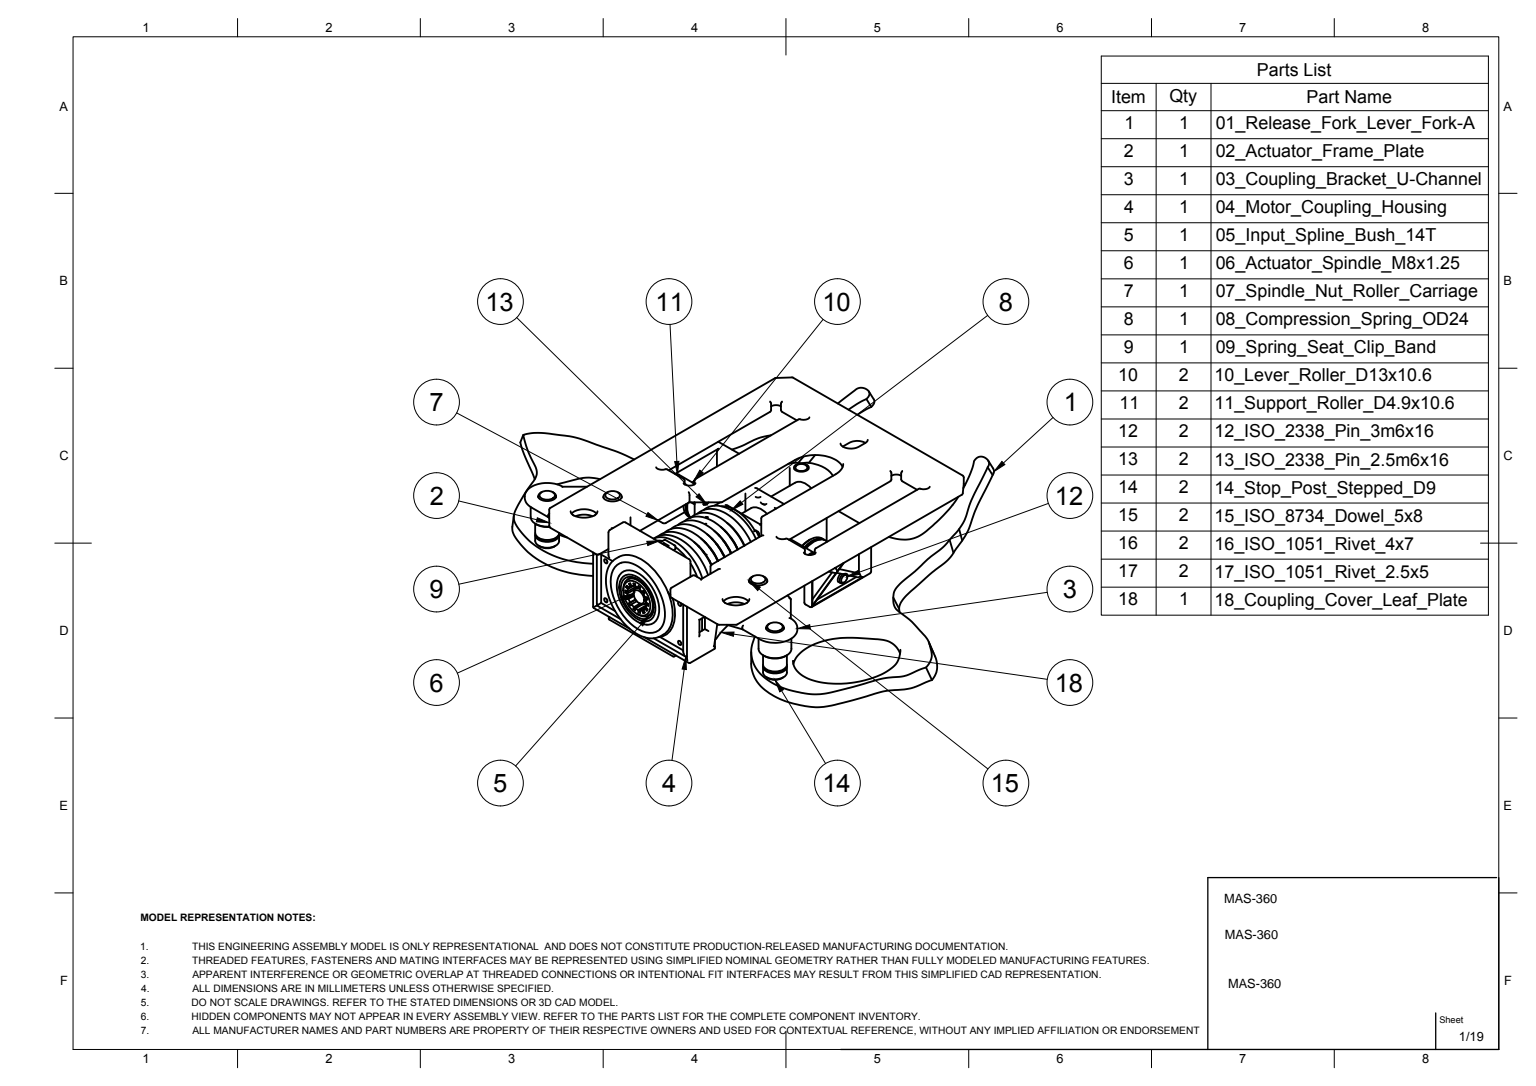
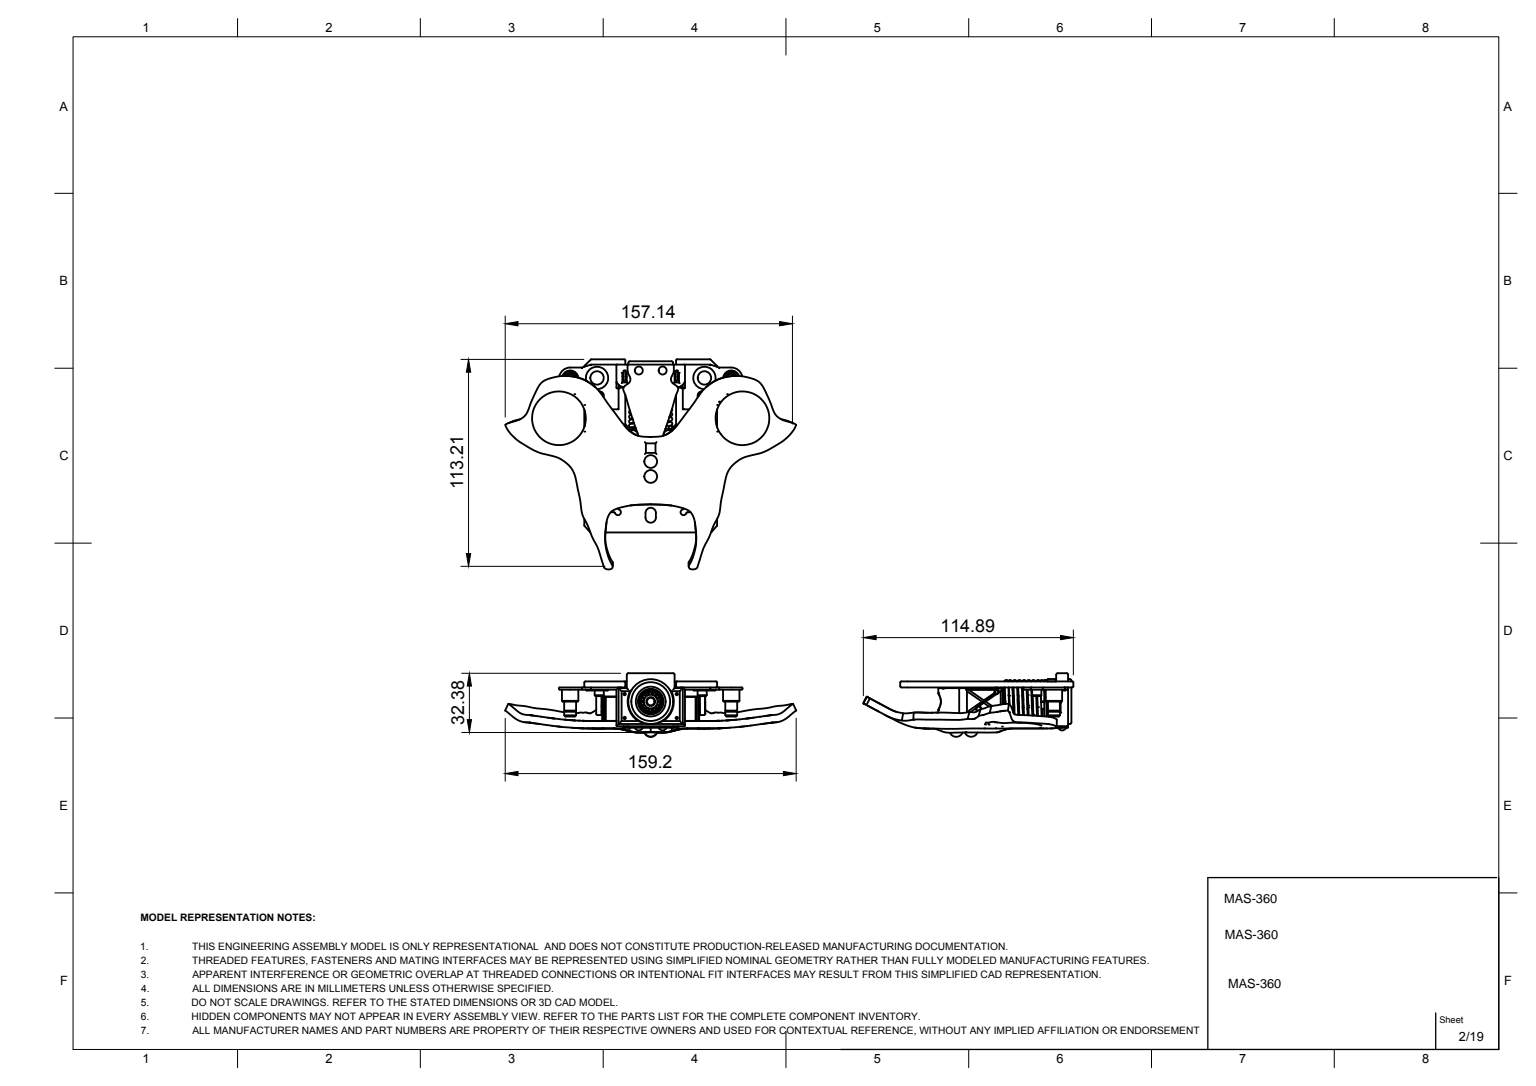
ISO-10303-21;
HEADER;
/* Generated by software containing ST-Developer
 * from STEP Tools, Inc. (www.steptools.com) 
 */

FILE_DESCRIPTION(
/* description */ (''),
/* implementation_level */ '2;1');

FILE_NAME(
/* name */ 'MAS-360',
/* time_stamp */ '2026-11-04T18:53:29-08:00',
/* author */ (''),
/* organization */ (''),
/* preprocessor_version */ 'ST-DEVELOPER v20.2',
/* originating_system */ 'Autodesk Translation Framework v15.17.0.0',
/* authorisation */ '');

FILE_SCHEMA (('AUTOMOTIVE_DESIGN { 1 0 10303 214 3 1 1 }'));
ENDSEC;

DATA;
#10=MECHANICAL_DESIGN_GEOMETRIC_PRESENTATION_REPRESENTATION('',(#1327,#1328,
#1329,#1330,#1331,#1332,#1333,#1334,#1335,#1336,#1337,#1338,#1339,#1340,
#1341,#1342,#1343,#1344),#100031);
#11=ITEM_DEFINED_TRANSFORMATION($,$,#20335,#22499);
#12=ITEM_DEFINED_TRANSFORMATION($,$,#20343,#22500);
#13=ITEM_DEFINED_TRANSFORMATION($,$,#20892,#22501);
#14=ITEM_DEFINED_TRANSFORMATION($,$,#21261,#22502);
#15=ITEM_DEFINED_TRANSFORMATION($,$,#21437,#22503);
#16=ITEM_DEFINED_TRANSFORMATION($,$,#21537,#22504);
#17=ITEM_DEFINED_TRANSFORMATION($,$,#21611,#22505);
#18=ITEM_DEFINED_TRANSFORMATION($,$,#22152,#22506);
#19=ITEM_DEFINED_TRANSFORMATION($,$,#22157,#22507);
#20=ITEM_DEFINED_TRANSFORMATION($,$,#22351,#22508);
#21=ITEM_DEFINED_TRANSFORMATION($,$,#22404,#22509);
#22=ITEM_DEFINED_TRANSFORMATION($,$,#22417,#22510);
#23=ITEM_DEFINED_TRANSFORMATION($,$,#22427,#22511);
#24=ITEM_DEFINED_TRANSFORMATION($,$,#22437,#22512);
#25=ITEM_DEFINED_TRANSFORMATION($,$,#22465,#22513);
#26=ITEM_DEFINED_TRANSFORMATION($,$,#22475,#22514);
#27=ITEM_DEFINED_TRANSFORMATION($,$,#22489,#22515);
#28=ITEM_DEFINED_TRANSFORMATION($,$,#22218,#22516);
#29=ITEM_DEFINED_TRANSFORMATION($,$,#22351,#22517);
#30=ITEM_DEFINED_TRANSFORMATION($,$,#22404,#22518);
#31=ITEM_DEFINED_TRANSFORMATION($,$,#22417,#22519);
#32=ITEM_DEFINED_TRANSFORMATION($,$,#22427,#22520);
#33=ITEM_DEFINED_TRANSFORMATION($,$,#22437,#22521);
#34=ITEM_DEFINED_TRANSFORMATION($,$,#22465,#22522);
#35=ITEM_DEFINED_TRANSFORMATION($,$,#22475,#22523);
#36=ITEM_DEFINED_TRANSFORMATION($,$,#22489,#22524);
#37=(
REPRESENTATION_RELATIONSHIP($,$,#100101,#100100)
REPRESENTATION_RELATIONSHIP_WITH_TRANSFORMATION(#11)
SHAPE_REPRESENTATION_RELATIONSHIP()
);
#38=(
REPRESENTATION_RELATIONSHIP($,$,#100102,#100100)
REPRESENTATION_RELATIONSHIP_WITH_TRANSFORMATION(#12)
SHAPE_REPRESENTATION_RELATIONSHIP()
);
#39=(
REPRESENTATION_RELATIONSHIP($,$,#100103,#100100)
REPRESENTATION_RELATIONSHIP_WITH_TRANSFORMATION(#13)
SHAPE_REPRESENTATION_RELATIONSHIP()
);
#40=(
REPRESENTATION_RELATIONSHIP($,$,#100104,#100100)
REPRESENTATION_RELATIONSHIP_WITH_TRANSFORMATION(#14)
SHAPE_REPRESENTATION_RELATIONSHIP()
);
#41=(
REPRESENTATION_RELATIONSHIP($,$,#100105,#100100)
REPRESENTATION_RELATIONSHIP_WITH_TRANSFORMATION(#15)
SHAPE_REPRESENTATION_RELATIONSHIP()
);
#42=(
REPRESENTATION_RELATIONSHIP($,$,#100106,#100100)
REPRESENTATION_RELATIONSHIP_WITH_TRANSFORMATION(#16)
SHAPE_REPRESENTATION_RELATIONSHIP()
);
#43=(
REPRESENTATION_RELATIONSHIP($,$,#100107,#100100)
REPRESENTATION_RELATIONSHIP_WITH_TRANSFORMATION(#17)
SHAPE_REPRESENTATION_RELATIONSHIP()
);
#44=(
REPRESENTATION_RELATIONSHIP($,$,#100108,#100100)
REPRESENTATION_RELATIONSHIP_WITH_TRANSFORMATION(#18)
SHAPE_REPRESENTATION_RELATIONSHIP()
);
#45=(
REPRESENTATION_RELATIONSHIP($,$,#100109,#100100)
REPRESENTATION_RELATIONSHIP_WITH_TRANSFORMATION(#19)
SHAPE_REPRESENTATION_RELATIONSHIP()
);
#46=(
REPRESENTATION_RELATIONSHIP($,$,#100111,#100100)
REPRESENTATION_RELATIONSHIP_WITH_TRANSFORMATION(#20)
SHAPE_REPRESENTATION_RELATIONSHIP()
);
#47=(
REPRESENTATION_RELATIONSHIP($,$,#100112,#100100)
REPRESENTATION_RELATIONSHIP_WITH_TRANSFORMATION(#21)
SHAPE_REPRESENTATION_RELATIONSHIP()
);
#48=(
REPRESENTATION_RELATIONSHIP($,$,#100113,#100100)
REPRESENTATION_RELATIONSHIP_WITH_TRANSFORMATION(#22)
SHAPE_REPRESENTATION_RELATIONSHIP()
);
#49=(
REPRESENTATION_RELATIONSHIP($,$,#100114,#100100)
REPRESENTATION_RELATIONSHIP_WITH_TRANSFORMATION(#23)
SHAPE_REPRESENTATION_RELATIONSHIP()
);
#50=(
REPRESENTATION_RELATIONSHIP($,$,#100115,#100100)
REPRESENTATION_RELATIONSHIP_WITH_TRANSFORMATION(#24)
SHAPE_REPRESENTATION_RELATIONSHIP()
);
#51=(
REPRESENTATION_RELATIONSHIP($,$,#100116,#100100)
REPRESENTATION_RELATIONSHIP_WITH_TRANSFORMATION(#25)
SHAPE_REPRESENTATION_RELATIONSHIP()
);
#52=(
REPRESENTATION_RELATIONSHIP($,$,#100117,#100100)
REPRESENTATION_RELATIONSHIP_WITH_TRANSFORMATION(#26)
SHAPE_REPRESENTATION_RELATIONSHIP()
);
#53=(
REPRESENTATION_RELATIONSHIP($,$,#100118,#100100)
REPRESENTATION_RELATIONSHIP_WITH_TRANSFORMATION(#27)
SHAPE_REPRESENTATION_RELATIONSHIP()
);
#54=(
REPRESENTATION_RELATIONSHIP($,$,#100110,#100100)
REPRESENTATION_RELATIONSHIP_WITH_TRANSFORMATION(#28)
SHAPE_REPRESENTATION_RELATIONSHIP()
);
#55=(
REPRESENTATION_RELATIONSHIP($,$,#100111,#100100)
REPRESENTATION_RELATIONSHIP_WITH_TRANSFORMATION(#29)
SHAPE_REPRESENTATION_RELATIONSHIP()
);
#56=(
REPRESENTATION_RELATIONSHIP($,$,#100112,#100100)
REPRESENTATION_RELATIONSHIP_WITH_TRANSFORMATION(#30)
SHAPE_REPRESENTATION_RELATIONSHIP()
);
#57=(
REPRESENTATION_RELATIONSHIP($,$,#100113,#100100)
REPRESENTATION_RELATIONSHIP_WITH_TRANSFORMATION(#31)
SHAPE_REPRESENTATION_RELATIONSHIP()
);
#58=(
REPRESENTATION_RELATIONSHIP($,$,#100114,#100100)
REPRESENTATION_RELATIONSHIP_WITH_TRANSFORMATION(#32)
SHAPE_REPRESENTATION_RELATIONSHIP()
);
#59=(
REPRESENTATION_RELATIONSHIP($,$,#100115,#100100)
REPRESENTATION_RELATIONSHIP_WITH_TRANSFORMATION(#33)
SHAPE_REPRESENTATION_RELATIONSHIP()
);
#60=(
REPRESENTATION_RELATIONSHIP($,$,#100116,#100100)
REPRESENTATION_RELATIONSHIP_WITH_TRANSFORMATION(#34)
SHAPE_REPRESENTATION_RELATIONSHIP()
);
#61=(
REPRESENTATION_RELATIONSHIP($,$,#100117,#100100)
REPRESENTATION_RELATIONSHIP_WITH_TRANSFORMATION(#35)
SHAPE_REPRESENTATION_RELATIONSHIP()
);
#62=(
REPRESENTATION_RELATIONSHIP($,$,#100118,#100100)
REPRESENTATION_RELATIONSHIP_WITH_TRANSFORMATION(#36)
SHAPE_REPRESENTATION_RELATIONSHIP()
);
#63=CONTEXT_DEPENDENT_SHAPE_REPRESENTATION(#37,#100074);
#64=CONTEXT_DEPENDENT_SHAPE_REPRESENTATION(#38,#100075);
#65=CONTEXT_DEPENDENT_SHAPE_REPRESENTATION(#39,#100076);
#66=CONTEXT_DEPENDENT_SHAPE_REPRESENTATION(#40,#100077);
#67=CONTEXT_DEPENDENT_SHAPE_REPRESENTATION(#41,#100078);
#68=CONTEXT_DEPENDENT_SHAPE_REPRESENTATION(#42,#100079);
#69=CONTEXT_DEPENDENT_SHAPE_REPRESENTATION(#43,#100080);
#70=CONTEXT_DEPENDENT_SHAPE_REPRESENTATION(#44,#100081);
#71=CONTEXT_DEPENDENT_SHAPE_REPRESENTATION(#45,#100082);
#72=CONTEXT_DEPENDENT_SHAPE_REPRESENTATION(#46,#100083);
#73=CONTEXT_DEPENDENT_SHAPE_REPRESENTATION(#47,#100084);
#74=CONTEXT_DEPENDENT_SHAPE_REPRESENTATION(#48,#100085);
#75=CONTEXT_DEPENDENT_SHAPE_REPRESENTATION(#49,#100086);
#76=CONTEXT_DEPENDENT_SHAPE_REPRESENTATION(#50,#100087);
#77=CONTEXT_DEPENDENT_SHAPE_REPRESENTATION(#51,#100088);
#78=CONTEXT_DEPENDENT_SHAPE_REPRESENTATION(#52,#100089);
#79=CONTEXT_DEPENDENT_SHAPE_REPRESENTATION(#53,#100090);
#80=CONTEXT_DEPENDENT_SHAPE_REPRESENTATION(#54,#100091);
#81=CONTEXT_DEPENDENT_SHAPE_REPRESENTATION(#55,#100092);
#82=CONTEXT_DEPENDENT_SHAPE_REPRESENTATION(#56,#100093);
#83=CONTEXT_DEPENDENT_SHAPE_REPRESENTATION(#57,#100094);
#84=CONTEXT_DEPENDENT_SHAPE_REPRESENTATION(#58,#100095);
#85=CONTEXT_DEPENDENT_SHAPE_REPRESENTATION(#59,#100096);
#86=CONTEXT_DEPENDENT_SHAPE_REPRESENTATION(#60,#100097);
#87=CONTEXT_DEPENDENT_SHAPE_REPRESENTATION(#61,#100098);
#88=CONTEXT_DEPENDENT_SHAPE_REPRESENTATION(#62,#100099);
#89=NEXT_ASSEMBLY_USAGE_OCCURRENCE('01_Release_Fork_Lever_Fork-A:1',
'01_Release_Fork_Lever_Fork-A:1','01_Release_Fork_Lever_Fork-A:1',#100120,
#100121,'01_Release_Fork_Lever_Fork-A:1');
#90=NEXT_ASSEMBLY_USAGE_OCCURRENCE('02_Actuator_Frame_Plate:1',
'02_Actuator_Frame_Plate:1','02_Actuator_Frame_Plate:1',#100120,#100122,
'02_Actuator_Frame_Plate:1');
#91=NEXT_ASSEMBLY_USAGE_OCCURRENCE('03_Coupling_Bracket_U-Channel:1',
'03_Coupling_Bracket_U-Channel:1','03_Coupling_Bracket_U-Channel:1',#100120,
#100123,'03_Coupling_Bracket_U-Channel:1');
#92=NEXT_ASSEMBLY_USAGE_OCCURRENCE('04_Motor_Coupling_Housing:1',
'04_Motor_Coupling_Housing:1','04_Motor_Coupling_Housing:1',#100120,#100124,
'04_Motor_Coupling_Housing:1');
#93=NEXT_ASSEMBLY_USAGE_OCCURRENCE('05_Input_Spline_Bush_14T:1',
'05_Input_Spline_Bush_14T:1','05_Input_Spline_Bush_14T:1',#100120,#100125,
'05_Input_Spline_Bush_14T:1');
#94=NEXT_ASSEMBLY_USAGE_OCCURRENCE('06_Actuator_Spindle_M8x1.25:1',
'06_Actuator_Spindle_M8x1.25:1','06_Actuator_Spindle_M8x1.25:1',#100120,
#100126,'06_Actuator_Spindle_M8x1.25:1');
#95=NEXT_ASSEMBLY_USAGE_OCCURRENCE('07_Spindle_Nut_Roller_Carriage:1',
'07_Spindle_Nut_Roller_Carriage:1','07_Spindle_Nut_Roller_Carriage:1',#100120,
#100127,'07_Spindle_Nut_Roller_Carriage:1');
#96=NEXT_ASSEMBLY_USAGE_OCCURRENCE('08_Compression_Spring_OD24:1',
'08_Compression_Spring_OD24:1','08_Compression_Spring_OD24:1',#100120,#100128,
'08_Compression_Spring_OD24:1');
#97=NEXT_ASSEMBLY_USAGE_OCCURRENCE('09_Spring_Seat_Clip_Band:1',
'09_Spring_Seat_Clip_Band:1','09_Spring_Seat_Clip_Band:1',#100120,#100129,
'09_Spring_Seat_Clip_Band:1');
#98=NEXT_ASSEMBLY_USAGE_OCCURRENCE('10_Lever_Roller_D13x10.6:1',
'10_Lever_Roller_D13x10.6:1','10_Lever_Roller_D13x10.6:1',#100120,#100131,
'10_Lever_Roller_D13x10.6:1');
#99=NEXT_ASSEMBLY_USAGE_OCCURRENCE('11_Support_Roller_D4.9x10.6:1',
'11_Support_Roller_D4.9x10.6:1','11_Support_Roller_D4.9x10.6:1',#100120,
#100132,'11_Support_Roller_D4.9x10.6:1');
#100=NEXT_ASSEMBLY_USAGE_OCCURRENCE('12_ISO_2338_Pin_3m6x16:1',
'12_ISO_2338_Pin_3m6x16:1','12_ISO_2338_Pin_3m6x16:1',#100120,#100133,
'12_ISO_2338_Pin_3m6x16:1');
#101=NEXT_ASSEMBLY_USAGE_OCCURRENCE('13_ISO_2338_Pin_2.5m6x16:1',
'13_ISO_2338_Pin_2.5m6x16:1','13_ISO_2338_Pin_2.5m6x16:1',#100120,#100134,
'13_ISO_2338_Pin_2.5m6x16:1');
#102=NEXT_ASSEMBLY_USAGE_OCCURRENCE('14_Stop_Post_Stepped_D9:1',
'14_Stop_Post_Stepped_D9:1','14_Stop_Post_Stepped_D9:1',#100120,#100135,
'14_Stop_Post_Stepped_D9:1');
#103=NEXT_ASSEMBLY_USAGE_OCCURRENCE('15_ISO_8734_Dowel_5x8:1',
'15_ISO_8734_Dowel_5x8:1','15_ISO_8734_Dowel_5x8:1',#100120,#100136,
'15_ISO_8734_Dowel_5x8:1');
#104=NEXT_ASSEMBLY_USAGE_OCCURRENCE('16_ISO_1051_Rivet_4x7:1',
'16_ISO_1051_Rivet_4x7:1','16_ISO_1051_Rivet_4x7:1',#100120,#100137,
'16_ISO_1051_Rivet_4x7:1');
#105=NEXT_ASSEMBLY_USAGE_OCCURRENCE('17_ISO_1051_Rivet_2.5x5:1',
'17_ISO_1051_Rivet_2.5x5:1','17_ISO_1051_Rivet_2.5x5:1',#100120,#100138,
'17_ISO_1051_Rivet_2.5x5:1');
#106=NEXT_ASSEMBLY_USAGE_OCCURRENCE('18_Coupling_Cover_Leaf_Plate:1',
'18_Coupling_Cover_Leaf_Plate:1','18_Coupling_Cover_Leaf_Plate:1',#100120,
#100130,'18_Coupling_Cover_Leaf_Plate:1');
#107=NEXT_ASSEMBLY_USAGE_OCCURRENCE('10_Lever_Roller_D13x10.6:2',
'10_Lever_Roller_D13x10.6:2','10_Lever_Roller_D13x10.6:2',#100120,#100131,
'10_Lever_Roller_D13x10.6:2');
#108=NEXT_ASSEMBLY_USAGE_OCCURRENCE('11_Support_Roller_D4.9x10.6:2',
'11_Support_Roller_D4.9x10.6:2','11_Support_Roller_D4.9x10.6:2',#100120,
#100132,'11_Support_Roller_D4.9x10.6:2');
#109=NEXT_ASSEMBLY_USAGE_OCCURRENCE('12_ISO_2338_Pin_3m6x16:2',
'12_ISO_2338_Pin_3m6x16:2','12_ISO_2338_Pin_3m6x16:2',#100120,#100133,
'12_ISO_2338_Pin_3m6x16:2');
#110=NEXT_ASSEMBLY_USAGE_OCCURRENCE('13_ISO_2338_Pin_2.5m6x16:2',
'13_ISO_2338_Pin_2.5m6x16:2','13_ISO_2338_Pin_2.5m6x16:2',#100120,#100134,
'13_ISO_2338_Pin_2.5m6x16:2');
#111=NEXT_ASSEMBLY_USAGE_OCCURRENCE('14_Stop_Post_Stepped_D9:2',
'14_Stop_Post_Stepped_D9:2','14_Stop_Post_Stepped_D9:2',#100120,#100135,
'14_Stop_Post_Stepped_D9:2');
#112=NEXT_ASSEMBLY_USAGE_OCCURRENCE('15_ISO_8734_Dowel_5x8:2',
'15_ISO_8734_Dowel_5x8:2','15_ISO_8734_Dowel_5x8:2',#100120,#100136,
'15_ISO_8734_Dowel_5x8:2');
#113=NEXT_ASSEMBLY_USAGE_OCCURRENCE('16_ISO_1051_Rivet_4x7:2',
'16_ISO_1051_Rivet_4x7:2','16_ISO_1051_Rivet_4x7:2',#100120,#100137,
'16_ISO_1051_Rivet_4x7:2');
#114=NEXT_ASSEMBLY_USAGE_OCCURRENCE('17_ISO_1051_Rivet_2.5x5:2',
'17_ISO_1051_Rivet_2.5x5:2','17_ISO_1051_Rivet_2.5x5:2',#100120,#100138,
'17_ISO_1051_Rivet_2.5x5:2');
#115=(
BOUNDED_SURFACE()
B_SPLINE_SURFACE(2,2,((#92994,#92995,#92996),(#92997,#92998,#92999),(#93000,
#93001,#93002)),.UNSPECIFIED.,.F.,.F.,.F.)
B_SPLINE_SURFACE_WITH_KNOTS((3,3),(3,3),(1.57079632679489,3.14159265358979),
(0.249866624394877,1.57079632679493),.UNSPECIFIED.)
GEOMETRIC_REPRESENTATION_ITEM()
RATIONAL_B_SPLINE_SURFACE(((1.,0.789707138049851,1.),(0.707106781186533,
0.558407272466459,0.707106781186533),(1.,0.789707138049851,1.)))
REPRESENTATION_ITEM('')
SURFACE()
);
#116=(
BOUNDED_SURFACE()
B_SPLINE_SURFACE(2,2,((#93105,#93106,#93107),(#93108,#93109,#93110),(#93111,
#93112,#93113)),.UNSPECIFIED.,.F.,.F.,.F.)
B_SPLINE_SURFACE_WITH_KNOTS((3,3),(3,3),(1.57079632679486,3.14159265358979),
(-0.510805552608252,0.510805552608253),.UNSPECIFIED.)
GEOMETRIC_REPRESENTATION_ITEM()
RATIONAL_B_SPLINE_SURFACE(((1.,0.872350972065279,1.),(0.707106781186551,
0.616845287922038,0.707106781186551),(1.,0.872350972065279,1.)))
REPRESENTATION_ITEM('')
SURFACE()
);
#117=SPHERICAL_SURFACE('',#20359,0.6);
#118=SPHERICAL_SURFACE('',#20362,0.6);
#119=SPHERICAL_SURFACE('',#20376,0.6);
#120=SPHERICAL_SURFACE('',#20379,0.6);
#121=SPHERICAL_SURFACE('',#20389,0.6);
#122=SPHERICAL_SURFACE('',#20391,0.6);
#123=SPHERICAL_SURFACE('',#20401,0.6);
#124=SPHERICAL_SURFACE('',#20404,0.6);
#125=SPHERICAL_SURFACE('',#20414,0.6);
#126=SPHERICAL_SURFACE('',#20417,0.6);
#127=SPHERICAL_SURFACE('',#20430,0.6);
#128=SPHERICAL_SURFACE('',#20432,0.6);
#129=SPHERICAL_SURFACE('',#20487,0.6);
#130=SPHERICAL_SURFACE('',#20492,0.6);
#131=SPHERICAL_SURFACE('',#20504,0.6);
#132=SPHERICAL_SURFACE('',#20509,0.600000000000001);
#133=SPHERICAL_SURFACE('',#20513,0.6);
#134=SPHERICAL_SURFACE('',#20518,0.600000000000001);
#135=SPHERICAL_SURFACE('',#20523,0.600000000000001);
#136=SPHERICAL_SURFACE('',#20530,0.6);
#137=SPHERICAL_SURFACE('',#20535,0.6);
#138=SPHERICAL_SURFACE('',#20540,0.6);
#139=SPHERICAL_SURFACE('',#20545,0.6);
#140=SPHERICAL_SURFACE('',#20554,0.6);
#141=SPHERICAL_SURFACE('',#20558,0.6);
#142=SPHERICAL_SURFACE('',#20566,0.6);
#143=SPHERICAL_SURFACE('',#20577,0.6);
#144=SPHERICAL_SURFACE('',#20582,0.6);
#145=SPHERICAL_SURFACE('',#20603,0.600000000000001);
#146=SPHERICAL_SURFACE('',#20608,0.600000000000001);
#147=SPHERICAL_SURFACE('',#20613,0.600000000000001);
#148=SPHERICAL_SURFACE('',#20618,0.600000000000001);
#149=SPHERICAL_SURFACE('',#20627,0.600000000000001);
#150=SPHERICAL_SURFACE('',#20635,0.6);
#151=SPHERICAL_SURFACE('',#20640,0.6);
#152=SPHERICAL_SURFACE('',#20645,0.6);
#153=SPHERICAL_SURFACE('',#20650,0.6);
#154=SPHERICAL_SURFACE('',#20655,0.6);
#155=SPHERICAL_SURFACE('',#20660,0.6);
#156=SPHERICAL_SURFACE('',#20690,0.600000000000001);
#157=SPHERICAL_SURFACE('',#20697,0.6);
#158=SPHERICAL_SURFACE('',#20698,0.6);
#159=SPHERICAL_SURFACE('',#20704,0.6);
#160=SPHERICAL_SURFACE('',#20713,0.600000000000001);
#161=SPHERICAL_SURFACE('',#20716,0.600000000000005);
#162=SPHERICAL_SURFACE('',#20721,0.6);
#163=SPHERICAL_SURFACE('',#20729,0.6);
#164=SPHERICAL_SURFACE('',#20732,0.6);
#165=SPHERICAL_SURFACE('',#20737,0.6);
#166=SPHERICAL_SURFACE('',#20742,0.6);
#167=SPHERICAL_SURFACE('',#20749,0.6);
#168=SPHERICAL_SURFACE('',#20755,0.6);
#169=SPHERICAL_SURFACE('',#20763,0.6);
#170=SPHERICAL_SURFACE('',#20769,0.600000000000001);
#171=SPHERICAL_SURFACE('',#20779,0.600000000000001);
#172=SPHERICAL_SURFACE('',#20788,0.600000000000001);
#173=SPHERICAL_SURFACE('',#20793,0.600000000000001);
#174=SPHERICAL_SURFACE('',#20798,0.600000000000001);
#175=SPHERICAL_SURFACE('',#20810,0.6);
#176=SPHERICAL_SURFACE('',#20815,0.6);
#177=SPHERICAL_SURFACE('',#20820,0.6);
#178=SPHERICAL_SURFACE('',#20825,0.6);
#179=SPHERICAL_SURFACE('',#20830,0.6);
#180=SPHERICAL_SURFACE('',#20832,0.6);
#181=SPHERICAL_SURFACE('',#20936,0.4);
#182=SPHERICAL_SURFACE('',#20950,0.4);
#183=SPHERICAL_SURFACE('',#20969,0.4);
#184=SPHERICAL_SURFACE('',#20993,0.4);
#185=SPHERICAL_SURFACE('',#21262,0.800000000000001);
#186=SPHERICAL_SURFACE('',#21266,0.8);
#187=SPHERICAL_SURFACE('',#21275,0.800000000000001);
#188=SPHERICAL_SURFACE('',#21285,0.800000000000001);
#189=SPHERICAL_SURFACE('',#21292,0.800000000000003);
#190=SPHERICAL_SURFACE('',#21298,0.800000000000001);
#191=SPHERICAL_SURFACE('',#21302,0.800000000000001);
#192=SPHERICAL_SURFACE('',#21308,0.800000000000001);
#193=SPHERICAL_SURFACE('',#21315,0.8);
#194=SPHERICAL_SURFACE('',#21323,0.8);
#195=SPHERICAL_SURFACE('',#21330,0.8);
#196=SPHERICAL_SURFACE('',#21334,0.8);
#197=SPHERICAL_SURFACE('',#21671,0.6);
#198=SPHERICAL_SURFACE('',#21685,0.6);
#199=SPHERICAL_SURFACE('',#21687,0.6);
#200=SPHERICAL_SURFACE('',#21738,0.6);
#201=SPHERICAL_SURFACE('',#21740,0.6);
#202=SPHERICAL_SURFACE('',#21744,0.6);
#203=SPHERICAL_SURFACE('',#21773,0.6);
#204=SPHERICAL_SURFACE('',#21778,0.6);
#205=SPHERICAL_SURFACE('',#21825,0.6);
#206=SPHERICAL_SURFACE('',#21828,0.6);
#207=SPHERICAL_SURFACE('',#21856,0.6);
#208=SPHERICAL_SURFACE('',#21866,0.6);
#209=SPHERICAL_SURFACE('',#21974,0.6);
#210=SPHERICAL_SURFACE('',#21975,0.6);
#211=SPHERICAL_SURFACE('',#21984,0.6);
#212=SPHERICAL_SURFACE('',#21997,0.6);
#213=SPHERICAL_SURFACE('',#21999,0.6);
#214=SPHERICAL_SURFACE('',#22008,0.6);
#215=SPHERICAL_SURFACE('',#22076,0.6);
#216=SPHERICAL_SURFACE('',#22078,0.6);
#217=SPHERICAL_SURFACE('',#22231,0.3);
#218=SPHERICAL_SURFACE('',#22233,0.3);
#219=SPHERICAL_SURFACE('',#22235,0.3);
#220=SPHERICAL_SURFACE('',#22237,0.3);
#221=SPHERICAL_SURFACE('',#22253,0.3);
#222=SPHERICAL_SURFACE('',#22257,0.3);
#223=SPHERICAL_SURFACE('',#22268,0.3);
#224=SPHERICAL_SURFACE('',#22270,0.3);
#225=SPHERICAL_SURFACE('',#22476,3.75208333333333);
#226=SPHERICAL_SURFACE('',#22490,2.36333333333333);
#227=CONICAL_SURFACE('',#20353,4.08,0.785398163397448);
#228=CONICAL_SURFACE('',#20885,4.08,0.785398163397448);
#229=CONICAL_SURFACE('',#21430,4.075,0.785398163397448);
#230=CONICAL_SURFACE('',#21438,5.5488,0.785398163397448);
#231=CONICAL_SURFACE('',#21447,5.4672,0.785398163397448);
#232=CONICAL_SURFACE('',#21595,3.6736,0.785398163397448);
#233=CONICAL_SURFACE('',#21596,3.5,0.78539816339745);
#234=CONICAL_SURFACE('',#21608,2.244,0.785398163397449);
#235=CONICAL_SURFACE('',#22396,6.2832,0.785398163397447);
#236=CONICAL_SURFACE('',#22400,6.2832,0.785398163397447);
#237=CONICAL_SURFACE('',#22405,2.3256,0.785398163397447);
#238=CONICAL_SURFACE('',#22410,2.3256,0.785398163397447);
#239=CONICAL_SURFACE('',#22418,1.3368,0.785398163397446);
#240=CONICAL_SURFACE('',#22423,1.3368,0.785398163397446);
#241=CONICAL_SURFACE('',#22428,1.0868,0.785398163397447);
#242=CONICAL_SURFACE('',#22433,1.0868,0.785398163397447);
#243=CONICAL_SURFACE('',#22440,2.2848,0.785398163397448);
#244=CONICAL_SURFACE('',#22448,4.284,0.785398163397447);
#245=CONICAL_SURFACE('',#22462,2.9376,0.785398163397446);
#246=CONICAL_SURFACE('',#22466,2.2552,0.785398163397448);
#247=CONICAL_SURFACE('',#22471,2.2552,0.785398163397448);
#248=CONICAL_SURFACE('',#22486,3.0368,0.785398163397448);
#249=CONICAL_SURFACE('',#22496,1.1276,0.785398163397447);
#250=CIRCLE('',#20345,3.84773593128807);
#251=CIRCLE('',#20346,0.6);
#252=CIRCLE('',#20347,3.672);
#253=CIRCLE('',#20348,3.672);
#254=CIRCLE('',#20349,3.84773593128807);
#255=CIRCLE('',#20351,3.672);
#256=CIRCLE('',#20352,3.672);
#257=CIRCLE('',#20354,4.31226406871192);
#258=CIRCLE('',#20355,4.31226406871192);
#259=CIRCLE('',#20357,0.600000000000001);
#260=CIRCLE('',#20358,0.599999999999999);
#261=CIRCLE('',#20360,0.6);
#262=CIRCLE('',#20361,0.599999999999999);
#263=CIRCLE('',#20363,0.599999999999999);
#264=CIRCLE('',#20364,0.6);
#265=CIRCLE('',#20366,0.599999999999999);
#266=CIRCLE('',#20368,1.632);
#267=CIRCLE('',#20369,0.599999999999998);
#268=CIRCLE('',#20370,2.232);
#269=CIRCLE('',#20372,1.632);
#270=CIRCLE('',#20374,0.600000000000001);
#271=CIRCLE('',#20375,0.599999999999998);
#272=CIRCLE('',#20377,0.6);
#273=CIRCLE('',#20378,0.599999999999999);
#274=CIRCLE('',#20380,0.6);
#275=CIRCLE('',#20382,2.232);
#276=CIRCLE('',#20383,0.6);
#277=CIRCLE('',#20384,1.632);
#278=CIRCLE('',#20387,0.600000000000001);
#279=CIRCLE('',#20388,0.599999999999998);
#280=CIRCLE('',#20390,0.599999999999999);
#281=CIRCLE('',#20392,0.599999999999999);
#282=CIRCLE('',#20393,0.6);
#283=CIRCLE('',#20395,0.599999999999999);
#284=CIRCLE('',#20397,1.632);
#285=CIRCLE('',#20399,0.600000000000001);
#286=CIRCLE('',#20400,0.600000000000003);
#287=CIRCLE('',#20402,0.6);
#288=CIRCLE('',#20403,0.599999999999999);
#289=CIRCLE('',#20405,0.6);
#290=CIRCLE('',#20407,2.232);
#291=CIRCLE('',#20408,0.600000000000001);
#292=CIRCLE('',#20409,1.632);
#293=CIRCLE('',#20412,0.600000000000001);
#294=CIRCLE('',#20413,0.600000000000003);
#295=CIRCLE('',#20415,0.6);
#296=CIRCLE('',#20416,0.6);
#297=CIRCLE('',#20418,0.6);
#298=CIRCLE('',#20419,0.6);
#299=CIRCLE('',#20421,2.232);
#300=CIRCLE('',#20422,0.6);
#301=CIRCLE('',#20423,1.632);
#302=CIRCLE('',#20425,0.6);
#303=CIRCLE('',#20428,0.599999999999996);
#304=CIRCLE('',#20429,0.599999999999999);
#305=CIRCLE('',#20431,0.599999999999999);
#306=CIRCLE('',#20433,0.599999999999999);
#307=CIRCLE('',#20434,0.6);
#308=CIRCLE('',#20436,0.599999999999999);
#309=CIRCLE('',#20438,1.632);
#310=CIRCLE('',#20440,3.1);
#311=CIRCLE('',#20441,0.6);
#312=CIRCLE('',#20442,2.5);
#313=CIRCLE('',#20443,2.5);
#314=CIRCLE('',#20445,8.1888);
#315=CIRCLE('',#20446,4.272);
#316=CIRCLE('',#20447,3.456);
#317=CIRCLE('',#20448,3.456);
#318=CIRCLE('',#20449,2.232);
#319=CIRCLE('',#20450,2.232);
#320=CIRCLE('',#20451,2.232);
#321=CIRCLE('',#20452,2.232);
#322=CIRCLE('',#20453,3.1);
#323=CIRCLE('',#20454,2.232);
#324=CIRCLE('',#20455,2.232);
#325=CIRCLE('',#20456,2.232);
#326=CIRCLE('',#20457,2.232);
#327=CIRCLE('',#20458,4.272);
#328=CIRCLE('',#20460,2.5);
#329=CIRCLE('',#20461,2.5);
#330=CIRCLE('',#20463,0.6);
#331=CIRCLE('',#20464,3.672);
#332=CIRCLE('',#20465,3.672);
#333=CIRCLE('',#20467,3.672);
#334=CIRCLE('',#20468,3.672);
#335=CIRCLE('',#20470,0.6);
#336=CIRCLE('',#20472,0.600000000000005);
#337=CIRCLE('',#20473,0.6);
#338=CIRCLE('',#20475,0.6);
#339=CIRCLE('',#20476,2.856);
#340=CIRCLE('',#20478,0.6);
#341=CIRCLE('',#20480,2.856);
#342=CIRCLE('',#20482,2.856);
#343=CIRCLE('',#20485,0.600000000000001);
#344=CIRCLE('',#20488,0.600000000000001);
#345=CIRCLE('',#20489,0.6);
#346=CIRCLE('',#20490,0.6);
#347=CIRCLE('',#20493,0.600000000000001);
#348=CIRCLE('',#20494,0.6);
#349=CIRCLE('',#20497,0.599999999999998);
#350=CIRCLE('',#20499,0.600000000000001);
#351=CIRCLE('',#20500,1.632);
#352=CIRCLE('',#20503,0.600000000000001);
#353=CIRCLE('',#20505,0.599999999999999);
#354=CIRCLE('',#20506,0.6);
#355=CIRCLE('',#20508,0.600000000000001);
#356=CIRCLE('',#20510,0.600000000000001);
#357=CIRCLE('',#20511,0.600000000000001);
#358=CIRCLE('',#20512,0.599999999999991);
#359=CIRCLE('',#20514,0.600000000000001);
#360=CIRCLE('',#20515,0.6);
#361=CIRCLE('',#20516,0.600000000000003);
#362=CIRCLE('',#20519,0.600000000000001);
#363=CIRCLE('',#20520,0.600000000000001);
#364=CIRCLE('',#20521,0.599999999999996);
#365=CIRCLE('',#20524,0.599999999999996);
#366=CIRCLE('',#20525,0.600000000000001);
#367=CIRCLE('',#20526,0.600000000000001);
#368=CIRCLE('',#20529,0.600000000000001);
#369=CIRCLE('',#20531,0.600000000000003);
#370=CIRCLE('',#20532,0.6);
#371=CIRCLE('',#20534,0.600000000000001);
#372=CIRCLE('',#20536,0.600000000000003);
#373=CIRCLE('',#20537,0.599999999999999);
#374=CIRCLE('',#20539,0.599999999999996);
#375=CIRCLE('',#20541,0.599999999999999);
#376=CIRCLE('',#20542,0.599999999999998);
#377=CIRCLE('',#20544,0.60000000000001);
#378=CIRCLE('',#20546,0.600000000000003);
#379=CIRCLE('',#20547,0.599999999999999);
#380=CIRCLE('',#20552,0.600000000000003);
#381=CIRCLE('',#20555,0.600000000000001);
#382=CIRCLE('',#20556,0.6);
#383=CIRCLE('',#20557,0.600000000000001);
#384=CIRCLE('',#20559,0.6);
#385=CIRCLE('',#20560,0.599999999999999);
#386=CIRCLE('',#20561,0.6);
#387=CIRCLE('',#20564,0.600000000000003);
#388=CIRCLE('',#20565,1.632);
#389=CIRCLE('',#20567,0.600000000000001);
#390=CIRCLE('',#20568,0.6);
#391=CIRCLE('',#20570,0.600000000000005);
#392=CIRCLE('',#20572,1.632);
#393=CIRCLE('',#20573,0.599999999999998);
#394=CIRCLE('',#20578,0.6);
#395=CIRCLE('',#20579,0.6);
#396=CIRCLE('',#20580,0.6);
#397=CIRCLE('',#20583,0.599999999999998);
#398=CIRCLE('',#20585,2.232);
#399=CIRCLE('',#20586,0.6);
#400=CIRCLE('',#20587,1.632);
#401=CIRCLE('',#20589,0.599999999999999);
#402=CIRCLE('',#20592,0.600000000000004);
#403=CIRCLE('',#20595,0.600000000000001);
#404=CIRCLE('',#20597,0.6);
#405=CIRCLE('',#20598,2.5);
#406=CIRCLE('',#20599,2.5);
#407=CIRCLE('',#20601,2.5);
#408=CIRCLE('',#20602,2.5);
#409=CIRCLE('',#20604,0.600000000000001);
#410=CIRCLE('',#20605,0.600000000000001);
#411=CIRCLE('',#20606,0.599999999999999);
#412=CIRCLE('',#20609,0.599999999999996);
#413=CIRCLE('',#20610,0.600000000000001);
#414=CIRCLE('',#20611,0.599999999999996);
#415=CIRCLE('',#20614,0.599999999999987);
#416=CIRCLE('',#20615,0.600000000000001);
#417=CIRCLE('',#20616,0.600000000000001);
#418=CIRCLE('',#20619,0.600000000000001);
#419=CIRCLE('',#20620,0.600000000000001);
#420=CIRCLE('',#20621,0.600000000000001);
#421=CIRCLE('',#20628,0.600000000000005);
#422=CIRCLE('',#20629,0.600000000000001);
#423=CIRCLE('',#20630,0.600000000000001);
#424=CIRCLE('',#20634,0.600000000000001);
#425=CIRCLE('',#20636,0.599999999999999);
#426=CIRCLE('',#20637,0.599999999999999);
#427=CIRCLE('',#20639,0.600000000000001);
#428=CIRCLE('',#20641,0.600000000000003);
#429=CIRCLE('',#20642,0.599999999999999);
#430=CIRCLE('',#20644,0.600000000000001);
#431=CIRCLE('',#20646,0.599999999999999);
#432=CIRCLE('',#20647,0.599999999999999);
#433=CIRCLE('',#20649,0.599999999999996);
#434=CIRCLE('',#20651,0.599999999999999);
#435=CIRCLE('',#20652,0.600000000000001);
#436=CIRCLE('',#20654,0.599999999999996);
#437=CIRCLE('',#20656,0.600000000000003);
#438=CIRCLE('',#20657,0.599999999999999);
#439=CIRCLE('',#20659,0.600000000000001);
#440=CIRCLE('',#20661,0.599999999999999);
#441=CIRCLE('',#20678,3.1);
#442=CIRCLE('',#20679,0.6);
#443=CIRCLE('',#20681,8.1888);
#444=CIRCLE('',#20682,2.232);
#445=CIRCLE('',#20683,2.232);
#446=CIRCLE('',#20684,2.232);
#447=CIRCLE('',#20685,3.456);
#448=CIRCLE('',#20686,3.456);
#449=CIRCLE('',#20687,4.73652813742386);
#450=CIRCLE('',#20688,4.73652813742386);
#451=CIRCLE('',#20689,3.1);
#452=CIRCLE('',#20691,0.600000000000001);
#453=CIRCLE('',#20693,0.600000000000001);
#454=CIRCLE('',#20696,0.600000000000003);
#455=CIRCLE('',#20705,0.600000000000001);
#456=CIRCLE('',#20706,0.600000000000003);
#457=CIRCLE('',#20707,0.6);
#458=CIRCLE('',#20714,0.599999999999999);
#459=CIRCLE('',#20715,0.600000000000001);
#460=CIRCLE('',#20717,0.600000000000001);
#461=CIRCLE('',#20718,0.600000000000005);
#462=CIRCLE('',#20719,0.599999999999998);
#463=CIRCLE('',#20722,0.599999999999998);
#464=CIRCLE('',#20723,0.599999999999999);
#465=CIRCLE('',#20724,0.599999999999999);
#466=CIRCLE('',#20726,1.632);
#467=CIRCLE('',#20728,0.599999999999998);
#468=CIRCLE('',#20730,0.6);
#469=CIRCLE('',#20731,0.599999999999999);
#470=CIRCLE('',#20733,0.6);
#471=CIRCLE('',#20734,0.599999999999999);
#472=CIRCLE('',#20735,0.6);
#473=CIRCLE('',#20738,0.6);
#474=CIRCLE('',#20740,1.632);
#475=CIRCLE('',#20743,0.599999999999998);
#476=CIRCLE('',#20744,0.6);
#477=CIRCLE('',#20747,1.632);
#478=CIRCLE('',#20748,0.600000000000003);
#479=CIRCLE('',#20750,0.600000000000001);
#480=CIRCLE('',#20751,0.599999999999999);
#481=CIRCLE('',#20753,0.6);
#482=CIRCLE('',#20754,1.632);
#483=CIRCLE('',#20756,0.6);
#484=CIRCLE('',#20757,0.599999999999999);
#485=CIRCLE('',#20758,0.6);
#486=CIRCLE('',#20762,0.600000000000003);
#487=CIRCLE('',#20764,0.599999999999999);
#488=CIRCLE('',#20768,0.599999999999999);
#489=CIRCLE('',#20770,0.600000000000001);
#490=CIRCLE('',#20771,0.600000000000001);
#491=CIRCLE('',#20772,0.599999999999999);
#492=CIRCLE('',#20774,0.600000000000001);
#493=CIRCLE('',#20775,7.5888);
#494=CIRCLE('',#20780,0.600000000000001);
#495=CIRCLE('',#20781,0.600000000000001);
#496=CIRCLE('',#20782,0.600000000000001);
#497=CIRCLE('',#20789,0.600000000000001);
#498=CIRCLE('',#20790,0.600000000000001);
#499=CIRCLE('',#20791,0.600000000000001);
#500=CIRCLE('',#20794,0.600000000000001);
#501=CIRCLE('',#20795,0.600000000000001);
#502=CIRCLE('',#20796,0.599999999999996);
#503=CIRCLE('',#20799,0.599999999999996);
#504=CIRCLE('',#20800,0.600000000000001);
#505=CIRCLE('',#20801,0.599999999999999);
#506=CIRCLE('',#20805,0.599999999999999);
#507=CIRCLE('',#20807,0.600000000000001);
#508=CIRCLE('',#20809,0.599999999999996);
#509=CIRCLE('',#20811,0.599999999999999);
#510=CIRCLE('',#20812,0.599999999999999);
#511=CIRCLE('',#20814,0.600000000000001);
#512=CIRCLE('',#20816,0.599999999999999);
#513=CIRCLE('',#20817,0.600000000000003);
#514=CIRCLE('',#20819,0.600000000000001);
#515=CIRCLE('',#20821,0.599999999999999);
#516=CIRCLE('',#20822,0.599999999999999);
#517=CIRCLE('',#20824,0.599999999999999);
#518=CIRCLE('',#20826,0.599999999999999);
#519=CIRCLE('',#20827,0.6);
#520=CIRCLE('',#20829,0.600000000000001);
#521=CIRCLE('',#20831,0.599999999999999);
#522=CIRCLE('',#20833,0.6);
#523=CIRCLE('',#20835,0.600000000000001);
#524=CIRCLE('',#20855,0.600000000000001);
#525=CIRCLE('',#20857,7.5888);
#526=CIRCLE('',#20863,1.632);
#527=CIRCLE('',#20868,0.6);
#528=CIRCLE('',#20870,0.600000000000001);
#529=CIRCLE('',#20871,0.6);
#530=CIRCLE('',#20873,0.6);
#531=CIRCLE('',#20874,2.856);
#532=CIRCLE('',#20876,0.6);
#533=CIRCLE('',#20880,0.6);
#534=CIRCLE('',#20882,4.31226406871192);
#535=CIRCLE('',#20883,0.6);
#536=CIRCLE('',#20884,4.31226406871192);
#537=CIRCLE('',#20886,3.84773593128807);
#538=CIRCLE('',#20887,3.84773593128807);
#539=CIRCLE('',#20889,0.6);
#540=CIRCLE('',#20937,0.4);
#541=CIRCLE('',#20938,0.4);
#542=CIRCLE('',#20939,0.399999999999999);
#543=CIRCLE('',#20951,0.400000000000003);
#544=CIRCLE('',#20952,0.399999999999999);
#545=CIRCLE('',#20953,0.400000000000001);
#546=CIRCLE('',#20965,0.4);
#547=CIRCLE('',#20970,0.4);
#548=CIRCLE('',#20971,0.400000000000001);
#549=CIRCLE('',#20972,0.399999999999999);
#550=CIRCLE('',#20977,5.72);
#551=CIRCLE('',#20978,6.12);
#552=CIRCLE('',#20984,6.12);
#553=CIRCLE('',#20992,0.4);
#554=CIRCLE('',#20994,0.399999999999999);
#555=CIRCLE('',#20995,0.4);
#556=CIRCLE('',#21012,0.4);
#557=CIRCLE('',#21014,6.12);
#558=CIRCLE('',#21015,5.72);
#559=CIRCLE('',#21025,6.12);
#560=CIRCLE('',#21032,0.400000000000009);
#561=CIRCLE('',#21033,5.72);
#562=CIRCLE('',#21041,4.072);
#563=CIRCLE('',#21042,2.848);
#564=CIRCLE('',#21043,2.9);
#565=CIRCLE('',#21045,5.72);
#566=CIRCLE('',#21046,0.4);
#567=CIRCLE('',#21047,6.12);
#568=CIRCLE('',#21048,6.12);
#569=CIRCLE('',#21050,4.072);
#570=CIRCLE('',#21052,6.12);
#571=CIRCLE('',#21054,0.4);
#572=CIRCLE('',#21065,5.72);
#573=CIRCLE('',#21067,4.072);
#574=CIRCLE('',#21068,2.9);
#575=CIRCLE('',#21069,2.848);
#576=CIRCLE('',#21071,5.72);
#577=CIRCLE('',#21072,0.4);
#578=CIRCLE('',#21073,6.12);
#579=CIRCLE('',#21074,6.12);
#580=CIRCLE('',#21076,4.072);
#581=CIRCLE('',#21078,6.12);
#582=CIRCLE('',#21080,0.4);
#583=CIRCLE('',#21081,3.672);
#584=CIRCLE('',#21082,3.672);
#585=CIRCLE('',#21084,3.672);
#586=CIRCLE('',#21085,3.672);
#587=CIRCLE('',#21087,0.4);
#588=CIRCLE('',#21089,0.4);
#589=CIRCLE('',#21090,3.672);
#590=CIRCLE('',#21091,3.672);
#591=CIRCLE('',#21093,3.672);
#592=CIRCLE('',#21094,3.672);
#593=CIRCLE('',#21096,0.4);
#594=CIRCLE('',#21098,0.4);
#595=CIRCLE('',#21099,2.448);
#596=CIRCLE('',#21100,2.448);
#597=CIRCLE('',#21102,2.448);
#598=CIRCLE('',#21103,2.448);
#599=CIRCLE('',#21105,2.848);
#600=CIRCLE('',#21106,0.4);
#601=CIRCLE('',#21108,2.9);
#602=CIRCLE('',#21110,0.4);
#603=CIRCLE('',#21111,2.5);
#604=CIRCLE('',#21112,2.5);
#605=CIRCLE('',#21114,2.5);
#606=CIRCLE('',#21115,2.5);
#607=CIRCLE('',#21117,2.9);
#608=CIRCLE('',#21118,0.4);
#609=CIRCLE('',#21120,2.848);
#610=CIRCLE('',#21122,0.4);
#611=CIRCLE('',#21123,2.5);
#612=CIRCLE('',#21124,2.5);
#613=CIRCLE('',#21126,2.5);
#614=CIRCLE('',#21127,2.5);
#615=CIRCLE('',#21129,0.4);
#616=CIRCLE('',#21131,0.4);
#617=CIRCLE('',#21132,2.448);
#618=CIRCLE('',#21133,2.448);
#619=CIRCLE('',#21135,2.448);
#620=CIRCLE('',#21136,2.448);
#621=CIRCLE('',#21138,0.4);
#622=CIRCLE('',#21140,1.7);
#623=CIRCLE('',#21141,0.4);
#624=CIRCLE('',#21142,1.3);
#625=CIRCLE('',#21143,1.3);
#626=CIRCLE('',#21145,1.3);
#627=CIRCLE('',#21146,1.3);
#628=CIRCLE('',#21148,1.7);
#629=CIRCLE('',#21160,1.7);
#630=CIRCLE('',#21161,0.4);
#631=CIRCLE('',#21163,1.7);
#632=CIRCLE('',#21172,0.4);
#633=CIRCLE('',#21173,1.3);
#634=CIRCLE('',#21174,1.3);
#635=CIRCLE('',#21176,1.3);
#636=CIRCLE('',#21177,1.3);
#637=CIRCLE('',#21179,0.4);
#638=CIRCLE('',#21191,0.4);
#639=CIRCLE('',#21196,0.4);
#640=CIRCLE('',#21209,0.4);
#641=CIRCLE('',#21214,0.4);
#642=CIRCLE('',#21217,0.4);
#643=CIRCLE('',#21218,0.4);
#644=CIRCLE('',#21219,0.4);
#645=CIRCLE('',#21221,0.4);
#646=CIRCLE('',#21222,0.4);
#647=CIRCLE('',#21224,0.4);
#648=CIRCLE('',#21225,0.4);
#649=CIRCLE('',#21228,0.4);
#650=CIRCLE('',#21229,0.4);
#651=CIRCLE('',#21231,0.4);
#652=CIRCLE('',#21237,0.4);
#653=CIRCLE('',#21238,0.4);
#654=CIRCLE('',#21239,0.4);
#655=CIRCLE('',#21241,0.4);
#656=CIRCLE('',#21242,0.4);
#657=CIRCLE('',#21244,0.4);
#658=CIRCLE('',#21245,0.4);
#659=CIRCLE('',#21248,0.4);
#660=CIRCLE('',#21249,0.4);
#661=CIRCLE('',#21251,0.4);
#662=CIRCLE('',#21263,0.800000000000001);
#663=CIRCLE('',#21264,0.800000000000001);
#664=CIRCLE('',#21265,0.800000000000001);
#665=CIRCLE('',#21267,0.800000000000001);
#666=CIRCLE('',#21268,0.8);
#667=CIRCLE('',#21269,0.800000000000001);
#668=CIRCLE('',#21271,0.800000000000001);
#669=CIRCLE('',#21273,0.8);
#670=CIRCLE('',#21276,0.800000000000001);
#671=CIRCLE('',#21277,0.800000000000001);
#672=CIRCLE('',#21278,0.800000000000001);
#673=CIRCLE('',#21280,0.800000000000001);
#674=CIRCLE('',#21286,0.800000000000001);
#675=CIRCLE('',#21287,0.800000000000001);
#676=CIRCLE('',#21288,0.800000000000001);
#677=CIRCLE('',#21291,0.800000000000001);
#678=CIRCLE('',#21293,0.800000000000001);
#679=CIRCLE('',#21294,0.800000000000003);
#680=CIRCLE('',#21295,0.800000000000001);
#681=CIRCLE('',#21299,0.800000000000001);
#682=CIRCLE('',#21300,0.800000000000001);
#683=CIRCLE('',#21301,0.800000000000001);
#684=CIRCLE('',#21303,0.8);
#685=CIRCLE('',#21304,0.800000000000001);
#686=CIRCLE('',#21305,0.800000000000001);
#687=CIRCLE('',#21307,0.8);
#688=CIRCLE('',#21309,0.800000000000001);
#689=CIRCLE('',#21310,0.800000000000001);
#690=CIRCLE('',#21311,0.800000000000001);
#691=CIRCLE('',#21316,0.799999999999998);
#692=CIRCLE('',#21317,0.799999999999997);
#693=CIRCLE('',#21318,0.799999999999999);
#694=CIRCLE('',#21322,0.800000000000001);
#695=CIRCLE('',#21324,0.799999999999999);
#696=CIRCLE('',#21325,0.800000000000001);
#697=CIRCLE('',#21328,0.800000000000001);
#698=CIRCLE('',#21331,0.799999999999999);
#699=CIRCLE('',#21332,12.24);
#700=CIRCLE('',#21333,12.24);
#701=CIRCLE('',#21335,0.800000000000001);
#702=CIRCLE('',#21338,2.1);
#703=CIRCLE('',#21339,2.1);
#704=CIRCLE('',#21350,5.7528);
#705=CIRCLE('',#21351,0.8);
#706=CIRCLE('',#21352,6.3648);
#707=CIRCLE('',#21354,5.7528);
#708=CIRCLE('',#21356,11.44);
#709=CIRCLE('',#21357,0.8);
#710=CIRCLE('',#21358,12.24);
#711=CIRCLE('',#21360,11.3943409947345);
#712=CIRCLE('',#21362,12.24);
#713=CIRCLE('',#21363,12.24);
#714=CIRCLE('',#21364,12.24);
#715=CIRCLE('',#21365,12.24);
#716=CIRCLE('',#21366,12.24);
#717=CIRCLE('',#21367,12.24);
#718=CIRCLE('',#21369,10.608);
#719=CIRCLE('',#21370,0.8);
#720=CIRCLE('',#21372,0.8);
#721=CIRCLE('',#21373,1.3);
#722=CIRCLE('',#21374,1.3);
#723=CIRCLE('',#21376,1.3);
#724=CIRCLE('',#21378,0.8);
#725=CIRCLE('',#21379,1.3);
#726=CIRCLE('',#21380,1.3);
#727=CIRCLE('',#21382,1.3);
#728=CIRCLE('',#21389,12.648);
#729=CIRCLE('',#21391,12.648);
#730=CIRCLE('',#21399,0.6528);
#731=CIRCLE('',#21400,0.8);
#732=CIRCLE('',#21401,1.13703729720046);
#733=CIRCLE('',#21403,1.13703729720046);
#734=CIRCLE('',#21405,0.6528);
#735=CIRCLE('',#21406,0.8);
#736=CIRCLE('',#21408,0.6528);
#737=CIRCLE('',#21409,0.8);
#738=CIRCLE('',#21410,1.13703729720046);
#739=CIRCLE('',#21412,1.13703729720046);
#740=CIRCLE('',#21414,0.6528);
#741=CIRCLE('',#21415,0.8);
#742=CIRCLE('',#21417,8.16);
#743=CIRCLE('',#21418,0.8);
#744=CIRCLE('',#21419,7.0176);
#745=CIRCLE('',#21429,3.975);
#746=CIRCLE('',#21431,3.975);
#747=CIRCLE('',#21432,4.175);
#748=CIRCLE('',#21439,5.712);
#749=CIRCLE('',#21440,5.3856);
#750=CIRCLE('',#21441,5.712);
#751=CIRCLE('',#21443,5.712);
#752=CIRCLE('',#21444,5.712);
#753=CIRCLE('',#21446,2.448);
#754=CIRCLE('',#21448,5.2224);
#755=CIRCLE('',#21450,4.488);
#756=CIRCLE('',#21451,4.488);
#757=CIRCLE('',#21452,4.488);
#758=CIRCLE('',#21453,4.488);
#759=CIRCLE('',#21454,4.488);
#760=CIRCLE('',#21455,4.488);
#761=CIRCLE('',#21456,4.488);
#762=CIRCLE('',#21457,4.488);
#763=CIRCLE('',#21458,4.488);
#764=CIRCLE('',#21459,4.488);
#765=CIRCLE('',#21460,4.488);
#766=CIRCLE('',#21461,4.488);
#767=CIRCLE('',#21462,4.488);
#768=CIRCLE('',#21463,4.488);
#769=CIRCLE('',#21468,4.488);
#770=CIRCLE('',#21473,4.488);
#771=CIRCLE('',#21478,4.488);
#772=CIRCLE('',#21483,4.488);
#773=CIRCLE('',#21488,4.488);
#774=CIRCLE('',#21493,4.488);
#775=CIRCLE('',#21498,4.488);
#776=CIRCLE('',#21503,4.488);
#777=CIRCLE('',#21508,4.488);
#778=CIRCLE('',#21513,4.488);
#779=CIRCLE('',#21518,4.488);
#780=CIRCLE('',#21523,4.488);
#781=CIRCLE('',#21528,4.488);
#782=CIRCLE('',#21533,4.488);
#783=CIRCLE('',#21534,2.448);
#784=CIRCLE('',#21539,3.22275);
#785=CIRCLE('',#21579,3.933);
#786=CIRCLE('',#21580,3.933);
#787=CIRCLE('',#21582,3.22275);
#788=CIRCLE('',#21584,1.02);
#789=CIRCLE('',#21585,1.02);
#790=CIRCLE('',#21588,3.933);
#791=CIRCLE('',#21589,3.933);
#792=CIRCLE('',#21591,3.933);
#793=CIRCLE('',#21592,3.933);
#794=CIRCLE('',#21594,3.3472);
#795=CIRCLE('',#21597,3.);
#796=CIRCLE('',#21599,3.);
#797=CIRCLE('',#21601,3.95);
#798=CIRCLE('',#21603,3.95);
#799=CIRCLE('',#21605,2.448);
#800=CIRCLE('',#21607,2.448);
#801=CIRCLE('',#21609,2.04);
#802=CIRCLE('',#21613,10.608);
#803=CIRCLE('',#21614,10.008);
#804=CIRCLE('',#21617,10.608);
#805=CIRCLE('',#21618,10.008);
#806=CIRCLE('',#21621,10.008);
#807=CIRCLE('',#21622,10.608);
#808=CIRCLE('',#21625,10.608);
#809=CIRCLE('',#21626,10.008);
#810=CIRCLE('',#21629,10.608);
#811=CIRCLE('',#21630,10.008);
#812=CIRCLE('',#21633,0.6);
#813=CIRCLE('',#21634,0.6);
#814=CIRCLE('',#21638,0.6);
#815=CIRCLE('',#21640,0.6);
#816=CIRCLE('',#21641,0.6);
#817=CIRCLE('',#21642,8.376);
#818=CIRCLE('',#21643,0.6);
#819=CIRCLE('',#21644,0.6);
#820=CIRCLE('',#21646,0.6);
#821=CIRCLE('',#21649,0.6);
#822=CIRCLE('',#21662,1.25);
#823=CIRCLE('',#21664,1.25);
#824=CIRCLE('',#21665,1.25);
#825=CIRCLE('',#21668,0.599999999999999);
#826=CIRCLE('',#21669,0.600000000000001);
#827=CIRCLE('',#21672,0.599999999999999);
#828=CIRCLE('',#21673,0.600000000000001);
#829=CIRCLE('',#21677,0.599999999999999);
#830=CIRCLE('',#21679,0.600000000000001);
#831=CIRCLE('',#21681,0.600000000000001);
#832=CIRCLE('',#21682,0.600000000000001);
#833=CIRCLE('',#21684,0.600000000000001);
#834=CIRCLE('',#21686,0.599999999999999);
#835=CIRCLE('',#21688,0.599999999999999);
#836=CIRCLE('',#21694,0.600000000000001);
#837=CIRCLE('',#21696,0.6);
#838=CIRCLE('',#21698,0.600000000000001);
#839=CIRCLE('',#21699,0.600000000000001);
#840=CIRCLE('',#21700,8.976);
#841=CIRCLE('',#21702,0.6);
#842=CIRCLE('',#21705,0.6);
#843=CIRCLE('',#21707,10.008);
#844=CIRCLE('',#21708,10.608);
#845=CIRCLE('',#21711,10.608);
#846=CIRCLE('',#21712,10.608);
#847=CIRCLE('',#21713,10.608);
#848=CIRCLE('',#21714,10.608);
#849=CIRCLE('',#21716,4.65);
#850=CIRCLE('',#21718,0.6);
#851=CIRCLE('',#21719,4.05);
#852=CIRCLE('',#21720,4.05);
#853=CIRCLE('',#21723,8.976);
#854=CIRCLE('',#21724,8.976);
#855=CIRCLE('',#21726,1.09801213496934);
#856=CIRCLE('',#21727,0.6);
#857=CIRCLE('',#21728,1.632);
#858=CIRCLE('',#21731,0.6);
#859=CIRCLE('',#21733,0.600000000000001);
#860=CIRCLE('',#21734,0.599999999999999);
#861=CIRCLE('',#21736,0.600000000000001);
#862=CIRCLE('',#21737,0.599999999999999);
#863=CIRCLE('',#21739,0.599999999999999);
#864=CIRCLE('',#21741,0.600000000000003);
#865=CIRCLE('',#21743,0.599999999999998);
#866=CIRCLE('',#21745,0.6);
#867=CIRCLE('',#21755,0.600000000000003);
#868=CIRCLE('',#21757,1.25);
#869=CIRCLE('',#21758,1.25);
#870=CIRCLE('',#21759,1.25);
#871=CIRCLE('',#21760,1.25);
#872=CIRCLE('',#21764,1.5);
#873=CIRCLE('',#21765,1.5);
#874=CIRCLE('',#21766,1.5);
#875=CIRCLE('',#21768,0.600000000000001);
#876=CIRCLE('',#21769,0.599999999999998);
#877=CIRCLE('',#21771,0.600000000000001);
#878=CIRCLE('',#21774,0.599999999999999);
#879=CIRCLE('',#21776,0.600000000000001);
#880=CIRCLE('',#21779,0.599999999999999);
#881=CIRCLE('',#21782,0.6);
#882=CIRCLE('',#21783,1.85);
#883=CIRCLE('',#21784,1.85);
#884=CIRCLE('',#21785,2.1);
#885=CIRCLE('',#21787,1.85);
#886=CIRCLE('',#21788,0.6);
#887=CIRCLE('',#21789,1.25);
#888=CIRCLE('',#21790,1.25);
#889=CIRCLE('',#21791,1.85);
#890=CIRCLE('',#21794,0.599999999999999);
#891=CIRCLE('',#21796,1.25);
#892=CIRCLE('',#21798,2.1);
#893=CIRCLE('',#21799,0.6);
#894=CIRCLE('',#21800,1.5);
#895=CIRCLE('',#21801,1.5);
#896=CIRCLE('',#21803,1.5);
#897=CIRCLE('',#21806,0.6);
#898=CIRCLE('',#21808,0.6);
#899=CIRCLE('',#21810,0.599999999999999);
#900=CIRCLE('',#21813,0.6);
#901=CIRCLE('',#21821,0.599999999999999);
#902=CIRCLE('',#21823,0.600000000000001);
#903=CIRCLE('',#21824,0.599999999999999);
#904=CIRCLE('',#21827,0.600000000000001);
#905=CIRCLE('',#21830,2.57398786503066);
#906=CIRCLE('',#21831,2.57398786503066);
#907=CIRCLE('',#21832,0.6);
#908=CIRCLE('',#21833,1.0896);
#909=CIRCLE('',#21834,1.2528);
#910=CIRCLE('',#21835,1.2528);
#911=CIRCLE('',#21840,1.85);
#912=CIRCLE('',#21841,0.6);
#913=CIRCLE('',#21842,1.85);
#914=CIRCLE('',#21857,0.599999999999999);
#915=CIRCLE('',#21862,0.600000000000001);
#916=CIRCLE('',#21864,0.600000000000001);
#917=CIRCLE('',#21865,0.6);
#918=CIRCLE('',#21873,2.1);
#919=CIRCLE('',#21874,0.6);
#920=CIRCLE('',#21875,1.5);
#921=CIRCLE('',#21877,1.5);
#922=CIRCLE('',#21878,1.5);
#923=CIRCLE('',#21880,1.85);
#924=CIRCLE('',#21881,1.85);
#925=CIRCLE('',#21883,0.6);
#926=CIRCLE('',#21884,1.25);
#927=CIRCLE('',#21886,0.600000000000001);
#928=CIRCLE('',#21889,1.25);
#929=CIRCLE('',#21890,1.25);
#930=CIRCLE('',#21892,2.1);
#931=CIRCLE('',#21898,0.6);
#932=CIRCLE('',#21901,0.6);
#933=CIRCLE('',#21908,0.6);
#934=CIRCLE('',#21914,5.712);
#935=CIRCLE('',#21919,5.712);
#936=CIRCLE('',#21924,5.712);
#937=CIRCLE('',#21929,5.712);
#938=CIRCLE('',#21931,0.6);
#939=CIRCLE('',#21932,0.4896);
#940=CIRCLE('',#21933,0.4896);
#941=CIRCLE('',#21943,0.6);
#942=CIRCLE('',#21944,0.6528);
#943=CIRCLE('',#21945,0.6528);
#944=CIRCLE('',#21947,0.6528);
#945=CIRCLE('',#21949,0.6);
#946=CIRCLE('',#21950,0.6528);
#947=CIRCLE('',#21951,0.6528);
#948=CIRCLE('',#21953,0.6528);
#949=CIRCLE('',#21955,0.4896);
#950=CIRCLE('',#21957,2.04);
#951=CIRCLE('',#21958,0.6);
#952=CIRCLE('',#21960,1.85);
#953=CIRCLE('',#21961,0.6);
#954=CIRCLE('',#21962,1.85);
#955=CIRCLE('',#21964,0.599999999999999);
#956=CIRCLE('',#21966,2.1);
#957=CIRCLE('',#21967,0.6);
#958=CIRCLE('',#21970,0.600000000000001);
#959=CIRCLE('',#21971,0.599999999999999);
#960=CIRCLE('',#21973,0.600000000000001);
#961=CIRCLE('',#21976,0.599999999999999);
#962=CIRCLE('',#21978,0.600000000000001);
#963=CIRCLE('',#21980,0.600000000000001);
#964=CIRCLE('',#21983,0.599999999999999);
#965=CIRCLE('',#21985,0.6);
#966=CIRCLE('',#21987,0.6);
#967=CIRCLE('',#21989,0.6);
#968=CIRCLE('',#21991,0.600000000000001);
#969=CIRCLE('',#21993,0.600000000000001);
#970=CIRCLE('',#21994,0.600000000000001);
#971=CIRCLE('',#21996,0.600000000000001);
#972=CIRCLE('',#21998,0.599999999999999);
#973=CIRCLE('',#22000,0.599999999999999);
#974=CIRCLE('',#22003,0.600000000000001);
#975=CIRCLE('',#22006,0.600000000000001);
#976=CIRCLE('',#22010,1.85);
#977=CIRCLE('',#22011,0.6);
#978=CIRCLE('',#22012,1.25);
#979=CIRCLE('',#22013,1.25);
#980=CIRCLE('',#22015,1.25);
#981=CIRCLE('',#22016,1.25);
#982=CIRCLE('',#22017,1.25);
#983=CIRCLE('',#22018,1.25);
#984=CIRCLE('',#22019,1.25);
#985=CIRCLE('',#22021,0.6);
#986=CIRCLE('',#22022,2.1);
#987=CIRCLE('',#22030,0.600000000000001);
#988=CIRCLE('',#22039,0.599999999999999);
#989=CIRCLE('',#22040,0.6);
#990=CIRCLE('',#22048,1.5);
#991=CIRCLE('',#22049,0.6);
#992=CIRCLE('',#22065,0.600000000000005);
#993=CIRCLE('',#22072,0.600000000000001);
#994=CIRCLE('',#22074,0.600000000000001);
#995=CIRCLE('',#22075,0.600000000000001);
#996=CIRCLE('',#22077,0.600000000000003);
#997=CIRCLE('',#22081,0.6);
#998=CIRCLE('',#22086,0.6);
#999=CIRCLE('',#22088,2.1);
#1000=CIRCLE('',#22093,0.600000000000001);
#1001=CIRCLE('',#22105,0.6);
#1002=CIRCLE('',#22106,1.5);
#1003=CIRCLE('',#22107,1.5);
#1004=CIRCLE('',#22109,1.5);
#1005=CIRCLE('',#22110,1.5);
#1006=CIRCLE('',#22113,2.1);
#1007=CIRCLE('',#22159,4.6248);
#1008=CIRCLE('',#22160,0.3);
#1009=CIRCLE('',#22161,4.3248);
#1010=CIRCLE('',#22162,4.3248);
#1011=CIRCLE('',#22164,4.3248);
#1012=CIRCLE('',#22165,4.3248);
#1013=CIRCLE('',#22167,11.532);
#1014=CIRCLE('',#22169,0.3);
#1015=CIRCLE('',#22170,4.6248);
#1016=CIRCLE('',#22172,10.404);
#1017=CIRCLE('',#22174,10.404);
#1018=CIRCLE('',#22175,0.3);
#1019=CIRCLE('',#22176,10.704);
#1020=CIRCLE('',#22177,10.404);
#1021=CIRCLE('',#22179,10.92);
#1022=CIRCLE('',#22182,0.3);
#1023=CIRCLE('',#22183,11.22);
#1024=CIRCLE('',#22184,11.22);
#1025=CIRCLE('',#22186,11.22);
#1026=CIRCLE('',#22187,11.22);
#1027=CIRCLE('',#22188,11.22);
#1028=CIRCLE('',#22190,11.532);
#1029=CIRCLE('',#22191,0.3);
#1030=CIRCLE('',#22192,11.832);
#1031=CIRCLE('',#22193,11.832);
#1032=CIRCLE('',#22195,11.832);
#1033=CIRCLE('',#22196,11.832);
#1034=CIRCLE('',#22199,0.3);
#1035=CIRCLE('',#22220,0.3);
#1036=CIRCLE('',#22221,0.300000000000002);
#1037=CIRCLE('',#22223,0.300000000000011);
#1038=CIRCLE('',#22224,0.3);
#1039=CIRCLE('',#22226,0.3);
#1040=CIRCLE('',#22227,0.300000000000002);
#1041=CIRCLE('',#22229,0.300000000000002);
#1042=CIRCLE('',#22230,0.3);
#1043=CIRCLE('',#22232,0.3);
#1044=CIRCLE('',#22234,0.3);
#1045=CIRCLE('',#22236,0.3);
#1046=CIRCLE('',#22238,0.3);
#1047=CIRCLE('',#22240,0.3);
#1048=CIRCLE('',#22243,0.3);
#1049=CIRCLE('',#22245,1.6);
#1050=CIRCLE('',#22246,1.6);
#1051=CIRCLE('',#22249,0.3);
#1052=CIRCLE('',#22251,0.3);
#1053=CIRCLE('',#22252,0.299999999999996);
#1054=CIRCLE('',#22254,0.299999999999999);
#1055=CIRCLE('',#22256,0.3);
#1056=CIRCLE('',#22258,0.3);
#1057=CIRCLE('',#22259,0.3);
#1058=CIRCLE('',#22260,10.3590843121497);
#1059=CIRCLE('',#22261,0.3);
#1060=CIRCLE('',#22263,1.6);
#1061=CIRCLE('',#22264,1.6);
#1062=CIRCLE('',#22266,0.3);
#1063=CIRCLE('',#22267,0.299999999999998);
#1064=CIRCLE('',#22269,0.3);
#1065=CIRCLE('',#22271,0.3);
#1066=CIRCLE('',#22272,0.3);
#1067=CIRCLE('',#22273,10.3590843136505);
#1068=CIRCLE('',#22274,0.3);
#1069=CIRCLE('',#22275,0.300000000000002);
#1070=CIRCLE('',#22276,0.300000000000001);
#1071=CIRCLE('',#22277,0.3);
#1072=CIRCLE('',#22279,0.3);
#1073=CIRCLE('',#22281,0.3);
#1074=CIRCLE('',#22282,7.0176);
#1075=CIRCLE('',#22283,6.7176);
#1076=CIRCLE('',#22285,0.3);
#1077=CIRCLE('',#22286,0.300000000000001);
#1078=CIRCLE('',#22287,0.299999999999999);
#1079=CIRCLE('',#22289,1.224);
#1080=CIRCLE('',#22292,7.0176);
#1081=CIRCLE('',#22295,1.224);
#1082=CIRCLE('',#22297,0.3);
#1083=CIRCLE('',#22298,0.299999999999999);
#1084=CIRCLE('',#22299,0.3);
#1085=CIRCLE('',#22301,0.299999999999999);
#1086=CIRCLE('',#22302,0.3);
#1087=CIRCLE('',#22303,0.3);
#1088=CIRCLE('',#22306,2.35);
#1089=CIRCLE('',#22307,2.35);
#1090=CIRCLE('',#22309,0.3);
#1091=CIRCLE('',#22310,1.3);
#1092=CIRCLE('',#22311,1.3);
#1093=CIRCLE('',#22313,1.3);
#1094=CIRCLE('',#22314,1.3);
#1095=CIRCLE('',#22316,0.3);
#1096=CIRCLE('',#22318,0.3);
#1097=CIRCLE('',#22319,2.05);
#1098=CIRCLE('',#22320,2.05);
#1099=CIRCLE('',#22322,2.05);
#1100=CIRCLE('',#22323,2.05);
#1101=CIRCLE('',#22325,2.35);
#1102=CIRCLE('',#22326,0.3);
#1103=CIRCLE('',#22328,2.35);
#1104=CIRCLE('',#22330,0.3);
#1105=CIRCLE('',#22331,1.3);
#1106=CIRCLE('',#22332,1.3);
#1107=CIRCLE('',#22334,1.3);
#1108=CIRCLE('',#22335,1.3);
#1109=CIRCLE('',#22337,0.3);
#1110=CIRCLE('',#22339,0.3);
#1111=CIRCLE('',#22340,2.05);
#1112=CIRCLE('',#22341,2.05);
#1113=CIRCLE('',#22343,2.05);
#1114=CIRCLE('',#22344,2.05);
#1115=CIRCLE('',#22346,0.3);
#1116=CIRCLE('',#22353,2.8556);
#1117=CIRCLE('',#22354,1.55);
#1118=CIRCLE('',#22356,2.8556);
#1119=CIRCLE('',#22358,5.3856);
#1120=CIRCLE('',#22359,5.3856);
#1121=CIRCLE('',#22361,3.2636);
#1122=CIRCLE('',#22363,3.2636);
#1123=CIRCLE('',#22366,2.8556);
#1124=CIRCLE('',#22367,2.8556);
#1125=CIRCLE('',#22369,1.55);
#1126=CIRCLE('',#22371,3.2636);
#1127=CIRCLE('',#22372,3.2636);
#1128=CIRCLE('',#22374,5.3856);
#1129=CIRCLE('',#22376,5.3856);
#1130=CIRCLE('',#22378,6.0384);
#1131=CIRCLE('',#22380,6.528);
#1132=CIRCLE('',#22381,6.2424);
#1133=CIRCLE('',#22383,6.2424);
#1134=CIRCLE('',#22385,6.528);
#1135=CIRCLE('',#22387,6.528);
#1136=CIRCLE('',#22389,6.2424);
#1137=CIRCLE('',#22391,6.2424);
#1138=CIRCLE('',#22393,6.528);
#1139=CIRCLE('',#22395,6.528);
#1140=CIRCLE('',#22397,6.0384);
#1141=CIRCLE('',#22399,6.528);
#1142=CIRCLE('',#22406,2.448);
#1143=CIRCLE('',#22407,2.2032);
#1144=CIRCLE('',#22409,2.448);
#1145=CIRCLE('',#22411,2.2032);
#1146=CIRCLE('',#22413,1.3);
#1147=CIRCLE('',#22415,1.3);
#1148=CIRCLE('',#22419,1.5);
#1149=CIRCLE('',#22420,1.1736);
#1150=CIRCLE('',#22422,1.5);
#1151=CIRCLE('',#22424,1.1736);
#1152=CIRCLE('',#22429,1.25);
#1153=CIRCLE('',#22430,0.9236);
#1154=CIRCLE('',#22432,1.25);
#1155=CIRCLE('',#22434,0.9236);
#1156=CIRCLE('',#22439,2.1216);
#1157=CIRCLE('',#22441,2.448);
#1158=CIRCLE('',#22443,2.448);
#1159=CIRCLE('',#22445,4.488);
#1160=CIRCLE('',#22447,4.488);
#1161=CIRCLE('',#22449,4.08);
#1162=CIRCLE('',#22451,3.264);
#1163=CIRCLE('',#22453,3.264);
#1164=CIRCLE('',#22455,2.9376);
#1165=CIRCLE('',#22457,2.9376);
#1166=CIRCLE('',#22459,3.264);
#1167=CIRCLE('',#22461,3.264);
#1168=CIRCLE('',#22463,2.6112);
#1169=CIRCLE('',#22467,2.5);
#1170=CIRCLE('',#22468,2.0104);
#1171=CIRCLE('',#22470,2.5);
#1172=CIRCLE('',#22472,2.0104);
#1173=CIRCLE('',#22477,3.5);
#1174=CIRCLE('',#22479,2.);
#1175=CIRCLE('',#22481,2.);
#1176=CIRCLE('',#22483,3.2);
#1177=CIRCLE('',#22485,3.2);
#1178=CIRCLE('',#22487,2.8736);
#1179=CIRCLE('',#22491,2.2);
#1180=CIRCLE('',#22493,1.25);
#1181=CIRCLE('',#22495,1.25);
#1182=CIRCLE('',#22497,1.0052);
#1183=TOROIDAL_SURFACE('',#20344,4.272,0.6);
#1184=TOROIDAL_SURFACE('',#20367,2.232,0.6);
#1185=TOROIDAL_SURFACE('',#20381,2.232,0.6);
#1186=TOROIDAL_SURFACE('',#20406,2.232,0.6);
#1187=TOROIDAL_SURFACE('',#20420,2.232,0.6);
#1188=TOROIDAL_SURFACE('',#20439,3.1,0.6);
#1189=TOROIDAL_SURFACE('',#20462,4.272,0.6);
#1190=TOROIDAL_SURFACE('',#20469,4.272,0.6);
#1191=TOROIDAL_SURFACE('',#20474,3.456,0.6);
#1192=TOROIDAL_SURFACE('',#20479,3.456,0.6);
#1193=TOROIDAL_SURFACE('',#20486,2.232,0.6);
#1194=TOROIDAL_SURFACE('',#20498,2.232,0.6);
#1195=TOROIDAL_SURFACE('',#20563,2.232,0.6);
#1196=TOROIDAL_SURFACE('',#20571,2.232,0.6);
#1197=TOROIDAL_SURFACE('',#20575,2.232,0.6);
#1198=TOROIDAL_SURFACE('',#20581,2.232,0.6);
#1199=TOROIDAL_SURFACE('',#20584,2.232,0.6);
#1200=TOROIDAL_SURFACE('',#20596,3.1,0.6);
#1201=TOROIDAL_SURFACE('',#20677,3.1,0.6);
#1202=TOROIDAL_SURFACE('',#20725,2.232,0.6);
#1203=TOROIDAL_SURFACE('',#20741,2.232,0.6);
#1204=TOROIDAL_SURFACE('',#20746,2.232,0.6);
#1205=TOROIDAL_SURFACE('',#20752,2.232,0.6);
#1206=TOROIDAL_SURFACE('',#20773,8.1888,0.6);
#1207=TOROIDAL_SURFACE('',#20856,8.1888,0.6);
#1208=TOROIDAL_SURFACE('',#20862,2.232,0.6);
#1209=TOROIDAL_SURFACE('',#20867,3.1,0.6);
#1210=TOROIDAL_SURFACE('',#20872,3.456,0.6);
#1211=TOROIDAL_SURFACE('',#20877,3.456,0.6);
#1212=TOROIDAL_SURFACE('',#20879,4.73652813742386,0.6);
#1213=TOROIDAL_SURFACE('',#20881,4.73652813742386,0.6);
#1214=TOROIDAL_SURFACE('',#20888,4.272,0.6);
#1215=TOROIDAL_SURFACE('',#20976,5.72,0.4);
#1216=TOROIDAL_SURFACE('',#21013,5.72,0.4);
#1217=TOROIDAL_SURFACE('',#21031,5.72,0.4);
#1218=TOROIDAL_SURFACE('',#21044,5.72,0.4);
#1219=TOROIDAL_SURFACE('',#21064,5.72,0.4);
#1220=TOROIDAL_SURFACE('',#21070,5.72,0.4);
#1221=TOROIDAL_SURFACE('',#21079,4.072,0.4);
#1222=TOROIDAL_SURFACE('',#21086,4.072,0.4);
#1223=TOROIDAL_SURFACE('',#21088,4.072,0.4);
#1224=TOROIDAL_SURFACE('',#21095,4.072,0.4);
#1225=TOROIDAL_SURFACE('',#21097,2.848,0.4);
#1226=TOROIDAL_SURFACE('',#21104,2.848,0.4);
#1227=TOROIDAL_SURFACE('',#21109,2.9,0.4);
#1228=TOROIDAL_SURFACE('',#21116,2.9,0.4);
#1229=TOROIDAL_SURFACE('',#21121,2.9,0.4);
#1230=TOROIDAL_SURFACE('',#21128,2.9,0.4);
#1231=TOROIDAL_SURFACE('',#21130,2.848,0.4);
#1232=TOROIDAL_SURFACE('',#21137,2.848,0.4);
#1233=TOROIDAL_SURFACE('',#21139,1.7,0.4);
#1234=TOROIDAL_SURFACE('',#21159,1.7,0.4);
#1235=TOROIDAL_SURFACE('',#21171,1.7,0.4);
#1236=TOROIDAL_SURFACE('',#21178,1.7,0.4);
#1237=TOROIDAL_SURFACE('',#21349,6.5528,0.8);
#1238=TOROIDAL_SURFACE('',#21355,11.44,0.8);
#1239=TOROIDAL_SURFACE('',#21368,11.3943409947345,0.8);
#1240=TOROIDAL_SURFACE('',#21371,2.1,0.8);
#1241=TOROIDAL_SURFACE('',#21377,2.1,0.8);
#1242=TOROIDAL_SURFACE('',#21388,11.8802820935674,0.8);
#1243=TOROIDAL_SURFACE('',#21390,11.8802820935674,0.8);
#1244=TOROIDAL_SURFACE('',#21398,1.13703729720046,0.8);
#1245=TOROIDAL_SURFACE('',#21404,1.13703729720046,0.8);
#1246=TOROIDAL_SURFACE('',#21407,1.13703729720046,0.8);
#1247=TOROIDAL_SURFACE('',#21413,1.13703729720046,0.8);
#1248=TOROIDAL_SURFACE('',#21416,7.4416006562771,0.8);
#1249=TOROIDAL_SURFACE('',#21612,10.008,0.6);
#1250=TOROIDAL_SURFACE('',#21616,10.008,0.6);
#1251=TOROIDAL_SURFACE('',#21620,10.008,0.6);
#1252=TOROIDAL_SURFACE('',#21624,10.008,0.6);
#1253=TOROIDAL_SURFACE('',#21628,10.008,0.6);
#1254=TOROIDAL_SURFACE('',#21697,8.376,0.6);
#1255=TOROIDAL_SURFACE('',#21706,10.008,0.6);
#1256=TOROIDAL_SURFACE('',#21717,4.65,0.6);
#1257=TOROIDAL_SURFACE('',#21725,1.09801213496934,0.6);
#1258=TOROIDAL_SURFACE('',#21786,1.85,0.6);
#1259=TOROIDAL_SURFACE('',#21797,2.1,0.6);
#1260=TOROIDAL_SURFACE('',#21805,2.1,0.6);
#1261=TOROIDAL_SURFACE('',#21807,1.85,0.6);
#1262=TOROIDAL_SURFACE('',#21839,1.85,0.6);
#1263=TOROIDAL_SURFACE('',#21872,2.1,0.6);
#1264=TOROIDAL_SURFACE('',#21882,1.85,0.6);
#1265=TOROIDAL_SURFACE('',#21930,1.0896,0.6);
#1266=TOROIDAL_SURFACE('',#21942,1.2528,0.6);
#1267=TOROIDAL_SURFACE('',#21948,1.2528,0.6);
#1268=TOROIDAL_SURFACE('',#21956,2.57398786503066,0.6);
#1269=TOROIDAL_SURFACE('',#21959,1.85,0.6);
#1270=TOROIDAL_SURFACE('',#21965,2.1,0.6);
#1271=TOROIDAL_SURFACE('',#22009,1.85,0.6);
#1272=TOROIDAL_SURFACE('',#22085,2.1,0.6);
#1273=TOROIDAL_SURFACE('',#22087,2.1,0.6);
#1274=TOROIDAL_SURFACE('',#22104,2.1,0.6);
#1275=TOROIDAL_SURFACE('',#22112,2.1,0.6);
#1276=TOROIDAL_SURFACE('',#22158,4.6248,0.3);
#1277=TOROIDAL_SURFACE('',#22168,4.6248,0.3);
#1278=TOROIDAL_SURFACE('',#22173,10.704,0.3);
#1279=TOROIDAL_SURFACE('',#22181,10.92,0.3);
#1280=TOROIDAL_SURFACE('',#22189,11.532,0.3);
#1281=TOROIDAL_SURFACE('',#22198,11.532,0.3);
#1282=TOROIDAL_SURFACE('',#22280,6.7176,0.3);
#1283=TOROIDAL_SURFACE('',#22308,1.6,0.3);
#1284=TOROIDAL_SURFACE('',#22315,1.6,0.3);
#1285=TOROIDAL_SURFACE('',#22317,2.35,0.3);
#1286=TOROIDAL_SURFACE('',#22324,2.35,0.3);
#1287=TOROIDAL_SURFACE('',#22329,1.6,0.3);
#1288=TOROIDAL_SURFACE('',#22336,1.6,0.3);
#1289=TOROIDAL_SURFACE('',#22338,2.35,0.3);
#1290=TOROIDAL_SURFACE('',#22345,2.35,0.3);
#1291=SHAPE_REPRESENTATION_RELATIONSHIP('SRR','None',#100101,#1309);
#1292=SHAPE_REPRESENTATION_RELATIONSHIP('SRR','None',#100102,#1310);
#1293=SHAPE_REPRESENTATION_RELATIONSHIP('SRR','None',#100103,#1311);
#1294=SHAPE_REPRESENTATION_RELATIONSHIP('SRR','None',#100104,#1312);
#1295=SHAPE_REPRESENTATION_RELATIONSHIP('SRR','None',#100105,#1313);
#1296=SHAPE_REPRESENTATION_RELATIONSHIP('SRR','None',#100106,#1314);
#1297=SHAPE_REPRESENTATION_RELATIONSHIP('SRR','None',#100107,#1315);
#1298=SHAPE_REPRESENTATION_RELATIONSHIP('SRR','None',#100108,#1316);
#1299=SHAPE_REPRESENTATION_RELATIONSHIP('SRR','None',#100109,#1317);
#1300=SHAPE_REPRESENTATION_RELATIONSHIP('SRR','None',#100110,#1318);
#1301=SHAPE_REPRESENTATION_RELATIONSHIP('SRR','None',#100111,#1319);
#1302=SHAPE_REPRESENTATION_RELATIONSHIP('SRR','None',#100112,#1320);
#1303=SHAPE_REPRESENTATION_RELATIONSHIP('SRR','None',#100113,#1321);
#1304=SHAPE_REPRESENTATION_RELATIONSHIP('SRR','None',#100114,#1322);
#1305=SHAPE_REPRESENTATION_RELATIONSHIP('SRR','None',#100115,#1323);
#1306=SHAPE_REPRESENTATION_RELATIONSHIP('SRR','None',#100116,#1324);
#1307=SHAPE_REPRESENTATION_RELATIONSHIP('SRR','None',#100117,#1325);
#1308=SHAPE_REPRESENTATION_RELATIONSHIP('SRR','None',#100118,#1326);
#1309=ADVANCED_BREP_SHAPE_REPRESENTATION('',(#1345),#100013);
#1310=ADVANCED_BREP_SHAPE_REPRESENTATION('',(#1346),#100014);
#1311=ADVANCED_BREP_SHAPE_REPRESENTATION('',(#1347),#100015);
#1312=ADVANCED_BREP_SHAPE_REPRESENTATION('',(#1348),#100016);
#1313=ADVANCED_BREP_SHAPE_REPRESENTATION('',(#1349),#100017);
#1314=ADVANCED_BREP_SHAPE_REPRESENTATION('',(#1350),#100018);
#1315=ADVANCED_BREP_SHAPE_REPRESENTATION('',(#1351),#100019);
#1316=ADVANCED_BREP_SHAPE_REPRESENTATION('',(#1352),#100020);
#1317=ADVANCED_BREP_SHAPE_REPRESENTATION('',(#1353),#100021);
#1318=ADVANCED_BREP_SHAPE_REPRESENTATION('',(#1354),#100022);
#1319=ADVANCED_BREP_SHAPE_REPRESENTATION('',(#1355),#100023);
#1320=ADVANCED_BREP_SHAPE_REPRESENTATION('',(#1356),#100024);
#1321=ADVANCED_BREP_SHAPE_REPRESENTATION('',(#1357),#100025);
#1322=ADVANCED_BREP_SHAPE_REPRESENTATION('',(#1358),#100026);
#1323=ADVANCED_BREP_SHAPE_REPRESENTATION('',(#1359),#100027);
#1324=ADVANCED_BREP_SHAPE_REPRESENTATION('',(#1360),#100028);
#1325=ADVANCED_BREP_SHAPE_REPRESENTATION('',(#1361),#100029);
#1326=ADVANCED_BREP_SHAPE_REPRESENTATION('',(#1362),#100030);
#1327=STYLED_ITEM('',(#100200),#1345);
#1328=STYLED_ITEM('',(#100201),#1346);
#1329=STYLED_ITEM('',(#100201),#1347);
#1330=STYLED_ITEM('',(#100201),#1348);
#1331=STYLED_ITEM('',(#100200),#1349);
#1332=STYLED_ITEM('',(#100200),#1350);
#1333=STYLED_ITEM('',(#100202),#1351);
#1334=STYLED_ITEM('',(#100203),#1352);
#1335=STYLED_ITEM('',(#100203),#1353);
#1336=STYLED_ITEM('',(#100200),#1354);
#1337=STYLED_ITEM('',(#100200),#1355);
#1338=STYLED_ITEM('',(#100200),#1356);
#1339=STYLED_ITEM('',(#100203),#1357);
#1340=STYLED_ITEM('',(#100203),#1358);
#1341=STYLED_ITEM('',(#100200),#1359);
#1342=STYLED_ITEM('',(#100204),#1360);
#1343=STYLED_ITEM('',(#100204),#1361);
#1344=STYLED_ITEM('',(#100204),#1362);
#1345=MANIFOLD_SOLID_BREP('Body1',#20117);
#1346=MANIFOLD_SOLID_BREP('Body1',#20118);
#1347=MANIFOLD_SOLID_BREP('Body1',#20119);
#1348=MANIFOLD_SOLID_BREP('Body1',#20120);
#1349=MANIFOLD_SOLID_BREP('Body1',#20121);
#1350=MANIFOLD_SOLID_BREP('Body1',#20122);
#1351=MANIFOLD_SOLID_BREP('Body1',#20123);
#1352=MANIFOLD_SOLID_BREP('Body1',#20124);
#1353=MANIFOLD_SOLID_BREP('Body1',#20125);
#1354=MANIFOLD_SOLID_BREP('Body1',#20126);
#1355=MANIFOLD_SOLID_BREP('Body1',#20127);
#1356=MANIFOLD_SOLID_BREP('Body1',#20128);
#1357=MANIFOLD_SOLID_BREP('Body1',#20129);
#1358=MANIFOLD_SOLID_BREP('Body1',#20130);
#1359=MANIFOLD_SOLID_BREP('Body1',#20131);
#1360=MANIFOLD_SOLID_BREP('Body1',#20132);
#1361=MANIFOLD_SOLID_BREP('Body1',#20133);
#1362=MANIFOLD_SOLID_BREP('Body1',#20134);
#1363=PLANE('',#20342);
#1364=PLANE('',#20385);
#1365=PLANE('',#20410);
#1366=PLANE('',#20426);
#1367=PLANE('',#20444);
#1368=PLANE('',#20483);
#1369=PLANE('',#20495);
#1370=PLANE('',#20548);
#1371=PLANE('',#20549);
#1372=PLANE('',#20553);
#1373=PLANE('',#20590);
#1374=PLANE('',#20662);
#1375=PLANE('',#20665);
#1376=PLANE('',#20669);
#1377=PLANE('',#20670);
#1378=PLANE('',#20671);
#1379=PLANE('',#20676);
#1380=PLANE('',#20680);
#1381=PLANE('',#20700);
#1382=PLANE('',#20709);
#1383=PLANE('',#20710);
#1384=PLANE('',#20711);
#1385=PLANE('',#20765);
#1386=PLANE('',#20838);
#1387=PLANE('',#20839);
#1388=PLANE('',#20843);
#1389=PLANE('',#20844);
#1390=PLANE('',#20845);
#1391=PLANE('',#20848);
#1392=PLANE('',#20850);
#1393=PLANE('',#20852);
#1394=PLANE('',#20858);
#1395=PLANE('',#20860);
#1396=PLANE('',#20866);
#1397=PLANE('',#20890);
#1398=PLANE('',#20891);
#1399=PLANE('',#20901);
#1400=PLANE('',#20902);
#1401=PLANE('',#20903);
#1402=PLANE('',#20915);
#1403=PLANE('',#20916);
#1404=PLANE('',#20922);
#1405=PLANE('',#20932);
#1406=PLANE('',#20933);
#1407=PLANE('',#20934);
#1408=PLANE('',#20942);
#1409=PLANE('',#20957);
#1410=PLANE('',#20980);
#1411=PLANE('',#20981);
#1412=PLANE('',#20982);
#1413=PLANE('',#20985);
#1414=PLANE('',#20986);
#1415=PLANE('',#21009);
#1416=PLANE('',#21010);
#1417=PLANE('',#21023);
#1418=PLANE('',#21026);
#1419=PLANE('',#21027);
#1420=PLANE('',#21028);
#1421=PLANE('',#21040);
#1422=PLANE('',#21049);
#1423=PLANE('',#21066);
#1424=PLANE('',#21075);
#1425=PLANE('',#21107);
#1426=PLANE('',#21119);
#1427=PLANE('',#21147);
#1428=PLANE('',#21155);
#1429=PLANE('',#21156);
#1430=PLANE('',#21157);
#1431=PLANE('',#21162);
#1432=PLANE('',#21188);
#1433=PLANE('',#21189);
#1434=PLANE('',#21197);
#1435=PLANE('',#21206);
#1436=PLANE('',#21207);
#1437=PLANE('',#21215);
#1438=PLANE('',#21223);
#1439=PLANE('',#21226);
#1440=PLANE('',#21227);
#1441=PLANE('',#21232);
#1442=PLANE('',#21233);
#1443=PLANE('',#21234);
#1444=PLANE('',#21243);
#1445=PLANE('',#21246);
#1446=PLANE('',#21247);
#1447=PLANE('',#21252);
#1448=PLANE('',#21253);
#1449=PLANE('',#21254);
#1450=PLANE('',#21256);
#1451=PLANE('',#21257);
#1452=PLANE('',#21258);
#1453=PLANE('',#21259);
#1454=PLANE('',#21260);
#1455=PLANE('',#21336);
#1456=PLANE('',#21337);
#1457=PLANE('',#21340);
#1458=PLANE('',#21342);
#1459=PLANE('',#21343);
#1460=PLANE('',#21348);
#1461=PLANE('',#21359);
#1462=PLANE('',#21392);
#1463=PLANE('',#21402);
#1464=PLANE('',#21411);
#1465=PLANE('',#21420);
#1466=PLANE('',#21421);
#1467=PLANE('',#21422);
#1468=PLANE('',#21423);
#1469=PLANE('',#21424);
#1470=PLANE('',#21425);
#1471=PLANE('',#21426);
#1472=PLANE('',#21427);
#1473=PLANE('',#21428);
#1474=PLANE('',#21434);
#1475=PLANE('',#21435);
#1476=PLANE('',#21436);
#1477=PLANE('',#21445);
#1478=PLANE('',#21449);
#1479=PLANE('',#21464);
#1480=PLANE('',#21465);
#1481=PLANE('',#21466);
#1482=PLANE('',#21469);
#1483=PLANE('',#21470);
#1484=PLANE('',#21471);
#1485=PLANE('',#21474);
#1486=PLANE('',#21475);
#1487=PLANE('',#21476);
#1488=PLANE('',#21479);
#1489=PLANE('',#21480);
#1490=PLANE('',#21481);
#1491=PLANE('',#21484);
#1492=PLANE('',#21485);
#1493=PLANE('',#21486);
#1494=PLANE('',#21489);
#1495=PLANE('',#21490);
#1496=PLANE('',#21491);
#1497=PLANE('',#21494);
#1498=PLANE('',#21495);
#1499=PLANE('',#21496);
#1500=PLANE('',#21499);
#1501=PLANE('',#21500);
#1502=PLANE('',#21501);
#1503=PLANE('',#21504);
#1504=PLANE('',#21505);
#1505=PLANE('',#21506);
#1506=PLANE('',#21509);
#1507=PLANE('',#21510);
#1508=PLANE('',#21511);
#1509=PLANE('',#21514);
#1510=PLANE('',#21515);
#1511=PLANE('',#21516);
#1512=PLANE('',#21519);
#1513=PLANE('',#21520);
#1514=PLANE('',#21521);
#1515=PLANE('',#21524);
#1516=PLANE('',#21525);
#1517=PLANE('',#21526);
#1518=PLANE('',#21529);
#1519=PLANE('',#21530);
#1520=PLANE('',#21531);
#1521=PLANE('',#21532);
#1522=PLANE('',#21586);
#1523=PLANE('',#21587);
#1524=PLANE('',#21590);
#1525=PLANE('',#21593);
#1526=PLANE('',#21600);
#1527=PLANE('',#21604);
#1528=PLANE('',#21610);
#1529=PLANE('',#21615);
#1530=PLANE('',#21619);
#1531=PLANE('',#21627);
#1532=PLANE('',#21631);
#1533=PLANE('',#21635);
#1534=PLANE('',#21639);
#1535=PLANE('',#21658);
#1536=PLANE('',#21659);
#1537=PLANE('',#21661);
#1538=PLANE('',#21663);
#1539=PLANE('',#21666);
#1540=PLANE('',#21689);
#1541=PLANE('',#21692);
#1542=PLANE('',#21695);
#1543=PLANE('',#21704);
#1544=PLANE('',#21715);
#1545=PLANE('',#21729);
#1546=PLANE('',#21752);
#1547=PLANE('',#21781);
#1548=PLANE('',#21804);
#1549=PLANE('',#21814);
#1550=PLANE('',#21816);
#1551=PLANE('',#21819);
#1552=PLANE('',#21829);
#1553=PLANE('',#21845);
#1554=PLANE('',#21848);
#1555=PLANE('',#21851);
#1556=PLANE('',#21855);
#1557=PLANE('',#21869);
#1558=PLANE('',#21879);
#1559=PLANE('',#21891);
#1560=PLANE('',#21894);
#1561=PLANE('',#21899);
#1562=PLANE('',#21903);
#1563=PLANE('',#21906);
#1564=PLANE('',#21909);
#1565=PLANE('',#21913);
#1566=PLANE('',#21918);
#1567=PLANE('',#21923);
#1568=PLANE('',#21928);
#1569=PLANE('',#21935);
#1570=PLANE('',#21937);
#1571=PLANE('',#21939);
#1572=PLANE('',#21941);
#1573=PLANE('',#21968);
#1574=PLANE('',#21986);
#1575=PLANE('',#22001);
#1576=PLANE('',#22020);
#1577=PLANE('',#22024);
#1578=PLANE('',#22028);
#1579=PLANE('',#22029);
#1580=PLANE('',#22031);
#1581=PLANE('',#22045);
#1582=PLANE('',#22046);
#1583=PLANE('',#22047);
#1584=PLANE('',#22060);
#1585=PLANE('',#22061);
#1586=PLANE('',#22066);
#1587=PLANE('',#22084);
#1588=PLANE('',#22089);
#1589=PLANE('',#22090);
#1590=PLANE('',#22091);
#1591=PLANE('',#22092);
#1592=PLANE('',#22095);
#1593=PLANE('',#22098);
#1594=PLANE('',#22100);
#1595=PLANE('',#22102);
#1596=PLANE('',#22103);
#1597=PLANE('',#22111);
#1598=PLANE('',#22114);
#1599=PLANE('',#22115);
#1600=PLANE('',#22116);
#1601=PLANE('',#22117);
#1602=PLANE('',#22118);
#1603=PLANE('',#22119);
#1604=PLANE('',#22120);
#1605=PLANE('',#22121);
#1606=PLANE('',#22122);
#1607=PLANE('',#22123);
#1608=PLANE('',#22124);
#1609=PLANE('',#22125);
#1610=PLANE('',#22126);
#1611=PLANE('',#22127);
#1612=PLANE('',#22128);
#1613=PLANE('',#22129);
#1614=PLANE('',#22130);
#1615=PLANE('',#22131);
#1616=PLANE('',#22132);
#1617=PLANE('',#22133);
#1618=PLANE('',#22134);
#1619=PLANE('',#22135);
#1620=PLANE('',#22136);
#1621=PLANE('',#22137);
#1622=PLANE('',#22138);
#1623=PLANE('',#22139);
#1624=PLANE('',#22142);
#1625=PLANE('',#22143);
#1626=PLANE('',#22144);
#1627=PLANE('',#22145);
#1628=PLANE('',#22146);
#1629=PLANE('',#22147);
#1630=PLANE('',#22148);
#1631=PLANE('',#22149);
#1632=PLANE('',#22150);
#1633=PLANE('',#22151);
#1634=PLANE('',#22153);
#1635=PLANE('',#22154);
#1636=PLANE('',#22155);
#1637=PLANE('',#22156);
#1638=PLANE('',#22166);
#1639=PLANE('',#22171);
#1640=PLANE('',#22178);
#1641=PLANE('',#22197);
#1642=PLANE('',#22208);
#1643=PLANE('',#22209);
#1644=PLANE('',#22210);
#1645=PLANE('',#22211);
#1646=PLANE('',#22212);
#1647=PLANE('',#22213);
#1648=PLANE('',#22214);
#1649=PLANE('',#22215);
#1650=PLANE('',#22216);
#1651=PLANE('',#22217);
#1652=PLANE('',#22241);
#1653=PLANE('',#22244);
#1654=PLANE('',#22247);
#1655=PLANE('',#22262);
#1656=PLANE('',#22288);
#1657=PLANE('',#22293);
#1658=PLANE('',#22296);
#1659=PLANE('',#22305);
#1660=PLANE('',#22327);
#1661=PLANE('',#22347);
#1662=PLANE('',#22350);
#1663=PLANE('',#22352);
#1664=PLANE('',#22360);
#1665=PLANE('',#22364);
#1666=PLANE('',#22368);
#1667=PLANE('',#22373);
#1668=PLANE('',#22377);
#1669=PLANE('',#22379);
#1670=PLANE('',#22384);
#1671=PLANE('',#22388);
#1672=PLANE('',#22392);
#1673=PLANE('',#22401);
#1674=PLANE('',#22403);
#1675=PLANE('',#22412);
#1676=PLANE('',#22416);
#1677=PLANE('',#22425);
#1678=PLANE('',#22426);
#1679=PLANE('',#22435);
#1680=PLANE('',#22436);
#1681=PLANE('',#22438);
#1682=PLANE('',#22444);
#1683=PLANE('',#22450);
#1684=PLANE('',#22454);
#1685=PLANE('',#22458);
#1686=PLANE('',#22464);
#1687=PLANE('',#22473);
#1688=PLANE('',#22474);
#1689=PLANE('',#22478);
#1690=PLANE('',#22482);
#1691=PLANE('',#22488);
#1692=PLANE('',#22492);
#1693=PLANE('',#22498);
#1694=FACE_BOUND('',#6186,.T.);
#1695=FACE_BOUND('',#6187,.T.);
#1696=FACE_BOUND('',#6188,.T.);
#1697=FACE_BOUND('',#6189,.T.);
#1698=FACE_BOUND('',#6190,.T.);
#1699=FACE_BOUND('',#6193,.T.);
#1700=FACE_BOUND('',#6194,.T.);
#1701=FACE_BOUND('',#6195,.T.);
#1702=FACE_BOUND('',#6196,.T.);
#1703=FACE_BOUND('',#6316,.T.);
#1704=FACE_BOUND('',#6317,.T.);
#1705=FACE_BOUND('',#6318,.T.);
#1706=FACE_BOUND('',#6319,.T.);
#1707=FACE_BOUND('',#6320,.T.);
#1708=FACE_BOUND('',#6321,.T.);
#1709=FACE_BOUND('',#6322,.T.);
#1710=FACE_BOUND('',#6424,.T.);
#1711=FACE_BOUND('',#6425,.T.);
#1712=FACE_BOUND('',#6426,.T.);
#1713=FACE_BOUND('',#6427,.T.);
#1714=FACE_BOUND('',#6428,.T.);
#1715=FACE_BOUND('',#6429,.T.);
#1716=FACE_BOUND('',#6430,.T.);
#1717=FACE_BOUND('',#6546,.T.);
#1718=FACE_BOUND('',#6554,.T.);
#1719=FACE_BOUND('',#6565,.T.);
#1720=FACE_BOUND('',#6604,.T.);
#1721=FACE_BOUND('',#6623,.T.);
#1722=FACE_BOUND('',#6624,.T.);
#1723=FACE_BOUND('',#6625,.T.);
#1724=FACE_BOUND('',#6628,.T.);
#1725=FACE_BOUND('',#6638,.T.);
#1726=FACE_BOUND('',#6639,.T.);
#1727=FACE_BOUND('',#6640,.T.);
#1728=FACE_BOUND('',#6643,.T.);
#1729=FACE_BOUND('',#6655,.T.);
#1730=FACE_BOUND('',#6656,.T.);
#1731=FACE_BOUND('',#6657,.T.);
#1732=FACE_BOUND('',#6662,.T.);
#1733=FACE_BOUND('',#6663,.T.);
#1734=FACE_BOUND('',#6664,.T.);
#1735=FACE_BOUND('',#6674,.T.);
#1736=FACE_BOUND('',#6675,.T.);
#1737=FACE_BOUND('',#6676,.T.);
#1738=FACE_BOUND('',#6677,.T.);
#1739=FACE_BOUND('',#6687,.T.);
#1740=FACE_BOUND('',#6688,.T.);
#1741=FACE_BOUND('',#6689,.T.);
#1742=FACE_BOUND('',#6690,.T.);
#1743=FACE_BOUND('',#6778,.T.);
#1744=FACE_BOUND('',#6779,.T.);
#1745=FACE_BOUND('',#6792,.T.);
#1746=FACE_BOUND('',#6810,.T.);
#1747=FACE_BOUND('',#6811,.T.);
#1748=FACE_BOUND('',#6815,.T.);
#1749=FACE_BOUND('',#6816,.T.);
#1750=FACE_BOUND('',#6820,.T.);
#1751=FACE_BOUND('',#6828,.T.);
#1752=FACE_BOUND('',#6830,.T.);
#1753=FACE_BOUND('',#6834,.T.);
#1754=FACE_BOUND('',#6840,.T.);
#1755=FACE_BOUND('',#6843,.T.);
#1756=FACE_BOUND('',#6900,.T.);
#1757=FACE_BOUND('',#6951,.T.);
#1758=FACE_BOUND('',#6956,.T.);
#1759=FACE_BOUND('',#6959,.T.);
#1760=FACE_BOUND('',#7006,.T.);
#1761=FACE_BOUND('',#7011,.T.);
#1762=FACE_BOUND('',#7036,.T.);
#1763=FACE_BOUND('',#7043,.T.);
#1764=FACE_BOUND('',#7059,.T.);
#1765=FACE_BOUND('',#7060,.T.);
#1766=FACE_BOUND('',#7061,.T.);
#1767=FACE_BOUND('',#7062,.T.);
#1768=FACE_BOUND('',#7086,.T.);
#1769=FACE_BOUND('',#7091,.T.);
#1770=FACE_BOUND('',#7130,.T.);
#1771=FACE_BOUND('',#7154,.T.);
#1772=FACE_BOUND('',#7155,.T.);
#1773=FACE_BOUND('',#7226,.T.);
#1774=FACE_BOUND('',#7247,.T.);
#1775=FACE_BOUND('',#7248,.T.);
#1776=FACE_BOUND('',#7253,.T.);
#1777=FACE_BOUND('',#7256,.T.);
#1778=FACE_BOUND('',#7259,.T.);
#1779=FACE_BOUND('',#7263,.T.);
#1780=FACE_BOUND('',#7267,.T.);
#1781=FACE_BOUND('',#7276,.T.);
#1782=FACE_BOUND('',#7296,.T.);
#1783=FACE_BOUND('',#7297,.T.);
#1784=FACE_BOUND('',#7308,.T.);
#1785=FACE_BOUND('',#7309,.T.);
#1786=FACE_BOUND('',#7342,.T.);
#1787=FACE_BOUND('',#7343,.T.);
#1788=FACE_BOUND('',#7351,.T.);
#1789=FACE_BOUND('',#7352,.T.);
#1790=FACE_BOUND('',#7364,.T.);
#1791=FACE_BOUND('',#7368,.T.);
#1792=FACE_BOUND('',#7371,.T.);
#1793=FACE_BOUND('',#7374,.T.);
#1794=FACE_BOUND('',#7377,.T.);
#1795=FACE_BOUND('',#7380,.T.);
#1796=FACE_BOUND('',#7382,.T.);
#1797=FACE_BOUND('',#7385,.T.);
#1798=FACE_BOUND('',#7388,.T.);
#1799=FACE_BOUND('',#7391,.T.);
#1800=FACE_BOUND('',#7397,.T.);
#1801=FACE_BOUND('',#7400,.T.);
#1802=FACE_BOUND('',#7405,.T.);
#1803=FACE_BOUND('',#7408,.T.);
#1804=FACE_BOUND('',#7423,.T.);
#1805=FACE_BOUND('',#7427,.T.);
#1806=FACE_BOUND('',#7430,.T.);
#1807=FACE_BOUND('',#7433,.T.);
#1808=FACE_BOUND('',#7444,.T.);
#1809=FACE_BOUND('',#7447,.T.);
#1810=FACE_BOUND('',#7453,.T.);
#1811=ELLIPSE('',#20337,11.3271425811526,8.17324773003453);
#1812=ELLIPSE('',#20338,11.1453149409752,7.84400958474998);
#1813=ELLIPSE('',#20502,0.649435320175436,0.6);
#1814=ELLIPSE('',#20624,0.848528137423857,0.6);
#1815=ELLIPSE('',#20626,0.848528137423857,0.6);
#1816=ELLIPSE('',#20668,0.848528137423857,0.6);
#1817=ELLIPSE('',#20673,0.848528137423857,0.6);
#1818=ELLIPSE('',#20675,0.649435320175435,0.6);
#1819=ELLIPSE('',#20778,0.649435320175437,0.6);
#1820=ELLIPSE('',#20785,0.848528137423857,0.6);
#1821=ELLIPSE('',#20787,0.848528137423857,0.6);
#1822=ELLIPSE('',#20837,0.649435320175436,0.6);
#1823=ELLIPSE('',#20842,0.848528137423857,0.6);
#1824=ELLIPSE('',#20847,0.848528137423857,0.6);
#1825=ELLIPSE('',#20894,0.565685424949238,0.4);
#1826=ELLIPSE('',#20895,0.565685424949238,0.4);
#1827=ELLIPSE('',#20897,0.565685424949238,0.4);
#1828=ELLIPSE('',#20899,0.565685424949238,0.4);
#1829=ELLIPSE('',#20904,0.565685424949239,0.4);
#1830=ELLIPSE('',#20906,0.406004087997522,0.4);
#1831=ELLIPSE('',#20908,0.565685424949238,0.4);
#1832=ELLIPSE('',#20909,0.565685424949238,0.4);
#1833=ELLIPSE('',#20911,0.565685424949238,0.4);
#1834=ELLIPSE('',#20912,0.565685424949238,0.4);
#1835=ELLIPSE('',#20918,0.522676873082012,0.4);
#1836=ELLIPSE('',#20919,0.406004087997522,0.4);
#1837=ELLIPSE('',#20921,0.406004087997522,0.4);
#1838=ELLIPSE('',#20923,0.574176487625014,0.4);
#1839=ELLIPSE('',#20925,0.565685424949238,0.4);
#1840=ELLIPSE('',#20926,0.565685424949238,0.4);
#1841=ELLIPSE('',#20928,0.565685424949238,0.4);
#1842=ELLIPSE('',#20930,0.565685424949238,0.4);
#1843=ELLIPSE('',#20935,0.565685424949239,0.4);
#1844=ELLIPSE('',#20941,0.565685424949238,0.4);
#1845=ELLIPSE('',#20944,0.405232582893276,0.4);
#1846=ELLIPSE('',#20946,0.565685424949238,0.4);
#1847=ELLIPSE('',#20948,0.56568542494924,0.4);
#1848=ELLIPSE('',#20949,0.405232582893277,0.4);
#1849=ELLIPSE('',#20956,0.405232582893276,0.4);
#1850=ELLIPSE('',#20959,0.565685424949238,0.4);
#1851=ELLIPSE('',#20961,0.404631208637699,0.4);
#1852=ELLIPSE('',#20963,0.41193011418047,0.4);
#1853=ELLIPSE('',#20966,0.405232582893276,0.4);
#1854=ELLIPSE('',#20968,0.405232582893276,0.4);
#1855=ELLIPSE('',#20974,0.565685424949237,0.4);
#1856=ELLIPSE('',#20989,0.43295688011696,0.4);
#1857=ELLIPSE('',#20991,0.565685424949238,0.4);
#1858=ELLIPSE('',#20997,0.405232582893276,0.4);
#1859=ELLIPSE('',#20999,0.522676873082012,0.4);
#1860=ELLIPSE('',#21000,0.406004087997522,0.4);
#1861=ELLIPSE('',#21002,0.565685424949238,0.4);
#1862=ELLIPSE('',#21003,0.565685424949238,0.4);
#1863=ELLIPSE('',#21005,0.565685424949238,0.4);
#1864=ELLIPSE('',#21006,0.565685424949238,0.4);
#1865=ELLIPSE('',#21017,0.41193011418047,0.4);
#1866=ELLIPSE('',#21019,0.404631208637698,0.4);
#1867=ELLIPSE('',#21021,0.56568542494924,0.4);
#1868=ELLIPSE('',#21030,0.405232582893276,0.4);
#1869=ELLIPSE('',#21036,0.411930114180469,0.4);
#1870=ELLIPSE('',#21038,0.404631208637699,0.4);
#1871=ELLIPSE('',#21055,0.405232582893276,0.4);
#1872=ELLIPSE('',#21058,0.565685424949238,0.4);
#1873=ELLIPSE('',#21060,0.404631208637698,0.4);
#1874=ELLIPSE('',#21062,0.411930114180471,0.4);
#1875=ELLIPSE('',#21150,0.574176487625014,0.4);
#1876=ELLIPSE('',#21151,0.432956880116957,0.4);
#1877=ELLIPSE('',#21153,0.432956880116958,0.4);
#1878=ELLIPSE('',#21165,0.432956880116959,0.4);
#1879=ELLIPSE('',#21166,0.432956880116958,0.4);
#1880=ELLIPSE('',#21169,0.432956880116958,0.4);
#1881=ELLIPSE('',#21181,0.565685424949238,0.4);
#1882=ELLIPSE('',#21182,0.565685424949238,0.4);
#1883=ELLIPSE('',#21184,0.565685424949238,0.4);
#1884=ELLIPSE('',#21186,0.565685424949238,0.4);
#1885=ELLIPSE('',#21192,0.565685424949238,0.4);
#1886=ELLIPSE('',#21194,0.565685424949238,0.4);
#1887=ELLIPSE('',#21199,0.565685424949238,0.4);
#1888=ELLIPSE('',#21200,0.565685424949238,0.4);
#1889=ELLIPSE('',#21202,0.565685424949238,0.4);
#1890=ELLIPSE('',#21204,0.565685424949238,0.4);
#1891=ELLIPSE('',#21210,0.565685424949238,0.4);
#1892=ELLIPSE('',#21212,0.565685424949238,0.4);
#1893=ELLIPSE('',#21282,1.13137084989848,0.8);
#1894=ELLIPSE('',#21284,1.13137084989848,0.8);
#1895=ELLIPSE('',#21314,1.13137084989848,0.8);
#1896=ELLIPSE('',#21346,1.13137084989848,0.8);
#1897=ELLIPSE('',#21384,1.13137084989848,0.800000000000001);
#1898=ELLIPSE('',#21385,1.13137084989848,0.800000000000001);
#1899=ELLIPSE('',#21394,1.13137084989848,0.8);
#1900=ELLIPSE('',#21396,1.13137084989848,0.799999999999998);
#1901=ELLIPSE('',#21637,0.848528137423856,0.6);
#1902=ELLIPSE('',#21647,0.848528137423857,0.6);
#1903=ELLIPSE('',#21651,1.29110397126991,0.6);
#1904=ELLIPSE('',#21652,2.01675243255473,0.6);
#1905=ELLIPSE('',#21653,1.29110397126991,0.6);
#1906=ELLIPSE('',#21654,2.01675243255473,0.6);
#1907=ELLIPSE('',#21655,1.05620174691084,0.6);
#1908=ELLIPSE('',#21656,1.05620174691084,0.6);
#1909=ELLIPSE('',#21657,0.641695030633084,0.6);
#1910=ELLIPSE('',#21660,0.641695030633085,0.600000000000001);
#1911=ELLIPSE('',#21670,0.628456956755705,0.6);
#1912=ELLIPSE('',#21675,0.677615091396383,0.6);
#1913=ELLIPSE('',#21676,0.677615091396385,0.6);
#1914=ELLIPSE('',#21691,0.848528137423857,0.6);
#1915=ELLIPSE('',#21747,1.29110397126991,0.6);
#1916=ELLIPSE('',#21749,1.2911039712699,0.6);
#1917=ELLIPSE('',#21751,0.641695030633084,0.6);
#1918=ELLIPSE('',#21754,0.848528137423857,0.6);
#1919=ELLIPSE('',#21762,0.72905961291191,0.600000000000001);
#1920=ELLIPSE('',#21772,0.848528137423857,0.6);
#1921=ELLIPSE('',#21777,0.848528137423857,0.6);
#1922=ELLIPSE('',#21793,0.848528137423857,0.6);
#1923=ELLIPSE('',#21811,0.848528137423857,0.6);
#1924=ELLIPSE('',#21818,0.848528137423857,0.6);
#1925=ELLIPSE('',#21837,0.848528137423857,0.6);
#1926=ELLIPSE('',#21844,0.84852813742386,0.6);
#1927=ELLIPSE('',#21847,0.729059612911909,0.6);
#1928=ELLIPSE('',#21850,1.05620174691084,0.6);
#1929=ELLIPSE('',#21853,0.848528137423857,0.6);
#1930=ELLIPSE('',#21854,0.677615091396383,0.6);
#1931=ELLIPSE('',#21859,2.01675243255473,0.6);
#1932=ELLIPSE('',#21868,0.848528137423857,0.6);
#1933=ELLIPSE('',#21871,0.848528137423857,0.6);
#1934=ELLIPSE('',#21887,0.848528137423857,0.6);
#1935=ELLIPSE('',#21896,0.848528137423856,0.6);
#1936=ELLIPSE('',#21902,0.848528137423857,0.6);
#1937=ELLIPSE('',#21905,0.848528137423857,0.6);
#1938=ELLIPSE('',#21911,0.848528137423857,0.6);
#1939=ELLIPSE('',#21912,0.848528137423857,0.6);
#1940=ELLIPSE('',#21916,0.848528137423857,0.6);
#1941=ELLIPSE('',#21917,0.848528137423857,0.6);
#1942=ELLIPSE('',#21921,0.848528137423857,0.6);
#1943=ELLIPSE('',#21922,0.848528137423857,0.6);
#1944=ELLIPSE('',#21926,0.848528137423857,0.6);
#1945=ELLIPSE('',#21927,0.848528137423857,0.6);
#1946=ELLIPSE('',#21981,0.848528137423857,0.6);
#1947=ELLIPSE('',#22007,0.848528137423857,0.6);
#1948=ELLIPSE('',#22026,2.01675243255473,0.6);
#1949=ELLIPSE('',#22027,1.2911039712699,0.6);
#1950=ELLIPSE('',#22033,0.848528137423857,0.6);
#1951=ELLIPSE('',#22034,0.848528137423856,0.6);
#1952=ELLIPSE('',#22035,1.29110397126991,0.6);
#1953=ELLIPSE('',#22036,1.2911039712699,0.6);
#1954=ELLIPSE('',#22038,2.01675243255473,0.6);
#1955=ELLIPSE('',#22041,0.848528137423857,0.6);
#1956=ELLIPSE('',#22042,2.01675243255472,0.6);
#1957=ELLIPSE('',#22043,1.05620174691084,0.6);
#1958=ELLIPSE('',#22044,1.05620174691084,0.6);
#1959=ELLIPSE('',#22051,0.729059612911909,0.6);
#1960=ELLIPSE('',#22052,1.05620174691084,0.6);
#1961=ELLIPSE('',#22053,0.641695030633084,0.6);
#1962=ELLIPSE('',#22055,0.729059612911907,0.6);
#1963=ELLIPSE('',#22056,1.05620174691084,0.6);
#1964=ELLIPSE('',#22057,0.641695030633084,0.6);
#1965=ELLIPSE('',#22059,1.29110397126991,0.6);
#1966=ELLIPSE('',#22062,0.641695030633084,0.6);
#1967=ELLIPSE('',#22063,1.05620174691084,0.6);
#1968=ELLIPSE('',#22067,0.641695030633084,0.6);
#1969=ELLIPSE('',#22068,1.05620174691084,0.6);
#1970=ELLIPSE('',#22069,1.05620174691084,0.6);
#1971=ELLIPSE('',#22080,0.848528137423857,0.6);
#1972=ELLIPSE('',#22082,2.01675243255473,0.6);
#1973=ELLIPSE('',#22096,1.05620174691084,0.6);
#1974=ELLIPSE('',#22201,0.424264068711929,0.3);
#1975=ELLIPSE('',#22202,0.424264068711929,0.3);
#1976=ELLIPSE('',#22204,0.424264068711929,0.3);
#1977=ELLIPSE('',#22206,0.424264068711929,0.3);
#1978=ELLIPSE('',#22290,2.28040158611643,0.428995210802967);
#1979=ELLIPSE('',#22294,2.23144347816224,0.415540935948683);
#1980=LINE('',#28809,#3267);
#1981=LINE('',#55728,#3268);
#1982=LINE('',#56082,#3269);
#1983=LINE('',#56334,#3270);
#1984=LINE('',#56576,#3271);
#1985=LINE('',#56606,#3272);
#1986=LINE('',#56688,#3273);
#1987=LINE('',#56725,#3274);
#1988=LINE('',#56751,#3275);
#1989=LINE('',#56752,#3276);
#1990=LINE('',#56777,#3277);
#1991=LINE('',#56803,#3278);
#1992=LINE('',#56804,#3279);
#1993=LINE('',#56830,#3280);
#1994=LINE('',#56831,#3281);
#1995=LINE('',#56856,#3282);
#1996=LINE('',#56885,#3283);
#1997=LINE('',#56926,#3284);
#1998=LINE('',#56963,#3285);
#1999=LINE('',#56997,#3286);
#2000=LINE('',#56998,#3287);
#2001=LINE('',#57040,#3288);
#2002=LINE('',#57041,#3289);
#2003=LINE('',#57079,#3290);
#2004=LINE('',#57080,#3291);
#2005=LINE('',#57109,#3292);
#2006=LINE('',#57130,#3293);
#2007=LINE('',#57168,#3294);
#2008=LINE('',#57169,#3295);
#2009=LINE('',#57170,#3296);
#2010=LINE('',#57199,#3297);
#2011=LINE('',#57240,#3298);
#2012=LINE('',#57269,#3299);
#2013=LINE('',#57294,#3300);
#2014=LINE('',#57311,#3301);
#2015=LINE('',#57336,#3302);
#2016=LINE('',#57337,#3303);
#2017=LINE('',#57358,#3304);
#2018=LINE('',#57379,#3305);
#2019=LINE('',#57408,#3306);
#2020=LINE('',#57450,#3307);
#2021=LINE('',#57451,#3308);
#2022=LINE('',#57496,#3309);
#2023=LINE('',#57533,#3310);
#2024=LINE('',#57535,#3311);
#2025=LINE('',#57536,#3312);
#2026=LINE('',#57578,#3313);
#2027=LINE('',#57579,#3314);
#2028=LINE('',#57625,#3315);
#2029=LINE('',#57626,#3316);
#2030=LINE('',#57671,#3317);
#2031=LINE('',#57704,#3318);
#2032=LINE('',#57737,#3319);
#2033=LINE('',#57770,#3320);
#2034=LINE('',#57800,#3321);
#2035=LINE('',#57801,#3322);
#2036=LINE('',#57839,#3323);
#2037=LINE('',#57840,#3324);
#2038=LINE('',#57873,#3325);
#2039=LINE('',#57894,#3326);
#2040=LINE('',#57911,#3327);
#2041=LINE('',#57928,#3328);
#2042=LINE('',#57962,#3329);
#2043=LINE('',#57963,#3330);
#2044=LINE('',#57964,#3331);
#2045=LINE('',#58001,#3332);
#2046=LINE('',#58034,#3333);
#2047=LINE('',#58051,#3334);
#2048=LINE('',#58088,#3335);
#2049=LINE('',#58113,#3336);
#2050=LINE('',#58162,#3337);
#2051=LINE('',#58191,#3338);
#2052=LINE('',#58224,#3339);
#2053=LINE('',#58289,#3340);
#2054=LINE('',#58330,#3341);
#2055=LINE('',#58367,#3342);
#2056=LINE('',#58368,#3343);
#2057=LINE('',#58393,#3344);
#2058=LINE('',#58430,#3345);
#2059=LINE('',#58467,#3346);
#2060=LINE('',#58484,#3347);
#2061=LINE('',#58533,#3348);
#2062=LINE('',#58550,#3349);
#2063=LINE('',#58575,#3350);
#2064=LINE('',#58608,#3351);
#2065=LINE('',#58646,#3352);
#2066=LINE('',#58647,#3353);
#2067=LINE('',#58684,#3354);
#2068=LINE('',#58849,#3355);
#2069=LINE('',#59048,#3356);
#2070=LINE('',#59081,#3357);
#2071=LINE('',#59084,#3358);
#2072=LINE('',#59093,#3359);
#2073=LINE('',#59096,#3360);
#2074=LINE('',#59107,#3361);
#2075=LINE('',#59110,#3362);
#2076=LINE('',#59120,#3363);
#2077=LINE('',#59125,#3364);
#2078=LINE('',#59128,#3365);
#2079=LINE('',#59142,#3366);
#2080=LINE('',#59147,#3367);
#2081=LINE('',#59150,#3368);
#2082=LINE('',#59159,#3369);
#2083=LINE('',#59162,#3370);
#2084=LINE('',#59169,#3371);
#2085=LINE('',#59172,#3372);
#2086=LINE('',#59186,#3373);
#2087=LINE('',#59192,#3374);
#2088=LINE('',#59195,#3375);
#2089=LINE('',#59212,#3376);
#2090=LINE('',#59215,#3377);
#2091=LINE('',#59218,#3378);
#2092=LINE('',#59219,#3379);
#2093=LINE('',#59224,#3380);
#2094=LINE('',#59227,#3381);
#2095=LINE('',#59236,#3382);
#2096=LINE('',#59239,#3383);
#2097=LINE('',#59253,#3384);
#2098=LINE('',#59255,#3385);
#2099=LINE('',#59257,#3386);
#2100=LINE('',#59259,#3387);
#2101=LINE('',#59261,#3388);
#2102=LINE('',#59263,#3389);
#2103=LINE('',#59265,#3390);
#2104=LINE('',#59267,#3391);
#2105=LINE('',#59269,#3392);
#2106=LINE('',#59271,#3393);
#2107=LINE('',#59273,#3394);
#2108=LINE('',#59275,#3395);
#2109=LINE('',#59277,#3396);
#2110=LINE('',#59279,#3397);
#2111=LINE('',#59281,#3398);
#2112=LINE('',#59283,#3399);
#2113=LINE('',#59285,#3400);
#2114=LINE('',#59287,#3401);
#2115=LINE('',#59289,#3402);
#2116=LINE('',#59291,#3403);
#2117=LINE('',#59293,#3404);
#2118=LINE('',#59295,#3405);
#2119=LINE('',#59298,#3406);
#2120=LINE('',#59303,#3407);
#2121=LINE('',#59307,#3408);
#2122=LINE('',#59310,#3409);
#2123=LINE('',#59314,#3410);
#2124=LINE('',#59318,#3411);
#2125=LINE('',#59321,#3412);
#2126=LINE('',#59329,#3413);
#2127=LINE('',#59331,#3414);
#2128=LINE('',#59333,#3415);
#2129=LINE('',#59336,#3416);
#2130=LINE('',#59341,#3417);
#2131=LINE('',#59353,#3418);
#2132=LINE('',#59363,#3419);
#2133=LINE('',#59372,#3420);
#2134=LINE('',#59377,#3421);
#2135=LINE('',#59380,#3422);
#2136=LINE('',#59383,#3423);
#2137=LINE('',#59384,#3424);
#2138=LINE('',#59387,#3425);
#2139=LINE('',#59401,#3426);
#2140=LINE('',#59404,#3427);
#2141=LINE('',#59415,#3428);
#2142=LINE('',#59423,#3429);
#2143=LINE('',#59437,#3430);
#2144=LINE('',#59445,#3431);
#2145=LINE('',#59453,#3432);
#2146=LINE('',#59457,#3433);
#2147=LINE('',#59466,#3434);
#2148=LINE('',#59467,#3435);
#2149=LINE('',#59476,#3436);
#2150=LINE('',#59477,#3437);
#2151=LINE('',#59486,#3438);
#2152=LINE('',#59487,#3439);
#2153=LINE('',#59493,#3440);
#2154=LINE('',#59495,#3441);
#2155=LINE('',#59497,#3442);
#2156=LINE('',#59500,#3443);
#2157=LINE('',#59503,#3444);
#2158=LINE('',#59505,#3445);
#2159=LINE('',#59520,#3446);
#2160=LINE('',#59521,#3447);
#2161=LINE('',#59533,#3448);
#2162=LINE('',#59557,#3449);
#2163=LINE('',#59559,#3450);
#2164=LINE('',#59561,#3451);
#2165=LINE('',#59563,#3452);
#2166=LINE('',#59568,#3453);
#2167=LINE('',#59578,#3454);
#2168=LINE('',#59589,#3455);
#2169=LINE('',#59597,#3456);
#2170=LINE('',#59605,#3457);
#2171=LINE('',#59613,#3458);
#2172=LINE('',#59616,#3459);
#2173=LINE('',#59621,#3460);
#2174=LINE('',#59629,#3461);
#2175=LINE('',#59631,#3462);
#2176=LINE('',#59636,#3463);
#2177=LINE('',#59637,#3464);
#2178=LINE('',#59646,#3465);
#2179=LINE('',#59647,#3466);
#2180=LINE('',#59656,#3467);
#2181=LINE('',#59657,#3468);
#2182=LINE('',#59666,#3469);
#2183=LINE('',#59667,#3470);
#2184=LINE('',#59676,#3471);
#2185=LINE('',#59677,#3472);
#2186=LINE('',#59684,#3473);
#2187=LINE('',#59689,#3474);
#2188=LINE('',#59691,#3475);
#2189=LINE('',#59692,#3476);
#2190=LINE('',#59694,#3477);
#2191=LINE('',#59696,#3478);
#2192=LINE('',#59698,#3479);
#2193=LINE('',#59701,#3480);
#2194=LINE('',#59704,#3481);
#2195=LINE('',#59706,#3482);
#2196=LINE('',#59709,#3483);
#2197=LINE('',#59710,#3484);
#2198=LINE('',#59712,#3485);
#2199=LINE('',#59715,#3486);
#2200=LINE('',#59719,#3487);
#2201=LINE('',#59722,#3488);
#2202=LINE('',#59724,#3489);
#2203=LINE('',#59731,#3490);
#2204=LINE('',#59733,#3491);
#2205=LINE('',#59737,#3492);
#2206=LINE('',#59739,#3493);
#2207=LINE('',#59741,#3494);
#2208=LINE('',#59743,#3495);
#2209=LINE('',#59745,#3496);
#2210=LINE('',#59747,#3497);
#2211=LINE('',#59749,#3498);
#2212=LINE('',#59751,#3499);
#2213=LINE('',#59753,#3500);
#2214=LINE('',#59754,#3501);
#2215=LINE('',#59755,#3502);
#2216=LINE('',#59756,#3503);
#2217=LINE('',#59757,#3504);
#2218=LINE('',#59761,#3505);
#2219=LINE('',#59765,#3506);
#2220=LINE('',#59769,#3507);
#2221=LINE('',#59773,#3508);
#2222=LINE('',#59777,#3509);
#2223=LINE('',#59787,#3510);
#2224=LINE('',#59789,#3511);
#2225=LINE('',#59791,#3512);
#2226=LINE('',#59793,#3513);
#2227=LINE('',#59800,#3514);
#2228=LINE('',#59809,#3515);
#2229=LINE('',#59813,#3516);
#2230=LINE('',#59815,#3517);
#2231=LINE('',#59827,#3518);
#2232=LINE('',#59840,#3519);
#2233=LINE('',#59841,#3520);
#2234=LINE('',#59852,#3521);
#2235=LINE('',#59853,#3522);
#2236=LINE('',#59864,#3523);
#2237=LINE('',#59884,#3524);
#2238=LINE('',#59885,#3525);
#2239=LINE('',#59887,#3526);
#2240=LINE('',#59889,#3527);
#2241=LINE('',#59892,#3528);
#2242=LINE('',#59896,#3529);
#2243=LINE('',#59901,#3530);
#2244=LINE('',#59913,#3531);
#2245=LINE('',#59916,#3532);
#2246=LINE('',#59925,#3533);
#2247=LINE('',#59928,#3534);
#2248=LINE('',#59933,#3535);
#2249=LINE('',#59941,#3536);
#2250=LINE('',#59949,#3537);
#2251=LINE('',#59957,#3538);
#2252=LINE('',#59959,#3539);
#2253=LINE('',#59964,#3540);
#2254=LINE('',#59965,#3541);
#2255=LINE('',#59968,#3542);
#2256=LINE('',#59973,#3543);
#2257=LINE('',#59974,#3544);
#2258=LINE('',#59982,#3545);
#2259=LINE('',#59983,#3546);
#2260=LINE('',#59991,#3547);
#2261=LINE('',#59992,#3548);
#2262=LINE('',#60000,#3549);
#2263=LINE('',#60001,#3550);
#2264=LINE('',#60007,#3551);
#2265=LINE('',#60009,#3552);
#2266=LINE('',#60017,#3553);
#2267=LINE('',#60020,#3554);
#2268=LINE('',#60023,#3555);
#2269=LINE('',#60025,#3556);
#2270=LINE('',#60029,#3557);
#2271=LINE('',#60032,#3558);
#2272=LINE('',#60035,#3559);
#2273=LINE('',#60036,#3560);
#2274=LINE('',#60038,#3561);
#2275=LINE('',#60042,#3562);
#2276=LINE('',#60045,#3563);
#2277=LINE('',#60051,#3564);
#2278=LINE('',#60056,#3565);
#2279=LINE('',#60058,#3566);
#2280=LINE('',#60064,#3567);
#2281=LINE('',#60078,#3568);
#2282=LINE('',#60081,#3569);
#2283=LINE('',#60095,#3570);
#2284=LINE('',#60104,#3571);
#2285=LINE('',#60108,#3572);
#2286=LINE('',#60112,#3573);
#2287=LINE('',#60114,#3574);
#2288=LINE('',#60118,#3575);
#2289=LINE('',#60120,#3576);
#2290=LINE('',#60123,#3577);
#2291=LINE('',#60124,#3578);
#2292=LINE('',#60127,#3579);
#2293=LINE('',#60129,#3580);
#2294=LINE('',#60130,#3581);
#2295=LINE('',#60133,#3582);
#2296=LINE('',#60134,#3583);
#2297=LINE('',#60138,#3584);
#2298=LINE('',#60142,#3585);
#2299=LINE('',#60144,#3586);
#2300=LINE('',#60146,#3587);
#2301=LINE('',#60147,#3588);
#2302=LINE('',#60168,#3589);
#2303=LINE('',#60172,#3590);
#2304=LINE('',#60175,#3591);
#2305=LINE('',#60180,#3592);
#2306=LINE('',#60184,#3593);
#2307=LINE('',#60186,#3594);
#2308=LINE('',#60187,#3595);
#2309=LINE('',#60189,#3596);
#2310=LINE('',#60193,#3597);
#2311=LINE('',#60195,#3598);
#2312=LINE('',#60197,#3599);
#2313=LINE('',#60199,#3600);
#2314=LINE('',#60201,#3601);
#2315=LINE('',#60202,#3602);
#2316=LINE('',#60208,#3603);
#2317=LINE('',#60229,#3604);
#2318=LINE('',#60232,#3605);
#2319=LINE('',#60237,#3606);
#2320=LINE('',#60239,#3607);
#2321=LINE('',#60240,#3608);
#2322=LINE('',#60244,#3609);
#2323=LINE('',#60248,#3610);
#2324=LINE('',#60252,#3611);
#2325=LINE('',#60254,#3612);
#2326=LINE('',#60258,#3613);
#2327=LINE('',#60260,#3614);
#2328=LINE('',#60263,#3615);
#2329=LINE('',#60264,#3616);
#2330=LINE('',#60267,#3617);
#2331=LINE('',#60269,#3618);
#2332=LINE('',#60270,#3619);
#2333=LINE('',#60273,#3620);
#2334=LINE('',#60274,#3621);
#2335=LINE('',#60277,#3622);
#2336=LINE('',#60279,#3623);
#2337=LINE('',#60281,#3624);
#2338=LINE('',#60283,#3625);
#2339=LINE('',#60294,#3626);
#2340=LINE('',#60297,#3627);
#2341=LINE('',#60299,#3628);
#2342=LINE('',#60301,#3629);
#2343=LINE('',#60303,#3630);
#2344=LINE('',#60305,#3631);
#2345=LINE('',#60307,#3632);
#2346=LINE('',#60309,#3633);
#2347=LINE('',#60311,#3634);
#2348=LINE('',#60313,#3635);
#2349=LINE('',#60315,#3636);
#2350=LINE('',#60316,#3637);
#2351=LINE('',#60319,#3638);
#2352=LINE('',#60324,#3639);
#2353=LINE('',#60328,#3640);
#2354=LINE('',#60338,#3641);
#2355=LINE('',#60341,#3642);
#2356=LINE('',#60344,#3643);
#2357=LINE('',#60345,#3644);
#2358=LINE('',#60348,#3645);
#2359=LINE('',#60352,#3646);
#2360=LINE('',#60355,#3647);
#2361=LINE('',#60358,#3648);
#2362=LINE('',#60361,#3649);
#2363=LINE('',#60365,#3650);
#2364=LINE('',#60369,#3651);
#2365=LINE('',#60373,#3652);
#2366=LINE('',#60375,#3653);
#2367=LINE('',#60384,#3654);
#2368=LINE('',#60419,#3655);
#2369=LINE('',#60420,#3656);
#2370=LINE('',#60423,#3657);
#2371=LINE('',#60424,#3658);
#2372=LINE('',#60427,#3659);
#2373=LINE('',#60428,#3660);
#2374=LINE('',#60431,#3661);
#2375=LINE('',#60432,#3662);
#2376=LINE('',#60435,#3663);
#2377=LINE('',#60439,#3664);
#2378=LINE('',#60440,#3665);
#2379=LINE('',#60442,#3666);
#2380=LINE('',#60444,#3667);
#2381=LINE('',#60448,#3668);
#2382=LINE('',#60454,#3669);
#2383=LINE('',#60462,#3670);
#2384=LINE('',#60468,#3671);
#2385=LINE('',#60472,#3672);
#2386=LINE('',#60475,#3673);
#2387=LINE('',#60480,#3674);
#2388=LINE('',#60484,#3675);
#2389=LINE('',#60486,#3676);
#2390=LINE('',#60487,#3677);
#2391=LINE('',#60489,#3678);
#2392=LINE('',#60492,#3679);
#2393=LINE('',#60494,#3680);
#2394=LINE('',#60495,#3681);
#2395=LINE('',#60496,#3682);
#2396=LINE('',#60501,#3683);
#2397=LINE('',#60502,#3684);
#2398=LINE('',#60538,#3685);
#2399=LINE('',#60541,#3686);
#2400=LINE('',#60544,#3687);
#2401=LINE('',#60547,#3688);
#2402=LINE('',#60550,#3689);
#2403=LINE('',#60553,#3690);
#2404=LINE('',#60554,#3691);
#2405=LINE('',#60557,#3692);
#2406=LINE('',#60558,#3693);
#2407=LINE('',#60561,#3694);
#2408=LINE('',#60565,#3695);
#2409=LINE('',#60566,#3696);
#2410=LINE('',#60569,#3697);
#2411=LINE('',#60570,#3698);
#2412=LINE('',#60572,#3699);
#2413=LINE('',#60575,#3700);
#2414=LINE('',#60611,#3701);
#2415=LINE('',#60614,#3702);
#2416=LINE('',#60618,#3703);
#2417=LINE('',#60621,#3704);
#2418=LINE('',#60642,#3705);
#2419=LINE('',#60648,#3706);
#2420=LINE('',#60651,#3707);
#2421=LINE('',#60654,#3708);
#2422=LINE('',#60658,#3709);
#2423=LINE('',#60662,#3710);
#2424=LINE('',#60666,#3711);
#2425=LINE('',#60717,#3712);
#2426=LINE('',#60727,#3713);
#2427=LINE('',#60741,#3714);
#2428=LINE('',#60758,#3715);
#2429=LINE('',#60777,#3716);
#2430=LINE('',#60783,#3717);
#2431=LINE('',#60797,#3718);
#2432=LINE('',#60811,#3719);
#2433=LINE('',#60827,#3720);
#2434=LINE('',#60831,#3721);
#2435=LINE('',#60832,#3722);
#2436=LINE('',#60833,#3723);
#2437=LINE('',#60835,#3724);
#2438=LINE('',#60836,#3725);
#2439=LINE('',#60841,#3726);
#2440=LINE('',#60843,#3727);
#2441=LINE('',#60845,#3728);
#2442=LINE('',#60846,#3729);
#2443=LINE('',#60849,#3730);
#2444=LINE('',#60851,#3731);
#2445=LINE('',#60853,#3732);
#2446=LINE('',#60854,#3733);
#2447=LINE('',#60857,#3734);
#2448=LINE('',#60863,#3735);
#2449=LINE('',#60865,#3736);
#2450=LINE('',#60868,#3737);
#2451=LINE('',#60869,#3738);
#2452=LINE('',#60872,#3739);
#2453=LINE('',#60873,#3740);
#2454=LINE('',#60875,#3741);
#2455=LINE('',#60883,#3742);
#2456=LINE('',#60885,#3743);
#2457=LINE('',#60887,#3744);
#2458=LINE('',#60888,#3745);
#2459=LINE('',#60891,#3746);
#2460=LINE('',#60893,#3747);
#2461=LINE('',#60895,#3748);
#2462=LINE('',#60897,#3749);
#2463=LINE('',#60899,#3750);
#2464=LINE('',#60901,#3751);
#2465=LINE('',#60903,#3752);
#2466=LINE('',#60904,#3753);
#2467=LINE('',#60907,#3754);
#2468=LINE('',#60909,#3755);
#2469=LINE('',#60911,#3756);
#2470=LINE('',#60913,#3757);
#2471=LINE('',#60915,#3758);
#2472=LINE('',#60917,#3759);
#2473=LINE('',#60919,#3760);
#2474=LINE('',#60920,#3761);
#2475=LINE('',#60938,#3762);
#2476=LINE('',#60948,#3763);
#2477=LINE('',#60952,#3764);
#2478=LINE('',#60956,#3765);
#2479=LINE('',#60959,#3766);
#2480=LINE('',#60962,#3767);
#2481=LINE('',#60964,#3768);
#2482=LINE('',#60965,#3769);
#2483=LINE('',#60968,#3770);
#2484=LINE('',#60969,#3771);
#2485=LINE('',#60978,#3772);
#2486=LINE('',#60980,#3773);
#2487=LINE('',#60985,#3774);
#2488=LINE('',#60989,#3775);
#2489=LINE('',#60993,#3776);
#2490=LINE('',#60996,#3777);
#2491=LINE('',#60999,#3778);
#2492=LINE('',#61001,#3779);
#2493=LINE('',#61002,#3780);
#2494=LINE('',#61005,#3781);
#2495=LINE('',#61006,#3782);
#2496=LINE('',#61015,#3783);
#2497=LINE('',#61017,#3784);
#2498=LINE('',#61023,#3785);
#2499=LINE('',#61027,#3786);
#2500=LINE('',#61030,#3787);
#2501=LINE('',#61035,#3788);
#2502=LINE('',#61039,#3789);
#2503=LINE('',#61044,#3790);
#2504=LINE('',#61045,#3791);
#2505=LINE('',#61047,#3792);
#2506=LINE('',#61050,#3793);
#2507=LINE('',#61055,#3794);
#2508=LINE('',#61060,#3795);
#2509=LINE('',#61061,#3796);
#2510=LINE('',#61062,#3797);
#2511=LINE('',#61064,#3798);
#2512=LINE('',#61066,#3799);
#2513=LINE('',#61069,#3800);
#2514=LINE('',#61075,#3801);
#2515=LINE('',#61079,#3802);
#2516=LINE('',#61082,#3803);
#2517=LINE('',#61087,#3804);
#2518=LINE('',#61091,#3805);
#2519=LINE('',#61096,#3806);
#2520=LINE('',#61097,#3807);
#2521=LINE('',#61099,#3808);
#2522=LINE('',#61102,#3809);
#2523=LINE('',#61107,#3810);
#2524=LINE('',#61112,#3811);
#2525=LINE('',#61113,#3812);
#2526=LINE('',#61114,#3813);
#2527=LINE('',#61116,#3814);
#2528=LINE('',#61118,#3815);
#2529=LINE('',#61121,#3816);
#2530=LINE('',#61146,#3817);
#2531=LINE('',#61147,#3818);
#2532=LINE('',#61152,#3819);
#2533=LINE('',#61153,#3820);
#2534=LINE('',#61155,#3821);
#2535=LINE('',#61156,#3822);
#2536=LINE('',#61167,#3823);
#2537=LINE('',#61168,#3824);
#2538=LINE('',#61171,#3825);
#2539=LINE('',#61173,#3826);
#2540=LINE('',#61177,#3827);
#2541=LINE('',#61179,#3828);
#2542=LINE('',#61189,#3829);
#2543=LINE('',#61190,#3830);
#2544=LINE('',#61195,#3831);
#2545=LINE('',#61196,#3832);
#2546=LINE('',#61205,#3833);
#2547=LINE('',#61206,#3834);
#2548=LINE('',#61208,#3835);
#2549=LINE('',#61209,#3836);
#2550=LINE('',#61228,#3837);
#2551=LINE('',#61229,#3838);
#2552=LINE('',#61238,#3839);
#2553=LINE('',#61239,#3840);
#2554=LINE('',#61242,#3841);
#2555=LINE('',#61244,#3842);
#2556=LINE('',#61254,#3843);
#2557=LINE('',#61255,#3844);
#2558=LINE('',#61257,#3845);
#2559=LINE('',#61258,#3846);
#2560=LINE('',#61263,#3847);
#2561=LINE('',#61264,#3848);
#2562=LINE('',#61270,#3849);
#2563=LINE('',#61271,#3850);
#2564=LINE('',#61275,#3851);
#2565=LINE('',#61276,#3852);
#2566=LINE('',#61278,#3853);
#2567=LINE('',#61279,#3854);
#2568=LINE('',#61389,#3855);
#2569=LINE('',#61391,#3856);
#2570=LINE('',#61397,#3857);
#2571=LINE('',#61399,#3858);
#2572=LINE('',#61403,#3859);
#2573=LINE('',#61406,#3860);
#2574=LINE('',#61409,#3861);
#2575=LINE('',#61411,#3862);
#2576=LINE('',#61412,#3863);
#2577=LINE('',#61414,#3864);
#2578=LINE('',#61424,#3865);
#2579=LINE('',#61436,#3866);
#2580=LINE('',#61459,#3867);
#2581=LINE('',#61469,#3868);
#2582=LINE('',#61474,#3869);
#2583=LINE('',#61478,#3870);
#2584=LINE('',#61496,#3871);
#2585=LINE('',#61497,#3872);
#2586=LINE('',#61516,#3873);
#2587=LINE('',#61517,#3874);
#2588=LINE('',#61558,#3875);
#2589=LINE('',#61560,#3876);
#2590=LINE('',#61561,#3877);
#2591=LINE('',#61565,#3878);
#2592=LINE('',#61568,#3879);
#2593=LINE('',#61571,#3880);
#2594=LINE('',#61619,#3881);
#2595=LINE('',#61622,#3882);
#2596=LINE('',#61632,#3883);
#2597=LINE('',#61640,#3884);
#2598=LINE('',#61646,#3885);
#2599=LINE('',#61653,#3886);
#2600=LINE('',#61655,#3887);
#2601=LINE('',#61657,#3888);
#2602=LINE('',#61661,#3889);
#2603=LINE('',#61663,#3890);
#2604=LINE('',#61665,#3891);
#2605=LINE('',#61669,#3892);
#2606=LINE('',#61671,#3893);
#2607=LINE('',#61673,#3894);
#2608=LINE('',#61677,#3895);
#2609=LINE('',#61679,#3896);
#2610=LINE('',#61681,#3897);
#2611=LINE('',#61685,#3898);
#2612=LINE('',#61687,#3899);
#2613=LINE('',#61689,#3900);
#2614=LINE('',#61693,#3901);
#2615=LINE('',#61695,#3902);
#2616=LINE('',#61697,#3903);
#2617=LINE('',#61701,#3904);
#2618=LINE('',#61703,#3905);
#2619=LINE('',#61705,#3906);
#2620=LINE('',#61709,#3907);
#2621=LINE('',#61711,#3908);
#2622=LINE('',#61713,#3909);
#2623=LINE('',#61717,#3910);
#2624=LINE('',#61719,#3911);
#2625=LINE('',#61721,#3912);
#2626=LINE('',#61725,#3913);
#2627=LINE('',#61727,#3914);
#2628=LINE('',#61729,#3915);
#2629=LINE('',#61733,#3916);
#2630=LINE('',#61735,#3917);
#2631=LINE('',#61737,#3918);
#2632=LINE('',#61741,#3919);
#2633=LINE('',#61743,#3920);
#2634=LINE('',#61745,#3921);
#2635=LINE('',#61749,#3922);
#2636=LINE('',#61751,#3923);
#2637=LINE('',#61753,#3924);
#2638=LINE('',#61757,#3925);
#2639=LINE('',#61759,#3926);
#2640=LINE('',#61760,#3927);
#2641=LINE('',#61763,#3928);
#2642=LINE('',#61765,#3929);
#2643=LINE('',#61766,#3930);
#2644=LINE('',#61769,#3931);
#2645=LINE('',#61771,#3932);
#2646=LINE('',#61772,#3933);
#2647=LINE('',#61774,#3934);
#2648=LINE('',#61778,#3935);
#2649=LINE('',#61781,#3936);
#2650=LINE('',#61782,#3937);
#2651=LINE('',#61785,#3938);
#2652=LINE('',#61787,#3939);
#2653=LINE('',#61788,#3940);
#2654=LINE('',#61790,#3941);
#2655=LINE('',#61794,#3942);
#2656=LINE('',#61797,#3943);
#2657=LINE('',#61798,#3944);
#2658=LINE('',#61801,#3945);
#2659=LINE('',#61803,#3946);
#2660=LINE('',#61804,#3947);
#2661=LINE('',#61806,#3948);
#2662=LINE('',#61810,#3949);
#2663=LINE('',#61813,#3950);
#2664=LINE('',#61814,#3951);
#2665=LINE('',#61817,#3952);
#2666=LINE('',#61819,#3953);
#2667=LINE('',#61820,#3954);
#2668=LINE('',#61822,#3955);
#2669=LINE('',#61826,#3956);
#2670=LINE('',#61829,#3957);
#2671=LINE('',#61830,#3958);
#2672=LINE('',#61833,#3959);
#2673=LINE('',#61835,#3960);
#2674=LINE('',#61836,#3961);
#2675=LINE('',#61838,#3962);
#2676=LINE('',#61842,#3963);
#2677=LINE('',#61845,#3964);
#2678=LINE('',#61846,#3965);
#2679=LINE('',#61849,#3966);
#2680=LINE('',#61851,#3967);
#2681=LINE('',#61852,#3968);
#2682=LINE('',#61854,#3969);
#2683=LINE('',#61858,#3970);
#2684=LINE('',#61861,#3971);
#2685=LINE('',#61862,#3972);
#2686=LINE('',#61865,#3973);
#2687=LINE('',#61867,#3974);
#2688=LINE('',#61868,#3975);
#2689=LINE('',#61870,#3976);
#2690=LINE('',#61874,#3977);
#2691=LINE('',#61877,#3978);
#2692=LINE('',#61878,#3979);
#2693=LINE('',#61881,#3980);
#2694=LINE('',#61883,#3981);
#2695=LINE('',#61884,#3982);
#2696=LINE('',#61886,#3983);
#2697=LINE('',#61890,#3984);
#2698=LINE('',#61893,#3985);
#2699=LINE('',#61894,#3986);
#2700=LINE('',#61897,#3987);
#2701=LINE('',#61899,#3988);
#2702=LINE('',#61900,#3989);
#2703=LINE('',#61902,#3990);
#2704=LINE('',#61906,#3991);
#2705=LINE('',#61909,#3992);
#2706=LINE('',#61910,#3993);
#2707=LINE('',#61913,#3994);
#2708=LINE('',#61915,#3995);
#2709=LINE('',#61916,#3996);
#2710=LINE('',#61918,#3997);
#2711=LINE('',#61922,#3998);
#2712=LINE('',#61925,#3999);
#2713=LINE('',#61926,#4000);
#2714=LINE('',#61929,#4001);
#2715=LINE('',#61931,#4002);
#2716=LINE('',#61932,#4003);
#2717=LINE('',#61934,#4004);
#2718=LINE('',#61938,#4005);
#2719=LINE('',#61941,#4006);
#2720=LINE('',#61942,#4007);
#2721=LINE('',#61945,#4008);
#2722=LINE('',#61947,#4009);
#2723=LINE('',#61948,#4010);
#2724=LINE('',#61950,#4011);
#2725=LINE('',#61954,#4012);
#2726=LINE('',#61957,#4013);
#2727=LINE('',#61958,#4014);
#2728=LINE('',#61961,#4015);
#2729=LINE('',#61963,#4016);
#2730=LINE('',#61964,#4017);
#2731=LINE('',#61966,#4018);
#2732=LINE('',#61970,#4019);
#2733=LINE('',#61973,#4020);
#2734=LINE('',#61975,#4021);
#2735=LINE('',#61976,#4022);
#2736=LINE('',#61979,#4023);
#2737=LINE('',#61980,#4024);
#2738=LINE('',#61982,#4025);
#2739=LINE('',#61989,#4026);
#2740=LINE('',#61994,#4027);
#2741=LINE('',#62177,#4028);
#2742=LINE('',#62607,#4029);
#2743=LINE('',#63034,#4030);
#2744=LINE('',#63490,#4031);
#2745=LINE('',#63954,#4032);
#2746=LINE('',#64297,#4033);
#2747=LINE('',#64695,#4034);
#2748=LINE('',#65028,#4035);
#2749=LINE('',#65420,#4036);
#2750=LINE('',#65803,#4037);
#2751=LINE('',#66202,#4038);
#2752=LINE('',#66758,#4039);
#2753=LINE('',#67219,#4040);
#2754=LINE('',#67749,#4041);
#2755=LINE('',#68202,#4042);
#2756=LINE('',#68741,#4043);
#2757=LINE('',#69203,#4044);
#2758=LINE('',#69714,#4045);
#2759=LINE('',#70197,#4046);
#2760=LINE('',#70661,#4047);
#2761=LINE('',#71128,#4048);
#2762=LINE('',#71592,#4049);
#2763=LINE('',#72044,#4050);
#2764=LINE('',#72530,#4051);
#2765=LINE('',#72983,#4052);
#2766=LINE('',#73456,#4053);
#2767=LINE('',#73924,#4054);
#2768=LINE('',#74396,#4055);
#2769=LINE('',#74858,#4056);
#2770=LINE('',#75318,#4057);
#2771=LINE('',#75804,#4058);
#2772=LINE('',#76261,#4059);
#2773=LINE('',#76732,#4060);
#2774=LINE('',#77194,#4061);
#2775=LINE('',#77655,#4062);
#2776=LINE('',#78092,#4063);
#2777=LINE('',#78388,#4064);
#2778=LINE('',#78748,#4065);
#2779=LINE('',#88562,#4066);
#2780=LINE('',#90954,#4067);
#2781=LINE('',#90957,#4068);
#2782=LINE('',#90962,#4069);
#2783=LINE('',#90969,#4070);
#2784=LINE('',#90976,#4071);
#2785=LINE('',#90979,#4072);
#2786=LINE('',#91011,#4073);
#2787=LINE('',#91050,#4074);
#2788=LINE('',#91051,#4075);
#2789=LINE('',#91106,#4076);
#2790=LINE('',#91108,#4077);
#2791=LINE('',#91160,#4078);
#2792=LINE('',#91199,#4079);
#2793=LINE('',#91200,#4080);
#2794=LINE('',#91206,#4081);
#2795=LINE('',#91209,#4082);
#2796=LINE('',#91212,#4083);
#2797=LINE('',#91214,#4084);
#2798=LINE('',#91215,#4085);
#2799=LINE('',#91220,#4086);
#2800=LINE('',#91224,#4087);
#2801=LINE('',#91228,#4088);
#2802=LINE('',#91232,#4089);
#2803=LINE('',#91236,#4090);
#2804=LINE('',#91240,#4091);
#2805=LINE('',#91244,#4092);
#2806=LINE('',#91246,#4093);
#2807=LINE('',#91248,#4094);
#2808=LINE('',#91249,#4095);
#2809=LINE('',#91251,#4096);
#2810=LINE('',#91252,#4097);
#2811=LINE('',#91268,#4098);
#2812=LINE('',#91272,#4099);
#2813=LINE('',#91277,#4100);
#2814=LINE('',#91290,#4101);
#2815=LINE('',#91312,#4102);
#2816=LINE('',#91318,#4103);
#2817=LINE('',#91322,#4104);
#2818=LINE('',#91326,#4105);
#2819=LINE('',#91330,#4106);
#2820=LINE('',#91332,#4107);
#2821=LINE('',#91333,#4108);
#2822=LINE('',#91338,#4109);
#2823=LINE('',#91339,#4110);
#2824=LINE('',#91342,#4111);
#2825=LINE('',#91345,#4112);
#2826=LINE('',#91348,#4113);
#2827=LINE('',#91350,#4114);
#2828=LINE('',#91352,#4115);
#2829=LINE('',#91356,#4116);
#2830=LINE('',#91358,#4117);
#2831=LINE('',#91361,#4118);
#2832=LINE('',#91365,#4119);
#2833=LINE('',#91367,#4120);
#2834=LINE('',#91369,#4121);
#2835=LINE('',#91371,#4122);
#2836=LINE('',#91372,#4123);
#2837=LINE('',#91376,#4124);
#2838=LINE('',#91380,#4125);
#2839=LINE('',#91397,#4126);
#2840=LINE('',#91401,#4127);
#2841=LINE('',#91406,#4128);
#2842=LINE('',#91407,#4129);
#2843=LINE('',#91412,#4130);
#2844=LINE('',#91415,#4131);
#2845=LINE('',#91429,#4132);
#2846=LINE('',#91431,#4133);
#2847=LINE('',#91438,#4134);
#2848=LINE('',#91440,#4135);
#2849=LINE('',#91442,#4136);
#2850=LINE('',#91443,#4137);
#2851=LINE('',#91446,#4138);
#2852=LINE('',#91449,#4139);
#2853=LINE('',#91451,#4140);
#2854=LINE('',#91453,#4141);
#2855=LINE('',#91455,#4142);
#2856=LINE('',#91457,#4143);
#2857=LINE('',#91459,#4144);
#2858=LINE('',#91460,#4145);
#2859=LINE('',#91463,#4146);
#2860=LINE('',#91469,#4147);
#2861=LINE('',#91471,#4148);
#2862=LINE('',#91472,#4149);
#2863=LINE('',#91483,#4150);
#2864=LINE('',#91495,#4151);
#2865=LINE('',#91498,#4152);
#2866=LINE('',#91502,#4153);
#2867=LINE('',#91503,#4154);
#2868=LINE('',#91568,#4155);
#2869=LINE('',#91569,#4156);
#2870=LINE('',#91572,#4157);
#2871=LINE('',#91575,#4158);
#2872=LINE('',#91595,#4159);
#2873=LINE('',#91596,#4160);
#2874=LINE('',#91617,#4161);
#2875=LINE('',#91620,#4162);
#2876=LINE('',#91655,#4163);
#2877=LINE('',#91813,#4164);
#2878=LINE('',#91834,#4165);
#2879=LINE('',#91841,#4166);
#2880=LINE('',#91844,#4167);
#2881=LINE('',#91848,#4168);
#2882=LINE('',#91851,#4169);
#2883=LINE('',#91857,#4170);
#2884=LINE('',#91865,#4171);
#2885=LINE('',#91886,#4172);
#2886=LINE('',#91890,#4173);
#2887=LINE('',#91896,#4174);
#2888=LINE('',#91900,#4175);
#2889=LINE('',#91902,#4176);
#2890=LINE('',#91905,#4177);
#2891=LINE('',#91918,#4178);
#2892=LINE('',#91921,#4179);
#2893=LINE('',#91923,#4180);
#2894=LINE('',#91926,#4181);
#2895=LINE('',#91931,#4182);
#2896=LINE('',#91933,#4183);
#2897=LINE('',#91954,#4184);
#2898=LINE('',#91982,#4185);
#2899=LINE('',#91985,#4186);
#2900=LINE('',#91987,#4187);
#2901=LINE('',#91993,#4188);
#2902=LINE('',#92000,#4189);
#2903=LINE('',#92007,#4190);
#2904=LINE('',#92009,#4191);
#2905=LINE('',#92013,#4192);
#2906=LINE('',#92016,#4193);
#2907=LINE('',#92020,#4194);
#2908=LINE('',#92022,#4195);
#2909=LINE('',#92024,#4196);
#2910=LINE('',#92029,#4197);
#2911=LINE('',#92059,#4198);
#2912=LINE('',#92063,#4199);
#2913=LINE('',#92066,#4200);
#2914=LINE('',#92070,#4201);
#2915=LINE('',#92082,#4202);
#2916=LINE('',#92084,#4203);
#2917=LINE('',#92085,#4204);
#2918=LINE('',#92108,#4205);
#2919=LINE('',#92112,#4206);
#2920=LINE('',#92115,#4207);
#2921=LINE('',#92117,#4208);
#2922=LINE('',#92119,#4209);
#2923=LINE('',#92122,#4210);
#2924=LINE('',#92124,#4211);
#2925=LINE('',#92126,#4212);
#2926=LINE('',#92127,#4213);
#2927=LINE('',#92130,#4214);
#2928=LINE('',#92132,#4215);
#2929=LINE('',#92138,#4216);
#2930=LINE('',#92145,#4217);
#2931=LINE('',#92146,#4218);
#2932=LINE('',#92151,#4219);
#2933=LINE('',#92153,#4220);
#2934=LINE('',#92155,#4221);
#2935=LINE('',#92159,#4222);
#2936=LINE('',#92161,#4223);
#2937=LINE('',#92163,#4224);
#2938=LINE('',#92165,#4225);
#2939=LINE('',#92167,#4226);
#2940=LINE('',#92169,#4227);
#2941=LINE('',#92171,#4228);
#2942=LINE('',#92172,#4229);
#2943=LINE('',#92174,#4230);
#2944=LINE('',#92176,#4231);
#2945=LINE('',#92177,#4232);
#2946=LINE('',#92179,#4233);
#2947=LINE('',#92180,#4234);
#2948=LINE('',#92183,#4235);
#2949=LINE('',#92185,#4236);
#2950=LINE('',#92187,#4237);
#2951=LINE('',#92188,#4238);
#2952=LINE('',#92191,#4239);
#2953=LINE('',#92193,#4240);
#2954=LINE('',#92197,#4241);
#2955=LINE('',#92199,#4242);
#2956=LINE('',#92200,#4243);
#2957=LINE('',#92208,#4244);
#2958=LINE('',#92210,#4245);
#2959=LINE('',#92235,#4246);
#2960=LINE('',#92236,#4247);
#2961=LINE('',#92239,#4248);
#2962=LINE('',#92241,#4249);
#2963=LINE('',#92242,#4250);
#2964=LINE('',#92246,#4251);
#2965=LINE('',#92249,#4252);
#2966=LINE('',#92250,#4253);
#2967=LINE('',#92254,#4254);
#2968=LINE('',#92257,#4255);
#2969=LINE('',#92258,#4256);
#2970=LINE('',#92260,#4257);
#2971=LINE('',#92265,#4258);
#2972=LINE('',#92270,#4259);
#2973=LINE('',#92280,#4260);
#2974=LINE('',#92284,#4261);
#2975=LINE('',#92286,#4262);
#2976=LINE('',#92288,#4263);
#2977=LINE('',#92290,#4264);
#2978=LINE('',#92292,#4265);
#2979=LINE('',#92293,#4266);
#2980=LINE('',#92297,#4267);
#2981=LINE('',#92309,#4268);
#2982=LINE('',#92315,#4269);
#2983=LINE('',#92317,#4270);
#2984=LINE('',#92319,#4271);
#2985=LINE('',#92321,#4272);
#2986=LINE('',#92323,#4273);
#2987=LINE('',#92351,#4274);
#2988=LINE('',#92353,#4275);
#2989=LINE('',#92357,#4276);
#2990=LINE('',#92364,#4277);
#2991=LINE('',#92366,#4278);
#2992=LINE('',#92372,#4279);
#2993=LINE('',#92374,#4280);
#2994=LINE('',#92375,#4281);
#2995=LINE('',#92376,#4282);
#2996=LINE('',#92380,#4283);
#2997=LINE('',#92383,#4284);
#2998=LINE('',#92385,#4285);
#2999=LINE('',#92386,#4286);
#3000=LINE('',#92390,#4287);
#3001=LINE('',#92393,#4288);
#3002=LINE('',#92394,#4289);
#3003=LINE('',#92399,#4290);
#3004=LINE('',#92403,#4291);
#3005=LINE('',#92405,#4292);
#3006=LINE('',#92409,#4293);
#3007=LINE('',#92410,#4294);
#3008=LINE('',#92415,#4295);
#3009=LINE('',#92419,#4296);
#3010=LINE('',#92421,#4297);
#3011=LINE('',#92425,#4298);
#3012=LINE('',#92426,#4299);
#3013=LINE('',#92431,#4300);
#3014=LINE('',#92435,#4301);
#3015=LINE('',#92437,#4302);
#3016=LINE('',#92441,#4303);
#3017=LINE('',#92442,#4304);
#3018=LINE('',#92464,#4305);
#3019=LINE('',#92468,#4306);
#3020=LINE('',#92470,#4307);
#3021=LINE('',#92474,#4308);
#3022=LINE('',#92475,#4309);
#3023=LINE('',#92483,#4310);
#3024=LINE('',#92485,#4311);
#3025=LINE('',#92487,#4312);
#3026=LINE('',#92489,#4313);
#3027=LINE('',#92491,#4314);
#3028=LINE('',#92493,#4315);
#3029=LINE('',#92495,#4316);
#3030=LINE('',#92497,#4317);
#3031=LINE('',#92506,#4318);
#3032=LINE('',#92516,#4319);
#3033=LINE('',#92520,#4320);
#3034=LINE('',#92548,#4321);
#3035=LINE('',#92551,#4322);
#3036=LINE('',#92557,#4323);
#3037=LINE('',#92558,#4324);
#3038=LINE('',#92560,#4325);
#3039=LINE('',#92561,#4326);
#3040=LINE('',#92576,#4327);
#3041=LINE('',#92584,#4328);
#3042=LINE('',#92586,#4329);
#3043=LINE('',#92588,#4330);
#3044=LINE('',#92590,#4331);
#3045=LINE('',#92592,#4332);
#3046=LINE('',#92596,#4333);
#3047=LINE('',#92598,#4334);
#3048=LINE('',#92600,#4335);
#3049=LINE('',#92601,#4336);
#3050=LINE('',#92608,#4337);
#3051=LINE('',#92609,#4338);
#3052=LINE('',#92613,#4339);
#3053=LINE('',#92617,#4340);
#3054=LINE('',#92624,#4341);
#3055=LINE('',#92626,#4342);
#3056=LINE('',#92627,#4343);
#3057=LINE('',#92645,#4344);
#3058=LINE('',#92656,#4345);
#3059=LINE('',#92660,#4346);
#3060=LINE('',#92714,#4347);
#3061=LINE('',#92718,#4348);
#3062=LINE('',#92744,#4349);
#3063=LINE('',#92748,#4350);
#3064=LINE('',#92760,#4351);
#3065=LINE('',#92770,#4352);
#3066=LINE('',#92772,#4353);
#3067=LINE('',#92776,#4354);
#3068=LINE('',#92777,#4355);
#3069=LINE('',#92780,#4356);
#3070=LINE('',#92783,#4357);
#3071=LINE('',#92784,#4358);
#3072=LINE('',#92788,#4359);
#3073=LINE('',#92790,#4360);
#3074=LINE('',#92792,#4361);
#3075=LINE('',#92793,#4362);
#3076=LINE('',#92799,#4363);
#3077=LINE('',#92805,#4364);
#3078=LINE('',#92811,#4365);
#3079=LINE('',#92819,#4366);
#3080=LINE('',#92823,#4367);
#3081=LINE('',#92826,#4368);
#3082=LINE('',#92829,#4369);
#3083=LINE('',#92830,#4370);
#3084=LINE('',#92834,#4371);
#3085=LINE('',#92836,#4372);
#3086=LINE('',#92838,#4373);
#3087=LINE('',#92839,#4374);
#3088=LINE('',#92842,#4375);
#3089=LINE('',#92844,#4376);
#3090=LINE('',#92854,#4377);
#3091=LINE('',#92873,#4378);
#3092=LINE('',#92876,#4379);
#3093=LINE('',#92881,#4380);
#3094=LINE('',#92883,#4381);
#3095=LINE('',#92886,#4382);
#3096=LINE('',#92889,#4383);
#3097=LINE('',#92891,#4384);
#3098=LINE('',#92896,#4385);
#3099=LINE('',#92898,#4386);
#3100=LINE('',#92900,#4387);
#3101=LINE('',#92905,#4388);
#3102=LINE('',#92910,#4389);
#3103=LINE('',#92912,#4390);
#3104=LINE('',#92914,#4391);
#3105=LINE('',#92919,#4392);
#3106=LINE('',#92933,#4393);
#3107=LINE('',#92957,#4394);
#3108=LINE('',#92986,#4395);
#3109=LINE('',#92988,#4396);
#3110=LINE('',#92989,#4397);
#3111=LINE('',#92991,#4398);
#3112=LINE('',#93005,#4399);
#3113=LINE('',#93010,#4400);
#3114=LINE('',#93012,#4401);
#3115=LINE('',#93024,#4402);
#3116=LINE('',#93026,#4403);
#3117=LINE('',#93029,#4404);
#3118=LINE('',#93031,#4405);
#3119=LINE('',#93032,#4406);
#3120=LINE('',#93034,#4407);
#3121=LINE('',#93036,#4408);
#3122=LINE('',#93038,#4409);
#3123=LINE('',#93041,#4410);
#3124=LINE('',#93043,#4411);
#3125=LINE('',#93044,#4412);
#3126=LINE('',#93046,#4413);
#3127=LINE('',#93055,#4414);
#3128=LINE('',#93058,#4415);
#3129=LINE('',#93104,#4416);
#3130=LINE('',#93128,#4417);
#3131=LINE('',#93131,#4418);
#3132=LINE('',#93135,#4419);
#3133=LINE('',#93136,#4420);
#3134=LINE('',#93138,#4421);
#3135=LINE('',#93141,#4422);
#3136=LINE('',#93145,#4423);
#3137=LINE('',#93146,#4424);
#3138=LINE('',#93148,#4425);
#3139=LINE('',#93151,#4426);
#3140=LINE('',#93155,#4427);
#3141=LINE('',#93156,#4428);
#3142=LINE('',#93158,#4429);
#3143=LINE('',#93162,#4430);
#3144=LINE('',#93163,#4431);
#3145=LINE('',#93165,#4432);
#3146=LINE('',#93167,#4433);
#3147=LINE('',#93175,#4434);
#3148=LINE('',#93176,#4435);
#3149=LINE('',#93178,#4436);
#3150=LINE('',#93179,#4437);
#3151=LINE('',#93226,#4438);
#3152=LINE('',#93320,#4439);
#3153=LINE('',#97681,#4440);
#3154=LINE('',#97707,#4441);
#3155=LINE('',#97716,#4442);
#3156=LINE('',#97722,#4443);
#3157=LINE('',#97725,#4444);
#3158=LINE('',#97736,#4445);
#3159=LINE('',#97746,#4446);
#3160=LINE('',#97750,#4447);
#3161=LINE('',#97754,#4448);
#3162=LINE('',#97756,#4449);
#3163=LINE('',#97760,#4450);
#3164=LINE('',#97762,#4451);
#3165=LINE('',#97765,#4452);
#3166=LINE('',#97766,#4453);
#3167=LINE('',#97768,#4454);
#3168=LINE('',#97769,#4455);
#3169=LINE('',#97771,#4456);
#3170=LINE('',#97775,#4457);
#3171=LINE('',#97777,#4458);
#3172=LINE('',#97779,#4459);
#3173=LINE('',#97780,#4460);
#3174=LINE('',#97783,#4461);
#3175=LINE('',#97785,#4462);
#3176=LINE('',#97786,#4463);
#3177=LINE('',#97789,#4464);
#3178=LINE('',#97790,#4465);
#3179=LINE('',#97793,#4466);
#3180=LINE('',#97794,#4467);
#3181=LINE('',#97796,#4468);
#3182=LINE('',#97799,#4469);
#3183=LINE('',#97807,#4470);
#3184=LINE('',#97810,#4471);
#3185=LINE('',#97816,#4472);
#3186=LINE('',#97818,#4473);
#3187=LINE('',#97823,#4474);
#3188=LINE('',#97826,#4475);
#3189=LINE('',#97831,#4476);
#3190=LINE('',#97833,#4477);
#3191=LINE('',#97844,#4478);
#3192=LINE('',#97847,#4479);
#3193=LINE('',#97850,#4480);
#3194=LINE('',#97851,#4481);
#3195=LINE('',#97854,#4482);
#3196=LINE('',#97858,#4483);
#3197=LINE('',#97889,#4484);
#3198=LINE('',#97923,#4485);
#3199=LINE('',#97929,#4486);
#3200=LINE('',#97932,#4487);
#3201=LINE('',#97937,#4488);
#3202=LINE('',#97939,#4489);
#3203=LINE('',#98313,#4490);
#3204=LINE('',#98546,#4491);
#3205=LINE('',#98555,#4492);
#3206=LINE('',#98952,#4493);
#3207=LINE('',#99248,#4494);
#3208=LINE('',#99251,#4495);
#3209=LINE('',#99259,#4496);
#3210=LINE('',#99261,#4497);
#3211=LINE('',#99394,#4498);
#3212=LINE('',#99396,#4499);
#3213=LINE('',#99400,#4500);
#3214=LINE('',#99426,#4501);
#3215=LINE('',#99452,#4502);
#3216=LINE('',#99455,#4503);
#3217=LINE('',#99551,#4504);
#3218=LINE('',#99636,#4505);
#3219=LINE('',#99637,#4506);
#3220=LINE('',#99651,#4507);
#3221=LINE('',#99665,#4508);
#3222=LINE('',#99674,#4509);
#3223=LINE('',#99685,#4510);
#3224=LINE('',#99699,#4511);
#3225=LINE('',#99707,#4512);
#3226=LINE('',#99709,#4513);
#3227=LINE('',#99720,#4514);
#3228=LINE('',#99725,#4515);
#3229=LINE('',#99732,#4516);
#3230=LINE('',#99739,#4517);
#3231=LINE('',#99748,#4518);
#3232=LINE('',#99755,#4519);
#3233=LINE('',#99767,#4520);
#3234=LINE('',#99774,#4521);
#3235=LINE('',#99781,#4522);
#3236=LINE('',#99788,#4523);
#3237=LINE('',#99792,#4524);
#3238=LINE('',#99797,#4525);
#3239=LINE('',#99799,#4526);
#3240=LINE('',#99802,#4527);
#3241=LINE('',#99809,#4528);
#3242=LINE('',#99814,#4529);
#3243=LINE('',#99817,#4530);
#3244=LINE('',#99825,#4531);
#3245=LINE('',#99832,#4532);
#3246=LINE('',#99837,#4533);
#3247=LINE('',#99840,#4534);
#3248=LINE('',#99849,#4535);
#3249=LINE('',#99854,#4536);
#3250=LINE('',#99857,#4537);
#3251=LINE('',#99868,#4538);
#3252=LINE('',#99872,#4539);
#3253=LINE('',#99879,#4540);
#3254=LINE('',#99882,#4541);
#3255=LINE('',#99890,#4542);
#3256=LINE('',#99897,#4543);
#3257=LINE('',#99904,#4544);
#3258=LINE('',#99907,#4545);
#3259=LINE('',#99915,#4546);
#3260=LINE('',#99920,#4547);
#3261=LINE('',#99923,#4548);
#3262=LINE('',#99937,#4549);
#3263=LINE('',#99944,#4550);
#3264=LINE('',#99947,#4551);
#3265=LINE('',#99960,#4552);
#3266=LINE('',#99963,#4553);
#3267=VECTOR('',#22531,14.688);
#3268=VECTOR('',#22538,14.688);
#3269=VECTOR('',#22541,2.05);
#3270=VECTOR('',#22544,2.05);
#3271=VECTOR('',#22545,10.);
#3272=VECTOR('',#22546,10.);
#3273=VECTOR('',#22547,10.);
#3274=VECTOR('',#22548,10.);
#3275=VECTOR('',#22551,10.);
#3276=VECTOR('',#22552,10.);
#3277=VECTOR('',#22553,10.);
#3278=VECTOR('',#22554,10.);
#3279=VECTOR('',#22555,10.);
#3280=VECTOR('',#22556,10.);
#3281=VECTOR('',#22557,10.);
#3282=VECTOR('',#22558,10.);
#3283=VECTOR('',#22559,10.);
#3284=VECTOR('',#22560,10.);
#3285=VECTOR('',#22561,10.);
#3286=VECTOR('',#22562,10.);
#3287=VECTOR('',#22563,10.);
#3288=VECTOR('',#22564,10.);
#3289=VECTOR('',#22565,10.);
#3290=VECTOR('',#22566,10.);
#3291=VECTOR('',#22567,10.);
#3292=VECTOR('',#22568,10.);
#3293=VECTOR('',#22569,9.99999999999999);
#3294=VECTOR('',#22570,10.);
#3295=VECTOR('',#22571,10.);
#3296=VECTOR('',#22572,10.);
#3297=VECTOR('',#22573,10.);
#3298=VECTOR('',#22574,9.99999999999999);
#3299=VECTOR('',#22575,10.);
#3300=VECTOR('',#22576,10.);
#3301=VECTOR('',#22577,10.);
#3302=VECTOR('',#22578,9.99999999999999);
#3303=VECTOR('',#22579,10.);
#3304=VECTOR('',#22580,10.);
#3305=VECTOR('',#22581,10.);
#3306=VECTOR('',#22582,10.);
#3307=VECTOR('',#22583,10.);
#3308=VECTOR('',#22584,10.);
#3309=VECTOR('',#22585,10.);
#3310=VECTOR('',#22586,10.);
#3311=VECTOR('',#22587,10.);
#3312=VECTOR('',#22588,10.);
#3313=VECTOR('',#22589,10.);
#3314=VECTOR('',#22590,10.);
#3315=VECTOR('',#22591,10.);
#3316=VECTOR('',#22592,10.);
#3317=VECTOR('',#22593,10.);
#3318=VECTOR('',#22594,10.);
#3319=VECTOR('',#22595,10.);
#3320=VECTOR('',#22596,10.);
#3321=VECTOR('',#22597,10.);
#3322=VECTOR('',#22598,10.);
#3323=VECTOR('',#22599,10.);
#3324=VECTOR('',#22600,10.);
#3325=VECTOR('',#22601,10.);
#3326=VECTOR('',#22602,10.);
#3327=VECTOR('',#22603,10.);
#3328=VECTOR('',#22604,10.);
#3329=VECTOR('',#22605,10.);
#3330=VECTOR('',#22606,10.);
#3331=VECTOR('',#22607,10.);
#3332=VECTOR('',#22608,10.);
#3333=VECTOR('',#22609,10.);
#3334=VECTOR('',#22610,10.);
#3335=VECTOR('',#22611,10.);
#3336=VECTOR('',#22612,10.);
#3337=VECTOR('',#22613,10.);
#3338=VECTOR('',#22614,10.);
#3339=VECTOR('',#22615,10.);
#3340=VECTOR('',#22616,10.);
#3341=VECTOR('',#22617,10.);
#3342=VECTOR('',#22618,10.);
#3343=VECTOR('',#22619,10.);
#3344=VECTOR('',#22620,10.);
#3345=VECTOR('',#22621,10.);
#3346=VECTOR('',#22622,10.);
#3347=VECTOR('',#22623,10.);
#3348=VECTOR('',#22624,10.);
#3349=VECTOR('',#22625,10.);
#3350=VECTOR('',#22626,10.);
#3351=VECTOR('',#22627,10.);
#3352=VECTOR('',#22628,10.);
#3353=VECTOR('',#22629,10.);
#3354=VECTOR('',#22630,10.);
#3355=VECTOR('',#22631,10.);
#3356=VECTOR('',#22632,9.99999999999999);
#3357=VECTOR('',#22653,3.672);
#3358=VECTOR('',#22656,4.08);
#3359=VECTOR('',#22665,10.);
#3360=VECTOR('',#22668,10.);
#3361=VECTOR('',#22683,10.);
#3362=VECTOR('',#22686,10.);
#3363=VECTOR('',#22699,10.);
#3364=VECTOR('',#22704,10.);
#3365=VECTOR('',#22707,10.);
#3366=VECTOR('',#22728,10.);
#3367=VECTOR('',#22733,10.);
#3368=VECTOR('',#22736,10.);
#3369=VECTOR('',#22749,10.);
#3370=VECTOR('',#22752,10.);
#3371=VECTOR('',#22761,10.);
#3372=VECTOR('',#22764,10.);
#3373=VECTOR('',#22785,10.);
#3374=VECTOR('',#22790,10.);
#3375=VECTOR('',#22793,10.);
#3376=VECTOR('',#22816,10.);
#3377=VECTOR('',#22819,10.);
#3378=VECTOR('',#22822,10.);
#3379=VECTOR('',#22823,10.);
#3380=VECTOR('',#22828,10.);
#3381=VECTOR('',#22831,10.);
#3382=VECTOR('',#22844,10.);
#3383=VECTOR('',#22847,10.);
#3384=VECTOR('',#22864,10.);
#3385=VECTOR('',#22865,10.);
#3386=VECTOR('',#22866,10.);
#3387=VECTOR('',#22867,10.);
#3388=VECTOR('',#22868,10.);
#3389=VECTOR('',#22869,10.);
#3390=VECTOR('',#22870,10.);
#3391=VECTOR('',#22871,10.);
#3392=VECTOR('',#22872,10.);
#3393=VECTOR('',#22873,10.);
#3394=VECTOR('',#22874,10.);
#3395=VECTOR('',#22875,10.);
#3396=VECTOR('',#22876,10.);
#3397=VECTOR('',#22877,10.);
#3398=VECTOR('',#22878,10.);
#3399=VECTOR('',#22879,10.);
#3400=VECTOR('',#22880,10.);
#3401=VECTOR('',#22881,10.);
#3402=VECTOR('',#22882,10.);
#3403=VECTOR('',#22883,10.);
#3404=VECTOR('',#22884,10.);
#3405=VECTOR('',#22885,10.);
#3406=VECTOR('',#22888,10.);
#3407=VECTOR('',#22891,10.);
#3408=VECTOR('',#22894,10.);
#3409=VECTOR('',#22897,10.);
#3410=VECTOR('',#22900,10.);
#3411=VECTOR('',#22903,10.);
#3412=VECTOR('',#22906,10.);
#3413=VECTOR('',#22913,10.);
#3414=VECTOR('',#22916,10.);
#3415=VECTOR('',#22919,10.);
#3416=VECTOR('',#22922,10.);
#3417=VECTOR('',#22927,2.5);
#3418=VECTOR('',#22942,3.672);
#3419=VECTOR('',#22955,10.);
#3420=VECTOR('',#22968,10.);
#3421=VECTOR('',#22975,10.);
#3422=VECTOR('',#22978,10.);
#3423=VECTOR('',#22981,10.);
#3424=VECTOR('',#22982,10.);
#3425=VECTOR('',#22985,10.);
#3426=VECTOR('',#23008,10.);
#3427=VECTOR('',#23011,10.);
#3428=VECTOR('',#23026,10.);
#3429=VECTOR('',#23037,10.);
#3430=VECTOR('',#23056,10.);
#3431=VECTOR('',#23067,10.);
#3432=VECTOR('',#23078,10.);
#3433=VECTOR('',#23083,10.);
#3434=VECTOR('',#23094,10.);
#3435=VECTOR('',#23095,10.);
#3436=VECTOR('',#23106,10.);
#3437=VECTOR('',#23107,10.);
#3438=VECTOR('',#23118,10.);
#3439=VECTOR('',#23119,10.);
#3440=VECTOR('',#23128,10.);
#3441=VECTOR('',#23131,10.);
#3442=VECTOR('',#23134,10.);
#3443=VECTOR('',#23137,10.);
#3444=VECTOR('',#23140,10.);
#3445=VECTOR('',#23143,10.);
#3446=VECTOR('',#23162,10.);
#3447=VECTOR('',#23163,10.);
#3448=VECTOR('',#23180,10.);
#3449=VECTOR('',#23217,10.);
#3450=VECTOR('',#23220,10.);
#3451=VECTOR('',#23223,10.);
#3452=VECTOR('',#23226,10.);
#3453=VECTOR('',#23233,10.);
#3454=VECTOR('',#23246,2.5);
#3455=VECTOR('',#23261,10.);
#3456=VECTOR('',#23272,10.);
#3457=VECTOR('',#23283,10.);
#3458=VECTOR('',#23294,10.);
#3459=VECTOR('',#23297,10.);
#3460=VECTOR('',#23304,10.);
#3461=VECTOR('',#23315,10.);
#3462=VECTOR('',#23318,10.);
#3463=VECTOR('',#23323,10.);
#3464=VECTOR('',#23324,10.);
#3465=VECTOR('',#23335,10.);
#3466=VECTOR('',#23336,10.);
#3467=VECTOR('',#23347,10.);
#3468=VECTOR('',#23348,10.);
#3469=VECTOR('',#23359,10.);
#3470=VECTOR('',#23360,10.);
#3471=VECTOR('',#23371,10.);
#3472=VECTOR('',#23372,10.);
#3473=VECTOR('',#23381,10.);
#3474=VECTOR('',#23390,10.);
#3475=VECTOR('',#23393,10.);
#3476=VECTOR('',#23394,10.);
#3477=VECTOR('',#23397,10.);
#3478=VECTOR('',#23400,10.);
#3479=VECTOR('',#23403,10.);
#3480=VECTOR('',#23406,10.);
#3481=VECTOR('',#23409,10.);
#3482=VECTOR('',#23412,10.);
#3483=VECTOR('',#23415,10.);
#3484=VECTOR('',#23416,10.);
#3485=VECTOR('',#23419,10.);
#3486=VECTOR('',#23422,10.);
#3487=VECTOR('',#23427,10.);
#3488=VECTOR('',#23430,10.);
#3489=VECTOR('',#23433,10.);
#3490=VECTOR('',#23442,10.);
#3491=VECTOR('',#23443,10.);
#3492=VECTOR('',#23446,10.);
#3493=VECTOR('',#23447,10.);
#3494=VECTOR('',#23448,10.);
#3495=VECTOR('',#23449,10.);
#3496=VECTOR('',#23450,10.);
#3497=VECTOR('',#23451,10.);
#3498=VECTOR('',#23452,10.);
#3499=VECTOR('',#23453,10.);
#3500=VECTOR('',#23454,10.);
#3501=VECTOR('',#23455,10.);
#3502=VECTOR('',#23456,10.);
#3503=VECTOR('',#23457,10.);
#3504=VECTOR('',#23458,10.);
#3505=VECTOR('',#23461,10.);
#3506=VECTOR('',#23464,10.);
#3507=VECTOR('',#23467,10.);
#3508=VECTOR('',#23470,10.);
#3509=VECTOR('',#23475,10.);
#3510=VECTOR('',#23488,10.);
#3511=VECTOR('',#23491,10.);
#3512=VECTOR('',#23494,10.);
#3513=VECTOR('',#23497,10.);
#3514=VECTOR('',#23510,10.);
#3515=VECTOR('',#23523,10.);
#3516=VECTOR('',#23530,10.);
#3517=VECTOR('',#23533,10.);
#3518=VECTOR('',#23550,10.);
#3519=VECTOR('',#23567,10.);
#3520=VECTOR('',#23568,10.);
#3521=VECTOR('',#23585,10.);
#3522=VECTOR('',#23586,10.);
#3523=VECTOR('',#23605,10.);
#3524=VECTOR('',#23634,10.);
#3525=VECTOR('',#23635,10.);
#3526=VECTOR('',#23638,10.);
#3527=VECTOR('',#23641,10.);
#3528=VECTOR('',#23644,10.);
#3529=VECTOR('',#23651,10.);
#3530=VECTOR('',#23658,10.);
#3531=VECTOR('',#23675,10.);
#3532=VECTOR('',#23678,10.);
#3533=VECTOR('',#23691,10.);
#3534=VECTOR('',#23694,10.);
#3535=VECTOR('',#23701,10.);
#3536=VECTOR('',#23712,10.);
#3537=VECTOR('',#23723,10.);
#3538=VECTOR('',#23734,10.);
#3539=VECTOR('',#23737,10.);
#3540=VECTOR('',#23742,10.);
#3541=VECTOR('',#23743,10.);
#3542=VECTOR('',#23748,10.);
#3543=VECTOR('',#23753,10.);
#3544=VECTOR('',#23754,10.);
#3545=VECTOR('',#23765,10.);
#3546=VECTOR('',#23766,10.);
#3547=VECTOR('',#23777,10.);
#3548=VECTOR('',#23778,10.);
#3549=VECTOR('',#23789,10.);
#3550=VECTOR('',#23790,10.);
#3551=VECTOR('',#23799,10.);
#3552=VECTOR('',#23802,10.);
#3553=VECTOR('',#23815,10.);
#3554=VECTOR('',#23818,10.);
#3555=VECTOR('',#23823,10.);
#3556=VECTOR('',#23826,10.);
#3557=VECTOR('',#23831,10.);
#3558=VECTOR('',#23836,10.);
#3559=VECTOR('',#23839,10.);
#3560=VECTOR('',#23840,10.);
#3561=VECTOR('',#23843,10.);
#3562=VECTOR('',#23850,10.);
#3563=VECTOR('',#23855,10.);
#3564=VECTOR('',#23864,10.);
#3565=VECTOR('',#23873,10.);
#3566=VECTOR('',#23876,10.);
#3567=VECTOR('',#23887,10.);
#3568=VECTOR('',#23912,10.);
#3569=VECTOR('',#23917,10.);
#3570=VECTOR('',#23936,4.08);
#3571=VECTOR('',#23949,10.);
#3572=VECTOR('',#23952,10.);
#3573=VECTOR('',#23957,10.);
#3574=VECTOR('',#23958,10.);
#3575=VECTOR('',#23963,10.);
#3576=VECTOR('',#23964,10.);
#3577=VECTOR('',#23969,10.);
#3578=VECTOR('',#23970,10.);
#3579=VECTOR('',#23973,10.);
#3580=VECTOR('',#23974,10.);
#3581=VECTOR('',#23975,10.);
#3582=VECTOR('',#23978,10.);
#3583=VECTOR('',#23979,10.);
#3584=VECTOR('',#23982,10.);
#3585=VECTOR('',#23985,10.);
#3586=VECTOR('',#23986,10.);
#3587=VECTOR('',#23987,10.);
#3588=VECTOR('',#23988,10.);
#3589=VECTOR('',#23993,10.);
#3590=VECTOR('',#23996,10.);
#3591=VECTOR('',#23999,10.);
#3592=VECTOR('',#24004,10.);
#3593=VECTOR('',#24011,10.);
#3594=VECTOR('',#24014,10.);
#3595=VECTOR('',#24015,10.);
#3596=VECTOR('',#24018,10.);
#3597=VECTOR('',#24021,10.);
#3598=VECTOR('',#24022,10.);
#3599=VECTOR('',#24023,10.);
#3600=VECTOR('',#24024,10.);
#3601=VECTOR('',#24025,10.);
#3602=VECTOR('',#24026,10.);
#3603=VECTOR('',#24033,10.);
#3604=VECTOR('',#24036,10.);
#3605=VECTOR('',#24039,10.);
#3606=VECTOR('',#24044,10.);
#3607=VECTOR('',#24045,10.);
#3608=VECTOR('',#24046,10.);
#3609=VECTOR('',#24049,10.);
#3610=VECTOR('',#24052,10.);
#3611=VECTOR('',#24057,10.);
#3612=VECTOR('',#24058,10.);
#3613=VECTOR('',#24063,10.);
#3614=VECTOR('',#24064,10.);
#3615=VECTOR('',#24069,10.);
#3616=VECTOR('',#24070,10.);
#3617=VECTOR('',#24073,10.);
#3618=VECTOR('',#24074,10.);
#3619=VECTOR('',#24075,10.);
#3620=VECTOR('',#24078,10.);
#3621=VECTOR('',#24079,10.);
#3622=VECTOR('',#24082,10.);
#3623=VECTOR('',#24083,10.);
#3624=VECTOR('',#24084,10.);
#3625=VECTOR('',#24085,10.);
#3626=VECTOR('',#24100,10.);
#3627=VECTOR('',#24103,10.);
#3628=VECTOR('',#24104,10.);
#3629=VECTOR('',#24105,10.);
#3630=VECTOR('',#24106,10.);
#3631=VECTOR('',#24107,10.);
#3632=VECTOR('',#24108,10.);
#3633=VECTOR('',#24109,10.);
#3634=VECTOR('',#24110,10.);
#3635=VECTOR('',#24111,10.);
#3636=VECTOR('',#24112,10.);
#3637=VECTOR('',#24113,10.);
#3638=VECTOR('',#24116,10.);
#3639=VECTOR('',#24123,10.);
#3640=VECTOR('',#24128,10.);
#3641=VECTOR('',#24143,10.);
#3642=VECTOR('',#24146,10.);
#3643=VECTOR('',#24149,10.);
#3644=VECTOR('',#24150,10.);
#3645=VECTOR('',#24153,10.);
#3646=VECTOR('',#24158,10.);
#3647=VECTOR('',#24161,10.);
#3648=VECTOR('',#24164,10.);
#3649=VECTOR('',#24167,10.);
#3650=VECTOR('',#24170,10.);
#3651=VECTOR('',#24173,10.);
#3652=VECTOR('',#24178,10.);
#3653=VECTOR('',#24181,10.);
#3654=VECTOR('',#24196,10.);
#3655=VECTOR('',#24205,10.);
#3656=VECTOR('',#24206,10.);
#3657=VECTOR('',#24209,10.);
#3658=VECTOR('',#24210,10.);
#3659=VECTOR('',#24213,10.);
#3660=VECTOR('',#24214,10.);
#3661=VECTOR('',#24217,10.);
#3662=VECTOR('',#24218,10.);
#3663=VECTOR('',#24221,10.);
#3664=VECTOR('',#24226,10.);
#3665=VECTOR('',#24227,10.);
#3666=VECTOR('',#24230,10.);
#3667=VECTOR('',#24233,10.);
#3668=VECTOR('',#24238,10.);
#3669=VECTOR('',#24245,10.);
#3670=VECTOR('',#24256,10.);
#3671=VECTOR('',#24263,10.);
#3672=VECTOR('',#24266,10.);
#3673=VECTOR('',#24269,10.);
#3674=VECTOR('',#24274,10.);
#3675=VECTOR('',#24281,10.);
#3676=VECTOR('',#24284,10.);
#3677=VECTOR('',#24285,10.);
#3678=VECTOR('',#24288,10.);
#3679=VECTOR('',#24291,10.);
#3680=VECTOR('',#24292,10.);
#3681=VECTOR('',#24293,10.);
#3682=VECTOR('',#24294,10.);
#3683=VECTOR('',#24299,10.);
#3684=VECTOR('',#24300,10.);
#3685=VECTOR('',#24309,10.);
#3686=VECTOR('',#24312,10.);
#3687=VECTOR('',#24315,10.);
#3688=VECTOR('',#24318,10.);
#3689=VECTOR('',#24321,10.);
#3690=VECTOR('',#24326,10.);
#3691=VECTOR('',#24327,10.);
#3692=VECTOR('',#24330,10.);
#3693=VECTOR('',#24331,10.);
#3694=VECTOR('',#24334,10.);
#3695=VECTOR('',#24339,10.);
#3696=VECTOR('',#24340,10.);
#3697=VECTOR('',#24343,10.);
#3698=VECTOR('',#24344,10.);
#3699=VECTOR('',#24347,10.);
#3700=VECTOR('',#24350,10.);
#3701=VECTOR('',#24361,10.);
#3702=VECTOR('',#24364,10.);
#3703=VECTOR('',#24369,10.);
#3704=VECTOR('',#24374,10.);
#3705=VECTOR('',#24399,6.12);
#3706=VECTOR('',#24406,10.);
#3707=VECTOR('',#24411,10.);
#3708=VECTOR('',#24414,10.);
#3709=VECTOR('',#24419,10.);
#3710=VECTOR('',#24424,10.);
#3711=VECTOR('',#24429,10.);
#3712=VECTOR('',#24458,6.12);
#3713=VECTOR('',#24471,3.672);
#3714=VECTOR('',#24490,3.672);
#3715=VECTOR('',#24513,2.448);
#3716=VECTOR('',#24538,2.5);
#3717=VECTOR('',#24547,10.);
#3718=VECTOR('',#24564,2.5);
#3719=VECTOR('',#24583,2.448);
#3720=VECTOR('',#24604,1.3);
#3721=VECTOR('',#24607,10.);
#3722=VECTOR('',#24608,10.);
#3723=VECTOR('',#24609,10.);
#3724=VECTOR('',#24610,10.);
#3725=VECTOR('',#24611,10.);
#3726=VECTOR('',#24614,10.);
#3727=VECTOR('',#24615,10.);
#3728=VECTOR('',#24616,10.);
#3729=VECTOR('',#24617,10.);
#3730=VECTOR('',#24618,10.);
#3731=VECTOR('',#24619,10.);
#3732=VECTOR('',#24620,10.);
#3733=VECTOR('',#24621,10.);
#3734=VECTOR('',#24624,10.);
#3735=VECTOR('',#24633,10.);
#3736=VECTOR('',#24636,10.);
#3737=VECTOR('',#24639,10.);
#3738=VECTOR('',#24640,10.);
#3739=VECTOR('',#24643,10.);
#3740=VECTOR('',#24644,10.);
#3741=VECTOR('',#24647,10.);
#3742=VECTOR('',#24658,10.);
#3743=VECTOR('',#24659,10.);
#3744=VECTOR('',#24660,10.);
#3745=VECTOR('',#24661,10.);
#3746=VECTOR('',#24662,10.);
#3747=VECTOR('',#24663,10.);
#3748=VECTOR('',#24664,10.);
#3749=VECTOR('',#24665,10.);
#3750=VECTOR('',#24666,10.);
#3751=VECTOR('',#24667,10.);
#3752=VECTOR('',#24668,10.);
#3753=VECTOR('',#24669,10.);
#3754=VECTOR('',#24670,10.);
#3755=VECTOR('',#24671,10.);
#3756=VECTOR('',#24672,10.);
#3757=VECTOR('',#24673,10.);
#3758=VECTOR('',#24674,10.);
#3759=VECTOR('',#24675,10.);
#3760=VECTOR('',#24676,10.);
#3761=VECTOR('',#24677,10.);
#3762=VECTOR('',#24704,1.3);
#3763=VECTOR('',#24717,10.);
#3764=VECTOR('',#24722,10.);
#3765=VECTOR('',#24727,10.);
#3766=VECTOR('',#24732,10.);
#3767=VECTOR('',#24735,10.);
#3768=VECTOR('',#24736,10.);
#3769=VECTOR('',#24737,10.);
#3770=VECTOR('',#24740,10.);
#3771=VECTOR('',#24741,10.);
#3772=VECTOR('',#24756,10.);
#3773=VECTOR('',#24759,10.);
#3774=VECTOR('',#24764,10.);
#3775=VECTOR('',#24769,10.);
#3776=VECTOR('',#24774,10.);
#3777=VECTOR('',#24779,10.);
#3778=VECTOR('',#24782,10.);
#3779=VECTOR('',#24783,10.);
#3780=VECTOR('',#24784,10.);
#3781=VECTOR('',#24787,10.);
#3782=VECTOR('',#24788,10.);
#3783=VECTOR('',#24803,10.);
#3784=VECTOR('',#24806,10.);
#3785=VECTOR('',#24811,10.);
#3786=VECTOR('',#24814,10.);
#3787=VECTOR('',#24817,10.);
#3788=VECTOR('',#24822,10.);
#3789=VECTOR('',#24827,10.);
#3790=VECTOR('',#24832,10.);
#3791=VECTOR('',#24833,10.);
#3792=VECTOR('',#24836,10.);
#3793=VECTOR('',#24839,10.);
#3794=VECTOR('',#24844,10.);
#3795=VECTOR('',#24849,10.);
#3796=VECTOR('',#24850,10.);
#3797=VECTOR('',#24851,10.);
#3798=VECTOR('',#24854,10.);
#3799=VECTOR('',#24857,10.);
#3800=VECTOR('',#24862,10.);
#3801=VECTOR('',#24867,10.);
#3802=VECTOR('',#24870,10.);
#3803=VECTOR('',#24873,10.);
#3804=VECTOR('',#24878,10.);
#3805=VECTOR('',#24883,10.);
#3806=VECTOR('',#24888,10.);
#3807=VECTOR('',#24889,10.);
#3808=VECTOR('',#24892,10.);
#3809=VECTOR('',#24895,10.);
#3810=VECTOR('',#24900,10.);
#3811=VECTOR('',#24905,10.);
#3812=VECTOR('',#24906,10.);
#3813=VECTOR('',#24907,10.);
#3814=VECTOR('',#24910,10.);
#3815=VECTOR('',#24913,10.);
#3816=VECTOR('',#24918,10.);
#3817=VECTOR('',#24951,10.);
#3818=VECTOR('',#24952,10.);
#3819=VECTOR('',#24957,10.);
#3820=VECTOR('',#24958,10.);
#3821=VECTOR('',#24961,10.);
#3822=VECTOR('',#24962,10.);
#3823=VECTOR('',#24975,10.);
#3824=VECTOR('',#24976,10.);
#3825=VECTOR('',#24979,10.);
#3826=VECTOR('',#24980,10.);
#3827=VECTOR('',#24985,10.);
#3828=VECTOR('',#24986,10.);
#3829=VECTOR('',#24999,10.);
#3830=VECTOR('',#25000,10.);
#3831=VECTOR('',#25005,10.);
#3832=VECTOR('',#25006,10.);
#3833=VECTOR('',#25017,10.);
#3834=VECTOR('',#25018,10.);
#3835=VECTOR('',#25021,10.);
#3836=VECTOR('',#25022,10.);
#3837=VECTOR('',#25043,10.);
#3838=VECTOR('',#25044,10.);
#3839=VECTOR('',#25055,10.);
#3840=VECTOR('',#25056,10.);
#3841=VECTOR('',#25059,10.);
#3842=VECTOR('',#25060,10.);
#3843=VECTOR('',#25073,10.);
#3844=VECTOR('',#25074,10.);
#3845=VECTOR('',#25077,10.);
#3846=VECTOR('',#25078,10.);
#3847=VECTOR('',#25083,10.);
#3848=VECTOR('',#25084,10.);
#3849=VECTOR('',#25093,10.);
#3850=VECTOR('',#25094,10.);
#3851=VECTOR('',#25099,10.);
#3852=VECTOR('',#25100,10.);
#3853=VECTOR('',#25103,10.);
#3854=VECTOR('',#25104,10.);
#3855=VECTOR('',#25119,10.);
#3856=VECTOR('',#25122,10.);
#3857=VECTOR('',#25129,10.);
#3858=VECTOR('',#25132,10.);
#3859=VECTOR('',#25139,10.);
#3860=VECTOR('',#25142,10.);
#3861=VECTOR('',#25145,10.);
#3862=VECTOR('',#25148,10.);
#3863=VECTOR('',#25149,10.);
#3864=VECTOR('',#25152,10.);
#3865=VECTOR('',#25165,5.7528);
#3866=VECTOR('',#25180,12.24);
#3867=VECTOR('',#25209,1.3);
#3868=VECTOR('',#25222,1.3);
#3869=VECTOR('',#25227,0.8);
#3870=VECTOR('',#25230,10.);
#3871=VECTOR('',#25235,10.);
#3872=VECTOR('',#25236,0.8);
#3873=VECTOR('',#25239,0.8);
#3874=VECTOR('',#25240,10.);
#3875=VECTOR('',#25251,10.);
#3876=VECTOR('',#25252,0.8);
#3877=VECTOR('',#25253,10.);
#3878=VECTOR('',#25258,10.);
#3879=VECTOR('',#25261,10.);
#3880=VECTOR('',#25266,10.);
#3881=VECTOR('',#25335,4.075);
#3882=VECTOR('',#25340,3.975);
#3883=VECTOR('',#25353,5.5488);
#3884=VECTOR('',#25364,5.712);
#3885=VECTOR('',#25371,5.4672);
#3886=VECTOR('',#25378,10.);
#3887=VECTOR('',#25379,10.);
#3888=VECTOR('',#25380,10.);
#3889=VECTOR('',#25383,10.);
#3890=VECTOR('',#25384,10.);
#3891=VECTOR('',#25385,10.);
#3892=VECTOR('',#25388,10.);
#3893=VECTOR('',#25389,10.);
#3894=VECTOR('',#25390,10.);
#3895=VECTOR('',#25393,10.);
#3896=VECTOR('',#25394,10.);
#3897=VECTOR('',#25395,10.);
#3898=VECTOR('',#25398,10.);
#3899=VECTOR('',#25399,10.);
#3900=VECTOR('',#25400,10.);
#3901=VECTOR('',#25403,10.);
#3902=VECTOR('',#25404,10.);
#3903=VECTOR('',#25405,10.);
#3904=VECTOR('',#25408,10.);
#3905=VECTOR('',#25409,10.);
#3906=VECTOR('',#25410,10.);
#3907=VECTOR('',#25413,10.);
#3908=VECTOR('',#25414,10.);
#3909=VECTOR('',#25415,10.);
#3910=VECTOR('',#25418,10.);
#3911=VECTOR('',#25419,10.);
#3912=VECTOR('',#25420,10.);
#3913=VECTOR('',#25423,10.);
#3914=VECTOR('',#25424,10.);
#3915=VECTOR('',#25425,10.);
#3916=VECTOR('',#25428,10.);
#3917=VECTOR('',#25429,10.);
#3918=VECTOR('',#25430,10.);
#3919=VECTOR('',#25433,10.);
#3920=VECTOR('',#25434,10.);
#3921=VECTOR('',#25435,10.);
#3922=VECTOR('',#25438,10.);
#3923=VECTOR('',#25439,10.);
#3924=VECTOR('',#25440,10.);
#3925=VECTOR('',#25443,10.);
#3926=VECTOR('',#25444,10.);
#3927=VECTOR('',#25445,10.);
#3928=VECTOR('',#25448,10.);
#3929=VECTOR('',#25449,10.);
#3930=VECTOR('',#25450,10.);
#3931=VECTOR('',#25453,10.);
#3932=VECTOR('',#25454,10.);
#3933=VECTOR('',#25455,10.);
#3934=VECTOR('',#25458,10.);
#3935=VECTOR('',#25463,10.);
#3936=VECTOR('',#25466,10.);
#3937=VECTOR('',#25467,10.);
#3938=VECTOR('',#25470,10.);
#3939=VECTOR('',#25471,10.);
#3940=VECTOR('',#25472,10.);
#3941=VECTOR('',#25475,10.);
#3942=VECTOR('',#25480,10.);
#3943=VECTOR('',#25483,10.);
#3944=VECTOR('',#25484,10.);
#3945=VECTOR('',#25487,10.);
#3946=VECTOR('',#25488,10.);
#3947=VECTOR('',#25489,10.);
#3948=VECTOR('',#25492,10.);
#3949=VECTOR('',#25497,10.);
#3950=VECTOR('',#25500,10.);
#3951=VECTOR('',#25501,10.);
#3952=VECTOR('',#25504,10.);
#3953=VECTOR('',#25505,10.);
#3954=VECTOR('',#25506,10.);
#3955=VECTOR('',#25509,10.);
#3956=VECTOR('',#25514,10.);
#3957=VECTOR('',#25517,10.);
#3958=VECTOR('',#25518,10.);
#3959=VECTOR('',#25521,10.);
#3960=VECTOR('',#25522,10.);
#3961=VECTOR('',#25523,10.);
#3962=VECTOR('',#25526,10.);
#3963=VECTOR('',#25531,10.);
#3964=VECTOR('',#25534,10.);
#3965=VECTOR('',#25535,10.);
#3966=VECTOR('',#25538,10.);
#3967=VECTOR('',#25539,10.);
#3968=VECTOR('',#25540,10.);
#3969=VECTOR('',#25543,10.);
#3970=VECTOR('',#25548,10.);
#3971=VECTOR('',#25551,10.);
#3972=VECTOR('',#25552,10.);
#3973=VECTOR('',#25555,10.);
#3974=VECTOR('',#25556,10.);
#3975=VECTOR('',#25557,10.);
#3976=VECTOR('',#25560,10.);
#3977=VECTOR('',#25565,10.);
#3978=VECTOR('',#25568,10.);
#3979=VECTOR('',#25569,10.);
#3980=VECTOR('',#25572,10.);
#3981=VECTOR('',#25573,10.);
#3982=VECTOR('',#25574,10.);
#3983=VECTOR('',#25577,10.);
#3984=VECTOR('',#25582,10.);
#3985=VECTOR('',#25585,10.);
#3986=VECTOR('',#25586,10.);
#3987=VECTOR('',#25589,10.);
#3988=VECTOR('',#25590,10.);
#3989=VECTOR('',#25591,10.);
#3990=VECTOR('',#25594,10.);
#3991=VECTOR('',#25599,10.);
#3992=VECTOR('',#25602,10.);
#3993=VECTOR('',#25603,10.);
#3994=VECTOR('',#25606,10.);
#3995=VECTOR('',#25607,10.);
#3996=VECTOR('',#25608,10.);
#3997=VECTOR('',#25611,10.);
#3998=VECTOR('',#25616,10.);
#3999=VECTOR('',#25619,10.);
#4000=VECTOR('',#25620,10.);
#4001=VECTOR('',#25623,10.);
#4002=VECTOR('',#25624,10.);
#4003=VECTOR('',#25625,10.);
#4004=VECTOR('',#25628,10.);
#4005=VECTOR('',#25633,10.);
#4006=VECTOR('',#25636,10.);
#4007=VECTOR('',#25637,10.);
#4008=VECTOR('',#25640,10.);
#4009=VECTOR('',#25641,10.);
#4010=VECTOR('',#25642,10.);
#4011=VECTOR('',#25645,10.);
#4012=VECTOR('',#25650,10.);
#4013=VECTOR('',#25653,10.);
#4014=VECTOR('',#25654,10.);
#4015=VECTOR('',#25657,10.);
#4016=VECTOR('',#25658,10.);
#4017=VECTOR('',#25659,10.);
#4018=VECTOR('',#25662,10.);
#4019=VECTOR('',#25667,10.);
#4020=VECTOR('',#25670,10.);
#4021=VECTOR('',#25671,10.);
#4022=VECTOR('',#25672,10.);
#4023=VECTOR('',#25675,10.);
#4024=VECTOR('',#25676,10.);
#4025=VECTOR('',#25679,10.);
#4026=VECTOR('',#25690,2.448);
#4027=VECTOR('',#25695,3.22275);
#4028=VECTOR('',#25700,3.22275);
#4029=VECTOR('',#25703,3.22275);
#4030=VECTOR('',#25706,3.22275);
#4031=VECTOR('',#25709,3.22275);
#4032=VECTOR('',#25712,3.22275);
#4033=VECTOR('',#25715,3.22275);
#4034=VECTOR('',#25718,3.22275);
#4035=VECTOR('',#25721,3.22275);
#4036=VECTOR('',#25724,3.22275);
#4037=VECTOR('',#25727,3.22275);
#4038=VECTOR('',#25730,3.22275);
#4039=VECTOR('',#25733,3.22275);
#4040=VECTOR('',#25736,3.22275);
#4041=VECTOR('',#25739,3.22275);
#4042=VECTOR('',#25742,3.22275);
#4043=VECTOR('',#25745,3.22275);
#4044=VECTOR('',#25748,3.22275);
#4045=VECTOR('',#25751,3.22275);
#4046=VECTOR('',#25754,3.22275);
#4047=VECTOR('',#25757,3.22275);
#4048=VECTOR('',#25760,3.22275);
#4049=VECTOR('',#25763,3.22275);
#4050=VECTOR('',#25766,3.22275);
#4051=VECTOR('',#25769,3.22275);
#4052=VECTOR('',#25772,3.22275);
#4053=VECTOR('',#25775,3.22275);
#4054=VECTOR('',#25778,3.22275);
#4055=VECTOR('',#25781,3.22275);
#4056=VECTOR('',#25784,3.22275);
#4057=VECTOR('',#25787,3.22275);
#4058=VECTOR('',#25790,3.22275);
#4059=VECTOR('',#25793,3.22275);
#4060=VECTOR('',#25796,3.22275);
#4061=VECTOR('',#25799,3.22275);
#4062=VECTOR('',#25802,3.22275);
#4063=VECTOR('',#25805,3.22275);
#4064=VECTOR('',#25808,3.22275);
#4065=VECTOR('',#25811,3.22275);
#4066=VECTOR('',#25826,1.02);
#4067=VECTOR('',#25849,3.6736);
#4068=VECTOR('',#25852,3.5);
#4069=VECTOR('',#25859,3.);
#4070=VECTOR('',#25868,3.95);
#4071=VECTOR('',#25877,2.448);
#4072=VECTOR('',#25880,2.244);
#4073=VECTOR('',#25895,10.);
#4074=VECTOR('',#25904,10.);
#4075=VECTOR('',#25905,10.);
#4076=VECTOR('',#25914,10.);
#4077=VECTOR('',#25915,10.);
#4078=VECTOR('',#25924,10.);
#4079=VECTOR('',#25933,10.);
#4080=VECTOR('',#25934,10.);
#4081=VECTOR('',#25939,10.);
#4082=VECTOR('',#25942,10.);
#4083=VECTOR('',#25945,10.);
#4084=VECTOR('',#25946,10.);
#4085=VECTOR('',#25947,10.);
#4086=VECTOR('',#25952,10.);
#4087=VECTOR('',#25957,10.);
#4088=VECTOR('',#25960,10.);
#4089=VECTOR('',#25963,10.);
#4090=VECTOR('',#25966,10.);
#4091=VECTOR('',#25969,10.);
#4092=VECTOR('',#25972,10.);
#4093=VECTOR('',#25973,10.);
#4094=VECTOR('',#25974,10.);
#4095=VECTOR('',#25975,10.);
#4096=VECTOR('',#25976,10.);
#4097=VECTOR('',#25977,10.);
#4098=VECTOR('',#25982,10.);
#4099=VECTOR('',#25987,10.);
#4100=VECTOR('',#25992,10.);
#4101=VECTOR('',#25997,10.);
#4102=VECTOR('',#25998,10.);
#4103=VECTOR('',#26003,10.);
#4104=VECTOR('',#26006,10.);
#4105=VECTOR('',#26009,10.);
#4106=VECTOR('',#26014,10.);
#4107=VECTOR('',#26015,10.);
#4108=VECTOR('',#26016,10.);
#4109=VECTOR('',#26021,10.);
#4110=VECTOR('',#26022,10.);
#4111=VECTOR('',#26025,10.);
#4112=VECTOR('',#26028,10.);
#4113=VECTOR('',#26031,10.);
#4114=VECTOR('',#26032,10.);
#4115=VECTOR('',#26033,10.);
#4116=VECTOR('',#26036,10.);
#4117=VECTOR('',#26037,10.);
#4118=VECTOR('',#26040,10.);
#4119=VECTOR('',#26043,10.);
#4120=VECTOR('',#26044,10.);
#4121=VECTOR('',#26045,10.);
#4122=VECTOR('',#26046,10.);
#4123=VECTOR('',#26047,10.);
#4124=VECTOR('',#26050,10.);
#4125=VECTOR('',#26053,10.);
#4126=VECTOR('',#26068,10.);
#4127=VECTOR('',#26073,10.);
#4128=VECTOR('',#26078,10.);
#4129=VECTOR('',#26079,10.);
#4130=VECTOR('',#26084,10.);
#4131=VECTOR('',#26087,10.);
#4132=VECTOR('',#26090,10.);
#4133=VECTOR('',#26093,10.);
#4134=VECTOR('',#26104,10.);
#4135=VECTOR('',#26105,10.);
#4136=VECTOR('',#26106,10.);
#4137=VECTOR('',#26107,10.);
#4138=VECTOR('',#26110,10.);
#4139=VECTOR('',#26115,10.);
#4140=VECTOR('',#26116,10.);
#4141=VECTOR('',#26117,10.);
#4142=VECTOR('',#26118,10.);
#4143=VECTOR('',#26119,10.);
#4144=VECTOR('',#26120,10.);
#4145=VECTOR('',#26121,10.);
#4146=VECTOR('',#26124,10.);
#4147=VECTOR('',#26131,10.);
#4148=VECTOR('',#26132,10.);
#4149=VECTOR('',#26133,10.);
#4150=VECTOR('',#26146,10.);
#4151=VECTOR('',#26149,10.);
#4152=VECTOR('',#26152,10.);
#4153=VECTOR('',#26155,10.);
#4154=VECTOR('',#26156,10.);
#4155=VECTOR('',#26165,10.);
#4156=VECTOR('',#26166,10.);
#4157=VECTOR('',#26169,10.);
#4158=VECTOR('',#26172,10.);
#4159=VECTOR('',#26175,10.);
#4160=VECTOR('',#26176,10.);
#4161=VECTOR('',#26179,10.);
#4162=VECTOR('',#26182,10.);
#4163=VECTOR('',#26197,4.05);
#4164=VECTOR('',#26204,10.);
#4165=VECTOR('',#26217,10.);
#4166=VECTOR('',#26224,10.);
#4167=VECTOR('',#26227,10.);
#4168=VECTOR('',#26232,10.);
#4169=VECTOR('',#26235,10.);
#4170=VECTOR('',#26246,10.);
#4171=VECTOR('',#26257,10.);
#4172=VECTOR('',#26262,10.);
#4173=VECTOR('',#26267,10.);
#4174=VECTOR('',#26276,10.);
#4175=VECTOR('',#26281,1.25);
#4176=VECTOR('',#26282,10.);
#4177=VECTOR('',#26285,10.);
#4178=VECTOR('',#26286,10.);
#4179=VECTOR('',#26289,10.);
#4180=VECTOR('',#26290,10.);
#4181=VECTOR('',#26293,10.);
#4182=VECTOR('',#26298,10.);
#4183=VECTOR('',#26299,10.);
#4184=VECTOR('',#26300,10.);
#4185=VECTOR('',#26305,1.5);
#4186=VECTOR('',#26308,10.);
#4187=VECTOR('',#26309,10.);
#4188=VECTOR('',#26316,10.);
#4189=VECTOR('',#26325,10.);
#4190=VECTOR('',#26334,10.);
#4191=VECTOR('',#26337,10.);
#4192=VECTOR('',#26344,10.);
#4193=VECTOR('',#26347,10.);
#4194=VECTOR('',#26350,10.);
#4195=VECTOR('',#26351,10.);
#4196=VECTOR('',#26352,10.);
#4197=VECTOR('',#26357,10.);
#4198=VECTOR('',#26374,10.);
#4199=VECTOR('',#26377,10.);
#4200=VECTOR('',#26380,10.);
#4201=VECTOR('',#26385,1.25);
#4202=VECTOR('',#26400,1.5);
#4203=VECTOR('',#26403,10.);
#4204=VECTOR('',#26404,10.);
#4205=VECTOR('',#26417,10.);
#4206=VECTOR('',#26422,10.);
#4207=VECTOR('',#26425,10.);
#4208=VECTOR('',#26428,10.);
#4209=VECTOR('',#26431,10.);
#4210=VECTOR('',#26434,10.);
#4211=VECTOR('',#26435,10.);
#4212=VECTOR('',#26436,10.);
#4213=VECTOR('',#26437,10.);
#4214=VECTOR('',#26442,10.);
#4215=VECTOR('',#26445,10.);
#4216=VECTOR('',#26456,10.);
#4217=VECTOR('',#26467,10.);
#4218=VECTOR('',#26468,10.);
#4219=VECTOR('',#26473,10.);
#4220=VECTOR('',#26474,10.);
#4221=VECTOR('',#26475,10.);
#4222=VECTOR('',#26478,10.);
#4223=VECTOR('',#26479,10.);
#4224=VECTOR('',#26480,10.);
#4225=VECTOR('',#26481,10.);
#4226=VECTOR('',#26482,10.);
#4227=VECTOR('',#26483,10.);
#4228=VECTOR('',#26484,10.);
#4229=VECTOR('',#26485,10.);
#4230=VECTOR('',#26486,10.);
#4231=VECTOR('',#26487,10.);
#4232=VECTOR('',#26488,10.);
#4233=VECTOR('',#26489,10.);
#4234=VECTOR('',#26490,10.);
#4235=VECTOR('',#26491,10.);
#4236=VECTOR('',#26492,10.);
#4237=VECTOR('',#26493,10.);
#4238=VECTOR('',#26494,10.);
#4239=VECTOR('',#26495,10.);
#4240=VECTOR('',#26496,10.);
#4241=VECTOR('',#26499,10.);
#4242=VECTOR('',#26500,10.);
#4243=VECTOR('',#26501,10.);
#4244=VECTOR('',#26510,10.);
#4245=VECTOR('',#26513,10.);
#4246=VECTOR('',#26526,10.);
#4247=VECTOR('',#26527,10.);
#4248=VECTOR('',#26530,10.);
#4249=VECTOR('',#26531,10.);
#4250=VECTOR('',#26532,10.);
#4251=VECTOR('',#26537,10.);
#4252=VECTOR('',#26540,10.);
#4253=VECTOR('',#26541,10.);
#4254=VECTOR('',#26546,10.);
#4255=VECTOR('',#26549,10.);
#4256=VECTOR('',#26550,10.);
#4257=VECTOR('',#26553,10.);
#4258=VECTOR('',#26560,10.);
#4259=VECTOR('',#26569,10.);
#4260=VECTOR('',#26586,10.);
#4261=VECTOR('',#26591,10.);
#4262=VECTOR('',#26592,10.);
#4263=VECTOR('',#26593,10.);
#4264=VECTOR('',#26594,10.);
#4265=VECTOR('',#26595,10.);
#4266=VECTOR('',#26596,10.);
#4267=VECTOR('',#26601,10.);
#4268=VECTOR('',#26616,1.5);
#4269=VECTOR('',#26621,10.);
#4270=VECTOR('',#26622,10.);
#4271=VECTOR('',#26623,10.);
#4272=VECTOR('',#26624,10.);
#4273=VECTOR('',#26625,10.);
#4274=VECTOR('',#26646,1.25);
#4275=VECTOR('',#26649,10.);
#4276=VECTOR('',#26654,10.);
#4277=VECTOR('',#26665,10.);
#4278=VECTOR('',#26668,10.);
#4279=VECTOR('',#26675,10.);
#4280=VECTOR('',#26678,10.);
#4281=VECTOR('',#26679,10.);
#4282=VECTOR('',#26680,10.);
#4283=VECTOR('',#26685,10.);
#4284=VECTOR('',#26688,10.);
#4285=VECTOR('',#26689,10.);
#4286=VECTOR('',#26690,10.);
#4287=VECTOR('',#26695,10.);
#4288=VECTOR('',#26698,10.);
#4289=VECTOR('',#26699,10.);
#4290=VECTOR('',#26704,10.);
#4291=VECTOR('',#26709,10.);
#4292=VECTOR('',#26710,10.);
#4293=VECTOR('',#26713,10.);
#4294=VECTOR('',#26714,10.);
#4295=VECTOR('',#26719,10.);
#4296=VECTOR('',#26724,10.);
#4297=VECTOR('',#26725,10.);
#4298=VECTOR('',#26728,10.);
#4299=VECTOR('',#26729,10.);
#4300=VECTOR('',#26734,10.);
#4301=VECTOR('',#26739,10.);
#4302=VECTOR('',#26740,10.);
#4303=VECTOR('',#26743,10.);
#4304=VECTOR('',#26744,10.);
#4305=VECTOR('',#26749,10.);
#4306=VECTOR('',#26754,10.);
#4307=VECTOR('',#26755,10.);
#4308=VECTOR('',#26758,10.);
#4309=VECTOR('',#26759,10.);
#4310=VECTOR('',#26770,10.);
#4311=VECTOR('',#26773,10.);
#4312=VECTOR('',#26776,10.);
#4313=VECTOR('',#26779,10.);
#4314=VECTOR('',#26782,10.);
#4315=VECTOR('',#26785,10.);
#4316=VECTOR('',#26788,10.);
#4317=VECTOR('',#26791,10.);
#4318=VECTOR('',#26802,0.6528);
#4319=VECTOR('',#26815,0.6528);
#4320=VECTOR('',#26820,0.4896);
#4321=VECTOR('',#26839,10.);
#4322=VECTOR('',#26842,10.);
#4323=VECTOR('',#26851,10.);
#4324=VECTOR('',#26852,10.);
#4325=VECTOR('',#26853,10.);
#4326=VECTOR('',#26854,10.);
#4327=VECTOR('',#26879,10.);
#4328=VECTOR('',#26892,10.);
#4329=VECTOR('',#26893,10.);
#4330=VECTOR('',#26894,10.);
#4331=VECTOR('',#26895,10.);
#4332=VECTOR('',#26896,10.);
#4333=VECTOR('',#26899,10.);
#4334=VECTOR('',#26900,10.);
#4335=VECTOR('',#26901,10.);
#4336=VECTOR('',#26902,10.);
#4337=VECTOR('',#26911,10.);
#4338=VECTOR('',#26912,10.);
#4339=VECTOR('',#26917,10.);
#4340=VECTOR('',#26924,10.);
#4341=VECTOR('',#26935,10.);
#4342=VECTOR('',#26936,10.);
#4343=VECTOR('',#26937,10.);
#4344=VECTOR('',#26964,1.25);
#4345=VECTOR('',#26967,10.);
#4346=VECTOR('',#26970,10.);
#4347=VECTOR('',#26973,10.);
#4348=VECTOR('',#26976,10.);
#4349=VECTOR('',#26977,10.);
#4350=VECTOR('',#26980,10.);
#4351=VECTOR('',#26983,10.);
#4352=VECTOR('',#26996,10.);
#4353=VECTOR('',#26997,10.);
#4354=VECTOR('',#27002,10.);
#4355=VECTOR('',#27003,10.);
#4356=VECTOR('',#27006,10.);
#4357=VECTOR('',#27009,10.);
#4358=VECTOR('',#27010,10.);
#4359=VECTOR('',#27013,10.);
#4360=VECTOR('',#27014,10.);
#4361=VECTOR('',#27015,10.);
#4362=VECTOR('',#27016,10.);
#4363=VECTOR('',#27021,10.);
#4364=VECTOR('',#27026,10.);
#4365=VECTOR('',#27033,10.);
#4366=VECTOR('',#27042,10.);
#4367=VECTOR('',#27045,10.);
#4368=VECTOR('',#27048,10.);
#4369=VECTOR('',#27051,10.);
#4370=VECTOR('',#27052,10.);
#4371=VECTOR('',#27055,10.);
#4372=VECTOR('',#27056,10.);
#4373=VECTOR('',#27057,10.);
#4374=VECTOR('',#27058,10.);
#4375=VECTOR('',#27061,10.);
#4376=VECTOR('',#27062,10.);
#4377=VECTOR('',#27073,10.);
#4378=VECTOR('',#27074,10.);
#4379=VECTOR('',#27077,10.);
#4380=VECTOR('',#27084,10.);
#4381=VECTOR('',#27085,10.);
#4382=VECTOR('',#27090,10.);
#4383=VECTOR('',#27093,10.);
#4384=VECTOR('',#27096,10.);
#4385=VECTOR('',#27101,10.);
#4386=VECTOR('',#27102,10.);
#4387=VECTOR('',#27103,10.);
#4388=VECTOR('',#27110,10.);
#4389=VECTOR('',#27115,10.);
#4390=VECTOR('',#27116,10.);
#4391=VECTOR('',#27117,10.);
#4392=VECTOR('',#27124,10.);
#4393=VECTOR('',#27149,10.);
#4394=VECTOR('',#27152,10.);
#4395=VECTOR('',#27165,10.);
#4396=VECTOR('',#27166,10.);
#4397=VECTOR('',#27167,10.);
#4398=VECTOR('',#27170,10.);
#4399=VECTOR('',#27179,10.);
#4400=VECTOR('',#27184,10.);
#4401=VECTOR('',#27185,10.);
#4402=VECTOR('',#27186,10.);
#4403=VECTOR('',#27189,10.);
#4404=VECTOR('',#27192,10.);
#4405=VECTOR('',#27193,10.);
#4406=VECTOR('',#27194,10.);
#4407=VECTOR('',#27197,10.);
#4408=VECTOR('',#27200,10.);
#4409=VECTOR('',#27203,10.);
#4410=VECTOR('',#27206,10.);
#4411=VECTOR('',#27207,10.);
#4412=VECTOR('',#27208,10.);
#4413=VECTOR('',#27211,10.);
#4414=VECTOR('',#27222,1.5);
#4415=VECTOR('',#27225,10.);
#4416=VECTOR('',#27230,10.);
#4417=VECTOR('',#27237,10.);
#4418=VECTOR('',#27242,10.);
#4419=VECTOR('',#27247,10.);
#4420=VECTOR('',#27248,10.);
#4421=VECTOR('',#27251,10.);
#4422=VECTOR('',#27256,10.);
#4423=VECTOR('',#27261,10.);
#4424=VECTOR('',#27262,10.);
#4425=VECTOR('',#27265,10.);
#4426=VECTOR('',#27270,10.);
#4427=VECTOR('',#27275,10.);
#4428=VECTOR('',#27276,10.);
#4429=VECTOR('',#27279,10.);
#4430=VECTOR('',#27284,10.);
#4431=VECTOR('',#27285,10.);
#4432=VECTOR('',#27288,10.);
#4433=VECTOR('',#27291,10.);
#4434=VECTOR('',#27306,10.);
#4435=VECTOR('',#27307,10.);
#4436=VECTOR('',#27310,10.);
#4437=VECTOR('',#27311,10.);
#4438=VECTOR('',#27336,10.);
#4439=VECTOR('',#27341,10.);
#4440=VECTOR('',#27358,4.3248);
#4441=VECTOR('',#27393,10.404);
#4442=VECTOR('',#27404,11.22);
#4443=VECTOR('',#27409,10.);
#4444=VECTOR('',#27412,10.);
#4445=VECTOR('',#27425,11.832);
#4446=VECTOR('',#27438,10.);
#4447=VECTOR('',#27441,10.);
#4448=VECTOR('',#27446,10.);
#4449=VECTOR('',#27447,10.);
#4450=VECTOR('',#27452,10.);
#4451=VECTOR('',#27453,10.);
#4452=VECTOR('',#27458,10.);
#4453=VECTOR('',#27459,10.);
#4454=VECTOR('',#27462,10.);
#4455=VECTOR('',#27463,10.);
#4456=VECTOR('',#27466,10.);
#4457=VECTOR('',#27469,10.);
#4458=VECTOR('',#27470,10.);
#4459=VECTOR('',#27471,10.);
#4460=VECTOR('',#27472,10.);
#4461=VECTOR('',#27475,10.);
#4462=VECTOR('',#27476,10.);
#4463=VECTOR('',#27477,10.);
#4464=VECTOR('',#27480,10.);
#4465=VECTOR('',#27481,10.);
#4466=VECTOR('',#27484,10.);
#4467=VECTOR('',#27485,10.);
#4468=VECTOR('',#27488,10.);
#4469=VECTOR('',#27493,10.);
#4470=VECTOR('',#27502,10.);
#4471=VECTOR('',#27505,10.);
#4472=VECTOR('',#27510,10.);
#4473=VECTOR('',#27513,10.);
#4474=VECTOR('',#27518,10.);
#4475=VECTOR('',#27521,10.);
#4476=VECTOR('',#27526,10.);
#4477=VECTOR('',#27529,10.);
#4478=VECTOR('',#27548,10.);
#4479=VECTOR('',#27551,10.);
#4480=VECTOR('',#27554,10.);
#4481=VECTOR('',#27555,10.);
#4482=VECTOR('',#27558,10.);
#4483=VECTOR('',#27563,10.);
#4484=VECTOR('',#27564,10.);
#4485=VECTOR('',#27573,10.);
#4486=VECTOR('',#27580,10.);
#4487=VECTOR('',#27583,10.);
#4488=VECTOR('',#27590,10.);
#4489=VECTOR('',#27593,10.);
#4490=VECTOR('',#27602,10.);
#4491=VECTOR('',#27607,10.);
#4492=VECTOR('',#27616,10.);
#4493=VECTOR('',#27629,10.);
#4494=VECTOR('',#27642,10.);
#4495=VECTOR('',#27645,10.);
#4496=VECTOR('',#27656,10.);
#4497=VECTOR('',#27657,10.);
#4498=VECTOR('',#27666,10.);
#4499=VECTOR('',#27667,10.);
#4500=VECTOR('',#27670,10.);
#4501=VECTOR('',#27675,10.);
#4502=VECTOR('',#27682,10.);
#4503=VECTOR('',#27685,10.);
#4504=VECTOR('',#27696,10.);
#4505=VECTOR('',#27705,10.);
#4506=VECTOR('',#27706,10.);
#4507=VECTOR('',#27723,1.3);
#4508=VECTOR('',#27742,2.05);
#4509=VECTOR('',#27755,10.);
#4510=VECTOR('',#27768,1.3);
#4511=VECTOR('',#27787,2.05);
#4512=VECTOR('',#27800,10.);
#4513=VECTOR('',#27803,10.);
#4514=VECTOR('',#27818,2.8556);
#4515=VECTOR('',#27823,5.3856);
#4516=VECTOR('',#27832,3.2636);
#4517=VECTOR('',#27841,2.8556);
#4518=VECTOR('',#27852,3.2636);
#4519=VECTOR('',#27861,5.3856);
#4520=VECTOR('',#27876,6.2424);
#4521=VECTOR('',#27885,6.528);
#4522=VECTOR('',#27894,6.2424);
#4523=VECTOR('',#27903,6.528);
#4524=VECTOR('',#27908,6.2832);
#4525=VECTOR('',#27915,6.528);
#4526=VECTOR('',#27918,6.2832);
#4527=VECTOR('',#27923,1.55);
#4528=VECTOR('',#27932,2.3256);
#4529=VECTOR('',#27939,2.448);
#4530=VECTOR('',#27942,2.3256);
#4531=VECTOR('',#27953,1.3);
#4532=VECTOR('',#27962,1.3368);
#4533=VECTOR('',#27969,1.5);
#4534=VECTOR('',#27972,1.3368);
#4535=VECTOR('',#27985,1.0868);
#4536=VECTOR('',#27992,1.25);
#4537=VECTOR('',#27995,1.0868);
#4538=VECTOR('',#28012,2.2848);
#4539=VECTOR('',#28017,2.448);
#4540=VECTOR('',#28026,4.488);
#4541=VECTOR('',#28029,4.284);
#4542=VECTOR('',#28040,3.264);
#4543=VECTOR('',#28049,2.9376);
#4544=VECTOR('',#28058,3.264);
#4545=VECTOR('',#28061,2.9376);
#4546=VECTOR('',#28072,2.2552);
#4547=VECTOR('',#28079,2.5);
#4548=VECTOR('',#28082,2.2552);
#4549=VECTOR('',#28103,2.);
#4550=VECTOR('',#28112,3.2);
#4551=VECTOR('',#28115,3.0368);
#4552=VECTOR('',#28134,1.25);
#4553=VECTOR('',#28137,1.1276);
#4554=CYLINDRICAL_SURFACE('',#20336,14.688);
#4555=CYLINDRICAL_SURFACE('',#20339,14.688);
#4556=CYLINDRICAL_SURFACE('',#20340,2.05);
#4557=CYLINDRICAL_SURFACE('',#20341,2.05);
#4558=CYLINDRICAL_SURFACE('',#20350,3.672);
#4559=CYLINDRICAL_SURFACE('',#20356,0.6);
#4560=CYLINDRICAL_SURFACE('',#20365,0.6);
#4561=CYLINDRICAL_SURFACE('',#20371,1.632);
#4562=CYLINDRICAL_SURFACE('',#20373,0.6);
#4563=CYLINDRICAL_SURFACE('',#20386,0.6);
#4564=CYLINDRICAL_SURFACE('',#20394,0.6);
#4565=CYLINDRICAL_SURFACE('',#20396,1.632);
#4566=CYLINDRICAL_SURFACE('',#20398,0.6);
#4567=CYLINDRICAL_SURFACE('',#20411,0.6);
#4568=CYLINDRICAL_SURFACE('',#20424,0.6);
#4569=CYLINDRICAL_SURFACE('',#20427,0.6);
#4570=CYLINDRICAL_SURFACE('',#20435,0.6);
#4571=CYLINDRICAL_SURFACE('',#20437,1.632);
#4572=CYLINDRICAL_SURFACE('',#20459,2.5);
#4573=CYLINDRICAL_SURFACE('',#20466,3.672);
#4574=CYLINDRICAL_SURFACE('',#20471,0.6);
#4575=CYLINDRICAL_SURFACE('',#20477,0.6);
#4576=CYLINDRICAL_SURFACE('',#20481,2.856);
#4577=CYLINDRICAL_SURFACE('',#20484,0.6);
#4578=CYLINDRICAL_SURFACE('',#20491,0.6);
#4579=CYLINDRICAL_SURFACE('',#20496,0.6);
#4580=CYLINDRICAL_SURFACE('',#20501,0.6);
#4581=CYLINDRICAL_SURFACE('',#20507,0.6);
#4582=CYLINDRICAL_SURFACE('',#20517,0.6);
#4583=CYLINDRICAL_SURFACE('',#20522,0.6);
#4584=CYLINDRICAL_SURFACE('',#20527,0.6);
#4585=CYLINDRICAL_SURFACE('',#20528,0.6);
#4586=CYLINDRICAL_SURFACE('',#20533,0.6);
#4587=CYLINDRICAL_SURFACE('',#20538,0.6);
#4588=CYLINDRICAL_SURFACE('',#20543,0.6);
#4589=CYLINDRICAL_SURFACE('',#20550,0.6);
#4590=CYLINDRICAL_SURFACE('',#20551,0.6);
#4591=CYLINDRICAL_SURFACE('',#20562,0.6);
#4592=CYLINDRICAL_SURFACE('',#20569,0.6);
#4593=CYLINDRICAL_SURFACE('',#20574,0.6);
#4594=CYLINDRICAL_SURFACE('',#20576,0.6);
#4595=CYLINDRICAL_SURFACE('',#20588,0.6);
#4596=CYLINDRICAL_SURFACE('',#20591,0.6);
#4597=CYLINDRICAL_SURFACE('',#20593,1.632);
#4598=CYLINDRICAL_SURFACE('',#20594,0.6);
#4599=CYLINDRICAL_SURFACE('',#20600,2.5);
#4600=CYLINDRICAL_SURFACE('',#20607,0.6);
#4601=CYLINDRICAL_SURFACE('',#20612,0.6);
#4602=CYLINDRICAL_SURFACE('',#20617,0.6);
#4603=CYLINDRICAL_SURFACE('',#20622,0.6);
#4604=CYLINDRICAL_SURFACE('',#20623,0.6);
#4605=CYLINDRICAL_SURFACE('',#20625,0.6);
#4606=CYLINDRICAL_SURFACE('',#20631,0.6);
#4607=CYLINDRICAL_SURFACE('',#20632,0.6);
#4608=CYLINDRICAL_SURFACE('',#20633,0.6);
#4609=CYLINDRICAL_SURFACE('',#20638,0.6);
#4610=CYLINDRICAL_SURFACE('',#20643,0.6);
#4611=CYLINDRICAL_SURFACE('',#20648,0.6);
#4612=CYLINDRICAL_SURFACE('',#20653,0.6);
#4613=CYLINDRICAL_SURFACE('',#20658,0.6);
#4614=CYLINDRICAL_SURFACE('',#20663,0.6);
#4615=CYLINDRICAL_SURFACE('',#20664,0.6);
#4616=CYLINDRICAL_SURFACE('',#20666,0.6);
#4617=CYLINDRICAL_SURFACE('',#20667,0.6);
#4618=CYLINDRICAL_SURFACE('',#20672,0.6);
#4619=CYLINDRICAL_SURFACE('',#20674,0.6);
#4620=CYLINDRICAL_SURFACE('',#20692,0.6);
#4621=CYLINDRICAL_SURFACE('',#20694,0.6);
#4622=CYLINDRICAL_SURFACE('',#20695,0.6);
#4623=CYLINDRICAL_SURFACE('',#20699,1.632);
#4624=CYLINDRICAL_SURFACE('',#20701,0.6);
#4625=CYLINDRICAL_SURFACE('',#20702,0.6);
#4626=CYLINDRICAL_SURFACE('',#20703,0.6);
#4627=CYLINDRICAL_SURFACE('',#20708,0.6);
#4628=CYLINDRICAL_SURFACE('',#20712,0.6);
#4629=CYLINDRICAL_SURFACE('',#20720,0.6);
#4630=CYLINDRICAL_SURFACE('',#20727,0.6);
#4631=CYLINDRICAL_SURFACE('',#20736,0.6);
#4632=CYLINDRICAL_SURFACE('',#20739,1.632);
#4633=CYLINDRICAL_SURFACE('',#20745,0.6);
#4634=CYLINDRICAL_SURFACE('',#20759,0.6);
#4635=CYLINDRICAL_SURFACE('',#20760,0.6);
#4636=CYLINDRICAL_SURFACE('',#20761,0.6);
#4637=CYLINDRICAL_SURFACE('',#20766,1.632);
#4638=CYLINDRICAL_SURFACE('',#20767,0.6);
#4639=CYLINDRICAL_SURFACE('',#20776,0.6);
#4640=CYLINDRICAL_SURFACE('',#20777,0.6);
#4641=CYLINDRICAL_SURFACE('',#20783,0.6);
#4642=CYLINDRICAL_SURFACE('',#20784,0.6);
#4643=CYLINDRICAL_SURFACE('',#20786,0.6);
#4644=CYLINDRICAL_SURFACE('',#20792,0.6);
#4645=CYLINDRICAL_SURFACE('',#20797,0.6);
#4646=CYLINDRICAL_SURFACE('',#20802,0.6);
#4647=CYLINDRICAL_SURFACE('',#20803,0.6);
#4648=CYLINDRICAL_SURFACE('',#20804,0.6);
#4649=CYLINDRICAL_SURFACE('',#20806,0.6);
#4650=CYLINDRICAL_SURFACE('',#20808,0.6);
#4651=CYLINDRICAL_SURFACE('',#20813,0.6);
#4652=CYLINDRICAL_SURFACE('',#20818,0.6);
#4653=CYLINDRICAL_SURFACE('',#20823,0.6);
#4654=CYLINDRICAL_SURFACE('',#20828,0.6);
#4655=CYLINDRICAL_SURFACE('',#20834,0.6);
#4656=CYLINDRICAL_SURFACE('',#20836,0.6);
#4657=CYLINDRICAL_SURFACE('',#20840,0.6);
#4658=CYLINDRICAL_SURFACE('',#20841,0.6);
#4659=CYLINDRICAL_SURFACE('',#20846,0.6);
#4660=CYLINDRICAL_SURFACE('',#20849,0.6);
#4661=CYLINDRICAL_SURFACE('',#20851,0.6);
#4662=CYLINDRICAL_SURFACE('',#20853,0.6);
#4663=CYLINDRICAL_SURFACE('',#20854,0.6);
#4664=CYLINDRICAL_SURFACE('',#20859,7.5888);
#4665=CYLINDRICAL_SURFACE('',#20861,0.6);
#4666=CYLINDRICAL_SURFACE('',#20864,0.6);
#4667=CYLINDRICAL_SURFACE('',#20865,1.632);
#4668=CYLINDRICAL_SURFACE('',#20869,0.6);
#4669=CYLINDRICAL_SURFACE('',#20875,0.6);
#4670=CYLINDRICAL_SURFACE('',#20878,2.856);
#4671=CYLINDRICAL_SURFACE('',#20893,0.4);
#4672=CYLINDRICAL_SURFACE('',#20896,0.4);
#4673=CYLINDRICAL_SURFACE('',#20898,0.4);
#4674=CYLINDRICAL_SURFACE('',#20900,0.4);
#4675=CYLINDRICAL_SURFACE('',#20905,0.4);
#4676=CYLINDRICAL_SURFACE('',#20907,0.4);
#4677=CYLINDRICAL_SURFACE('',#20910,0.4);
#4678=CYLINDRICAL_SURFACE('',#20913,0.4);
#4679=CYLINDRICAL_SURFACE('',#20914,0.4);
#4680=CYLINDRICAL_SURFACE('',#20917,0.4);
#4681=CYLINDRICAL_SURFACE('',#20920,0.4);
#4682=CYLINDRICAL_SURFACE('',#20924,0.4);
#4683=CYLINDRICAL_SURFACE('',#20927,0.4);
#4684=CYLINDRICAL_SURFACE('',#20929,0.4);
#4685=CYLINDRICAL_SURFACE('',#20931,0.4);
#4686=CYLINDRICAL_SURFACE('',#20940,0.4);
#4687=CYLINDRICAL_SURFACE('',#20943,0.4);
#4688=CYLINDRICAL_SURFACE('',#20945,0.4);
#4689=CYLINDRICAL_SURFACE('',#20947,0.4);
#4690=CYLINDRICAL_SURFACE('',#20954,0.4);
#4691=CYLINDRICAL_SURFACE('',#20955,0.4);
#4692=CYLINDRICAL_SURFACE('',#20958,0.4);
#4693=CYLINDRICAL_SURFACE('',#20960,0.4);
#4694=CYLINDRICAL_SURFACE('',#20962,0.4);
#4695=CYLINDRICAL_SURFACE('',#20964,0.4);
#4696=CYLINDRICAL_SURFACE('',#20967,0.4);
#4697=CYLINDRICAL_SURFACE('',#20973,0.4);
#4698=CYLINDRICAL_SURFACE('',#20975,0.4);
#4699=CYLINDRICAL_SURFACE('',#20979,0.4);
#4700=CYLINDRICAL_SURFACE('',#20983,6.12);
#4701=CYLINDRICAL_SURFACE('',#20987,0.4);
#4702=CYLINDRICAL_SURFACE('',#20988,0.4);
#4703=CYLINDRICAL_SURFACE('',#20990,0.4);
#4704=CYLINDRICAL_SURFACE('',#20996,0.4);
#4705=CYLINDRICAL_SURFACE('',#20998,0.4);
#4706=CYLINDRICAL_SURFACE('',#21001,0.4);
#4707=CYLINDRICAL_SURFACE('',#21004,0.4);
#4708=CYLINDRICAL_SURFACE('',#21007,0.4);
#4709=CYLINDRICAL_SURFACE('',#21008,0.4);
#4710=CYLINDRICAL_SURFACE('',#21011,0.4);
#4711=CYLINDRICAL_SURFACE('',#21016,0.4);
#4712=CYLINDRICAL_SURFACE('',#21018,0.4);
#4713=CYLINDRICAL_SURFACE('',#21020,0.4);
#4714=CYLINDRICAL_SURFACE('',#21022,0.4);
#4715=CYLINDRICAL_SURFACE('',#21024,6.12);
#4716=CYLINDRICAL_SURFACE('',#21029,0.4);
#4717=CYLINDRICAL_SURFACE('',#21034,0.4);
#4718=CYLINDRICAL_SURFACE('',#21035,0.4);
#4719=CYLINDRICAL_SURFACE('',#21037,0.4);
#4720=CYLINDRICAL_SURFACE('',#21039,0.4);
#4721=CYLINDRICAL_SURFACE('',#21051,6.12);
#4722=CYLINDRICAL_SURFACE('',#21053,0.4);
#4723=CYLINDRICAL_SURFACE('',#21056,0.4);
#4724=CYLINDRICAL_SURFACE('',#21057,0.4);
#4725=CYLINDRICAL_SURFACE('',#21059,0.4);
#4726=CYLINDRICAL_SURFACE('',#21061,0.4);
#4727=CYLINDRICAL_SURFACE('',#21063,0.4);
#4728=CYLINDRICAL_SURFACE('',#21077,6.12);
#4729=CYLINDRICAL_SURFACE('',#21083,3.672);
#4730=CYLINDRICAL_SURFACE('',#21092,3.672);
#4731=CYLINDRICAL_SURFACE('',#21101,2.448);
#4732=CYLINDRICAL_SURFACE('',#21113,2.5);
#4733=CYLINDRICAL_SURFACE('',#21125,2.5);
#4734=CYLINDRICAL_SURFACE('',#21134,2.448);
#4735=CYLINDRICAL_SURFACE('',#21144,1.3);
#4736=CYLINDRICAL_SURFACE('',#21149,0.4);
#4737=CYLINDRICAL_SURFACE('',#21152,0.4);
#4738=CYLINDRICAL_SURFACE('',#21154,0.4);
#4739=CYLINDRICAL_SURFACE('',#21158,0.4);
#4740=CYLINDRICAL_SURFACE('',#21164,0.4);
#4741=CYLINDRICAL_SURFACE('',#21167,0.4);
#4742=CYLINDRICAL_SURFACE('',#21168,0.4);
#4743=CYLINDRICAL_SURFACE('',#21170,0.4);
#4744=CYLINDRICAL_SURFACE('',#21175,1.3);
#4745=CYLINDRICAL_SURFACE('',#21180,0.4);
#4746=CYLINDRICAL_SURFACE('',#21183,0.4);
#4747=CYLINDRICAL_SURFACE('',#21185,0.4);
#4748=CYLINDRICAL_SURFACE('',#21187,0.4);
#4749=CYLINDRICAL_SURFACE('',#21190,0.4);
#4750=CYLINDRICAL_SURFACE('',#21193,0.4);
#4751=CYLINDRICAL_SURFACE('',#21195,0.4);
#4752=CYLINDRICAL_SURFACE('',#21198,0.4);
#4753=CYLINDRICAL_SURFACE('',#21201,0.4);
#4754=CYLINDRICAL_SURFACE('',#21203,0.4);
#4755=CYLINDRICAL_SURFACE('',#21205,0.4);
#4756=CYLINDRICAL_SURFACE('',#21208,0.4);
#4757=CYLINDRICAL_SURFACE('',#21211,0.4);
#4758=CYLINDRICAL_SURFACE('',#21213,0.4);
#4759=CYLINDRICAL_SURFACE('',#21216,0.4);
#4760=CYLINDRICAL_SURFACE('',#21220,0.4);
#4761=CYLINDRICAL_SURFACE('',#21230,0.4);
#4762=CYLINDRICAL_SURFACE('',#21235,0.4);
#4763=CYLINDRICAL_SURFACE('',#21236,0.4);
#4764=CYLINDRICAL_SURFACE('',#21240,0.4);
#4765=CYLINDRICAL_SURFACE('',#21250,0.4);
#4766=CYLINDRICAL_SURFACE('',#21255,0.4);
#4767=CYLINDRICAL_SURFACE('',#21270,0.8);
#4768=CYLINDRICAL_SURFACE('',#21272,0.8);
#4769=CYLINDRICAL_SURFACE('',#21274,0.8);
#4770=CYLINDRICAL_SURFACE('',#21279,0.8);
#4771=CYLINDRICAL_SURFACE('',#21281,0.8);
#4772=CYLINDRICAL_SURFACE('',#21283,0.8);
#4773=CYLINDRICAL_SURFACE('',#21289,0.8);
#4774=CYLINDRICAL_SURFACE('',#21290,0.8);
#4775=CYLINDRICAL_SURFACE('',#21296,0.8);
#4776=CYLINDRICAL_SURFACE('',#21297,0.8);
#4777=CYLINDRICAL_SURFACE('',#21306,0.8);
#4778=CYLINDRICAL_SURFACE('',#21312,0.8);
#4779=CYLINDRICAL_SURFACE('',#21313,0.8);
#4780=CYLINDRICAL_SURFACE('',#21319,0.8);
#4781=CYLINDRICAL_SURFACE('',#21320,0.8);
#4782=CYLINDRICAL_SURFACE('',#21321,0.8);
#4783=CYLINDRICAL_SURFACE('',#21326,0.8);
#4784=CYLINDRICAL_SURFACE('',#21327,0.8);
#4785=CYLINDRICAL_SURFACE('',#21329,0.8);
#4786=CYLINDRICAL_SURFACE('',#21341,0.8);
#4787=CYLINDRICAL_SURFACE('',#21344,0.8);
#4788=CYLINDRICAL_SURFACE('',#21345,0.8);
#4789=CYLINDRICAL_SURFACE('',#21347,0.8);
#4790=CYLINDRICAL_SURFACE('',#21353,5.7528);
#4791=CYLINDRICAL_SURFACE('',#21361,12.24);
#4792=CYLINDRICAL_SURFACE('',#21375,1.3);
#4793=CYLINDRICAL_SURFACE('',#21381,1.3);
#4794=CYLINDRICAL_SURFACE('',#21383,0.8);
#4795=CYLINDRICAL_SURFACE('',#21386,0.8);
#4796=CYLINDRICAL_SURFACE('',#21387,0.799999999999998);
#4797=CYLINDRICAL_SURFACE('',#21393,0.8);
#4798=CYLINDRICAL_SURFACE('',#21395,0.799999999999998);
#4799=CYLINDRICAL_SURFACE('',#21397,0.8);
#4800=CYLINDRICAL_SURFACE('',#21433,3.975);
#4801=CYLINDRICAL_SURFACE('',#21442,5.712);
#4802=CYLINDRICAL_SURFACE('',#21467,4.488);
#4803=CYLINDRICAL_SURFACE('',#21472,4.488);
#4804=CYLINDRICAL_SURFACE('',#21477,4.488);
#4805=CYLINDRICAL_SURFACE('',#21482,4.488);
#4806=CYLINDRICAL_SURFACE('',#21487,4.488);
#4807=CYLINDRICAL_SURFACE('',#21492,4.488);
#4808=CYLINDRICAL_SURFACE('',#21497,4.488);
#4809=CYLINDRICAL_SURFACE('',#21502,4.488);
#4810=CYLINDRICAL_SURFACE('',#21507,4.488);
#4811=CYLINDRICAL_SURFACE('',#21512,4.488);
#4812=CYLINDRICAL_SURFACE('',#21517,4.488);
#4813=CYLINDRICAL_SURFACE('',#21522,4.488);
#4814=CYLINDRICAL_SURFACE('',#21527,4.488);
#4815=CYLINDRICAL_SURFACE('',#21535,4.488);
#4816=CYLINDRICAL_SURFACE('',#21536,2.448);
#4817=CYLINDRICAL_SURFACE('',#21538,3.22275);
#4818=CYLINDRICAL_SURFACE('',#21540,3.22275);
#4819=CYLINDRICAL_SURFACE('',#21541,3.22275);
#4820=CYLINDRICAL_SURFACE('',#21542,3.22275);
#4821=CYLINDRICAL_SURFACE('',#21543,3.22275);
#4822=CYLINDRICAL_SURFACE('',#21544,3.22275);
#4823=CYLINDRICAL_SURFACE('',#21545,3.22275);
#4824=CYLINDRICAL_SURFACE('',#21546,3.22275);
#4825=CYLINDRICAL_SURFACE('',#21547,3.22275);
#4826=CYLINDRICAL_SURFACE('',#21548,3.22275);
#4827=CYLINDRICAL_SURFACE('',#21549,3.22275);
#4828=CYLINDRICAL_SURFACE('',#21550,3.22275);
#4829=CYLINDRICAL_SURFACE('',#21551,3.22275);
#4830=CYLINDRICAL_SURFACE('',#21552,3.22275);
#4831=CYLINDRICAL_SURFACE('',#21553,3.22275);
#4832=CYLINDRICAL_SURFACE('',#21554,3.22275);
#4833=CYLINDRICAL_SURFACE('',#21555,3.22275);
#4834=CYLINDRICAL_SURFACE('',#21556,3.22275);
#4835=CYLINDRICAL_SURFACE('',#21557,3.22275);
#4836=CYLINDRICAL_SURFACE('',#21558,3.22275);
#4837=CYLINDRICAL_SURFACE('',#21559,3.22275);
#4838=CYLINDRICAL_SURFACE('',#21560,3.22275);
#4839=CYLINDRICAL_SURFACE('',#21561,3.22275);
#4840=CYLINDRICAL_SURFACE('',#21562,3.22275);
#4841=CYLINDRICAL_SURFACE('',#21563,3.22275);
#4842=CYLINDRICAL_SURFACE('',#21564,3.22275);
#4843=CYLINDRICAL_SURFACE('',#21565,3.22275);
#4844=CYLINDRICAL_SURFACE('',#21566,3.22275);
#4845=CYLINDRICAL_SURFACE('',#21567,3.22275);
#4846=CYLINDRICAL_SURFACE('',#21568,3.22275);
#4847=CYLINDRICAL_SURFACE('',#21569,3.22275);
#4848=CYLINDRICAL_SURFACE('',#21570,3.22275);
#4849=CYLINDRICAL_SURFACE('',#21571,3.22275);
#4850=CYLINDRICAL_SURFACE('',#21572,3.22275);
#4851=CYLINDRICAL_SURFACE('',#21573,3.22275);
#4852=CYLINDRICAL_SURFACE('',#21574,3.22275);
#4853=CYLINDRICAL_SURFACE('',#21575,3.22275);
#4854=CYLINDRICAL_SURFACE('',#21576,3.22275);
#4855=CYLINDRICAL_SURFACE('',#21577,3.22275);
#4856=CYLINDRICAL_SURFACE('',#21578,3.933);
#4857=CYLINDRICAL_SURFACE('',#21581,3.22275);
#4858=CYLINDRICAL_SURFACE('',#21583,1.02);
#4859=CYLINDRICAL_SURFACE('',#21598,3.);
#4860=CYLINDRICAL_SURFACE('',#21602,3.95);
#4861=CYLINDRICAL_SURFACE('',#21606,2.448);
#4862=CYLINDRICAL_SURFACE('',#21623,0.6);
#4863=CYLINDRICAL_SURFACE('',#21632,0.6);
#4864=CYLINDRICAL_SURFACE('',#21636,0.6);
#4865=CYLINDRICAL_SURFACE('',#21645,0.6);
#4866=CYLINDRICAL_SURFACE('',#21648,0.6);
#4867=CYLINDRICAL_SURFACE('',#21650,0.6);
#4868=CYLINDRICAL_SURFACE('',#21667,0.6);
#4869=CYLINDRICAL_SURFACE('',#21674,0.6);
#4870=CYLINDRICAL_SURFACE('',#21678,0.6);
#4871=CYLINDRICAL_SURFACE('',#21680,0.6);
#4872=CYLINDRICAL_SURFACE('',#21683,0.6);
#4873=CYLINDRICAL_SURFACE('',#21690,0.6);
#4874=CYLINDRICAL_SURFACE('',#21693,0.6);
#4875=CYLINDRICAL_SURFACE('',#21701,0.6);
#4876=CYLINDRICAL_SURFACE('',#21703,0.6);
#4877=CYLINDRICAL_SURFACE('',#21709,0.6);
#4878=CYLINDRICAL_SURFACE('',#21710,10.608);
#4879=CYLINDRICAL_SURFACE('',#21721,4.05);
#4880=CYLINDRICAL_SURFACE('',#21722,8.976);
#4881=CYLINDRICAL_SURFACE('',#21730,0.6);
#4882=CYLINDRICAL_SURFACE('',#21732,0.6);
#4883=CYLINDRICAL_SURFACE('',#21735,0.6);
#4884=CYLINDRICAL_SURFACE('',#21742,0.6);
#4885=CYLINDRICAL_SURFACE('',#21746,0.6);
#4886=CYLINDRICAL_SURFACE('',#21748,0.6);
#4887=CYLINDRICAL_SURFACE('',#21750,0.6);
#4888=CYLINDRICAL_SURFACE('',#21753,0.6);
#4889=CYLINDRICAL_SURFACE('',#21756,1.25);
#4890=CYLINDRICAL_SURFACE('',#21761,0.600000000000001);
#4891=CYLINDRICAL_SURFACE('',#21763,1.5);
#4892=CYLINDRICAL_SURFACE('',#21767,0.6);
#4893=CYLINDRICAL_SURFACE('',#21770,0.6);
#4894=CYLINDRICAL_SURFACE('',#21775,0.6);
#4895=CYLINDRICAL_SURFACE('',#21780,0.6);
#4896=CYLINDRICAL_SURFACE('',#21792,0.6);
#4897=CYLINDRICAL_SURFACE('',#21795,1.25);
#4898=CYLINDRICAL_SURFACE('',#21802,1.5);
#4899=CYLINDRICAL_SURFACE('',#21809,0.6);
#4900=CYLINDRICAL_SURFACE('',#21812,0.6);
#4901=CYLINDRICAL_SURFACE('',#21815,0.6);
#4902=CYLINDRICAL_SURFACE('',#21817,0.6);
#4903=CYLINDRICAL_SURFACE('',#21820,0.6);
#4904=CYLINDRICAL_SURFACE('',#21822,0.6);
#4905=CYLINDRICAL_SURFACE('',#21826,0.6);
#4906=CYLINDRICAL_SURFACE('',#21836,0.6);
#4907=CYLINDRICAL_SURFACE('',#21838,0.6);
#4908=CYLINDRICAL_SURFACE('',#21843,0.6);
#4909=CYLINDRICAL_SURFACE('',#21846,0.6);
#4910=CYLINDRICAL_SURFACE('',#21849,0.6);
#4911=CYLINDRICAL_SURFACE('',#21852,0.6);
#4912=CYLINDRICAL_SURFACE('',#21858,0.6);
#4913=CYLINDRICAL_SURFACE('',#21860,0.6);
#4914=CYLINDRICAL_SURFACE('',#21861,0.6);
#4915=CYLINDRICAL_SURFACE('',#21863,0.6);
#4916=CYLINDRICAL_SURFACE('',#21867,0.6);
#4917=CYLINDRICAL_SURFACE('',#21870,0.6);
#4918=CYLINDRICAL_SURFACE('',#21876,1.5);
#4919=CYLINDRICAL_SURFACE('',#21885,0.6);
#4920=CYLINDRICAL_SURFACE('',#21888,1.25);
#4921=CYLINDRICAL_SURFACE('',#21893,0.6);
#4922=CYLINDRICAL_SURFACE('',#21895,0.6);
#4923=CYLINDRICAL_SURFACE('',#21897,0.6);
#4924=CYLINDRICAL_SURFACE('',#21900,0.6);
#4925=CYLINDRICAL_SURFACE('',#21904,0.6);
#4926=CYLINDRICAL_SURFACE('',#21907,0.6);
#4927=CYLINDRICAL_SURFACE('',#21910,0.6);
#4928=CYLINDRICAL_SURFACE('',#21915,0.6);
#4929=CYLINDRICAL_SURFACE('',#21920,0.6);
#4930=CYLINDRICAL_SURFACE('',#21925,0.6);
#4931=CYLINDRICAL_SURFACE('',#21934,0.6);
#4932=CYLINDRICAL_SURFACE('',#21936,0.6);
#4933=CYLINDRICAL_SURFACE('',#21938,0.6);
#4934=CYLINDRICAL_SURFACE('',#21940,0.6);
#4935=CYLINDRICAL_SURFACE('',#21946,0.6528);
#4936=CYLINDRICAL_SURFACE('',#21952,0.6528);
#4937=CYLINDRICAL_SURFACE('',#21954,0.4896);
#4938=CYLINDRICAL_SURFACE('',#21963,0.6);
#4939=CYLINDRICAL_SURFACE('',#21969,0.6);
#4940=CYLINDRICAL_SURFACE('',#21972,0.6);
#4941=CYLINDRICAL_SURFACE('',#21977,0.6);
#4942=CYLINDRICAL_SURFACE('',#21979,0.6);
#4943=CYLINDRICAL_SURFACE('',#21982,0.6);
#4944=CYLINDRICAL_SURFACE('',#21988,0.6);
#4945=CYLINDRICAL_SURFACE('',#21990,0.6);
#4946=CYLINDRICAL_SURFACE('',#21992,0.6);
#4947=CYLINDRICAL_SURFACE('',#21995,0.6);
#4948=CYLINDRICAL_SURFACE('',#22002,0.6);
#4949=CYLINDRICAL_SURFACE('',#22004,0.6);
#4950=CYLINDRICAL_SURFACE('',#22005,0.6);
#4951=CYLINDRICAL_SURFACE('',#22014,1.25);
#4952=CYLINDRICAL_SURFACE('',#22023,0.6);
#4953=CYLINDRICAL_SURFACE('',#22025,0.6);
#4954=CYLINDRICAL_SURFACE('',#22032,0.6);
#4955=CYLINDRICAL_SURFACE('',#22037,0.6);
#4956=CYLINDRICAL_SURFACE('',#22050,0.6);
#4957=CYLINDRICAL_SURFACE('',#22054,0.6);
#4958=CYLINDRICAL_SURFACE('',#22058,0.6);
#4959=CYLINDRICAL_SURFACE('',#22064,0.6);
#4960=CYLINDRICAL_SURFACE('',#22070,0.6);
#4961=CYLINDRICAL_SURFACE('',#22071,0.6);
#4962=CYLINDRICAL_SURFACE('',#22073,0.6);
#4963=CYLINDRICAL_SURFACE('',#22079,0.6);
#4964=CYLINDRICAL_SURFACE('',#22083,0.6);
#4965=CYLINDRICAL_SURFACE('',#22094,0.6);
#4966=CYLINDRICAL_SURFACE('',#22097,0.6);
#4967=CYLINDRICAL_SURFACE('',#22099,0.6);
#4968=CYLINDRICAL_SURFACE('',#22101,0.6);
#4969=CYLINDRICAL_SURFACE('',#22108,1.5);
#4970=CYLINDRICAL_SURFACE('',#22140,5.712);
#4971=CYLINDRICAL_SURFACE('',#22141,5.712);
#4972=CYLINDRICAL_SURFACE('',#22163,4.3248);
#4973=CYLINDRICAL_SURFACE('',#22180,10.404);
#4974=CYLINDRICAL_SURFACE('',#22185,11.22);
#4975=CYLINDRICAL_SURFACE('',#22194,11.832);
#4976=CYLINDRICAL_SURFACE('',#22200,0.3);
#4977=CYLINDRICAL_SURFACE('',#22203,0.3);
#4978=CYLINDRICAL_SURFACE('',#22205,0.3);
#4979=CYLINDRICAL_SURFACE('',#22207,0.3);
#4980=CYLINDRICAL_SURFACE('',#22219,0.3);
#4981=CYLINDRICAL_SURFACE('',#22222,0.3);
#4982=CYLINDRICAL_SURFACE('',#22225,0.3);
#4983=CYLINDRICAL_SURFACE('',#22228,0.3);
#4984=CYLINDRICAL_SURFACE('',#22239,0.3);
#4985=CYLINDRICAL_SURFACE('',#22242,0.3);
#4986=CYLINDRICAL_SURFACE('',#22248,0.3);
#4987=CYLINDRICAL_SURFACE('',#22250,0.300092189998616);
#4988=CYLINDRICAL_SURFACE('',#22255,0.3);
#4989=CYLINDRICAL_SURFACE('',#22265,0.300092189989763);
#4990=CYLINDRICAL_SURFACE('',#22278,0.3);
#4991=CYLINDRICAL_SURFACE('',#22284,0.3);
#4992=CYLINDRICAL_SURFACE('',#22291,7.0176);
#4993=CYLINDRICAL_SURFACE('',#22300,1.224);
#4994=CYLINDRICAL_SURFACE('',#22304,1.224);
#4995=CYLINDRICAL_SURFACE('',#22312,1.3);
#4996=CYLINDRICAL_SURFACE('',#22321,2.05);
#4997=CYLINDRICAL_SURFACE('',#22333,1.3);
#4998=CYLINDRICAL_SURFACE('',#22342,2.05);
#4999=CYLINDRICAL_SURFACE('',#22348,1.224);
#5000=CYLINDRICAL_SURFACE('',#22349,1.224);
#5001=CYLINDRICAL_SURFACE('',#22355,2.8556);
#5002=CYLINDRICAL_SURFACE('',#22357,5.3856);
#5003=CYLINDRICAL_SURFACE('',#22362,3.2636);
#5004=CYLINDRICAL_SURFACE('',#22365,2.8556);
#5005=CYLINDRICAL_SURFACE('',#22370,3.2636);
#5006=CYLINDRICAL_SURFACE('',#22375,5.3856);
#5007=CYLINDRICAL_SURFACE('',#22382,6.2424);
#5008=CYLINDRICAL_SURFACE('',#22386,6.528);
#5009=CYLINDRICAL_SURFACE('',#22390,6.2424);
#5010=CYLINDRICAL_SURFACE('',#22394,6.528);
#5011=CYLINDRICAL_SURFACE('',#22398,6.528);
#5012=CYLINDRICAL_SURFACE('',#22402,1.55);
#5013=CYLINDRICAL_SURFACE('',#22408,2.448);
#5014=CYLINDRICAL_SURFACE('',#22414,1.3);
#5015=CYLINDRICAL_SURFACE('',#22421,1.5);
#5016=CYLINDRICAL_SURFACE('',#22431,1.25);
#5017=CYLINDRICAL_SURFACE('',#22442,2.448);
#5018=CYLINDRICAL_SURFACE('',#22446,4.488);
#5019=CYLINDRICAL_SURFACE('',#22452,3.264);
#5020=CYLINDRICAL_SURFACE('',#22456,2.9376);
#5021=CYLINDRICAL_SURFACE('',#22460,3.264);
#5022=CYLINDRICAL_SURFACE('',#22469,2.5);
#5023=CYLINDRICAL_SURFACE('',#22480,2.);
#5024=CYLINDRICAL_SURFACE('',#22484,3.2);
#5025=CYLINDRICAL_SURFACE('',#22494,1.25);
#5026=FACE_OUTER_BOUND('',#6183,.T.);
#5027=FACE_OUTER_BOUND('',#6184,.T.);
#5028=FACE_OUTER_BOUND('',#6185,.T.);
#5029=FACE_OUTER_BOUND('',#6191,.T.);
#5030=FACE_OUTER_BOUND('',#6192,.T.);
#5031=FACE_OUTER_BOUND('',#6197,.T.);
#5032=FACE_OUTER_BOUND('',#6198,.T.);
#5033=FACE_OUTER_BOUND('',#6199,.T.);
#5034=FACE_OUTER_BOUND('',#6200,.T.);
#5035=FACE_OUTER_BOUND('',#6201,.T.);
#5036=FACE_OUTER_BOUND('',#6202,.T.);
#5037=FACE_OUTER_BOUND('',#6203,.T.);
#5038=FACE_OUTER_BOUND('',#6204,.T.);
#5039=FACE_OUTER_BOUND('',#6205,.T.);
#5040=FACE_OUTER_BOUND('',#6206,.T.);
#5041=FACE_OUTER_BOUND('',#6207,.T.);
#5042=FACE_OUTER_BOUND('',#6208,.T.);
#5043=FACE_OUTER_BOUND('',#6209,.T.);
#5044=FACE_OUTER_BOUND('',#6210,.T.);
#5045=FACE_OUTER_BOUND('',#6211,.T.);
#5046=FACE_OUTER_BOUND('',#6212,.T.);
#5047=FACE_OUTER_BOUND('',#6213,.T.);
#5048=FACE_OUTER_BOUND('',#6214,.T.);
#5049=FACE_OUTER_BOUND('',#6215,.T.);
#5050=FACE_OUTER_BOUND('',#6216,.T.);
#5051=FACE_OUTER_BOUND('',#6217,.T.);
#5052=FACE_OUTER_BOUND('',#6218,.T.);
#5053=FACE_OUTER_BOUND('',#6219,.T.);
#5054=FACE_OUTER_BOUND('',#6220,.T.);
#5055=FACE_OUTER_BOUND('',#6221,.T.);
#5056=FACE_OUTER_BOUND('',#6222,.T.);
#5057=FACE_OUTER_BOUND('',#6223,.T.);
#5058=FACE_OUTER_BOUND('',#6224,.T.);
#5059=FACE_OUTER_BOUND('',#6225,.T.);
#5060=FACE_OUTER_BOUND('',#6226,.T.);
#5061=FACE_OUTER_BOUND('',#6227,.T.);
#5062=FACE_OUTER_BOUND('',#6228,.T.);
#5063=FACE_OUTER_BOUND('',#6229,.T.);
#5064=FACE_OUTER_BOUND('',#6230,.T.);
#5065=FACE_OUTER_BOUND('',#6231,.T.);
#5066=FACE_OUTER_BOUND('',#6232,.T.);
#5067=FACE_OUTER_BOUND('',#6233,.T.);
#5068=FACE_OUTER_BOUND('',#6234,.T.);
#5069=FACE_OUTER_BOUND('',#6235,.T.);
#5070=FACE_OUTER_BOUND('',#6236,.T.);
#5071=FACE_OUTER_BOUND('',#6237,.T.);
#5072=FACE_OUTER_BOUND('',#6238,.T.);
#5073=FACE_OUTER_BOUND('',#6239,.T.);
#5074=FACE_OUTER_BOUND('',#6240,.T.);
#5075=FACE_OUTER_BOUND('',#6241,.T.);
#5076=FACE_OUTER_BOUND('',#6242,.T.);
#5077=FACE_OUTER_BOUND('',#6243,.T.);
#5078=FACE_OUTER_BOUND('',#6244,.T.);
#5079=FACE_OUTER_BOUND('',#6245,.T.);
#5080=FACE_OUTER_BOUND('',#6246,.T.);
#5081=FACE_OUTER_BOUND('',#6247,.T.);
#5082=FACE_OUTER_BOUND('',#6248,.T.);
#5083=FACE_OUTER_BOUND('',#6249,.T.);
#5084=FACE_OUTER_BOUND('',#6250,.T.);
#5085=FACE_OUTER_BOUND('',#6251,.T.);
#5086=FACE_OUTER_BOUND('',#6252,.T.);
#5087=FACE_OUTER_BOUND('',#6253,.T.);
#5088=FACE_OUTER_BOUND('',#6254,.T.);
#5089=FACE_OUTER_BOUND('',#6255,.T.);
#5090=FACE_OUTER_BOUND('',#6256,.T.);
#5091=FACE_OUTER_BOUND('',#6257,.T.);
#5092=FACE_OUTER_BOUND('',#6258,.T.);
#5093=FACE_OUTER_BOUND('',#6259,.T.);
#5094=FACE_OUTER_BOUND('',#6260,.T.);
#5095=FACE_OUTER_BOUND('',#6261,.T.);
#5096=FACE_OUTER_BOUND('',#6262,.T.);
#5097=FACE_OUTER_BOUND('',#6263,.T.);
#5098=FACE_OUTER_BOUND('',#6264,.T.);
#5099=FACE_OUTER_BOUND('',#6265,.T.);
#5100=FACE_OUTER_BOUND('',#6266,.T.);
#5101=FACE_OUTER_BOUND('',#6267,.T.);
#5102=FACE_OUTER_BOUND('',#6268,.T.);
#5103=FACE_OUTER_BOUND('',#6269,.T.);
#5104=FACE_OUTER_BOUND('',#6270,.T.);
#5105=FACE_OUTER_BOUND('',#6271,.T.);
#5106=FACE_OUTER_BOUND('',#6272,.T.);
#5107=FACE_OUTER_BOUND('',#6273,.T.);
#5108=FACE_OUTER_BOUND('',#6274,.T.);
#5109=FACE_OUTER_BOUND('',#6275,.T.);
#5110=FACE_OUTER_BOUND('',#6276,.T.);
#5111=FACE_OUTER_BOUND('',#6277,.T.);
#5112=FACE_OUTER_BOUND('',#6278,.T.);
#5113=FACE_OUTER_BOUND('',#6279,.T.);
#5114=FACE_OUTER_BOUND('',#6280,.T.);
#5115=FACE_OUTER_BOUND('',#6281,.T.);
#5116=FACE_OUTER_BOUND('',#6282,.T.);
#5117=FACE_OUTER_BOUND('',#6283,.T.);
#5118=FACE_OUTER_BOUND('',#6284,.T.);
#5119=FACE_OUTER_BOUND('',#6285,.T.);
#5120=FACE_OUTER_BOUND('',#6286,.T.);
#5121=FACE_OUTER_BOUND('',#6287,.T.);
#5122=FACE_OUTER_BOUND('',#6288,.T.);
#5123=FACE_OUTER_BOUND('',#6289,.T.);
#5124=FACE_OUTER_BOUND('',#6290,.T.);
#5125=FACE_OUTER_BOUND('',#6291,.T.);
#5126=FACE_OUTER_BOUND('',#6292,.T.);
#5127=FACE_OUTER_BOUND('',#6293,.T.);
#5128=FACE_OUTER_BOUND('',#6294,.T.);
#5129=FACE_OUTER_BOUND('',#6295,.T.);
#5130=FACE_OUTER_BOUND('',#6296,.T.);
#5131=FACE_OUTER_BOUND('',#6297,.T.);
#5132=FACE_OUTER_BOUND('',#6298,.T.);
#5133=FACE_OUTER_BOUND('',#6299,.T.);
#5134=FACE_OUTER_BOUND('',#6300,.T.);
#5135=FACE_OUTER_BOUND('',#6301,.T.);
#5136=FACE_OUTER_BOUND('',#6302,.T.);
#5137=FACE_OUTER_BOUND('',#6303,.T.);
#5138=FACE_OUTER_BOUND('',#6304,.T.);
#5139=FACE_OUTER_BOUND('',#6305,.T.);
#5140=FACE_OUTER_BOUND('',#6306,.T.);
#5141=FACE_OUTER_BOUND('',#6307,.T.);
#5142=FACE_OUTER_BOUND('',#6308,.T.);
#5143=FACE_OUTER_BOUND('',#6309,.T.);
#5144=FACE_OUTER_BOUND('',#6310,.T.);
#5145=FACE_OUTER_BOUND('',#6311,.T.);
#5146=FACE_OUTER_BOUND('',#6312,.T.);
#5147=FACE_OUTER_BOUND('',#6313,.T.);
#5148=FACE_OUTER_BOUND('',#6314,.T.);
#5149=FACE_OUTER_BOUND('',#6315,.T.);
#5150=FACE_OUTER_BOUND('',#6323,.T.);
#5151=FACE_OUTER_BOUND('',#6324,.T.);
#5152=FACE_OUTER_BOUND('',#6325,.T.);
#5153=FACE_OUTER_BOUND('',#6326,.T.);
#5154=FACE_OUTER_BOUND('',#6327,.T.);
#5155=FACE_OUTER_BOUND('',#6328,.T.);
#5156=FACE_OUTER_BOUND('',#6329,.T.);
#5157=FACE_OUTER_BOUND('',#6330,.T.);
#5158=FACE_OUTER_BOUND('',#6331,.T.);
#5159=FACE_OUTER_BOUND('',#6332,.T.);
#5160=FACE_OUTER_BOUND('',#6333,.T.);
#5161=FACE_OUTER_BOUND('',#6334,.T.);
#5162=FACE_OUTER_BOUND('',#6335,.T.);
#5163=FACE_OUTER_BOUND('',#6336,.T.);
#5164=FACE_OUTER_BOUND('',#6337,.T.);
#5165=FACE_OUTER_BOUND('',#6338,.T.);
#5166=FACE_OUTER_BOUND('',#6339,.T.);
#5167=FACE_OUTER_BOUND('',#6340,.T.);
#5168=FACE_OUTER_BOUND('',#6341,.T.);
#5169=FACE_OUTER_BOUND('',#6342,.T.);
#5170=FACE_OUTER_BOUND('',#6343,.T.);
#5171=FACE_OUTER_BOUND('',#6344,.T.);
#5172=FACE_OUTER_BOUND('',#6345,.T.);
#5173=FACE_OUTER_BOUND('',#6346,.T.);
#5174=FACE_OUTER_BOUND('',#6347,.T.);
#5175=FACE_OUTER_BOUND('',#6348,.T.);
#5176=FACE_OUTER_BOUND('',#6349,.T.);
#5177=FACE_OUTER_BOUND('',#6350,.T.);
#5178=FACE_OUTER_BOUND('',#6351,.T.);
#5179=FACE_OUTER_BOUND('',#6352,.T.);
#5180=FACE_OUTER_BOUND('',#6353,.T.);
#5181=FACE_OUTER_BOUND('',#6354,.T.);
#5182=FACE_OUTER_BOUND('',#6355,.T.);
#5183=FACE_OUTER_BOUND('',#6356,.T.);
#5184=FACE_OUTER_BOUND('',#6357,.T.);
#5185=FACE_OUTER_BOUND('',#6358,.T.);
#5186=FACE_OUTER_BOUND('',#6359,.T.);
#5187=FACE_OUTER_BOUND('',#6360,.T.);
#5188=FACE_OUTER_BOUND('',#6361,.T.);
#5189=FACE_OUTER_BOUND('',#6362,.T.);
#5190=FACE_OUTER_BOUND('',#6363,.T.);
#5191=FACE_OUTER_BOUND('',#6364,.T.);
#5192=FACE_OUTER_BOUND('',#6365,.T.);
#5193=FACE_OUTER_BOUND('',#6366,.T.);
#5194=FACE_OUTER_BOUND('',#6367,.T.);
#5195=FACE_OUTER_BOUND('',#6368,.T.);
#5196=FACE_OUTER_BOUND('',#6369,.T.);
#5197=FACE_OUTER_BOUND('',#6370,.T.);
#5198=FACE_OUTER_BOUND('',#6371,.T.);
#5199=FACE_OUTER_BOUND('',#6372,.T.);
#5200=FACE_OUTER_BOUND('',#6373,.T.);
#5201=FACE_OUTER_BOUND('',#6374,.T.);
#5202=FACE_OUTER_BOUND('',#6375,.T.);
#5203=FACE_OUTER_BOUND('',#6376,.T.);
#5204=FACE_OUTER_BOUND('',#6377,.T.);
#5205=FACE_OUTER_BOUND('',#6378,.T.);
#5206=FACE_OUTER_BOUND('',#6379,.T.);
#5207=FACE_OUTER_BOUND('',#6380,.T.);
#5208=FACE_OUTER_BOUND('',#6381,.T.);
#5209=FACE_OUTER_BOUND('',#6382,.T.);
#5210=FACE_OUTER_BOUND('',#6383,.T.);
#5211=FACE_OUTER_BOUND('',#6384,.T.);
#5212=FACE_OUTER_BOUND('',#6385,.T.);
#5213=FACE_OUTER_BOUND('',#6386,.T.);
#5214=FACE_OUTER_BOUND('',#6387,.T.);
#5215=FACE_OUTER_BOUND('',#6388,.T.);
#5216=FACE_OUTER_BOUND('',#6389,.T.);
#5217=FACE_OUTER_BOUND('',#6390,.T.);
#5218=FACE_OUTER_BOUND('',#6391,.T.);
#5219=FACE_OUTER_BOUND('',#6392,.T.);
#5220=FACE_OUTER_BOUND('',#6393,.T.);
#5221=FACE_OUTER_BOUND('',#6394,.T.);
#5222=FACE_OUTER_BOUND('',#6395,.T.);
#5223=FACE_OUTER_BOUND('',#6396,.T.);
#5224=FACE_OUTER_BOUND('',#6397,.T.);
#5225=FACE_OUTER_BOUND('',#6398,.T.);
#5226=FACE_OUTER_BOUND('',#6399,.T.);
#5227=FACE_OUTER_BOUND('',#6400,.T.);
#5228=FACE_OUTER_BOUND('',#6401,.T.);
#5229=FACE_OUTER_BOUND('',#6402,.T.);
#5230=FACE_OUTER_BOUND('',#6403,.T.);
#5231=FACE_OUTER_BOUND('',#6404,.T.);
#5232=FACE_OUTER_BOUND('',#6405,.T.);
#5233=FACE_OUTER_BOUND('',#6406,.T.);
#5234=FACE_OUTER_BOUND('',#6407,.T.);
#5235=FACE_OUTER_BOUND('',#6408,.T.);
#5236=FACE_OUTER_BOUND('',#6409,.T.);
#5237=FACE_OUTER_BOUND('',#6410,.T.);
#5238=FACE_OUTER_BOUND('',#6411,.T.);
#5239=FACE_OUTER_BOUND('',#6412,.T.);
#5240=FACE_OUTER_BOUND('',#6413,.T.);
#5241=FACE_OUTER_BOUND('',#6414,.T.);
#5242=FACE_OUTER_BOUND('',#6415,.T.);
#5243=FACE_OUTER_BOUND('',#6416,.T.);
#5244=FACE_OUTER_BOUND('',#6417,.T.);
#5245=FACE_OUTER_BOUND('',#6418,.T.);
#5246=FACE_OUTER_BOUND('',#6419,.T.);
#5247=FACE_OUTER_BOUND('',#6420,.T.);
#5248=FACE_OUTER_BOUND('',#6421,.T.);
#5249=FACE_OUTER_BOUND('',#6422,.T.);
#5250=FACE_OUTER_BOUND('',#6423,.T.);
#5251=FACE_OUTER_BOUND('',#6431,.T.);
#5252=FACE_OUTER_BOUND('',#6432,.T.);
#5253=FACE_OUTER_BOUND('',#6433,.T.);
#5254=FACE_OUTER_BOUND('',#6434,.T.);
#5255=FACE_OUTER_BOUND('',#6435,.T.);
#5256=FACE_OUTER_BOUND('',#6436,.T.);
#5257=FACE_OUTER_BOUND('',#6437,.T.);
#5258=FACE_OUTER_BOUND('',#6438,.T.);
#5259=FACE_OUTER_BOUND('',#6439,.T.);
#5260=FACE_OUTER_BOUND('',#6440,.T.);
#5261=FACE_OUTER_BOUND('',#6441,.T.);
#5262=FACE_OUTER_BOUND('',#6442,.T.);
#5263=FACE_OUTER_BOUND('',#6443,.T.);
#5264=FACE_OUTER_BOUND('',#6444,.T.);
#5265=FACE_OUTER_BOUND('',#6445,.T.);
#5266=FACE_OUTER_BOUND('',#6446,.T.);
#5267=FACE_OUTER_BOUND('',#6447,.T.);
#5268=FACE_OUTER_BOUND('',#6448,.T.);
#5269=FACE_OUTER_BOUND('',#6449,.T.);
#5270=FACE_OUTER_BOUND('',#6450,.T.);
#5271=FACE_OUTER_BOUND('',#6451,.T.);
#5272=FACE_OUTER_BOUND('',#6452,.T.);
#5273=FACE_OUTER_BOUND('',#6453,.T.);
#5274=FACE_OUTER_BOUND('',#6454,.T.);
#5275=FACE_OUTER_BOUND('',#6455,.T.);
#5276=FACE_OUTER_BOUND('',#6456,.T.);
#5277=FACE_OUTER_BOUND('',#6457,.T.);
#5278=FACE_OUTER_BOUND('',#6458,.T.);
#5279=FACE_OUTER_BOUND('',#6459,.T.);
#5280=FACE_OUTER_BOUND('',#6460,.T.);
#5281=FACE_OUTER_BOUND('',#6461,.T.);
#5282=FACE_OUTER_BOUND('',#6462,.T.);
#5283=FACE_OUTER_BOUND('',#6463,.T.);
#5284=FACE_OUTER_BOUND('',#6464,.T.);
#5285=FACE_OUTER_BOUND('',#6465,.T.);
#5286=FACE_OUTER_BOUND('',#6466,.T.);
#5287=FACE_OUTER_BOUND('',#6467,.T.);
#5288=FACE_OUTER_BOUND('',#6468,.T.);
#5289=FACE_OUTER_BOUND('',#6469,.T.);
#5290=FACE_OUTER_BOUND('',#6470,.T.);
#5291=FACE_OUTER_BOUND('',#6471,.T.);
#5292=FACE_OUTER_BOUND('',#6472,.T.);
#5293=FACE_OUTER_BOUND('',#6473,.T.);
#5294=FACE_OUTER_BOUND('',#6474,.T.);
#5295=FACE_OUTER_BOUND('',#6475,.T.);
#5296=FACE_OUTER_BOUND('',#6476,.T.);
#5297=FACE_OUTER_BOUND('',#6477,.T.);
#5298=FACE_OUTER_BOUND('',#6478,.T.);
#5299=FACE_OUTER_BOUND('',#6479,.T.);
#5300=FACE_OUTER_BOUND('',#6480,.T.);
#5301=FACE_OUTER_BOUND('',#6481,.T.);
#5302=FACE_OUTER_BOUND('',#6482,.T.);
#5303=FACE_OUTER_BOUND('',#6483,.T.);
#5304=FACE_OUTER_BOUND('',#6484,.T.);
#5305=FACE_OUTER_BOUND('',#6485,.T.);
#5306=FACE_OUTER_BOUND('',#6486,.T.);
#5307=FACE_OUTER_BOUND('',#6487,.T.);
#5308=FACE_OUTER_BOUND('',#6488,.T.);
#5309=FACE_OUTER_BOUND('',#6489,.T.);
#5310=FACE_OUTER_BOUND('',#6490,.T.);
#5311=FACE_OUTER_BOUND('',#6491,.T.);
#5312=FACE_OUTER_BOUND('',#6492,.T.);
#5313=FACE_OUTER_BOUND('',#6493,.T.);
#5314=FACE_OUTER_BOUND('',#6494,.T.);
#5315=FACE_OUTER_BOUND('',#6495,.T.);
#5316=FACE_OUTER_BOUND('',#6496,.T.);
#5317=FACE_OUTER_BOUND('',#6497,.T.);
#5318=FACE_OUTER_BOUND('',#6498,.T.);
#5319=FACE_OUTER_BOUND('',#6499,.T.);
#5320=FACE_OUTER_BOUND('',#6500,.T.);
#5321=FACE_OUTER_BOUND('',#6501,.T.);
#5322=FACE_OUTER_BOUND('',#6502,.T.);
#5323=FACE_OUTER_BOUND('',#6503,.T.);
#5324=FACE_OUTER_BOUND('',#6504,.T.);
#5325=FACE_OUTER_BOUND('',#6505,.T.);
#5326=FACE_OUTER_BOUND('',#6506,.T.);
#5327=FACE_OUTER_BOUND('',#6507,.T.);
#5328=FACE_OUTER_BOUND('',#6508,.T.);
#5329=FACE_OUTER_BOUND('',#6509,.T.);
#5330=FACE_OUTER_BOUND('',#6510,.T.);
#5331=FACE_OUTER_BOUND('',#6511,.T.);
#5332=FACE_OUTER_BOUND('',#6512,.T.);
#5333=FACE_OUTER_BOUND('',#6513,.T.);
#5334=FACE_OUTER_BOUND('',#6514,.T.);
#5335=FACE_OUTER_BOUND('',#6515,.T.);
#5336=FACE_OUTER_BOUND('',#6516,.T.);
#5337=FACE_OUTER_BOUND('',#6517,.T.);
#5338=FACE_OUTER_BOUND('',#6518,.T.);
#5339=FACE_OUTER_BOUND('',#6519,.T.);
#5340=FACE_OUTER_BOUND('',#6520,.T.);
#5341=FACE_OUTER_BOUND('',#6521,.T.);
#5342=FACE_OUTER_BOUND('',#6522,.T.);
#5343=FACE_OUTER_BOUND('',#6523,.T.);
#5344=FACE_OUTER_BOUND('',#6524,.T.);
#5345=FACE_OUTER_BOUND('',#6525,.T.);
#5346=FACE_OUTER_BOUND('',#6526,.T.);
#5347=FACE_OUTER_BOUND('',#6527,.T.);
#5348=FACE_OUTER_BOUND('',#6528,.T.);
#5349=FACE_OUTER_BOUND('',#6529,.T.);
#5350=FACE_OUTER_BOUND('',#6530,.T.);
#5351=FACE_OUTER_BOUND('',#6531,.T.);
#5352=FACE_OUTER_BOUND('',#6532,.T.);
#5353=FACE_OUTER_BOUND('',#6533,.T.);
#5354=FACE_OUTER_BOUND('',#6534,.T.);
#5355=FACE_OUTER_BOUND('',#6535,.T.);
#5356=FACE_OUTER_BOUND('',#6536,.T.);
#5357=FACE_OUTER_BOUND('',#6537,.T.);
#5358=FACE_OUTER_BOUND('',#6538,.T.);
#5359=FACE_OUTER_BOUND('',#6539,.T.);
#5360=FACE_OUTER_BOUND('',#6540,.T.);
#5361=FACE_OUTER_BOUND('',#6541,.T.);
#5362=FACE_OUTER_BOUND('',#6542,.T.);
#5363=FACE_OUTER_BOUND('',#6543,.T.);
#5364=FACE_OUTER_BOUND('',#6544,.T.);
#5365=FACE_OUTER_BOUND('',#6545,.T.);
#5366=FACE_OUTER_BOUND('',#6547,.T.);
#5367=FACE_OUTER_BOUND('',#6548,.T.);
#5368=FACE_OUTER_BOUND('',#6549,.T.);
#5369=FACE_OUTER_BOUND('',#6550,.T.);
#5370=FACE_OUTER_BOUND('',#6551,.T.);
#5371=FACE_OUTER_BOUND('',#6552,.T.);
#5372=FACE_OUTER_BOUND('',#6553,.T.);
#5373=FACE_OUTER_BOUND('',#6555,.T.);
#5374=FACE_OUTER_BOUND('',#6556,.T.);
#5375=FACE_OUTER_BOUND('',#6557,.T.);
#5376=FACE_OUTER_BOUND('',#6558,.T.);
#5377=FACE_OUTER_BOUND('',#6559,.T.);
#5378=FACE_OUTER_BOUND('',#6560,.T.);
#5379=FACE_OUTER_BOUND('',#6561,.T.);
#5380=FACE_OUTER_BOUND('',#6562,.T.);
#5381=FACE_OUTER_BOUND('',#6563,.T.);
#5382=FACE_OUTER_BOUND('',#6564,.T.);
#5383=FACE_OUTER_BOUND('',#6566,.T.);
#5384=FACE_OUTER_BOUND('',#6567,.T.);
#5385=FACE_OUTER_BOUND('',#6568,.T.);
#5386=FACE_OUTER_BOUND('',#6569,.T.);
#5387=FACE_OUTER_BOUND('',#6570,.T.);
#5388=FACE_OUTER_BOUND('',#6571,.T.);
#5389=FACE_OUTER_BOUND('',#6572,.T.);
#5390=FACE_OUTER_BOUND('',#6573,.T.);
#5391=FACE_OUTER_BOUND('',#6574,.T.);
#5392=FACE_OUTER_BOUND('',#6575,.T.);
#5393=FACE_OUTER_BOUND('',#6576,.T.);
#5394=FACE_OUTER_BOUND('',#6577,.T.);
#5395=FACE_OUTER_BOUND('',#6578,.T.);
#5396=FACE_OUTER_BOUND('',#6579,.T.);
#5397=FACE_OUTER_BOUND('',#6580,.T.);
#5398=FACE_OUTER_BOUND('',#6581,.T.);
#5399=FACE_OUTER_BOUND('',#6582,.T.);
#5400=FACE_OUTER_BOUND('',#6583,.T.);
#5401=FACE_OUTER_BOUND('',#6584,.T.);
#5402=FACE_OUTER_BOUND('',#6585,.T.);
#5403=FACE_OUTER_BOUND('',#6586,.T.);
#5404=FACE_OUTER_BOUND('',#6587,.T.);
#5405=FACE_OUTER_BOUND('',#6588,.T.);
#5406=FACE_OUTER_BOUND('',#6589,.T.);
#5407=FACE_OUTER_BOUND('',#6590,.T.);
#5408=FACE_OUTER_BOUND('',#6591,.T.);
#5409=FACE_OUTER_BOUND('',#6592,.T.);
#5410=FACE_OUTER_BOUND('',#6593,.T.);
#5411=FACE_OUTER_BOUND('',#6594,.T.);
#5412=FACE_OUTER_BOUND('',#6595,.T.);
#5413=FACE_OUTER_BOUND('',#6596,.T.);
#5414=FACE_OUTER_BOUND('',#6597,.T.);
#5415=FACE_OUTER_BOUND('',#6598,.T.);
#5416=FACE_OUTER_BOUND('',#6599,.T.);
#5417=FACE_OUTER_BOUND('',#6600,.T.);
#5418=FACE_OUTER_BOUND('',#6601,.T.);
#5419=FACE_OUTER_BOUND('',#6602,.T.);
#5420=FACE_OUTER_BOUND('',#6603,.T.);
#5421=FACE_OUTER_BOUND('',#6605,.T.);
#5422=FACE_OUTER_BOUND('',#6606,.T.);
#5423=FACE_OUTER_BOUND('',#6607,.T.);
#5424=FACE_OUTER_BOUND('',#6608,.T.);
#5425=FACE_OUTER_BOUND('',#6609,.T.);
#5426=FACE_OUTER_BOUND('',#6610,.T.);
#5427=FACE_OUTER_BOUND('',#6611,.T.);
#5428=FACE_OUTER_BOUND('',#6612,.T.);
#5429=FACE_OUTER_BOUND('',#6613,.T.);
#5430=FACE_OUTER_BOUND('',#6614,.T.);
#5431=FACE_OUTER_BOUND('',#6615,.T.);
#5432=FACE_OUTER_BOUND('',#6616,.T.);
#5433=FACE_OUTER_BOUND('',#6617,.T.);
#5434=FACE_OUTER_BOUND('',#6618,.T.);
#5435=FACE_OUTER_BOUND('',#6619,.T.);
#5436=FACE_OUTER_BOUND('',#6620,.T.);
#5437=FACE_OUTER_BOUND('',#6621,.T.);
#5438=FACE_OUTER_BOUND('',#6622,.T.);
#5439=FACE_OUTER_BOUND('',#6626,.T.);
#5440=FACE_OUTER_BOUND('',#6627,.T.);
#5441=FACE_OUTER_BOUND('',#6629,.T.);
#5442=FACE_OUTER_BOUND('',#6630,.T.);
#5443=FACE_OUTER_BOUND('',#6631,.T.);
#5444=FACE_OUTER_BOUND('',#6632,.T.);
#5445=FACE_OUTER_BOUND('',#6633,.T.);
#5446=FACE_OUTER_BOUND('',#6634,.T.);
#5447=FACE_OUTER_BOUND('',#6635,.T.);
#5448=FACE_OUTER_BOUND('',#6636,.T.);
#5449=FACE_OUTER_BOUND('',#6637,.T.);
#5450=FACE_OUTER_BOUND('',#6641,.T.);
#5451=FACE_OUTER_BOUND('',#6642,.T.);
#5452=FACE_OUTER_BOUND('',#6644,.T.);
#5453=FACE_OUTER_BOUND('',#6645,.T.);
#5454=FACE_OUTER_BOUND('',#6646,.T.);
#5455=FACE_OUTER_BOUND('',#6647,.T.);
#5456=FACE_OUTER_BOUND('',#6648,.T.);
#5457=FACE_OUTER_BOUND('',#6649,.T.);
#5458=FACE_OUTER_BOUND('',#6650,.T.);
#5459=FACE_OUTER_BOUND('',#6651,.T.);
#5460=FACE_OUTER_BOUND('',#6652,.T.);
#5461=FACE_OUTER_BOUND('',#6653,.T.);
#5462=FACE_OUTER_BOUND('',#6654,.T.);
#5463=FACE_OUTER_BOUND('',#6658,.T.);
#5464=FACE_OUTER_BOUND('',#6659,.T.);
#5465=FACE_OUTER_BOUND('',#6660,.T.);
#5466=FACE_OUTER_BOUND('',#6661,.T.);
#5467=FACE_OUTER_BOUND('',#6665,.T.);
#5468=FACE_OUTER_BOUND('',#6666,.T.);
#5469=FACE_OUTER_BOUND('',#6667,.T.);
#5470=FACE_OUTER_BOUND('',#6668,.T.);
#5471=FACE_OUTER_BOUND('',#6669,.T.);
#5472=FACE_OUTER_BOUND('',#6670,.T.);
#5473=FACE_OUTER_BOUND('',#6671,.T.);
#5474=FACE_OUTER_BOUND('',#6672,.T.);
#5475=FACE_OUTER_BOUND('',#6673,.T.);
#5476=FACE_OUTER_BOUND('',#6678,.T.);
#5477=FACE_OUTER_BOUND('',#6679,.T.);
#5478=FACE_OUTER_BOUND('',#6680,.T.);
#5479=FACE_OUTER_BOUND('',#6681,.T.);
#5480=FACE_OUTER_BOUND('',#6682,.T.);
#5481=FACE_OUTER_BOUND('',#6683,.T.);
#5482=FACE_OUTER_BOUND('',#6684,.T.);
#5483=FACE_OUTER_BOUND('',#6685,.T.);
#5484=FACE_OUTER_BOUND('',#6686,.T.);
#5485=FACE_OUTER_BOUND('',#6691,.T.);
#5486=FACE_OUTER_BOUND('',#6692,.T.);
#5487=FACE_OUTER_BOUND('',#6693,.T.);
#5488=FACE_OUTER_BOUND('',#6694,.T.);
#5489=FACE_OUTER_BOUND('',#6695,.T.);
#5490=FACE_OUTER_BOUND('',#6696,.T.);
#5491=FACE_OUTER_BOUND('',#6697,.T.);
#5492=FACE_OUTER_BOUND('',#6698,.T.);
#5493=FACE_OUTER_BOUND('',#6699,.T.);
#5494=FACE_OUTER_BOUND('',#6700,.T.);
#5495=FACE_OUTER_BOUND('',#6701,.T.);
#5496=FACE_OUTER_BOUND('',#6702,.T.);
#5497=FACE_OUTER_BOUND('',#6703,.T.);
#5498=FACE_OUTER_BOUND('',#6704,.T.);
#5499=FACE_OUTER_BOUND('',#6705,.T.);
#5500=FACE_OUTER_BOUND('',#6706,.T.);
#5501=FACE_OUTER_BOUND('',#6707,.T.);
#5502=FACE_OUTER_BOUND('',#6708,.T.);
#5503=FACE_OUTER_BOUND('',#6709,.T.);
#5504=FACE_OUTER_BOUND('',#6710,.T.);
#5505=FACE_OUTER_BOUND('',#6711,.T.);
#5506=FACE_OUTER_BOUND('',#6712,.T.);
#5507=FACE_OUTER_BOUND('',#6713,.T.);
#5508=FACE_OUTER_BOUND('',#6714,.T.);
#5509=FACE_OUTER_BOUND('',#6715,.T.);
#5510=FACE_OUTER_BOUND('',#6716,.T.);
#5511=FACE_OUTER_BOUND('',#6717,.T.);
#5512=FACE_OUTER_BOUND('',#6718,.T.);
#5513=FACE_OUTER_BOUND('',#6719,.T.);
#5514=FACE_OUTER_BOUND('',#6720,.T.);
#5515=FACE_OUTER_BOUND('',#6721,.T.);
#5516=FACE_OUTER_BOUND('',#6722,.T.);
#5517=FACE_OUTER_BOUND('',#6723,.T.);
#5518=FACE_OUTER_BOUND('',#6724,.T.);
#5519=FACE_OUTER_BOUND('',#6725,.T.);
#5520=FACE_OUTER_BOUND('',#6726,.T.);
#5521=FACE_OUTER_BOUND('',#6727,.T.);
#5522=FACE_OUTER_BOUND('',#6728,.T.);
#5523=FACE_OUTER_BOUND('',#6729,.T.);
#5524=FACE_OUTER_BOUND('',#6730,.T.);
#5525=FACE_OUTER_BOUND('',#6731,.T.);
#5526=FACE_OUTER_BOUND('',#6732,.T.);
#5527=FACE_OUTER_BOUND('',#6733,.T.);
#5528=FACE_OUTER_BOUND('',#6734,.T.);
#5529=FACE_OUTER_BOUND('',#6735,.T.);
#5530=FACE_OUTER_BOUND('',#6736,.T.);
#5531=FACE_OUTER_BOUND('',#6737,.T.);
#5532=FACE_OUTER_BOUND('',#6738,.T.);
#5533=FACE_OUTER_BOUND('',#6739,.T.);
#5534=FACE_OUTER_BOUND('',#6740,.T.);
#5535=FACE_OUTER_BOUND('',#6741,.T.);
#5536=FACE_OUTER_BOUND('',#6742,.T.);
#5537=FACE_OUTER_BOUND('',#6743,.T.);
#5538=FACE_OUTER_BOUND('',#6744,.T.);
#5539=FACE_OUTER_BOUND('',#6745,.T.);
#5540=FACE_OUTER_BOUND('',#6746,.T.);
#5541=FACE_OUTER_BOUND('',#6747,.T.);
#5542=FACE_OUTER_BOUND('',#6748,.T.);
#5543=FACE_OUTER_BOUND('',#6749,.T.);
#5544=FACE_OUTER_BOUND('',#6750,.T.);
#5545=FACE_OUTER_BOUND('',#6751,.T.);
#5546=FACE_OUTER_BOUND('',#6752,.T.);
#5547=FACE_OUTER_BOUND('',#6753,.T.);
#5548=FACE_OUTER_BOUND('',#6754,.T.);
#5549=FACE_OUTER_BOUND('',#6755,.T.);
#5550=FACE_OUTER_BOUND('',#6756,.T.);
#5551=FACE_OUTER_BOUND('',#6757,.T.);
#5552=FACE_OUTER_BOUND('',#6758,.T.);
#5553=FACE_OUTER_BOUND('',#6759,.T.);
#5554=FACE_OUTER_BOUND('',#6760,.T.);
#5555=FACE_OUTER_BOUND('',#6761,.T.);
#5556=FACE_OUTER_BOUND('',#6762,.T.);
#5557=FACE_OUTER_BOUND('',#6763,.T.);
#5558=FACE_OUTER_BOUND('',#6764,.T.);
#5559=FACE_OUTER_BOUND('',#6765,.T.);
#5560=FACE_OUTER_BOUND('',#6766,.T.);
#5561=FACE_OUTER_BOUND('',#6767,.T.);
#5562=FACE_OUTER_BOUND('',#6768,.T.);
#5563=FACE_OUTER_BOUND('',#6769,.T.);
#5564=FACE_OUTER_BOUND('',#6770,.T.);
#5565=FACE_OUTER_BOUND('',#6771,.T.);
#5566=FACE_OUTER_BOUND('',#6772,.T.);
#5567=FACE_OUTER_BOUND('',#6773,.T.);
#5568=FACE_OUTER_BOUND('',#6774,.T.);
#5569=FACE_OUTER_BOUND('',#6775,.T.);
#5570=FACE_OUTER_BOUND('',#6776,.T.);
#5571=FACE_OUTER_BOUND('',#6777,.T.);
#5572=FACE_OUTER_BOUND('',#6780,.T.);
#5573=FACE_OUTER_BOUND('',#6781,.T.);
#5574=FACE_OUTER_BOUND('',#6782,.T.);
#5575=FACE_OUTER_BOUND('',#6783,.T.);
#5576=FACE_OUTER_BOUND('',#6784,.T.);
#5577=FACE_OUTER_BOUND('',#6785,.T.);
#5578=FACE_OUTER_BOUND('',#6786,.T.);
#5579=FACE_OUTER_BOUND('',#6787,.T.);
#5580=FACE_OUTER_BOUND('',#6788,.T.);
#5581=FACE_OUTER_BOUND('',#6789,.T.);
#5582=FACE_OUTER_BOUND('',#6790,.T.);
#5583=FACE_OUTER_BOUND('',#6791,.T.);
#5584=FACE_OUTER_BOUND('',#6793,.T.);
#5585=FACE_OUTER_BOUND('',#6794,.T.);
#5586=FACE_OUTER_BOUND('',#6795,.T.);
#5587=FACE_OUTER_BOUND('',#6796,.T.);
#5588=FACE_OUTER_BOUND('',#6797,.T.);
#5589=FACE_OUTER_BOUND('',#6798,.T.);
#5590=FACE_OUTER_BOUND('',#6799,.T.);
#5591=FACE_OUTER_BOUND('',#6800,.T.);
#5592=FACE_OUTER_BOUND('',#6801,.T.);
#5593=FACE_OUTER_BOUND('',#6802,.T.);
#5594=FACE_OUTER_BOUND('',#6803,.T.);
#5595=FACE_OUTER_BOUND('',#6804,.T.);
#5596=FACE_OUTER_BOUND('',#6805,.T.);
#5597=FACE_OUTER_BOUND('',#6806,.T.);
#5598=FACE_OUTER_BOUND('',#6807,.T.);
#5599=FACE_OUTER_BOUND('',#6808,.T.);
#5600=FACE_OUTER_BOUND('',#6809,.T.);
#5601=FACE_OUTER_BOUND('',#6812,.T.);
#5602=FACE_OUTER_BOUND('',#6813,.T.);
#5603=FACE_OUTER_BOUND('',#6814,.T.);
#5604=FACE_OUTER_BOUND('',#6817,.T.);
#5605=FACE_OUTER_BOUND('',#6818,.T.);
#5606=FACE_OUTER_BOUND('',#6819,.T.);
#5607=FACE_OUTER_BOUND('',#6821,.T.);
#5608=FACE_OUTER_BOUND('',#6822,.T.);
#5609=FACE_OUTER_BOUND('',#6823,.T.);
#5610=FACE_OUTER_BOUND('',#6824,.T.);
#5611=FACE_OUTER_BOUND('',#6825,.T.);
#5612=FACE_OUTER_BOUND('',#6826,.T.);
#5613=FACE_OUTER_BOUND('',#6827,.T.);
#5614=FACE_OUTER_BOUND('',#6829,.T.);
#5615=FACE_OUTER_BOUND('',#6831,.T.);
#5616=FACE_OUTER_BOUND('',#6832,.T.);
#5617=FACE_OUTER_BOUND('',#6833,.T.);
#5618=FACE_OUTER_BOUND('',#6835,.T.);
#5619=FACE_OUTER_BOUND('',#6836,.T.);
#5620=FACE_OUTER_BOUND('',#6837,.T.);
#5621=FACE_OUTER_BOUND('',#6838,.T.);
#5622=FACE_OUTER_BOUND('',#6839,.T.);
#5623=FACE_OUTER_BOUND('',#6841,.T.);
#5624=FACE_OUTER_BOUND('',#6842,.T.);
#5625=FACE_OUTER_BOUND('',#6844,.T.);
#5626=FACE_OUTER_BOUND('',#6845,.T.);
#5627=FACE_OUTER_BOUND('',#6846,.T.);
#5628=FACE_OUTER_BOUND('',#6847,.T.);
#5629=FACE_OUTER_BOUND('',#6848,.T.);
#5630=FACE_OUTER_BOUND('',#6849,.T.);
#5631=FACE_OUTER_BOUND('',#6850,.T.);
#5632=FACE_OUTER_BOUND('',#6851,.T.);
#5633=FACE_OUTER_BOUND('',#6852,.T.);
#5634=FACE_OUTER_BOUND('',#6853,.T.);
#5635=FACE_OUTER_BOUND('',#6854,.T.);
#5636=FACE_OUTER_BOUND('',#6855,.T.);
#5637=FACE_OUTER_BOUND('',#6856,.T.);
#5638=FACE_OUTER_BOUND('',#6857,.T.);
#5639=FACE_OUTER_BOUND('',#6858,.T.);
#5640=FACE_OUTER_BOUND('',#6859,.T.);
#5641=FACE_OUTER_BOUND('',#6860,.T.);
#5642=FACE_OUTER_BOUND('',#6861,.T.);
#5643=FACE_OUTER_BOUND('',#6862,.T.);
#5644=FACE_OUTER_BOUND('',#6863,.T.);
#5645=FACE_OUTER_BOUND('',#6864,.T.);
#5646=FACE_OUTER_BOUND('',#6865,.T.);
#5647=FACE_OUTER_BOUND('',#6866,.T.);
#5648=FACE_OUTER_BOUND('',#6867,.T.);
#5649=FACE_OUTER_BOUND('',#6868,.T.);
#5650=FACE_OUTER_BOUND('',#6869,.T.);
#5651=FACE_OUTER_BOUND('',#6870,.T.);
#5652=FACE_OUTER_BOUND('',#6871,.T.);
#5653=FACE_OUTER_BOUND('',#6872,.T.);
#5654=FACE_OUTER_BOUND('',#6873,.T.);
#5655=FACE_OUTER_BOUND('',#6874,.T.);
#5656=FACE_OUTER_BOUND('',#6875,.T.);
#5657=FACE_OUTER_BOUND('',#6876,.T.);
#5658=FACE_OUTER_BOUND('',#6877,.T.);
#5659=FACE_OUTER_BOUND('',#6878,.T.);
#5660=FACE_OUTER_BOUND('',#6879,.T.);
#5661=FACE_OUTER_BOUND('',#6880,.T.);
#5662=FACE_OUTER_BOUND('',#6881,.T.);
#5663=FACE_OUTER_BOUND('',#6882,.T.);
#5664=FACE_OUTER_BOUND('',#6883,.T.);
#5665=FACE_OUTER_BOUND('',#6884,.T.);
#5666=FACE_OUTER_BOUND('',#6885,.T.);
#5667=FACE_OUTER_BOUND('',#6886,.T.);
#5668=FACE_OUTER_BOUND('',#6887,.T.);
#5669=FACE_OUTER_BOUND('',#6888,.T.);
#5670=FACE_OUTER_BOUND('',#6889,.T.);
#5671=FACE_OUTER_BOUND('',#6890,.T.);
#5672=FACE_OUTER_BOUND('',#6891,.T.);
#5673=FACE_OUTER_BOUND('',#6892,.T.);
#5674=FACE_OUTER_BOUND('',#6893,.T.);
#5675=FACE_OUTER_BOUND('',#6894,.T.);
#5676=FACE_OUTER_BOUND('',#6895,.T.);
#5677=FACE_OUTER_BOUND('',#6896,.T.);
#5678=FACE_OUTER_BOUND('',#6897,.T.);
#5679=FACE_OUTER_BOUND('',#6898,.T.);
#5680=FACE_OUTER_BOUND('',#6899,.T.);
#5681=FACE_OUTER_BOUND('',#6901,.T.);
#5682=FACE_OUTER_BOUND('',#6902,.T.);
#5683=FACE_OUTER_BOUND('',#6903,.T.);
#5684=FACE_OUTER_BOUND('',#6904,.T.);
#5685=FACE_OUTER_BOUND('',#6905,.T.);
#5686=FACE_OUTER_BOUND('',#6906,.T.);
#5687=FACE_OUTER_BOUND('',#6907,.T.);
#5688=FACE_OUTER_BOUND('',#6908,.T.);
#5689=FACE_OUTER_BOUND('',#6909,.T.);
#5690=FACE_OUTER_BOUND('',#6910,.T.);
#5691=FACE_OUTER_BOUND('',#6911,.T.);
#5692=FACE_OUTER_BOUND('',#6912,.T.);
#5693=FACE_OUTER_BOUND('',#6913,.T.);
#5694=FACE_OUTER_BOUND('',#6914,.T.);
#5695=FACE_OUTER_BOUND('',#6915,.T.);
#5696=FACE_OUTER_BOUND('',#6916,.T.);
#5697=FACE_OUTER_BOUND('',#6917,.T.);
#5698=FACE_OUTER_BOUND('',#6918,.T.);
#5699=FACE_OUTER_BOUND('',#6919,.T.);
#5700=FACE_OUTER_BOUND('',#6920,.T.);
#5701=FACE_OUTER_BOUND('',#6921,.T.);
#5702=FACE_OUTER_BOUND('',#6922,.T.);
#5703=FACE_OUTER_BOUND('',#6923,.T.);
#5704=FACE_OUTER_BOUND('',#6924,.T.);
#5705=FACE_OUTER_BOUND('',#6925,.T.);
#5706=FACE_OUTER_BOUND('',#6926,.T.);
#5707=FACE_OUTER_BOUND('',#6927,.T.);
#5708=FACE_OUTER_BOUND('',#6928,.T.);
#5709=FACE_OUTER_BOUND('',#6929,.T.);
#5710=FACE_OUTER_BOUND('',#6930,.T.);
#5711=FACE_OUTER_BOUND('',#6931,.T.);
#5712=FACE_OUTER_BOUND('',#6932,.T.);
#5713=FACE_OUTER_BOUND('',#6933,.T.);
#5714=FACE_OUTER_BOUND('',#6934,.T.);
#5715=FACE_OUTER_BOUND('',#6935,.T.);
#5716=FACE_OUTER_BOUND('',#6936,.T.);
#5717=FACE_OUTER_BOUND('',#6937,.T.);
#5718=FACE_OUTER_BOUND('',#6938,.T.);
#5719=FACE_OUTER_BOUND('',#6939,.T.);
#5720=FACE_OUTER_BOUND('',#6940,.T.);
#5721=FACE_OUTER_BOUND('',#6941,.T.);
#5722=FACE_OUTER_BOUND('',#6942,.T.);
#5723=FACE_OUTER_BOUND('',#6943,.T.);
#5724=FACE_OUTER_BOUND('',#6944,.T.);
#5725=FACE_OUTER_BOUND('',#6945,.T.);
#5726=FACE_OUTER_BOUND('',#6946,.T.);
#5727=FACE_OUTER_BOUND('',#6947,.T.);
#5728=FACE_OUTER_BOUND('',#6948,.T.);
#5729=FACE_OUTER_BOUND('',#6949,.T.);
#5730=FACE_OUTER_BOUND('',#6950,.T.);
#5731=FACE_OUTER_BOUND('',#6952,.T.);
#5732=FACE_OUTER_BOUND('',#6953,.T.);
#5733=FACE_OUTER_BOUND('',#6954,.T.);
#5734=FACE_OUTER_BOUND('',#6955,.T.);
#5735=FACE_OUTER_BOUND('',#6957,.T.);
#5736=FACE_OUTER_BOUND('',#6958,.T.);
#5737=FACE_OUTER_BOUND('',#6960,.T.);
#5738=FACE_OUTER_BOUND('',#6961,.T.);
#5739=FACE_OUTER_BOUND('',#6962,.T.);
#5740=FACE_OUTER_BOUND('',#6963,.T.);
#5741=FACE_OUTER_BOUND('',#6964,.T.);
#5742=FACE_OUTER_BOUND('',#6965,.T.);
#5743=FACE_OUTER_BOUND('',#6966,.T.);
#5744=FACE_OUTER_BOUND('',#6967,.T.);
#5745=FACE_OUTER_BOUND('',#6968,.T.);
#5746=FACE_OUTER_BOUND('',#6969,.T.);
#5747=FACE_OUTER_BOUND('',#6970,.T.);
#5748=FACE_OUTER_BOUND('',#6971,.T.);
#5749=FACE_OUTER_BOUND('',#6972,.T.);
#5750=FACE_OUTER_BOUND('',#6973,.T.);
#5751=FACE_OUTER_BOUND('',#6974,.T.);
#5752=FACE_OUTER_BOUND('',#6975,.T.);
#5753=FACE_OUTER_BOUND('',#6976,.T.);
#5754=FACE_OUTER_BOUND('',#6977,.T.);
#5755=FACE_OUTER_BOUND('',#6978,.T.);
#5756=FACE_OUTER_BOUND('',#6979,.T.);
#5757=FACE_OUTER_BOUND('',#6980,.T.);
#5758=FACE_OUTER_BOUND('',#6981,.T.);
#5759=FACE_OUTER_BOUND('',#6982,.T.);
#5760=FACE_OUTER_BOUND('',#6983,.T.);
#5761=FACE_OUTER_BOUND('',#6984,.T.);
#5762=FACE_OUTER_BOUND('',#6985,.T.);
#5763=FACE_OUTER_BOUND('',#6986,.T.);
#5764=FACE_OUTER_BOUND('',#6987,.T.);
#5765=FACE_OUTER_BOUND('',#6988,.T.);
#5766=FACE_OUTER_BOUND('',#6989,.T.);
#5767=FACE_OUTER_BOUND('',#6990,.T.);
#5768=FACE_OUTER_BOUND('',#6991,.T.);
#5769=FACE_OUTER_BOUND('',#6992,.T.);
#5770=FACE_OUTER_BOUND('',#6993,.T.);
#5771=FACE_OUTER_BOUND('',#6994,.T.);
#5772=FACE_OUTER_BOUND('',#6995,.T.);
#5773=FACE_OUTER_BOUND('',#6996,.T.);
#5774=FACE_OUTER_BOUND('',#6997,.T.);
#5775=FACE_OUTER_BOUND('',#6998,.T.);
#5776=FACE_OUTER_BOUND('',#6999,.T.);
#5777=FACE_OUTER_BOUND('',#7000,.T.);
#5778=FACE_OUTER_BOUND('',#7001,.T.);
#5779=FACE_OUTER_BOUND('',#7002,.T.);
#5780=FACE_OUTER_BOUND('',#7003,.T.);
#5781=FACE_OUTER_BOUND('',#7004,.T.);
#5782=FACE_OUTER_BOUND('',#7005,.T.);
#5783=FACE_OUTER_BOUND('',#7007,.T.);
#5784=FACE_OUTER_BOUND('',#7008,.T.);
#5785=FACE_OUTER_BOUND('',#7009,.T.);
#5786=FACE_OUTER_BOUND('',#7010,.T.);
#5787=FACE_OUTER_BOUND('',#7012,.T.);
#5788=FACE_OUTER_BOUND('',#7013,.T.);
#5789=FACE_OUTER_BOUND('',#7014,.T.);
#5790=FACE_OUTER_BOUND('',#7015,.T.);
#5791=FACE_OUTER_BOUND('',#7016,.T.);
#5792=FACE_OUTER_BOUND('',#7017,.T.);
#5793=FACE_OUTER_BOUND('',#7018,.T.);
#5794=FACE_OUTER_BOUND('',#7019,.T.);
#5795=FACE_OUTER_BOUND('',#7020,.T.);
#5796=FACE_OUTER_BOUND('',#7021,.T.);
#5797=FACE_OUTER_BOUND('',#7022,.T.);
#5798=FACE_OUTER_BOUND('',#7023,.T.);
#5799=FACE_OUTER_BOUND('',#7024,.T.);
#5800=FACE_OUTER_BOUND('',#7025,.T.);
#5801=FACE_OUTER_BOUND('',#7026,.T.);
#5802=FACE_OUTER_BOUND('',#7027,.T.);
#5803=FACE_OUTER_BOUND('',#7028,.T.);
#5804=FACE_OUTER_BOUND('',#7029,.T.);
#5805=FACE_OUTER_BOUND('',#7030,.T.);
#5806=FACE_OUTER_BOUND('',#7031,.T.);
#5807=FACE_OUTER_BOUND('',#7032,.T.);
#5808=FACE_OUTER_BOUND('',#7033,.T.);
#5809=FACE_OUTER_BOUND('',#7034,.T.);
#5810=FACE_OUTER_BOUND('',#7035,.T.);
#5811=FACE_OUTER_BOUND('',#7037,.T.);
#5812=FACE_OUTER_BOUND('',#7038,.T.);
#5813=FACE_OUTER_BOUND('',#7039,.T.);
#5814=FACE_OUTER_BOUND('',#7040,.T.);
#5815=FACE_OUTER_BOUND('',#7041,.T.);
#5816=FACE_OUTER_BOUND('',#7042,.T.);
#5817=FACE_OUTER_BOUND('',#7044,.T.);
#5818=FACE_OUTER_BOUND('',#7045,.T.);
#5819=FACE_OUTER_BOUND('',#7046,.T.);
#5820=FACE_OUTER_BOUND('',#7047,.T.);
#5821=FACE_OUTER_BOUND('',#7048,.T.);
#5822=FACE_OUTER_BOUND('',#7049,.T.);
#5823=FACE_OUTER_BOUND('',#7050,.T.);
#5824=FACE_OUTER_BOUND('',#7051,.T.);
#5825=FACE_OUTER_BOUND('',#7052,.T.);
#5826=FACE_OUTER_BOUND('',#7053,.T.);
#5827=FACE_OUTER_BOUND('',#7054,.T.);
#5828=FACE_OUTER_BOUND('',#7055,.T.);
#5829=FACE_OUTER_BOUND('',#7056,.T.);
#5830=FACE_OUTER_BOUND('',#7057,.T.);
#5831=FACE_OUTER_BOUND('',#7058,.T.);
#5832=FACE_OUTER_BOUND('',#7063,.T.);
#5833=FACE_OUTER_BOUND('',#7064,.T.);
#5834=FACE_OUTER_BOUND('',#7065,.T.);
#5835=FACE_OUTER_BOUND('',#7066,.T.);
#5836=FACE_OUTER_BOUND('',#7067,.T.);
#5837=FACE_OUTER_BOUND('',#7068,.T.);
#5838=FACE_OUTER_BOUND('',#7069,.T.);
#5839=FACE_OUTER_BOUND('',#7070,.T.);
#5840=FACE_OUTER_BOUND('',#7071,.T.);
#5841=FACE_OUTER_BOUND('',#7072,.T.);
#5842=FACE_OUTER_BOUND('',#7073,.T.);
#5843=FACE_OUTER_BOUND('',#7074,.T.);
#5844=FACE_OUTER_BOUND('',#7075,.T.);
#5845=FACE_OUTER_BOUND('',#7076,.T.);
#5846=FACE_OUTER_BOUND('',#7077,.T.);
#5847=FACE_OUTER_BOUND('',#7078,.T.);
#5848=FACE_OUTER_BOUND('',#7079,.T.);
#5849=FACE_OUTER_BOUND('',#7080,.T.);
#5850=FACE_OUTER_BOUND('',#7081,.T.);
#5851=FACE_OUTER_BOUND('',#7082,.T.);
#5852=FACE_OUTER_BOUND('',#7083,.T.);
#5853=FACE_OUTER_BOUND('',#7084,.T.);
#5854=FACE_OUTER_BOUND('',#7085,.T.);
#5855=FACE_OUTER_BOUND('',#7087,.T.);
#5856=FACE_OUTER_BOUND('',#7088,.T.);
#5857=FACE_OUTER_BOUND('',#7089,.T.);
#5858=FACE_OUTER_BOUND('',#7090,.T.);
#5859=FACE_OUTER_BOUND('',#7092,.T.);
#5860=FACE_OUTER_BOUND('',#7093,.T.);
#5861=FACE_OUTER_BOUND('',#7094,.T.);
#5862=FACE_OUTER_BOUND('',#7095,.T.);
#5863=FACE_OUTER_BOUND('',#7096,.T.);
#5864=FACE_OUTER_BOUND('',#7097,.T.);
#5865=FACE_OUTER_BOUND('',#7098,.T.);
#5866=FACE_OUTER_BOUND('',#7099,.T.);
#5867=FACE_OUTER_BOUND('',#7100,.T.);
#5868=FACE_OUTER_BOUND('',#7101,.T.);
#5869=FACE_OUTER_BOUND('',#7102,.T.);
#5870=FACE_OUTER_BOUND('',#7103,.T.);
#5871=FACE_OUTER_BOUND('',#7104,.T.);
#5872=FACE_OUTER_BOUND('',#7105,.T.);
#5873=FACE_OUTER_BOUND('',#7106,.T.);
#5874=FACE_OUTER_BOUND('',#7107,.T.);
#5875=FACE_OUTER_BOUND('',#7108,.T.);
#5876=FACE_OUTER_BOUND('',#7109,.T.);
#5877=FACE_OUTER_BOUND('',#7110,.T.);
#5878=FACE_OUTER_BOUND('',#7111,.T.);
#5879=FACE_OUTER_BOUND('',#7112,.T.);
#5880=FACE_OUTER_BOUND('',#7113,.T.);
#5881=FACE_OUTER_BOUND('',#7114,.T.);
#5882=FACE_OUTER_BOUND('',#7115,.T.);
#5883=FACE_OUTER_BOUND('',#7116,.T.);
#5884=FACE_OUTER_BOUND('',#7117,.T.);
#5885=FACE_OUTER_BOUND('',#7118,.T.);
#5886=FACE_OUTER_BOUND('',#7119,.T.);
#5887=FACE_OUTER_BOUND('',#7120,.T.);
#5888=FACE_OUTER_BOUND('',#7121,.T.);
#5889=FACE_OUTER_BOUND('',#7122,.T.);
#5890=FACE_OUTER_BOUND('',#7123,.T.);
#5891=FACE_OUTER_BOUND('',#7124,.T.);
#5892=FACE_OUTER_BOUND('',#7125,.T.);
#5893=FACE_OUTER_BOUND('',#7126,.T.);
#5894=FACE_OUTER_BOUND('',#7127,.T.);
#5895=FACE_OUTER_BOUND('',#7128,.T.);
#5896=FACE_OUTER_BOUND('',#7129,.T.);
#5897=FACE_OUTER_BOUND('',#7131,.T.);
#5898=FACE_OUTER_BOUND('',#7132,.T.);
#5899=FACE_OUTER_BOUND('',#7133,.T.);
#5900=FACE_OUTER_BOUND('',#7134,.T.);
#5901=FACE_OUTER_BOUND('',#7135,.T.);
#5902=FACE_OUTER_BOUND('',#7136,.T.);
#5903=FACE_OUTER_BOUND('',#7137,.T.);
#5904=FACE_OUTER_BOUND('',#7138,.T.);
#5905=FACE_OUTER_BOUND('',#7139,.T.);
#5906=FACE_OUTER_BOUND('',#7140,.T.);
#5907=FACE_OUTER_BOUND('',#7141,.T.);
#5908=FACE_OUTER_BOUND('',#7142,.T.);
#5909=FACE_OUTER_BOUND('',#7143,.T.);
#5910=FACE_OUTER_BOUND('',#7144,.T.);
#5911=FACE_OUTER_BOUND('',#7145,.T.);
#5912=FACE_OUTER_BOUND('',#7146,.T.);
#5913=FACE_OUTER_BOUND('',#7147,.T.);
#5914=FACE_OUTER_BOUND('',#7148,.T.);
#5915=FACE_OUTER_BOUND('',#7149,.T.);
#5916=FACE_OUTER_BOUND('',#7150,.T.);
#5917=FACE_OUTER_BOUND('',#7151,.T.);
#5918=FACE_OUTER_BOUND('',#7152,.T.);
#5919=FACE_OUTER_BOUND('',#7153,.T.);
#5920=FACE_OUTER_BOUND('',#7156,.T.);
#5921=FACE_OUTER_BOUND('',#7157,.T.);
#5922=FACE_OUTER_BOUND('',#7158,.T.);
#5923=FACE_OUTER_BOUND('',#7159,.T.);
#5924=FACE_OUTER_BOUND('',#7160,.T.);
#5925=FACE_OUTER_BOUND('',#7161,.T.);
#5926=FACE_OUTER_BOUND('',#7162,.T.);
#5927=FACE_OUTER_BOUND('',#7163,.T.);
#5928=FACE_OUTER_BOUND('',#7164,.T.);
#5929=FACE_OUTER_BOUND('',#7165,.T.);
#5930=FACE_OUTER_BOUND('',#7166,.T.);
#5931=FACE_OUTER_BOUND('',#7167,.T.);
#5932=FACE_OUTER_BOUND('',#7168,.T.);
#5933=FACE_OUTER_BOUND('',#7169,.T.);
#5934=FACE_OUTER_BOUND('',#7170,.T.);
#5935=FACE_OUTER_BOUND('',#7171,.T.);
#5936=FACE_OUTER_BOUND('',#7172,.T.);
#5937=FACE_OUTER_BOUND('',#7173,.T.);
#5938=FACE_OUTER_BOUND('',#7174,.T.);
#5939=FACE_OUTER_BOUND('',#7175,.T.);
#5940=FACE_OUTER_BOUND('',#7176,.T.);
#5941=FACE_OUTER_BOUND('',#7177,.T.);
#5942=FACE_OUTER_BOUND('',#7178,.T.);
#5943=FACE_OUTER_BOUND('',#7179,.T.);
#5944=FACE_OUTER_BOUND('',#7180,.T.);
#5945=FACE_OUTER_BOUND('',#7181,.T.);
#5946=FACE_OUTER_BOUND('',#7182,.T.);
#5947=FACE_OUTER_BOUND('',#7183,.T.);
#5948=FACE_OUTER_BOUND('',#7184,.T.);
#5949=FACE_OUTER_BOUND('',#7185,.T.);
#5950=FACE_OUTER_BOUND('',#7186,.T.);
#5951=FACE_OUTER_BOUND('',#7187,.T.);
#5952=FACE_OUTER_BOUND('',#7188,.T.);
#5953=FACE_OUTER_BOUND('',#7189,.T.);
#5954=FACE_OUTER_BOUND('',#7190,.T.);
#5955=FACE_OUTER_BOUND('',#7191,.T.);
#5956=FACE_OUTER_BOUND('',#7192,.T.);
#5957=FACE_OUTER_BOUND('',#7193,.T.);
#5958=FACE_OUTER_BOUND('',#7194,.T.);
#5959=FACE_OUTER_BOUND('',#7195,.T.);
#5960=FACE_OUTER_BOUND('',#7196,.T.);
#5961=FACE_OUTER_BOUND('',#7197,.T.);
#5962=FACE_OUTER_BOUND('',#7198,.T.);
#5963=FACE_OUTER_BOUND('',#7199,.T.);
#5964=FACE_OUTER_BOUND('',#7200,.T.);
#5965=FACE_OUTER_BOUND('',#7201,.T.);
#5966=FACE_OUTER_BOUND('',#7202,.T.);
#5967=FACE_OUTER_BOUND('',#7203,.T.);
#5968=FACE_OUTER_BOUND('',#7204,.T.);
#5969=FACE_OUTER_BOUND('',#7205,.T.);
#5970=FACE_OUTER_BOUND('',#7206,.T.);
#5971=FACE_OUTER_BOUND('',#7207,.T.);
#5972=FACE_OUTER_BOUND('',#7208,.T.);
#5973=FACE_OUTER_BOUND('',#7209,.T.);
#5974=FACE_OUTER_BOUND('',#7210,.T.);
#5975=FACE_OUTER_BOUND('',#7211,.T.);
#5976=FACE_OUTER_BOUND('',#7212,.T.);
#5977=FACE_OUTER_BOUND('',#7213,.T.);
#5978=FACE_OUTER_BOUND('',#7214,.T.);
#5979=FACE_OUTER_BOUND('',#7215,.T.);
#5980=FACE_OUTER_BOUND('',#7216,.T.);
#5981=FACE_OUTER_BOUND('',#7217,.T.);
#5982=FACE_OUTER_BOUND('',#7218,.T.);
#5983=FACE_OUTER_BOUND('',#7219,.T.);
#5984=FACE_OUTER_BOUND('',#7220,.T.);
#5985=FACE_OUTER_BOUND('',#7221,.T.);
#5986=FACE_OUTER_BOUND('',#7222,.T.);
#5987=FACE_OUTER_BOUND('',#7223,.T.);
#5988=FACE_OUTER_BOUND('',#7224,.T.);
#5989=FACE_OUTER_BOUND('',#7225,.T.);
#5990=FACE_OUTER_BOUND('',#7227,.T.);
#5991=FACE_OUTER_BOUND('',#7228,.T.);
#5992=FACE_OUTER_BOUND('',#7229,.T.);
#5993=FACE_OUTER_BOUND('',#7230,.T.);
#5994=FACE_OUTER_BOUND('',#7231,.T.);
#5995=FACE_OUTER_BOUND('',#7232,.T.);
#5996=FACE_OUTER_BOUND('',#7233,.T.);
#5997=FACE_OUTER_BOUND('',#7234,.T.);
#5998=FACE_OUTER_BOUND('',#7235,.T.);
#5999=FACE_OUTER_BOUND('',#7236,.T.);
#6000=FACE_OUTER_BOUND('',#7237,.T.);
#6001=FACE_OUTER_BOUND('',#7238,.T.);
#6002=FACE_OUTER_BOUND('',#7239,.T.);
#6003=FACE_OUTER_BOUND('',#7240,.T.);
#6004=FACE_OUTER_BOUND('',#7241,.T.);
#6005=FACE_OUTER_BOUND('',#7242,.T.);
#6006=FACE_OUTER_BOUND('',#7243,.T.);
#6007=FACE_OUTER_BOUND('',#7244,.T.);
#6008=FACE_OUTER_BOUND('',#7245,.T.);
#6009=FACE_OUTER_BOUND('',#7246,.T.);
#6010=FACE_OUTER_BOUND('',#7249,.T.);
#6011=FACE_OUTER_BOUND('',#7250,.T.);
#6012=FACE_OUTER_BOUND('',#7251,.T.);
#6013=FACE_OUTER_BOUND('',#7252,.T.);
#6014=FACE_OUTER_BOUND('',#7254,.T.);
#6015=FACE_OUTER_BOUND('',#7255,.T.);
#6016=FACE_OUTER_BOUND('',#7257,.T.);
#6017=FACE_OUTER_BOUND('',#7258,.T.);
#6018=FACE_OUTER_BOUND('',#7260,.T.);
#6019=FACE_OUTER_BOUND('',#7261,.T.);
#6020=FACE_OUTER_BOUND('',#7262,.T.);
#6021=FACE_OUTER_BOUND('',#7264,.T.);
#6022=FACE_OUTER_BOUND('',#7265,.T.);
#6023=FACE_OUTER_BOUND('',#7266,.T.);
#6024=FACE_OUTER_BOUND('',#7268,.T.);
#6025=FACE_OUTER_BOUND('',#7269,.T.);
#6026=FACE_OUTER_BOUND('',#7270,.T.);
#6027=FACE_OUTER_BOUND('',#7271,.T.);
#6028=FACE_OUTER_BOUND('',#7272,.T.);
#6029=FACE_OUTER_BOUND('',#7273,.T.);
#6030=FACE_OUTER_BOUND('',#7274,.T.);
#6031=FACE_OUTER_BOUND('',#7275,.T.);
#6032=FACE_OUTER_BOUND('',#7277,.T.);
#6033=FACE_OUTER_BOUND('',#7278,.T.);
#6034=FACE_OUTER_BOUND('',#7279,.T.);
#6035=FACE_OUTER_BOUND('',#7280,.T.);
#6036=FACE_OUTER_BOUND('',#7281,.T.);
#6037=FACE_OUTER_BOUND('',#7282,.T.);
#6038=FACE_OUTER_BOUND('',#7283,.T.);
#6039=FACE_OUTER_BOUND('',#7284,.T.);
#6040=FACE_OUTER_BOUND('',#7285,.T.);
#6041=FACE_OUTER_BOUND('',#7286,.T.);
#6042=FACE_OUTER_BOUND('',#7287,.T.);
#6043=FACE_OUTER_BOUND('',#7288,.T.);
#6044=FACE_OUTER_BOUND('',#7289,.T.);
#6045=FACE_OUTER_BOUND('',#7290,.T.);
#6046=FACE_OUTER_BOUND('',#7291,.T.);
#6047=FACE_OUTER_BOUND('',#7292,.T.);
#6048=FACE_OUTER_BOUND('',#7293,.T.);
#6049=FACE_OUTER_BOUND('',#7294,.T.);
#6050=FACE_OUTER_BOUND('',#7295,.T.);
#6051=FACE_OUTER_BOUND('',#7298,.T.);
#6052=FACE_OUTER_BOUND('',#7299,.T.);
#6053=FACE_OUTER_BOUND('',#7300,.T.);
#6054=FACE_OUTER_BOUND('',#7301,.T.);
#6055=FACE_OUTER_BOUND('',#7302,.T.);
#6056=FACE_OUTER_BOUND('',#7303,.T.);
#6057=FACE_OUTER_BOUND('',#7304,.T.);
#6058=FACE_OUTER_BOUND('',#7305,.T.);
#6059=FACE_OUTER_BOUND('',#7306,.T.);
#6060=FACE_OUTER_BOUND('',#7307,.T.);
#6061=FACE_OUTER_BOUND('',#7310,.T.);
#6062=FACE_OUTER_BOUND('',#7311,.T.);
#6063=FACE_OUTER_BOUND('',#7312,.T.);
#6064=FACE_OUTER_BOUND('',#7313,.T.);
#6065=FACE_OUTER_BOUND('',#7314,.T.);
#6066=FACE_OUTER_BOUND('',#7315,.T.);
#6067=FACE_OUTER_BOUND('',#7316,.T.);
#6068=FACE_OUTER_BOUND('',#7317,.T.);
#6069=FACE_OUTER_BOUND('',#7318,.T.);
#6070=FACE_OUTER_BOUND('',#7319,.T.);
#6071=FACE_OUTER_BOUND('',#7320,.T.);
#6072=FACE_OUTER_BOUND('',#7321,.T.);
#6073=FACE_OUTER_BOUND('',#7322,.T.);
#6074=FACE_OUTER_BOUND('',#7323,.T.);
#6075=FACE_OUTER_BOUND('',#7324,.T.);
#6076=FACE_OUTER_BOUND('',#7325,.T.);
#6077=FACE_OUTER_BOUND('',#7326,.T.);
#6078=FACE_OUTER_BOUND('',#7327,.T.);
#6079=FACE_OUTER_BOUND('',#7328,.T.);
#6080=FACE_OUTER_BOUND('',#7329,.T.);
#6081=FACE_OUTER_BOUND('',#7330,.T.);
#6082=FACE_OUTER_BOUND('',#7331,.T.);
#6083=FACE_OUTER_BOUND('',#7332,.T.);
#6084=FACE_OUTER_BOUND('',#7333,.T.);
#6085=FACE_OUTER_BOUND('',#7334,.T.);
#6086=FACE_OUTER_BOUND('',#7335,.T.);
#6087=FACE_OUTER_BOUND('',#7336,.T.);
#6088=FACE_OUTER_BOUND('',#7337,.T.);
#6089=FACE_OUTER_BOUND('',#7338,.T.);
#6090=FACE_OUTER_BOUND('',#7339,.T.);
#6091=FACE_OUTER_BOUND('',#7340,.T.);
#6092=FACE_OUTER_BOUND('',#7341,.T.);
#6093=FACE_OUTER_BOUND('',#7344,.T.);
#6094=FACE_OUTER_BOUND('',#7345,.T.);
#6095=FACE_OUTER_BOUND('',#7346,.T.);
#6096=FACE_OUTER_BOUND('',#7347,.T.);
#6097=FACE_OUTER_BOUND('',#7348,.T.);
#6098=FACE_OUTER_BOUND('',#7349,.T.);
#6099=FACE_OUTER_BOUND('',#7350,.T.);
#6100=FACE_OUTER_BOUND('',#7353,.T.);
#6101=FACE_OUTER_BOUND('',#7354,.T.);
#6102=FACE_OUTER_BOUND('',#7355,.T.);
#6103=FACE_OUTER_BOUND('',#7356,.T.);
#6104=FACE_OUTER_BOUND('',#7357,.T.);
#6105=FACE_OUTER_BOUND('',#7358,.T.);
#6106=FACE_OUTER_BOUND('',#7359,.T.);
#6107=FACE_OUTER_BOUND('',#7360,.T.);
#6108=FACE_OUTER_BOUND('',#7361,.T.);
#6109=FACE_OUTER_BOUND('',#7362,.T.);
#6110=FACE_OUTER_BOUND('',#7363,.T.);
#6111=FACE_OUTER_BOUND('',#7365,.T.);
#6112=FACE_OUTER_BOUND('',#7366,.T.);
#6113=FACE_OUTER_BOUND('',#7367,.T.);
#6114=FACE_OUTER_BOUND('',#7369,.T.);
#6115=FACE_OUTER_BOUND('',#7370,.T.);
#6116=FACE_OUTER_BOUND('',#7372,.T.);
#6117=FACE_OUTER_BOUND('',#7373,.T.);
#6118=FACE_OUTER_BOUND('',#7375,.T.);
#6119=FACE_OUTER_BOUND('',#7376,.T.);
#6120=FACE_OUTER_BOUND('',#7378,.T.);
#6121=FACE_OUTER_BOUND('',#7379,.T.);
#6122=FACE_OUTER_BOUND('',#7381,.T.);
#6123=FACE_OUTER_BOUND('',#7383,.T.);
#6124=FACE_OUTER_BOUND('',#7384,.T.);
#6125=FACE_OUTER_BOUND('',#7386,.T.);
#6126=FACE_OUTER_BOUND('',#7387,.T.);
#6127=FACE_OUTER_BOUND('',#7389,.T.);
#6128=FACE_OUTER_BOUND('',#7390,.T.);
#6129=FACE_OUTER_BOUND('',#7392,.T.);
#6130=FACE_OUTER_BOUND('',#7393,.T.);
#6131=FACE_OUTER_BOUND('',#7394,.T.);
#6132=FACE_OUTER_BOUND('',#7395,.T.);
#6133=FACE_OUTER_BOUND('',#7396,.T.);
#6134=FACE_OUTER_BOUND('',#7398,.T.);
#6135=FACE_OUTER_BOUND('',#7399,.T.);
#6136=FACE_OUTER_BOUND('',#7401,.T.);
#6137=FACE_OUTER_BOUND('',#7402,.T.);
#6138=FACE_OUTER_BOUND('',#7403,.T.);
#6139=FACE_OUTER_BOUND('',#7404,.T.);
#6140=FACE_OUTER_BOUND('',#7406,.T.);
#6141=FACE_OUTER_BOUND('',#7407,.T.);
#6142=FACE_OUTER_BOUND('',#7409,.T.);
#6143=FACE_OUTER_BOUND('',#7410,.T.);
#6144=FACE_OUTER_BOUND('',#7411,.T.);
#6145=FACE_OUTER_BOUND('',#7412,.T.);
#6146=FACE_OUTER_BOUND('',#7413,.T.);
#6147=FACE_OUTER_BOUND('',#7414,.T.);
#6148=FACE_OUTER_BOUND('',#7415,.T.);
#6149=FACE_OUTER_BOUND('',#7416,.T.);
#6150=FACE_OUTER_BOUND('',#7417,.T.);
#6151=FACE_OUTER_BOUND('',#7418,.T.);
#6152=FACE_OUTER_BOUND('',#7419,.T.);
#6153=FACE_OUTER_BOUND('',#7420,.T.);
#6154=FACE_OUTER_BOUND('',#7421,.T.);
#6155=FACE_OUTER_BOUND('',#7422,.T.);
#6156=FACE_OUTER_BOUND('',#7424,.T.);
#6157=FACE_OUTER_BOUND('',#7425,.T.);
#6158=FACE_OUTER_BOUND('',#7426,.T.);
#6159=FACE_OUTER_BOUND('',#7428,.T.);
#6160=FACE_OUTER_BOUND('',#7429,.T.);
#6161=FACE_OUTER_BOUND('',#7431,.T.);
#6162=FACE_OUTER_BOUND('',#7432,.T.);
#6163=FACE_OUTER_BOUND('',#7434,.T.);
#6164=FACE_OUTER_BOUND('',#7435,.T.);
#6165=FACE_OUTER_BOUND('',#7436,.T.);
#6166=FACE_OUTER_BOUND('',#7437,.T.);
#6167=FACE_OUTER_BOUND('',#7438,.T.);
#6168=FACE_OUTER_BOUND('',#7439,.T.);
#6169=FACE_OUTER_BOUND('',#7440,.T.);
#6170=FACE_OUTER_BOUND('',#7441,.T.);
#6171=FACE_OUTER_BOUND('',#7442,.T.);
#6172=FACE_OUTER_BOUND('',#7443,.T.);
#6173=FACE_OUTER_BOUND('',#7445,.T.);
#6174=FACE_OUTER_BOUND('',#7446,.T.);
#6175=FACE_OUTER_BOUND('',#7448,.T.);
#6176=FACE_OUTER_BOUND('',#7449,.T.);
#6177=FACE_OUTER_BOUND('',#7450,.T.);
#6178=FACE_OUTER_BOUND('',#7451,.T.);
#6179=FACE_OUTER_BOUND('',#7452,.T.);
#6180=FACE_OUTER_BOUND('',#7454,.T.);
#6181=FACE_OUTER_BOUND('',#7455,.T.);
#6182=FACE_OUTER_BOUND('',#7456,.T.);
#6183=EDGE_LOOP('',(#12899,#12900,#12901,#12902,#12903,#12904,#12905,#12906,
#12907,#12908,#12909,#12910,#12911,#12912,#12913));
#6184=EDGE_LOOP('',(#12914,#12915,#12916,#12917,#12918,#12919));
#6185=EDGE_LOOP('',(#12920,#12921,#12922,#12923,#12924,#12925,#12926,#12927,
#12928,#12929,#12930,#12931,#12932,#12933,#12934,#12935,#12936,#12937,#12938,
#12939,#12940,#12941,#12942,#12943,#12944,#12945,#12946,#12947,#12948,#12949,
#12950,#12951,#12952,#12953,#12954,#12955,#12956,#12957,#12958,#12959,#12960,
#12961,#12962,#12963,#12964,#12965,#12966,#12967,#12968,#12969,#12970,#12971,
#12972,#12973,#12974,#12975,#12976,#12977,#12978,#12979,#12980,#12981,#12982,
#12983,#12984,#12985,#12986,#12987));
#6186=EDGE_LOOP('',(#12988,#12989,#12990,#12991,#12992,#12993,#12994,#12995,
#12996,#12997,#12998));
#6187=EDGE_LOOP('',(#12999,#13000,#13001));
#6188=EDGE_LOOP('',(#13002,#13003,#13004,#13005,#13006,#13007,#13008,#13009,
#13010,#13011));
#6189=EDGE_LOOP('',(#13012,#13013,#13014));
#6190=EDGE_LOOP('',(#13015,#13016,#13017,#13018,#13019,#13020,#13021,#13022,
#13023,#13024,#13025));
#6191=EDGE_LOOP('',(#13026,#13027,#13028,#13029,#13030,#13031,#13032,#13033,
#13034,#13035,#13036,#13037,#13038,#13039,#13040));
#6192=EDGE_LOOP('',(#13041,#13042,#13043,#13044,#13045,#13046,#13047,#13048,
#13049,#13050,#13051,#13052,#13053,#13054,#13055,#13056,#13057,#13058,#13059,
#13060,#13061,#13062,#13063,#13064,#13065,#13066,#13067,#13068,#13069,#13070,
#13071,#13072,#13073,#13074,#13075,#13076,#13077,#13078,#13079,#13080,#13081,
#13082,#13083,#13084,#13085,#13086,#13087,#13088,#13089,#13090,#13091,#13092,
#13093,#13094,#13095,#13096,#13097,#13098,#13099,#13100,#13101,#13102,#13103,
#13104,#13105,#13106,#13107,#13108));
#6193=EDGE_LOOP('',(#13109,#13110,#13111,#13112,#13113,#13114,#13115,#13116,
#13117,#13118,#13119));
#6194=EDGE_LOOP('',(#13120,#13121,#13122));
#6195=EDGE_LOOP('',(#13123,#13124,#13125));
#6196=EDGE_LOOP('',(#13126,#13127,#13128,#13129,#13130,#13131,#13132,#13133,
#13134,#13135,#13136));
#6197=EDGE_LOOP('',(#13137,#13138,#13139,#13140,#13141,#13142,#13143,#13144,
#13145,#13146,#13147,#13148,#13149,#13150,#13151));
#6198=EDGE_LOOP('',(#13152,#13153,#13154,#13155,#13156,#13157));
#6199=EDGE_LOOP('',(#13158,#13159,#13160,#13161,#13162,#13163,#13164,#13165,
#13166,#13167,#13168,#13169,#13170,#13171,#13172));
#6200=EDGE_LOOP('',(#13173,#13174,#13175,#13176,#13177,#13178,#13179));
#6201=EDGE_LOOP('',(#13180,#13181,#13182,#13183,#13184,#13185));
#6202=EDGE_LOOP('',(#13186,#13187,#13188,#13189,#13190,#13191,#13192));
#6203=EDGE_LOOP('',(#13193,#13194,#13195,#13196,#13197,#13198,#13199));
#6204=EDGE_LOOP('',(#13200,#13201,#13202,#13203,#13204,#13205));
#6205=EDGE_LOOP('',(#13206,#13207,#13208,#13209,#13210,#13211,#13212));
#6206=EDGE_LOOP('',(#13213,#13214,#13215,#13216));
#6207=EDGE_LOOP('',(#13217,#13218,#13219,#13220,#13221));
#6208=EDGE_LOOP('',(#13222,#13223,#13224,#13225,#13226));
#6209=EDGE_LOOP('',(#13227,#13228,#13229,#13230,#13231,#13232,#13233,#13234));
#6210=EDGE_LOOP('',(#13235,#13236,#13237,#13238));
#6211=EDGE_LOOP('',(#13239,#13240,#13241,#13242));
#6212=EDGE_LOOP('',(#13243,#13244,#13245,#13246));
#6213=EDGE_LOOP('',(#13247,#13248,#13249,#13250,#13251));
#6214=EDGE_LOOP('',(#13252,#13253,#13254,#13255,#13256,#13257));
#6215=EDGE_LOOP('',(#13258,#13259,#13260,#13261,#13262));
#6216=EDGE_LOOP('',(#13263,#13264,#13265,#13266));
#6217=EDGE_LOOP('',(#13267,#13268,#13269,#13270));
#6218=EDGE_LOOP('',(#13271,#13272,#13273,#13274));
#6219=EDGE_LOOP('',(#13275,#13276,#13277,#13278,#13279));
#6220=EDGE_LOOP('',(#13280,#13281,#13282,#13283,#13284,#13285));
#6221=EDGE_LOOP('',(#13286,#13287,#13288,#13289,#13290,#13291));
#6222=EDGE_LOOP('',(#13292,#13293,#13294,#13295,#13296));
#6223=EDGE_LOOP('',(#13297,#13298,#13299,#13300));
#6224=EDGE_LOOP('',(#13301,#13302,#13303,#13304,#13305));
#6225=EDGE_LOOP('',(#13306,#13307,#13308,#13309));
#6226=EDGE_LOOP('',(#13310,#13311,#13312,#13313));
#6227=EDGE_LOOP('',(#13314,#13315,#13316,#13317));
#6228=EDGE_LOOP('',(#13318,#13319,#13320,#13321));
#6229=EDGE_LOOP('',(#13322,#13323,#13324,#13325));
#6230=EDGE_LOOP('',(#13326,#13327,#13328,#13329));
#6231=EDGE_LOOP('',(#13330,#13331,#13332,#13333));
#6232=EDGE_LOOP('',(#13334,#13335,#13336,#13337));
#6233=EDGE_LOOP('',(#13338,#13339,#13340,#13341));
#6234=EDGE_LOOP('',(#13342,#13343,#13344,#13345,#13346));
#6235=EDGE_LOOP('',(#13347,#13348,#13349,#13350,#13351));
#6236=EDGE_LOOP('',(#13352,#13353,#13354,#13355,#13356));
#6237=EDGE_LOOP('',(#13357,#13358,#13359,#13360,#13361,#13362));
#6238=EDGE_LOOP('',(#13363,#13364,#13365,#13366,#13367,#13368));
#6239=EDGE_LOOP('',(#13369,#13370,#13371,#13372,#13373));
#6240=EDGE_LOOP('',(#13374,#13375,#13376,#13377));
#6241=EDGE_LOOP('',(#13378,#13379,#13380,#13381));
#6242=EDGE_LOOP('',(#13382,#13383,#13384,#13385));
#6243=EDGE_LOOP('',(#13386,#13387,#13388,#13389,#13390));
#6244=EDGE_LOOP('',(#13391,#13392,#13393,#13394,#13395,#13396));
#6245=EDGE_LOOP('',(#13397,#13398,#13399,#13400,#13401));
#6246=EDGE_LOOP('',(#13402,#13403,#13404,#13405));
#6247=EDGE_LOOP('',(#13406,#13407,#13408,#13409));
#6248=EDGE_LOOP('',(#13410,#13411,#13412,#13413));
#6249=EDGE_LOOP('',(#13414,#13415,#13416,#13417,#13418));
#6250=EDGE_LOOP('',(#13419,#13420,#13421,#13422));
#6251=EDGE_LOOP('',(#13423,#13424,#13425,#13426));
#6252=EDGE_LOOP('',(#13427,#13428,#13429,#13430));
#6253=EDGE_LOOP('',(#13431,#13432,#13433,#13434));
#6254=EDGE_LOOP('',(#13435,#13436,#13437,#13438));
#6255=EDGE_LOOP('',(#13439,#13440,#13441,#13442));
#6256=EDGE_LOOP('',(#13443,#13444,#13445,#13446));
#6257=EDGE_LOOP('',(#13447,#13448,#13449,#13450));
#6258=EDGE_LOOP('',(#13451,#13452,#13453,#13454));
#6259=EDGE_LOOP('',(#13455,#13456,#13457,#13458));
#6260=EDGE_LOOP('',(#13459,#13460,#13461,#13462));
#6261=EDGE_LOOP('',(#13463,#13464,#13465,#13466));
#6262=EDGE_LOOP('',(#13467,#13468,#13469,#13470));
#6263=EDGE_LOOP('',(#13471,#13472,#13473,#13474));
#6264=EDGE_LOOP('',(#13475,#13476,#13477,#13478));
#6265=EDGE_LOOP('',(#13479,#13480,#13481,#13482));
#6266=EDGE_LOOP('',(#13483,#13484,#13485,#13486));
#6267=EDGE_LOOP('',(#13487,#13488,#13489,#13490));
#6268=EDGE_LOOP('',(#13491,#13492,#13493,#13494));
#6269=EDGE_LOOP('',(#13495,#13496,#13497,#13498,#13499));
#6270=EDGE_LOOP('',(#13500,#13501,#13502,#13503,#13504));
#6271=EDGE_LOOP('',(#13505,#13506,#13507,#13508));
#6272=EDGE_LOOP('',(#13509,#13510,#13511,#13512,#13513));
#6273=EDGE_LOOP('',(#13514,#13515,#13516,#13517));
#6274=EDGE_LOOP('',(#13518,#13519,#13520,#13521));
#6275=EDGE_LOOP('',(#13522,#13523,#13524,#13525));
#6276=EDGE_LOOP('',(#13526,#13527,#13528,#13529,#13530));
#6277=EDGE_LOOP('',(#13531,#13532,#13533,#13534));
#6278=EDGE_LOOP('',(#13535,#13536,#13537,#13538));
#6279=EDGE_LOOP('',(#13539,#13540,#13541,#13542,#13543,#13544));
#6280=EDGE_LOOP('',(#13545,#13546,#13547,#13548,#13549,#13550));
#6281=EDGE_LOOP('',(#13551,#13552,#13553,#13554,#13555,#13556));
#6282=EDGE_LOOP('',(#13557,#13558,#13559,#13560));
#6283=EDGE_LOOP('',(#13561,#13562,#13563));
#6284=EDGE_LOOP('',(#13564,#13565,#13566));
#6285=EDGE_LOOP('',(#13567,#13568,#13569,#13570));
#6286=EDGE_LOOP('',(#13571,#13572,#13573,#13574));
#6287=EDGE_LOOP('',(#13575,#13576,#13577,#13578));
#6288=EDGE_LOOP('',(#13579,#13580,#13581,#13582));
#6289=EDGE_LOOP('',(#13583,#13584,#13585));
#6290=EDGE_LOOP('',(#13586,#13587,#13588));
#6291=EDGE_LOOP('',(#13589,#13590,#13591,#13592));
#6292=EDGE_LOOP('',(#13593,#13594,#13595,#13596));
#6293=EDGE_LOOP('',(#13597,#13598,#13599,#13600));
#6294=EDGE_LOOP('',(#13601,#13602,#13603));
#6295=EDGE_LOOP('',(#13604,#13605,#13606));
#6296=EDGE_LOOP('',(#13607,#13608,#13609,#13610));
#6297=EDGE_LOOP('',(#13611,#13612,#13613,#13614));
#6298=EDGE_LOOP('',(#13615,#13616,#13617,#13618));
#6299=EDGE_LOOP('',(#13619,#13620,#13621));
#6300=EDGE_LOOP('',(#13622,#13623,#13624));
#6301=EDGE_LOOP('',(#13625,#13626,#13627,#13628));
#6302=EDGE_LOOP('',(#13629,#13630,#13631,#13632));
#6303=EDGE_LOOP('',(#13633,#13634,#13635,#13636));
#6304=EDGE_LOOP('',(#13637,#13638,#13639));
#6305=EDGE_LOOP('',(#13640,#13641,#13642));
#6306=EDGE_LOOP('',(#13643,#13644,#13645,#13646));
#6307=EDGE_LOOP('',(#13647,#13648,#13649,#13650));
#6308=EDGE_LOOP('',(#13651,#13652,#13653,#13654));
#6309=EDGE_LOOP('',(#13655,#13656,#13657,#13658));
#6310=EDGE_LOOP('',(#13659,#13660,#13661));
#6311=EDGE_LOOP('',(#13662,#13663,#13664));
#6312=EDGE_LOOP('',(#13665,#13666,#13667,#13668));
#6313=EDGE_LOOP('',(#13669,#13670,#13671,#13672));
#6314=EDGE_LOOP('',(#13673,#13674,#13675,#13676,#13677));
#6315=EDGE_LOOP('',(#13678,#13679,#13680,#13681,#13682,#13683,#13684,#13685,
#13686,#13687,#13688,#13689,#13690,#13691,#13692,#13693,#13694,#13695,#13696,
#13697,#13698,#13699,#13700,#13701));
#6316=EDGE_LOOP('',(#13702));
#6317=EDGE_LOOP('',(#13703,#13704,#13705,#13706));
#6318=EDGE_LOOP('',(#13707,#13708,#13709,#13710,#13711,#13712,#13713,#13714));
#6319=EDGE_LOOP('',(#13715));
#6320=EDGE_LOOP('',(#13716,#13717,#13718,#13719,#13720,#13721,#13722,#13723));
#6321=EDGE_LOOP('',(#13724));
#6322=EDGE_LOOP('',(#13725));
#6323=EDGE_LOOP('',(#13726,#13727,#13728,#13729,#13730,#13731));
#6324=EDGE_LOOP('',(#13732,#13733,#13734,#13735,#13736));
#6325=EDGE_LOOP('',(#13737,#13738,#13739,#13740,#13741,#13742));
#6326=EDGE_LOOP('',(#13743,#13744,#13745,#13746,#13747));
#6327=EDGE_LOOP('',(#13748,#13749,#13750,#13751));
#6328=EDGE_LOOP('',(#13752,#13753,#13754,#13755));
#6329=EDGE_LOOP('',(#13756,#13757,#13758,#13759));
#6330=EDGE_LOOP('',(#13760,#13761,#13762,#13763));
#6331=EDGE_LOOP('',(#13764,#13765,#13766,#13767));
#6332=EDGE_LOOP('',(#13768,#13769,#13770,#13771));
#6333=EDGE_LOOP('',(#13772,#13773,#13774,#13775));
#6334=EDGE_LOOP('',(#13776,#13777,#13778,#13779));
#6335=EDGE_LOOP('',(#13780,#13781,#13782));
#6336=EDGE_LOOP('',(#13783,#13784,#13785,#13786));
#6337=EDGE_LOOP('',(#13787,#13788,#13789));
#6338=EDGE_LOOP('',(#13790,#13791,#13792,#13793));
#6339=EDGE_LOOP('',(#13794,#13795,#13796,#13797));
#6340=EDGE_LOOP('',(#13798,#13799,#13800,#13801));
#6341=EDGE_LOOP('',(#13802,#13803,#13804,#13805));
#6342=EDGE_LOOP('',(#13806,#13807,#13808));
#6343=EDGE_LOOP('',(#13809,#13810,#13811,#13812));
#6344=EDGE_LOOP('',(#13813,#13814,#13815));
#6345=EDGE_LOOP('',(#13816,#13817,#13818));
#6346=EDGE_LOOP('',(#13819,#13820,#13821,#13822));
#6347=EDGE_LOOP('',(#13823,#13824,#13825));
#6348=EDGE_LOOP('',(#13826,#13827,#13828,#13829));
#6349=EDGE_LOOP('',(#13830,#13831,#13832));
#6350=EDGE_LOOP('',(#13833,#13834,#13835,#13836));
#6351=EDGE_LOOP('',(#13837,#13838,#13839,#13840));
#6352=EDGE_LOOP('',(#13841,#13842,#13843));
#6353=EDGE_LOOP('',(#13844,#13845,#13846,#13847));
#6354=EDGE_LOOP('',(#13848,#13849,#13850));
#6355=EDGE_LOOP('',(#13851,#13852,#13853,#13854));
#6356=EDGE_LOOP('',(#13855,#13856,#13857));
#6357=EDGE_LOOP('',(#13858,#13859,#13860,#13861));
#6358=EDGE_LOOP('',(#13862,#13863,#13864));
#6359=EDGE_LOOP('',(#13865,#13866,#13867,#13868));
#6360=EDGE_LOOP('',(#13869,#13870,#13871,#13872));
#6361=EDGE_LOOP('',(#13873,#13874,#13875,#13876));
#6362=EDGE_LOOP('',(#13877,#13878,#13879,#13880));
#6363=EDGE_LOOP('',(#13881,#13882,#13883,#13884));
#6364=EDGE_LOOP('',(#13885,#13886,#13887));
#6365=EDGE_LOOP('',(#13888,#13889,#13890));
#6366=EDGE_LOOP('',(#13891,#13892,#13893,#13894));
#6367=EDGE_LOOP('',(#13895,#13896,#13897,#13898));
#6368=EDGE_LOOP('',(#13899,#13900,#13901));
#6369=EDGE_LOOP('',(#13902,#13903,#13904,#13905));
#6370=EDGE_LOOP('',(#13906,#13907,#13908,#13909));
#6371=EDGE_LOOP('',(#13910,#13911,#13912,#13913));
#6372=EDGE_LOOP('',(#13914,#13915,#13916,#13917));
#6373=EDGE_LOOP('',(#13918,#13919,#13920,#13921));
#6374=EDGE_LOOP('',(#13922,#13923,#13924));
#6375=EDGE_LOOP('',(#13925,#13926,#13927,#13928));
#6376=EDGE_LOOP('',(#13929,#13930,#13931));
#6377=EDGE_LOOP('',(#13932,#13933,#13934,#13935));
#6378=EDGE_LOOP('',(#13936,#13937,#13938,#13939));
#6379=EDGE_LOOP('',(#13940,#13941,#13942,#13943));
#6380=EDGE_LOOP('',(#13944,#13945,#13946,#13947));
#6381=EDGE_LOOP('',(#13948,#13949,#13950,#13951));
#6382=EDGE_LOOP('',(#13952,#13953,#13954,#13955));
#6383=EDGE_LOOP('',(#13956,#13957,#13958,#13959,#13960));
#6384=EDGE_LOOP('',(#13961,#13962,#13963,#13964,#13965,#13966));
#6385=EDGE_LOOP('',(#13967,#13968,#13969));
#6386=EDGE_LOOP('',(#13970,#13971,#13972,#13973));
#6387=EDGE_LOOP('',(#13974,#13975,#13976));
#6388=EDGE_LOOP('',(#13977,#13978,#13979,#13980));
#6389=EDGE_LOOP('',(#13981,#13982,#13983));
#6390=EDGE_LOOP('',(#13984,#13985,#13986,#13987));
#6391=EDGE_LOOP('',(#13988,#13989,#13990));
#6392=EDGE_LOOP('',(#13991,#13992,#13993,#13994));
#6393=EDGE_LOOP('',(#13995,#13996,#13997,#13998));
#6394=EDGE_LOOP('',(#13999,#14000,#14001,#14002));
#6395=EDGE_LOOP('',(#14003,#14004,#14005));
#6396=EDGE_LOOP('',(#14006,#14007,#14008,#14009));
#6397=EDGE_LOOP('',(#14010,#14011,#14012,#14013));
#6398=EDGE_LOOP('',(#14014,#14015,#14016,#14017));
#6399=EDGE_LOOP('',(#14018,#14019,#14020));
#6400=EDGE_LOOP('',(#14021,#14022,#14023,#14024));
#6401=EDGE_LOOP('',(#14025,#14026,#14027));
#6402=EDGE_LOOP('',(#14028,#14029,#14030,#14031));
#6403=EDGE_LOOP('',(#14032,#14033,#14034));
#6404=EDGE_LOOP('',(#14035,#14036,#14037,#14038));
#6405=EDGE_LOOP('',(#14039,#14040,#14041));
#6406=EDGE_LOOP('',(#14042,#14043,#14044,#14045));
#6407=EDGE_LOOP('',(#14046,#14047,#14048));
#6408=EDGE_LOOP('',(#14049,#14050,#14051,#14052));
#6409=EDGE_LOOP('',(#14053,#14054,#14055));
#6410=EDGE_LOOP('',(#14056,#14057,#14058,#14059));
#6411=EDGE_LOOP('',(#14060,#14061,#14062,#14063));
#6412=EDGE_LOOP('',(#14064,#14065,#14066,#14067));
#6413=EDGE_LOOP('',(#14068,#14069,#14070,#14071));
#6414=EDGE_LOOP('',(#14072,#14073,#14074,#14075));
#6415=EDGE_LOOP('',(#14076,#14077,#14078,#14079));
#6416=EDGE_LOOP('',(#14080,#14081,#14082,#14083));
#6417=EDGE_LOOP('',(#14084,#14085,#14086,#14087));
#6418=EDGE_LOOP('',(#14088,#14089,#14090,#14091));
#6419=EDGE_LOOP('',(#14092,#14093,#14094,#14095));
#6420=EDGE_LOOP('',(#14096,#14097,#14098,#14099));
#6421=EDGE_LOOP('',(#14100,#14101,#14102,#14103));
#6422=EDGE_LOOP('',(#14104,#14105,#14106,#14107,#14108));
#6423=EDGE_LOOP('',(#14109,#14110,#14111,#14112,#14113,#14114,#14115,#14116,
#14117,#14118,#14119,#14120,#14121,#14122,#14123,#14124,#14125,#14126,#14127,
#14128,#14129,#14130,#14131,#14132));
#6424=EDGE_LOOP('',(#14133,#14134,#14135,#14136,#14137,#14138,#14139,#14140));
#6425=EDGE_LOOP('',(#14141,#14142,#14143,#14144));
#6426=EDGE_LOOP('',(#14145));
#6427=EDGE_LOOP('',(#14146,#14147,#14148,#14149,#14150,#14151,#14152,#14153));
#6428=EDGE_LOOP('',(#14154));
#6429=EDGE_LOOP('',(#14155));
#6430=EDGE_LOOP('',(#14156));
#6431=EDGE_LOOP('',(#14157,#14158,#14159));
#6432=EDGE_LOOP('',(#14160,#14161,#14162,#14163));
#6433=EDGE_LOOP('',(#14164,#14165,#14166,#14167));
#6434=EDGE_LOOP('',(#14168,#14169,#14170,#14171));
#6435=EDGE_LOOP('',(#14172,#14173,#14174));
#6436=EDGE_LOOP('',(#14175,#14176,#14177));
#6437=EDGE_LOOP('',(#14178,#14179,#14180,#14181));
#6438=EDGE_LOOP('',(#14182,#14183,#14184,#14185));
#6439=EDGE_LOOP('',(#14186,#14187,#14188,#14189));
#6440=EDGE_LOOP('',(#14190,#14191,#14192,#14193));
#6441=EDGE_LOOP('',(#14194,#14195,#14196,#14197));
#6442=EDGE_LOOP('',(#14198,#14199,#14200));
#6443=EDGE_LOOP('',(#14201,#14202,#14203,#14204));
#6444=EDGE_LOOP('',(#14205,#14206,#14207,#14208));
#6445=EDGE_LOOP('',(#14209,#14210,#14211,#14212));
#6446=EDGE_LOOP('',(#14213,#14214,#14215,#14216));
#6447=EDGE_LOOP('',(#14217,#14218,#14219,#14220));
#6448=EDGE_LOOP('',(#14221,#14222,#14223));
#6449=EDGE_LOOP('',(#14224,#14225,#14226));
#6450=EDGE_LOOP('',(#14227,#14228,#14229,#14230));
#6451=EDGE_LOOP('',(#14231,#14232,#14233));
#6452=EDGE_LOOP('',(#14234,#14235,#14236,#14237));
#6453=EDGE_LOOP('',(#14238,#14239,#14240,#14241));
#6454=EDGE_LOOP('',(#14242,#14243,#14244));
#6455=EDGE_LOOP('',(#14245,#14246,#14247));
#6456=EDGE_LOOP('',(#14248,#14249,#14250,#14251));
#6457=EDGE_LOOP('',(#14252,#14253,#14254));
#6458=EDGE_LOOP('',(#14255,#14256,#14257,#14258));
#6459=EDGE_LOOP('',(#14259,#14260,#14261,#14262));
#6460=EDGE_LOOP('',(#14263,#14264,#14265));
#6461=EDGE_LOOP('',(#14266,#14267,#14268,#14269));
#6462=EDGE_LOOP('',(#14270,#14271,#14272,#14273));
#6463=EDGE_LOOP('',(#14274,#14275,#14276));
#6464=EDGE_LOOP('',(#14277,#14278,#14279,#14280));
#6465=EDGE_LOOP('',(#14281,#14282,#14283));
#6466=EDGE_LOOP('',(#14284,#14285,#14286,#14287));
#6467=EDGE_LOOP('',(#14288,#14289,#14290,#14291));
#6468=EDGE_LOOP('',(#14292,#14293,#14294,#14295));
#6469=EDGE_LOOP('',(#14296,#14297,#14298));
#6470=EDGE_LOOP('',(#14299,#14300,#14301,#14302));
#6471=EDGE_LOOP('',(#14303,#14304,#14305,#14306));
#6472=EDGE_LOOP('',(#14307,#14308,#14309,#14310));
#6473=EDGE_LOOP('',(#14311,#14312,#14313));
#6474=EDGE_LOOP('',(#14314,#14315,#14316,#14317));
#6475=EDGE_LOOP('',(#14318,#14319,#14320,#14321));
#6476=EDGE_LOOP('',(#14322,#14323,#14324,#14325));
#6477=EDGE_LOOP('',(#14326,#14327,#14328));
#6478=EDGE_LOOP('',(#14329,#14330,#14331,#14332));
#6479=EDGE_LOOP('',(#14333,#14334,#14335,#14336));
#6480=EDGE_LOOP('',(#14337,#14338,#14339,#14340));
#6481=EDGE_LOOP('',(#14341,#14342,#14343));
#6482=EDGE_LOOP('',(#14344,#14345,#14346,#14347));
#6483=EDGE_LOOP('',(#14348,#14349,#14350));
#6484=EDGE_LOOP('',(#14351,#14352,#14353,#14354));
#6485=EDGE_LOOP('',(#14355,#14356,#14357));
#6486=EDGE_LOOP('',(#14358,#14359,#14360,#14361));
#6487=EDGE_LOOP('',(#14362,#14363,#14364,#14365));
#6488=EDGE_LOOP('',(#14366,#14367,#14368,#14369));
#6489=EDGE_LOOP('',(#14370,#14371,#14372,#14373));
#6490=EDGE_LOOP('',(#14374,#14375,#14376,#14377));
#6491=EDGE_LOOP('',(#14378,#14379,#14380));
#6492=EDGE_LOOP('',(#14381,#14382,#14383,#14384));
#6493=EDGE_LOOP('',(#14385,#14386,#14387));
#6494=EDGE_LOOP('',(#14388,#14389,#14390,#14391));
#6495=EDGE_LOOP('',(#14392,#14393,#14394));
#6496=EDGE_LOOP('',(#14395,#14396,#14397,#14398));
#6497=EDGE_LOOP('',(#14399,#14400,#14401));
#6498=EDGE_LOOP('',(#14402,#14403,#14404,#14405));
#6499=EDGE_LOOP('',(#14406,#14407,#14408));
#6500=EDGE_LOOP('',(#14409,#14410,#14411));
#6501=EDGE_LOOP('',(#14412,#14413,#14414,#14415));
#6502=EDGE_LOOP('',(#14416,#14417,#14418,#14419));
#6503=EDGE_LOOP('',(#14420,#14421,#14422,#14423));
#6504=EDGE_LOOP('',(#14424,#14425,#14426,#14427));
#6505=EDGE_LOOP('',(#14428,#14429,#14430,#14431));
#6506=EDGE_LOOP('',(#14432,#14433,#14434,#14435));
#6507=EDGE_LOOP('',(#14436,#14437,#14438,#14439));
#6508=EDGE_LOOP('',(#14440,#14441,#14442,#14443));
#6509=EDGE_LOOP('',(#14444,#14445,#14446,#14447));
#6510=EDGE_LOOP('',(#14448,#14449,#14450,#14451));
#6511=EDGE_LOOP('',(#14452,#14453,#14454,#14455));
#6512=EDGE_LOOP('',(#14456,#14457,#14458,#14459));
#6513=EDGE_LOOP('',(#14460,#14461,#14462,#14463));
#6514=EDGE_LOOP('',(#14464,#14465,#14466,#14467));
#6515=EDGE_LOOP('',(#14468,#14469,#14470,#14471));
#6516=EDGE_LOOP('',(#14472,#14473,#14474,#14475));
#6517=EDGE_LOOP('',(#14476,#14477,#14478,#14479));
#6518=EDGE_LOOP('',(#14480,#14481,#14482,#14483));
#6519=EDGE_LOOP('',(#14484,#14485,#14486,#14487));
#6520=EDGE_LOOP('',(#14488,#14489,#14490,#14491));
#6521=EDGE_LOOP('',(#14492,#14493,#14494,#14495));
#6522=EDGE_LOOP('',(#14496,#14497,#14498,#14499));
#6523=EDGE_LOOP('',(#14500,#14501,#14502,#14503));
#6524=EDGE_LOOP('',(#14504,#14505,#14506,#14507));
#6525=EDGE_LOOP('',(#14508,#14509,#14510,#14511));
#6526=EDGE_LOOP('',(#14512,#14513,#14514,#14515));
#6527=EDGE_LOOP('',(#14516,#14517,#14518,#14519,#14520));
#6528=EDGE_LOOP('',(#14521,#14522,#14523,#14524));
#6529=EDGE_LOOP('',(#14525,#14526,#14527,#14528));
#6530=EDGE_LOOP('',(#14529,#14530,#14531,#14532));
#6531=EDGE_LOOP('',(#14533,#14534,#14535,#14536));
#6532=EDGE_LOOP('',(#14537,#14538,#14539,#14540));
#6533=EDGE_LOOP('',(#14541,#14542,#14543,#14544,#14545));
#6534=EDGE_LOOP('',(#14546,#14547,#14548,#14549,#14550));
#6535=EDGE_LOOP('',(#14551,#14552,#14553,#14554,#14555,#14556));
#6536=EDGE_LOOP('',(#14557,#14558,#14559,#14560,#14561,#14562));
#6537=EDGE_LOOP('',(#14563,#14564,#14565,#14566));
#6538=EDGE_LOOP('',(#14567,#14568,#14569,#14570));
#6539=EDGE_LOOP('',(#14571,#14572,#14573,#14574));
#6540=EDGE_LOOP('',(#14575,#14576,#14577,#14578));
#6541=EDGE_LOOP('',(#14579,#14580,#14581,#14582));
#6542=EDGE_LOOP('',(#14583,#14584,#14585,#14586));
#6543=EDGE_LOOP('',(#14587,#14588,#14589,#14590));
#6544=EDGE_LOOP('',(#14591,#14592,#14593,#14594));
#6545=EDGE_LOOP('',(#14595,#14596,#14597,#14598,#14599,#14600));
#6546=EDGE_LOOP('',(#14601,#14602,#14603,#14604));
#6547=EDGE_LOOP('',(#14605,#14606,#14607,#14608));
#6548=EDGE_LOOP('',(#14609,#14610,#14611,#14612));
#6549=EDGE_LOOP('',(#14613,#14614,#14615,#14616));
#6550=EDGE_LOOP('',(#14617,#14618,#14619,#14620));
#6551=EDGE_LOOP('',(#14621,#14622,#14623,#14624));
#6552=EDGE_LOOP('',(#14625,#14626,#14627,#14628));
#6553=EDGE_LOOP('',(#14629,#14630,#14631,#14632,#14633,#14634));
#6554=EDGE_LOOP('',(#14635,#14636,#14637,#14638));
#6555=EDGE_LOOP('',(#14639,#14640,#14641,#14642));
#6556=EDGE_LOOP('',(#14643,#14644,#14645,#14646));
#6557=EDGE_LOOP('',(#14647,#14648,#14649,#14650,#14651));
#6558=EDGE_LOOP('',(#14652,#14653,#14654,#14655));
#6559=EDGE_LOOP('',(#14656,#14657,#14658,#14659));
#6560=EDGE_LOOP('',(#14660,#14661,#14662,#14663));
#6561=EDGE_LOOP('',(#14664,#14665,#14666,#14667));
#6562=EDGE_LOOP('',(#14668,#14669,#14670,#14671));
#6563=EDGE_LOOP('',(#14672,#14673,#14674,#14675));
#6564=EDGE_LOOP('',(#14676,#14677,#14678,#14679,#14680,#14681));
#6565=EDGE_LOOP('',(#14682,#14683,#14684,#14685));
#6566=EDGE_LOOP('',(#14686,#14687,#14688));
#6567=EDGE_LOOP('',(#14689,#14690,#14691,#14692));
#6568=EDGE_LOOP('',(#14693,#14694,#14695,#14696,#14697,#14698,#14699,#14700,
#14701,#14702,#14703,#14704));
#6569=EDGE_LOOP('',(#14705,#14706,#14707,#14708));
#6570=EDGE_LOOP('',(#14709,#14710,#14711,#14712));
#6571=EDGE_LOOP('',(#14713,#14714,#14715,#14716));
#6572=EDGE_LOOP('',(#14717,#14718,#14719));
#6573=EDGE_LOOP('',(#14720,#14721,#14722,#14723));
#6574=EDGE_LOOP('',(#14724,#14725,#14726,#14727));
#6575=EDGE_LOOP('',(#14728,#14729,#14730,#14731));
#6576=EDGE_LOOP('',(#14732,#14733,#14734,#14735));
#6577=EDGE_LOOP('',(#14736,#14737,#14738,#14739));
#6578=EDGE_LOOP('',(#14740,#14741,#14742,#14743));
#6579=EDGE_LOOP('',(#14744,#14745,#14746,#14747));
#6580=EDGE_LOOP('',(#14748,#14749,#14750,#14751));
#6581=EDGE_LOOP('',(#14752,#14753,#14754));
#6582=EDGE_LOOP('',(#14755,#14756,#14757,#14758));
#6583=EDGE_LOOP('',(#14759,#14760,#14761,#14762));
#6584=EDGE_LOOP('',(#14763,#14764,#14765,#14766));
#6585=EDGE_LOOP('',(#14767,#14768,#14769,#14770));
#6586=EDGE_LOOP('',(#14771,#14772,#14773,#14774));
#6587=EDGE_LOOP('',(#14775,#14776,#14777,#14778));
#6588=EDGE_LOOP('',(#14779,#14780,#14781,#14782));
#6589=EDGE_LOOP('',(#14783,#14784,#14785,#14786));
#6590=EDGE_LOOP('',(#14787,#14788,#14789,#14790));
#6591=EDGE_LOOP('',(#14791,#14792,#14793,#14794));
#6592=EDGE_LOOP('',(#14795,#14796,#14797,#14798));
#6593=EDGE_LOOP('',(#14799,#14800,#14801,#14802));
#6594=EDGE_LOOP('',(#14803,#14804,#14805,#14806));
#6595=EDGE_LOOP('',(#14807,#14808,#14809));
#6596=EDGE_LOOP('',(#14810,#14811,#14812,#14813));
#6597=EDGE_LOOP('',(#14814,#14815,#14816,#14817));
#6598=EDGE_LOOP('',(#14818,#14819,#14820,#14821));
#6599=EDGE_LOOP('',(#14822,#14823,#14824,#14825));
#6600=EDGE_LOOP('',(#14826,#14827,#14828,#14829));
#6601=EDGE_LOOP('',(#14830,#14831,#14832,#14833));
#6602=EDGE_LOOP('',(#14834,#14835,#14836,#14837));
#6603=EDGE_LOOP('',(#14838,#14839,#14840,#14841,#14842,#14843));
#6604=EDGE_LOOP('',(#14844,#14845,#14846,#14847));
#6605=EDGE_LOOP('',(#14848,#14849,#14850,#14851));
#6606=EDGE_LOOP('',(#14852,#14853,#14854,#14855));
#6607=EDGE_LOOP('',(#14856,#14857,#14858,#14859));
#6608=EDGE_LOOP('',(#14860,#14861,#14862,#14863));
#6609=EDGE_LOOP('',(#14864,#14865,#14866,#14867));
#6610=EDGE_LOOP('',(#14868,#14869,#14870,#14871));
#6611=EDGE_LOOP('',(#14872,#14873,#14874,#14875));
#6612=EDGE_LOOP('',(#14876,#14877,#14878,#14879));
#6613=EDGE_LOOP('',(#14880,#14881,#14882,#14883));
#6614=EDGE_LOOP('',(#14884,#14885,#14886,#14887));
#6615=EDGE_LOOP('',(#14888,#14889,#14890,#14891));
#6616=EDGE_LOOP('',(#14892,#14893,#14894,#14895));
#6617=EDGE_LOOP('',(#14896,#14897,#14898,#14899));
#6618=EDGE_LOOP('',(#14900,#14901,#14902,#14903));
#6619=EDGE_LOOP('',(#14904,#14905,#14906,#14907));
#6620=EDGE_LOOP('',(#14908,#14909,#14910,#14911));
#6621=EDGE_LOOP('',(#14912,#14913,#14914,#14915));
#6622=EDGE_LOOP('',(#14916,#14917,#14918,#14919,#14920,#14921,#14922,#14923));
#6623=EDGE_LOOP('',(#14924));
#6624=EDGE_LOOP('',(#14925));
#6625=EDGE_LOOP('',(#14926));
#6626=EDGE_LOOP('',(#14927,#14928,#14929,#14930,#14931));
#6627=EDGE_LOOP('',(#14932));
#6628=EDGE_LOOP('',(#14933));
#6629=EDGE_LOOP('',(#14934,#14935,#14936,#14937,#14938));
#6630=EDGE_LOOP('',(#14939,#14940,#14941,#14942));
#6631=EDGE_LOOP('',(#14943,#14944,#14945,#14946));
#6632=EDGE_LOOP('',(#14947,#14948,#14949,#14950));
#6633=EDGE_LOOP('',(#14951,#14952,#14953,#14954));
#6634=EDGE_LOOP('',(#14955,#14956,#14957,#14958));
#6635=EDGE_LOOP('',(#14959,#14960,#14961,#14962));
#6636=EDGE_LOOP('',(#14963,#14964,#14965,#14966));
#6637=EDGE_LOOP('',(#14967,#14968,#14969,#14970,#14971,#14972,#14973,#14974));
#6638=EDGE_LOOP('',(#14975));
#6639=EDGE_LOOP('',(#14976));
#6640=EDGE_LOOP('',(#14977));
#6641=EDGE_LOOP('',(#14978,#14979,#14980,#14981,#14982));
#6642=EDGE_LOOP('',(#14983));
#6643=EDGE_LOOP('',(#14984));
#6644=EDGE_LOOP('',(#14985,#14986,#14987,#14988,#14989));
#6645=EDGE_LOOP('',(#14990,#14991,#14992,#14993,#14994));
#6646=EDGE_LOOP('',(#14995,#14996,#14997,#14998,#14999,#15000));
#6647=EDGE_LOOP('',(#15001,#15002,#15003,#15004,#15005));
#6648=EDGE_LOOP('',(#15006,#15007,#15008,#15009,#15010));
#6649=EDGE_LOOP('',(#15011,#15012,#15013,#15014,#15015,#15016));
#6650=EDGE_LOOP('',(#15017,#15018,#15019,#15020,#15021));
#6651=EDGE_LOOP('',(#15022,#15023,#15024,#15025,#15026));
#6652=EDGE_LOOP('',(#15027,#15028,#15029,#15030,#15031,#15032));
#6653=EDGE_LOOP('',(#15033,#15034,#15035,#15036,#15037));
#6654=EDGE_LOOP('',(#15038,#15039,#15040,#15041,#15042,#15043,#15044,#15045,
#15046,#15047,#15048));
#6655=EDGE_LOOP('',(#15049));
#6656=EDGE_LOOP('',(#15050));
#6657=EDGE_LOOP('',(#15051));
#6658=EDGE_LOOP('',(#15052,#15053,#15054,#15055,#15056));
#6659=EDGE_LOOP('',(#15057,#15058,#15059,#15060,#15061,#15062));
#6660=EDGE_LOOP('',(#15063,#15064,#15065,#15066,#15067));
#6661=EDGE_LOOP('',(#15068,#15069,#15070,#15071,#15072,#15073,#15074,#15075,
#15076,#15077,#15078));
#6662=EDGE_LOOP('',(#15079));
#6663=EDGE_LOOP('',(#15080));
#6664=EDGE_LOOP('',(#15081));
#6665=EDGE_LOOP('',(#15082,#15083,#15084,#15085,#15086));
#6666=EDGE_LOOP('',(#15087,#15088,#15089,#15090,#15091,#15092));
#6667=EDGE_LOOP('',(#15093,#15094,#15095,#15096,#15097));
#6668=EDGE_LOOP('',(#15098,#15099,#15100,#15101,#15102));
#6669=EDGE_LOOP('',(#15103,#15104,#15105,#15106,#15107,#15108));
#6670=EDGE_LOOP('',(#15109,#15110,#15111,#15112,#15113));
#6671=EDGE_LOOP('',(#15114,#15115,#15116,#15117,#15118));
#6672=EDGE_LOOP('',(#15119,#15120,#15121,#15122,#15123,#15124));
#6673=EDGE_LOOP('',(#15125,#15126,#15127,#15128,#15129,#15130,#15131,#15132,
#15133,#15134));
#6674=EDGE_LOOP('',(#15135));
#6675=EDGE_LOOP('',(#15136,#15137,#15138,#15139));
#6676=EDGE_LOOP('',(#15140,#15141,#15142,#15143));
#6677=EDGE_LOOP('',(#15144));
#6678=EDGE_LOOP('',(#15145,#15146,#15147,#15148,#15149,#15150));
#6679=EDGE_LOOP('',(#15151,#15152,#15153,#15154));
#6680=EDGE_LOOP('',(#15155,#15156,#15157,#15158,#15159,#15160));
#6681=EDGE_LOOP('',(#15161,#15162,#15163,#15164));
#6682=EDGE_LOOP('',(#15165,#15166,#15167,#15168));
#6683=EDGE_LOOP('',(#15169,#15170,#15171,#15172));
#6684=EDGE_LOOP('',(#15173,#15174,#15175,#15176));
#6685=EDGE_LOOP('',(#15177,#15178,#15179,#15180,#15181));
#6686=EDGE_LOOP('',(#15182,#15183,#15184,#15185,#15186,#15187));
#6687=EDGE_LOOP('',(#15188,#15189,#15190,#15191,#15192,#15193,#15194,#15195));
#6688=EDGE_LOOP('',(#15196,#15197,#15198,#15199,#15200,#15201,#15202,#15203));
#6689=EDGE_LOOP('',(#15204));
#6690=EDGE_LOOP('',(#15205));
#6691=EDGE_LOOP('',(#15206,#15207,#15208,#15209));
#6692=EDGE_LOOP('',(#15210,#15211,#15212,#15213));
#6693=EDGE_LOOP('',(#15214,#15215,#15216,#15217));
#6694=EDGE_LOOP('',(#15218,#15219,#15220,#15221));
#6695=EDGE_LOOP('',(#15222,#15223,#15224,#15225,#15226));
#6696=EDGE_LOOP('',(#15227,#15228,#15229,#15230,#15231,#15232));
#6697=EDGE_LOOP('',(#15233,#15234,#15235,#15236,#15237));
#6698=EDGE_LOOP('',(#15238,#15239,#15240,#15241));
#6699=EDGE_LOOP('',(#15242,#15243,#15244,#15245));
#6700=EDGE_LOOP('',(#15246,#15247,#15248,#15249));
#6701=EDGE_LOOP('',(#15250,#15251,#15252,#15253));
#6702=EDGE_LOOP('',(#15254,#15255,#15256,#15257));
#6703=EDGE_LOOP('',(#15258,#15259,#15260,#15261));
#6704=EDGE_LOOP('',(#15262,#15263,#15264,#15265));
#6705=EDGE_LOOP('',(#15266,#15267,#15268,#15269));
#6706=EDGE_LOOP('',(#15270,#15271,#15272,#15273));
#6707=EDGE_LOOP('',(#15274,#15275,#15276,#15277));
#6708=EDGE_LOOP('',(#15278,#15279,#15280,#15281));
#6709=EDGE_LOOP('',(#15282,#15283,#15284,#15285));
#6710=EDGE_LOOP('',(#15286,#15287,#15288,#15289));
#6711=EDGE_LOOP('',(#15290,#15291,#15292,#15293));
#6712=EDGE_LOOP('',(#15294,#15295,#15296,#15297));
#6713=EDGE_LOOP('',(#15298,#15299,#15300,#15301));
#6714=EDGE_LOOP('',(#15302,#15303,#15304,#15305));
#6715=EDGE_LOOP('',(#15306,#15307,#15308,#15309));
#6716=EDGE_LOOP('',(#15310,#15311,#15312,#15313));
#6717=EDGE_LOOP('',(#15314,#15315,#15316,#15317));
#6718=EDGE_LOOP('',(#15318,#15319,#15320,#15321,#15322,#15323));
#6719=EDGE_LOOP('',(#15324,#15325,#15326,#15327));
#6720=EDGE_LOOP('',(#15328,#15329,#15330,#15331,#15332,#15333,#15334,#15335,
#15336,#15337,#15338,#15339,#15340,#15341));
#6721=EDGE_LOOP('',(#15342,#15343,#15344,#15345));
#6722=EDGE_LOOP('',(#15346,#15347,#15348,#15349,#15350,#15351));
#6723=EDGE_LOOP('',(#15352,#15353,#15354,#15355,#15356,#15357));
#6724=EDGE_LOOP('',(#15358,#15359,#15360,#15361));
#6725=EDGE_LOOP('',(#15362,#15363,#15364,#15365,#15366,#15367));
#6726=EDGE_LOOP('',(#15368,#15369,#15370,#15371));
#6727=EDGE_LOOP('',(#15372,#15373,#15374,#15375));
#6728=EDGE_LOOP('',(#15376,#15377,#15378,#15379,#15380,#15381));
#6729=EDGE_LOOP('',(#15382,#15383,#15384,#15385));
#6730=EDGE_LOOP('',(#15386,#15387,#15388,#15389,#15390,#15391,#15392,#15393,
#15394,#15395,#15396,#15397,#15398,#15399));
#6731=EDGE_LOOP('',(#15400,#15401,#15402,#15403));
#6732=EDGE_LOOP('',(#15404,#15405,#15406,#15407,#15408,#15409));
#6733=EDGE_LOOP('',(#15410,#15411,#15412,#15413,#15414,#15415));
#6734=EDGE_LOOP('',(#15416,#15417,#15418,#15419));
#6735=EDGE_LOOP('',(#15420,#15421,#15422,#15423,#15424,#15425));
#6736=EDGE_LOOP('',(#15426,#15427,#15428,#15429));
#6737=EDGE_LOOP('',(#15430,#15431,#15432,#15433));
#6738=EDGE_LOOP('',(#15434,#15435,#15436,#15437));
#6739=EDGE_LOOP('',(#15438,#15439,#15440,#15441));
#6740=EDGE_LOOP('',(#15442,#15443,#15444,#15445));
#6741=EDGE_LOOP('',(#15446,#15447,#15448,#15449,#15450));
#6742=EDGE_LOOP('',(#15451,#15452,#15453,#15454));
#6743=EDGE_LOOP('',(#15455,#15456,#15457));
#6744=EDGE_LOOP('',(#15458,#15459,#15460));
#6745=EDGE_LOOP('',(#15461,#15462,#15463,#15464));
#6746=EDGE_LOOP('',(#15465,#15466,#15467,#15468));
#6747=EDGE_LOOP('',(#15469,#15470,#15471,#15472));
#6748=EDGE_LOOP('',(#15473,#15474,#15475));
#6749=EDGE_LOOP('',(#15476,#15477,#15478,#15479));
#6750=EDGE_LOOP('',(#15480,#15481,#15482,#15483));
#6751=EDGE_LOOP('',(#15484,#15485,#15486,#15487));
#6752=EDGE_LOOP('',(#15488,#15489,#15490));
#6753=EDGE_LOOP('',(#15491,#15492,#15493,#15494));
#6754=EDGE_LOOP('',(#15495,#15496,#15497,#15498));
#6755=EDGE_LOOP('',(#15499,#15500,#15501));
#6756=EDGE_LOOP('',(#15502,#15503,#15504,#15505));
#6757=EDGE_LOOP('',(#15506,#15507,#15508,#15509));
#6758=EDGE_LOOP('',(#15510,#15511,#15512));
#6759=EDGE_LOOP('',(#15513,#15514,#15515));
#6760=EDGE_LOOP('',(#15516,#15517,#15518,#15519));
#6761=EDGE_LOOP('',(#15520,#15521,#15522));
#6762=EDGE_LOOP('',(#15523,#15524,#15525,#15526));
#6763=EDGE_LOOP('',(#15527,#15528,#15529,#15530));
#6764=EDGE_LOOP('',(#15531,#15532,#15533));
#6765=EDGE_LOOP('',(#15534,#15535,#15536,#15537));
#6766=EDGE_LOOP('',(#15538,#15539,#15540,#15541));
#6767=EDGE_LOOP('',(#15542,#15543,#15544,#15545));
#6768=EDGE_LOOP('',(#15546,#15547,#15548));
#6769=EDGE_LOOP('',(#15549,#15550,#15551,#15552));
#6770=EDGE_LOOP('',(#15553,#15554,#15555,#15556));
#6771=EDGE_LOOP('',(#15557,#15558,#15559,#15560));
#6772=EDGE_LOOP('',(#15561,#15562,#15563,#15564));
#6773=EDGE_LOOP('',(#15565,#15566,#15567));
#6774=EDGE_LOOP('',(#15568,#15569,#15570,#15571));
#6775=EDGE_LOOP('',(#15572,#15573,#15574));
#6776=EDGE_LOOP('',(#15575,#15576,#15577,#15578));
#6777=EDGE_LOOP('',(#15579,#15580,#15581,#15582,#15583,#15584,#15585));
#6778=EDGE_LOOP('',(#15586));
#6779=EDGE_LOOP('',(#15587));
#6780=EDGE_LOOP('',(#15588,#15589,#15590,#15591));
#6781=EDGE_LOOP('',(#15592,#15593,#15594,#15595));
#6782=EDGE_LOOP('',(#15596,#15597,#15598,#15599));
#6783=EDGE_LOOP('',(#15600,#15601,#15602,#15603));
#6784=EDGE_LOOP('',(#15604,#15605,#15606,#15607));
#6785=EDGE_LOOP('',(#15608,#15609,#15610,#15611));
#6786=EDGE_LOOP('',(#15612,#15613,#15614,#15615));
#6787=EDGE_LOOP('',(#15616,#15617,#15618,#15619));
#6788=EDGE_LOOP('',(#15620,#15621,#15622,#15623));
#6789=EDGE_LOOP('',(#15624,#15625,#15626,#15627));
#6790=EDGE_LOOP('',(#15628,#15629,#15630,#15631));
#6791=EDGE_LOOP('',(#15632));
#6792=EDGE_LOOP('',(#15633));
#6793=EDGE_LOOP('',(#15634,#15635,#15636,#15637,#15638,#15639,#15640,#15641,
#15642,#15643,#15644,#15645,#15646));
#6794=EDGE_LOOP('',(#15647,#15648,#15649,#15650));
#6795=EDGE_LOOP('',(#15651,#15652,#15653,#15654,#15655));
#6796=EDGE_LOOP('',(#15656,#15657,#15658,#15659,#15660));
#6797=EDGE_LOOP('',(#15661,#15662,#15663,#15664,#15665));
#6798=EDGE_LOOP('',(#15666,#15667,#15668,#15669,#15670));
#6799=EDGE_LOOP('',(#15671,#15672,#15673,#15674));
#6800=EDGE_LOOP('',(#15675,#15676,#15677,#15678));
#6801=EDGE_LOOP('',(#15679,#15680,#15681,#15682));
#6802=EDGE_LOOP('',(#15683,#15684,#15685,#15686,#15687));
#6803=EDGE_LOOP('',(#15688,#15689,#15690,#15691));
#6804=EDGE_LOOP('',(#15692,#15693,#15694,#15695,#15696,#15697,#15698,#15699,
#15700,#15701,#15702,#15703,#15704,#15705,#15706,#15707,#15708,#15709));
#6805=EDGE_LOOP('',(#15710,#15711,#15712,#15713));
#6806=EDGE_LOOP('',(#15714,#15715,#15716,#15717));
#6807=EDGE_LOOP('',(#15718,#15719,#15720,#15721));
#6808=EDGE_LOOP('',(#15722,#15723,#15724,#15725));
#6809=EDGE_LOOP('',(#15726,#15727,#15728,#15729));
#6810=EDGE_LOOP('',(#15730));
#6811=EDGE_LOOP('',(#15731));
#6812=EDGE_LOOP('',(#15732,#15733,#15734,#15735));
#6813=EDGE_LOOP('',(#15736,#15737,#15738,#15739));
#6814=EDGE_LOOP('',(#15740,#15741,#15742,#15743));
#6815=EDGE_LOOP('',(#15744));
#6816=EDGE_LOOP('',(#15745));
#6817=EDGE_LOOP('',(#15746,#15747,#15748,#15749));
#6818=EDGE_LOOP('',(#15750,#15751,#15752,#15753));
#6819=EDGE_LOOP('',(#15754));
#6820=EDGE_LOOP('',(#15755));
#6821=EDGE_LOOP('',(#15756));
#6822=EDGE_LOOP('',(#15757));
#6823=EDGE_LOOP('',(#15758));
#6824=EDGE_LOOP('',(#15759));
#6825=EDGE_LOOP('',(#15760));
#6826=EDGE_LOOP('',(#15761));
#6827=EDGE_LOOP('',(#15762));
#6828=EDGE_LOOP('',(#15763));
#6829=EDGE_LOOP('',(#15764));
#6830=EDGE_LOOP('',(#15765));
#6831=EDGE_LOOP('',(#15766,#15767,#15768,#15769));
#6832=EDGE_LOOP('',(#15770,#15771,#15772,#15773));
#6833=EDGE_LOOP('',(#15774,#15775,#15776,#15777,#15778,#15779,#15780,#15781));
#6834=EDGE_LOOP('',(#15782));
#6835=EDGE_LOOP('',(#15783,#15784,#15785,#15786));
#6836=EDGE_LOOP('',(#15787,#15788,#15789,#15790));
#6837=EDGE_LOOP('',(#15791,#15792,#15793,#15794,#15795));
#6838=EDGE_LOOP('',(#15796,#15797,#15798,#15799,#15800,#15801));
#6839=EDGE_LOOP('',(#15802));
#6840=EDGE_LOOP('',(#15803));
#6841=EDGE_LOOP('',(#15804,#15805,#15806,#15807,#15808));
#6842=EDGE_LOOP('',(#15809));
#6843=EDGE_LOOP('',(#15810,#15811,#15812,#15813,#15814,#15815,#15816,#15817,
#15818,#15819,#15820,#15821,#15822,#15823,#15824,#15825,#15826,#15827,#15828,
#15829,#15830,#15831,#15832,#15833,#15834,#15835,#15836,#15837,#15838,#15839,
#15840,#15841,#15842,#15843,#15844,#15845,#15846,#15847,#15848,#15849,#15850,
#15851,#15852,#15853,#15854,#15855,#15856,#15857,#15858,#15859,#15860,#15861,
#15862,#15863,#15864,#15865));
#6844=EDGE_LOOP('',(#15866,#15867,#15868,#15869));
#6845=EDGE_LOOP('',(#15870,#15871,#15872,#15873));
#6846=EDGE_LOOP('',(#15874,#15875,#15876,#15877));
#6847=EDGE_LOOP('',(#15878,#15879,#15880,#15881));
#6848=EDGE_LOOP('',(#15882,#15883,#15884,#15885));
#6849=EDGE_LOOP('',(#15886,#15887,#15888,#15889));
#6850=EDGE_LOOP('',(#15890,#15891,#15892,#15893));
#6851=EDGE_LOOP('',(#15894,#15895,#15896,#15897));
#6852=EDGE_LOOP('',(#15898,#15899,#15900,#15901));
#6853=EDGE_LOOP('',(#15902,#15903,#15904,#15905));
#6854=EDGE_LOOP('',(#15906,#15907,#15908,#15909));
#6855=EDGE_LOOP('',(#15910,#15911,#15912,#15913));
#6856=EDGE_LOOP('',(#15914,#15915,#15916,#15917));
#6857=EDGE_LOOP('',(#15918,#15919,#15920,#15921));
#6858=EDGE_LOOP('',(#15922,#15923,#15924,#15925));
#6859=EDGE_LOOP('',(#15926,#15927,#15928,#15929));
#6860=EDGE_LOOP('',(#15930,#15931,#15932,#15933));
#6861=EDGE_LOOP('',(#15934,#15935,#15936,#15937));
#6862=EDGE_LOOP('',(#15938,#15939,#15940,#15941));
#6863=EDGE_LOOP('',(#15942,#15943,#15944,#15945));
#6864=EDGE_LOOP('',(#15946,#15947,#15948,#15949));
#6865=EDGE_LOOP('',(#15950,#15951,#15952,#15953));
#6866=EDGE_LOOP('',(#15954,#15955,#15956,#15957));
#6867=EDGE_LOOP('',(#15958,#15959,#15960,#15961));
#6868=EDGE_LOOP('',(#15962,#15963,#15964,#15965));
#6869=EDGE_LOOP('',(#15966,#15967,#15968,#15969));
#6870=EDGE_LOOP('',(#15970,#15971,#15972,#15973));
#6871=EDGE_LOOP('',(#15974,#15975,#15976,#15977));
#6872=EDGE_LOOP('',(#15978,#15979,#15980,#15981));
#6873=EDGE_LOOP('',(#15982,#15983,#15984,#15985));
#6874=EDGE_LOOP('',(#15986,#15987,#15988,#15989));
#6875=EDGE_LOOP('',(#15990,#15991,#15992,#15993));
#6876=EDGE_LOOP('',(#15994,#15995,#15996,#15997));
#6877=EDGE_LOOP('',(#15998,#15999,#16000,#16001));
#6878=EDGE_LOOP('',(#16002,#16003,#16004,#16005));
#6879=EDGE_LOOP('',(#16006,#16007,#16008,#16009));
#6880=EDGE_LOOP('',(#16010,#16011,#16012,#16013));
#6881=EDGE_LOOP('',(#16014,#16015,#16016,#16017));
#6882=EDGE_LOOP('',(#16018,#16019,#16020,#16021));
#6883=EDGE_LOOP('',(#16022,#16023,#16024,#16025));
#6884=EDGE_LOOP('',(#16026,#16027,#16028,#16029));
#6885=EDGE_LOOP('',(#16030,#16031,#16032,#16033));
#6886=EDGE_LOOP('',(#16034,#16035,#16036,#16037));
#6887=EDGE_LOOP('',(#16038,#16039,#16040,#16041));
#6888=EDGE_LOOP('',(#16042,#16043,#16044,#16045));
#6889=EDGE_LOOP('',(#16046,#16047,#16048,#16049));
#6890=EDGE_LOOP('',(#16050,#16051,#16052,#16053));
#6891=EDGE_LOOP('',(#16054,#16055,#16056,#16057));
#6892=EDGE_LOOP('',(#16058,#16059,#16060,#16061));
#6893=EDGE_LOOP('',(#16062,#16063,#16064,#16065));
#6894=EDGE_LOOP('',(#16066,#16067,#16068,#16069));
#6895=EDGE_LOOP('',(#16070,#16071,#16072,#16073));
#6896=EDGE_LOOP('',(#16074,#16075,#16076,#16077));
#6897=EDGE_LOOP('',(#16078,#16079,#16080,#16081));
#6898=EDGE_LOOP('',(#16082,#16083,#16084,#16085));
#6899=EDGE_LOOP('',(#16086,#16087,#16088,#16089,#16090,#16091,#16092,#16093,
#16094,#16095,#16096,#16097,#16098,#16099,#16100,#16101,#16102,#16103,#16104,
#16105,#16106,#16107,#16108,#16109,#16110,#16111,#16112,#16113,#16114,#16115,
#16116,#16117,#16118,#16119,#16120,#16121,#16122,#16123,#16124,#16125,#16126,
#16127,#16128,#16129,#16130,#16131,#16132,#16133,#16134,#16135,#16136,#16137,
#16138,#16139,#16140,#16141));
#6900=EDGE_LOOP('',(#16142));
#6901=EDGE_LOOP('',(#16143,#16144,#16145,#16146));
#6902=EDGE_LOOP('',(#16147,#16148,#16149,#16150));
#6903=EDGE_LOOP('',(#16151,#16152,#16153,#16154));
#6904=EDGE_LOOP('',(#16155,#16156,#16157,#16158,#16159,#16160));
#6905=EDGE_LOOP('',(#16161,#16162,#16163,#16164,#16165,#16166));
#6906=EDGE_LOOP('',(#16167,#16168,#16169,#16170,#16171,#16172));
#6907=EDGE_LOOP('',(#16173,#16174,#16175,#16176,#16177));
#6908=EDGE_LOOP('',(#16178,#16179,#16180,#16181,#16182,#16183));
#6909=EDGE_LOOP('',(#16184,#16185,#16186,#16187,#16188));
#6910=EDGE_LOOP('',(#16189,#16190,#16191,#16192,#16193,#16194));
#6911=EDGE_LOOP('',(#16195,#16196,#16197,#16198,#16199));
#6912=EDGE_LOOP('',(#16200,#16201,#16202,#16203,#16204,#16205));
#6913=EDGE_LOOP('',(#16206,#16207,#16208,#16209,#16210));
#6914=EDGE_LOOP('',(#16211,#16212,#16213,#16214,#16215,#16216));
#6915=EDGE_LOOP('',(#16217,#16218,#16219,#16220,#16221));
#6916=EDGE_LOOP('',(#16222,#16223,#16224,#16225,#16226,#16227));
#6917=EDGE_LOOP('',(#16228,#16229,#16230,#16231,#16232));
#6918=EDGE_LOOP('',(#16233,#16234,#16235,#16236,#16237,#16238));
#6919=EDGE_LOOP('',(#16239,#16240,#16241,#16242,#16243));
#6920=EDGE_LOOP('',(#16244,#16245,#16246,#16247,#16248,#16249));
#6921=EDGE_LOOP('',(#16250,#16251,#16252,#16253,#16254));
#6922=EDGE_LOOP('',(#16255,#16256,#16257,#16258,#16259,#16260));
#6923=EDGE_LOOP('',(#16261,#16262,#16263,#16264,#16265));
#6924=EDGE_LOOP('',(#16266,#16267,#16268,#16269,#16270,#16271));
#6925=EDGE_LOOP('',(#16272,#16273,#16274,#16275,#16276));
#6926=EDGE_LOOP('',(#16277,#16278,#16279,#16280,#16281,#16282));
#6927=EDGE_LOOP('',(#16283,#16284,#16285,#16286,#16287,#16288));
#6928=EDGE_LOOP('',(#16289,#16290,#16291,#16292,#16293));
#6929=EDGE_LOOP('',(#16294,#16295,#16296,#16297,#16298,#16299));
#6930=EDGE_LOOP('',(#16300,#16301,#16302,#16303,#16304));
#6931=EDGE_LOOP('',(#16305,#16306,#16307,#16308,#16309,#16310));
#6932=EDGE_LOOP('',(#16311,#16312,#16313,#16314,#16315));
#6933=EDGE_LOOP('',(#16316,#16317,#16318,#16319,#16320,#16321));
#6934=EDGE_LOOP('',(#16322,#16323,#16324,#16325,#16326,#16327));
#6935=EDGE_LOOP('',(#16328,#16329,#16330,#16331,#16332));
#6936=EDGE_LOOP('',(#16333,#16334,#16335,#16336,#16337,#16338));
#6937=EDGE_LOOP('',(#16339,#16340,#16341,#16342,#16343));
#6938=EDGE_LOOP('',(#16344,#16345,#16346,#16347,#16348,#16349));
#6939=EDGE_LOOP('',(#16350,#16351,#16352,#16353,#16354,#16355));
#6940=EDGE_LOOP('',(#16356,#16357,#16358,#16359,#16360,#16361));
#6941=EDGE_LOOP('',(#16362,#16363,#16364,#16365,#16366,#16367));
#6942=EDGE_LOOP('',(#16368,#16369,#16370,#16371,#16372,#16373,#16374,#16375,
#16376,#16377,#16378,#16379,#16380,#16381,#16382,#16383,#16384,#16385,#16386,
#16387,#16388,#16389,#16390,#16391,#16392,#16393,#16394,#16395,#16396,#16397,
#16398,#16399,#16400,#16401,#16402,#16403,#16404,#16405,#16406,#16407,#16408,
#16409,#16410,#16411,#16412,#16413,#16414,#16415,#16416,#16417,#16418,#16419,
#16420,#16421,#16422,#16423,#16424,#16425,#16426,#16427,#16428,#16429,#16430,
#16431,#16432,#16433,#16434,#16435,#16436,#16437,#16438,#16439,#16440,#16441,
#16442,#16443,#16444,#16445,#16446,#16447,#16448,#16449));
#6943=EDGE_LOOP('',(#16450,#16451,#16452,#16453,#16454,#16455));
#6944=EDGE_LOOP('',(#16456,#16457,#16458,#16459));
#6945=EDGE_LOOP('',(#16460));
#6946=EDGE_LOOP('',(#16461,#16462,#16463,#16464,#16465));
#6947=EDGE_LOOP('',(#16466,#16467,#16468,#16469,#16470,#16471,#16472,#16473,
#16474,#16475,#16476,#16477,#16478,#16479,#16480,#16481,#16482,#16483,#16484,
#16485,#16486,#16487,#16488,#16489,#16490,#16491,#16492,#16493,#16494,#16495,
#16496,#16497,#16498,#16499,#16500,#16501,#16502,#16503,#16504,#16505,#16506,
#16507,#16508,#16509,#16510,#16511,#16512,#16513,#16514,#16515,#16516,#16517,
#16518,#16519,#16520,#16521,#16522,#16523,#16524,#16525,#16526,#16527,#16528,
#16529,#16530,#16531,#16532,#16533,#16534,#16535,#16536,#16537,#16538,#16539,
#16540,#16541,#16542,#16543,#16544,#16545,#16546,#16547,#16548,#16549,#16550,
#16551,#16552,#16553,#16554,#16555,#16556,#16557,#16558,#16559,#16560,#16561,
#16562,#16563,#16564,#16565,#16566,#16567,#16568,#16569,#16570,#16571,#16572,
#16573,#16574,#16575,#16576,#16577,#16578,#16579,#16580,#16581,#16582,#16583,
#16584,#16585,#16586,#16587));
#6948=EDGE_LOOP('',(#16588,#16589,#16590,#16591,#16592));
#6949=EDGE_LOOP('',(#16593,#16594,#16595,#16596,#16597,#16598,#16599,#16600,
#16601,#16602,#16603,#16604,#16605,#16606,#16607,#16608,#16609,#16610,#16611,
#16612,#16613,#16614,#16615,#16616,#16617,#16618,#16619,#16620,#16621,#16622,
#16623,#16624,#16625,#16626,#16627,#16628,#16629,#16630,#16631,#16632,#16633,
#16634,#16635,#16636,#16637,#16638,#16639,#16640,#16641,#16642,#16643,#16644,
#16645,#16646,#16647,#16648,#16649,#16650,#16651,#16652,#16653,#16654,#16655,
#16656,#16657,#16658,#16659,#16660,#16661,#16662,#16663,#16664,#16665,#16666,
#16667,#16668,#16669,#16670,#16671,#16672,#16673,#16674,#16675,#16676,#16677,
#16678,#16679,#16680,#16681,#16682,#16683,#16684,#16685,#16686,#16687,#16688,
#16689,#16690,#16691,#16692,#16693,#16694,#16695,#16696,#16697,#16698,#16699));
#6950=EDGE_LOOP('',(#16700));
#6951=EDGE_LOOP('',(#16701));
#6952=EDGE_LOOP('',(#16702,#16703,#16704,#16705,#16706,#16707,#16708));
#6953=EDGE_LOOP('',(#16709,#16710,#16711,#16712,#16713,#16714,#16715));
#6954=EDGE_LOOP('',(#16716,#16717,#16718,#16719));
#6955=EDGE_LOOP('',(#16720));
#6956=EDGE_LOOP('',(#16721));
#6957=EDGE_LOOP('',(#16722,#16723,#16724,#16725));
#6958=EDGE_LOOP('',(#16726));
#6959=EDGE_LOOP('',(#16727));
#6960=EDGE_LOOP('',(#16728,#16729,#16730,#16731));
#6961=EDGE_LOOP('',(#16732,#16733,#16734,#16735));
#6962=EDGE_LOOP('',(#16736));
#6963=EDGE_LOOP('',(#16737,#16738,#16739,#16740));
#6964=EDGE_LOOP('',(#16741,#16742));
#6965=EDGE_LOOP('',(#16743,#16744,#16745,#16746,#16747));
#6966=EDGE_LOOP('',(#16748,#16749,#16750));
#6967=EDGE_LOOP('',(#16751,#16752,#16753,#16754,#16755));
#6968=EDGE_LOOP('',(#16756,#16757,#16758,#16759));
#6969=EDGE_LOOP('',(#16760,#16761,#16762,#16763,#16764));
#6970=EDGE_LOOP('',(#16765,#16766,#16767,#16768));
#6971=EDGE_LOOP('',(#16769,#16770,#16771,#16772,#16773));
#6972=EDGE_LOOP('',(#16774,#16775,#16776));
#6973=EDGE_LOOP('',(#16777,#16778,#16779,#16780));
#6974=EDGE_LOOP('',(#16781,#16782,#16783,#16784));
#6975=EDGE_LOOP('',(#16785,#16786,#16787,#16788));
#6976=EDGE_LOOP('',(#16789,#16790,#16791,#16792,#16793,#16794,#16795,#16796,
#16797,#16798,#16799,#16800,#16801,#16802,#16803,#16804,#16805,#16806,#16807,
#16808));
#6977=EDGE_LOOP('',(#16809,#16810,#16811,#16812,#16813));
#6978=EDGE_LOOP('',(#16814,#16815,#16816,#16817));
#6979=EDGE_LOOP('',(#16818,#16819,#16820,#16821,#16822,#16823,#16824,#16825,
#16826,#16827,#16828,#16829,#16830,#16831,#16832));
#6980=EDGE_LOOP('',(#16833,#16834,#16835,#16836));
#6981=EDGE_LOOP('',(#16837,#16838,#16839,#16840));
#6982=EDGE_LOOP('',(#16841,#16842,#16843,#16844));
#6983=EDGE_LOOP('',(#16845,#16846,#16847,#16848,#16849,#16850,#16851,#16852,
#16853));
#6984=EDGE_LOOP('',(#16854,#16855,#16856,#16857,#16858));
#6985=EDGE_LOOP('',(#16859,#16860,#16861,#16862,#16863,#16864));
#6986=EDGE_LOOP('',(#16865,#16866,#16867,#16868,#16869));
#6987=EDGE_LOOP('',(#16870,#16871,#16872,#16873,#16874,#16875,#16876,#16877));
#6988=EDGE_LOOP('',(#16878,#16879,#16880,#16881,#16882));
#6989=EDGE_LOOP('',(#16883,#16884,#16885,#16886));
#6990=EDGE_LOOP('',(#16887,#16888,#16889,#16890,#16891));
#6991=EDGE_LOOP('',(#16892,#16893,#16894));
#6992=EDGE_LOOP('',(#16895,#16896,#16897));
#6993=EDGE_LOOP('',(#16898,#16899,#16900,#16901,#16902,#16903));
#6994=EDGE_LOOP('',(#16904,#16905,#16906,#16907));
#6995=EDGE_LOOP('',(#16908,#16909,#16910,#16911,#16912,#16913,#16914,#16915,
#16916,#16917));
#6996=EDGE_LOOP('',(#16918,#16919,#16920,#16921));
#6997=EDGE_LOOP('',(#16922,#16923,#16924,#16925,#16926,#16927));
#6998=EDGE_LOOP('',(#16928,#16929,#16930,#16931));
#6999=EDGE_LOOP('',(#16932,#16933,#16934,#16935,#16936));
#7000=EDGE_LOOP('',(#16937,#16938,#16939,#16940,#16941));
#7001=EDGE_LOOP('',(#16942,#16943,#16944,#16945,#16946));
#7002=EDGE_LOOP('',(#16947,#16948,#16949,#16950));
#7003=EDGE_LOOP('',(#16951,#16952,#16953,#16954));
#7004=EDGE_LOOP('',(#16955,#16956,#16957,#16958,#16959,#16960,#16961,#16962,
#16963,#16964,#16965,#16966,#16967,#16968,#16969,#16970,#16971,#16972,#16973,
#16974));
#7005=EDGE_LOOP('',(#16975,#16976));
#7006=EDGE_LOOP('',(#16977));
#7007=EDGE_LOOP('',(#16978,#16979,#16980,#16981,#16982));
#7008=EDGE_LOOP('',(#16983,#16984,#16985,#16986,#16987,#16988));
#7009=EDGE_LOOP('',(#16989,#16990,#16991,#16992,#16993));
#7010=EDGE_LOOP('',(#16994,#16995,#16996,#16997,#16998,#16999));
#7011=EDGE_LOOP('',(#17000));
#7012=EDGE_LOOP('',(#17001,#17002,#17003,#17004));
#7013=EDGE_LOOP('',(#17005));
#7014=EDGE_LOOP('',(#17006,#17007,#17008,#17009,#17010));
#7015=EDGE_LOOP('',(#17011,#17012,#17013,#17014));
#7016=EDGE_LOOP('',(#17015,#17016,#17017,#17018));
#7017=EDGE_LOOP('',(#17019,#17020,#17021));
#7018=EDGE_LOOP('',(#17022,#17023,#17024));
#7019=EDGE_LOOP('',(#17025,#17026,#17027,#17028));
#7020=EDGE_LOOP('',(#17029,#17030,#17031));
#7021=EDGE_LOOP('',(#17032,#17033,#17034,#17035,#17036,#17037));
#7022=EDGE_LOOP('',(#17038,#17039,#17040,#17041));
#7023=EDGE_LOOP('',(#17042,#17043,#17044,#17045,#17046));
#7024=EDGE_LOOP('',(#17047,#17048,#17049,#17050));
#7025=EDGE_LOOP('',(#17051,#17052,#17053,#17054,#17055,#17056,#17057));
#7026=EDGE_LOOP('',(#17058,#17059,#17060,#17061,#17062,#17063,#17064,#17065,
#17066,#17067,#17068,#17069,#17070,#17071,#17072,#17073,#17074,#17075));
#7027=EDGE_LOOP('',(#17076,#17077,#17078,#17079,#17080,#17081,#17082,#17083,
#17084));
#7028=EDGE_LOOP('',(#17085,#17086,#17087,#17088,#17089,#17090,#17091,#17092));
#7029=EDGE_LOOP('',(#17093,#17094,#17095,#17096));
#7030=EDGE_LOOP('',(#17097,#17098,#17099,#17100));
#7031=EDGE_LOOP('',(#17101,#17102,#17103));
#7032=EDGE_LOOP('',(#17104,#17105,#17106,#17107));
#7033=EDGE_LOOP('',(#17108,#17109,#17110));
#7034=EDGE_LOOP('',(#17111,#17112,#17113,#17114));
#7035=EDGE_LOOP('',(#17115,#17116,#17117,#17118,#17119,#17120,#17121,#17122,
#17123,#17124,#17125,#17126,#17127));
#7036=EDGE_LOOP('',(#17128));
#7037=EDGE_LOOP('',(#17129,#17130,#17131,#17132,#17133,#17134,#17135));
#7038=EDGE_LOOP('',(#17136,#17137,#17138,#17139,#17140,#17141));
#7039=EDGE_LOOP('',(#17142,#17143,#17144,#17145,#17146));
#7040=EDGE_LOOP('',(#17147,#17148,#17149,#17150,#17151));
#7041=EDGE_LOOP('',(#17152,#17153,#17154,#17155,#17156));
#7042=EDGE_LOOP('',(#17157,#17158,#17159,#17160,#17161,#17162,#17163));
#7043=EDGE_LOOP('',(#17164));
#7044=EDGE_LOOP('',(#17165,#17166,#17167,#17168));
#7045=EDGE_LOOP('',(#17169,#17170,#17171,#17172,#17173,#17174));
#7046=EDGE_LOOP('',(#17175,#17176,#17177,#17178,#17179,#17180));
#7047=EDGE_LOOP('',(#17181,#17182,#17183,#17184));
#7048=EDGE_LOOP('',(#17185,#17186,#17187,#17188));
#7049=EDGE_LOOP('',(#17189,#17190,#17191,#17192,#17193));
#7050=EDGE_LOOP('',(#17194,#17195,#17196,#17197,#17198,#17199,#17200,#17201));
#7051=EDGE_LOOP('',(#17202,#17203,#17204,#17205,#17206));
#7052=EDGE_LOOP('',(#17207,#17208,#17209,#17210,#17211,#17212));
#7053=EDGE_LOOP('',(#17213,#17214,#17215,#17216));
#7054=EDGE_LOOP('',(#17217,#17218,#17219,#17220));
#7055=EDGE_LOOP('',(#17221,#17222,#17223));
#7056=EDGE_LOOP('',(#17224,#17225,#17226,#17227));
#7057=EDGE_LOOP('',(#17228,#17229,#17230));
#7058=EDGE_LOOP('',(#17231,#17232,#17233,#17234,#17235,#17236,#17237,#17238,
#17239,#17240,#17241,#17242,#17243,#17244,#17245,#17246,#17247,#17248,#17249,
#17250,#17251,#17252,#17253,#17254,#17255,#17256,#17257,#17258,#17259,#17260,
#17261,#17262,#17263,#17264));
#7059=EDGE_LOOP('',(#17265,#17266,#17267,#17268));
#7060=EDGE_LOOP('',(#17269,#17270,#17271,#17272,#17273,#17274));
#7061=EDGE_LOOP('',(#17275));
#7062=EDGE_LOOP('',(#17276));
#7063=EDGE_LOOP('',(#17277,#17278,#17279,#17280));
#7064=EDGE_LOOP('',(#17281,#17282,#17283,#17284));
#7065=EDGE_LOOP('',(#17285,#17286,#17287,#17288,#17289,#17290));
#7066=EDGE_LOOP('',(#17291,#17292,#17293,#17294,#17295,#17296));
#7067=EDGE_LOOP('',(#17297,#17298,#17299,#17300));
#7068=EDGE_LOOP('',(#17301,#17302,#17303,#17304,#17305));
#7069=EDGE_LOOP('',(#17306,#17307,#17308,#17309));
#7070=EDGE_LOOP('',(#17310,#17311,#17312,#17313));
#7071=EDGE_LOOP('',(#17314,#17315,#17316,#17317));
#7072=EDGE_LOOP('',(#17318,#17319,#17320,#17321,#17322,#17323,#17324));
#7073=EDGE_LOOP('',(#17325,#17326,#17327,#17328));
#7074=EDGE_LOOP('',(#17329,#17330,#17331));
#7075=EDGE_LOOP('',(#17332,#17333,#17334,#17335,#17336,#17337,#17338));
#7076=EDGE_LOOP('',(#17339,#17340,#17341,#17342));
#7077=EDGE_LOOP('',(#17343,#17344,#17345,#17346));
#7078=EDGE_LOOP('',(#17347,#17348,#17349,#17350));
#7079=EDGE_LOOP('',(#17351,#17352,#17353));
#7080=EDGE_LOOP('',(#17354,#17355,#17356,#17357,#17358));
#7081=EDGE_LOOP('',(#17359,#17360,#17361,#17362,#17363,#17364,#17365,#17366));
#7082=EDGE_LOOP('',(#17367,#17368,#17369,#17370,#17371));
#7083=EDGE_LOOP('',(#17372,#17373,#17374,#17375));
#7084=EDGE_LOOP('',(#17376,#17377,#17378,#17379,#17380));
#7085=EDGE_LOOP('',(#17381,#17382,#17383,#17384,#17385,#17386,#17387));
#7086=EDGE_LOOP('',(#17388));
#7087=EDGE_LOOP('',(#17389,#17390,#17391,#17392,#17393,#17394));
#7088=EDGE_LOOP('',(#17395,#17396,#17397,#17398,#17399,#17400));
#7089=EDGE_LOOP('',(#17401,#17402,#17403,#17404,#17405));
#7090=EDGE_LOOP('',(#17406,#17407,#17408,#17409,#17410,#17411,#17412));
#7091=EDGE_LOOP('',(#17413));
#7092=EDGE_LOOP('',(#17414,#17415,#17416,#17417));
#7093=EDGE_LOOP('',(#17418,#17419,#17420,#17421));
#7094=EDGE_LOOP('',(#17422,#17423,#17424,#17425));
#7095=EDGE_LOOP('',(#17426,#17427,#17428,#17429));
#7096=EDGE_LOOP('',(#17430,#17431,#17432,#17433));
#7097=EDGE_LOOP('',(#17434,#17435,#17436,#17437));
#7098=EDGE_LOOP('',(#17438,#17439,#17440,#17441,#17442,#17443,#17444,#17445,
#17446,#17447));
#7099=EDGE_LOOP('',(#17448,#17449,#17450,#17451));
#7100=EDGE_LOOP('',(#17452,#17453,#17454,#17455,#17456,#17457));
#7101=EDGE_LOOP('',(#17458,#17459,#17460,#17461));
#7102=EDGE_LOOP('',(#17462,#17463,#17464,#17465));
#7103=EDGE_LOOP('',(#17466,#17467,#17468,#17469));
#7104=EDGE_LOOP('',(#17470,#17471,#17472,#17473,#17474,#17475));
#7105=EDGE_LOOP('',(#17476,#17477,#17478,#17479));
#7106=EDGE_LOOP('',(#17480,#17481,#17482,#17483,#17484,#17485));
#7107=EDGE_LOOP('',(#17486,#17487,#17488,#17489));
#7108=EDGE_LOOP('',(#17490,#17491,#17492,#17493,#17494,#17495));
#7109=EDGE_LOOP('',(#17496,#17497,#17498,#17499,#17500,#17501,#17502));
#7110=EDGE_LOOP('',(#17503,#17504,#17505,#17506,#17507,#17508));
#7111=EDGE_LOOP('',(#17509,#17510,#17511,#17512,#17513,#17514,#17515));
#7112=EDGE_LOOP('',(#17516,#17517,#17518,#17519));
#7113=EDGE_LOOP('',(#17520,#17521,#17522,#17523));
#7114=EDGE_LOOP('',(#17524,#17525,#17526,#17527));
#7115=EDGE_LOOP('',(#17528,#17529,#17530,#17531));
#7116=EDGE_LOOP('',(#17532,#17533,#17534,#17535));
#7117=EDGE_LOOP('',(#17536,#17537,#17538,#17539));
#7118=EDGE_LOOP('',(#17540,#17541,#17542,#17543));
#7119=EDGE_LOOP('',(#17544,#17545,#17546,#17547));
#7120=EDGE_LOOP('',(#17548,#17549,#17550,#17551,#17552));
#7121=EDGE_LOOP('',(#17553,#17554,#17555,#17556,#17557));
#7122=EDGE_LOOP('',(#17558,#17559,#17560,#17561,#17562));
#7123=EDGE_LOOP('',(#17563,#17564,#17565,#17566,#17567));
#7124=EDGE_LOOP('',(#17568,#17569,#17570,#17571,#17572));
#7125=EDGE_LOOP('',(#17573,#17574,#17575,#17576,#17577,#17578));
#7126=EDGE_LOOP('',(#17579,#17580,#17581,#17582,#17583,#17584,#17585));
#7127=EDGE_LOOP('',(#17586,#17587,#17588,#17589,#17590,#17591));
#7128=EDGE_LOOP('',(#17592,#17593,#17594,#17595,#17596));
#7129=EDGE_LOOP('',(#17597,#17598,#17599,#17600,#17601,#17602,#17603,#17604,
#17605,#17606,#17607,#17608,#17609));
#7130=EDGE_LOOP('',(#17610));
#7131=EDGE_LOOP('',(#17611,#17612,#17613,#17614));
#7132=EDGE_LOOP('',(#17615,#17616,#17617,#17618));
#7133=EDGE_LOOP('',(#17619,#17620,#17621));
#7134=EDGE_LOOP('',(#17622,#17623,#17624));
#7135=EDGE_LOOP('',(#17625,#17626,#17627,#17628));
#7136=EDGE_LOOP('',(#17629,#17630,#17631,#17632));
#7137=EDGE_LOOP('',(#17633,#17634,#17635,#17636));
#7138=EDGE_LOOP('',(#17637,#17638,#17639));
#7139=EDGE_LOOP('',(#17640,#17641,#17642,#17643,#17644,#17645,#17646,#17647,
#17648,#17649,#17650));
#7140=EDGE_LOOP('',(#17651,#17652,#17653,#17654));
#7141=EDGE_LOOP('',(#17655,#17656,#17657,#17658,#17659));
#7142=EDGE_LOOP('',(#17660,#17661,#17662,#17663));
#7143=EDGE_LOOP('',(#17664,#17665,#17666,#17667,#17668));
#7144=EDGE_LOOP('',(#17669,#17670,#17671));
#7145=EDGE_LOOP('',(#17672,#17673,#17674));
#7146=EDGE_LOOP('',(#17675,#17676,#17677,#17678,#17679,#17680));
#7147=EDGE_LOOP('',(#17681,#17682,#17683,#17684));
#7148=EDGE_LOOP('',(#17685,#17686,#17687,#17688));
#7149=EDGE_LOOP('',(#17689,#17690,#17691,#17692));
#7150=EDGE_LOOP('',(#17693,#17694,#17695));
#7151=EDGE_LOOP('',(#17696,#17697,#17698,#17699,#17700));
#7152=EDGE_LOOP('',(#17701,#17702,#17703,#17704,#17705,#17706,#17707,#17708,
#17709,#17710,#17711,#17712,#17713,#17714,#17715,#17716,#17717,#17718,#17719,
#17720));
#7153=EDGE_LOOP('',(#17721,#17722,#17723,#17724,#17725,#17726));
#7154=EDGE_LOOP('',(#17727));
#7155=EDGE_LOOP('',(#17728));
#7156=EDGE_LOOP('',(#17729,#17730,#17731,#17732));
#7157=EDGE_LOOP('',(#17733,#17734,#17735,#17736));
#7158=EDGE_LOOP('',(#17737,#17738,#17739,#17740,#17741,#17742));
#7159=EDGE_LOOP('',(#17743,#17744,#17745,#17746));
#7160=EDGE_LOOP('',(#17747,#17748,#17749,#17750,#17751,#17752,#17753));
#7161=EDGE_LOOP('',(#17754,#17755,#17756,#17757));
#7162=EDGE_LOOP('',(#17758,#17759,#17760,#17761,#17762,#17763));
#7163=EDGE_LOOP('',(#17764,#17765,#17766,#17767,#17768,#17769,#17770,#17771,
#17772,#17773,#17774,#17775,#17776,#17777));
#7164=EDGE_LOOP('',(#17778,#17779,#17780,#17781));
#7165=EDGE_LOOP('',(#17782,#17783,#17784,#17785));
#7166=EDGE_LOOP('',(#17786,#17787,#17788,#17789,#17790));
#7167=EDGE_LOOP('',(#17791,#17792,#17793,#17794,#17795,#17796,#17797,#17798,
#17799,#17800));
#7168=EDGE_LOOP('',(#17801,#17802,#17803,#17804,#17805,#17806,#17807));
#7169=EDGE_LOOP('',(#17808,#17809,#17810,#17811,#17812,#17813));
#7170=EDGE_LOOP('',(#17814,#17815,#17816,#17817));
#7171=EDGE_LOOP('',(#17818,#17819,#17820,#17821,#17822,#17823,#17824,#17825));
#7172=EDGE_LOOP('',(#17826,#17827,#17828,#17829));
#7173=EDGE_LOOP('',(#17830,#17831,#17832,#17833,#17834,#17835,#17836,#17837));
#7174=EDGE_LOOP('',(#17838,#17839,#17840,#17841));
#7175=EDGE_LOOP('',(#17842,#17843,#17844,#17845));
#7176=EDGE_LOOP('',(#17846,#17847,#17848,#17849));
#7177=EDGE_LOOP('',(#17850,#17851,#17852));
#7178=EDGE_LOOP('',(#17853,#17854,#17855));
#7179=EDGE_LOOP('',(#17856,#17857,#17858,#17859,#17860,#17861,#17862,#17863,
#17864,#17865,#17866,#17867,#17868,#17869));
#7180=EDGE_LOOP('',(#17870,#17871,#17872,#17873));
#7181=EDGE_LOOP('',(#17874,#17875,#17876,#17877,#17878,#17879));
#7182=EDGE_LOOP('',(#17880,#17881,#17882,#17883));
#7183=EDGE_LOOP('',(#17884,#17885,#17886,#17887,#17888));
#7184=EDGE_LOOP('',(#17889,#17890,#17891,#17892,#17893));
#7185=EDGE_LOOP('',(#17894,#17895,#17896,#17897));
#7186=EDGE_LOOP('',(#17898,#17899,#17900,#17901,#17902));
#7187=EDGE_LOOP('',(#17903,#17904,#17905,#17906,#17907));
#7188=EDGE_LOOP('',(#17908,#17909,#17910,#17911));
#7189=EDGE_LOOP('',(#17912,#17913,#17914,#17915));
#7190=EDGE_LOOP('',(#17916,#17917,#17918,#17919,#17920,#17921,#17922));
#7191=EDGE_LOOP('',(#17923,#17924,#17925,#17926));
#7192=EDGE_LOOP('',(#17927,#17928,#17929,#17930));
#7193=EDGE_LOOP('',(#17931,#17932,#17933,#17934,#17935,#17936));
#7194=EDGE_LOOP('',(#17937,#17938,#17939,#17940));
#7195=EDGE_LOOP('',(#17941,#17942,#17943,#17944,#17945,#17946));
#7196=EDGE_LOOP('',(#17947,#17948,#17949,#17950));
#7197=EDGE_LOOP('',(#17951,#17952,#17953,#17954));
#7198=EDGE_LOOP('',(#17955,#17956,#17957,#17958,#17959));
#7199=EDGE_LOOP('',(#17960,#17961,#17962,#17963,#17964,#17965,#17966,#17967,
#17968,#17969));
#7200=EDGE_LOOP('',(#17970,#17971,#17972,#17973));
#7201=EDGE_LOOP('',(#17974,#17975,#17976,#17977));
#7202=EDGE_LOOP('',(#17978,#17979,#17980,#17981,#17982));
#7203=EDGE_LOOP('',(#17983,#17984,#17985,#17986,#17987));
#7204=EDGE_LOOP('',(#17988,#17989,#17990,#17991,#17992));
#7205=EDGE_LOOP('',(#17993,#17994,#17995,#17996));
#7206=EDGE_LOOP('',(#17997,#17998,#17999,#18000));
#7207=EDGE_LOOP('',(#18001,#18002,#18003,#18004));
#7208=EDGE_LOOP('',(#18005,#18006,#18007,#18008));
#7209=EDGE_LOOP('',(#18009,#18010,#18011));
#7210=EDGE_LOOP('',(#18012,#18013,#18014,#18015));
#7211=EDGE_LOOP('',(#18016,#18017,#18018,#18019,#18020));
#7212=EDGE_LOOP('',(#18021,#18022,#18023,#18024));
#7213=EDGE_LOOP('',(#18025,#18026,#18027,#18028));
#7214=EDGE_LOOP('',(#18029,#18030,#18031));
#7215=EDGE_LOOP('',(#18032,#18033,#18034,#18035));
#7216=EDGE_LOOP('',(#18036,#18037,#18038,#18039,#18040,#18041));
#7217=EDGE_LOOP('',(#18042,#18043,#18044,#18045));
#7218=EDGE_LOOP('',(#18046,#18047,#18048,#18049));
#7219=EDGE_LOOP('',(#18050,#18051,#18052));
#7220=EDGE_LOOP('',(#18053,#18054,#18055,#18056));
#7221=EDGE_LOOP('',(#18057,#18058,#18059,#18060));
#7222=EDGE_LOOP('',(#18061,#18062,#18063,#18064,#18065,#18066));
#7223=EDGE_LOOP('',(#18067,#18068,#18069,#18070,#18071));
#7224=EDGE_LOOP('',(#18072,#18073,#18074));
#7225=EDGE_LOOP('',(#18075));
#7226=EDGE_LOOP('',(#18076));
#7227=EDGE_LOOP('',(#18077));
#7228=EDGE_LOOP('',(#18078));
#7229=EDGE_LOOP('',(#18079));
#7230=EDGE_LOOP('',(#18080,#18081,#18082,#18083));
#7231=EDGE_LOOP('',(#18084,#18085,#18086,#18087));
#7232=EDGE_LOOP('',(#18088,#18089,#18090,#18091));
#7233=EDGE_LOOP('',(#18092,#18093,#18094,#18095));
#7234=EDGE_LOOP('',(#18096,#18097,#18098,#18099));
#7235=EDGE_LOOP('',(#18100,#18101,#18102,#18103));
#7236=EDGE_LOOP('',(#18104,#18105,#18106,#18107,#18108,#18109));
#7237=EDGE_LOOP('',(#18110,#18111,#18112,#18113));
#7238=EDGE_LOOP('',(#18114,#18115,#18116,#18117,#18118,#18119,#18120,#18121,
#18122,#18123));
#7239=EDGE_LOOP('',(#18124,#18125,#18126,#18127));
#7240=EDGE_LOOP('',(#18128,#18129,#18130,#18131));
#7241=EDGE_LOOP('',(#18132,#18133,#18134,#18135,#18136));
#7242=EDGE_LOOP('',(#18137,#18138));
#7243=EDGE_LOOP('',(#18139,#18140,#18141,#18142,#18143,#18144,#18145));
#7244=EDGE_LOOP('',(#18146,#18147));
#7245=EDGE_LOOP('',(#18148,#18149,#18150,#18151,#18152,#18153,#18154));
#7246=EDGE_LOOP('',(#18155,#18156,#18157,#18158,#18159,#18160,#18161,#18162));
#7247=EDGE_LOOP('',(#18163,#18164));
#7248=EDGE_LOOP('',(#18165,#18166));
#7249=EDGE_LOOP('',(#18167,#18168,#18169,#18170,#18171,#18172,#18173,#18174,
#18175,#18176));
#7250=EDGE_LOOP('',(#18177,#18178,#18179,#18180,#18181));
#7251=EDGE_LOOP('',(#18182,#18183,#18184,#18185,#18186,#18187));
#7252=EDGE_LOOP('',(#18188));
#7253=EDGE_LOOP('',(#18189));
#7254=EDGE_LOOP('',(#18190,#18191,#18192,#18193,#18194));
#7255=EDGE_LOOP('',(#18195));
#7256=EDGE_LOOP('',(#18196));
#7257=EDGE_LOOP('',(#18197,#18198,#18199,#18200,#18201));
#7258=EDGE_LOOP('',(#18202));
#7259=EDGE_LOOP('',(#18203));
#7260=EDGE_LOOP('',(#18204,#18205,#18206,#18207,#18208));
#7261=EDGE_LOOP('',(#18209,#18210,#18211,#18212,#18213));
#7262=EDGE_LOOP('',(#18214,#18215,#18216,#18217,#18218));
#7263=EDGE_LOOP('',(#18219,#18220,#18221,#18222));
#7264=EDGE_LOOP('',(#18223,#18224,#18225,#18226,#18227));
#7265=EDGE_LOOP('',(#18228,#18229,#18230,#18231,#18232,#18233));
#7266=EDGE_LOOP('',(#18234));
#7267=EDGE_LOOP('',(#18235));
#7268=EDGE_LOOP('',(#18236,#18237,#18238,#18239,#18240));
#7269=EDGE_LOOP('',(#18241,#18242,#18243,#18244));
#7270=EDGE_LOOP('',(#18245,#18246,#18247,#18248));
#7271=EDGE_LOOP('',(#18249,#18250,#18251,#18252));
#7272=EDGE_LOOP('',(#18253,#18254,#18255,#18256));
#7273=EDGE_LOOP('',(#18257,#18258,#18259,#18260));
#7274=EDGE_LOOP('',(#18261,#18262,#18263,#18264));
#7275=EDGE_LOOP('',(#18265,#18266,#18267,#18268));
#7276=EDGE_LOOP('',(#18269,#18270,#18271,#18272));
#7277=EDGE_LOOP('',(#18273,#18274,#18275,#18276));
#7278=EDGE_LOOP('',(#18277,#18278,#18279,#18280));
#7279=EDGE_LOOP('',(#18281,#18282,#18283,#18284));
#7280=EDGE_LOOP('',(#18285,#18286,#18287,#18288));
#7281=EDGE_LOOP('',(#18289,#18290,#18291,#18292));
#7282=EDGE_LOOP('',(#18293,#18294,#18295,#18296));
#7283=EDGE_LOOP('',(#18297,#18298,#18299,#18300));
#7284=EDGE_LOOP('',(#18301,#18302,#18303,#18304));
#7285=EDGE_LOOP('',(#18305,#18306,#18307,#18308));
#7286=EDGE_LOOP('',(#18309,#18310,#18311,#18312));
#7287=EDGE_LOOP('',(#18313,#18314,#18315,#18316));
#7288=EDGE_LOOP('',(#18317,#18318,#18319));
#7289=EDGE_LOOP('',(#18320,#18321,#18322));
#7290=EDGE_LOOP('',(#18323,#18324,#18325));
#7291=EDGE_LOOP('',(#18326,#18327,#18328));
#7292=EDGE_LOOP('',(#18329,#18330,#18331,#18332));
#7293=EDGE_LOOP('',(#18333,#18334,#18335,#18336));
#7294=EDGE_LOOP('',(#18337,#18338,#18339,#18340));
#7295=EDGE_LOOP('',(#18341,#18342,#18343,#18344,#18345,#18346));
#7296=EDGE_LOOP('',(#18347));
#7297=EDGE_LOOP('',(#18348));
#7298=EDGE_LOOP('',(#18349,#18350,#18351,#18352));
#7299=EDGE_LOOP('',(#18353,#18354,#18355,#18356));
#7300=EDGE_LOOP('',(#18357,#18358,#18359,#18360));
#7301=EDGE_LOOP('',(#18361,#18362,#18363));
#7302=EDGE_LOOP('',(#18364,#18365,#18366,#18367));
#7303=EDGE_LOOP('',(#18368,#18369,#18370));
#7304=EDGE_LOOP('',(#18371,#18372,#18373,#18374));
#7305=EDGE_LOOP('',(#18375,#18376,#18377,#18378,#18379,#18380,#18381,#18382,
#18383,#18384,#18385,#18386));
#7306=EDGE_LOOP('',(#18387,#18388,#18389,#18390));
#7307=EDGE_LOOP('',(#18391,#18392,#18393,#18394,#18395,#18396));
#7308=EDGE_LOOP('',(#18397));
#7309=EDGE_LOOP('',(#18398));
#7310=EDGE_LOOP('',(#18399,#18400,#18401,#18402));
#7311=EDGE_LOOP('',(#18403,#18404,#18405));
#7312=EDGE_LOOP('',(#18406,#18407,#18408));
#7313=EDGE_LOOP('',(#18409,#18410,#18411,#18412));
#7314=EDGE_LOOP('',(#18413,#18414,#18415,#18416,#18417,#18418,#18419,#18420,
#18421,#18422,#18423,#18424));
#7315=EDGE_LOOP('',(#18425,#18426,#18427,#18428));
#7316=EDGE_LOOP('',(#18429,#18430,#18431,#18432));
#7317=EDGE_LOOP('',(#18433,#18434,#18435,#18436));
#7318=EDGE_LOOP('',(#18437,#18438,#18439,#18440));
#7319=EDGE_LOOP('',(#18441,#18442,#18443,#18444));
#7320=EDGE_LOOP('',(#18445,#18446,#18447,#18448));
#7321=EDGE_LOOP('',(#18449,#18450,#18451,#18452));
#7322=EDGE_LOOP('',(#18453,#18454,#18455,#18456));
#7323=EDGE_LOOP('',(#18457,#18458,#18459,#18460));
#7324=EDGE_LOOP('',(#18461,#18462,#18463,#18464));
#7325=EDGE_LOOP('',(#18465,#18466,#18467,#18468));
#7326=EDGE_LOOP('',(#18469,#18470,#18471,#18472));
#7327=EDGE_LOOP('',(#18473,#18474,#18475,#18476,#18477,#18478,#18479,#18480,
#18481));
#7328=EDGE_LOOP('',(#18482,#18483,#18484,#18485));
#7329=EDGE_LOOP('',(#18486,#18487,#18488,#18489,#18490,#18491,#18492,#18493,
#18494));
#7330=EDGE_LOOP('',(#18495,#18496,#18497,#18498));
#7331=EDGE_LOOP('',(#18499,#18500,#18501,#18502,#18503));
#7332=EDGE_LOOP('',(#18504,#18505,#18506,#18507));
#7333=EDGE_LOOP('',(#18508,#18509,#18510));
#7334=EDGE_LOOP('',(#18511,#18512,#18513,#18514));
#7335=EDGE_LOOP('',(#18515,#18516,#18517,#18518));
#7336=EDGE_LOOP('',(#18519,#18520,#18521,#18522,#18523));
#7337=EDGE_LOOP('',(#18524,#18525,#18526,#18527));
#7338=EDGE_LOOP('',(#18528,#18529,#18530,#18531));
#7339=EDGE_LOOP('',(#18532,#18533,#18534));
#7340=EDGE_LOOP('',(#18535,#18536,#18537,#18538));
#7341=EDGE_LOOP('',(#18539,#18540,#18541,#18542));
#7342=EDGE_LOOP('',(#18543));
#7343=EDGE_LOOP('',(#18544));
#7344=EDGE_LOOP('',(#18545,#18546,#18547,#18548,#18549));
#7345=EDGE_LOOP('',(#18550,#18551,#18552,#18553,#18554,#18555));
#7346=EDGE_LOOP('',(#18556,#18557,#18558,#18559,#18560));
#7347=EDGE_LOOP('',(#18561,#18562,#18563,#18564,#18565));
#7348=EDGE_LOOP('',(#18566,#18567,#18568,#18569,#18570,#18571));
#7349=EDGE_LOOP('',(#18572,#18573,#18574,#18575,#18576));
#7350=EDGE_LOOP('',(#18577,#18578,#18579,#18580,#18581,#18582));
#7351=EDGE_LOOP('',(#18583));
#7352=EDGE_LOOP('',(#18584));
#7353=EDGE_LOOP('',(#18585,#18586,#18587,#18588,#18589));
#7354=EDGE_LOOP('',(#18590,#18591,#18592,#18593,#18594,#18595));
#7355=EDGE_LOOP('',(#18596,#18597,#18598,#18599,#18600));
#7356=EDGE_LOOP('',(#18601,#18602,#18603,#18604,#18605));
#7357=EDGE_LOOP('',(#18606,#18607,#18608,#18609,#18610,#18611));
#7358=EDGE_LOOP('',(#18612,#18613,#18614,#18615,#18616));
#7359=EDGE_LOOP('',(#18617,#18618,#18619,#18620,#18621,#18622));
#7360=EDGE_LOOP('',(#18623,#18624,#18625,#18626));
#7361=EDGE_LOOP('',(#18627,#18628,#18629,#18630));
#7362=EDGE_LOOP('',(#18631,#18632,#18633,#18634));
#7363=EDGE_LOOP('',(#18635));
#7364=EDGE_LOOP('',(#18636));
#7365=EDGE_LOOP('',(#18637,#18638,#18639,#18640));
#7366=EDGE_LOOP('',(#18641,#18642,#18643,#18644));
#7367=EDGE_LOOP('',(#18645));
#7368=EDGE_LOOP('',(#18646));
#7369=EDGE_LOOP('',(#18647,#18648,#18649,#18650));
#7370=EDGE_LOOP('',(#18651));
#7371=EDGE_LOOP('',(#18652));
#7372=EDGE_LOOP('',(#18653,#18654,#18655,#18656));
#7373=EDGE_LOOP('',(#18657));
#7374=EDGE_LOOP('',(#18658));
#7375=EDGE_LOOP('',(#18659,#18660,#18661,#18662));
#7376=EDGE_LOOP('',(#18663));
#7377=EDGE_LOOP('',(#18664));
#7378=EDGE_LOOP('',(#18665,#18666,#18667,#18668));
#7379=EDGE_LOOP('',(#18669));
#7380=EDGE_LOOP('',(#18670));
#7381=EDGE_LOOP('',(#18671));
#7382=EDGE_LOOP('',(#18672));
#7383=EDGE_LOOP('',(#18673,#18674,#18675,#18676));
#7384=EDGE_LOOP('',(#18677));
#7385=EDGE_LOOP('',(#18678));
#7386=EDGE_LOOP('',(#18679,#18680,#18681,#18682));
#7387=EDGE_LOOP('',(#18683));
#7388=EDGE_LOOP('',(#18684));
#7389=EDGE_LOOP('',(#18685,#18686,#18687,#18688));
#7390=EDGE_LOOP('',(#18689));
#7391=EDGE_LOOP('',(#18690));
#7392=EDGE_LOOP('',(#18691,#18692,#18693,#18694));
#7393=EDGE_LOOP('',(#18695,#18696,#18697,#18698));
#7394=EDGE_LOOP('',(#18699,#18700,#18701,#18702));
#7395=EDGE_LOOP('',(#18703,#18704,#18705,#18706));
#7396=EDGE_LOOP('',(#18707));
#7397=EDGE_LOOP('',(#18708));
#7398=EDGE_LOOP('',(#18709,#18710,#18711,#18712));
#7399=EDGE_LOOP('',(#18713));
#7400=EDGE_LOOP('',(#18714));
#7401=EDGE_LOOP('',(#18715,#18716,#18717,#18718));
#7402=EDGE_LOOP('',(#18719,#18720,#18721,#18722));
#7403=EDGE_LOOP('',(#18723,#18724,#18725,#18726));
#7404=EDGE_LOOP('',(#18727));
#7405=EDGE_LOOP('',(#18728));
#7406=EDGE_LOOP('',(#18729,#18730,#18731,#18732));
#7407=EDGE_LOOP('',(#18733));
#7408=EDGE_LOOP('',(#18734));
#7409=EDGE_LOOP('',(#18735,#18736,#18737,#18738));
#7410=EDGE_LOOP('',(#18739,#18740,#18741,#18742));
#7411=EDGE_LOOP('',(#18743,#18744,#18745,#18746));
#7412=EDGE_LOOP('',(#18747));
#7413=EDGE_LOOP('',(#18748));
#7414=EDGE_LOOP('',(#18749,#18750,#18751,#18752));
#7415=EDGE_LOOP('',(#18753,#18754,#18755,#18756));
#7416=EDGE_LOOP('',(#18757,#18758,#18759,#18760));
#7417=EDGE_LOOP('',(#18761));
#7418=EDGE_LOOP('',(#18762));
#7419=EDGE_LOOP('',(#18763));
#7420=EDGE_LOOP('',(#18764,#18765,#18766,#18767));
#7421=EDGE_LOOP('',(#18768,#18769,#18770,#18771));
#7422=EDGE_LOOP('',(#18772));
#7423=EDGE_LOOP('',(#18773));
#7424=EDGE_LOOP('',(#18774,#18775,#18776,#18777));
#7425=EDGE_LOOP('',(#18778,#18779,#18780,#18781));
#7426=EDGE_LOOP('',(#18782));
#7427=EDGE_LOOP('',(#18783));
#7428=EDGE_LOOP('',(#18784,#18785,#18786,#18787));
#7429=EDGE_LOOP('',(#18788));
#7430=EDGE_LOOP('',(#18789));
#7431=EDGE_LOOP('',(#18790,#18791,#18792,#18793));
#7432=EDGE_LOOP('',(#18794));
#7433=EDGE_LOOP('',(#18795));
#7434=EDGE_LOOP('',(#18796,#18797,#18798,#18799));
#7435=EDGE_LOOP('',(#18800,#18801,#18802,#18803));
#7436=EDGE_LOOP('',(#18804));
#7437=EDGE_LOOP('',(#18805,#18806,#18807,#18808));
#7438=EDGE_LOOP('',(#18809,#18810,#18811,#18812));
#7439=EDGE_LOOP('',(#18813,#18814,#18815,#18816));
#7440=EDGE_LOOP('',(#18817));
#7441=EDGE_LOOP('',(#18818));
#7442=EDGE_LOOP('',(#18819));
#7443=EDGE_LOOP('',(#18820));
#7444=EDGE_LOOP('',(#18821));
#7445=EDGE_LOOP('',(#18822,#18823,#18824,#18825));
#7446=EDGE_LOOP('',(#18826));
#7447=EDGE_LOOP('',(#18827));
#7448=EDGE_LOOP('',(#18828,#18829,#18830,#18831));
#7449=EDGE_LOOP('',(#18832,#18833,#18834,#18835));
#7450=EDGE_LOOP('',(#18836));
#7451=EDGE_LOOP('',(#18837));
#7452=EDGE_LOOP('',(#18838));
#7453=EDGE_LOOP('',(#18839));
#7454=EDGE_LOOP('',(#18840,#18841,#18842,#18843));
#7455=EDGE_LOOP('',(#18844,#18845,#18846,#18847));
#7456=EDGE_LOOP('',(#18848));
#7457=B_SPLINE_CURVE_WITH_KNOTS('',3,(#28468,#28469,#28470,#28471,#28472,
#28473),.UNSPECIFIED.,.F.,.F.,(4,1,1,4),(-0.999999999999995,-0.571428571428571,
-0.285714285714286,0.),.UNSPECIFIED.);
#7458=B_SPLINE_CURVE_WITH_KNOTS('',3,(#28475,#28476,#28477,#28478,#28479,
#28480,#28481,#28482),.UNSPECIFIED.,.F.,.F.,(4,2,2,4),(-13.0076216717983,
-12.6762562420903,-11.8531689108674,-11.7197155434785),.UNSPECIFIED.);
#7459=B_SPLINE_CURVE_WITH_KNOTS('',3,(#28483,#28484,#28485,#28486,#28487,
#28488,#28489,#28490,#28491,#28492,#28493,#28494,#28495,#28496,#28497,#28498,
#28499,#28500,#28501,#28502,#28503,#28504,#28505,#28506,#28507,#28508,#28509,
#28510,#28511,#28512,#28513,#28514,#28515,#28516,#28517,#28518,#28519,#28520,
#28521,#28522,#28523),.UNSPECIFIED.,.F.,.F.,(4,2,2,1,1,2,2,1,2,1,1,1,2,
1,1,1,2,1,1,1,1,1,1,1,1,1,1,2,1,1,4),(-11.7197155434785,-11.05258106389,
-10.1188927640438,-8.47830334468407,-7.04278760274435,-6.83771392532439,
-5.90055842268743,-5.54885349043522,-5.09666143468238,-4.98988621289018,
-4.88311099109797,-4.50939771482526,-4.24245966034475,-3.88978669781647,
-3.67818292029951,-3.43131184652972,-3.11390618025428,-3.0769781504351,
-2.96619406097756,-2.81848194170084,-2.7076978522433,-2.5230577031474,-1.93220922604053,
-1.78449710676381,-1.74756907694463,-1.34136074893366,-1.04593651038022,
-0.750512271826782,-0.60979122085926,-0.469070169891739,0.),
 .UNSPECIFIED.);
#7460=B_SPLINE_CURVE_WITH_KNOTS('',3,(#28525,#28526,#28527,#28528,#28529,
#28530),.UNSPECIFIED.,.F.,.F.,(4,1,1,4),(0.,0.469070169891739,0.60979122085926,
0.750512271826782),.UNSPECIFIED.);
#7461=B_SPLINE_CURVE_WITH_KNOTS('',3,(#28532,#28533,#28534,#28535,#28536,
#28537,#28538,#28539,#28540,#28541,#28542,#28543,#28544,#28545,#28546,#28547,
#28548,#28549,#28550,#28551,#28552,#28553,#28554,#28555,#28556,#28557,#28558,
#28559,#28560,#28561,#28562,#28563,#28564,#28565,#28566,#28567,#28568,#28569,
#28570,#28571,#28572,#28573,#28574,#28575,#28576,#28577,#28578,#28579,#28580,
#28581,#28582,#28583,#28584,#28585,#28586,#28587,#28588,#28589,#28590,#28591,
#28592,#28593,#28594,#28595,#28596,#28597,#28598,#28599,#28600,#28601,#28602,
#28603,#28604,#28605,#28606,#28607,#28608,#28609,#28610,#28611,#28612,#28613,
#28614,#28615,#28616,#28617,#28618,#28619,#28620,#28621,#28622,#28623,#28624,
#28625,#28626,#28627,#28628,#28629,#28630,#28631,#28632,#28633,#28634,#28635,
#28636,#28637,#28638,#28639,#28640,#28641,#28642,#28643,#28644,#28645,#28646,
#28647,#28648,#28649,#28650,#28651,#28652,#28653,#28654,#28655,#28656,#28657,
#28658,#28659,#28660,#28661,#28662,#28663,#28664,#28665,#28666,#28667,#28668,
#28669,#28670,#28671,#28672,#28673,#28674,#28675,#28676,#28677,#28678,#28679,
#28680,#28681,#28682,#28683,#28684,#28685,#28686,#28687,#28688,#28689,#28690,
#28691,#28692,#28693,#28694,#28695,#28696,#28697,#28698,#28699,#28700,#28701,
#28702,#28703,#28704,#28705,#28706),.UNSPECIFIED.,.F.,.F.,(4,3,3,3,3,3,
3,3,3,3,3,3,3,3,3,3,3,3,3,3,3,3,3,3,3,3,3,3,3,3,3,3,3,3,3,3,3,3,3,3,3,3,
3,3,3,3,3,3,3,3,3,3,3,3,3,3,3,3,4),(0.750707263401336,0.751073491522809,
0.770788600839354,0.797141727621928,0.801285493755856,0.847209334720936,
0.851576628686437,0.892702424300306,0.909155014790277,0.945842604423156,
0.959283328964777,0.973653029900114,1.02857295555953,1.04593651038022,1.10213659378528,
1.15946870078418,1.21910603297729,1.25714745759372,1.32249197142089,1.33169604227939,
1.34136074893366,1.40008364166717,1.46200856506941,1.53008670118818,1.60161378753395,
1.67565478609667,1.72643723062008,1.74756907694463,1.78449710676381,1.85969939535229,
1.93220922604053,2.0009848480779,2.06808195029472,2.1044635537539,2.17677612815408,
2.25426089464543,2.33537778995665,2.42383992559276,2.48665348358685,2.5230577031474,
2.55048767867042,2.63206152994388,2.7076978522433,2.81035120800203,2.81848194170084,
2.86928839618313,2.89438186295904,2.94470693815227,2.96619406097756,2.99737852476675,
3.02773642991363,3.05710875945002,3.07552489670663,3.0769781504351,3.08925644295071,
3.10116317170119,3.11177854192958,3.11306990045168,3.11390618025428),
 .UNSPECIFIED.);
#7462=B_SPLINE_CURVE_WITH_KNOTS('',3,(#28708,#28709,#28710,#28711,#28712,
#28713,#28714),.UNSPECIFIED.,.F.,.F.,(4,1,1,1,4),(3.1140516289664,3.43131184652972,
3.67818292029951,3.88978669781647,4.24245966034475),.UNSPECIFIED.);
#7463=B_SPLINE_CURVE_WITH_KNOTS('',3,(#28716,#28717,#28718,#28719,#28720,
#28721,#28722),.UNSPECIFIED.,.F.,.F.,(4,1,1,1,4),(4.24281193045545,4.50939771482526,
4.88311099109797,4.98988621289018,5.09562751764158),.UNSPECIFIED.);
#7464=B_SPLINE_CURVE_WITH_KNOTS('',3,(#28724,#28725,#28726,#28727,#28728,
#28729,#28730,#28731,#28732,#28733,#28734,#28735,#28736,#28737,#28738,#28739,
#28740,#28741,#28742,#28743,#28744,#28745,#28746,#28747,#28748,#28749,#28750,
#28751,#28752,#28753,#28754,#28755,#28756,#28757,#28758,#28759,#28760,#28761,
#28762,#28763,#28764,#28765,#28766,#28767,#28768,#28769,#28770,#28771,#28772,
#28773,#28774,#28775),.UNSPECIFIED.,.F.,.F.,(4,3,3,3,3,3,3,3,3,3,3,3,3,
3,3,3,3,4),(5.09666143468238,5.15433284711348,5.21357578985293,5.27511503720701,
5.34195092279717,5.41296344455248,5.48882370921057,5.4948675217662,5.54885349043522,
5.62257616633349,5.69588741785513,5.71679169498887,5.78286561201951,5.79781169784479,
5.83813276584378,5.84909385748713,5.87479360889014,5.90049336029315),
 .UNSPECIFIED.);
#7465=B_SPLINE_CURVE_WITH_KNOTS('',3,(#28777,#28778,#28779,#28780),
 .UNSPECIFIED.,.F.,.F.,(4,4),(5.90055842268743,6.83750114647945),
 .UNSPECIFIED.);
#7466=B_SPLINE_CURVE_WITH_KNOTS('',3,(#28782,#28783,#28784,#28785,#28786,
#28787),.UNSPECIFIED.,.F.,.F.,(4,1,1,4),(6.83771392532439,7.04278760274435,
8.47830334468407,10.1186669136909),.UNSPECIFIED.);
#7467=B_SPLINE_CURVE_WITH_KNOTS('',3,(#28789,#28790,#28791,#28792),
 .UNSPECIFIED.,.F.,.F.,(4,4),(10.1188927640438,11.05258106389),
 .UNSPECIFIED.);
#7468=B_SPLINE_CURVE_WITH_KNOTS('',3,(#28794,#28795,#28796,#28797),
 .UNSPECIFIED.,.F.,.F.,(4,4),(11.0525853415176,11.8531689108674),
 .UNSPECIFIED.);
#7469=B_SPLINE_CURVE_WITH_KNOTS('',3,(#28799,#28800,#28801,#28802),
 .UNSPECIFIED.,.F.,.F.,(4,4),(11.8532319611187,12.6762562420903),
 .UNSPECIFIED.);
#7470=B_SPLINE_CURVE_WITH_KNOTS('',3,(#28803,#28804,#28805,#28806),
 .UNSPECIFIED.,.F.,.F.,(4,4),(12.6763300349415,13.0076216717983),
 .UNSPECIFIED.);
#7471=B_SPLINE_CURVE_WITH_KNOTS('',3,(#28811,#28812,#28813,#28814,#28815,
#28816,#28817,#28818,#28819,#28820,#28821,#28822,#28823,#28824,#28825,#28826,
#28827,#28828,#28829,#28830,#28831,#28832,#28833,#28834,#28835,#28836,#28837,
#28838,#28839,#28840,#28841,#28842),.UNSPECIFIED.,.F.,.F.,(4,1,1,1,2,1,
1,1,1,2,1,1,1,2,1,1,1,2,2,1,2,2,4),(-9.55960092302324,-9.1896794456085,
-8.81975796819377,-8.44983649077903,-8.0799150133643,-8.03266253512535,
-7.98541005688641,-7.89090510040853,-7.70189518745276,-7.32387536154123,
-7.17881214312514,-7.03374892470906,-6.88868570629297,-6.74362248787689,
-6.67050437063,-6.59738625338311,-6.45115001888933,-6.15867754990177,-5.47160541199434,
-4.26766323501505,-3.06372105803577,-2.37819810334092,-1.88848372186453),
 .UNSPECIFIED.);
#7472=B_SPLINE_CURVE_WITH_KNOTS('',3,(#28843,#28844,#28845,#28846,#28847,
#28848,#28849,#28850,#28851,#28852,#28853,#28854,#28855),.UNSPECIFIED.,
 .F.,.F.,(4,2,2,1,2,1,1,4),(-1.88848372186453,-1.79056374069951,-1.18667868852568,
-0.800342864550781,-0.414007040575882,-0.310505280431912,-0.207003520287941,
0.),.UNSPECIFIED.);
#7473=B_SPLINE_CURVE_WITH_KNOTS('',3,(#38650,#38651,#38652,#38653,#38654,
#38655,#38656,#38657,#38658),.UNSPECIFIED.,.F.,.F.,(4,1,1,1,1,1,4),(0.,
0.208981284264062,0.626943852792187,0.835925137056249,1.04490642132031,
1.25388770558437,1.46286898984844),.UNSPECIFIED.);
#7474=B_SPLINE_CURVE_WITH_KNOTS('',3,(#38660,#38661,#38662,#38663,#38664,
#38665,#38666,#38667,#38668),.UNSPECIFIED.,.F.,.F.,(4,1,1,1,1,1,4),(1.46286898984844,
1.57811142102339,1.80859628337331,1.92383871454827,2.03908114572322,2.15432357689818,
2.26956600807314),.UNSPECIFIED.);
#7475=B_SPLINE_CURVE_WITH_KNOTS('',3,(#38670,#38671,#38672,#38673,#38674,
#38675,#38676,#38677,#38678,#38679,#38680,#38681,#38682,#38683,#38684,#38685,
#38686,#38687,#38688,#38689,#38690,#38691,#38692,#38693,#38694,#38695,#38696,
#38697,#38698,#38699,#38700,#38701,#38702,#38703,#38704,#38705,#38706,#38707,
#38708,#38709,#38710,#38711,#38712,#38713,#38714,#38715,#38716,#38717,#38718,
#38719,#38720,#38721,#38722,#38723,#38724,#38725,#38726,#38727,#38728,#38729,
#38730,#38731,#38732,#38733,#38734,#38735,#38736,#38737,#38738,#38739,#38740,
#38741,#38742,#38743,#38744,#38745,#38746,#38747,#38748,#38749,#38750,#38751,
#38752,#38753,#38754,#38755,#38756,#38757,#38758,#38759,#38760,#38761,#38762,
#38763),.UNSPECIFIED.,.F.,.F.,(4,3,3,3,3,3,3,3,3,3,3,3,3,3,3,3,3,3,3,3,
3,3,3,3,3,3,3,3,3,3,3,4),(2.26956600807314,2.31868576460897,2.36442460789209,
2.40351503906262,2.42718620051329,2.44122087175842,2.44260547023316,2.45341326627912,
2.46020489685124,2.46598765674336,2.4975277476721,2.51361070216978,2.52906783860085,
2.54765629078654,2.56502674195218,2.57656452038008,2.61240308621125,2.61582222590599,
2.62445098833827,2.62880283765034,2.63139315501457,2.63314063742138,2.65910316373393,
2.6848523253642,2.7024591242981,2.70904066964155,2.74512184182599,2.77027473318896,
2.78990851485099,2.83207741398362,2.86861528379491,2.87518401914012),
 .UNSPECIFIED.);
#7476=B_SPLINE_CURVE_WITH_KNOTS('',3,(#38765,#38766,#38767,#38768,#38769,
#38770,#38771,#38772,#38773,#38774),.UNSPECIFIED.,.F.,.F.,(4,2,2,2,4),(7.35574899264912E-13,
0.182950620511092,0.366672640482893,0.532787709398147,0.700945883028127),
 .UNSPECIFIED.);
#7477=B_SPLINE_CURVE_WITH_KNOTS('',3,(#38776,#38777,#38778,#38779,#38780,
#38781),.UNSPECIFIED.,.F.,.F.,(4,2,4),(0.,0.425557203103372,0.889753425869099),
 .UNSPECIFIED.);
#7478=B_SPLINE_CURVE_WITH_KNOTS('',3,(#38783,#38784,#38785,#38786,#38787,
#38788,#38789,#38790,#38791,#38792,#38793,#38794),.UNSPECIFIED.,.F.,.F.,
(4,1,1,1,1,1,1,1,1,4),(4.48918216137468,4.66429138725693,4.75184600019805,
4.83940061313917,5.53983751666817,5.89005596843266,6.06516519431491,6.24027442019716,
6.59049287196166,6.94071132372615),.UNSPECIFIED.);
#7479=B_SPLINE_CURVE_WITH_KNOTS('',3,(#38796,#38797,#38798,#38799),
 .UNSPECIFIED.,.F.,.F.,(4,4),(6.94071132372615,7.92790045161141),
 .UNSPECIFIED.);
#7480=B_SPLINE_CURVE_WITH_KNOTS('',3,(#38801,#38802,#38803,#38804,#38805,
#38806,#38807,#38808,#38809),.UNSPECIFIED.,.F.,.F.,(4,1,1,1,1,1,4),(7.92790045161141,
8.77117777664964,9.19281643916875,9.61445510168786,10.036093764207,10.4577324267261,
10.8793710892452),.UNSPECIFIED.);
#7481=B_SPLINE_CURVE_WITH_KNOTS('',3,(#38811,#38812,#38813,#38814,#38815,
#38816,#38817,#38818),.UNSPECIFIED.,.F.,.F.,(4,2,2,4),(3.5904242252203E-11,
0.260393756917535,0.343613662591379,0.431907573073398),.UNSPECIFIED.);
#7482=B_SPLINE_CURVE_WITH_KNOTS('',3,(#38820,#38821,#38822,#38823,#38824,
#38825),.UNSPECIFIED.,.F.,.F.,(4,1,1,4),(12.3501209228208,13.0134488895805,
13.455667534087,13.897886155505),.UNSPECIFIED.);
#7483=B_SPLINE_CURVE_WITH_KNOTS('',3,(#38827,#38828,#38829,#38830,#38831,
#38832,#38833,#38834,#38835,#38836,#38837,#38838,#38839,#38840,#38841,#38842,
#38843,#38844,#38845,#38846,#38847,#38848,#38849,#38850,#38851,#38852,#38853,
#38854,#38855,#38856,#38857,#38858,#38859,#38860,#38861,#38862,#38863,#38864,
#38865,#38866,#38867,#38868,#38869,#38870,#38871,#38872,#38873,#38874,#38875,
#38876,#38877,#38878,#38879,#38880,#38881,#38882,#38883,#38884,#38885,#38886,
#38887,#38888,#38889,#38890,#38891,#38892,#38893,#38894,#38895,#38896,#38897,
#38898,#38899,#38900,#38901,#38902,#38903,#38904,#38905,#38906,#38907,#38908,
#38909,#38910,#38911,#38912,#38913,#38914,#38915,#38916,#38917,#38918,#38919,
#38920,#38921,#38922,#38923,#38924,#38925,#38926,#38927,#38928,#38929,#38930,
#38931,#38932,#38933,#38934,#38935),.UNSPECIFIED.,.F.,.F.,(4,3,3,3,3,3,
3,3,3,3,3,3,3,3,3,3,3,3,3,3,3,3,3,3,3,3,3,3,3,3,3,3,3,3,3,3,4),(13.8978861785935,
13.9380361760921,13.9783662868224,14.0186963975526,14.0811238320635,14.1320902001938,
14.2193450517567,14.309644201861,14.3469219867698,14.4395096610908,14.5292417963811,
14.6174410389455,14.7034058274742,14.7629556872226,14.8165856516271,14.862262798083,
14.9374055100664,15.0109004941316,15.0838111850265,15.1563912070055,15.1837216712462,
15.255912890478,15.3277216735112,15.398965330592,15.4693404586375,15.5051805444094,
15.5645429684139,15.6227879721599,15.6376791692706,15.6977923210042,15.7622158692884,
15.8266394175726,15.8921244883675,15.960846906809,16.0317141617619,16.1063877532203,
16.1480982806684),.UNSPECIFIED.);
#7484=B_SPLINE_CURVE_WITH_KNOTS('',3,(#38937,#38938,#38939,#38940,#38941,
#38942,#38943,#38944),.UNSPECIFIED.,.F.,.F.,(4,1,1,1,1,4),(16.1480989104869,
17.1122318399124,17.4336096896379,17.7549875393634,17.9156764642262,18.3977432388145),
 .UNSPECIFIED.);
#7485=B_SPLINE_CURVE_WITH_KNOTS('',3,(#38946,#38947,#38948,#38949,#38950),
 .UNSPECIFIED.,.F.,.F.,(4,1,4),(-27.614177239717,-26.6900911654903,-25.4579763998548),
 .UNSPECIFIED.);
#7486=B_SPLINE_CURVE_WITH_KNOTS('',3,(#38952,#38953,#38954,#38955,#38956,
#38957,#38958,#38959,#38960,#38961,#38962,#38963,#38964,#38965,#38966,#38967,
#38968,#38969,#38970,#38971,#38972,#38973,#38974,#38975,#38976,#38977,#38978,
#38979,#38980,#38981,#38982,#38983,#38984,#38985,#38986,#38987,#38988,#38989,
#38990,#38991,#38992,#38993,#38994,#38995,#38996,#38997,#38998,#38999,#39000,
#39001,#39002,#39003,#39004,#39005,#39006,#39007,#39008,#39009,#39010,#39011,
#39012,#39013,#39014,#39015,#39016,#39017,#39018,#39019,#39020,#39021,#39022,
#39023,#39024,#39025,#39026,#39027,#39028,#39029,#39030,#39031,#39032,#39033,
#39034,#39035,#39036,#39037,#39038,#39039,#39040,#39041,#39042,#39043,#39044,
#39045,#39046,#39047,#39048,#39049,#39050,#39051),.UNSPECIFIED.,.F.,.F.,
(4,3,3,3,3,3,3,3,3,3,3,3,3,3,3,3,3,3,3,3,3,3,3,3,3,3,3,3,3,3,3,3,3,4),(-25.4579763998548,
-25.3889893896019,-25.3213768105525,-25.2555098807919,-25.2220083007855,
-25.1146742426374,-25.010880056723,-24.9872519938033,-24.8083237297656,
-24.6450684781262,-24.5215312467475,-24.3975168143727,-24.1846371236323,
-23.9923963326571,-23.8672870216316,-23.7144002286166,-23.6130418747886,
-23.4679899517189,-23.3238431903892,-23.1802452769976,-23.1590824865092,
-23.0157070639962,-22.8650467350538,-22.8068274361495,-22.7212423399242,
-22.5325850737667,-22.3597054148946,-22.2394602855688,-22.0850152108554,
-21.9930212690266,-21.8160728505053,-21.7959801689209,-21.7477190509971,
-21.7463678515301),.UNSPECIFIED.);
#7487=B_SPLINE_CURVE_WITH_KNOTS('',3,(#39053,#39054,#39055,#39056,#39057,
#39058,#39059,#39060,#39061),.UNSPECIFIED.,.F.,.F.,(4,1,1,1,1,1,4),(-21.7463678506673,
-21.0251854504292,-19.5828206499531,-18.861638249715,-18.140455849477,-17.4192734492389,
-16.6980910490008),.UNSPECIFIED.);
#7488=B_SPLINE_CURVE_WITH_KNOTS('',3,(#39063,#39064,#39065,#39066,#39067,
#39068,#39069,#39070,#39071,#39072),.UNSPECIFIED.,.F.,.F.,(4,1,1,1,1,1,
1,4),(-16.6980910490008,-16.0242682824596,-14.6766227493771,-14.0027999828359,
-13.3289772162947,-12.6551544497534,-12.3182430664828,-11.9813316832122),
 .UNSPECIFIED.);
#7489=B_SPLINE_CURVE_WITH_KNOTS('',3,(#39074,#39075,#39076,#39077,#39078,
#39079,#39080,#39081),.UNSPECIFIED.,.F.,.F.,(4,1,1,1,1,4),(-11.9813316832122,
-11.8608434310554,-11.7403551788986,-11.2584021702716,-10.7764491616445,
-10.2944961530174),.UNSPECIFIED.);
#7490=B_SPLINE_CURVE_WITH_KNOTS('',3,(#39083,#39084,#39085,#39086,#39087,
#39088,#39089,#39090,#39091),.UNSPECIFIED.,.F.,.F.,(4,1,1,1,1,1,4),(-10.2944961530174,
-9.9233650238383,-9.5522338946592,-9.18110276548009,-8.43884050712189,-8.06770937794279,
-7.69657824876369),.UNSPECIFIED.);
#7491=B_SPLINE_CURVE_WITH_KNOTS('',3,(#39093,#39094,#39095,#39096,#39097,
#39098,#39099,#39100,#39101,#39102),.UNSPECIFIED.,.F.,.F.,(4,1,1,1,1,1,
1,4),(-7.69657824876369,-7.30181972429585,-7.10444046206193,-6.90706119982801,
-6.80837156871105,-6.70968193759409,-6.51230267536017,-6.31492341312625),
 .UNSPECIFIED.);
#7492=B_SPLINE_CURVE_WITH_KNOTS('',3,(#39104,#39105,#39106,#39107,#39108,
#39109,#39110,#39111,#39112,#39113),.UNSPECIFIED.,.F.,.F.,(4,2,2,2,4),(6.84506442931943E-11,
0.102096969345333,0.201193147379825,0.268916988037693,0.641886390881406),
 .UNSPECIFIED.);
#7493=B_SPLINE_CURVE_WITH_KNOTS('',3,(#39115,#39116,#39117,#39118,#39119,
#39120),.UNSPECIFIED.,.F.,.F.,(4,1,1,4),(-5.24963521037055,-5.08288401419063,
-4.74938156648641,-4.08237667107798),.UNSPECIFIED.);
#7494=B_SPLINE_CURVE_WITH_KNOTS('',3,(#39122,#39123,#39124,#39125,#39126,
#39127),.UNSPECIFIED.,.F.,.F.,(4,1,1,4),(-4.08237667107798,-3.69276867472374,
-3.43303001048758,-3.17329134625142),.UNSPECIFIED.);
#7495=B_SPLINE_CURVE_WITH_KNOTS('',3,(#39129,#39130,#39131,#39132,#39133,
#39134),.UNSPECIFIED.,.F.,.F.,(4,1,1,4),(-3.17329134625142,-3.0004111005852,
-2.65465060925274,-1.96312962658784),.UNSPECIFIED.);
#7496=B_SPLINE_CURVE_WITH_KNOTS('',3,(#39136,#39137,#39138,#39139,#39140,
#39141),.UNSPECIFIED.,.F.,.F.,(4,1,1,4),(-1.96312962658784,-1.63061718285122,
-1.46436096098291,-0.799336073509661),.UNSPECIFIED.);
#7497=B_SPLINE_CURVE_WITH_KNOTS('',3,(#39143,#39144,#39145,#39146,#39147,
#39148,#39149,#39150,#39151,#39152,#39153,#39154,#39155,#39156,#39157,#39158),
 .UNSPECIFIED.,.F.,.F.,(4,2,2,2,2,2,2,4),(0.,0.0152664079390442,0.027653014192354,
0.0523618805947198,0.101540119432788,0.198808909364561,0.307282372348676,
0.415444261708341),.UNSPECIFIED.);
#7498=B_SPLINE_CURVE_WITH_KNOTS('',3,(#39160,#39161,#39162,#39163),
 .UNSPECIFIED.,.F.,.F.,(4,4),(-0.083360384276397,0.),.UNSPECIFIED.);
#7499=B_SPLINE_CURVE_WITH_KNOTS('',3,(#39165,#39166,#39167,#39168,#39169,
#39170,#39171,#39172,#39173,#39174,#39175,#39176,#39177,#39178,#39179,#39180,
#39181,#39182,#39183,#39184),.UNSPECIFIED.,.F.,.F.,(4,2,2,2,2,2,2,2,2,4),
(-0.858618632215441,-0.796721982029608,-0.711742820019591,-0.588477642133705,
-0.447897244908574,-0.350522204727673,-0.263299666311678,-0.166095103471627,
-0.0806423683440006,0.),.UNSPECIFIED.);
#7500=B_SPLINE_CURVE_WITH_KNOTS('',3,(#39186,#39187,#39188,#39189),
 .UNSPECIFIED.,.F.,.F.,(4,4),(0.,0.0412699530886637),.UNSPECIFIED.);
#7501=B_SPLINE_CURVE_WITH_KNOTS('',3,(#39191,#39192,#39193,#39194,#39195,
#39196,#39197,#39198,#39199,#39200,#39201,#39202,#39203,#39204,#39205,#39206,
#39207,#39208,#39209,#39210,#39211,#39212,#39213,#39214,#39215,#39216,#39217,
#39218,#39219,#39220,#39221,#39222,#39223,#39224,#39225,#39226,#39227,#39228,
#39229,#39230,#39231,#39232,#39233,#39234,#39235,#39236,#39237,#39238,#39239,
#39240,#39241,#39242,#39243,#39244,#39245,#39246,#39247,#39248,#39249,#39250,
#39251,#39252,#39253,#39254,#39255,#39256,#39257,#39258,#39259,#39260,#39261,
#39262,#39263),.UNSPECIFIED.,.F.,.F.,(4,3,3,3,3,3,3,3,3,3,3,3,3,3,3,3,3,
3,3,3,3,3,3,3,4),(0.0412699530886637,0.0818316212945925,0.127280583877176,
0.167222965675975,0.208677982151513,0.222888544302312,0.27017141431169,
0.306401513271525,0.345336818831997,0.360014116656582,0.363335263361059,
0.366168598848722,0.380743899105821,0.389827752889108,0.404046010130338,
0.437987441830756,0.459544829305343,0.475688276182035,0.525660573069947,
0.570392796077007,0.596688962991176,0.616464757561649,0.631242934104657,
0.642319205961073,0.675577463733683),.UNSPECIFIED.);
#7502=B_SPLINE_CURVE_WITH_KNOTS('',3,(#39265,#39266,#39267,#39268,#39269,
#39270,#39271),.UNSPECIFIED.,.F.,.F.,(4,1,1,1,4),(0.675577463735769,0.762573445120124,
0.936565407888833,1.11055737065754,1.28454933342625),.UNSPECIFIED.);
#7503=B_SPLINE_CURVE_WITH_KNOTS('',3,(#39273,#39274,#39275,#39276,#39277,
#39278,#39279,#39280,#39281,#39282),.UNSPECIFIED.,.F.,.F.,(4,1,1,1,1,1,
1,4),(1.28454933342625,1.68637707337851,1.88729094335464,1.93751941084867,
1.9877478783427,2.08820481333076,2.28911868330689,2.69094642325915),
 .UNSPECIFIED.);
#7504=B_SPLINE_CURVE_WITH_KNOTS('',3,(#39284,#39285,#39286,#39287,#39288,
#39289,#39290),.UNSPECIFIED.,.F.,.F.,(4,1,1,1,4),(2.69094642325915,3.62889794602885,
4.25419896120866,4.56684946879856,4.87949997638846),.UNSPECIFIED.);
#7505=B_SPLINE_CURVE_WITH_KNOTS('',3,(#39292,#39293,#39294,#39295,#39296,
#39297,#39298,#39299,#39300,#39301,#39302,#39303,#39304,#39305,#39306,#39307,
#39308,#39309,#39310,#39311,#39312,#39313,#39314,#39315,#39316,#39317,#39318,
#39319,#39320,#39321,#39322,#39323,#39324,#39325,#39326,#39327,#39328,#39329,
#39330,#39331,#39332,#39333,#39334,#39335,#39336,#39337,#39338,#39339,#39340,
#39341,#39342,#39343,#39344,#39345,#39346,#39347,#39348,#39349,#39350,#39351,
#39352,#39353,#39354,#39355,#39356,#39357,#39358,#39359,#39360,#39361,#39362,
#39363,#39364,#39365,#39366,#39367,#39368,#39369,#39370),.UNSPECIFIED.,
 .F.,.F.,(4,3,3,3,3,3,3,3,3,3,3,3,3,3,3,3,3,3,3,3,3,3,3,3,3,3,4),(4.87949998907266,
4.95846601833617,5.03754218990488,5.11201692992118,5.20633440915355,5.23893182822998,
5.33304562294149,5.42574668845617,5.51308570121414,5.56887242574961,5.57705083698662,
5.58713238475521,5.66474271049979,5.74432138797377,5.80956779051934,5.8835277857574,
5.96178045115228,5.96678376268769,6.04208474405206,6.13407813110945,6.21754073459664,
6.27460169758478,6.34310415203667,6.36106023233793,6.39702927495987,6.45672816597949,
6.5071186511175),.UNSPECIFIED.);
#7506=B_SPLINE_CURVE_WITH_KNOTS('',3,(#39372,#39373,#39374,#39375,#39376,
#39377,#39378,#39379,#39380,#39381,#39382,#39383,#39384,#39385,#39386,#39387,
#39388,#39389,#39390,#39391,#39392,#39393,#39394,#39395,#39396,#39397,#39398,
#39399,#39400,#39401,#39402,#39403,#39404,#39405,#39406,#39407,#39408,#39409,
#39410,#39411,#39412,#39413,#39414,#39415,#39416,#39417,#39418,#39419,#39420,
#39421,#39422,#39423,#39424,#39425,#39426,#39427,#39428,#39429,#39430,#39431,
#39432,#39433,#39434,#39435,#39436,#39437,#39438,#39439,#39440,#39441,#39442,
#39443,#39444,#39445,#39446,#39447,#39448,#39449,#39450,#39451,#39452,#39453,
#39454,#39455,#39456,#39457,#39458,#39459,#39460,#39461,#39462,#39463,#39464,
#39465,#39466,#39467,#39468,#39469,#39470,#39471,#39472,#39473,#39474),
 .UNSPECIFIED.,.F.,.F.,(4,3,3,3,3,3,3,3,3,3,3,3,3,3,3,3,3,3,3,3,3,3,3,3,
3,3,3,3,3,3,3,3,3,3,4),(6.50711865139611,6.50759747783067,6.55849518506602,
6.6055514827624,6.62030760880029,6.68061776690407,6.712779658626,6.76357285335593,
6.7827251429892,6.78667493342774,6.84072368001367,6.89838802619721,6.91844066613449,
6.9313826792552,6.93513738770287,6.96985591801162,7.02127116988874,7.08319431987471,
7.12333562472304,7.21448912595546,7.22693217739724,7.31027538715254,7.32976268115149,
7.39278093652575,7.48282966703091,7.48400843678286,7.53542368865998,7.54291222503036,
7.6182601558594,7.67703169440616,7.74108469616848,7.80585932729412,7.89114585771929,
7.94672668976107,7.94674570367697),.UNSPECIFIED.);
#7507=B_SPLINE_CURVE_WITH_KNOTS('',3,(#39476,#39477,#39478,#39479,#39480,
#39481,#39482,#39483,#39484,#39485,#39486),.UNSPECIFIED.,.F.,.F.,(4,1,1,
1,1,1,1,1,4),(0.,0.561198674779733,0.701498343474666,0.841798012169599,
0.982097680864532,1.12239734955947,1.40299668694933,1.6835960243392,1.96419536172906),
 .UNSPECIFIED.);
#7508=B_SPLINE_CURVE_WITH_KNOTS('',3,(#39488,#39489,#39490,#39491,#39492,
#39493,#39494,#39495,#39496,#39497,#39498,#39499,#39500,#39501,#39502,#39503,
#39504,#39505,#39506,#39507,#39508,#39509,#39510,#39511,#39512,#39513,#39514,
#39515,#39516,#39517,#39518,#39519,#39520,#39521,#39522,#39523,#39524,#39525,
#39526,#39527,#39528,#39529,#39530,#39531,#39532,#39533,#39534,#39535,#39536,
#39537,#39538,#39539,#39540,#39541,#39542,#39543,#39544,#39545,#39546,#39547,
#39548,#39549,#39550,#39551,#39552,#39553,#39554,#39555,#39556,#39557,#39558,
#39559,#39560,#39561,#39562,#39563,#39564,#39565,#39566,#39567,#39568,#39569,
#39570,#39571,#39572,#39573,#39574,#39575,#39576,#39577,#39578,#39579,#39580,
#39581),.UNSPECIFIED.,.F.,.F.,(4,3,3,3,3,3,3,3,3,3,3,3,3,3,3,3,3,3,3,3,
3,3,3,3,3,3,3,3,3,3,3,4),(1.96419536172906,2.02278079718735,2.08132684226757,
2.14059323164455,2.1643872272574,2.1995405412518,2.29893902795959,2.31381748093507,
2.34843033506652,2.43488572077454,2.55267608477937,2.66314540186569,2.67023090029728,
2.67711184811797,2.7608378847451,2.83320698228256,2.89993723462245,2.90557607982002,
2.97452259973018,3.04107121308078,3.10415755340534,3.12000863076421,3.14092125934276,
3.20590661407528,3.26963227096302,3.33186628772024,3.3762664388655,3.37817772008658,
3.45298028284022,3.52444999935711,3.59189483482569,3.61161161838824),
 .UNSPECIFIED.);
#7509=B_SPLINE_CURVE_WITH_KNOTS('',3,(#39583,#39584,#39585,#39586,#39587,
#39588,#39589),.UNSPECIFIED.,.F.,.F.,(4,1,1,1,4),(3.61161161838824,4.07783568596737,
4.23324370849375,4.54405975354651,4.69946777607289),.UNSPECIFIED.);
#7510=B_SPLINE_CURVE_WITH_KNOTS('',3,(#39591,#39592,#39593,#39594,#39595,
#39596,#39597,#39598,#39599,#39600,#39601,#39602,#39603,#39604,#39605,#39606,
#39607,#39608,#39609,#39610,#39611,#39612,#39613,#39614,#39615,#39616,#39617,
#39618,#39619,#39620,#39621,#39622,#39623,#39624,#39625,#39626,#39627,#39628,
#39629,#39630,#39631,#39632,#39633,#39634,#39635,#39636,#39637,#39638,#39639,
#39640,#39641,#39642,#39643,#39644,#39645,#39646,#39647,#39648,#39649,#39650,
#39651,#39652,#39653,#39654,#39655,#39656,#39657,#39658,#39659,#39660,#39661,
#39662,#39663,#39664,#39665,#39666,#39667,#39668,#39669),.UNSPECIFIED.,
 .F.,.F.,(4,3,3,3,3,3,3,3,3,3,3,3,3,3,3,3,3,3,3,3,3,3,3,3,3,3,4),(4.69946777607289,
4.70008212677047,4.72337034362506,4.74665856047964,4.78464222436074,4.79437105296614,
4.86335173767338,4.89331619143087,4.99100694367976,5.09449896259877,5.10579756798661,
5.21863815454279,5.34210882161955,5.47819569571612,5.58490842306537,5.73454801258545,
5.80455488046634,5.84054271537192,6.04704511696064,6.10124092996291,6.16726926099793,
6.23355124993576,6.36668501266555,6.43343772256572,6.46683837248413,6.50024667222643,
6.63337020876143),.UNSPECIFIED.);
#7511=B_SPLINE_CURVE_WITH_KNOTS('',3,(#39671,#39672,#39673,#39674,#39675,
#39676,#39677,#39678,#39679,#39680,#39681,#39682,#39683,#39684,#39685,#39686,
#39687,#39688,#39689,#39690,#39691,#39692,#39693,#39694,#39695,#39696,#39697,
#39698,#39699,#39700,#39701,#39702,#39703,#39704,#39705,#39706,#39707,#39708,
#39709,#39710,#39711,#39712,#39713,#39714,#39715,#39716,#39717,#39718,#39719,
#39720,#39721,#39722),.UNSPECIFIED.,.F.,.F.,(4,3,3,3,3,3,3,3,3,3,3,3,3,
3,3,3,3,4),(6.63337020876143,6.71835164595222,6.76468949711311,6.7848176488122,
6.86918510077649,6.91824398486027,7.12465942928312,7.21977330459364,7.45975726452654,
7.55231050612421,7.69215232698206,7.72134807390837,7.73908189390303,7.95493068281924,
8.18846010117661,8.41215537152321,8.61841637768341,8.77692550510397),
 .UNSPECIFIED.);
#7512=B_SPLINE_CURVE_WITH_KNOTS('',3,(#39724,#39725,#39726,#39727,#39728,
#39729),.UNSPECIFIED.,.F.,.F.,(4,1,1,4),(8.77692550510397,9.17723620667681,
9.97785760982251,11.5791004161139),.UNSPECIFIED.);
#7513=B_SPLINE_CURVE_WITH_KNOTS('',3,(#39731,#39732,#39733,#39734),
 .UNSPECIFIED.,.F.,.F.,(4,4),(11.5791004161139,11.7855397152994),
 .UNSPECIFIED.);
#7514=B_SPLINE_CURVE_WITH_KNOTS('',3,(#39736,#39737,#39738,#39739,#39740,
#39741,#39742,#39743,#39744,#39745,#39746,#39747,#39748,#39749,#39750,#39751,
#39752,#39753,#39754,#39755,#39756,#39757,#39758,#39759,#39760,#39761,#39762,
#39763,#39764,#39765,#39766,#39767,#39768,#39769,#39770,#39771,#39772,#39773,
#39774,#39775,#39776,#39777,#39778,#39779,#39780,#39781,#39782,#39783,#39784,
#39785,#39786,#39787),.UNSPECIFIED.,.F.,.F.,(4,3,3,3,3,3,3,3,3,3,3,3,3,
3,3,3,3,4),(0.,0.0536833715747986,0.107366743149597,0.161050114724396,0.214733486299194,
0.228154329192894,0.241575172086594,0.268416857873993,0.322100229448792,
0.34058124806175,0.37578360102359,0.429466972598389,0.509992029960587,0.590517087322785,
0.644200458897583,0.648567865518541,0.697883830472382,0.75156720204718),
 .UNSPECIFIED.);
#7515=B_SPLINE_CURVE_WITH_KNOTS('',3,(#39789,#39790,#39791,#39792),
 .UNSPECIFIED.,.F.,.F.,(4,4),(-76.3862538744791,-75.2949305236969),
 .UNSPECIFIED.);
#7516=B_SPLINE_CURVE_WITH_KNOTS('',3,(#39794,#39795,#39796,#39797,#39798,
#39799,#39800,#39801,#39802,#39803,#39804,#39805,#39806,#39807,#39808,#39809),
 .UNSPECIFIED.,.F.,.F.,(4,2,2,2,2,2,2,4),(0.,0.183117048783268,0.366537301552345,
0.538130301316899,0.626221380614023,0.670497094381026,0.692705457368327,
0.719797781043186),.UNSPECIFIED.);
#7517=B_SPLINE_CURVE_WITH_KNOTS('',3,(#39811,#39812,#39813,#39814,#39815),
 .UNSPECIFIED.,.F.,.F.,(4,1,4),(-66.1031756239825,-60.0916422517874,-52.076264422194),
 .UNSPECIFIED.);
#7518=B_SPLINE_CURVE_WITH_KNOTS('',3,(#39817,#39818,#39819,#39820,#39821,
#39822,#39823,#39824),.UNSPECIFIED.,.F.,.F.,(4,1,1,1,1,4),(-52.076264422194,
-47.0953817384218,-43.7747932825737,-42.1144990546496,-41.2843519406876,
-40.4542048267256),.UNSPECIFIED.);
#7519=B_SPLINE_CURVE_WITH_KNOTS('',3,(#39826,#39827,#39828,#39829,#39830,
#39831,#39832,#39833,#39834,#39835,#39836,#39837,#39838,#39839,#39840,#39841,
#39842,#39843,#39844,#39845,#39846,#39847,#39848,#39849,#39850,#39851,#39852,
#39853,#39854,#39855,#39856,#39857,#39858,#39859,#39860,#39861,#39862,#39863,
#39864,#39865,#39866,#39867,#39868,#39869,#39870,#39871,#39872,#39873,#39874,
#39875,#39876,#39877,#39878,#39879,#39880,#39881,#39882,#39883,#39884,#39885,
#39886,#39887,#39888,#39889,#39890,#39891,#39892,#39893,#39894,#39895,#39896,
#39897,#39898,#39899,#39900,#39901,#39902,#39903,#39904,#39905,#39906,#39907,
#39908,#39909,#39910,#39911,#39912,#39913,#39914,#39915,#39916,#39917,#39918,
#39919,#39920,#39921,#39922,#39923,#39924,#39925,#39926,#39927,#39928,#39929,
#39930,#39931,#39932,#39933,#39934,#39935,#39936,#39937,#39938,#39939,#39940,
#39941,#39942,#39943,#39944,#39945,#39946,#39947,#39948,#39949,#39950,#39951,
#39952,#39953,#39954,#39955,#39956,#39957,#39958,#39959,#39960,#39961),
 .UNSPECIFIED.,.F.,.F.,(4,3,3,3,3,3,3,3,3,3,3,3,3,3,3,3,3,3,3,3,3,3,3,3,
3,3,3,3,3,3,3,3,3,3,3,3,3,3,3,3,3,3,3,3,3,4),(-40.4542048267256,-40.1022888941731,
-39.7562065398827,-39.4194632193958,-39.1058191008429,-38.933143939164,
-38.6244983462993,-38.3981006364017,-38.3280947633795,-38.2582169507945,
-38.1717029265041,-38.1044071679005,-38.0424313761866,-37.8847341943161,
-37.8522360082441,-37.8370823843021,-37.6848449686041,-37.5482438086545,
-37.5103390037277,-37.4116426487049,-37.3168209132788,-37.26909277659,-37.2226826845227,
-37.0094865067236,-36.83127763601,-36.7421017606314,-36.702172602122,-36.6530687652964,
-36.5482684339635,-36.4793361229095,-36.3083732393702,-36.2040398925353,
-36.1567733945135,-36.1373900755466,-36.119432910608,-35.9439828384436,
-35.8910398520304,-35.7861271288821,-35.6763044151121,-35.5398153198633,
-35.475355900409,-35.431857525938,-35.3193842642253,-35.2761527725057,-35.1765274058965,
-35.1303480341168),.UNSPECIFIED.);
#7520=B_SPLINE_CURVE_WITH_KNOTS('',3,(#39963,#39964,#39965,#39966,#39967,
#39968,#39969,#39970,#39971,#39972,#39973,#39974,#39975,#39976,#39977,#39978,
#39979,#39980,#39981,#39982,#39983,#39984,#39985,#39986,#39987,#39988,#39989,
#39990,#39991,#39992,#39993,#39994,#39995,#39996,#39997,#39998,#39999,#40000,
#40001,#40002,#40003,#40004,#40005,#40006,#40007,#40008,#40009,#40010,#40011,
#40012,#40013,#40014,#40015,#40016,#40017,#40018,#40019,#40020,#40021,#40022,
#40023,#40024,#40025,#40026,#40027,#40028,#40029,#40030,#40031,#40032,#40033,
#40034,#40035),.UNSPECIFIED.,.F.,.F.,(4,3,3,3,3,3,3,3,3,3,3,3,3,3,3,3,3,
3,3,3,3,3,3,3,4),(-35.1303480022468,-35.1258447959463,-34.8587472887927,
-34.5695675087557,-34.2705671521664,-33.9510365315198,-33.7020281686448,
-33.4584584867811,-33.1570167675092,-32.7424918126182,-32.3093224434396,
-32.2207562081337,-31.7865689394453,-31.4628125680942,-31.1408963345733,
-30.9506241657775,-30.8303818716246,-30.4481649386763,-30.0912580436924,
-29.8395659206186,-29.6953645849095,-29.5361530629831,-29.3729500851293,
-29.2794465468541,-29.2787346184417),.UNSPECIFIED.);
#7521=B_SPLINE_CURVE_WITH_KNOTS('',3,(#40037,#40038,#40039,#40040,#40041,
#40042,#40043,#40044,#40045,#40046),.UNSPECIFIED.,.F.,.F.,(4,2,2,2,4),(0.,
0.081213735526853,0.152682973202012,0.298883812384628,0.584812965668925),
 .UNSPECIFIED.);
#7522=B_SPLINE_CURVE_WITH_KNOTS('',3,(#40048,#40049,#40050,#40051,#40052,
#40053,#40054,#40055),.UNSPECIFIED.,.F.,.F.,(4,1,1,1,1,4),(-20.9230961620266,
-17.7936201740765,-15.7073028487765,-14.6641441861265,-14.1425648548015,
-13.6209855234765),.UNSPECIFIED.);
#7523=B_SPLINE_CURVE_WITH_KNOTS('',3,(#40057,#40058,#40059,#40060,#40061,
#40062,#40063,#40064),.UNSPECIFIED.,.F.,.F.,(4,1,1,1,1,4),(-13.6209855234765,
-10.9458199140635,-10.0540980442592,-9.16237617445491,-8.2706543046506,
-7.37893243484629),.UNSPECIFIED.);
#7524=B_SPLINE_CURVE_WITH_KNOTS('',3,(#40066,#40067,#40068,#40069,#40070,
#40071,#40072,#40073,#40074,#40075,#40076),.UNSPECIFIED.,.F.,.F.,(4,1,1,
1,1,1,1,1,4),(-7.37893243484629,-6.86694230253758,-5.84296203792017,-4.81898177330275,
-4.56298670714839,-4.46698855734051,-4.30699164099404,-4.05099657483969,
-3.79500150868533),.UNSPECIFIED.);
#7525=B_SPLINE_CURVE_WITH_KNOTS('',3,(#40078,#40079,#40080,#40081,#40082,
#40083,#40084,#40085,#40086,#40087,#40088),.UNSPECIFIED.,.F.,.F.,(4,1,1,
1,1,1,1,1,4),(-3.79500150868533,-3.54558322444133,-3.04674665595333,-2.92203751383133,
-2.79732837170933,-2.67261922958733,-2.54791008746534,-2.29849180322134,
-2.04907351897734),.UNSPECIFIED.);
#7526=B_SPLINE_CURVE_WITH_KNOTS('',3,(#40090,#40091,#40092,#40093,#40094,
#40095,#40096,#40097,#40098,#40099),.UNSPECIFIED.,.F.,.F.,(4,1,1,1,1,1,
1,4),(-2.04907351897734,-1.91473526774895,-1.64605876529219,-1.5117205140638,
-1.37738226283542,-1.24304401160704,-1.17587488599285,-1.10870576037865),
 .UNSPECIFIED.);
#7527=B_SPLINE_CURVE_WITH_KNOTS('',3,(#40101,#40102,#40103,#40104,#40105,
#40106,#40107,#40108,#40109),.UNSPECIFIED.,.F.,.F.,(4,1,1,1,1,1,4),(-1.10870576037865,
-1.01091721837057,-0.913128676362484,-0.815340134354398,-0.766445863350356,
-0.619763050338228,-0.424185966322057),.UNSPECIFIED.);
#7528=B_SPLINE_CURVE_WITH_KNOTS('',3,(#40111,#40112,#40113,#40114),
 .UNSPECIFIED.,.F.,.F.,(4,4),(-0.424185966322057,0.),.UNSPECIFIED.);
#7529=B_SPLINE_CURVE_WITH_KNOTS('',3,(#40116,#40117,#40118,#40119,#40120,
#40121,#40122,#40123,#40124,#40125),.UNSPECIFIED.,.F.,.F.,(4,1,1,1,1,1,
1,4),(0.,0.21623669638068,0.324355044571019,0.432473392761359,0.540591740951699,
0.648710089142039,0.702769263237209,0.756828282974645),.UNSPECIFIED.);
#7530=B_SPLINE_CURVE_WITH_KNOTS('',3,(#40127,#40128,#40129,#40130,#40131,
#40132,#40133,#40134,#40135,#40136,#40137,#40138,#40139,#40140,#40141,#40142,
#40143,#40144,#40145,#40146,#40147,#40148,#40149,#40150,#40151,#40152,#40153,
#40154,#40155,#40156,#40157,#40158,#40159,#40160,#40161,#40162,#40163,#40164,
#40165,#40166,#40167,#40168,#40169,#40170,#40171,#40172,#40173,#40174,#40175,
#40176,#40177,#40178,#40179,#40180,#40181,#40182,#40183,#40184,#40185,#40186,
#40187,#40188,#40189,#40190,#40191,#40192,#40193,#40194,#40195,#40196,#40197,
#40198,#40199,#40200,#40201,#40202,#40203,#40204,#40205,#40206,#40207,#40208,
#40209,#40210,#40211,#40212,#40213,#40214,#40215,#40216,#40217,#40218,#40219,
#40220,#40221,#40222,#40223,#40224,#40225,#40226,#40227,#40228,#40229,#40230,
#40231,#40232,#40233,#40234,#40235,#40236,#40237,#40238,#40239,#40240,#40241,
#40242,#40243,#40244,#40245,#40246,#40247,#40248,#40249,#40250),
 .UNSPECIFIED.,.F.,.F.,(4,3,3,3,3,3,3,3,3,3,3,3,3,3,3,3,3,3,3,3,3,3,3,3,
3,3,3,3,3,3,3,3,3,3,3,3,3,3,3,3,3,4),(0.75682843983895,0.777855768006281,
0.798415570084359,0.818399869123068,0.828970599685942,0.84657569246793,
0.863552669234487,0.879734247088197,0.887389032088879,0.901112762039505,
0.912418616344217,0.919148302627896,0.933698235587157,0.937183843216286,
0.958433684197906,0.973254924393068,0.994408075484192,1.00932600556985,
1.02736154615824,1.03637931645244,1.04539708674663,1.06102318516838,1.07723388409314,
1.09375127908744,1.11068703369019,1.11753924910019,1.12521404406605,1.13678529162007,
1.15070887827124,1.16479420266661,1.17931025663697,1.18968141145376,1.20343576632493,
1.20608689093743,1.22052173269292,1.22575249263054,1.23445659171005,1.24399746592949,
1.2482472022461,1.254096563094,1.25979095927171,1.26182357380732),
 .UNSPECIFIED.);
#7531=B_SPLINE_CURVE_WITH_KNOTS('',3,(#40252,#40253,#40254,#40255,#40256,
#40257,#40258,#40259,#40260,#40261,#40262,#40263,#40264,#40265,#40266,#40267,
#40268,#40269,#40270,#40271,#40272,#40273,#40274,#40275,#40276,#40277,#40278,
#40279,#40280,#40281,#40282,#40283,#40284,#40285,#40286,#40287,#40288,#40289,
#40290,#40291,#40292,#40293,#40294,#40295,#40296,#40297,#40298,#40299,#40300,
#40301,#40302,#40303,#40304,#40305,#40306,#40307,#40308,#40309,#40310,#40311,
#40312,#40313,#40314,#40315,#40316,#40317,#40318),.UNSPECIFIED.,.F.,.F.,
(4,3,3,3,3,3,3,3,3,3,3,3,3,3,3,3,3,3,3,3,3,3,4),(1.26182357380732,1.26310836126709,
1.26448943174598,1.28057362669222,1.28823756969933,1.30269384661357,1.30996639391098,
1.32430281701794,1.32960413527727,1.33493261849779,1.34310096601661,1.3469432325596,
1.34924187664357,1.35187874054377,1.3592939367365,1.36865825613663,1.38371245588514,
1.38814353058811,1.39144562654905,1.39590278038911,1.4118599289142,1.42978166972109,
1.43249195629979),.UNSPECIFIED.);
#7532=B_SPLINE_CURVE_WITH_KNOTS('',3,(#40320,#40321,#40322,#40323,#40324,
#40325,#40326,#40327,#40328,#40329,#40330,#40331,#40332,#40333),
 .UNSPECIFIED.,.F.,.F.,(4,2,2,2,2,2,4),(0.,0.0578367417336795,0.106933208379369,
0.202213644056447,0.263225317305196,0.417445308347203,0.566894598811129),
 .UNSPECIFIED.);
#7533=B_SPLINE_CURVE_WITH_KNOTS('',3,(#40335,#40336,#40337,#40338,#40339,
#40340,#40341,#40342,#40343,#40344,#40345,#40346,#40347,#40348,#40349,#40350,
#40351,#40352,#40353,#40354,#40355,#40356,#40357,#40358,#40359,#40360,#40361,
#40362,#40363,#40364,#40365,#40366,#40367,#40368,#40369,#40370,#40371,#40372,
#40373,#40374,#40375,#40376,#40377,#40378,#40379,#40380,#40381,#40382,#40383,
#40384,#40385,#40386,#40387,#40388,#40389,#40390,#40391,#40392,#40393,#40394,
#40395,#40396,#40397,#40398,#40399,#40400,#40401,#40402,#40403,#40404,#40405,
#40406,#40407,#40408,#40409,#40410,#40411,#40412,#40413,#40414,#40415,#40416,
#40417,#40418,#40419,#40420,#40421,#40422,#40423,#40424,#40425),
 .UNSPECIFIED.,.F.,.F.,(4,3,3,3,3,3,3,3,3,3,3,3,3,3,3,3,3,3,3,3,3,3,3,3,
3,3,3,3,3,3,4),(1.56845677767309,1.56846172637483,1.57845303864828,1.58918112661639,
1.60105011224252,1.60181606521468,1.62530741495631,1.65075769300814,1.65649085724454,
1.66853464029784,1.67051106563605,1.69204727198684,1.70189392783942,1.71900500530774,
1.735253215381,1.73723529695383,1.7435930372664,1.74892582684199,1.75193285915179,
1.75254514822567,1.75874043000982,1.76460430548112,1.76861250292259,1.77474630213318,
1.78135331945415,1.78529214669338,1.79226862981698,1.79301029063736,1.79918428811343,
1.80197176948314,1.80197179046417),.UNSPECIFIED.);
#7534=B_SPLINE_CURVE_WITH_KNOTS('',3,(#40427,#40428,#40429,#40430,#40431,
#40432),.UNSPECIFIED.,.F.,.F.,(4,1,1,4),(1.80197179046417,1.80928949299685,
1.8129483442632,1.82758374932857),.UNSPECIFIED.);
#7535=B_SPLINE_CURVE_WITH_KNOTS('',3,(#40434,#40435,#40436,#40437,#40438,
#40439,#40440,#40441,#40442),.UNSPECIFIED.,.F.,.F.,(4,1,1,1,1,1,4),(1.82758374932857,
1.83805116497033,1.84328487279121,1.85898599625385,1.87992082753738,1.89038824317914,
1.9008556588209),.UNSPECIFIED.);
#7536=B_SPLINE_CURVE_WITH_KNOTS('',3,(#40444,#40445,#40446,#40447,#40448,
#40449,#40450,#40451,#40452,#40453,#40454,#40455),.UNSPECIFIED.,.F.,.F.,
(4,2,2,2,2,4),(0.,0.399925490199206,0.590873146475409,0.6853407600757,0.732736191576422,
0.780059088229237),.UNSPECIFIED.);
#7537=B_SPLINE_CURVE_WITH_KNOTS('',3,(#40457,#40458,#40459,#40460,#40461,
#40462,#40463,#40464),.UNSPECIFIED.,.F.,.F.,(4,1,1,1,1,4),(1.96650114296421,
1.97401285460172,1.97651675848088,1.98653237399755,2.00656360503089,2.03661045158091),
 .UNSPECIFIED.);
#7538=B_SPLINE_CURVE_WITH_KNOTS('',3,(#40466,#40467,#40468,#40469,#40470,
#40471,#40472,#40473,#40474,#40475,#40476,#40477,#40478,#40479,#40480,#40481,
#40482,#40483,#40484,#40485,#40486,#40487,#40488,#40489,#40490,#40491,#40492,
#40493,#40494,#40495,#40496,#40497,#40498,#40499,#40500,#40501,#40502,#40503,
#40504,#40505,#40506,#40507,#40508,#40509,#40510,#40511,#40512,#40513,#40514,
#40515,#40516,#40517,#40518,#40519,#40520,#40521,#40522,#40523,#40524,#40525,
#40526,#40527,#40528,#40529,#40530,#40531,#40532,#40533,#40534,#40535,#40536,
#40537,#40538,#40539,#40540,#40541),.UNSPECIFIED.,.F.,.F.,(4,3,3,3,3,3,
3,3,3,3,3,3,3,3,3,3,3,3,3,3,3,3,3,3,3,4),(2.03661045158091,2.04094396755524,
2.04146916453237,2.04613737339918,2.05247626445997,2.05498033734634,2.05614902505797,
2.05989481366869,2.06138177904424,2.06402869927639,2.06416861681123,2.06575962872735,
2.06835564146826,2.06972997740258,2.07334626528165,2.07526740689269,2.07848486059925,
2.08105152526794,2.08251647649159,2.0869107221265,2.09126152036397,2.09170330290054,
2.09261961436811,2.09495872614039,2.09994461036642,2.10087562037983),
 .UNSPECIFIED.);
#7539=B_SPLINE_CURVE_WITH_KNOTS('',3,(#40543,#40544,#40545,#40546,#40547,
#40548,#40549,#40550),.UNSPECIFIED.,.F.,.F.,(4,1,1,1,1,4),(2.10087562037983,
2.11383027239681,2.12678492441379,2.13973957643076,2.15269422844774,2.19155818449868),
 .UNSPECIFIED.);
#7540=B_SPLINE_CURVE_WITH_KNOTS('',3,(#40551,#40552,#40553,#40554,#40555,
#40556,#40557,#40558,#40559,#40560,#40561),.UNSPECIFIED.,.F.,.F.,(4,1,1,
1,1,1,1,1,4),(2.19155818449868,2.25090656855756,2.280580760587,2.31025495261644,
2.32509204863116,2.33992914464588,2.36960333667532,2.48830010479308,2.60699687291084),
 .UNSPECIFIED.);
#7541=B_SPLINE_CURVE_WITH_KNOTS('',3,(#40564,#40565,#40566,#40567),
 .UNSPECIFIED.,.F.,.F.,(4,4),(8.92039936009897,9.19419977830157),
 .UNSPECIFIED.);
#7542=B_SPLINE_CURVE_WITH_KNOTS('',3,(#40569,#40570,#40571,#40572,#40573),
 .UNSPECIFIED.,.F.,.F.,(4,1,4),(8.15775006426363,8.53897544224619,8.92020082022876),
 .UNSPECIFIED.);
#7543=B_SPLINE_CURVE_WITH_KNOTS('',3,(#40575,#40576,#40577,#40578,#40579,
#40580,#40581,#40582,#40583,#40584),.UNSPECIFIED.,.F.,.F.,(4,1,1,1,1,1,
1,4),(6.48647098475663,6.695380869695,6.79983581216419,7.11320063957175,
7.32211052451013,7.73993029438688,7.94884017932526,8.15741223597716),
 .UNSPECIFIED.);
#7544=B_SPLINE_CURVE_WITH_KNOTS('',3,(#40586,#40587,#40588,#40589,#40590,
#40591,#40592,#40593),.UNSPECIFIED.,.F.,.F.,(4,1,1,1,1,4),(5.69008244730366,
5.73985673089448,6.08827671603015,6.28737385039339,6.38692241757501,6.48619760405534),
 .UNSPECIFIED.);
#7545=B_SPLINE_CURVE_WITH_KNOTS('',3,(#40595,#40596,#40597,#40598,#40599,
#40600),.UNSPECIFIED.,.F.,.F.,(4,1,1,4),(5.0872072523488,5.23775148821748,
5.46391696776057,5.68999089118309),.UNSPECIFIED.);
#7546=B_SPLINE_CURVE_WITH_KNOTS('',3,(#40602,#40603,#40604,#40605,#40606,
#40607,#40608,#40609,#40610,#40611,#40612,#40613,#40614,#40615,#40616,#40617,
#40618,#40619,#40620,#40621,#40622,#40623,#40624,#40625,#40626,#40627,#40628,
#40629,#40630,#40631,#40632,#40633,#40634,#40635,#40636,#40637,#40638,#40639,
#40640,#40641,#40642,#40643,#40644,#40645,#40646,#40647,#40648,#40649,#40650,
#40651,#40652,#40653,#40654,#40655,#40656,#40657,#40658,#40659,#40660,#40661,
#40662,#40663,#40664,#40665,#40666,#40667,#40668,#40669,#40670,#40671,#40672,
#40673,#40674,#40675,#40676,#40677,#40678,#40679,#40680,#40681,#40682,#40683,
#40684,#40685,#40686,#40687,#40688,#40689),.UNSPECIFIED.,.F.,.F.,(4,3,3,
3,3,3,3,3,3,3,3,3,3,3,3,3,3,3,3,3,3,3,3,3,3,3,3,3,3,4),(4.51907254078117,
4.53712760209195,4.55524502799627,4.58345241158194,4.59126693036747,4.63722241805352,
4.67952721516863,4.7331373450095,4.76807910083128,4.77947322679447,4.78810538931333,
4.79482326640033,4.80302085665306,4.85270069873456,4.89887935926951,4.92360162081649,
4.94505801980446,4.95913352209898,4.9876580014522,4.99800173990669,5.00635849847016,
5.01618248080543,5.0429821330202,5.04445279252107,5.04585552133343,5.06059676426369,
5.06978178523498,5.07641636177966,5.08212660863856,5.08697450185542),
 .UNSPECIFIED.);
#7547=B_SPLINE_CURVE_WITH_KNOTS('',3,(#40691,#40692,#40693,#40694,#40695,
#40696,#40697,#40698,#40699,#40700,#40701,#40702,#40703,#40704,#40705,#40706,
#40707,#40708,#40709,#40710,#40711,#40712,#40713,#40714,#40715,#40716,#40717,
#40718,#40719,#40720,#40721,#40722,#40723,#40724,#40725,#40726,#40727),
 .UNSPECIFIED.,.F.,.F.,(4,3,3,3,3,3,3,3,3,3,3,3,4),(3.85684119100481,3.91047824257307,
3.95181977233274,4.01079062239622,4.04211759527654,4.1085062410119,4.17423090387904,
4.21136616955803,4.27069680674408,4.33497634591462,4.3997079256963,4.46637693241926,
4.51901017618764),.UNSPECIFIED.);
#7548=B_SPLINE_CURVE_WITH_KNOTS('',3,(#40729,#40730,#40731,#40732,#40733,
#40734,#40735,#40736,#40737,#40738,#40739,#40740,#40741,#40742,#40743,#40744,
#40745,#40746,#40747,#40748,#40749,#40750,#40751,#40752,#40753,#40754,#40755,
#40756,#40757,#40758,#40759,#40760,#40761,#40762,#40763,#40764,#40765,#40766,
#40767,#40768,#40769,#40770,#40771,#40772,#40773,#40774,#40775,#40776,#40777,
#40778,#40779,#40780,#40781,#40782,#40783,#40784,#40785,#40786,#40787,#40788,
#40789,#40790,#40791,#40792,#40793,#40794,#40795,#40796,#40797,#40798,#40799,
#40800,#40801,#40802,#40803,#40804,#40805,#40806,#40807,#40808,#40809,#40810,
#40811,#40812,#40813,#40814,#40815,#40816,#40817,#40818,#40819,#40820,#40821,
#40822,#40823,#40824,#40825,#40826,#40827,#40828),.UNSPECIFIED.,.F.,.F.,
(4,3,3,3,3,3,3,3,3,3,3,3,3,3,3,3,3,3,3,3,3,3,3,3,3,3,3,3,3,3,3,3,3,4),(1.53737298748225,
1.537475501564,1.62471277683277,1.68224296751281,1.77970297709453,1.78982695102308,
1.89509654051106,1.94309417534619,2.01390543033174,2.13717094946317,2.22810612528141,
2.34701828393927,2.47132786358456,2.4844090542388,2.49779593851528,2.611265334802,
2.69705547180907,2.7627193750795,2.88707829944944,2.90505995762026,3.03180902855002,
3.05948850905774,3.17551646821549,3.28049105931471,3.31567602520587,3.3763625860723,
3.46415464024906,3.54686387816802,3.61857318381905,3.62957311608698,3.69899296203923,
3.76450131194205,3.82520333218962,3.8565699837029),.UNSPECIFIED.);
#7549=B_SPLINE_CURVE_WITH_KNOTS('',3,(#40830,#40831,#40832,#40833,#40834),
 .UNSPECIFIED.,.F.,.F.,(4,1,4),(0.876829184656479,1.28960453962952,1.53726975261334),
 .UNSPECIFIED.);
#7550=B_SPLINE_CURVE_WITH_KNOTS('',3,(#40836,#40837,#40838,#40839),
 .UNSPECIFIED.,.F.,.F.,(4,4),(0.308773622131097,0.87661110736348),
 .UNSPECIFIED.);
#7551=B_SPLINE_CURVE_WITH_KNOTS('',3,(#40843,#40844,#40845,#40846,#40847,
#40848,#40849,#40850),.UNSPECIFIED.,.F.,.F.,(4,1,1,1,1,4),(0.775828301632668,
0.878761919402114,0.982054302260506,1.0853466851189,1.18863906797729,1.29193144447076),
 .UNSPECIFIED.);
#7552=B_SPLINE_CURVE_WITH_KNOTS('',3,(#40852,#40853,#40854,#40855,#40856,
#40857,#40858,#40859,#40860,#40861,#40862,#40863,#40864,#40865,#40866,#40867,
#40868,#40869,#40870,#40871,#40872,#40873,#40874,#40875,#40876,#40877,#40878,
#40879,#40880,#40881,#40882,#40883,#40884,#40885,#40886,#40887,#40888,#40889,
#40890,#40891,#40892,#40893,#40894,#40895,#40896,#40897,#40898,#40899,#40900,
#40901,#40902,#40903,#40904,#40905,#40906,#40907,#40908,#40909,#40910,#40911,
#40912,#40913,#40914,#40915,#40916,#40917,#40918,#40919,#40920,#40921),
 .UNSPECIFIED.,.F.,.F.,(4,3,3,3,3,3,3,3,3,3,3,3,3,3,3,3,3,3,3,3,3,3,3,4),
(0.226711159264386,0.240430118696369,0.254149078128352,0.281586996992319,
0.309024915856286,0.336462834720253,0.345475183164287,0.367386959070664,
0.395956346646867,0.424538765869713,0.44621451017612,0.473767544818013,
0.501191131249028,0.528641986740118,0.555966185631988,0.582919689839201,
0.609300375584998,0.634902866651908,0.6564639477599,0.665717861087855,0.694693069811103,
0.720593698815789,0.751264274684911,0.775469536543723),.UNSPECIFIED.);
#7553=B_SPLINE_CURVE_WITH_KNOTS('',3,(#40922,#40923,#40924,#40925,#40926,
#40927,#40928,#40929,#40930,#40931,#40932,#40933,#40934,#40935,#40936,#40937,
#40938,#40939,#40940,#40941,#40942,#40943,#40944,#40945,#40946,#40947,#40948,
#40949,#40950,#40951,#40952,#40953,#40954,#40955,#40956,#40957,#40958,#40959,
#40960,#40961,#40962,#40963,#40964,#40965,#40966,#40967,#40968,#40969,#40970,
#40971,#40972,#40973,#40974,#40975,#40976),.UNSPECIFIED.,.F.,.F.,(4,3,3,
3,3,3,3,3,3,3,3,3,3,3,3,3,3,3,4),(0.,0.00642281904770877,0.0274552042125774,
0.0483280032850625,0.0693493298709818,0.0906129623706381,0.112532404043595,
0.127771446025698,0.136026695558631,0.157567456770955,0.177849900137661,
0.181368927411508,0.193072040312714,0.201907114453229,0.209483636975919,
0.213952085004803,0.218360348732736,0.222453779943677,0.226477259692083),
 .UNSPECIFIED.);
#7554=B_SPLINE_CURVE_WITH_KNOTS('',3,(#40979,#40980,#40981,#40982),
 .UNSPECIFIED.,.F.,.F.,(4,4),(-0.314285883924713,-0.267175740076542),
 .UNSPECIFIED.);
#7555=B_SPLINE_CURVE_WITH_KNOTS('',3,(#40984,#40985,#40986,#40987,#40988,
#40989,#40990,#40991,#40992,#40993,#40994,#40995,#40996,#40997,#40998,#40999,
#41000,#41001,#41002,#41003,#41004,#41005,#41006,#41007,#41008,#41009,#41010,
#41011,#41012,#41013,#41014),.UNSPECIFIED.,.F.,.F.,(4,3,3,3,3,3,3,3,3,3,
4),(-0.267175770913084,-0.202641536318522,-0.184830688168289,-0.122723770586227,
-0.0570251245949306,7.73147172802893E-5,0.0628601143819659,0.123897646499237,
0.184935178616508,0.242766080933253,0.26717572254583),.UNSPECIFIED.);
#7556=B_SPLINE_CURVE_WITH_KNOTS('',3,(#41016,#41017,#41018,#41019),
 .UNSPECIFIED.,.F.,.F.,(4,4),(0.267175770913084,0.314279348079497),
 .UNSPECIFIED.);
#7557=B_SPLINE_CURVE_WITH_KNOTS('',3,(#41021,#41022,#41023,#41024),
 .UNSPECIFIED.,.F.,.F.,(4,4),(0.314279364233837,0.330164730316111),
 .UNSPECIFIED.);
#7558=B_SPLINE_CURVE_WITH_KNOTS('',3,(#41026,#41027,#41028,#41029,#41030,
#41031,#41032,#41033,#41034,#41035,#41036,#41037,#41038,#41039,#41040),
 .UNSPECIFIED.,.F.,.F.,(4,1,1,1,1,1,1,1,1,1,2,4),(-0.292787369885449,-0.24676514268468,
-0.186369611422536,-0.125974080160392,-0.0655785488982472,-0.00518301763610282,
0.0552125136260416,0.115608044888186,0.17600357615033,0.236399107412475,
0.296794638674619,0.297794018458462),.UNSPECIFIED.);
#7559=B_SPLINE_CURVE_WITH_KNOTS('',3,(#41042,#41043,#41044,#41045,#41046,
#41047),.UNSPECIFIED.,.F.,.F.,(4,2,4),(0.292787369885449,0.307160673946825,
0.361386326815235),.UNSPECIFIED.);
#7560=B_SPLINE_CURVE_WITH_KNOTS('',3,(#41049,#41050,#41051,#41052,#41053),
 .UNSPECIFIED.,.F.,.F.,(4,1,4),(-0.297985235446007,0.0164065923085981,0.299498223131783),
 .UNSPECIFIED.);
#7561=B_SPLINE_CURVE_WITH_KNOTS('',3,(#41055,#41056,#41057,#41058),
 .UNSPECIFIED.,.F.,.F.,(4,4),(0.297985235446007,0.361048915455649),
 .UNSPECIFIED.);
#7562=B_SPLINE_CURVE_WITH_KNOTS('',3,(#41060,#41061,#41062,#41063,#41064,
#41065,#41066,#41067),.UNSPECIFIED.,.F.,.F.,(4,2,2,4),(-0.329193263838381,
-0.328202711224253,0.275040863381023,0.32931292451793),.UNSPECIFIED.);
#7563=B_SPLINE_CURVE_WITH_KNOTS('',3,(#41068,#41069,#41070,#41071),
 .UNSPECIFIED.,.F.,.F.,(4,4),(-0.330172300337303,-0.314285888542252),
 .UNSPECIFIED.);
#7564=B_SPLINE_CURVE_WITH_KNOTS('',3,(#41074,#41075,#41076,#41077,#41078,
#41079,#41080,#41081,#41082,#41083,#41084,#41085,#41086,#41087,#41088,#41089,
#41090,#41091,#41092,#41093,#41094,#41095,#41096,#41097,#41098,#41099,#41100,
#41101,#41102,#41103,#41104,#41105,#41106,#41107,#41108,#41109,#41110,#41111,
#41112,#41113,#41114,#41115,#41116,#41117,#41118,#41119,#41120,#41121,#41122,
#41123,#41124,#41125,#41126,#41127,#41128,#41129,#41130,#41131),
 .UNSPECIFIED.,.F.,.F.,(4,3,3,3,3,3,3,3,3,3,3,3,3,3,3,3,3,3,3,4),(0.922264651271228,
0.95196229570932,0.980227193678782,0.985427844641358,1.01109405489662,1.03772298675017,
1.06426603988274,1.07002883462318,1.08636335889452,1.11299901067983,1.14013007212248,
1.14501308601341,1.17206434693218,1.19916477205921,1.2038740932211,1.21783674573549,
1.2452436598711,1.27296352011674,1.27880009503193,1.29174070129165),
 .UNSPECIFIED.);
#7565=B_SPLINE_CURVE_WITH_KNOTS('',3,(#41133,#41134,#41135,#41136,#41137,
#41138,#41139,#41140,#41141,#41142,#41143),.UNSPECIFIED.,.F.,.F.,(4,1,1,
1,1,1,1,1,4),(0.076362086282034,0.245533853727799,0.330119737450682,0.414705621173564,
0.583877388619329,0.668463272342212,0.753049156065094,0.795342097926536,
0.922220923510859),.UNSPECIFIED.);
#7566=B_SPLINE_CURVE_WITH_KNOTS('',3,(#41144,#41145,#41146,#41147,#41148,
#41149,#41150,#41151,#41152,#41153,#41154,#41155,#41156),.UNSPECIFIED.,
 .F.,.F.,(4,3,3,3,4),(0.,0.0131413461079839,0.0403155240278326,0.046632901256244,
0.076362086282034),.UNSPECIFIED.);
#7567=B_SPLINE_CURVE_WITH_KNOTS('',3,(#41363,#41364,#41365,#41366,#41367),
 .UNSPECIFIED.,.F.,.F.,(4,1,4),(-1.,-0.571428571428571,0.),
 .UNSPECIFIED.);
#7568=B_SPLINE_CURVE_WITH_KNOTS('',3,(#41369,#41370,#41371,#41372,#41373,
#41374),.UNSPECIFIED.,.F.,.F.,(4,1,1,4),(0.,0.207003520287941,0.310505280431912,
0.414007040575882),.UNSPECIFIED.);
#7569=B_SPLINE_CURVE_WITH_KNOTS('',3,(#41376,#41377,#41378,#41379,#41380),
 .UNSPECIFIED.,.F.,.F.,(4,1,4),(0.41430190159583,0.800342864550781,1.18640341854514),
 .UNSPECIFIED.);
#7570=B_SPLINE_CURVE_WITH_KNOTS('',3,(#41382,#41383,#41384,#41385),
 .UNSPECIFIED.,.F.,.F.,(4,4),(1.18667868852568,1.79026296795331),
 .UNSPECIFIED.);
#7571=B_SPLINE_CURVE_WITH_KNOTS('',3,(#41387,#41388,#41389,#41390),
 .UNSPECIFIED.,.F.,.F.,(4,4),(1.79056374069951,2.37790470859936),
 .UNSPECIFIED.);
#7572=B_SPLINE_CURVE_WITH_KNOTS('',3,(#41392,#41393,#41394,#41395),
 .UNSPECIFIED.,.F.,.F.,(4,4),(2.37819810334092,3.06372105803577),
 .UNSPECIFIED.);
#7573=B_SPLINE_CURVE_WITH_KNOTS('',3,(#41397,#41398,#41399,#41400,#41401),
 .UNSPECIFIED.,.F.,.F.,(4,1,4),(3.06374723112025,4.26766323501505,5.47160541199434),
 .UNSPECIFIED.);
#7574=B_SPLINE_CURVE_WITH_KNOTS('',3,(#41403,#41404,#41405,#41406,#41407,
#41408,#41409,#41410,#41411,#41412,#41413,#41414,#41415,#41416,#41417,#41418,
#41419,#41420,#41421,#41422,#41423,#41424,#41425,#41426,#41427,#41428,#41429,
#41430,#41431,#41432,#41433,#41434,#41435,#41436,#41437,#41438,#41439,#41440,
#41441,#41442,#41443,#41444,#41445,#41446,#41447,#41448,#41449,#41450,#41451,
#41452,#41453,#41454),.UNSPECIFIED.,.F.,.F.,(4,3,3,3,3,3,3,3,3,3,3,3,3,
3,3,3,3,4),(5.47162410746305,5.47176153560927,5.52922135523733,5.57009016359045,
5.58683833384667,5.64822065753784,5.66347324806546,5.72523068157049,5.78644857689101,
5.83662615005217,5.83886338715682,5.90578533070501,5.97118984657676,5.99390868625701,
6.00292892981675,6.0644494923277,6.1289173026227,6.15867754990177),
 .UNSPECIFIED.);
#7575=B_SPLINE_CURVE_WITH_KNOTS('',3,(#41456,#41457,#41458,#41459,#41460,
#41461,#41462,#41463,#41464,#41465,#41466,#41467,#41468,#41469,#41470,#41471,
#41472,#41473,#41474,#41475,#41476,#41477,#41478,#41479,#41480,#41481,#41482,
#41483,#41484,#41485,#41486,#41487,#41488,#41489,#41490,#41491,#41492,#41493,
#41494,#41495,#41496,#41497,#41498,#41499,#41500,#41501,#41502,#41503,#41504,
#41505,#41506,#41507,#41508,#41509,#41510,#41511,#41512,#41513,#41514,#41515,
#41516),.UNSPECIFIED.,.F.,.F.,(4,3,3,3,3,3,3,3,3,3,3,3,3,3,3,3,3,3,3,3,
4),(6.15871642666174,6.15875530745073,6.17769523512538,6.19663516280003,
6.19981654499319,6.22890881990579,6.23445739445574,6.28406964878603,6.30977254860284,
6.36393898412319,6.4210906697559,6.45115001888933,6.4580679089126,6.52098880059716,
6.5825270089927,6.59738625338311,6.63690964823477,6.67050437063,6.70043365602453,
6.7287738754379,6.74301820316605),.UNSPECIFIED.);
#7576=B_SPLINE_CURVE_WITH_KNOTS('',3,(#41518,#41519,#41520,#41521,#41522,
#41523,#41524),.UNSPECIFIED.,.F.,.F.,(4,1,1,1,4),(6.74362248787689,6.88868570629297,
7.03374892470906,7.17881214312514,7.32387536154123),.UNSPECIFIED.);
#7577=B_SPLINE_CURVE_WITH_KNOTS('',3,(#41526,#41527,#41528,#41529,#41530,
#41531,#41532,#41533),.UNSPECIFIED.,.F.,.F.,(4,1,1,1,1,4),(7.32434227776303,
7.70189518745276,7.89090510040853,7.98541005688641,8.03266253512535,8.0799150133643),
 .UNSPECIFIED.);
#7578=B_SPLINE_CURVE_WITH_KNOTS('',3,(#41534,#41535,#41536,#41537,#41538,
#41539,#41540),.UNSPECIFIED.,.F.,.F.,(4,1,1,1,4),(8.08029222326494,8.44983649077903,
8.81975796819377,9.1896794456085,9.55960092302324),.UNSPECIFIED.);
#7579=B_SPLINE_CURVE_WITH_KNOTS('',3,(#52343,#52344,#52345,#52346,#52347,
#52348,#52349,#52350,#52351),.UNSPECIFIED.,.F.,.F.,(4,1,1,1,1,1,4),(0.,
0.208981284264062,0.626943852792187,0.835925137056249,1.04490642132031,
1.25388770558437,1.46286897295086),.UNSPECIFIED.);
#7580=B_SPLINE_CURVE_WITH_KNOTS('',3,(#52353,#52354,#52355,#52356,#52357,
#52358,#52359,#52360,#52361,#52362,#52363),.UNSPECIFIED.,.F.,.F.,(4,1,1,
1,1,1,1,1,4),(2.19155818661609,2.25090656855756,2.280580760587,2.31025495261644,
2.32509204863116,2.33992914464588,2.36960333667532,2.48830010479308,2.60699687291084),
 .UNSPECIFIED.);
#7581=B_SPLINE_CURVE_WITH_KNOTS('',3,(#52365,#52366,#52367,#52368,#52369,
#52370,#52371,#52372,#52373,#52374,#52375,#52376,#52377,#52378,#52379,#52380,
#52381,#52382,#52383,#52384,#52385,#52386,#52387,#52388,#52389,#52390,#52391,
#52392,#52393,#52394,#52395,#52396,#52397,#52398,#52399,#52400,#52401,#52402,
#52403,#52404,#52405,#52406,#52407,#52408,#52409,#52410,#52411,#52412,#52413,
#52414,#52415,#52416,#52417,#52418,#52419,#52420,#52421,#52422,#52423,#52424,
#52425,#52426,#52427,#52428,#52429,#52430,#52431,#52432,#52433,#52434,#52435,
#52436,#52437,#52438,#52439,#52440,#52441,#52442,#52443,#52444,#52445,#52446,
#52447,#52448,#52449),.UNSPECIFIED.,.F.,.F.,(4,3,3,3,3,3,3,3,3,3,3,3,3,
3,3,3,3,3,3,3,3,3,3,3,3,3,3,3,4),(2.10087562040851,2.10088372270372,2.10247346027013,
2.10307601393069,2.10530413110765,2.10956542752656,2.1098519820788,2.11383027239681,
2.1191966968775,2.12453719979532,2.12678492441379,2.12874159509156,2.13208059695754,
2.13544318756292,2.13854861386098,2.13973957643076,2.14058122681814,2.14566146932938,
2.1509697282011,2.15269422844774,2.15809938906919,2.16160847183393,2.16688124293776,
2.17213694886275,2.17745117941117,2.18283434334936,2.18837389162331,2.19070800154593,
2.1915581843749),.UNSPECIFIED.);
#7582=B_SPLINE_CURVE_WITH_KNOTS('',3,(#52451,#52452,#52453,#52454,#52455,
#52456,#52457,#52458,#52459,#52460,#52461,#52462,#52463,#52464,#52465,#52466,
#52467,#52468,#52469,#52470,#52471,#52472,#52473,#52474,#52475,#52476,#52477,
#52478,#52479,#52480,#52481,#52482,#52483,#52484,#52485,#52486,#52487,#52488,
#52489,#52490,#52491,#52492,#52493,#52494,#52495,#52496,#52497,#52498,#52499,
#52500,#52501,#52502,#52503,#52504,#52505,#52506,#52507,#52508,#52509,#52510,
#52511,#52512,#52513,#52514,#52515,#52516,#52517,#52518,#52519,#52520,#52521,
#52522,#52523,#52524,#52525,#52526,#52527,#52528,#52529),.UNSPECIFIED.,
 .F.,.F.,(4,3,3,3,3,3,3,3,3,3,3,3,3,3,3,3,3,3,3,3,3,3,3,3,3,3,4),(2.03661045158091,
2.04096442896004,2.04146916453237,2.04613737339918,2.05268993684172,2.05312613965519,
2.05483225415638,2.05497936272896,2.05614902505797,2.05989669434489,2.06181300865997,
2.06416787026005,2.06638674823242,2.06835564146826,2.06972997740258,2.07334448964751,
2.07503624001787,2.07828886994786,2.08055225390468,2.08251295441833,2.08611159999046,
2.09083174338144,2.09155081643771,2.09169749444627,2.09495872614039,2.10019830691549,
2.10087562037779),.UNSPECIFIED.);
#7583=B_SPLINE_CURVE_WITH_KNOTS('',3,(#52531,#52532,#52533,#52534,#52535,
#52536,#52537,#52538),.UNSPECIFIED.,.F.,.F.,(4,1,1,1,1,4),(1.96650114296421,
1.97401285460172,1.97651675848088,1.98653237399755,2.00656360503089,2.03661045158091),
 .UNSPECIFIED.);
#7584=B_SPLINE_CURVE_WITH_KNOTS('',3,(#52540,#52541,#52542,#52543),
 .UNSPECIFIED.,.F.,.F.,(4,4),(1.9008556588209,1.96650114296421),
 .UNSPECIFIED.);
#7585=B_SPLINE_CURVE_WITH_KNOTS('',3,(#52545,#52546,#52547,#52548,#52549,
#52550,#52551,#52552,#52553,#52554,#52555,#52556,#52557,#52558,#52559,#52560,
#52561,#52562,#52563,#52564,#52565,#52566,#52567,#52568,#52569,#52570,#52571,
#52572,#52573,#52574,#52575,#52576,#52577,#52578,#52579,#52580,#52581,#52582,
#52583,#52584,#52585,#52586,#52587,#52588,#52589,#52590,#52591,#52592,#52593,
#52594,#52595,#52596,#52597,#52598,#52599,#52600,#52601,#52602,#52603,#52604,
#52605,#52606,#52607,#52608),.UNSPECIFIED.,.F.,.F.,(4,3,3,3,3,3,3,3,3,3,
3,3,3,3,3,3,3,3,3,3,3,4),(1.82758374932864,1.83223656565234,1.83571939203226,
1.83805116497033,1.84328487279121,1.84723441497955,1.84752017146434,1.85145117989987,
1.85343502410761,1.85550702434553,1.85898599625385,1.85962279895688,1.86512727908069,
1.8703298765575,1.87389394219687,1.878955199903,1.87992082753738,1.8853048835742,
1.89038824317914,1.89383938180255,1.89888316294158,1.90085565882082),
 .UNSPECIFIED.);
#7586=B_SPLINE_CURVE_WITH_KNOTS('',3,(#52610,#52611,#52612,#52613,#52614,
#52615,#52616,#52617),.UNSPECIFIED.,.F.,.F.,(4,2,2,4),(0.,0.115811547018689,
0.233145512161403,0.495737219621106),.UNSPECIFIED.);
#7587=B_SPLINE_CURVE_WITH_KNOTS('',3,(#52619,#52620,#52621,#52622,#52623,
#52624,#52625,#52626,#52627,#52628,#52629,#52630,#52631,#52632,#52633,#52634,
#52635,#52636,#52637,#52638,#52639,#52640,#52641,#52642,#52643,#52644,#52645,
#52646,#52647,#52648,#52649,#52650,#52651,#52652,#52653,#52654,#52655,#52656,
#52657,#52658,#52659,#52660,#52661,#52662,#52663,#52664,#52665,#52666,#52667,
#52668,#52669,#52670,#52671,#52672,#52673,#52674,#52675,#52676,#52677,#52678,
#52679,#52680,#52681,#52682,#52683,#52684,#52685,#52686,#52687,#52688,#52689,
#52690,#52691,#52692,#52693,#52694,#52695,#52696,#52697,#52698,#52699,#52700,
#52701,#52702,#52703),.UNSPECIFIED.,.F.,.F.,(4,3,3,3,3,3,3,3,3,3,3,3,3,
3,3,3,3,3,3,3,3,3,3,3,3,3,3,3,4),(1.56845677768168,1.57875898200853,1.5902875236116,
1.60181606521468,1.6232153440662,1.64400711162625,1.65649115942018,1.66853464029784,
1.67051171542687,1.69446829604668,1.70189392783942,1.71857357161021,1.73390383611253,
1.735253215381,1.7372376198041,1.7435930372664,1.74883573095845,1.75193285915179,
1.7525462632204,1.75878493231427,1.76473025775148,1.76861250292259,1.774746297528,
1.78151033410548,1.78529214669338,1.79301009099815,1.79922230536369,1.8019717371715,
1.80197179046417),.UNSPECIFIED.);
#7588=B_SPLINE_CURVE_WITH_KNOTS('',3,(#52705,#52706,#52707,#52708,#52709,
#52710,#52711),.UNSPECIFIED.,.F.,.F.,(4,1,1,1,4),(1.43249195629979,1.45191550221026,
1.4616272751655,1.4907625940312,1.56845677767309),.UNSPECIFIED.);
#7589=B_SPLINE_CURVE_WITH_KNOTS('',3,(#52713,#52714,#52715,#52716,#52717,
#52718,#52719,#52720,#52721,#52722,#52723,#52724,#52725,#52726,#52727,#52728,
#52729,#52730,#52731,#52732,#52733,#52734,#52735,#52736,#52737,#52738,#52739,
#52740,#52741,#52742,#52743,#52744,#52745,#52746,#52747,#52748,#52749,#52750,
#52751,#52752,#52753,#52754,#52755,#52756,#52757,#52758,#52759,#52760,#52761,
#52762,#52763,#52764,#52765,#52766,#52767,#52768,#52769,#52770,#52771,#52772,
#52773,#52774,#52775,#52776,#52777,#52778,#52779,#52780,#52781,#52782),
 .UNSPECIFIED.,.F.,.F.,(4,3,3,3,3,3,3,3,3,3,3,3,3,3,3,3,3,3,3,3,3,3,3,4),
(1.26182357380732,1.26321146371325,1.27965145505579,1.28695964770261,1.30171395524456,
1.30640755132645,1.31070783169197,1.32482659735197,1.32772758608418,1.33496166264828,
1.34362369478369,1.34924187664357,1.35187874054377,1.35931072547827,1.36767009102177,
1.36865825613663,1.38372247757944,1.38551167246194,1.39144562654905,1.39591154434102,
1.40850579340837,1.41185992891419,1.41833945977598,1.43249195629979),
 .UNSPECIFIED.);
#7590=B_SPLINE_CURVE_WITH_KNOTS('',3,(#52784,#52785,#52786,#52787,#52788,
#52789,#52790,#52791,#52792,#52793,#52794,#52795,#52796,#52797,#52798,#52799,
#52800,#52801,#52802,#52803,#52804,#52805,#52806,#52807,#52808,#52809,#52810,
#52811,#52812,#52813,#52814,#52815,#52816,#52817,#52818,#52819,#52820,#52821,
#52822,#52823,#52824,#52825,#52826,#52827,#52828,#52829,#52830,#52831,#52832,
#52833,#52834,#52835,#52836,#52837,#52838,#52839,#52840,#52841,#52842,#52843,
#52844,#52845,#52846,#52847,#52848,#52849,#52850,#52851,#52852,#52853,#52854,
#52855,#52856,#52857,#52858,#52859,#52860,#52861,#52862,#52863,#52864,#52865,
#52866,#52867,#52868,#52869,#52870,#52871,#52872,#52873,#52874,#52875,#52876,
#52877,#52878,#52879,#52880,#52881,#52882,#52883,#52884,#52885,#52886,#52887,
#52888,#52889,#52890,#52891,#52892,#52893,#52894,#52895,#52896,#52897,#52898,
#52899,#52900,#52901,#52902,#52903,#52904,#52905,#52906,#52907),
 .UNSPECIFIED.,.F.,.F.,(4,3,3,3,3,3,3,3,3,3,3,3,3,3,3,3,3,3,3,3,3,3,3,3,
3,3,3,3,3,3,3,3,3,3,3,3,3,3,3,3,3,4),(0.756828437332379,0.758034303676285,
0.783022641448518,0.80599662056723,0.828970599685942,0.847245434940196,
0.865650791288596,0.884491811769908,0.887471652364765,0.901112762039505,
0.914245954975312,0.919148302627896,0.935599586414352,0.937183843216286,
0.958717360320901,0.973254924393068,0.995700399707761,1.00932600556985,
1.02736154615824,1.03637931645244,1.04539708674663,1.06072425960333,1.07628417862955,
1.09205523917646,1.10854629296799,1.11753924910019,1.12498697740592,1.13697906116791,
1.15138005679454,1.16628135084883,1.18230149406609,1.18968141145376,1.20308754755323,
1.20616298993056,1.2203814875239,1.22575249263054,1.23458163997862,1.24312622221273,
1.24848732199679,1.25626046603962,1.26177001350472,1.26182357380732),
 .UNSPECIFIED.);
#7591=B_SPLINE_CURVE_WITH_KNOTS('',3,(#52909,#52910,#52911,#52912,#52913,
#52914,#52915,#52916,#52917,#52918,#52919,#52920,#52921,#52922,#52923,#52924,
#52925,#52926,#52927,#52928,#52929,#52930,#52931,#52932,#52933,#52934,#52935,
#52936,#52937,#52938,#52939,#52940,#52941,#52942,#52943,#52944,#52945,#52946,
#52947,#52948,#52949,#52950,#52951,#52952,#52953,#52954,#52955,#52956,#52957,
#52958,#52959,#52960,#52961,#52962,#52963,#52964,#52965,#52966,#52967,#52968,
#52969,#52970,#52971,#52972,#52973,#52974,#52975,#52976,#52977,#52978,#52979,
#52980,#52981,#52982,#52983,#52984,#52985,#52986,#52987,#52988,#52989,#52990),
 .UNSPECIFIED.,.F.,.F.,(4,3,3,3,3,3,3,3,3,3,3,3,3,3,3,3,3,3,3,3,3,3,3,3,
3,3,3,4),(0.,0.039559842189632,0.0812965112238326,0.126691965812033,0.168113098584215,
0.21623669638068,0.255008832123529,0.297122618085817,0.324355044571019,
0.340152984197433,0.385149402756223,0.417620481855091,0.432473392761359,
0.483357467834262,0.537497172053552,0.540591740951699,0.571362633267615,
0.597869133211754,0.626131984061165,0.648710089142039,0.661547104722673,
0.678554902855057,0.689471163857318,0.702769263237209,0.720830101771721,
0.738829266170943,0.75573965977665,0.756828430570164),.UNSPECIFIED.);
#7592=B_SPLINE_CURVE_WITH_KNOTS('',3,(#52992,#52993,#52994,#52995,#52996,
#52997),.UNSPECIFIED.,.F.,.F.,(4,2,4),(1.03501879872334E-10,0.211555879027688,
0.425996794857508),.UNSPECIFIED.);
#7593=B_SPLINE_CURVE_WITH_KNOTS('',3,(#52999,#53000,#53001,#53002,#53003,
#53004,#53005,#53006,#53007),.UNSPECIFIED.,.F.,.F.,(4,1,1,1,1,1,4),(-1.10870576037865,
-1.01091721837057,-0.913128676362484,-0.815340134354398,-0.766445863350356,
-0.619763050338228,-0.424185972875504),.UNSPECIFIED.);
#7594=B_SPLINE_CURVE_WITH_KNOTS('',3,(#53009,#53010,#53011,#53012,#53013,
#53014,#53015,#53016,#53017,#53018),.UNSPECIFIED.,.F.,.F.,(4,1,1,1,1,1,
1,4),(-2.04907351897734,-1.91473526774895,-1.64605876529219,-1.5117205140638,
-1.37738226283542,-1.24304401160704,-1.17587488599285,-1.10870576037865),
 .UNSPECIFIED.);
#7595=B_SPLINE_CURVE_WITH_KNOTS('',3,(#53020,#53021,#53022,#53023,#53024,
#53025,#53026,#53027,#53028,#53029,#53030),.UNSPECIFIED.,.F.,.F.,(4,1,1,
1,1,1,1,1,4),(-3.79500099688023,-3.54558322444133,-3.04674665595333,-2.92203751383133,
-2.79732837170933,-2.67261922958733,-2.54791008746534,-2.29849180322134,
-2.04907351897734),.UNSPECIFIED.);
#7596=B_SPLINE_CURVE_WITH_KNOTS('',3,(#53032,#53033,#53034,#53035,#53036,
#53037,#53038,#53039,#53040,#53041,#53042,#53043,#53044,#53045,#53046,#53047,
#53048,#53049,#53050,#53051,#53052,#53053,#53054,#53055,#53056,#53057,#53058,
#53059,#53060,#53061,#53062,#53063,#53064,#53065,#53066,#53067,#53068,#53069,
#53070,#53071,#53072,#53073,#53074,#53075,#53076,#53077,#53078,#53079,#53080,
#53081,#53082,#53083,#53084,#53085,#53086,#53087,#53088,#53089,#53090,#53091,
#53092,#53093,#53094,#53095,#53096,#53097,#53098,#53099,#53100,#53101,#53102,
#53103,#53104,#53105,#53106,#53107,#53108,#53109,#53110,#53111,#53112,#53113,
#53114,#53115,#53116,#53117,#53118,#53119,#53120,#53121,#53122,#53123,#53124,
#53125),.UNSPECIFIED.,.F.,.F.,(4,3,3,3,3,3,3,3,3,3,3,3,3,3,3,3,3,3,3,3,
3,3,3,3,3,3,3,3,3,3,3,4),(-7.37893243484629,-7.09721253804601,-6.86694230253758,
-6.54165526017816,-6.25323500527255,-6.10927151562258,-5.88100661174727,
-5.84296203792017,-5.64313657722973,-5.45391307940915,-5.27371499028469,
-5.10400017747741,-5.04555890996164,-4.89298656830114,-4.81898177330275,
-4.64872543377383,-4.56298670714839,-4.50669086603314,-4.46698855734051,
-4.38699009916728,-4.30699164099404,-4.2439746894317,-4.17377747724209,
-4.1052835011459,-4.05099657483969,-4.00647424691738,-3.94815423137164,
-3.9004735048502,-3.87188483858507,-3.84491918341313,-3.81938938067703,
-3.79500153778596),.UNSPECIFIED.);
#7597=B_SPLINE_CURVE_WITH_KNOTS('',3,(#53127,#53128,#53129,#53130,#53131,
#53132,#53133,#53134,#53135,#53136,#53137,#53138,#53139,#53140,#53141,#53142,
#53143,#53144,#53145,#53146,#53147,#53148,#53149,#53150,#53151,#53152,#53153,
#53154,#53155,#53156,#53157,#53158,#53159,#53160,#53161,#53162,#53163,#53164,
#53165,#53166,#53167,#53168,#53169,#53170,#53171,#53172,#53173,#53174,#53175,
#53176,#53177,#53178,#53179,#53180,#53181,#53182,#53183,#53184,#53185,#53186,
#53187,#53188,#53189,#53190),.UNSPECIFIED.,.F.,.F.,(4,3,3,3,3,3,3,3,3,3,
3,3,3,3,3,3,3,3,3,3,3,4),(-13.6209854494249,-12.8511378970195,-12.0643898935444,
-11.3085768590722,-10.9458199140635,-10.4479935674583,-10.0540980442592,
-9.67335324653639,-9.31475312865825,-9.16237617445491,-8.77668431314733,
-8.42708589080824,-8.2706543046506,-8.04416328397843,-7.81656010161982,
-7.70334373657069,-7.58867356571361,-7.5400351581434,-7.47104988566852,
-7.40480342889605,-7.38202025346192,-7.37893251061186),.UNSPECIFIED.);
#7598=B_SPLINE_CURVE_WITH_KNOTS('',3,(#53192,#53193,#53194,#53195,#53196,
#53197,#53198,#53199),.UNSPECIFIED.,.F.,.F.,(4,1,1,1,1,4),(-20.9230961620266,
-17.7936201740765,-15.7073028487765,-14.6641441861265,-14.1425648548015,
-13.6209855234765),.UNSPECIFIED.);
#7599=B_SPLINE_CURVE_WITH_KNOTS('',3,(#53201,#53202,#53203,#53204,#53205,
#53206,#53207,#53208,#53209,#53210,#53211,#53212,#53213,#53214,#53215,#53216,
#53217,#53218,#53219,#53220,#53221,#53222,#53223,#53224,#53225,#53226,#53227,
#53228,#53229,#53230,#53231,#53232,#53233,#53234,#53235,#53236,#53237,#53238,
#53239,#53240,#53241,#53242,#53243,#53244,#53245,#53246,#53247,#53248,#53249,
#53250,#53251,#53252,#53253,#53254,#53255,#53256,#53257,#53258,#53259,#53260,
#53261,#53262,#53263,#53264,#53265,#53266,#53267,#53268,#53269,#53270,#53271,
#53272,#53273,#53274,#53275,#53276,#53277,#53278,#53279,#53280,#53281,#53282,
#53283,#53284,#53285,#53286,#53287,#53288,#53289,#53290,#53291,#53292,#53293,
#53294,#53295,#53296,#53297),.UNSPECIFIED.,.F.,.F.,(4,3,3,3,3,3,3,3,3,3,
3,3,3,3,3,3,3,3,3,3,3,3,3,3,3,3,3,3,3,3,3,3,4),(-29.2787346184417,-29.1096960603127,
-28.9240346326721,-28.7261490220601,-28.6427305271377,-28.6263089729943,
-28.4309678069006,-28.3150441010112,-28.2510346319925,-28.0852673066811,
-27.7865835801735,-27.7048845006206,-27.1030463193419,-26.3994219069812,
-26.2152821750297,-26.0888102114573,-25.6957974946206,-25.5456719507069,
-25.467698483279,-25.227004099114,-25.196215795191,-25.1722521850178,-24.8236888062035,
-24.5049209466192,-23.9082511095742,-23.4566708142076,-23.3115812725292,
-22.884956861632,-22.600429531231,-22.1810961889299,-22.0014436072201,-21.4779708271961,
-20.9230961620266),.UNSPECIFIED.);
#7600=B_SPLINE_CURVE_WITH_KNOTS('',3,(#53299,#53300,#53301,#53302,#53303,
#53304,#53305),.UNSPECIFIED.,.F.,.F.,(4,1,1,1,4),(-35.1303480341168,-33.4584584867811,
-31.7865689394453,-30.9506241657775,-29.2787346184417),.UNSPECIFIED.);
#7601=B_SPLINE_CURVE_WITH_KNOTS('',3,(#53307,#53308,#53309,#53310,#53311,
#53312,#53313,#53314,#53315,#53316,#53317,#53318,#53319,#53320,#53321,#53322,
#53323,#53324,#53325,#53326,#53327,#53328,#53329,#53330,#53331,#53332,#53333,
#53334,#53335,#53336,#53337,#53338,#53339,#53340,#53341,#53342,#53343,#53344,
#53345,#53346,#53347,#53348,#53349,#53350,#53351,#53352,#53353,#53354,#53355,
#53356,#53357,#53358,#53359,#53360,#53361,#53362,#53363,#53364,#53365,#53366,
#53367,#53368,#53369,#53370,#53371,#53372,#53373,#53374,#53375,#53376,#53377,
#53378,#53379,#53380,#53381,#53382,#53383,#53384,#53385,#53386,#53387,#53388,
#53389,#53390,#53391,#53392,#53393,#53394,#53395,#53396,#53397,#53398,#53399,
#53400,#53401,#53402,#53403,#53404,#53405,#53406,#53407,#53408,#53409,#53410,
#53411,#53412,#53413,#53414,#53415,#53416,#53417,#53418,#53419,#53420,#53421,
#53422,#53423,#53424,#53425,#53426,#53427,#53428,#53429,#53430,#53431,#53432,
#53433,#53434,#53435,#53436,#53437,#53438,#53439),.UNSPECIFIED.,.F.,.F.,
(4,3,3,3,3,3,3,3,3,3,3,3,3,3,3,3,3,3,3,3,3,3,3,3,3,3,3,3,3,3,3,3,3,3,3,
3,3,3,3,3,3,3,3,3,4),(-40.4542025593683,-40.2883379357545,-40.1291560510175,
-40.0863253858464,-39.7317546341407,-39.3799231675408,-39.1055719541562,
-38.9809430220555,-38.932487814856,-38.7733967870736,-38.6017505770459,
-38.38709626168,-38.3278541581916,-38.2684208184249,-38.172441946314,-38.0773070542021,
-38.015978412303,-37.8649593582531,-37.8489781650965,-37.8363222855412,
-37.6893279450614,-37.5506150705823,-37.5098081397409,-37.4119021961033,
-37.308503196221,-37.2599229565623,-37.0129942138183,-36.9983061965739,
-36.8094454257336,-36.7412333947959,-36.6544112504103,-36.5012970422284,
-36.3546539033726,-36.1589984452356,-36.1281858125416,-35.929935933668,
-35.8935455269148,-35.8445105517863,-35.7695403285612,-35.5371810458801,
-35.4574426980158,-35.314925666407,-35.27725046187,-35.1434968058668,-35.1303480341168),
 .UNSPECIFIED.);
#7602=B_SPLINE_CURVE_WITH_KNOTS('',3,(#53441,#53442,#53443,#53444,#53445,
#53446,#53447,#53448,#53449,#53450,#53451,#53452,#53453,#53454,#53455,#53456,
#53457,#53458,#53459,#53460,#53461,#53462,#53463,#53464,#53465,#53466,#53467,
#53468,#53469,#53470,#53471,#53472,#53473,#53474,#53475,#53476,#53477,#53478,
#53479,#53480,#53481,#53482,#53483,#53484,#53485,#53486,#53487,#53488,#53489,
#53490,#53491,#53492,#53493,#53494,#53495,#53496,#53497,#53498,#53499,#53500,
#53501,#53502,#53503,#53504,#53505,#53506,#53507,#53508,#53509,#53510,#53511,
#53512,#53513,#53514,#53515,#53516,#53517,#53518,#53519,#53520,#53521,#53522,
#53523,#53524,#53525,#53526,#53527,#53528,#53529,#53530,#53531,#53532,#53533,
#53534,#53535,#53536,#53537),.UNSPECIFIED.,.F.,.F.,(4,3,3,3,3,3,3,3,3,3,
3,3,3,3,3,3,3,3,3,3,3,3,3,3,3,3,3,3,3,3,3,3,4),(-52.076264422194,-52.0737402609872,
-51.1412180731238,-50.9105567633614,-50.6813407101697,-50.2280521562142,
-49.3467857029178,-49.298229902108,-48.9208946312172,-48.5057751083927,
-47.6156904523358,-47.0953817384218,-46.9581990673406,-46.257134327466,
-45.5668109774429,-44.8893364381591,-44.1815864308004,-43.7747932825737,
-42.9979057491396,-42.1621977116501,-42.1144990546496,-41.7255776485795,
-41.2843519406876,-41.0649893227899,-40.9009393220907,-40.7763014969501,
-40.7368893213915,-40.6649750650259,-40.5977989171732,-40.5344428881694,
-40.4755069476578,-40.4591070372058,-40.4542057498323),.UNSPECIFIED.);
#7603=B_SPLINE_CURVE_WITH_KNOTS('',3,(#53539,#53540,#53541,#53542,#53543),
 .UNSPECIFIED.,.F.,.F.,(4,1,4),(-66.1031756239825,-60.0916422517874,-52.076264422194),
 .UNSPECIFIED.);
#7604=B_SPLINE_CURVE_WITH_KNOTS('',3,(#53545,#53546,#53547,#53548),
 .UNSPECIFIED.,.F.,.F.,(4,4),(-75.2949305236969,-66.1031756239825),
 .UNSPECIFIED.);
#7605=B_SPLINE_CURVE_WITH_KNOTS('',3,(#53550,#53551,#53552,#53553,#53554,
#53555),.UNSPECIFIED.,.F.,.F.,(4,2,4),(0.,0.0420132838931537,0.0846653479954924),
 .UNSPECIFIED.);
#7606=B_SPLINE_CURVE_WITH_KNOTS('',3,(#53557,#53558,#53559,#53560,#53561,
#53562,#53563,#53564,#53565,#53566,#53567,#53568,#53569,#53570,#53571,#53572,
#53573,#53574),.UNSPECIFIED.,.F.,.F.,(4,1,1,1,1,1,1,1,1,1,1,1,1,1,1,4),
(0.,0.0536833715747986,0.107366743149597,0.161050114724396,0.214733486299194,
0.228154329192894,0.241575172086594,0.268416857873993,0.322100229448792,
0.37578360102359,0.429466972598389,0.509992029960587,0.590517087322785,
0.644200458897583,0.697883830472382,0.75156720204718),.UNSPECIFIED.);
#7607=B_SPLINE_CURVE_WITH_KNOTS('',3,(#53576,#53577,#53578,#53579,#53580,
#53581),.UNSPECIFIED.,.F.,.F.,(4,2,4),(0.,0.021085550105349,0.0417920803786918),
 .UNSPECIFIED.);
#7608=B_SPLINE_CURVE_WITH_KNOTS('',3,(#53583,#53584,#53585,#53586,#53587,
#53588,#53589,#53590,#53591,#53592,#53593,#53594),.UNSPECIFIED.,.F.,.F.,
(4,2,2,2,2,4),(0.,0.050505315546523,0.100790126577494,0.199632092084437,
0.400786097856356,0.745503643800359),.UNSPECIFIED.);
#7609=B_SPLINE_CURVE_WITH_KNOTS('',3,(#53596,#53597,#53598,#53599,#53600,
#53601,#53602,#53603,#53604,#53605,#53606,#53607,#53608,#53609,#53610,#53611,
#53612,#53613,#53614,#53615,#53616,#53617,#53618,#53619,#53620,#53621,#53622,
#53623,#53624,#53625,#53626,#53627,#53628,#53629,#53630,#53631,#53632,#53633,
#53634,#53635,#53636,#53637,#53638,#53639,#53640,#53641,#53642,#53643,#53644),
 .UNSPECIFIED.,.F.,.F.,(4,3,3,3,3,3,3,3,3,3,3,3,3,3,3,3,4),(6.63337020876143,
6.7190850448111,6.73676856887547,6.77580516745678,6.89645053985051,6.91763430915923,
7.16564608140866,7.19816645514471,7.4501548123097,7.55120883330657,7.59415354968106,
7.72134807390837,7.95982866477617,8.31850358376712,8.58822017944783,8.63541402258988,
8.77692550510397),.UNSPECIFIED.);
#7610=B_SPLINE_CURVE_WITH_KNOTS('',3,(#53646,#53647,#53648,#53649,#53650),
 .UNSPECIFIED.,.F.,.F.,(4,1,4),(4.69946777607289,5.80455488046634,6.63337020876143),
 .UNSPECIFIED.);
#7611=B_SPLINE_CURVE_WITH_KNOTS('',3,(#53652,#53653,#53654,#53655,#53656,
#53657,#53658,#53659,#53660,#53661,#53662,#53663,#53664,#53665,#53666,#53667,
#53668,#53669),.UNSPECIFIED.,.F.,.F.,(4,2,2,2,2,2,2,2,4),(5.5366310029957E-11,
0.170051968698641,0.346390851185846,0.408566423903585,0.45559735651897,
0.526633190057164,0.562379031383655,0.580309052858196,0.602548551079055),
 .UNSPECIFIED.);
#7612=B_SPLINE_CURVE_WITH_KNOTS('',3,(#53671,#53672,#53673,#53674,#53675,
#53676,#53677,#53678,#53679,#53680,#53681,#53682,#53683,#53684,#53685,#53686,
#53687,#53688,#53689,#53690,#53691,#53692,#53693,#53694,#53695,#53696,#53697,
#53698,#53699,#53700,#53701,#53702,#53703,#53704,#53705,#53706,#53707,#53708,
#53709,#53710,#53711,#53712,#53713,#53714,#53715,#53716,#53717,#53718,#53719,
#53720,#53721,#53722,#53723,#53724,#53725,#53726,#53727,#53728,#53729,#53730,
#53731,#53732,#53733,#53734,#53735,#53736,#53737,#53738,#53739,#53740,#53741,
#53742,#53743,#53744,#53745,#53746,#53747,#53748,#53749,#53750,#53751,#53752,
#53753,#53754,#53755,#53756,#53757,#53758,#53759,#53760,#53761,#53762,#53763,
#53764,#53765,#53766,#53767),.UNSPECIFIED.,.F.,.F.,(4,3,3,3,3,3,3,3,3,3,
3,3,3,3,3,3,3,3,3,3,3,3,3,3,3,3,3,3,3,3,3,3,4),(1.96419536172906,1.96505190012007,
2.00759893446084,2.05907348647213,2.14856512578498,2.16116833461418,2.1995405412518,
2.29009841588943,2.31368035746746,2.34538948007777,2.43488572077454,2.56742771999767,
2.67023090029728,2.67502081956359,2.75992963007049,2.83275285494525,2.90048454253916,
2.90557607982002,2.9770366712957,3.04749917809138,3.10307095323777,3.12007497461443,
3.14092125934276,3.20896093626124,3.27403989704861,3.33678902877863,3.3762664388655,
3.37737317695638,3.45628612936796,3.53381374195537,3.60353111799624,3.61134135454277,
3.61161161790059),.UNSPECIFIED.);
#7613=B_SPLINE_CURVE_WITH_KNOTS('',3,(#53769,#53770,#53771,#53772,#53773,
#53774,#53775,#53776,#53777,#53778,#53779,#53780,#53781,#53782,#53783,#53784,
#53785,#53786,#53787,#53788,#53789,#53790,#53791,#53792,#53793,#53794,#53795,
#53796,#53797,#53798,#53799,#53800,#53801,#53802,#53803,#53804,#53805,#53806,
#53807,#53808,#53809,#53810,#53811,#53812,#53813,#53814,#53815,#53816,#53817,
#53818,#53819,#53820,#53821,#53822,#53823,#53824,#53825,#53826,#53827,#53828,
#53829,#53830,#53831,#53832,#53833,#53834,#53835,#53836,#53837,#53838,#53839,
#53840,#53841,#53842,#53843,#53844,#53845,#53846,#53847,#53848,#53849,#53850,
#53851,#53852,#53853,#53854,#53855,#53856,#53857,#53858,#53859,#53860,#53861,
#53862,#53863,#53864,#53865),.UNSPECIFIED.,.F.,.F.,(4,3,3,3,3,3,3,3,3,3,
3,3,3,3,3,3,3,3,3,3,3,3,3,3,3,3,3,3,3,3,3,3,4),(0.,1.8138297394372E-5,0.121063268185862,
0.17473067075732,0.307769204317186,0.337354379440942,0.449276527110338,
0.552000632372627,0.561198674779733,0.602830722877044,0.699305190558911,
0.701498343474666,0.823662523240613,0.841798012169599,0.955815263928068,
0.982097680864532,1.06417937027259,1.11100143720994,1.12239734955947,1.22569592643638,
1.32149205669811,1.32899450331328,1.40299668694933,1.42878061011154,1.50546259251116,
1.55154822774982,1.62807430325076,1.6835960243392,1.77144305862835,1.79740964584924,
1.87394598522444,1.9554396253416,1.96419535735387),.UNSPECIFIED.);
#7614=B_SPLINE_CURVE_WITH_KNOTS('',3,(#53867,#53868,#53869,#53870,#53871,
#53872,#53873,#53874,#53875,#53876,#53877,#53878,#53879),.UNSPECIFIED.,
 .F.,.F.,(4,1,1,1,1,1,1,1,1,1,4),(6.5071186511175,6.712779658626,6.91844066613449,
6.96985591801162,7.02127116988874,7.22693217739724,7.32976268115149,7.48400843678286,
7.53542368865998,7.74108469616848,7.94674570367697),.UNSPECIFIED.);
#7615=B_SPLINE_CURVE_WITH_KNOTS('',3,(#53881,#53882,#53883,#53884,#53885,
#53886,#53887,#53888,#53889),.UNSPECIFIED.,.F.,.F.,(4,1,1,1,1,1,4),(4.87949997638846,
5.11201692992118,5.57705083698662,5.80956779051934,6.04208474405206,6.27460169758478,
6.5071186511175),.UNSPECIFIED.);
#7616=B_SPLINE_CURVE_WITH_KNOTS('',3,(#53891,#53892,#53893,#53894,#53895,
#53896,#53897),.UNSPECIFIED.,.F.,.F.,(4,1,1,1,4),(2.69094642325915,3.62889794602885,
4.25419896120866,4.56684946879856,4.87949997638846),.UNSPECIFIED.);
#7617=B_SPLINE_CURVE_WITH_KNOTS('',3,(#53899,#53900,#53901,#53902,#53903,
#53904,#53905,#53906,#53907,#53908,#53909,#53910,#53911,#53912,#53913,#53914,
#53915,#53916,#53917,#53918,#53919,#53920,#53921,#53922,#53923,#53924,#53925,
#53926,#53927,#53928,#53929,#53930,#53931,#53932,#53933,#53934,#53935,#53936,
#53937,#53938,#53939,#53940,#53941,#53942,#53943,#53944,#53945,#53946,#53947,
#53948,#53949,#53950,#53951,#53952,#53953,#53954,#53955,#53956,#53957,#53958,
#53959,#53960,#53961,#53962,#53963,#53964,#53965,#53966,#53967,#53968,#53969,
#53970,#53971,#53972,#53973,#53974,#53975,#53976,#53977,#53978,#53979,#53980,
#53981,#53982,#53983,#53984,#53985,#53986,#53987,#53988,#53989,#53990,#53991,
#53992,#53993,#53994,#53995,#53996,#53997,#53998),.UNSPECIFIED.,.F.,.F.,
(4,3,3,3,3,3,3,3,3,3,3,3,3,3,3,3,3,3,3,3,3,3,3,3,3,3,3,3,3,3,3,3,3,4),(1.28454933342625,
1.284663099846,1.32335780443299,1.33323468515429,1.34320009665895,1.36341289207583,
1.40509748435979,1.42665711008932,1.44876554198746,1.4998586819635,1.54419214844141,
1.59590059132183,1.64959023195339,1.65716554088604,1.68637707337851,1.75981977009417,
1.84800901712936,1.88729094335464,1.92692609574672,1.93751941084867,1.9877478783427,
2.07341022478126,2.08212877066919,2.08820481333076,2.24310543462275,2.28911868330689,
2.38245055444688,2.50274947638037,2.53443926298747,2.59672405888692,2.61222200346954,
2.65158421336434,2.68765429596537,2.69094642325915),.UNSPECIFIED.);
#7618=B_SPLINE_CURVE_WITH_KNOTS('',3,(#54000,#54001,#54002,#54003,#54004,
#54005,#54006),.UNSPECIFIED.,.F.,.F.,(4,1,1,1,4),(0.675577463735769,0.762573445120124,
0.936565407888833,1.11055737065754,1.28454933342625),.UNSPECIFIED.);
#7619=B_SPLINE_CURVE_WITH_KNOTS('',3,(#54008,#54009,#54010,#54011,#54012,
#54013,#54014,#54015,#54016,#54017,#54018,#54019,#54020,#54021,#54022,#54023,
#54024,#54025,#54026,#54027,#54028,#54029,#54030,#54031,#54032,#54033,#54034,
#54035,#54036,#54037,#54038,#54039,#54040,#54041,#54042,#54043,#54044,#54045,
#54046,#54047,#54048,#54049,#54050,#54051,#54052,#54053,#54054,#54055,#54056,
#54057,#54058,#54059,#54060,#54061,#54062),.UNSPECIFIED.,.F.,.F.,(4,3,3,
3,3,3,3,3,3,3,3,3,3,3,3,3,3,3,4),(0.0412699530928034,0.0821005929720136,
0.127945523936301,0.168857136488049,0.20941548589726,0.22294409466857,0.269878070913077,
0.316812047157585,0.355434901557536,0.364399147418465,0.383769517079644,
0.404141522876379,0.451848303292714,0.459901618097689,0.522642871293701,
0.532913366941116,0.604380509650793,0.639978986693281,0.675577463735768),
 .UNSPECIFIED.);
#7620=B_SPLINE_CURVE_WITH_KNOTS('',3,(#54064,#54065,#54066,#54067),
 .UNSPECIFIED.,.F.,.F.,(4,4),(0.,0.0412699530886637),.UNSPECIFIED.);
#7621=B_SPLINE_CURVE_WITH_KNOTS('',3,(#54069,#54070,#54071,#54072,#54073,
#54074,#54075,#54076,#54077,#54078,#54079,#54080,#54081,#54082,#54083,#54084,
#54085,#54086,#54087,#54088,#54089,#54090,#54091,#54092,#54093,#54094),
 .UNSPECIFIED.,.F.,.F.,(4,1,1,1,1,1,1,1,1,1,1,1,1,1,1,1,1,1,1,1,1,1,1,4),
(0.,0.0539979975781232,0.107995995156246,0.215991990312493,0.269989987890616,
0.323987985468739,0.377985983046862,0.431983980624985,0.458982979414047,
0.472482478808578,0.485981978203109,0.49948147759764,0.51298097699217,0.519730726689436,
0.521418164113752,0.526480476386701,0.529855351235334,0.533230226083967,
0.536605100932599,0.538292538356915,0.539979975781232,0.593977973359355,
0.647975970937478,0.755971966093725),.UNSPECIFIED.);
#7622=B_SPLINE_CURVE_WITH_KNOTS('',3,(#54096,#54097,#54098,#54099),
 .UNSPECIFIED.,.F.,.F.,(4,4),(-0.0833603842763953,0.),.UNSPECIFIED.);
#7623=B_SPLINE_CURVE_WITH_KNOTS('',3,(#54101,#54102,#54103,#54104,#54105,
#54106),.UNSPECIFIED.,.F.,.F.,(4,1,1,4),(-0.799336073509661,-0.594771590871585,
-0.39020710823351,-0.0833603842763964),.UNSPECIFIED.);
#7624=B_SPLINE_CURVE_WITH_KNOTS('',3,(#54108,#54109,#54110,#54111,#54112,
#54113,#54114,#54115,#54116,#54117,#54118,#54119,#54120,#54121,#54122,#54123),
 .UNSPECIFIED.,.F.,.F.,(4,2,2,2,2,2,2,4),(0.0118379321062938,0.107024163210369,
0.335817375141192,0.559775143232002,0.672782851896336,0.729545183131027,
0.757993915544536,0.787301420911162),.UNSPECIFIED.);
#7625=B_SPLINE_CURVE_WITH_KNOTS('',3,(#54125,#54126,#54127,#54128,#54129,
#54130),.UNSPECIFIED.,.F.,.F.,(4,1,1,4),(-3.17329134625142,-3.0004111005852,
-2.65465060925274,-1.96312962658784),.UNSPECIFIED.);
#7626=B_SPLINE_CURVE_WITH_KNOTS('',3,(#54132,#54133,#54134,#54135,#54136,
#54137),.UNSPECIFIED.,.F.,.F.,(4,1,1,4),(-4.08237667107798,-3.69276867472374,
-3.43303001048758,-3.17329134625142),.UNSPECIFIED.);
#7627=B_SPLINE_CURVE_WITH_KNOTS('',3,(#54139,#54140,#54141,#54142,#54143,
#54144,#54145,#54146,#54147,#54148,#54149,#54150,#54151,#54152,#54153,#54154,
#54155,#54156,#54157,#54158,#54159,#54160,#54161,#54162,#54163,#54164,#54165,
#54166,#54167,#54168,#54169,#54170,#54171,#54172,#54173,#54174,#54175,#54176,
#54177,#54178,#54179,#54180,#54181,#54182,#54183,#54184,#54185,#54186,#54187,
#54188,#54189,#54190,#54191,#54192,#54193,#54194,#54195,#54196,#54197,#54198,
#54199,#54200,#54201,#54202,#54203,#54204,#54205,#54206,#54207,#54208,#54209,
#54210,#54211),.UNSPECIFIED.,.F.,.F.,(4,3,3,3,3,3,3,3,3,3,3,3,3,3,3,3,3,
3,3,3,3,3,3,3,4),(-5.24963523804274,-5.22555794291826,-5.19586107911791,
-5.18687812799744,-5.14098553954611,-5.12430645426268,-5.08288401419063,
-5.01504766740605,-4.99102394383036,-4.91855573999006,-4.84257002484868,
-4.76122999602307,-4.74938156648641,-4.68977118521554,-4.60201605684906,
-4.51864743190061,-4.48764588312174,-4.41261409008418,-4.37103514543172,
-4.30477017347109,-4.24196226368263,-4.18335539931493,-4.16463763971098,
-4.11019379776344,-4.08237667199167),.UNSPECIFIED.);
#7628=B_SPLINE_CURVE_WITH_KNOTS('',3,(#54213,#54214,#54215,#54216,#54217,
#54218,#54219),.UNSPECIFIED.,.F.,.F.,(4,1,1,1,4),(-6.31492339087005,-6.01055536310239,
-5.85837133809046,-5.5540032880666,-5.24963523804274),.UNSPECIFIED.);
#7629=B_SPLINE_CURVE_WITH_KNOTS('',3,(#54221,#54222,#54223,#54224,#54225,
#54226,#54227,#54228,#54229,#54230,#54231,#54232,#54233,#54234,#54235,#54236,
#54237,#54238,#54239,#54240,#54241,#54242,#54243,#54244,#54245,#54246,#54247,
#54248,#54249,#54250,#54251,#54252,#54253,#54254,#54255,#54256,#54257,#54258,
#54259,#54260,#54261,#54262,#54263,#54264,#54265,#54266,#54267,#54268,#54269,
#54270,#54271,#54272,#54273,#54274,#54275,#54276,#54277,#54278,#54279,#54280,
#54281,#54282,#54283,#54284),.UNSPECIFIED.,.F.,.F.,(4,3,3,3,3,3,3,3,3,3,
3,3,3,3,3,3,3,3,3,3,3,4),(-7.69657824876369,-7.69585220010023,-7.63949305537026,
-7.5897176515031,-7.56210720609799,-7.48884902843925,-7.43938651036202,
-7.32366994771237,-7.30181972429585,-7.22643881215268,-7.10444046206193,
-7.091900638509,-6.97438837483062,-6.90706119982801,-6.89058485139341,-6.80837156871105,
-6.74329402873901,-6.70968193759409,-6.54917179381872,-6.51230267536017,
-6.37970879985935,-6.31492341362349),.UNSPECIFIED.);
#7630=B_SPLINE_CURVE_WITH_KNOTS('',3,(#54286,#54287,#54288,#54289,#54290,
#54291,#54292,#54293,#54294),.UNSPECIFIED.,.F.,.F.,(4,1,1,1,1,1,4),(-10.2944961530174,
-9.9233650238383,-9.5522338946592,-9.18110276548009,-8.43884050712189,-8.06770937794279,
-7.69657825451453),.UNSPECIFIED.);
#7631=B_SPLINE_CURVE_WITH_KNOTS('',3,(#54296,#54297,#54298,#54299,#54300,
#54301,#54302,#54303),.UNSPECIFIED.,.F.,.F.,(4,1,1,1,1,4),(-11.9813316832122,
-11.8608434310554,-11.7403551788986,-11.2584021702716,-10.7764491616445,
-10.2944961530174),.UNSPECIFIED.);
#7632=B_SPLINE_CURVE_WITH_KNOTS('',3,(#54305,#54306,#54307,#54308,#54309,
#54310,#54311,#54312,#54313,#54314),.UNSPECIFIED.,.F.,.F.,(4,1,1,1,1,1,
1,4),(-16.6980910490008,-16.0242682824596,-14.6766227493771,-14.0027999828359,
-13.3289772162947,-12.6551544497534,-12.3182430664828,-11.9813316832122),
 .UNSPECIFIED.);
#7633=B_SPLINE_CURVE_WITH_KNOTS('',3,(#54316,#54317,#54318,#54319,#54320,
#54321,#54322,#54323,#54324),.UNSPECIFIED.,.F.,.F.,(4,1,1,1,1,1,4),(-21.7463678506673,
-21.0251854504292,-19.5828206499531,-18.861638249715,-18.140455849477,-17.4192734492389,
-16.6980910490008),.UNSPECIFIED.);
#7634=B_SPLINE_CURVE_WITH_KNOTS('',3,(#54326,#54327,#54328,#54329,#54330,
#54331,#54332),.UNSPECIFIED.,.F.,.F.,(4,1,1,1,4),(-25.457976371469,-24.3975168143727,
-23.8672870216316,-22.8068274361495,-21.7463678506673),.UNSPECIFIED.);
#7635=B_SPLINE_CURVE_WITH_KNOTS('',3,(#54334,#54335,#54336,#54337,#54338,
#54339,#54340,#54341),.UNSPECIFIED.,.F.,.F.,(4,2,2,4),(0.,0.213844974168118,
0.318336498142317,0.426627456126852),.UNSPECIFIED.);
#7636=B_SPLINE_CURVE_WITH_KNOTS('',3,(#54343,#54344,#54345,#54346,#54347,
#54348,#54349,#54350,#54351,#54352,#54353,#54354,#54355,#54356,#54357,#54358,
#54359,#54360,#54361,#54362,#54363,#54364,#54365,#54366,#54367,#54368,#54369,
#54370,#54371,#54372,#54373,#54374,#54375,#54376,#54377,#54378,#54379,#54380,
#54381,#54382,#54383,#54384,#54385,#54386,#54387,#54388,#54389,#54390,#54391,
#54392,#54393,#54394,#54395,#54396,#54397,#54398,#54399,#54400,#54401,#54402,
#54403,#54404,#54405,#54406,#54407,#54408,#54409,#54410,#54411,#54412,#54413,
#54414,#54415,#54416,#54417,#54418,#54419,#54420,#54421,#54422,#54423,#54424,
#54425,#54426,#54427),.UNSPECIFIED.,.F.,.F.,(4,3,3,3,3,3,3,3,3,3,3,3,3,
3,3,3,3,3,3,3,3,3,3,3,3,3,3,3,4),(16.1480982907358,16.2248435932826,16.3131664751049,
16.4010510064408,16.4871457020177,16.6179036047363,16.6781446318289,16.8189376696365,
16.955144254623,17.0336892409042,17.0716499935151,17.0956876497882,17.1122342271853,
17.1875859385791,17.2753698848045,17.3642719148437,17.402362983002,17.4328164230854,
17.5413519673841,17.6932989709641,17.7543954310227,17.8465699788546,17.9023081464328,
17.9153013030841,18.0357572506602,18.1619936402749,18.2808910196376,18.3561955540817,
18.3977432388145),.UNSPECIFIED.);
#7637=B_SPLINE_CURVE_WITH_KNOTS('',3,(#54429,#54430,#54431,#54432,#54433,
#54434,#54435,#54436,#54437,#54438,#54439,#54440,#54441,#54442,#54443,#54444,
#54445,#54446,#54447,#54448,#54449,#54450,#54451,#54452,#54453,#54454,#54455,
#54456,#54457,#54458,#54459,#54460,#54461,#54462,#54463,#54464,#54465,#54466,
#54467,#54468,#54469,#54470,#54471,#54472,#54473,#54474,#54475,#54476,#54477,
#54478,#54479,#54480,#54481,#54482,#54483,#54484,#54485,#54486,#54487,#54488,
#54489,#54490,#54491,#54492,#54493,#54494,#54495,#54496,#54497,#54498,#54499,
#54500,#54501,#54502,#54503,#54504,#54505,#54506,#54507,#54508,#54509,#54510,
#54511,#54512,#54513,#54514,#54515,#54516,#54517,#54518,#54519,#54520,#54521,
#54522,#54523,#54524,#54525,#54526,#54527,#54528,#54529,#54530,#54531,#54532,
#54533,#54534),.UNSPECIFIED.,.F.,.F.,(4,3,3,3,3,3,3,3,3,3,3,3,3,3,3,3,3,
3,3,3,3,3,3,3,3,3,3,3,3,3,3,3,3,3,3,4),(13.8978862047801,13.8984130587941,
13.9451297113282,13.9886893494331,14.0168480477334,14.0848270634095,14.131175493238,
14.2193450517567,14.3102533857122,14.3465462347775,14.4385871510249,14.5269329935135,
14.6138701631047,14.6996609714898,14.7622448570774,14.8183725724115,14.862262798083,
14.9426275163738,15.0148788949253,15.0849903110361,15.1538012013756,15.1837216712462,
15.2582774812726,15.3362859342931,15.420896880999,15.5051805444094,15.5789709859087,
15.6375672112739,15.7048255919162,15.7713399419104,15.8266394175726,15.9080154600573,
15.9937473972911,16.0847574555634,16.1427982324843,16.1480982907358),
 .UNSPECIFIED.);
#7638=B_SPLINE_CURVE_WITH_KNOTS('',3,(#54536,#54537,#54538,#54539,#54540,
#54541,#54542,#54543,#54544,#54545,#54546,#54547,#54548,#54549,#54550,#54551,
#54552,#54553,#54554,#54555,#54556,#54557,#54558,#54559,#54560,#54561,#54562,
#54563,#54564,#54565,#54566,#54567,#54568,#54569,#54570,#54571,#54572,#54573,
#54574,#54575,#54576,#54577,#54578,#54579,#54580,#54581,#54582,#54583,#54584),
 .UNSPECIFIED.,.F.,.F.,(4,3,3,3,3,3,3,3,3,3,3,3,3,3,3,3,4),(12.3501209228208,
12.3501377830757,12.4774048190594,12.5359956487871,12.6983861874045,12.7208084228289,
12.8726544490315,12.9290663407961,13.0134488895805,13.0860855995525,13.231115647179,
13.3679133715857,13.455667534087,13.4592103546039,13.6071368603549,13.7603835918095,
13.8978861785935),.UNSPECIFIED.);
#7639=B_SPLINE_CURVE_WITH_KNOTS('',3,(#54586,#54587,#54588,#54589,#54590,
#54591,#54592,#54593,#54594),.UNSPECIFIED.,.F.,.F.,(4,1,1,1,1,1,4),(10.8793710892452,
11.0894782083274,11.2995853274097,11.5096924464919,11.7197995655741,11.9299066846563,
12.3501209228208),.UNSPECIFIED.);
#7640=B_SPLINE_CURVE_WITH_KNOTS('',3,(#54596,#54597,#54598,#54599,#54600,
#54601,#54602,#54603,#54604,#54605,#54606,#54607,#54608,#54609,#54610,#54611,
#54612,#54613,#54614,#54615,#54616,#54617,#54618,#54619,#54620,#54621,#54622,
#54623,#54624,#54625,#54626,#54627,#54628,#54629,#54630,#54631,#54632,#54633,
#54634,#54635,#54636,#54637,#54638,#54639,#54640,#54641,#54642,#54643,#54644,
#54645,#54646,#54647,#54648,#54649,#54650,#54651,#54652,#54653,#54654,#54655,
#54656,#54657,#54658,#54659,#54660,#54661,#54662,#54663,#54664,#54665,#54666,
#54667,#54668),.UNSPECIFIED.,.F.,.F.,(4,3,3,3,3,3,3,3,3,3,3,3,3,3,3,3,3,
3,3,3,3,3,3,3,4),(7.92790045161141,7.92790443383917,8.08238192001809,8.21014604617211,
8.3584935347356,8.50965281881294,8.66649295639789,8.68369720698906,8.77117777664964,
8.93535063493343,9.07053253199945,9.19281643916875,9.2095400889765,9.34694768700197,
9.5026441951939,9.61445510168786,9.81054146163073,9.89179677630612,10.0351653028737,
10.036093764207,10.2469130954665,10.4577324267261,10.6253794515734,10.7842352433031,
10.8793710891041),.UNSPECIFIED.);
#7641=B_SPLINE_CURVE_WITH_KNOTS('',3,(#54670,#54671,#54672,#54673,#54674,
#54675),.UNSPECIFIED.,.F.,.F.,(4,2,4),(0.,0.241870352729709,0.496358334674456),
 .UNSPECIFIED.);
#7642=B_SPLINE_CURVE_WITH_KNOTS('',3,(#54677,#54678,#54679,#54680,#54681,
#54682,#54683,#54684,#54685,#54686,#54687,#54688,#54689,#54690,#54691,#54692,
#54693,#54694,#54695,#54696,#54697,#54698,#54699,#54700,#54701,#54702,#54703,
#54704,#54705,#54706,#54707,#54708,#54709,#54710,#54711,#54712,#54713,#54714,
#54715,#54716,#54717,#54718,#54719,#54720,#54721,#54722,#54723,#54724,#54725,
#54726,#54727,#54728,#54729,#54730,#54731,#54732,#54733,#54734,#54735,#54736,
#54737,#54738,#54739,#54740,#54741,#54742,#54743,#54744,#54745,#54746,#54747,
#54748,#54749,#54750,#54751,#54752,#54753,#54754,#54755),.UNSPECIFIED.,
 .F.,.F.,(4,3,3,3,3,3,3,3,3,3,3,3,3,3,3,3,3,3,3,3,3,3,3,3,3,3,4),(4.48918216137468,
4.57836268956684,4.66429138725693,4.70204447593824,4.75184600019805,4.83940061313917,
4.92497557084337,5.00655520602809,5.10614528180705,5.20279005119437,5.30456419127571,
5.44718714106359,5.5287983194506,5.53983751666817,5.74220502779296,5.79984794218939,
5.89005596843266,5.98727783913441,6.06516519431491,6.21635416528659,6.24027442019716,
6.44087192221132,6.52618822266893,6.59049287196166,6.84221467108407,6.94070913857473,
6.94071132372615),.UNSPECIFIED.);
#7643=B_SPLINE_CURVE_WITH_KNOTS('',3,(#54757,#54758,#54759,#54760),
 .UNSPECIFIED.,.F.,.F.,(4,4),(3.57654770812807,4.48918216137468),
 .UNSPECIFIED.);
#7644=B_SPLINE_CURVE_WITH_KNOTS('',3,(#54762,#54763,#54764,#54765,#54766,
#54767,#54768,#54769,#54770,#54771,#54772,#54773,#54774,#54775,#54776,#54777,
#54778,#54779,#54780,#54781,#54782,#54783,#54784,#54785,#54786,#54787,#54788,
#54789,#54790,#54791,#54792,#54793,#54794,#54795,#54796,#54797,#54798,#54799,
#54800,#54801),.UNSPECIFIED.,.F.,.F.,(4,3,3,3,3,3,3,3,3,3,3,3,3,4),(2.87518401914012,
3.02563515937007,3.11017562117646,3.17608629960003,3.18735576179043,3.2379900880792,
3.30733349478453,3.35480663273688,3.37667690148986,3.39282841371691,3.43385902271625,
3.47939932986374,3.53071044652234,3.57654770812807),.UNSPECIFIED.);
#7645=B_SPLINE_CURVE_WITH_KNOTS('',3,(#54803,#54804,#54805,#54806,#54807,
#54808,#54809,#54810,#54811,#54812,#54813,#54814,#54815,#54816,#54817,#54818,
#54819,#54820,#54821,#54822,#54823,#54824,#54825,#54826,#54827,#54828,#54829,
#54830,#54831,#54832,#54833,#54834,#54835,#54836,#54837,#54838,#54839,#54840,
#54841,#54842,#54843,#54844,#54845,#54846,#54847,#54848,#54849,#54850,#54851,
#54852,#54853,#54854,#54855,#54856,#54857,#54858,#54859,#54860,#54861,#54862,
#54863,#54864,#54865,#54866,#54867,#54868,#54869,#54870,#54871,#54872,#54873,
#54874,#54875,#54876,#54877,#54878,#54879,#54880,#54881),.UNSPECIFIED.,
 .F.,.F.,(4,3,3,3,3,3,3,3,3,3,3,3,3,3,3,3,3,3,3,3,3,3,3,3,3,3,4),(2.26956600808026,
2.30568082207415,2.31814480426122,2.35518314641223,2.39329029907104,2.43342479089149,
2.44265392439187,2.46304008322477,2.5008316930767,2.50395325324957,2.52910268948728,
2.55062012891362,2.55910730470815,2.57081062046563,2.60742859742941,2.61583165898047,
2.62631661195726,2.63142841550033,2.65685256816584,2.68832611522751,2.70246454006634,
2.70904066964155,2.74494826348243,2.77791213560758,2.82654807737385,2.85614989666385,
2.87518401914012),.UNSPECIFIED.);
#7646=B_SPLINE_CURVE_WITH_KNOTS('',3,(#54882,#54883,#54884,#54885,#54886,
#54887,#54888,#54889,#54890,#54891,#54892,#54893,#54894,#54895,#54896,#54897,
#54898,#54899,#54900,#54901,#54902,#54903,#54904,#54905,#54906,#54907,#54908,
#54909,#54910,#54911,#54912,#54913,#54914,#54915,#54916,#54917,#54918,#54919,
#54920,#54921,#54922,#54923,#54924,#54925,#54926,#54927,#54928,#54929,#54930,
#54931,#54932,#54933,#54934,#54935,#54936,#54937,#54938,#54939,#54940,#54941,
#54942,#54943,#54944,#54945,#54946,#54947,#54948,#54949,#54950,#54951,#54952,
#54953,#54954,#54955,#54956,#54957,#54958,#54959,#54960,#54961,#54962,#54963,
#54964,#54965,#54966,#54967,#54968,#54969,#54970,#54971,#54972,#54973,#54974,
#54975,#54976,#54977,#54978),.UNSPECIFIED.,.F.,.F.,(4,3,3,3,3,3,3,3,3,3,
3,3,3,3,3,3,3,3,3,3,3,3,3,3,3,3,3,3,3,3,3,3,4),(1.46286899092626,1.46985285769437,
1.5137075307432,1.55730858759994,1.57811142102339,1.61237368561188,1.64995874630276,
1.68914538920166,1.72860789735176,1.74425867666418,1.78111773623103,1.79707974781328,
1.80859628337331,1.84907728093944,1.889870666217,1.92383871454827,1.96141591955071,
1.96555135546924,2.00234636696739,2.03908114572322,2.05196363571095,2.07839684177744,
2.10581001941975,2.12770951388927,2.15432357689818,2.18891560494525,2.1991989789344,
2.22850627287637,2.23444430767235,2.25199383424393,2.26342001656095,2.26950924404891,
2.26956600807314),.UNSPECIFIED.);
#7647=B_SPLINE_CURVE_WITH_KNOTS('',3,(#54983,#54984,#54985,#54986),
 .UNSPECIFIED.,.F.,.F.,(4,4),(8.29205753853133,8.85500373849296),
 .UNSPECIFIED.);
#7648=B_SPLINE_CURVE_WITH_KNOTS('',3,(#54988,#54989,#54990,#54991),
 .UNSPECIFIED.,.F.,.F.,(4,4),(7.63533633256183,8.29189845043642),
 .UNSPECIFIED.);
#7649=B_SPLINE_CURVE_WITH_KNOTS('',3,(#54993,#54994,#54995,#54996,#54997),
 .UNSPECIFIED.,.F.,.F.,(4,1,4),(5.32811515172559,6.48172574214371,7.63514290575142),
 .UNSPECIFIED.);
#7650=B_SPLINE_CURVE_WITH_KNOTS('',3,(#54999,#55000,#55001,#55002,#55003,
#55004,#55005,#55006,#55007,#55008,#55009,#55010,#55011,#55012,#55013,#55014,
#55015,#55016,#55017,#55018,#55019,#55020,#55021,#55022,#55023,#55024,#55025,
#55026,#55027,#55028,#55029,#55030,#55031,#55032,#55033,#55034,#55035,#55036,
#55037,#55038,#55039,#55040,#55041,#55042,#55043,#55044,#55045,#55046,#55047,
#55048,#55049,#55050),.UNSPECIFIED.,.F.,.F.,(4,3,3,3,3,3,3,3,3,3,3,3,3,
3,3,3,3,4),(4.66932841177279,4.73492083097529,4.79747132048363,4.8190732798771,
4.8275011041002,4.8860357191341,4.94431270889177,4.97628795542774,4.97834918285331,
5.03679836578301,5.09530709015466,5.14398063744379,5.2028087815468,5.21750136742543,
5.23326287582971,5.28067425968518,5.32743480017277,5.32765283089508),
 .UNSPECIFIED.);
#7651=B_SPLINE_CURVE_WITH_KNOTS('',3,(#55052,#55053,#55054,#55055),
 .UNSPECIFIED.,.F.,.F.,(4,4),(4.10897615004708,4.66916207727921),
 .UNSPECIFIED.);
#7652=B_SPLINE_CURVE_WITH_KNOTS('',3,(#55057,#55058,#55059,#55060,#55061,
#55062,#55063,#55064,#55065,#55066,#55067,#55068,#55069,#55070,#55071,#55072,
#55073,#55074,#55075,#55076,#55077,#55078,#55079,#55080,#55081,#55082,#55083,
#55084,#55085,#55086,#55087,#55088,#55089,#55090,#55091,#55092,#55093,#55094,
#55095,#55096,#55097,#55098,#55099,#55100,#55101,#55102,#55103,#55104,#55105,
#55106,#55107,#55108,#55109,#55110,#55111,#55112,#55113,#55114,#55115,#55116,
#55117,#55118,#55119,#55120,#55121,#55122,#55123,#55124,#55125,#55126,#55127,
#55128,#55129,#55130,#55131,#55132,#55133,#55134,#55135,#55136,#55137,#55138),
 .UNSPECIFIED.,.F.,.F.,(4,3,3,3,3,3,3,3,3,3,3,3,3,3,3,3,3,3,3,3,3,3,3,3,
3,3,3,4),(3.55050287755944,3.58233413005538,3.61346023613394,3.64477916715078,
3.67699342493071,3.685706834098,3.71988312339799,3.7380145269766,3.77519268224312,
3.81488249921756,3.82215303959738,3.8294256312647,3.86853740020997,3.89174467951658,
3.93186243524685,3.96260357314154,3.96888700811733,4.00385538849654,4.03492331319416,
4.03861769654365,4.05423052961338,4.07222654910159,4.08279331553507,4.09092247278122,
4.09689520868099,4.10262179682547,4.10783906800098,4.10834838496996),
 .UNSPECIFIED.);
#7653=B_SPLINE_CURVE_WITH_KNOTS('',3,(#55140,#55141,#55142,#55143,#55144),
 .UNSPECIFIED.,.F.,.F.,(4,1,4),(2.82488904953941,3.18769596354942,3.5497180136926),
 .UNSPECIFIED.);
#7654=B_SPLINE_CURVE_WITH_KNOTS('',3,(#55146,#55147,#55148,#55149,#55150,
#55151,#55152,#55153,#55154,#55155,#55156),.UNSPECIFIED.,.F.,.F.,(4,1,1,
1,1,1,1,1,4),(1.00983872354131,1.23672001429108,1.46360130504084,1.91736388654036,
2.37112646803988,2.59800775878964,2.71144840416452,2.76816872685197,2.82467737519672),
 .UNSPECIFIED.);
#7655=B_SPLINE_CURVE_WITH_KNOTS('',3,(#55158,#55159,#55160,#55161,#55162,
#55163),.UNSPECIFIED.,.F.,.F.,(4,1,1,4),(0.268956516008204,0.639397619774759,
0.824618171658037,1.00958216337679),.UNSPECIFIED.);
#7656=B_SPLINE_CURVE_WITH_KNOTS('',3,(#55164,#55165,#55166,#55167),
 .UNSPECIFIED.,.F.,.F.,(4,4),(0.,0.268918781548623),.UNSPECIFIED.);
#7657=B_SPLINE_CURVE_WITH_KNOTS('',3,(#55170,#55171,#55172,#55173,#55174),
 .UNSPECIFIED.,.F.,.F.,(4,1,4),(1.03844659662145,1.19032888736264,1.29158374785677),
 .UNSPECIFIED.);
#7658=B_SPLINE_CURVE_WITH_KNOTS('',3,(#55176,#55177,#55178,#55179,#55180,
#55181,#55182,#55183,#55184),.UNSPECIFIED.,.F.,.F.,(4,1,1,1,1,1,4),(0.489962919054084,
0.599485472462595,0.709225753502309,0.818966034542023,0.928706315581737,
0.983576456101594,1.03817397537901),.UNSPECIFIED.);
#7659=B_SPLINE_CURVE_WITH_KNOTS('',3,(#55185,#55186,#55187,#55188,#55189,
#55190,#55191,#55192,#55193),.UNSPECIFIED.,.F.,.F.,(4,1,1,1,1,1,4),(0.,
0.0979490382845762,0.195898076569152,0.293847114853729,0.391796153138305,
0.440770672280593,0.489745191422881),.UNSPECIFIED.);
#7660=B_SPLINE_CURVE_WITH_KNOTS('',3,(#55196,#55197,#55198,#55199),
 .UNSPECIFIED.,.F.,.F.,(4,4),(1.18065640410841,1.2915881661436),
 .UNSPECIFIED.);
#7661=B_SPLINE_CURVE_WITH_KNOTS('',3,(#55201,#55202,#55203,#55204,#55205,
#55206,#55207,#55208,#55209),.UNSPECIFIED.,.F.,.F.,(4,1,1,1,1,1,4),(0.334860544053774,
0.50397957342097,0.673148781092829,0.757733384928759,0.842317988764689,
1.01148719643655,1.18065599249865),.UNSPECIFIED.);
#7662=B_SPLINE_CURVE_WITH_KNOTS('',3,(#55210,#55211,#55212,#55213,#55214,
#55215),.UNSPECIFIED.,.F.,.F.,(4,1,1,4),(0.,0.133924146299644,0.234367256024377,
0.334810365749111),.UNSPECIFIED.);
#7663=B_SPLINE_CURVE_WITH_KNOTS('',3,(#55493,#55494,#55495,#55496,#55497,
#55498),.UNSPECIFIED.,.F.,.F.,(4,1,1,4),(-1.,-0.571428571428571,-0.285714285714286,
0.),.UNSPECIFIED.);
#7664=B_SPLINE_CURVE_WITH_KNOTS('',3,(#55500,#55501,#55502,#55503,#55504,
#55505,#55506,#55507,#55508,#55509,#55510,#55511,#55512,#55513,#55514,#55515,
#55516,#55517,#55518,#55519,#55520,#55521,#55522,#55523,#55524,#55525,#55526,
#55527,#55528,#55529,#55530,#55531,#55532,#55533,#55534,#55535,#55536,#55537,
#55538,#55539,#55540,#55541,#55542,#55543,#55544,#55545,#55546,#55547,#55548,
#55549,#55550,#55551,#55552,#55553,#55554,#55555,#55556,#55557,#55558,#55559,
#55560,#55561,#55562,#55563,#55564,#55565,#55566,#55567,#55568,#55569,#55570,
#55571,#55572,#55573,#55574,#55575,#55576,#55577,#55578,#55579,#55580,#55581,
#55582,#55583,#55584,#55585,#55586,#55587,#55588,#55589,#55590,#55591,#55592,
#55593,#55594,#55595,#55596,#55597,#55598,#55599,#55600,#55601,#55602,#55603,
#55604,#55605,#55606,#55607,#55608,#55609,#55610,#55611,#55612,#55613,#55614,
#55615,#55616,#55617,#55618,#55619,#55620,#55621,#55622,#55623,#55624,#55625,
#55626,#55627,#55628,#55629,#55630,#55631,#55632,#55633,#55634,#55635,#55636,
#55637,#55638,#55639,#55640,#55641,#55642,#55643,#55644,#55645,#55646,#55647,
#55648,#55649,#55650,#55651,#55652,#55653,#55654,#55655,#55656,#55657,#55658,
#55659,#55660,#55661,#55662,#55663,#55664,#55665,#55666,#55667,#55668,#55669,
#55670,#55671,#55672,#55673,#55674,#55675,#55676,#55677,#55678,#55679,#55680,
#55681,#55682,#55683,#55684,#55685,#55686,#55687,#55688,#55689,#55690,#55691,
#55692,#55693,#55694,#55695,#55696,#55697,#55698,#55699,#55700,#55701,#55702,
#55703,#55704),.UNSPECIFIED.,.F.,.F.,(4,3,3,3,3,3,3,3,3,3,3,3,3,3,3,3,3,
3,3,3,3,3,3,3,3,3,3,3,3,3,3,3,3,3,3,3,3,3,3,3,3,3,3,3,3,3,3,3,3,3,3,3,3,
3,3,3,3,3,3,3,3,3,3,3,3,3,3,3,4),(-9.19419977830157,-9.10967608036533,-9.02523282363516,
-8.94087429868734,-8.92020082022876,-8.83188380164302,-8.74236525285732,
-8.65258172389636,-8.56298604858251,-8.53897544224619,-8.46560848396481,
-8.38864387903952,-8.31528837316212,-8.2419149911821,-8.16847927352024,
-8.15775006426363,-8.07380735585024,-7.98974952828677,-7.94884017932526,
-7.87139630781852,-7.79379299394296,-7.73993029438688,-7.66519283888366,
-7.59001323218429,-7.5145357766191,-7.43911146275571,-7.36405403236351,
-7.32211052451013,-7.21765558204094,-7.12139380485458,-7.11320063957175,
-7.04908916983143,-6.9851270843274,-6.92121820544923,-6.85730830828777,
-6.79983581216419,-6.73688596392217,-6.695380869695,-6.62424896314964,-6.55311746674484,
-6.48647098475663,-6.43485622044857,-6.38692241757501,-6.33535788303195,
-6.28737385039339,-6.22503102968951,-6.16273885291714,-6.1004508403693,
-6.08827671603015,-5.99093468403265,-5.89334485331293,-5.79536092392622,
-5.73985673089448,-5.70857737642468,-5.69008244730366,-5.63354107741789,
-5.5779611592562,-5.52093906350838,-5.46391696776057,-5.39948019473393,
-5.33491566029492,-5.27038189381646,-5.23775148821748,-5.16837194734185,
-5.09905627112296,-5.08697450185542,-5.0692256166783,-5.01597896114694,
-4.99026184062722),.UNSPECIFIED.);
#7665=B_SPLINE_CURVE_WITH_KNOTS('',3,(#55705,#55706,#55707,#55708,#55709,
#55710,#55711,#55712,#55713,#55714,#55715,#55716,#55717,#55718,#55719,#55720,
#55721,#55722,#55723,#55724,#55725),.UNSPECIFIED.,.F.,.F.,(4,1,1,2,1,2,
1,1,1,2,1,2,2,4),(-4.99026184062445,-4.94498342043847,-4.80299233902153,
-4.51901017618764,-4.27069680674408,-3.85684119100481,-3.05948850905774,
-2.69705547180907,-1.68224296751281,-1.53726975261334,-1.28960453962952,
-0.876829184656479,-0.308773384377632,0.),.UNSPECIFIED.);
#7666=B_SPLINE_CURVE_WITH_KNOTS('',3,(#55730,#55731,#55732,#55733,#55734,
#55735,#55736,#55737,#55738,#55739,#55740,#55741,#55742,#55743,#55744),
 .UNSPECIFIED.,.F.,.F.,(4,2,2,2,1,2,2,4),(-9.1649736818217,-8.85500373849296,
-8.29205753853133,-7.63533633256183,-6.48172574214371,-5.32811515172559,
-4.66932841177279,-4.19968198790815),.UNSPECIFIED.);
#7667=B_SPLINE_CURVE_WITH_KNOTS('',3,(#55745,#55746,#55747,#55748,#55749,
#55750,#55751,#55752,#55753,#55754,#55755,#55756,#55757,#55758,#55759,#55760,
#55761,#55762,#55763,#55764,#55765,#55766,#55767,#55768,#55769,#55770,#55771),
 .UNSPECIFIED.,.F.,.F.,(4,2,1,1,1,2,1,2,1,1,1,1,1,1,1,2,1,1,2,4),(-4.19968198790815,
-4.10834838496996,-4.03861769654365,-3.96888700811733,-3.8294256312647,
-3.55050287755944,-3.18769596354942,-2.82488904953941,-2.76816872685197,
-2.71144840416452,-2.59800775878964,-2.37112646803988,-1.91736388654036,
-1.46360130504084,-1.23672001429108,-1.00983872354131,-0.824618171658037,
-0.639397619774759,-0.268956516008204,0.),.UNSPECIFIED.);
#7668=B_SPLINE_CURVE_WITH_KNOTS('',3,(#55962,#55963,#55964,#55965,#55966),
 .UNSPECIFIED.,.F.,.F.,(4,1,4),(-1.,-0.571428571428571,0.),
 .UNSPECIFIED.);
#7669=B_SPLINE_CURVE_WITH_KNOTS('',3,(#56053,#56054,#56055,#56056,#56057),
 .UNSPECIFIED.,.F.,.F.,(4,1,4),(-0.999999907726918,-0.571428571428571,0.),
 .UNSPECIFIED.);
#7670=B_SPLINE_CURVE_WITH_KNOTS('',3,(#56059,#56060,#56061,#56062,#56063,
#56064,#56065,#56066),.UNSPECIFIED.,.F.,.F.,(4,1,1,2,4),(-1.29174070129165,
-1.21783674573549,-1.07002883462318,-0.922220923510859,-0.822192426456486),
 .UNSPECIFIED.);
#7671=B_SPLINE_CURVE_WITH_KNOTS('',3,(#56067,#56068,#56069,#56070,#56071,
#56072,#56073,#56074,#56075,#56076,#56077,#56078,#56079),.UNSPECIFIED.,
 .F.,.F.,(4,1,1,1,1,1,1,1,2,4),(-0.822192426456486,-0.795342097926536,-0.753049156065094,
-0.668463272342212,-0.583877388619329,-0.414705621173564,-0.330119737450682,
-0.245533853727799,-0.076362086282034,0.),.UNSPECIFIED.);
#7672=B_SPLINE_CURVE_WITH_KNOTS('',3,(#56084,#56085,#56086,#56087,#56088,
#56089,#56090,#56091,#56092,#56093,#56094),.UNSPECIFIED.,.F.,.F.,(4,2,1,
1,1,1,1,4),(-1.2915881661436,-1.18065640410841,-1.01148719643655,-0.842317988764689,
-0.757733384928759,-0.673148781092829,-0.50397957342097,-0.434852353670097),
 .UNSPECIFIED.);
#7673=B_SPLINE_CURVE_WITH_KNOTS('',3,(#56095,#56096,#56097,#56098,#56099,
#56100,#56101,#56102),.UNSPECIFIED.,.F.,.F.,(4,2,1,1,4),(-0.434852353670097,
-0.334810365749111,-0.234367256024377,-0.133924146299644,0.),
 .UNSPECIFIED.);
#7674=B_SPLINE_CURVE_WITH_KNOTS('',3,(#56178,#56179,#56180,#56181,#56182),
 .UNSPECIFIED.,.F.,.F.,(4,1,4),(-1.,-0.571428571428571,0.),
 .UNSPECIFIED.);
#7675=B_SPLINE_CURVE_WITH_KNOTS('',3,(#56299,#56300,#56301,#56302,#56303),
 .UNSPECIFIED.,.F.,.F.,(4,1,4),(-0.999999920592112,-0.571428571428571,0.),
 .UNSPECIFIED.);
#7676=B_SPLINE_CURVE_WITH_KNOTS('',3,(#56305,#56306,#56307,#56308,#56309,
#56310,#56311,#56312),.UNSPECIFIED.,.F.,.F.,(4,1,1,1,1,4),(-1.29193145083568,
-1.18863906797729,-1.0853466851189,-0.982054302260506,-0.878761919402114,
-0.824095347984701),.UNSPECIFIED.);
#7677=B_SPLINE_CURVE_WITH_KNOTS('',3,(#56313,#56314,#56315,#56316,#56317,
#56318,#56319,#56320,#56321,#56322,#56323,#56324,#56325,#56326,#56327,#56328,
#56329,#56330,#56331),.UNSPECIFIED.,.F.,.F.,(4,2,1,1,1,1,1,1,1,1,1,2,1,
1,4),(-0.824095347984701,-0.775469536543723,-0.720593698815789,-0.665717861087855,
-0.555966185631988,-0.44621451017612,-0.336462834720253,-0.309024915856286,
-0.281586996992319,-0.254149078128352,-0.240430118696369,-0.226711159264386,
-0.181368927411508,-0.136026695558631,0.),.UNSPECIFIED.);
#7678=B_SPLINE_CURVE_WITH_KNOTS('',3,(#56336,#56337,#56338,#56339,#56340,
#56341,#56342,#56343,#56344,#56345,#56346,#56347,#56348,#56349),
 .UNSPECIFIED.,.F.,.F.,(4,1,2,1,1,1,1,1,2,4),(-1.29158374785677,-1.19032888736264,
-1.03844659662145,-0.983576456101594,-0.928706315581737,-0.818966034542023,
-0.709225753502309,-0.599485472462595,-0.489745191422881,-0.441202445761129),
 .UNSPECIFIED.);
#7679=B_SPLINE_CURVE_WITH_KNOTS('',3,(#56350,#56351,#56352,#56353,#56354,
#56355,#56356,#56357,#56358,#56359,#56360,#56361,#56362,#56363,#56364,#56365,
#56366,#56367,#56368,#56369,#56370,#56371,#56372,#56373,#56374,#56375,#56376,
#56377,#56378,#56379,#56380,#56381,#56382,#56383,#56384,#56385,#56386,#56387,
#56388,#56389,#56390,#56391,#56392,#56393,#56394,#56395,#56396,#56397,#56398,
#56399,#56400,#56401,#56402,#56403,#56404,#56405,#56406,#56407,#56408,#56409,
#56410,#56411,#56412,#56413,#56414,#56415,#56416,#56417,#56418,#56419),
 .UNSPECIFIED.,.F.,.F.,(4,3,3,3,3,3,3,3,3,3,3,3,3,3,3,3,3,3,3,3,3,3,3,4),
(-0.441202445748346,-0.440770672280593,-0.405187169748375,-0.391796153138305,
-0.370654147970551,-0.34952071493269,-0.328392763829246,-0.307253153744854,
-0.293847114853729,-0.270911242372769,-0.247950260814622,-0.224979378588364,
-0.201991894436606,-0.195898076569152,-0.171410816998008,-0.148142630717063,
-0.124879289690075,-0.101624933779237,-0.0979490382845762,-0.0768368069651967,
-0.055721769904546,-0.0346058366391704,-0.013467980506352,0.),
 .UNSPECIFIED.);
#7680=B_SPLINE_CURVE_WITH_KNOTS('',3,(#56515,#56516,#56517,#56518,#56519),
 .UNSPECIFIED.,.F.,.F.,(4,1,4),(-1.,-0.571428571428571,0.),
 .UNSPECIFIED.);
#7681=B_SPLINE_CURVE_WITH_KNOTS('',3,(#56553,#56554,#56555,#56556,#56557,
#56558,#56559,#56560,#56561,#56562,#56563,#56564,#56565,#56566),
 .UNSPECIFIED.,.F.,.F.,(4,2,2,2,2,2,4),(-0.0984980483372994,-0.0979809036544454,
-0.0915892250220569,-0.0852756446727988,-0.0728984092156269,-0.0491501163779407,
0.),.UNSPECIFIED.);
#7682=B_SPLINE_CURVE_WITH_KNOTS('',3,(#56568,#56569,#56570,#56571,#56572,
#56573,#56574,#56575),.UNSPECIFIED.,.F.,.F.,(4,2,2,4),(-0.0967838852773191,
-0.0481707148393364,0.,0.000510029835108177),.UNSPECIFIED.);
#7683=B_SPLINE_CURVE_WITH_KNOTS('',3,(#56598,#56599,#56600,#56601,#56602,
#56603,#56604,#56605),.UNSPECIFIED.,.F.,.F.,(4,2,2,4),(0.,0.0483258768809437,
0.0962566348254112,0.096764418539181),.UNSPECIFIED.);
#7684=B_SPLINE_CURVE_WITH_KNOTS('',3,(#56676,#56677,#56678,#56679,#56680,
#56681,#56682,#56683,#56684,#56685,#56686,#56687),.UNSPECIFIED.,.F.,.F.,
(4,2,2,2,2,4),(-0.0983831478381398,-0.0490393370760392,-0.0251933545123771,
-0.012733468587,0.,0.000519901458665688),.UNSPECIFIED.);
#7685=B_SPLINE_CURVE_WITH_KNOTS('',3,(#60150,#60151,#60152,#60153,#60154,
#60155,#60156,#60157,#60158,#60159,#60160,#60161,#60162,#60163,#60164,#60165),
 .UNSPECIFIED.,.F.,.F.,(4,2,2,2,2,2,2,4),(0.272063574481699,0.273032221187168,
0.283104685038129,0.293177148889091,0.303249612740052,0.323878507973205,
0.334192955589781,0.334675296855046),.UNSPECIFIED.);
#7686=B_SPLINE_CURVE_WITH_KNOTS('',3,(#60212,#60213,#60214,#60215,#60216,
#60217,#60218,#60219,#60220,#60221,#60222,#60223,#60224,#60225,#60226,#60227),
 .UNSPECIFIED.,.F.,.F.,(4,2,2,2,2,2,2,4),(0.0707623923472314,0.0712447336124956,
0.0815591812290722,0.102188076462226,0.112260540313187,0.122333004164148,
0.13240546801511,0.13337411472058),.UNSPECIFIED.);
#7687=B_SPLINE_CURVE_WITH_KNOTS('',3,(#60390,#60391,#60392,#60393,#60394,
#60395,#60396,#60397,#60398,#60399,#60400,#60401,#60402,#60403,#60404,#60405,
#60406,#60407,#60408,#60409,#60410,#60411,#60412,#60413,#60414,#60415,#60416,
#60417),.UNSPECIFIED.,.F.,.F.,(4,3,3,3,3,3,3,3,3,4),(-0.0655070673051713,
-0.055900414383695,-0.0509627360763416,-0.0429749138091241,-0.0358530951083412,
-0.0278292322065516,-0.0195094227834791,-0.00979725211699082,0.,0.000308517528353623),
 .UNSPECIFIED.);
#7688=B_SPLINE_CURVE_WITH_KNOTS('',3,(#60508,#60509,#60510,#60511,#60512,
#60513,#60514,#60515,#60516,#60517,#60518,#60519,#60520,#60521,#60522,#60523,
#60524,#60525,#60526,#60527,#60528,#60529,#60530,#60531,#60532,#60533,#60534,
#60535),.UNSPECIFIED.,.F.,.F.,(4,3,3,3,3,3,3,3,3,4),(-0.131322652134434,
-0.131014134605989,-0.121216882489304,-0.111504711823152,-0.10288152233867,
-0.0951610394988666,-0.0866179312032352,-0.0800513985314073,-0.0695209906596313,
-0.0655070673030884),.UNSPECIFIED.);
#7689=B_SPLINE_CURVE_WITH_KNOTS('',3,(#60582,#60583,#60584,#60585,#60586,
#60587,#60588,#60589,#60590,#60591,#60592,#60593,#60594,#60595,#60596,#60597,
#60598,#60599,#60600,#60601,#60602,#60603,#60604,#60605,#60606,#60607,#60608,
#60609),.UNSPECIFIED.,.F.,.F.,(4,3,3,3,3,3,3,3,3,4),(-0.131322652140315,
-0.13101413461217,-0.121216882493846,-0.111504711827276,-0.102881522342513,
-0.0951610395023411,-0.0866179312064961,-0.0800513985342769,-0.0695209906621001,
-0.0655070673053875),.UNSPECIFIED.);
#7690=B_SPLINE_CURVE_WITH_KNOTS('',3,(#60667,#60668,#60669,#60670,#60671,
#60672,#60673,#60674,#60675,#60676,#60677,#60678,#60679,#60680,#60681,#60682,
#60683,#60684,#60685,#60686,#60687,#60688,#60689,#60690,#60691,#60692,#60693,
#60694),.UNSPECIFIED.,.F.,.F.,(4,3,3,3,3,3,3,3,3,4),(-0.000308517528449134,
0.,0.00979725211682612,0.0195094227831066,0.0281326122676244,0.0358530951076058,
0.0443962034033454,0.050962736075265,0.0614931439471759,0.0655070673037764),
 .UNSPECIFIED.);
#7691=B_SPLINE_CURVE_WITH_KNOTS('',3,(#61321,#61322,#61323,#61324,#61325,
#61326,#61327,#61328),.UNSPECIFIED.,.F.,.F.,(4,1,1,2,4),(0.886448358529016,
0.974711394590892,1.06297443065277,1.3277635388384,1.32899011332275),
 .UNSPECIFIED.);
#7692=B_SPLINE_CURVE_WITH_KNOTS('',3,(#61330,#61331,#61332,#61333),
 .UNSPECIFIED.,.F.,.F.,(4,4),(-0.111726598224603,-0.107341152681297),
 .UNSPECIFIED.);
#7693=B_SPLINE_CURVE_WITH_KNOTS('',3,(#61334,#61335,#61336,#61337,#61338,
#61339,#61340,#61341,#61342,#61343,#61344),.UNSPECIFIED.,.F.,.F.,(4,1,2,
2,2,4),(-0.107341152681297,-0.0558632991123017,0.,0.110861644323643,0.224510220235513,
0.333435958612223),.UNSPECIFIED.);
#7694=B_SPLINE_CURVE_WITH_KNOTS('',3,(#61380,#61381,#61382,#61383,#61384,
#61385),.UNSPECIFIED.,.F.,.F.,(4,2,4),(-0.00122657448435937,0.,0.44131518030938),
 .UNSPECIFIED.);
#7695=B_SPLINE_CURVE_WITH_KNOTS('',3,(#61482,#61483,#61484,#61485,#61486,
#61487,#61488,#61489,#61490,#61491,#61492,#61493,#61494,#61495),
 .UNSPECIFIED.,.F.,.F.,(4,2,2,2,2,2,4),(-4.00267101076923,-3.97980879370467,
-3.86999664917252,-3.77335331431691,-3.71746622872759,-3.69720180919271,
-3.6853266531919),.UNSPECIFIED.);
#7696=B_SPLINE_CURVE_WITH_KNOTS('',3,(#61500,#61501,#61502,#61503,#61504,
#61505,#61506,#61507,#61508,#61509,#61510,#61511,#61512,#61513,#61514,#61515),
 .UNSPECIFIED.,.F.,.F.,(4,2,2,2,2,2,2,4),(-0.827425542979679,-0.826220339571657,
-0.824592036045519,-0.820443574755297,-0.781909027879826,-0.745118942396318,
-0.725073379095867,-0.724859868833872),.UNSPECIFIED.);
#7697=B_SPLINE_CURVE_WITH_KNOTS('',3,(#61522,#61523,#61524,#61525,#61526,
#61527,#61528,#61529,#61530,#61531,#61532,#61533,#61534,#61535),
 .UNSPECIFIED.,.F.,.F.,(4,2,2,2,2,2,4),(0.0275854854772956,0.0545477001455191,
0.147140622467183,0.269392757315554,0.297346368764049,0.310172163976987,
0.314080909465034),.UNSPECIFIED.);
#7698=B_SPLINE_CURVE_WITH_KNOTS('',3,(#61538,#61539,#61540,#61541,#61542,
#61543,#61544,#61545,#61546,#61547,#61548,#61549,#61550,#61551,#61552,#61553,
#61554,#61555),.UNSPECIFIED.,.F.,.F.,(4,2,2,2,2,2,2,2,4),(0.121304483487225,
0.121522867409781,0.122956741161004,0.125266692582563,0.133381651141487,
0.155840009541048,0.198528123526881,0.228063475003939,0.232050075067381),
 .UNSPECIFIED.);
#7699=B_SPLINE_CURVE_WITH_KNOTS('',3,(#61996,#61997,#61998,#61999,#62000,
#62001,#62002,#62003,#62004,#62005,#62006,#62007,#62008,#62009,#62010,#62011,
#62012,#62013,#62014,#62015,#62016,#62017,#62018,#62019,#62020,#62021,#62022,
#62023,#62024,#62025,#62026,#62027,#62028,#62029,#62030,#62031,#62032,#62033,
#62034,#62035,#62036,#62037,#62038,#62039,#62040,#62041,#62042,#62043,#62044,
#62045,#62046,#62047,#62048,#62049,#62050,#62051,#62052,#62053,#62054,#62055,
#62056,#62057,#62058,#62059,#62060,#62061,#62062,#62063,#62064,#62065,#62066,
#62067,#62068,#62069,#62070,#62071,#62072,#62073,#62074,#62075,#62076,#62077,
#62078,#62079,#62080,#62081,#62082,#62083,#62084,#62085,#62086,#62087,#62088,
#62089,#62090,#62091,#62092,#62093,#62094,#62095,#62096,#62097,#62098,#62099,
#62100,#62101,#62102,#62103,#62104),.UNSPECIFIED.,.F.,.F.,(4,3,3,3,3,3,
3,3,3,3,3,3,3,3,3,3,3,3,3,3,3,3,3,3,3,3,3,3,3,3,3,3,3,3,3,3,4),(10.3762744482256,
10.4685616448508,10.5607276261043,10.6547964435211,10.7468093354631,10.8387943991844,
10.9307772613786,11.0264024873936,11.1185108557443,11.2106815902354,11.3029864495802,
11.3132781654386,11.4065164375908,11.4996317690644,11.5926515496584,11.6856071336555,
11.7785297343733,11.8714439672823,11.9643744342891,12.0574057190744,12.15049000187,
12.2437296619365,12.3127933039653,12.4057444841292,12.4985679912201,12.5912916301099,
12.6839457888757,12.7765638151076,12.8691706791047,12.9617913353808,13.0545109207409,
13.1472819693773,13.2402091284387,13.3123084424921,13.4054129193392,13.4983783998293,
13.5490822577306),.UNSPECIFIED.);
#7700=B_SPLINE_CURVE_WITH_KNOTS('',3,(#62107,#62108,#62109,#62110,#62111,
#62112,#62113,#62114,#62115,#62116,#62117,#62118,#62119,#62120,#62121,#62122,
#62123,#62124,#62125,#62126,#62127,#62128,#62129,#62130,#62131,#62132,#62133,
#62134,#62135,#62136,#62137,#62138,#62139,#62140,#62141,#62142,#62143,#62144,
#62145,#62146,#62147,#62148,#62149,#62150,#62151,#62152,#62153,#62154,#62155,
#62156,#62157,#62158,#62159,#62160,#62161,#62162,#62163,#62164,#62165,#62166,
#62167,#62168,#62169,#62170,#62171,#62172,#62173),.UNSPECIFIED.,.F.,.F.,
(4,3,3,3,3,3,3,3,3,3,3,3,3,3,3,3,3,3,3,3,3,3,4),(11.6152142277551,11.7104709514056,
11.805672798299,11.9008419087062,11.9960272735159,12.0912269901345,12.186461164303,
12.2817499296462,12.3771800378493,12.472688391674,12.5683655133993,12.6147293662818,
12.7068652367845,12.7988611340536,12.8925181866135,12.9843156369482,13.0760684890777,
13.1678025610073,13.2628813093886,13.3547002092736,13.4465675973497,13.5385499644351,
13.5481175545326),.UNSPECIFIED.);
#7701=B_SPLINE_CURVE_WITH_KNOTS('',3,(#62179,#62180,#62181,#62182,#62183,
#62184,#62185,#62186,#62187,#62188,#62189,#62190,#62191,#62192,#62193,#62194,
#62195,#62196,#62197,#62198,#62199,#62200,#62201,#62202,#62203,#62204,#62205,
#62206,#62207,#62208,#62209,#62210,#62211,#62212,#62213,#62214,#62215,#62216,
#62217,#62218,#62219,#62220,#62221,#62222,#62223,#62224,#62225,#62226,#62227,
#62228,#62229,#62230,#62231,#62232,#62233,#62234,#62235,#62236,#62237,#62238,
#62239,#62240,#62241,#62242,#62243,#62244,#62245,#62246,#62247,#62248,#62249,
#62250,#62251,#62252,#62253,#62254,#62255,#62256,#62257,#62258,#62259,#62260,
#62261,#62262,#62263,#62264,#62265,#62266,#62267,#62268,#62269,#62270,#62271,
#62272,#62273,#62274,#62275,#62276,#62277,#62278,#62279,#62280,#62281,#62282,
#62283,#62284,#62285,#62286,#62287,#62288,#62289,#62290,#62291,#62292,#62293,
#62294,#62295,#62296,#62297,#62298,#62299,#62300,#62301,#62302,#62303,#62304,
#62305,#62306,#62307,#62308,#62309,#62310,#62311,#62312,#62313,#62314,#62315,
#62316,#62317),.UNSPECIFIED.,.F.,.F.,(4,3,3,3,3,3,3,3,3,3,3,3,3,3,3,3,3,
3,3,3,3,3,3,3,3,3,3,3,3,3,3,3,3,3,3,3,3,3,3,3,3,3,3,3,3,3,4),(15.7079632679493,
15.801862704237,15.8957881015399,15.9897621227233,16.0838725098807,16.1780606852298,
16.2724168889073,16.3108538580724,16.403934049719,16.4968882171655,16.5897439863011,
16.6825319537682,16.775284780659,16.8680272835037,16.9607842637073,17.053640404213,
17.1465483531614,17.2396115558221,17.3103689965991,17.403446464583,17.4963979243741,
17.5892510054323,17.6820363258165,17.7747865316696,17.8675264427482,17.9602808637086,
18.0531345118179,18.1460400015679,18.2391008256502,18.3098841351259,18.4029568890223,
18.495903548684,18.5887517503804,18.6815320919292,18.7742772593972,18.8670120783317,
18.9597613591359,19.0526098238704,19.1455100981482,19.2385657080346,19.3093992736527,
19.4024726918571,19.4954250802269,19.5882679505022,19.681046896648,19.7737939705685,
19.8316169097465),.UNSPECIFIED.);
#7702=B_SPLINE_CURVE_WITH_KNOTS('',3,(#62318,#62319,#62320,#62321,#62322,
#62323,#62324,#62325,#62326,#62327,#62328,#62329,#62330,#62331,#62332,#62333,
#62334,#62335,#62336,#62337,#62338,#62339,#62340,#62341,#62342,#62343,#62344,
#62345,#62346,#62347,#62348,#62349,#62350,#62351,#62352,#62353,#62354,#62355,
#62356,#62357,#62358,#62359,#62360,#62361,#62362,#62363,#62364,#62365,#62366,
#62367,#62368,#62369,#62370,#62371,#62372,#62373,#62374,#62375,#62376,#62377,
#62378,#62379,#62380,#62381,#62382,#62383,#62384,#62385,#62386,#62387,#62388,
#62389,#62390),.UNSPECIFIED.,.F.,.F.,(4,3,3,3,3,3,3,3,3,3,3,3,3,3,3,3,3,
3,3,3,3,3,3,3,4),(13.5490822577306,13.6444249231416,13.7372107374818,13.8299755857438,
13.9227442480459,14.0200140812891,14.1129202918713,14.20589203575,14.2990021749612,
14.3118235810189,14.4049182756249,14.4978873068571,14.5907582790323,14.6835618991959,
14.7763306500945,14.8690893301786,14.9618627229779,15.054735542364,15.1476603440171,
15.2407405112384,15.3113387195456,15.4149720236937,15.5182945666206,15.6210595353514,
15.7079632677657),.UNSPECIFIED.);
#7703=B_SPLINE_CURVE_WITH_KNOTS('',3,(#62392,#62393,#62394,#62395,#62396,
#62397,#62398,#62399,#62400,#62401,#62402,#62403,#62404,#62405,#62406,#62407,
#62408,#62409,#62410,#62411,#62412,#62413,#62414,#62415,#62416,#62417,#62418,
#62419,#62420,#62421,#62422,#62423,#62424,#62425,#62426,#62427,#62428,#62429,
#62430,#62431,#62432,#62433,#62434,#62435,#62436,#62437,#62438,#62439,#62440,
#62441,#62442,#62443,#62444,#62445,#62446,#62447,#62448,#62449,#62450,#62451,
#62452,#62453,#62454,#62455,#62456,#62457,#62458,#62459,#62460,#62461,#62462,
#62463,#62464),.UNSPECIFIED.,.F.,.F.,(4,3,3,3,3,3,3,3,3,3,3,3,3,3,3,3,3,
3,3,3,3,3,3,3,4),(13.5481175545326,13.6142445048086,13.7074539898319,13.8005374759601,
13.8935224081086,13.9864387418312,14.079319398333,14.1721890329815,14.2650722854203,
14.358052555288,14.4510836331598,14.5442670228022,14.6137596433353,14.7069979410332,
14.8001132987202,14.8931331061577,14.9860887178402,15.0790113467516,15.1719256083309,
15.264856104453,15.357887418871,15.4509717316316,15.5442114219034,15.6132747818621,
15.7079632679492),.UNSPECIFIED.);
#7704=B_SPLINE_CURVE_WITH_KNOTS('',3,(#62465,#62466,#62467,#62468,#62469,
#62470,#62471,#62472,#62473,#62474,#62475,#62476,#62477,#62478,#62479,#62480,
#62481,#62482,#62483,#62484,#62485,#62486,#62487,#62488,#62489,#62490,#62491,
#62492,#62493,#62494,#62495,#62496,#62497,#62498,#62499,#62500,#62501,#62502,
#62503,#62504,#62505,#62506,#62507,#62508,#62509,#62510,#62511,#62512,#62513,
#62514,#62515,#62516,#62517,#62518,#62519,#62520,#62521,#62522,#62523,#62524,
#62525,#62526,#62527,#62528,#62529,#62530,#62531,#62532,#62533,#62534,#62535,
#62536,#62537,#62538,#62539,#62540,#62541,#62542,#62543,#62544,#62545,#62546,
#62547,#62548,#62549,#62550,#62551,#62552,#62553,#62554,#62555,#62556,#62557,
#62558,#62559,#62560,#62561,#62562,#62563,#62564,#62565,#62566,#62567,#62568,
#62569,#62570,#62571,#62572,#62573,#62574,#62575,#62576,#62577,#62578,#62579,
#62580,#62581,#62582,#62583,#62584,#62585,#62586,#62587,#62588,#62589,#62590,
#62591,#62592,#62593,#62594,#62595,#62596,#62597,#62598,#62599,#62600,#62601,
#62602,#62603),.UNSPECIFIED.,.F.,.F.,(4,3,3,3,3,3,3,3,3,3,3,3,3,3,3,3,3,
3,3,3,3,3,3,3,3,3,3,3,3,3,3,3,3,3,3,3,3,3,3,3,3,3,3,3,3,3,4),(15.7079632682196,
15.7997431632769,15.8914080252224,15.9829843740528,16.0745131018752,16.1660202549873,
16.2575318536328,16.3491336017902,16.4407804137139,16.5325825781659,16.6127899203889,
16.7058910985793,16.7988663175293,16.8917431744402,16.984552195471,17.0773260480196,
17.1700895232903,17.2628673973129,17.3557441784495,17.4486726596649,17.5417560010965,
17.6123050589156,17.7053997604146,17.7983687987123,17.8912397781156,17.9840434057244,
18.076812164199,18.1695708519817,18.262344252594,18.3552170799245,18.448141889607,
18.5412220649159,18.6118201974424,18.7048774940281,18.7978084850565,18.890640828656,
18.9834050917185,19.0761340503132,19.1688525487697,19.2615854161865,19.354417423974,
19.4473011913083,19.5403403836925,19.6113353359692,19.7044230626322,19.7973722083033,
19.8322838807155),.UNSPECIFIED.);
#7705=B_SPLINE_CURVE_WITH_KNOTS('',3,(#62609,#62610,#62611,#62612,#62613,
#62614,#62615,#62616,#62617,#62618,#62619,#62620,#62621,#62622,#62623,#62624,
#62625,#62626,#62627,#62628,#62629,#62630,#62631,#62632,#62633,#62634,#62635,
#62636,#62637,#62638,#62639,#62640,#62641,#62642,#62643,#62644,#62645,#62646,
#62647,#62648,#62649,#62650,#62651,#62652,#62653,#62654,#62655,#62656,#62657,
#62658,#62659,#62660,#62661,#62662,#62663,#62664,#62665,#62666,#62667,#62668,
#62669,#62670,#62671,#62672,#62673,#62674,#62675,#62676,#62677,#62678,#62679,
#62680,#62681,#62682,#62683,#62684,#62685,#62686,#62687,#62688,#62689,#62690,
#62691,#62692,#62693,#62694,#62695,#62696,#62697,#62698,#62699,#62700,#62701,
#62702,#62703,#62704,#62705,#62706,#62707,#62708,#62709,#62710,#62711,#62712,
#62713,#62714,#62715,#62716,#62717,#62718,#62719,#62720,#62721,#62722,#62723,
#62724,#62725,#62726,#62727,#62728,#62729,#62730,#62731,#62732,#62733,#62734,
#62735,#62736,#62737,#62738,#62739,#62740,#62741,#62742,#62743,#62744),
 .UNSPECIFIED.,.F.,.F.,(4,3,3,3,3,3,3,3,3,3,3,3,3,3,3,3,3,3,3,3,3,3,3,3,
3,3,3,3,3,3,3,3,3,3,3,3,3,3,3,3,3,3,3,3,3,4),(21.9911485752977,22.1009390578722,
22.2120192264695,22.307944689233,22.4010201395792,22.4939695339534,22.5868205047926,
22.67960365598,22.7723516570805,22.8650893303511,22.9578414829215,23.0506928288605,
23.1435959940919,23.2366544809095,23.3074598277597,23.4005351530306,23.4934844215758,
23.5863352660045,23.679118290433,23.7718661646011,23.8646037109164,23.9573557366592,
24.0502069567598,24.1431099965046,24.2361683597274,24.3069749662865,24.4000502264934,
24.4929994285521,24.585850205167,24.6786331600566,24.7713809636478,24.8641184384285,
24.9568703917587,25.049721538522,25.1426245043015,25.2356827932911,25.3064901048132,
25.3995782757944,25.4925102707237,25.5853528984435,25.6781310827416,25.7708696868248,
25.8636232533134,25.9563823167374,26.0492200497298,26.1142762800646),
 .UNSPECIFIED.);
#7706=B_SPLINE_CURVE_WITH_KNOTS('',3,(#62745,#62746,#62747,#62748,#62749,
#62750,#62751,#62752,#62753,#62754,#62755,#62756,#62757,#62758,#62759,#62760,
#62761,#62762,#62763,#62764,#62765,#62766,#62767,#62768,#62769,#62770,#62771,
#62772,#62773,#62774,#62775,#62776,#62777,#62778,#62779,#62780,#62781,#62782,
#62783,#62784,#62785,#62786,#62787,#62788,#62789,#62790,#62791,#62792,#62793,
#62794,#62795,#62796,#62797,#62798,#62799,#62800,#62801,#62802,#62803,#62804,
#62805,#62806,#62807,#62808,#62809,#62810,#62811,#62812,#62813,#62814,#62815,
#62816,#62817),.UNSPECIFIED.,.F.,.F.,(4,3,3,3,3,3,3,3,3,3,3,3,3,3,3,3,3,
3,3,3,3,3,3,3,4),(19.8316169097465,19.9243614290183,20.0204996748086,20.1133834001034,
20.2111489061414,20.3089144121794,20.4019899358734,20.4949394080688,20.5877904610795,
20.6805737006823,20.7733217940077,20.8660595632167,20.9588118153459,21.0516632658938,
21.1445665387003,21.2376251368815,21.3084295507062,21.4011773356687,21.4938045011336,
21.5863363897949,21.67879825315,21.7712257642586,21.8636335735842,21.9560698252548,
21.9911485751289),.UNSPECIFIED.);
#7707=B_SPLINE_CURVE_WITH_KNOTS('',3,(#62819,#62820,#62821,#62822,#62823,
#62824,#62825,#62826,#62827,#62828,#62829,#62830,#62831,#62832,#62833,#62834,
#62835,#62836,#62837,#62838,#62839,#62840,#62841,#62842,#62843,#62844,#62845,
#62846,#62847,#62848,#62849,#62850,#62851,#62852,#62853,#62854,#62855,#62856,
#62857,#62858,#62859,#62860,#62861,#62862,#62863,#62864,#62865,#62866,#62867,
#62868,#62869,#62870,#62871,#62872,#62873,#62874,#62875,#62876,#62877,#62878,
#62879,#62880,#62881,#62882,#62883,#62884,#62885,#62886,#62887,#62888,#62889,
#62890,#62891),.UNSPECIFIED.,.F.,.F.,(4,3,3,3,3,3,3,3,3,3,3,3,3,3,3,3,3,
3,3,3,3,3,3,3,4),(19.8322838807155,19.9296047049381,20.0223747342139,20.1151201566221,
20.2078657798381,20.3006364048605,20.3935117970783,20.4864484588977,20.5795288783454,
20.6108504744959,20.7039279435914,20.796879404527,20.8897324867605,20.9825178083623,
21.0752680154586,21.1680079278048,21.2607623500554,21.353615999483,21.446521490569,
21.5395823160024,21.6103656130227,21.7152591306476,21.8197981287288,21.9237013079083,
21.9911485749378),.UNSPECIFIED.);
#7708=B_SPLINE_CURVE_WITH_KNOTS('',3,(#62892,#62893,#62894,#62895,#62896,
#62897,#62898,#62899,#62900,#62901,#62902,#62903,#62904,#62905,#62906,#62907,
#62908,#62909,#62910,#62911,#62912,#62913,#62914,#62915,#62916,#62917,#62918,
#62919,#62920,#62921,#62922,#62923,#62924,#62925,#62926,#62927,#62928,#62929,
#62930,#62931,#62932,#62933,#62934,#62935,#62936,#62937,#62938,#62939,#62940,
#62941,#62942,#62943,#62944,#62945,#62946,#62947,#62948,#62949,#62950,#62951,
#62952,#62953,#62954,#62955,#62956,#62957,#62958,#62959,#62960,#62961,#62962,
#62963,#62964,#62965,#62966,#62967,#62968,#62969,#62970,#62971,#62972,#62973,
#62974,#62975,#62976,#62977,#62978,#62979,#62980,#62981,#62982,#62983,#62984,
#62985,#62986,#62987,#62988,#62989,#62990,#62991,#62992,#62993,#62994,#62995,
#62996,#62997,#62998,#62999,#63000,#63001,#63002,#63003,#63004,#63005,#63006,
#63007,#63008,#63009,#63010,#63011,#63012,#63013,#63014,#63015,#63016,#63017,
#63018,#63019,#63020,#63021,#63022,#63023,#63024,#63025,#63026,#63027,#63028,
#63029,#63030),.UNSPECIFIED.,.F.,.F.,(4,3,3,3,3,3,3,3,3,3,3,3,3,3,3,3,3,
3,3,3,3,3,3,3,3,3,3,3,3,3,3,3,3,3,3,3,3,3,3,3,3,3,3,3,3,3,4),(21.9911485751288,
22.0847067914567,22.1782793405872,22.2718895786102,22.3656265377757,22.4594329192013,
22.5534084578545,22.6098807515494,22.7029569153201,22.7959070291147,22.8887587243788,
22.9815426045203,23.0742913371258,23.1670297435889,23.2597826301769,23.3526347068616,
23.4455386021667,23.5385978103277,23.6093958900762,23.702471413893,23.7954208862163,
23.8882719393601,23.9810551791027,24.0738032725722,24.1665410419292,24.2592932942106,
24.3521447449158,24.4450480178827,24.5381066162279,24.608911028603,24.7019859816036,
24.79493487186,24.8877853325149,24.9805679664762,25.0733154461881,25.166052594514,
25.2588042191871,25.3516550358887,25.4445576703103,25.5376156292532,25.6084261671297,
25.7015007924706,25.7944540138807,25.8872964718783,25.9800748558386,26.0728176554707,
26.1148515779882),.UNSPECIFIED.);
#7709=B_SPLINE_CURVE_WITH_KNOTS('',3,(#63036,#63037,#63038,#63039,#63040,
#63041,#63042,#63043,#63044,#63045,#63046,#63047,#63048,#63049,#63050,#63051,
#63052,#63053,#63054,#63055,#63056,#63057,#63058,#63059,#63060,#63061,#63062,
#63063,#63064,#63065,#63066,#63067,#63068,#63069,#63070,#63071,#63072,#63073,
#63074,#63075,#63076,#63077,#63078,#63079,#63080,#63081,#63082,#63083,#63084,
#63085,#63086,#63087,#63088,#63089,#63090,#63091,#63092,#63093,#63094,#63095,
#63096,#63097,#63098,#63099,#63100,#63101,#63102,#63103,#63104,#63105,#63106,
#63107,#63108,#63109,#63110,#63111,#63112,#63113,#63114,#63115,#63116,#63117,
#63118,#63119,#63120,#63121,#63122,#63123,#63124,#63125,#63126,#63127,#63128,
#63129,#63130,#63131,#63132,#63133,#63134,#63135,#63136,#63137,#63138,#63139,
#63140,#63141,#63142,#63143,#63144,#63145,#63146,#63147,#63148,#63149,#63150,
#63151,#63152,#63153,#63154,#63155,#63156,#63157,#63158,#63159,#63160,#63161,
#63162,#63163,#63164,#63165,#63166,#63167,#63168,#63169,#63170,#63171,#63172,
#63173,#63174),.UNSPECIFIED.,.F.,.F.,(4,3,3,3,3,3,3,3,3,3,3,3,3,3,3,3,3,
3,3,3,3,3,3,3,3,3,3,3,3,3,3,3,3,3,3,3,3,3,3,3,3,3,3,3,3,3,4),(28.2743338823085,
28.3050355203935,28.3981108323836,28.4910600870279,28.583910916957,28.6766939260394,
28.7694417843463,28.8621793143023,28.9549313232044,29.0477825258147,29.1406855476817,
29.2337438925711,29.3045506589203,29.3976259671484,29.4905752179945,29.5834260440944,
29.6762090493171,29.7689569037467,29.8616944298121,29.9544464348151,30.0472976335374,
30.1402006515163,30.2332589925582,30.3040657974471,30.3971411050901,30.4900903553313,
30.5829411808073,30.6757241853799,30.7684720391435,30.861209564528,30.9539615688355,
31.0468127668442,31.1397157840982,31.2327741244043,31.3035809359738,31.3966562449754,
31.4896054965963,31.5824563234711,31.6752393294658,31.7679871846652,31.8607247114976,
31.9534767172635,32.0463279167379,32.1392309354639,32.2322892772372,32.3030960745006,
32.398493560417),.UNSPECIFIED.);
#7710=B_SPLINE_CURVE_WITH_KNOTS('',3,(#63175,#63176,#63177,#63178,#63179,
#63180,#63181,#63182,#63183,#63184,#63185,#63186,#63187,#63188,#63189,#63190,
#63191,#63192,#63193,#63194,#63195,#63196,#63197,#63198,#63199,#63200,#63201,
#63202,#63203,#63204,#63205,#63206,#63207,#63208,#63209,#63210,#63211,#63212,
#63213,#63214,#63215,#63216,#63217,#63218,#63219,#63220,#63221,#63222,#63223,
#63224,#63225,#63226,#63227,#63228,#63229,#63230,#63231,#63232,#63233,#63234,
#63235,#63236,#63237,#63238,#63239,#63240,#63241,#63242,#63243,#63244,#63245,
#63246,#63247),.UNSPECIFIED.,.F.,.F.,(4,3,3,3,3,3,3,3,3,3,3,3,3,3,3,3,3,
3,3,3,3,3,3,3,4),(26.1142762800646,26.2101407617023,26.30600524334,26.3990805521692,
26.4920298036781,26.5848806305009,26.6776636365352,26.7704114918303,26.8631490188147,
26.9559010247892,27.048752224559,27.1416552436292,27.2347135858238,27.3055203818668,
27.398127088502,27.4906081096177,27.5829916645036,27.6753091644605,27.7675934136574,
27.8598697536049,27.9521635127291,28.0445556641859,28.137003309307,28.2295960455401,
28.2743338820371),.UNSPECIFIED.);
#7711=B_SPLINE_CURVE_WITH_KNOTS('',3,(#63249,#63250,#63251,#63252,#63253,
#63254,#63255,#63256,#63257,#63258,#63259,#63260,#63261,#63262,#63263,#63264,
#63265,#63266,#63267,#63268,#63269,#63270,#63271,#63272,#63273,#63274,#63275,
#63276,#63277,#63278,#63279,#63280,#63281,#63282,#63283,#63284,#63285,#63286,
#63287,#63288,#63289,#63290,#63291,#63292,#63293,#63294,#63295,#63296,#63297,
#63298,#63299,#63300,#63301,#63302,#63303,#63304,#63305,#63306,#63307,#63308,
#63309,#63310,#63311,#63312,#63313,#63314,#63315,#63316,#63317,#63318,#63319,
#63320,#63321,#63322,#63323,#63324),.UNSPECIFIED.,.F.,.F.,(4,3,3,3,3,3,
3,3,3,3,3,3,3,3,3,3,3,3,3,3,3,3,3,3,3,4),(26.1148515779882,26.2075927385225,
26.3003596186431,26.3932316639966,26.48616563344,26.5792426776218,26.6079413056565,
26.7010166309318,26.793965899482,26.8868167439165,26.9795997683517,27.0723476425272,
27.1650851888503,27.257837214602,27.3506884347121,27.4435914744667,27.5366498377001,
27.6074564441833,27.7004615096694,27.7933436061491,27.8861277750852,27.983179301891,
28.0758475566346,28.1684942988224,28.2611592745444,28.2743338823084),
 .UNSPECIFIED.);
#7712=B_SPLINE_CURVE_WITH_KNOTS('',3,(#63325,#63326,#63327,#63328,#63329,
#63330,#63331,#63332,#63333,#63334,#63335,#63336,#63337,#63338,#63339,#63340,
#63341,#63342,#63343,#63344,#63345,#63346,#63347,#63348,#63349,#63350,#63351,
#63352,#63353,#63354,#63355,#63356,#63357,#63358,#63359,#63360,#63361,#63362,
#63363,#63364,#63365,#63366,#63367,#63368,#63369,#63370,#63371,#63372,#63373,
#63374,#63375,#63376,#63377,#63378,#63379,#63380,#63381,#63382,#63383,#63384,
#63385,#63386,#63387,#63388,#63389,#63390,#63391,#63392,#63393,#63394,#63395,
#63396,#63397,#63398,#63399,#63400,#63401,#63402,#63403,#63404,#63405,#63406,
#63407,#63408,#63409,#63410,#63411,#63412,#63413,#63414,#63415,#63416,#63417,
#63418,#63419,#63420,#63421,#63422,#63423,#63424,#63425,#63426,#63427,#63428,
#63429,#63430,#63431,#63432,#63433,#63434,#63435,#63436,#63437,#63438,#63439,
#63440,#63441,#63442,#63443,#63444,#63445,#63446,#63447,#63448,#63449,#63450,
#63451,#63452,#63453,#63454,#63455,#63456,#63457,#63458,#63459,#63460,#63461,
#63462,#63463,#63464,#63465,#63466,#63467,#63468,#63469,#63470,#63471,#63472,
#63473,#63474,#63475,#63476,#63477,#63478,#63479,#63480,#63481,#63482,#63483,
#63484,#63485,#63486),.UNSPECIFIED.,.F.,.F.,(4,2,2,2,2,2,2,2,2,2,2,2,2,
2,2,2,2,2,2,2,2,2,2,2,2,2,2,2,2,2,2,2,2,2,2,2,2,2,2,2,2,2,2,2,2,2,2,2,2,
2,2,2,2,2,2,2,2,2,2,2,2,2,2,2,2,2,2,2,2,2,2,2,2,2,2,2,2,2,2,2,4),(-4.06009964275302,
-3.97992804425977,-3.96517398667009,-3.95678377382771,-3.95452870825207,
-3.9531780547404,-3.95196135775498,-3.95038794534511,-3.94698733061644,
-3.91886649491486,-3.91045137537565,-3.85776107645835,-3.82255752159171,
-3.80754592901665,-3.79758773386062,-3.79413282759724,-3.79210932390034,
-3.78993640432826,-3.78714302821738,-3.78266268571291,-3.75832162644589,
-3.70528286411963,-3.66421138389992,-3.64457413495014,-3.63430714257539,
-3.63189422565866,-3.63050841326076,-3.62929859484687,-3.62775822086802,
-3.62471682384807,-3.60590243236951,-3.5725571285863,-3.48761628522174,
-3.47943881250414,-3.47327952724946,-3.47042080337634,-3.46836213818299,
-3.46632966626124,-3.46357617879369,-3.45819033677073,-3.39359557716868,
-3.31963054963236,-3.31109910549482,-3.30883090241771,-3.30747727247695,
-3.30626125705462,-3.30469314677703,-3.30132078000891,-3.2742951446889,
-3.18912983371585,-3.16632631665581,-3.15261180098397,-3.14870379115348,
-3.1463089258773,-3.14413616406669,-3.14134342034613,-3.13686495810699,
-3.11255043628448,-3.10990108166594,-3.09652553009939,-3.09486150594946,
-3.09394210084471,-3.01861394134868,-2.9988052292843,-2.9884762911639,-2.98605865522537,
-2.98467177976948,-2.98346207776363,-2.9819232178282,-2.97878652000038,
-2.95864089803314,-2.86592438364308,-2.84329961633336,-2.82966428311039,
-2.82576435743104,-2.82337134818679,-2.82119823648568,-2.81840219482107,
-2.81260245303326,-2.73661235803911,-2.72814588356085),.UNSPECIFIED.);
#7713=B_SPLINE_CURVE_WITH_KNOTS('',3,(#63492,#63493,#63494,#63495,#63496,
#63497,#63498,#63499,#63500,#63501,#63502,#63503,#63504,#63505,#63506,#63507,
#63508,#63509,#63510,#63511,#63512,#63513,#63514,#63515,#63516,#63517,#63518,
#63519,#63520,#63521,#63522,#63523,#63524,#63525,#63526,#63527,#63528,#63529,
#63530,#63531,#63532,#63533,#63534,#63535,#63536,#63537,#63538,#63539,#63540,
#63541,#63542,#63543,#63544,#63545,#63546,#63547,#63548,#63549,#63550,#63551,
#63552,#63553,#63554,#63555,#63556,#63557,#63558,#63559,#63560,#63561,#63562,
#63563,#63564,#63565,#63566,#63567,#63568,#63569,#63570,#63571,#63572,#63573,
#63574,#63575,#63576,#63577,#63578,#63579,#63580,#63581,#63582,#63583,#63584,
#63585,#63586,#63587,#63588,#63589,#63590,#63591,#63592,#63593,#63594,#63595,
#63596,#63597,#63598,#63599,#63600,#63601,#63602,#63603,#63604,#63605,#63606,
#63607,#63608,#63609,#63610,#63611,#63612,#63613,#63614,#63615,#63616,#63617,
#63618,#63619,#63620,#63621,#63622,#63623,#63624,#63625,#63626,#63627),
 .UNSPECIFIED.,.F.,.F.,(4,3,3,3,3,3,3,3,3,3,3,3,3,3,3,3,3,3,3,3,3,3,3,3,
3,3,3,3,3,3,3,3,3,3,3,3,3,3,3,3,3,3,3,3,3,4),(34.557519189488,34.6505344770621,
34.7422837385077,34.8340075184537,34.9257316641358,35.0197091206221,35.1115640588596,
35.2066027744702,35.3016414900809,35.3947167985334,35.4876660495984,35.5805168759114,
35.6732998813377,35.7660477359647,35.8587852622214,35.951537267409,36.0443884663047,
36.1372914844509,36.2303498256485,36.3011566286076,36.3942319370643,36.4871811881334,
36.5800320144501,36.6728150198798,36.7655628745103,36.8583004007699,36.951052405961,
37.0439036048593,37.136806623008,37.2298649642077,37.3006717671344,37.3937470756148,
37.486696326708,37.5795471530493,37.672330158504,37.7650780131595,37.8578155394447,
37.9505675446612,38.0434187435853,38.1363217617599,38.2293801029855,38.3001869056612,
38.3955381070791,38.4884751037719,38.5850334075524,38.6815917113328),
 .UNSPECIFIED.);
#7714=B_SPLINE_CURVE_WITH_KNOTS('',3,(#63628,#63629,#63630,#63631,#63632,
#63633,#63634,#63635,#63636,#63637,#63638,#63639,#63640,#63641,#63642,#63643,
#63644,#63645,#63646,#63647,#63648,#63649,#63650,#63651,#63652,#63653,#63654,
#63655,#63656,#63657,#63658,#63659,#63660,#63661,#63662,#63663,#63664,#63665,
#63666,#63667,#63668,#63669,#63670,#63671,#63672,#63673,#63674,#63675,#63676,
#63677,#63678,#63679,#63680,#63681,#63682,#63683,#63684,#63685,#63686,#63687,
#63688,#63689,#63690,#63691,#63692,#63693,#63694,#63695,#63696,#63697,#63698,
#63699,#63700),.UNSPECIFIED.,.F.,.F.,(4,3,3,3,3,3,3,3,3,3,3,3,3,3,3,3,3,
3,3,3,3,3,3,3,4),(32.398493560417,32.4914400181045,32.584288739484,32.6770705647979,
32.7698178594356,32.862555445206,32.9553081292875,33.0481603497384,33.1410649461116,
33.234124163174,33.3026112130273,33.3956865213933,33.48863577237,33.5814865985929,
33.6742696039268,33.7670174584601,33.859754984622,33.9525069897136,34.0453581885121,
34.1382612065603,34.2313195476595,34.3021263515541,34.4230279815628,34.5413368973612,
34.5575191892658),.UNSPECIFIED.);
#7715=B_SPLINE_CURVE_WITH_KNOTS('',3,(#63701,#63702,#63703,#63704,#63705,
#63706,#63707,#63708,#63709,#63710,#63711,#63712,#63713,#63714,#63715,#63716,
#63717,#63718,#63719,#63720,#63721,#63722,#63723,#63724,#63725,#63726,#63727,
#63728,#63729,#63730,#63731,#63732,#63733,#63734,#63735,#63736,#63737,#63738,
#63739,#63740,#63741,#63742,#63743,#63744,#63745,#63746,#63747,#63748,#63749,
#63750,#63751,#63752,#63753,#63754,#63755,#63756,#63757,#63758,#63759,#63760,
#63761,#63762,#63763,#63764,#63765,#63766,#63767,#63768,#63769,#63770,#63771,
#63772,#63773,#63774,#63775,#63776,#63777,#63778,#63779,#63780,#63781,#63782,
#63783,#63784,#63785,#63786,#63787,#63788,#63789,#63790,#63791,#63792,#63793,
#63794,#63795,#63796,#63797,#63798,#63799,#63800,#63801,#63802,#63803,#63804,
#63805,#63806,#63807,#63808,#63809,#63810,#63811,#63812,#63813,#63814,#63815,
#63816,#63817,#63818,#63819,#63820,#63821,#63822,#63823,#63824,#63825,#63826,
#63827,#63828,#63829,#63830,#63831,#63832,#63833,#63834,#63835,#63836,#63837,
#63838,#63839,#63840,#63841,#63842,#63843,#63844,#63845,#63846,#63847,#63848,
#63849,#63850,#63851,#63852,#63853,#63854,#63855,#63856,#63857,#63858,#63859,
#63860,#63861,#63862,#63863,#63864,#63865,#63866,#63867,#63868,#63869,#63870,
#63871,#63872,#63873,#63874,#63875,#63876,#63877,#63878,#63879,#63880,#63881,
#63882,#63883,#63884,#63885,#63886,#63887,#63888,#63889,#63890,#63891,#63892,
#63893,#63894,#63895,#63896,#63897,#63898,#63899,#63900,#63901,#63902,#63903,
#63904,#63905,#63906,#63907,#63908,#63909,#63910,#63911,#63912,#63913,#63914,
#63915,#63916,#63917,#63918,#63919,#63920,#63921,#63922,#63923,#63924,#63925,
#63926,#63927,#63928,#63929,#63930,#63931,#63932,#63933,#63934,#63935,#63936,
#63937,#63938,#63939,#63940,#63941,#63942,#63943,#63944,#63945,#63946,#63947,
#63948,#63949,#63950),.UNSPECIFIED.,.F.,.F.,(4,2,2,2,2,2,2,2,2,2,2,2,2,
2,2,2,2,2,2,2,2,2,2,2,2,2,2,2,2,2,2,2,2,2,2,2,2,2,2,2,2,2,2,2,2,2,2,2,2,
2,2,2,2,2,2,2,2,2,2,2,2,2,2,2,2,2,2,2,2,2,2,2,2,2,2,2,2,2,2,2,2,2,2,2,2,
2,2,2,2,2,2,2,2,2,2,2,2,2,2,2,2,2,2,2,2,2,2,2,2,2,2,2,2,2,2,2,2,2,2,2,2,
2,2,2,4),(-2.72814588356085,-2.69177019645693,-2.67469536912849,-2.6653842791166,
-2.66304772262018,-2.66167889882582,-2.66046631150317,-2.65889895582188,
-2.65561775181486,-2.63158790163194,-2.62226201497484,-2.58316380457146,
-2.53923007112731,-2.50878040828248,-2.50381151041301,-2.50118462972761,
-2.49923549235549,-2.49680525591804,-2.49273872662273,-2.48427542112654,
-2.39726184509183,-2.37454583812146,-2.35350537375744,-2.3427389936437,
-2.34028905285507,-2.33889500416378,-2.33768617044934,-2.33615765294834,
-2.3331718265721,-2.31558103914529,-2.3114885611968,-2.21984808954366,-2.19740622093779,
-2.18385187173493,-2.17996005560742,-2.17756878509788,-2.17539512226456,
-2.17259538194739,-2.16677713791361,-2.12156670703388,-2.05122762924548,
-2.03046261082839,-2.02873442653731,-2.01974902820571,-2.01735889172253,
-2.01596410454751,-2.01475542108896,-2.01322811613195,-2.01014890330072,
-1.98368475041267,-1.93598780387023,-1.86441515715643,-1.8585190716148,
-1.85573432728855,-1.85355637139788,-1.8511808486918,-1.84735993970525,
-1.83448580519281,-1.81355154928986,-1.73889503830003,-1.7219793371213,
-1.69829405485457,-1.69502441251635,-1.69345924589282,-1.69224683121482,
-1.69087653377583,-1.68853364736509,-1.67914819348075,-1.66188264541755,
-1.61609963980977,-1.5414427893468,-1.53560596690257,-1.53280254004759,
-1.53062834547738,-1.52823883758531,-1.52435515703171,-1.51088134676842,
-1.48861763988004,-1.39802364593873,-1.39223862795602,-1.3749313452562,
-1.37196007320653,-1.37043463216816,-1.36922597841465,-1.36782958747718,
-1.36536929923475,-1.35445976583099,-1.33301233667467,-1.281722969468,-1.21874264275385,
-1.21334850096477,-1.21059263099112,-1.20855930969112,-1.20635326583741,
-1.20334556885714,-1.19640858621183,-1.12672517474231,-1.08757374952794,
-1.07608608943866,-1.05245554303779,-1.04918756186492,-1.04762263744003,
-1.04641015718119,-1.0450395089811,-1.04269538767841,-1.03329678168576,
-1.01599754217349,-0.97008734354019,-0.895598191242403,-0.889757955984397,
-0.886953712970418,-0.884779250325259,-0.882389815124442,-0.878507075747928,
-0.86504464698163,-0.842807184137572,-0.752802436087622,-0.729463685135623,
-0.726205556361693,-0.724642475779657,-0.723430104813524,-0.722058136793483,
-0.719755606108128,-0.710772727979108,-0.698275120787947),.UNSPECIFIED.);
#7716=B_SPLINE_CURVE_WITH_KNOTS('',3,(#63956,#63957,#63958,#63959,#63960,
#63961,#63962,#63963),.UNSPECIFIED.,.F.,.F.,(4,1,1,1,1,4),(40.8407078890674,
41.2987323212414,42.2982474597682,43.297762598295,44.2972777368217,44.9636567851415),
 .UNSPECIFIED.);
#7717=B_SPLINE_CURVE_WITH_KNOTS('',3,(#63964,#63965,#63966,#63967,#63968,
#63969,#63970,#63971,#63972,#63973,#63974,#63975,#63976,#63977,#63978,#63979,
#63980,#63981,#63982,#63983,#63984,#63985,#63986,#63987,#63988,#63989,#63990,
#63991,#63992,#63993,#63994,#63995,#63996,#63997,#63998,#63999,#64000,#64001,
#64002,#64003,#64004,#64005,#64006,#64007,#64008,#64009,#64010,#64011,#64012,
#64013,#64014,#64015,#64016,#64017,#64018,#64019,#64020,#64021,#64022,#64023,
#64024,#64025,#64026,#64027,#64028,#64029,#64030,#64031,#64032,#64033,#64034,
#64035,#64036),.UNSPECIFIED.,.F.,.F.,(4,3,3,3,3,3,3,3,3,3,3,3,3,3,3,3,3,
3,3,3,3,3,3,3,4),(38.6815917113328,38.7743373141285,38.8670751954702,38.9598301622261,
39.0526857539774,39.1455955076823,39.2386576504075,39.2997020441879,39.3927773526555,
39.4857266037357,39.578577430063,39.6713604355043,39.7641082901464,39.8568458164183,
39.9495978216212,40.0424490205317,40.1353520386925,40.2284103799043,40.2992171827147,
40.3954403882719,40.4915029124347,40.5873785224333,40.6831438364891,40.7787909004466,
40.8407044966676),.UNSPECIFIED.);
#7718=B_SPLINE_CURVE_WITH_KNOTS('',3,(#64038,#64039,#64040,#64041,#64042,
#64043,#64044,#64045,#64046,#64047,#64048,#64049,#64050,#64051,#64052,#64053,
#64054,#64055,#64056,#64057,#64058,#64059,#64060,#64061,#64062,#64063,#64064,
#64065,#64066,#64067,#64068,#64069,#64070,#64071,#64072,#64073,#64074,#64075,
#64076,#64077,#64078,#64079,#64080,#64081,#64082,#64083,#64084,#64085,#64086,
#64087,#64088,#64089,#64090,#64091,#64092,#64093,#64094,#64095,#64096,#64097,
#64098,#64099,#64100,#64101,#64102,#64103,#64104,#64105,#64106,#64107,#64108,
#64109,#64110,#64111,#64112,#64113,#64114,#64115,#64116,#64117,#64118,#64119,
#64120,#64121,#64122,#64123),.UNSPECIFIED.,.F.,.F.,(4,2,2,2,2,2,2,2,2,2,
2,2,2,2,2,2,2,2,2,2,2,2,2,2,2,2,2,2,2,2,2,2,2,2,2,2,2,2,2,2,2,2,4),(-0.698275120787947,
-0.694481754168329,-0.65359834429961,-0.578887684233614,-0.576569126139477,
-0.568139734998153,-0.564785870407424,-0.562739283312044,-0.560542299228753,
-0.55758817756562,-0.551187301956559,-0.518818663659694,-0.456087107595393,
-0.407076956377958,-0.40346512407881,-0.401852332517518,-0.40062951497057,
-0.399297883999417,-0.397128777122514,-0.39078755961723,-0.380253630449211,
-0.342088828524308,-0.30547068583101,-0.249936696390069,-0.244560221483311,
-0.241808730477856,-0.239776381400394,-0.237569209632325,-0.234556060611483,
-0.23122828167922,-0.209077898377296,-0.177515406120868,-0.150746248996183,
-0.112175633548954,-0.083931029342986,-0.0805266912655971,-0.0789523815532209,
-0.0777353548320273,-0.0763847196102382,-0.0749803046708111,-0.0728817699842837,
-0.0690783852891989,-0.000960649026662135),.UNSPECIFIED.);
#7719=B_SPLINE_CURVE_WITH_KNOTS('',3,(#64124,#64125,#64126,#64127,#64128,
#64129,#64130,#64131,#64132,#64133,#64134,#64135,#64136,#64137,#64138,#64139,
#64140,#64141,#64142,#64143,#64144,#64145,#64146,#64147,#64148,#64149,#64150,
#64151,#64152,#64153,#64154,#64155,#64156,#64157,#64158,#64159,#64160,#64161,
#64162,#64163,#64164,#64165,#64166,#64167,#64168,#64169,#64170,#64171,#64172,
#64173,#64174,#64175,#64176,#64177,#64178,#64179,#64180,#64181,#64182,#64183,
#64184,#64185,#64186,#64187,#64188,#64189,#64190,#64191,#64192,#64193,#64194,
#64195,#64196,#64197,#64198,#64199,#64200,#64201,#64202,#64203,#64204,#64205,
#64206,#64207,#64208,#64209,#64210,#64211,#64212,#64213,#64214,#64215,#64216,
#64217,#64218,#64219,#64220,#64221,#64222,#64223,#64224,#64225,#64226,#64227,
#64228,#64229,#64230,#64231,#64232,#64233,#64234,#64235,#64236,#64237,#64238,
#64239,#64240,#64241,#64242,#64243,#64244,#64245,#64246,#64247,#64248,#64249,
#64250,#64251,#64252,#64253,#64254,#64255,#64256,#64257,#64258,#64259,#64260,
#64261,#64262,#64263,#64264,#64265,#64266,#64267,#64268,#64269,#64270,#64271,
#64272,#64273,#64274,#64275,#64276,#64277,#64278,#64279,#64280,#64281,#64282,
#64283,#64284,#64285,#64286,#64287,#64288,#64289,#64290,#64291,#64292,#64293),
 .UNSPECIFIED.,.F.,.F.,(4,2,2,2,2,2,2,2,2,2,2,2,2,2,2,2,2,2,2,2,2,2,2,2,
2,2,2,2,2,2,2,2,2,2,2,2,2,2,2,2,2,2,2,2,2,2,2,2,2,2,2,2,2,2,2,2,2,2,2,2,
2,2,2,2,2,2,2,2,2,2,2,2,2,2,2,2,2,2,2,2,2,2,2,2,4),(-4.0612507056947,-3.99202977575391,
-3.98577881057836,-3.98222911984111,-3.97979640459323,-3.97742408197083,
-3.97524503370926,-3.97245334071522,-3.96652141533724,-3.89685826979705,
-3.86584932583547,-3.8236133732283,-3.81861094457848,-3.81717794025091,
-3.8158073704685,-3.81459495984103,-3.81303013495953,-3.8097623808746,-3.7861333078054,
-3.77473796988285,-3.7542447443314,-3.71336236918133,-3.6797773212617,-3.66791235714937,
-3.65962581215465,-3.65713960343181,-3.65473005278243,-3.6525601792093,
-3.64979354641334,-3.6454015300522,-3.62249741686864,-3.61044938039733,
-3.5968227551182,-3.54055228905148,-3.5022385741652,-3.49630373938915,-3.4942794784051,
-3.49293703422616,-3.49171784914348,-3.49012803862183,-3.48745817868347,
-3.47097173587069,-3.46779248679077,-3.43521151009245,-3.35011627573823,
-3.33783876516051,-3.33409499609949,-3.3317195680478,-3.32954142462936,
-3.32675606230569,-3.32085724289751,-3.27111715895282,-3.2322756078014,
-3.19641892663022,-3.18194008908594,-3.17366279865676,-3.17141824798157,
-3.17006989349282,-3.16885249613876,-3.16727450776883,-3.16464470905579,
-3.14895241260511,-3.05240067973554,-3.0291282786678,-3.01520770265688,
-3.0112791872356,-3.0088798054648,-3.00670819738217,-3.00392425108982,-2.99947457783985,
-2.97561243519846,-2.97408799060702,-2.97263934896084,-2.95434332048045,
-2.88206334934274,-2.86162985528179,-2.85107770609007,-2.84864352035311,
-2.84725302616619,-2.84604387431351,-2.84451053707853,-2.84150191877917,
-2.82340927730233,-2.72895044739071,-2.72876388076409),.UNSPECIFIED.);
#7720=B_SPLINE_CURVE_WITH_KNOTS('',3,(#64299,#64300,#64301,#64302,#64303,
#64304,#64305,#64306,#64307,#64308,#64309,#64310,#64311,#64312,#64313,#64314,
#64315,#64316,#64317,#64318,#64319,#64320,#64321,#64322,#64323,#64324,#64325,
#64326,#64327,#64328,#64329,#64330,#64331,#64332,#64333,#64334,#64335,#64336,
#64337,#64338,#64339,#64340,#64341,#64342,#64343,#64344,#64345,#64346,#64347,
#64348,#64349,#64350,#64351,#64352,#64353,#64354,#64355,#64356,#64357,#64358,
#64359,#64360,#64361,#64362,#64363,#64364,#64365,#64366,#64367,#64368,#64369,
#64370,#64371,#64372,#64373,#64374,#64375,#64376,#64377,#64378,#64379,#64380,
#64381,#64382,#64383,#64384,#64385,#64386,#64387,#64388,#64389,#64390,#64391,
#64392,#64393,#64394,#64395,#64396,#64397,#64398,#64399,#64400,#64401,#64402,
#64403,#64404,#64405,#64406,#64407,#64408,#64409,#64410,#64411,#64412,#64413,
#64414,#64415,#64416,#64417,#64418,#64419,#64420,#64421,#64422,#64423,#64424,
#64425,#64426,#64427,#64428,#64429,#64430,#64431,#64432,#64433,#64434,#64435,
#64436,#64437),.UNSPECIFIED.,.F.,.F.,(4,3,3,3,3,3,3,3,3,3,3,3,3,3,3,3,3,
3,3,3,3,3,3,3,3,3,3,3,3,3,3,3,3,3,3,3,3,3,3,3,3,3,3,3,3,3,4),(47.1238898038472,
47.2690103312467,47.295823152402,47.3888984608709,47.4818477119524,47.5746985382818,
47.6674815437246,47.7602293983682,47.8529669246414,47.9457189298455,48.0385701287575,
48.1314731469199,48.2245314881333,48.2953382909288,48.3884135993978,48.4813628504793,
48.5742136768088,48.6669966822516,48.7597445368951,48.8524820631684,48.9452340683726,
49.0380852672846,49.1309882854469,49.2240466266604,49.2948534294556,49.3879287379245,
49.4808779890061,49.5737288153355,49.6665118207783,49.7592596754218,49.8519972016951,
49.9447492068992,50.0376004058112,50.1305034239736,50.2235617651871,50.2943685679823,
50.3874468243774,50.480398265598,50.5762688023673,50.6690483864422,50.7617925555681,
50.8545261311983,50.9472739191532,51.0401081233949,51.1329944299035,51.2260053885434,
51.2473625597526),.UNSPECIFIED.);
#7721=B_SPLINE_CURVE_WITH_KNOTS('',3,(#64438,#64439,#64440,#64441,#64442,
#64443),.UNSPECIFIED.,.F.,.F.,(4,1,1,4),(44.9636567851415,45.2967928753485,
46.2963080138753,47.1238839646002),.UNSPECIFIED.);
#7722=B_SPLINE_CURVE_WITH_KNOTS('',3,(#64444,#64445,#64446,#64447,#64448,
#64449,#64450,#64451,#64452,#64453,#64454,#64455,#64456,#64457,#64458,#64459,
#64460,#64461,#64462,#64463,#64464,#64465,#64466,#64467,#64468,#64469,#64470,
#64471,#64472,#64473,#64474,#64475,#64476,#64477,#64478,#64479,#64480,#64481,
#64482,#64483,#64484,#64485,#64486,#64487,#64488,#64489,#64490,#64491,#64492,
#64493,#64494,#64495,#64496,#64497,#64498,#64499,#64500,#64501,#64502,#64503,
#64504,#64505,#64506,#64507,#64508,#64509,#64510,#64511,#64512,#64513,#64514,
#64515,#64516,#64517,#64518,#64519,#64520,#64521,#64522,#64523,#64524,#64525,
#64526,#64527,#64528,#64529,#64530,#64531,#64532,#64533,#64534,#64535,#64536,
#64537,#64538,#64539,#64540,#64541,#64542,#64543,#64544,#64545,#64546,#64547,
#64548,#64549,#64550,#64551,#64552,#64553,#64554,#64555,#64556,#64557,#64558,
#64559,#64560,#64561,#64562,#64563,#64564,#64565,#64566,#64567,#64568,#64569,
#64570,#64571,#64572,#64573,#64574,#64575,#64576,#64577,#64578,#64579,#64580,
#64581,#64582,#64583,#64584,#64585,#64586,#64587,#64588,#64589,#64590,#64591,
#64592,#64593,#64594,#64595,#64596,#64597,#64598,#64599,#64600,#64601,#64602,
#64603,#64604,#64605,#64606,#64607,#64608,#64609,#64610,#64611,#64612,#64613,
#64614,#64615,#64616,#64617,#64618,#64619,#64620,#64621,#64622,#64623,#64624,
#64625,#64626,#64627,#64628,#64629,#64630,#64631,#64632,#64633,#64634,#64635,
#64636,#64637,#64638,#64639,#64640,#64641,#64642,#64643,#64644,#64645,#64646,
#64647,#64648,#64649,#64650,#64651,#64652,#64653,#64654,#64655,#64656,#64657,
#64658,#64659,#64660,#64661,#64662,#64663,#64664,#64665,#64666,#64667,#64668,
#64669,#64670,#64671,#64672,#64673,#64674,#64675,#64676,#64677,#64678,#64679,
#64680,#64681,#64682,#64683,#64684,#64685,#64686,#64687,#64688,#64689,#64690,
#64691),.UNSPECIFIED.,.F.,.F.,(4,2,2,2,2,2,2,2,2,2,2,2,2,2,2,2,2,2,2,2,
2,2,2,2,2,2,2,2,2,2,2,2,2,2,2,2,2,2,2,2,2,2,2,2,2,2,2,2,2,2,2,2,2,2,2,2,
2,2,2,2,2,2,2,2,2,2,2,2,2,2,2,2,2,2,2,2,2,2,2,2,2,2,2,2,2,2,2,2,2,2,2,2,
2,2,2,2,2,2,2,2,2,2,2,2,2,2,2,2,2,2,2,2,2,2,2,2,2,2,2,2,2,2,2,4),(-2.72876388076409,
-2.70602756235829,-2.69226073086636,-2.68834769640442,-2.68595185125752,
-2.68377957454858,-2.68098937381791,-2.67521891085425,-2.5980940570774,
-2.53558913764033,-2.52768699829943,-2.52547884152408,-2.52413869965223,
-2.52291909162726,-2.52132535198181,-2.51864161040144,-2.50186592293099,
-2.49699869828275,-2.48767090755633,-2.4445283258113,-2.37305419959333,
-2.36697078421131,-2.36411985033116,-2.36193931598696,-2.3598631099989,
-2.35694252463151,-2.34915560857357,-2.34605591497491,-2.26875091452462,
-2.21225011000985,-2.20472664652994,-2.20255672876644,-2.20122508894515,
-2.20000261584029,-2.19839076081773,-2.19478300369353,-2.15157901288759,
-2.13963522134518,-2.08940052766873,-2.06236063068565,-2.04684165996687,
-2.04276264129758,-2.04032955827826,-2.03816420018406,-2.03543801766571,
-2.03117758609425,-2.00596574729667,-1.9496717496429,-1.88867971437931,
-1.8819080804077,-1.8797373446587,-1.87853822289915,-1.87744802182779,-1.87595362009319,
-1.87303552811591,-1.85260943450499,-1.81963255525067,-1.73231608544955,
-1.72708474619877,-1.72172197231819,-1.71897428525977,-1.7169431841603,
-1.71473585613343,-1.71171977789322,-1.70473385443277,-1.64117642788127,
-1.59865860289724,-1.5782920231787,-1.56051261179462,-1.55751723321027,
-1.55598671581549,-1.55477778106601,-1.55338527508967,-1.55094209177177,
-1.54026747308313,-1.51949089623647,-1.44927318145286,-1.40402799963735,
-1.39820944487283,-1.39540963885789,-1.39323596155489,-1.3908447119159,
-1.38695301317143,-1.37339996795555,-1.35095797420423,-1.25928426084271,
-1.2553040496369,-1.23757931627163,-1.23458650537719,-1.2330564434065,-1.23184742982321,
-1.23045433970987,-1.22800893195824,-1.21730619280207,-1.19645074136639,
-1.12648050037713,-1.08108697270815,-1.07526514695507,-1.07246451857569,
-1.07029053698862,-1.06789928970158,-1.06400835211364,-1.05046548273603,
-1.02804727024587,-0.936520137852073,-0.932813543499302,-0.914648270766425,
-0.911635716583265,-0.910101318196676,-0.9088918114962,-0.907501443260302,
-0.905068778167366,-0.89454260015925,-0.874187499231618,-0.783057456156521,
-0.756866100645749,-0.75228490523195,-0.749491188763659,-0.7473117221757,
-0.744940117456575,-0.741137677410085,-0.72868292852517,-0.708565803663826,
-0.698900011106378),.UNSPECIFIED.);
#7723=B_SPLINE_CURVE_WITH_KNOTS('',3,(#64697,#64698,#64699,#64700,#64701,
#64702,#64703,#64704),.UNSPECIFIED.,.F.,.F.,(4,1,1,1,1,4),(53.4070839884957,
54.2924291220894,55.2919442606161,56.2914593991429,57.2909745376696,57.5317208912133),
 .UNSPECIFIED.);
#7724=B_SPLINE_CURVE_WITH_KNOTS('',3,(#64705,#64706,#64707,#64708,#64709,
#64710,#64711,#64712,#64713,#64714,#64715,#64716,#64717,#64718,#64719,#64720,
#64721,#64722,#64723,#64724,#64725,#64726,#64727,#64728,#64729,#64730,#64731,
#64732,#64733,#64734,#64735,#64736,#64737,#64738,#64739,#64740,#64741,#64742,
#64743,#64744,#64745,#64746,#64747,#64748,#64749,#64750,#64751,#64752,#64753,
#64754,#64755,#64756,#64757,#64758,#64759,#64760,#64761,#64762,#64763,#64764,
#64765,#64766,#64767,#64768,#64769,#64770,#64771,#64772,#64773,#64774,#64775,
#64776,#64777),.UNSPECIFIED.,.F.,.F.,(4,3,3,3,3,3,3,3,3,3,3,3,3,3,3,3,3,
3,3,3,3,3,3,3,4),(51.2473625597526,51.2938837065091,51.386959014978,51.4799082660596,
51.5727590923892,51.6655420978319,51.7582899524755,51.8510274787487,51.9437794839529,
52.0366306828649,52.1295337010273,52.2225920422408,52.2933988450358,52.3864741535047,
52.4794234045863,52.5722742309156,52.6650572363584,52.7578050910019,52.8505426172751,
52.9432946224792,53.0361458213912,53.1290488395536,53.222107180767,53.2929139835626,
53.4070751110268),.UNSPECIFIED.);
#7725=B_SPLINE_CURVE_WITH_KNOTS('',3,(#64779,#64780,#64781,#64782,#64783,
#64784,#64785,#64786,#64787,#64788,#64789,#64790,#64791,#64792,#64793,#64794,
#64795,#64796,#64797,#64798,#64799,#64800,#64801,#64802,#64803,#64804,#64805,
#64806,#64807,#64808,#64809,#64810,#64811,#64812,#64813,#64814,#64815,#64816,
#64817,#64818,#64819,#64820,#64821,#64822,#64823,#64824,#64825,#64826,#64827,
#64828,#64829,#64830,#64831,#64832,#64833,#64834,#64835,#64836,#64837,#64838,
#64839,#64840,#64841,#64842,#64843,#64844,#64845,#64846,#64847,#64848,#64849,
#64850,#64851,#64852,#64853,#64854,#64855,#64856,#64857,#64858,#64859,#64860,
#64861,#64862),.UNSPECIFIED.,.F.,.F.,(4,2,2,2,2,2,2,2,2,2,2,2,2,2,2,2,2,
2,2,2,2,2,2,2,2,2,2,2,2,2,2,2,2,2,2,2,2,2,2,2,2,4),(-0.698900011106378,
-0.664621630843526,-0.616528634413205,-0.592100740903726,-0.588805704293141,
-0.587252280301598,-0.586038107846558,-0.584675991467339,-0.582416399969052,
-0.573965824956321,-0.50096915406343,-0.473014118631769,-0.459328988812959,
-0.456875210752135,-0.433699831937314,-0.429291313732653,-0.426519650652467,
-0.424349205785662,-0.42194248599253,-0.417982213918182,-0.404016206776864,
-0.380538053041719,-0.313060341648312,-0.269698333722163,-0.266089288043848,
-0.264477082834381,-0.26325443855795,-0.261922709538034,-0.260545508384321,
-0.256155984822727,-0.221941283444193,-0.195052399865455,-0.118521449148602,
-0.116433301572504,-0.107893624668228,-0.104521269988041,-0.102471308191436,
-0.100276752428945,-0.097336400912601,-0.0907751578210967,-0.0820187210215503,
-0.00096106920673559),.UNSPECIFIED.);
#7726=B_SPLINE_CURVE_WITH_KNOTS('',3,(#64863,#64864,#64865,#64866,#64867,
#64868,#64869,#64870,#64871,#64872,#64873,#64874,#64875,#64876,#64877,#64878,
#64879,#64880,#64881,#64882,#64883,#64884,#64885,#64886,#64887,#64888,#64889,
#64890,#64891,#64892,#64893,#64894,#64895,#64896,#64897,#64898,#64899,#64900,
#64901,#64902,#64903,#64904,#64905,#64906,#64907,#64908,#64909,#64910,#64911,
#64912,#64913,#64914,#64915,#64916,#64917,#64918,#64919,#64920,#64921,#64922,
#64923,#64924,#64925,#64926,#64927,#64928,#64929,#64930,#64931,#64932,#64933,
#64934,#64935,#64936,#64937,#64938,#64939,#64940,#64941,#64942,#64943,#64944,
#64945,#64946,#64947,#64948,#64949,#64950,#64951,#64952,#64953,#64954,#64955,
#64956,#64957,#64958,#64959,#64960,#64961,#64962,#64963,#64964,#64965,#64966,
#64967,#64968,#64969,#64970,#64971,#64972,#64973,#64974,#64975,#64976,#64977,
#64978,#64979,#64980,#64981,#64982,#64983,#64984,#64985,#64986,#64987,#64988,
#64989,#64990,#64991,#64992,#64993,#64994,#64995,#64996,#64997,#64998,#64999,
#65000,#65001,#65002,#65003,#65004,#65005,#65006,#65007,#65008,#65009,#65010,
#65011,#65012,#65013,#65014,#65015,#65016,#65017,#65018,#65019,#65020,#65021,
#65022,#65023,#65024),.UNSPECIFIED.,.F.,.F.,(4,2,2,2,2,2,2,2,2,2,2,2,2,
2,2,2,2,2,2,2,2,2,2,2,2,2,2,2,2,2,2,2,2,2,2,2,2,2,2,2,2,2,2,2,2,2,2,2,2,
2,2,2,2,2,2,2,2,2,2,2,2,2,2,2,2,2,2,2,2,2,2,2,2,2,2,2,2,2,2,2,4),(-4.06068215332971,
-4.01016739059331,-4.00563546502231,-4.0034750215586,-4.00204496752844,
-4.00067647320423,-3.99946368735555,-3.99789541860962,-3.99460996949297,
-3.97046173073304,-3.94341465850605,-3.92453635391737,-3.90748724446368,
-3.85923553553613,-3.84585301283487,-3.84194707613627,-3.83955247588097,
-3.83737929525466,-3.83458509090088,-3.82879611066212,-3.75232872134662,
-3.70466219579208,-3.68981300428414,-3.68141227696476,-3.67915992946697,
-3.67779944745224,-3.67658487540966,-3.67502853482328,-3.67171841939994,
-3.64683347272879,-3.5986079407557,-3.5277772219995,-3.52091448859619,-3.51791991256651,
-3.51571617170279,-3.51367980834526,-3.5103799048344,-3.50227006628849,
-3.49960685706945,-3.4225178097056,-3.36580317974603,-3.35829040904099,
-3.35612722825411,-3.3547870362861,-3.35356705766937,-3.35197239791703,
-3.34928616392161,-3.33246838087751,-3.23688512807977,-3.21377106282806,
-3.19991935773195,-3.19599730288214,-3.19359912742348,-3.19142682324009,
-3.188639494635,-3.18417941815438,-3.16015656097722,-3.15886779619432,-3.15733800062712,
-3.13904129165035,-3.1137563079839,-3.0656739991336,-3.04605268995558,-3.03579126197613,
-3.03337866513771,-3.03199287042536,-3.03078296031161,-3.02924233038554,
-3.02609695918307,-3.00574312816377,-2.91319853156648,-2.89060292282442,
-2.87698036037882,-2.87308162481383,-2.87068881823995,-2.86851554397552,
-2.86571880733699,-2.85991586749835,-2.81554783012779,-2.74408992563194,
-2.72867715037577),.UNSPECIFIED.);
#7727=B_SPLINE_CURVE_WITH_KNOTS('',3,(#65030,#65031,#65032,#65033,#65034,
#65035,#65036,#65037,#65038,#65039,#65040,#65041,#65042,#65043,#65044,#65045,
#65046,#65047,#65048,#65049,#65050,#65051,#65052,#65053,#65054,#65055,#65056,
#65057,#65058,#65059,#65060,#65061,#65062,#65063,#65064,#65065,#65066,#65067,
#65068,#65069,#65070,#65071,#65072,#65073,#65074,#65075,#65076,#65077,#65078,
#65079,#65080,#65081,#65082,#65083,#65084,#65085,#65086,#65087,#65088,#65089,
#65090,#65091,#65092,#65093,#65094,#65095,#65096,#65097,#65098,#65099,#65100,
#65101,#65102,#65103,#65104,#65105,#65106,#65107,#65108,#65109,#65110,#65111,
#65112,#65113,#65114,#65115,#65116,#65117,#65118,#65119,#65120,#65121,#65122,
#65123,#65124,#65125,#65126,#65127,#65128,#65129,#65130,#65131,#65132,#65133,
#65134,#65135,#65136,#65137,#65138,#65139,#65140,#65141,#65142,#65143,#65144,
#65145,#65146,#65147,#65148,#65149,#65150,#65151,#65152,#65153,#65154,#65155,
#65156,#65157,#65158,#65159,#65160,#65161,#65162,#65163,#65164,#65165,#65166,
#65167,#65168),.UNSPECIFIED.,.F.,.F.,(4,3,3,3,3,3,3,3,3,3,3,3,3,3,3,3,3,
3,3,3,3,3,3,3,3,3,3,3,3,3,3,3,3,3,3,3,3,3,3,3,3,3,3,3,3,3,4),(59.6902604182064,
59.7842625762968,59.8782936636862,59.9723761264494,60.0665973185503,60.1608983242092,
60.2553670544362,60.2895199532499,60.3825952617188,60.4755445128005,60.5683953391299,
60.6611783445727,60.7539261992163,60.8466637254895,60.9394157306936,61.0322669296056,
61.125169947768,61.2182282889814,61.2890350917767,61.3821104002456,61.4750596513273,
61.5679104776568,61.6606934830996,61.7534413377431,61.8461788640163,61.9389308692204,
62.0317820681324,62.1246850862947,62.2177434275082,62.2885502303035,62.3816255387724,
62.474574789854,62.5674256161836,62.6602086216264,62.75295647627,62.8456940025433,
62.9384460077475,63.0312972066595,63.1242002248218,63.2172585660352,63.2880653688302,
63.3811374997221,63.4740886781739,63.5669306360504,63.659708699058,63.7524558212429,
63.8139030978781),.UNSPECIFIED.);
#7728=B_SPLINE_CURVE_WITH_KNOTS('',3,(#65169,#65170,#65171,#65172,#65173,
#65174),.UNSPECIFIED.,.F.,.F.,(4,1,1,4),(57.5317208912133,58.2904896761964,
59.2900048147232,59.6902534604737),.UNSPECIFIED.);
#7729=B_SPLINE_CURVE_WITH_KNOTS('',3,(#65175,#65176,#65177,#65178,#65179,
#65180,#65181,#65182,#65183,#65184,#65185,#65186,#65187,#65188,#65189,#65190,
#65191,#65192,#65193,#65194,#65195,#65196,#65197,#65198,#65199,#65200,#65201,
#65202,#65203,#65204,#65205,#65206,#65207,#65208,#65209,#65210,#65211,#65212,
#65213,#65214,#65215,#65216,#65217,#65218,#65219,#65220,#65221,#65222,#65223,
#65224,#65225,#65226,#65227,#65228,#65229,#65230,#65231,#65232,#65233,#65234,
#65235,#65236,#65237,#65238,#65239,#65240,#65241,#65242,#65243,#65244,#65245,
#65246,#65247,#65248,#65249,#65250,#65251,#65252,#65253,#65254,#65255,#65256,
#65257,#65258,#65259,#65260,#65261,#65262,#65263,#65264,#65265,#65266,#65267,
#65268,#65269,#65270,#65271,#65272,#65273,#65274,#65275,#65276,#65277,#65278,
#65279,#65280,#65281,#65282,#65283,#65284,#65285,#65286,#65287,#65288,#65289,
#65290,#65291,#65292,#65293,#65294,#65295,#65296,#65297,#65298,#65299,#65300,
#65301,#65302,#65303,#65304,#65305,#65306,#65307,#65308,#65309,#65310,#65311,
#65312,#65313,#65314,#65315,#65316,#65317,#65318,#65319,#65320,#65321,#65322,
#65323,#65324,#65325,#65326,#65327,#65328,#65329,#65330,#65331,#65332,#65333,
#65334,#65335,#65336,#65337,#65338,#65339,#65340,#65341,#65342,#65343,#65344,
#65345,#65346,#65347,#65348,#65349,#65350,#65351,#65352,#65353,#65354,#65355,
#65356,#65357,#65358,#65359,#65360,#65361,#65362,#65363,#65364,#65365,#65366,
#65367,#65368,#65369,#65370,#65371,#65372,#65373,#65374,#65375,#65376,#65377,
#65378,#65379,#65380,#65381,#65382,#65383,#65384,#65385,#65386,#65387,#65388,
#65389,#65390,#65391,#65392,#65393,#65394,#65395,#65396,#65397,#65398,#65399,
#65400,#65401,#65402,#65403,#65404,#65405,#65406,#65407,#65408,#65409,#65410,
#65411,#65412,#65413,#65414,#65415,#65416),.UNSPECIFIED.,.F.,.F.,(4,2,2,
2,2,2,2,2,2,2,2,2,2,2,2,2,2,2,2,2,2,2,2,2,2,2,2,2,2,2,2,2,2,2,2,2,2,2,2,
2,2,2,2,2,2,2,2,2,2,2,2,2,2,2,2,2,2,2,2,2,2,2,2,2,2,2,2,2,2,2,2,2,2,2,2,
2,2,2,2,2,2,2,2,2,2,2,2,2,2,2,2,2,2,2,2,2,2,2,2,2,2,2,2,2,2,2,2,2,2,2,2,
2,2,2,2,2,2,2,2,2,4),(-2.72867715037577,-2.72350407496648,-2.71289780256903,
-2.71045956996983,-2.7090681448379,-2.70785905156677,-2.70632691622698,
-2.7033240763568,-2.6853563718748,-2.68156789265345,-2.59001279875908,-2.56758563996592,
-2.55403799014216,-2.55014696977012,-2.54775594541731,-2.54558234649511,
-2.54278246399505,-2.53696310998938,-2.49167948101183,-2.42159372062447,
-2.40070650571641,-2.38999416984859,-2.38754828733318,-2.38615521232169,
-2.38494638716493,-2.38341679765986,-2.38042561307028,-2.36272687962605,
-2.30347046810249,-2.23548875402994,-2.22901404479245,-2.22608979732971,
-2.22389810728979,-2.22184417016827,-2.21844985692808,-2.20977639605324,
-2.20785070940592,-2.13190923664674,-2.07019963873847,-2.06572801028936,
-2.06395013605944,-2.06270319861711,-2.06157159851997,-2.06003674240042,
-2.05703041579629,-2.03124821076372,-1.98393231425603,-1.96311396042574,
-1.91178647330223,-1.90586452634126,-1.90307477011337,-1.90089603121276,
-1.89852283013627,-1.89471261053369,-1.88193890002056,-1.86122446382206,
-1.80297127806423,-1.7460374583062,-1.74250172915425,-1.74090302913681,
-1.73968256174143,-1.73834460923278,-1.73614666178869,-1.72834864008394,
-1.66756532909262,-1.59504583184413,-1.59273614794498,-1.58429649915555,
-1.58094122807485,-1.57889461635511,-1.57669824672687,-1.57374606860842,
-1.56711899847704,-1.55825199323859,-1.53608757523221,-1.44611393163774,
-1.42265032937607,-1.41938806983371,-1.41782425288784,-1.41661188217892,
-1.41524053939206,-1.41289334816374,-1.40345803212728,-1.38606288984755,
-1.33982106713559,-1.26581435253348,-1.25996542384353,-1.25715945918686,
-1.25498474766144,-1.25259613138786,-1.2487171680703,-1.23529188428178,
-1.21313777151261,-1.12323423133126,-1.09967625403648,-1.09641051067266,
-1.09484592602631,-1.09363337371947,-1.09226227760491,-1.08991654809614,
-1.08050059269318,-1.06315678286072,-1.01708785574675,-0.942809611863748,
-0.936966950096965,-0.934162055932783,-0.931987316175677,-0.929597805724423,
-0.925715457600736,-0.912259444858125,-0.890037214079459,-0.799709511656546,
-0.776638477923404,-0.773389424747365,-0.771828023925658,-0.770615724651503,
-0.769242488722856,-0.766887502364802,-0.757361245570541,-0.739728680357567,
-0.698670975029854),.UNSPECIFIED.);
#7730=B_SPLINE_CURVE_WITH_KNOTS('',3,(#65422,#65423,#65424,#65425,#65426,
#65427,#65428,#65429),.UNSPECIFIED.,.F.,.F.,(4,1,1,1,1,4),(65.9734521657886,
66.2866107844105,67.2861259229373,68.285641061464,69.2851561999908,70.0962929016582),
 .UNSPECIFIED.);
#7731=B_SPLINE_CURVE_WITH_KNOTS('',3,(#65430,#65431,#65432,#65433,#65434,
#65435,#65436,#65437,#65438,#65439,#65440,#65441,#65442,#65443,#65444,#65445,
#65446,#65447,#65448,#65449,#65450,#65451,#65452,#65453,#65454,#65455,#65456,
#65457,#65458,#65459,#65460,#65461,#65462,#65463,#65464,#65465,#65466,#65467,
#65468,#65469,#65470,#65471,#65472,#65473,#65474,#65475,#65476,#65477,#65478,
#65479,#65480,#65481,#65482,#65483,#65484,#65485,#65486,#65487,#65488,#65489,
#65490,#65491,#65492,#65493,#65494,#65495,#65496,#65497,#65498,#65499,#65500,
#65501,#65502),.UNSPECIFIED.,.F.,.F.,(4,3,3,3,3,3,3,3,3,3,3,3,3,3,3,3,3,
3,3,3,3,3,3,3,4),(63.8139030978781,63.9066474418343,64.001880708215,64.0947651897081,
64.1911728485326,64.287580507357,64.380655815826,64.4736050669074,64.5664558932367,
64.6592388986794,64.751986753323,64.8447242795962,64.9374762848006,65.0303274837126,
65.123230501875,65.2162888430884,65.2870956458838,65.37978898859,65.4723622086882,
65.564840709142,65.6572498016576,65.7496260993385,65.8419832821929,65.9343713417692,
65.973445725386),.UNSPECIFIED.);
#7732=B_SPLINE_CURVE_WITH_KNOTS('',3,(#65504,#65505,#65506,#65507,#65508,
#65509,#65510,#65511,#65512,#65513,#65514,#65515,#65516,#65517,#65518,#65519,
#65520,#65521,#65522,#65523,#65524,#65525,#65526,#65527,#65528,#65529,#65530,
#65531,#65532,#65533,#65534,#65535,#65536,#65537,#65538,#65539,#65540,#65541,
#65542,#65543,#65544,#65545,#65546,#65547,#65548,#65549,#65550,#65551,#65552,
#65553,#65554,#65555,#65556,#65557,#65558,#65559,#65560,#65561,#65562,#65563,
#65564,#65565,#65566,#65567,#65568,#65569,#65570,#65571,#65572,#65573,#65574,
#65575,#65576,#65577,#65578,#65579,#65580,#65581,#65582,#65583,#65584,#65585,
#65586,#65587,#65588,#65589),.UNSPECIFIED.,.F.,.F.,(4,2,2,2,2,2,2,2,2,2,
2,2,2,2,2,2,2,2,2,2,2,2,2,2,2,2,2,2,2,2,2,2,2,2,2,2,2,2,2,2,2,2,4),(-0.698670975029854,
-0.692823758210332,-0.619834095291595,-0.613960179767915,-0.61117919205671,
-0.609001231608271,-0.60670600431764,-0.603057183924118,-0.598757398167659,
-0.590584728168661,-0.505518213053075,-0.472576763803538,-0.471041835003278,
-0.453279465037479,-0.450284201222689,-0.448753387532379,-0.447544037092701,
-0.446150848025735,-0.4437059697061,-0.433016337434033,-0.412200570169519,
-0.366623274314038,-0.296924322599318,-0.291577216408451,-0.28883307806977,
-0.286802414879055,-0.284744543073832,-0.281876158665878,-0.275661204429219,
-0.267397018166896,-0.247307535613368,-0.203469221567176,-0.163588703485155,
-0.155263457366295,-0.130778221950257,-0.127480746525178,-0.125926659863407,
-0.124712189090788,-0.123349980676063,-0.12104447028807,-0.1121016596629,
-0.0959764796556443,-0.000961420122294117),.UNSPECIFIED.);
#7733=B_SPLINE_CURVE_WITH_KNOTS('',3,(#65590,#65591,#65592,#65593,#65594,
#65595,#65596,#65597,#65598,#65599,#65600,#65601,#65602,#65603,#65604,#65605,
#65606,#65607,#65608,#65609,#65610,#65611,#65612,#65613,#65614,#65615,#65616,
#65617,#65618,#65619,#65620,#65621,#65622,#65623,#65624,#65625,#65626,#65627,
#65628,#65629,#65630,#65631,#65632,#65633,#65634,#65635,#65636,#65637,#65638,
#65639,#65640,#65641,#65642,#65643,#65644,#65645,#65646,#65647,#65648,#65649,
#65650,#65651,#65652,#65653,#65654,#65655,#65656,#65657,#65658,#65659,#65660,
#65661,#65662,#65663,#65664,#65665,#65666,#65667,#65668,#65669,#65670,#65671,
#65672,#65673,#65674,#65675,#65676,#65677,#65678,#65679,#65680,#65681,#65682,
#65683,#65684,#65685,#65686,#65687,#65688,#65689,#65690,#65691,#65692,#65693,
#65694,#65695,#65696,#65697,#65698,#65699,#65700,#65701,#65702,#65703,#65704,
#65705,#65706,#65707,#65708,#65709,#65710,#65711,#65712,#65713,#65714,#65715,
#65716,#65717,#65718,#65719,#65720,#65721,#65722,#65723,#65724,#65725,#65726,
#65727,#65728,#65729,#65730,#65731,#65732,#65733,#65734,#65735,#65736,#65737,
#65738,#65739,#65740,#65741,#65742,#65743,#65744,#65745,#65746,#65747,#65748,
#65749,#65750,#65751,#65752,#65753,#65754,#65755,#65756,#65757,#65758,#65759,
#65760,#65761,#65762,#65763,#65764,#65765,#65766,#65767,#65768,#65769,#65770,
#65771,#65772,#65773,#65774,#65775,#65776,#65777,#65778,#65779,#65780,#65781,
#65782,#65783,#65784,#65785,#65786,#65787,#65788,#65789,#65790,#65791,#65792,
#65793,#65794,#65795,#65796,#65797,#65798,#65799),.UNSPECIFIED.,.F.,.F.,
(4,2,2,2,2,2,2,2,2,2,2,2,2,2,2,2,2,2,2,2,2,2,2,2,2,2,2,2,2,2,2,2,2,2,2,
2,2,2,2,2,2,2,2,2,2,2,2,2,2,2,2,2,2,2,2,2,2,2,2,2,2,2,2,2,2,2,2,2,2,2,2,
2,2,2,2,2,2,2,2,2,2,2,2,2,2,2,2,2,2,2,2,2,2,2,2,2,2,2,2,2,2,2,2,2,4),(-4.03619647859404,
-4.00809560787024,-4.00448225059761,-4.00202961525425,-4.00000131875697,
-3.99805863747667,-3.99555167918774,-3.99121004393426,-3.97419108135287,
-3.97153499754223,-3.95858297357044,-3.91144482001015,-3.85027590673282,
-3.84248202592952,-3.84029403739073,-3.83896400863578,-3.83775209233207,
-3.83616637406576,-3.83266647616008,-3.77540646349739,-3.7262991672328,
-3.70047909168305,-3.69061502854576,-3.68569640163624,-3.68162020687213,
-3.67921365188643,-3.67920325006476,-3.67919269124366,-3.67918197277497,
-3.67917109195598,-3.67916004607431,-3.67914883235244,-3.6791374479344,
-3.67912588994352,-3.67911415545363,-3.67910224146535,-3.67909014493247,
-3.6790778627553,-3.67906539177035,-3.6790527287561,-3.6790398704526,-3.67902681353936,
-3.67901355459893,-3.67900009018701,-3.6789864166821,-3.67897268481082,
-3.67895802553466,-3.6789423755487,-3.67892566713863,-3.67890782795825,
-3.67674380707064,-3.67397297347634,-3.6680914963686,-3.61764329708662,
-3.5629577084575,-3.52519736541063,-3.52088099693056,-3.51913529924332,
-3.51790067272656,-3.51677258600318,-3.51523195235049,-3.51218254848548,
-3.48396307303133,-3.39891886334032,-3.3774930570738,-3.36885471474969,
-3.36438786215256,-3.36061713192714,-3.35828193829274,-3.35612484208294,
-3.35335910345943,-3.34765699647645,-3.27008450488472,-3.20884616877966,
-3.20104817914338,-3.19885982728458,-3.1975297444059,-3.19631789735988,
-3.19473242895523,-3.19205856183358,-3.17523020180477,-3.08041523800341,
-3.05747873455699,-3.04373049714645,-3.03983625825116,-3.03745477821521,
-3.03529739268434,-3.0325289217795,-3.02681273198776,-2.94973204157224,
-2.88806015314576,-2.88023589715105,-2.87804497313629,-2.87671433692944,
-2.87550270319164,-2.87391847662165,-2.87042634739002,-2.8128213530936,
-2.76383108936271,-2.73816152981094,-2.72324021783761,-2.71923333894717,
-2.71682661077525,-2.71467416823324,-2.71282346300387),.UNSPECIFIED.);
#7734=B_SPLINE_CURVE_WITH_KNOTS('',3,(#65805,#65806,#65807,#65808,#65809,
#65810,#65811,#65812,#65813,#65814,#65815,#65816,#65817,#65818,#65819,#65820,
#65821,#65822,#65823,#65824,#65825,#65826,#65827,#65828,#65829,#65830,#65831,
#65832,#65833,#65834,#65835,#65836,#65837,#65838,#65839,#65840,#65841,#65842,
#65843,#65844,#65845,#65846,#65847,#65848,#65849,#65850,#65851,#65852,#65853,
#65854,#65855,#65856,#65857,#65858,#65859,#65860,#65861,#65862,#65863,#65864,
#65865,#65866,#65867,#65868,#65869,#65870,#65871,#65872,#65873,#65874,#65875,
#65876,#65877,#65878,#65879,#65880,#65881,#65882,#65883,#65884,#65885,#65886,
#65887,#65888,#65889,#65890,#65891,#65892,#65893,#65894,#65895,#65896,#65897,
#65898,#65899,#65900,#65901,#65902,#65903,#65904,#65905,#65906,#65907,#65908,
#65909,#65910,#65911,#65912,#65913,#65914,#65915,#65916,#65917,#65918,#65919,
#65920,#65921,#65922,#65923,#65924,#65925,#65926,#65927,#65928,#65929,#65930,
#65931,#65932,#65933,#65934,#65935,#65936,#65937,#65938,#65939,#65940,#65941,
#65942,#65943,#65944,#65945,#65946),.UNSPECIFIED.,.F.,.F.,(4,3,3,3,3,3,
3,3,3,3,3,3,3,3,3,3,3,3,3,3,3,3,3,3,3,3,3,3,3,3,3,3,3,3,3,3,3,3,3,3,3,3,
3,3,3,3,3,4),(72.2566310325656,72.2837016155711,72.37677692404,72.4697261751215,
72.5625770014511,72.6553600068939,72.7481078615374,72.8408453878106,72.9335973930147,
73.0264485919267,73.1193516100891,73.2124099513025,73.2832167540979,73.3762920625668,
73.4692413136484,73.5620921399779,73.6548751454206,73.7476230000642,73.8403605263374,
73.9331125315415,74.0259637304535,74.1188667486159,74.2119250898294,74.2827318926246,
74.3758072010935,74.468756452175,74.5616072785045,74.6543902839473,74.7471381385908,
74.839875664864,74.9326276700682,75.0254788689801,75.1183818871425,75.211440228356,
75.2822470311514,75.3753223396203,75.4682715907019,75.5611224170314,75.6539054224742,
75.7466532771177,75.8393908033909,75.9321428085951,76.0249940075071,76.1178970256695,
76.210955366883,76.2817621696781,76.374851433623,76.380801467099),
 .UNSPECIFIED.);
#7735=B_SPLINE_CURVE_WITH_KNOTS('',3,(#65947,#65948,#65949,#65950,#65951,
#65952),.UNSPECIFIED.,.F.,.F.,(4,1,1,4),(70.0962929016582,70.2846713385176,
71.2841864770443,72.2566272414748),.UNSPECIFIED.);
#7736=B_SPLINE_CURVE_WITH_KNOTS('',3,(#65953,#65954,#65955,#65956,#65957,
#65958,#65959,#65960,#65961,#65962,#65963,#65964,#65965,#65966,#65967,#65968,
#65969,#65970,#65971,#65972,#65973,#65974,#65975,#65976,#65977,#65978,#65979,
#65980,#65981,#65982,#65983,#65984,#65985,#65986,#65987,#65988,#65989,#65990,
#65991,#65992,#65993,#65994,#65995,#65996,#65997,#65998,#65999,#66000,#66001,
#66002,#66003,#66004,#66005,#66006,#66007,#66008,#66009,#66010,#66011,#66012,
#66013,#66014,#66015,#66016,#66017,#66018,#66019,#66020,#66021,#66022,#66023,
#66024,#66025,#66026,#66027,#66028,#66029,#66030,#66031,#66032,#66033,#66034,
#66035,#66036,#66037,#66038,#66039,#66040,#66041,#66042,#66043,#66044,#66045,
#66046,#66047,#66048,#66049,#66050,#66051,#66052,#66053,#66054,#66055,#66056,
#66057,#66058,#66059,#66060,#66061,#66062,#66063,#66064,#66065,#66066,#66067,
#66068,#66069,#66070,#66071,#66072,#66073,#66074,#66075,#66076,#66077,#66078,
#66079,#66080,#66081,#66082,#66083,#66084,#66085,#66086,#66087,#66088,#66089,
#66090,#66091,#66092,#66093,#66094,#66095,#66096,#66097,#66098,#66099,#66100,
#66101,#66102,#66103,#66104,#66105,#66106,#66107,#66108,#66109,#66110,#66111,
#66112,#66113,#66114,#66115,#66116,#66117,#66118,#66119,#66120,#66121,#66122,
#66123,#66124,#66125,#66126,#66127,#66128,#66129,#66130,#66131,#66132,#66133,
#66134,#66135,#66136,#66137,#66138,#66139,#66140,#66141,#66142,#66143,#66144,
#66145,#66146,#66147,#66148,#66149,#66150,#66151,#66152,#66153,#66154,#66155,
#66156,#66157,#66158,#66159,#66160,#66161,#66162,#66163,#66164,#66165,#66166,
#66167,#66168,#66169,#66170,#66171,#66172,#66173,#66174,#66175,#66176,#66177,
#66178,#66179,#66180,#66181,#66182,#66183,#66184,#66185,#66186,#66187,#66188,
#66189,#66190,#66191,#66192,#66193,#66194,#66195,#66196,#66197,#66198),
 .UNSPECIFIED.,.F.,.F.,(4,2,2,2,2,2,2,2,2,2,2,2,2,2,2,2,2,2,2,2,2,2,2,2,
2,2,2,2,2,2,2,2,2,2,2,2,2,2,2,2,2,2,2,2,2,2,2,2,2,2,2,2,2,2,2,2,2,2,2,2,
2,2,2,2,2,2,2,2,2,2,2,2,2,2,2,2,2,2,2,2,2,2,2,2,2,2,2,2,2,2,2,2,2,2,2,2,
2,2,2,2,2,2,2,2,2,2,2,2,2,2,2,2,2,2,2,2,2,2,2,2,2,2,4),(-2.71282346300387,
-2.71195001267204,-2.70766508087925,-2.68614652012974,-2.59027107316476,
-2.57026216330264,-2.5598826085674,-2.55747199598722,-2.55609227919899,
-2.55489080165277,-2.55336498530999,-2.55036438706897,-2.53213835472559,
-2.53155062342198,-2.49852763948949,-2.41412170693746,-2.40185705050541,
-2.39811859083517,-2.39577148623095,-2.393604037411,-2.3908111081901,-2.38619997321621,
-2.35901042891315,-2.34699181388133,-2.3450678046571,-2.34442344452801,
-2.27062411729961,-2.24980866519993,-2.23914361759669,-2.2367120766484,
-2.23532774382593,-2.23412686365069,-2.23260779242953,-2.22963857897059,
-2.21210268904967,-2.20809273471183,-2.11706870009749,-2.09477709593845,
-2.08131325677669,-2.07744730149775,-2.07507189348216,-2.07291263164853,
-2.07013141496413,-2.06435157391243,-2.01943223056741,-1.94998010095846,
-1.9404679404936,-1.91955881753204,-1.91640663883009,-1.91487075813651,
-1.91366840032819,-1.91229549358337,-1.90991540464985,-1.89993594979191,
-1.88103433376462,-1.77069743540713,-1.767724277275,-1.75931203894651,-1.75597457548543,
-1.7539409924426,-1.75176026778187,-1.74883201311585,-1.74227081926397,
-1.73349895408688,-1.71160660346678,-1.6230273179456,-1.59881209953064,
-1.59554106945206,-1.59399853115264,-1.59279267210641,-1.59143966663562,
-1.58914870702585,-1.58024989926437,-1.56419027039911,-1.54003092374437,
-1.48200758979014,-1.46790802729868,-1.44185251571303,-1.43730028268749,
-1.43452493998363,-1.43236023742578,-1.43000513236345,-1.42623009320188,
-1.41363054025839,-1.39324757705729,-1.37106249507141,-1.29548306605084,
-1.27775242624812,-1.27477340730196,-1.27325229440039,-1.27205132246873,
-1.2706685888863,-1.26824400916414,-1.25767293758014,-1.23712697205462,
-1.16679448607912,-1.12228766638433,-1.11651573685802,-1.11373608906869,
-1.11157704807818,-1.10920087608156,-1.10533141352298,-1.09183287044736,
-1.06945994169842,-0.977920863755642,-0.957170174292333,-0.954024060577004,
-0.95248930389804,-0.951286960949317,-0.949913110514963,-0.947529108902472,
-0.937500993239768,-0.918467300685122,-0.85724353276297,-0.801741171713293,
-0.796398138609899,-0.793664512253074,-0.791645723315301,-0.789453630618654,
-0.786461699382029,-0.779546580694334,-0.723083846394838,-0.696237685186134),
 .UNSPECIFIED.);
#7737=B_SPLINE_CURVE_WITH_KNOTS('',3,(#66204,#66205,#66206,#66207,#66208,
#66209,#66210,#66211,#66212,#66213,#66214,#66215,#66216,#66217,#66218,#66219,
#66220,#66221,#66222,#66223,#66224,#66225,#66226,#66227,#66228,#66229,#66230,
#66231,#66232,#66233,#66234,#66235,#66236,#66237,#66238,#66239,#66240,#66241,
#66242,#66243,#66244,#66245,#66246,#66247,#66248,#66249,#66250,#66251,#66252,
#66253,#66254,#66255,#66256,#66257,#66258,#66259,#66260,#66261,#66262,#66263,
#66264,#66265,#66266,#66267,#66268,#66269,#66270,#66271,#66272,#66273,#66274,
#66275,#66276,#66277,#66278,#66279,#66280,#66281,#66282,#66283,#66284,#66285,
#66286,#66287,#66288,#66289,#66290,#66291,#66292,#66293,#66294,#66295,#66296,
#66297,#66298,#66299,#66300,#66301,#66302,#66303,#66304,#66305,#66306,#66307,
#66308,#66309,#66310,#66311,#66312,#66313,#66314,#66315,#66316,#66317,#66318,
#66319,#66320,#66321,#66322,#66323,#66324,#66325,#66326,#66327,#66328,#66329,
#66330,#66331,#66332,#66333,#66334,#66335,#66336,#66337,#66338,#66339,#66340,
#66341,#66342),.UNSPECIFIED.,.F.,.F.,(4,3,3,3,3,3,3,3,3,3,3,3,3,3,3,3,3,
3,3,3,3,3,3,3,3,3,3,3,3,3,3,3,3,3,3,3,3,3,3,3,3,3,3,3,3,3,4),(78.5398163397452,
78.6323777454344,78.7241557666759,78.8159095945813,78.9076650481199,79.0008256824045,
79.0927135108167,79.1865105480376,79.2803075852584,79.3733828937274,79.4663321448089,
79.5591829711384,79.6519659765812,79.7447138312248,79.837451357498,79.9302033627021,
80.023054561614,80.1159575797763,80.2090159209898,80.2798227237852,80.3728980322541,
80.4658472833355,80.5586981096652,80.6514811151079,80.7442289697515,80.8369664960247,
80.929718501229,81.022569700141,81.1154727183036,81.2085310595171,81.2793378623119,
81.3724131707809,81.4653624218621,81.5582132481916,81.6509962536344,81.7437441082779,
81.8364816345511,81.9292336397553,82.0220848386673,82.1149878568298,82.2080461980432,
82.2788530008387,82.375109601286,82.4680451601066,82.5608939237312,82.6536708061284,
82.663879402628),.UNSPECIFIED.);
#7738=B_SPLINE_CURVE_WITH_KNOTS('',3,(#66343,#66344,#66345,#66346,#66347,
#66348,#66349,#66350,#66351,#66352,#66353,#66354,#66355,#66356,#66357,#66358,
#66359,#66360,#66361,#66362,#66363,#66364,#66365,#66366,#66367,#66368,#66369,
#66370,#66371,#66372,#66373,#66374,#66375,#66376,#66377,#66378,#66379,#66380,
#66381,#66382,#66383,#66384,#66385,#66386,#66387,#66388,#66389,#66390,#66391,
#66392,#66393,#66394,#66395,#66396,#66397,#66398,#66399,#66400,#66401,#66402,
#66403,#66404,#66405,#66406,#66407,#66408,#66409,#66410,#66411,#66412,#66413,
#66414,#66415),.UNSPECIFIED.,.F.,.F.,(4,3,3,3,3,3,3,3,3,3,3,3,3,3,3,3,3,
3,3,3,3,3,3,3,4),(76.380801467099,76.4737435786687,76.5665890335125,76.6593690393854,
76.7521154870988,76.8448531975143,76.9376069776423,77.0304608283556,77.1233679280772,
77.2164285534006,77.2812773082049,77.3743526166739,77.4673018677554,77.5601526940849,
77.6529356995276,77.7456835541712,77.8384210804444,77.9311730856486,78.0240242845606,
78.116927302723,78.2099856439365,78.2807924467317,78.4009736434012,78.5186931112108,
78.5398163394889),.UNSPECIFIED.);
#7739=B_SPLINE_CURVE_WITH_KNOTS('',3,(#66417,#66418,#66419,#66420,#66421,
#66422,#66423,#66424,#66425,#66426,#66427,#66428,#66429,#66430,#66431,#66432,
#66433,#66434,#66435,#66436,#66437,#66438,#66439,#66440,#66441,#66442,#66443,
#66444,#66445,#66446,#66447,#66448,#66449,#66450,#66451,#66452,#66453,#66454,
#66455,#66456,#66457,#66458,#66459,#66460,#66461,#66462,#66463,#66464,#66465,
#66466,#66467,#66468,#66469,#66470,#66471,#66472,#66473,#66474,#66475,#66476,
#66477,#66478,#66479,#66480,#66481,#66482,#66483,#66484,#66485,#66486,#66487,
#66488,#66489,#66490,#66491,#66492,#66493,#66494,#66495,#66496,#66497,#66498,
#66499,#66500,#66501,#66502,#66503,#66504,#66505,#66506,#66507,#66508,#66509,
#66510,#66511,#66512,#66513,#66514,#66515,#66516,#66517,#66518,#66519,#66520,
#66521,#66522,#66523,#66524,#66525,#66526,#66527,#66528,#66529,#66530,#66531,
#66532,#66533,#66534,#66535,#66536,#66537,#66538,#66539,#66540,#66541,#66542,
#66543,#66544,#66545,#66546,#66547,#66548,#66549,#66550,#66551,#66552,#66553,
#66554,#66555,#66556,#66557,#66558,#66559,#66560,#66561,#66562,#66563,#66564,
#66565,#66566,#66567,#66568,#66569,#66570,#66571,#66572,#66573,#66574,#66575,
#66576,#66577,#66578),.UNSPECIFIED.,.F.,.F.,(4,2,2,2,2,2,2,2,2,2,2,2,2,
2,2,2,2,2,2,2,2,2,2,2,2,2,2,2,2,2,2,2,2,2,2,2,2,2,2,2,2,2,2,2,2,2,2,2,2,
2,2,2,2,2,2,2,2,2,2,2,2,2,2,2,2,2,2,2,2,2,2,2,2,2,2,2,2,2,2,2,4),(-0.696237685186134,
-0.675519558018449,-0.63707121428382,-0.633868815383757,-0.632289699751432,
-0.631151450179954,-0.62994933489026,-0.628297395338522,-0.626437311549927,
-0.623224737378464,-0.59937290706623,-0.551993457336766,-0.480880591906853,
-0.475023217996447,-0.472256733081436,-0.470093047332004,-0.467733078494461,
-0.463937163530348,-0.451147023877335,-0.430349155678461,-0.37587278332947,
-0.348494934235186,-0.316229019233684,-0.312760130818892,-0.311180063771606,
-0.3100031458416,-0.309999456281614,-0.309995806463445,-0.309992189866261,
-0.309988606157959,-0.309985054915406,-0.309981535819848,-0.309978048491879,
-0.309974592527943,-0.309971167610816,-0.309967773405964,-0.309964409568612,
-0.309961075745882,-0.309957771642774,-0.309954496902071,-0.30995125121917,
-0.309948034197928,-0.309944845575585,-0.30994168509736,-0.309938552419312,
-0.309935447209036,-0.309932369207409,-0.309929318090706,-0.309926293635987,
-0.30992329550613,-0.309920323410833,-0.309917377125776,-0.309915182175273,
-0.309912971521832,-0.309910765262554,-0.309908563412812,-0.309906365965786,
-0.309904172890775,-0.309901984153585,-0.309899799744197,-0.309897619594419,
-0.309895443784985,-0.309893272298244,-0.30989110505302,-0.308550667851128,
-0.307131486242876,-0.304997177291619,-0.301101797104602,-0.292132144811765,
-0.262433051302041,-0.164279929548461,-0.162678479377572,-0.154449448137997,
-0.151129851316645,-0.149090120683716,-0.146889582561246,-0.143911480787282,
-0.137139189781584,-0.128027141416022,-0.104998842794788,-0.000961222373964137),
 .UNSPECIFIED.);
#7740=B_SPLINE_CURVE_WITH_KNOTS('',3,(#66579,#66580,#66581,#66582,#66583,
#66584,#66585,#66586,#66587,#66588,#66589,#66590,#66591,#66592,#66593,#66594,
#66595,#66596,#66597,#66598,#66599,#66600,#66601,#66602,#66603,#66604,#66605,
#66606,#66607,#66608,#66609,#66610,#66611,#66612,#66613,#66614,#66615,#66616,
#66617,#66618,#66619,#66620,#66621,#66622,#66623,#66624,#66625,#66626,#66627,
#66628,#66629,#66630,#66631,#66632,#66633,#66634,#66635,#66636,#66637,#66638,
#66639,#66640,#66641,#66642,#66643,#66644,#66645,#66646,#66647,#66648,#66649,
#66650,#66651,#66652,#66653,#66654,#66655,#66656,#66657,#66658,#66659,#66660,
#66661,#66662,#66663,#66664,#66665,#66666,#66667,#66668,#66669,#66670,#66671,
#66672,#66673,#66674,#66675,#66676,#66677,#66678,#66679,#66680,#66681,#66682,
#66683,#66684,#66685,#66686,#66687,#66688,#66689,#66690,#66691,#66692,#66693,
#66694,#66695,#66696,#66697,#66698,#66699,#66700,#66701,#66702,#66703,#66704,
#66705,#66706,#66707,#66708,#66709,#66710,#66711,#66712,#66713,#66714,#66715,
#66716,#66717,#66718,#66719,#66720,#66721,#66722,#66723,#66724,#66725,#66726,
#66727,#66728,#66729,#66730,#66731,#66732,#66733,#66734,#66735,#66736,#66737,
#66738,#66739,#66740,#66741,#66742,#66743,#66744,#66745,#66746,#66747,#66748,
#66749,#66750,#66751,#66752,#66753,#66754),.UNSPECIFIED.,.F.,.F.,(4,2,2,
2,2,2,2,2,2,2,2,2,2,2,2,2,2,2,2,2,2,2,2,2,2,2,2,2,2,2,2,2,2,2,2,2,2,2,2,
2,2,2,2,2,2,2,2,2,2,2,2,2,2,2,2,2,2,2,2,2,2,2,2,2,2,2,2,2,2,2,2,2,2,2,2,
2,2,2,2,2,2,2,2,2,2,2,2,4),(-4.05943779606569,-4.05345026639121,-4.04937125481813,
-4.04778731189876,-4.04658704028464,-4.04542945739733,-4.04427265622474,
-4.04231135777569,-4.03703563664029,-4.02875353085773,-3.95031088242969,
-3.92314694508256,-3.89313164899935,-3.88818239634357,-3.88556062224259,
-3.88340436345589,-3.88089933367909,-3.8766058757658,-3.86029037889877,
-3.85691847335429,-3.84967007276564,-3.83128400784498,-3.7578363111733,
-3.73768340141623,-3.73077027769674,-3.72754503646094,-3.7256764746319,
-3.72401795386332,-3.72280903317128,-3.7216637241096,-3.72007428244317,
-3.71684927119908,-3.67775103490949,-3.63533718282447,-3.57269258993827,
-3.56634300135146,-3.56344278369877,-3.56125578350722,-3.55919647411765,
-3.55577034916008,-3.54689076585914,-3.4449722742975,-3.40946946957931,
-3.4055134280881,-3.40335586861807,-3.40192725752373,-3.40058160606482,
-3.39940508476045,-3.39786762443795,-3.39473597666216,-3.37468828546699,
-3.28193568244436,-3.25930760931743,-3.24567235800386,-3.24177351831663,
-3.23938140286203,-3.23720925216673,-3.23441465623715,-3.22861866947255,
-3.15261089554197,-3.08915493135136,-3.08119750761457,-3.07898443646193,
-3.07764351047602,-3.07642474020449,-3.07483418114361,-3.07146685277802,
-3.04290505166636,-3.00097468545075,-2.92786175903349,-2.92093316603533,
-2.91792795207206,-2.91572328851612,-2.91369092657029,-2.91093587962425,
-2.90554190084967,-2.84431123868312,-2.79134437728056,-2.76985703612609,
-2.75893672734631,-2.75647660291086,-2.75508072570095,-2.75387277482531,
-2.75234856053968,-2.7493806904627,-2.73211639887814,-2.73136055880086,
-2.72791817214398),.UNSPECIFIED.);
#7741=B_SPLINE_CURVE_WITH_KNOTS('',3,(#66760,#66761,#66762,#66763,#66764,
#66765,#66766,#66767,#66768,#66769,#66770,#66771,#66772,#66773,#66774,#66775,
#66776,#66777,#66778,#66779,#66780,#66781,#66782,#66783,#66784,#66785,#66786,
#66787,#66788,#66789,#66790,#66791,#66792,#66793,#66794,#66795,#66796,#66797,
#66798,#66799,#66800,#66801,#66802,#66803,#66804,#66805,#66806,#66807,#66808,
#66809,#66810,#66811,#66812,#66813,#66814,#66815,#66816,#66817,#66818,#66819,
#66820,#66821,#66822,#66823,#66824,#66825,#66826,#66827,#66828,#66829,#66830,
#66831,#66832,#66833,#66834,#66835,#66836,#66837,#66838,#66839,#66840,#66841,
#66842,#66843,#66844,#66845,#66846,#66847,#66848,#66849,#66850,#66851,#66852,
#66853,#66854,#66855,#66856,#66857,#66858,#66859,#66860,#66861,#66862,#66863,
#66864,#66865,#66866,#66867,#66868,#66869,#66870,#66871,#66872,#66873,#66874,
#66875,#66876,#66877,#66878,#66879,#66880,#66881,#66882,#66883,#66884,#66885,
#66886,#66887,#66888,#66889,#66890,#66891,#66892,#66893,#66894,#66895,#66896,
#66897,#66898),.UNSPECIFIED.,.F.,.F.,(4,3,3,3,3,3,3,3,3,3,3,3,3,3,3,3,3,
3,3,3,3,3,3,3,3,3,3,3,3,3,3,3,3,3,3,3,3,3,3,3,3,3,3,3,3,3,4),(84.8230016471138,
84.9221960598312,85.0217585077651,85.1215123023174,85.2215704894812,85.277398416419,
85.3704737248879,85.4634229759694,85.5562738022989,85.6490568077416,85.7418046623852,
85.8345421886584,85.9272941938625,86.0201453927745,86.1130484109369,86.2061067521504,
86.2769135549458,86.3699888634147,86.4629381144963,86.5557889408258,86.6485719462685,
86.7413198009121,86.8340573271853,86.9268093323895,87.0196605313014,87.1125635494638,
87.2056218906773,87.2764286934725,87.3695040019414,87.4624532530229,87.5553040793525,
87.6480870847952,87.7408349394388,87.833572465712,87.9263244709162,88.0191756698281,
88.1120786879905,88.205137029204,88.2759438319993,88.3690008063904,88.461940195998,
88.5547870208806,88.6475662149387,88.740312112707,88.8330399906779,88.925793178824,
88.9462551936448),.UNSPECIFIED.);
#7742=B_SPLINE_CURVE_WITH_KNOTS('',3,(#66899,#66900,#66901,#66902,#66903,
#66904,#66905,#66906,#66907,#66908,#66909,#66910,#66911,#66912,#66913,#66914,
#66915,#66916,#66917,#66918,#66919,#66920,#66921,#66922,#66923,#66924,#66925,
#66926,#66927,#66928,#66929,#66930,#66931,#66932,#66933,#66934,#66935,#66936,
#66937,#66938,#66939,#66940,#66941,#66942,#66943,#66944,#66945,#66946,#66947,
#66948,#66949,#66950,#66951,#66952,#66953,#66954,#66955,#66956,#66957,#66958,
#66959,#66960,#66961,#66962,#66963,#66964,#66965,#66966,#66967,#66968,#66969,
#66970,#66971),.UNSPECIFIED.,.F.,.F.,(4,3,3,3,3,3,3,3,3,3,3,3,3,3,3,3,3,
3,3,3,3,3,3,3,4),(82.663879402628,82.756624238485,82.8493623215592,82.9421184586138,
83.034975745376,83.1278880647113,83.2209516972694,83.2783681393655,83.3714434478346,
83.4643926989164,83.5572435252462,83.6500265306889,83.7427743853325,83.8355119116059,
83.9282639168099,84.0211151157219,84.1140181338843,84.2070764750979,84.2778832778922,
84.3739789574075,84.4699157807353,84.5656692160942,84.6613146280951,84.7568461508212,
84.8230016469248),.UNSPECIFIED.);
#7743=B_SPLINE_CURVE_WITH_KNOTS('',3,(#66972,#66973,#66974,#66975,#66976,
#66977,#66978,#66979,#66980,#66981,#66982,#66983,#66984,#66985,#66986,#66987,
#66988,#66989,#66990,#66991,#66992,#66993,#66994,#66995,#66996,#66997,#66998,
#66999,#67000,#67001,#67002,#67003,#67004,#67005,#67006,#67007,#67008,#67009,
#67010,#67011,#67012,#67013,#67014,#67015,#67016,#67017,#67018,#67019,#67020,
#67021,#67022,#67023,#67024,#67025,#67026,#67027,#67028,#67029,#67030,#67031,
#67032,#67033,#67034,#67035,#67036,#67037,#67038,#67039,#67040,#67041,#67042,
#67043,#67044,#67045,#67046,#67047,#67048,#67049,#67050,#67051,#67052,#67053,
#67054,#67055,#67056,#67057,#67058,#67059,#67060,#67061,#67062,#67063,#67064,
#67065,#67066,#67067,#67068,#67069,#67070,#67071,#67072,#67073,#67074,#67075,
#67076,#67077,#67078,#67079,#67080,#67081,#67082,#67083,#67084,#67085,#67086,
#67087,#67088,#67089,#67090,#67091,#67092,#67093,#67094,#67095,#67096,#67097,
#67098,#67099,#67100,#67101,#67102,#67103,#67104,#67105,#67106,#67107,#67108,
#67109,#67110,#67111,#67112,#67113,#67114,#67115,#67116,#67117,#67118,#67119,
#67120,#67121,#67122,#67123,#67124,#67125,#67126,#67127,#67128,#67129,#67130,
#67131,#67132,#67133,#67134,#67135,#67136,#67137,#67138,#67139,#67140,#67141,
#67142,#67143,#67144,#67145,#67146,#67147,#67148,#67149,#67150,#67151,#67152,
#67153,#67154,#67155,#67156,#67157,#67158,#67159,#67160,#67161,#67162,#67163,
#67164,#67165,#67166,#67167,#67168,#67169,#67170,#67171,#67172,#67173,#67174,
#67175,#67176,#67177,#67178,#67179,#67180,#67181,#67182,#67183,#67184,#67185,
#67186,#67187,#67188,#67189,#67190,#67191,#67192,#67193,#67194,#67195,#67196,
#67197,#67198,#67199,#67200,#67201,#67202,#67203,#67204,#67205,#67206,#67207,
#67208,#67209,#67210,#67211,#67212,#67213,#67214,#67215),.UNSPECIFIED.,
 .F.,.F.,(4,2,2,2,2,2,2,2,2,2,2,2,2,2,2,2,2,2,2,2,2,2,2,2,2,2,2,2,2,2,2,
2,2,2,2,2,2,2,2,2,2,2,2,2,2,2,2,2,2,2,2,2,2,2,2,2,2,2,2,2,2,2,2,2,2,2,2,
2,2,2,2,2,2,2,2,2,2,2,2,2,2,2,2,2,2,2,2,2,2,2,2,2,2,2,2,2,2,2,2,2,2,2,2,
2,2,2,2,2,2,2,2,2,2,2,2,2,2,2,2,2,2,4),(-2.72791817214398,-2.72757626591806,
-2.63606423622718,-2.61364743619176,-2.60010597703889,-2.59621670021499,
-2.59382673984744,-2.59165410327153,-2.58885545353705,-2.58303863684278,
-2.53777278075375,-2.46757445614939,-2.4468006529931,-2.43612968947032,
-2.43368754860676,-2.4322956772014,-2.4310873152038,-2.42955755808693,-2.42656376975906,
-2.40879609562139,-2.40362799523738,-2.36164703988015,-2.31387673393604,
-2.29115522479557,-2.27747843013807,-2.27357525369854,-2.27118208793889,
-2.26901004012297,-2.26621705573284,-2.26042974982179,-2.18406065452215,
-2.13955489082282,-2.12253517903094,-2.11324633531875,-2.11091222739375,
-2.10954426436202,-2.10833205980341,-2.10676469062215,-2.10348165207084,
-2.0793708307666,-2.07038120131137,-2.03098267213065,-2.00150754288925,
-1.98320508308051,-1.9569259361281,-1.95234162313692,-1.94954767734819,
-1.94736904150918,-1.94499935936886,-1.94120222235277,-1.9285404958871,
-1.90806703907829,-1.86348636951593,-1.85221772371789,-1.79250429774525,
-1.78936577225568,-1.78779773404084,-1.78665788573919,-1.78541928043255,
-1.78368315126966,-1.77946496675649,-1.77353820369554,-1.75739282920614,
-1.73312304476404,-1.67426543170373,-1.66107005697728,-1.65678086589297,
-1.63388940415156,-1.62949949223706,-1.62673412195209,-1.62456520901261,
-1.62215669461167,-1.618185424533,-1.60382042053993,-1.57951830025907,-1.47524112956354,
-1.46763106527624,-1.46535938045523,-1.46400507216974,-1.46291118894332,
-1.46138455471068,-1.45830817447062,-1.43196075869977,-1.38442482316929,
-1.31258924828251,-1.30669155012857,-1.30390667812202,-1.30172889928891,
-1.29935385059284,-1.2955343206081,-1.28267057289477,-1.26175827083863,
-1.18787387231184,-1.14697220243633,-1.14373246823237,-1.14213897733664,
-1.14099222527729,-1.13975828868846,-1.1380491629104,-1.13399267647375,
-1.12835480743113,-1.05489408021853,-0.989838763503215,-0.984451155629457,
-0.98169725921509,-0.979664731717884,-0.977458909751686,-0.974450370147237,
-0.967506352156097,-0.958102665041172,-0.934031818129519,-0.831849242160278,
-0.822171057473247,-0.819712181452299,-0.818301385567433,-0.817094137215332,
-0.815588126430419,-0.812613955076298,-0.790352774030541,-0.752809828950054,
-0.72170275952839,-0.698709454689423),.UNSPECIFIED.);
#7744=B_SPLINE_CURVE_WITH_KNOTS('',3,(#67221,#67222,#67223,#67224,#67225,
#67226,#67227,#67228,#67229,#67230,#67231,#67232,#67233,#67234,#67235,#67236,
#67237,#67238,#67239,#67240,#67241,#67242,#67243,#67244,#67245,#67246,#67247,
#67248,#67249,#67250,#67251,#67252,#67253,#67254,#67255,#67256,#67257,#67258,
#67259,#67260,#67261,#67262,#67263,#67264,#67265,#67266,#67267,#67268,#67269,
#67270,#67271,#67272,#67273,#67274,#67275,#67276,#67277,#67278,#67279,#67280,
#67281,#67282,#67283,#67284,#67285,#67286,#67287,#67288,#67289,#67290,#67291,
#67292,#67293,#67294,#67295,#67296,#67297,#67298,#67299,#67300,#67301,#67302,
#67303,#67304,#67305,#67306,#67307,#67308,#67309,#67310,#67311,#67312,#67313,
#67314,#67315,#67316,#67317,#67318,#67319,#67320,#67321,#67322,#67323,#67324,
#67325,#67326,#67327,#67328,#67329,#67330,#67331,#67332,#67333,#67334,#67335,
#67336,#67337,#67338,#67339,#67340,#67341,#67342,#67343,#67344,#67345,#67346,
#67347,#67348,#67349,#67350,#67351,#67352,#67353,#67354,#67355,#67356,#67357,
#67358,#67359),.UNSPECIFIED.,.F.,.F.,(4,3,3,3,3,3,3,3,3,3,3,3,3,3,3,3,3,
3,3,3,3,3,3,3,3,3,3,3,3,3,3,3,3,3,3,3,3,3,3,3,3,3,3,3,3,3,4),(91.1061869541044,
91.2531720643649,91.2744892475796,91.3675645560485,91.46051380713,91.5533646334596,
91.6461476389023,91.7388954935459,91.8316330198191,91.9243850250232,92.0172362239352,
92.1101392420976,92.2031975833111,92.2740043861063,92.3670796945753,92.4600289456567,
92.5528797719863,92.6456627774291,92.7384106320726,92.8311481583459,92.9239001635501,
93.0167513624621,93.1096543806244,93.2027127218379,93.2735195246331,93.366594833102,
93.4595440841836,93.5523949105131,93.6451779159559,93.7379257705994,93.8306632968727,
93.9234153020768,94.0162665009888,94.1091695191512,94.2022278603647,94.2730346631599,
94.3661126845117,94.4590639501153,94.5553905369303,94.6481700190462,94.7409142923435,
94.8336481781563,94.9263964823739,95.0192322633309,95.11212029076,95.2051350095969,
95.2296766446352),.UNSPECIFIED.);
#7745=B_SPLINE_CURVE_WITH_KNOTS('',3,(#67360,#67361,#67362,#67363,#67364,
#67365,#67366,#67367,#67368,#67369,#67370,#67371,#67372,#67373,#67374,#67375,
#67376,#67377,#67378,#67379,#67380,#67381,#67382,#67383,#67384,#67385,#67386,
#67387,#67388,#67389,#67390,#67391,#67392,#67393,#67394,#67395,#67396,#67397,
#67398,#67399,#67400,#67401,#67402,#67403,#67404,#67405,#67406,#67407,#67408,
#67409,#67410,#67411,#67412,#67413,#67414,#67415,#67416,#67417,#67418,#67419,
#67420,#67421,#67422,#67423,#67424,#67425,#67426,#67427,#67428,#67429,#67430,
#67431,#67432),.UNSPECIFIED.,.F.,.F.,(4,3,3,3,3,3,3,3,3,3,3,3,3,3,3,3,3,
3,3,3,3,3,3,3,4),(88.9462551936448,89.0391158747113,89.1320332819789,89.2250999323282,
89.2754589705261,89.368534278995,89.4614835300766,89.5543343564061,89.6471173618489,
89.7398652164924,89.8326027427657,89.9253547479699,90.0182059468818,90.1111089650442,
90.2041673062577,90.2749741090528,90.3666596755061,90.4591005853075,90.5505540119022,
90.6419502073382,90.7333153498863,90.8265332508942,90.9179528502677,91.0120699020928,
91.1061869539178),.UNSPECIFIED.);
#7746=B_SPLINE_CURVE_WITH_KNOTS('',3,(#67434,#67435,#67436,#67437,#67438,
#67439,#67440,#67441,#67442,#67443,#67444,#67445,#67446,#67447,#67448,#67449,
#67450,#67451,#67452,#67453,#67454,#67455,#67456,#67457,#67458,#67459,#67460,
#67461,#67462,#67463,#67464,#67465,#67466,#67467,#67468,#67469,#67470,#67471,
#67472,#67473,#67474,#67475,#67476,#67477,#67478,#67479,#67480,#67481,#67482,
#67483,#67484,#67485,#67486,#67487,#67488,#67489,#67490,#67491,#67492,#67493,
#67494,#67495,#67496,#67497,#67498,#67499,#67500,#67501,#67502,#67503,#67504,
#67505,#67506,#67507,#67508,#67509,#67510,#67511,#67512,#67513,#67514,#67515,
#67516,#67517,#67518,#67519,#67520,#67521,#67522,#67523,#67524,#67525,#67526,
#67527,#67528,#67529),.UNSPECIFIED.,.F.,.F.,(4,2,2,2,2,2,2,2,2,2,2,2,2,
2,2,2,2,2,2,2,2,2,2,2,2,2,2,2,2,2,2,2,2,2,2,2,2,2,2,2,2,2,2,2,2,2,2,4),
(-0.698709454689423,-0.666843047260533,-0.661476341095949,-0.65872745721161,
-0.656695869584792,-0.654533359844537,-0.651607160765785,-0.648348827884347,
-0.642816925899491,-0.60419136741942,-0.522692176465372,-0.518714738765864,
-0.500239647899331,-0.49721286352588,-0.495675406849351,-0.494465613389275,
-0.493077291147427,-0.490653923314244,-0.480253064841465,-0.460248997720133,
-0.432060003842914,-0.393483763796674,-0.343849805060601,-0.337942919617727,
-0.335155682029959,-0.333024184723614,-0.330711578533513,-0.328309636399378,
-0.324834993657877,-0.318771010917819,-0.272728776753478,-0.221750380227524,
-0.178215503478459,-0.174605378645141,-0.172992857261096,-0.17177004161356,
-0.170438198229673,-0.16826830305091,-0.160748296120402,-0.104322696345831,
-0.0266090166975272,-0.0167918801592759,-0.0132205824828429,-0.0111319304901992,
-0.00903511934187455,-0.00692965682314765,-0.00390544029746683,-0.000960255622328456),
 .UNSPECIFIED.);
#7747=B_SPLINE_CURVE_WITH_KNOTS('',3,(#67530,#67531,#67532,#67533,#67534,
#67535,#67536,#67537,#67538,#67539,#67540,#67541,#67542,#67543,#67544,#67545,
#67546,#67547,#67548,#67549,#67550,#67551,#67552,#67553,#67554,#67555,#67556,
#67557,#67558,#67559,#67560,#67561,#67562,#67563,#67564,#67565,#67566,#67567,
#67568,#67569,#67570,#67571,#67572,#67573,#67574,#67575,#67576,#67577,#67578,
#67579,#67580,#67581,#67582,#67583,#67584,#67585,#67586,#67587,#67588,#67589,
#67590,#67591,#67592,#67593,#67594,#67595,#67596,#67597,#67598,#67599,#67600,
#67601,#67602,#67603,#67604,#67605,#67606,#67607,#67608,#67609,#67610,#67611,
#67612,#67613,#67614,#67615,#67616,#67617,#67618,#67619,#67620,#67621,#67622,
#67623,#67624,#67625,#67626,#67627,#67628,#67629,#67630,#67631,#67632,#67633,
#67634,#67635,#67636,#67637,#67638,#67639,#67640,#67641,#67642,#67643,#67644,
#67645,#67646,#67647,#67648,#67649,#67650,#67651,#67652,#67653,#67654,#67655,
#67656,#67657,#67658,#67659,#67660,#67661,#67662,#67663,#67664,#67665,#67666,
#67667,#67668,#67669,#67670,#67671,#67672,#67673,#67674,#67675,#67676,#67677,
#67678,#67679,#67680,#67681,#67682,#67683,#67684,#67685,#67686,#67687,#67688,
#67689,#67690,#67691,#67692,#67693,#67694,#67695,#67696,#67697,#67698,#67699,
#67700,#67701,#67702,#67703,#67704,#67705,#67706,#67707,#67708,#67709,#67710,
#67711,#67712,#67713,#67714,#67715,#67716,#67717,#67718,#67719,#67720,#67721,
#67722,#67723,#67724,#67725,#67726,#67727,#67728,#67729,#67730,#67731,#67732,
#67733,#67734,#67735,#67736,#67737,#67738,#67739,#67740,#67741,#67742,#67743,
#67744,#67745),.UNSPECIFIED.,.F.,.F.,(4,2,2,2,2,2,2,2,2,2,2,2,2,2,2,2,2,
2,2,2,2,2,2,2,2,2,2,2,2,2,2,2,2,2,2,2,2,2,2,2,2,2,2,2,2,2,2,2,2,2,2,2,2,
2,2,2,2,2,2,2,2,2,2,2,2,2,2,2,2,2,2,2,2,2,2,2,2,2,2,2,2,2,2,2,2,2,2,2,2,
2,2,2,2,2,2,2,2,2,2,2,2,2,2,2,2,2,2,4),(-4.07343079861933,-4.05868086012299,
-4.00070276921845,-3.94757887152325,-3.93322662474479,-3.92499404069726,
-3.92274888238868,-3.92139757638515,-3.92017571218205,-3.91858954295225,
-3.91513791088693,-3.88524540260387,-3.84114529928722,-3.76918518529934,
-3.76518640952024,-3.76256311752847,-3.76009117896046,-3.76007768496206,
-3.76006641279559,-3.76005478721725,-3.76004279342015,-3.76003041574761,
-3.76001763766328,-3.76000444167587,-3.75999080921395,-3.75997672065096,
-3.7599621551369,-3.75994709050131,-3.75993150320342,-3.75991536818062,
-3.75989865870716,-3.75988134626247,-3.75986340042684,-3.75984478867069,
-3.75982547613537,-3.75980542545279,-3.75978459651623,-3.7597629461998,
-3.75974042808431,-3.75971699210076,-3.75969258416886,-3.75966714577552,
-3.75964061362145,-3.75961407793517,-3.75747458745472,-3.75467131028805,
-3.74903269843729,-3.67049183693619,-3.62629931062385,-3.61011557126601,
-3.60417269546198,-3.59994234018484,-3.5982003266796,-3.59695721127157,
-3.59581297562757,-3.59423857414969,-3.5910863099696,-3.53129239165828,
-3.48233396966627,-3.44807027094141,-3.44286467798937,-3.43973730486539,
-3.43690281053057,-3.43475000691286,-3.43268445406497,-3.42925470231979,
-3.42040355244149,-3.41907416512816,-3.33567645248822,-3.29983126820865,
-3.28534028525411,-3.27705013432687,-3.27479938695166,-3.27344676232086,
-3.27222512888126,-3.27064114535644,-3.26800028572343,-3.25221357285803,
-3.18228815148936,-3.12209639384945,-3.11578947928084,-3.11289038014352,
-3.11069660767051,-3.10862529989861,-3.10573986943086,-3.09821343094713,
-3.09470483027559,-3.01714854722788,-2.96042814404654,-2.95287698461928,
-2.95069935961224,-2.9493630513823,-2.94813633708804,-2.94651895044135,
-2.94289906091532,-2.89964953477856,-2.88756018818637,-2.82321089587945,
-2.79577825945987,-2.79092530355689,-2.78831755263476,-2.78617382284054,
-2.78364519987737,-2.77927657401761,-2.76227589742534,-2.75942583678824,
-2.7523504486624,-2.73686895463578),.UNSPECIFIED.);
#7748=B_SPLINE_CURVE_WITH_KNOTS('',3,(#67751,#67752,#67753,#67754,#67755,
#67756,#67757,#67758,#67759,#67760,#67761,#67762,#67763,#67764,#67765,#67766,
#67767,#67768,#67769,#67770,#67771,#67772,#67773,#67774,#67775,#67776,#67777,
#67778,#67779,#67780,#67781,#67782,#67783,#67784,#67785,#67786,#67787,#67788,
#67789,#67790,#67791,#67792,#67793,#67794,#67795,#67796,#67797,#67798,#67799,
#67800,#67801,#67802,#67803,#67804,#67805,#67806,#67807,#67808,#67809,#67810,
#67811,#67812,#67813,#67814,#67815,#67816,#67817,#67818,#67819,#67820,#67821,
#67822,#67823,#67824,#67825,#67826,#67827,#67828,#67829,#67830,#67831,#67832,
#67833,#67834,#67835,#67836,#67837,#67838,#67839,#67840,#67841,#67842,#67843,
#67844,#67845,#67846,#67847,#67848,#67849,#67850,#67851,#67852,#67853,#67854,
#67855,#67856,#67857,#67858,#67859,#67860,#67861,#67862,#67863,#67864,#67865,
#67866,#67867,#67868,#67869,#67870,#67871,#67872,#67873,#67874,#67875,#67876,
#67877,#67878,#67879,#67880,#67881,#67882,#67883,#67884,#67885,#67886,#67887,
#67888,#67889),.UNSPECIFIED.,.F.,.F.,(4,3,3,3,3,3,3,3,3,3,3,3,3,3,3,3,3,
3,3,3,3,3,3,3,3,3,3,3,3,3,3,3,3,3,3,3,3,3,3,3,3,3,3,3,3,3,4),(97.389372261552,
97.4811078775329,97.5727347819261,97.6642817274812,97.7557867563104,97.8472759289302,
97.9387752853951,98.0303675879002,98.1220101752803,98.2138004326156,98.2710952172669,
98.3641705257358,98.4571197768173,98.5499706031467,98.6427536085893,98.7355014632329,
98.828238989506,98.9209909947099,99.0138421936218,99.1067452117843,99.1998035529977,
99.2706103557937,99.3636856642626,99.4566349153438,99.5494857416735,99.6422687471163,
99.7350166017598,99.8277541280328,99.9205061332367,100.013357332149,100.106260350311,
100.199318691524,100.27012549432,100.363200802789,100.45615005387,100.5490008802,
100.641783885643,100.734531740286,100.827269266559,100.920021271764,101.012872470675,
101.105775488838,101.198833830051,101.269640632847,101.362717406679,101.455655050019,
101.513685257635),.UNSPECIFIED.);
#7749=B_SPLINE_CURVE_WITH_KNOTS('',3,(#67890,#67891,#67892,#67893,#67894,
#67895,#67896,#67897,#67898,#67899,#67900,#67901,#67902,#67903,#67904,#67905,
#67906,#67907,#67908,#67909,#67910,#67911,#67912,#67913,#67914,#67915,#67916,
#67917,#67918,#67919,#67920,#67921,#67922,#67923,#67924,#67925,#67926,#67927,
#67928,#67929,#67930,#67931,#67932,#67933,#67934,#67935,#67936,#67937,#67938,
#67939,#67940,#67941,#67942,#67943,#67944,#67945,#67946,#67947,#67948,#67949,
#67950,#67951,#67952,#67953,#67954,#67955,#67956,#67957,#67958,#67959,#67960,
#67961,#67962),.UNSPECIFIED.,.F.,.F.,(4,3,3,3,3,3,3,3,3,3,3,3,3,3,3,3,3,
3,3,3,3,3,3,3,4),(95.2296766446352,95.2725498016866,95.3656251101555,95.4585743612371,
95.5514251875666,95.6442081930094,95.736956047653,95.8296935739262,95.9224455791303,
96.0152967780422,96.1081997962046,96.2012581374181,96.2720649402134,96.3651402486823,
96.458089499764,96.5509403260934,96.6437233315362,96.7364711861798,96.829208712453,
96.9219607176573,97.0148119165692,97.1077149347317,97.2007732759451,97.2715800787402,
97.389372261284),.UNSPECIFIED.);
#7750=B_SPLINE_CURVE_WITH_KNOTS('',3,(#67963,#67964,#67965,#67966,#67967,
#67968,#67969,#67970,#67971,#67972,#67973,#67974,#67975,#67976,#67977,#67978,
#67979,#67980,#67981,#67982,#67983,#67984,#67985,#67986,#67987,#67988,#67989,
#67990,#67991,#67992,#67993,#67994,#67995,#67996,#67997,#67998,#67999,#68000,
#68001,#68002,#68003,#68004,#68005,#68006,#68007,#68008,#68009,#68010,#68011,
#68012,#68013,#68014,#68015,#68016,#68017,#68018,#68019,#68020,#68021,#68022,
#68023,#68024,#68025,#68026,#68027,#68028,#68029,#68030,#68031,#68032,#68033,
#68034,#68035,#68036,#68037,#68038,#68039,#68040,#68041,#68042,#68043,#68044,
#68045,#68046,#68047,#68048,#68049,#68050,#68051,#68052,#68053,#68054,#68055,
#68056,#68057,#68058,#68059,#68060,#68061,#68062,#68063,#68064,#68065,#68066,
#68067,#68068,#68069,#68070,#68071,#68072,#68073,#68074,#68075,#68076,#68077,
#68078,#68079,#68080,#68081,#68082,#68083,#68084,#68085,#68086,#68087,#68088,
#68089,#68090,#68091,#68092,#68093,#68094,#68095,#68096,#68097,#68098,#68099,
#68100,#68101,#68102,#68103,#68104,#68105,#68106,#68107,#68108,#68109,#68110,
#68111,#68112,#68113,#68114,#68115,#68116,#68117,#68118,#68119,#68120,#68121,
#68122,#68123,#68124,#68125,#68126,#68127,#68128,#68129,#68130,#68131,#68132,
#68133,#68134,#68135,#68136,#68137,#68138,#68139,#68140,#68141,#68142,#68143,
#68144,#68145,#68146,#68147,#68148,#68149,#68150,#68151,#68152,#68153,#68154,
#68155,#68156,#68157,#68158,#68159,#68160,#68161,#68162,#68163,#68164,#68165,
#68166,#68167,#68168,#68169,#68170,#68171,#68172,#68173,#68174,#68175,#68176,
#68177,#68178,#68179,#68180,#68181,#68182,#68183,#68184,#68185,#68186,#68187,
#68188,#68189,#68190,#68191,#68192,#68193,#68194,#68195,#68196,#68197,#68198),
 .UNSPECIFIED.,.F.,.F.,(4,2,2,2,2,2,2,2,2,2,2,2,2,2,2,2,2,2,2,2,2,2,2,2,
2,2,2,2,2,2,2,2,2,2,2,2,2,2,2,2,2,2,2,2,2,2,2,2,2,2,2,2,2,2,2,2,2,2,2,2,
2,2,2,2,2,2,2,2,2,2,2,2,2,2,2,2,2,2,2,2,2,2,2,2,2,2,2,2,2,2,2,2,2,2,2,2,
2,2,2,2,2,2,2,2,2,2,2,2,2,2,2,2,2,2,2,2,2,4),(-2.73686895463578,-2.73388730285763,
-2.66011865704339,-2.63988763936745,-2.6293958949297,-2.62696028404078,
-2.62556643453363,-2.62435276064524,-2.62281159969532,-2.61967941241045,
-2.59983448907064,-2.58191759228708,-2.53965441226648,-2.47516168097801,
-2.46814886853108,-2.46512174206217,-2.46290653940541,-2.46086833666914,
-2.4581112612923,-2.45273078577678,-2.39846961740717,-2.36789471114992,
-2.30864033319991,-2.30411095537683,-2.30232010844391,-2.30106744101009,
-2.29993312179565,-2.29839794978084,-2.29540098596644,-2.27026090131758,
-2.25842758730487,-2.21615921911973,-2.14971664683455,-2.14368826812459,
-2.14084178207042,-2.13865544145626,-2.13656674090385,-2.13301890294904,
-2.12340974795611,-2.03651462736593,-1.99755993244561,-1.98218304391205,
-1.97956310119471,-1.97798514365945,-1.97676418151719,-1.97540796471224,
-1.97314182278633,-1.96469028643018,-1.89264997288797,-1.82552428878395,
-1.82014081083182,-1.81738292016307,-1.81534447340827,-1.81312935298962,
-1.8101029698597,-1.80309471206197,-1.73997465401417,-1.69748958517456,
-1.67433022377027,-1.65820723893921,-1.65554908162721,-1.65395992169028,
-1.65273743118205,-1.65138723380575,-1.64914780072375,-1.6409780263386,
-1.62677989769963,-1.59201912493646,-1.50700320710355,-1.5040027496952,
-1.49645892661612,-1.49357055413664,-1.49149835632751,-1.48930476274978,
-1.48640779825481,-1.48011304796233,-1.42040269999896,-1.35099130777964,
-1.33420361338767,-1.33151255295096,-1.32991376317028,-1.32868986548002,
-1.32734455212532,-1.32512690971973,-1.31718074812204,-1.25420022609978,
-1.17713917059732,-1.17134014377745,-1.1685383275136,-1.16635798993175,
-1.16395425009545,-1.16003057412773,-1.14624918161625,-1.12332016493283,
-1.02892694259301,-1.01022124786251,-1.00717659223332,-1.00563227182597,
-1.00441819657332,-1.00302621045053,-1.00059944440604,-0.990228090045812,
-0.970336686344806,-0.894802018007452,-0.893861286757274,-0.892185982919815,
-0.878754979068072,-0.876472456611157,-0.851775628695121,-0.847261070117154,
-0.844452129634196,-0.842270673831992,-0.839870173828236,-0.835961861536232,
-0.822335439318625,-0.799757619653653,-0.707428796331635,-0.699700907542827),
 .UNSPECIFIED.);
#7751=B_SPLINE_CURVE_WITH_KNOTS('',3,(#68204,#68205,#68206,#68207,#68208,
#68209,#68210,#68211,#68212,#68213,#68214,#68215,#68216,#68217,#68218,#68219,
#68220,#68221,#68222,#68223,#68224,#68225,#68226,#68227,#68228,#68229,#68230,
#68231,#68232,#68233,#68234,#68235,#68236,#68237,#68238,#68239,#68240,#68241,
#68242,#68243,#68244,#68245,#68246,#68247,#68248,#68249,#68250,#68251,#68252,
#68253,#68254,#68255,#68256,#68257,#68258,#68259,#68260,#68261,#68262,#68263,
#68264,#68265,#68266,#68267,#68268,#68269,#68270,#68271,#68272,#68273,#68274,
#68275,#68276,#68277,#68278,#68279,#68280,#68281,#68282,#68283,#68284,#68285,
#68286,#68287,#68288,#68289,#68290,#68291,#68292,#68293,#68294,#68295,#68296,
#68297,#68298,#68299,#68300,#68301,#68302,#68303,#68304,#68305,#68306,#68307,
#68308,#68309,#68310,#68311,#68312,#68313,#68314,#68315,#68316,#68317,#68318,
#68319,#68320,#68321,#68322,#68323,#68324,#68325,#68326,#68327,#68328,#68329,
#68330,#68331,#68332,#68333,#68334,#68335,#68336,#68337,#68338,#68339,#68340,
#68341,#68342),.UNSPECIFIED.,.F.,.F.,(4,3,3,3,3,3,3,3,3,3,3,3,3,3,3,3,3,
3,3,3,3,3,3,3,3,3,3,3,3,3,3,3,3,3,3,3,3,3,3,3,3,3,3,3,3,3,4),(103.672557568464,
103.766647671507,103.860769614952,103.954945648423,104.049262783787,104.143661761202,
104.238228269711,104.268186048427,104.361261356896,104.454210607977,104.547061434307,
104.63984443975,104.732592294393,104.825329820666,104.91808182587,105.010933024782,
105.103836042945,105.196894384158,105.267701186954,105.360776495423,105.453725746505,
105.546576572834,105.639359578277,105.73210743292,105.824844959194,105.917596964398,
106.01044816331,106.103351181473,106.196409522686,106.267216325481,106.36029163395,
106.453240885032,106.546091711361,106.638874716804,106.731622571448,106.824360097721,
106.917112102925,107.009963301837,107.10286632,107.195924661213,107.266731464008,
107.359803164529,107.452753997043,107.545595921847,107.638373985326,107.731122073524,
107.796189056121),.UNSPECIFIED.);
#7752=B_SPLINE_CURVE_WITH_KNOTS('',3,(#68343,#68344,#68345,#68346,#68347,
#68348,#68349,#68350,#68351,#68352,#68353,#68354,#68355,#68356,#68357,#68358,
#68359,#68360,#68361,#68362,#68363,#68364,#68365,#68366,#68367,#68368,#68369,
#68370,#68371,#68372,#68373,#68374,#68375,#68376,#68377,#68378,#68379,#68380,
#68381,#68382,#68383,#68384,#68385,#68386,#68387,#68388,#68389,#68390,#68391,
#68392,#68393,#68394,#68395,#68396,#68397,#68398,#68399,#68400,#68401,#68402,
#68403,#68404,#68405,#68406,#68407,#68408,#68409,#68410,#68411,#68412),
 .UNSPECIFIED.,.F.,.F.,(4,3,3,3,3,3,3,3,3,3,3,3,3,3,3,3,3,3,3,3,3,3,3,4),
(101.513685257635,101.608119071853,101.700876645965,101.793615016353,101.886358993441,
101.982058187924,102.074941828636,102.172048800005,102.269155771374,102.362231079843,
102.455180330925,102.548031157254,102.640814162697,102.733562017341,102.826299543614,
102.919051548818,103.01190274773,103.104805765893,103.197864107106,103.268670909901,
103.371807499052,103.474650856928,103.576968184871,103.672557568288),
 .UNSPECIFIED.);
#7753=B_SPLINE_CURVE_WITH_KNOTS('',3,(#68414,#68415,#68416,#68417,#68418,
#68419,#68420,#68421,#68422,#68423,#68424,#68425,#68426,#68427,#68428,#68429,
#68430,#68431,#68432,#68433,#68434,#68435,#68436,#68437,#68438,#68439,#68440,
#68441,#68442,#68443,#68444,#68445,#68446,#68447,#68448,#68449,#68450,#68451,
#68452,#68453,#68454,#68455,#68456,#68457,#68458,#68459,#68460,#68461,#68462,
#68463,#68464,#68465,#68466,#68467,#68468,#68469,#68470,#68471,#68472,#68473,
#68474,#68475,#68476,#68477,#68478,#68479,#68480,#68481,#68482,#68483,#68484,
#68485,#68486,#68487,#68488,#68489,#68490,#68491,#68492,#68493,#68494,#68495,
#68496,#68497,#68498,#68499,#68500,#68501,#68502,#68503,#68504,#68505,#68506,
#68507,#68508,#68509,#68510,#68511,#68512,#68513,#68514,#68515,#68516,#68517,
#68518,#68519,#68520,#68521,#68522,#68523,#68524,#68525,#68526,#68527,#68528,
#68529,#68530,#68531,#68532,#68533,#68534,#68535,#68536,#68537,#68538,#68539,
#68540,#68541,#68542,#68543,#68544,#68545,#68546,#68547,#68548,#68549,#68550,
#68551,#68552,#68553,#68554,#68555,#68556,#68557,#68558,#68559,#68560,#68561,
#68562,#68563,#68564,#68565,#68566,#68567,#68568,#68569,#68570,#68571,#68572,
#68573),.UNSPECIFIED.,.F.,.F.,(4,2,2,2,2,2,2,2,2,2,2,2,2,2,2,2,2,2,2,2,
2,2,2,2,2,2,2,2,2,2,2,2,2,2,2,2,2,2,2,2,2,2,2,2,2,2,2,2,2,2,2,2,2,2,2,2,
2,2,2,2,2,2,2,2,2,2,2,2,2,2,2,2,2,2,2,2,2,2,2,4),(-0.699700907542827,-0.686276977291691,
-0.683090925269945,-0.681538817046756,-0.680323886225827,-0.67896463697359,
-0.676645519823317,-0.673816968646951,-0.668059250540234,-0.587081823132608,
-0.529188097564907,-0.52377856154388,-0.521013837396152,-0.518973503301894,
-0.51675938760021,-0.51373985575832,-0.506771888317632,-0.433021140757069,
-0.396756974035746,-0.362681609868573,-0.359151545261417,-0.357550439722318,
-0.356326037876926,-0.356323848908466,-0.356321668848628,-0.35631949503184,
-0.356317327499221,-0.356315166128531,-0.35631301087063,-0.356310861764773,
-0.356308718876209,-0.356306582117758,-0.356304451406605,-0.356302326795541,
-0.356300208305847,-0.356298095798876,-0.356295989256645,-0.356293888744311,
-0.356291794264536,-0.356289705718492,-0.356287623082072,-0.356285546382978,
-0.356283475636906,-0.356281410790512,-0.356279351818326,-0.356277298610011,
-0.356275251223554,-0.356273209631598,-0.356271173873063,-0.356269143935612,
-0.356267119756429,-0.356265101212907,-0.356263088398756,-0.356261081377777,
-0.354927488733254,-0.352714821937657,-0.350038332508006,-0.344697150099441,
-0.330767951082596,-0.295818739667679,-0.211059178126563,-0.207945712296062,
-0.200515320845831,-0.19765094718273,-0.195589496447442,-0.193401317782504,
-0.190501403999757,-0.184159968387535,-0.121984694899469,-0.0691891517033401,
-0.0603199487069786,-0.0391893757664143,-0.0360126303896894,-0.0344656778862046,
-0.0332550758510056,-0.0321181940600108,-0.0307556468514484,-0.0287583570317623,
-0.021127039844488,-0.000959563674068928),.UNSPECIFIED.);
#7754=B_SPLINE_CURVE_WITH_KNOTS('',3,(#68574,#68575,#68576,#68577,#68578,
#68579,#68580,#68581,#68582,#68583,#68584,#68585,#68586,#68587,#68588,#68589,
#68590,#68591,#68592,#68593,#68594,#68595,#68596,#68597,#68598,#68599,#68600,
#68601,#68602,#68603,#68604,#68605,#68606,#68607,#68608,#68609,#68610,#68611,
#68612,#68613,#68614,#68615,#68616,#68617,#68618,#68619,#68620,#68621,#68622,
#68623,#68624,#68625,#68626,#68627,#68628,#68629,#68630,#68631,#68632,#68633,
#68634,#68635,#68636,#68637,#68638,#68639,#68640,#68641,#68642,#68643,#68644,
#68645,#68646,#68647,#68648,#68649,#68650,#68651,#68652,#68653,#68654,#68655,
#68656,#68657,#68658,#68659,#68660,#68661,#68662,#68663,#68664,#68665,#68666,
#68667,#68668,#68669,#68670,#68671,#68672,#68673,#68674,#68675,#68676,#68677,
#68678,#68679,#68680,#68681,#68682,#68683,#68684,#68685,#68686,#68687,#68688,
#68689,#68690,#68691,#68692,#68693,#68694,#68695,#68696,#68697,#68698,#68699,
#68700,#68701,#68702,#68703,#68704,#68705,#68706,#68707,#68708,#68709,#68710,
#68711,#68712,#68713,#68714,#68715,#68716,#68717,#68718,#68719,#68720,#68721,
#68722,#68723,#68724,#68725,#68726,#68727,#68728,#68729,#68730,#68731,#68732,
#68733,#68734,#68735,#68736,#68737),.UNSPECIFIED.,.F.,.F.,(4,2,2,2,2,2,
2,2,2,2,2,2,2,2,2,2,2,2,2,2,2,2,2,2,2,2,2,2,2,2,2,2,2,2,2,2,2,2,2,2,2,2,
2,2,2,2,2,2,2,2,2,2,2,2,2,2,2,2,2,2,2,2,2,2,2,2,2,2,2,2,2,2,2,2,2,2,2,2,
2,2,2,4),(-4.06129944956447,-3.97151586264303,-3.95158912669357,-3.93917790955167,
-3.93540729509048,-3.93304290918269,-3.93086148363844,-3.92805330769949,
-3.92342290913847,-3.89628110083149,-3.88370298359696,-3.82449984179205,
-3.79387526844183,-3.78197789163054,-3.77720478610657,-3.77368640709198,
-3.7720720349562,-3.77091915711506,-3.76976961872058,-3.76816585116467,
-3.76399544257687,-3.75809392296904,-3.68917863719632,-3.62163510889708,
-3.61463414732928,-3.6116154975118,-3.6094077678175,-3.60737732831911,-3.60463210061525,
-3.59927873050048,-3.53116209791604,-3.47478810332283,-3.46036544553658,
-3.4548915060975,-3.45216734064375,-3.44993412374128,-3.44859050843053,
-3.44737828965449,-3.44581465811106,-3.44255273325622,-3.41908873370272,
-3.32918274164586,-3.30702628181322,-3.29816119141286,-3.29153503242736,
-3.28858317450383,-3.2863870081591,-3.28434055739519,-3.2809854956126,-3.27254604705071,
-3.27023564293484,-3.19767550216652,-3.16159285770879,-3.14041018890563,
-3.12959450428564,-3.12714121018804,-3.12574651895218,-3.12453791794615,
-3.1230107162738,-3.12003053070776,-3.10254433619555,-3.00756772688076,
-2.98455719726473,-2.97075187851068,-2.96683505873477,-2.96443841173925,
-2.96226639903812,-2.95947792022273,-2.95501294001386,-2.93090117019321,
-2.9122987851847,-2.91164859934651,-2.83687096950397,-2.81698081522216,
-2.80662296006521,-2.80420334496349,-2.80281613370736,-2.8016066461644,
-2.80006872129379,-2.79693615006555,-2.77688322487906,-2.72883210508927),
 .UNSPECIFIED.);
#7755=B_SPLINE_CURVE_WITH_KNOTS('',3,(#68743,#68744,#68745,#68746,#68747,
#68748,#68749,#68750,#68751,#68752,#68753,#68754,#68755,#68756,#68757,#68758,
#68759,#68760,#68761,#68762,#68763,#68764,#68765,#68766,#68767,#68768,#68769,
#68770,#68771,#68772,#68773,#68774,#68775,#68776,#68777,#68778,#68779,#68780,
#68781,#68782,#68783,#68784,#68785,#68786,#68787,#68788,#68789,#68790,#68791,
#68792,#68793,#68794,#68795,#68796,#68797,#68798,#68799,#68800,#68801,#68802,
#68803,#68804,#68805,#68806,#68807,#68808,#68809,#68810,#68811,#68812,#68813,
#68814,#68815,#68816,#68817,#68818,#68819,#68820,#68821,#68822,#68823,#68824,
#68825,#68826,#68827,#68828,#68829,#68830,#68831,#68832,#68833,#68834,#68835,
#68836,#68837,#68838,#68839,#68840,#68841,#68842,#68843,#68844,#68845,#68846,
#68847,#68848,#68849,#68850,#68851,#68852,#68853,#68854,#68855,#68856,#68857,
#68858,#68859,#68860,#68861,#68862,#68863,#68864,#68865,#68866,#68867,#68868,
#68869,#68870,#68871,#68872,#68873,#68874,#68875,#68876,#68877,#68878),
 .UNSPECIFIED.,.F.,.F.,(4,3,3,3,3,3,3,3,3,3,3,3,3,3,3,3,3,3,3,3,3,3,3,3,
3,3,3,3,3,3,3,3,3,3,3,3,3,3,3,3,3,3,3,3,3,4),(109.955742875803,110.066352379532,
110.178347846238,110.265276879588,110.358352188057,110.451301439139,110.544152265468,
110.636935270911,110.729683125555,110.822420651828,110.915172657032,111.008023855944,
111.100926874107,111.19398521532,111.264792018115,111.357867326584,111.450816577665,
111.543667403995,111.636450409438,111.729198264081,111.821935790354,111.914687795559,
112.007538994471,112.100442012633,112.193500353846,112.264307156642,112.357382465111,
112.450331716192,112.543182542522,112.635965547965,112.728713402608,112.821450928881,
112.914202934085,113.007054132997,113.09995715116,113.193015492373,113.263822295168,
113.356909923667,113.449841610519,113.542684098276,113.635462310275,113.728201109468,
113.820956427048,113.913717308636,114.00656069971,114.078874363373),
 .UNSPECIFIED.);
#7756=B_SPLINE_CURVE_WITH_KNOTS('',3,(#68879,#68880,#68881,#68882,#68883,
#68884,#68885,#68886,#68887,#68888,#68889,#68890,#68891,#68892,#68893,#68894,
#68895,#68896,#68897,#68898,#68899,#68900,#68901,#68902,#68903,#68904,#68905,
#68906,#68907,#68908,#68909,#68910,#68911,#68912,#68913,#68914,#68915,#68916,
#68917,#68918,#68919,#68920,#68921,#68922,#68923,#68924,#68925,#68926,#68927,
#68928,#68929,#68930,#68931,#68932,#68933,#68934,#68935,#68936,#68937,#68938,
#68939,#68940,#68941,#68942,#68943,#68944,#68945,#68946,#68947,#68948,#68949,
#68950,#68951),.UNSPECIFIED.,.F.,.F.,(4,3,3,3,3,3,3,3,3,3,3,3,3,3,3,3,3,
3,3,3,3,3,3,3,4),(107.796189056121,107.888934141404,107.983262256686,108.076148385988,
108.171197494262,108.266246602535,108.359321911004,108.452271162085,108.545121988415,
108.637904993858,108.730652848501,108.823390374774,108.916142379978,109.00899357889,
109.101896597053,109.194954938266,109.265761741061,109.358401812315,109.450922236623,
109.543348474802,109.635705896307,109.728032055204,109.820339659303,109.912680590917,
109.955742875643),.UNSPECIFIED.);
#7757=B_SPLINE_CURVE_WITH_KNOTS('',3,(#68952,#68953,#68954,#68955,#68956,
#68957,#68958,#68959,#68960,#68961,#68962,#68963,#68964,#68965,#68966,#68967,
#68968,#68969,#68970,#68971,#68972,#68973,#68974,#68975,#68976,#68977,#68978,
#68979,#68980,#68981,#68982,#68983,#68984,#68985,#68986,#68987,#68988,#68989,
#68990,#68991,#68992,#68993,#68994,#68995,#68996,#68997,#68998,#68999,#69000,
#69001,#69002,#69003,#69004,#69005,#69006,#69007,#69008,#69009,#69010,#69011,
#69012,#69013,#69014,#69015,#69016,#69017,#69018,#69019,#69020,#69021,#69022,
#69023,#69024,#69025,#69026,#69027,#69028,#69029,#69030,#69031,#69032,#69033,
#69034,#69035,#69036,#69037,#69038,#69039,#69040,#69041,#69042,#69043,#69044,
#69045,#69046,#69047,#69048,#69049,#69050,#69051,#69052,#69053,#69054,#69055,
#69056,#69057,#69058,#69059,#69060,#69061,#69062,#69063,#69064,#69065,#69066,
#69067,#69068,#69069,#69070,#69071,#69072,#69073,#69074,#69075,#69076,#69077,
#69078,#69079,#69080,#69081,#69082,#69083,#69084,#69085,#69086,#69087,#69088,
#69089,#69090,#69091,#69092,#69093,#69094,#69095,#69096,#69097,#69098,#69099,
#69100,#69101,#69102,#69103,#69104,#69105,#69106,#69107,#69108,#69109,#69110,
#69111,#69112,#69113,#69114,#69115,#69116,#69117,#69118,#69119,#69120,#69121,
#69122,#69123,#69124,#69125,#69126,#69127,#69128,#69129,#69130,#69131,#69132,
#69133,#69134,#69135,#69136,#69137,#69138,#69139,#69140,#69141,#69142,#69143,
#69144,#69145,#69146,#69147,#69148,#69149,#69150,#69151,#69152,#69153,#69154,
#69155,#69156,#69157,#69158,#69159,#69160,#69161,#69162,#69163,#69164,#69165,
#69166,#69167,#69168,#69169,#69170,#69171,#69172,#69173,#69174,#69175,#69176,
#69177,#69178,#69179,#69180,#69181,#69182,#69183,#69184,#69185,#69186,#69187,
#69188,#69189,#69190,#69191,#69192,#69193,#69194,#69195,#69196,#69197,#69198,
#69199),.UNSPECIFIED.,.F.,.F.,(4,2,2,2,2,2,2,2,2,2,2,2,2,2,2,2,2,2,2,2,
2,2,2,2,2,2,2,2,2,2,2,2,2,2,2,2,2,2,2,2,2,2,2,2,2,2,2,2,2,2,2,2,2,2,2,2,
2,2,2,2,2,2,2,2,2,2,2,2,2,2,2,2,2,2,2,2,2,2,2,2,2,2,2,2,2,2,2,2,2,2,2,2,
2,2,2,2,2,2,2,2,2,2,2,2,2,2,2,2,2,2,2,2,2,2,2,2,2,2,2,2,2,2,2,4),(-2.72883210508927,
-2.6841013492052,-2.66146619148852,-2.64782669258225,-2.64392664933061,
-2.64153379778537,-2.6393609802297,-2.63656552850915,-2.63076777465074,
-2.55473613567879,-2.50993870810493,-2.49287229865924,-2.48356477933245,
-2.48122871033572,-2.47986009745189,-2.47864764736345,-2.4770804028602,
-2.47379919688275,-2.44976056957312,-2.44050155878647,-2.39639801574435,
-2.32997950921624,-2.32304639898441,-2.32003989149577,-2.31783453259101,
-2.31580170768498,-2.31304630455377,-2.30765243667475,-2.24501528304617,
-2.19337101920306,-2.1719123281163,-2.16100097949913,-2.15854102102134,
-2.15714494235822,-2.15593663334916,-2.15441172994718,-2.15144180856355,
-2.13414924667854,-2.09658843617803,-2.03156058092475,-2.03115640637577,
-2.02774431840743,-2.00409062487207,-1.99965389048755,-1.9968739845647,
-1.99470301124488,-1.99230176301732,-1.98836434117902,-1.97435177457992,
-1.95086494018577,-1.85290350080089,-1.8387391983045,-1.83619038522102,
-1.83463637041616,-1.83342220206355,-1.83206060483199,-1.82975673906367,
-1.82082769340627,-1.80473550240286,-1.79142580027802,-1.69024688906587,
-1.68833882962245,-1.67850324606158,-1.67492935530327,-1.67284063072717,
-1.67066521932038,-1.66785080218272,-1.66195654730544,-1.61618253528898,
-1.52504637561318,-1.51514132746889,-1.51266220554993,-1.51124681249597,
-1.51004002260378,-1.50854012896904,-1.5055953042289,-1.48431844973386,
-1.44908562752498,-1.36528407491663,-1.36323806846359,-1.35498641881049,
-1.35166285507353,-1.34962226533088,-1.34742202800553,-1.34444649872162,
-1.33768940068295,-1.32860323088797,-1.30566737323272,-1.21109256500193,
-1.19305057683538,-1.19004395938819,-1.18851090748547,-1.18730160743296,
-1.18591051780852,-1.18347427146321,-1.17289763340506,-1.15239965219208,
-1.08045093077643,-1.03648697106238,-1.03069121398188,-1.0278956565347,
-1.02572227912818,-1.02332832774368,-1.01942540299238,-1.00576496657007,
-0.983081827162041,-0.889992956048792,-0.870192546954515,-0.867069731336651,
-0.865533440972608,-0.864323729552294,-0.862934566324437,-0.860507480771691,
-0.850057292791093,-0.829915631721224,-0.756292265417527,-0.737894637092599,
-0.732583435711295,-0.711756182889704,-0.707496295141879,-0.704770004335944,
-0.702604276151083,-0.700219330519851,-0.698829799056907),.UNSPECIFIED.);
#7758=B_SPLINE_CURVE_WITH_KNOTS('',3,(#69205,#69206,#69207,#69208,#69209,
#69210,#69211,#69212,#69213,#69214,#69215,#69216,#69217,#69218,#69219,#69220,
#69221,#69222,#69223,#69224,#69225,#69226,#69227,#69228,#69229,#69230,#69231,
#69232,#69233,#69234,#69235,#69236,#69237,#69238,#69239,#69240,#69241,#69242,
#69243,#69244,#69245,#69246,#69247,#69248,#69249,#69250,#69251,#69252,#69253,
#69254,#69255,#69256,#69257,#69258,#69259,#69260,#69261,#69262,#69263,#69264,
#69265,#69266,#69267,#69268,#69269,#69270,#69271,#69272,#69273,#69274,#69275,
#69276,#69277,#69278,#69279,#69280,#69281,#69282,#69283,#69284,#69285,#69286,
#69287,#69288,#69289,#69290,#69291,#69292,#69293,#69294,#69295,#69296,#69297,
#69298,#69299,#69300,#69301,#69302,#69303,#69304,#69305,#69306,#69307,#69308,
#69309,#69310,#69311,#69312,#69313,#69314,#69315,#69316,#69317,#69318,#69319,
#69320,#69321,#69322,#69323,#69324,#69325,#69326,#69327,#69328,#69329,#69330,
#69331,#69332,#69333,#69334,#69335,#69336,#69337,#69338,#69339,#69340,#69341,
#69342,#69343,#69344,#69345,#69346),.UNSPECIFIED.,.F.,.F.,(4,3,3,3,3,3,
3,3,3,3,3,3,3,3,3,3,3,3,3,3,3,3,3,3,3,3,3,3,3,3,3,3,3,3,3,3,3,3,3,3,3,3,
3,3,3,3,3,4),(116.238928182823,116.262367710749,116.355443019218,116.448392270299,
116.541243096629,116.634026102072,116.726773956715,116.819511482989,116.912263488193,
117.005114687105,117.098017705267,117.191076046481,117.261882849275,117.354958157744,
117.447907408825,117.540758235155,117.633541240597,117.726289095241,117.819026621514,
117.911778626718,118.00462982563,118.097532843793,118.190591185006,118.261397987802,
118.354473296271,118.447422547353,118.540273373682,118.633056379125,118.725804233769,
118.818541760042,118.911293765246,119.004144964158,119.097047982321,119.190106323534,
119.260913126329,119.353988434798,119.446937685879,119.539788512209,119.632571517652,
119.725319372295,119.818056898568,119.910808903772,120.003660102684,120.096563120847,
120.18962146206,120.260428264856,120.353515438102,120.36310897423),
 .UNSPECIFIED.);
#7759=B_SPLINE_CURVE_WITH_KNOTS('',3,(#69347,#69348,#69349,#69350,#69351,
#69352,#69353,#69354,#69355,#69356,#69357,#69358,#69359,#69360,#69361,#69362,
#69363,#69364,#69365,#69366,#69367,#69368,#69369,#69370,#69371,#69372,#69373,
#69374,#69375,#69376,#69377,#69378,#69379,#69380,#69381,#69382,#69383,#69384,
#69385,#69386,#69387,#69388,#69389,#69390,#69391,#69392,#69393,#69394,#69395,
#69396,#69397,#69398,#69399,#69400,#69401,#69402,#69403,#69404,#69405,#69406,
#69407,#69408,#69409,#69410,#69411,#69412,#69413,#69414,#69415,#69416,#69417,
#69418,#69419),.UNSPECIFIED.,.F.,.F.,(4,3,3,3,3,3,3,3,3,3,3,3,3,3,3,3,3,
3,3,3,3,3,3,3,4),(114.078874363373,114.171925674316,114.263337433695,114.356412742164,
114.449361993246,114.542212819575,114.634995825018,114.727743679662,114.820481205935,
114.913233211139,115.006084410051,115.098987428214,115.192045769427,115.262852572222,
115.355560923056,115.44814349422,115.540628385212,115.633046882578,115.725431735228,
115.817808179262,115.910201437255,116.002693497524,116.095240289185,116.187934829135,
116.238928182608),.UNSPECIFIED.);
#7760=B_SPLINE_CURVE_WITH_KNOTS('',3,(#69421,#69422,#69423,#69424,#69425,
#69426,#69427,#69428,#69429,#69430,#69431,#69432,#69433,#69434,#69435,#69436,
#69437,#69438,#69439,#69440,#69441,#69442,#69443,#69444,#69445,#69446,#69447,
#69448,#69449,#69450,#69451,#69452,#69453,#69454,#69455,#69456,#69457,#69458,
#69459,#69460,#69461,#69462,#69463,#69464,#69465,#69466,#69467,#69468,#69469,
#69470,#69471,#69472,#69473,#69474,#69475,#69476,#69477,#69478,#69479,#69480,
#69481,#69482,#69483,#69484,#69485,#69486,#69487,#69488,#69489,#69490,#69491,
#69492,#69493,#69494,#69495,#69496,#69497,#69498,#69499,#69500,#69501,#69502,
#69503,#69504,#69505,#69506,#69507,#69508,#69509,#69510,#69511,#69512,#69513,
#69514,#69515,#69516,#69517,#69518),.UNSPECIFIED.,.F.,.F.,(4,2,2,2,2,2,
2,2,2,2,2,2,2,2,2,2,2,2,2,2,2,2,2,2,2,2,2,2,2,2,2,2,2,2,2,2,2,2,2,2,2,2,
2,2,2,2,2,2,4),(-0.698829799056907,-0.696283571084546,-0.691577884397476,
-0.682320401807412,-0.658777460441537,-0.594435323804517,-0.548031763846652,
-0.544415798399543,-0.54280221646017,-0.541579234139466,-0.540247882620269,
-0.538080176332597,-0.53058121904335,-0.474473115536343,-0.407688301766228,
-0.403537468993245,-0.395057480192895,-0.386288396708483,-0.382878033263585,
-0.380820634461199,-0.378629963688585,-0.375773329976131,-0.36961868589772,
-0.361453985045792,-0.341698772604676,-0.301511021545795,-0.256424265931702,
-0.250739562221718,-0.246149332569339,-0.242452966807125,-0.224275436340046,
-0.221262349514428,-0.219727851903959,-0.218518354530284,-0.217128095134346,
-0.21469585739779,-0.204175085882081,-0.183835028169646,-0.117555057193131,
-0.104050809409281,-0.0673725117839966,-0.0618635266257452,-0.0590867455823338,
-0.0569155169559284,-0.0548907916827107,-0.0525321504819316,-0.0491630845345916,
-0.0363424731010816,-0.000959780702671639),.UNSPECIFIED.);
#7761=B_SPLINE_CURVE_WITH_KNOTS('',3,(#69519,#69520,#69521,#69522,#69523,
#69524,#69525,#69526,#69527,#69528,#69529,#69530,#69531,#69532,#69533,#69534,
#69535,#69536,#69537,#69538,#69539,#69540,#69541,#69542,#69543,#69544,#69545,
#69546,#69547,#69548,#69549,#69550,#69551,#69552,#69553,#69554,#69555,#69556,
#69557,#69558,#69559,#69560,#69561,#69562,#69563,#69564,#69565,#69566,#69567,
#69568,#69569,#69570,#69571,#69572,#69573,#69574,#69575,#69576,#69577,#69578,
#69579,#69580,#69581,#69582,#69583,#69584,#69585,#69586,#69587,#69588,#69589,
#69590,#69591,#69592,#69593,#69594,#69595,#69596,#69597,#69598,#69599,#69600,
#69601,#69602,#69603,#69604,#69605,#69606,#69607,#69608,#69609,#69610,#69611,
#69612,#69613,#69614,#69615,#69616,#69617,#69618,#69619,#69620,#69621,#69622,
#69623,#69624,#69625,#69626,#69627,#69628,#69629,#69630,#69631,#69632,#69633,
#69634,#69635,#69636,#69637,#69638,#69639,#69640,#69641,#69642,#69643,#69644,
#69645,#69646,#69647,#69648,#69649,#69650,#69651,#69652,#69653,#69654,#69655,
#69656,#69657,#69658,#69659,#69660,#69661,#69662,#69663,#69664,#69665,#69666,
#69667,#69668,#69669,#69670,#69671,#69672,#69673,#69674,#69675,#69676,#69677,
#69678,#69679,#69680,#69681,#69682,#69683,#69684,#69685,#69686,#69687,#69688,
#69689,#69690,#69691,#69692,#69693,#69694,#69695,#69696,#69697,#69698,#69699,
#69700,#69701,#69702,#69703,#69704,#69705,#69706,#69707,#69708,#69709,#69710),
 .UNSPECIFIED.,.F.,.F.,(4,2,2,2,2,2,2,2,2,2,2,2,2,2,2,2,2,2,2,2,2,2,2,2,
2,2,2,2,2,2,2,2,2,2,2,2,2,2,2,2,2,2,2,2,2,2,2,2,2,2,2,2,2,2,2,2,2,2,2,2,
2,2,2,2,2,2,2,2,2,2,2,2,2,2,2,2,2,2,2,2,2,2,2,2,2,2,2,2,2,2,2,2,2,2,2,4),
(-4.05953948686282,-4.02804717577849,-3.96639928240388,-3.95854999347298,
-3.95634738771327,-3.9550086713052,-3.9537889795346,-3.95219327647582,-3.94950221092906,
-3.93256736994538,-3.9111114248824,-3.8606273404071,-3.82470830543548,-3.80955149306956,
-3.79952132351166,-3.79607170407889,-3.79404796095421,-3.79187750704361,
-3.78910054767651,-3.7846730447942,-3.76116755294912,-3.75483229669635,
-3.69956780167767,-3.63946713098213,-3.6349485083312,-3.63316339283032,
-3.63191523201871,-3.63078535967416,-3.62925670285534,-3.62627392473511,
-3.60133038383909,-3.59959761812075,-3.56742826705854,-3.51147451009267,
-3.49038028512578,-3.48182197790361,-3.47737701085475,-3.47363453691837,
-3.47128784834473,-3.47128420386158,-3.47128054925519,-3.4712768844594,
-3.47127320949574,-3.47126952428425,-3.47126582877831,-3.47126212291703,
-3.47125840666092,-3.47125467999486,-3.47125094285677,-3.47124719524596,
-3.471243437102,-3.47123966835957,-3.47123588900434,-3.46905960782723,-3.46628384948736,
-3.46043259606198,-3.38656982718402,-3.3402154807693,-3.32279031209362,
-3.31334540447379,-3.31099794060826,-3.30962682601396,-3.30841490733978,
-3.30685201653149,-3.30359288322983,-3.28019472580136,-3.19516950811749,
-3.16978371419665,-3.15495502179838,-3.15093967076339,-3.14852122248431,
-3.14635408162173,-3.14360559448257,-3.13927118409039,-3.11727380187453,
-3.1133801939102,-3.09496196018341,-3.02118365504073,-3.00109466504002,
-2.99066586918709,-2.98824112673003,-2.98685287582207,-2.98564368408787,
-2.98410770285012,-2.98098433340946,-2.96114515167558,-2.86819425500871,
-2.84553086029295,-2.83187926459257,-2.82797827943683,-2.82558538826315,
-2.82341288808368,-2.82061833962584,-2.81482424680385,-2.7708603527225,
-2.72806160371598),.UNSPECIFIED.);
#7762=B_SPLINE_CURVE_WITH_KNOTS('',3,(#69716,#69717,#69718,#69719,#69720,
#69721,#69722,#69723,#69724,#69725,#69726,#69727,#69728,#69729,#69730,#69731,
#69732,#69733,#69734,#69735,#69736,#69737,#69738,#69739,#69740,#69741,#69742,
#69743,#69744,#69745,#69746,#69747,#69748,#69749,#69750,#69751,#69752,#69753,
#69754,#69755,#69756,#69757,#69758,#69759,#69760,#69761,#69762,#69763,#69764,
#69765,#69766,#69767,#69768,#69769,#69770,#69771,#69772,#69773,#69774,#69775,
#69776,#69777,#69778,#69779,#69780,#69781,#69782,#69783,#69784,#69785,#69786,
#69787,#69788,#69789,#69790,#69791,#69792,#69793,#69794,#69795,#69796,#69797,
#69798,#69799,#69800,#69801,#69802,#69803,#69804,#69805,#69806,#69807,#69808,
#69809,#69810,#69811,#69812,#69813,#69814,#69815,#69816,#69817,#69818,#69819,
#69820,#69821,#69822,#69823,#69824,#69825,#69826,#69827,#69828,#69829,#69830,
#69831,#69832,#69833,#69834,#69835,#69836,#69837,#69838,#69839,#69840,#69841,
#69842,#69843,#69844,#69845,#69846,#69847,#69848,#69849,#69850,#69851,#69852,
#69853,#69854),.UNSPECIFIED.,.F.,.F.,(4,3,3,3,3,3,3,3,3,3,3,3,3,3,3,3,3,
3,3,3,3,3,3,3,3,3,3,3,3,3,3,3,3,3,3,3,3,3,3,3,3,3,3,3,3,3,4),(122.522113490002,
122.614221013806,122.706029130239,122.797814360325,122.889602493242,122.98194529004,
123.073867389215,123.166420534826,123.258973680436,123.352048988905,123.444998239987,
123.537849066316,123.630632071759,123.723379926402,123.816117452676,123.90886945788,
124.001720656792,124.094623674954,124.187682016168,124.258488818963,124.351564127432,
124.444513378513,124.537364204843,124.630147210286,124.722895064929,124.815632591202,
124.908384596407,125.001235795318,125.094138813481,125.187197154694,125.25800395749,
125.351079265959,125.44402851704,125.53687934337,125.629662348812,125.722410203456,
125.815147729729,125.907899734933,126.000750933845,126.093653952008,126.186712293221,
126.257519096016,126.354681067361,126.447615201551,126.540462792668,126.633238985787,
126.646166981397),.UNSPECIFIED.);
#7763=B_SPLINE_CURVE_WITH_KNOTS('',3,(#69855,#69856,#69857,#69858,#69859,
#69860,#69861,#69862,#69863,#69864,#69865,#69866,#69867,#69868,#69869,#69870,
#69871,#69872,#69873,#69874,#69875,#69876,#69877,#69878,#69879,#69880,#69881,
#69882,#69883,#69884,#69885,#69886,#69887,#69888,#69889,#69890,#69891,#69892,
#69893,#69894,#69895,#69896,#69897,#69898,#69899,#69900,#69901,#69902,#69903,
#69904,#69905,#69906,#69907,#69908,#69909,#69910,#69911,#69912,#69913,#69914,
#69915,#69916,#69917,#69918,#69919,#69920,#69921,#69922,#69923,#69924,#69925,
#69926,#69927),.UNSPECIFIED.,.F.,.F.,(4,3,3,3,3,3,3,3,3,3,3,3,3,3,3,3,3,
3,3,3,3,3,3,3,4),(120.36310897423,120.456046782208,120.54888901282,120.641667237396,
120.734412876219,120.827150749232,120.91990566331,121.012761178263,121.105670815306,
121.198732890817,121.259943403382,121.353018711851,121.445967962932,121.538818789262,
121.631601794705,121.724349649348,121.817087175621,121.909839180825,122.002690379737,
122.095593397899,122.188651739113,122.259458541909,122.378943455942,122.496088061442,
122.522113489712),.UNSPECIFIED.);
#7764=B_SPLINE_CURVE_WITH_KNOTS('',3,(#69928,#69929,#69930,#69931,#69932,
#69933,#69934,#69935,#69936,#69937,#69938,#69939,#69940,#69941,#69942,#69943,
#69944,#69945,#69946,#69947,#69948,#69949,#69950,#69951,#69952,#69953,#69954,
#69955,#69956,#69957,#69958,#69959,#69960,#69961,#69962,#69963,#69964,#69965,
#69966,#69967,#69968,#69969,#69970,#69971,#69972,#69973,#69974,#69975,#69976,
#69977,#69978,#69979,#69980,#69981,#69982,#69983,#69984,#69985,#69986,#69987,
#69988,#69989,#69990,#69991,#69992,#69993,#69994,#69995,#69996,#69997,#69998,
#69999,#70000,#70001,#70002,#70003,#70004,#70005,#70006,#70007,#70008,#70009,
#70010,#70011,#70012,#70013,#70014,#70015,#70016,#70017,#70018,#70019,#70020,
#70021,#70022,#70023,#70024,#70025,#70026,#70027,#70028,#70029,#70030,#70031,
#70032,#70033,#70034,#70035,#70036,#70037,#70038,#70039,#70040,#70041,#70042,
#70043,#70044,#70045,#70046,#70047,#70048,#70049,#70050,#70051,#70052,#70053,
#70054,#70055,#70056,#70057,#70058,#70059,#70060,#70061,#70062,#70063,#70064,
#70065,#70066,#70067,#70068,#70069,#70070,#70071,#70072,#70073,#70074,#70075,
#70076,#70077,#70078,#70079,#70080,#70081,#70082,#70083,#70084,#70085,#70086,
#70087,#70088,#70089,#70090,#70091,#70092,#70093,#70094,#70095,#70096,#70097,
#70098,#70099,#70100,#70101,#70102,#70103,#70104,#70105,#70106,#70107,#70108,
#70109,#70110,#70111,#70112,#70113,#70114,#70115,#70116,#70117,#70118,#70119,
#70120,#70121,#70122,#70123,#70124,#70125,#70126,#70127,#70128,#70129,#70130,
#70131,#70132,#70133,#70134,#70135,#70136,#70137,#70138,#70139,#70140,#70141,
#70142,#70143,#70144,#70145,#70146,#70147,#70148,#70149,#70150,#70151,#70152,
#70153,#70154,#70155,#70156,#70157,#70158,#70159,#70160,#70161,#70162,#70163,
#70164,#70165,#70166,#70167,#70168,#70169,#70170,#70171,#70172,#70173,#70174,
#70175,#70176,#70177,#70178,#70179,#70180,#70181,#70182,#70183,#70184,#70185,
#70186,#70187,#70188,#70189,#70190,#70191,#70192,#70193),.UNSPECIFIED.,
 .F.,.F.,(4,2,2,2,2,2,2,2,2,2,2,2,2,2,2,2,2,2,2,2,2,2,2,2,2,2,2,2,2,2,2,
2,2,2,2,2,2,2,2,2,2,2,2,2,2,2,2,2,2,2,2,2,2,2,2,2,2,2,2,2,2,2,2,2,2,2,2,
2,2,2,2,2,2,2,2,2,2,2,2,2,2,2,2,2,2,2,2,2,2,2,2,2,2,2,2,2,2,2,2,2,2,2,2,
2,2,2,2,2,2,2,2,2,2,2,2,2,2,2,2,2,2,2,2,2,2,2,2,2,2,2,2,2,4),(-2.72806160371598,
-2.69888338142189,-2.67839882741157,-2.66782932224088,-2.66539423811918,
-2.66400374012005,-2.66279490550071,-2.66126238715696,-2.65825664047353,
-2.64026252180287,-2.63538895716395,-2.6270834926754,-2.54340626855923,
-2.52203106568523,-2.508956214092,-2.50511476799622,-2.50273514854462,-2.5005592320277,
-2.49778502694809,-2.49194113288248,-2.41780109569306,-2.37163929988056,
-2.35427337529901,-2.34485131700401,-2.34250587520145,-2.34113528022046,
-2.33992338574495,-2.33835994563103,-2.33509761985756,-2.31160129531681,
-2.30823998944257,-2.26456356245751,-2.19125805651105,-2.18431857555433,
-2.18131119871924,-2.17910592268382,-2.17707367981462,-2.1743198360413,
-2.16893131379304,-2.11123761132658,-2.0305335632662,-2.02205832394373,
-2.01969181789282,-2.01831646417313,-2.01722657586411,-2.01573275322975,
-2.01281629785216,-1.99242185431692,-1.95952371040605,-1.87212020111034,
-1.86792491119328,-1.86137627378458,-1.85868818720353,-1.85667220563599,
-1.85445271214574,-1.85136742998131,-1.84397572512746,-1.81167326964969,
-1.71214799531086,-1.69970928484751,-1.69726635150294,-1.69572776854459,
-1.6945181913891,-1.69313134864069,-1.69071351622612,-1.68037985450563,
-1.66056012468515,-1.58531909736759,-1.58436809280869,-1.58271914516889,
-1.56929482908524,-1.56722009427172,-1.54245182500913,-1.53794814689526,
-1.53514783971042,-1.53297423732035,-1.53058353811107,-1.52669378654129,
-1.51315796654392,-1.49075411318256,-1.39930497583082,-1.39597207984956,
-1.37739183906319,-1.37436075142821,-1.37282255047578,-1.3716129005424,
-1.37022555762943,-1.36780585411014,-1.35744952599924,-1.33756770196131,
-1.26270629800734,-1.26188754619618,-1.2614466864697,-1.2598540866088,-1.24630564923713,
-1.24467196781882,-1.2435717746257,-1.21946138662273,-1.21499601683425,
-1.2122071870316,-1.21003484446982,-1.20763777607806,-1.2037201382674,-1.18991068920238,
-1.16688886543605,-1.07180623019604,-1.05435244406824,-1.05137349378257,
-1.04984637142369,-1.04863754927178,-1.04724227673317,-1.04478717249939,
-1.03395102234872,-1.01271493268722,-0.971951618413559,-0.89790973947994,
-0.892058985882461,-0.88928272211937,-0.887105716227925,-0.884725442045078,
-0.880884125927783,-0.867821042142076,-0.846472329926201,-0.763267470149372,
-0.755653994097213,-0.731814253632982,-0.728538875876849,-0.726972421183132,
-0.725759674828243,-0.724389729536665,-0.722049112380113,-0.712877250629526,
-0.698254248219955),.UNSPECIFIED.);
#7765=B_SPLINE_CURVE_WITH_KNOTS('',3,(#70199,#70200,#70201,#70202,#70203,
#70204,#70205,#70206,#70207,#70208,#70209,#70210,#70211,#70212,#70213,#70214,
#70215,#70216,#70217,#70218,#70219,#70220,#70221,#70222,#70223,#70224,#70225,
#70226,#70227,#70228,#70229,#70230,#70231,#70232,#70233,#70234,#70235,#70236,
#70237,#70238,#70239,#70240,#70241,#70242,#70243,#70244,#70245,#70246,#70247,
#70248,#70249,#70250,#70251,#70252,#70253,#70254,#70255,#70256,#70257,#70258,
#70259,#70260,#70261,#70262,#70263,#70264,#70265,#70266,#70267,#70268,#70269,
#70270,#70271,#70272,#70273,#70274,#70275,#70276,#70277,#70278,#70279,#70280,
#70281,#70282,#70283,#70284,#70285,#70286,#70287,#70288,#70289,#70290,#70291,
#70292,#70293,#70294,#70295,#70296,#70297,#70298,#70299,#70300,#70301,#70302,
#70303,#70304,#70305,#70306,#70307,#70308,#70309,#70310,#70311,#70312,#70313,
#70314,#70315,#70316,#70317,#70318,#70319,#70320,#70321,#70322,#70323,#70324,
#70325,#70326,#70327,#70328,#70329,#70330,#70331,#70332,#70333,#70334,#70335,
#70336,#70337),.UNSPECIFIED.,.F.,.F.,(4,3,3,3,3,3,3,3,3,3,3,3,3,3,3,3,3,
3,3,3,3,3,3,3,3,3,3,3,3,3,3,3,3,3,3,3,3,3,3,3,3,3,3,3,3,3,4),(128.805298797385,
128.904677691686,129.004435593514,129.104391172187,129.204654417159,129.256064511597,
129.349139820066,129.442089071147,129.534939897477,129.62772290292,129.720470757563,
129.813208283837,129.905960289041,129.998811487953,130.091714506115,130.184772847329,
130.255579650123,130.348654958592,130.441604209673,130.534455036003,130.627238041446,
130.719985896089,130.812723422362,130.905475427566,130.998326626478,131.091229644641,
131.184287985854,131.25509478865,131.348170097119,131.441119348201,131.53397017453,
131.626753179973,131.719501034617,131.81223856089,131.904990566094,131.997841765006,
132.090744783169,132.183803124382,132.254609927177,132.347666574696,132.440605721842,
132.533452388277,132.626231507612,132.718977855737,132.811706217422,132.904461102758,
132.928545070227),.UNSPECIFIED.);
#7766=B_SPLINE_CURVE_WITH_KNOTS('',3,(#70338,#70339,#70340,#70341,#70342,
#70343,#70344,#70345,#70346,#70347,#70348,#70349,#70350,#70351,#70352,#70353,
#70354,#70355,#70356,#70357,#70358,#70359,#70360,#70361,#70362,#70363,#70364,
#70365,#70366,#70367,#70368,#70369,#70370,#70371,#70372,#70373,#70374,#70375,
#70376,#70377,#70378,#70379,#70380,#70381,#70382,#70383,#70384,#70385,#70386,
#70387,#70388,#70389,#70390,#70391,#70392,#70393,#70394,#70395,#70396,#70397,
#70398,#70399,#70400,#70401,#70402,#70403,#70404,#70405,#70406,#70407,#70408,
#70409,#70410),.UNSPECIFIED.,.F.,.F.,(4,3,3,3,3,3,3,3,3,3,3,3,3,3,3,3,3,
3,3,3,3,3,3,3,4),(126.646166981397,126.738911088157,126.83164941077,126.924406755924,
127.017265771619,127.110180690541,127.203245854743,127.257034234543,127.350109543012,
127.443058794094,127.535909620423,127.628692625866,127.721440480509,127.814178006783,
127.906930011986,127.999781210898,128.092684229061,128.185742570274,128.25654937307,
128.352519890112,128.448333313375,128.543966784371,128.639494412394,128.734912471125,
128.805298797182),.UNSPECIFIED.);
#7767=B_SPLINE_CURVE_WITH_KNOTS('',3,(#70412,#70413,#70414,#70415,#70416,
#70417,#70418,#70419,#70420,#70421,#70422,#70423,#70424,#70425,#70426,#70427,
#70428,#70429,#70430,#70431,#70432,#70433,#70434,#70435,#70436,#70437,#70438,
#70439,#70440,#70441,#70442,#70443,#70444,#70445,#70446,#70447,#70448,#70449,
#70450,#70451,#70452,#70453,#70454,#70455,#70456,#70457,#70458,#70459,#70460,
#70461,#70462,#70463,#70464,#70465,#70466,#70467,#70468,#70469,#70470,#70471,
#70472,#70473,#70474,#70475,#70476,#70477,#70478,#70479,#70480,#70481,#70482,
#70483,#70484,#70485,#70486,#70487,#70488,#70489,#70490,#70491,#70492,#70493,
#70494,#70495,#70496,#70497),.UNSPECIFIED.,.F.,.F.,(4,2,2,2,2,2,2,2,2,2,
2,2,2,2,2,2,2,2,2,2,2,2,2,2,2,2,2,2,2,2,2,2,2,2,2,2,2,2,2,2,2,2,4),(-0.698254248219955,
-0.696102458516538,-0.635703733506079,-0.57518441543688,-0.569787984618583,
-0.567031427577486,-0.56499783329478,-0.56279171896029,-0.56061624404223,
-0.555477492209153,-0.522551661170759,-0.460002500985555,-0.435548709256675,
-0.409042994892415,-0.405726524438106,-0.404145618701489,-0.402927650588259,
-0.401580471982622,-0.399341792948716,-0.391326356640898,-0.37740592219274,
-0.343734221167373,-0.305915556585983,-0.252260526407009,-0.246902563946533,
-0.24415582419305,-0.242124683685358,-0.239916596334023,-0.237737657931382,
-0.234827254215558,-0.220808933442814,-0.183594512867419,-0.155274513005722,
-0.135713331536938,-0.0865880444975021,-0.082976479782648,-0.0813637553983931,
-0.0801409672278459,-0.0788093454703919,-0.0766402066409501,-0.0740683031706375,
-0.069014208624824,-0.000960727163108736),.UNSPECIFIED.);
#7768=B_SPLINE_CURVE_WITH_KNOTS('',3,(#70498,#70499,#70500,#70501,#70502,
#70503,#70504,#70505,#70506,#70507,#70508,#70509,#70510,#70511,#70512,#70513,
#70514,#70515,#70516,#70517,#70518,#70519,#70520,#70521,#70522,#70523,#70524,
#70525,#70526,#70527,#70528,#70529,#70530,#70531,#70532,#70533,#70534,#70535,
#70536,#70537,#70538,#70539,#70540,#70541,#70542,#70543,#70544,#70545,#70546,
#70547,#70548,#70549,#70550,#70551,#70552,#70553,#70554,#70555,#70556,#70557,
#70558,#70559,#70560,#70561,#70562,#70563,#70564,#70565,#70566,#70567,#70568,
#70569,#70570,#70571,#70572,#70573,#70574,#70575,#70576,#70577,#70578,#70579,
#70580,#70581,#70582,#70583,#70584,#70585,#70586,#70587,#70588,#70589,#70590,
#70591,#70592,#70593,#70594,#70595,#70596,#70597,#70598,#70599,#70600,#70601,
#70602,#70603,#70604,#70605,#70606,#70607,#70608,#70609,#70610,#70611,#70612,
#70613,#70614,#70615,#70616,#70617,#70618,#70619,#70620,#70621,#70622,#70623,
#70624,#70625,#70626,#70627,#70628,#70629,#70630,#70631,#70632,#70633,#70634,
#70635,#70636,#70637,#70638,#70639,#70640,#70641,#70642,#70643,#70644,#70645,
#70646,#70647,#70648,#70649,#70650,#70651,#70652,#70653,#70654,#70655,#70656,
#70657),.UNSPECIFIED.,.F.,.F.,(4,2,2,2,2,2,2,2,2,2,2,2,2,2,2,2,2,2,2,2,
2,2,2,2,2,2,2,2,2,2,2,2,2,2,2,2,2,2,2,2,2,2,2,2,2,2,2,2,2,2,2,2,2,2,2,2,
2,2,2,2,2,2,2,2,2,2,2,2,2,2,2,2,2,2,2,2,2,2,2,4),(-4.06075106093832,-3.99275036976407,
-3.9870394039298,-3.98370816777374,-3.98069268381622,-3.97848566267548,
-3.97645475111405,-3.97370717918828,-3.96834418522565,-3.90077993838917,
-3.86942222463597,-3.82865236952972,-3.82115784686525,-3.81895120518124,
-3.81761144710722,-3.81639180828979,-3.81479751869627,-3.81128481555614,
-3.75311507797128,-3.70942281512221,-3.67988888438663,-3.6690300230973,
-3.66130573155778,-3.65887183688258,-3.65649879022691,-3.65432033547206,
-3.65153113825552,-3.64696413637091,-3.62102581528763,-3.60265705529881,
-3.54800463754439,-3.50467275325379,-3.49836723347806,-3.49617304162426,
-3.49483604299982,-3.49361549207006,-3.49201540129283,-3.48847143678877,
-3.45269017344621,-3.37752958586565,-3.35410805051516,-3.34488481108031,
-3.33809530996548,-3.33508634047439,-3.33288044749564,-3.33084802253915,
-3.32809452057118,-3.32270841780889,-3.26569571332101,-3.22603231864836,
-3.20121539918965,-3.18483342318615,-3.17884583715928,-3.17459385746229,
-3.17285187725894,-3.17161196867734,-3.17047308885195,-3.16890941538682,
-3.16578898478335,-3.10338486944329,-3.02806989536521,-3.01671510848104,
-3.01306663349531,-3.01072957300689,-3.00853879031984,-3.00566914982275,
-3.00082878499004,-2.96898495607456,-2.87514949668317,-2.86088624025076,
-2.85269824021717,-2.85046225338921,-2.84911585911558,-2.84789801161689,
-2.84631649294655,-2.84367454400887,-2.82774200210274,-2.82025644963418,
-2.72989675923859,-2.72842990354347),.UNSPECIFIED.);
#7769=B_SPLINE_CURVE_WITH_KNOTS('',3,(#70663,#70664,#70665,#70666,#70667,
#70668,#70669,#70670,#70671,#70672,#70673,#70674,#70675,#70676,#70677,#70678,
#70679,#70680,#70681,#70682,#70683,#70684,#70685,#70686,#70687,#70688,#70689,
#70690,#70691,#70692,#70693,#70694,#70695,#70696,#70697,#70698,#70699,#70700,
#70701,#70702,#70703,#70704,#70705,#70706,#70707,#70708,#70709,#70710,#70711,
#70712,#70713,#70714,#70715,#70716,#70717,#70718,#70719,#70720,#70721,#70722,
#70723,#70724,#70725,#70726,#70727,#70728,#70729,#70730,#70731,#70732,#70733,
#70734,#70735,#70736,#70737,#70738,#70739,#70740,#70741,#70742,#70743,#70744,
#70745,#70746,#70747,#70748,#70749,#70750,#70751,#70752,#70753,#70754,#70755,
#70756,#70757,#70758,#70759,#70760,#70761,#70762,#70763,#70764,#70765,#70766,
#70767,#70768,#70769,#70770,#70771,#70772,#70773,#70774,#70775,#70776,#70777,
#70778,#70779,#70780,#70781,#70782,#70783,#70784,#70785,#70786,#70787,#70788,
#70789,#70790,#70791,#70792,#70793,#70794,#70795,#70796,#70797,#70798,#70799,
#70800,#70801),.UNSPECIFIED.,.F.,.F.,(4,3,3,3,3,3,3,3,3,3,3,3,3,3,3,3,3,
3,3,3,3,3,3,3,3,3,3,3,3,3,3,3,3,3,3,3,3,3,3,3,3,3,3,3,3,3,4),(135.088484104361,
135.237436223158,135.253155342757,135.346230651226,135.439179902308,135.532030728637,
135.62481373408,135.717561588724,135.810299114997,135.903051120201,135.995902319113,
136.088805337276,136.181863678489,136.252670481284,136.345745789753,136.438695040834,
136.531545867164,136.624328872607,136.71707672725,136.809814253523,136.902566258727,
136.995417457639,137.088320475802,137.181378817015,137.252185619811,137.34526092828,
137.438210179361,137.531061005691,137.623844011134,137.716591865777,137.80932939205,
137.902081397254,137.994932596166,138.087835614329,138.180893955542,138.251700758337,
138.344778545276,138.4377296359,138.534512329863,138.627291714081,138.720036095634,
138.81277029574,138.905519120361,138.998356489675,139.091246249693,139.184264767409,
139.211991187604),.UNSPECIFIED.);
#7770=B_SPLINE_CURVE_WITH_KNOTS('',3,(#70802,#70803,#70804,#70805,#70806,
#70807,#70808,#70809,#70810,#70811,#70812,#70813,#70814,#70815,#70816,#70817,
#70818,#70819,#70820,#70821,#70822,#70823,#70824,#70825,#70826,#70827,#70828,
#70829,#70830,#70831,#70832,#70833,#70834,#70835,#70836,#70837,#70838,#70839,
#70840,#70841,#70842,#70843,#70844,#70845,#70846,#70847,#70848,#70849,#70850,
#70851,#70852,#70853,#70854,#70855,#70856,#70857,#70858,#70859,#70860,#70861,
#70862,#70863,#70864,#70865,#70866,#70867,#70868,#70869,#70870,#70871,#70872,
#70873,#70874),.UNSPECIFIED.,.F.,.F.,(4,3,3,3,3,3,3,3,3,3,3,3,3,3,3,3,3,
3,3,3,3,3,3,3,4),(132.928545070227,133.021407547004,133.114327621085,133.207395885124,
133.254125065704,133.347200374173,133.440149625254,133.533000451584,133.625783457027,
133.71853131167,133.811268837943,133.904020843148,133.99687204206,134.089775060222,
134.182833401435,134.25364020423,134.345326368138,134.438221085142,134.529675013034,
134.621071924508,134.712437996792,134.806449523636,134.897871489002,134.993177796584,
135.088484104166),.UNSPECIFIED.);
#7771=B_SPLINE_CURVE_WITH_KNOTS('',3,(#70875,#70876,#70877,#70878,#70879,
#70880,#70881,#70882,#70883,#70884,#70885,#70886,#70887,#70888,#70889,#70890,
#70891,#70892,#70893,#70894,#70895,#70896,#70897,#70898,#70899,#70900,#70901,
#70902,#70903,#70904,#70905,#70906,#70907,#70908,#70909,#70910,#70911,#70912,
#70913,#70914,#70915,#70916,#70917,#70918,#70919,#70920,#70921,#70922,#70923,
#70924,#70925,#70926,#70927,#70928,#70929,#70930,#70931,#70932,#70933,#70934,
#70935,#70936,#70937,#70938,#70939,#70940,#70941,#70942,#70943,#70944,#70945,
#70946,#70947,#70948,#70949,#70950,#70951,#70952,#70953,#70954,#70955,#70956,
#70957,#70958,#70959,#70960,#70961,#70962,#70963,#70964,#70965,#70966,#70967,
#70968,#70969,#70970,#70971,#70972,#70973,#70974,#70975,#70976,#70977,#70978,
#70979,#70980,#70981,#70982,#70983,#70984,#70985,#70986,#70987,#70988,#70989,
#70990,#70991,#70992,#70993,#70994,#70995,#70996,#70997,#70998,#70999,#71000,
#71001,#71002,#71003,#71004,#71005,#71006,#71007,#71008,#71009,#71010,#71011,
#71012,#71013,#71014,#71015,#71016,#71017,#71018,#71019,#71020,#71021,#71022,
#71023,#71024,#71025,#71026,#71027,#71028,#71029,#71030,#71031,#71032,#71033,
#71034,#71035,#71036,#71037,#71038,#71039,#71040,#71041,#71042,#71043,#71044,
#71045,#71046,#71047,#71048,#71049,#71050,#71051,#71052,#71053,#71054,#71055,
#71056,#71057,#71058,#71059,#71060,#71061,#71062,#71063,#71064,#71065,#71066,
#71067,#71068,#71069,#71070,#71071,#71072,#71073,#71074,#71075,#71076,#71077,
#71078,#71079,#71080,#71081,#71082,#71083,#71084,#71085,#71086,#71087,#71088,
#71089,#71090,#71091,#71092,#71093,#71094,#71095,#71096,#71097,#71098,#71099,
#71100,#71101,#71102,#71103,#71104,#71105,#71106,#71107,#71108,#71109,#71110,
#71111,#71112,#71113,#71114,#71115,#71116,#71117,#71118,#71119,#71120,#71121,
#71122,#71123,#71124),.UNSPECIFIED.,.F.,.F.,(4,2,2,2,2,2,2,2,2,2,2,2,2,
2,2,2,2,2,2,2,2,2,2,2,2,2,2,2,2,2,2,2,2,2,2,2,2,2,2,2,2,2,2,2,2,2,2,2,2,
2,2,2,2,2,2,2,2,2,2,2,2,2,2,2,2,2,2,2,2,2,2,2,2,2,2,2,2,2,2,2,2,2,2,2,2,
2,2,2,2,2,2,2,2,2,2,2,2,2,2,2,2,2,2,2,2,2,2,2,2,2,2,2,2,2,2,2,2,2,2,2,2,
2,2,2,4),(-2.72842990354347,-2.70766769512995,-2.6942083450261,-2.69032641412718,
-2.68793745525578,-2.68576341178936,-2.68295968932953,-2.67712046877146,
-2.63063934267072,-2.5880968797651,-2.55250460569061,-2.53809976652567,
-2.52985337158713,-2.52761196869737,-2.52626444661439,-2.52504706458398,
-2.52346812029311,-2.52003765440959,-2.49066090251216,-2.44506140859784,
-2.37653288206304,-2.36952857624585,-2.36650951654422,-2.36430187674465,
-2.36227179210575,-2.35952745695151,-2.3541770481256,-2.28584341494831,
-2.23778788037546,-2.21777201815287,-2.20736906762255,-2.20494608305251,
-2.20355813185942,-2.20234875391929,-2.20081195290185,-2.1977868448031,
-2.17933208759673,-2.1753358924617,-2.08437847485296,-2.06205206729347,
-2.05313873604425,-2.04648403466199,-2.0435272227084,-2.04133043614501,
-2.0392856062088,-2.03648311220173,-2.030903432398,-1.97413015221405,-1.92470006520282,
-1.9015739586996,-1.88541533275022,-1.88276232408945,-1.88117770976386,
-1.87995959945233,-1.8786151925395,-1.87638740526087,-1.8682819902373,-1.85421801922655,
-1.81989185582541,-1.73472430248931,-1.7293547575476,-1.72342226494308,
-1.72058897177721,-1.71840420938142,-1.71605222655256,-1.71233554621172,
-1.70039715851024,-1.61408834712132,-1.59029772359292,-1.56321271142551,
-1.55983930037145,-1.55827120114759,-1.55705541744229,-1.55570227929214,
-1.55343542648626,-1.54491496137658,-1.47115370504828,-1.44011485971511,
-1.43564879486142,-1.42803458413242,-1.40474841923989,-1.4003341190964,
-1.39756113872085,-1.39539111341917,-1.39298634665299,-1.38903270132803,
-1.37485292224637,-1.35098092468692,-1.25034652258437,-1.23908396608546,
-1.23672112735015,-1.23520707213294,-1.23399943703651,-1.23259510849258,
-1.23009818647201,-1.21865563785451,-1.14229811453678,-1.08350902914624,
-1.07811614283608,-1.07536084387891,-1.07332790972965,-1.07112225295888,
-1.0681150247259,-1.06117886109398,-0.990354423422638,-0.952969625905835,
-0.940083104741701,-0.933118628276231,-0.916759211860557,-0.914095936035225,
-0.912508195943698,-0.911289487506822,-0.90994636280351,-0.907724848615461,
-0.899686326135728,-0.834882493174149,-0.760393619317092,-0.754552239014083,
-0.751748112899278,-0.749574036381803,-0.747185322837953,-0.743304422160899,
-0.72985492972577,-0.707644843877127,-0.69888673766205),.UNSPECIFIED.);
#7772=B_SPLINE_CURVE_WITH_KNOTS('',3,(#71130,#71131,#71132,#71133,#71134,
#71135,#71136,#71137,#71138,#71139,#71140,#71141,#71142,#71143,#71144,#71145,
#71146,#71147,#71148,#71149,#71150,#71151,#71152,#71153,#71154,#71155,#71156,
#71157,#71158,#71159,#71160,#71161,#71162,#71163,#71164,#71165,#71166,#71167,
#71168,#71169,#71170,#71171,#71172,#71173,#71174,#71175,#71176,#71177,#71178,
#71179,#71180,#71181,#71182,#71183,#71184,#71185,#71186,#71187,#71188,#71189,
#71190,#71191,#71192,#71193,#71194,#71195,#71196,#71197,#71198,#71199,#71200,
#71201,#71202,#71203,#71204,#71205,#71206,#71207,#71208,#71209,#71210,#71211,
#71212,#71213,#71214,#71215,#71216,#71217,#71218,#71219,#71220,#71221,#71222,
#71223,#71224,#71225,#71226,#71227,#71228,#71229,#71230,#71231,#71232,#71233,
#71234,#71235,#71236,#71237,#71238,#71239,#71240,#71241,#71242,#71243,#71244,
#71245,#71246,#71247,#71248,#71249,#71250,#71251,#71252,#71253,#71254,#71255,
#71256,#71257,#71258,#71259,#71260,#71261,#71262,#71263,#71264,#71265,#71266,
#71267,#71268),.UNSPECIFIED.,.F.,.F.,(4,3,3,3,3,3,3,3,3,3,3,3,3,3,3,3,3,
3,3,3,3,3,3,3,3,3,3,3,3,3,3,3,3,3,3,3,3,3,3,3,3,3,3,3,3,3,4),(141.371669411806,
141.463384214536,141.554991223589,141.646519531568,141.738006772963,141.829479020253,
141.920962326293,142.012539031028,142.104166831879,142.195941236867,142.249761312444,
142.342836620913,142.435785871994,142.528636698324,142.621419703766,142.71416755841,
142.806905084683,142.899657089887,142.992508288799,143.085411306962,143.178469648175,
143.249276450971,143.34235175944,143.435301010522,143.528151836851,143.620934842294,
143.713682696937,143.806420223211,143.899172228415,143.992023427327,144.084926445489,
144.177984786703,144.248791589498,144.341866897967,144.434816149048,144.527666975378,
144.620449980821,144.713197835464,144.805935361737,144.898687366942,144.991538565854,
145.084441584016,145.17749992523,145.248306728025,145.341382587312,145.434319351534,
145.495979852349),.UNSPECIFIED.);
#7773=B_SPLINE_CURVE_WITH_KNOTS('',3,(#71269,#71270,#71271,#71272,#71273,
#71274,#71275,#71276,#71277,#71278,#71279,#71280,#71281,#71282,#71283,#71284,
#71285,#71286,#71287,#71288,#71289,#71290,#71291,#71292,#71293,#71294,#71295,
#71296,#71297,#71298,#71299,#71300,#71301,#71302,#71303,#71304,#71305,#71306,
#71307,#71308,#71309,#71310,#71311,#71312,#71313,#71314,#71315,#71316,#71317,
#71318,#71319,#71320,#71321,#71322,#71323,#71324,#71325,#71326,#71327,#71328,
#71329,#71330,#71331,#71332,#71333,#71334,#71335,#71336,#71337,#71338,#71339,
#71340,#71341),.UNSPECIFIED.,.F.,.F.,(4,3,3,3,3,3,3,3,3,3,3,3,3,3,3,3,3,
3,3,3,3,3,3,3,4),(139.211991187604,139.251215896864,139.344291205333,139.437240456415,
139.530091282744,139.622874288187,139.715622142831,139.808359669104,139.901111674308,
139.99396287322,140.086865891383,140.179924232596,140.250731035391,140.34380634386,
140.436755594941,140.529606421271,140.622389426714,140.715137281357,140.807874807631,
140.900626812835,140.993478011747,141.086381029909,141.179439371123,141.250246173918,
141.371669411541),.UNSPECIFIED.);
#7774=B_SPLINE_CURVE_WITH_KNOTS('',3,(#71343,#71344,#71345,#71346,#71347,
#71348,#71349,#71350,#71351,#71352,#71353,#71354,#71355,#71356,#71357,#71358,
#71359,#71360,#71361,#71362,#71363,#71364,#71365,#71366,#71367,#71368,#71369,
#71370,#71371,#71372,#71373,#71374,#71375,#71376,#71377,#71378,#71379,#71380,
#71381,#71382,#71383,#71384,#71385,#71386,#71387,#71388,#71389,#71390,#71391,
#71392,#71393,#71394,#71395,#71396,#71397,#71398,#71399,#71400,#71401,#71402,
#71403,#71404,#71405,#71406,#71407,#71408,#71409,#71410,#71411,#71412,#71413,
#71414,#71415,#71416,#71417,#71418,#71419,#71420),.UNSPECIFIED.,.F.,.F.,
(4,2,2,2,2,2,2,2,2,2,2,2,2,2,2,2,2,2,2,2,2,2,2,2,2,2,2,2,2,2,2,2,2,2,2,
2,2,2,4),(-0.69888673766205,-0.61737787321185,-0.594275608976044,-0.591026220873479,
-0.589465041978538,-0.588253091333074,-0.587117868684638,-0.585062158207513,
-0.578589646343834,-0.535932535679405,-0.486495518521697,-0.437574746740716,
-0.431689648993861,-0.428906969588854,-0.426729261503032,-0.424352620734406,
-0.420526861896465,-0.407607888619948,-0.386575505212662,-0.314006926819699,
-0.271968688127983,-0.268365761394296,-0.266754730065773,-0.265532332063873,
-0.264200190209017,-0.262822357527625,-0.258425659352045,-0.225457271361734,
-0.198905423977322,-0.168653175776428,-0.114842416928233,-0.109483429210097,
-0.106736599750281,-0.104705605295463,-0.102497882458647,-0.0994803463246609,
-0.0924869291109943,-0.0829993670765108,-0.000961141795237354),
 .UNSPECIFIED.);
#7775=B_SPLINE_CURVE_WITH_KNOTS('',3,(#71421,#71422,#71423,#71424,#71425,
#71426,#71427,#71428,#71429,#71430,#71431,#71432,#71433,#71434,#71435,#71436,
#71437,#71438,#71439,#71440,#71441,#71442,#71443,#71444,#71445,#71446,#71447,
#71448,#71449,#71450,#71451,#71452,#71453,#71454,#71455,#71456,#71457,#71458,
#71459,#71460,#71461,#71462,#71463,#71464,#71465,#71466,#71467,#71468,#71469,
#71470,#71471,#71472,#71473,#71474,#71475,#71476,#71477,#71478,#71479,#71480,
#71481,#71482,#71483,#71484,#71485,#71486,#71487,#71488,#71489,#71490,#71491,
#71492,#71493,#71494,#71495,#71496,#71497,#71498,#71499,#71500,#71501,#71502,
#71503,#71504,#71505,#71506,#71507,#71508,#71509,#71510,#71511,#71512,#71513,
#71514,#71515,#71516,#71517,#71518,#71519,#71520,#71521,#71522,#71523,#71524,
#71525,#71526,#71527,#71528,#71529,#71530,#71531,#71532,#71533,#71534,#71535,
#71536,#71537,#71538,#71539,#71540,#71541,#71542,#71543,#71544,#71545,#71546,
#71547,#71548,#71549,#71550,#71551,#71552,#71553,#71554,#71555,#71556,#71557,
#71558,#71559,#71560,#71561,#71562,#71563,#71564,#71565,#71566,#71567,#71568,
#71569,#71570,#71571,#71572,#71573,#71574,#71575,#71576,#71577,#71578,#71579,
#71580,#71581,#71582,#71583,#71584,#71585,#71586,#71587,#71588),
 .UNSPECIFIED.,.F.,.F.,(4,2,2,2,2,2,2,2,2,2,2,2,2,2,2,2,2,2,2,2,2,2,2,2,
2,2,2,2,2,2,2,2,2,2,2,2,2,2,2,2,2,2,2,2,2,2,2,2,2,2,2,2,2,2,2,2,2,2,2,2,
2,2,2,2,2,2,2,2,2,2,2,2,2,2,2,2,2,2,2,2,2,2,2,4),(-4.06093435138946,-4.01153152329989,
-4.00789799007013,-4.00586629122596,-4.00448963764063,-4.0031583524371,
-4.00193575656261,-4.00032313025772,-3.99671113649732,-3.94836980179485,
-3.93081203940535,-3.91540010078564,-3.8783489475813,-3.85346745779512,
-3.84649300711091,-3.84347886169196,-3.841271802689,-3.83924014409437,-3.83649047935593,
-3.83112019156007,-3.77619062026438,-3.74501588752085,-3.70204042269368,
-3.69068050460192,-3.68378080101615,-3.68168021627958,-3.68054226929608,
-3.67933272562805,-3.67779581283627,-3.67477078687394,-3.65632486505783,
-3.65227377042139,-3.60355190709301,-3.53018787326717,-3.52350438671813,
-3.52054201660475,-3.51834394656903,-3.51629995882664,-3.51295859473903,
-3.50460146736822,-3.50270997680874,-3.41873810735623,-3.3835693899566,
-3.369279173774,-3.36110458940688,-3.35887608705832,-3.35752108400561,-3.35630532340663,
-3.35473949451488,-3.35215100395849,-3.3372448520238,-3.23999313708196,
-3.2166081869537,-3.20263822828317,-3.19870472567385,-3.19630417514178,
-3.19413273119173,-3.19135069325714,-3.18562245873916,-3.10696899088985,
-3.04581173522982,-3.03799123386341,-3.0357910532956,-3.03445261470516,
-3.03323232429893,-3.03163469322602,-3.02810467681065,-2.97096909782754,
-2.92135992783375,-2.8951429948549,-2.87996436177344,-2.87591591822703,
-2.87348960525738,-2.87132304597746,-2.86858561631221,-2.86428873470835,
-2.84289084550076,-2.83880702740414,-2.83710395355222,-2.82351885727087,
-2.82195046521615,-2.82092381306869,-2.74570799838588,-2.72901630049176),
 .UNSPECIFIED.);
#7776=B_SPLINE_CURVE_WITH_KNOTS('',3,(#71594,#71595,#71596,#71597,#71598,
#71599,#71600,#71601,#71602,#71603,#71604,#71605,#71606,#71607,#71608,#71609,
#71610,#71611,#71612,#71613,#71614,#71615,#71616,#71617,#71618,#71619,#71620,
#71621,#71622,#71623,#71624,#71625,#71626,#71627,#71628,#71629,#71630,#71631,
#71632,#71633,#71634,#71635,#71636,#71637,#71638,#71639,#71640,#71641,#71642,
#71643,#71644,#71645,#71646,#71647,#71648,#71649,#71650,#71651,#71652,#71653,
#71654,#71655,#71656,#71657,#71658,#71659,#71660,#71661,#71662,#71663,#71664,
#71665,#71666,#71667,#71668,#71669,#71670,#71671,#71672,#71673,#71674,#71675,
#71676,#71677,#71678,#71679,#71680,#71681,#71682,#71683,#71684,#71685,#71686,
#71687,#71688,#71689,#71690,#71691,#71692,#71693,#71694,#71695,#71696,#71697,
#71698,#71699,#71700,#71701,#71702,#71703,#71704,#71705,#71706,#71707,#71708,
#71709,#71710,#71711,#71712,#71713,#71714,#71715,#71716,#71717,#71718,#71719,
#71720,#71721,#71722,#71723,#71724,#71725,#71726,#71727,#71728,#71729,#71730,
#71731,#71732),.UNSPECIFIED.,.F.,.F.,(4,3,3,3,3,3,3,3,3,3,3,3,3,3,3,3,3,
3,3,3,3,3,3,3,3,3,3,3,3,3,3,3,3,3,3,3,3,3,3,3,3,3,3,3,3,3,4),(147.654854718721,
147.749034590717,147.843249280477,147.937520831394,148.031935902181,148.126434874257,
148.221101205661,148.246852143605,148.339927452074,148.432876703156,148.525727529485,
148.618510534928,148.711258389572,148.803995915845,148.896747921049,148.989599119961,
149.082502138124,149.175560479337,149.246367282132,149.339442590601,149.432391841682,
149.525242668012,149.618025673454,149.710773528098,149.803511054371,149.896263059575,
149.989114258487,150.08201727665,150.175075617863,150.245882420659,150.338957729128,
150.431906980209,150.524757806539,150.617540811982,150.710288666625,150.803026192899,
150.895778198103,150.988629397015,151.081532415177,151.174590756391,151.245397559185,
151.338468831933,151.431419321105,151.524261223258,151.617039297619,151.709788393534,
151.778475043453),.UNSPECIFIED.);
#7777=B_SPLINE_CURVE_WITH_KNOTS('',3,(#71733,#71734,#71735,#71736,#71737,
#71738,#71739,#71740,#71741,#71742,#71743,#71744,#71745,#71746,#71747,#71748,
#71749,#71750,#71751,#71752,#71753,#71754,#71755,#71756,#71757,#71758,#71759,
#71760,#71761,#71762,#71763,#71764,#71765,#71766,#71767,#71768,#71769,#71770,
#71771,#71772,#71773,#71774,#71775,#71776,#71777,#71778,#71779,#71780,#71781,
#71782,#71783,#71784,#71785,#71786,#71787,#71788,#71789,#71790,#71791,#71792,
#71793,#71794,#71795,#71796,#71797,#71798,#71799,#71800,#71801,#71802),
 .UNSPECIFIED.,.F.,.F.,(4,3,3,3,3,3,3,3,3,3,3,3,3,3,3,3,3,3,3,3,3,3,3,4),
(145.495979852349,145.589960104124,145.682716610858,145.775454763184,145.868199371119,
145.963104994977,146.055990070736,146.151905968644,146.247821866552,146.340897175021,
146.433846426103,146.526697252432,146.619480257875,146.712228112519,146.804965638792,
146.897717643997,146.990568842909,147.083471861071,147.176530202285,147.247337005078,
147.350216986418,147.452811717714,147.554895483707,147.654854718549),
 .UNSPECIFIED.);
#7778=B_SPLINE_CURVE_WITH_KNOTS('',3,(#71803,#71804,#71805,#71806,#71807,
#71808,#71809,#71810,#71811,#71812,#71813,#71814,#71815,#71816,#71817,#71818,
#71819,#71820,#71821,#71822,#71823,#71824,#71825,#71826,#71827,#71828,#71829,
#71830,#71831,#71832,#71833,#71834,#71835,#71836,#71837,#71838,#71839,#71840,
#71841,#71842,#71843,#71844,#71845,#71846,#71847,#71848,#71849,#71850,#71851,
#71852,#71853,#71854,#71855,#71856,#71857,#71858,#71859,#71860,#71861,#71862,
#71863,#71864,#71865,#71866,#71867,#71868,#71869,#71870,#71871,#71872,#71873,
#71874,#71875,#71876,#71877,#71878,#71879,#71880,#71881,#71882,#71883,#71884,
#71885,#71886,#71887,#71888,#71889,#71890,#71891,#71892,#71893,#71894,#71895,
#71896,#71897,#71898,#71899,#71900,#71901,#71902,#71903,#71904,#71905,#71906,
#71907,#71908,#71909,#71910,#71911,#71912,#71913,#71914,#71915,#71916,#71917,
#71918,#71919,#71920,#71921,#71922,#71923,#71924,#71925,#71926,#71927,#71928,
#71929,#71930,#71931,#71932,#71933,#71934,#71935,#71936,#71937,#71938,#71939,
#71940,#71941,#71942,#71943,#71944,#71945,#71946,#71947,#71948,#71949,#71950,
#71951,#71952,#71953,#71954,#71955,#71956,#71957,#71958,#71959,#71960,#71961,
#71962,#71963,#71964,#71965,#71966,#71967,#71968,#71969,#71970,#71971,#71972,
#71973,#71974,#71975,#71976,#71977,#71978,#71979,#71980,#71981,#71982,#71983,
#71984,#71985,#71986,#71987,#71988,#71989,#71990,#71991,#71992,#71993,#71994,
#71995,#71996,#71997,#71998,#71999,#72000,#72001,#72002,#72003,#72004,#72005,
#72006,#72007,#72008,#72009,#72010,#72011,#72012,#72013,#72014,#72015,#72016,
#72017,#72018,#72019,#72020,#72021,#72022,#72023,#72024,#72025,#72026,#72027,
#72028,#72029,#72030,#72031,#72032,#72033,#72034,#72035,#72036,#72037,#72038,
#72039,#72040),.UNSPECIFIED.,.F.,.F.,(4,2,2,2,2,2,2,2,2,2,2,2,2,2,2,2,2,
2,2,2,2,2,2,2,2,2,2,2,2,2,2,2,2,2,2,2,2,2,2,2,2,2,2,2,2,2,2,2,2,2,2,2,2,
2,2,2,2,2,2,2,2,2,2,2,2,2,2,2,2,2,2,2,2,2,2,2,2,2,2,2,2,2,2,2,2,2,2,2,2,
2,2,2,2,2,2,2,2,2,2,2,2,2,2,2,2,2,2,2,2,2,2,2,2,2,2,2,2,2,4),(-2.72901630049176,
-2.72588029484488,-2.71554420431033,-2.71312586823548,-2.71173875403762,
-2.71052894744365,-2.70899008968555,-2.70595629961924,-2.6873194778769,
-2.59330998046564,-2.57046281203296,-2.55672882229577,-2.55281870986864,
-2.55042328960037,-2.54825050475498,-2.54545840305993,-2.53967951871034,
-2.46283569056572,-2.4000599990981,-2.39214097159969,-2.38993093493505,
-2.38859024706071,-2.38737056367352,-2.38577729038927,-2.38309555495988,
-2.36636665265747,-2.36348263533094,-2.3080487493928,-2.23712415971649,
-2.23126258824115,-2.22845421704563,-2.22627925759363,-2.22418772303356,
-2.22060091265583,-2.21068025805306,-2.12938578572331,-2.09248124940335,
-2.07769558917056,-2.06929209686111,-2.0670355730592,-2.06568446694449,
-2.06446765524131,-2.06289447889109,-2.05949583878602,-2.03146916409239,
-1.98357305133032,-1.91431881122955,-1.9089700478127,-1.90622580222741,
-1.90419542231494,-1.9019871110333,-1.89896650844108,-1.89195582167329,
-1.82240058939648,-1.77796017705985,-1.74836136439719,-1.74492514771631,
-1.74334489704457,-1.74212709261085,-1.74077972603305,-1.73853993891986,
-1.73031419686828,-1.71596244845137,-1.680570361235,-1.59700231945177,-1.59465226744745,
-1.58660505333646,-1.58331582383525,-1.58128151727221,-1.57907643227049,
-1.57607366703063,-1.56916411469123,-1.55981954888957,-1.53596303824289,
-1.43546509614923,-1.42402577210174,-1.42164993718324,-1.42013165984848,
-1.41892341312118,-1.41752150841245,-1.41503670331932,-1.40377937417503,
-1.32822615235987,-1.2683871392199,-1.26299112223109,-1.26023463817137,
-1.25820103060483,-1.25599483710384,-1.25298722417104,-1.24605171485911,
-1.1821508514095,-1.13971819026412,-1.12039022732583,-1.1017834573835,-1.09875077771291,
-1.09721207318116,-1.0960021810802,-1.09461473225072,-1.0921952559819,-1.08184595260976,
-1.06198529371962,-0.98695710065982,-0.945058158606808,-0.939326159771434,
-0.936543030143212,-0.93437106551414,-0.931970277146261,-0.928037154741231,
-0.914076572114394,-0.890711584586582,-0.793545756854862,-0.77844788971629,
-0.775848604212841,-0.774279368708628,-0.773062877220329,-0.771709140413467,
-0.769441699493578,-0.760923745953994,-0.698659185575319),.UNSPECIFIED.);
#7779=B_SPLINE_CURVE_WITH_KNOTS('',3,(#72046,#72047,#72048,#72049,#72050,
#72051,#72052,#72053,#72054,#72055,#72056,#72057,#72058,#72059,#72060,#72061,
#72062,#72063,#72064,#72065,#72066,#72067,#72068,#72069,#72070,#72071,#72072,
#72073,#72074,#72075,#72076,#72077,#72078,#72079,#72080,#72081,#72082,#72083,
#72084,#72085,#72086,#72087,#72088,#72089,#72090,#72091,#72092,#72093,#72094,
#72095,#72096,#72097,#72098,#72099,#72100,#72101,#72102,#72103,#72104,#72105,
#72106,#72107,#72108,#72109,#72110,#72111,#72112,#72113,#72114,#72115,#72116,
#72117,#72118,#72119,#72120,#72121,#72122,#72123,#72124,#72125,#72126,#72127,
#72128,#72129,#72130,#72131,#72132,#72133,#72134,#72135,#72136,#72137,#72138,
#72139,#72140,#72141,#72142,#72143,#72144,#72145,#72146,#72147,#72148,#72149,
#72150,#72151,#72152,#72153,#72154,#72155,#72156,#72157,#72158,#72159,#72160,
#72161,#72162,#72163,#72164,#72165,#72166,#72167,#72168,#72169,#72170,#72171,
#72172,#72173,#72174,#72175,#72176,#72177,#72178,#72179,#72180,#72181),
 .UNSPECIFIED.,.F.,.F.,(4,3,3,3,3,3,3,3,3,3,3,3,3,3,3,3,3,3,3,3,3,3,3,3,
3,3,3,3,3,3,3,3,3,3,3,3,3,3,3,3,3,3,3,3,3,4),(153.938040026209,154.04907363987,
154.161545321533,154.243942974766,154.337018283235,154.429967534316,154.522818360646,
154.615601366089,154.708349220732,154.801086747005,154.893838752209,154.986689951121,
155.079592969284,155.172651310497,155.243458113292,155.336533421761,155.429482672842,
155.522333499172,155.615116504615,155.707864359258,155.800601885531,155.893353890736,
155.986205089648,156.07910810781,156.172166449023,156.242973251819,156.336048560288,
156.42899781137,156.521848637699,156.614631643142,156.707379497786,156.800117024059,
156.892869029263,156.985720228175,157.078623246338,157.171681587551,157.242488390346,
157.335575759881,157.428507308114,157.521349741414,157.614127982882,157.706866895333,
157.799623116126,157.892384934503,157.985231229661,158.0611738712),
 .UNSPECIFIED.);
#7780=B_SPLINE_CURVE_WITH_KNOTS('',3,(#72182,#72183,#72184,#72185,#72186,
#72187,#72188,#72189,#72190,#72191,#72192,#72193,#72194,#72195,#72196,#72197,
#72198,#72199,#72200,#72201,#72202,#72203,#72204,#72205,#72206,#72207,#72208,
#72209,#72210,#72211,#72212,#72213,#72214,#72215,#72216,#72217,#72218,#72219,
#72220,#72221,#72222,#72223,#72224,#72225,#72226,#72227,#72228,#72229,#72230,
#72231,#72232,#72233,#72234,#72235,#72236,#72237,#72238,#72239,#72240,#72241,
#72242,#72243,#72244,#72245,#72246,#72247,#72248,#72249,#72250,#72251,#72252,
#72253,#72254),.UNSPECIFIED.,.F.,.F.,(4,3,3,3,3,3,3,3,3,3,3,3,3,3,3,3,3,
3,3,3,3,3,3,3,4),(151.778475043453,151.871220907862,151.964643855325,152.057531651525,
152.151222174619,152.244912697712,152.337988006181,152.430937257262,152.523788083591,
152.616571089034,152.709318943678,152.802056469951,152.894808475155,152.987659674067,
153.08056269223,153.173621033443,153.244427836239,153.337016135053,153.429485246562,
153.521860686742,153.614167880084,153.706445323099,153.798704748058,153.890999970072,
153.9380400259),.UNSPECIFIED.);
#7781=B_SPLINE_CURVE_WITH_KNOTS('',3,(#72256,#72257,#72258,#72259,#72260,
#72261,#72262,#72263,#72264,#72265,#72266,#72267,#72268,#72269,#72270,#72271,
#72272,#72273,#72274,#72275,#72276,#72277,#72278,#72279,#72280,#72281,#72282,
#72283,#72284,#72285,#72286,#72287,#72288,#72289,#72290,#72291,#72292,#72293,
#72294,#72295,#72296,#72297,#72298,#72299,#72300,#72301,#72302,#72303,#72304,
#72305,#72306,#72307,#72308,#72309,#72310,#72311,#72312,#72313,#72314,#72315,
#72316,#72317,#72318,#72319,#72320,#72321,#72322,#72323,#72324,#72325,#72326,
#72327,#72328,#72329,#72330,#72331,#72332,#72333,#72334,#72335,#72336,#72337,
#72338,#72339,#72340,#72341,#72342,#72343,#72344,#72345,#72346,#72347,#72348,
#72349,#72350,#72351,#72352,#72353,#72354,#72355,#72356,#72357,#72358,#72359,
#72360,#72361,#72362,#72363,#72364,#72365,#72366,#72367,#72368,#72369,#72370,
#72371,#72372,#72373,#72374,#72375,#72376,#72377,#72378,#72379,#72380,#72381,
#72382,#72383,#72384,#72385,#72386,#72387),.UNSPECIFIED.,.F.,.F.,(4,2,2,
2,2,2,2,2,2,2,2,2,2,2,2,2,2,2,2,2,2,2,2,2,2,2,2,2,2,2,2,2,2,2,2,2,2,2,2,
2,2,2,2,2,2,2,2,2,2,2,2,2,2,2,2,2,2,2,2,2,2,2,2,2,2,4),(-0.698659185575319,
-0.687266515453911,-0.622356187764353,-0.616969918375531,-0.614215814685308,
-0.612182701337184,-0.610019936900468,-0.607121258634964,-0.603881266552389,
-0.598394520947855,-0.560376419496656,-0.490122354470279,-0.48025461911514,
-0.456084254210486,-0.452797334160289,-0.451245263777175,-0.450031031409607,
-0.448667611165948,-0.446356722551842,-0.437352533337298,-0.421071586591021,
-0.371014250546084,-0.299259701627354,-0.29336012398568,-0.290574201590711,
-0.288395530193951,-0.288370833317646,-0.288347238818523,-0.288324689518502,
-0.288303131734123,-0.288282515070775,-0.288262792170785,-0.288243918504708,
-0.288225852161942,-0.288208553689533,-0.288191985917783,-0.288176113790564,
-0.288160904224996,-0.288146325992296,-0.288132349575939,-0.288118947105193,
-0.288106092203015,-0.288093759882848,-0.288081926500809,-0.288068418482872,
-0.288055037864439,-0.288041781084367,-0.288028646155354,-0.288015631104619,
-0.288002734006105,-0.285546058246958,-0.281311570021109,-0.276154174713262,
-0.265653300801223,-0.237507845314393,-0.170139024840153,-0.157172011659093,
-0.13312383978533,-0.129841074410973,-0.128289806795767,-0.127075677672748,
-0.125711792394532,-0.12339880635479,-0.114370410182652,-0.0980277981269592,
-0.000961400426472246),.UNSPECIFIED.);
#7782=B_SPLINE_CURVE_WITH_KNOTS('',3,(#72388,#72389,#72390,#72391,#72392,
#72393,#72394,#72395,#72396,#72397,#72398,#72399,#72400,#72401,#72402,#72403,
#72404,#72405,#72406,#72407,#72408,#72409,#72410,#72411,#72412,#72413,#72414,
#72415,#72416,#72417,#72418,#72419,#72420,#72421,#72422,#72423,#72424,#72425,
#72426,#72427,#72428,#72429,#72430,#72431,#72432,#72433,#72434,#72435,#72436,
#72437,#72438,#72439,#72440,#72441,#72442,#72443,#72444,#72445,#72446,#72447,
#72448,#72449,#72450,#72451,#72452,#72453,#72454,#72455,#72456,#72457,#72458,
#72459,#72460,#72461,#72462,#72463,#72464,#72465,#72466,#72467,#72468,#72469,
#72470,#72471,#72472,#72473,#72474,#72475,#72476,#72477,#72478,#72479,#72480,
#72481,#72482,#72483,#72484,#72485,#72486,#72487,#72488,#72489,#72490,#72491,
#72492,#72493,#72494,#72495,#72496,#72497,#72498,#72499,#72500,#72501,#72502,
#72503,#72504,#72505,#72506,#72507,#72508,#72509,#72510,#72511,#72512,#72513,
#72514,#72515,#72516,#72517,#72518,#72519,#72520,#72521,#72522,#72523,#72524,
#72525,#72526),.UNSPECIFIED.,.F.,.F.,(4,3,3,3,3,3,3,3,3,3,3,3,3,3,3,3,3,
3,3,3,3,3,3,3,3,3,3,3,3,3,3,3,3,3,3,3,3,3,3,3,3,3,3,3,3,3,4),(153.9380400259,
154.031841518464,154.125665311938,154.219534280467,154.313536546128,154.407613950455,
154.50185962512,154.545879037082,154.638954345551,154.731903596633,154.824754422962,
154.917537428405,155.010285283049,155.103022809322,155.195774814526,155.288626013438,
155.381529031601,155.474587372814,155.545394175609,155.638469484078,155.731418735159,
155.824269561489,155.917052566932,156.009800421575,156.102537947848,156.195289953053,
156.288141151965,156.381044170127,156.47410251134,156.544909314136,156.637984622605,
156.730933873686,156.823784700016,156.916567705459,157.009315560102,157.102053086375,
157.194805091579,157.287656290491,157.380559308654,157.473617649867,157.544424452662,
157.637497610758,157.730449616904,157.823291694321,157.916069797578,158.008814802925,
158.061709245204),.UNSPECIFIED.);
#7783=B_SPLINE_CURVE_WITH_KNOTS('',3,(#72532,#72533,#72534,#72535,#72536,
#72537,#72538,#72539,#72540,#72541,#72542,#72543,#72544,#72545,#72546,#72547,
#72548,#72549,#72550,#72551,#72552,#72553,#72554,#72555,#72556,#72557,#72558,
#72559,#72560,#72561,#72562,#72563,#72564,#72565,#72566,#72567,#72568,#72569,
#72570,#72571,#72572,#72573,#72574,#72575,#72576,#72577,#72578,#72579,#72580,
#72581,#72582,#72583,#72584,#72585,#72586,#72587,#72588,#72589,#72590,#72591,
#72592,#72593,#72594,#72595,#72596,#72597,#72598,#72599,#72600,#72601,#72602,
#72603,#72604,#72605,#72606,#72607,#72608,#72609,#72610,#72611,#72612,#72613,
#72614,#72615,#72616,#72617,#72618,#72619,#72620,#72621,#72622,#72623,#72624,
#72625,#72626,#72627,#72628,#72629,#72630,#72631,#72632,#72633,#72634,#72635,
#72636,#72637,#72638,#72639,#72640,#72641,#72642,#72643,#72644,#72645,#72646,
#72647,#72648,#72649,#72650,#72651,#72652,#72653,#72654,#72655,#72656,#72657,
#72658,#72659,#72660,#72661,#72662,#72663,#72664,#72665,#72666,#72667,#72668,
#72669,#72670,#72671,#72672,#72673),.UNSPECIFIED.,.F.,.F.,(4,3,3,3,3,3,
3,3,3,3,3,3,3,3,3,3,3,3,3,3,3,3,3,3,3,3,3,3,3,3,3,3,3,3,3,3,3,3,3,3,3,3,
3,3,3,3,3,4),(160.22122533308,160.241033805926,160.334109114395,160.427058365477,
160.519909191806,160.612692197249,160.705440051892,160.798177578166,160.89092958337,
160.983780782282,161.076683800445,161.169742141658,161.240548944453,161.333624252922,
161.426573504003,161.519424330333,161.612207335776,161.704955190419,161.797692716692,
161.890444721897,161.983295920809,162.076198938971,162.169257280184,162.24006408298,
162.333139391449,162.42608864253,162.51893946886,162.611722474303,162.704470328946,
162.797207855219,162.889959860423,162.982811059335,163.075714077498,163.168772418711,
163.239579221506,163.332654529975,163.425603781056,163.518454607386,163.611237612829,
163.703985467472,163.796722993745,163.88947499895,163.982326197861,164.075229216024,
164.168287557237,164.239094360033,164.332179484883,164.345416085528),
 .UNSPECIFIED.);
#7784=B_SPLINE_CURVE_WITH_KNOTS('',3,(#72674,#72675,#72676,#72677,#72678,
#72679,#72680,#72681,#72682,#72683,#72684,#72685,#72686,#72687,#72688,#72689,
#72690,#72691,#72692,#72693,#72694,#72695,#72696,#72697,#72698,#72699,#72700,
#72701,#72702,#72703,#72704,#72705,#72706,#72707,#72708,#72709,#72710,#72711,
#72712,#72713,#72714,#72715,#72716,#72717,#72718,#72719,#72720,#72721,#72722,
#72723,#72724,#72725,#72726,#72727,#72728,#72729,#72730,#72731,#72732,#72733,
#72734,#72735,#72736,#72737,#72738,#72739,#72740,#72741,#72742,#72743,#72744,
#72745,#72746),.UNSPECIFIED.,.F.,.F.,(4,3,3,3,3,3,3,3,3,3,3,3,3,3,3,3,3,
3,3,3,3,3,3,3,4),(158.0611738712,158.154226324278,158.242003528873,158.335078837342,
158.428028088423,158.520878914753,158.613661920196,158.706409774839,158.799147301112,
158.891899306317,158.984750505229,159.077653523391,159.170711864604,159.241518667399,
159.334279950863,159.426915408281,159.519453075191,159.611924161267,159.704361393212,
159.796789950703,159.889234999661,159.98177900834,160.074377343998,160.167124708233,
160.221225332896),.UNSPECIFIED.);
#7785=B_SPLINE_CURVE_WITH_KNOTS('',3,(#72748,#72749,#72750,#72751,#72752,
#72753,#72754,#72755,#72756,#72757,#72758,#72759,#72760,#72761,#72762,#72763,
#72764,#72765,#72766,#72767,#72768,#72769,#72770,#72771,#72772,#72773,#72774,
#72775,#72776,#72777,#72778,#72779,#72780,#72781,#72782,#72783,#72784,#72785,
#72786,#72787,#72788,#72789,#72790,#72791,#72792,#72793,#72794,#72795,#72796,
#72797,#72798,#72799,#72800,#72801,#72802,#72803,#72804,#72805,#72806,#72807,
#72808,#72809,#72810,#72811,#72812,#72813,#72814,#72815,#72816,#72817,#72818,
#72819,#72820,#72821,#72822,#72823),.UNSPECIFIED.,.F.,.F.,(4,3,3,3,3,3,
3,3,3,3,3,3,3,3,3,3,3,3,3,3,3,3,3,3,3,4),(158.061709245204,158.154451987715,
158.251823888583,158.344704552456,158.43765085974,158.530736002963,158.543939591189,
158.637014899658,158.729964150739,158.822814977069,158.915597982512,159.008345837155,
159.101083363429,159.193835368633,159.286686567545,159.379589585707,159.472647926921,
159.543454729716,159.636279965892,159.72898388903,159.821591754,159.914128724522,
160.006629196486,160.099109132765,160.191614229513,160.22122533308),
 .UNSPECIFIED.);
#7786=B_SPLINE_CURVE_WITH_KNOTS('',3,(#72824,#72825,#72826,#72827,#72828,
#72829,#72830,#72831,#72832,#72833,#72834,#72835,#72836,#72837,#72838,#72839,
#72840,#72841,#72842,#72843,#72844,#72845,#72846,#72847,#72848,#72849,#72850,
#72851,#72852,#72853,#72854,#72855,#72856,#72857,#72858,#72859,#72860,#72861,
#72862,#72863,#72864,#72865,#72866,#72867,#72868,#72869,#72870,#72871,#72872,
#72873,#72874,#72875,#72876,#72877,#72878,#72879,#72880,#72881,#72882,#72883,
#72884,#72885,#72886,#72887,#72888,#72889,#72890,#72891,#72892,#72893,#72894,
#72895,#72896,#72897,#72898,#72899,#72900,#72901,#72902,#72903,#72904,#72905,
#72906,#72907,#72908,#72909,#72910,#72911,#72912,#72913,#72914,#72915,#72916,
#72917,#72918,#72919,#72920,#72921,#72922,#72923,#72924,#72925,#72926,#72927,
#72928,#72929,#72930,#72931,#72932,#72933,#72934,#72935,#72936,#72937,#72938,
#72939,#72940,#72941,#72942,#72943,#72944,#72945,#72946,#72947,#72948,#72949,
#72950,#72951,#72952,#72953,#72954,#72955,#72956,#72957,#72958,#72959,#72960,
#72961,#72962,#72963,#72964,#72965,#72966,#72967,#72968,#72969,#72970,#72971,
#72972,#72973,#72974,#72975,#72976,#72977,#72978,#72979),.UNSPECIFIED.,
 .F.,.F.,(4,2,2,2,2,2,2,2,2,2,2,2,2,2,2,2,2,2,2,2,2,2,2,2,2,2,2,2,2,2,2,
2,2,2,2,2,2,2,2,2,2,2,2,2,2,2,2,2,2,2,2,2,2,2,2,2,2,2,2,2,2,2,2,2,2,2,2,
2,2,2,2,2,2,2,2,2,2,4),(-4.05945128562048,-4.041155615787,-3.96822305735629,
-3.95974543906513,-3.95748283761133,-3.95613082929757,-3.95491508830725,
-3.95334577591954,-3.9499649216044,-3.9225742929906,-3.91027746944697,-3.86234400841248,
-3.82583015536063,-3.81066255166307,-3.80062850272235,-3.79718115304648,
-3.79515755425338,-3.79298773552869,-3.79021391736335,-3.78579606338421,
-3.76244312156547,-3.7563929350647,-3.70573924716846,-3.64476492051424,
-3.6369572793063,-3.63475894152135,-3.63342124781676,-3.63220136847798,
-3.63060391511297,-3.62707284668614,-3.56994341699948,-3.51539368170489,
-3.49248589976508,-3.48340788196599,-3.47670951636516,-3.47375105999008,
-3.47154383658876,-3.46951425843179,-3.46677079532305,-3.46142264065606,
-3.39273544649311,-3.34509188086973,-3.32505480631329,-3.31464494853154,
-3.31222180014704,-3.31083399522521,-3.30962489668847,-3.30808864885882,
-3.30496345058287,-3.28507478640793,-3.26523581763717,-3.22340431140956,
-3.16086200942504,-3.15398071286598,-3.15098361266331,-3.14878015255424,
-3.14674555589994,-3.14345187975107,-3.13537402198371,-3.13267340178628,
-3.05582409796174,-2.99894158311332,-2.99139393853123,-2.98922186692513,
-2.98788995657361,-2.98666799641334,-2.98505785126534,-2.98145816821869,
-2.93978845584888,-2.88546371535253,-2.83676602464008,-2.83075906639412,
-2.8279230611756,-2.82574492911033,-2.82366419049867,-2.82013017169038,
-2.8105608213515,-2.72811779794129),.UNSPECIFIED.);
#7787=B_SPLINE_CURVE_WITH_KNOTS('',3,(#72985,#72986,#72987,#72988,#72989,
#72990,#72991,#72992,#72993,#72994,#72995,#72996,#72997,#72998,#72999,#73000,
#73001,#73002,#73003,#73004,#73005,#73006,#73007,#73008,#73009,#73010,#73011,
#73012,#73013,#73014,#73015,#73016,#73017,#73018,#73019,#73020,#73021,#73022,
#73023,#73024,#73025,#73026,#73027,#73028,#73029,#73030,#73031,#73032,#73033,
#73034,#73035,#73036,#73037,#73038,#73039,#73040,#73041,#73042,#73043,#73044,
#73045,#73046,#73047,#73048,#73049,#73050,#73051,#73052,#73053,#73054,#73055,
#73056,#73057,#73058,#73059,#73060,#73061,#73062,#73063,#73064,#73065,#73066,
#73067,#73068,#73069,#73070,#73071,#73072,#73073,#73074,#73075,#73076,#73077,
#73078,#73079,#73080,#73081,#73082,#73083,#73084,#73085,#73086,#73087,#73088,
#73089,#73090,#73091,#73092,#73093,#73094,#73095,#73096,#73097,#73098,#73099,
#73100,#73101,#73102,#73103,#73104,#73105,#73106,#73107,#73108,#73109,#73110,
#73111,#73112,#73113,#73114,#73115,#73116,#73117,#73118,#73119,#73120,#73121,
#73122,#73123),.UNSPECIFIED.,.F.,.F.,(4,3,3,3,3,3,3,3,3,3,3,3,3,3,3,3,3,
3,3,3,3,3,3,3,3,3,3,3,3,3,3,3,3,3,3,3,3,3,3,3,3,3,3,3,3,3,4),(166.504410640259,
166.596297384287,166.688136850633,166.779954822237,166.871777056864,166.963690802419,
167.055648939086,167.147767225871,167.237639775614,167.330715084083,167.423664335165,
167.516515161494,167.609298166937,167.702046021581,167.794783547854,167.887535553058,
167.98038675197,168.073289770132,168.166348111346,168.23715491414,168.330230222609,
168.42317947369,168.51603030002,168.608813305462,168.701561160106,168.794298686379,
168.887050691583,168.979901890495,169.072804908657,169.165863249871,169.236670052667,
169.329745361136,169.422694612218,169.515545438547,169.60832844399,169.701076298634,
169.793813824907,169.886565830111,169.979417029023,170.072320047186,170.165378388399,
170.236185191194,170.329275020313,170.422212993343,170.515063477816,170.607841724268,
170.6284544512),.UNSPECIFIED.);
#7788=B_SPLINE_CURVE_WITH_KNOTS('',3,(#73124,#73125,#73126,#73127,#73128,
#73129,#73130,#73131,#73132,#73133,#73134,#73135,#73136,#73137,#73138,#73139,
#73140,#73141,#73142,#73143,#73144,#73145,#73146,#73147,#73148,#73149,#73150,
#73151,#73152,#73153,#73154,#73155,#73156,#73157,#73158,#73159,#73160,#73161,
#73162,#73163,#73164,#73165,#73166,#73167,#73168,#73169,#73170,#73171,#73172,
#73173,#73174,#73175,#73176,#73177,#73178,#73179,#73180,#73181,#73182,#73183,
#73184,#73185,#73186,#73187,#73188,#73189,#73190,#73191,#73192,#73193,#73194,
#73195,#73196),.UNSPECIFIED.,.F.,.F.,(4,3,3,3,3,3,3,3,3,3,3,3,3,3,3,3,3,
3,3,3,3,3,3,3,4),(164.345416085528,164.438349632499,164.531188681243,164.623965162733,
164.716710030763,164.809448104393,164.90220419039,164.995061403628,165.087973612034,
165.181037179722,165.23860949856,165.331684807029,165.42463405811,165.51748488444,
165.610267889883,165.703015744526,165.795753270799,165.888505276004,165.981356474916,
166.074259493078,166.167317834292,166.238124637087,166.356936113553,166.47352002816,
166.504410640098),.UNSPECIFIED.);
#7789=B_SPLINE_CURVE_WITH_KNOTS('',3,(#73197,#73198,#73199,#73200,#73201,
#73202,#73203,#73204,#73205,#73206,#73207,#73208,#73209,#73210,#73211,#73212,
#73213,#73214,#73215,#73216,#73217,#73218,#73219,#73220,#73221,#73222,#73223,
#73224,#73225,#73226,#73227,#73228,#73229,#73230,#73231,#73232,#73233,#73234,
#73235,#73236,#73237,#73238,#73239,#73240,#73241,#73242,#73243,#73244,#73245,
#73246,#73247,#73248,#73249,#73250,#73251,#73252,#73253,#73254,#73255,#73256,
#73257,#73258,#73259,#73260,#73261,#73262,#73263,#73264,#73265,#73266,#73267,
#73268,#73269,#73270,#73271,#73272,#73273,#73274,#73275,#73276,#73277,#73278,
#73279,#73280,#73281,#73282,#73283,#73284,#73285,#73286,#73287,#73288,#73289,
#73290,#73291,#73292,#73293,#73294,#73295,#73296,#73297,#73298,#73299,#73300,
#73301,#73302,#73303,#73304,#73305,#73306,#73307,#73308,#73309,#73310,#73311,
#73312,#73313,#73314,#73315,#73316,#73317,#73318,#73319,#73320,#73321,#73322,
#73323,#73324,#73325,#73326,#73327,#73328,#73329,#73330,#73331,#73332,#73333,
#73334,#73335,#73336,#73337,#73338,#73339,#73340,#73341,#73342,#73343,#73344,
#73345,#73346,#73347,#73348,#73349,#73350,#73351,#73352,#73353,#73354,#73355,
#73356,#73357,#73358,#73359,#73360,#73361,#73362,#73363,#73364,#73365,#73366,
#73367,#73368,#73369,#73370,#73371,#73372,#73373,#73374,#73375,#73376,#73377,
#73378,#73379,#73380,#73381,#73382,#73383,#73384,#73385,#73386,#73387,#73388,
#73389,#73390,#73391,#73392,#73393,#73394,#73395,#73396,#73397,#73398,#73399,
#73400,#73401,#73402,#73403,#73404,#73405,#73406,#73407,#73408,#73409,#73410,
#73411,#73412,#73413,#73414,#73415,#73416,#73417,#73418,#73419,#73420,#73421,
#73422,#73423,#73424,#73425,#73426,#73427,#73428,#73429,#73430,#73431,#73432,
#73433,#73434,#73435,#73436,#73437,#73438,#73439,#73440,#73441,#73442,#73443,
#73444,#73445,#73446,#73447,#73448,#73449,#73450,#73451,#73452),
 .UNSPECIFIED.,.F.,.F.,(4,2,2,2,2,2,2,2,2,2,2,2,2,2,2,2,2,2,2,2,2,2,2,2,
2,2,2,2,2,2,2,2,2,2,2,2,2,2,2,2,2,2,2,2,2,2,2,2,2,2,2,2,2,2,2,2,2,2,2,2,
2,2,2,2,2,2,2,2,2,2,2,2,2,2,2,2,2,2,2,2,2,2,2,2,2,2,2,2,2,2,2,2,2,2,2,2,
2,2,2,2,2,2,2,2,2,2,2,2,2,2,2,2,2,2,2,2,2,2,2,2,2,2,2,2,2,2,2,4),(-2.72811779794129,
-2.72395110668382,-2.67214372911574,-2.66770327696862,-2.66593056720559,
-2.66468478331899,-2.66355240133755,-2.66201398564284,-2.65899323474141,
-2.63265304698429,-2.62727950601053,-2.58612276171778,-2.54256551362552,
-2.522557501376,-2.51010895070006,-2.50633454472439,-2.50396952913755,-2.50178871273713,
-2.49898297806673,-2.49436014269696,-2.46735794526941,-2.45451366521268,
-2.45257996453047,-2.42732072097454,-2.35444894230556,-2.34597271640488,
-2.34370972377173,-2.34235733079876,-2.34114114016076,-2.3395711107769,
-2.33618819295914,-2.30875441231986,-2.22227930203469,-2.2006097493273,
-2.19188462749187,-2.18534205429394,-2.18240550078208,-2.18021194879892,
-2.17816159727414,-2.17478554877441,-2.16622125912555,-2.16412020904491,
-2.08915274747851,-2.03056794345043,-2.02305692286148,-2.02079664516133,
-2.01944485868361,-2.01835037092282,-2.0168193746106,-2.0137214999958,-1.9863704763543,
-1.98179260014154,-1.91866485598044,-1.86807240373345,-1.86216145073006,
-1.85937396663502,-1.85719573536469,-1.85482180445761,-1.85100760403844,
-1.8381945786011,-1.8173935604341,-1.74966121054221,-1.70246644744588,-1.69885221381119,
-1.69723921972435,-1.69601660680437,-1.69468557699312,-1.69251822885215,
-1.6850189049682,-1.62888906401457,-1.55123210913802,-1.5471206336117,-1.54005485758152,
-1.53725177005974,-1.53520665040658,-1.53300968839347,-1.5300528838765,
-1.52339923649665,-1.51448732470994,-1.49216475184124,-1.40120640086452,
-1.39713375453935,-1.37866987777084,-1.37564401409106,-1.37410692220622,
-1.37289736368568,-1.37150925279333,-1.36908611389428,-1.35868416845536,
-1.33867537156219,-1.26448736477213,-1.24604259680287,-1.24474684748415,
-1.22073604873522,-1.21627691660736,-1.21348996404287,-1.21131783025235,
-1.20891971810611,-1.20499748437284,-1.1911423305844,-1.16801659902872,
-1.07231322063664,-1.05557206801261,-1.0528895752296,-1.05129602192942,
-1.05007622009373,-1.04873550241299,-1.04652563350474,-1.03860937833421,
-0.975893656646214,-0.89903356947111,-0.893254984098914,-0.890462776620163,
-0.888289796714404,-0.885894047037265,-0.881983139126685,-0.868243816872639,
-0.845382206504173,-0.755778912812782,-0.749368840161065,-0.732556805166441,
-0.729870738587598,-0.728276089402476,-0.727056060560214,-0.725715748591423,
-0.723507933882403,-0.715781123137751,-0.698279883412001),.UNSPECIFIED.);
#7790=B_SPLINE_CURVE_WITH_KNOTS('',3,(#73458,#73459,#73460,#73461,#73462,
#73463,#73464,#73465,#73466,#73467,#73468,#73469,#73470,#73471,#73472,#73473,
#73474,#73475,#73476,#73477,#73478,#73479,#73480,#73481,#73482,#73483,#73484,
#73485,#73486,#73487,#73488,#73489,#73490,#73491,#73492,#73493,#73494,#73495,
#73496,#73497,#73498,#73499,#73500,#73501,#73502,#73503,#73504,#73505,#73506,
#73507,#73508,#73509,#73510,#73511,#73512,#73513,#73514,#73515,#73516,#73517,
#73518,#73519,#73520,#73521,#73522,#73523,#73524,#73525,#73526,#73527,#73528,
#73529,#73530,#73531,#73532,#73533,#73534,#73535,#73536,#73537,#73538,#73539,
#73540,#73541,#73542,#73543,#73544,#73545,#73546,#73547,#73548,#73549,#73550,
#73551,#73552,#73553,#73554,#73555,#73556,#73557,#73558,#73559,#73560,#73561,
#73562,#73563,#73564,#73565,#73566,#73567,#73568,#73569,#73570,#73571,#73572,
#73573,#73574,#73575,#73576,#73577,#73578,#73579,#73580,#73581,#73582,#73583,
#73584,#73585,#73586,#73587,#73588,#73589,#73590,#73591,#73592,#73593,#73594,
#73595,#73596),.UNSPECIFIED.,.F.,.F.,(4,3,3,3,3,3,3,3,3,3,3,3,3,3,3,3,3,
3,3,3,3,3,3,3,3,3,3,3,3,3,3,3,3,3,3,3,3,3,3,3,3,3,3,3,3,3,4),(172.787595947656,
172.8871626731,172.987119762976,173.087281060253,173.187753394168,173.234730606774,
173.327805915243,173.420755166325,173.513605992654,173.606388998097,173.699136852741,
173.791874379014,173.884626384218,173.97747758313,174.070380601293,174.163438942506,
174.234245745301,174.32732105377,174.420270304851,174.513121131181,174.605904136624,
174.698651991267,174.79138951754,174.884141522745,174.976992721657,175.069895739819,
175.162954081032,175.233760883828,175.326836192297,175.419785443378,175.512636269708,
175.605419275151,175.698167129794,175.790904656067,175.883656661271,175.976507860183,
176.069410878346,176.162469219559,176.233276022354,176.326332345594,176.419271252874,
176.512117763458,176.604896810671,176.697643619617,176.79037247548,176.883129099829,
176.910835117971),.UNSPECIFIED.);
#7791=B_SPLINE_CURVE_WITH_KNOTS('',3,(#73597,#73598,#73599,#73600,#73601,
#73602,#73603,#73604,#73605,#73606,#73607,#73608,#73609,#73610,#73611,#73612,
#73613,#73614,#73615,#73616,#73617,#73618,#73619,#73620,#73621,#73622,#73623,
#73624,#73625,#73626,#73627,#73628,#73629,#73630,#73631,#73632,#73633,#73634,
#73635,#73636,#73637,#73638,#73639,#73640,#73641,#73642,#73643,#73644,#73645,
#73646,#73647,#73648,#73649,#73650,#73651,#73652,#73653,#73654,#73655,#73656,
#73657,#73658,#73659,#73660,#73661,#73662,#73663,#73664,#73665,#73666,#73667,
#73668,#73669),.UNSPECIFIED.,.F.,.F.,(4,3,3,3,3,3,3,3,3,3,3,3,3,3,3,3,3,
3,3,3,3,3,3,3,4),(170.6284544512,170.721197866704,170.813936466662,170.906695057718,
170.999555836272,171.092473388744,171.185540126405,171.235700329721,171.32877563819,
171.421724889271,171.514575715601,171.607358721043,171.700106575687,171.79284410196,
171.885596107164,171.978447306076,172.071350324239,172.164408665452,172.235215468247,
172.331063150332,172.426755440666,172.522271127769,172.617683064162,172.712989713064,
172.787595947439),.UNSPECIFIED.);
#7792=B_SPLINE_CURVE_WITH_KNOTS('',3,(#73671,#73672,#73673,#73674,#73675,
#73676,#73677,#73678,#73679,#73680,#73681,#73682,#73683,#73684,#73685,#73686,
#73687,#73688,#73689,#73690,#73691,#73692,#73693,#73694,#73695,#73696,#73697,
#73698,#73699,#73700,#73701,#73702,#73703,#73704,#73705,#73706,#73707,#73708,
#73709,#73710,#73711,#73712,#73713,#73714,#73715,#73716,#73717,#73718,#73719,
#73720,#73721,#73722,#73723,#73724,#73725,#73726,#73727,#73728,#73729,#73730,
#73731,#73732,#73733,#73734,#73735,#73736,#73737,#73738,#73739,#73740,#73741,
#73742,#73743,#73744,#73745,#73746,#73747,#73748,#73749,#73750,#73751,#73752,
#73753,#73754,#73755,#73756,#73757,#73758),.UNSPECIFIED.,.F.,.F.,(4,2,2,
2,2,2,2,2,2,2,2,2,2,2,2,2,2,2,2,2,2,2,2,2,2,2,2,2,2,2,2,2,2,2,2,2,2,2,2,
2,2,2,2,4),(-0.698279883412001,-0.655716239155022,-0.582384763997299,-0.580089716678059,
-0.571647991594463,-0.568292023643063,-0.566245027112785,-0.564048275461205,
-0.561889775826729,-0.556910973500573,-0.52418670685209,-0.461881483768417,
-0.429319886945314,-0.425595040338129,-0.409551507910414,-0.406903546297833,
-0.405320093762229,-0.404101759828532,-0.402755900656432,-0.400523120639394,
-0.392568704408371,-0.378793281726092,-0.345569525091147,-0.306496731668398,
-0.253420285334502,-0.248068499169068,-0.245323342899425,-0.243292601448471,
-0.241084199689339,-0.238904706007487,-0.235992792150057,-0.22194899313286,
-0.185427869244203,-0.157367425044713,-0.110411449899891,-0.0872156099288681,
-0.0839625211221422,-0.0824004538400775,-0.0811882228664128,-0.0798157059024843,
-0.0774634337029379,-0.0746186557645858,-0.0688073377720556,-0.000960765454798418),
 .UNSPECIFIED.);
#7793=B_SPLINE_CURVE_WITH_KNOTS('',3,(#73759,#73760,#73761,#73762,#73763,
#73764,#73765,#73766,#73767,#73768,#73769,#73770,#73771,#73772,#73773,#73774,
#73775,#73776,#73777,#73778,#73779,#73780,#73781,#73782,#73783,#73784,#73785,
#73786,#73787,#73788,#73789,#73790,#73791,#73792,#73793,#73794,#73795,#73796,
#73797,#73798,#73799,#73800,#73801,#73802,#73803,#73804,#73805,#73806,#73807,
#73808,#73809,#73810,#73811,#73812,#73813,#73814,#73815,#73816,#73817,#73818,
#73819,#73820,#73821,#73822,#73823,#73824,#73825,#73826,#73827,#73828,#73829,
#73830,#73831,#73832,#73833,#73834,#73835,#73836,#73837,#73838,#73839,#73840,
#73841,#73842,#73843,#73844,#73845,#73846,#73847,#73848,#73849,#73850,#73851,
#73852,#73853,#73854,#73855,#73856,#73857,#73858,#73859,#73860,#73861,#73862,
#73863,#73864,#73865,#73866,#73867,#73868,#73869,#73870,#73871,#73872,#73873,
#73874,#73875,#73876,#73877,#73878,#73879,#73880,#73881,#73882,#73883,#73884,
#73885,#73886,#73887,#73888,#73889,#73890,#73891,#73892,#73893,#73894,#73895,
#73896,#73897,#73898,#73899,#73900,#73901,#73902,#73903,#73904,#73905,#73906,
#73907,#73908,#73909,#73910,#73911,#73912,#73913,#73914,#73915,#73916,#73917,
#73918,#73919,#73920),.UNSPECIFIED.,.F.,.F.,(4,2,2,2,2,2,2,2,2,2,2,2,2,
2,2,2,2,2,2,2,2,2,2,2,2,2,2,2,2,2,2,2,2,2,2,2,2,2,2,2,2,2,2,2,2,2,2,2,2,
2,2,2,2,2,2,2,2,2,2,2,2,2,2,2,2,2,2,2,2,2,2,2,2,2,2,2,2,2,2,2,4),(-4.0614106989193,
-3.99228506372147,-3.9876033094368,-3.98469694766783,-3.98251988180079,
-3.98031316472839,-3.97828193046893,-3.97553300655311,-3.97016465951742,
-3.90361299184908,-3.87182005557505,-3.83040509925833,-3.82297583915289,
-3.82077735713258,-3.81943943627122,-3.81821925041248,-3.81662126200902,
-3.8130884750255,-3.75601465138605,-3.71827807558768,-3.683855053423,-3.67179005332648,
-3.66339375805551,-3.6608980041791,-3.65848190585864,-3.65631387026672,
-3.65356015755285,-3.64797400788947,-3.61102704137617,-3.58185610201154,
-3.5087902943652,-3.50054759970581,-3.49817514379088,-3.49678754776283,
-3.49557802092071,-3.49404043260096,-3.49101194429058,-3.47248585425543,
-3.45310768893786,-3.37788492837381,-3.35541179000501,-3.34645631485711,
-3.33982506483717,-3.33684465478391,-3.3346436528514,-3.33260437061923,
-3.32982411963792,-3.32289272752485,-3.31858543406109,-3.24097232964601,
-3.18473761487104,-3.17723174205773,-3.17506364343871,-3.17373240724197,
-3.17250978747459,-3.17089703598277,-3.16728437570639,-3.11928508348387,
-3.05839292779267,-3.03369225449793,-3.01915348230543,-3.01516469340242,
-3.01275174097405,-3.01058280133526,-3.00782284075543,-3.0022062971183,
-2.96431096727881,-2.96194062159995,-2.96100161645296,-2.96004101568985,
-2.88505864429494,-2.86519668185836,-2.85484839930311,-2.85242921512255,
-2.85104194936685,-2.84983222304432,-2.8482937448214,-2.84515920897857,
-2.82506877194222,-2.73229937467288,-2.72904212225825),.UNSPECIFIED.);
#7794=B_SPLINE_CURVE_WITH_KNOTS('',3,(#73926,#73927,#73928,#73929,#73930,
#73931,#73932,#73933,#73934,#73935,#73936,#73937,#73938,#73939,#73940,#73941,
#73942,#73943,#73944,#73945,#73946,#73947,#73948,#73949,#73950,#73951,#73952,
#73953,#73954,#73955,#73956,#73957,#73958,#73959,#73960,#73961,#73962,#73963,
#73964,#73965,#73966,#73967,#73968,#73969,#73970,#73971,#73972,#73973,#73974,
#73975,#73976,#73977,#73978,#73979,#73980,#73981,#73982,#73983,#73984,#73985,
#73986,#73987,#73988,#73989,#73990,#73991,#73992,#73993,#73994,#73995,#73996,
#73997,#73998,#73999,#74000,#74001,#74002,#74003,#74004,#74005,#74006,#74007,
#74008,#74009,#74010,#74011,#74012,#74013,#74014,#74015,#74016,#74017,#74018,
#74019,#74020,#74021,#74022,#74023,#74024,#74025,#74026,#74027,#74028,#74029,
#74030,#74031,#74032,#74033,#74034,#74035,#74036,#74037,#74038,#74039,#74040,
#74041,#74042,#74043,#74044,#74045,#74046,#74047,#74048,#74049,#74050,#74051,
#74052,#74053,#74054,#74055,#74056,#74057,#74058,#74059,#74060,#74061,#74062,
#74063,#74064),.UNSPECIFIED.,.F.,.F.,(4,3,3,3,3,3,3,3,3,3,3,3,3,3,3,3,3,
3,3,3,3,3,3,3,3,3,3,3,3,3,3,3,3,3,3,3,3,3,3,3,3,3,3,3,3,3,4),(179.070781254618,
179.221807303043,179.231821437935,179.324896746404,179.417845997485,179.510696823815,
179.603479829258,179.696227683901,179.788965210175,179.881717215379,179.974568414291,
180.067471432453,180.160529773666,180.231336576461,180.32441188493,180.417361136011,
180.510211962341,180.602994967784,180.695742822427,180.7884803487,180.881232353904,
180.974083552816,181.066986570979,181.160044912192,181.230851714988,181.323927023457,
181.416876274539,181.509727100868,181.602510106311,181.695257960955,181.787995487228,
181.880747492432,181.973598691344,182.066501709507,182.15956005072,182.230366853515,
182.323444406673,182.416395322955,182.513634181647,182.606413472028,182.699157965924,
182.791892484436,182.884641833602,182.97748080292,183.070372307203,183.163394662495,
183.194306192493),.UNSPECIFIED.);
#7795=B_SPLINE_CURVE_WITH_KNOTS('',3,(#74065,#74066,#74067,#74068,#74069,
#74070,#74071,#74072,#74073,#74074,#74075,#74076,#74077,#74078,#74079,#74080,
#74081,#74082,#74083,#74084,#74085,#74086,#74087,#74088,#74089,#74090,#74091,
#74092,#74093,#74094,#74095,#74096,#74097,#74098,#74099,#74100,#74101,#74102,
#74103,#74104,#74105,#74106,#74107,#74108,#74109,#74110,#74111,#74112,#74113,
#74114,#74115,#74116,#74117,#74118,#74119,#74120,#74121,#74122,#74123,#74124,
#74125,#74126,#74127,#74128,#74129,#74130,#74131,#74132,#74133,#74134,#74135,
#74136,#74137,#74138,#74139,#74140),.UNSPECIFIED.,.F.,.F.,(4,3,3,3,3,3,
3,3,3,3,3,3,3,3,3,3,3,3,3,3,3,3,3,3,3,4),(176.910835117971,177.003699424499,
177.09662219951,177.189692119164,177.232791160881,177.32586646935,177.418815720431,
177.511666546761,177.604449552204,177.697197406847,177.789934933121,177.882686938325,
177.975538137237,178.068441155399,178.161499496613,178.232306299408,178.323994332173,
178.417342697453,178.508798385829,178.600197264804,178.69156550965,178.786369445841,
178.877795002929,178.969259727769,179.060827527326,179.070781254415),
 .UNSPECIFIED.);
#7796=B_SPLINE_CURVE_WITH_KNOTS('',3,(#74141,#74142,#74143,#74144,#74145,
#74146,#74147,#74148,#74149,#74150,#74151,#74152,#74153,#74154,#74155,#74156,
#74157,#74158,#74159,#74160,#74161,#74162,#74163,#74164,#74165,#74166,#74167,
#74168,#74169,#74170,#74171,#74172,#74173,#74174,#74175,#74176,#74177,#74178,
#74179,#74180,#74181,#74182,#74183,#74184,#74185,#74186,#74187,#74188,#74189,
#74190,#74191,#74192,#74193,#74194,#74195,#74196,#74197,#74198,#74199,#74200,
#74201,#74202,#74203,#74204,#74205,#74206,#74207,#74208,#74209,#74210,#74211,
#74212,#74213,#74214,#74215,#74216,#74217,#74218,#74219,#74220,#74221,#74222,
#74223,#74224,#74225,#74226,#74227,#74228,#74229,#74230,#74231,#74232,#74233,
#74234,#74235,#74236,#74237,#74238,#74239,#74240,#74241,#74242,#74243,#74244,
#74245,#74246,#74247,#74248,#74249,#74250,#74251,#74252,#74253,#74254,#74255,
#74256,#74257,#74258,#74259,#74260,#74261,#74262,#74263,#74264,#74265,#74266,
#74267,#74268,#74269,#74270,#74271,#74272,#74273,#74274,#74275,#74276,#74277,
#74278,#74279,#74280,#74281,#74282,#74283,#74284,#74285,#74286,#74287,#74288,
#74289,#74290,#74291,#74292,#74293,#74294,#74295,#74296,#74297,#74298,#74299,
#74300,#74301,#74302,#74303,#74304,#74305,#74306,#74307,#74308,#74309,#74310,
#74311,#74312,#74313,#74314,#74315,#74316,#74317,#74318,#74319,#74320,#74321,
#74322,#74323,#74324,#74325,#74326,#74327,#74328,#74329,#74330,#74331,#74332,
#74333,#74334,#74335,#74336,#74337,#74338,#74339,#74340,#74341,#74342,#74343,
#74344,#74345,#74346,#74347,#74348,#74349,#74350,#74351,#74352,#74353,#74354,
#74355,#74356,#74357,#74358,#74359,#74360,#74361,#74362,#74363,#74364,#74365,
#74366,#74367,#74368,#74369,#74370,#74371,#74372,#74373,#74374,#74375,#74376,
#74377,#74378,#74379,#74380,#74381,#74382,#74383,#74384,#74385,#74386,#74387,
#74388,#74389,#74390,#74391,#74392),.UNSPECIFIED.,.F.,.F.,(4,2,2,2,2,2,
2,2,2,2,2,2,2,2,2,2,2,2,2,2,2,2,2,2,2,2,2,2,2,2,2,2,2,2,2,2,2,2,2,2,2,2,
2,2,2,2,2,2,2,2,2,2,2,2,2,2,2,2,2,2,2,2,2,2,2,2,2,2,2,2,2,2,2,2,2,2,2,2,
2,2,2,2,2,2,2,2,2,2,2,2,2,2,2,2,2,2,2,2,2,2,2,2,2,2,2,2,2,2,2,2,2,2,2,2,
2,2,2,2,2,2,2,2,2,2,2,4),(-2.72904212225825,-2.7096651709315,-2.69602545808056,
-2.69212494961878,-2.68973172616695,-2.68755851411208,-2.68476247527617,
-2.67896321621483,-2.60289747541373,-2.55810956252402,-2.54104292983353,
-2.531734842726,-2.52939845241835,-2.52802961859972,-2.52681695116883,-2.52524939679029,
-2.52196743925711,-2.49791946724824,-2.48831897280193,-2.44442462656818,
-2.37821246114565,-2.37121657832867,-2.36819874187792,-2.36599108684224,
-2.36396035244451,-2.36121417440949,-2.35585731864392,-2.28806768611129,
-2.24097684756257,-2.21987855483446,-2.20909205322214,-2.20664071608534,
-2.20524638594833,-2.20403762870615,-2.2025096226319,-2.19952604277416,
-2.18197753713693,-2.1057616669061,-2.05512938201318,-2.04826665240209,
-2.04527229631557,-2.0430688012067,-2.04103272414874,-2.03826530770182,
-2.03140910827594,-1.96482105341071,-1.92029027564777,-1.91226534281901,
-1.88762034289611,-1.88431836815378,-1.88276371444013,-1.88154949997741,
-1.88018835115652,-1.87788636516013,-1.86897814098527,-1.85293841799216,
-1.82864051509322,-1.76889916123524,-1.75624620062414,-1.75442947408398,
-1.72945902116641,-1.72494443156872,-1.72214066848004,-1.71996643204178,
-1.71757709850527,-1.71369419516701,-1.70022795258352,-1.67798121549115,
-1.58749193959003,-1.58071857266496,-1.56420097464093,-1.56152953528697,
-1.55993925426578,-1.55871998778577,-1.55737774395299,-1.5551608703745,
-1.54717265089241,-1.48324292026851,-1.40774467666465,-1.40193223307344,
-1.3991334599275,-1.39695973527136,-1.39456757618578,-1.39067246937472,
-1.37708835451865,-1.35457718661359,-1.26249713958991,-1.24151098694972,
-1.23833977044067,-1.23679385334928,-1.23558327972654,-1.2342005934865,
-1.23180260751651,-1.22173477837889,-1.2026493164265,-1.09681243331176,
-1.09099732815778,-1.08874740821701,-1.08022367300834,-1.07685411898269,
-1.07480477302285,-1.07261004571721,-1.06966802390856,-1.06309704576979,
-1.05432417256677,-1.03248820457026,-0.944742200725109,-0.941821990447943,
-0.918543457617666,-0.91528760267979,-0.913725036381304,-0.912512799338056,
-0.911140692820344,-0.908790086456956,-0.8993135626672,-0.881810415545471,
-0.796462788900646,-0.792002954519274,-0.760893371064953,-0.756081833748309,
-0.753220249612018,-0.751030370257043,-0.748689176677537,-0.74502366105497,
-0.733530766169098,-0.69895630341018),.UNSPECIFIED.);
#7797=B_SPLINE_CURVE_WITH_KNOTS('',3,(#74398,#74399,#74400,#74401,#74402,
#74403,#74404,#74405,#74406,#74407,#74408,#74409,#74410,#74411,#74412,#74413,
#74414,#74415,#74416,#74417,#74418,#74419,#74420,#74421,#74422,#74423,#74424,
#74425,#74426,#74427,#74428,#74429,#74430,#74431,#74432,#74433,#74434,#74435,
#74436,#74437,#74438,#74439,#74440,#74441,#74442,#74443,#74444,#74445,#74446,
#74447,#74448,#74449,#74450,#74451,#74452,#74453,#74454,#74455,#74456,#74457,
#74458,#74459,#74460,#74461,#74462,#74463,#74464,#74465,#74466,#74467,#74468,
#74469,#74470,#74471,#74472,#74473,#74474,#74475,#74476,#74477,#74478,#74479,
#74480,#74481,#74482,#74483,#74484,#74485,#74486,#74487,#74488,#74489,#74490,
#74491,#74492,#74493,#74494,#74495,#74496,#74497,#74498,#74499,#74500,#74501,
#74502,#74503,#74504,#74505,#74506,#74507,#74508,#74509,#74510,#74511,#74512,
#74513,#74514,#74515,#74516,#74517,#74518,#74519,#74520,#74521,#74522,#74523,
#74524,#74525,#74526,#74527,#74528,#74529,#74530,#74531,#74532,#74533,#74534,
#74535,#74536),.UNSPECIFIED.,.F.,.F.,(4,3,3,3,3,3,3,3,3,3,3,3,3,3,3,3,3,
3,3,3,3,3,3,3,3,3,3,3,3,3,3,3,3,3,3,3,3,3,3,3,3,3,3,3,3,3,4),(185.35396656206,
185.445661763843,185.537250107984,185.62876102844,185.720231746724,185.81168834625,
185.903156891666,185.994719296751,186.086333618337,186.178093488036,186.228427407622,
186.321502716091,186.414451967172,186.507302793502,186.600085798945,186.692833653589,
186.785571179862,186.878323185066,186.971174383978,187.064077402141,187.157135743354,
187.227942546149,187.321017854618,187.413967105699,187.506817932029,187.599600937472,
187.692348792115,187.785086318389,187.877838323593,187.970689522505,188.063592540667,
188.156650881881,188.227457684676,188.320532993145,188.413482244226,188.506333070556,
188.599116075998,188.691863930642,188.784601456915,188.877353462119,188.970204661031,
189.063107679194,189.156166020407,189.226972823202,189.320047778457,189.412983705485,
189.478274198416),.UNSPECIFIED.);
#7798=B_SPLINE_CURVE_WITH_KNOTS('',3,(#74537,#74538,#74539,#74540,#74541,
#74542,#74543,#74544,#74545,#74546,#74547,#74548,#74549,#74550,#74551,#74552,
#74553,#74554,#74555,#74556,#74557,#74558,#74559,#74560,#74561,#74562,#74563,
#74564,#74565,#74566,#74567,#74568,#74569,#74570,#74571,#74572,#74573,#74574,
#74575,#74576,#74577,#74578,#74579,#74580,#74581,#74582,#74583,#74584,#74585,
#74586,#74587,#74588,#74589,#74590,#74591,#74592,#74593,#74594,#74595,#74596,
#74597,#74598,#74599,#74600,#74601,#74602,#74603,#74604,#74605,#74606,#74607,
#74608,#74609),.UNSPECIFIED.,.F.,.F.,(4,3,3,3,3,3,3,3,3,3,3,3,3,3,3,3,3,
3,3,3,3,3,3,3,4),(183.194306192493,183.229881992042,183.322957300511,183.415906551592,
183.508757377922,183.601540383365,183.694288238008,183.787025764281,183.879777769486,
183.972628968398,184.06553198656,184.158590327773,184.229397130569,184.322472439038,
184.41542169012,184.508272516449,184.601055521892,184.693803376535,184.786540902809,
184.879292908013,184.972144106925,185.065047125087,185.158105466301,185.228912269095,
185.353966561798),.UNSPECIFIED.);
#7799=B_SPLINE_CURVE_WITH_KNOTS('',3,(#74611,#74612,#74613,#74614,#74615,
#74616,#74617,#74618,#74619,#74620,#74621,#74622,#74623,#74624,#74625,#74626,
#74627,#74628,#74629,#74630,#74631,#74632,#74633,#74634,#74635,#74636,#74637,
#74638,#74639,#74640,#74641,#74642,#74643,#74644,#74645,#74646,#74647,#74648,
#74649,#74650,#74651,#74652,#74653,#74654,#74655,#74656,#74657,#74658,#74659,
#74660,#74661,#74662,#74663,#74664,#74665,#74666,#74667,#74668,#74669,#74670,
#74671,#74672,#74673,#74674,#74675,#74676,#74677,#74678,#74679,#74680,#74681,
#74682,#74683,#74684,#74685,#74686,#74687,#74688),.UNSPECIFIED.,.F.,.F.,
(4,2,2,2,2,2,2,2,2,2,2,2,2,2,2,2,2,2,2,2,2,2,2,2,2,2,2,2,2,2,2,2,2,2,2,
2,2,2,4),(-0.69895630341018,-0.653222363512318,-0.595973469885204,-0.592443956624196,
-0.590846319211679,-0.589625926629394,-0.588495068878159,-0.586538692516284,
-0.580868418552731,-0.547466923850817,-0.495683828749448,-0.438965088257273,
-0.433579876649729,-0.430826256283266,-0.428793471788008,-0.426586925954228,
-0.423576601641367,-0.416624914529298,-0.4072087442495,-0.383095294269286,
-0.313154443422782,-0.273184331142939,-0.269947121986367,-0.268354061644838,
-0.267207245452141,-0.26597284971414,-0.264745458556692,-0.261806726216356,
-0.238946538780567,-0.203054838158422,-0.121755971280362,-0.111837607330222,
-0.108250977057591,-0.106159380370009,-0.103984232393372,-0.101175423469589,
-0.095312231075147,-0.0242159529617381,-0.000961145727620849),
 .UNSPECIFIED.);
#7800=B_SPLINE_CURVE_WITH_KNOTS('',3,(#74689,#74690,#74691,#74692,#74693,
#74694,#74695,#74696,#74697,#74698,#74699,#74700,#74701,#74702,#74703,#74704,
#74705,#74706,#74707,#74708,#74709,#74710,#74711,#74712,#74713,#74714,#74715,
#74716,#74717,#74718,#74719,#74720,#74721,#74722,#74723,#74724,#74725,#74726,
#74727,#74728,#74729,#74730,#74731,#74732,#74733,#74734,#74735,#74736,#74737,
#74738,#74739,#74740,#74741,#74742,#74743,#74744,#74745,#74746,#74747,#74748,
#74749,#74750,#74751,#74752,#74753,#74754,#74755,#74756,#74757,#74758,#74759,
#74760,#74761,#74762,#74763,#74764,#74765,#74766,#74767,#74768,#74769,#74770,
#74771,#74772,#74773,#74774,#74775,#74776,#74777,#74778,#74779,#74780,#74781,
#74782,#74783,#74784,#74785,#74786,#74787,#74788,#74789,#74790,#74791,#74792,
#74793,#74794,#74795,#74796,#74797,#74798,#74799,#74800,#74801,#74802,#74803,
#74804,#74805,#74806,#74807,#74808,#74809,#74810,#74811,#74812,#74813,#74814,
#74815,#74816,#74817,#74818,#74819,#74820,#74821,#74822,#74823,#74824,#74825,
#74826,#74827,#74828,#74829,#74830,#74831,#74832,#74833,#74834,#74835,#74836,
#74837,#74838,#74839,#74840,#74841,#74842,#74843,#74844,#74845,#74846,#74847,
#74848,#74849,#74850,#74851,#74852,#74853,#74854),.UNSPECIFIED.,.F.,.F.,
(4,2,2,2,2,2,2,2,2,2,2,2,2,2,2,2,2,2,2,2,2,2,2,2,2,2,2,2,2,2,2,2,2,2,2,
2,2,2,2,2,2,2,2,2,2,2,2,2,2,2,2,2,2,2,2,2,2,2,2,2,2,2,2,2,2,2,2,2,2,2,2,
2,2,2,2,2,2,2,2,2,2,2,4),(-4.06105614040862,-4.01281509053043,-4.00918237775696,
-4.00715091961412,-4.00577429085302,-4.00444297002081,-4.00322015272408,
-4.00160697777479,-3.99799269723706,-3.95063061388278,-3.93289700077417,
-3.91725583559134,-3.87962863295169,-3.85473739475367,-3.84775867645504,
-3.84474353435691,-3.8425360666918,-3.84050425667464,-3.83775472853369,
-3.83238572033902,-3.77765707346459,-3.74665168036196,-3.70336625740058,
-3.69195226863712,-3.68502734002993,-3.68292407769409,-3.68178582067001,
-3.6805762200488,-3.67904032207358,-3.67602061250708,-3.65769797190969,
-3.65326931918034,-3.63978204584763,-3.56391094538317,-3.52917299141871,
-3.52394190915962,-3.52126000404874,-3.5191181986428,-3.51666235107179,
-3.5124817117955,-3.50379872002775,-3.42153333535804,-3.38535990467376,
-3.37068115605294,-3.36513834285786,-3.36238930390365,-3.36012995751842,
-3.35878476540911,-3.35757256118003,-3.3560108768971,-3.35275979510313,
-3.32962131565407,-3.32150112954287,-3.23813619279374,-3.21678114772272,
-3.20371386731093,-3.19987208624882,-3.19749169098694,-3.19531468560247,
-3.19253857351094,-3.18668871495556,-3.11265819380833,-3.06637870434854,
-3.04897584105275,-3.03953839183453,-3.03719095473982,-3.03581952563101,
-3.03460711186989,-3.03304329301138,-3.02978120372506,-3.00632433996406,
-2.99841654155468,-2.95776715607303,-2.88427405163893,-2.87840260427826,
-2.87559216264935,-2.87341677426765,-2.87132572876852,-2.8677420163138,
-2.85784365320879,-2.77609765754925,-2.73947398900245,-2.72901306494186),
 .UNSPECIFIED.);
#7801=B_SPLINE_CURVE_WITH_KNOTS('',3,(#74860,#74861,#74862,#74863,#74864,
#74865,#74866,#74867,#74868,#74869,#74870,#74871,#74872,#74873,#74874,#74875,
#74876,#74877,#74878,#74879,#74880,#74881,#74882,#74883,#74884,#74885,#74886,
#74887,#74888,#74889,#74890,#74891,#74892,#74893,#74894,#74895,#74896,#74897,
#74898,#74899,#74900,#74901,#74902,#74903,#74904,#74905,#74906,#74907,#74908,
#74909,#74910,#74911,#74912,#74913,#74914,#74915,#74916,#74917,#74918,#74919,
#74920,#74921,#74922,#74923,#74924,#74925,#74926,#74927,#74928,#74929,#74930,
#74931,#74932,#74933,#74934,#74935,#74936,#74937,#74938,#74939,#74940,#74941,
#74942,#74943,#74944,#74945,#74946,#74947,#74948,#74949,#74950,#74951,#74952,
#74953,#74954,#74955,#74956,#74957,#74958,#74959,#74960,#74961,#74962,#74963,
#74964,#74965,#74966,#74967,#74968,#74969,#74970,#74971,#74972,#74973,#74974,
#74975,#74976,#74977,#74978,#74979,#74980,#74981,#74982,#74983,#74984,#74985,
#74986,#74987,#74988,#74989,#74990,#74991,#74992,#74993,#74994,#74995,#74996,
#74997,#74998),.UNSPECIFIED.,.F.,.F.,(4,3,3,3,3,3,3,3,3,3,3,3,3,3,3,3,3,
3,3,3,3,3,3,3,3,3,3,3,3,3,3,3,3,3,3,3,3,3,3,3,3,3,3,3,3,3,4),(191.637151868978,
191.731423354596,191.825732704026,191.920101744143,192.014616768741,192.109217785349,
192.203986010753,192.225518238783,192.318593547252,192.411542798333,192.504393624663,
192.597176630106,192.689924484749,192.782662011022,192.875414016227,192.968265215139,
193.061168233301,193.154226574514,193.225033377309,193.318108685778,193.41105793686,
193.503908763189,193.596691768632,193.689439623275,193.782177149549,193.874929154753,
193.967780353665,194.060683371827,194.15374171304,194.224548515836,194.317623824305,
194.410573075386,194.503423901716,194.596206907159,194.688954761803,194.781692288076,
194.87444429328,194.967295492192,195.060198510355,195.153256851568,195.224063654363,
195.317134501935,195.410084650361,195.502926540283,195.595704635939,195.688454781277,
195.760761063421),.UNSPECIFIED.);
#7802=B_SPLINE_CURVE_WITH_KNOTS('',3,(#74999,#75000,#75001,#75002,#75003,
#75004,#75005,#75006,#75007,#75008,#75009,#75010,#75011,#75012,#75013,#75014,
#75015,#75016,#75017,#75018,#75019,#75020,#75021,#75022,#75023,#75024,#75025,
#75026,#75027,#75028,#75029,#75030,#75031,#75032,#75033,#75034,#75035,#75036,
#75037,#75038,#75039,#75040,#75041,#75042,#75043,#75044,#75045,#75046,#75047,
#75048,#75049,#75050,#75051,#75052,#75053,#75054,#75055,#75056,#75057,#75058,
#75059,#75060,#75061,#75062,#75063,#75064,#75065,#75066,#75067,#75068),
 .UNSPECIFIED.,.F.,.F.,(4,3,3,3,3,3,3,3,3,3,3,3,3,3,3,3,3,3,3,3,3,3,3,4),
(189.478274198416,189.57180091883,189.664556387319,189.757294350647,189.850039618445,
189.944151704266,190.037038229662,190.131763095696,190.226487961729,190.319563270198,
190.41251252128,190.505363347609,190.598146353052,190.690894207695,190.783631733968,
190.876383739173,190.969234938085,191.062137956247,191.155196297461,191.226003100256,
191.328790292394,191.431140646895,191.534146257852,191.63715186881),
 .UNSPECIFIED.);
#7803=B_SPLINE_CURVE_WITH_KNOTS('',3,(#75069,#75070,#75071,#75072,#75073,
#75074,#75075,#75076,#75077,#75078,#75079,#75080,#75081,#75082,#75083,#75084,
#75085,#75086,#75087,#75088,#75089,#75090,#75091,#75092,#75093,#75094,#75095,
#75096,#75097,#75098,#75099,#75100,#75101,#75102,#75103,#75104,#75105,#75106,
#75107,#75108,#75109,#75110,#75111,#75112,#75113,#75114,#75115,#75116,#75117,
#75118,#75119,#75120,#75121,#75122,#75123,#75124,#75125,#75126,#75127,#75128,
#75129,#75130,#75131,#75132,#75133,#75134,#75135,#75136,#75137,#75138,#75139,
#75140,#75141,#75142,#75143,#75144,#75145,#75146,#75147,#75148,#75149,#75150,
#75151,#75152,#75153,#75154,#75155,#75156,#75157,#75158,#75159,#75160,#75161,
#75162,#75163,#75164,#75165,#75166,#75167,#75168,#75169,#75170,#75171,#75172,
#75173,#75174,#75175,#75176,#75177,#75178,#75179,#75180,#75181,#75182,#75183,
#75184,#75185,#75186,#75187,#75188,#75189,#75190,#75191,#75192,#75193,#75194,
#75195,#75196,#75197,#75198,#75199,#75200,#75201,#75202,#75203,#75204,#75205,
#75206,#75207,#75208,#75209,#75210,#75211,#75212,#75213,#75214,#75215,#75216,
#75217,#75218,#75219,#75220,#75221,#75222,#75223,#75224,#75225,#75226,#75227,
#75228,#75229,#75230,#75231,#75232,#75233,#75234,#75235,#75236,#75237,#75238,
#75239,#75240,#75241,#75242,#75243,#75244,#75245,#75246,#75247,#75248,#75249,
#75250,#75251,#75252,#75253,#75254,#75255,#75256,#75257,#75258,#75259,#75260,
#75261,#75262,#75263,#75264,#75265,#75266,#75267,#75268,#75269,#75270,#75271,
#75272,#75273,#75274,#75275,#75276,#75277,#75278,#75279,#75280,#75281,#75282,
#75283,#75284,#75285,#75286,#75287,#75288,#75289,#75290,#75291,#75292,#75293,
#75294,#75295,#75296,#75297,#75298,#75299,#75300,#75301,#75302,#75303,#75304,
#75305,#75306,#75307,#75308,#75309,#75310,#75311,#75312,#75313,#75314),
 .UNSPECIFIED.,.F.,.F.,(4,2,2,2,2,2,2,2,2,2,2,2,2,2,2,2,2,2,2,2,2,2,2,2,
2,2,2,2,2,2,2,2,2,2,2,2,2,2,2,2,2,2,2,2,2,2,2,2,2,2,2,2,2,2,2,2,2,2,2,2,
2,2,2,2,2,2,2,2,2,2,2,2,2,2,2,2,2,2,2,2,2,2,2,2,2,2,2,2,2,2,2,2,2,2,2,2,
2,2,2,2,2,2,2,2,2,2,2,2,2,2,2,2,2,2,2,2,2,2,2,2,2,2,4),(-2.72901306494186,
-2.72477364011638,-2.71640486488902,-2.71415145026102,-2.71280096346963,
-2.71158385092473,-2.71000915187469,-2.70739100514283,-2.69193033226944,
-2.68750566272187,-2.63576830998419,-2.56158533791962,-2.55552669117122,
-2.55268006862981,-2.55049970367852,-2.54842130129309,-2.54490219628208,
-2.53544222733974,-2.44749595013701,-2.41838914949135,-2.40238529547798,
-2.39349142334825,-2.39119028661007,-2.38982910201483,-2.38861448840587,
-2.38705885655547,-2.38375306194745,-2.35901108167993,-2.28438538781544,
-2.23833748639376,-2.23243698840548,-2.22962077866105,-2.22744450301178,
-2.22535534409205,-2.2217817092066,-2.21195290468737,-2.12895815915762,
-2.0931354471405,-2.07866495134814,-2.07039051731158,-2.06814586635709,
-2.06679727495931,-2.06557954094937,-2.06400095361309,-2.06057440453013,
-2.03141688303343,-1.95842185949297,-1.94007620069372,-1.91404559796006,
-1.90947252280475,-1.90668100432502,-1.90450158603502,-1.90212834963577,
-1.8983196141261,-1.8855650713607,-1.86489414908399,-1.81657315048713,-1.78022925891761,
-1.77208955338483,-1.76500916385351,-1.74873667024826,-1.74607715321061,
-1.74449027015011,-1.74327138853623,-1.74192717813143,-1.73970195716114,
-1.73162975110238,-1.66626549521913,-1.59234549952807,-1.58649397242468,
-1.58368735969116,-1.58151241079025,-1.57912380012112,-1.5752454417142,
-1.56182810048295,-1.53969243827198,-1.44991094673835,-1.42619877569986,
-1.42292752427725,-1.4213617844141,-1.42014901582044,-1.41877841679308,
-1.41643524069789,-1.40705154140513,-1.38979259026638,-1.34404220538955,
-1.26929918769843,-1.263462838317,-1.26068910544669,-1.25851218652711,-1.25613006982783,
-1.2522814915,-1.23915287902074,-1.21766047132007,-1.13287256271414,-1.10343549751271,
-1.10000222809799,-1.09842229768116,-1.09720429179256,-1.09585621698809,
-1.09361420501081,-1.08536886914662,-1.07097113259015,-1.03541541954631,
-0.952066357763789,-0.949787545788717,-0.941671350205491,-0.938369985271233,
-0.93633306752268,-0.934128994280459,-0.931134448914878,-0.92427390750016,
-0.876439924359826,-0.821000778995854,-0.780688685812408,-0.777451952840973,
-0.775858898687265,-0.774711981768323,-0.773477367847489,-0.771766465900398,
-0.767701893927945,-0.762050299029744,-0.69862383258841),.UNSPECIFIED.);
#7804=B_SPLINE_CURVE_WITH_KNOTS('',3,(#75320,#75321,#75322,#75323,#75324,
#75325,#75326,#75327,#75328,#75329,#75330,#75331,#75332,#75333,#75334,#75335,
#75336,#75337,#75338,#75339,#75340,#75341,#75342,#75343,#75344,#75345,#75346,
#75347,#75348,#75349,#75350,#75351,#75352,#75353,#75354,#75355,#75356,#75357,
#75358,#75359,#75360,#75361,#75362,#75363,#75364,#75365,#75366,#75367,#75368,
#75369,#75370,#75371,#75372,#75373,#75374,#75375,#75376,#75377,#75378,#75379,
#75380,#75381,#75382,#75383,#75384,#75385,#75386,#75387,#75388,#75389,#75390,
#75391,#75392,#75393,#75394,#75395,#75396,#75397,#75398,#75399,#75400,#75401,
#75402,#75403,#75404,#75405,#75406,#75407,#75408,#75409,#75410,#75411,#75412,
#75413,#75414,#75415,#75416,#75417,#75418,#75419,#75420,#75421,#75422,#75423,
#75424,#75425,#75426,#75427,#75428,#75429,#75430,#75431,#75432,#75433,#75434,
#75435,#75436,#75437,#75438,#75439,#75440,#75441,#75442,#75443,#75444,#75445,
#75446,#75447,#75448,#75449,#75450,#75451,#75452,#75453,#75454,#75455),
 .UNSPECIFIED.,.F.,.F.,(4,3,3,3,3,3,3,3,3,3,3,3,3,3,3,3,3,3,3,3,3,3,3,3,
3,3,3,3,3,3,3,3,3,3,3,3,3,3,3,3,3,3,3,3,3,4),(197.920337176455,198.031805350229,
198.144766608287,198.222609069943,198.315684378412,198.408633629494,198.501484455823,
198.594267461266,198.687015315909,198.779752842183,198.872504847387,198.965356046299,
199.058259064462,199.151317405675,199.22212420847,199.315199516939,199.40814876802,
199.50099959435,199.593782599793,199.686530454436,199.779267980709,199.872019985914,
199.964871184826,200.057774202988,200.150832544201,200.221639346997,200.314714655466,
200.407663906547,200.500514732877,200.59329773832,200.686045592963,200.778783119236,
200.87153512444,200.964386323352,201.057289341515,201.150347682728,201.221154485523,
201.314241596727,201.407173008952,201.500015390413,201.592793663975,201.685532692314,
201.7782898269,201.871052592644,201.963901834055,202.043473694958),
 .UNSPECIFIED.);
#7805=B_SPLINE_CURVE_WITH_KNOTS('',3,(#75456,#75457,#75458,#75459,#75460,
#75461,#75462,#75463,#75464,#75465,#75466,#75467,#75468,#75469,#75470,#75471,
#75472,#75473,#75474,#75475,#75476,#75477,#75478,#75479,#75480,#75481,#75482,
#75483,#75484,#75485,#75486,#75487,#75488,#75489,#75490,#75491,#75492,#75493,
#75494,#75495,#75496,#75497,#75498,#75499,#75500,#75501,#75502,#75503,#75504,
#75505,#75506,#75507,#75508,#75509,#75510,#75511,#75512,#75513,#75514,#75515,
#75516,#75517,#75518,#75519,#75520,#75521,#75522,#75523,#75524,#75525,#75526,
#75527,#75528),.UNSPECIFIED.,.F.,.F.,(4,3,3,3,3,3,3,3,3,3,3,3,3,3,3,3,3,
3,3,3,3,3,3,3,4),(195.760761063421,195.85350774476,195.946350525372,196.039240210634,
196.132291560014,196.22357879289,196.316654101359,196.40960335244,196.502454178769,
196.595237184212,196.687985038856,196.780722565129,196.873474570333,196.966325769245,
197.059228787407,197.15228712862,197.223093931416,197.315631945497,197.408051216362,
197.500377312576,197.592635711061,197.684865852227,197.777078489631,197.86932941234,
197.920337176157),.UNSPECIFIED.);
#7806=B_SPLINE_CURVE_WITH_KNOTS('',3,(#75530,#75531,#75532,#75533,#75534,
#75535,#75536,#75537,#75538,#75539,#75540,#75541,#75542,#75543,#75544,#75545,
#75546,#75547,#75548,#75549,#75550,#75551,#75552,#75553,#75554,#75555,#75556,
#75557,#75558,#75559,#75560,#75561,#75562,#75563,#75564,#75565,#75566,#75567,
#75568,#75569,#75570,#75571,#75572,#75573,#75574,#75575,#75576,#75577,#75578,
#75579,#75580,#75581,#75582,#75583,#75584,#75585,#75586,#75587,#75588,#75589,
#75590,#75591,#75592,#75593,#75594,#75595,#75596,#75597,#75598,#75599,#75600,
#75601,#75602,#75603,#75604,#75605,#75606,#75607,#75608,#75609,#75610,#75611,
#75612,#75613,#75614,#75615,#75616,#75617,#75618,#75619,#75620,#75621,#75622,
#75623,#75624,#75625,#75626,#75627,#75628,#75629,#75630,#75631,#75632,#75633,
#75634,#75635,#75636,#75637,#75638,#75639,#75640,#75641,#75642,#75643,#75644,
#75645,#75646,#75647,#75648,#75649,#75650,#75651,#75652,#75653,#75654,#75655,
#75656,#75657,#75658,#75659,#75660,#75661),.UNSPECIFIED.,.F.,.F.,(4,2,2,
2,2,2,2,2,2,2,2,2,2,2,2,2,2,2,2,2,2,2,2,2,2,2,2,2,2,2,2,2,2,2,2,2,2,2,2,
2,2,2,2,2,2,2,2,2,2,2,2,2,2,2,2,2,2,2,2,2,2,2,2,2,2,4),(-0.69862383258841,
-0.688206000384788,-0.623497102447362,-0.618109859171754,-0.61535552328661,
-0.613322367576281,-0.611159681285807,-0.608261189507177,-0.605021558347607,
-0.599535663912179,-0.561528443492525,-0.491622262480999,-0.481349664126729,
-0.457224093883082,-0.453938725562586,-0.452370224694936,-0.45115713940628,
-0.449788168472257,-0.447452320511715,-0.438156169058778,-0.421125009291424,
-0.371411706140605,-0.300422273982887,-0.294512655811967,-0.291724827940602,
-0.289545903590539,-0.2895211130373,-0.289497431938669,-0.289474802519147,
-0.28945317053688,-0.289432485096465,-0.289412698379625,-0.289393765449707,
-0.289375644026989,-0.289358294325546,-0.28934167885546,-0.289325762273646,
-0.289310511248986,-0.289295894329481,-0.289281881787081,-0.289268445533295,
-0.289255559022813,-0.289243197126645,-0.289231336030225,-0.289217823197679,
-0.289204437977887,-0.289191176814999,-0.289178037708408,-0.289165018682222,
-0.289152117811758,-0.286696323519249,-0.282464003546999,-0.277310946950807,
-0.266822157181432,-0.238722877026035,-0.173853007258257,-0.154236015493879,
-0.134054366045775,-0.130915486417587,-0.129375926588919,-0.128165853573525,
-0.126778746031436,-0.124361179437544,-0.114039305183661,-0.0942556630349844,
-0.000961385530181774),.UNSPECIFIED.);
#7807=B_SPLINE_CURVE_WITH_KNOTS('',3,(#75662,#75663,#75664,#75665,#75666,
#75667,#75668,#75669,#75670,#75671,#75672,#75673,#75674,#75675,#75676,#75677,
#75678,#75679,#75680,#75681,#75682,#75683,#75684,#75685,#75686,#75687,#75688,
#75689,#75690,#75691,#75692,#75693,#75694,#75695,#75696,#75697,#75698,#75699,
#75700,#75701,#75702,#75703,#75704,#75705,#75706,#75707,#75708,#75709,#75710,
#75711,#75712,#75713,#75714,#75715,#75716,#75717,#75718,#75719,#75720,#75721,
#75722,#75723,#75724,#75725,#75726,#75727,#75728,#75729,#75730,#75731,#75732,
#75733,#75734,#75735,#75736,#75737,#75738,#75739,#75740,#75741,#75742,#75743,
#75744,#75745,#75746,#75747,#75748,#75749,#75750,#75751,#75752,#75753,#75754,
#75755,#75756,#75757,#75758,#75759,#75760,#75761,#75762,#75763,#75764,#75765,
#75766,#75767,#75768,#75769,#75770,#75771,#75772,#75773,#75774,#75775,#75776,
#75777,#75778,#75779,#75780,#75781,#75782,#75783,#75784,#75785,#75786,#75787,
#75788,#75789,#75790,#75791,#75792,#75793,#75794,#75795,#75796,#75797,#75798,
#75799,#75800),.UNSPECIFIED.,.F.,.F.,(4,3,3,3,3,3,3,3,3,3,3,3,3,3,3,3,3,
3,3,3,3,3,3,3,3,3,3,3,3,3,3,3,3,3,3,3,3,3,3,3,3,3,3,3,3,3,4),(197.920337176157,
198.014222382866,198.108132654103,198.202090688791,198.296184290483,198.390354989505,
198.484693712474,198.52454513226,198.617620440729,198.710569691811,198.80342051814,
198.896203523583,198.988951378226,199.0816889045,199.174440909704,199.267292108616,
199.360195126778,199.453253467992,199.524060270786,199.617135579255,199.710084830336,
199.802935656666,199.895718662109,199.988466516752,200.081204043025,200.173956048229,
200.266807247141,200.359710265304,200.452768606517,200.523575409313,200.616650717782,
200.709599968864,200.802450795193,200.895233800636,200.98798165528,201.080719181553,
201.173471186757,201.266322385669,201.359225403832,201.452283745045,201.52309054784,
201.616163269426,201.709114923502,201.801956943226,201.894735022355,201.987480895189,
202.043995148801),.UNSPECIFIED.);
#7808=B_SPLINE_CURVE_WITH_KNOTS('',3,(#75806,#75807,#75808,#75809,#75810,
#75811,#75812,#75813,#75814,#75815,#75816,#75817,#75818,#75819,#75820,#75821,
#75822,#75823,#75824,#75825,#75826,#75827,#75828,#75829,#75830,#75831,#75832,
#75833,#75834,#75835,#75836,#75837,#75838,#75839,#75840,#75841,#75842,#75843,
#75844,#75845,#75846,#75847,#75848,#75849,#75850,#75851,#75852,#75853,#75854,
#75855,#75856,#75857,#75858,#75859,#75860,#75861,#75862,#75863,#75864,#75865,
#75866,#75867,#75868,#75869,#75870,#75871,#75872,#75873,#75874,#75875,#75876,
#75877,#75878,#75879,#75880,#75881,#75882,#75883,#75884,#75885,#75886,#75887,
#75888,#75889,#75890,#75891,#75892,#75893,#75894,#75895,#75896,#75897,#75898,
#75899,#75900,#75901,#75902,#75903,#75904,#75905,#75906,#75907,#75908,#75909,
#75910,#75911,#75912,#75913,#75914,#75915,#75916,#75917,#75918,#75919,#75920,
#75921,#75922,#75923,#75924,#75925,#75926,#75927,#75928,#75929,#75930,#75931,
#75932,#75933,#75934,#75935,#75936,#75937,#75938,#75939,#75940,#75941,#75942,
#75943,#75944,#75945,#75946,#75947),.UNSPECIFIED.,.F.,.F.,(4,3,3,3,3,3,
3,3,3,3,3,3,3,3,3,3,3,3,3,3,3,3,3,3,3,3,3,3,3,3,3,3,3,3,3,3,3,3,3,3,3,3,
3,3,3,3,3,4),(204.203522483337,204.219699901104,204.312775209573,204.405724460654,
204.498575286984,204.591358292427,204.68410614707,204.776843673343,204.869595678547,
204.962446877459,205.055349895621,205.148408236835,205.219215039631,205.3122903481,
205.405239599181,205.498090425511,205.590873430954,205.683621285597,205.77635881187,
205.869110817074,205.961962015986,206.054865034149,206.147923375362,206.218730178157,
206.311805486626,206.404754737707,206.497605564037,206.59038856948,206.683136424123,
206.775873950396,206.8686259556,206.961477154512,207.054380172675,207.147438513888,
207.218245316684,207.311320625153,207.404269876235,207.497120702564,207.589903708007,
207.682651562651,207.775389088924,207.868141094128,207.96099229304,208.053895311203,
208.146953652416,208.217760455211,208.310843573954,208.327722804751),
 .UNSPECIFIED.);
#7809=B_SPLINE_CURVE_WITH_KNOTS('',3,(#75948,#75949,#75950,#75951,#75952,
#75953,#75954,#75955,#75956,#75957,#75958,#75959,#75960,#75961,#75962,#75963,
#75964,#75965,#75966,#75967,#75968,#75969,#75970,#75971,#75972,#75973,#75974,
#75975,#75976,#75977,#75978,#75979,#75980,#75981,#75982,#75983,#75984,#75985,
#75986,#75987,#75988,#75989,#75990,#75991,#75992,#75993,#75994,#75995,#75996,
#75997,#75998,#75999,#76000,#76001,#76002,#76003,#76004,#76005,#76006,#76007,
#76008,#76009,#76010,#76011,#76012,#76013,#76014,#76015,#76016,#76017,#76018,
#76019,#76020),.UNSPECIFIED.,.F.,.F.,(4,3,3,3,3,3,3,3,3,3,3,3,3,3,3,3,3,
3,3,3,3,3,3,3,4),(202.043473694958,202.136527332252,202.22066962405,202.313744932519,
202.406694183601,202.49954500993,202.592328015373,202.685075870017,202.77781339629,
202.870565401494,202.963416600406,203.056319618569,203.149377959782,203.220184762577,
203.313000399415,203.405690164659,203.498282027013,203.590807109206,203.683298119373,
203.775780178135,203.868278392127,203.960875689901,204.053526894021,204.146328371649,
204.203522483032),.UNSPECIFIED.);
#7810=B_SPLINE_CURVE_WITH_KNOTS('',3,(#76022,#76023,#76024,#76025,#76026,
#76027,#76028,#76029,#76030,#76031,#76032,#76033,#76034,#76035,#76036,#76037,
#76038,#76039,#76040,#76041,#76042,#76043,#76044,#76045,#76046,#76047,#76048,
#76049,#76050,#76051,#76052,#76053,#76054,#76055,#76056,#76057,#76058,#76059,
#76060,#76061,#76062,#76063,#76064,#76065,#76066,#76067,#76068,#76069,#76070,
#76071,#76072,#76073,#76074,#76075,#76076,#76077,#76078,#76079,#76080,#76081,
#76082,#76083,#76084,#76085,#76086,#76087,#76088,#76089,#76090,#76091,#76092,
#76093,#76094,#76095,#76096,#76097),.UNSPECIFIED.,.F.,.F.,(4,3,3,3,3,3,
3,3,3,3,3,3,3,3,3,3,3,3,3,3,3,3,3,3,3,4),(202.043995148801,202.136738543329,
202.233205329089,202.326087595671,202.419036158692,202.512122828016,202.522605686367,
202.615680994836,202.708630245918,202.801481072247,202.89426407769,202.987011932334,
203.079749458607,203.172501463811,203.265352662723,203.358255680885,203.451314022099,
203.522120824893,203.614889200762,203.707536779099,203.800088879478,203.892570730299,
203.985017664774,204.077444682146,204.169899266479,204.203522483337),
 .UNSPECIFIED.);
#7811=B_SPLINE_CURVE_WITH_KNOTS('',3,(#76098,#76099,#76100,#76101,#76102,
#76103,#76104,#76105,#76106,#76107,#76108,#76109,#76110,#76111,#76112,#76113,
#76114,#76115,#76116,#76117,#76118,#76119,#76120,#76121,#76122,#76123,#76124,
#76125,#76126,#76127,#76128,#76129,#76130,#76131,#76132,#76133,#76134,#76135,
#76136,#76137,#76138,#76139,#76140,#76141,#76142,#76143,#76144,#76145,#76146,
#76147,#76148,#76149,#76150,#76151,#76152,#76153,#76154,#76155,#76156,#76157,
#76158,#76159,#76160,#76161,#76162,#76163,#76164,#76165,#76166,#76167,#76168,
#76169,#76170,#76171,#76172,#76173,#76174,#76175,#76176,#76177,#76178,#76179,
#76180,#76181,#76182,#76183,#76184,#76185,#76186,#76187,#76188,#76189,#76190,
#76191,#76192,#76193,#76194,#76195,#76196,#76197,#76198,#76199,#76200,#76201,
#76202,#76203,#76204,#76205,#76206,#76207,#76208,#76209,#76210,#76211,#76212,
#76213,#76214,#76215,#76216,#76217,#76218,#76219,#76220,#76221,#76222,#76223,
#76224,#76225,#76226,#76227,#76228,#76229,#76230,#76231,#76232,#76233,#76234,
#76235,#76236,#76237,#76238,#76239,#76240,#76241,#76242,#76243,#76244,#76245,
#76246,#76247,#76248,#76249,#76250,#76251,#76252,#76253,#76254,#76255,#76256,
#76257),.UNSPECIFIED.,.F.,.F.,(4,2,2,2,2,2,2,2,2,2,2,2,2,2,2,2,2,2,2,2,
2,2,2,2,2,2,2,2,2,2,2,2,2,2,2,2,2,2,2,2,2,2,2,2,2,2,2,2,2,2,2,2,2,2,2,2,
2,2,2,2,2,2,2,2,2,2,2,2,2,2,2,2,2,2,2,2,2,2,2,4),(-4.05986099759803,-4.02576223123953,
-3.96872201555675,-3.96116384617764,-3.95899062086544,-3.95765841144894,
-3.95643647240339,-3.954826756049,-3.95122967675135,-3.9100451979651,-3.86444290545402,
-3.8271367881249,-3.81211578674789,-3.80215777048877,-3.79870928481081,
-3.79668581398197,-3.79451411551451,-3.79172809227603,-3.78727116476695,
-3.76328723965276,-3.75678359119935,-3.7074043137533,-3.64629138354934,
-3.63847432402484,-3.63627473711878,-3.63493658034862,-3.63371649037272,
-3.63211904573086,-3.62858913687769,-3.57131498764554,-3.51638324418888,
-3.49379665177095,-3.48480907633369,-3.47816462200802,-3.47521520166415,
-3.47300924714719,-3.4709770026663,-3.46822410630542,-3.46284026184193,
-3.39804152928679,-3.32427463907567,-3.31575333375218,-3.31348614838437,
-3.31213279533161,-3.31091680218605,-3.3093484227072,-3.30597434864698,
-3.27887885092024,-3.19369867665139,-3.17095811182818,-3.16192678464934,
-3.15520190713397,-3.15223228821098,-3.15003318425868,-3.14799133516145,
-3.14520089482977,-3.13820949621613,-3.13398935005969,-3.05641953614232,
-3.00015056469761,-2.99264255687667,-2.99047428636812,-2.98914304204955,
-2.98792048552601,-2.98630791357827,-2.98269605167618,-2.93823928713803,
-2.87377305793219,-2.84909369421916,-2.83456419641673,-2.83057639883793,
-2.82816373125916,-2.82599484577514,-2.82323467753118,-2.8188632027548,
-2.79628602049327,-2.78766796436437,-2.78318617050587,-2.75237580113267,
-2.72824210628548),.UNSPECIFIED.);
#7812=B_SPLINE_CURVE_WITH_KNOTS('',3,(#76263,#76264,#76265,#76266,#76267,
#76268,#76269,#76270,#76271,#76272,#76273,#76274,#76275,#76276,#76277,#76278,
#76279,#76280,#76281,#76282,#76283,#76284,#76285,#76286,#76287,#76288,#76289,
#76290,#76291,#76292,#76293,#76294,#76295,#76296,#76297,#76298,#76299,#76300,
#76301,#76302,#76303,#76304,#76305,#76306,#76307,#76308,#76309,#76310,#76311,
#76312,#76313,#76314,#76315,#76316,#76317,#76318,#76319,#76320,#76321,#76322,
#76323,#76324,#76325,#76326,#76327,#76328,#76329,#76330,#76331,#76332,#76333,
#76334,#76335,#76336,#76337,#76338,#76339,#76340,#76341,#76342,#76343,#76344,
#76345,#76346,#76347,#76348,#76349,#76350,#76351,#76352,#76353,#76354,#76355,
#76356,#76357,#76358,#76359,#76360,#76361,#76362,#76363,#76364,#76365,#76366,
#76367,#76368,#76369,#76370,#76371,#76372,#76373,#76374,#76375,#76376,#76377,
#76378,#76379,#76380,#76381,#76382,#76383,#76384,#76385,#76386,#76387,#76388,
#76389,#76390,#76391,#76392,#76393,#76394,#76395,#76396,#76397,#76398,#76399,
#76400,#76401),.UNSPECIFIED.,.F.,.F.,(4,3,3,3,3,3,3,3,3,3,3,3,3,3,3,3,3,
3,3,3,3,3,3,3,3,3,3,3,3,3,3,3,3,3,3,3,3,3,3,3,3,3,3,3,3,3,4),(210.486707790516,
210.578625634296,210.670497716477,210.762349785492,210.85420756602,210.94615796819,
211.038153997138,211.13030926565,211.216305870791,211.30938117926,211.402330430342,
211.495181256671,211.587964262114,211.680712116758,211.773449643031,211.866201648235,
211.959052847147,212.05195586531,212.145014206523,212.215821009318,212.308896317787,
212.401845568869,212.494696395198,212.587479400641,212.680227255284,212.772964781557,
212.865716786762,212.958567985674,213.051471003836,213.144529345049,213.215336147845,
213.308411456314,213.401360707395,213.494211533725,213.586994539168,213.679742393811,
213.772479920084,213.865231925288,213.9580831242,214.050986142363,214.144044483576,
214.214851286371,214.307940588984,214.400878110334,214.493728177278,214.586506318758,
214.610741815597),.UNSPECIFIED.);
#7813=B_SPLINE_CURVE_WITH_KNOTS('',3,(#76402,#76403,#76404,#76405,#76406,
#76407,#76408,#76409,#76410,#76411,#76412,#76413,#76414,#76415,#76416,#76417,
#76418,#76419,#76420,#76421,#76422,#76423,#76424,#76425,#76426,#76427,#76428,
#76429,#76430,#76431,#76432,#76433,#76434,#76435,#76436,#76437,#76438,#76439,
#76440,#76441,#76442,#76443,#76444,#76445,#76446,#76447,#76448,#76449,#76450,
#76451,#76452,#76453,#76454,#76455,#76456,#76457,#76458,#76459,#76460,#76461,
#76462,#76463,#76464,#76465,#76466,#76467,#76468,#76469,#76470,#76471,#76472,
#76473,#76474),.UNSPECIFIED.,.F.,.F.,(4,3,3,3,3,3,3,3,3,3,3,3,3,3,3,3,3,
3,3,3,3,3,3,3,4),(208.327722804751,208.420652133282,208.513488042509,208.606262819109,
208.699006954437,208.791745266695,208.884502562575,208.977361508141,209.070276321948,
209.163341423797,209.217275593738,209.310350902207,209.403300153288,209.496150979618,
209.588933985061,209.681681839704,209.774419365978,209.867171371182,209.960022570094,
210.052925588256,210.145983929469,210.216790732264,210.334950410375,210.450987392898,
210.486707790339),.UNSPECIFIED.);
#7814=B_SPLINE_CURVE_WITH_KNOTS('',3,(#76475,#76476,#76477,#76478,#76479,
#76480,#76481,#76482,#76483,#76484,#76485,#76486,#76487,#76488,#76489,#76490,
#76491,#76492,#76493,#76494,#76495,#76496,#76497,#76498,#76499,#76500,#76501,
#76502,#76503,#76504,#76505,#76506,#76507,#76508,#76509,#76510,#76511,#76512,
#76513,#76514,#76515,#76516,#76517,#76518,#76519,#76520,#76521,#76522,#76523,
#76524,#76525,#76526,#76527,#76528,#76529,#76530,#76531,#76532,#76533,#76534,
#76535,#76536,#76537,#76538,#76539,#76540,#76541,#76542,#76543,#76544,#76545,
#76546,#76547,#76548,#76549,#76550,#76551,#76552,#76553,#76554,#76555,#76556,
#76557,#76558,#76559,#76560,#76561,#76562,#76563,#76564,#76565,#76566,#76567,
#76568,#76569,#76570,#76571,#76572,#76573,#76574,#76575,#76576,#76577,#76578,
#76579,#76580,#76581,#76582,#76583,#76584,#76585,#76586,#76587,#76588,#76589,
#76590,#76591,#76592,#76593,#76594,#76595,#76596,#76597,#76598,#76599,#76600,
#76601,#76602,#76603,#76604,#76605,#76606,#76607,#76608,#76609,#76610,#76611,
#76612,#76613,#76614,#76615,#76616,#76617,#76618,#76619,#76620,#76621,#76622,
#76623,#76624,#76625,#76626,#76627,#76628,#76629,#76630,#76631,#76632,#76633,
#76634,#76635,#76636,#76637,#76638,#76639,#76640,#76641,#76642,#76643,#76644,
#76645,#76646,#76647,#76648,#76649,#76650,#76651,#76652,#76653,#76654,#76655,
#76656,#76657,#76658,#76659,#76660,#76661,#76662,#76663,#76664,#76665,#76666,
#76667,#76668,#76669,#76670,#76671,#76672,#76673,#76674,#76675,#76676,#76677,
#76678,#76679,#76680,#76681,#76682,#76683,#76684,#76685,#76686,#76687,#76688,
#76689,#76690,#76691,#76692,#76693,#76694,#76695,#76696,#76697,#76698,#76699,
#76700,#76701,#76702,#76703,#76704,#76705,#76706,#76707,#76708,#76709,#76710,
#76711,#76712,#76713,#76714,#76715,#76716,#76717,#76718,#76719,#76720,#76721,
#76722,#76723,#76724,#76725,#76726,#76727,#76728),.UNSPECIFIED.,.F.,.F.,
(4,2,2,2,2,2,2,2,2,2,2,2,2,2,2,2,2,2,2,2,2,2,2,2,2,2,2,2,2,2,2,2,2,2,2,
2,2,2,2,2,2,2,2,2,2,2,2,2,2,2,2,2,2,2,2,2,2,2,2,2,2,2,2,2,2,2,2,2,2,2,2,
2,2,2,2,2,2,2,2,2,2,2,2,2,2,2,2,2,2,2,2,2,2,2,2,2,2,2,2,2,2,2,2,2,2,2,2,
2,2,2,2,2,2,2,2,2,2,2,2,2,2,2,2,2,2,2,4),(-2.72824210628548,-2.67852407763522,
-2.67287321466086,-2.6688095324003,-2.66709909064221,-2.66586484198403,
-2.66471828953474,-2.66312578185406,-2.65902535892125,-2.64055267506025,
-2.54774833062229,-2.52510852554374,-2.5114665411853,-2.50756594854955,
-2.50517279445116,-2.50299972483053,-2.50020398057078,-2.49440573473097,
-2.41835748719278,-2.37356069082141,-2.35649321346231,-2.34718495941917,
-2.3448486449642,-2.34347987711388,-2.34226728236056,-2.34069984098145,
-2.33741818772582,-2.31337497309463,-2.30378412772626,-2.30091872085506,
-2.25866528852906,-2.22182349637285,-2.20120518060028,-2.18847445192995,
-2.18466896546489,-2.18229687319757,-2.18011791145235,-2.17732615666466,
-2.17275093318077,-2.1466641883321,-2.13214669930338,-2.10263952289169,
-2.07570264161224,-2.03065325308063,-2.0294374316876,-2.02382022735442,
-2.02180480281561,-2.02063687971356,-2.01941507978655,-2.01777911045846,
-2.01413552917229,-1.96425809066924,-1.89487396085978,-1.88902732452201,
-1.86747550260778,-1.86316897048048,-1.86042871358817,-1.85826204701629,
-1.85583784366866,-1.85179817552488,-1.83671275203561,-1.81071424854568,
-1.76123192226472,-1.70357778772267,-1.70005372611599,-1.69845726120448,
-1.69723721782919,-1.69589835975162,-1.69369604001752,-1.68585301898887,
-1.62433239010156,-1.5461605463489,-1.54041984804851,-1.53763543573816,
-1.53546379460622,-1.53306471272793,-1.52913745393183,-1.51522927559619,
-1.4919817953294,-1.39553371564686,-1.37965592789621,-1.37701655758102,
-1.37543572110865,-1.37421787633615,-1.37287090985163,-1.37063274642979,
-1.3624233887018,-1.34811096154892,-1.3128625450552,-1.2290793513748,-1.22700430765647,
-1.21877196034975,-1.21545156787524,-1.21341151436176,-1.21121075714733,
-1.20823258703191,-1.20146112658946,-1.1923507701389,-1.16932960721208,
-1.07425177338058,-1.05678977944133,-1.05381036013184,-1.05228311815893,
-1.0510742634838,-1.0496790235126,-1.04722414799254,-1.03639168413504,-1.01516637589849,
-0.975616759790904,-0.900292475584009,-0.894472192478007,-0.891671752273947,
-0.889497670426158,-0.887106064350868,-0.883213984609284,-0.869661591757753,
-0.847222502185259,-0.758360745244659,-0.734227241895671,-0.730941726183378,
-0.729373242301046,-0.728160209938668,-0.726791342088824,-0.724455769088684,
-0.715345680138289,-0.698729442027986,-0.698305350374428),.UNSPECIFIED.);
#7815=B_SPLINE_CURVE_WITH_KNOTS('',3,(#76734,#76735,#76736,#76737,#76738,
#76739,#76740,#76741,#76742,#76743,#76744,#76745,#76746,#76747,#76748,#76749,
#76750,#76751,#76752,#76753,#76754,#76755,#76756,#76757,#76758,#76759,#76760,
#76761,#76762,#76763,#76764,#76765,#76766,#76767,#76768,#76769,#76770,#76771,
#76772,#76773,#76774,#76775,#76776,#76777,#76778,#76779,#76780,#76781,#76782,
#76783,#76784,#76785,#76786,#76787,#76788,#76789,#76790,#76791,#76792,#76793,
#76794,#76795,#76796,#76797,#76798,#76799,#76800,#76801,#76802,#76803,#76804,
#76805,#76806,#76807,#76808,#76809,#76810,#76811,#76812,#76813,#76814,#76815,
#76816,#76817,#76818,#76819,#76820,#76821,#76822,#76823,#76824,#76825,#76826,
#76827,#76828,#76829,#76830,#76831,#76832,#76833,#76834,#76835,#76836,#76837,
#76838,#76839,#76840,#76841,#76842,#76843,#76844,#76845,#76846,#76847,#76848,
#76849,#76850,#76851,#76852,#76853,#76854,#76855,#76856,#76857,#76858,#76859,
#76860,#76861,#76862,#76863,#76864,#76865,#76866,#76867,#76868,#76869,#76870,
#76871,#76872),.UNSPECIFIED.,.F.,.F.,(4,3,3,3,3,3,3,3,3,3,3,3,3,3,3,3,3,
3,3,3,3,3,3,3,3,3,3,3,3,3,3,3,3,3,3,3,3,3,3,3,3,3,3,3,3,3,4),(216.769893097926,
216.869651071983,216.969811169133,217.070182213147,217.17086776107,217.213396701952,
217.306472010421,217.399421261502,217.492272087832,217.585055093275,217.677802947918,
217.770540474191,217.863292479395,217.956143678307,218.04904669647,218.142105037683,
218.212911840478,218.305987148947,218.398936400028,218.491787226358,218.5845702318,
218.677318086444,218.770055612717,218.862807617921,218.955658816833,219.048561834995,
219.141620176209,219.212426979005,219.305502287474,219.398451538556,219.491302364886,
219.584085370329,219.676833224973,219.769570751246,219.862322756451,219.955173955363,
220.048076973526,220.14113531474,220.211942117532,220.304998119087,220.397936789095,
220.490783146426,220.583562124117,220.676309404351,220.769038764856,220.861797170051,
220.893125340463),.UNSPECIFIED.);
#7816=B_SPLINE_CURVE_WITH_KNOTS('',3,(#76873,#76874,#76875,#76876,#76877,
#76878,#76879,#76880,#76881,#76882,#76883,#76884,#76885,#76886,#76887,#76888,
#76889,#76890,#76891,#76892,#76893,#76894,#76895,#76896,#76897,#76898,#76899,
#76900,#76901,#76902,#76903,#76904,#76905,#76906,#76907,#76908,#76909,#76910,
#76911,#76912,#76913,#76914,#76915,#76916,#76917,#76918,#76919,#76920,#76921,
#76922,#76923,#76924,#76925,#76926,#76927,#76928,#76929,#76930,#76931,#76932,
#76933,#76934,#76935,#76936,#76937,#76938,#76939,#76940,#76941,#76942,#76943,
#76944,#76945),.UNSPECIFIED.,.F.,.F.,(4,3,3,3,3,3,3,3,3,3,3,3,3,3,3,3,3,
3,3,3,3,3,3,3,4),(214.610741815597,214.703484577683,214.796223492791,214.888983367554,
214.981845942894,215.074766162879,215.167834515814,215.214366424898,215.307441733367,
215.400390984448,215.493241810778,215.58602481622,215.678772670864,215.771510197137,
215.864262202342,215.957113401254,216.050016419416,216.14307476063,216.213881563425,
216.309608703086,216.405182094946,216.50058214959,216.595880461535,216.691077732157,
216.769893097696),.UNSPECIFIED.);
#7817=B_SPLINE_CURVE_WITH_KNOTS('',3,(#76947,#76948,#76949,#76950,#76951,
#76952,#76953,#76954,#76955,#76956,#76957,#76958,#76959,#76960,#76961,#76962,
#76963,#76964,#76965,#76966,#76967,#76968,#76969,#76970,#76971,#76972,#76973,
#76974,#76975,#76976,#76977,#76978,#76979,#76980,#76981,#76982,#76983,#76984,
#76985,#76986,#76987,#76988,#76989,#76990,#76991,#76992,#76993,#76994,#76995,
#76996,#76997,#76998,#76999,#77000,#77001,#77002,#77003,#77004,#77005,#77006,
#77007,#77008,#77009,#77010,#77011,#77012,#77013,#77014,#77015,#77016,#77017,
#77018,#77019,#77020,#77021,#77022,#77023,#77024,#77025,#77026,#77027,#77028,
#77029,#77030,#77031,#77032),.UNSPECIFIED.,.F.,.F.,(4,2,2,2,2,2,2,2,2,2,
2,2,2,2,2,2,2,2,2,2,2,2,2,2,2,2,2,2,2,2,2,2,2,2,2,2,2,2,2,2,2,2,4),(-0.698305350374428,
-0.656602296723661,-0.5836007993435,-0.581296347343703,-0.572859560935384,
-0.569504337187169,-0.567457413271066,-0.565260446374895,-0.562365998599244,
-0.556090346092476,-0.525063542871785,-0.463552101857718,-0.428094800229727,
-0.41086283905656,-0.407895258124277,-0.406370511292322,-0.405161787517078,
-0.403764614847878,-0.401301228903959,-0.390569851377794,-0.369562917374765,
-0.311750669171721,-0.254652755354803,-0.249264796733979,-0.246510347511368,
-0.244477230676223,-0.242270594034031,-0.240094263862954,-0.237191031589334,
-0.223294328449439,-0.187307110233393,-0.159451886526668,-0.12645111570544,
-0.104840459848454,-0.0879709537271096,-0.0852821735269327,-0.0836867663510794,
-0.0824666652261892,-0.0811268171269208,-0.0789209138754966,-0.076294655508303,
-0.0710918457574639,-0.000960804717552517),.UNSPECIFIED.);
#7818=B_SPLINE_CURVE_WITH_KNOTS('',3,(#77033,#77034,#77035,#77036,#77037,
#77038,#77039,#77040,#77041,#77042,#77043,#77044,#77045,#77046,#77047,#77048,
#77049,#77050,#77051,#77052,#77053,#77054,#77055,#77056,#77057,#77058,#77059,
#77060,#77061,#77062,#77063,#77064,#77065,#77066,#77067,#77068,#77069,#77070,
#77071,#77072,#77073,#77074,#77075,#77076,#77077,#77078,#77079,#77080,#77081,
#77082,#77083,#77084,#77085,#77086,#77087,#77088,#77089,#77090,#77091,#77092,
#77093,#77094,#77095,#77096,#77097,#77098,#77099,#77100,#77101,#77102,#77103,
#77104,#77105,#77106,#77107,#77108,#77109,#77110,#77111,#77112,#77113,#77114,
#77115,#77116,#77117,#77118,#77119,#77120,#77121,#77122,#77123,#77124,#77125,
#77126,#77127,#77128,#77129,#77130,#77131,#77132,#77133,#77134,#77135,#77136,
#77137,#77138,#77139,#77140,#77141,#77142,#77143,#77144,#77145,#77146,#77147,
#77148,#77149,#77150,#77151,#77152,#77153,#77154,#77155,#77156,#77157,#77158,
#77159,#77160,#77161,#77162,#77163,#77164,#77165,#77166,#77167,#77168,#77169,
#77170,#77171,#77172,#77173,#77174,#77175,#77176,#77177,#77178,#77179,#77180,
#77181,#77182,#77183,#77184,#77185,#77186,#77187,#77188,#77189,#77190),
 .UNSPECIFIED.,.F.,.F.,(4,2,2,2,2,2,2,2,2,2,2,2,2,2,2,2,2,2,2,2,2,2,2,2,
2,2,2,2,2,2,2,2,2,2,2,2,2,2,2,2,2,2,2,2,2,2,2,2,2,2,2,2,2,2,2,2,2,2,2,2,
2,2,2,2,2,2,2,2,2,2,2,2,2,2,2,2,2,2,4),(-4.06074652321885,-4.00420181140675,
-3.99046747971543,-3.98674482363625,-3.98424035421656,-3.98181813822638,
-3.97965121865307,-3.97690789302334,-3.97155361209754,-3.93882987105843,
-3.93475254135369,-3.90520762882977,-3.8730234492749,-3.83125007689878,
-3.82362382756395,-3.82138927291519,-3.82004326991225,-3.81882544732652,
-3.81724352392913,-3.81379724292883,-3.75215627857054,-3.70260485625695,
-3.67926851237964,-3.66536382420609,-3.66144859956524,-3.65903440907588,
-3.65686599649988,-3.65410895013348,-3.64850613561617,-3.61103029927893,
-3.55822868792299,-3.50356807558886,-3.4996998197946,-3.497990063621,-3.49675603121309,
-3.49560946577059,-3.49401663354439,-3.49077951948604,-3.45026773922722,
-3.37510109841307,-3.35479905282181,-3.34647261850833,-3.34021854013855,
-3.33734456972756,-3.33515162047842,-3.33310015854671,-3.3297184103972,
-3.32112023375118,-3.31910826908826,-3.24301297294014,-3.18148255110523,
-3.17698672771155,-3.17520505285234,-3.17395741806212,-3.17282663671404,
-3.17129486673413,-3.16830044296302,-3.14295811528901,-3.13611906064314,
-3.05370880117024,-3.03243234602709,-3.01940152557661,-3.01556419497734,
-3.01318516247597,-3.01100847128319,-3.00823148459069,-3.0023749898022,
-2.9287361382604,-2.88222220729951,-2.86474412707506,-2.8552786728533,-2.85292930212111,
-2.85155765059864,-2.85034563626801,-2.84878312725429,-2.84552656855973,
-2.82221202367707,-2.73218752784015,-2.72845886412415),.UNSPECIFIED.);
#7819=B_SPLINE_CURVE_WITH_KNOTS('',3,(#77196,#77197,#77198,#77199,#77200,
#77201,#77202,#77203,#77204,#77205,#77206,#77207,#77208,#77209,#77210,#77211,
#77212,#77213,#77214,#77215,#77216,#77217,#77218,#77219,#77220,#77221,#77222,
#77223,#77224,#77225,#77226,#77227,#77228,#77229,#77230,#77231,#77232,#77233,
#77234,#77235,#77236,#77237,#77238,#77239,#77240,#77241,#77242,#77243,#77244,
#77245,#77246,#77247,#77248,#77249,#77250,#77251,#77252,#77253,#77254,#77255,
#77256,#77257,#77258,#77259,#77260,#77261,#77262,#77263,#77264,#77265,#77266,
#77267,#77268,#77269,#77270,#77271,#77272,#77273,#77274,#77275,#77276,#77277,
#77278,#77279,#77280,#77281,#77282,#77283,#77284,#77285,#77286,#77287,#77288,
#77289,#77290,#77291,#77292,#77293,#77294,#77295,#77296,#77297,#77298,#77299,
#77300,#77301,#77302,#77303,#77304,#77305,#77306,#77307,#77308,#77309,#77310,
#77311,#77312,#77313,#77314,#77315,#77316,#77317,#77318,#77319,#77320,#77321,
#77322,#77323,#77324,#77325,#77326,#77327,#77328,#77329,#77330,#77331),
 .UNSPECIFIED.,.F.,.F.,(4,3,3,3,3,3,3,3,3,3,3,3,3,3,3,3,3,3,3,3,3,3,3,3,
3,3,3,3,3,3,3,3,3,3,3,3,3,3,3,3,3,3,3,3,3,4),(223.053078404875,223.210487533112,
223.303562841579,223.396512092659,223.489362918987,223.582145924429,223.674893779071,
223.767631305342,223.860383310545,223.953234509456,224.046137527617,224.139195868829,
224.210002671639,224.303077980105,224.396027231183,224.48887805751,224.581661062949,
224.67440891759,224.76714644386,224.859898449061,224.95274964797,225.045652666129,
225.13871100734,225.209517810166,225.302593118647,225.395542369741,225.488393196082,
225.581176201537,225.673924056193,225.766661582478,225.859413587694,225.952264786618,
226.045167804792,226.138226146017,226.209032948693,226.302110268686,226.395061011251,
226.492756092736,226.58553529333,226.678279903642,226.771014744662,226.863764622504,
226.956605203468,227.049498463682,227.142524695251,227.176621663132),
 .UNSPECIFIED.);
#7820=B_SPLINE_CURVE_WITH_KNOTS('',3,(#77332,#77333,#77334,#77335,#77336,
#77337,#77338,#77339,#77340,#77341,#77342,#77343,#77344,#77345,#77346,#77347,
#77348,#77349,#77350,#77351,#77352,#77353,#77354,#77355,#77356,#77357,#77358,
#77359,#77360,#77361,#77362,#77363,#77364,#77365,#77366,#77367,#77368,#77369,
#77370,#77371,#77372,#77373,#77374,#77375,#77376,#77377,#77378,#77379,#77380,
#77381,#77382,#77383,#77384,#77385,#77386,#77387,#77388,#77389,#77390,#77391,
#77392,#77393,#77394,#77395,#77396,#77397,#77398,#77399,#77400,#77401,#77402,
#77403,#77404,#77405,#77406,#77407),.UNSPECIFIED.,.F.,.F.,(4,3,3,3,3,3,
3,3,3,3,3,3,3,3,3,3,3,3,3,3,3,3,3,3,3,4),(220.893125340463,220.985991510786,
221.078917020852,221.171988638053,221.211457256059,221.304532564527,221.397481815608,
221.490332641937,221.583115647379,221.675863502022,221.768601028295,221.861353033499,
221.95420423241,222.047107250572,222.140165591785,222.210972394585,222.302663566803,
222.396465421535,222.487924128935,222.579326226343,222.670697886161,222.766293015787,
222.857723389603,222.949193261442,223.040767905907,223.053078404664),
 .UNSPECIFIED.);
#7821=B_SPLINE_CURVE_WITH_KNOTS('',3,(#77408,#77409,#77410,#77411,#77412,
#77413,#77414,#77415,#77416,#77417,#77418,#77419,#77420,#77421,#77422,#77423,
#77424,#77425,#77426,#77427,#77428,#77429,#77430,#77431,#77432,#77433,#77434,
#77435,#77436,#77437,#77438,#77439,#77440,#77441,#77442,#77443,#77444,#77445,
#77446,#77447,#77448,#77449,#77450,#77451,#77452,#77453,#77454,#77455,#77456,
#77457,#77458,#77459,#77460,#77461,#77462,#77463,#77464,#77465,#77466,#77467,
#77468,#77469,#77470,#77471,#77472,#77473,#77474,#77475,#77476,#77477,#77478,
#77479,#77480,#77481,#77482,#77483,#77484,#77485,#77486,#77487,#77488,#77489,
#77490,#77491,#77492,#77493,#77494,#77495,#77496,#77497,#77498,#77499,#77500,
#77501,#77502,#77503,#77504,#77505,#77506,#77507,#77508,#77509,#77510,#77511,
#77512,#77513,#77514,#77515,#77516,#77517,#77518,#77519,#77520,#77521,#77522,
#77523,#77524,#77525,#77526,#77527,#77528,#77529,#77530,#77531,#77532,#77533,
#77534,#77535,#77536,#77537,#77538,#77539,#77540,#77541,#77542,#77543,#77544,
#77545,#77546,#77547,#77548,#77549,#77550,#77551,#77552,#77553,#77554,#77555,
#77556,#77557,#77558,#77559,#77560,#77561,#77562,#77563,#77564,#77565,#77566,
#77567,#77568,#77569,#77570,#77571,#77572,#77573,#77574,#77575,#77576,#77577,
#77578,#77579,#77580,#77581,#77582,#77583,#77584,#77585,#77586,#77587,#77588,
#77589,#77590,#77591,#77592,#77593,#77594,#77595,#77596,#77597,#77598,#77599,
#77600,#77601,#77602,#77603,#77604,#77605,#77606,#77607,#77608,#77609,#77610,
#77611,#77612,#77613,#77614,#77615,#77616,#77617,#77618,#77619,#77620,#77621,
#77622,#77623,#77624,#77625,#77626,#77627,#77628,#77629,#77630,#77631,#77632,
#77633,#77634,#77635,#77636,#77637,#77638,#77639,#77640,#77641,#77642,#77643,
#77644,#77645,#77646,#77647,#77648,#77649,#77650,#77651),.UNSPECIFIED.,
 .F.,.F.,(4,2,2,2,2,2,2,2,2,2,2,2,2,2,2,2,2,2,2,2,2,2,2,2,2,2,2,2,2,2,2,
2,2,2,2,2,2,2,2,2,2,2,2,2,2,2,2,2,2,2,2,2,2,2,2,2,2,2,2,2,2,2,2,2,2,2,2,
2,2,2,2,2,2,2,2,2,2,2,2,2,2,2,2,2,2,2,2,2,2,2,2,2,2,2,2,2,2,2,2,2,2,2,2,
2,2,2,2,2,2,2,2,2,2,2,2,2,2,2,2,2,2,4),(-2.72845886412415,-2.71001279977591,
-2.69657787429951,-2.69269857406263,-2.69031027732171,-2.68813620453566,
-2.68533155419949,-2.67948715661297,-2.60527466696577,-2.55914728337796,
-2.54179073794797,-2.53237180970001,-2.53002637276707,-2.52865564050188,
-2.52744353242815,-2.52587969369927,-2.5226161019591,-2.49909467156313,
-2.43991905172684,-2.37881321260368,-2.37183825355244,-2.36882434268467,
-2.36661762755231,-2.36458640597858,-2.36183751579458,-2.35646928375539,
-2.30151500041319,-2.27032292316156,-2.21287082737795,-2.20839393884449,
-2.20661536930995,-2.20536841789368,-2.20423715498222,-2.20270323302731,
-2.19970015270593,-2.17402919617101,-2.16293092294055,-2.11020944659234,
-2.05482308593342,-2.04866328370565,-2.04579791762929,-2.04361539114066,
-2.04154405610076,-2.03864134239,-2.03096905040347,-1.99518099585338,-1.94535750253001,
-1.88874768203199,-1.88520913094023,-1.88361006582725,-1.88238970260562,
-1.88105227281296,-1.87885604177945,-1.87107282816111,-1.81051782954846,
-1.7377736667202,-1.73545842664585,-1.72702575517347,-1.72367198292562,
-1.72162588679548,-1.71942976397209,-1.71647738319536,-1.70984760486484,
-1.70097567802221,-1.67879259321744,-1.58869294089384,-1.56539872153345,
-1.56214273229629,-1.56058029499789,-1.55936824693066,-1.55799645161876,
-1.55564660270053,-1.54617606268826,-1.5286873839148,-1.48216183136456,
-1.46323556128996,-1.40881717619814,-1.40345244271557,-1.40070427770551,
-1.39867307942983,-1.39646589373025,-1.39345045557174,-1.38646801001133,
-1.32377633119451,-1.28161764831226,-1.25869018225871,-1.24214087145075,
-1.23946814558484,-1.23787760757627,-1.23665844839001,-1.23531664944845,
-1.23310120508212,-1.22512541286547,-1.16139587585269,-1.08569561489839,
-1.07988968784281,-1.07709243740587,-1.07491917577603,-1.07252679925682,
-1.06862970216058,-1.05502230906744,-1.03245745711464,-0.940054888513039,
-0.91946872661804,-0.916313859413043,-0.914771331100262,-0.913561239757791,
-0.912176688746589,-0.909769726874033,-0.899582201415185,-0.880167558926365,
-0.790388161454498,-0.784314923696493,-0.761221371325372,-0.75681819724679,
-0.754048339794272,-0.75187833410778,-0.749471100226588,-0.745507681248915,
-0.73123229426808,-0.707140932609663,-0.698901174862512),.UNSPECIFIED.);
#7822=B_SPLINE_CURVE_WITH_KNOTS('',3,(#77657,#77658,#77659,#77660,#77661,
#77662,#77663,#77664,#77665,#77666,#77667,#77668,#77669,#77670,#77671,#77672,
#77673,#77674,#77675,#77676,#77677,#77678,#77679,#77680,#77681,#77682,#77683,
#77684,#77685,#77686,#77687,#77688,#77689,#77690,#77691,#77692,#77693,#77694,
#77695,#77696,#77697,#77698,#77699,#77700,#77701,#77702,#77703,#77704,#77705,
#77706,#77707,#77708,#77709,#77710,#77711,#77712,#77713,#77714,#77715,#77716,
#77717,#77718,#77719,#77720,#77721,#77722,#77723,#77724,#77725,#77726,#77727,
#77728,#77729,#77730,#77731,#77732,#77733,#77734,#77735,#77736,#77737,#77738,
#77739,#77740,#77741,#77742,#77743,#77744,#77745,#77746,#77747,#77748,#77749,
#77750,#77751,#77752,#77753,#77754,#77755,#77756,#77757,#77758,#77759,#77760,
#77761,#77762,#77763,#77764,#77765,#77766,#77767,#77768,#77769,#77770,#77771,
#77772,#77773,#77774,#77775,#77776,#77777,#77778,#77779,#77780,#77781,#77782,
#77783,#77784,#77785,#77786,#77787,#77788,#77789,#77790,#77791,#77792,#77793,
#77794,#77795),.UNSPECIFIED.,.F.,.F.,(4,3,3,3,3,3,3,3,3,3,3,3,3,3,3,3,3,
3,3,3,3,3,3,3,3,3,3,3,3,3,3,3,3,3,3,3,3,3,3,3,3,3,3,3,3,3,4),(229.336263712314,
229.42794052537,229.51951143474,229.611006217099,229.702461675838,229.793903904296,
229.885358977926,229.976908380405,230.068510528856,230.160257179368,230.2070935028,
230.300168811201,230.393118062213,230.485968888472,230.578751893843,230.671499748413,
230.764237274613,230.856989279742,230.949840478579,231.042743496666,231.135801837804,
231.206608641326,231.299683950353,231.392633201994,231.485484028883,231.578267034885,
231.671014890088,231.763752416918,231.856504422678,231.949355622139,232.042258640847,
232.135316982596,232.206123779853,232.299199087417,232.392148337595,232.484999163024,
232.577782167573,232.670530021328,232.763267546718,232.856019551046,232.948870749098,
233.041773766408,233.134832106789,233.20563891838,233.298712979945,233.391648111515,
233.460568299342),.UNSPECIFIED.);
#7823=B_SPLINE_CURVE_WITH_KNOTS('',3,(#77796,#77797,#77798,#77799,#77800,
#77801,#77802,#77803,#77804,#77805,#77806,#77807,#77808,#77809,#77810,#77811,
#77812,#77813,#77814,#77815,#77816,#77817,#77818,#77819,#77820,#77821,#77822,
#77823,#77824,#77825,#77826,#77827,#77828,#77829,#77830,#77831,#77832,#77833,
#77834,#77835,#77836,#77837,#77838,#77839,#77840,#77841,#77842,#77843,#77844,
#77845,#77846,#77847,#77848,#77849,#77850,#77851,#77852,#77853,#77854,#77855,
#77856,#77857,#77858,#77859,#77860,#77861,#77862,#77863,#77864,#77865,#77866,
#77867,#77868),.UNSPECIFIED.,.F.,.F.,(4,3,3,3,3,3,3,3,3,3,3,3,3,3,3,3,3,
3,3,3,3,3,3,3,4),(227.176621663132,227.208548087219,227.301623395672,227.394572646738,
227.487423473051,227.580206478477,227.672954333105,227.765691859361,227.858443864549,
227.951295063444,228.04419808159,228.137256422787,228.208063225746,228.301138534298,
228.394087785463,228.486938611876,228.579721617402,228.672469472128,228.765206998484,
228.857959003771,228.950810202764,229.043713221007,229.1367715623,229.207578364273,
229.336263712055),.UNSPECIFIED.);
#7824=B_SPLINE_CURVE_WITH_KNOTS('',3,(#77870,#77871,#77872,#77873,#77874,
#77875,#77876,#77877,#77878,#77879,#77880,#77881,#77882,#77883,#77884,#77885,
#77886,#77887,#77888,#77889,#77890,#77891,#77892,#77893,#77894,#77895,#77896,
#77897,#77898,#77899,#77900,#77901,#77902,#77903,#77904,#77905,#77906,#77907,
#77908,#77909,#77910,#77911,#77912,#77913,#77914,#77915,#77916,#77917,#77918,
#77919,#77920,#77921,#77922,#77923,#77924,#77925,#77926,#77927,#77928,#77929,
#77930,#77931,#77932,#77933,#77934,#77935,#77936,#77937,#77938,#77939,#77940,
#77941,#77942,#77943,#77944,#77945,#77946,#77947,#77948,#77949),
 .UNSPECIFIED.,.F.,.F.,(4,2,2,2,2,2,2,2,2,2,2,2,2,2,2,2,2,2,2,2,2,2,2,2,
2,2,2,2,2,2,2,2,2,2,2,2,2,2,2,4),(-0.698901174862512,-0.611495796291315,
-0.596051005993559,-0.593433809350015,-0.591859456069309,-0.590642471395465,
-0.589510302508336,-0.587519147633891,-0.581576145476372,-0.545177789928452,
-0.494622345725019,-0.439993713122243,-0.434626150818557,-0.431877052633319,
-0.429845415760875,-0.427637996498952,-0.424622675931284,-0.417642456949691,
-0.35579623815866,-0.308932067628198,-0.297335225995657,-0.273758642113154,
-0.270492487481298,-0.268927908972513,-0.267715454508635,-0.266580401025271,
-0.265228370368795,-0.261099824300877,-0.229049521682879,-0.202712653639273,
-0.171785000905427,-0.117145974473519,-0.111778219304424,-0.109029046073699,
-0.106997365292933,-0.104789909502786,-0.101774559122264,-0.0947943609913781,
-0.0329865007214043,-0.000961184047303124),.UNSPECIFIED.);
#7825=B_SPLINE_CURVE_WITH_KNOTS('',3,(#77950,#77951,#77952,#77953,#77954,
#77955,#77956,#77957,#77958,#77959,#77960,#77961,#77962,#77963,#77964,#77965,
#77966,#77967,#77968,#77969,#77970,#77971,#77972,#77973,#77974,#77975,#77976,
#77977,#77978,#77979,#77980,#77981,#77982,#77983,#77984,#77985,#77986,#77987,
#77988,#77989,#77990,#77991,#77992,#77993,#77994,#77995,#77996,#77997,#77998,
#77999,#78000,#78001,#78002,#78003,#78004,#78005,#78006,#78007,#78008,#78009,
#78010,#78011,#78012,#78013,#78014,#78015,#78016,#78017,#78018,#78019,#78020,
#78021,#78022,#78023,#78024,#78025,#78026,#78027,#78028,#78029,#78030,#78031,
#78032,#78033,#78034,#78035,#78036,#78037,#78038,#78039,#78040,#78041,#78042,
#78043,#78044,#78045,#78046,#78047,#78048,#78049,#78050,#78051,#78052,#78053,
#78054,#78055,#78056,#78057,#78058,#78059,#78060,#78061,#78062,#78063,#78064,
#78065,#78066,#78067,#78068,#78069,#78070,#78071,#78072,#78073,#78074,#78075,
#78076,#78077,#78078,#78079,#78080,#78081,#78082,#78083,#78084,#78085,#78086,
#78087,#78088),.UNSPECIFIED.,.F.,.F.,(4,3,3,3,3,3,3,3,3,3,3,3,3,3,3,3,3,
3,3,3,3,3,3,3,3,3,3,3,3,3,3,3,3,3,3,3,3,3,3,3,3,3,3,3,3,3,4),(229.336263712055,
229.480732042408,229.509514426589,229.602589735044,229.695538986112,229.788389812428,
229.881172817857,229.973920672487,230.066658198747,230.159410203938,230.252261402838,
230.345164420987,230.438222762188,230.509029565116,230.602104873569,230.695054124635,
230.787904950948,230.880687956375,230.973435811002,231.066173337259,231.158925342446,
231.251776541342,231.344679559487,231.437737900684,231.508544703643,231.601620012195,
231.69456926336,231.787420089773,231.880203095299,231.972950950026,232.065688476382,
232.158440481668,232.251291680662,232.344194698905,232.437253040198,232.50805984217,
232.601138183882,232.694089688861,232.789794782308,232.882574404265,232.975318536495,
233.068052000494,233.160799602059,233.253633237029,233.346518921955,233.439528525831,
233.459730436439),.UNSPECIFIED.);
#7826=B_SPLINE_CURVE_WITH_KNOTS('',3,(#78094,#78095,#78096,#78097,#78098,
#78099,#78100,#78101,#78102,#78103,#78104,#78105,#78106,#78107,#78108,#78109,
#78110,#78111,#78112,#78113,#78114,#78115,#78116,#78117,#78118,#78119,#78120,
#78121,#78122,#78123,#78124,#78125,#78126,#78127,#78128,#78129,#78130,#78131,
#78132,#78133,#78134,#78135,#78136,#78137,#78138,#78139,#78140,#78141,#78142,
#78143,#78144,#78145,#78146,#78147,#78148,#78149,#78150,#78151,#78152,#78153,
#78154,#78155,#78156,#78157,#78158,#78159,#78160,#78161,#78162,#78163,#78164,
#78165,#78166,#78167,#78168,#78169,#78170,#78171,#78172,#78173,#78174,#78175,
#78176,#78177,#78178,#78179,#78180,#78181,#78182,#78183,#78184,#78185,#78186,
#78187,#78188,#78189,#78190,#78191,#78192,#78193,#78194,#78195,#78196,#78197,
#78198,#78199,#78200,#78201,#78202,#78203,#78204,#78205,#78206,#78207,#78208,
#78209,#78210,#78211,#78212,#78213,#78214,#78215,#78216,#78217,#78218,#78219,
#78220,#78221,#78222,#78223,#78224,#78225,#78226,#78227,#78228,#78229,#78230,
#78231,#78232),.UNSPECIFIED.,.F.,.F.,(4,3,3,3,3,3,3,3,3,3,3,3,3,3,3,3,3,
3,3,3,3,3,3,3,3,3,3,3,3,3,3,3,3,3,3,3,3,3,3,3,3,3,3,3,3,3,4),(235.619449019234,
235.713813979303,235.80821992053,235.907211023888,236.001831808201,236.096541649386,
236.191416982274,236.20418433396,236.297259643421,236.390208895436,236.483059722638,
236.575842728861,236.668590584227,236.761328111166,236.854080116978,236.946931316405,
237.039834335032,237.132892676623,237.203699472487,237.29677480437,237.389724078969,
237.482574928889,237.575357957936,237.668105836185,237.760843386037,237.853595414767,
237.946446636975,238.039349678344,238.132408042374,238.203214611014,238.296289867411,
238.389239066424,238.482089840753,238.574872794507,238.667620597668,238.760358072723,
238.853110027033,238.945961175863,239.038864144314,239.131922436942,239.20272974954,
239.295800196545,239.388750028471,239.481591937618,239.574370085677,239.667121342208,
239.743047127969),.UNSPECIFIED.);
#7827=B_SPLINE_CURVE_WITH_KNOTS('',3,(#78233,#78234,#78235,#78236,#78237,
#78238,#78239,#78240,#78241,#78242,#78243,#78244,#78245,#78246,#78247,#78248,
#78249,#78250,#78251,#78252,#78253,#78254,#78255,#78256,#78257,#78258,#78259,
#78260,#78261,#78262,#78263,#78264,#78265,#78266,#78267,#78268,#78269,#78270,
#78271,#78272,#78273,#78274,#78275,#78276,#78277,#78278,#78279,#78280,#78281,
#78282,#78283,#78284,#78285,#78286,#78287,#78288,#78289,#78290,#78291,#78292,
#78293,#78294,#78295,#78296,#78297,#78298,#78299,#78300,#78301,#78302),
 .UNSPECIFIED.,.F.,.F.,(4,3,3,3,3,3,3,3,3,3,3,3,3,3,3,3,3,3,3,3,3,3,3,4),
(233.460568299342,233.553641519038,233.646395978204,233.739133781382,233.831879737838,
233.925198317605,234.018086306996,234.111620181952,234.205154056907,234.298229369038,
234.391178623795,234.484029453808,234.576812462933,234.669560321256,234.762297851202,
234.855049860068,234.947901062601,235.040804084369,235.133862429124,235.204669195433,
235.308364151342,235.410472004582,235.514960511826,235.61944901907),
 .UNSPECIFIED.);
#7828=B_SPLINE_CURVE_WITH_KNOTS('',3,(#78304,#78305,#78306,#78307,#78308,
#78309,#78310,#78311,#78312,#78313,#78314,#78315,#78316,#78317,#78318,#78319,
#78320,#78321,#78322,#78323,#78324,#78325,#78326,#78327,#78328,#78329,#78330,
#78331,#78332,#78333,#78334,#78335,#78336,#78337,#78338,#78339,#78340,#78341,
#78342,#78343,#78344,#78345,#78346,#78347,#78348,#78349,#78350,#78351,#78352,
#78353,#78354,#78355,#78356,#78357,#78358,#78359,#78360,#78361,#78362,#78363,
#78364,#78365,#78366,#78367,#78368,#78369,#78370,#78371,#78372,#78373,#78374,
#78375,#78376),.UNSPECIFIED.,.F.,.F.,(4,3,3,3,3,3,3,3,3,3,3,3,3,3,3,3,3,
3,3,3,3,3,3,3,4),(233.459730436439,233.507574980696,233.600650289097,233.693599540109,
233.786450366367,233.879233371738,233.971981226308,234.064718752508,234.157470757637,
234.250321956474,234.34322497456,234.436283315698,234.507090119223,234.600165428251,
234.693114679893,234.785965506785,234.878748512788,234.971496367992,235.064233894824,
235.156985900585,235.249837100047,235.342740118756,235.435798460507,235.50660525775,
235.619449019234),.UNSPECIFIED.);
#7829=B_SPLINE_CURVE_WITH_KNOTS('',3,(#78377,#78378,#78379,#78380,#78381,
#78382,#78383,#78384),.UNSPECIFIED.,.F.,.F.,(4,1,1,1,1,4),(235.619457915363,
236.506120396277,237.505635534803,238.50515067333,239.504665811857,239.744094875057),
 .UNSPECIFIED.);
#7830=B_SPLINE_CURVE_WITH_KNOTS('',3,(#78390,#78391,#78392,#78393,#78394,
#78395,#78396,#78397,#78398,#78399,#78400,#78401,#78402,#78403,#78404,#78405,
#78406,#78407,#78408,#78409,#78410,#78411,#78412,#78413,#78414,#78415,#78416,
#78417,#78418,#78419,#78420,#78421,#78422,#78423,#78424,#78425,#78426,#78427,
#78428,#78429,#78430,#78431,#78432,#78433,#78434,#78435,#78436,#78437,#78438,
#78439,#78440,#78441,#78442,#78443,#78444,#78445,#78446,#78447,#78448,#78449,
#78450,#78451,#78452,#78453,#78454,#78455,#78456,#78457,#78458,#78459,#78460,
#78461,#78462,#78463,#78464,#78465,#78466,#78467,#78468,#78469,#78470,#78471,
#78472,#78473,#78474,#78475,#78476,#78477,#78478,#78479,#78480,#78481,#78482,
#78483,#78484,#78485,#78486,#78487,#78488,#78489,#78490,#78491,#78492,#78493,
#78494,#78495,#78496,#78497,#78498,#78499,#78500,#78501,#78502,#78503,#78504,
#78505,#78506,#78507,#78508,#78509,#78510,#78511,#78512,#78513,#78514,#78515,
#78516,#78517,#78518,#78519,#78520,#78521,#78522,#78523,#78524,#78525),
 .UNSPECIFIED.,.F.,.F.,(4,3,3,3,3,3,3,3,3,3,3,3,3,3,3,3,3,3,3,3,3,3,3,3,
3,3,3,3,3,3,3,3,3,3,3,3,3,3,3,3,3,3,3,3,3,4),(241.902634326701,242.014547276602,
242.128011485217,242.201275165121,242.294350730384,242.387300235814,242.480151313763,
242.572934565756,242.665682663774,242.758420429985,242.851172671426,242.944024099428,
243.036927343076,243.12998590156,243.200790303647,243.293866473918,243.386816592658,
243.479668291321,243.572452172529,243.665200904769,243.757939309439,243.850692192807,
243.943544264079,244.036448152747,244.129507352332,244.200305442174,244.293378028059,
244.386324553392,244.479172654295,244.571952945761,244.664698094259,244.757432925305,
244.850182249303,244.943030805156,245.035931197279,245.128986967606,245.199820580701,
245.292909915226,245.385843649138,245.478688419339,245.571469145869,245.664210688667,
245.756971097239,245.849737147195,245.942591646576,246.025775112553),
 .UNSPECIFIED.);
#7831=B_SPLINE_CURVE_WITH_KNOTS('',3,(#78526,#78527,#78528,#78529,#78530,
#78531,#78532,#78533,#78534,#78535,#78536,#78537,#78538,#78539,#78540,#78541,
#78542,#78543,#78544,#78545,#78546,#78547,#78548,#78549,#78550,#78551,#78552,
#78553,#78554,#78555,#78556,#78557,#78558,#78559,#78560,#78561,#78562,#78563,
#78564,#78565,#78566,#78567,#78568,#78569,#78570,#78571,#78572,#78573,#78574,
#78575,#78576,#78577,#78578,#78579,#78580,#78581,#78582,#78583,#78584,#78585,
#78586,#78587,#78588,#78589,#78590,#78591,#78592,#78593,#78594,#78595,#78596,
#78597,#78598),.UNSPECIFIED.,.F.,.F.,(4,3,3,3,3,3,3,3,3,3,3,3,3,3,3,3,3,
3,3,3,3,3,3,3,4),(239.743047127969,239.835794683293,239.928638893887,240.02153087869,
240.114583385812,240.202244888067,240.295320341527,240.38826973839,240.481120711097,
240.573903863212,240.666651864664,240.75938953771,240.85214168948,240.944993033731,
241.037896196778,241.130954680623,241.201760026594,241.29424884327,241.386619345769,
241.478897153144,241.571107792623,241.663291651751,241.755458500974,241.847666146414,
241.902634326414),.UNSPECIFIED.);
#7832=B_SPLINE_CURVE_WITH_KNOTS('',3,(#78600,#78601,#78602,#78603,#78604,
#78605),.UNSPECIFIED.,.F.,.F.,(4,1,1,4),(239.744094875057,240.504180950384,
241.50369608891,241.902627319837),.UNSPECIFIED.);
#7833=B_SPLINE_CURVE_WITH_KNOTS('',3,(#78606,#78607,#78608,#78609,#78610,
#78611,#78612,#78613,#78614,#78615,#78616,#78617,#78618,#78619,#78620,#78621,
#78622,#78623,#78624,#78625,#78626,#78627,#78628,#78629,#78630,#78631,#78632,
#78633,#78634,#78635,#78636,#78637,#78638,#78639,#78640,#78641,#78642,#78643,
#78644,#78645,#78646,#78647,#78648,#78649,#78650,#78651,#78652,#78653,#78654,
#78655,#78656,#78657,#78658,#78659,#78660,#78661,#78662,#78663,#78664,#78665,
#78666,#78667,#78668,#78669,#78670,#78671,#78672,#78673,#78674,#78675,#78676,
#78677,#78678,#78679,#78680,#78681,#78682,#78683,#78684,#78685,#78686,#78687,
#78688,#78689,#78690,#78691,#78692,#78693,#78694,#78695,#78696,#78697,#78698,
#78699,#78700,#78701,#78702,#78703,#78704,#78705,#78706,#78707,#78708,#78709,
#78710,#78711,#78712,#78713,#78714,#78715,#78716,#78717,#78718,#78719,#78720,
#78721,#78722,#78723,#78724,#78725,#78726,#78727,#78728,#78729,#78730,#78731,
#78732,#78733,#78734,#78735,#78736,#78737,#78738,#78739,#78740,#78741,#78742,
#78743,#78744),.UNSPECIFIED.,.F.,.F.,(4,3,3,3,3,3,3,3,3,3,3,3,3,3,3,3,3,
3,3,3,3,3,3,3,3,3,3,3,3,3,3,3,3,3,3,3,3,3,3,3,3,3,3,3,3,3,4),(241.902634326414,
241.996604979565,242.090603522195,242.184652469409,242.278839297194,242.373105210619,
242.467538925424,242.503211227437,242.596286557953,242.689235830694,242.782086678273,
242.87486970427,242.967617579037,243.060355124983,243.153107149387,243.245958366654,
243.338861402733,243.431919760961,243.502726365964,243.59580181966,243.68875121676,
243.781602189705,243.874385342059,243.96713334375,244.059871017034,244.152623169041,
244.245474513527,244.33837767681,244.431436160885,244.502241504491,244.59531643186,
244.688265301624,244.781115746902,244.873898373223,244.966645850041,245.059383000215,
245.152134631479,245.244985462082,245.337888114483,245.430946097903,245.501756643018,
245.594829187545,245.687780746752,245.780622969611,245.873401283084,245.966148308563,
246.026281163792),.UNSPECIFIED.);
#7834=B_SPLINE_CURVE_WITH_KNOTS('',3,(#78750,#78751,#78752,#78753,#78754,
#78755,#78756,#78757,#78758,#78759,#78760,#78761,#78762,#78763,#78764,#78765,
#78766,#78767,#78768,#78769,#78770,#78771,#78772,#78773,#78774,#78775,#78776,
#78777,#78778,#78779,#78780,#78781,#78782,#78783,#78784,#78785,#78786,#78787,
#78788,#78789,#78790,#78791,#78792,#78793,#78794,#78795,#78796,#78797,#78798,
#78799,#78800,#78801,#78802,#78803,#78804,#78805,#78806,#78807,#78808,#78809,
#78810,#78811,#78812,#78813,#78814,#78815,#78816,#78817,#78818,#78819,#78820,
#78821,#78822,#78823,#78824,#78825,#78826,#78827,#78828,#78829,#78830,#78831,
#78832,#78833,#78834,#78835,#78836,#78837,#78838,#78839,#78840,#78841,#78842,
#78843,#78844,#78845,#78846,#78847,#78848,#78849,#78850,#78851,#78852,#78853,
#78854,#78855,#78856,#78857,#78858,#78859,#78860,#78861,#78862,#78863,#78864,
#78865,#78866,#78867,#78868,#78869,#78870,#78871,#78872,#78873,#78874,#78875,
#78876,#78877,#78878,#78879,#78880,#78881,#78882,#78883,#78884,#78885,#78886,
#78887,#78888,#78889,#78890,#78891),.UNSPECIFIED.,.F.,.F.,(4,3,3,3,3,3,
3,3,3,3,3,3,3,3,3,3,3,3,3,3,3,3,3,3,3,3,3,3,3,3,3,3,3,3,3,3,3,3,3,3,3,3,
3,3,3,3,3,4),(248.185819633594,248.198365996281,248.291463087134,248.384434034099,
248.477306443604,248.570110777739,248.662879798763,248.755638305531,248.848411081612,
248.941282600742,249.034205720857,249.127283599223,249.197881134808,249.290981271026,
249.383955651114,249.47683187142,249.569640561775,249.662414271377,249.755177791293,
249.84795589757,249.940833200336,250.033762364561,250.126846646318,250.197396273335,
250.290340851261,250.38315907809,250.475878752769,250.56853093863,250.661148212794,
250.753755544434,250.846377887958,250.939101043765,251.031876711656,251.12481016674,
251.196911411862,251.290167611414,251.38329726983,251.476327792447,251.569288701951,
251.662213301877,251.755126210699,251.848052030612,251.94107355418,252.034145218454,
252.127367725925,252.196426550388,252.289631618365,252.310073042627),
 .UNSPECIFIED.);
#7835=B_SPLINE_CURVE_WITH_KNOTS('',3,(#78892,#78893,#78894,#78895,#78896,
#78897,#78898,#78899,#78900,#78901,#78902,#78903,#78904,#78905,#78906,#78907,
#78908,#78909,#78910,#78911,#78912,#78913,#78914,#78915,#78916,#78917,#78918,
#78919,#78920,#78921,#78922,#78923,#78924,#78925,#78926,#78927,#78928,#78929,
#78930,#78931,#78932,#78933,#78934,#78935,#78936,#78937,#78938,#78939,#78940,
#78941,#78942,#78943,#78944,#78945,#78946,#78947,#78948,#78949,#78950,#78951,
#78952,#78953,#78954,#78955,#78956,#78957,#78958,#78959,#78960,#78961,#78962,
#78963,#78964),.UNSPECIFIED.,.F.,.F.,(4,3,3,3,3,3,3,3,3,3,3,3,3,3,3,3,3,
3,3,3,3,3,3,3,4),(246.025775112553,246.118832148656,246.199335719228,246.292415864885,
246.385369995563,246.478225737109,246.57101369087,246.66376651257,246.756509018734,
246.849266010765,246.942122176217,247.035030157428,247.128093404009,247.198850857755,
247.291703398481,247.384429991938,247.477058559664,247.569620194277,247.662147570796,
247.75466576799,247.847199850451,247.939833337813,248.032520394819,248.125359274108,
248.185819633352),.UNSPECIFIED.);
#7836=B_SPLINE_CURVE_WITH_KNOTS('',3,(#78966,#78967,#78968,#78969,#78970,
#78971,#78972,#78973,#78974,#78975,#78976,#78977,#78978,#78979,#78980,#78981,
#78982,#78983,#78984,#78985,#78986,#78987,#78988,#78989,#78990,#78991,#78992,
#78993,#78994,#78995,#78996,#78997,#78998,#78999,#79000,#79001,#79002,#79003,
#79004,#79005,#79006,#79007,#79008,#79009,#79010,#79011,#79012,#79013,#79014,
#79015,#79016,#79017,#79018,#79019,#79020,#79021,#79022,#79023,#79024,#79025,
#79026,#79027,#79028,#79029,#79030,#79031,#79032,#79033,#79034,#79035,#79036,
#79037,#79038),.UNSPECIFIED.,.F.,.F.,(4,3,3,3,3,3,3,3,3,3,3,3,3,3,3,3,3,
3,3,3,3,3,3,3,4),(246.026281163792,246.119025485589,246.214587059578,246.307471173777,
246.40437147766,246.501271781544,246.594347953035,246.687298073003,246.780149772899,
246.872933655342,246.965682388819,247.058420794725,247.151173679327,247.244025751824,
247.336929641714,247.429988842502,247.500786920071,247.593497367521,247.686087513679,
247.778582742491,247.871008346648,247.963400609079,248.055773554489,248.148176514885,
248.185819633594),.UNSPECIFIED.);
#7837=B_SPLINE_CURVE_WITH_KNOTS('',3,(#79039,#79040,#79041,#79042,#79043,
#79044,#79045,#79046),.UNSPECIFIED.,.F.,.F.,(4,1,1,1,1,4),(248.18582614159,
248.500302058598,249.499817197125,250.499332335651,251.498847474178,252.308677356644),
 .UNSPECIFIED.);
#7838=B_SPLINE_CURVE_WITH_KNOTS('',3,(#79050,#79051,#79052,#79053,#79054,
#79055,#79056,#79057,#79058,#79059,#79060,#79061,#79062,#79063,#79064,#79065,
#79066,#79067,#79068,#79069,#79070,#79071,#79072,#79073,#79074,#79075,#79076,
#79077,#79078,#79079,#79080,#79081,#79082,#79083,#79084,#79085,#79086,#79087,
#79088,#79089,#79090,#79091,#79092,#79093,#79094,#79095,#79096,#79097,#79098,
#79099,#79100,#79101,#79102,#79103,#79104,#79105,#79106,#79107,#79108,#79109,
#79110,#79111,#79112,#79113,#79114,#79115,#79116,#79117,#79118,#79119,#79120,
#79121,#79122),.UNSPECIFIED.,.F.,.F.,(4,3,3,3,3,3,3,3,3,3,3,3,3,3,3,3,3,
3,3,3,3,3,3,3,4),(-4.09274904019422,-3.99806055410705,-3.90933401922389,
-3.82072263115133,-3.73220278454794,-3.64049561342698,-3.55208063682188,
-3.46368033464884,-3.37527351717314,-3.286838995271,-3.19830733410243,-3.10971782729645,
-3.02100177211767,-2.99854541558029,-2.91073114418483,-2.82302915589964,
-2.73541486759979,-2.64786150605922,-2.56033956926054,-2.472826981501,-2.38530167908133,
-2.29768996361524,-2.21003219394396,-2.12224023889375,-2.0613590937516),
 .UNSPECIFIED.);
#7839=B_SPLINE_CURVE_WITH_KNOTS('',3,(#79126,#79127,#79128,#79129,#79130),
 .UNSPECIFIED.,.F.,.F.,(4,1,4),(0.,0.999515138526753,1.11004521091174),
 .UNSPECIFIED.);
#7840=B_SPLINE_CURVE_WITH_KNOTS('',3,(#79132,#79133,#79134,#79135,#79136,
#79137,#79138,#79139,#79140,#79141,#79142,#79143,#79144,#79145,#79146,#79147,
#79148,#79149,#79150,#79151,#79152,#79153,#79154,#79155,#79156,#79157,#79158,
#79159,#79160,#79161,#79162,#79163,#79164,#79165,#79166,#79167,#79168,#79169,
#79170,#79171,#79172,#79173,#79174,#79175,#79176,#79177,#79178,#79179,#79180,
#79181,#79182,#79183,#79184,#79185,#79186,#79187,#79188,#79189,#79190,#79191,
#79192,#79193,#79194,#79195,#79196,#79197,#79198,#79199,#79200,#79201,#79202,
#79203,#79204,#79205,#79206,#79207,#79208,#79209,#79210,#79211,#79212,#79213,
#79214,#79215,#79216,#79217,#79218,#79219,#79220,#79221,#79222,#79223,#79224,
#79225,#79226,#79227,#79228,#79229,#79230,#79231,#79232,#79233,#79234,#79235,
#79236,#79237,#79238,#79239,#79240,#79241,#79242,#79243,#79244,#79245,#79246,
#79247,#79248,#79249,#79250,#79251,#79252,#79253,#79254,#79255,#79256,#79257,
#79258,#79259,#79260,#79261,#79262,#79263,#79264,#79265,#79266,#79267,#79268,
#79269,#79270,#79271,#79272,#79273,#79274,#79275,#79276,#79277,#79278,#79279,
#79280,#79281,#79282,#79283,#79284,#79285,#79286,#79287,#79288,#79289,#79290,
#79291,#79292,#79293,#79294,#79295,#79296,#79297,#79298,#79299,#79300,#79301,
#79302,#79303,#79304,#79305,#79306,#79307,#79308,#79309,#79310,#79311,#79312,
#79313,#79314,#79315,#79316,#79317,#79318,#79319,#79320,#79321,#79322,#79323,
#79324,#79325,#79326,#79327,#79328,#79329,#79330,#79331,#79332,#79333,#79334,
#79335,#79336,#79337,#79338,#79339,#79340,#79341,#79342,#79343,#79344,#79345,
#79346,#79347,#79348,#79349,#79350,#79351,#79352,#79353,#79354,#79355,#79356,
#79357),.UNSPECIFIED.,.F.,.F.,(4,3,3,3,3,3,3,3,3,3,3,3,3,3,3,3,3,3,3,3,
3,3,3,3,3,3,3,3,3,3,3,3,3,3,3,3,3,3,3,3,3,3,3,3,3,3,3,3,3,3,3,3,3,3,3,3,
3,3,3,3,3,3,3,3,3,3,3,3,3,3,3,3,3,3,3,4),(1.11004521091174,1.19654441799083,
1.28293646607715,1.3724481924492,1.45870649482798,1.54494140864206,1.63117580777507,
1.71743256483515,1.80378323591016,1.89018992682975,1.97672445273537,1.99903027705352,
2.08771220340936,2.17627947182013,2.26475572191515,2.35647943362329,2.44485231996562,
2.53321114595239,2.62157713365239,2.70997150502374,2.79846419126683,2.88701535992536,
2.97569427651059,2.99854541558028,3.08725486513629,3.17585242746601,3.26436169446516,
3.3560740519204,3.44448659204278,3.53288746941176,3.62129787310793,3.70973899383516,
3.79828167792104,3.88688480079563,3.97561815529859,3.99806055410704,4.08649685647091,
4.17481697886979,4.26304487091473,4.35486122362961,4.44298432440019,4.53109327174227,
4.61920955868426,4.70735467852735,4.79560005164762,4.8839047331063,4.9723402938607,
4.9975756926338,5.08615468069272,5.17461904443609,5.26299255454003,5.3547548391176,
5.44302609570133,5.53128388824983,5.61954955605335,5.70784443890993,5.79623939193333,
5.88469373435058,5.97327791518406,5.99709083116056,6.0856636771011,6.17412216660342,
6.26249007643259,6.35425456308943,6.4425209458385,6.53077414267478,6.61903549927753,
6.70732636205143,6.79571775052301,6.88416878954928,6.97275007846284,6.99660596968732,
7.09576204967982,7.19407935025374,7.29365481995553,7.39323028965731),
 .UNSPECIFIED.);
#7841=B_SPLINE_CURVE_WITH_KNOTS('',3,(#79359,#79360,#79361,#79362,#79363,
#79364,#79365,#79366,#79367,#79368),.UNSPECIFIED.,.F.,.F.,(4,1,1,1,1,1,
1,4),(7.39323051809133,7.99612110821409,8.99563624674086,9.99515138526763,
10.9946665237944,11.9941816623212,12.9936968008479,13.6764158252709),
 .UNSPECIFIED.);
#7842=B_SPLINE_CURVE_WITH_KNOTS('',3,(#79370,#79371,#79372,#79373,#79374,
#79375,#79376,#79377,#79378,#79379,#79380,#79381,#79382,#79383,#79384,#79385,
#79386,#79387,#79388,#79389,#79390,#79391,#79392,#79393,#79394,#79395,#79396,
#79397,#79398,#79399,#79400,#79401,#79402,#79403,#79404,#79405,#79406,#79407,
#79408,#79409,#79410,#79411,#79412,#79413,#79414,#79415,#79416,#79417,#79418,
#79419,#79420,#79421,#79422,#79423,#79424,#79425,#79426,#79427,#79428,#79429,
#79430,#79431,#79432,#79433,#79434,#79435,#79436,#79437,#79438,#79439,#79440,
#79441,#79442,#79443,#79444,#79445,#79446,#79447,#79448,#79449,#79450,#79451,
#79452,#79453,#79454,#79455,#79456,#79457,#79458,#79459,#79460,#79461,#79462,
#79463,#79464,#79465,#79466,#79467,#79468,#79469,#79470,#79471,#79472,#79473,
#79474,#79475,#79476,#79477,#79478,#79479,#79480,#79481,#79482,#79483,#79484,
#79485,#79486,#79487,#79488,#79489,#79490,#79491,#79492,#79493,#79494,#79495,
#79496,#79497,#79498,#79499,#79500,#79501,#79502,#79503,#79504,#79505,#79506,
#79507,#79508,#79509,#79510,#79511,#79512,#79513,#79514,#79515,#79516,#79517,
#79518,#79519,#79520,#79521,#79522,#79523,#79524,#79525,#79526,#79527,#79528,
#79529,#79530,#79531,#79532,#79533,#79534,#79535,#79536,#79537,#79538,#79539,
#79540,#79541,#79542,#79543,#79544,#79545,#79546,#79547,#79548,#79549,#79550,
#79551,#79552,#79553,#79554,#79555,#79556,#79557,#79558,#79559,#79560,#79561,
#79562,#79563,#79564,#79565,#79566,#79567,#79568,#79569,#79570,#79571,#79572,
#79573,#79574,#79575,#79576,#79577,#79578,#79579,#79580,#79581,#79582,#79583,
#79584,#79585,#79586,#79587,#79588,#79589,#79590,#79591,#79592),
 .UNSPECIFIED.,.F.,.F.,(4,3,3,3,3,3,3,3,3,3,3,3,3,3,3,3,3,3,3,3,3,3,3,3,
3,3,3,3,3,3,3,3,3,3,3,3,3,3,3,3,3,3,3,3,3,3,3,3,3,3,3,3,3,3,3,3,3,3,3,3,
3,3,3,3,3,3,3,3,3,3,3,3,3,3,4),(13.6764160373865,13.7808737156826,13.8870428275287,
13.9932119393747,14.0817664757986,14.1702062997995,14.2585552123784,14.3503266955688,
14.4385733694417,14.5268066274285,14.6150478355601,14.7033183604559,14.7916892311257,
14.880119622141,14.9686802307502,14.9927270779015,15.0812814953253,15.16972119964,
15.2580699919952,15.3498415200493,15.4380880731251,15.5263212103106,15.6145622977665,
15.7028327022423,15.7912034534845,15.8796337255028,15.9681942166741,15.9922422164282,
16.0807965719483,16.1692362130696,16.2575849410238,16.3493564927652,16.4376029788168,
16.5258360481204,16.6140770669054,16.7023474019894,16.7907180831137,16.8791482845041,
16.9677087048413,16.991757354955,17.0803117779812,17.1687514875251,17.2571002847314,
17.3488718108252,17.4371183677683,17.5253515084495,17.6135925990237,17.7018630062345,
17.790233759625,17.8786640334521,17.9672245259167,17.9912724934817,18.0798268952625,
18.1682665833952,18.2566153590514,18.348386893171,18.4366334283541,18.5248665472347,
18.6131076159914,18.7013780013908,18.7897487330894,18.8781789852675,18.9667394563144,
18.9907876320085,19.0788961928086,19.1668903635541,19.2547944509364,19.3428952860973,
19.4307012445493,19.5184950937299,19.6062986484043,19.6946242693592,19.7825588282261,
19.871079980225,19.9596011322238),.UNSPECIFIED.);
#7843=B_SPLINE_CURVE_WITH_KNOTS('',3,(#79594,#79595,#79596,#79597,#79598,
#79599,#79600,#79601,#79602,#79603,#79604,#79605,#79606,#79607,#79608,#79609,
#79610,#79611,#79612,#79613,#79614,#79615,#79616,#79617,#79618,#79619,#79620,
#79621,#79622,#79623,#79624,#79625,#79626,#79627,#79628,#79629,#79630,#79631,
#79632,#79633,#79634,#79635,#79636,#79637,#79638,#79639,#79640,#79641,#79642,
#79643,#79644,#79645,#79646,#79647,#79648,#79649,#79650,#79651,#79652,#79653,
#79654,#79655,#79656,#79657,#79658,#79659,#79660,#79661,#79662,#79663,#79664,
#79665,#79666,#79667,#79668,#79669,#79670,#79671,#79672,#79673,#79674,#79675,
#79676,#79677,#79678,#79679,#79680,#79681,#79682,#79683,#79684,#79685,#79686,
#79687,#79688,#79689,#79690,#79691,#79692,#79693,#79694,#79695,#79696,#79697,
#79698,#79699,#79700,#79701,#79702,#79703,#79704,#79705,#79706,#79707,#79708,
#79709,#79710,#79711,#79712,#79713,#79714,#79715,#79716,#79717,#79718,#79719,
#79720,#79721,#79722,#79723,#79724,#79725,#79726,#79727,#79728,#79729,#79730,
#79731,#79732,#79733,#79734,#79735,#79736,#79737,#79738,#79739,#79740,#79741,
#79742,#79743,#79744,#79745,#79746,#79747,#79748,#79749,#79750,#79751,#79752,
#79753,#79754,#79755,#79756,#79757,#79758,#79759,#79760,#79761,#79762,#79763,
#79764,#79765,#79766,#79767,#79768,#79769,#79770,#79771,#79772,#79773,#79774,
#79775,#79776,#79777,#79778,#79779,#79780,#79781,#79782,#79783,#79784,#79785,
#79786,#79787,#79788,#79789,#79790,#79791,#79792,#79793,#79794,#79795,#79796,
#79797,#79798,#79799,#79800,#79801,#79802,#79803,#79804,#79805,#79806,#79807,
#79808,#79809,#79810,#79811,#79812,#79813,#79814,#79815,#79816,#79817,#79818,
#79819,#79820,#79821,#79822),.UNSPECIFIED.,.F.,.F.,(4,3,3,3,3,3,3,3,3,3,
3,3,3,3,3,3,3,3,3,3,3,3,3,3,3,3,3,3,3,3,3,3,3,3,3,3,3,3,3,3,3,3,3,3,3,3,
3,3,3,3,3,3,3,3,3,3,3,3,3,3,3,3,3,3,3,3,3,3,3,3,3,3,3,3,3,3,4),(19.9596011324505,
19.9903027705352,20.0788571753237,20.1672968664412,20.2556456450556,20.3474171780564,
20.4356637161121,20.5238968378287,20.6121379093813,20.7004082975332,20.7887790319058,
20.8772092867154,20.9657697603104,20.989817909062,21.0783723102708,21.1668119977757,
21.2551607727494,21.3469323071043,21.4351788414715,21.5234119594882,21.6116530273334,
21.6999234117745,21.7882941424499,21.8767243935656,21.9652848635004,21.9893330475888,
22.0778874482409,22.1663271351713,22.2546759095531,22.3464474441234,22.434693977859,
22.5229270952307,22.6111681624178,22.6994385461886,22.7878092761785,22.8762395265992,
22.96479999583,22.9888481861155,23.0774025880603,23.1658422763025,23.2541910520137,
23.3459625860922,23.4342091211927,23.5224422399398,23.6106833085118,23.6989536936755,
23.787324425063,23.8757546768859,23.9643151475147,23.9883633246423,24.0769177260085,
24.1653574136662,24.2537061887876,24.3454777230853,24.4337242575869,24.5219573757327,
24.6101984437018,24.6984688282613,24.7868395590461,24.8752698102663,24.9638302802972,
24.9878784631691,25.0764328645092,25.1648725521388,25.2532213272304,25.3449928615386,
25.4332393960058,25.5214725141157,25.6097135820472,25.6979839665675,25.7863546973111,
25.8747849484889,25.9633454184758,25.9873936016958,26.1024227289662,26.2150525142496,
26.2427863701391),.UNSPECIFIED.);
#7844=B_SPLINE_CURVE_WITH_KNOTS('',3,(#79824,#79825,#79826,#79827,#79828,
#79829,#79830,#79831,#79832,#79833),.UNSPECIFIED.,.F.,.F.,(4,1,1,1,1,1,
1,4),(26.2427864396301,26.9869087402226,27.9864238787494,28.9859390172761,
29.9854541558029,30.9849692943297,31.9844844328564,32.5259717468097),
 .UNSPECIFIED.);
#7845=B_SPLINE_CURVE_WITH_KNOTS('',3,(#79835,#79836,#79837,#79838,#79839,
#79840,#79841,#79842,#79843,#79844,#79845,#79846,#79847,#79848,#79849,#79850,
#79851,#79852,#79853,#79854,#79855,#79856,#79857,#79858,#79859,#79860,#79861,
#79862,#79863,#79864,#79865,#79866,#79867,#79868,#79869,#79870,#79871,#79872,
#79873,#79874,#79875,#79876,#79877,#79878,#79879,#79880,#79881,#79882,#79883,
#79884,#79885,#79886,#79887,#79888,#79889,#79890,#79891,#79892,#79893,#79894,
#79895,#79896,#79897,#79898,#79899,#79900,#79901,#79902,#79903,#79904,#79905,
#79906,#79907,#79908,#79909,#79910,#79911,#79912,#79913,#79914,#79915,#79916,
#79917,#79918,#79919,#79920,#79921,#79922,#79923,#79924,#79925,#79926,#79927,
#79928,#79929,#79930,#79931,#79932,#79933,#79934,#79935,#79936,#79937,#79938,
#79939,#79940,#79941,#79942,#79943,#79944,#79945,#79946,#79947,#79948,#79949,
#79950,#79951,#79952,#79953,#79954,#79955,#79956,#79957,#79958,#79959,#79960,
#79961,#79962,#79963,#79964,#79965,#79966,#79967,#79968,#79969,#79970,#79971,
#79972,#79973,#79974,#79975,#79976,#79977,#79978,#79979,#79980,#79981,#79982,
#79983,#79984,#79985,#79986,#79987,#79988,#79989,#79990,#79991,#79992,#79993,
#79994,#79995,#79996,#79997,#79998,#79999,#80000,#80001,#80002,#80003,#80004,
#80005,#80006,#80007,#80008,#80009,#80010,#80011,#80012,#80013,#80014,#80015,
#80016,#80017,#80018,#80019,#80020,#80021,#80022,#80023,#80024,#80025,#80026,
#80027,#80028,#80029,#80030,#80031,#80032,#80033,#80034,#80035,#80036,#80037,
#80038,#80039,#80040,#80041,#80042,#80043,#80044,#80045,#80046,#80047,#80048,
#80049,#80050,#80051,#80052,#80053,#80054,#80055,#80056,#80057,#80058,#80059,
#80060),.UNSPECIFIED.,.F.,.F.,(4,3,3,3,3,3,3,3,3,3,3,3,3,3,3,3,3,3,3,3,
3,3,3,3,3,3,3,3,3,3,3,3,3,3,3,3,3,3,3,3,3,3,3,3,3,3,3,3,3,3,3,3,3,3,3,3,
3,3,3,3,3,3,3,3,3,3,3,3,3,3,3,3,3,3,3,4),(32.525971971786,32.6201758608884,
32.7147113282288,32.8094143342101,32.9044060802361,32.9839995713832,33.0725539728206,
33.1609936605494,33.2493424357416,33.3411139700126,33.4293605045839,33.517593622799,
33.6058346908367,33.6941050754642,33.7824758063156,33.8709060576017,33.959466527697,
33.9835147099099,34.0720691113478,34.160508799077,34.2488575742697,34.3406291085406,
34.4288756431123,34.5171087613279,34.605349829366,34.6936202139939,34.7819909448457,
34.8704211961323,34.958981666228,34.9830298484367,35.0715842498749,35.1600239376044,
35.2483727127975,35.3401442470682,35.4283907816403,35.5166238998561,35.6048649678946,
35.6931353525228,35.781506083375,35.8699363346619,35.958496804758,35.9825449869634,
36.0710993884013,36.1595390761305,36.2478878513232,36.3396593855941,36.4279059201658,
36.5161390383814,36.6043801064195,36.6926504910474,36.7810212218993,36.8694514731859,
36.9580119432816,36.9820601254902,37.0706145269282,37.1590542146575,37.2474029898504,
37.3391745241212,37.4274210586931,37.5156541769087,37.603895244947,37.6921656295751,
37.7805363604271,37.8689666117138,37.9575270818097,37.981575264017,38.0688080689725,
38.1559267275216,38.2429457173611,38.3299097067977,38.4168412476983,38.5037628572331,
38.5907342193606,38.6777330343992,38.7648291874566,38.8091570539893),
 .UNSPECIFIED.);
#7846=B_SPLINE_CURVE_WITH_KNOTS('',3,(#80062,#80063,#80064,#80065,#80066,
#80067,#80068,#80069,#80070,#80071,#80072),.UNSPECIFIED.,.F.,.F.,(4,1,1,
1,1,1,1,1,4),(38.8091570539893,38.9810904025437,39.9806055410705,40.9801206795973,
41.979635818124,42.9791509566508,43.9786660951776,44.9781812337044,45.0923423611689),
 .UNSPECIFIED.);
#7847=B_SPLINE_CURVE_WITH_KNOTS('',3,(#80074,#80075,#80076,#80077,#80078,
#80079,#80080,#80081,#80082,#80083,#80084,#80085,#80086,#80087,#80088,#80089,
#80090,#80091,#80092,#80093,#80094,#80095,#80096,#80097,#80098,#80099,#80100,
#80101,#80102,#80103,#80104,#80105,#80106,#80107,#80108,#80109,#80110,#80111,
#80112,#80113,#80114,#80115,#80116,#80117,#80118,#80119,#80120,#80121,#80122,
#80123,#80124,#80125,#80126,#80127,#80128,#80129,#80130,#80131,#80132,#80133,
#80134,#80135,#80136,#80137,#80138,#80139,#80140,#80141,#80142,#80143,#80144,
#80145,#80146,#80147,#80148,#80149,#80150,#80151,#80152,#80153,#80154,#80155,
#80156,#80157,#80158,#80159,#80160,#80161,#80162,#80163,#80164,#80165,#80166,
#80167,#80168,#80169,#80170,#80171,#80172,#80173,#80174,#80175,#80176,#80177,
#80178,#80179,#80180,#80181,#80182,#80183,#80184,#80185,#80186,#80187,#80188,
#80189,#80190,#80191,#80192,#80193,#80194,#80195,#80196,#80197,#80198,#80199,
#80200,#80201,#80202,#80203,#80204,#80205,#80206,#80207,#80208,#80209,#80210,
#80211,#80212,#80213,#80214,#80215,#80216,#80217,#80218,#80219,#80220,#80221,
#80222,#80223,#80224,#80225,#80226,#80227,#80228,#80229,#80230,#80231,#80232,
#80233,#80234,#80235,#80236,#80237,#80238,#80239,#80240,#80241,#80242,#80243,
#80244,#80245,#80246,#80247,#80248,#80249,#80250,#80251,#80252,#80253,#80254,
#80255,#80256,#80257,#80258,#80259,#80260,#80261,#80262,#80263,#80264,#80265,
#80266,#80267,#80268,#80269,#80270,#80271,#80272,#80273,#80274,#80275,#80276,
#80277,#80278,#80279,#80280,#80281,#80282,#80283,#80284,#80285,#80286,#80287,
#80288,#80289,#80290,#80291,#80292,#80293,#80294,#80295,#80296),
 .UNSPECIFIED.,.F.,.F.,(4,3,3,3,3,3,3,3,3,3,3,3,3,3,3,3,3,3,3,3,3,3,3,3,
3,3,3,3,3,3,3,3,3,3,3,3,3,3,3,3,3,3,3,3,3,3,3,3,3,3,3,3,3,3,3,3,3,3,3,3,
3,3,3,3,3,3,3,3,3,3,3,3,3,3,4),(45.0923423611689,45.1796430982707,45.2668439792167,
45.3557005283435,45.442782837144,45.5298464622534,45.6169138198322,45.7071094579319,
45.7943002142326,45.8859982932319,45.9776963722311,46.0662507736692,46.1546904613985,
46.2430392365914,46.3348107708622,46.4230573054341,46.5112904236498,46.599531491688,
46.6878018763162,46.7761726071682,46.8646028584548,46.9531633285507,46.9772115107579,
47.065765912196,47.1542055999253,47.242554375118,47.3343259093888,47.4225724439607,
47.5108055621764,47.5990466302145,47.6873170148423,47.7756877456943,47.8641179969809,
47.9526784670765,47.9767266492846,48.0652810507226,48.1537207384518,48.2420695136444,
48.3338410479152,48.4220875824871,48.5103207007027,48.598561768741,48.6868321533692,
48.7752028842212,48.8636331355078,48.9521936056038,48.9762417878114,49.0647961892494,
49.1532358769787,49.2415846521716,49.3333561864424,49.4216027210143,49.50983583923,
49.5980769072683,49.686347291896,49.7747180227479,49.863148274035,49.9517087441309,
49.9757569263381,50.064311327776,50.1527510155053,50.2410997906977,50.3328713249686,
50.4211178595405,50.5093509777562,50.5975920457948,50.6858624304227,50.7742331612748,
50.8626634125615,50.9512238826574,50.9752720648649,51.0753359098083,51.1734347141415,
51.27448107939,51.3755274446384),.UNSPECIFIED.);
#7848=B_SPLINE_CURVE_WITH_KNOTS('',3,(#80298,#80299,#80300,#80301,#80302,
#80303,#80304,#80305,#80306,#80307),.UNSPECIFIED.,.F.,.F.,(4,1,1,1,1,1,
1,4),(51.3755276683485,51.9747872033916,52.9743023419184,53.9738174804452,
54.973332618972,55.9728477574987,56.9723628960255,57.6587129755281),
 .UNSPECIFIED.);
#7849=B_SPLINE_CURVE_WITH_KNOTS('',3,(#80309,#80310,#80311,#80312,#80313,
#80314,#80315,#80316,#80317,#80318,#80319,#80320,#80321,#80322,#80323,#80324,
#80325,#80326,#80327,#80328,#80329,#80330,#80331,#80332,#80333,#80334,#80335,
#80336,#80337,#80338,#80339,#80340,#80341,#80342,#80343,#80344,#80345,#80346,
#80347,#80348,#80349,#80350,#80351,#80352,#80353,#80354,#80355,#80356,#80357,
#80358,#80359,#80360,#80361,#80362,#80363,#80364,#80365,#80366,#80367,#80368,
#80369,#80370,#80371,#80372,#80373,#80374,#80375,#80376,#80377,#80378,#80379,
#80380,#80381,#80382,#80383,#80384,#80385,#80386,#80387,#80388,#80389,#80390,
#80391,#80392,#80393,#80394,#80395,#80396,#80397,#80398,#80399,#80400,#80401,
#80402,#80403,#80404,#80405,#80406,#80407,#80408,#80409,#80410,#80411,#80412,
#80413,#80414,#80415,#80416,#80417,#80418,#80419,#80420,#80421,#80422,#80423,
#80424,#80425,#80426,#80427,#80428,#80429,#80430,#80431,#80432,#80433,#80434,
#80435,#80436,#80437,#80438,#80439,#80440,#80441,#80442,#80443,#80444,#80445,
#80446,#80447,#80448,#80449,#80450,#80451,#80452,#80453,#80454,#80455,#80456,
#80457,#80458,#80459,#80460,#80461,#80462,#80463,#80464,#80465,#80466,#80467,
#80468,#80469,#80470,#80471,#80472,#80473,#80474,#80475,#80476,#80477,#80478,
#80479,#80480,#80481,#80482,#80483,#80484,#80485,#80486,#80487,#80488,#80489,
#80490,#80491,#80492,#80493,#80494,#80495,#80496,#80497,#80498,#80499,#80500,
#80501,#80502,#80503,#80504,#80505,#80506,#80507,#80508,#80509,#80510,#80511,
#80512,#80513,#80514,#80515,#80516,#80517,#80518,#80519,#80520,#80521,#80522,
#80523,#80524,#80525,#80526,#80527,#80528,#80529,#80530,#80531),
 .UNSPECIFIED.,.F.,.F.,(4,3,3,3,3,3,3,3,3,3,3,3,3,3,3,3,3,3,3,3,3,3,3,3,
3,3,3,3,3,3,3,3,3,3,3,3,3,3,3,3,3,3,3,3,3,3,3,3,3,3,3,3,3,3,3,3,3,3,3,3,
3,3,3,3,3,3,3,3,3,3,3,3,3,3,4),(57.6587131819983,57.7635561766369,57.8696480169293,
57.9718780345523,58.0604324359903,58.1488721237196,58.2372208989125,58.3289924331833,
58.4172389677552,58.5054720859708,58.5937131540089,58.681983538637,58.7703542694889,
58.8587845207756,58.9473449908714,58.971393173079,59.059947574517,59.1483872622463,
59.2367360374391,59.3285075717099,59.4167541062818,59.5049872244974,59.5932282925357,
59.6814986771637,59.7698694080157,59.8582996593024,59.9468601293982,59.9709083116058,
60.0594627130438,60.1479024007732,60.236251175966,60.3280227102368,60.4162692448087,
60.5045023630244,60.5927434310627,60.6810138156907,60.7693845465427,60.8578147978294,
60.9463752679252,60.9704234501326,61.0589778515706,61.1474175392999,61.2357663144927,
61.3275378487635,61.4157843833353,61.5040175015509,61.5922585695892,61.6805289542171,
61.7688996850691,61.8573299363557,61.9458904064515,61.9699385886593,62.0584929900973,
62.1469326778267,62.2352814530195,62.3270529872903,62.4152995218621,62.5035326400778,
62.5917737081161,62.6800440927442,62.7684148235962,62.8568450748829,62.9454055449787,
62.9694537271861,63.0576099768535,63.1456517950404,63.2336034379488,63.3221402935183,
63.409993392867,63.4978342680855,63.5856846894268,63.6747380876961,63.7627199693434,
63.8523091259238,63.9418982825042),.UNSPECIFIED.);
#7850=B_SPLINE_CURVE_WITH_KNOTS('',3,(#80533,#80534,#80535,#80536,#80537,
#80538,#80539,#80540,#80541,#80542,#80543,#80544,#80545,#80546,#80547,#80548,
#80549,#80550,#80551,#80552,#80553,#80554,#80555,#80556,#80557,#80558,#80559,
#80560,#80561,#80562,#80563,#80564,#80565,#80566,#80567,#80568,#80569,#80570,
#80571,#80572,#80573,#80574,#80575,#80576,#80577,#80578,#80579,#80580,#80581,
#80582,#80583,#80584,#80585,#80586,#80587,#80588,#80589,#80590,#80591,#80592,
#80593,#80594,#80595,#80596,#80597,#80598,#80599,#80600,#80601,#80602,#80603,
#80604,#80605,#80606,#80607,#80608,#80609,#80610,#80611,#80612,#80613,#80614,
#80615,#80616,#80617,#80618,#80619,#80620,#80621,#80622,#80623,#80624,#80625,
#80626,#80627,#80628,#80629,#80630,#80631,#80632,#80633,#80634,#80635,#80636,
#80637,#80638,#80639,#80640,#80641,#80642,#80643,#80644,#80645,#80646,#80647,
#80648,#80649,#80650,#80651,#80652,#80653,#80654,#80655,#80656,#80657,#80658,
#80659,#80660,#80661,#80662,#80663,#80664,#80665,#80666,#80667,#80668,#80669,
#80670,#80671,#80672,#80673,#80674,#80675,#80676,#80677,#80678,#80679,#80680,
#80681,#80682,#80683,#80684,#80685,#80686,#80687,#80688,#80689,#80690,#80691,
#80692,#80693,#80694,#80695,#80696,#80697,#80698,#80699,#80700,#80701,#80702,
#80703,#80704,#80705,#80706,#80707,#80708,#80709,#80710,#80711,#80712,#80713,
#80714,#80715,#80716,#80717,#80718,#80719,#80720,#80721,#80722,#80723,#80724,
#80725,#80726,#80727,#80728,#80729,#80730,#80731,#80732,#80733,#80734,#80735,
#80736,#80737,#80738,#80739,#80740,#80741,#80742,#80743,#80744,#80745,#80746,
#80747,#80748,#80749,#80750,#80751,#80752,#80753,#80754,#80755,#80756,#80757,
#80758,#80759,#80760,#80761),.UNSPECIFIED.,.F.,.F.,(4,3,3,3,3,3,3,3,3,3,
3,3,3,3,3,3,3,3,3,3,3,3,3,3,3,3,3,3,3,3,3,3,3,3,3,3,3,3,3,3,3,3,3,3,3,3,
3,3,3,3,3,3,3,3,3,3,3,3,3,3,3,3,3,3,3,3,3,3,3,3,3,3,3,3,3,3,4),(63.9418982827076,
63.9689688657128,64.0575232671507,64.1459629548799,64.2343117300728,64.3260832643437,
64.4143297989155,64.5025629171311,64.5908039851692,64.6790743697972,64.7674451006491,
64.8558753519356,64.9444358220313,64.9684840042396,65.0570384056776,65.1454780934069,
65.2338268685997,65.3255984028705,65.4138449374424,65.502078055658,65.5903191236962,
65.6785895083243,65.7669602391763,65.8553904904629,65.9439509605588,65.9679991427663,
66.0565535442043,66.1449932319336,66.2333420071265,66.3251135413973,66.4133600759691,
66.5015931941848,66.5898342622231,66.6781046468511,66.766475377703,66.8549056289897,
66.9434660990856,66.9675142812931,67.0560686827311,67.1445083704604,67.2328571456533,
67.3246286799241,67.412875214496,67.5011083327116,67.5893494007499,67.6776197853779,
67.7659905162299,67.8544207675166,67.9429812376125,67.9670294198199,68.0555838212579,
68.1440235089871,68.2323722841799,68.3241438184508,68.4123903530226,68.5006234712382,
68.5888645392764,68.6771349239043,68.7655056547563,68.8539359060429,68.9424963761388,
68.9665445583466,69.0550989597846,69.143538647514,69.2318874227069,69.3236589569777,
69.4119054915496,69.5001386097652,69.5883796778035,69.6766500624318,69.7650207932838,
69.8534510445703,69.9420115146663,69.9660596968734,70.0804033841329,70.1924681488945,
70.2250835097423),.UNSPECIFIED.);
#7851=B_SPLINE_CURVE_WITH_KNOTS('',3,(#80763,#80764,#80765,#80766,#80767,
#80768,#80769,#80770,#80771,#80772),.UNSPECIFIED.,.F.,.F.,(4,1,1,1,1,1,
1,4),(70.2250835898872,70.9655748354001,71.9650899739269,72.9646051124537,
73.9641202509804,74.9636353895072,75.9631505280339,76.5082688970668),
 .UNSPECIFIED.);
#7852=B_SPLINE_CURVE_WITH_KNOTS('',3,(#80774,#80775,#80776,#80777,#80778,
#80779,#80780,#80781,#80782,#80783,#80784,#80785,#80786,#80787,#80788,#80789,
#80790,#80791,#80792,#80793,#80794,#80795,#80796,#80797,#80798,#80799,#80800,
#80801,#80802,#80803,#80804,#80805,#80806,#80807,#80808,#80809,#80810,#80811,
#80812,#80813,#80814,#80815,#80816,#80817,#80818,#80819,#80820,#80821,#80822,
#80823,#80824,#80825,#80826,#80827,#80828,#80829,#80830,#80831,#80832,#80833,
#80834,#80835,#80836,#80837,#80838,#80839,#80840,#80841,#80842,#80843,#80844,
#80845,#80846,#80847,#80848,#80849,#80850,#80851,#80852,#80853,#80854,#80855,
#80856,#80857,#80858,#80859,#80860,#80861,#80862,#80863,#80864,#80865,#80866,
#80867,#80868,#80869,#80870,#80871,#80872,#80873,#80874,#80875,#80876,#80877,
#80878,#80879,#80880,#80881,#80882,#80883,#80884,#80885,#80886,#80887,#80888,
#80889,#80890,#80891,#80892,#80893,#80894,#80895,#80896,#80897,#80898,#80899,
#80900,#80901,#80902,#80903,#80904,#80905,#80906,#80907,#80908,#80909,#80910,
#80911,#80912,#80913,#80914,#80915,#80916,#80917,#80918,#80919,#80920,#80921,
#80922,#80923,#80924,#80925,#80926,#80927,#80928,#80929,#80930,#80931,#80932,
#80933,#80934,#80935,#80936,#80937,#80938,#80939,#80940,#80941,#80942,#80943,
#80944,#80945,#80946,#80947,#80948,#80949,#80950,#80951,#80952,#80953,#80954,
#80955,#80956,#80957,#80958,#80959,#80960,#80961,#80962,#80963,#80964,#80965,
#80966,#80967,#80968,#80969,#80970,#80971,#80972,#80973,#80974,#80975,#80976,
#80977,#80978,#80979,#80980,#80981,#80982,#80983,#80984,#80985,#80986,#80987,
#80988,#80989,#80990,#80991,#80992,#80993,#80994,#80995,#80996,#80997,#80998,
#80999),.UNSPECIFIED.,.F.,.F.,(4,3,3,3,3,3,3,3,3,3,3,3,3,3,3,3,3,3,3,3,
3,3,3,3,3,3,3,3,3,3,3,3,3,3,3,3,3,3,3,3,3,3,3,3,3,3,3,3,3,3,3,3,3,3,3,3,
3,3,3,3,3,3,3,3,3,3,3,3,3,3,3,3,3,3,3,4),(76.5082691399735,76.6026454255836,
76.697363068653,76.7922538820692,76.8874364963458,76.9626656665607,77.0512200679987,
77.1396597557281,77.2280085309208,77.3197800651916,77.4080265997635,77.4962597179792,
77.5845007860174,77.6727711706453,77.7611419014973,77.8495721527841,77.9381326228799,
77.9621808050875,78.0507352065255,78.1391748942548,78.2275236694476,78.3192952037184,
78.4075417382902,78.4957748565058,78.584015924544,78.672286309172,78.760657040024,
78.8490872913106,78.9376477614065,78.9616959436142,79.0502503450522,79.1386900327815,
79.2270388079743,79.3188103422452,79.407056876817,79.4952899950327,79.5835310630709,
79.6718014476989,79.7601721785509,79.8486024298375,79.9371628999333,79.961211082141,
80.049765483579,80.1382051713083,80.2265539465012,80.318325480772,80.4065720153439,
80.4948051335595,80.5830462015978,80.6713165862258,80.7596873170778,80.8481175683645,
80.9366780384603,80.9607262206678,81.0492806221058,81.1377203098352,81.2260690850281,
81.3178406192989,81.4060871538708,81.4943202720864,81.5825613401247,81.6708317247528,
81.7592024556047,81.8476327068913,81.9361931769871,81.9602413591946,82.0474735219598,
82.1345915975361,82.2216101893339,82.3085738643474,82.3955051745341,82.482426637279,
82.5693987263293,82.6563983044652,82.7434972344772,82.7914542042464),
 .UNSPECIFIED.);
#7853=B_SPLINE_CURVE_WITH_KNOTS('',3,(#81001,#81002,#81003,#81004,#81005,
#81006,#81007,#81008,#81009,#81010,#81011),.UNSPECIFIED.,.F.,.F.,(4,1,1,
1,1,1,1,1,4),(82.7914542042464,82.9597564977213,83.9592716362481,84.9587867747749,
85.9583019133016,86.9578170518284,87.9573321903551,88.9568473288819,89.074639511426),
 .UNSPECIFIED.);
#7854=B_SPLINE_CURVE_WITH_KNOTS('',3,(#81013,#81014,#81015,#81016,#81017,
#81018,#81019,#81020,#81021,#81022,#81023,#81024,#81025,#81026,#81027,#81028,
#81029,#81030,#81031,#81032,#81033,#81034,#81035,#81036,#81037,#81038,#81039,
#81040,#81041,#81042,#81043,#81044,#81045,#81046,#81047,#81048,#81049,#81050,
#81051,#81052,#81053,#81054,#81055,#81056,#81057,#81058,#81059,#81060,#81061,
#81062,#81063,#81064,#81065,#81066,#81067,#81068,#81069,#81070,#81071,#81072,
#81073,#81074,#81075,#81076,#81077,#81078,#81079,#81080,#81081,#81082,#81083,
#81084,#81085,#81086,#81087,#81088,#81089,#81090,#81091,#81092,#81093,#81094,
#81095,#81096,#81097,#81098,#81099,#81100,#81101,#81102,#81103,#81104,#81105,
#81106,#81107,#81108,#81109,#81110,#81111,#81112,#81113,#81114,#81115,#81116,
#81117,#81118,#81119,#81120,#81121,#81122,#81123,#81124,#81125,#81126,#81127,
#81128,#81129,#81130,#81131,#81132,#81133,#81134,#81135,#81136,#81137,#81138,
#81139,#81140,#81141,#81142,#81143,#81144,#81145,#81146,#81147,#81148,#81149,
#81150,#81151,#81152,#81153,#81154,#81155,#81156,#81157,#81158,#81159,#81160,
#81161,#81162,#81163,#81164,#81165,#81166,#81167,#81168,#81169,#81170,#81171,
#81172,#81173,#81174,#81175,#81176,#81177,#81178,#81179,#81180,#81181,#81182,
#81183,#81184,#81185,#81186,#81187,#81188,#81189,#81190,#81191,#81192,#81193,
#81194,#81195,#81196,#81197,#81198,#81199,#81200,#81201,#81202,#81203,#81204,
#81205,#81206,#81207,#81208,#81209,#81210,#81211,#81212,#81213,#81214,#81215,
#81216,#81217,#81218,#81219,#81220,#81221,#81222,#81223,#81224,#81225,#81226,
#81227,#81228,#81229,#81230,#81231,#81232,#81233,#81234,#81235,#81236,#81237,
#81238),.UNSPECIFIED.,.F.,.F.,(4,3,3,3,3,3,3,3,3,3,3,3,3,3,3,3,3,3,3,3,
3,3,3,3,3,3,3,3,3,3,3,3,3,3,3,3,3,3,3,3,3,3,3,3,3,3,3,3,3,3,3,3,3,3,3,3,
3,3,3,3,3,3,3,3,3,3,3,3,3,3,3,3,3,3,3,4),(89.074639511426,89.1619192926847,
89.2491000317712,89.3375078362259,89.4245720601888,89.5116182563224,89.5986688526275,
89.6880922563228,89.7752668003224,89.8658146338655,89.9563624674086,90.0449168688466,
90.133356556576,90.2217053317688,90.3134768660396,90.4017234006115,90.4899565188271,
90.5781975868654,90.6664679714935,90.7548387023455,90.8432689536321,90.9318294237279,
90.9558776059354,91.0444320073733,91.1328716951027,91.2212204702956,91.3129920045664,
91.4012385391384,91.489471657354,91.5777127253922,91.6659831100203,91.7543538408723,
91.842784092159,91.9313445622549,91.9553927444622,92.0439471459002,92.1323868336295,
92.2207356088222,92.312507143093,92.4007536776648,92.4889867958805,92.5772278639185,
92.6654982485467,92.7538689793986,92.8422992306851,92.9308597007809,92.9549078829889,
93.0434622844269,93.1319019721563,93.2202507473492,93.31202228162,93.4002688161919,
93.4885019344076,93.5767430024456,93.6650133870734,93.7533841179253,93.8418143692118,
93.9303748393076,93.9544230215157,94.0429774229538,94.1314171106833,94.2197658858762,
94.311537420147,94.3997839547188,94.4880170729345,94.5762581409729,94.6645285256012,
94.7528992564532,94.8413295077404,94.9298899778364,94.9539381600425,95.0549097698975,
95.1527638742767,95.2552942368696,95.3524272501556,95.3578245994625),
 .UNSPECIFIED.);
#7855=B_SPLINE_CURVE_WITH_KNOTS('',3,(#81240,#81241,#81242,#81243,#81244,
#81245,#81246,#81247,#81248,#81249),.UNSPECIFIED.,.F.,.F.,(4,1,1,1,1,1,
1,4),(95.3578248186056,95.9534532985692,96.952968437096,97.9524835756227,
98.9519987141495,99.9515138526763,100.951028991203,101.641010125785),
 .UNSPECIFIED.);
#7856=B_SPLINE_CURVE_WITH_KNOTS('',3,(#81251,#81252,#81253,#81254,#81255,
#81256,#81257,#81258,#81259,#81260,#81261,#81262,#81263,#81264,#81265,#81266,
#81267,#81268,#81269,#81270,#81271,#81272,#81273,#81274,#81275,#81276,#81277,
#81278,#81279,#81280,#81281,#81282,#81283,#81284,#81285,#81286,#81287,#81288,
#81289,#81290,#81291,#81292,#81293,#81294,#81295,#81296,#81297,#81298,#81299,
#81300,#81301,#81302,#81303,#81304,#81305,#81306,#81307,#81308,#81309,#81310,
#81311,#81312,#81313,#81314,#81315,#81316,#81317,#81318,#81319,#81320,#81321,
#81322,#81323,#81324,#81325,#81326,#81327,#81328,#81329,#81330,#81331,#81332,
#81333,#81334,#81335,#81336,#81337,#81338,#81339,#81340,#81341,#81342,#81343,
#81344,#81345,#81346,#81347,#81348,#81349,#81350,#81351,#81352,#81353,#81354,
#81355,#81356,#81357,#81358,#81359,#81360,#81361,#81362,#81363,#81364,#81365,
#81366,#81367,#81368,#81369,#81370,#81371,#81372,#81373,#81374,#81375,#81376,
#81377,#81378,#81379,#81380,#81381,#81382,#81383,#81384,#81385,#81386,#81387,
#81388,#81389,#81390,#81391,#81392,#81393,#81394,#81395,#81396,#81397,#81398,
#81399,#81400,#81401,#81402,#81403,#81404,#81405,#81406,#81407,#81408,#81409,
#81410,#81411,#81412,#81413,#81414,#81415,#81416,#81417,#81418,#81419,#81420,
#81421,#81422,#81423,#81424,#81425,#81426,#81427,#81428,#81429,#81430,#81431,
#81432,#81433,#81434,#81435,#81436,#81437,#81438,#81439,#81440,#81441,#81442,
#81443,#81444,#81445,#81446,#81447,#81448,#81449,#81450,#81451,#81452,#81453,
#81454,#81455,#81456,#81457,#81458,#81459,#81460,#81461,#81462,#81463,#81464,
#81465,#81466,#81467,#81468,#81469,#81470,#81471,#81472,#81473),
 .UNSPECIFIED.,.F.,.F.,(4,3,3,3,3,3,3,3,3,3,3,3,3,3,3,3,3,3,3,3,3,3,3,3,
3,3,3,3,3,3,3,3,3,3,3,3,3,3,3,3,3,3,3,3,3,3,3,3,3,3,3,3,3,3,3,3,3,3,3,3,
3,3,3,3,3,3,3,3,3,3,3,3,3,3,4),(101.641010326215,101.746247243759,101.852779011131,
101.95054412973,102.039098531168,102.127538218897,102.21588699409,102.307658528361,
102.395905062932,102.484138181148,102.572379249186,102.660649633814,102.749020364665,
102.837450615952,102.926011086048,102.950059268257,103.038613669695,103.127053357424,
103.215402132616,103.307173666887,103.395420201459,103.483653319674,103.571894387712,
103.66016477234,103.748535503192,103.836965754478,103.925526224574,103.949574406783,
104.038128808221,104.12656849595,104.214917271143,104.306688805414,104.394935339986,
104.483168458202,104.57140952624,104.659679910868,104.74805064172,104.836480893007,
104.925041363102,104.94908954531,105.037643946748,105.126083634478,105.21443240967,
105.306203943941,105.394450478513,105.482683596729,105.570924664767,105.659195049395,
105.747565780248,105.835996031534,105.92455650163,105.948604683837,106.037159085275,
106.125598773004,106.213947548197,106.305719082468,106.39396561704,106.482198735256,
106.570439803294,106.658710187922,106.747080918774,106.83551117006,106.924071640156,
106.948119822364,107.036325090243,107.124415885493,107.212416411561,107.301388789214,
107.389290338596,107.477179538862,107.565078113673,107.654857443451,107.742887885958,
107.833541659372,107.924195432786),.UNSPECIFIED.);
#7857=B_SPLINE_CURVE_WITH_KNOTS('',3,(#81475,#81476,#81477,#81478,#81479,
#81480,#81481,#81482,#81483,#81484,#81485,#81486,#81487,#81488,#81489,#81490,
#81491,#81492,#81493,#81494,#81495,#81496,#81497,#81498,#81499,#81500,#81501,
#81502,#81503,#81504,#81505,#81506,#81507,#81508,#81509,#81510,#81511,#81512,
#81513,#81514,#81515,#81516,#81517,#81518,#81519,#81520,#81521,#81522,#81523,
#81524,#81525,#81526,#81527,#81528,#81529,#81530,#81531,#81532,#81533,#81534,
#81535,#81536,#81537,#81538,#81539,#81540,#81541,#81542,#81543,#81544,#81545,
#81546,#81547,#81548,#81549,#81550,#81551,#81552,#81553,#81554,#81555,#81556,
#81557,#81558,#81559,#81560,#81561,#81562,#81563,#81564,#81565,#81566,#81567,
#81568,#81569,#81570,#81571,#81572,#81573,#81574,#81575,#81576,#81577,#81578,
#81579,#81580,#81581,#81582,#81583,#81584,#81585,#81586,#81587,#81588,#81589,
#81590,#81591,#81592,#81593,#81594,#81595,#81596,#81597,#81598,#81599,#81600,
#81601,#81602,#81603,#81604,#81605,#81606,#81607,#81608,#81609,#81610,#81611,
#81612,#81613,#81614,#81615,#81616,#81617,#81618,#81619,#81620,#81621,#81622,
#81623,#81624,#81625,#81626,#81627,#81628,#81629,#81630,#81631,#81632,#81633,
#81634,#81635,#81636,#81637,#81638,#81639,#81640,#81641,#81642,#81643,#81644,
#81645,#81646,#81647,#81648,#81649,#81650,#81651,#81652,#81653,#81654,#81655,
#81656,#81657,#81658,#81659,#81660,#81661,#81662,#81663,#81664,#81665,#81666,
#81667,#81668,#81669,#81670,#81671,#81672,#81673,#81674,#81675,#81676,#81677,
#81678,#81679,#81680,#81681,#81682,#81683,#81684,#81685,#81686,#81687,#81688,
#81689,#81690,#81691,#81692,#81693,#81694,#81695,#81696,#81697,#81698,#81699,
#81700,#81701,#81702,#81703),.UNSPECIFIED.,.F.,.F.,(4,3,3,3,3,3,3,3,3,3,
3,3,3,3,3,3,3,3,3,3,3,3,3,3,3,3,3,3,3,3,3,3,3,3,3,3,3,3,3,3,3,3,3,3,3,3,
3,3,3,3,3,3,3,3,3,3,3,3,3,3,3,3,3,3,3,3,3,3,3,3,3,3,3,3,3,3,4),(107.924195432965,
107.94763496089,108.036189362328,108.124629050057,108.21297782525,108.304749359521,
108.392995894093,108.481229012309,108.569470080347,108.657740464975,108.746111195827,
108.834541447114,108.92310191721,108.947150099417,109.035704500855,109.124144188584,
109.212492963777,109.304264498048,109.39251103262,109.480744150836,109.568985218874,
109.657255603502,109.745626334354,109.834056585641,109.922617055736,109.946665237944,
110.035219639382,110.123659327112,110.212008102304,110.303779636575,110.392026171147,
110.480259289363,110.568500357401,110.65677074203,110.745141472882,110.833571724168,
110.922132194264,110.946180376471,111.034734777909,111.123174465638,111.21152324083,
111.303294775101,111.391541309673,111.479774427888,111.568015495926,111.656285880554,
111.744656611406,111.833086862692,111.921647332788,111.945695514997,112.034249916435,
112.122689604164,112.211038379357,112.302809913628,112.3910564482,112.479289566415,
112.567530634454,112.655801019082,112.744171749934,112.83260200122,112.921162471316,
112.945210653524,113.033765054962,113.122204742692,113.210553517885,113.302325052156,
113.390571586728,113.478804704944,113.567045772982,113.65531615761,113.743686888462,
113.832117139749,113.920677609846,113.944725792051,114.058407016934,114.16992096901,
114.207380649555),.UNSPECIFIED.);
#7858=B_SPLINE_CURVE_WITH_KNOTS('',3,(#81705,#81706,#81707,#81708,#81709,
#81710,#81711,#81712,#81713,#81714),.UNSPECIFIED.,.F.,.F.,(4,1,1,1,1,1,
1,4),(114.207380740144,114.944240930578,115.943756069104,116.943271207631,
117.942786346158,118.942301484685,119.941816623212,120.490566047324),
 .UNSPECIFIED.);
#7859=B_SPLINE_CURVE_WITH_KNOTS('',3,(#81716,#81717,#81718,#81719,#81720,
#81721,#81722,#81723,#81724,#81725,#81726,#81727,#81728,#81729,#81730,#81731,
#81732,#81733,#81734,#81735,#81736,#81737,#81738,#81739,#81740,#81741,#81742,
#81743,#81744,#81745,#81746,#81747,#81748,#81749,#81750,#81751,#81752,#81753,
#81754,#81755,#81756,#81757,#81758,#81759,#81760,#81761,#81762,#81763,#81764,
#81765,#81766,#81767,#81768,#81769,#81770,#81771,#81772,#81773,#81774,#81775,
#81776,#81777,#81778,#81779,#81780,#81781,#81782,#81783,#81784,#81785,#81786,
#81787,#81788,#81789,#81790,#81791,#81792,#81793,#81794,#81795,#81796,#81797,
#81798,#81799,#81800,#81801,#81802,#81803,#81804,#81805,#81806,#81807,#81808,
#81809,#81810,#81811,#81812,#81813,#81814,#81815,#81816,#81817,#81818,#81819,
#81820,#81821,#81822,#81823,#81824,#81825,#81826,#81827,#81828,#81829,#81830,
#81831,#81832,#81833,#81834,#81835,#81836,#81837,#81838,#81839,#81840,#81841,
#81842,#81843,#81844,#81845,#81846,#81847,#81848,#81849,#81850,#81851,#81852,
#81853,#81854,#81855,#81856,#81857,#81858,#81859,#81860,#81861,#81862,#81863,
#81864,#81865,#81866,#81867,#81868,#81869,#81870,#81871,#81872,#81873,#81874,
#81875,#81876,#81877,#81878,#81879,#81880,#81881,#81882,#81883,#81884,#81885,
#81886,#81887,#81888,#81889,#81890,#81891,#81892,#81893,#81894,#81895,#81896,
#81897,#81898,#81899,#81900,#81901,#81902,#81903,#81904,#81905,#81906,#81907,
#81908,#81909,#81910,#81911,#81912,#81913,#81914,#81915,#81916,#81917,#81918,
#81919,#81920,#81921,#81922,#81923,#81924,#81925,#81926,#81927,#81928,#81929,
#81930,#81931,#81932,#81933,#81934,#81935,#81936,#81937,#81938,#81939,#81940,
#81941),.UNSPECIFIED.,.F.,.F.,(4,3,3,3,3,3,3,3,3,3,3,3,3,3,3,3,3,3,3,3,
3,3,3,3,3,3,3,3,3,3,3,3,3,3,3,3,3,3,3,3,3,3,3,3,3,3,3,3,3,3,3,3,3,3,3,3,
3,3,3,3,3,3,3,3,3,3,3,3,3,3,3,3,3,3,3,4),(120.490566307756,120.585118114269,
120.680021397524,120.775103661094,120.870480885623,120.941331761738,121.029886163176,
121.118325850906,121.206674626099,121.29844616037,121.386692694942,121.474925813157,
121.563166881196,121.651437265824,121.739807996676,121.828238247963,121.916798718059,
121.940846900265,122.029401301703,122.117840989432,122.206189764625,122.297961298896,
122.386207833468,122.474440951684,122.562682019722,122.65095240435,122.739323135202,
122.827753386489,122.916313856585,122.940362038792,123.02891644023,123.117356127959,
123.205704903152,123.297476437423,123.385722971995,123.473956090211,123.562197158249,
123.650467542877,123.738838273729,123.827268525016,123.915828995112,123.939877177319,
124.028431578757,124.116871266486,124.205220041679,124.296991575949,124.385238110521,
124.473471228737,124.561712296775,124.649982681402,124.738353412254,124.826783663541,
124.915344133636,124.939392315845,125.027946717283,125.116386405012,125.204735180205,
125.296506714476,125.384753249047,125.472986367263,125.561227435301,125.649497819929,
125.737868550781,125.826298802068,125.914859272163,125.938907454372,126.026140185572,
126.11325888379,126.20027827459,126.287242825609,126.374175088105,126.461097578889,
126.548071560608,126.63507305944,126.722175935449,126.773751354504),
 .UNSPECIFIED.);
#7860=B_SPLINE_CURVE_WITH_KNOTS('',3,(#81943,#81944,#81945,#81946,#81947,
#81948,#81949,#81950,#81951,#81952,#81953),.UNSPECIFIED.,.F.,.F.,(4,1,1,
1,1,1,1,1,4),(126.773751354504,126.938422592899,127.937937731426,128.937452869952,
129.936968008479,130.936483147006,131.935998285533,132.935513424059,133.056936661683),
 .UNSPECIFIED.);
#7861=B_SPLINE_CURVE_WITH_KNOTS('',3,(#81955,#81956,#81957,#81958,#81959,
#81960,#81961,#81962,#81963,#81964,#81965,#81966,#81967,#81968,#81969,#81970,
#81971,#81972,#81973,#81974,#81975,#81976,#81977,#81978,#81979,#81980,#81981,
#81982,#81983,#81984,#81985,#81986,#81987,#81988,#81989,#81990,#81991,#81992,
#81993,#81994,#81995,#81996,#81997,#81998,#81999,#82000,#82001,#82002,#82003,
#82004,#82005,#82006,#82007,#82008,#82009,#82010,#82011,#82012,#82013,#82014,
#82015,#82016,#82017,#82018,#82019,#82020,#82021,#82022,#82023,#82024,#82025,
#82026,#82027,#82028,#82029,#82030,#82031,#82032,#82033,#82034,#82035,#82036,
#82037,#82038,#82039,#82040,#82041,#82042,#82043,#82044,#82045,#82046,#82047,
#82048,#82049,#82050,#82051,#82052,#82053,#82054,#82055,#82056,#82057,#82058,
#82059,#82060,#82061,#82062,#82063,#82064,#82065,#82066,#82067,#82068,#82069,
#82070,#82071,#82072,#82073,#82074,#82075,#82076,#82077,#82078,#82079,#82080,
#82081,#82082,#82083,#82084,#82085,#82086,#82087,#82088,#82089,#82090,#82091,
#82092,#82093,#82094,#82095,#82096,#82097,#82098,#82099,#82100,#82101,#82102,
#82103,#82104,#82105,#82106,#82107,#82108,#82109,#82110,#82111,#82112,#82113,
#82114,#82115,#82116,#82117,#82118,#82119,#82120,#82121,#82122,#82123,#82124,
#82125,#82126,#82127,#82128,#82129,#82130,#82131,#82132,#82133,#82134,#82135,
#82136,#82137,#82138,#82139,#82140,#82141,#82142,#82143,#82144,#82145,#82146,
#82147,#82148,#82149,#82150,#82151,#82152,#82153,#82154,#82155,#82156,#82157,
#82158,#82159,#82160,#82161,#82162,#82163,#82164,#82165,#82166,#82167,#82168,
#82169,#82170,#82171,#82172,#82173,#82174,#82175,#82176,#82177,#82178,#82179,
#82180),.UNSPECIFIED.,.F.,.F.,(4,3,3,3,3,3,3,3,3,3,3,3,3,3,3,3,3,3,3,3,
3,3,3,3,3,3,3,3,3,3,3,3,3,3,3,3,3,3,3,3,3,3,3,3,3,3,3,3,3,3,3,3,3,3,3,3,
3,3,3,3,3,3,3,3,3,3,3,3,3,3,3,3,3,3,3,4),(133.056936661683,133.144196640644,
133.231358408055,133.319317177371,133.406364512018,133.493394486404,133.580429539472,
133.66907929525,133.75623885054,133.845633706563,133.935028562586,134.023582964024,
134.112022651753,134.200371426946,134.292142961217,134.380389495789,134.468622614005,
134.556863682043,134.645134066671,134.733504797523,134.821935048809,134.910495518905,
134.934543701113,135.023098102551,135.111537790281,135.199886565474,135.291658099744,
135.379904634316,135.468137752532,135.556378820571,135.644649205199,135.733019936051,
135.821450187337,135.910010657433,135.93405883964,136.022613241078,136.111052928807,
136.199401703999,136.29117323827,136.379419772842,136.467652891057,136.555893959095,
136.644164343723,136.732535074575,136.820965325861,136.909525795957,136.933573978166,
137.022128379604,137.110568067333,137.198916842526,137.290688376797,137.378934911368,
137.467168029584,137.555409097622,137.64367948225,137.732050213102,137.820480464389,
137.909040934484,137.933089116693,138.021643518131,138.110083205861,138.198431981054,
138.290203515325,138.378450049897,138.466683168112,138.554924236151,138.643194620779,
138.731565351631,138.819995602918,138.908556073014,138.93260425522,139.034483630081,
139.132097818871,139.229434282969,139.326360752829,139.340121754662),
 .UNSPECIFIED.);
#7862=B_SPLINE_CURVE_WITH_KNOTS('',3,(#82182,#82183,#82184,#82185,#82186,
#82187,#82188,#82189,#82190,#82191),.UNSPECIFIED.,.F.,.F.,(4,1,1,1,1,1,
1,4),(139.340121968863,139.932119393747,140.931634532274,141.9311496708,
142.930664809327,143.930179947854,144.929695086381,145.623307276042),
 .UNSPECIFIED.);
#7863=B_SPLINE_CURVE_WITH_KNOTS('',3,(#82193,#82194,#82195,#82196,#82197,
#82198,#82199,#82200,#82201,#82202,#82203,#82204,#82205,#82206,#82207,#82208,
#82209,#82210,#82211,#82212,#82213,#82214,#82215,#82216,#82217,#82218,#82219,
#82220,#82221,#82222,#82223,#82224,#82225,#82226,#82227,#82228,#82229,#82230,
#82231,#82232,#82233,#82234,#82235,#82236,#82237,#82238,#82239,#82240,#82241,
#82242,#82243,#82244,#82245,#82246,#82247,#82248,#82249,#82250,#82251,#82252,
#82253,#82254,#82255,#82256,#82257,#82258,#82259,#82260,#82261,#82262,#82263,
#82264,#82265,#82266,#82267,#82268,#82269,#82270,#82271,#82272,#82273,#82274,
#82275,#82276,#82277,#82278,#82279,#82280,#82281,#82282,#82283,#82284,#82285,
#82286,#82287,#82288,#82289,#82290,#82291,#82292,#82293,#82294,#82295,#82296,
#82297,#82298,#82299,#82300,#82301,#82302,#82303,#82304,#82305,#82306,#82307,
#82308,#82309,#82310,#82311,#82312,#82313,#82314,#82315,#82316,#82317,#82318,
#82319,#82320,#82321,#82322,#82323,#82324,#82325,#82326,#82327,#82328,#82329,
#82330,#82331,#82332,#82333,#82334,#82335,#82336,#82337,#82338,#82339,#82340,
#82341,#82342,#82343,#82344,#82345,#82346,#82347,#82348,#82349,#82350,#82351,
#82352,#82353,#82354,#82355,#82356,#82357,#82358,#82359,#82360,#82361,#82362,
#82363,#82364,#82365,#82366,#82367,#82368,#82369,#82370,#82371,#82372,#82373,
#82374,#82375,#82376,#82377,#82378,#82379,#82380,#82381,#82382,#82383,#82384,
#82385,#82386,#82387,#82388,#82389,#82390,#82391,#82392,#82393,#82394,#82395,
#82396,#82397,#82398,#82399,#82400,#82401,#82402,#82403,#82404,#82405,#82406,
#82407,#82408,#82409,#82410,#82411,#82412,#82413,#82414,#82415),
 .UNSPECIFIED.,.F.,.F.,(4,3,3,3,3,3,3,3,3,3,3,3,3,3,3,3,3,3,3,3,3,3,3,3,
3,3,3,3,3,3,3,3,3,3,3,3,3,3,3,3,3,3,3,3,3,3,3,3,3,3,3,3,3,3,3,3,3,3,3,3,
3,3,3,3,3,3,3,3,3,3,3,3,3,3,4),(145.623307470037,145.728947897427,145.835931712352,
145.929210224907,146.017764626345,146.106204314075,146.194553089268,146.286324623538,
146.37457115811,146.462804276326,146.551045344364,146.639315728992,146.727686459845,
146.816116711131,146.904677181227,146.928725363434,147.017279764872,147.105719452601,
147.194068227794,147.285839762065,147.374086296637,147.462319414853,147.550560482891,
147.638830867519,147.727201598371,147.815631849658,147.904192319754,147.928240501961,
148.016794903399,148.105234591128,148.193583366321,148.285354900592,148.373601435164,
148.46183455338,148.550075621418,148.638346006046,148.726716736898,148.815146988185,
148.903707458281,148.927755640488,149.016310041926,149.104749729655,149.193098504848,
149.284870039118,149.37311657369,149.461349691906,149.549590759944,149.637861144571,
149.726231875423,149.81466212671,149.903222596805,149.927270779014,150.015825180452,
150.104264868181,150.192613643374,150.284385177645,150.372631712217,150.460864830432,
150.549105898471,150.637376283099,150.72574701395,150.814177265237,150.902737735333,
150.926785917541,151.015041546976,151.103182663218,151.191233414591,151.28064081067,
151.368592133533,151.456530971977,151.5444790009,151.63498239648,151.723062649854,
151.814777616538,151.906492583222),.UNSPECIFIED.);
#7864=B_SPLINE_CURVE_WITH_KNOTS('',3,(#82417,#82418,#82419,#82420,#82421,
#82422,#82423,#82424,#82425,#82426,#82427,#82428),.UNSPECIFIED.,.F.,.F.,
(4,2,1,1,1,1,1,1,4),(151.906492583222,151.926301056068,152.925816194595,
153.925331333121,154.924846471648,155.924361610175,156.923876748702,157.923391887229,
158.189674734771),.UNSPECIFIED.);
#7865=B_SPLINE_CURVE_WITH_KNOTS('',3,(#82430,#82431,#82432,#82433,#82434,
#82435,#82436,#82437,#82438,#82439,#82440,#82441,#82442,#82443,#82444,#82445,
#82446,#82447,#82448,#82449,#82450,#82451,#82452,#82453,#82454,#82455,#82456,
#82457,#82458,#82459,#82460,#82461,#82462,#82463,#82464,#82465,#82466,#82467,
#82468,#82469,#82470,#82471,#82472,#82473,#82474,#82475,#82476,#82477,#82478,
#82479,#82480,#82481,#82482,#82483,#82484,#82485,#82486,#82487,#82488,#82489,
#82490,#82491,#82492,#82493,#82494,#82495,#82496,#82497,#82498,#82499,#82500,
#82501,#82502,#82503,#82504,#82505,#82506,#82507,#82508,#82509,#82510,#82511,
#82512,#82513,#82514,#82515,#82516,#82517,#82518,#82519,#82520,#82521,#82522,
#82523,#82524,#82525,#82526,#82527,#82528,#82529,#82530,#82531,#82532,#82533,
#82534,#82535,#82536,#82537,#82538,#82539,#82540,#82541,#82542,#82543,#82544,
#82545,#82546,#82547,#82548,#82549,#82550,#82551,#82552,#82553,#82554,#82555,
#82556,#82557,#82558,#82559,#82560,#82561,#82562,#82563,#82564,#82565,#82566,
#82567,#82568,#82569,#82570,#82571,#82572,#82573,#82574,#82575,#82576,#82577,
#82578,#82579,#82580,#82581,#82582,#82583,#82584,#82585,#82586,#82587,#82588,
#82589,#82590,#82591,#82592,#82593,#82594,#82595,#82596,#82597,#82598,#82599,
#82600,#82601,#82602,#82603,#82604,#82605,#82606,#82607,#82608,#82609,#82610,
#82611,#82612,#82613,#82614,#82615,#82616,#82617,#82618,#82619,#82620,#82621,
#82622,#82623,#82624,#82625,#82626,#82627,#82628,#82629,#82630,#82631,#82632,
#82633,#82634,#82635,#82636,#82637,#82638,#82639,#82640,#82641,#82642,#82643,
#82644,#82645,#82646,#82647,#82648,#82649,#82650,#82651,#82652,#82653,#82654,
#82655),.UNSPECIFIED.,.F.,.F.,(4,3,3,3,3,3,3,3,3,3,3,3,3,3,3,3,3,3,3,3,
3,3,3,3,3,3,3,3,3,3,3,3,3,3,3,3,3,3,3,3,3,3,3,3,3,3,3,3,3,3,3,3,3,3,3,3,
3,3,3,3,3,3,3,3,3,3,3,3,3,3,3,3,3,3,3,4),(158.189677890401,158.28133153232,
158.368710202749,158.456068790346,158.543429479056,158.630814450445,158.718295863631,
158.8058337789,158.893502610368,158.922907025755,159.011461427193,159.099901114922,
159.188249890115,159.280021424386,159.368267958958,159.456501077174,159.544742145212,
159.63301252984,159.721383260692,159.809813511979,159.898373982075,159.922422164282,
160.01097656572,160.09941625345,160.187765028642,160.279536562913,160.367783097485,
160.456016215701,160.544257283739,160.632527668367,160.720898399219,160.809328650506,
160.897889120601,160.921937302809,161.010491704247,161.098931391976,161.187280167169,
161.27905170144,161.367298236012,161.455531354228,161.543772422266,161.632042806894,
161.720413537746,161.808843789033,161.897404259129,161.921452441336,162.010006842774,
162.098446530503,162.186795305695,162.278566839966,162.366813374538,162.455046492753,
162.543287560791,162.631557945419,162.719928676271,162.808358927557,162.896919397653,
162.920967579862,163.0095219813,163.097961669029,163.186310444222,163.278081978493,
163.366328513065,163.45456163128,163.542802699318,163.631073083946,163.719443814798,
163.807874066084,163.89643453618,163.920482718389,164.01167483213,164.102725861115,
164.195260195231,164.286049488575,164.379456343078,164.472863197581),
 .UNSPECIFIED.);
#7866=B_SPLINE_CURVE_WITH_KNOTS('',3,(#82657,#82658,#82659,#82660,#82661,
#82662,#82663,#82664,#82665,#82666),.UNSPECIFIED.,.F.,.F.,(4,1,1,1,1,1,
1,4),(164.472867375453,164.919997856916,165.919512995443,166.919028133969,
167.918543272496,168.918058411023,169.91757354955,170.756048504761),
 .UNSPECIFIED.);
#7867=B_SPLINE_CURVE_WITH_KNOTS('',3,(#82668,#82669,#82670,#82671,#82672,
#82673,#82674,#82675,#82676,#82677,#82678),.UNSPECIFIED.,.F.,.F.,(4,1,1,
1,1,1,1,1,4),(170.756048504761,170.917088688076,171.916603826603,172.91611896513,
173.915634103657,174.915149242183,175.91466438071,176.914179519237,177.03923381194),
 .UNSPECIFIED.);
#7868=B_SPLINE_CURVE_WITH_KNOTS('',3,(#82680,#82681,#82682,#82683,#82684,
#82685,#82686,#82687,#82688,#82689,#82690,#82691,#82692,#82693,#82694,#82695,
#82696,#82697,#82698,#82699,#82700,#82701,#82702,#82703,#82704,#82705,#82706,
#82707,#82708,#82709,#82710,#82711,#82712,#82713,#82714,#82715,#82716,#82717,
#82718,#82719,#82720,#82721,#82722,#82723,#82724,#82725,#82726,#82727,#82728,
#82729,#82730,#82731,#82732,#82733,#82734,#82735,#82736,#82737,#82738,#82739,
#82740,#82741,#82742,#82743,#82744,#82745,#82746,#82747,#82748,#82749,#82750,
#82751,#82752,#82753,#82754,#82755,#82756,#82757,#82758,#82759,#82760,#82761,
#82762,#82763,#82764,#82765,#82766,#82767,#82768,#82769,#82770,#82771,#82772,
#82773,#82774,#82775,#82776,#82777,#82778,#82779,#82780,#82781,#82782,#82783,
#82784,#82785,#82786,#82787,#82788,#82789,#82790,#82791,#82792,#82793,#82794,
#82795,#82796,#82797,#82798,#82799,#82800,#82801,#82802,#82803,#82804,#82805,
#82806,#82807,#82808,#82809,#82810,#82811,#82812,#82813,#82814,#82815,#82816,
#82817,#82818,#82819,#82820,#82821,#82822,#82823,#82824,#82825,#82826,#82827,
#82828,#82829,#82830,#82831,#82832,#82833,#82834,#82835,#82836,#82837,#82838,
#82839,#82840,#82841,#82842,#82843,#82844,#82845,#82846,#82847,#82848,#82849,
#82850,#82851,#82852,#82853,#82854,#82855,#82856,#82857,#82858,#82859,#82860,
#82861,#82862,#82863,#82864,#82865,#82866,#82867,#82868,#82869,#82870,#82871,
#82872,#82873,#82874,#82875,#82876,#82877,#82878,#82879,#82880,#82881,#82882,
#82883,#82884,#82885,#82886,#82887,#82888,#82889,#82890,#82891,#82892,#82893,
#82894,#82895,#82896,#82897,#82898,#82899,#82900,#82901,#82902,#82903,#82904,
#82905),.UNSPECIFIED.,.F.,.F.,(4,3,3,3,3,3,3,3,3,3,3,3,3,3,3,3,3,3,3,3,
3,3,3,3,3,3,3,3,3,3,3,3,3,3,3,3,3,3,3,3,3,3,3,3,3,3,3,3,3,3,3,3,3,3,3,3,
3,3,3,3,3,3,3,3,3,3,3,3,3,3,3,3,3,3,3,4),(177.03923381194,177.126475142022,
177.213619107611,177.30112855138,177.388160191197,177.475175149924,177.562195876577,
177.650070571874,177.737216360473,177.825455509119,177.913694657764,178.002249059202,
178.090688746931,178.179037522124,178.270809056395,178.359055590967,178.447288709183,
178.535529777221,178.623800161849,178.712170892701,178.800601143988,178.889161614084,
178.913209796291,179.001764197729,179.090203885458,179.17855266065,179.270324194921,
179.358570729493,179.446803847708,179.535044915746,179.623315300374,179.711686031225,
179.800116282512,179.888676752608,179.912724934817,180.001279336255,180.089719023984,
180.178067799177,180.269839333448,180.35808586802,180.446318986235,180.534560054274,
180.622830438902,180.711201169754,180.799631421041,180.888191891136,180.912240073344,
181.000794474782,181.089234162512,181.177582937705,181.269354471975,181.357601006547,
181.445834124763,181.534075192802,181.62234557743,181.710716308282,181.799146559569,
181.887707029665,181.911755211871,182.000309613309,182.088749301038,182.177098076231,
182.268869610502,182.357116145074,182.44534926329,182.533590331328,182.621860715958,
182.71023144681,182.798661698097,182.887222168193,182.911270350398,183.014057490355,
183.111436425305,183.208546480735,183.305258922378,183.322418910228),
 .UNSPECIFIED.);
#7869=B_SPLINE_CURVE_WITH_KNOTS('',3,(#82907,#82908,#82909,#82910,#82911,
#82912,#82913,#82914,#82915,#82916),.UNSPECIFIED.,.F.,.F.,(4,1,1,1,1,1,
1,4),(183.32241911912,183.910785488924,184.910300627451,185.909815765978,
186.909330904505,187.908846043031,188.908361181558,189.605604426299),
 .UNSPECIFIED.);
#7870=B_SPLINE_CURVE_WITH_KNOTS('',3,(#82918,#82919,#82920,#82921,#82922,
#82923,#82924,#82925,#82926,#82927,#82928,#82929,#82930,#82931,#82932,#82933,
#82934,#82935,#82936,#82937,#82938,#82939,#82940,#82941,#82942,#82943,#82944,
#82945,#82946,#82947,#82948,#82949,#82950,#82951,#82952,#82953,#82954,#82955,
#82956,#82957,#82958,#82959,#82960,#82961,#82962,#82963,#82964,#82965,#82966,
#82967,#82968,#82969,#82970,#82971,#82972,#82973,#82974,#82975,#82976,#82977,
#82978,#82979,#82980,#82981,#82982,#82983,#82984,#82985,#82986,#82987,#82988,
#82989,#82990,#82991,#82992,#82993,#82994,#82995,#82996,#82997,#82998,#82999,
#83000,#83001,#83002,#83003,#83004,#83005,#83006,#83007,#83008,#83009,#83010,
#83011,#83012,#83013,#83014,#83015,#83016,#83017,#83018,#83019,#83020,#83021,
#83022,#83023,#83024,#83025,#83026,#83027,#83028,#83029,#83030,#83031,#83032,
#83033,#83034,#83035,#83036,#83037,#83038,#83039,#83040,#83041,#83042,#83043,
#83044,#83045,#83046,#83047,#83048,#83049,#83050,#83051,#83052,#83053,#83054,
#83055,#83056,#83057,#83058,#83059,#83060,#83061,#83062,#83063,#83064,#83065,
#83066,#83067,#83068,#83069,#83070,#83071,#83072,#83073,#83074,#83075,#83076,
#83077,#83078,#83079,#83080,#83081,#83082,#83083,#83084,#83085,#83086,#83087,
#83088,#83089,#83090,#83091,#83092,#83093,#83094,#83095,#83096,#83097,#83098,
#83099,#83100,#83101,#83102,#83103,#83104,#83105,#83106,#83107,#83108,#83109,
#83110,#83111,#83112,#83113,#83114,#83115,#83116,#83117,#83118,#83119,#83120,
#83121,#83122,#83123,#83124,#83125,#83126,#83127,#83128,#83129,#83130,#83131,
#83132,#83133,#83134,#83135,#83136,#83137,#83138,#83139,#83140),
 .UNSPECIFIED.,.F.,.F.,(4,3,3,3,3,3,3,3,3,3,3,3,3,3,3,3,3,3,3,3,3,3,3,3,
3,3,3,3,3,3,3,3,3,3,3,3,3,3,3,3,3,3,3,3,3,3,3,3,3,3,3,3,3,3,3,3,3,3,3,3,
3,3,3,3,3,3,3,3,3,3,3,3,3,3,4),(189.605604613475,189.711658493287,189.819107013171,
189.907876320085,189.996430721523,190.084870409252,190.173219184445,190.264990718716,
190.353237253288,190.441470371503,190.529711439541,190.617981824169,190.706352555021,
190.794782806308,190.883343276404,190.907391458612,190.99594586005,191.084385547779,
191.172734322972,191.264505857242,191.352752391814,191.440985510029,191.529226578067,
191.617496962695,191.705867693547,191.794297944834,191.882858414929,191.906906597138,
191.995460998576,192.083900686305,192.172249461498,192.264020995769,192.352267530341,
192.440500648556,192.528741716595,192.617012101223,192.705382832075,192.793813083361,
192.882373553457,192.906421735665,192.994976137103,193.083415824833,193.171764600026,
193.263536134296,193.351782668868,193.440015787084,193.528256855123,193.616527239751,
193.704897970603,193.79332822189,193.881888691986,193.905936874192,193.99449127563,
194.082930963359,194.171279738552,194.263051272823,194.351297807395,194.439530925611,
194.527771993649,194.616042378277,194.704413109129,194.792843360415,194.881403830511,
194.905452012719,194.993759355444,195.081952145223,195.170054472789,195.259896380375,
195.347898808515,195.435888606357,195.523887397765,195.615112981694,195.703244301595,
195.796017017537,195.888789733479),.UNSPECIFIED.);
#7871=B_SPLINE_CURVE_WITH_KNOTS('',3,(#83142,#83143,#83144,#83145,#83146,
#83147,#83148,#83149,#83150,#83151,#83152,#83153),.UNSPECIFIED.,.F.,.F.,
(4,2,1,1,1,1,1,1,4),(195.888789733479,195.904967151245,196.904482289772,
197.903997428299,198.903512566826,199.903027705353,200.902542843879,201.902057982406,
202.171971572916),.UNSPECIFIED.);
#7872=B_SPLINE_CURVE_WITH_KNOTS('',3,(#83155,#83156,#83157,#83158,#83159,
#83160,#83161,#83162,#83163,#83164,#83165,#83166,#83167,#83168,#83169,#83170,
#83171,#83172,#83173,#83174,#83175,#83176,#83177,#83178,#83179,#83180,#83181,
#83182,#83183,#83184,#83185,#83186,#83187,#83188,#83189,#83190,#83191,#83192,
#83193,#83194,#83195,#83196,#83197,#83198,#83199,#83200,#83201,#83202,#83203,
#83204,#83205,#83206,#83207,#83208,#83209,#83210,#83211,#83212,#83213,#83214,
#83215,#83216,#83217,#83218,#83219,#83220,#83221,#83222,#83223,#83224,#83225,
#83226,#83227,#83228,#83229,#83230,#83231,#83232,#83233,#83234,#83235,#83236,
#83237,#83238,#83239,#83240,#83241,#83242,#83243,#83244,#83245,#83246,#83247,
#83248,#83249,#83250,#83251,#83252,#83253,#83254,#83255,#83256,#83257,#83258,
#83259,#83260,#83261,#83262,#83263,#83264,#83265,#83266,#83267,#83268,#83269,
#83270,#83271,#83272,#83273,#83274,#83275,#83276,#83277,#83278,#83279,#83280,
#83281,#83282,#83283,#83284,#83285,#83286,#83287,#83288,#83289,#83290,#83291,
#83292,#83293,#83294,#83295,#83296,#83297,#83298,#83299,#83300,#83301,#83302,
#83303,#83304,#83305,#83306,#83307,#83308,#83309,#83310,#83311,#83312,#83313,
#83314,#83315,#83316,#83317,#83318,#83319,#83320,#83321,#83322,#83323,#83324,
#83325,#83326,#83327,#83328,#83329,#83330,#83331,#83332,#83333,#83334,#83335,
#83336,#83337,#83338,#83339,#83340,#83341,#83342,#83343,#83344,#83345,#83346,
#83347,#83348,#83349,#83350,#83351,#83352,#83353,#83354,#83355,#83356,#83357,
#83358,#83359,#83360,#83361,#83362,#83363,#83364,#83365,#83366,#83367,#83368,
#83369,#83370,#83371,#83372,#83373,#83374,#83375,#83376,#83377,#83378,#83379,
#83380),.UNSPECIFIED.,.F.,.F.,(4,3,3,3,3,3,3,3,3,3,3,3,3,3,3,3,3,3,3,3,
3,3,3,3,3,3,3,3,3,3,3,3,3,3,3,3,3,3,3,3,3,3,3,3,3,3,3,3,3,3,3,3,3,3,3,3,
3,3,3,3,3,3,3,3,3,3,3,3,3,3,3,3,3,3,3,4),(202.171975040658,202.263174800692,
202.350584664857,202.437975665214,202.525369957242,202.612789694942,202.700306666439,
202.78788112853,202.875585818985,202.901573120933,202.990127522371,203.078567210101,
203.166915985293,203.258687519564,203.346934054136,203.435167172352,203.52340824039,
203.611678625018,203.70004935587,203.788479607157,203.877040077253,203.90108825946,
203.989642660898,204.078082348627,204.166431123819,204.25820265809,204.346449192662,
204.434682310877,204.522923378915,204.611193763543,204.699564494395,204.787994745681,
204.876555215777,204.900603397986,204.989157799424,205.077597487154,205.165946262346,
205.257717796617,205.345964331189,205.434197449405,205.522438517443,205.61070890207,
205.699079632922,205.787509884209,205.876070354305,205.900118536513,205.988672937951,
206.077112625681,206.165461400874,206.257232935144,206.345479469716,206.433712587932,
206.521953655971,206.6102240406,206.698594771452,206.787025022738,206.875585492834,
206.89963367504,206.988188076478,207.076627764207,207.164976539401,207.256748073671,
207.344994608243,207.433227726459,207.521468794497,207.609739179125,207.698109909977,
207.786540161264,207.87510063136,207.899148813567,207.990226239938,208.081164061968,
208.174663133436,208.265343039278,208.360251693558,208.455160347838),
 .UNSPECIFIED.);
#7873=B_SPLINE_CURVE_WITH_KNOTS('',3,(#83382,#83383,#83384,#83385,#83386,
#83387,#83388,#83389,#83390,#83391),.UNSPECIFIED.,.F.,.F.,(4,1,1,1,1,1,
1,4),(208.455164776037,208.898663952093,209.89817909062,210.897694229147,
211.897209367674,212.8967245062,213.896239644727,214.738345655017),
 .UNSPECIFIED.);
#7874=B_SPLINE_CURVE_WITH_KNOTS('',3,(#83393,#83394,#83395,#83396,#83397,
#83398,#83399,#83400,#83401,#83402,#83403),.UNSPECIFIED.,.F.,.F.,(4,1,1,
1,1,1,1,1,4),(214.738345655017,214.895754783254,215.895269921781,216.894785060307,
217.894300198834,218.893815337361,219.893330475888,220.892845614415,221.021530962197),
 .UNSPECIFIED.);
#7875=B_SPLINE_CURVE_WITH_KNOTS('',3,(#83405,#83406,#83407,#83408,#83409,
#83410,#83411,#83412,#83413,#83414,#83415,#83416,#83417,#83418,#83419,#83420,
#83421,#83422,#83423,#83424,#83425,#83426,#83427,#83428,#83429,#83430,#83431,
#83432,#83433,#83434,#83435,#83436,#83437,#83438,#83439,#83440,#83441,#83442,
#83443,#83444,#83445,#83446,#83447,#83448,#83449,#83450,#83451,#83452,#83453,
#83454,#83455,#83456,#83457,#83458,#83459,#83460,#83461,#83462,#83463,#83464,
#83465,#83466,#83467,#83468,#83469,#83470,#83471,#83472,#83473,#83474,#83475,
#83476,#83477,#83478,#83479,#83480,#83481,#83482,#83483,#83484,#83485,#83486,
#83487,#83488,#83489,#83490,#83491,#83492,#83493,#83494,#83495,#83496,#83497,
#83498,#83499,#83500,#83501,#83502,#83503,#83504,#83505,#83506,#83507,#83508,
#83509,#83510,#83511,#83512,#83513,#83514,#83515,#83516,#83517,#83518,#83519,
#83520,#83521,#83522,#83523,#83524,#83525,#83526,#83527,#83528,#83529,#83530,
#83531,#83532,#83533,#83534,#83535,#83536,#83537,#83538,#83539,#83540,#83541,
#83542,#83543,#83544,#83545,#83546,#83547,#83548,#83549,#83550,#83551,#83552,
#83553,#83554,#83555,#83556,#83557,#83558,#83559,#83560,#83561,#83562,#83563,
#83564,#83565,#83566,#83567,#83568,#83569,#83570,#83571,#83572,#83573,#83574,
#83575,#83576,#83577,#83578,#83579,#83580,#83581,#83582,#83583,#83584,#83585,
#83586,#83587,#83588,#83589,#83590,#83591,#83592,#83593,#83594,#83595,#83596,
#83597,#83598,#83599,#83600,#83601,#83602,#83603,#83604,#83605,#83606,#83607,
#83608,#83609,#83610,#83611,#83612,#83613,#83614,#83615,#83616,#83617,#83618,
#83619,#83620,#83621,#83622,#83623,#83624,#83625,#83626,#83627,#83628,#83629,
#83630),.UNSPECIFIED.,.F.,.F.,(4,3,3,3,3,3,3,3,3,3,3,3,3,3,3,3,3,3,3,3,
3,3,3,3,3,3,3,3,3,3,3,3,3,3,3,3,3,3,3,3,3,3,3,3,3,3,3,3,3,3,3,3,3,3,3,3,
3,3,3,3,3,3,3,3,3,3,3,3,3,3,3,3,3,3,3,4),(221.021530962197,221.108754796741,
221.195882130097,221.282941957953,221.369959096486,221.456960244626,221.543967860593,
221.63106608368,221.718199326175,221.805477327452,221.892360752941,221.980915154314,
222.069354841978,222.157703617104,222.2494751514,222.337721685902,222.425954804048,
222.514195872016,222.602466256572,222.690836987352,222.779267238567,222.867827708591,
222.891875891468,222.980430293437,223.068869981698,223.157218757425,223.248990291496,
223.3372368266,223.425469945346,223.513711013913,223.601981399067,223.690352130439,
223.778782382243,223.867342852848,223.891391029995,223.979945430572,224.068385117442,
224.156733891777,224.24850542637,224.336751960095,224.424985077469,224.513226144672,
224.601496528473,224.689867258511,224.778297508992,224.866857978299,224.890906168522,
224.979460569799,225.067900257359,225.156249032376,225.24802056671,225.336267101086,
225.4245002191,225.512741286931,225.601011671346,225.689382401977,225.777812653038,
225.866373122903,225.890421307048,225.97897571197,226.067415403196,226.155764181893,
226.247535714853,226.335782252927,226.424015374639,226.512256446163,226.600526834263,
226.688897568548,226.77732782325,226.865888296708,226.889936445575,226.987493993785,
227.084658138073,227.181562779715,227.278077411535,227.304716066149),
 .UNSPECIFIED.);
#7876=B_SPLINE_CURVE_WITH_KNOTS('',3,(#83632,#83633,#83634,#83635,#83636,
#83637,#83638,#83639,#83640,#83641),.UNSPECIFIED.,.F.,.F.,(4,1,1,1,1,1,
1,4),(227.304716269377,227.889451584102,228.888966722629,229.888481861155,
230.887996999682,231.887512138209,232.887027276736,233.587901576556),
 .UNSPECIFIED.);
#7877=B_SPLINE_CURVE_WITH_KNOTS('',3,(#83643,#83644,#83645,#83646,#83647,
#83648,#83649,#83650,#83651,#83652,#83653,#83654,#83655,#83656,#83657,#83658,
#83659,#83660,#83661,#83662,#83663,#83664,#83665,#83666,#83667,#83668,#83669,
#83670,#83671,#83672,#83673,#83674,#83675,#83676,#83677,#83678,#83679,#83680,
#83681,#83682,#83683,#83684,#83685,#83686,#83687,#83688,#83689,#83690,#83691,
#83692,#83693,#83694,#83695,#83696,#83697,#83698,#83699,#83700,#83701,#83702,
#83703,#83704,#83705,#83706,#83707,#83708,#83709,#83710,#83711,#83712,#83713,
#83714,#83715,#83716,#83717,#83718,#83719,#83720,#83721,#83722,#83723,#83724,
#83725,#83726,#83727,#83728,#83729,#83730,#83731,#83732,#83733,#83734,#83735,
#83736,#83737,#83738,#83739,#83740,#83741,#83742,#83743,#83744,#83745,#83746,
#83747,#83748,#83749,#83750,#83751,#83752,#83753,#83754,#83755,#83756,#83757,
#83758,#83759,#83760,#83761,#83762,#83763,#83764,#83765,#83766,#83767,#83768,
#83769,#83770,#83771,#83772,#83773,#83774,#83775,#83776,#83777,#83778,#83779,
#83780,#83781,#83782,#83783,#83784,#83785,#83786,#83787,#83788,#83789,#83790,
#83791,#83792,#83793,#83794,#83795,#83796,#83797,#83798,#83799,#83800,#83801,
#83802,#83803,#83804,#83805,#83806,#83807,#83808,#83809,#83810,#83811,#83812,
#83813,#83814,#83815,#83816,#83817,#83818,#83819,#83820,#83821,#83822,#83823,
#83824,#83825,#83826,#83827,#83828,#83829,#83830,#83831,#83832,#83833,#83834,
#83835,#83836,#83837,#83838,#83839,#83840,#83841,#83842,#83843,#83844,#83845,
#83846,#83847,#83848,#83849,#83850,#83851,#83852,#83853,#83854,#83855,#83856,
#83857,#83858,#83859,#83860,#83861,#83862,#83863,#83864,#83865,#83866,#83867,
#83868),.UNSPECIFIED.,.F.,.F.,(4,3,3,3,3,3,3,3,3,3,3,3,3,3,3,3,3,3,3,3,
3,3,3,3,3,3,3,3,3,3,3,3,3,3,3,3,3,3,3,3,3,3,3,3,3,3,3,3,3,3,3,3,3,3,3,3,
3,3,3,3,3,3,3,3,3,3,3,3,3,3,3,3,3,3,3,4),(233.587901756539,233.694378808573,
233.802304697791,233.886542415262,233.975097061021,234.063536990865,234.151886005719,
234.243657449228,234.331904215935,234.420137563137,234.508378856785,234.596649463416,
234.685020409845,234.773450873236,234.862011548726,234.886057553789,234.974612775169,
235.063053288167,235.151402892939,235.243174117861,235.331421487515,235.419655441421,
235.50789734487,235.596168563739,235.68454012287,235.77297119999,235.861532485909,
235.885572692316,235.974124503413,236.06256159786,236.150907779833,236.242680286209,
236.330924243718,236.419154795135,236.507393309305,236.595661155676,236.684029384112,
236.77245715074,236.861015181431,236.885087830843,236.973644590983,237.062086624006,
237.150437728593,237.24220838369,237.330457194067,237.41869256461,237.50693585923,
237.595208442402,237.68358131942,237.772013689061,237.860576220479,237.88460296937,
237.973161973041,238.061606301539,238.149959750189,238.241729544902,238.329980804653,
238.418218659028,238.506464469126,238.594739596636,238.683115047461,238.771550011202,
238.860115146021,238.884118107896,238.972460561993,239.060688395686,239.148825659066,
239.239108312124,239.327145265534,239.415169489258,239.503202570966,239.595173649107,
239.68333984933,239.771567865194,239.859922378897,239.871086883532),
 .UNSPECIFIED.);
#7878=B_SPLINE_CURVE_WITH_KNOTS('',3,(#83870,#83871,#83872,#83873,#83874,
#83875,#83876,#83877,#83878,#83879,#83880,#83881,#83882,#83883,#83884,#83885,
#83886,#83887,#83888,#83889,#83890,#83891,#83892,#83893,#83894,#83895,#83896,
#83897,#83898,#83899,#83900,#83901,#83902,#83903,#83904,#83905,#83906,#83907,
#83908,#83909,#83910,#83911,#83912,#83913,#83914,#83915,#83916,#83917,#83918,
#83919,#83920,#83921,#83922,#83923,#83924,#83925,#83926,#83927,#83928,#83929,
#83930,#83931,#83932,#83933,#83934,#83935,#83936,#83937,#83938,#83939,#83940,
#83941,#83942,#83943,#83944,#83945,#83946,#83947,#83948,#83949,#83950,#83951,
#83952,#83953,#83954,#83955,#83956,#83957,#83958,#83959,#83960,#83961,#83962,
#83963,#83964,#83965,#83966,#83967,#83968,#83969,#83970,#83971,#83972,#83973,
#83974,#83975,#83976,#83977,#83978,#83979,#83980,#83981,#83982,#83983,#83984,
#83985,#83986,#83987,#83988,#83989,#83990,#83991,#83992,#83993,#83994,#83995,
#83996,#83997,#83998,#83999,#84000,#84001,#84002,#84003,#84004,#84005,#84006,
#84007,#84008,#84009,#84010,#84011,#84012,#84013,#84014,#84015,#84016,#84017,
#84018,#84019,#84020,#84021,#84022,#84023,#84024,#84025,#84026,#84027,#84028,
#84029,#84030,#84031,#84032,#84033,#84034,#84035,#84036,#84037,#84038,#84039,
#84040,#84041,#84042,#84043,#84044,#84045,#84046,#84047,#84048,#84049,#84050),
 .UNSPECIFIED.,.F.,.F.,(4,3,3,3,3,3,3,3,3,3,3,3,3,3,3,3,3,3,3,3,3,3,3,3,
3,3,3,3,3,3,3,3,3,3,3,3,3,3,3,3,3,3,3,3,3,3,3,3,3,3,3,3,3,3,3,3,3,3,3,3,
4),(239.871086883736,239.883633246423,239.972208372219,240.060668706586,
240.149038028121,240.240801822725,240.329068529199,240.417321647942,240.505582524723,
240.593872505738,240.682262421262,240.770711641347,240.859290618007,240.88314838495,
240.97172640819,241.060189991207,241.148562903905,241.240325481352,241.32859660096,
241.416854426589,241.505120297491,241.593415553553,241.681811129969,241.770266242208,
241.858851401616,241.882663523477,241.97109354429,242.059408581874,242.147632580698,
242.239450840861,242.327573045086,242.415682201121,242.503799801744,242.591947340844,
242.680196761928,242.768506443136,242.856948365817,242.882178662003,242.970905168179,
243.059516527781,243.14803634618,243.239743527974,243.328158477201,243.416558752347,
243.504965543172,243.593400038828,243.681931674474,243.770521156149,243.859237186955,
243.88169380053,243.96950795302,244.057209821738,244.14482398992,244.232377230877,
244.319899046808,244.407411513512,244.49493669478,244.582548289539,244.670205938562,
244.757997774109,244.81888007831),.UNSPECIFIED.);
#7879=B_SPLINE_CURVE_WITH_KNOTS('',3,(#84054,#84055,#84056,#84057,#84058,
#84059,#84060,#84061),.UNSPECIFIED.,.F.,.F.,(4,1,1,1,1,4),(-246.88023921611,
-245.880724077584,-244.881208939057,-243.88169380053,-242.882178662003,
-242.853790713018),.UNSPECIFIED.);
#7880=B_SPLINE_CURVE_WITH_KNOTS('',3,(#84063,#84064,#84065,#84066,#84067,
#84068,#84069,#84070,#84071,#84072,#84073,#84074,#84075,#84076,#84077,#84078,
#84079,#84080,#84081,#84082,#84083,#84084,#84085,#84086,#84087,#84088,#84089,
#84090,#84091,#84092,#84093,#84094,#84095,#84096,#84097,#84098,#84099,#84100,
#84101,#84102,#84103,#84104,#84105,#84106,#84107,#84108,#84109,#84110,#84111,
#84112,#84113,#84114,#84115,#84116,#84117,#84118,#84119,#84120,#84121,#84122,
#84123,#84124,#84125,#84126,#84127,#84128,#84129,#84130,#84131,#84132,#84133,
#84134,#84135,#84136,#84137,#84138,#84139,#84140,#84141,#84142,#84143,#84144,
#84145,#84146,#84147,#84148,#84149,#84150,#84151,#84152,#84153,#84154,#84155,
#84156,#84157,#84158,#84159,#84160,#84161,#84162,#84163,#84164,#84165,#84166,
#84167,#84168,#84169,#84170,#84171,#84172,#84173,#84174,#84175,#84176,#84177,
#84178,#84179,#84180,#84181,#84182,#84183,#84184,#84185,#84186,#84187,#84188,
#84189,#84190,#84191,#84192,#84193,#84194,#84195,#84196,#84197,#84198,#84199,
#84200,#84201,#84202,#84203,#84204,#84205,#84206,#84207,#84208,#84209,#84210,
#84211,#84212,#84213,#84214,#84215,#84216,#84217,#84218,#84219,#84220,#84221,
#84222,#84223,#84224,#84225,#84226,#84227,#84228,#84229,#84230,#84231,#84232,
#84233,#84234,#84235,#84236,#84237,#84238,#84239,#84240,#84241,#84242,#84243,
#84244,#84245,#84246,#84247,#84248,#84249,#84250,#84251,#84252,#84253,#84254,
#84255,#84256,#84257,#84258,#84259,#84260,#84261,#84262,#84263,#84264,#84265,
#84266,#84267,#84268,#84269,#84270,#84271,#84272,#84273,#84274,#84275,#84276,
#84277,#84278,#84279,#84280,#84281,#84282,#84283,#84284,#84285),
 .UNSPECIFIED.,.F.,.F.,(4,3,3,3,3,3,3,3,3,3,3,3,3,3,3,3,3,3,3,3,3,3,3,3,
3,3,3,3,3,3,3,3,3,3,3,3,3,3,3,3,3,3,3,3,3,3,3,3,3,3,3,3,3,3,3,3,3,3,3,3,
3,3,3,3,3,3,3,3,3,3,3,3,3,3,4),(-242.853790713018,-242.765773024893,-242.677869948349,
-242.590057088657,-242.501632893009,-242.413917985828,-242.326214927956,
-242.238501828221,-242.149542252035,-242.061695811257,-241.972179667367,
-241.882663523477,-241.794084508876,-241.705620118365,-241.6172465813,-241.525484306756,
-241.437213022899,-241.348955203009,-241.260689507824,-241.172394597576,
-241.083999617283,-240.995545247635,-240.906961039838,-240.88314838495,
-240.794575532451,-240.706117036234,-240.617749119541,-240.525984635402,
-240.437718245461,-240.349465041323,-240.261203677315,-240.172912807041,
-240.084521410963,-239.996070364259,-239.907489067623,-239.883633246423,
-239.795095981985,-239.706673656451,-239.618342446681,-239.526564404333,
-239.438335833301,-239.350120795425,-239.261897905745,-239.173645778763,
-239.085293331673,-238.996881402064,-238.908339167613,-238.884118107896,
-238.795559054846,-238.707114685267,-238.618761203808,-238.526991424503,
-238.438740152753,-238.350502294075,-238.262256487372,-238.173981370968,
-238.085605942618,-237.997171008,-237.908605911828,-237.88460296937,-237.796046512253,
-237.707604724215,-237.619253806823,-237.527483059826,-237.439234291475,
-237.350998909353,-237.262755549564,-237.174482847605,-237.086109772928,
-236.997677159474,-236.909114318416,-236.885087830843,-236.778947052171,
-236.673986362008,-236.570605614479),.UNSPECIFIED.);
#7881=B_SPLINE_CURVE_WITH_KNOTS('',3,(#84287,#84288,#84289,#84290,#84291,
#84292,#84293,#84294,#84295,#84296),.UNSPECIFIED.,.F.,.F.,(4,1,1,1,1,1,
1,4),(-236.570605405839,-235.885572692316,-234.886057553789,-233.886542415262,
-232.887027276736,-231.887512138209,-230.887996999682,-230.287420098659),
 .UNSPECIFIED.);
#7882=B_SPLINE_CURVE_WITH_KNOTS('',3,(#84298,#84299,#84300,#84301,#84302,
#84303,#84304,#84305,#84306,#84307,#84308,#84309,#84310,#84311,#84312,#84313,
#84314,#84315,#84316,#84317,#84318,#84319,#84320,#84321,#84322,#84323,#84324,
#84325,#84326,#84327,#84328,#84329,#84330,#84331,#84332,#84333,#84334,#84335,
#84336,#84337,#84338,#84339,#84340,#84341,#84342,#84343,#84344,#84345,#84346,
#84347,#84348,#84349,#84350,#84351,#84352,#84353,#84354,#84355,#84356,#84357,
#84358,#84359,#84360,#84361,#84362,#84363,#84364,#84365,#84366,#84367,#84368,
#84369,#84370,#84371,#84372,#84373,#84374,#84375,#84376,#84377,#84378,#84379,
#84380,#84381,#84382,#84383,#84384,#84385,#84386,#84387,#84388,#84389,#84390,
#84391,#84392,#84393,#84394,#84395,#84396,#84397,#84398,#84399,#84400,#84401,
#84402,#84403,#84404,#84405,#84406,#84407,#84408,#84409,#84410,#84411,#84412,
#84413,#84414,#84415,#84416,#84417,#84418,#84419,#84420,#84421,#84422,#84423,
#84424,#84425,#84426,#84427,#84428,#84429,#84430,#84431,#84432,#84433,#84434,
#84435,#84436,#84437,#84438,#84439,#84440,#84441,#84442,#84443,#84444,#84445,
#84446,#84447,#84448,#84449,#84450,#84451,#84452,#84453,#84454,#84455,#84456,
#84457,#84458,#84459,#84460,#84461,#84462,#84463,#84464,#84465,#84466,#84467,
#84468,#84469,#84470,#84471,#84472,#84473,#84474,#84475,#84476,#84477,#84478,
#84479,#84480,#84481,#84482,#84483,#84484,#84485,#84486,#84487,#84488,#84489,
#84490,#84491,#84492,#84493,#84494,#84495,#84496,#84497,#84498,#84499,#84500,
#84501,#84502,#84503,#84504,#84505,#84506,#84507,#84508,#84509,#84510,#84511,
#84512,#84513,#84514,#84515,#84516,#84517,#84518,#84519,#84520,#84521,#84522,
#84523),.UNSPECIFIED.,.F.,.F.,(4,3,3,3,3,3,3,3,3,3,3,3,3,3,3,3,3,3,3,3,
3,3,3,3,3,3,3,3,3,3,3,3,3,3,3,3,3,3,3,3,3,3,3,3,3,3,3,3,3,3,3,3,3,3,3,3,
3,3,3,3,3,3,3,3,3,3,3,3,3,3,3,3,3,3,3,4),(-230.287419873382,-230.187685370325,
-230.089695435759,-229.989088648457,-229.888481861155,-229.799927438089,
-229.711487728505,-229.623138931259,-229.53136740518,-229.443120848196,
-229.354887707474,-229.266646616858,-229.178376209606,-229.090005456174,
-229.001575182305,-228.9130146898,-228.888966722629,-228.80041232085,-228.71197263272,
-228.623623857066,-228.531852322945,-228.443605787764,-228.355372668885,
-228.267131600131,-228.178861214733,-228.090490483036,-228.002060230859,
-227.913499759814,-227.889451584102,-227.800897188767,-227.712457507237,
-227.624108738331,-227.532337201737,-227.444090673634,-227.355857561944,
-227.267616500481,-227.17934612247,-227.090975398267,-227.002545153654,
-226.913984690219,-226.889936445575,-226.80138204078,-226.712942349655,
-226.624593571034,-226.532822038036,-226.444575499973,-226.35634237825,
-226.26810130669,-226.179830918531,-226.091460184152,-226.003029929335,
-225.914469455733,-225.890421307048,-225.80186690584,-225.713427218336,
-225.625078443363,-225.533306909008,-225.445060374642,-225.356827256626,
-225.268586188782,-225.180315804342,-225.091945073667,-225.003514822552,
-224.914954352618,-224.890906168522,-224.803533528896,-224.716274617417,
-224.627269639174,-224.540163709119,-224.453089248357,-224.366023837001,
-224.275576575621,-224.188419159953,-224.101213336875,-224.013898682601,
-224.00423479148),.UNSPECIFIED.);
#7883=B_SPLINE_CURVE_WITH_KNOTS('',3,(#84525,#84526,#84527,#84528,#84529,
#84530,#84531,#84532,#84533,#84534,#84535),.UNSPECIFIED.,.F.,.F.,(4,1,1,
1,1,1,1,1,4),(-224.00423479148,-223.891391029995,-222.891875891468,-221.892360752941,
-220.892845614415,-219.893330475888,-218.893815337361,-217.894300198834,
-217.7210494843),.UNSPECIFIED.);
#7884=B_SPLINE_CURVE_WITH_KNOTS('',3,(#84537,#84538,#84539,#84540,#84541,
#84542,#84543,#84544,#84545,#84546,#84547,#84548,#84549,#84550,#84551,#84552,
#84553,#84554,#84555,#84556,#84557,#84558,#84559,#84560,#84561,#84562,#84563,
#84564,#84565,#84566,#84567,#84568,#84569,#84570,#84571,#84572,#84573,#84574,
#84575,#84576,#84577,#84578,#84579,#84580,#84581,#84582,#84583,#84584,#84585,
#84586,#84587,#84588,#84589,#84590,#84591,#84592,#84593,#84594,#84595,#84596,
#84597,#84598,#84599,#84600,#84601,#84602,#84603,#84604,#84605,#84606,#84607,
#84608,#84609,#84610,#84611,#84612,#84613,#84614,#84615,#84616,#84617,#84618,
#84619,#84620,#84621,#84622,#84623,#84624,#84625,#84626,#84627,#84628,#84629,
#84630,#84631,#84632,#84633,#84634,#84635,#84636,#84637,#84638,#84639,#84640,
#84641,#84642,#84643,#84644,#84645,#84646,#84647,#84648,#84649,#84650,#84651,
#84652,#84653,#84654,#84655,#84656,#84657,#84658,#84659,#84660,#84661,#84662,
#84663,#84664,#84665,#84666,#84667,#84668,#84669,#84670,#84671,#84672,#84673,
#84674,#84675,#84676,#84677,#84678,#84679,#84680,#84681,#84682,#84683,#84684,
#84685,#84686,#84687,#84688,#84689,#84690,#84691,#84692,#84693,#84694,#84695,
#84696,#84697,#84698,#84699,#84700,#84701,#84702,#84703,#84704,#84705,#84706,
#84707,#84708,#84709,#84710,#84711,#84712,#84713,#84714,#84715,#84716,#84717,
#84718,#84719,#84720,#84721,#84722,#84723,#84724,#84725,#84726,#84727,#84728,
#84729,#84730,#84731,#84732,#84733,#84734,#84735,#84736,#84737,#84738,#84739,
#84740,#84741,#84742,#84743,#84744,#84745,#84746,#84747,#84748,#84749,#84750,
#84751,#84752,#84753,#84754,#84755,#84756,#84757,#84758,#84759,#84760,#84761,
#84762),.UNSPECIFIED.,.F.,.F.,(4,3,3,3,3,3,3,3,3,3,3,3,3,3,3,3,3,3,3,3,
3,3,3,3,3,3,3,3,3,3,3,3,3,3,3,3,3,3,3,3,3,3,3,3,3,3,3,3,3,3,3,3,3,3,3,3,
3,3,3,3,3,3,3,3,3,3,3,3,3,3,3,3,3,3,3,4),(-217.7210494843,-217.633946217353,
-217.546927581786,-217.45996462197,-217.373029360669,-217.286099284211,
-217.199151886862,-217.112114065454,-217.02502534541,-216.937804740184,
-216.894785060307,-216.806230658872,-216.717790971146,-216.629442195957,
-216.537670661685,-216.449424127116,-216.361191008904,-216.272949940869,
-216.184679556244,-216.096308825396,-216.007878574112,-215.91931810402,
-215.895269921781,-215.806715520344,-215.718275832616,-215.629927057425,
-215.538155523154,-215.449908988583,-215.361675870369,-215.273434802332,
-215.185164417706,-215.096793686855,-215.00836343557,-214.919802965476,
-214.895754783254,-214.807200381814,-214.718760694083,-214.630411918888,
-214.538640384618,-214.450393850045,-214.362160731827,-214.273919663787,
-214.185649279157,-214.097278548303,-214.008848297015,-213.920287826917,
-213.896239644727,-213.807685243289,-213.719245555561,-213.630896780368,
-213.539125246097,-213.450878711526,-213.362645593311,-213.274404525273,
-213.186134140645,-213.097763409794,-213.009333158508,-212.920772688412,
-212.8967245062,-212.808170104762,-212.719730417033,-212.63138164184,-212.53961010757,
-212.451363572998,-212.363130454783,-212.274889386745,-212.186619002118,
-212.098248271266,-212.00981801998,-211.921257549884,-211.897209367674,
-211.802221668775,-211.707535983373,-211.613032966347,-211.51880605863,
-211.437864395501),.UNSPECIFIED.);
#7885=B_SPLINE_CURVE_WITH_KNOTS('',3,(#84764,#84765,#84766,#84767,#84768,
#84769,#84770,#84771,#84772,#84773),.UNSPECIFIED.,.F.,.F.,(4,1,1,1,1,1,
1,4),(-211.43786417712,-210.897694229147,-209.89817909062,-208.898663952093,
-207.899148813567,-206.89963367504,-205.900118536513,-205.154678869941),
 .UNSPECIFIED.);
#7886=B_SPLINE_CURVE_WITH_KNOTS('',3,(#84775,#84776,#84777,#84778,#84779,
#84780,#84781,#84782,#84783,#84784,#84785,#84786,#84787,#84788,#84789,#84790,
#84791,#84792,#84793,#84794,#84795,#84796,#84797,#84798,#84799,#84800,#84801,
#84802,#84803,#84804,#84805,#84806,#84807,#84808,#84809,#84810,#84811,#84812,
#84813,#84814,#84815,#84816,#84817,#84818,#84819,#84820,#84821,#84822,#84823,
#84824,#84825,#84826,#84827,#84828,#84829,#84830,#84831,#84832,#84833,#84834,
#84835,#84836,#84837,#84838,#84839,#84840,#84841,#84842,#84843,#84844,#84845,
#84846,#84847,#84848,#84849,#84850,#84851,#84852,#84853,#84854,#84855,#84856,
#84857,#84858,#84859,#84860,#84861,#84862,#84863,#84864,#84865,#84866,#84867,
#84868,#84869,#84870,#84871,#84872,#84873,#84874,#84875,#84876,#84877,#84878,
#84879,#84880,#84881,#84882,#84883,#84884,#84885,#84886,#84887,#84888,#84889,
#84890,#84891,#84892,#84893,#84894,#84895,#84896,#84897,#84898,#84899,#84900,
#84901,#84902,#84903,#84904,#84905,#84906,#84907,#84908,#84909,#84910,#84911,
#84912,#84913,#84914,#84915,#84916,#84917,#84918,#84919,#84920,#84921,#84922,
#84923,#84924,#84925,#84926,#84927,#84928,#84929,#84930,#84931,#84932,#84933,
#84934,#84935,#84936,#84937,#84938,#84939,#84940,#84941,#84942,#84943,#84944,
#84945,#84946,#84947,#84948,#84949,#84950,#84951,#84952,#84953,#84954,#84955,
#84956,#84957,#84958,#84959,#84960,#84961,#84962,#84963,#84964,#84965,#84966,
#84967,#84968,#84969,#84970,#84971,#84972,#84973,#84974,#84975,#84976,#84977,
#84978,#84979,#84980,#84981,#84982,#84983,#84984,#84985,#84986,#84987,#84988,
#84989,#84990,#84991,#84992,#84993,#84994,#84995,#84996,#84997,#84998,#84999,
#85000,#85001,#85002,#85003),.UNSPECIFIED.,.F.,.F.,(4,3,3,3,3,3,3,3,3,3,
3,3,3,3,3,3,3,3,3,3,3,3,3,3,3,3,3,3,3,3,3,3,3,3,3,3,3,3,3,3,3,3,3,3,3,3,
3,3,3,3,3,3,3,3,3,3,3,3,3,3,3,3,3,3,3,3,3,3,3,3,3,3,3,3,3,3,4),(-205.154678738782,
-205.041978910697,-204.926813848051,-204.900603397986,-204.812048996549,
-204.723609308821,-204.635260533629,-204.543488999358,-204.455242464787,
-204.367009346572,-204.278768278535,-204.190497893908,-204.102127163057,
-204.013696911771,-203.925136441676,-203.90108825946,-203.812533858022,
-203.724094170292,-203.635745395099,-203.543973860829,-203.455727326257,
-203.367494208041,-203.279253140003,-203.190982755375,-203.102612024522,
-203.014181773236,-202.92562130314,-202.901573120933,-202.813018719495,
-202.724579031765,-202.636230256572,-202.544458722301,-202.456212187729,
-202.367979069513,-202.279738001475,-202.191467616847,-202.103096885994,
-202.014666634708,-201.926106164611,-201.902057982406,-201.813503580968,
-201.725063893239,-201.636715118046,-201.544943583775,-201.456697049203,
-201.368463930988,-201.280222862949,-201.191952478321,-201.103581747469,
-201.015151496183,-200.926591026087,-200.902542843879,-200.813988442441,
-200.725548754712,-200.63719997952,-200.545428445249,-200.457181910677,
-200.368948792462,-200.280707724424,-200.192437339796,-200.104066608944,
-200.015636357657,-199.927075887562,-199.903027705353,-199.814473303915,
-199.726033616186,-199.637684840994,-199.545913306723,-199.457666772151,
-199.369433653935,-199.281192585897,-199.19292220127,-199.104551470418,
-199.016121219131,-198.927560749036,-198.903512566826,-198.871493562761),
 .UNSPECIFIED.);
#7887=B_SPLINE_CURVE_WITH_KNOTS('',3,(#85005,#85006,#85007,#85008,#85009,
#85010,#85011,#85012,#85013,#85014,#85015,#85016,#85017,#85018,#85019,#85020,
#85021,#85022,#85023,#85024,#85025,#85026,#85027,#85028,#85029,#85030,#85031,
#85032,#85033,#85034,#85035,#85036,#85037,#85038,#85039,#85040,#85041,#85042,
#85043,#85044,#85045,#85046,#85047,#85048,#85049,#85050,#85051,#85052,#85053,
#85054,#85055,#85056,#85057,#85058,#85059,#85060,#85061,#85062,#85063,#85064,
#85065,#85066,#85067,#85068,#85069,#85070,#85071,#85072,#85073,#85074,#85075,
#85076,#85077,#85078,#85079,#85080,#85081,#85082,#85083,#85084,#85085,#85086,
#85087,#85088,#85089,#85090,#85091,#85092,#85093,#85094,#85095,#85096,#85097,
#85098,#85099,#85100,#85101,#85102,#85103,#85104,#85105,#85106,#85107,#85108,
#85109,#85110,#85111,#85112,#85113,#85114,#85115,#85116,#85117,#85118,#85119,
#85120,#85121,#85122,#85123,#85124,#85125,#85126,#85127,#85128,#85129,#85130,
#85131,#85132,#85133,#85134,#85135,#85136,#85137,#85138,#85139,#85140,#85141,
#85142,#85143,#85144,#85145,#85146,#85147,#85148,#85149,#85150,#85151,#85152,
#85153,#85154,#85155,#85156,#85157,#85158,#85159,#85160,#85161,#85162,#85163,
#85164,#85165,#85166,#85167,#85168,#85169,#85170,#85171,#85172,#85173,#85174,
#85175,#85176,#85177,#85178,#85179,#85180,#85181,#85182,#85183,#85184,#85185,
#85186,#85187,#85188,#85189,#85190,#85191,#85192,#85193,#85194,#85195,#85196,
#85197,#85198,#85199,#85200,#85201,#85202,#85203,#85204,#85205,#85206,#85207,
#85208,#85209,#85210,#85211,#85212,#85213,#85214,#85215,#85216,#85217,#85218,
#85219,#85220,#85221,#85222,#85223,#85224,#85225,#85226,#85227),
 .UNSPECIFIED.,.F.,.F.,(4,3,3,3,3,3,3,3,3,3,3,3,3,3,3,3,3,3,3,3,3,3,3,3,
3,3,3,3,3,3,3,3,3,3,3,3,3,3,3,3,3,3,3,3,3,3,3,3,3,3,3,3,3,3,3,3,3,3,3,3,
3,3,3,3,3,3,3,3,3,3,3,3,3,3,4),(-198.871493562533,-198.783408527569,-198.6954365812,
-198.607553404627,-198.519608907586,-198.431820567895,-198.344043110297,
-198.256254704546,-198.168190385484,-198.080268257862,-197.992132843081,
-197.903997428299,-197.815443026861,-197.727003339132,-197.638654563939,
-197.546883029668,-197.458636495096,-197.37040337688,-197.282162308842,
-197.193891924214,-197.105521193362,-197.017090942075,-196.928530471979,
-196.904482289772,-196.815927888334,-196.727488200604,-196.639139425411,
-196.54736789114,-196.459121356568,-196.370888238353,-196.282647170314,
-196.194376785686,-196.106006054834,-196.017575803547,-195.929015333451,
-195.904967151245,-195.816412749807,-195.727973062078,-195.639624286886,
-195.547852752615,-195.459606218043,-195.371373099828,-195.28313203179,
-195.194861647162,-195.106490916311,-195.018060665024,-194.929500194928,
-194.905452012719,-194.816897611281,-194.728457923552,-194.640109148359,
-194.548337614088,-194.460091079516,-194.371857961301,-194.283616893262,
-194.195346508634,-194.106975777782,-194.018545526496,-193.9299850564,-193.905936874192,
-193.817382472754,-193.728942785024,-193.640594009831,-193.54882247556,
-193.460575940988,-193.372342822773,-193.284101754734,-193.195831370106,
-193.107460639254,-193.019030387966,-192.93046991787,-192.906421735665,
-192.800699836041,-192.694504152843,-192.588308469644),.UNSPECIFIED.);
#7888=B_SPLINE_CURVE_WITH_KNOTS('',3,(#85229,#85230,#85231,#85232,#85233,
#85234,#85235,#85236,#85237,#85238),.UNSPECIFIED.,.F.,.F.,(4,1,1,1,1,1,
1,4),(-192.588308255582,-191.906906597138,-190.907391458612,-189.907876320085,
-188.908361181558,-187.908846043031,-186.909330904505,-186.305122948402),
 .UNSPECIFIED.);
#7889=B_SPLINE_CURVE_WITH_KNOTS('',3,(#85240,#85241,#85242,#85243,#85244,
#85245,#85246,#85247,#85248,#85249,#85250,#85251,#85252,#85253,#85254,#85255,
#85256,#85257,#85258,#85259,#85260,#85261,#85262,#85263,#85264,#85265,#85266,
#85267,#85268,#85269,#85270,#85271,#85272,#85273,#85274,#85275,#85276,#85277,
#85278,#85279,#85280,#85281,#85282,#85283,#85284,#85285,#85286,#85287,#85288,
#85289,#85290,#85291,#85292,#85293,#85294,#85295,#85296,#85297,#85298,#85299,
#85300,#85301,#85302,#85303,#85304,#85305,#85306,#85307,#85308,#85309,#85310,
#85311,#85312,#85313,#85314,#85315,#85316,#85317,#85318,#85319,#85320,#85321,
#85322,#85323,#85324,#85325,#85326,#85327,#85328,#85329,#85330,#85331,#85332,
#85333,#85334,#85335,#85336,#85337,#85338,#85339,#85340,#85341,#85342,#85343,
#85344,#85345,#85346,#85347,#85348,#85349,#85350,#85351,#85352,#85353,#85354,
#85355,#85356,#85357,#85358,#85359,#85360,#85361,#85362,#85363,#85364,#85365,
#85366,#85367,#85368,#85369,#85370,#85371,#85372,#85373,#85374,#85375,#85376,
#85377,#85378,#85379,#85380,#85381,#85382,#85383,#85384,#85385,#85386,#85387,
#85388,#85389,#85390,#85391,#85392,#85393,#85394,#85395,#85396,#85397,#85398,
#85399,#85400,#85401,#85402,#85403,#85404,#85405,#85406,#85407,#85408,#85409,
#85410,#85411,#85412,#85413,#85414,#85415,#85416,#85417,#85418,#85419,#85420,
#85421,#85422,#85423,#85424,#85425,#85426,#85427,#85428,#85429,#85430,#85431,
#85432,#85433,#85434,#85435,#85436,#85437,#85438,#85439,#85440,#85441,#85442,
#85443,#85444,#85445,#85446,#85447,#85448,#85449,#85450,#85451,#85452,#85453,
#85454,#85455,#85456,#85457,#85458,#85459,#85460,#85461,#85462,#85463,#85464,
#85465),.UNSPECIFIED.,.F.,.F.,(4,3,3,3,3,3,3,3,3,3,3,3,3,3,3,3,3,3,3,3,
3,3,3,3,3,3,3,3,3,3,3,3,3,3,3,3,3,3,3,3,3,3,3,3,3,3,3,3,3,3,3,3,3,3,3,3,
3,3,3,3,3,3,3,3,3,3,3,3,3,3,3,3,3,3,3,4),(-186.305122719083,-186.206295980807,
-186.108059058831,-186.008937412404,-185.909815765978,-185.82126136454,
-185.73282167681,-185.644472901617,-185.552701367347,-185.464454832775,
-185.376221714559,-185.28798064652,-185.199710261892,-185.11133953104,-185.022909279753,
-184.934348809657,-184.910300627451,-184.821746226013,-184.733306538283,
-184.64495776309,-184.55318622882,-184.464939694248,-184.376706576032,-184.288465507994,
-184.200195123365,-184.111824392513,-184.023394141226,-183.93483367113,
-183.910785488924,-183.822231087486,-183.733791399757,-183.645442624565,
-183.553671090294,-183.465424555722,-183.377191437507,-183.288950369469,
-183.200679984841,-183.112309253989,-183.023879002703,-182.935318532607,
-182.911270350398,-182.82271594896,-182.734276261231,-182.645927486038,
-182.554155951767,-182.465909417195,-182.377676298979,-182.289435230941,
-182.201164846313,-182.112794115461,-182.024363864175,-181.935803394079,
-181.911755211871,-181.823200810433,-181.734761122703,-181.64641234751,
-181.554640813239,-181.466394278667,-181.378161160451,-181.289920092413,
-181.201649707785,-181.113278976933,-181.024848725646,-180.93628825555,
-180.912240073344,-180.824848370936,-180.737570403042,-180.648116307815,
-180.560991488546,-180.473898053107,-180.386813595069,-180.295594606608,
-180.208417027578,-180.121190868464,-180.033854467656,-180.021937641223),
 .UNSPECIFIED.);
#7890=B_SPLINE_CURVE_WITH_KNOTS('',3,(#85467,#85468,#85469,#85470,#85471,
#85472,#85473,#85474,#85475,#85476,#85477),.UNSPECIFIED.,.F.,.F.,(4,1,1,
1,1,1,1,1,4),(-180.021937641223,-179.912724934817,-178.913209796291,-177.913694657764,
-176.914179519237,-175.91466438071,-174.915149242184,-173.915634103657,
-173.738752334043),.UNSPECIFIED.);
#7891=B_SPLINE_CURVE_WITH_KNOTS('',3,(#85479,#85480,#85481,#85482,#85483,
#85484,#85485,#85486,#85487,#85488,#85489,#85490,#85491,#85492,#85493,#85494,
#85495,#85496,#85497,#85498,#85499,#85500,#85501,#85502,#85503,#85504,#85505,
#85506,#85507,#85508,#85509,#85510,#85511,#85512,#85513,#85514,#85515,#85516,
#85517,#85518,#85519,#85520,#85521,#85522,#85523,#85524,#85525,#85526,#85527,
#85528,#85529,#85530,#85531,#85532,#85533,#85534,#85535,#85536,#85537,#85538,
#85539,#85540,#85541,#85542,#85543,#85544,#85545,#85546,#85547,#85548,#85549,
#85550,#85551,#85552,#85553,#85554,#85555,#85556,#85557,#85558,#85559,#85560,
#85561,#85562,#85563,#85564,#85565,#85566,#85567,#85568,#85569,#85570,#85571,
#85572,#85573,#85574,#85575,#85576,#85577,#85578,#85579,#85580,#85581,#85582,
#85583,#85584,#85585,#85586,#85587,#85588,#85589,#85590,#85591,#85592,#85593,
#85594,#85595,#85596,#85597,#85598,#85599,#85600,#85601,#85602,#85603,#85604,
#85605,#85606,#85607,#85608,#85609,#85610,#85611,#85612,#85613,#85614,#85615,
#85616,#85617,#85618,#85619,#85620,#85621,#85622,#85623,#85624,#85625,#85626,
#85627,#85628,#85629,#85630,#85631,#85632,#85633,#85634,#85635,#85636,#85637,
#85638,#85639,#85640,#85641,#85642,#85643,#85644,#85645,#85646,#85647,#85648,
#85649,#85650,#85651,#85652,#85653,#85654,#85655,#85656,#85657,#85658,#85659,
#85660,#85661,#85662,#85663,#85664,#85665,#85666,#85667,#85668,#85669,#85670,
#85671,#85672,#85673,#85674,#85675,#85676,#85677,#85678,#85679,#85680,#85681,
#85682,#85683,#85684,#85685,#85686,#85687,#85688,#85689,#85690,#85691,#85692,
#85693,#85694,#85695,#85696,#85697,#85698,#85699,#85700,#85701,#85702,#85703,
#85704),.UNSPECIFIED.,.F.,.F.,(4,3,3,3,3,3,3,3,3,3,3,3,3,3,3,3,3,3,3,3,
3,3,3,3,3,3,3,3,3,3,3,3,3,3,3,3,3,3,3,3,3,3,3,3,3,3,3,3,3,3,3,3,3,3,3,3,
3,3,3,3,3,3,3,3,3,3,3,3,3,3,3,3,3,3,3,4),(-173.738752334043,-173.651651184399,
-173.564633597389,-173.477670273051,-173.390733687792,-173.303801330066,
-173.216850695373,-173.129809112975,-173.0427157747,-172.955491530016,-172.91611896513,
-172.827564563692,-172.739124875963,-172.65077610077,-172.559004566499,
-172.470758031927,-172.382524913711,-172.294283845673,-172.206013461045,
-172.117642730193,-172.029212478907,-171.940652008811,-171.916603826603,
-171.828049425165,-171.739609737435,-171.651260962242,-171.559489427972,
-171.4712428934,-171.383009775184,-171.294768707145,-171.206498322517,-171.118127591665,
-171.029697340378,-170.941136870282,-170.917088688076,-170.828534286638,
-170.740094598909,-170.651745823717,-170.559974289446,-170.471727754874,
-170.383494636659,-170.295253568621,-170.206983183993,-170.118612453141,
-170.030182201854,-169.941621731759,-169.91757354955,-169.829019148112,
-169.740579460383,-169.65223068519,-169.560459150919,-169.472212616347,
-169.383979498132,-169.295738430094,-169.207468045466,-169.119097314613,
-169.030667063327,-168.942106593231,-168.918058411023,-168.829504009585,
-168.741064321855,-168.652715546662,-168.560944012392,-168.47269747782,
-168.384464359604,-168.296223291566,-168.207952906938,-168.119582176085,
-168.031151924799,-167.942591454702,-167.918543272496,-167.823739794189,
-167.729232464533,-167.634903277923,-167.54084246258,-167.45556722681),
 .UNSPECIFIED.);
#7892=B_SPLINE_CURVE_WITH_KNOTS('',3,(#85706,#85707,#85708,#85709,#85710,
#85711,#85712,#85713,#85714,#85715),.UNSPECIFIED.,.F.,.F.,(4,1,1,1,1,1,
1,4),(-167.455567026863,-166.919028133969,-165.919512995443,-164.919997856916,
-163.920482718389,-162.920967579862,-161.921452441336,-161.172381719684),
 .UNSPECIFIED.);
#7893=B_SPLINE_CURVE_WITH_KNOTS('',3,(#85717,#85718,#85719,#85720,#85721,
#85722,#85723,#85724,#85725,#85726,#85727,#85728,#85729,#85730,#85731,#85732,
#85733,#85734,#85735,#85736,#85737,#85738,#85739,#85740,#85741,#85742,#85743,
#85744,#85745,#85746,#85747,#85748,#85749,#85750,#85751,#85752,#85753,#85754,
#85755,#85756,#85757,#85758,#85759,#85760,#85761,#85762,#85763,#85764,#85765,
#85766,#85767,#85768,#85769,#85770,#85771,#85772,#85773,#85774,#85775,#85776,
#85777,#85778,#85779,#85780,#85781,#85782,#85783,#85784,#85785,#85786,#85787,
#85788,#85789,#85790,#85791,#85792,#85793,#85794,#85795,#85796,#85797,#85798,
#85799,#85800,#85801,#85802,#85803,#85804,#85805,#85806,#85807,#85808,#85809,
#85810,#85811,#85812,#85813,#85814,#85815,#85816,#85817,#85818,#85819,#85820,
#85821,#85822,#85823,#85824,#85825,#85826,#85827,#85828,#85829,#85830,#85831,
#85832,#85833,#85834,#85835,#85836,#85837,#85838,#85839,#85840,#85841,#85842,
#85843,#85844,#85845,#85846,#85847,#85848,#85849,#85850,#85851,#85852,#85853,
#85854,#85855,#85856,#85857,#85858,#85859,#85860,#85861,#85862,#85863,#85864,
#85865,#85866,#85867,#85868,#85869,#85870,#85871,#85872,#85873,#85874,#85875,
#85876,#85877,#85878,#85879,#85880,#85881,#85882,#85883,#85884,#85885,#85886,
#85887,#85888,#85889,#85890,#85891,#85892,#85893,#85894,#85895,#85896,#85897,
#85898,#85899,#85900,#85901,#85902,#85903,#85904,#85905,#85906,#85907,#85908,
#85909,#85910,#85911,#85912,#85913,#85914,#85915,#85916,#85917,#85918,#85919,
#85920,#85921,#85922,#85923,#85924,#85925,#85926,#85927,#85928,#85929,#85930,
#85931,#85932,#85933,#85934,#85935,#85936,#85937,#85938,#85939,#85940,#85941,
#85942,#85943,#85944,#85945),.UNSPECIFIED.,.F.,.F.,(4,3,3,3,3,3,3,3,3,3,
3,3,3,3,3,3,3,3,3,3,3,3,3,3,3,3,3,3,3,3,3,3,3,3,3,3,3,3,3,3,3,3,3,3,3,3,
3,3,3,3,3,3,3,3,3,3,3,3,3,3,3,3,3,3,3,3,3,3,3,3,3,3,3,3,3,3,4),(-161.172381610342,
-161.059073294057,-160.943174354892,-160.921937302809,-160.833382901371,
-160.744943213641,-160.656594438448,-160.564822904177,-160.476576369605,
-160.38834325139,-160.300102183351,-160.211831798723,-160.123461067871,
-160.035030816584,-159.946470346488,-159.922422164282,-159.833867762844,
-159.745428075115,-159.657079299922,-159.565307765651,-159.477061231079,
-159.388828112864,-159.300587044825,-159.212316660197,-159.123945929345,
-159.035515678059,-158.946955207963,-158.922907025755,-158.834352624317,
-158.745912936587,-158.657564161395,-158.565792627124,-158.477546092552,
-158.389312974336,-158.301071906298,-158.21280152167,-158.124430790818,
-158.036000539531,-157.947440069435,-157.923391887228,-157.83483748579,
-157.746397798061,-157.658049022869,-157.566277488598,-157.478030954026,
-157.389797835811,-157.301556767773,-157.213286383145,-157.124915652293,
-157.036485401007,-156.947924930911,-156.923876748702,-156.835322347264,
-156.746882659535,-156.658533884342,-156.566762350071,-156.478515815499,
-156.390282697283,-156.302041629245,-156.213771244617,-156.125400513765,
-156.036970262479,-155.948409792383,-155.924361610175,-155.835807208737,
-155.747367521008,-155.659018745815,-155.567247211544,-155.479000676972,
-155.390767558756,-155.302526490718,-155.21425610609,-155.125885375237,
-155.037455123951,-154.948894653855,-154.924846471648,-154.889196412504),
 .UNSPECIFIED.);
#7894=B_SPLINE_CURVE_WITH_KNOTS('',3,(#85947,#85948,#85949,#85950,#85951,
#85952,#85953,#85954,#85955,#85956,#85957,#85958,#85959,#85960,#85961,#85962,
#85963,#85964,#85965,#85966,#85967,#85968,#85969,#85970,#85971,#85972,#85973,
#85974,#85975,#85976,#85977,#85978,#85979,#85980,#85981,#85982,#85983,#85984,
#85985,#85986,#85987,#85988,#85989,#85990,#85991,#85992,#85993,#85994,#85995,
#85996,#85997,#85998,#85999,#86000,#86001,#86002,#86003,#86004,#86005,#86006,
#86007,#86008,#86009,#86010,#86011,#86012,#86013,#86014,#86015,#86016,#86017,
#86018,#86019,#86020,#86021,#86022,#86023,#86024,#86025,#86026,#86027,#86028,
#86029,#86030,#86031,#86032,#86033,#86034,#86035,#86036,#86037,#86038,#86039,
#86040,#86041,#86042,#86043,#86044,#86045,#86046,#86047,#86048,#86049,#86050,
#86051,#86052,#86053,#86054,#86055,#86056,#86057,#86058,#86059,#86060,#86061,
#86062,#86063,#86064,#86065,#86066,#86067,#86068,#86069,#86070,#86071,#86072,
#86073,#86074,#86075,#86076,#86077,#86078,#86079,#86080,#86081,#86082,#86083,
#86084,#86085,#86086,#86087,#86088,#86089,#86090,#86091,#86092,#86093,#86094,
#86095,#86096,#86097,#86098,#86099,#86100,#86101,#86102,#86103,#86104,#86105,
#86106,#86107,#86108,#86109,#86110,#86111,#86112,#86113,#86114,#86115,#86116,
#86117,#86118,#86119,#86120,#86121,#86122,#86123,#86124,#86125,#86126,#86127,
#86128,#86129,#86130,#86131,#86132,#86133,#86134,#86135,#86136,#86137,#86138,
#86139,#86140,#86141,#86142,#86143,#86144,#86145,#86146,#86147,#86148,#86149,
#86150,#86151,#86152,#86153,#86154,#86155,#86156,#86157,#86158,#86159,#86160,
#86161,#86162,#86163,#86164,#86165,#86166,#86167,#86168,#86169),
 .UNSPECIFIED.,.F.,.F.,(4,3,3,3,3,3,3,3,3,3,3,3,3,3,3,3,3,3,3,3,3,3,3,3,
3,3,3,3,3,3,3,3,3,3,3,3,3,3,3,3,3,3,3,3,3,3,3,3,3,3,3,3,3,3,3,3,3,3,3,3,
3,3,3,3,3,3,3,3,3,3,3,3,3,3,4),(-154.889196412254,-154.801158728298,-154.713233796906,
-154.625397253078,-154.537622184238,-154.449879442421,-154.362147142838,
-154.274403413472,-154.186569833671,-154.098691851588,-154.010667087164,
-153.925331333121,-153.836776931683,-153.748337243954,-153.659988468762,
-153.568216934491,-153.479970399919,-153.391737281704,-153.303496213666,
-153.215225829038,-153.126855098186,-153.038424846899,-152.949864376804,
-152.925816194595,-152.837261793157,-152.748822105428,-152.660473330235,
-152.568701795964,-152.480455261392,-152.392222143177,-152.303981075138,
-152.21571069051,-152.127339959658,-152.038909708372,-151.950349238276,
-151.926301056068,-151.83774665463,-151.7493069669,-151.660958191708,-151.569186657437,
-151.480940122865,-151.392707004649,-151.30446593661,-151.216195551982,
-151.12782482113,-151.039394569843,-150.950834099747,-150.926785917541,
-150.838231516103,-150.749791828374,-150.661443053181,-150.56967151891,
-150.481424984338,-150.393191866122,-150.304950798084,-150.216680413455,
-150.128309682603,-150.039879431317,-149.951318961221,-149.927270779014,
-149.838716377576,-149.750276689847,-149.661927914655,-149.570156380384,
-149.481909845812,-149.393676727597,-149.305435659559,-149.217165274931,
-149.128794544079,-149.040364292792,-148.951803822697,-148.927755640488,
-148.822446806093,-148.714229065279,-148.606011324466),.UNSPECIFIED.);
#7895=B_SPLINE_CURVE_WITH_KNOTS('',3,(#86171,#86172,#86173,#86174,#86175,
#86176,#86177,#86178,#86179,#86180),.UNSPECIFIED.,.F.,.F.,(4,1,1,1,1,1,
1,4),(-148.606011105325,-147.928240501961,-146.928725363434,-145.929210224907,
-144.929695086381,-143.930179947854,-142.930664809327,-142.322825798145),
 .UNSPECIFIED.);
#7896=B_SPLINE_CURVE_WITH_KNOTS('',3,(#86182,#86183,#86184,#86185,#86186,
#86187,#86188,#86189,#86190,#86191),.UNSPECIFIED.,.F.,.F.,(4,1,1,1,1,1,
1,4),(-142.322825798145,-141.9311496708,-140.931634532274,-139.932119393747,
-138.93260425522,-137.933089116693,-136.933573978166,-136.039640490966),
 .UNSPECIFIED.);
#7897=B_SPLINE_CURVE_WITH_KNOTS('',3,(#86193,#86194,#86195,#86196,#86197,
#86198,#86199,#86200,#86201,#86202,#86203),.UNSPECIFIED.,.F.,.F.,(4,1,1,
1,1,1,1,1,4),(-136.039640490966,-135.93405883964,-134.934543701113,-133.935028562586,
-132.935513424059,-131.935998285533,-130.936483147006,-129.936968008479,
-129.756455183786),.UNSPECIFIED.);
#7898=B_SPLINE_CURVE_WITH_KNOTS('',3,(#86205,#86206,#86207,#86208,#86209,
#86210,#86211,#86212,#86213,#86214,#86215,#86216,#86217,#86218,#86219,#86220,
#86221,#86222,#86223,#86224,#86225,#86226,#86227,#86228,#86229,#86230,#86231,
#86232,#86233,#86234,#86235,#86236,#86237,#86238,#86239,#86240,#86241,#86242,
#86243,#86244,#86245,#86246,#86247,#86248,#86249,#86250,#86251,#86252,#86253,
#86254,#86255,#86256,#86257,#86258,#86259,#86260,#86261,#86262,#86263,#86264,
#86265,#86266,#86267,#86268,#86269,#86270,#86271,#86272,#86273,#86274,#86275,
#86276,#86277,#86278,#86279,#86280,#86281,#86282,#86283,#86284,#86285,#86286,
#86287,#86288,#86289,#86290,#86291,#86292,#86293,#86294,#86295,#86296,#86297,
#86298,#86299,#86300,#86301,#86302,#86303,#86304,#86305,#86306,#86307,#86308,
#86309,#86310,#86311,#86312,#86313,#86314,#86315,#86316,#86317,#86318,#86319,
#86320,#86321,#86322,#86323,#86324,#86325,#86326,#86327,#86328,#86329,#86330,
#86331,#86332,#86333,#86334,#86335,#86336,#86337,#86338,#86339,#86340,#86341,
#86342,#86343,#86344,#86345,#86346,#86347,#86348,#86349,#86350,#86351,#86352,
#86353,#86354,#86355,#86356,#86357,#86358,#86359,#86360,#86361,#86362,#86363,
#86364,#86365,#86366,#86367,#86368,#86369,#86370,#86371,#86372,#86373,#86374,
#86375,#86376,#86377,#86378,#86379,#86380,#86381,#86382,#86383,#86384,#86385,
#86386,#86387,#86388,#86389,#86390,#86391,#86392,#86393,#86394,#86395,#86396,
#86397,#86398,#86399,#86400,#86401,#86402,#86403,#86404,#86405,#86406,#86407,
#86408,#86409,#86410,#86411,#86412,#86413,#86414,#86415,#86416,#86417,#86418,
#86419,#86420,#86421,#86422,#86423,#86424,#86425,#86426,#86427,#86428,#86429,
#86430),.UNSPECIFIED.,.F.,.F.,(4,3,3,3,3,3,3,3,3,3,3,3,3,3,3,3,3,3,3,3,
3,3,3,3,3,3,3,3,3,3,3,3,3,3,3,3,3,3,3,3,3,3,3,3,3,3,3,3,3,3,3,3,3,3,3,3,
3,3,3,3,3,3,3,3,3,3,3,3,3,3,3,3,3,3,3,4),(-129.756455183786,-129.66935498244,
-129.577867218379,-129.490904202965,-129.403965797651,-129.317029494613,
-129.230072791103,-129.143023997227,-129.05592154166,-128.968690340322,
-128.937452869952,-128.848898468514,-128.760458780785,-128.672110005592,
-128.580338471322,-128.49209193675,-128.403858818535,-128.315617750497,
-128.227347365869,-128.138976635018,-128.050546383731,-127.961985913635,
-127.937937731426,-127.849383329988,-127.760943642259,-127.672594867066,
-127.580823332796,-127.492576798224,-127.404343680008,-127.31610261197,
-127.227832227342,-127.13946149649,-127.051031245203,-126.962470775107,
-126.938422592899,-126.849868191461,-126.761428503731,-126.673079728539,
-126.581308194268,-126.493061659696,-126.40482854148,-126.316587473442,
-126.228317088813,-126.139946357961,-126.051516106674,-125.962955636579,
-125.938907454372,-125.850353052934,-125.761913365205,-125.673564590012,
-125.581793055741,-125.493546521169,-125.405313402953,-125.317072334915,
-125.228801950287,-125.140431219435,-125.052000968148,-124.963440498052,
-124.939392315845,-124.850837914407,-124.762398226678,-124.674049451486,
-124.582277917215,-124.494031382643,-124.405798264428,-124.31755719639,
-124.229286811762,-124.14091608091,-124.052485829624,-123.963925359529,
-123.939877177319,-123.845254519537,-123.750922331933,-123.656763961693,
-123.562866404263,-123.473270057579),.UNSPECIFIED.);
#7899=B_SPLINE_CURVE_WITH_KNOTS('',3,(#86432,#86433,#86434,#86435,#86436,
#86437,#86438,#86439,#86440,#86441),.UNSPECIFIED.,.F.,.F.,(4,1,1,1,1,1,
1,4),(-123.473269876606,-122.940362038792,-121.940846900265,-120.941331761738,
-119.941816623212,-118.942301484685,-117.942786346158,-117.190084569427),
 .UNSPECIFIED.);
#7900=B_SPLINE_CURVE_WITH_KNOTS('',3,(#86443,#86444,#86445,#86446,#86447,
#86448,#86449,#86450,#86451,#86452,#86453,#86454,#86455,#86456,#86457,#86458,
#86459,#86460,#86461,#86462,#86463,#86464,#86465,#86466,#86467,#86468,#86469,
#86470,#86471,#86472,#86473,#86474,#86475,#86476,#86477,#86478,#86479,#86480,
#86481,#86482,#86483,#86484,#86485,#86486,#86487,#86488,#86489,#86490,#86491,
#86492,#86493,#86494,#86495,#86496,#86497,#86498,#86499,#86500,#86501,#86502,
#86503,#86504,#86505,#86506,#86507,#86508,#86509,#86510,#86511,#86512,#86513,
#86514,#86515,#86516,#86517,#86518,#86519,#86520,#86521,#86522,#86523,#86524,
#86525,#86526,#86527,#86528,#86529,#86530,#86531,#86532,#86533,#86534,#86535,
#86536,#86537,#86538,#86539,#86540,#86541,#86542,#86543,#86544,#86545,#86546,
#86547,#86548,#86549,#86550,#86551,#86552,#86553,#86554,#86555,#86556,#86557,
#86558,#86559,#86560,#86561,#86562,#86563,#86564,#86565,#86566,#86567,#86568,
#86569,#86570,#86571,#86572,#86573,#86574,#86575,#86576,#86577,#86578,#86579,
#86580,#86581,#86582,#86583,#86584,#86585,#86586,#86587,#86588,#86589,#86590,
#86591,#86592,#86593,#86594,#86595,#86596,#86597,#86598,#86599,#86600,#86601,
#86602,#86603,#86604,#86605,#86606,#86607,#86608,#86609,#86610,#86611,#86612,
#86613,#86614,#86615,#86616,#86617,#86618,#86619,#86620,#86621,#86622,#86623,
#86624,#86625,#86626,#86627,#86628,#86629,#86630,#86631,#86632,#86633,#86634,
#86635,#86636,#86637,#86638,#86639,#86640,#86641,#86642,#86643,#86644,#86645,
#86646,#86647,#86648,#86649,#86650,#86651,#86652,#86653,#86654,#86655,#86656,
#86657,#86658,#86659,#86660,#86661,#86662,#86663,#86664,#86665,#86666,#86667,
#86668,#86669,#86670,#86671),.UNSPECIFIED.,.F.,.F.,(4,3,3,3,3,3,3,3,3,3,
3,3,3,3,3,3,3,3,3,3,3,3,3,3,3,3,3,3,3,3,3,3,3,3,3,3,3,3,3,3,3,3,3,3,3,3,
3,3,3,3,3,3,3,3,3,3,3,3,3,3,3,3,3,3,3,3,3,3,3,3,3,3,3,3,3,3,4),(-117.190084482236,
-117.076148942948,-116.959487829622,-116.943271207631,-116.854716806193,
-116.766277118464,-116.677928343272,-116.586156809001,-116.497910274429,
-116.409677156214,-116.321436088176,-116.233165703548,-116.144794972696,
-116.05636472141,-115.967804251314,-115.943756069104,-115.855201667666,
-115.766761979937,-115.678413204744,-115.586641670474,-115.498395135902,
-115.410162017687,-115.321920949649,-115.233650565021,-115.145279834169,
-115.056849582883,-114.968289112787,-114.944240930578,-114.85568652914,
-114.767246841411,-114.678898066218,-114.587126531947,-114.498879997375,
-114.410646879159,-114.322405811121,-114.234135426493,-114.145764695641,
-114.057334444354,-113.968773974258,-113.944725792051,-113.856171390613,
-113.767731702883,-113.679382927691,-113.58761139342,-113.499364858848,
-113.411131740632,-113.322890672594,-113.234620287966,-113.146249557113,
-113.057819305827,-112.969258835731,-112.945210653524,-112.856656252086,
-112.768216564357,-112.679867789164,-112.588096254893,-112.499849720321,
-112.411616602105,-112.323375534067,-112.235105149439,-112.146734418587,
-112.0583041673,-111.969743697204,-111.945695514997,-111.857141113559,-111.76870142583,
-111.680352650638,-111.588581116367,-111.500334581795,-111.41210146358,
-111.323860395542,-111.235590010914,-111.147219280062,-111.058789028776,
-110.97022855868,-110.946180376471,-110.906899262247),.UNSPECIFIED.);
#7901=B_SPLINE_CURVE_WITH_KNOTS('',3,(#86673,#86674,#86675,#86676,#86677,
#86678,#86679,#86680,#86681,#86682),.UNSPECIFIED.,.F.,.F.,(4,1,1,1,1,1,
1,4),(-110.906894042246,-109.946665237944,-108.947150099417,-107.94763496089,
-106.948119822364,-105.948604683837,-104.94908954531,-104.623720933803),
 .UNSPECIFIED.);
#7902=B_SPLINE_CURVE_WITH_KNOTS('',3,(#86684,#86685,#86686,#86687,#86688,
#86689,#86690,#86691,#86692,#86693,#86694,#86695,#86696,#86697,#86698,#86699,
#86700,#86701,#86702,#86703,#86704,#86705,#86706,#86707,#86708,#86709,#86710,
#86711,#86712,#86713,#86714,#86715,#86716,#86717,#86718,#86719,#86720,#86721,
#86722,#86723,#86724,#86725,#86726,#86727,#86728,#86729,#86730,#86731,#86732,
#86733,#86734,#86735,#86736,#86737,#86738,#86739,#86740,#86741,#86742,#86743,
#86744,#86745,#86746,#86747,#86748,#86749,#86750,#86751,#86752,#86753,#86754,
#86755,#86756,#86757,#86758,#86759,#86760,#86761,#86762,#86763,#86764,#86765,
#86766,#86767,#86768,#86769,#86770,#86771,#86772,#86773,#86774,#86775,#86776,
#86777,#86778,#86779,#86780,#86781,#86782,#86783,#86784,#86785,#86786,#86787,
#86788,#86789,#86790,#86791,#86792,#86793,#86794,#86795,#86796,#86797,#86798,
#86799,#86800,#86801,#86802,#86803,#86804,#86805,#86806,#86807,#86808,#86809,
#86810,#86811,#86812,#86813,#86814,#86815,#86816,#86817,#86818,#86819,#86820,
#86821,#86822,#86823,#86824,#86825,#86826,#86827,#86828,#86829,#86830,#86831,
#86832,#86833,#86834,#86835,#86836,#86837,#86838,#86839,#86840,#86841,#86842,
#86843,#86844,#86845,#86846,#86847,#86848,#86849,#86850,#86851,#86852,#86853,
#86854,#86855,#86856,#86857,#86858,#86859,#86860,#86861,#86862,#86863,#86864,
#86865,#86866,#86867,#86868,#86869,#86870,#86871,#86872,#86873,#86874,#86875,
#86876,#86877,#86878,#86879,#86880,#86881,#86882,#86883,#86884,#86885,#86886,
#86887,#86888,#86889,#86890,#86891,#86892,#86893,#86894,#86895,#86896,#86897,
#86898,#86899,#86900,#86901,#86902,#86903,#86904,#86905,#86906,#86907,#86908,
#86909),.UNSPECIFIED.,.F.,.F.,(4,3,3,3,3,3,3,3,3,3,3,3,3,3,3,3,3,3,3,3,
3,3,3,3,3,3,3,3,3,3,3,3,3,3,3,3,3,3,3,3,3,3,3,3,3,3,3,3,3,3,3,3,3,3,3,3,
3,3,3,3,3,3,3,3,3,3,3,3,3,3,3,3,3,3,3,4),(-104.623713955068,-104.535644705966,
-104.447593713946,-104.359539482352,-104.271460517181,-104.183279470856,
-104.095042939218,-104.006661658045,-103.949574406783,-103.861020005345,
-103.772580317616,-103.684231542424,-103.592460008153,-103.504213473581,
-103.415980355366,-103.327739287328,-103.239468902701,-103.151098171849,
-103.062667920562,-102.974107450467,-102.950059268257,-102.861504866819,
-102.77306517909,-102.684716403897,-102.592944869626,-102.504698335054,
-102.416465216839,-102.3282241488,-102.239953764172,-102.15158303332,-102.063152782034,
-101.974592311938,-101.95054412973,-101.861989728292,-101.773550040562,
-101.685201265369,-101.593429731098,-101.505183196526,-101.41695007831,
-101.328709010272,-101.240438625644,-101.152067894791,-101.063637643504,
-100.975077173408,-100.951028991203,-100.862474589765,-100.774034902036,
-100.685686126843,-100.593914592572,-100.505668058,-100.417434939784,-100.329193871746,
-100.240923487118,-100.152552756266,-100.064122504979,-99.9755620348834,
-99.9515138526763,-99.8629594512383,-99.774519763509,-99.686170988316,-99.5943994540452,
-99.5061529194733,-99.4179198012576,-99.3296787332196,-99.241408348592,
-99.15303761774,-99.0646073664534,-98.9760468963575,-98.9519987141495,-98.862422794307,
-98.7729691408607,-98.6836176547323,-98.5943606830314,-98.5051598633551,
-98.4159876281948,-98.3405286478881),.UNSPECIFIED.);
#7903=B_SPLINE_CURVE_WITH_KNOTS('',3,(#86911,#86912,#86913,#86914,#86915,
#86916,#86917,#86918,#86919,#86920),.UNSPECIFIED.,.F.,.F.,(4,1,1,1,1,1,
1,4),(-98.3405213020582,-97.9524835756228,-96.952968437096,-95.9534532985692,
-94.9539381600425,-93.9544230215157,-92.9549078829889,-92.057352313836),
 .UNSPECIFIED.);
#7904=B_SPLINE_CURVE_WITH_KNOTS('',3,(#86922,#86923,#86924,#86925,#86926,
#86927,#86928,#86929,#86930,#86931,#86932,#86933,#86934,#86935,#86936,#86937,
#86938,#86939,#86940,#86941,#86942,#86943,#86944,#86945,#86946,#86947,#86948,
#86949,#86950,#86951,#86952,#86953,#86954,#86955,#86956,#86957,#86958,#86959,
#86960,#86961,#86962,#86963,#86964,#86965,#86966,#86967,#86968,#86969,#86970,
#86971,#86972,#86973,#86974,#86975,#86976,#86977,#86978,#86979,#86980,#86981,
#86982,#86983,#86984,#86985,#86986,#86987,#86988,#86989,#86990,#86991,#86992,
#86993,#86994,#86995,#86996,#86997,#86998,#86999,#87000,#87001,#87002,#87003,
#87004,#87005,#87006,#87007,#87008,#87009,#87010,#87011,#87012,#87013,#87014,
#87015,#87016,#87017,#87018,#87019,#87020,#87021,#87022,#87023,#87024,#87025,
#87026,#87027,#87028,#87029,#87030,#87031,#87032,#87033,#87034,#87035,#87036,
#87037,#87038,#87039,#87040,#87041,#87042,#87043,#87044,#87045,#87046,#87047,
#87048,#87049,#87050,#87051,#87052,#87053,#87054,#87055,#87056,#87057,#87058,
#87059,#87060,#87061,#87062,#87063,#87064,#87065,#87066,#87067,#87068,#87069,
#87070,#87071,#87072,#87073,#87074,#87075,#87076,#87077,#87078,#87079,#87080,
#87081,#87082,#87083,#87084,#87085,#87086,#87087,#87088,#87089,#87090,#87091,
#87092,#87093,#87094,#87095,#87096,#87097,#87098,#87099,#87100,#87101,#87102,
#87103,#87104,#87105,#87106,#87107,#87108,#87109,#87110,#87111,#87112,#87113,
#87114,#87115,#87116,#87117,#87118,#87119,#87120,#87121,#87122,#87123,#87124,
#87125,#87126,#87127,#87128,#87129,#87130,#87131,#87132,#87133,#87134,#87135,
#87136,#87137,#87138,#87139,#87140,#87141,#87142,#87143,#87144,#87145,#87146,
#87147),.UNSPECIFIED.,.F.,.F.,(4,3,3,3,3,3,3,3,3,3,3,3,3,3,3,3,3,3,3,3,
3,3,3,3,3,3,3,3,3,3,3,3,3,3,3,3,3,3,3,3,3,3,3,3,3,3,3,3,3,3,3,3,3,3,3,3,
3,3,3,3,3,3,3,3,3,3,3,3,3,3,3,3,3,3,3,4),(-92.0573433407085,-91.9553927444622,
-91.8668383430241,-91.7783986552946,-91.6900498801017,-91.5982783458309,
-91.5100318112589,-91.421798693043,-91.3335576250045,-91.2452872403763,
-91.1569165095242,-91.0684862582373,-90.9799257881413,-90.9558776059354,
-90.8673232044974,-90.7788835167681,-90.6905347415753,-90.5987632073045,
-90.5105166727327,-90.422283554517,-90.3340424864788,-90.2457721018508,
-90.1574013709988,-90.0689711197121,-89.9804106496163,-89.9563624674086,
-89.8678080659707,-89.7793683782414,-89.6910196030486,-89.5992480687778,
-89.5110015342059,-89.4227684159903,-89.3345273479521,-89.2462569633242,
-89.1578862324723,-89.0694559811856,-88.9808955110898,-88.9568473288819,
-88.8682929274439,-88.7798532397146,-88.6915044645217,-88.5997329302509,
-88.511486395679,-88.4232532774634,-88.3350122094251,-88.2467418247971,
-88.1583710939451,-88.0699408426584,-87.9813803725626,-87.9573321903551,
-87.8687777889171,-87.7803381011878,-87.6919893259951,-87.6002177917242,
-87.5119712571524,-87.4237381389367,-87.3354970708985,-87.2472266862704,
-87.1588559554184,-87.0704257041317,-86.9818652340359,-86.9578170518284,
-86.8692626503904,-86.780822962661,-86.6924741874681,-86.6007026531973,
-86.5124561186254,-86.4242230004098,-86.3359819323716,-86.2477115477435,
-86.1593408168916,-86.0709105656049,-85.9823500955091,-85.9583019133016,
-85.8255508273588,-85.7741580335289),.UNSPECIFIED.);
#7905=B_SPLINE_CURVE_WITH_KNOTS('',3,(#87149,#87150,#87151,#87152,#87153,
#87154,#87155,#87156,#87157,#87158),.UNSPECIFIED.,.F.,.F.,(4,1,1,1,1,1,
1,4),(-85.7741532391098,-84.9587867747748,-83.9592716362481,-82.9597564977213,
-81.9602413591946,-80.9607262206678,-79.961211082141,-79.4909727263493),
 .UNSPECIFIED.);
#7906=B_SPLINE_CURVE_WITH_KNOTS('',3,(#87160,#87161,#87162,#87163,#87164,
#87165,#87166,#87167,#87168,#87169),.UNSPECIFIED.,.F.,.F.,(4,1,1,1,1,1,
1,4),(-79.4909727263493,-78.9616959436142,-77.9621808050875,-76.9626656665607,
-75.963150528034,-74.9636353895072,-73.9641202509805,-73.2077874191697),
 .UNSPECIFIED.);
#7907=B_SPLINE_CURVE_WITH_KNOTS('',3,(#87171,#87172,#87173,#87174,#87175,
#87176,#87177,#87178,#87179,#87180,#87181,#87182,#87183,#87184,#87185,#87186,
#87187,#87188,#87189,#87190,#87191,#87192,#87193,#87194,#87195,#87196,#87197,
#87198,#87199,#87200,#87201,#87202,#87203,#87204,#87205,#87206,#87207,#87208,
#87209,#87210,#87211,#87212,#87213,#87214,#87215,#87216,#87217,#87218,#87219,
#87220,#87221,#87222,#87223,#87224,#87225,#87226,#87227,#87228,#87229,#87230,
#87231,#87232,#87233,#87234,#87235,#87236,#87237,#87238,#87239,#87240,#87241,
#87242,#87243,#87244,#87245,#87246,#87247,#87248,#87249,#87250,#87251,#87252,
#87253,#87254,#87255,#87256,#87257,#87258,#87259,#87260,#87261,#87262,#87263,
#87264,#87265,#87266,#87267,#87268,#87269,#87270,#87271,#87272,#87273,#87274,
#87275,#87276,#87277,#87278,#87279,#87280,#87281,#87282,#87283,#87284,#87285,
#87286,#87287,#87288,#87289,#87290,#87291,#87292,#87293,#87294,#87295,#87296,
#87297,#87298,#87299,#87300,#87301,#87302,#87303,#87304,#87305,#87306,#87307,
#87308,#87309,#87310,#87311,#87312,#87313,#87314,#87315,#87316,#87317,#87318,
#87319,#87320,#87321,#87322,#87323,#87324,#87325,#87326,#87327,#87328,#87329,
#87330,#87331,#87332,#87333,#87334,#87335,#87336,#87337,#87338,#87339,#87340,
#87341,#87342,#87343,#87344,#87345,#87346,#87347,#87348,#87349,#87350,#87351,
#87352,#87353,#87354,#87355,#87356,#87357,#87358,#87359,#87360,#87361,#87362,
#87363,#87364,#87365,#87366,#87367,#87368,#87369,#87370,#87371,#87372,#87373,
#87374,#87375,#87376,#87377,#87378,#87379,#87380,#87381,#87382,#87383,#87384,
#87385,#87386,#87387,#87388,#87389,#87390,#87391,#87392,#87393,#87394,#87395,
#87396,#87397,#87398,#87399),.UNSPECIFIED.,.F.,.F.,(4,3,3,3,3,3,3,3,3,3,
3,3,3,3,3,3,3,3,3,3,3,3,3,3,3,3,3,3,3,3,3,3,3,3,3,3,3,3,3,3,3,3,3,3,3,3,
3,3,3,3,3,3,3,3,3,3,3,3,3,3,3,3,3,3,3,3,3,3,3,3,3,3,3,3,3,3,4),(-73.2077873547606,
-73.0932049597969,-72.9757514791561,-72.9646051124537,-72.8760507110156,
-72.7876110232862,-72.6992622480933,-72.6074907138225,-72.5192441792505,
-72.4310110610349,-72.3427699929966,-72.2544996083684,-72.1661288775164,
-72.0776986262297,-71.9891381561337,-71.9650899739269,-71.8765355724889,
-71.7880958847597,-71.6997471095669,-71.6079755752961,-71.5197290407243,
-71.4314959225087,-71.3432548544705,-71.2549844698426,-71.1666137389907,
-71.0781834877041,-70.9896230176082,-70.9655748354002,-70.8770204339622,
-70.7885807462329,-70.7002319710401,-70.6084604367693,-70.5202139021974,
-70.4319807839818,-70.3437397159435,-70.2554693313156,-70.1670986004636,
-70.0786683491769,-69.9901078790811,-69.9660596968734,-69.8775052954354,
-69.789065607706,-69.7007168325132,-69.6089452982423,-69.5206987636705,
-69.4324656454548,-69.3442245774165,-69.2559541927885,-69.1675834619365,
-69.0791532106498,-68.9905927405539,-68.9665445583466,-68.8779901569086,
-68.7895504691793,-68.7012016939865,-68.6094301597157,-68.5211836251439,
-68.4329505069282,-68.34470943889,-68.256439054262,-68.16806832341,-68.0796380721234,
-67.9910776020276,-67.9670294198199,-67.8784750183819,-67.7900353306526,
-67.7016865554598,-67.609915021189,-67.5216684866171,-67.4334353684015,
-67.3451943003633,-67.2569239157355,-67.1685531848836,-67.080122933597,
-66.9915624635012,-66.9675142812931,-66.9246021119901),.UNSPECIFIED.);
#7908=B_SPLINE_CURVE_WITH_KNOTS('',3,(#87401,#87402,#87403,#87404,#87405,
#87406,#87407,#87408,#87409,#87410),.UNSPECIFIED.,.F.,.F.,(4,1,1,1,1,1,
1,4),(-66.9245965145714,-65.9679991427663,-64.9684840042396,-63.9689688657128,
-62.9694537271861,-61.9699385886593,-60.9704234501325,-60.6414239154789),
 .UNSPECIFIED.);
#7909=B_SPLINE_CURVE_WITH_KNOTS('',3,(#87412,#87413,#87414,#87415,#87416,
#87417,#87418,#87419,#87420,#87421,#87422,#87423,#87424,#87425,#87426,#87427,
#87428,#87429,#87430,#87431,#87432,#87433,#87434,#87435,#87436,#87437,#87438,
#87439,#87440,#87441,#87442,#87443,#87444,#87445,#87446,#87447,#87448,#87449,
#87450,#87451,#87452,#87453,#87454,#87455,#87456,#87457,#87458,#87459,#87460,
#87461,#87462,#87463,#87464,#87465,#87466,#87467,#87468,#87469,#87470,#87471,
#87472,#87473,#87474,#87475,#87476,#87477,#87478,#87479,#87480,#87481,#87482,
#87483,#87484,#87485,#87486,#87487,#87488,#87489,#87490,#87491,#87492,#87493,
#87494,#87495,#87496,#87497,#87498,#87499,#87500,#87501,#87502,#87503,#87504,
#87505,#87506,#87507,#87508,#87509,#87510,#87511,#87512,#87513,#87514,#87515,
#87516,#87517,#87518,#87519,#87520,#87521,#87522,#87523,#87524,#87525,#87526,
#87527,#87528,#87529,#87530,#87531,#87532,#87533,#87534,#87535,#87536,#87537,
#87538,#87539,#87540,#87541,#87542,#87543,#87544,#87545,#87546,#87547,#87548,
#87549,#87550,#87551,#87552,#87553,#87554,#87555,#87556,#87557,#87558,#87559,
#87560,#87561,#87562,#87563,#87564,#87565,#87566,#87567,#87568,#87569,#87570,
#87571,#87572,#87573,#87574,#87575,#87576,#87577,#87578,#87579,#87580,#87581,
#87582,#87583,#87584,#87585,#87586,#87587,#87588,#87589,#87590,#87591,#87592,
#87593,#87594,#87595,#87596,#87597,#87598,#87599,#87600,#87601,#87602,#87603,
#87604,#87605,#87606,#87607,#87608,#87609,#87610,#87611,#87612,#87613,#87614,
#87615,#87616,#87617,#87618,#87619,#87620,#87621,#87622,#87623,#87624,#87625,
#87626,#87627,#87628,#87629,#87630,#87631,#87632,#87633,#87634,#87635,#87636,
#87637),.UNSPECIFIED.,.F.,.F.,(4,3,3,3,3,3,3,3,3,3,3,3,3,3,3,3,3,3,3,3,
3,3,3,3,3,3,3,3,3,3,3,3,3,3,3,3,3,3,3,3,3,3,3,3,3,3,3,3,3,3,3,3,3,3,3,3,
3,3,3,3,3,3,3,3,3,3,3,3,3,3,3,3,3,3,3,4),(-60.6414168048105,-60.553296060957,
-60.4651918097365,-60.3770826180884,-60.2889470544044,-60.2007081252582,
-60.1124123690869,-60.0239725402644,-59.9709083116058,-59.8823539101678,
-59.7939142224383,-59.7055654472453,-59.6137939129745,-59.5255473784026,
-59.4373142601871,-59.3490731921489,-59.2608028075208,-59.1724320766688,
-59.0840018253821,-58.9954413552862,-58.971393173079,-58.882838771641,-58.7943990839117,
-58.7060503087186,-58.6142787744478,-58.526032239876,-58.4377991216604,
-58.3495580536221,-58.2612876689941,-58.1729169381422,-58.0844866868554,
-57.9959262167595,-57.9718780345522,-57.8833236331142,-57.7948839453851,
-57.7065351701922,-57.6147636359213,-57.5265171013496,-57.4382839831339,
-57.3500429150957,-57.2617725304679,-57.173401799616,-57.0849715483293,
-56.9964110782334,-56.9723628960255,-56.8838084945875,-56.795368806858,
-56.707020031665,-56.6152484973942,-56.5270019628223,-56.4387688446066,
-56.3505277765684,-56.2622573919405,-56.1738866610886,-56.0854564098019,
-55.9968959397059,-55.9728477574987,-55.8842933560608,-55.7958536683313,
-55.7075048931387,-55.6157333588678,-55.527486824296,-55.4392537060804,
-55.3510126380422,-55.2627422534145,-55.1743715225625,-55.0859412712757,
-54.99738080118,-54.973332618972,-54.8838398296381,-54.7944684518599,-54.7051982540858,
-54.6160204771488,-54.5268978074483,-54.4378006945073,-54.3582314976309),
 .UNSPECIFIED.);
#7910=B_SPLINE_CURVE_WITH_KNOTS('',3,(#87639,#87640,#87641,#87642,#87643,
#87644,#87645,#87646,#87647,#87648),.UNSPECIFIED.,.F.,.F.,(4,1,1,1,1,1,
1,4),(-54.3582240635315,-53.9738174804452,-52.9743023419184,-51.9747872033917,
-50.9752720648649,-49.9757569263381,-48.9762417878114,-48.075055138789),
 .UNSPECIFIED.);
#7911=B_SPLINE_CURVE_WITH_KNOTS('',3,(#87650,#87651,#87652,#87653,#87654,
#87655,#87656,#87657,#87658,#87659,#87660,#87661,#87662,#87663,#87664,#87665,
#87666,#87667,#87668,#87669,#87670,#87671,#87672,#87673,#87674,#87675,#87676,
#87677,#87678,#87679,#87680,#87681,#87682,#87683,#87684,#87685,#87686,#87687,
#87688,#87689,#87690,#87691,#87692,#87693,#87694,#87695,#87696,#87697,#87698,
#87699,#87700,#87701,#87702,#87703,#87704,#87705,#87706,#87707,#87708,#87709,
#87710,#87711,#87712,#87713,#87714,#87715,#87716,#87717,#87718,#87719,#87720,
#87721,#87722,#87723,#87724,#87725,#87726,#87727,#87728,#87729,#87730,#87731,
#87732,#87733,#87734,#87735,#87736,#87737,#87738,#87739,#87740,#87741,#87742,
#87743,#87744,#87745,#87746,#87747,#87748,#87749,#87750,#87751,#87752,#87753,
#87754,#87755,#87756,#87757,#87758,#87759,#87760,#87761,#87762,#87763,#87764,
#87765,#87766,#87767,#87768,#87769,#87770,#87771,#87772,#87773,#87774,#87775,
#87776,#87777,#87778,#87779,#87780,#87781,#87782,#87783,#87784,#87785,#87786,
#87787,#87788,#87789,#87790,#87791,#87792,#87793,#87794,#87795,#87796,#87797,
#87798,#87799,#87800,#87801,#87802,#87803,#87804,#87805,#87806,#87807,#87808,
#87809,#87810,#87811,#87812,#87813,#87814,#87815,#87816,#87817,#87818,#87819,
#87820,#87821,#87822,#87823,#87824,#87825,#87826,#87827,#87828,#87829,#87830,
#87831,#87832,#87833,#87834,#87835,#87836,#87837,#87838,#87839,#87840,#87841,
#87842,#87843,#87844,#87845,#87846,#87847,#87848,#87849,#87850,#87851,#87852,
#87853,#87854,#87855,#87856,#87857,#87858,#87859,#87860,#87861,#87862,#87863,
#87864,#87865,#87866,#87867,#87868,#87869,#87870,#87871,#87872,#87873,#87874,
#87875),.UNSPECIFIED.,.F.,.F.,(4,3,3,3,3,3,3,3,3,3,3,3,3,3,3,3,3,3,3,3,
3,3,3,3,3,3,3,3,3,3,3,3,3,3,3,3,3,3,3,3,3,3,3,3,3,3,3,3,3,3,3,3,3,3,3,3,
3,3,3,3,3,3,3,3,3,3,3,3,3,3,3,3,3,3,3,4),(-48.0750461904513,-47.9767266492846,
-47.8881722478465,-47.7997325601169,-47.7113837849239,-47.6196122506532,
-47.5313657160812,-47.4431325978654,-47.3548915298271,-47.266621145199,
-47.1782504143468,-47.08982016306,-47.001259692964,-46.9772115107578,-46.8886571093199,
-46.8002174215906,-46.7118686463979,-46.620097112127,-46.5318505775552,
-46.4436174593396,-46.3553763913014,-46.2671060066735,-46.1787352758216,
-46.090305024535,-46.0017445544392,-45.9776963722311,-45.8891419707931,
-45.8007022830638,-45.712353507871,-45.6205819736002,-45.5323354390283,
-45.4441023208127,-45.3558612527744,-45.2675908681464,-45.1792201372944,
-45.0907898860077,-45.0022294159119,-44.9781812337043,-44.8896268322663,
-44.801187144537,-44.7128383693442,-44.6210668350733,-44.5328203005015,
-44.4445871822858,-44.3563461142475,-44.2680757296195,-44.1797049987675,
-44.0912747474808,-44.002714277385,-43.9786660951776,-43.8901116937396,
-43.8016720060103,-43.7133232308176,-43.6215516965467,-43.5333051619749,
-43.4450720437592,-43.3568309757211,-43.2685605910932,-43.1801898602412,
-43.0917596089546,-43.0031991388587,-42.9791509566508,-42.8905965552128,
-42.8021568674835,-42.7138080922906,-42.6220365580198,-42.533790023448,
-42.4455569052323,-42.357315837194,-42.2690454525658,-42.1806747217138,
-42.0922444704272,-42.0036840003312,-41.979635818124,-41.8482965029249,
-41.7918608832718),.UNSPECIFIED.);
#7912=B_SPLINE_CURVE_WITH_KNOTS('',3,(#87877,#87878,#87879,#87880,#87881,
#87882,#87883,#87884,#87885,#87886),.UNSPECIFIED.,.F.,.F.,(4,1,1,1,1,1,
1,4),(-41.7918564217168,-40.9801206795973,-39.9806055410705,-38.9810904025437,
-37.981575264017,-36.9820601254902,-35.9825449869635,-35.5086755760922),
 .UNSPECIFIED.);
#7913=B_SPLINE_CURVE_WITH_KNOTS('',3,(#87888,#87889,#87890,#87891,#87892,
#87893,#87894,#87895,#87896,#87897),.UNSPECIFIED.,.F.,.F.,(4,1,1,1,1,1,
1,4),(-35.5086755760922,-34.9830298484367,-33.9835147099099,-32.9839995713832,
-31.9844844328564,-30.9849692943296,-29.9854541558029,-29.2254902689126),
 .UNSPECIFIED.);
#7914=B_SPLINE_CURVE_WITH_KNOTS('',3,(#87899,#87900,#87901,#87902,#87903,
#87904,#87905,#87906,#87907,#87908,#87909,#87910,#87911,#87912,#87913,#87914,
#87915,#87916,#87917,#87918,#87919,#87920,#87921,#87922,#87923,#87924,#87925,
#87926,#87927,#87928,#87929,#87930,#87931,#87932,#87933,#87934,#87935,#87936,
#87937,#87938,#87939,#87940,#87941,#87942,#87943,#87944,#87945,#87946,#87947,
#87948,#87949,#87950,#87951,#87952,#87953,#87954,#87955,#87956,#87957,#87958,
#87959,#87960,#87961,#87962,#87963,#87964,#87965,#87966,#87967,#87968,#87969,
#87970,#87971,#87972,#87973,#87974,#87975,#87976,#87977,#87978,#87979,#87980,
#87981,#87982,#87983,#87984,#87985,#87986,#87987,#87988,#87989,#87990,#87991,
#87992,#87993,#87994,#87995,#87996,#87997,#87998,#87999,#88000,#88001,#88002,
#88003,#88004,#88005,#88006,#88007,#88008,#88009,#88010,#88011,#88012,#88013,
#88014,#88015,#88016,#88017,#88018,#88019,#88020,#88021,#88022,#88023,#88024,
#88025,#88026,#88027,#88028,#88029,#88030,#88031,#88032,#88033,#88034,#88035,
#88036,#88037,#88038,#88039,#88040,#88041,#88042,#88043,#88044,#88045,#88046,
#88047,#88048,#88049,#88050,#88051,#88052,#88053,#88054,#88055,#88056,#88057,
#88058,#88059,#88060,#88061,#88062,#88063,#88064,#88065,#88066,#88067,#88068,
#88069,#88070,#88071,#88072,#88073,#88074,#88075,#88076,#88077,#88078,#88079,
#88080,#88081,#88082,#88083,#88084,#88085,#88086,#88087,#88088,#88089,#88090,
#88091,#88092,#88093,#88094,#88095,#88096,#88097,#88098,#88099,#88100,#88101,
#88102,#88103,#88104,#88105,#88106,#88107,#88108,#88109,#88110,#88111,#88112,
#88113,#88114,#88115,#88116,#88117,#88118,#88119,#88120,#88121,#88122,#88123,
#88124),.UNSPECIFIED.,.F.,.F.,(4,3,3,3,3,3,3,3,3,3,3,3,3,3,3,3,3,3,3,3,
3,3,3,3,3,3,3,3,3,3,3,3,3,3,3,3,3,3,3,3,3,3,3,3,3,3,3,3,3,3,3,3,3,3,3,3,
3,3,3,3,3,3,3,3,3,3,3,3,3,3,3,3,3,3,3,4),(-29.2254902272523,-29.1057146222642,
-28.9859390172761,-28.8973846158514,-28.8089449281353,-28.7205961529556,
-28.6288246186798,-28.5405780841208,-28.4523449659179,-28.3641038978923,
-28.2758335132768,-28.187462782437,-28.0990325311624,-28.0104720610784,
-27.9864238787494,-27.8978694773265,-27.8094297896124,-27.7210810144349,
-27.6293094801583,-27.5410629456021,-27.4528298274022,-27.3645887593798,
-27.2763183747675,-27.1879476439314,-27.0995173926606,-27.0109569225804,
-26.9869087402226,-26.8983543387054,-26.8099146508967,-26.7215658756244,
-26.6297943413833,-26.5415478067323,-26.4533146884377,-26.3650736203208,
-26.2768032356146,-26.1884325046853,-26.1000022533219,-26.0114417831506,
-25.9873936016958,-25.8988392003665,-25.8103995127456,-25.7220507376609,
-25.6302792033494,-25.542032668884,-25.453799550774,-25.3655584828405,-25.2772880983163,
-25.1889173675661,-25.1004871163802,-25.0119266463829,-24.9878784631691,
-24.899324061796,-24.8108843741328,-24.7225355990072,-24.6307640647116,
-24.5425175302093,-24.4542844120639,-24.3660433440966,-24.2777729595402,
-24.1894022287601,-24.1009719775459,-24.0124115075223,-23.9883633246423,
-23.8998089226723,-23.8113692344095,-23.7230204586822,-23.6312489246113,
-23.5430023895063,-23.4547692707586,-23.3665282021903,-23.2782578170346,
-23.1898870856612,-23.1014568338562,-23.0128963632503,-22.9888481861155,
-22.942304961733),.UNSPECIFIED.);
#7915=B_SPLINE_CURVE_WITH_KNOTS('',3,(#88126,#88127,#88128,#88129,#88130,
#88131,#88132,#88133,#88134,#88135),.UNSPECIFIED.,.F.,.F.,(4,1,1,1,1,1,
1,4),(-22.9422988168085,-21.9893330475888,-20.989817909062,-19.9903027705353,
-18.9907876320085,-17.9912724934817,-16.991757354955,-16.6591268838038),
 .UNSPECIFIED.);
#7916=B_SPLINE_CURVE_WITH_KNOTS('',3,(#88137,#88138,#88139,#88140,#88141,
#88142,#88143,#88144,#88145,#88146,#88147,#88148,#88149,#88150,#88151,#88152,
#88153,#88154,#88155,#88156,#88157,#88158,#88159,#88160,#88161,#88162,#88163,
#88164,#88165,#88166,#88167,#88168,#88169,#88170,#88171,#88172,#88173,#88174,
#88175,#88176,#88177,#88178,#88179,#88180,#88181,#88182,#88183,#88184,#88185,
#88186,#88187,#88188,#88189,#88190,#88191,#88192,#88193,#88194,#88195,#88196,
#88197,#88198,#88199,#88200,#88201,#88202,#88203,#88204,#88205,#88206,#88207,
#88208,#88209,#88210,#88211,#88212,#88213,#88214,#88215,#88216,#88217,#88218,
#88219,#88220,#88221,#88222,#88223,#88224,#88225,#88226,#88227,#88228,#88229,
#88230,#88231,#88232,#88233,#88234,#88235,#88236,#88237,#88238,#88239,#88240,
#88241,#88242,#88243,#88244,#88245,#88246,#88247,#88248,#88249,#88250,#88251,
#88252,#88253,#88254,#88255,#88256,#88257,#88258,#88259,#88260,#88261,#88262,
#88263,#88264,#88265,#88266,#88267,#88268,#88269,#88270,#88271,#88272,#88273,
#88274,#88275,#88276,#88277,#88278,#88279,#88280,#88281,#88282,#88283,#88284,
#88285,#88286,#88287,#88288,#88289,#88290,#88291,#88292,#88293,#88294,#88295,
#88296,#88297,#88298,#88299,#88300,#88301,#88302,#88303,#88304,#88305,#88306,
#88307,#88308,#88309,#88310,#88311,#88312,#88313,#88314,#88315,#88316,#88317,
#88318,#88319,#88320,#88321,#88322,#88323,#88324,#88325,#88326,#88327,#88328,
#88329,#88330,#88331,#88332,#88333,#88334,#88335,#88336,#88337,#88338,#88339,
#88340,#88341,#88342,#88343,#88344,#88345,#88346,#88347,#88348,#88349,#88350,
#88351,#88352,#88353,#88354,#88355,#88356,#88357,#88358,#88359,#88360,#88361,
#88362),.UNSPECIFIED.,.F.,.F.,(4,3,3,3,3,3,3,3,3,3,3,3,3,3,3,3,3,3,3,3,
3,3,3,3,3,3,3,3,3,3,3,3,3,3,3,3,3,3,3,3,3,3,3,3,3,3,3,3,3,3,3,3,3,3,3,3,
3,3,3,3,3,3,3,3,3,3,3,3,3,3,3,3,3,3,3,4),(-16.6591196545534,-16.5709460304396,
-16.4827871038465,-16.3946215082956,-16.3064278775447,-16.2181295773855,
-16.1297730926494,-16.0412731937529,-15.9922422164282,-15.9036877940136,
-15.8152480856589,-15.7268992902101,-15.6351277636715,-15.5468812098802,
-15.4586480728573,-15.3704069864418,-15.2821365838848,-15.1937658358538,
-15.1053355678029,-15.0167750816777,-14.9927270779014,-14.9041725382909,
-14.8157327116674,-14.7273837970277,-14.6356123148211,-14.5473656403005,
-14.4591323821879,-14.3708911744529,-14.2826206504764,-14.1942497814962,
-14.1058193926208,-14.0172587867959,-13.9932119393747,-13.9046579005256,
-13.8162185755933,-13.7278701629882,-13.6360984927206,-13.5478523179822,
-13.4596195579839,-13.3713788461756,-13.2831088154164,-13.1947384331657,
-13.1063085278465,-13.0177483971823,-12.9936968008479,-12.9051421549328,
-12.8167022249362,-12.7283532099315,-12.6365817664802,-12.548334999631,
-12.4601016522911,-12.3718603585081,-12.2835897517449,-12.195218805191,
-12.106788341677,-12.0182276660702,-11.9941816623212,-11.90562643978,-11.8171859256139,
-11.7288363196698,-11.6370650951853,-11.5488177243544,-11.4605837692713,
-11.3723418646475,-11.284070644607,-11.195699084313,-11.107268006035,-11.0187067189732,
-10.9946665237944,-10.9052576557781,-10.815969374525,-10.7267813186863,
-10.6376836161944,-10.5486400098947,-10.4596189026895,-10.3759343473738),
 .UNSPECIFIED.);
#7917=B_SPLINE_CURVE_WITH_KNOTS('',3,(#88363,#88364,#88365,#88366,#88367,
#88368,#88369,#88370,#88371,#88372),.UNSPECIFIED.,.F.,.F.,(4,1,1,1,1,1,
1,4),(-10.375926835712,-9.99515138526762,-8.99563624674086,-7.9961211082141,
-6.99660596968734,-5.99709083116058,-4.99757569263381,-4.09275795343756),
 .UNSPECIFIED.);
#7918=B_SPLINE_CURVE_WITH_KNOTS('',3,(#88375,#88376,#88377,#88378,#88379,
#88380),.UNSPECIFIED.,.F.,.F.,(4,1,1,4),(252.308677356644,252.498362612705,
253.497877751232,254.469000888742),.UNSPECIFIED.);
#7919=B_SPLINE_CURVE_WITH_KNOTS('',3,(#88382,#88383,#88384,#88385,#88386,
#88387,#88388,#88389,#88390,#88391,#88392,#88393,#88394,#88395,#88396,#88397,
#88398,#88399,#88400,#88401,#88402,#88403,#88404,#88405,#88406,#88407,#88408,
#88409,#88410,#88411,#88412,#88413,#88414,#88415,#88416,#88417,#88418,#88419,
#88420,#88421,#88422,#88423,#88424,#88425,#88426,#88427,#88428,#88429,#88430,
#88431,#88432,#88433,#88434,#88435,#88436,#88437,#88438,#88439,#88440,#88441,
#88442,#88443,#88444,#88445,#88446,#88447,#88448,#88449,#88450,#88451),
 .UNSPECIFIED.,.F.,.F.,(4,3,3,3,3,3,3,3,3,3,3,3,3,3,3,3,3,3,3,3,3,3,3,4),
(254.469004940773,254.497392889758,254.590649119483,254.68377880781,254.77680936004,
254.869770298601,254.962694927233,255.055607864379,255.148533712202,255.241555262876,
255.334626953852,255.427849487097,255.496908028285,255.589205413268,255.681379450479,
255.775485081436,255.867500738229,255.959486608717,256.051468320863,256.147157365181,
256.239259819415,256.331422968314,256.423718068013,256.434224498135),
 .UNSPECIFIED.);
#7920=B_SPLINE_CURVE_WITH_KNOTS('',3,(#88455,#88456,#88457,#88458,#88459,
#88460,#88461,#88462,#88463,#88464,#88465,#88466,#88467,#88468,#88469,#88470,
#88471,#88472,#88473,#88474,#88475,#88476,#88477,#88478,#88479,#88480,#88481,
#88482,#88483,#88484),.UNSPECIFIED.,.F.,.F.,(4,2,2,2,2,2,2,2,2,2,2,2,2,
2,4),(8.65291084783846E-5,0.077874969031854,0.0827087440970379,0.0857834642134888,
0.0886858313289599,0.0910799432465732,0.0938706143043208,0.0986813974108899,
0.117540885301815,0.170467162182005,0.225402500043114,0.23121802579301,
0.233440203541218,0.234288768021479,0.235068244192406),.UNSPECIFIED.);
#7921=B_SPLINE_CURVE_WITH_KNOTS('',3,(#88485,#88486,#88487,#88488,#88489,
#88490,#88491,#88492,#88493,#88494,#88495,#88496,#88497,#88498,#88499,#88500,
#88501,#88502,#88503,#88504,#88505,#88506,#88507,#88508,#88509,#88510,#88511,
#88512,#88513,#88514,#88515,#88516,#88517,#88518,#88519,#88520,#88521,#88522,
#88523,#88524,#88525,#88526,#88527,#88528,#88529,#88530,#88531,#88532,#88533,
#88534,#88535,#88536,#88537,#88538,#88539,#88540,#88541,#88542,#88543,#88544,
#88545,#88546,#88547,#88548,#88549,#88550,#88551,#88552,#88553,#88554,#88555,
#88556,#88557),.UNSPECIFIED.,.F.,.F.,(4,3,3,3,3,3,3,3,3,3,3,3,3,3,3,3,3,
3,3,3,3,3,3,3,4),(252.310073042627,252.403124865208,252.496086135635,252.588989817175,
252.681865086057,252.77473659135,252.867628972223,252.960624120039,253.053676529113,
253.146877714681,253.195941688915,253.288011824282,253.379955289568,253.471800843291,
253.563583111008,253.655333096758,253.747076606481,253.838839435191,253.930714929871,
254.022647931948,254.11475605418,254.195456827442,254.323775817272,254.448100230519,
254.468996577584),.UNSPECIFIED.);
#7922=B_SPLINE_CURVE_WITH_KNOTS('',3,(#88569,#88570,#88571,#88572,#88573,
#88574,#88575,#88576,#88577,#88578,#88579,#88580,#88581,#88582,#88583,#88584,
#88585,#88586,#88587,#88588,#88589,#88590,#88591,#88592,#88593,#88594,#88595,
#88596,#88597,#88598,#88599,#88600,#88601,#88602,#88603,#88604,#88605,#88606,
#88607,#88608,#88609,#88610,#88611,#88612,#88613,#88614,#88615,#88616,#88617,
#88618,#88619,#88620,#88621,#88622,#88623,#88624,#88625,#88626,#88627,#88628,
#88629,#88630,#88631,#88632,#88633,#88634,#88635,#88636,#88637,#88638,#88639,
#88640,#88641,#88642,#88643,#88644,#88645,#88646,#88647,#88648,#88649,#88650,
#88651,#88652,#88653,#88654,#88655,#88656,#88657,#88658,#88659,#88660,#88661,
#88662),.UNSPECIFIED.,.F.,.F.,(4,3,3,3,3,3,3,3,3,3,3,3,3,3,3,3,3,3,3,3,
3,3,3,3,3,3,3,3,3,3,3,4),(-0.733254803425731,-0.716860866713633,-0.679748362314261,
-0.642635857914888,-0.636142894777821,-0.600007081989827,-0.56382585245897,
-0.553070625843985,-0.54406265969124,-0.537131974197663,-0.501769106615608,
-0.46673168776426,-0.43271025548486,-0.39921344459524,-0.394763476316668,
-0.361144611505345,-0.341796862292531,-0.307536621934649,-0.28230306870699,
-0.26968629209316,-0.261838674652597,-0.25706951547933,-0.223658877959798,
-0.190162157167782,-0.157167270601885,-0.13748660874309,-0.127812017122585,
-0.123152698597241,-0.090954045835124,-0.059210042099216,-0.0284424625824032,
0.),.UNSPECIFIED.);
#7923=B_SPLINE_CURVE_WITH_KNOTS('',3,(#88663,#88664,#88665,#88666,#88667,
#88668,#88669,#88670,#88671,#88672,#88673,#88674,#88675,#88676,#88677,#88678,
#88679,#88680,#88681,#88682,#88683,#88684,#88685,#88686,#88687,#88688,#88689,
#88690,#88691,#88692,#88693,#88694,#88695,#88696,#88697,#88698,#88699,#88700,
#88701,#88702,#88703,#88704,#88705,#88706,#88707,#88708,#88709,#88710,#88711,
#88712,#88713,#88714,#88715,#88716,#88717,#88718,#88719,#88720,#88721,#88722,
#88723,#88724,#88725,#88726,#88727,#88728,#88729,#88730,#88731,#88732,#88733,
#88734,#88735,#88736,#88737,#88738,#88739,#88740,#88741,#88742,#88743,#88744,
#88745,#88746,#88747,#88748,#88749,#88750,#88751,#88752,#88753,#88754,#88755,
#88756),.UNSPECIFIED.,.F.,.F.,(4,3,3,3,3,3,3,3,3,3,3,3,3,3,3,3,3,3,3,3,
3,3,3,3,3,3,3,3,3,3,3,4),(-0.744397949170787,-0.724090770909356,-0.692915940750181,
-0.673393480001504,-0.66080333861376,-0.655138471145222,-0.623098446486558,
-0.590256033718165,-0.579287000783627,-0.573000422069116,-0.567857258151979,
-0.534328239229759,-0.500402513905905,-0.466554389450806,-0.444853816956689,
-0.43717569305135,-0.432782155152661,-0.397866775303715,-0.379066408601939,
-0.345035254109968,-0.311004099617997,-0.300241994933858,-0.295254487285989,
-0.26002895078779,-0.224649697158664,-0.188790758835381,-0.154352341293194,
-0.14704631389687,-0.110284735422653,-0.0734773653247291,-0.0367386826623646,
0.),.UNSPECIFIED.);
#7924=B_SPLINE_CURVE_WITH_KNOTS('',3,(#89758,#89759,#89760,#89761),
 .UNSPECIFIED.,.F.,.F.,(4,4),(-0.0803409632413212,0.),.UNSPECIFIED.);
#7925=B_SPLINE_CURVE_WITH_KNOTS('',3,(#89762,#89763,#89764,#89765,#89766,
#89767,#89768,#89769,#89770,#89771,#89772,#89773,#89774,#89775,#89776,#89777,
#89778,#89779,#89780,#89781,#89782,#89783,#89784,#89785,#89786,#89787,#89788,
#89789,#89790,#89791,#89792,#89793,#89794,#89795,#89796,#89797,#89798,#89799,
#89800,#89801,#89802,#89803,#89804,#89805,#89806,#89807,#89808,#89809,#89810,
#89811,#89812,#89813,#89814,#89815,#89816,#89817,#89818,#89819,#89820,#89821,
#89822,#89823,#89824,#89825,#89826,#89827,#89828,#89829,#89830,#89831,#89832,
#89833,#89834,#89835,#89836,#89837,#89838,#89839,#89840,#89841,#89842,#89843,
#89844,#89845,#89846,#89847,#89848,#89849,#89850,#89851,#89852,#89853,#89854,
#89855),.UNSPECIFIED.,.F.,.F.,(4,3,3,3,3,3,3,3,3,3,3,3,3,3,3,3,3,3,3,3,
3,3,3,3,3,3,3,3,3,3,3,4),(-0.744397949170576,-0.724090770909119,-0.692447050614166,
-0.660803330319212,-0.655138464383618,-0.623098432155756,-0.590256016159068,
-0.579286988813744,-0.573000381486176,-0.567857225037418,-0.534328202041861,
-0.500402475785612,-0.466554351992817,-0.444853787732292,-0.437346141655956,
-0.432781471426868,-0.397866091919205,-0.37906640860182,-0.345356387811567,
-0.311004091679875,-0.300241984011793,-0.291751811164854,-0.257317537005326,
-0.221788209983448,-0.185939475150322,-0.162697040756532,-0.153848887443103,
-0.146031932641978,-0.109290096749417,-0.0724860010487071,-0.0362430005243535,
0.),.UNSPECIFIED.);
#7926=B_SPLINE_CURVE_WITH_KNOTS('',3,(#89861,#89862,#89863,#89864,#89865,
#89866,#89867,#89868,#89869,#89870,#89871,#89872,#89873,#89874,#89875,#89876,
#89877,#89878,#89879,#89880,#89881,#89882,#89883,#89884,#89885,#89886,#89887,
#89888,#89889,#89890,#89891,#89892,#89893,#89894,#89895,#89896,#89897,#89898,
#89899,#89900,#89901,#89902,#89903,#89904,#89905,#89906,#89907,#89908,#89909,
#89910,#89911,#89912,#89913,#89914,#89915,#89916,#89917,#89918,#89919,#89920,
#89921,#89922,#89923,#89924,#89925,#89926,#89927,#89928,#89929,#89930,#89931,
#89932,#89933,#89934,#89935,#89936,#89937,#89938,#89939,#89940,#89941,#89942,
#89943,#89944,#89945),.UNSPECIFIED.,.F.,.F.,(4,3,3,3,3,3,3,3,3,3,3,3,3,
3,3,3,3,3,3,3,3,3,3,3,3,3,3,3,4),(-0.73325467290433,-0.716860866713702,
-0.679748364117748,-0.642635861521795,-0.636142895543889,-0.599983228880824,
-0.563846742146268,-0.544365777261658,-0.537678149333536,-0.502312771444872,
-0.467268175507533,-0.433239334102402,-0.399213462994925,-0.394763515206197,
-0.361144657010498,-0.341796862292533,-0.307557044899139,-0.273156786925689,
-0.262814068526211,-0.257069517219618,-0.223635413959772,-0.190149431339904,
-0.157260198228449,-0.127811989049523,-0.123152691782714,-0.0909540316151254,
-0.0592100170113393,-0.0284424232172037,-2.14959275585417E-14),
 .UNSPECIFIED.);
#7927=B_SPLINE_CURVE_WITH_KNOTS('',3,(#90946,#90947,#90948,#90949),
 .UNSPECIFIED.,.F.,.F.,(4,4),(0.,0.0803420936465104),.UNSPECIFIED.);
#7928=B_SPLINE_CURVE_WITH_KNOTS('',3,(#90986,#90987,#90988,#90989,#90990,
#90991,#90992,#90993,#90994,#90995),.UNSPECIFIED.,.F.,.F.,(4,2,2,2,4),(0.,
0.0198203077394276,0.0433989762369911,0.0727052081845461,0.108839631579722),
 .UNSPECIFIED.);
#7929=B_SPLINE_CURVE_WITH_KNOTS('',3,(#90999,#91000,#91001,#91002,#91003,
#91004,#91005,#91006,#91007,#91008),.UNSPECIFIED.,.F.,.F.,(4,2,2,2,4),(0.335564963946802,
0.371699387341978,0.401005619289533,0.424584287787096,0.444404595526524),
 .UNSPECIFIED.);
#7930=B_SPLINE_CURVE_WITH_KNOTS('',3,(#91015,#91016,#91017,#91018,#91019,
#91020,#91021,#91022,#91023,#91024,#91025,#91026),.UNSPECIFIED.,.F.,.F.,
(4,2,2,2,2,4),(0.,0.00831861880117899,0.0174994849977743,0.0424016409784866,
0.0803702669813532,0.139810685907233),.UNSPECIFIED.);
#7931=B_SPLINE_CURVE_WITH_KNOTS('',3,(#91030,#91031,#91032,#91033,#91034,
#91035,#91036,#91037),.UNSPECIFIED.,.F.,.F.,(4,2,2,4),(0.567555107088231,
0.577206887836704,0.594334223162494,0.613200757592396),.UNSPECIFIED.);
#7932=B_SPLINE_CURVE_WITH_KNOTS('',3,(#91039,#91040,#91041,#91042,#91043,
#91044,#91045,#91046),.UNSPECIFIED.,.F.,.F.,(4,2,2,4),(0.268421316333155,
0.291025391015721,0.313464123275544,0.318616532882621),.UNSPECIFIED.);
#7933=B_SPLINE_CURVE_WITH_KNOTS('',3,(#91057,#91058,#91059,#91060,#91061,
#91062,#91063,#91064),.UNSPECIFIED.,.F.,.F.,(4,2,2,4),(-0.373632853319188,
-0.370925235245078,-0.34375119436819,-0.312176495568083),.UNSPECIFIED.);
#7934=B_SPLINE_CURVE_WITH_KNOTS('',3,(#91066,#91067,#91068,#91069,#91070,
#91071,#91072,#91073),.UNSPECIFIED.,.F.,.F.,(4,2,2,4),(0.102055810558895,
0.10300662226153,0.123623520705077,0.14314601433674),.UNSPECIFIED.);
#7935=B_SPLINE_CURVE_WITH_KNOTS('',3,(#91076,#91077,#91078,#91079,#91080,
#91081,#91082,#91083,#91084,#91085,#91086,#91087,#91088,#91089,#91090,#91091,
#91092,#91093,#91094,#91095,#91096,#91097,#91098,#91099,#91100,#91101,#91102,
#91103),.UNSPECIFIED.,.F.,.F.,(4,3,3,3,3,3,3,3,3,4),(0.,0.0144825766165643,
0.0225740708747328,0.0346938168103142,0.0456054571019101,0.0576817551653054,
0.0695937263660513,0.0828019048720541,0.0960623063922353,0.0964246649222208),
 .UNSPECIFIED.);
#7936=B_SPLINE_CURVE_WITH_KNOTS('',3,(#91109,#91110,#91111,#91112,#91113,
#91114,#91115,#91116,#91117,#91118,#91119,#91120,#91121,#91122,#91123,#91124,
#91125,#91126,#91127,#91128,#91129,#91130,#91131,#91132,#91133,#91134,#91135,
#91136),.UNSPECIFIED.,.F.,.F.,(4,3,3,3,3,3,3,3,3,4),(-0.0962049341565272,
-0.0817008546465319,-0.0735973466051622,-0.0614596059708162,-0.0505317647059319,
-0.0384375364526582,-0.0265078790450698,-0.013280089798481,0.,0.000362896539003327),
 .UNSPECIFIED.);
#7937=B_SPLINE_CURVE_WITH_KNOTS('',3,(#91141,#91142,#91143,#91144,#91145,
#91146,#91147,#91148),.UNSPECIFIED.,.F.,.F.,(4,2,2,4),(0.620143406782201,
0.624498876460084,0.646574469367965,0.671320484075565),.UNSPECIFIED.);
#7938=B_SPLINE_CURVE_WITH_KNOTS('',3,(#91150,#91151,#91152,#91153,#91154,
#91155,#91156,#91157),.UNSPECIFIED.,.F.,.F.,(4,2,2,4),(-0.102413024431803,
-0.0708383256316961,-0.0436642847548089,-0.0409566666806992),
 .UNSPECIFIED.);
#7939=B_SPLINE_CURVE_WITH_KNOTS('',3,(#91164,#91165,#91166,#91167,#91168,
#91169,#91170,#91171),.UNSPECIFIED.,.F.,.F.,(4,2,2,4),(0.105220546930268,
0.118812208671315,0.137355851603631,0.150522503003572),.UNSPECIFIED.);
#7940=B_SPLINE_CURVE_WITH_KNOTS('',3,(#91175,#91176,#91177,#91178,#91179,
#91180,#91181,#91182,#91183,#91184,#91185,#91186),.UNSPECIFIED.,.F.,.F.,
(4,2,2,2,2,4),(0.481937503575851,0.54137792250173,0.579346548504597,0.604248704485309,
0.613429570681904,0.621748189483083),.UNSPECIFIED.);
#7941=B_SPLINE_CURVE_WITH_KNOTS('',3,(#91189,#91190,#91191,#91192,#91193,
#91194,#91195,#91196),.UNSPECIFIED.,.F.,.F.,(4,2,2,4),(0.0392364555962475,
0.0443888652033245,0.066827597463148,0.0894316721457135),.UNSPECIFIED.);
#7942=B_SPLINE_CURVE_WITH_KNOTS('',3,(#91255,#91256,#91257,#91258,#91259,
#91260,#91261,#91262,#91263,#91264),.UNSPECIFIED.,.F.,.F.,(4,2,2,2,4),(0.198387340813371,
0.203960430205622,0.218045744690312,0.232131059175001,0.241802651428953),
 .UNSPECIFIED.);
#7943=B_SPLINE_CURVE_WITH_KNOTS('',3,(#91281,#91282,#91283,#91284,#91285,
#91286),.UNSPECIFIED.,.F.,.F.,(4,2,4),(0.00719864469771614,0.0137080667973639,
0.0162984458358511),.UNSPECIFIED.);
#7944=B_SPLINE_CURVE_WITH_KNOTS('',3,(#91292,#91293,#91294,#91295,#91296,
#91297,#91298,#91299,#91300,#91301,#91302,#91303,#91304,#91305,#91306,#91307,
#91308,#91309,#91310),.UNSPECIFIED.,.F.,.F.,(4,2,2,2,3,2,2,2,4),(0.582619764185682,
0.587048813927463,0.608772997184351,0.63176112026293,0.65474924334151,0.67542743189983,
0.69610562045815,0.716170507416666,0.720537010002502),.UNSPECIFIED.);
#7945=B_SPLINE_CURVE_WITH_KNOTS('',3,(#91384,#91385,#91386,#91387,#91388,
#91389),.UNSPECIFIED.,.F.,.F.,(4,2,4),(-0.209156427629457,-0.206361653740428,
-0.198150656776162),.UNSPECIFIED.);
#7946=B_SPLINE_CURVE_WITH_KNOTS('',3,(#91418,#91419,#91420,#91421,#91422,
#91423,#91424,#91425,#91426,#91427),.UNSPECIFIED.,.F.,.F.,(4,2,2,2,4),(0.0519371314826972,
0.0616087237366522,0.0756940382213414,0.0897793527060307,0.0953524420982795),
 .UNSPECIFIED.);
#7947=B_SPLINE_CURVE_WITH_KNOTS('',3,(#91484,#91485,#91486,#91487,#91488,
#91489,#91490,#91491,#91492,#91493),.UNSPECIFIED.,.F.,.F.,(4,2,2,2,4),(0.198387340813371,
0.203960430205622,0.218045744690312,0.232131059175001,0.241802651428953),
 .UNSPECIFIED.);
#7948=B_SPLINE_CURVE_WITH_KNOTS('',3,(#91509,#91510,#91511,#91512,#91513,
#91514,#91515,#91516,#91517,#91518,#91519,#91520,#91521,#91522,#91523,#91524,
#91525,#91526,#91527,#91528,#91529,#91530,#91531,#91532,#91533,#91534,#91535,
#91536),.UNSPECIFIED.,.F.,.F.,(4,3,3,3,3,3,3,3,3,4),(-0.000362896539001219,
0.,0.0132800897984686,0.0265078790450441,0.0400863342838971,0.0505317647058842,
0.0641209451936965,0.0735973466050953,0.0904711570682583,0.0962049341564403),
 .UNSPECIFIED.);
#7949=B_SPLINE_CURVE_WITH_KNOTS('',3,(#91539,#91540,#91541,#91542,#91543,
#91544,#91545,#91546,#91547,#91548,#91549,#91550,#91551,#91552,#91553,#91554,
#91555,#91556,#91557,#91558,#91559,#91560,#91561,#91562,#91563,#91564,#91565,
#91566),.UNSPECIFIED.,.F.,.F.,(4,3,3,3,3,3,3,3,3,4),(-0.0964246649222091,
-0.0960623063922242,-0.0828019048720443,-0.0695937263660441,-0.0560354017445019,
-0.0456054571019059,-0.032036423132379,-0.0225740708747317,-0.00572527652771826,
0.),.UNSPECIFIED.);
#7950=B_SPLINE_CURVE_WITH_KNOTS('',3,(#91577,#91578,#91579,#91580,#91581,
#91582,#91583,#91584),.UNSPECIFIED.,.F.,.F.,(4,2,2,4),(-0.322668635476185,
-0.317356379278157,-0.294587204940379,-0.2718180306026),.UNSPECIFIED.);
#7951=B_SPLINE_CURVE_WITH_KNOTS('',3,(#91587,#91588,#91589,#91590,#91591,
#91592,#91593,#91594),.UNSPECIFIED.,.F.,.F.,(4,2,2,4),(-0.101192488668761,
-0.073104459771632,-0.045016430874503,-0.0417266688079848),
 .UNSPECIFIED.);
#7952=B_SPLINE_CURVE_WITH_KNOTS('',3,(#91598,#91599,#91600,#91601,#91602,
#91603,#91604,#91605),.UNSPECIFIED.,.F.,.F.,(4,2,2,4),(-0.35842166827265,
-0.355131906206132,-0.327043877309003,-0.298955848411874),.UNSPECIFIED.);
#7953=B_SPLINE_CURVE_WITH_KNOTS('',3,(#91608,#91609,#91610,#91611,#91612,
#91613,#91614,#91615),.UNSPECIFIED.,.F.,.F.,(4,2,2,4),(-0.0907502340909058,
-0.0679810597531271,-0.0452118854153484,-0.0398996293942076),
 .UNSPECIFIED.);
#7954=B_SPLINE_CURVE_WITH_KNOTS('',3,(#91633,#91634,#91635,#91636,#91637,
#91638,#91639,#91640,#91641,#91642,#91643),.UNSPECIFIED.,.F.,.F.,(4,1,1,
1,1,1,1,1,4),(0.,0.177176435663881,0.354352871327763,0.531529306991644,
0.708705742655525,0.885882178319406,1.06305861398329,1.18117623775921,1.24023145903364),
 .UNSPECIFIED.);
#7955=B_SPLINE_CURVE_WITH_KNOTS('',3,(#91644,#91645,#91646,#91647,#91648,
#91649,#91650,#91651,#91652,#91653,#91654),.UNSPECIFIED.,.F.,.F.,(4,1,1,
1,1,1,1,1,4),(1.24023145903364,1.29929386153513,1.41741148531105,1.65364673286289,
1.77176435663881,1.94894079230269,2.12611722796658,2.30329366363046,2.48047009929434),
 .UNSPECIFIED.);
#7956=B_SPLINE_CURVE_WITH_KNOTS('',3,(#91765,#91766,#91767,#91768,#91769,
#91770),.UNSPECIFIED.,.F.,.F.,(4,1,1,4),(-1.,-0.571428571428571,-0.285714285714286,
0.),.UNSPECIFIED.);
#7957=B_SPLINE_CURVE_WITH_KNOTS('',3,(#91771,#91772,#91773,#91774,#91775,
#91776,#91777,#91778,#91779,#91780,#91781,#91782,#91783,#91784,#91785,#91786,
#91787,#91788),.UNSPECIFIED.,.T.,.F.,(4,1,1,1,1,1,1,1,1,1,1,1,1,1,1,4),
(-2.48047009929434,-2.30329366363046,-2.12611722796658,-1.94894079230269,
-1.77176435663881,-1.65364673286289,-1.41741148531105,-1.29929386153513,
-1.18117623775921,-1.06305861398329,-0.885882178319406,-0.708705742655525,
-0.531529306991644,-0.354352871327763,-0.177176435663881,0.),
 .UNSPECIFIED.);
#7958=B_SPLINE_CURVE_WITH_KNOTS('',3,(#91793,#91794,#91795,#91796,#91797,
#91798,#91799,#91800,#91801,#91802,#91803,#91804,#91805,#91806,#91807,#91808,
#91809,#91810),.UNSPECIFIED.,.F.,.F.,(4,2,2,2,2,2,2,2,4),(1.09281023327069,
1.11399476693488,1.22799035827166,1.26102591181177,1.27988731437487,1.29913397363528,
1.33595457523744,1.42951419043064,1.46012340372434),.UNSPECIFIED.);
#7959=B_SPLINE_CURVE_WITH_KNOTS('',3,(#91823,#91824,#91825,#91826,#91827,
#91828,#91829,#91830,#91831,#91832),.UNSPECIFIED.,.F.,.F.,(4,2,2,2,4),(0.345676914394354,
0.355348506648306,0.369433821132995,0.383519135617684,0.389092225009936),
 .UNSPECIFIED.);
#7960=B_SPLINE_CURVE_WITH_KNOTS('',3,(#91867,#91868,#91869,#91870,#91871,
#91872,#91873,#91874,#91875,#91876),.UNSPECIFIED.,.F.,.F.,(4,2,2,2,4),(-0.190661625341085,
-0.178777035039909,-0.166892444738732,-0.14312326413638,-0.130096727258007),
 .UNSPECIFIED.);
#7961=B_SPLINE_CURVE_WITH_KNOTS('',3,(#91877,#91878,#91879,#91880,#91881,
#91882),.UNSPECIFIED.,.F.,.F.,(4,2,4),(-0.130096727258007,-0.117129563552769,
-0.0911358629691591),.UNSPECIFIED.);
#7962=B_SPLINE_CURVE_WITH_KNOTS('',3,(#91907,#91908,#91909,#91910,#91911,
#91912,#91913,#91914,#91915,#91916),.UNSPECIFIED.,.F.,.F.,(4,2,2,2,4),(0.193462588866382,
0.216085589979445,0.238708591092508,0.26177940398235,0.284850216872191),
 .UNSPECIFIED.);
#7963=B_SPLINE_CURVE_WITH_KNOTS('',3,(#91935,#91936,#91937,#91938,#91939,
#91940,#91941,#91942,#91943,#91944,#91945,#91946,#91947,#91948,#91949,#91950,
#91951,#91952),.UNSPECIFIED.,.F.,.F.,(4,2,2,2,2,2,2,2,4),(-0.415205355258057,
-0.40606214045211,-0.378053329963949,-0.350044519475788,-0.294026898499466,
-0.238009277523144,-0.210000467034983,-0.181991656546822,-0.172848441740874),
 .UNSPECIFIED.);
#7964=B_SPLINE_CURVE_WITH_KNOTS('',3,(#91956,#91957,#91958,#91959,#91960,
#91961,#91962,#91963,#91964,#91965),.UNSPECIFIED.,.F.,.F.,(4,2,2,2,4),(-0.261823472878211,
-0.204378823595008,-0.175621234943912,-0.146863646292815,-0.143979996599966),
 .UNSPECIFIED.);
#7965=B_SPLINE_CURVE_WITH_KNOTS('',3,(#91966,#91967,#91968,#91969,#91970,
#91971,#91972,#91973,#91974,#91975,#91976,#91977),.UNSPECIFIED.,.F.,.F.,
(4,2,2,2,2,4),(-0.252564986900111,-0.250043378084573,-0.229478062042114,
-0.208912745999654,-0.167782113914736,-0.167733445562344),.UNSPECIFIED.);
#7966=B_SPLINE_CURVE_WITH_KNOTS('',3,(#92043,#92044,#92045,#92046,#92047,
#92048,#92049,#92050,#92051,#92052,#92053,#92054,#92055,#92056),
 .UNSPECIFIED.,.F.,.F.,(4,2,2,2,2,2,4),(-0.000843143910697069,0.,0.0635581866099015,
0.111277859499319,0.158997532388736,0.222555718998638,0.223398862910045),
 .UNSPECIFIED.);
#7967=B_SPLINE_CURVE_WITH_KNOTS('',3,(#92090,#92091,#92092,#92093,#92094,
#92095,#92096,#92097,#92098,#92099,#92100,#92101,#92102,#92103),
 .UNSPECIFIED.,.F.,.F.,(4,2,2,2,2,2,4),(-0.000843143910697069,0.,0.0635581866099015,
0.111277859499319,0.158997532388736,0.222555718998638,0.223398862910045),
 .UNSPECIFIED.);
#7968=B_SPLINE_CURVE_WITH_KNOTS('',3,(#92218,#92219,#92220,#92221,#92222,
#92223,#92224,#92225,#92226,#92227,#92228,#92229,#92230,#92231),
 .UNSPECIFIED.,.F.,.F.,(4,2,2,2,2,2,4),(-0.000843143936325221,0.,0.0635581870754678,
0.11127786061665,0.158997534157832,0.222555721233299,0.223398865170335),
 .UNSPECIFIED.);
#7969=B_SPLINE_CURVE_WITH_KNOTS('',3,(#92329,#92330,#92331,#92332,#92333,
#92334,#92335,#92336,#92337,#92338,#92339,#92340,#92341,#92342),
 .UNSPECIFIED.,.F.,.F.,(4,2,2,2,2,2,4),(-0.000843143910697069,0.,0.0635581866099015,
0.111277859499319,0.158997532388736,0.222555718998638,0.223398862910045),
 .UNSPECIFIED.);
#7970=B_SPLINE_CURVE_WITH_KNOTS('',3,(#92445,#92446,#92447,#92448,#92449,
#92450,#92451,#92452),.UNSPECIFIED.,.F.,.F.,(4,2,2,4),(-0.170972401837901,
-0.1704030415541,-0.130663926012498,-0.0852015207771597),.UNSPECIFIED.);
#7971=B_SPLINE_CURVE_WITH_KNOTS('',3,(#92453,#92454,#92455,#92456,#92457,
#92458,#92459,#92460),.UNSPECIFIED.,.F.,.F.,(4,2,2,4),(-0.0852015207771597,
-0.0397391155418221,0.,0.000569360283792102),.UNSPECIFIED.);
#7972=B_SPLINE_CURVE_WITH_KNOTS('',3,(#92533,#92534,#92535,#92536,#92537,
#92538,#92539,#92540,#92541,#92542,#92543,#92544,#92545,#92546),
 .UNSPECIFIED.,.F.,.F.,(4,2,2,2,2,2,4),(-0.000843143910697069,0.,0.0635581866099015,
0.111277859499319,0.158997532388736,0.222555718998638,0.223398862910045),
 .UNSPECIFIED.);
#7973=B_SPLINE_CURVE_WITH_KNOTS('',3,(#92647,#92648,#92649,#92650,#92651,
#92652),.UNSPECIFIED.,.F.,.F.,(4,2,4),(0.091135862969159,0.117129563552768,
0.130096727258013),.UNSPECIFIED.);
#7974=B_SPLINE_CURVE_WITH_KNOTS('',3,(#92664,#92665,#92666,#92667,#92668,
#92669,#92670,#92671,#92672,#92673,#92674,#92675,#92676,#92677,#92678,#92679,
#92680,#92681,#92682,#92683,#92684,#92685,#92686,#92687,#92688,#92689,#92690,
#92691,#92692,#92693,#92694,#92695,#92696,#92697,#92698,#92699,#92700,#92701,
#92702,#92703,#92704,#92705,#92706,#92707,#92708,#92709,#92710,#92711,#92712),
 .UNSPECIFIED.,.F.,.F.,(4,3,3,3,3,3,3,3,3,3,3,3,3,3,3,3,4),(-0.000437248893796375,
-0.000327936670347281,-0.000218624446898187,0.,0.00769621191313966,0.0157118108669416,
0.024299765927154,0.0286905322178578,0.0386811779250504,0.0500503744658259,
0.0512366156247202,0.0620983057078456,0.0708608493966852,0.0729599957909709,
0.081430010034257,0.0896747028777473,0.0949866108739304),.UNSPECIFIED.);
#7975=B_SPLINE_CURVE_WITH_KNOTS('',3,(#92720,#92721,#92722,#92723,#92724,
#92725,#92726,#92727,#92728,#92729),.UNSPECIFIED.,.F.,.F.,(4,2,2,2,4),(0.105097916683049,
0.124999987614685,0.147923775725783,0.170693182296083,0.193462588866383),
 .UNSPECIFIED.);
#7976=B_SPLINE_CURVE_WITH_KNOTS('',3,(#92731,#92732,#92733,#92734,#92735,
#92736,#92737,#92738,#92739,#92740,#92741,#92742),.UNSPECIFIED.,.F.,.F.,
(4,2,2,2,2,4),(0.190661625341083,0.202546215642259,0.214430805943435,0.238199986545788,
0.264193687129397,0.287183234818408),.UNSPECIFIED.);
#7977=B_SPLINE_CURVE_WITH_KNOTS('',3,(#92749,#92750,#92751,#92752,#92753,
#92754,#92755,#92756,#92757,#92758),.UNSPECIFIED.,.F.,.F.,(4,2,2,2,4),(0.130096727258013,
0.143123264136378,0.16689244473873,0.178777035039906,0.190661625341083),
 .UNSPECIFIED.);
#7978=B_SPLINE_CURVE_WITH_KNOTS('',3,(#92856,#92857,#92858,#92859,#92860,
#92861,#92862,#92863,#92864,#92865,#92866,#92867,#92868,#92869,#92870,#92871),
 .UNSPECIFIED.,.F.,.F.,(4,3,3,3,3,4),(-0.0505851231124638,-0.0494104061932021,
-0.0393505169387521,-0.0372626146808706,-0.0276893855942847,-0.0247052030966232),
 .UNSPECIFIED.);
#7979=B_SPLINE_CURVE_WITH_KNOTS('',3,(#92934,#92935,#92936,#92937,#92938,
#92939,#92940,#92941,#92942,#92943,#92944,#92945,#92946,#92947,#92948,#92949,
#92950,#92951,#92952,#92953,#92954,#92955),.UNSPECIFIED.,.F.,.F.,(4,3,3,
3,3,3,3,4),(-0.0474813620491253,-0.0386630667071124,-0.0351633788899156,
-0.0253798710348694,-0.0187891022782665,-0.00732222521866259,0.,0.000730628320777441),
 .UNSPECIFIED.);
#7980=B_SPLINE_CURVE_WITH_KNOTS('',3,(#92963,#92964,#92965,#92966,#92967,
#92968,#92969,#92970,#92971,#92972),.UNSPECIFIED.,.F.,.F.,(4,2,2,2,4),(-0.296437784487761,
-0.268297213606933,-0.240327871275254,-0.215765565720465,-0.195631865775833),
 .UNSPECIFIED.);
#7981=B_SPLINE_CURVE_WITH_KNOTS('',3,(#92975,#92976,#92977,#92978,#92979,
#92980,#92981,#92982,#92983,#92984),.UNSPECIFIED.,.F.,.F.,(4,2,2,2,4),(-0.195631865775833,
-0.175498165831202,-0.150935860276413,-0.122966517944734,-0.0948259470639069),
 .UNSPECIFIED.);
#7982=B_SPLINE_CURVE_WITH_KNOTS('',3,(#93014,#93015,#93016,#93017,#93018,
#93019,#93020,#93021,#93022,#93023),.UNSPECIFIED.,.F.,.F.,(4,2,2,2,4),(0.0948259470639078,
0.122966517944735,0.150935860276413,0.175498165831201,0.195631865775832),
 .UNSPECIFIED.);
#7983=B_SPLINE_CURVE_WITH_KNOTS('',3,(#93059,#93060,#93061,#93062,#93063,
#93064,#93065,#93066,#93067,#93068,#93069,#93070,#93071,#93072,#93073,#93074,
#93075,#93076,#93077,#93078,#93079,#93080,#93081,#93082,#93083,#93084,#93085,
#93086,#93087,#93088,#93089,#93090,#93091,#93092,#93093,#93094,#93095,#93096,
#93097,#93098,#93099,#93100,#93101),.UNSPECIFIED.,.F.,.F.,(4,3,3,3,3,3,
3,3,3,3,3,3,3,3,4),(0.,0.00819151153137603,0.0168429948726552,0.0224161551166588,
0.0314142253231794,0.0424572406680403,0.0446099777430671,0.0563743860269171,
0.066180614352991,0.0674313049384604,0.0761831144290232,0.0844743257223039,
0.0922212797822719,0.0946135652781465,0.0947043969996347),.UNSPECIFIED.);
#7984=B_SPLINE_CURVE_WITH_KNOTS('',3,(#93117,#93118,#93119,#93120,#93121,
#93122,#93123,#93124,#93125,#93126),.UNSPECIFIED.,.F.,.F.,(4,2,2,2,4),(-0.195631865775832,
-0.175498165831201,-0.150935860276413,-0.122966517944735,-0.0948259470639078),
 .UNSPECIFIED.);
#7985=B_SPLINE_CURVE_WITH_KNOTS('',3,(#93194,#93195,#93196,#93197,#93198,
#93199,#93200,#93201,#93202,#93203,#93204,#93205,#93206,#93207,#93208,#93209,
#93210,#93211,#93212,#93213,#93214,#93215,#93216,#93217,#93218,#93219,#93220,
#93221,#93222,#93223,#93224,#93225),.UNSPECIFIED.,.F.,.F.,(4,2,2,2,2,2,
2,2,2,2,2,2,2,2,2,4),(3.54152458065573E-10,0.288711445101139,0.523258332244725,
0.921227317049852,1.09267154481917,1.12602826877806,1.13805490776081,1.14561247672485,
1.15218349843735,1.15992334586198,1.17330081210199,1.20544465265463,1.30433060811633,
1.73541082798229,2.00533365271455,2.34908372554942),.UNSPECIFIED.);
#7986=B_SPLINE_CURVE_WITH_KNOTS('',3,(#93229,#93230,#93231,#93232,#93233,
#93234,#93235,#93236,#93237,#93238),.UNSPECIFIED.,.F.,.F.,(4,2,2,2,4),(-0.235035705616533,
-0.164045621201278,-0.0870897131881243,-0.0381417578315876,0.),
 .UNSPECIFIED.);
#7987=B_SPLINE_CURVE_WITH_KNOTS('',3,(#93240,#93241,#93242,#93243,#93244,
#93245,#93246,#93247,#93248,#93249),.UNSPECIFIED.,.F.,.F.,(4,2,2,2,4),(-0.0803122862957921,
-0.0602646333915054,-0.0402202940526313,-0.0201483463522527,-3.56243524540593E-5),
 .UNSPECIFIED.);
#7988=B_SPLINE_CURVE_WITH_KNOTS('',3,(#93251,#93252,#93253,#93254,#93255,
#93256),.UNSPECIFIED.,.F.,.F.,(4,2,4),(8.43662143615864E-5,0.00327116298064693,
0.00646179051431274),.UNSPECIFIED.);
#7989=B_SPLINE_CURVE_WITH_KNOTS('',3,(#93258,#93259,#93260,#93261,#93262,
#93263,#93264,#93265,#93266,#93267),.UNSPECIFIED.,.F.,.F.,(4,2,2,2,4),(-0.106351401183245,
-0.0798864576605021,-0.0531877160318232,-0.0265812067152108,-7.06104949174502E-6),
 .UNSPECIFIED.);
#7990=B_SPLINE_CURVE_WITH_KNOTS('',3,(#93269,#93270,#93271,#93272,#93273,
#93274,#93275,#93276,#93277,#93278),.UNSPECIFIED.,.F.,.F.,(4,2,2,2,4),(-0.0971883190541716,
-0.0727561460747867,-0.048468056376207,-0.0242270507757942,0.),
 .UNSPECIFIED.);
#7991=B_SPLINE_CURVE_WITH_KNOTS('',3,(#93279,#93280,#93281,#93282,#93283,
#93284),.UNSPECIFIED.,.F.,.F.,(4,2,4),(-0.0301723368590298,-0.0150922159606526,
-2.55953913249195E-6),.UNSPECIFIED.);
#7992=B_SPLINE_CURVE_WITH_KNOTS('',3,(#93288,#93289,#93290,#93291,#93292,
#93293,#93294,#93295,#93296,#93297,#93298,#93299,#93300,#93301,#93302,#93303,
#93304,#93305,#93306,#93307,#93308,#93309,#93310,#93311,#93312,#93313,#93314,
#93315,#93316,#93317,#93318,#93319),.UNSPECIFIED.,.F.,.F.,(4,2,2,2,2,2,
2,2,2,2,2,2,2,2,2,4),(-2.01212438752124,-1.76578196828659,-1.5647664663706,
-1.20118246901991,-1.06053517315717,-1.02977885200715,-1.0193276272259,
-1.01279623524482,-1.00715009449403,-1.00055979488344,-0.989257775261865,
-0.96242213266161,-0.881471927659453,-0.518895860123459,-0.290806811506921,
-8.2501916409683E-10),.UNSPECIFIED.);
#7993=B_SPLINE_CURVE_WITH_KNOTS('',3,(#93323,#93324,#93325,#93326,#93327,
#93328,#93329,#93330,#93331,#93332),.UNSPECIFIED.,.F.,.F.,(4,2,2,2,4),(-0.189468447311924,
-0.155678960910493,-0.111541963335214,-0.0470106922386932,-7.10058815808075E-6),
 .UNSPECIFIED.);
#7994=B_SPLINE_CURVE_WITH_KNOTS('',3,(#93334,#93335,#93336,#93337,#93338,
#93339,#93340,#93341,#93342,#93343),.UNSPECIFIED.,.F.,.F.,(4,2,2,2,4),(-0.0812741980146226,
-0.061010630542918,-0.0406258560977219,-0.0203042042142377,0.),
 .UNSPECIFIED.);
#7995=B_SPLINE_CURVE_WITH_KNOTS('',3,(#93345,#93346,#93347,#93348,#93349,
#93350),.UNSPECIFIED.,.F.,.F.,(4,2,4),(-0.0064959341341575,-0.00329347810601311,
-8.81436577924804E-5),.UNSPECIFIED.);
#7996=B_SPLINE_CURVE_WITH_KNOTS('',3,(#93352,#93353,#93354,#93355,#93356,
#93357),.UNSPECIFIED.,.F.,.F.,(4,2,4),(-0.00936112110047215,-0.00472017132367055,
-6.30707363171211E-5),.UNSPECIFIED.);
#7997=B_SPLINE_CURVE_WITH_KNOTS('',3,(#93359,#93360,#93361,#93362,#93363,
#93364,#93365,#93366,#93367,#93368,#93369,#93370,#93371,#93372,#93373,#93374),
 .UNSPECIFIED.,.F.,.F.,(4,2,2,2,2,2,2,4),(-0.201490383661384,-0.178130230033713,
-0.154775766161226,-0.145700922114215,-0.102563961887103,-0.0587557032775208,
-0.029368346867021,-7.06104927835685E-6),.UNSPECIFIED.);
#7998=B_SPLINE_CURVE_WITH_KNOTS('',3,(#93375,#93376,#93377,#93378,#93379,
#93380),.UNSPECIFIED.,.F.,.F.,(4,2,4),(-0.0308102197342027,-0.0154008404140284,
0.),.UNSPECIFIED.);
#7999=B_SPLINE_CURVE_WITH_KNOTS('',3,(#94481,#94482,#94483,#94484,#94485,
#94486,#94487,#94488,#94489,#94490,#94491,#94492,#94493,#94494,#94495,#94496,
#94497,#94498,#94499,#94500,#94501,#94502,#94503,#94504,#94505,#94506,#94507,
#94508,#94509,#94510,#94511,#94512,#94513,#94514,#94515,#94516,#94517,#94518,
#94519,#94520,#94521,#94522,#94523,#94524,#94525,#94526,#94527,#94528,#94529,
#94530,#94531,#94532,#94533,#94534,#94535,#94536,#94537,#94538,#94539,#94540,
#94541,#94542,#94543,#94544,#94545,#94546,#94547,#94548,#94549,#94550,#94551,
#94552,#94553,#94554,#94555,#94556,#94557,#94558,#94559,#94560,#94561,#94562,
#94563,#94564,#94565,#94566,#94567,#94568,#94569,#94570,#94571,#94572,#94573,
#94574,#94575,#94576,#94577,#94578,#94579,#94580,#94581,#94582,#94583,#94584,
#94585,#94586,#94587,#94588,#94589,#94590,#94591,#94592,#94593,#94594,#94595,
#94596,#94597,#94598,#94599,#94600,#94601,#94602,#94603,#94604,#94605,#94606,
#94607,#94608,#94609,#94610,#94611,#94612,#94613,#94614,#94615,#94616,#94617,
#94618,#94619,#94620,#94621,#94622,#94623,#94624,#94625,#94626,#94627,#94628,
#94629,#94630,#94631,#94632,#94633,#94634,#94635,#94636,#94637,#94638,#94639,
#94640,#94641,#94642,#94643,#94644,#94645,#94646,#94647,#94648,#94649,#94650,
#94651,#94652,#94653,#94654,#94655,#94656,#94657,#94658,#94659,#94660,#94661,
#94662,#94663,#94664,#94665,#94666,#94667,#94668,#94669,#94670,#94671,#94672,
#94673,#94674,#94675,#94676,#94677,#94678,#94679,#94680,#94681,#94682,#94683,
#94684,#94685,#94686,#94687,#94688,#94689,#94690,#94691,#94692,#94693,#94694,
#94695,#94696,#94697,#94698,#94699,#94700,#94701,#94702,#94703,#94704,#94705,
#94706,#94707,#94708,#94709,#94710,#94711,#94712,#94713,#94714,#94715,#94716,
#94717,#94718,#94719,#94720,#94721,#94722,#94723,#94724,#94725,#94726,#94727,
#94728,#94729,#94730,#94731,#94732,#94733,#94734,#94735,#94736,#94737,#94738,
#94739,#94740,#94741,#94742,#94743,#94744,#94745,#94746,#94747,#94748,#94749,
#94750,#94751,#94752,#94753,#94754,#94755,#94756,#94757,#94758,#94759,#94760,
#94761,#94762,#94763,#94764,#94765,#94766,#94767,#94768,#94769,#94770,#94771,
#94772,#94773,#94774,#94775,#94776,#94777,#94778,#94779,#94780,#94781,#94782,
#94783,#94784,#94785,#94786,#94787,#94788,#94789,#94790,#94791,#94792,#94793,
#94794,#94795,#94796,#94797,#94798,#94799,#94800,#94801,#94802,#94803,#94804,
#94805,#94806,#94807,#94808,#94809,#94810,#94811,#94812,#94813,#94814,#94815,
#94816,#94817,#94818,#94819,#94820,#94821,#94822,#94823,#94824,#94825,#94826,
#94827,#94828,#94829,#94830,#94831,#94832,#94833,#94834,#94835,#94836,#94837,
#94838,#94839,#94840,#94841,#94842,#94843,#94844,#94845,#94846,#94847,#94848,
#94849,#94850,#94851,#94852,#94853,#94854,#94855,#94856,#94857,#94858,#94859,
#94860,#94861,#94862,#94863,#94864,#94865,#94866,#94867,#94868,#94869,#94870,
#94871,#94872,#94873,#94874,#94875,#94876,#94877,#94878,#94879,#94880,#94881,
#94882,#94883,#94884,#94885,#94886,#94887,#94888,#94889,#94890,#94891,#94892,
#94893,#94894,#94895,#94896,#94897,#94898,#94899,#94900,#94901,#94902,#94903,
#94904,#94905,#94906,#94907,#94908,#94909,#94910,#94911,#94912,#94913,#94914,
#94915,#94916,#94917,#94918,#94919,#94920,#94921,#94922,#94923,#94924,#94925,
#94926,#94927,#94928,#94929,#94930,#94931,#94932,#94933,#94934,#94935,#94936,
#94937,#94938,#94939,#94940,#94941,#94942,#94943,#94944,#94945,#94946,#94947,
#94948,#94949,#94950,#94951,#94952,#94953,#94954,#94955,#94956,#94957,#94958,
#94959,#94960,#94961,#94962,#94963,#94964,#94965,#94966,#94967,#94968,#94969,
#94970,#94971,#94972,#94973,#94974,#94975,#94976,#94977,#94978,#94979,#94980,
#94981,#94982,#94983,#94984,#94985,#94986,#94987,#94988,#94989,#94990,#94991,
#94992,#94993,#94994,#94995,#94996,#94997,#94998,#94999,#95000,#95001,#95002,
#95003,#95004,#95005,#95006,#95007,#95008,#95009,#95010,#95011,#95012,#95013,
#95014,#95015,#95016,#95017,#95018,#95019,#95020,#95021,#95022,#95023,#95024,
#95025,#95026,#95027,#95028,#95029,#95030,#95031,#95032,#95033,#95034,#95035,
#95036,#95037,#95038,#95039,#95040,#95041,#95042,#95043,#95044,#95045,#95046,
#95047,#95048,#95049,#95050,#95051,#95052,#95053,#95054,#95055,#95056,#95057,
#95058,#95059,#95060,#95061,#95062,#95063,#95064,#95065,#95066,#95067,#95068,
#95069,#95070,#95071,#95072,#95073,#95074,#95075,#95076,#95077,#95078,#95079,
#95080,#95081,#95082,#95083,#95084,#95085,#95086,#95087,#95088,#95089,#95090,
#95091,#95092,#95093,#95094,#95095,#95096,#95097,#95098,#95099,#95100,#95101,
#95102,#95103,#95104,#95105,#95106,#95107,#95108,#95109,#95110,#95111,#95112,
#95113,#95114,#95115,#95116,#95117,#95118,#95119,#95120,#95121,#95122,#95123,
#95124,#95125,#95126,#95127,#95128,#95129,#95130,#95131,#95132,#95133,#95134,
#95135,#95136,#95137,#95138,#95139,#95140,#95141,#95142,#95143,#95144,#95145,
#95146,#95147,#95148,#95149,#95150,#95151,#95152,#95153,#95154,#95155,#95156,
#95157,#95158,#95159,#95160,#95161,#95162,#95163,#95164,#95165,#95166,#95167,
#95168,#95169,#95170,#95171,#95172,#95173,#95174,#95175,#95176,#95177,#95178,
#95179,#95180,#95181,#95182,#95183,#95184,#95185,#95186,#95187,#95188,#95189,
#95190,#95191,#95192,#95193,#95194,#95195,#95196,#95197,#95198,#95199,#95200,
#95201,#95202,#95203,#95204,#95205,#95206,#95207,#95208,#95209,#95210,#95211,
#95212,#95213,#95214,#95215,#95216,#95217,#95218,#95219,#95220,#95221,#95222,
#95223,#95224,#95225,#95226,#95227,#95228,#95229,#95230,#95231,#95232,#95233,
#95234,#95235,#95236,#95237,#95238,#95239,#95240,#95241,#95242,#95243,#95244,
#95245,#95246,#95247,#95248,#95249,#95250,#95251,#95252,#95253,#95254,#95255,
#95256,#95257,#95258,#95259,#95260,#95261,#95262,#95263,#95264,#95265,#95266,
#95267,#95268,#95269,#95270,#95271,#95272,#95273,#95274,#95275,#95276,#95277,
#95278,#95279,#95280,#95281,#95282,#95283,#95284,#95285,#95286,#95287,#95288,
#95289,#95290,#95291,#95292,#95293,#95294,#95295,#95296,#95297,#95298,#95299,
#95300,#95301,#95302,#95303,#95304,#95305,#95306,#95307,#95308,#95309,#95310,
#95311,#95312,#95313,#95314,#95315,#95316,#95317,#95318,#95319,#95320,#95321,
#95322,#95323,#95324,#95325,#95326,#95327,#95328,#95329,#95330,#95331,#95332,
#95333,#95334,#95335,#95336,#95337,#95338,#95339,#95340,#95341,#95342,#95343,
#95344,#95345,#95346,#95347,#95348,#95349,#95350,#95351,#95352,#95353,#95354,
#95355,#95356,#95357,#95358,#95359,#95360,#95361,#95362,#95363,#95364,#95365,
#95366,#95367,#95368,#95369,#95370,#95371,#95372,#95373,#95374,#95375,#95376,
#95377,#95378,#95379,#95380,#95381,#95382,#95383,#95384,#95385,#95386,#95387,
#95388,#95389,#95390,#95391,#95392,#95393,#95394,#95395,#95396,#95397,#95398,
#95399,#95400,#95401,#95402,#95403,#95404,#95405,#95406,#95407,#95408,#95409,
#95410,#95411,#95412,#95413,#95414,#95415,#95416,#95417,#95418,#95419,#95420,
#95421,#95422,#95423,#95424,#95425,#95426,#95427,#95428,#95429,#95430,#95431,
#95432,#95433,#95434,#95435,#95436,#95437,#95438,#95439,#95440,#95441,#95442,
#95443,#95444,#95445,#95446,#95447,#95448,#95449,#95450,#95451,#95452,#95453,
#95454,#95455,#95456,#95457,#95458,#95459,#95460,#95461,#95462,#95463,#95464,
#95465,#95466,#95467,#95468,#95469,#95470,#95471,#95472,#95473,#95474,#95475,
#95476,#95477,#95478,#95479,#95480,#95481,#95482,#95483,#95484,#95485,#95486,
#95487,#95488,#95489,#95490,#95491,#95492,#95493,#95494,#95495,#95496,#95497,
#95498,#95499,#95500,#95501,#95502,#95503,#95504,#95505,#95506,#95507,#95508,
#95509,#95510,#95511,#95512,#95513,#95514,#95515,#95516,#95517,#95518,#95519,
#95520,#95521,#95522,#95523,#95524,#95525,#95526,#95527,#95528,#95529,#95530,
#95531,#95532,#95533,#95534,#95535,#95536,#95537,#95538,#95539,#95540,#95541,
#95542,#95543,#95544,#95545,#95546,#95547,#95548,#95549,#95550,#95551,#95552,
#95553,#95554,#95555,#95556,#95557,#95558,#95559,#95560,#95561,#95562,#95563,
#95564,#95565,#95566,#95567,#95568,#95569,#95570,#95571,#95572,#95573,#95574,
#95575,#95576,#95577,#95578,#95579,#95580,#95581,#95582,#95583,#95584,#95585,
#95586,#95587,#95588,#95589,#95590,#95591,#95592,#95593,#95594,#95595,#95596,
#95597,#95598,#95599,#95600,#95601,#95602,#95603,#95604,#95605,#95606,#95607,
#95608,#95609,#95610,#95611,#95612,#95613,#95614,#95615,#95616,#95617,#95618,
#95619,#95620,#95621,#95622,#95623,#95624,#95625,#95626,#95627,#95628,#95629,
#95630,#95631,#95632,#95633,#95634,#95635,#95636,#95637,#95638,#95639,#95640,
#95641,#95642,#95643,#95644,#95645,#95646,#95647,#95648,#95649,#95650,#95651,
#95652,#95653,#95654,#95655,#95656,#95657,#95658,#95659,#95660,#95661,#95662,
#95663,#95664,#95665,#95666),.UNSPECIFIED.,.F.,.F.,(4,3,3,3,3,3,3,3,3,3,
3,3,3,3,3,3,3,3,3,3,3,3,3,3,3,3,3,3,3,3,3,3,3,3,3,3,3,3,3,3,3,3,3,3,3,3,
3,3,3,3,3,3,3,3,3,3,3,3,3,3,3,3,3,3,3,3,3,3,3,3,3,3,3,3,3,3,3,3,3,3,3,3,
3,3,3,3,3,3,3,3,3,3,3,3,3,3,3,3,3,3,3,3,3,3,3,3,3,3,3,3,3,3,3,3,3,3,3,3,
3,3,3,3,3,3,3,3,3,3,3,3,3,3,3,3,3,3,3,3,3,3,3,3,3,3,3,3,3,3,3,3,3,3,3,3,
3,3,3,3,3,3,3,3,3,3,3,3,3,3,3,3,3,3,3,3,3,3,3,3,3,3,3,3,3,3,3,3,3,3,3,3,
3,3,3,3,3,3,3,3,3,3,3,3,3,3,3,3,3,3,3,3,3,3,3,3,3,3,3,3,3,3,3,3,3,3,3,3,
3,3,3,3,3,3,3,3,3,3,3,3,3,3,3,3,3,3,3,3,3,3,3,3,3,3,3,3,3,3,3,3,3,3,3,3,
3,3,3,3,3,3,3,3,3,3,3,3,3,3,3,3,3,3,3,3,3,3,3,3,3,3,3,3,3,3,3,3,3,3,3,3,
3,3,3,3,3,3,3,3,3,3,3,3,3,3,3,3,3,3,3,3,3,3,3,3,3,3,3,3,3,3,3,3,3,3,3,3,
3,3,3,3,3,3,3,3,3,3,3,3,3,3,3,3,3,3,3,3,3,3,3,3,3,3,3,3,3,3,3,3,3,3,3,3,
3,3,3,3,3,3,3,3,3,3,3,3,3,3,3,3,3,3,3,3,3,3,3,3,3,4),(-1.,-0.991071428571429,
-0.991071389429951,-0.982142857142857,-0.982142822785736,-0.973214285714286,
-0.973214273423607,-0.964285719587971,-0.964285714285714,-0.955357154845019,
-0.955357142857143,-0.946428582987328,-0.946428571428571,-0.937500007454815,
-0.9375,-0.928571435886753,-0.928571428571429,-0.919642857142857,-0.910714285714286,
-0.910714278487105,-0.903444178215078,-0.901785714285714,-0.8962006132777,
-0.892857142857143,-0.89285703296426,-0.888392835478123,-0.883928637991986,
-0.883928571428571,-0.880170831457046,-0.876470542060389,-0.875,-0.874999572863337,
-0.871518316066235,-0.868090467473807,-0.866071717001134,-0.866071428571429,
-0.863200415042696,-0.860343926901775,-0.857531528156535,-0.857143004738549,
-0.857142857142857,-0.854312859661374,-0.852678571428572,-0.850614304741742,
-0.848565036595157,-0.848214285714286,-0.846890953347238,-0.845982142857143,
-0.845238193734111,-0.843631148930307,-0.842633928571428,-0.840878948010448,
-0.839285714285714,-0.836887599372128,-0.834821428571428,-0.833333913300317,
-0.832589285714286,-0.831300035123872,-0.830357142857143,-0.828357848817079,
-0.826356039658343,-0.825892857142857,-0.823988309272079,-0.822088982612407,
-0.821428571428571,-0.821428367725019,-0.819505414596167,-0.8175860310261,
-0.816964285714285,-0.814956467981351,-0.812947024322632,-0.8125,-0.810292489456701,
-0.809523200608117,-0.807330760640928,-0.805140498994953,-0.803571428571428,
-0.801586644036287,-0.798469918994543,-0.795270754281138,-0.794642857142857,
-0.793650917020491,-0.790320032619685,-0.787044258957954,-0.785714306584564,
-0.785714285714286,-0.783413209641271,-0.781107750138836,-0.780867818478783,
-0.778951670344505,-0.777780830372113,-0.777338671144154,-0.775574097476839,
-0.773809523809524,-0.770273481108357,-0.769838188635457,-0.7689930392807,
-0.767153440241231,-0.765448900592731,-0.763199787229666,-0.761904871965663,
-0.761904761904762,-0.760089872236183,-0.758275764324489,-0.757077354179359,
-0.755244041175192,-0.75396837627968,-0.753538677089679,-0.751655164247817,
-0.75,-0.748015716198947,-0.747767857142857,-0.746029646317197,-0.743550537444313,
-0.741071428571428,-0.739773961496372,-0.738839285714285,-0.738095686705119,
-0.736694105353861,-0.735491071428571,-0.733673411592545,-0.732142857142857,
-0.730204502448423,-0.728272184556273,-0.727678571428572,-0.72619055472343,
-0.725446428571429,-0.724300149594122,-0.723214285714286,-0.721270255978889,
-0.719314481159982,-0.71875,-0.717013707960798,-0.715279745045851,-0.714285714285714,
-0.714284646236362,-0.712090385576223,-0.709893252584267,-0.708333333333333,
-0.706097031223049,-0.703882549937917,-0.702381642308063,-0.702380952380952,
-0.699974534521517,-0.697519859321161,-0.695069959055868,-0.692693401084694,
-0.69047619047619,-0.690474133472452,-0.688920512294885,-0.687369792937533,
-0.686507936507937,-0.684145833909582,-0.682539682539683,-0.680167707232127,
-0.678571620568218,-0.67621012605145,-0.674603174603175,-0.67261819681719,
-0.66998184520372,-0.667337275851678,-0.666667233377128,-0.666666666666667,
-0.663645875002391,-0.660576136857663,-0.658730158730159,-0.658729978699635,
-0.655155726859902,-0.651537345370322,-0.650793955011456,-0.650793650793651,
-0.64648921283136,-0.642857384281078,-0.642857142857143,-0.637654450300913,
-0.634921030719177,-0.634920634920635,-0.627923928049837,-0.626984354640624,
-0.626984126984127,-0.622156503929432,-0.619047619047619,-0.619047289450574,
-0.613700647719127,-0.608263744404841,-0.607142857142857,-0.607142848983513,
-0.599710180861582,-0.595238127445014,-0.595238095238095,-0.586752880028379,
-0.583333340923382,-0.583333333333333,-0.573056502544092,-0.571428587791853,
-0.571428571428571,-0.559523813525363,-0.55952380952381,-0.547619052167738,
-0.547619047619048,-0.535714288277056,-0.535714285714286,-0.523809523809524,
-0.515873015873016,-0.507936512898811,-0.507936507936508,-0.5,-0.499999995871733,
-0.492063492063492,-0.492063478197101,-0.484467253634067,-0.481481481481481,
-0.481481440717216,-0.476190476190476,-0.476190396250867,-0.471892865305429,
-0.46825409755741,-0.468253968253968,-0.464547293860793,-0.460878327493757,
-0.46031746031746,-0.460317416879269,-0.457285356553107,-0.45429626344784,
-0.452381592760412,-0.452380952380952,-0.44969797322538,-0.447000164675377,
-0.444320561617439,-0.441723294699108,-0.44047619047619,-0.440476006991694,
-0.438220240631386,-0.43596270509345,-0.43452380952381,-0.432270078724781,
-0.430045371855419,-0.428571428571429,-0.428568980975705,-0.426647084103455,
-0.424633391022285,-0.422619697941116,-0.422619047619048,-0.420858569468115,
-0.419096741455247,-0.417339083079523,-0.416666903236966,-0.416666666666667,
-0.414332050427676,-0.411997434188685,-0.409856872686492,-0.40771882742928,
-0.405591465610837,-0.404761904761905,-0.404761616116348,-0.403144853246966,
-0.401526682096213,-0.400793650793651,-0.398777598024052,-0.396825396825397,
-0.395471659185257,-0.39484126984127,-0.393176998777955,-0.392858194162737,
-0.39186507936508,-0.390357253125332,-0.388888888888889,-0.387207358382915,
-0.386904761904762,-0.385110812996099,-0.383928571428572,-0.382587499125909,
-0.381247225112031,-0.380952457568705,-0.380952380952381,-0.378563261893649,
-0.376224906962247,-0.375661375661376,-0.373920443009037,-0.372193839494745,
-0.37097458200055,-0.369358460438232,-0.3690480190967,-0.368026973539958,
-0.365516896588505,-0.365079365079365,-0.363326640224003,-0.363095238095238,
-0.361512105321307,-0.35992885568622,-0.358346761150496,-0.357145070531906,
-0.357142857142857,-0.355546286153388,-0.35394320567017,-0.353174603174603,
-0.351902018190071,-0.351190476190476,-0.349634484581003,-0.349206349206349,
-0.347221939748124,-0.3452375302899,-0.34325368577987,-0.341269841269841,
-0.339198036849855,-0.337301587301587,-0.33531747481785,-0.333333362334113,
-0.333333333333333,-0.331306663695514,-0.329285252778724,-0.327382478472304,
-0.327380952380952,-0.325604664984563,-0.323826219469051,-0.322049559443716,
-0.321428739717564,-0.321428571428571,-0.318170228212089,-0.314792094541723,
-0.311349092498602,-0.309524714317972,-0.30952380952381,-0.306242345183409,
-0.302855094187904,-0.299476694932263,-0.297619047619048,-0.297618383218759,
-0.293739893156044,-0.28972711509084,-0.285714337025636,-0.285714285714286,
-0.280392556199838,-0.274939048722368,-0.273809527057199,-0.273809523809524,
-0.267759242157021,-0.261904904421664,-0.261904761904762,-0.255743652740556,
-0.250000588693953,-0.25,-0.243006450702321,-0.238095981836014,-0.236300908282312,
-0.23015906433374,-0.23015873015873,-0.226125727537763,-0.222222574129115,
-0.222222222222222,-0.218754557253951,-0.215242389059935,-0.214286338712583,
-0.214285714285714,-0.209074191895231,-0.203699859680209,-0.2023814347069,
-0.202380952380952,-0.195767114280798,-0.190476314984547,-0.19047619047619,
-0.182700873239942,-0.178571466870454,-0.178571428571429,-0.166666671143928,
-0.166666666666667,-0.154761914101637,-0.154761904761905,-0.142857151151493,
-0.142857142857143,-0.133928577582602,-0.133928571428571,-0.125000003845394,
-0.125,-0.116071430990516,-0.116071428571429,-0.107142857142857,-0.0982142857142857,
-0.0892857142857143,-0.0803571428571428,-0.0714285714285714,-0.0714285693344336,
-0.0625,-0.0624999960539666,-0.0535714285714286,-0.0535714237366097,-0.0446428571428571,
-0.0446428521159013,-0.0357142857142857,-0.0267857244811938,-0.0267857142857143,
-0.0178571653672693,-0.0178571428571429,-0.00892859399562328,-0.00892857142857143,
0.),.UNSPECIFIED.);
#8000=B_SPLINE_CURVE_WITH_KNOTS('',3,(#95667,#95668,#95669,#95670,#95671,
#95672,#95673,#95674,#95675,#95676,#95677,#95678,#95679,#95680,#95681,#95682,
#95683,#95684,#95685,#95686,#95687,#95688,#95689,#95690,#95691,#95692,#95693,
#95694,#95695,#95696,#95697,#95698,#95699,#95700,#95701,#95702,#95703,#95704,
#95705,#95706,#95707,#95708,#95709,#95710,#95711,#95712,#95713,#95714,#95715,
#95716,#95717,#95718,#95719,#95720,#95721,#95722,#95723,#95724,#95725,#95726,
#95727,#95728,#95729,#95730,#95731,#95732,#95733,#95734,#95735,#95736,#95737,
#95738,#95739,#95740,#95741,#95742,#95743,#95744,#95745,#95746,#95747,#95748,
#95749,#95750,#95751,#95752,#95753,#95754,#95755,#95756,#95757,#95758,#95759,
#95760,#95761,#95762,#95763,#95764,#95765,#95766,#95767,#95768,#95769,#95770,
#95771,#95772,#95773,#95774,#95775,#95776,#95777,#95778,#95779,#95780,#95781,
#95782,#95783,#95784,#95785,#95786,#95787,#95788,#95789,#95790,#95791,#95792,
#95793,#95794,#95795,#95796,#95797,#95798,#95799,#95800,#95801,#95802,#95803,
#95804,#95805,#95806,#95807,#95808,#95809,#95810,#95811,#95812,#95813,#95814,
#95815,#95816,#95817,#95818,#95819,#95820,#95821,#95822,#95823,#95824,#95825,
#95826,#95827,#95828,#95829,#95830,#95831,#95832,#95833,#95834,#95835,#95836,
#95837,#95838,#95839,#95840,#95841,#95842,#95843,#95844,#95845,#95846,#95847,
#95848,#95849,#95850,#95851,#95852,#95853,#95854,#95855,#95856,#95857,#95858,
#95859,#95860,#95861,#95862,#95863,#95864,#95865,#95866,#95867,#95868,#95869,
#95870,#95871,#95872,#95873,#95874,#95875,#95876,#95877,#95878,#95879,#95880,
#95881,#95882,#95883,#95884,#95885,#95886,#95887,#95888,#95889,#95890,#95891,
#95892,#95893,#95894,#95895,#95896,#95897,#95898,#95899,#95900,#95901,#95902,
#95903,#95904,#95905,#95906,#95907,#95908,#95909,#95910,#95911,#95912,#95913,
#95914,#95915,#95916,#95917,#95918,#95919,#95920,#95921,#95922,#95923,#95924,
#95925,#95926,#95927,#95928,#95929,#95930,#95931,#95932,#95933,#95934,#95935,
#95936,#95937,#95938,#95939,#95940,#95941,#95942,#95943,#95944,#95945,#95946,
#95947,#95948,#95949,#95950,#95951,#95952,#95953,#95954,#95955,#95956,#95957,
#95958,#95959,#95960,#95961,#95962,#95963,#95964,#95965,#95966,#95967,#95968,
#95969,#95970,#95971,#95972,#95973,#95974,#95975,#95976,#95977,#95978,#95979,
#95980,#95981,#95982,#95983,#95984,#95985,#95986,#95987,#95988,#95989,#95990,
#95991,#95992,#95993,#95994,#95995,#95996,#95997,#95998,#95999,#96000,#96001,
#96002,#96003,#96004,#96005,#96006,#96007,#96008,#96009,#96010,#96011,#96012,
#96013,#96014,#96015,#96016,#96017,#96018,#96019,#96020,#96021,#96022,#96023,
#96024,#96025,#96026,#96027,#96028,#96029,#96030,#96031,#96032,#96033,#96034,
#96035,#96036,#96037,#96038,#96039,#96040,#96041,#96042,#96043,#96044,#96045,
#96046,#96047,#96048,#96049,#96050,#96051,#96052,#96053,#96054,#96055,#96056,
#96057,#96058,#96059,#96060,#96061,#96062,#96063,#96064,#96065,#96066,#96067,
#96068,#96069,#96070,#96071,#96072,#96073,#96074,#96075,#96076,#96077,#96078,
#96079,#96080,#96081,#96082,#96083,#96084,#96085,#96086,#96087,#96088,#96089,
#96090,#96091,#96092,#96093,#96094,#96095,#96096,#96097,#96098,#96099,#96100,
#96101,#96102,#96103,#96104,#96105,#96106,#96107,#96108,#96109,#96110,#96111,
#96112,#96113,#96114,#96115,#96116,#96117,#96118,#96119,#96120,#96121,#96122,
#96123,#96124,#96125,#96126,#96127,#96128,#96129,#96130,#96131,#96132,#96133,
#96134,#96135,#96136,#96137,#96138,#96139,#96140,#96141,#96142,#96143,#96144,
#96145,#96146,#96147,#96148,#96149,#96150,#96151,#96152,#96153,#96154,#96155,
#96156,#96157,#96158,#96159,#96160,#96161,#96162,#96163,#96164,#96165,#96166,
#96167,#96168,#96169,#96170,#96171,#96172,#96173,#96174,#96175,#96176,#96177,
#96178,#96179,#96180,#96181,#96182,#96183,#96184,#96185,#96186,#96187,#96188,
#96189,#96190,#96191,#96192,#96193,#96194,#96195,#96196,#96197,#96198,#96199,
#96200,#96201,#96202,#96203,#96204,#96205,#96206,#96207,#96208,#96209,#96210,
#96211,#96212,#96213,#96214,#96215,#96216,#96217,#96218,#96219,#96220,#96221,
#96222,#96223,#96224,#96225,#96226,#96227,#96228,#96229,#96230,#96231,#96232,
#96233,#96234,#96235,#96236,#96237,#96238,#96239,#96240,#96241,#96242,#96243,
#96244,#96245,#96246,#96247,#96248,#96249,#96250,#96251,#96252,#96253,#96254,
#96255,#96256,#96257,#96258,#96259,#96260,#96261,#96262,#96263,#96264,#96265,
#96266,#96267,#96268,#96269,#96270,#96271,#96272,#96273,#96274,#96275,#96276,
#96277,#96278,#96279,#96280,#96281,#96282,#96283,#96284,#96285,#96286,#96287,
#96288,#96289,#96290,#96291,#96292,#96293,#96294,#96295,#96296,#96297,#96298,
#96299,#96300,#96301,#96302,#96303,#96304,#96305,#96306,#96307,#96308,#96309,
#96310,#96311,#96312,#96313,#96314,#96315,#96316,#96317,#96318,#96319,#96320,
#96321,#96322,#96323,#96324,#96325,#96326,#96327,#96328,#96329,#96330,#96331,
#96332,#96333,#96334,#96335,#96336,#96337,#96338,#96339,#96340,#96341,#96342,
#96343,#96344,#96345,#96346,#96347,#96348,#96349,#96350,#96351,#96352,#96353,
#96354,#96355,#96356,#96357,#96358,#96359,#96360,#96361,#96362,#96363,#96364,
#96365,#96366,#96367,#96368,#96369,#96370,#96371,#96372,#96373,#96374,#96375,
#96376,#96377,#96378,#96379,#96380,#96381,#96382,#96383,#96384,#96385,#96386,
#96387,#96388,#96389,#96390,#96391,#96392,#96393,#96394,#96395,#96396,#96397,
#96398,#96399,#96400,#96401,#96402,#96403,#96404,#96405,#96406,#96407,#96408,
#96409,#96410,#96411,#96412,#96413,#96414,#96415,#96416,#96417,#96418,#96419,
#96420,#96421,#96422,#96423,#96424,#96425,#96426,#96427,#96428,#96429,#96430,
#96431,#96432,#96433,#96434,#96435,#96436,#96437,#96438,#96439,#96440,#96441,
#96442,#96443,#96444,#96445,#96446,#96447,#96448,#96449,#96450,#96451,#96452,
#96453,#96454,#96455,#96456,#96457,#96458,#96459,#96460,#96461,#96462,#96463,
#96464,#96465,#96466,#96467,#96468,#96469,#96470,#96471,#96472,#96473,#96474,
#96475,#96476,#96477,#96478,#96479,#96480,#96481,#96482,#96483,#96484,#96485,
#96486,#96487,#96488,#96489,#96490,#96491,#96492,#96493,#96494,#96495,#96496,
#96497,#96498,#96499,#96500,#96501,#96502,#96503,#96504,#96505,#96506,#96507,
#96508,#96509,#96510,#96511,#96512,#96513,#96514,#96515,#96516,#96517,#96518,
#96519,#96520,#96521,#96522,#96523,#96524,#96525,#96526,#96527,#96528,#96529,
#96530,#96531,#96532,#96533,#96534,#96535,#96536,#96537,#96538,#96539,#96540,
#96541,#96542,#96543,#96544,#96545,#96546,#96547,#96548,#96549,#96550,#96551,
#96552,#96553,#96554,#96555,#96556,#96557,#96558,#96559,#96560,#96561,#96562,
#96563,#96564,#96565,#96566,#96567,#96568,#96569,#96570,#96571,#96572,#96573,
#96574,#96575,#96576,#96577,#96578,#96579,#96580,#96581,#96582,#96583,#96584,
#96585,#96586,#96587,#96588,#96589,#96590,#96591,#96592,#96593,#96594,#96595,
#96596,#96597,#96598,#96599,#96600,#96601,#96602,#96603,#96604,#96605,#96606,
#96607,#96608,#96609,#96610,#96611,#96612,#96613,#96614,#96615,#96616,#96617,
#96618,#96619,#96620,#96621,#96622,#96623,#96624,#96625,#96626,#96627,#96628,
#96629,#96630,#96631,#96632,#96633,#96634,#96635,#96636,#96637,#96638,#96639,
#96640,#96641,#96642,#96643,#96644,#96645,#96646,#96647,#96648,#96649,#96650,
#96651,#96652,#96653,#96654,#96655,#96656,#96657,#96658,#96659,#96660,#96661,
#96662,#96663,#96664,#96665,#96666,#96667,#96668,#96669,#96670,#96671,#96672,
#96673,#96674,#96675,#96676,#96677,#96678,#96679,#96680,#96681,#96682,#96683,
#96684,#96685,#96686,#96687,#96688,#96689,#96690,#96691,#96692,#96693,#96694,
#96695,#96696,#96697,#96698,#96699,#96700,#96701,#96702,#96703,#96704,#96705,
#96706,#96707,#96708,#96709,#96710,#96711,#96712,#96713,#96714,#96715,#96716,
#96717,#96718,#96719,#96720,#96721,#96722,#96723,#96724,#96725,#96726,#96727,
#96728,#96729,#96730,#96731,#96732,#96733,#96734,#96735,#96736,#96737,#96738,
#96739,#96740,#96741,#96742,#96743,#96744,#96745,#96746,#96747,#96748,#96749,
#96750,#96751,#96752,#96753,#96754,#96755,#96756,#96757,#96758,#96759,#96760,
#96761,#96762,#96763,#96764,#96765,#96766,#96767,#96768,#96769,#96770,#96771,
#96772,#96773,#96774,#96775,#96776,#96777,#96778,#96779,#96780,#96781,#96782,
#96783,#96784,#96785,#96786,#96787,#96788,#96789,#96790,#96791,#96792,#96793,
#96794,#96795,#96796,#96797,#96798,#96799,#96800,#96801,#96802,#96803,#96804,
#96805,#96806,#96807,#96808,#96809,#96810,#96811,#96812,#96813,#96814,#96815,
#96816,#96817,#96818,#96819,#96820,#96821,#96822,#96823,#96824,#96825,#96826,
#96827,#96828,#96829,#96830,#96831,#96832,#96833,#96834,#96835,#96836,#96837,
#96838,#96839,#96840,#96841,#96842,#96843,#96844,#96845,#96846,#96847,#96848,
#96849,#96850,#96851,#96852,#96853,#96854,#96855),.UNSPECIFIED.,.F.,.F.,
(4,3,3,3,3,3,3,3,3,3,3,3,3,3,3,3,3,3,3,3,3,3,3,3,3,3,3,3,3,3,3,3,3,3,3,
3,3,3,3,3,3,3,3,3,3,3,3,3,3,3,3,3,3,3,3,3,3,3,3,3,3,3,3,3,3,3,3,3,3,3,3,
3,3,3,3,3,3,3,3,3,3,3,3,3,3,3,3,3,3,3,3,3,3,3,3,3,3,3,3,3,3,3,3,3,3,3,3,
3,3,3,3,3,3,3,3,3,3,3,3,3,3,3,3,3,3,3,3,3,3,3,3,3,3,3,3,3,3,3,3,3,3,3,3,
3,3,3,3,3,3,3,3,3,3,3,3,3,3,3,3,3,3,3,3,3,3,3,3,3,3,3,3,3,3,3,3,3,3,3,3,
3,3,3,3,3,3,3,3,3,3,3,3,3,3,3,3,3,3,3,3,3,3,3,3,3,3,3,3,3,3,3,3,3,3,3,3,
3,3,3,3,3,3,3,3,3,3,3,3,3,3,3,3,3,3,3,3,3,3,3,3,3,3,3,3,3,3,3,3,3,3,3,3,
3,3,3,3,3,3,3,3,3,3,3,3,3,3,3,3,3,3,3,3,3,3,3,3,3,3,3,3,3,3,3,3,3,3,3,3,
3,3,3,3,3,3,3,3,3,3,3,3,3,3,3,3,3,3,3,3,3,3,3,3,3,3,3,3,3,3,3,3,3,3,3,3,
3,3,3,3,3,3,3,3,3,3,3,3,3,3,3,3,3,3,3,3,3,3,3,3,3,3,3,3,3,3,3,3,3,3,3,3,
3,3,3,3,3,3,3,3,3,3,3,3,3,3,3,3,3,3,3,3,3,3,3,3,3,3,3,3,3,3,3,3,3,3,3,3,
3,4),(-1.,-0.991071428571429,-0.991071405973057,-0.982142857142857,-0.982142834599964,
-0.973214285714286,-0.973214275566846,-0.964285714285714,-0.955357148041666,
-0.955357142857143,-0.946428577574046,-0.946428571428571,-0.937500003529489,
-0.9375,-0.928571433763255,-0.928571428571429,-0.919642857142857,-0.919642854683641,
-0.910714285714286,-0.910714277856615,-0.90397538929407,-0.901785714285714,
-0.896448418480331,-0.892857142857143,-0.892857035697021,-0.888647751552121,
-0.884506308889022,-0.883928673279972,-0.883928571428571,-0.88041123636024,
-0.876936336614861,-0.875,-0.874999573070411,-0.871773427601126,-0.868596771569603,
-0.866071877050543,-0.866071428571429,-0.863553536977713,-0.861044051593477,
-0.858566757473106,-0.857142933290389,-0.857142857142857,-0.854570729186596,
-0.852678571428572,-0.85068776613329,-0.848709234709232,-0.848214285714286,
-0.846942082102984,-0.845982142857143,-0.845238122918132,-0.844308035714286,
-0.842397782896502,-0.84048082150259,-0.839285714285714,-0.836995449126508,
-0.834821428571428,-0.833333712411568,-0.832589285714286,-0.831404902334418,
-0.830357142857143,-0.828409477636648,-0.826459457474174,-0.825892857142857,
-0.824172305158491,-0.822455192368131,-0.821428571428571,-0.821428483905876,
-0.819673336332699,-0.817918766447867,-0.816964285714285,-0.814732142857143,
-0.812990646808756,-0.8125,-0.81036867528272,-0.809523164919251,-0.807406437369691,
-0.805288805989849,-0.803571428571428,-0.801586675846038,-0.798563483815412,
-0.795467160554859,-0.794642857142857,-0.793650901470626,-0.790649071482189,
-0.787671978429273,-0.785714352289099,-0.785714285714286,-0.783406367608846,
-0.781098449503405,-0.779191458689562,-0.777780811792261,-0.777453986656465,
-0.775780896057209,-0.774094604477016,-0.773809523809524,-0.771455749275321,
-0.76983811830604,-0.769213886916033,-0.767482043422238,-0.765748581194053,
-0.765559324410398,-0.763527082629347,-0.761904879293183,-0.761904761904762,
-0.760211049423132,-0.758515188736367,-0.757289982687192,-0.755564339818027,
-0.753968278094141,-0.753644991343596,-0.751592831764285,-0.75,-0.748096146219864,
-0.747767857142857,-0.74602971015346,-0.743681153771395,-0.741326561883123,
-0.741071428571428,-0.739858902252659,-0.738839285714285,-0.738095637949478,
-0.737165178571428,-0.735178034352797,-0.734654017857143,-0.732935246119744,
-0.732142857142857,-0.730345907498532,-0.728557322034361,-0.727678571428572,
-0.726190464852684,-0.725446428571429,-0.724330357142857,-0.723214285714286,
-0.72132026187379,-0.71941280023548,-0.71875,-0.717118396276431,-0.71548846609358,
-0.714285714285714,-0.714284569279444,-0.712216868730684,-0.710146110364231,
-0.708333333333333,-0.706148636368604,-0.70398158883087,-0.702381597545649,
-0.702380952380952,-0.700040414155766,-0.697649358235872,-0.695270917610902,
-0.692873554043546,-0.690611885254948,-0.69047619047619,-0.690474022748346,
-0.688991753412322,-0.687509575139147,-0.686507936507937,-0.68452380952381,
-0.682539682539683,-0.680209262317156,-0.678571642685386,-0.676249377708499,
-0.674603174603175,-0.672618218450647,-0.670006806663296,-0.667384818573573,
-0.666667242024944,-0.666666666666667,-0.663694851668887,-0.660671770900525,
-0.658730158730159,-0.658729982998985,-0.655241597700335,-0.651709329701969,
-0.650793945959924,-0.650793650793651,-0.646576917414535,-0.642857379584437,
-0.642857142857143,-0.637731109382087,-0.634921028244712,-0.634920634920635,
-0.627838030023722,-0.626984353632836,-0.626984126984127,-0.622201404100147,
-0.619047619047619,-0.619047284573871,-0.613777427854794,-0.608408257537255,
-0.607142857142857,-0.60714284698062,-0.599891750889435,-0.595238125156089,
-0.595238095238095,-0.586965854968285,-0.583333340606969,-0.583333333333333,
-0.573165496153514,-0.571428587757185,-0.571428571428571,-0.559523813319172,
-0.55952380952381,-0.547619052116877,-0.547619047619048,-0.535714288280767,
-0.535714285714286,-0.523809523809524,-0.515873015873016,-0.507936512944415,
-0.507936507936508,-0.5,-0.499999996192246,-0.492063492063492,-0.492063478932126,
-0.484366949200099,-0.481481481481481,-0.481481440867044,-0.476190476190476,
-0.476190397017408,-0.471865439838946,-0.468254089647458,-0.468253968253968,
-0.464527668076928,-0.460836274986932,-0.46031746031746,-0.460317411536264,
-0.457262710573874,-0.454249774708069,-0.452381581581904,-0.452380952380952,
-0.449658807753246,-0.446917421123731,-0.444194891123593,-0.441559195015103,
-0.44047619047619,-0.440475982902852,-0.438215137353949,-0.435950436844339,
-0.43452380952381,-0.432258637549228,-0.430021071347414,-0.428571428571429,
-0.428568978804424,-0.426612283828262,-0.424615914690795,-0.422619545553327,
-0.422619047619048,-0.42082140712734,-0.419022095758401,-0.417226299865472,
-0.416666926024893,-0.416666666666667,-0.414295625247005,-0.411934470395318,
-0.410714285714286,-0.408493656754785,-0.406283905537045,-0.404761904761905,
-0.404761500519256,-0.403096206743634,-0.401430208287845,-0.400793650793651,
-0.398674168851715,-0.396825396825397,-0.394841709488377,-0.392858022151356,
-0.390873455520123,-0.388888888888889,-0.38719943767456,-0.386904761904762,
-0.385050373824101,-0.383928571428572,-0.382549746643403,-0.381171896725573,
-0.380952388360775,-0.380952380952381,-0.378568097677262,-0.376234421773945,
-0.375661375661376,-0.373868318870882,-0.372088527038354,-0.370867219366802,
-0.369169637070213,-0.369047893358194,-0.367973292223084,-0.365573066819849,
-0.365079365079365,-0.363318762554276,-0.363095238095238,-0.361445407401825,
-0.359793003859393,-0.358140218092806,-0.357144903583603,-0.357142857142857,
-0.355473461491447,-0.35379548218963,-0.353174603174603,-0.351784903839666,
-0.351190476190476,-0.34957662682823,-0.349206349206349,-0.34722192436045,
-0.345237499514551,-0.343253670392196,-0.341269841269841,-0.339161731810482,
-0.337301587301587,-0.33531747285813,-0.333333358414672,-0.333333333333333,
-0.33058720143975,-0.32779333713046,-0.32738201480293,-0.324561543223382,
-0.321777713208721,-0.321428782196021,-0.321428571428571,-0.318114135640606,
-0.314667391319921,-0.311149612851616,-0.309524729436134,-0.30952380952381,
-0.306184336181973,-0.302734751919678,-0.299293445712499,-0.297619047619048,
-0.297618380297086,-0.293681890016858,-0.289613420134287,-0.285714341509276,
-0.285714285714286,-0.280358734025149,-0.274868515762482,-0.273809523809524,
-0.27380952123257,-0.267412328789522,-0.261904900810491,-0.261904761904762,
-0.255586576240464,-0.250000586120232,-0.25,-0.242926748541942,-0.238095989407649,
-0.236119277627551,-0.230159085420616,-0.23015873015873,-0.225712370063969,
-0.222222557900205,-0.222222222222222,-0.218457566983552,-0.21463599506096,
-0.214286334007192,-0.214285714285714,-0.208717915545674,-0.202946280865649,
-0.202381436484301,-0.202380952380952,-0.195616125035644,-0.190476317028105,
-0.19047619047619,-0.182509579807485,-0.178571468264927,-0.178571428571429,
-0.166666671858936,-0.166666666666667,-0.154761913973698,-0.154761904761905,
-0.142857150422022,-0.142857142857143,-0.133928577558453,-0.133928571428571,
-0.125000004530461,-0.125,-0.116071431663786,-0.116071428571429,-0.107142857142857,
-0.0982142857142857,-0.0892857142857143,-0.0803571428571428,-0.0714285714285714,
-0.0714285676312334,-0.0625,-0.0624999926286917,-0.0535714285714286,-0.0535714184078512,
-0.0446428571428571,-0.0446428453333455,-0.0357142857142857,-0.0357142806094605,
-0.0267857266263663,-0.0267857142857143,-0.0178571772374333,-0.0178571428571429,
-0.00892861062247156,-0.00892857142857143,0.),.UNSPECIFIED.);
#8001=B_SPLINE_CURVE_WITH_KNOTS('',3,(#96856,#96857,#96858,#96859,#96860,
#96861,#96862,#96863,#96864,#96865,#96866,#96867,#96868,#96869,#96870,#96871,
#96872,#96873,#96874,#96875,#96876,#96877),.UNSPECIFIED.,.F.,.F.,(4,2,2,
2,2,2,2,2,2,2,4),(2.02792568943256E-6,0.0187194797883834,0.0270317198253142,
0.0296490618871348,0.030599511546207,0.0312029606220119,0.0317333938792736,
0.0323700195550393,0.0334848245376639,0.0361983254288313,0.0852348509526712),
 .UNSPECIFIED.);
#8002=B_SPLINE_CURVE_WITH_KNOTS('',3,(#96878,#96879,#96880,#96881,#96882,
#96883,#96884,#96885,#96886,#96887,#96888,#96889,#96890,#96891,#96892,#96893,
#96894,#96895,#96896,#96897,#96898,#96899,#96900,#96901,#96902,#96903,#96904,
#96905,#96906,#96907,#96908,#96909,#96910,#96911,#96912,#96913,#96914,#96915,
#96916,#96917,#96918,#96919,#96920),.UNSPECIFIED.,.F.,.F.,(4,3,3,3,3,3,
3,3,3,3,3,3,3,3,4),(1.19276284565608E-6,0.00921698783890213,0.0187194648875106,
0.0270315500022582,0.0296489825432181,0.0305994303610185,0.031202876530675,
0.0317333058143584,0.0323699244425081,0.0334847132766303,0.0361981632966636,
0.0484645045289161,0.0595378820786154,0.0710363226551942,0.0852410290365269),
 .UNSPECIFIED.);
#8003=B_SPLINE_CURVE_WITH_KNOTS('',3,(#97860,#97861,#97862,#97863,#97864,
#97865,#97866,#97867,#97868,#97869,#97870,#97871,#97872,#97873,#97874,#97875,
#97876,#97877,#97878,#97879,#97880,#97881,#97882,#97883,#97884,#97885,#97886,
#97887),.UNSPECIFIED.,.F.,.F.,(4,1,1,1,1,1,1,1,1,1,1,1,1,1,1,1,1,1,1,1,
1,1,1,1,1,4),(3.41679525229117E-14,0.241483590676928,0.482967181353822,
0.96593436270761,1.2074179533845,1.4489015440614,1.69038513473829,1.81112693007674,
1.87149782774596,1.90168327658057,1.93186872541519,2.05261052075363,2.11298141842286,
2.17335231609208,2.2337232137613,2.29409411143053,2.35446500909975,2.41483590676897,
2.53557770210742,2.65631949744587,2.77706129278432,2.89780308812276,3.01854488346121,
3.13928667879966,3.2600284741381,3.38077026947655),.UNSPECIFIED.);
#8004=B_SPLINE_CURVE_WITH_KNOTS('',3,(#97890,#97891,#97892,#97893,#97894,
#97895,#97896,#97897,#97898,#97899,#97900,#97901,#97902,#97903,#97904,#97905,
#97906,#97907,#97908,#97909,#97910,#97911,#97912,#97913,#97914,#97915),
 .UNSPECIFIED.,.F.,.F.,(4,1,1,1,1,1,1,1,1,1,1,1,1,1,1,1,1,1,1,1,1,1,1,4),
(0.00128110943246098,0.1220229047709,0.242764700109339,0.363506495447778,
0.484248290786216,0.604990086124655,0.725731881463094,0.846473676801533,
0.906844574470752,0.967215472139972,1.02758636980919,1.08795726747841,1.14832816514763,
1.20869906281685,1.26906996048607,1.32944085815529,1.45018265349373,1.6916662441706,
1.93314983484748,2.17463342552436,2.41611701620124,2.89908419755499,3.14056778823187,
3.38205137890875),.UNSPECIFIED.);
#8005=B_SPLINE_CURVE_WITH_KNOTS('',3,(#98083,#98084,#98085,#98086,#98087,
#98088,#98089,#98090,#98091,#98092,#98093,#98094,#98095,#98096,#98097,#98098,
#98099,#98100,#98101,#98102,#98103,#98104,#98105,#98106,#98107,#98108,#98109,
#98110),.UNSPECIFIED.,.F.,.F.,(4,1,1,1,1,1,1,1,1,1,1,1,1,1,1,1,1,1,1,1,
1,1,1,1,1,4),(-3.38077026947655,-3.2600284741381,-3.13928667879966,-3.01854488346121,
-2.89780308812276,-2.77706129278432,-2.65631949744587,-2.53557770210742,
-2.41483590676897,-2.35446500909975,-2.29409411143053,-2.2337232137613,
-2.17335231609208,-2.11298141842286,-2.05261052075363,-1.93186872541519,
-1.90168327658057,-1.87149782774596,-1.81112693007674,-1.69038513473829,
-1.4489015440614,-1.2074179533845,-0.96593436270761,-0.482967181353822,
-0.241483590676928,-3.41679525229117E-14),.UNSPECIFIED.);
#8006=B_SPLINE_CURVE_WITH_KNOTS('',3,(#98253,#98254,#98255,#98256,#98257,
#98258,#98259,#98260,#98261,#98262,#98263,#98264,#98265,#98266,#98267,#98268,
#98269,#98270,#98271,#98272,#98273,#98274,#98275,#98276,#98277,#98278,#98279),
 .UNSPECIFIED.,.F.,.F.,(4,1,1,1,1,1,1,1,1,1,1,1,1,1,1,1,1,1,1,1,1,1,1,1,
4),(-3.41890546063757,-3.17478943294163,-2.93067340524569,-2.4424413498538,
-2.19832532215786,-1.95420929446192,-1.83215128061395,-1.71009326676598,
-1.46597723907004,-1.34391922522207,-1.2218612113741,-1.1913467079121,-1.16083220445011,
-1.09980319752612,-1.03877419060214,-0.977745183678154,-0.855687169830184,
-0.733629155982213,-0.611571142134242,-0.489513128286272,-0.367455114438301,
-0.24539710059033,-0.12333908674236,-0.0623100798183742,-0.00128107289438891),
 .UNSPECIFIED.);
#8007=B_SPLINE_CURVE_WITH_KNOTS('',3,(#98281,#98282,#98283,#98284,#98285,
#98286,#98287,#98288,#98289,#98290),.UNSPECIFIED.,.F.,.F.,(4,3,3,4),(0.,
0.0193508010140011,0.0377654905305143,0.0545713498196275),.UNSPECIFIED.);
#8008=B_SPLINE_CURVE_WITH_KNOTS('',3,(#98292,#98293,#98294,#98295),
 .UNSPECIFIED.,.F.,.F.,(4,4),(-0.324683822128034,0.),.UNSPECIFIED.);
#8009=B_SPLINE_CURVE_WITH_KNOTS('',3,(#98297,#98298,#98299,#98300,#98301,
#98302,#98303,#98304,#98305,#98306,#98307,#98308,#98309),.UNSPECIFIED.,
 .F.,.F.,(4,3,3,3,4),(0.,0.0219603143385993,0.0442891506855458,0.067805646823492,
0.0861862379095711),.UNSPECIFIED.);
#8010=B_SPLINE_CURVE_WITH_KNOTS('',3,(#98315,#98316,#98317,#98318),
 .UNSPECIFIED.,.F.,.F.,(4,4),(-0.0771338280522776,-3.23236617932421E-6),
 .UNSPECIFIED.);
#8011=B_SPLINE_CURVE_WITH_KNOTS('',3,(#98320,#98321,#98322,#98323),
 .UNSPECIFIED.,.F.,.F.,(4,4),(0.,0.0523726503223924),.UNSPECIFIED.);
#8012=B_SPLINE_CURVE_WITH_KNOTS('',3,(#98325,#98326,#98327,#98328,#98329,
#98330,#98331,#98332,#98333,#98334,#98335,#98336,#98337,#98338,#98339,#98340,
#98341,#98342,#98343,#98344,#98345,#98346),.UNSPECIFIED.,.F.,.F.,(4,3,3,
3,3,3,3,4),(-0.324714104720811,-0.275894006039472,-0.219811108021725,-0.164858331016294,
-0.117285452027523,-0.0705633041497707,-0.0225934601586412,-2.03395786214367E-15),
 .UNSPECIFIED.);
#8013=B_SPLINE_CURVE_WITH_KNOTS('',3,(#98347,#98348,#98349,#98350),
 .UNSPECIFIED.,.F.,.F.,(4,4),(0.,0.0900393973869889),.UNSPECIFIED.);
#8014=B_SPLINE_CURVE_WITH_KNOTS('',3,(#98487,#98488,#98489,#98490,#98491,
#98492,#98493,#98494,#98495,#98496,#98497,#98498,#98499,#98500,#98501,#98502,
#98503,#98504,#98505,#98506,#98507,#98508,#98509,#98510,#98511,#98512,#98513),
 .UNSPECIFIED.,.F.,.F.,(4,1,1,1,1,1,1,1,1,1,1,1,1,1,1,1,1,1,1,1,1,1,1,1,
4),(0.00128107289438891,0.0623100798183742,0.12333908674236,0.24539710059033,
0.367455114438301,0.489513128286272,0.611571142134242,0.733629155982213,
0.855687169830184,0.977745183678154,1.03877419060214,1.09980319752612,1.16083220445011,
1.1913467079121,1.2218612113741,1.34391922522207,1.46597723907004,1.71009326676598,
1.83215128061395,1.95420929446192,2.19832532215786,2.4424413498538,2.93067340524569,
3.17478943294163,3.41890546063757),.UNSPECIFIED.);
#8015=B_SPLINE_CURVE_WITH_KNOTS('',3,(#98517,#98518,#98519,#98520,#98521,
#98522,#98523,#98524,#98525,#98526,#98527,#98528,#98529,#98530,#98531,#98532,
#98533,#98534,#98535,#98536,#98537,#98538,#98539,#98540,#98541,#98542,#98543,
#98544,#98545),.UNSPECIFIED.,.F.,.F.,(4,1,1,1,1,1,1,1,1,1,1,1,1,1,1,1,1,
1,1,1,1,1,1,1,1,1,4),(0.,0.244116027696041,0.488232055392083,0.976464110784166,
1.22058013848021,1.46469616617625,1.70881219387229,1.83087020772031,1.89189921464432,
1.95292822156833,2.07498623541635,2.13601524234036,2.19704424926437,2.25807325618838,
2.28858775965039,2.31910226311239,2.3801312700364,2.44116027696041,2.56321829080843,
2.68527630465646,2.80733431850448,2.9293923323525,3.05145034620052,3.17350836004854,
3.29556637389656,3.35659538082057,3.41762438774458),.UNSPECIFIED.);
#8016=B_SPLINE_CURVE_WITH_KNOTS('',3,(#98707,#98708,#98709,#98710,#98711,
#98712,#98713,#98714,#98715,#98716,#98717,#98718,#98719,#98720,#98721,#98722,
#98723,#98724,#98725,#98726,#98727,#98728,#98729,#98730,#98731,#98732,#98733,
#98734,#98735),.UNSPECIFIED.,.F.,.F.,(4,1,1,1,1,1,1,1,1,1,1,1,1,1,1,1,1,
1,1,1,1,1,1,1,1,1,4),(-3.41762438774458,-3.35659538082057,-3.29556637389656,
-3.17350836004854,-3.05145034620052,-2.9293923323525,-2.80733431850448,
-2.68527630465646,-2.56321829080843,-2.44116027696041,-2.3801312700364,
-2.31910226311239,-2.28858775965039,-2.25807325618838,-2.19704424926437,
-2.13601524234036,-2.07498623541635,-1.95292822156833,-1.89189921464432,
-1.83087020772031,-1.70881219387229,-1.46469616617625,-1.22058013848021,
-0.976464110784166,-0.488232055392083,-0.244116027696041,0.),
 .UNSPECIFIED.);
#8017=B_SPLINE_CURVE_WITH_KNOTS('',3,(#98878,#98879,#98880,#98881,#98882,
#98883,#98884,#98885,#98886,#98887,#98888,#98889,#98890,#98891,#98892,#98893,
#98894,#98895,#98896,#98897,#98898,#98899,#98900,#98901,#98902,#98903),
 .UNSPECIFIED.,.F.,.F.,(4,1,1,1,1,1,1,1,1,1,1,1,1,1,1,1,1,1,1,1,1,1,1,4),
(-3.38205137890875,-3.14056778823187,-2.89908419755499,-2.41611701620124,
-2.17463342552436,-1.93314983484748,-1.6916662441706,-1.45018265349373,
-1.32944085815529,-1.26906996048607,-1.20869906281685,-1.14832816514763,
-1.08795726747841,-1.02758636980919,-0.967215472139972,-0.906844574470752,
-0.846473676801533,-0.725731881463094,-0.604990086124655,-0.484248290786216,
-0.363506495447778,-0.242764700109339,-0.1220229047709,-0.00128110943246098),
 .UNSPECIFIED.);
#8018=B_SPLINE_CURVE_WITH_KNOTS('',3,(#98905,#98906,#98907,#98908),
 .UNSPECIFIED.,.F.,.F.,(4,4),(0.,0.0900415523927057),.UNSPECIFIED.);
#8019=B_SPLINE_CURVE_WITH_KNOTS('',3,(#98910,#98911,#98912,#98913,#98914,
#98915,#98916,#98917,#98918,#98919,#98920,#98921,#98922,#98923,#98924,#98925,
#98926,#98927,#98928,#98929,#98930,#98931),.UNSPECIFIED.,.F.,.F.,(4,3,3,
3,3,3,3,4),(-0.324714104720872,-0.276900417543011,-0.230088047477266,-0.182596766871424,
-0.130785402885425,-0.0701896017717822,-0.0219763511414979,-9.48740063601895E-16),
 .UNSPECIFIED.);
#8020=B_SPLINE_CURVE_WITH_KNOTS('',3,(#98933,#98934,#98935,#98936),
 .UNSPECIFIED.,.F.,.F.,(4,4),(0.,0.0523713743724485),.UNSPECIFIED.);
#8021=B_SPLINE_CURVE_WITH_KNOTS('',3,(#98938,#98939,#98940,#98941,#98942,
#98943,#98944,#98945,#98946,#98947,#98948,#98949,#98950),.UNSPECIFIED.,
 .F.,.F.,(4,3,3,3,4),(-0.0771330433688407,-0.0532273517721988,-0.0290520233522164,
-0.00468787888284027,-1.22307313571325E-14),.UNSPECIFIED.);
#8022=B_SPLINE_CURVE_WITH_KNOTS('',3,(#98956,#98957,#98958,#98959,#98960,
#98961,#98962,#98963,#98964,#98965,#98966,#98967,#98968),.UNSPECIFIED.,
 .F.,.F.,(4,3,3,3,4),(1.94736699620138E-16,0.0234829329857791,0.0461120293622291,
0.068043235237682,0.0861862379095512),.UNSPECIFIED.);
#8023=B_SPLINE_CURVE_WITH_KNOTS('',3,(#98970,#98971,#98972,#98973),
 .UNSPECIFIED.,.F.,.F.,(4,4),(-0.324683822128098,0.),.UNSPECIFIED.);
#8024=B_SPLINE_CURVE_WITH_KNOTS('',3,(#98974,#98975,#98976,#98977,#98978,
#98979,#98980,#98981,#98982,#98983),.UNSPECIFIED.,.F.,.F.,(4,3,3,4),(0.,
0.0183070922409377,0.0374313150775962,0.0545713498196216),.UNSPECIFIED.);
#8025=B_SPLINE_CURVE_WITH_KNOTS('',3,(#99136,#99137,#99138,#99139),
 .UNSPECIFIED.,.F.,.F.,(4,4),(-0.0900415523927057,0.),.UNSPECIFIED.);
#8026=B_SPLINE_CURVE_WITH_KNOTS('',3,(#99163,#99164,#99165,#99166),
 .UNSPECIFIED.,.F.,.F.,(4,4),(9.48740063601895E-16,0.324714104720872),
 .UNSPECIFIED.);
#8027=B_SPLINE_CURVE_WITH_KNOTS('',3,(#99188,#99189,#99190,#99191),
 .UNSPECIFIED.,.F.,.F.,(4,4),(-0.0523713743724485,0.),.UNSPECIFIED.);
#8028=B_SPLINE_CURVE_WITH_KNOTS('',3,(#99224,#99225,#99226,#99227,#99228,
#99229),.UNSPECIFIED.,.F.,.F.,(4,2,4),(1.22307313571325E-14,0.0771338280521436,
0.0784358874721452),.UNSPECIFIED.);
#8029=B_SPLINE_CURVE_WITH_KNOTS('',3,(#99230,#99231,#99232,#99233,#99234,
#99235,#99236,#99237,#99238,#99239,#99240,#99241,#99242,#99243,#99244,#99245),
 .UNSPECIFIED.,.F.,.F.,(4,2,2,2,2,2,2,4),(-0.00022668224436296,0.,0.00761586611745941,
0.0150248302469871,0.0236797709907964,0.0310979044849912,0.0368289860988756,
0.0428654183141884),.UNSPECIFIED.);
#8030=B_SPLINE_CURVE_WITH_KNOTS('',3,(#99262,#99263,#99264,#99265,#99266,
#99267,#99268,#99269,#99270,#99271,#99272,#99273,#99274,#99275,#99276,#99277),
 .UNSPECIFIED.,.F.,.F.,(4,2,2,2,2,2,2,4),(-0.0509737628840132,-0.0507050440328071,
-0.0417234339127921,-0.0329872447452147,-0.0226497365660009,-0.0138121252681416,
-0.00708364657956319,0.),.UNSPECIFIED.);
#8031=B_SPLINE_CURVE_WITH_KNOTS('',3,(#99301,#99302,#99303,#99304),
 .UNSPECIFIED.,.F.,.F.,(4,4),(-0.0523726503223924,0.),.UNSPECIFIED.);
#8032=B_SPLINE_CURVE_WITH_KNOTS('',3,(#99336,#99337,#99338,#99339,#99340,
#99341),.UNSPECIFIED.,.F.,.F.,(4,2,4),(-0.00130205941990691,0.,0.0771338280522776),
 .UNSPECIFIED.);
#8033=B_SPLINE_CURVE_WITH_KNOTS('',3,(#99364,#99365,#99366,#99367),
 .UNSPECIFIED.,.F.,.F.,(4,4),(2.03395786214367E-15,0.324714104720811),
 .UNSPECIFIED.);
#8034=B_SPLINE_CURVE_WITH_KNOTS('',3,(#99388,#99389,#99390,#99391),
 .UNSPECIFIED.,.F.,.F.,(4,4),(-0.0900393973869889,0.),.UNSPECIFIED.);
#8035=B_SPLINE_CURVE_WITH_KNOTS('',3,(#99404,#99405,#99406,#99407,#99408,
#99409),.UNSPECIFIED.,.F.,.F.,(4,2,4),(-0.0750162613442511,-0.0337302597397184,
-6.17748433559551E-7),.UNSPECIFIED.);
#8036=B_SPLINE_CURVE_WITH_KNOTS('',3,(#99410,#99411,#99412,#99413,#99414,
#99415,#99416,#99417,#99418,#99419,#99420,#99421,#99422,#99423),
 .UNSPECIFIED.,.F.,.F.,(4,2,2,2,2,2,4),(-0.0264541140821501,-0.017390110288006,
-0.011146376492299,-0.00376454098685937,-0.00160326722853797,-0.00077940018444644,
0.),.UNSPECIFIED.);
#8037=B_SPLINE_CURVE_WITH_KNOTS('',3,(#99430,#99431,#99432,#99433,#99434,
#99435,#99436,#99437,#99438,#99439,#99440,#99441),.UNSPECIFIED.,.F.,.F.,
(4,2,2,2,2,4),(-0.0641362373983827,-0.0612026902636628,-0.0580728061365246,
-0.0499071281293661,-0.0252640899793066,-5.18312203295901E-7),
 .UNSPECIFIED.);
#8038=B_SPLINE_CURVE_WITH_KNOTS('',3,(#99443,#99444,#99445,#99446,#99447,
#99448),.UNSPECIFIED.,.F.,.F.,(4,2,4),(-0.0743753002286862,-0.0371638184856682,
-1.00312867462312E-6),.UNSPECIFIED.);
#8039=B_SPLINE_CURVE_WITH_KNOTS('',3,(#99480,#99481,#99482,#99483),
 .UNSPECIFIED.,.F.,.F.,(4,4),(0.,0.261923043407585),.UNSPECIFIED.);
#8040=B_SPLINE_CURVE_WITH_KNOTS('',3,(#99541,#99542,#99543,#99544),
 .UNSPECIFIED.,.F.,.F.,(4,4),(-0.0545713498196275,0.),.UNSPECIFIED.);
#8041=B_SPLINE_CURVE_WITH_KNOTS('',3,(#99547,#99548,#99549,#99550),
 .UNSPECIFIED.,.F.,.F.,(4,4),(-0.0545713498196216,0.),.UNSPECIFIED.);
#8042=B_SPLINE_CURVE_WITH_KNOTS('',3,(#99572,#99573,#99574,#99575),
 .UNSPECIFIED.,.F.,.F.,(4,4),(0.0627607787207755,0.324683822128098),
 .UNSPECIFIED.);
#8043=VERTEX_POINT('',#28466);
#8044=VERTEX_POINT('',#28467);
#8045=VERTEX_POINT('',#28474);
#8046=VERTEX_POINT('',#28524);
#8047=VERTEX_POINT('',#28531);
#8048=VERTEX_POINT('',#28707);
#8049=VERTEX_POINT('',#28715);
#8050=VERTEX_POINT('',#28723);
#8051=VERTEX_POINT('',#28776);
#8052=VERTEX_POINT('',#28781);
#8053=VERTEX_POINT('',#28788);
#8054=VERTEX_POINT('',#28793);
#8055=VERTEX_POINT('',#28798);
#8056=VERTEX_POINT('',#28808);
#8057=VERTEX_POINT('',#28810);
#8058=VERTEX_POINT('',#38648);
#8059=VERTEX_POINT('',#38649);
#8060=VERTEX_POINT('',#38659);
#8061=VERTEX_POINT('',#38669);
#8062=VERTEX_POINT('',#38764);
#8063=VERTEX_POINT('',#38775);
#8064=VERTEX_POINT('',#38782);
#8065=VERTEX_POINT('',#38795);
#8066=VERTEX_POINT('',#38800);
#8067=VERTEX_POINT('',#38810);
#8068=VERTEX_POINT('',#38819);
#8069=VERTEX_POINT('',#38826);
#8070=VERTEX_POINT('',#38936);
#8071=VERTEX_POINT('',#38945);
#8072=VERTEX_POINT('',#38951);
#8073=VERTEX_POINT('',#39052);
#8074=VERTEX_POINT('',#39062);
#8075=VERTEX_POINT('',#39073);
#8076=VERTEX_POINT('',#39082);
#8077=VERTEX_POINT('',#39092);
#8078=VERTEX_POINT('',#39103);
#8079=VERTEX_POINT('',#39114);
#8080=VERTEX_POINT('',#39121);
#8081=VERTEX_POINT('',#39128);
#8082=VERTEX_POINT('',#39135);
#8083=VERTEX_POINT('',#39142);
#8084=VERTEX_POINT('',#39159);
#8085=VERTEX_POINT('',#39164);
#8086=VERTEX_POINT('',#39185);
#8087=VERTEX_POINT('',#39190);
#8088=VERTEX_POINT('',#39264);
#8089=VERTEX_POINT('',#39272);
#8090=VERTEX_POINT('',#39283);
#8091=VERTEX_POINT('',#39291);
#8092=VERTEX_POINT('',#39371);
#8093=VERTEX_POINT('',#39475);
#8094=VERTEX_POINT('',#39487);
#8095=VERTEX_POINT('',#39582);
#8096=VERTEX_POINT('',#39590);
#8097=VERTEX_POINT('',#39670);
#8098=VERTEX_POINT('',#39723);
#8099=VERTEX_POINT('',#39730);
#8100=VERTEX_POINT('',#39735);
#8101=VERTEX_POINT('',#39788);
#8102=VERTEX_POINT('',#39793);
#8103=VERTEX_POINT('',#39810);
#8104=VERTEX_POINT('',#39816);
#8105=VERTEX_POINT('',#39825);
#8106=VERTEX_POINT('',#39962);
#8107=VERTEX_POINT('',#40036);
#8108=VERTEX_POINT('',#40047);
#8109=VERTEX_POINT('',#40056);
#8110=VERTEX_POINT('',#40065);
#8111=VERTEX_POINT('',#40077);
#8112=VERTEX_POINT('',#40089);
#8113=VERTEX_POINT('',#40100);
#8114=VERTEX_POINT('',#40110);
#8115=VERTEX_POINT('',#40115);
#8116=VERTEX_POINT('',#40126);
#8117=VERTEX_POINT('',#40251);
#8118=VERTEX_POINT('',#40319);
#8119=VERTEX_POINT('',#40334);
#8120=VERTEX_POINT('',#40426);
#8121=VERTEX_POINT('',#40433);
#8122=VERTEX_POINT('',#40443);
#8123=VERTEX_POINT('',#40456);
#8124=VERTEX_POINT('',#40465);
#8125=VERTEX_POINT('',#40542);
#8126=VERTEX_POINT('',#40562);
#8127=VERTEX_POINT('',#40563);
#8128=VERTEX_POINT('',#40568);
#8129=VERTEX_POINT('',#40574);
#8130=VERTEX_POINT('',#40585);
#8131=VERTEX_POINT('',#40594);
#8132=VERTEX_POINT('',#40601);
#8133=VERTEX_POINT('',#40690);
#8134=VERTEX_POINT('',#40728);
#8135=VERTEX_POINT('',#40829);
#8136=VERTEX_POINT('',#40835);
#8137=VERTEX_POINT('',#40841);
#8138=VERTEX_POINT('',#40842);
#8139=VERTEX_POINT('',#40851);
#8140=VERTEX_POINT('',#40977);
#8141=VERTEX_POINT('',#40978);
#8142=VERTEX_POINT('',#40983);
#8143=VERTEX_POINT('',#41015);
#8144=VERTEX_POINT('',#41020);
#8145=VERTEX_POINT('',#41025);
#8146=VERTEX_POINT('',#41041);
#8147=VERTEX_POINT('',#41048);
#8148=VERTEX_POINT('',#41054);
#8149=VERTEX_POINT('',#41059);
#8150=VERTEX_POINT('',#41072);
#8151=VERTEX_POINT('',#41073);
#8152=VERTEX_POINT('',#41132);
#8153=VERTEX_POINT('',#41362);
#8154=VERTEX_POINT('',#41368);
#8155=VERTEX_POINT('',#41375);
#8156=VERTEX_POINT('',#41381);
#8157=VERTEX_POINT('',#41386);
#8158=VERTEX_POINT('',#41391);
#8159=VERTEX_POINT('',#41396);
#8160=VERTEX_POINT('',#41402);
#8161=VERTEX_POINT('',#41455);
#8162=VERTEX_POINT('',#41517);
#8163=VERTEX_POINT('',#41525);
#8164=VERTEX_POINT('',#52341);
#8165=VERTEX_POINT('',#52342);
#8166=VERTEX_POINT('',#52352);
#8167=VERTEX_POINT('',#52364);
#8168=VERTEX_POINT('',#52450);
#8169=VERTEX_POINT('',#52530);
#8170=VERTEX_POINT('',#52539);
#8171=VERTEX_POINT('',#52544);
#8172=VERTEX_POINT('',#52609);
#8173=VERTEX_POINT('',#52618);
#8174=VERTEX_POINT('',#52704);
#8175=VERTEX_POINT('',#52712);
#8176=VERTEX_POINT('',#52783);
#8177=VERTEX_POINT('',#52908);
#8178=VERTEX_POINT('',#52991);
#8179=VERTEX_POINT('',#52998);
#8180=VERTEX_POINT('',#53008);
#8181=VERTEX_POINT('',#53019);
#8182=VERTEX_POINT('',#53031);
#8183=VERTEX_POINT('',#53126);
#8184=VERTEX_POINT('',#53191);
#8185=VERTEX_POINT('',#53200);
#8186=VERTEX_POINT('',#53298);
#8187=VERTEX_POINT('',#53306);
#8188=VERTEX_POINT('',#53440);
#8189=VERTEX_POINT('',#53538);
#8190=VERTEX_POINT('',#53544);
#8191=VERTEX_POINT('',#53549);
#8192=VERTEX_POINT('',#53556);
#8193=VERTEX_POINT('',#53575);
#8194=VERTEX_POINT('',#53582);
#8195=VERTEX_POINT('',#53595);
#8196=VERTEX_POINT('',#53645);
#8197=VERTEX_POINT('',#53651);
#8198=VERTEX_POINT('',#53670);
#8199=VERTEX_POINT('',#53768);
#8200=VERTEX_POINT('',#53866);
#8201=VERTEX_POINT('',#53880);
#8202=VERTEX_POINT('',#53890);
#8203=VERTEX_POINT('',#53898);
#8204=VERTEX_POINT('',#53999);
#8205=VERTEX_POINT('',#54007);
#8206=VERTEX_POINT('',#54063);
#8207=VERTEX_POINT('',#54068);
#8208=VERTEX_POINT('',#54095);
#8209=VERTEX_POINT('',#54100);
#8210=VERTEX_POINT('',#54107);
#8211=VERTEX_POINT('',#54124);
#8212=VERTEX_POINT('',#54131);
#8213=VERTEX_POINT('',#54138);
#8214=VERTEX_POINT('',#54212);
#8215=VERTEX_POINT('',#54220);
#8216=VERTEX_POINT('',#54285);
#8217=VERTEX_POINT('',#54295);
#8218=VERTEX_POINT('',#54304);
#8219=VERTEX_POINT('',#54315);
#8220=VERTEX_POINT('',#54325);
#8221=VERTEX_POINT('',#54333);
#8222=VERTEX_POINT('',#54342);
#8223=VERTEX_POINT('',#54428);
#8224=VERTEX_POINT('',#54535);
#8225=VERTEX_POINT('',#54585);
#8226=VERTEX_POINT('',#54595);
#8227=VERTEX_POINT('',#54669);
#8228=VERTEX_POINT('',#54676);
#8229=VERTEX_POINT('',#54756);
#8230=VERTEX_POINT('',#54761);
#8231=VERTEX_POINT('',#54802);
#8232=VERTEX_POINT('',#54979);
#8233=VERTEX_POINT('',#54980);
#8234=VERTEX_POINT('',#54982);
#8235=VERTEX_POINT('',#54987);
#8236=VERTEX_POINT('',#54992);
#8237=VERTEX_POINT('',#54998);
#8238=VERTEX_POINT('',#55051);
#8239=VERTEX_POINT('',#55056);
#8240=VERTEX_POINT('',#55139);
#8241=VERTEX_POINT('',#55145);
#8242=VERTEX_POINT('',#55157);
#8243=VERTEX_POINT('',#55168);
#8244=VERTEX_POINT('',#55169);
#8245=VERTEX_POINT('',#55175);
#8246=VERTEX_POINT('',#55194);
#8247=VERTEX_POINT('',#55195);
#8248=VERTEX_POINT('',#55200);
#8249=VERTEX_POINT('',#55492);
#8250=VERTEX_POINT('',#55499);
#8251=VERTEX_POINT('',#55727);
#8252=VERTEX_POINT('',#55729);
#8253=VERTEX_POINT('',#56052);
#8254=VERTEX_POINT('',#56058);
#8255=VERTEX_POINT('',#56081);
#8256=VERTEX_POINT('',#56083);
#8257=VERTEX_POINT('',#56298);
#8258=VERTEX_POINT('',#56304);
#8259=VERTEX_POINT('',#56333);
#8260=VERTEX_POINT('',#56335);
#8261=VERTEX_POINT('',#56552);
#8262=VERTEX_POINT('',#56567);
#8263=VERTEX_POINT('',#56597);
#8264=VERTEX_POINT('',#56675);
#8265=VERTEX_POINT('',#56802);
#8266=VERTEX_POINT('',#56829);
#8267=VERTEX_POINT('',#56996);
#8268=VERTEX_POINT('',#57039);
#8269=VERTEX_POINT('',#57078);
#8270=VERTEX_POINT('',#57167);
#8271=VERTEX_POINT('',#57449);
#8272=VERTEX_POINT('',#57534);
#8273=VERTEX_POINT('',#57577);
#8274=VERTEX_POINT('',#57624);
#8275=VERTEX_POINT('',#57799);
#8276=VERTEX_POINT('',#57838);
#8277=VERTEX_POINT('',#57961);
#8278=VERTEX_POINT('',#58645);
#8279=VERTEX_POINT('',#59067);
#8280=VERTEX_POINT('',#59068);
#8281=VERTEX_POINT('',#59070);
#8282=VERTEX_POINT('',#59072);
#8283=VERTEX_POINT('',#59077);
#8284=VERTEX_POINT('',#59078);
#8285=VERTEX_POINT('',#59083);
#8286=VERTEX_POINT('',#59085);
#8287=VERTEX_POINT('',#59089);
#8288=VERTEX_POINT('',#59090);
#8289=VERTEX_POINT('',#59092);
#8290=VERTEX_POINT('',#59094);
#8291=VERTEX_POINT('',#59098);
#8292=VERTEX_POINT('',#59102);
#8293=VERTEX_POINT('',#59106);
#8294=VERTEX_POINT('',#59108);
#8295=VERTEX_POINT('',#59112);
#8296=VERTEX_POINT('',#59114);
#8297=VERTEX_POINT('',#59118);
#8298=VERTEX_POINT('',#59122);
#8299=VERTEX_POINT('',#59124);
#8300=VERTEX_POINT('',#59126);
#8301=VERTEX_POINT('',#59130);
#8302=VERTEX_POINT('',#59136);
#8303=VERTEX_POINT('',#59138);
#8304=VERTEX_POINT('',#59144);
#8305=VERTEX_POINT('',#59145);
#8306=VERTEX_POINT('',#59148);
#8307=VERTEX_POINT('',#59154);
#8308=VERTEX_POINT('',#59158);
#8309=VERTEX_POINT('',#59160);
#8310=VERTEX_POINT('',#59166);
#8311=VERTEX_POINT('',#59168);
#8312=VERTEX_POINT('',#59170);
#8313=VERTEX_POINT('',#59174);
#8314=VERTEX_POINT('',#59180);
#8315=VERTEX_POINT('',#59182);
#8316=VERTEX_POINT('',#59188);
#8317=VERTEX_POINT('',#59189);
#8318=VERTEX_POINT('',#59191);
#8319=VERTEX_POINT('',#59193);
#8320=VERTEX_POINT('',#59197);
#8321=VERTEX_POINT('',#59201);
#8322=VERTEX_POINT('',#59205);
#8323=VERTEX_POINT('',#59207);
#8324=VERTEX_POINT('',#59211);
#8325=VERTEX_POINT('',#59213);
#8326=VERTEX_POINT('',#59217);
#8327=VERTEX_POINT('',#59221);
#8328=VERTEX_POINT('',#59222);
#8329=VERTEX_POINT('',#59225);
#8330=VERTEX_POINT('',#59231);
#8331=VERTEX_POINT('',#59235);
#8332=VERTEX_POINT('',#59237);
#8333=VERTEX_POINT('',#59243);
#8334=VERTEX_POINT('',#59245);
#8335=VERTEX_POINT('',#59247);
#8336=VERTEX_POINT('',#59251);
#8337=VERTEX_POINT('',#59252);
#8338=VERTEX_POINT('',#59254);
#8339=VERTEX_POINT('',#59256);
#8340=VERTEX_POINT('',#59258);
#8341=VERTEX_POINT('',#59260);
#8342=VERTEX_POINT('',#59262);
#8343=VERTEX_POINT('',#59264);
#8344=VERTEX_POINT('',#59266);
#8345=VERTEX_POINT('',#59268);
#8346=VERTEX_POINT('',#59270);
#8347=VERTEX_POINT('',#59272);
#8348=VERTEX_POINT('',#59274);
#8349=VERTEX_POINT('',#59276);
#8350=VERTEX_POINT('',#59278);
#8351=VERTEX_POINT('',#59280);
#8352=VERTEX_POINT('',#59282);
#8353=VERTEX_POINT('',#59284);
#8354=VERTEX_POINT('',#59286);
#8355=VERTEX_POINT('',#59288);
#8356=VERTEX_POINT('',#59290);
#8357=VERTEX_POINT('',#59292);
#8358=VERTEX_POINT('',#59294);
#8359=VERTEX_POINT('',#59296);
#8360=VERTEX_POINT('',#59299);
#8361=VERTEX_POINT('',#59301);
#8362=VERTEX_POINT('',#59302);
#8363=VERTEX_POINT('',#59304);
#8364=VERTEX_POINT('',#59306);
#8365=VERTEX_POINT('',#59309);
#8366=VERTEX_POINT('',#59311);
#8367=VERTEX_POINT('',#59313);
#8368=VERTEX_POINT('',#59315);
#8369=VERTEX_POINT('',#59317);
#8370=VERTEX_POINT('',#59319);
#8371=VERTEX_POINT('',#59323);
#8372=VERTEX_POINT('',#59325);
#8373=VERTEX_POINT('',#59326);
#8374=VERTEX_POINT('',#59328);
#8375=VERTEX_POINT('',#59334);
#8376=VERTEX_POINT('',#59337);
#8377=VERTEX_POINT('',#59340);
#8378=VERTEX_POINT('',#59342);
#8379=VERTEX_POINT('',#59346);
#8380=VERTEX_POINT('',#59348);
#8381=VERTEX_POINT('',#59352);
#8382=VERTEX_POINT('',#59354);
#8383=VERTEX_POINT('',#59360);
#8384=VERTEX_POINT('',#59362);
#8385=VERTEX_POINT('',#59366);
#8386=VERTEX_POINT('',#59370);
#8387=VERTEX_POINT('',#59376);
#8388=VERTEX_POINT('',#59378);
#8389=VERTEX_POINT('',#59382);
#8390=VERTEX_POINT('',#59386);
#8391=VERTEX_POINT('',#59392);
#8392=VERTEX_POINT('',#59397);
#8393=VERTEX_POINT('',#59403);
#8394=VERTEX_POINT('',#59407);
#8395=VERTEX_POINT('',#59411);
#8396=VERTEX_POINT('',#59413);
#8397=VERTEX_POINT('',#59417);
#8398=VERTEX_POINT('',#59421);
#8399=VERTEX_POINT('',#59425);
#8400=VERTEX_POINT('',#59426);
#8401=VERTEX_POINT('',#59431);
#8402=VERTEX_POINT('',#59433);
#8403=VERTEX_POINT('',#59439);
#8404=VERTEX_POINT('',#59440);
#8405=VERTEX_POINT('',#59447);
#8406=VERTEX_POINT('',#59448);
#8407=VERTEX_POINT('',#59455);
#8408=VERTEX_POINT('',#59459);
#8409=VERTEX_POINT('',#59463);
#8410=VERTEX_POINT('',#59464);
#8411=VERTEX_POINT('',#59469);
#8412=VERTEX_POINT('',#59473);
#8413=VERTEX_POINT('',#59474);
#8414=VERTEX_POINT('',#59479);
#8415=VERTEX_POINT('',#59483);
#8416=VERTEX_POINT('',#59484);
#8417=VERTEX_POINT('',#59489);
#8418=VERTEX_POINT('',#59499);
#8419=VERTEX_POINT('',#59501);
#8420=VERTEX_POINT('',#59507);
#8421=VERTEX_POINT('',#59509);
#8422=VERTEX_POINT('',#59513);
#8423=VERTEX_POINT('',#59514);
#8424=VERTEX_POINT('',#59516);
#8425=VERTEX_POINT('',#59523);
#8426=VERTEX_POINT('',#59527);
#8427=VERTEX_POINT('',#59531);
#8428=VERTEX_POINT('',#59535);
#8429=VERTEX_POINT('',#59543);
#8430=VERTEX_POINT('',#59550);
#8431=VERTEX_POINT('',#59552);
#8432=VERTEX_POINT('',#59556);
#8433=VERTEX_POINT('',#59567);
#8434=VERTEX_POINT('',#59571);
#8435=VERTEX_POINT('',#59573);
#8436=VERTEX_POINT('',#59577);
#8437=VERTEX_POINT('',#59579);
#8438=VERTEX_POINT('',#59583);
#8439=VERTEX_POINT('',#59584);
#8440=VERTEX_POINT('',#59591);
#8441=VERTEX_POINT('',#59592);
#8442=VERTEX_POINT('',#59599);
#8443=VERTEX_POINT('',#59600);
#8444=VERTEX_POINT('',#59607);
#8445=VERTEX_POINT('',#59608);
#8446=VERTEX_POINT('',#59615);
#8447=VERTEX_POINT('',#59619);
#8448=VERTEX_POINT('',#59623);
#8449=VERTEX_POINT('',#59624);
#8450=VERTEX_POINT('',#59633);
#8451=VERTEX_POINT('',#59634);
#8452=VERTEX_POINT('',#59639);
#8453=VERTEX_POINT('',#59643);
#8454=VERTEX_POINT('',#59644);
#8455=VERTEX_POINT('',#59649);
#8456=VERTEX_POINT('',#59653);
#8457=VERTEX_POINT('',#59654);
#8458=VERTEX_POINT('',#59659);
#8459=VERTEX_POINT('',#59663);
#8460=VERTEX_POINT('',#59664);
#8461=VERTEX_POINT('',#59669);
#8462=VERTEX_POINT('',#59673);
#8463=VERTEX_POINT('',#59674);
#8464=VERTEX_POINT('',#59679);
#8465=VERTEX_POINT('',#59683);
#8466=VERTEX_POINT('',#59700);
#8467=VERTEX_POINT('',#59702);
#8468=VERTEX_POINT('',#59708);
#8469=VERTEX_POINT('',#59714);
#8470=VERTEX_POINT('',#59718);
#8471=VERTEX_POINT('',#59720);
#8472=VERTEX_POINT('',#59726);
#8473=VERTEX_POINT('',#59730);
#8474=VERTEX_POINT('',#59732);
#8475=VERTEX_POINT('',#59734);
#8476=VERTEX_POINT('',#59736);
#8477=VERTEX_POINT('',#59738);
#8478=VERTEX_POINT('',#59740);
#8479=VERTEX_POINT('',#59742);
#8480=VERTEX_POINT('',#59744);
#8481=VERTEX_POINT('',#59746);
#8482=VERTEX_POINT('',#59748);
#8483=VERTEX_POINT('',#59750);
#8484=VERTEX_POINT('',#59752);
#8485=VERTEX_POINT('',#59758);
#8486=VERTEX_POINT('',#59760);
#8487=VERTEX_POINT('',#59762);
#8488=VERTEX_POINT('',#59764);
#8489=VERTEX_POINT('',#59767);
#8490=VERTEX_POINT('',#59768);
#8491=VERTEX_POINT('',#59770);
#8492=VERTEX_POINT('',#59772);
#8493=VERTEX_POINT('',#59775);
#8494=VERTEX_POINT('',#59778);
#8495=VERTEX_POINT('',#59780);
#8496=VERTEX_POINT('',#59785);
#8497=VERTEX_POINT('',#59803);
#8498=VERTEX_POINT('',#59805);
#8499=VERTEX_POINT('',#59817);
#8500=VERTEX_POINT('',#59821);
#8501=VERTEX_POINT('',#59822);
#8502=VERTEX_POINT('',#59829);
#8503=VERTEX_POINT('',#59831);
#8504=VERTEX_POINT('',#59837);
#8505=VERTEX_POINT('',#59838);
#8506=VERTEX_POINT('',#59846);
#8507=VERTEX_POINT('',#59847);
#8508=VERTEX_POINT('',#59860);
#8509=VERTEX_POINT('',#59866);
#8510=VERTEX_POINT('',#59870);
#8511=VERTEX_POINT('',#59874);
#8512=VERTEX_POINT('',#59878);
#8513=VERTEX_POINT('',#59879);
#8514=VERTEX_POINT('',#59890);
#8515=VERTEX_POINT('',#59899);
#8516=VERTEX_POINT('',#59903);
#8517=VERTEX_POINT('',#59904);
#8518=VERTEX_POINT('',#59909);
#8519=VERTEX_POINT('',#59915);
#8520=VERTEX_POINT('',#59919);
#8521=VERTEX_POINT('',#59920);
#8522=VERTEX_POINT('',#59927);
#8523=VERTEX_POINT('',#59931);
#8524=VERTEX_POINT('',#59935);
#8525=VERTEX_POINT('',#59936);
#8526=VERTEX_POINT('',#59943);
#8527=VERTEX_POINT('',#59944);
#8528=VERTEX_POINT('',#59951);
#8529=VERTEX_POINT('',#59952);
#8530=VERTEX_POINT('',#59961);
#8531=VERTEX_POINT('',#59962);
#8532=VERTEX_POINT('',#59970);
#8533=VERTEX_POINT('',#59971);
#8534=VERTEX_POINT('',#59979);
#8535=VERTEX_POINT('',#59980);
#8536=VERTEX_POINT('',#59988);
#8537=VERTEX_POINT('',#59989);
#8538=VERTEX_POINT('',#59997);
#8539=VERTEX_POINT('',#59998);
#8540=VERTEX_POINT('',#60006);
#8541=VERTEX_POINT('',#60015);
#8542=VERTEX_POINT('',#60019);
#8543=VERTEX_POINT('',#60028);
#8544=VERTEX_POINT('',#60034);
#8545=VERTEX_POINT('',#60050);
#8546=VERTEX_POINT('',#60073);
#8547=VERTEX_POINT('',#60085);
#8548=VERTEX_POINT('',#60086);
#8549=VERTEX_POINT('',#60091);
#8550=VERTEX_POINT('',#60092);
#8551=VERTEX_POINT('',#60102);
#8552=VERTEX_POINT('',#60103);
#8553=VERTEX_POINT('',#60105);
#8554=VERTEX_POINT('',#60107);
#8555=VERTEX_POINT('',#60111);
#8556=VERTEX_POINT('',#60113);
#8557=VERTEX_POINT('',#60117);
#8558=VERTEX_POINT('',#60119);
#8559=VERTEX_POINT('',#60126);
#8560=VERTEX_POINT('',#60128);
#8561=VERTEX_POINT('',#60132);
#8562=VERTEX_POINT('',#60136);
#8563=VERTEX_POINT('',#60137);
#8564=VERTEX_POINT('',#60139);
#8565=VERTEX_POINT('',#60141);
#8566=VERTEX_POINT('',#60143);
#8567=VERTEX_POINT('',#60145);
#8568=VERTEX_POINT('',#60149);
#8569=VERTEX_POINT('',#60166);
#8570=VERTEX_POINT('',#60170);
#8571=VERTEX_POINT('',#60171);
#8572=VERTEX_POINT('',#60173);
#8573=VERTEX_POINT('',#60178);
#8574=VERTEX_POINT('',#60179);
#8575=VERTEX_POINT('',#60191);
#8576=VERTEX_POINT('',#60192);
#8577=VERTEX_POINT('',#60194);
#8578=VERTEX_POINT('',#60196);
#8579=VERTEX_POINT('',#60198);
#8580=VERTEX_POINT('',#60200);
#8581=VERTEX_POINT('',#60204);
#8582=VERTEX_POINT('',#60206);
#8583=VERTEX_POINT('',#60210);
#8584=VERTEX_POINT('',#60211);
#8585=VERTEX_POINT('',#60228);
#8586=VERTEX_POINT('',#60230);
#8587=VERTEX_POINT('',#60234);
#8588=VERTEX_POINT('',#60236);
#8589=VERTEX_POINT('',#60238);
#8590=VERTEX_POINT('',#60242);
#8591=VERTEX_POINT('',#60243);
#8592=VERTEX_POINT('',#60245);
#8593=VERTEX_POINT('',#60247);
#8594=VERTEX_POINT('',#60251);
#8595=VERTEX_POINT('',#60253);
#8596=VERTEX_POINT('',#60257);
#8597=VERTEX_POINT('',#60259);
#8598=VERTEX_POINT('',#60266);
#8599=VERTEX_POINT('',#60268);
#8600=VERTEX_POINT('',#60272);
#8601=VERTEX_POINT('',#60276);
#8602=VERTEX_POINT('',#60278);
#8603=VERTEX_POINT('',#60280);
#8604=VERTEX_POINT('',#60282);
#8605=VERTEX_POINT('',#60286);
#8606=VERTEX_POINT('',#60288);
#8607=VERTEX_POINT('',#60292);
#8608=VERTEX_POINT('',#60296);
#8609=VERTEX_POINT('',#60298);
#8610=VERTEX_POINT('',#60300);
#8611=VERTEX_POINT('',#60302);
#8612=VERTEX_POINT('',#60304);
#8613=VERTEX_POINT('',#60306);
#8614=VERTEX_POINT('',#60308);
#8615=VERTEX_POINT('',#60310);
#8616=VERTEX_POINT('',#60312);
#8617=VERTEX_POINT('',#60314);
#8618=VERTEX_POINT('',#60318);
#8619=VERTEX_POINT('',#60322);
#8620=VERTEX_POINT('',#60327);
#8621=VERTEX_POINT('',#60332);
#8622=VERTEX_POINT('',#60337);
#8623=VERTEX_POINT('',#60339);
#8624=VERTEX_POINT('',#60343);
#8625=VERTEX_POINT('',#60347);
#8626=VERTEX_POINT('',#60351);
#8627=VERTEX_POINT('',#60353);
#8628=VERTEX_POINT('',#60357);
#8629=VERTEX_POINT('',#60359);
#8630=VERTEX_POINT('',#60363);
#8631=VERTEX_POINT('',#60364);
#8632=VERTEX_POINT('',#60366);
#8633=VERTEX_POINT('',#60368);
#8634=VERTEX_POINT('',#60372);
#8635=VERTEX_POINT('',#60378);
#8636=VERTEX_POINT('',#60386);
#8637=VERTEX_POINT('',#60388);
#8638=VERTEX_POINT('',#60422);
#8639=VERTEX_POINT('',#60426);
#8640=VERTEX_POINT('',#60430);
#8641=VERTEX_POINT('',#60434);
#8642=VERTEX_POINT('',#60438);
#8643=VERTEX_POINT('',#60446);
#8644=VERTEX_POINT('',#60450);
#8645=VERTEX_POINT('',#60452);
#8646=VERTEX_POINT('',#60456);
#8647=VERTEX_POINT('',#60460);
#8648=VERTEX_POINT('',#60464);
#8649=VERTEX_POINT('',#60466);
#8650=VERTEX_POINT('',#60470);
#8651=VERTEX_POINT('',#60471);
#8652=VERTEX_POINT('',#60473);
#8653=VERTEX_POINT('',#60478);
#8654=VERTEX_POINT('',#60479);
#8655=VERTEX_POINT('',#60491);
#8656=VERTEX_POINT('',#60493);
#8657=VERTEX_POINT('',#60498);
#8658=VERTEX_POINT('',#60499);
#8659=VERTEX_POINT('',#60504);
#8660=VERTEX_POINT('',#60506);
#8661=VERTEX_POINT('',#60537);
#8662=VERTEX_POINT('',#60539);
#8663=VERTEX_POINT('',#60543);
#8664=VERTEX_POINT('',#60545);
#8665=VERTEX_POINT('',#60549);
#8666=VERTEX_POINT('',#60556);
#8667=VERTEX_POINT('',#60560);
#8668=VERTEX_POINT('',#60564);
#8669=VERTEX_POINT('',#60568);
#8670=VERTEX_POINT('',#60574);
#8671=VERTEX_POINT('',#60578);
#8672=VERTEX_POINT('',#60580);
#8673=VERTEX_POINT('',#60613);
#8674=VERTEX_POINT('',#60617);
#8675=VERTEX_POINT('',#60623);
#8676=VERTEX_POINT('',#60625);
#8677=VERTEX_POINT('',#60627);
#8678=VERTEX_POINT('',#60630);
#8679=VERTEX_POINT('',#60632);
#8680=VERTEX_POINT('',#60634);
#8681=VERTEX_POINT('',#60638);
#8682=VERTEX_POINT('',#60641);
#8683=VERTEX_POINT('',#60645);
#8684=VERTEX_POINT('',#60647);
#8685=VERTEX_POINT('',#60653);
#8686=VERTEX_POINT('',#60657);
#8687=VERTEX_POINT('',#60661);
#8688=VERTEX_POINT('',#60665);
#8689=VERTEX_POINT('',#60698);
#8690=VERTEX_POINT('',#60700);
#8691=VERTEX_POINT('',#60702);
#8692=VERTEX_POINT('',#60705);
#8693=VERTEX_POINT('',#60707);
#8694=VERTEX_POINT('',#60709);
#8695=VERTEX_POINT('',#60713);
#8696=VERTEX_POINT('',#60716);
#8697=VERTEX_POINT('',#60720);
#8698=VERTEX_POINT('',#60722);
#8699=VERTEX_POINT('',#60726);
#8700=VERTEX_POINT('',#60728);
#8701=VERTEX_POINT('',#60734);
#8702=VERTEX_POINT('',#60736);
#8703=VERTEX_POINT('',#60740);
#8704=VERTEX_POINT('',#60742);
#8705=VERTEX_POINT('',#60748);
#8706=VERTEX_POINT('',#60750);
#8707=VERTEX_POINT('',#60754);
#8708=VERTEX_POINT('',#60755);
#8709=VERTEX_POINT('',#60760);
#8710=VERTEX_POINT('',#60764);
#8711=VERTEX_POINT('',#60767);
#8712=VERTEX_POINT('',#60769);
#8713=VERTEX_POINT('',#60773);
#8714=VERTEX_POINT('',#60774);
#8715=VERTEX_POINT('',#60779);
#8716=VERTEX_POINT('',#60784);
#8717=VERTEX_POINT('',#60787);
#8718=VERTEX_POINT('',#60789);
#8719=VERTEX_POINT('',#60793);
#8720=VERTEX_POINT('',#60794);
#8721=VERTEX_POINT('',#60801);
#8722=VERTEX_POINT('',#60803);
#8723=VERTEX_POINT('',#60807);
#8724=VERTEX_POINT('',#60808);
#8725=VERTEX_POINT('',#60815);
#8726=VERTEX_POINT('',#60817);
#8727=VERTEX_POINT('',#60819);
#8728=VERTEX_POINT('',#60823);
#8729=VERTEX_POINT('',#60824);
#8730=VERTEX_POINT('',#60829);
#8731=VERTEX_POINT('',#60830);
#8732=VERTEX_POINT('',#60834);
#8733=VERTEX_POINT('',#60837);
#8734=VERTEX_POINT('',#60839);
#8735=VERTEX_POINT('',#60840);
#8736=VERTEX_POINT('',#60842);
#8737=VERTEX_POINT('',#60844);
#8738=VERTEX_POINT('',#60847);
#8739=VERTEX_POINT('',#60848);
#8740=VERTEX_POINT('',#60850);
#8741=VERTEX_POINT('',#60852);
#8742=VERTEX_POINT('',#60856);
#8743=VERTEX_POINT('',#60861);
#8744=VERTEX_POINT('',#60867);
#8745=VERTEX_POINT('',#60871);
#8746=VERTEX_POINT('',#60878);
#8747=VERTEX_POINT('',#60882);
#8748=VERTEX_POINT('',#60884);
#8749=VERTEX_POINT('',#60886);
#8750=VERTEX_POINT('',#60889);
#8751=VERTEX_POINT('',#60890);
#8752=VERTEX_POINT('',#60892);
#8753=VERTEX_POINT('',#60894);
#8754=VERTEX_POINT('',#60896);
#8755=VERTEX_POINT('',#60898);
#8756=VERTEX_POINT('',#60900);
#8757=VERTEX_POINT('',#60902);
#8758=VERTEX_POINT('',#60905);
#8759=VERTEX_POINT('',#60906);
#8760=VERTEX_POINT('',#60908);
#8761=VERTEX_POINT('',#60910);
#8762=VERTEX_POINT('',#60912);
#8763=VERTEX_POINT('',#60914);
#8764=VERTEX_POINT('',#60916);
#8765=VERTEX_POINT('',#60918);
#8766=VERTEX_POINT('',#60921);
#8767=VERTEX_POINT('',#60931);
#8768=VERTEX_POINT('',#60933);
#8769=VERTEX_POINT('',#60937);
#8770=VERTEX_POINT('',#60939);
#8771=VERTEX_POINT('',#60945);
#8772=VERTEX_POINT('',#60947);
#8773=VERTEX_POINT('',#60951);
#8774=VERTEX_POINT('',#60955);
#8775=VERTEX_POINT('',#60961);
#8776=VERTEX_POINT('',#60963);
#8777=VERTEX_POINT('',#60967);
#8778=VERTEX_POINT('',#60976);
#8779=VERTEX_POINT('',#60982);
#8780=VERTEX_POINT('',#60984);
#8781=VERTEX_POINT('',#60988);
#8782=VERTEX_POINT('',#60992);
#8783=VERTEX_POINT('',#60998);
#8784=VERTEX_POINT('',#61000);
#8785=VERTEX_POINT('',#61004);
#8786=VERTEX_POINT('',#61013);
#8787=VERTEX_POINT('',#61019);
#8788=VERTEX_POINT('',#61020);
#8789=VERTEX_POINT('',#61022);
#8790=VERTEX_POINT('',#61024);
#8791=VERTEX_POINT('',#61026);
#8792=VERTEX_POINT('',#61028);
#8793=VERTEX_POINT('',#61032);
#8794=VERTEX_POINT('',#61034);
#8795=VERTEX_POINT('',#61038);
#8796=VERTEX_POINT('',#61040);
#8797=VERTEX_POINT('',#61042);
#8798=VERTEX_POINT('',#61049);
#8799=VERTEX_POINT('',#61051);
#8800=VERTEX_POINT('',#61053);
#8801=VERTEX_POINT('',#61057);
#8802=VERTEX_POINT('',#61058);
#8803=VERTEX_POINT('',#61071);
#8804=VERTEX_POINT('',#61072);
#8805=VERTEX_POINT('',#61074);
#8806=VERTEX_POINT('',#61076);
#8807=VERTEX_POINT('',#61078);
#8808=VERTEX_POINT('',#61080);
#8809=VERTEX_POINT('',#61084);
#8810=VERTEX_POINT('',#61086);
#8811=VERTEX_POINT('',#61090);
#8812=VERTEX_POINT('',#61092);
#8813=VERTEX_POINT('',#61094);
#8814=VERTEX_POINT('',#61101);
#8815=VERTEX_POINT('',#61103);
#8816=VERTEX_POINT('',#61105);
#8817=VERTEX_POINT('',#61109);
#8818=VERTEX_POINT('',#61110);
#8819=VERTEX_POINT('',#61129);
#8820=VERTEX_POINT('',#61130);
#8821=VERTEX_POINT('',#61132);
#8822=VERTEX_POINT('',#61136);
#8823=VERTEX_POINT('',#61137);
#8824=VERTEX_POINT('',#61139);
#8825=VERTEX_POINT('',#61143);
#8826=VERTEX_POINT('',#61144);
#8827=VERTEX_POINT('',#61149);
#8828=VERTEX_POINT('',#61150);
#8829=VERTEX_POINT('',#61158);
#8830=VERTEX_POINT('',#61159);
#8831=VERTEX_POINT('',#61161);
#8832=VERTEX_POINT('',#61165);
#8833=VERTEX_POINT('',#61170);
#8834=VERTEX_POINT('',#61172);
#8835=VERTEX_POINT('',#61176);
#8836=VERTEX_POINT('',#61178);
#8837=VERTEX_POINT('',#61182);
#8838=VERTEX_POINT('',#61183);
#8839=VERTEX_POINT('',#61185);
#8840=VERTEX_POINT('',#61192);
#8841=VERTEX_POINT('',#61193);
#8842=VERTEX_POINT('',#61198);
#8843=VERTEX_POINT('',#61199);
#8844=VERTEX_POINT('',#61201);
#8845=VERTEX_POINT('',#61211);
#8846=VERTEX_POINT('',#61212);
#8847=VERTEX_POINT('',#61214);
#8848=VERTEX_POINT('',#61218);
#8849=VERTEX_POINT('',#61219);
#8850=VERTEX_POINT('',#61221);
#8851=VERTEX_POINT('',#61225);
#8852=VERTEX_POINT('',#61226);
#8853=VERTEX_POINT('',#61231);
#8854=VERTEX_POINT('',#61232);
#8855=VERTEX_POINT('',#61234);
#8856=VERTEX_POINT('',#61241);
#8857=VERTEX_POINT('',#61243);
#8858=VERTEX_POINT('',#61247);
#8859=VERTEX_POINT('',#61248);
#8860=VERTEX_POINT('',#61250);
#8861=VERTEX_POINT('',#61260);
#8862=VERTEX_POINT('',#61261);
#8863=VERTEX_POINT('',#61266);
#8864=VERTEX_POINT('',#61273);
#8865=VERTEX_POINT('',#61320);
#8866=VERTEX_POINT('',#61329);
#8867=VERTEX_POINT('',#61377);
#8868=VERTEX_POINT('',#61392);
#8869=VERTEX_POINT('',#61394);
#8870=VERTEX_POINT('',#61405);
#8871=VERTEX_POINT('',#61407);
#8872=VERTEX_POINT('',#61416);
#8873=VERTEX_POINT('',#61418);
#8874=VERTEX_POINT('',#61422);
#8875=VERTEX_POINT('',#61426);
#8876=VERTEX_POINT('',#61428);
#8877=VERTEX_POINT('',#61432);
#8878=VERTEX_POINT('',#61435);
#8879=VERTEX_POINT('',#61437);
#8880=VERTEX_POINT('',#61440);
#8881=VERTEX_POINT('',#61442);
#8882=VERTEX_POINT('',#61444);
#8883=VERTEX_POINT('',#61448);
#8884=VERTEX_POINT('',#61452);
#8885=VERTEX_POINT('',#61454);
#8886=VERTEX_POINT('',#61458);
#8887=VERTEX_POINT('',#61462);
#8888=VERTEX_POINT('',#61464);
#8889=VERTEX_POINT('',#61468);
#8890=VERTEX_POINT('',#61472);
#8891=VERTEX_POINT('',#61473);
#8892=VERTEX_POINT('',#61475);
#8893=VERTEX_POINT('',#61477);
#8894=VERTEX_POINT('',#61481);
#8895=VERTEX_POINT('',#61499);
#8896=VERTEX_POINT('',#61521);
#8897=VERTEX_POINT('',#61536);
#8898=VERTEX_POINT('',#61557);
#8899=VERTEX_POINT('',#61559);
#8900=VERTEX_POINT('',#61563);
#8901=VERTEX_POINT('',#61567);
#8902=VERTEX_POINT('',#61573);
#8903=VERTEX_POINT('',#61575);
#8904=VERTEX_POINT('',#61579);
#8905=VERTEX_POINT('',#61582);
#8906=VERTEX_POINT('',#61586);
#8907=VERTEX_POINT('',#61588);
#8908=VERTEX_POINT('',#61592);
#8909=VERTEX_POINT('',#61595);
#8910=VERTEX_POINT('',#61599);
#8911=VERTEX_POINT('',#61601);
#8912=VERTEX_POINT('',#61613);
#8913=VERTEX_POINT('',#61616);
#8914=VERTEX_POINT('',#61618);
#8915=VERTEX_POINT('',#61628);
#8916=VERTEX_POINT('',#61629);
#8917=VERTEX_POINT('',#61631);
#8918=VERTEX_POINT('',#61636);
#8919=VERTEX_POINT('',#61637);
#8920=VERTEX_POINT('',#61642);
#8921=VERTEX_POINT('',#61645);
#8922=VERTEX_POINT('',#61649);
#8923=VERTEX_POINT('',#61650);
#8924=VERTEX_POINT('',#61652);
#8925=VERTEX_POINT('',#61654);
#8926=VERTEX_POINT('',#61656);
#8927=VERTEX_POINT('',#61658);
#8928=VERTEX_POINT('',#61660);
#8929=VERTEX_POINT('',#61662);
#8930=VERTEX_POINT('',#61664);
#8931=VERTEX_POINT('',#61666);
#8932=VERTEX_POINT('',#61668);
#8933=VERTEX_POINT('',#61670);
#8934=VERTEX_POINT('',#61672);
#8935=VERTEX_POINT('',#61674);
#8936=VERTEX_POINT('',#61676);
#8937=VERTEX_POINT('',#61678);
#8938=VERTEX_POINT('',#61680);
#8939=VERTEX_POINT('',#61682);
#8940=VERTEX_POINT('',#61684);
#8941=VERTEX_POINT('',#61686);
#8942=VERTEX_POINT('',#61688);
#8943=VERTEX_POINT('',#61690);
#8944=VERTEX_POINT('',#61692);
#8945=VERTEX_POINT('',#61694);
#8946=VERTEX_POINT('',#61696);
#8947=VERTEX_POINT('',#61698);
#8948=VERTEX_POINT('',#61700);
#8949=VERTEX_POINT('',#61702);
#8950=VERTEX_POINT('',#61704);
#8951=VERTEX_POINT('',#61706);
#8952=VERTEX_POINT('',#61708);
#8953=VERTEX_POINT('',#61710);
#8954=VERTEX_POINT('',#61712);
#8955=VERTEX_POINT('',#61714);
#8956=VERTEX_POINT('',#61716);
#8957=VERTEX_POINT('',#61718);
#8958=VERTEX_POINT('',#61720);
#8959=VERTEX_POINT('',#61722);
#8960=VERTEX_POINT('',#61724);
#8961=VERTEX_POINT('',#61726);
#8962=VERTEX_POINT('',#61728);
#8963=VERTEX_POINT('',#61730);
#8964=VERTEX_POINT('',#61732);
#8965=VERTEX_POINT('',#61734);
#8966=VERTEX_POINT('',#61736);
#8967=VERTEX_POINT('',#61738);
#8968=VERTEX_POINT('',#61740);
#8969=VERTEX_POINT('',#61742);
#8970=VERTEX_POINT('',#61744);
#8971=VERTEX_POINT('',#61746);
#8972=VERTEX_POINT('',#61748);
#8973=VERTEX_POINT('',#61750);
#8974=VERTEX_POINT('',#61752);
#8975=VERTEX_POINT('',#61754);
#8976=VERTEX_POINT('',#61756);
#8977=VERTEX_POINT('',#61758);
#8978=VERTEX_POINT('',#61762);
#8979=VERTEX_POINT('',#61764);
#8980=VERTEX_POINT('',#61768);
#8981=VERTEX_POINT('',#61770);
#8982=VERTEX_POINT('',#61776);
#8983=VERTEX_POINT('',#61780);
#8984=VERTEX_POINT('',#61784);
#8985=VERTEX_POINT('',#61786);
#8986=VERTEX_POINT('',#61792);
#8987=VERTEX_POINT('',#61796);
#8988=VERTEX_POINT('',#61800);
#8989=VERTEX_POINT('',#61802);
#8990=VERTEX_POINT('',#61808);
#8991=VERTEX_POINT('',#61812);
#8992=VERTEX_POINT('',#61816);
#8993=VERTEX_POINT('',#61818);
#8994=VERTEX_POINT('',#61824);
#8995=VERTEX_POINT('',#61828);
#8996=VERTEX_POINT('',#61832);
#8997=VERTEX_POINT('',#61834);
#8998=VERTEX_POINT('',#61840);
#8999=VERTEX_POINT('',#61844);
#9000=VERTEX_POINT('',#61848);
#9001=VERTEX_POINT('',#61850);
#9002=VERTEX_POINT('',#61856);
#9003=VERTEX_POINT('',#61860);
#9004=VERTEX_POINT('',#61864);
#9005=VERTEX_POINT('',#61866);
#9006=VERTEX_POINT('',#61872);
#9007=VERTEX_POINT('',#61876);
#9008=VERTEX_POINT('',#61880);
#9009=VERTEX_POINT('',#61882);
#9010=VERTEX_POINT('',#61888);
#9011=VERTEX_POINT('',#61892);
#9012=VERTEX_POINT('',#61896);
#9013=VERTEX_POINT('',#61898);
#9014=VERTEX_POINT('',#61904);
#9015=VERTEX_POINT('',#61908);
#9016=VERTEX_POINT('',#61912);
#9017=VERTEX_POINT('',#61914);
#9018=VERTEX_POINT('',#61920);
#9019=VERTEX_POINT('',#61924);
#9020=VERTEX_POINT('',#61928);
#9021=VERTEX_POINT('',#61930);
#9022=VERTEX_POINT('',#61936);
#9023=VERTEX_POINT('',#61940);
#9024=VERTEX_POINT('',#61944);
#9025=VERTEX_POINT('',#61946);
#9026=VERTEX_POINT('',#61952);
#9027=VERTEX_POINT('',#61956);
#9028=VERTEX_POINT('',#61960);
#9029=VERTEX_POINT('',#61962);
#9030=VERTEX_POINT('',#61968);
#9031=VERTEX_POINT('',#61972);
#9032=VERTEX_POINT('',#61974);
#9033=VERTEX_POINT('',#61978);
#9034=VERTEX_POINT('',#61985);
#9035=VERTEX_POINT('',#61992);
#9036=VERTEX_POINT('',#61993);
#9037=VERTEX_POINT('',#61995);
#9038=VERTEX_POINT('',#62105);
#9039=VERTEX_POINT('',#62175);
#9040=VERTEX_POINT('',#62176);
#9041=VERTEX_POINT('',#62178);
#9042=VERTEX_POINT('',#62391);
#9043=VERTEX_POINT('',#62605);
#9044=VERTEX_POINT('',#62606);
#9045=VERTEX_POINT('',#62608);
#9046=VERTEX_POINT('',#62818);
#9047=VERTEX_POINT('',#63032);
#9048=VERTEX_POINT('',#63033);
#9049=VERTEX_POINT('',#63035);
#9050=VERTEX_POINT('',#63248);
#9051=VERTEX_POINT('',#63488);
#9052=VERTEX_POINT('',#63489);
#9053=VERTEX_POINT('',#63491);
#9054=VERTEX_POINT('',#63952);
#9055=VERTEX_POINT('',#63953);
#9056=VERTEX_POINT('',#63955);
#9057=VERTEX_POINT('',#64037);
#9058=VERTEX_POINT('',#64295);
#9059=VERTEX_POINT('',#64296);
#9060=VERTEX_POINT('',#64298);
#9061=VERTEX_POINT('',#64693);
#9062=VERTEX_POINT('',#64694);
#9063=VERTEX_POINT('',#64696);
#9064=VERTEX_POINT('',#64778);
#9065=VERTEX_POINT('',#65026);
#9066=VERTEX_POINT('',#65027);
#9067=VERTEX_POINT('',#65029);
#9068=VERTEX_POINT('',#65418);
#9069=VERTEX_POINT('',#65419);
#9070=VERTEX_POINT('',#65421);
#9071=VERTEX_POINT('',#65503);
#9072=VERTEX_POINT('',#65801);
#9073=VERTEX_POINT('',#65802);
#9074=VERTEX_POINT('',#65804);
#9075=VERTEX_POINT('',#66200);
#9076=VERTEX_POINT('',#66201);
#9077=VERTEX_POINT('',#66203);
#9078=VERTEX_POINT('',#66416);
#9079=VERTEX_POINT('',#66756);
#9080=VERTEX_POINT('',#66757);
#9081=VERTEX_POINT('',#66759);
#9082=VERTEX_POINT('',#67217);
#9083=VERTEX_POINT('',#67218);
#9084=VERTEX_POINT('',#67220);
#9085=VERTEX_POINT('',#67433);
#9086=VERTEX_POINT('',#67747);
#9087=VERTEX_POINT('',#67748);
#9088=VERTEX_POINT('',#67750);
#9089=VERTEX_POINT('',#68200);
#9090=VERTEX_POINT('',#68201);
#9091=VERTEX_POINT('',#68203);
#9092=VERTEX_POINT('',#68413);
#9093=VERTEX_POINT('',#68739);
#9094=VERTEX_POINT('',#68740);
#9095=VERTEX_POINT('',#68742);
#9096=VERTEX_POINT('',#69201);
#9097=VERTEX_POINT('',#69202);
#9098=VERTEX_POINT('',#69204);
#9099=VERTEX_POINT('',#69420);
#9100=VERTEX_POINT('',#69712);
#9101=VERTEX_POINT('',#69713);
#9102=VERTEX_POINT('',#69715);
#9103=VERTEX_POINT('',#70195);
#9104=VERTEX_POINT('',#70196);
#9105=VERTEX_POINT('',#70198);
#9106=VERTEX_POINT('',#70411);
#9107=VERTEX_POINT('',#70659);
#9108=VERTEX_POINT('',#70660);
#9109=VERTEX_POINT('',#70662);
#9110=VERTEX_POINT('',#71126);
#9111=VERTEX_POINT('',#71127);
#9112=VERTEX_POINT('',#71129);
#9113=VERTEX_POINT('',#71342);
#9114=VERTEX_POINT('',#71590);
#9115=VERTEX_POINT('',#71591);
#9116=VERTEX_POINT('',#71593);
#9117=VERTEX_POINT('',#72042);
#9118=VERTEX_POINT('',#72043);
#9119=VERTEX_POINT('',#72045);
#9120=VERTEX_POINT('',#72255);
#9121=VERTEX_POINT('',#72528);
#9122=VERTEX_POINT('',#72529);
#9123=VERTEX_POINT('',#72531);
#9124=VERTEX_POINT('',#72747);
#9125=VERTEX_POINT('',#72981);
#9126=VERTEX_POINT('',#72982);
#9127=VERTEX_POINT('',#72984);
#9128=VERTEX_POINT('',#73454);
#9129=VERTEX_POINT('',#73455);
#9130=VERTEX_POINT('',#73457);
#9131=VERTEX_POINT('',#73670);
#9132=VERTEX_POINT('',#73922);
#9133=VERTEX_POINT('',#73923);
#9134=VERTEX_POINT('',#73925);
#9135=VERTEX_POINT('',#74394);
#9136=VERTEX_POINT('',#74395);
#9137=VERTEX_POINT('',#74397);
#9138=VERTEX_POINT('',#74610);
#9139=VERTEX_POINT('',#74856);
#9140=VERTEX_POINT('',#74857);
#9141=VERTEX_POINT('',#74859);
#9142=VERTEX_POINT('',#75316);
#9143=VERTEX_POINT('',#75317);
#9144=VERTEX_POINT('',#75319);
#9145=VERTEX_POINT('',#75529);
#9146=VERTEX_POINT('',#75802);
#9147=VERTEX_POINT('',#75803);
#9148=VERTEX_POINT('',#75805);
#9149=VERTEX_POINT('',#76021);
#9150=VERTEX_POINT('',#76259);
#9151=VERTEX_POINT('',#76260);
#9152=VERTEX_POINT('',#76262);
#9153=VERTEX_POINT('',#76730);
#9154=VERTEX_POINT('',#76731);
#9155=VERTEX_POINT('',#76733);
#9156=VERTEX_POINT('',#76946);
#9157=VERTEX_POINT('',#77192);
#9158=VERTEX_POINT('',#77193);
#9159=VERTEX_POINT('',#77195);
#9160=VERTEX_POINT('',#77653);
#9161=VERTEX_POINT('',#77654);
#9162=VERTEX_POINT('',#77656);
#9163=VERTEX_POINT('',#77869);
#9164=VERTEX_POINT('',#78090);
#9165=VERTEX_POINT('',#78091);
#9166=VERTEX_POINT('',#78093);
#9167=VERTEX_POINT('',#78303);
#9168=VERTEX_POINT('',#78386);
#9169=VERTEX_POINT('',#78387);
#9170=VERTEX_POINT('',#78389);
#9171=VERTEX_POINT('',#78599);
#9172=VERTEX_POINT('',#78746);
#9173=VERTEX_POINT('',#78747);
#9174=VERTEX_POINT('',#78749);
#9175=VERTEX_POINT('',#78965);
#9176=VERTEX_POINT('',#79048);
#9177=VERTEX_POINT('',#79049);
#9178=VERTEX_POINT('',#79123);
#9179=VERTEX_POINT('',#79125);
#9180=VERTEX_POINT('',#79131);
#9181=VERTEX_POINT('',#79358);
#9182=VERTEX_POINT('',#79369);
#9183=VERTEX_POINT('',#79593);
#9184=VERTEX_POINT('',#79823);
#9185=VERTEX_POINT('',#79834);
#9186=VERTEX_POINT('',#80061);
#9187=VERTEX_POINT('',#80073);
#9188=VERTEX_POINT('',#80297);
#9189=VERTEX_POINT('',#80308);
#9190=VERTEX_POINT('',#80532);
#9191=VERTEX_POINT('',#80762);
#9192=VERTEX_POINT('',#80773);
#9193=VERTEX_POINT('',#81000);
#9194=VERTEX_POINT('',#81012);
#9195=VERTEX_POINT('',#81239);
#9196=VERTEX_POINT('',#81250);
#9197=VERTEX_POINT('',#81474);
#9198=VERTEX_POINT('',#81704);
#9199=VERTEX_POINT('',#81715);
#9200=VERTEX_POINT('',#81942);
#9201=VERTEX_POINT('',#81954);
#9202=VERTEX_POINT('',#82181);
#9203=VERTEX_POINT('',#82192);
#9204=VERTEX_POINT('',#82416);
#9205=VERTEX_POINT('',#82429);
#9206=VERTEX_POINT('',#82656);
#9207=VERTEX_POINT('',#82667);
#9208=VERTEX_POINT('',#82679);
#9209=VERTEX_POINT('',#82906);
#9210=VERTEX_POINT('',#82917);
#9211=VERTEX_POINT('',#83141);
#9212=VERTEX_POINT('',#83154);
#9213=VERTEX_POINT('',#83381);
#9214=VERTEX_POINT('',#83392);
#9215=VERTEX_POINT('',#83404);
#9216=VERTEX_POINT('',#83631);
#9217=VERTEX_POINT('',#83642);
#9218=VERTEX_POINT('',#83869);
#9219=VERTEX_POINT('',#84051);
#9220=VERTEX_POINT('',#84053);
#9221=VERTEX_POINT('',#84062);
#9222=VERTEX_POINT('',#84286);
#9223=VERTEX_POINT('',#84297);
#9224=VERTEX_POINT('',#84524);
#9225=VERTEX_POINT('',#84536);
#9226=VERTEX_POINT('',#84763);
#9227=VERTEX_POINT('',#84774);
#9228=VERTEX_POINT('',#85004);
#9229=VERTEX_POINT('',#85228);
#9230=VERTEX_POINT('',#85239);
#9231=VERTEX_POINT('',#85466);
#9232=VERTEX_POINT('',#85478);
#9233=VERTEX_POINT('',#85705);
#9234=VERTEX_POINT('',#85716);
#9235=VERTEX_POINT('',#85946);
#9236=VERTEX_POINT('',#86170);
#9237=VERTEX_POINT('',#86181);
#9238=VERTEX_POINT('',#86192);
#9239=VERTEX_POINT('',#86204);
#9240=VERTEX_POINT('',#86431);
#9241=VERTEX_POINT('',#86442);
#9242=VERTEX_POINT('',#86672);
#9243=VERTEX_POINT('',#86683);
#9244=VERTEX_POINT('',#86910);
#9245=VERTEX_POINT('',#86921);
#9246=VERTEX_POINT('',#87148);
#9247=VERTEX_POINT('',#87159);
#9248=VERTEX_POINT('',#87170);
#9249=VERTEX_POINT('',#87400);
#9250=VERTEX_POINT('',#87411);
#9251=VERTEX_POINT('',#87638);
#9252=VERTEX_POINT('',#87649);
#9253=VERTEX_POINT('',#87876);
#9254=VERTEX_POINT('',#87887);
#9255=VERTEX_POINT('',#87898);
#9256=VERTEX_POINT('',#88125);
#9257=VERTEX_POINT('',#88136);
#9258=VERTEX_POINT('',#88374);
#9259=VERTEX_POINT('',#88381);
#9260=VERTEX_POINT('',#88452);
#9261=VERTEX_POINT('',#88454);
#9262=VERTEX_POINT('',#88559);
#9263=VERTEX_POINT('',#88561);
#9264=VERTEX_POINT('',#88566);
#9265=VERTEX_POINT('',#88567);
#9266=VERTEX_POINT('',#89857);
#9267=VERTEX_POINT('',#89859);
#9268=VERTEX_POINT('',#90951);
#9269=VERTEX_POINT('',#90956);
#9270=VERTEX_POINT('',#90960);
#9271=VERTEX_POINT('',#90964);
#9272=VERTEX_POINT('',#90967);
#9273=VERTEX_POINT('',#90971);
#9274=VERTEX_POINT('',#90974);
#9275=VERTEX_POINT('',#90978);
#9276=VERTEX_POINT('',#90984);
#9277=VERTEX_POINT('',#90985);
#9278=VERTEX_POINT('',#90996);
#9279=VERTEX_POINT('',#90998);
#9280=VERTEX_POINT('',#91013);
#9281=VERTEX_POINT('',#91014);
#9282=VERTEX_POINT('',#91027);
#9283=VERTEX_POINT('',#91029);
#9284=VERTEX_POINT('',#91038);
#9285=VERTEX_POINT('',#91049);
#9286=VERTEX_POINT('',#91053);
#9287=VERTEX_POINT('',#91054);
#9288=VERTEX_POINT('',#91056);
#9289=VERTEX_POINT('',#91065);
#9290=VERTEX_POINT('',#91074);
#9291=VERTEX_POINT('',#91105);
#9292=VERTEX_POINT('',#91107);
#9293=VERTEX_POINT('',#91138);
#9294=VERTEX_POINT('',#91140);
#9295=VERTEX_POINT('',#91149);
#9296=VERTEX_POINT('',#91162);
#9297=VERTEX_POINT('',#91163);
#9298=VERTEX_POINT('',#91172);
#9299=VERTEX_POINT('',#91174);
#9300=VERTEX_POINT('',#91187);
#9301=VERTEX_POINT('',#91198);
#9302=VERTEX_POINT('',#91202);
#9303=VERTEX_POINT('',#91203);
#9304=VERTEX_POINT('',#91205);
#9305=VERTEX_POINT('',#91207);
#9306=VERTEX_POINT('',#91211);
#9307=VERTEX_POINT('',#91213);
#9308=VERTEX_POINT('',#91217);
#9309=VERTEX_POINT('',#91219);
#9310=VERTEX_POINT('',#91223);
#9311=VERTEX_POINT('',#91225);
#9312=VERTEX_POINT('',#91227);
#9313=VERTEX_POINT('',#91229);
#9314=VERTEX_POINT('',#91231);
#9315=VERTEX_POINT('',#91233);
#9316=VERTEX_POINT('',#91235);
#9317=VERTEX_POINT('',#91237);
#9318=VERTEX_POINT('',#91239);
#9319=VERTEX_POINT('',#91241);
#9320=VERTEX_POINT('',#91243);
#9321=VERTEX_POINT('',#91245);
#9322=VERTEX_POINT('',#91247);
#9323=VERTEX_POINT('',#91250);
#9324=VERTEX_POINT('',#91254);
#9325=VERTEX_POINT('',#91265);
#9326=VERTEX_POINT('',#91267);
#9327=VERTEX_POINT('',#91271);
#9328=VERTEX_POINT('',#91275);
#9329=VERTEX_POINT('',#91276);
#9330=VERTEX_POINT('',#91278);
#9331=VERTEX_POINT('',#91280);
#9332=VERTEX_POINT('',#91287);
#9333=VERTEX_POINT('',#91289);
#9334=VERTEX_POINT('',#91291);
#9335=VERTEX_POINT('',#91311);
#9336=VERTEX_POINT('',#91313);
#9337=VERTEX_POINT('',#91315);
#9338=VERTEX_POINT('',#91317);
#9339=VERTEX_POINT('',#91319);
#9340=VERTEX_POINT('',#91321);
#9341=VERTEX_POINT('',#91323);
#9342=VERTEX_POINT('',#91325);
#9343=VERTEX_POINT('',#91329);
#9344=VERTEX_POINT('',#91331);
#9345=VERTEX_POINT('',#91335);
#9346=VERTEX_POINT('',#91337);
#9347=VERTEX_POINT('',#91341);
#9348=VERTEX_POINT('',#91343);
#9349=VERTEX_POINT('',#91347);
#9350=VERTEX_POINT('',#91349);
#9351=VERTEX_POINT('',#91351);
#9352=VERTEX_POINT('',#91353);
#9353=VERTEX_POINT('',#91355);
#9354=VERTEX_POINT('',#91357);
#9355=VERTEX_POINT('',#91359);
#9356=VERTEX_POINT('',#91363);
#9357=VERTEX_POINT('',#91364);
#9358=VERTEX_POINT('',#91366);
#9359=VERTEX_POINT('',#91368);
#9360=VERTEX_POINT('',#91370);
#9361=VERTEX_POINT('',#91374);
#9362=VERTEX_POINT('',#91375);
#9363=VERTEX_POINT('',#91377);
#9364=VERTEX_POINT('',#91379);
#9365=VERTEX_POINT('',#91390);
#9366=VERTEX_POINT('',#91394);
#9367=VERTEX_POINT('',#91396);
#9368=VERTEX_POINT('',#91399);
#9369=VERTEX_POINT('',#91403);
#9370=VERTEX_POINT('',#91404);
#9371=VERTEX_POINT('',#91409);
#9372=VERTEX_POINT('',#91411);
#9373=VERTEX_POINT('',#91413);
#9374=VERTEX_POINT('',#91417);
#9375=VERTEX_POINT('',#91428);
#9376=VERTEX_POINT('',#91437);
#9377=VERTEX_POINT('',#91439);
#9378=VERTEX_POINT('',#91441);
#9379=VERTEX_POINT('',#91445);
#9380=VERTEX_POINT('',#91450);
#9381=VERTEX_POINT('',#91452);
#9382=VERTEX_POINT('',#91454);
#9383=VERTEX_POINT('',#91456);
#9384=VERTEX_POINT('',#91458);
#9385=VERTEX_POINT('',#91462);
#9386=VERTEX_POINT('',#91466);
#9387=VERTEX_POINT('',#91468);
#9388=VERTEX_POINT('',#91470);
#9389=VERTEX_POINT('',#91474);
#9390=VERTEX_POINT('',#91476);
#9391=VERTEX_POINT('',#91480);
#9392=VERTEX_POINT('',#91481);
#9393=VERTEX_POINT('',#91497);
#9394=VERTEX_POINT('',#91499);
#9395=VERTEX_POINT('',#91501);
#9396=VERTEX_POINT('',#91505);
#9397=VERTEX_POINT('',#91506);
#9398=VERTEX_POINT('',#91508);
#9399=VERTEX_POINT('',#91537);
#9400=VERTEX_POINT('',#91571);
#9401=VERTEX_POINT('',#91573);
#9402=VERTEX_POINT('',#91576);
#9403=VERTEX_POINT('',#91585);
#9404=VERTEX_POINT('',#91597);
#9405=VERTEX_POINT('',#91606);
#9406=VERTEX_POINT('',#91616);
#9407=VERTEX_POINT('',#91618);
#9408=VERTEX_POINT('',#91622);
#9409=VERTEX_POINT('',#91625);
#9410=VERTEX_POINT('',#91627);
#9411=VERTEX_POINT('',#91631);
#9412=VERTEX_POINT('',#91632);
#9413=VERTEX_POINT('',#91764);
#9414=VERTEX_POINT('',#91790);
#9415=VERTEX_POINT('',#91792);
#9416=VERTEX_POINT('',#91811);
#9417=VERTEX_POINT('',#91815);
#9418=VERTEX_POINT('',#91817);
#9419=VERTEX_POINT('',#91822);
#9420=VERTEX_POINT('',#91833);
#9421=VERTEX_POINT('',#91837);
#9422=VERTEX_POINT('',#91838);
#9423=VERTEX_POINT('',#91840);
#9424=VERTEX_POINT('',#91842);
#9425=VERTEX_POINT('',#91846);
#9426=VERTEX_POINT('',#91849);
#9427=VERTEX_POINT('',#91862);
#9428=VERTEX_POINT('',#91864);
#9429=VERTEX_POINT('',#91866);
#9430=VERTEX_POINT('',#91884);
#9431=VERTEX_POINT('',#91888);
#9432=VERTEX_POINT('',#91894);
#9433=VERTEX_POINT('',#91898);
#9434=VERTEX_POINT('',#91901);
#9435=VERTEX_POINT('',#91903);
#9436=VERTEX_POINT('',#91906);
#9437=VERTEX_POINT('',#91917);
#9438=VERTEX_POINT('',#91919);
#9439=VERTEX_POINT('',#91922);
#9440=VERTEX_POINT('',#91924);
#9441=VERTEX_POINT('',#91928);
#9442=VERTEX_POINT('',#91929);
#9443=VERTEX_POINT('',#91932);
#9444=VERTEX_POINT('',#91934);
#9445=VERTEX_POINT('',#91953);
#9446=VERTEX_POINT('',#91955);
#9447=VERTEX_POINT('',#91979);
#9448=VERTEX_POINT('',#91981);
#9449=VERTEX_POINT('',#91983);
#9450=VERTEX_POINT('',#91986);
#9451=VERTEX_POINT('',#91990);
#9452=VERTEX_POINT('',#91992);
#9453=VERTEX_POINT('',#91996);
#9454=VERTEX_POINT('',#91998);
#9455=VERTEX_POINT('',#92004);
#9456=VERTEX_POINT('',#92006);
#9457=VERTEX_POINT('',#92015);
#9458=VERTEX_POINT('',#92017);
#9459=VERTEX_POINT('',#92019);
#9460=VERTEX_POINT('',#92021);
#9461=VERTEX_POINT('',#92023);
#9462=VERTEX_POINT('',#92025);
#9463=VERTEX_POINT('',#92027);
#9464=VERTEX_POINT('',#92030);
#9465=VERTEX_POINT('',#92033);
#9466=VERTEX_POINT('',#92034);
#9467=VERTEX_POINT('',#92036);
#9468=VERTEX_POINT('',#92038);
#9469=VERTEX_POINT('',#92041);
#9470=VERTEX_POINT('',#92058);
#9471=VERTEX_POINT('',#92060);
#9472=VERTEX_POINT('',#92062);
#9473=VERTEX_POINT('',#92064);
#9474=VERTEX_POINT('',#92068);
#9475=VERTEX_POINT('',#92072);
#9476=VERTEX_POINT('',#92074);
#9477=VERTEX_POINT('',#92076);
#9478=VERTEX_POINT('',#92080);
#9479=VERTEX_POINT('',#92105);
#9480=VERTEX_POINT('',#92107);
#9481=VERTEX_POINT('',#92111);
#9482=VERTEX_POINT('',#92113);
#9483=VERTEX_POINT('',#92121);
#9484=VERTEX_POINT('',#92123);
#9485=VERTEX_POINT('',#92125);
#9486=VERTEX_POINT('',#92144);
#9487=VERTEX_POINT('',#92147);
#9488=VERTEX_POINT('',#92150);
#9489=VERTEX_POINT('',#92152);
#9490=VERTEX_POINT('',#92154);
#9491=VERTEX_POINT('',#92156);
#9492=VERTEX_POINT('',#92158);
#9493=VERTEX_POINT('',#92160);
#9494=VERTEX_POINT('',#92162);
#9495=VERTEX_POINT('',#92164);
#9496=VERTEX_POINT('',#92166);
#9497=VERTEX_POINT('',#92168);
#9498=VERTEX_POINT('',#92170);
#9499=VERTEX_POINT('',#92173);
#9500=VERTEX_POINT('',#92175);
#9501=VERTEX_POINT('',#92178);
#9502=VERTEX_POINT('',#92181);
#9503=VERTEX_POINT('',#92182);
#9504=VERTEX_POINT('',#92184);
#9505=VERTEX_POINT('',#92186);
#9506=VERTEX_POINT('',#92189);
#9507=VERTEX_POINT('',#92190);
#9508=VERTEX_POINT('',#92192);
#9509=VERTEX_POINT('',#92194);
#9510=VERTEX_POINT('',#92196);
#9511=VERTEX_POINT('',#92198);
#9512=VERTEX_POINT('',#92201);
#9513=VERTEX_POINT('',#92203);
#9514=VERTEX_POINT('',#92206);
#9515=VERTEX_POINT('',#92212);
#9516=VERTEX_POINT('',#92213);
#9517=VERTEX_POINT('',#92216);
#9518=VERTEX_POINT('',#92233);
#9519=VERTEX_POINT('',#92238);
#9520=VERTEX_POINT('',#92240);
#9521=VERTEX_POINT('',#92244);
#9522=VERTEX_POINT('',#92248);
#9523=VERTEX_POINT('',#92252);
#9524=VERTEX_POINT('',#92256);
#9525=VERTEX_POINT('',#92261);
#9526=VERTEX_POINT('',#92279);
#9527=VERTEX_POINT('',#92283);
#9528=VERTEX_POINT('',#92285);
#9529=VERTEX_POINT('',#92287);
#9530=VERTEX_POINT('',#92289);
#9531=VERTEX_POINT('',#92291);
#9532=VERTEX_POINT('',#92295);
#9533=VERTEX_POINT('',#92299);
#9534=VERTEX_POINT('',#92301);
#9535=VERTEX_POINT('',#92305);
#9536=VERTEX_POINT('',#92306);
#9537=VERTEX_POINT('',#92311);
#9538=VERTEX_POINT('',#92312);
#9539=VERTEX_POINT('',#92314);
#9540=VERTEX_POINT('',#92316);
#9541=VERTEX_POINT('',#92318);
#9542=VERTEX_POINT('',#92320);
#9543=VERTEX_POINT('',#92322);
#9544=VERTEX_POINT('',#92326);
#9545=VERTEX_POINT('',#92347);
#9546=VERTEX_POINT('',#92348);
#9547=VERTEX_POINT('',#92354);
#9548=VERTEX_POINT('',#92362);
#9549=VERTEX_POINT('',#92368);
#9550=VERTEX_POINT('',#92370);
#9551=VERTEX_POINT('',#92378);
#9552=VERTEX_POINT('',#92382);
#9553=VERTEX_POINT('',#92384);
#9554=VERTEX_POINT('',#92388);
#9555=VERTEX_POINT('',#92392);
#9556=VERTEX_POINT('',#92396);
#9557=VERTEX_POINT('',#92398);
#9558=VERTEX_POINT('',#92402);
#9559=VERTEX_POINT('',#92404);
#9560=VERTEX_POINT('',#92406);
#9561=VERTEX_POINT('',#92408);
#9562=VERTEX_POINT('',#92412);
#9563=VERTEX_POINT('',#92414);
#9564=VERTEX_POINT('',#92418);
#9565=VERTEX_POINT('',#92420);
#9566=VERTEX_POINT('',#92422);
#9567=VERTEX_POINT('',#92424);
#9568=VERTEX_POINT('',#92428);
#9569=VERTEX_POINT('',#92430);
#9570=VERTEX_POINT('',#92434);
#9571=VERTEX_POINT('',#92436);
#9572=VERTEX_POINT('',#92438);
#9573=VERTEX_POINT('',#92440);
#9574=VERTEX_POINT('',#92444);
#9575=VERTEX_POINT('',#92461);
#9576=VERTEX_POINT('',#92463);
#9577=VERTEX_POINT('',#92467);
#9578=VERTEX_POINT('',#92469);
#9579=VERTEX_POINT('',#92471);
#9580=VERTEX_POINT('',#92473);
#9581=VERTEX_POINT('',#92477);
#9582=VERTEX_POINT('',#92479);
#9583=VERTEX_POINT('',#92499);
#9584=VERTEX_POINT('',#92501);
#9585=VERTEX_POINT('',#92505);
#9586=VERTEX_POINT('',#92509);
#9587=VERTEX_POINT('',#92511);
#9588=VERTEX_POINT('',#92515);
#9589=VERTEX_POINT('',#92519);
#9590=VERTEX_POINT('',#92523);
#9591=VERTEX_POINT('',#92527);
#9592=VERTEX_POINT('',#92528);
#9593=VERTEX_POINT('',#92531);
#9594=VERTEX_POINT('',#92549);
#9595=VERTEX_POINT('',#92553);
#9596=VERTEX_POINT('',#92559);
#9597=VERTEX_POINT('',#92573);
#9598=VERTEX_POINT('',#92575);
#9599=VERTEX_POINT('',#92583);
#9600=VERTEX_POINT('',#92585);
#9601=VERTEX_POINT('',#92587);
#9602=VERTEX_POINT('',#92589);
#9603=VERTEX_POINT('',#92591);
#9604=VERTEX_POINT('',#92593);
#9605=VERTEX_POINT('',#92595);
#9606=VERTEX_POINT('',#92597);
#9607=VERTEX_POINT('',#92599);
#9608=VERTEX_POINT('',#92605);
#9609=VERTEX_POINT('',#92606);
#9610=VERTEX_POINT('',#92612);
#9611=VERTEX_POINT('',#92623);
#9612=VERTEX_POINT('',#92625);
#9613=VERTEX_POINT('',#92636);
#9614=VERTEX_POINT('',#92638);
#9615=VERTEX_POINT('',#92640);
#9616=VERTEX_POINT('',#92644);
#9617=VERTEX_POINT('',#92646);
#9618=VERTEX_POINT('',#92653);
#9619=VERTEX_POINT('',#92655);
#9620=VERTEX_POINT('',#92657);
#9621=VERTEX_POINT('',#92659);
#9622=VERTEX_POINT('',#92661);
#9623=VERTEX_POINT('',#92663);
#9624=VERTEX_POINT('',#92713);
#9625=VERTEX_POINT('',#92715);
#9626=VERTEX_POINT('',#92717);
#9627=VERTEX_POINT('',#92719);
#9628=VERTEX_POINT('',#92730);
#9629=VERTEX_POINT('',#92743);
#9630=VERTEX_POINT('',#92745);
#9631=VERTEX_POINT('',#92747);
#9632=VERTEX_POINT('',#92762);
#9633=VERTEX_POINT('',#92767);
#9634=VERTEX_POINT('',#92768);
#9635=VERTEX_POINT('',#92771);
#9636=VERTEX_POINT('',#92775);
#9637=VERTEX_POINT('',#92779);
#9638=VERTEX_POINT('',#92782);
#9639=VERTEX_POINT('',#92786);
#9640=VERTEX_POINT('',#92787);
#9641=VERTEX_POINT('',#92789);
#9642=VERTEX_POINT('',#92791);
#9643=VERTEX_POINT('',#92795);
#9644=VERTEX_POINT('',#92796);
#9645=VERTEX_POINT('',#92798);
#9646=VERTEX_POINT('',#92800);
#9647=VERTEX_POINT('',#92802);
#9648=VERTEX_POINT('',#92804);
#9649=VERTEX_POINT('',#92808);
#9650=VERTEX_POINT('',#92810);
#9651=VERTEX_POINT('',#92814);
#9652=VERTEX_POINT('',#92816);
#9653=VERTEX_POINT('',#92818);
#9654=VERTEX_POINT('',#92820);
#9655=VERTEX_POINT('',#92822);
#9656=VERTEX_POINT('',#92824);
#9657=VERTEX_POINT('',#92828);
#9658=VERTEX_POINT('',#92832);
#9659=VERTEX_POINT('',#92833);
#9660=VERTEX_POINT('',#92835);
#9661=VERTEX_POINT('',#92837);
#9662=VERTEX_POINT('',#92841);
#9663=VERTEX_POINT('',#92843);
#9664=VERTEX_POINT('',#92845);
#9665=VERTEX_POINT('',#92849);
#9666=VERTEX_POINT('',#92850);
#9667=VERTEX_POINT('',#92852);
#9668=VERTEX_POINT('',#92855);
#9669=VERTEX_POINT('',#92872);
#9670=VERTEX_POINT('',#92874);
#9671=VERTEX_POINT('',#92879);
#9672=VERTEX_POINT('',#92882);
#9673=VERTEX_POINT('',#92887);
#9674=VERTEX_POINT('',#92893);
#9675=VERTEX_POINT('',#92895);
#9676=VERTEX_POINT('',#92897);
#9677=VERTEX_POINT('',#92899);
#9678=VERTEX_POINT('',#92903);
#9679=VERTEX_POINT('',#92907);
#9680=VERTEX_POINT('',#92909);
#9681=VERTEX_POINT('',#92911);
#9682=VERTEX_POINT('',#92913);
#9683=VERTEX_POINT('',#92915);
#9684=VERTEX_POINT('',#92932);
#9685=VERTEX_POINT('',#92962);
#9686=VERTEX_POINT('',#92973);
#9687=VERTEX_POINT('',#92987);
#9688=VERTEX_POINT('',#93007);
#9689=VERTEX_POINT('',#93009);
#9690=VERTEX_POINT('',#93011);
#9691=VERTEX_POINT('',#93013);
#9692=VERTEX_POINT('',#93028);
#9693=VERTEX_POINT('',#93030);
#9694=VERTEX_POINT('',#93040);
#9695=VERTEX_POINT('',#93042);
#9696=VERTEX_POINT('',#93048);
#9697=VERTEX_POINT('',#93050);
#9698=VERTEX_POINT('',#93054);
#9699=VERTEX_POINT('',#93056);
#9700=VERTEX_POINT('',#93115);
#9701=VERTEX_POINT('',#93134);
#9702=VERTEX_POINT('',#93144);
#9703=VERTEX_POINT('',#93154);
#9704=VERTEX_POINT('',#93161);
#9705=VERTEX_POINT('',#93192);
#9706=VERTEX_POINT('',#93193);
#9707=VERTEX_POINT('',#93228);
#9708=VERTEX_POINT('',#93239);
#9709=VERTEX_POINT('',#93250);
#9710=VERTEX_POINT('',#93257);
#9711=VERTEX_POINT('',#93268);
#9712=VERTEX_POINT('',#93286);
#9713=VERTEX_POINT('',#93287);
#9714=VERTEX_POINT('',#93322);
#9715=VERTEX_POINT('',#93333);
#9716=VERTEX_POINT('',#93344);
#9717=VERTEX_POINT('',#93351);
#9718=VERTEX_POINT('',#93358);
#9719=VERTEX_POINT('',#97672);
#9720=VERTEX_POINT('',#97674);
#9721=VERTEX_POINT('',#97676);
#9722=VERTEX_POINT('',#97680);
#9723=VERTEX_POINT('',#97682);
#9724=VERTEX_POINT('',#97686);
#9725=VERTEX_POINT('',#97689);
#9726=VERTEX_POINT('',#97693);
#9727=VERTEX_POINT('',#97696);
#9728=VERTEX_POINT('',#97697);
#9729=VERTEX_POINT('',#97699);
#9730=VERTEX_POINT('',#97704);
#9731=VERTEX_POINT('',#97709);
#9732=VERTEX_POINT('',#97711);
#9733=VERTEX_POINT('',#97715);
#9734=VERTEX_POINT('',#97718);
#9735=VERTEX_POINT('',#97719);
#9736=VERTEX_POINT('',#97721);
#9737=VERTEX_POINT('',#97723);
#9738=VERTEX_POINT('',#97727);
#9739=VERTEX_POINT('',#97729);
#9740=VERTEX_POINT('',#97731);
#9741=VERTEX_POINT('',#97735);
#9742=VERTEX_POINT('',#97737);
#9743=VERTEX_POINT('',#97744);
#9744=VERTEX_POINT('',#97745);
#9745=VERTEX_POINT('',#97747);
#9746=VERTEX_POINT('',#97749);
#9747=VERTEX_POINT('',#97753);
#9748=VERTEX_POINT('',#97755);
#9749=VERTEX_POINT('',#97759);
#9750=VERTEX_POINT('',#97761);
#9751=VERTEX_POINT('',#97773);
#9752=VERTEX_POINT('',#97774);
#9753=VERTEX_POINT('',#97776);
#9754=VERTEX_POINT('',#97778);
#9755=VERTEX_POINT('',#97782);
#9756=VERTEX_POINT('',#97784);
#9757=VERTEX_POINT('',#97788);
#9758=VERTEX_POINT('',#97792);
#9759=VERTEX_POINT('',#97803);
#9760=VERTEX_POINT('',#97804);
#9761=VERTEX_POINT('',#97806);
#9762=VERTEX_POINT('',#97808);
#9763=VERTEX_POINT('',#97812);
#9764=VERTEX_POINT('',#97813);
#9765=VERTEX_POINT('',#97815);
#9766=VERTEX_POINT('',#97820);
#9767=VERTEX_POINT('',#97822);
#9768=VERTEX_POINT('',#97824);
#9769=VERTEX_POINT('',#97828);
#9770=VERTEX_POINT('',#97830);
#9771=VERTEX_POINT('',#97843);
#9772=VERTEX_POINT('',#97845);
#9773=VERTEX_POINT('',#97849);
#9774=VERTEX_POINT('',#97853);
#9775=VERTEX_POINT('',#97857);
#9776=VERTEX_POINT('',#97859);
#9777=VERTEX_POINT('',#97888);
#9778=VERTEX_POINT('',#97916);
#9779=VERTEX_POINT('',#97918);
#9780=VERTEX_POINT('',#97922);
#9781=VERTEX_POINT('',#97926);
#9782=VERTEX_POINT('',#97928);
#9783=VERTEX_POINT('',#97930);
#9784=VERTEX_POINT('',#97936);
#9785=VERTEX_POINT('',#98082);
#9786=VERTEX_POINT('',#98252);
#9787=VERTEX_POINT('',#98280);
#9788=VERTEX_POINT('',#98291);
#9789=VERTEX_POINT('',#98296);
#9790=VERTEX_POINT('',#98310);
#9791=VERTEX_POINT('',#98312);
#9792=VERTEX_POINT('',#98314);
#9793=VERTEX_POINT('',#98319);
#9794=VERTEX_POINT('',#98324);
#9795=VERTEX_POINT('',#98486);
#9796=VERTEX_POINT('',#98516);
#9797=VERTEX_POINT('',#98547);
#9798=VERTEX_POINT('',#98549);
#9799=VERTEX_POINT('',#98552);
#9800=VERTEX_POINT('',#98554);
#9801=VERTEX_POINT('',#98706);
#9802=VERTEX_POINT('',#98877);
#9803=VERTEX_POINT('',#98904);
#9804=VERTEX_POINT('',#98909);
#9805=VERTEX_POINT('',#98932);
#9806=VERTEX_POINT('',#98937);
#9807=VERTEX_POINT('',#98951);
#9808=VERTEX_POINT('',#98953);
#9809=VERTEX_POINT('',#98955);
#9810=VERTEX_POINT('',#98969);
#9811=VERTEX_POINT('',#99135);
#9812=VERTEX_POINT('',#99161);
#9813=VERTEX_POINT('',#99187);
#9814=VERTEX_POINT('',#99223);
#9815=VERTEX_POINT('',#99247);
#9816=VERTEX_POINT('',#99249);
#9817=VERTEX_POINT('',#99253);
#9818=VERTEX_POINT('',#99254);
#9819=VERTEX_POINT('',#99260);
#9820=VERTEX_POINT('',#99298);
#9821=VERTEX_POINT('',#99300);
#9822=VERTEX_POINT('',#99362);
#9823=VERTEX_POINT('',#99393);
#9824=VERTEX_POINT('',#99395);
#9825=VERTEX_POINT('',#99397);
#9826=VERTEX_POINT('',#99399);
#9827=VERTEX_POINT('',#99401);
#9828=VERTEX_POINT('',#99403);
#9829=VERTEX_POINT('',#99425);
#9830=VERTEX_POINT('',#99429);
#9831=VERTEX_POINT('',#99442);
#9832=VERTEX_POINT('',#99449);
#9833=VERTEX_POINT('',#99451);
#9834=VERTEX_POINT('',#99453);
#9835=VERTEX_POINT('',#99478);
#9836=VERTEX_POINT('',#99546);
#9837=VERTEX_POINT('',#99639);
#9838=VERTEX_POINT('',#99641);
#9839=VERTEX_POINT('',#99644);
#9840=VERTEX_POINT('',#99646);
#9841=VERTEX_POINT('',#99650);
#9842=VERTEX_POINT('',#99652);
#9843=VERTEX_POINT('',#99658);
#9844=VERTEX_POINT('',#99660);
#9845=VERTEX_POINT('',#99664);
#9846=VERTEX_POINT('',#99666);
#9847=VERTEX_POINT('',#99670);
#9848=VERTEX_POINT('',#99675);
#9849=VERTEX_POINT('',#99678);
#9850=VERTEX_POINT('',#99680);
#9851=VERTEX_POINT('',#99684);
#9852=VERTEX_POINT('',#99686);
#9853=VERTEX_POINT('',#99692);
#9854=VERTEX_POINT('',#99694);
#9855=VERTEX_POINT('',#99698);
#9856=VERTEX_POINT('',#99700);
#9857=VERTEX_POINT('',#99713);
#9858=VERTEX_POINT('',#99715);
#9859=VERTEX_POINT('',#99718);
#9860=VERTEX_POINT('',#99722);
#9861=VERTEX_POINT('',#99724);
#9862=VERTEX_POINT('',#99728);
#9863=VERTEX_POINT('',#99731);
#9864=VERTEX_POINT('',#99736);
#9865=VERTEX_POINT('',#99738);
#9866=VERTEX_POINT('',#99742);
#9867=VERTEX_POINT('',#99745);
#9868=VERTEX_POINT('',#99747);
#9869=VERTEX_POINT('',#99751);
#9870=VERTEX_POINT('',#99754);
#9871=VERTEX_POINT('',#99758);
#9872=VERTEX_POINT('',#99761);
#9873=VERTEX_POINT('',#99763);
#9874=VERTEX_POINT('',#99766);
#9875=VERTEX_POINT('',#99770);
#9876=VERTEX_POINT('',#99773);
#9877=VERTEX_POINT('',#99777);
#9878=VERTEX_POINT('',#99780);
#9879=VERTEX_POINT('',#99784);
#9880=VERTEX_POINT('',#99787);
#9881=VERTEX_POINT('',#99791);
#9882=VERTEX_POINT('',#99795);
#9883=VERTEX_POINT('',#99806);
#9884=VERTEX_POINT('',#99808);
#9885=VERTEX_POINT('',#99812);
#9886=VERTEX_POINT('',#99816);
#9887=VERTEX_POINT('',#99820);
#9888=VERTEX_POINT('',#99823);
#9889=VERTEX_POINT('',#99829);
#9890=VERTEX_POINT('',#99831);
#9891=VERTEX_POINT('',#99835);
#9892=VERTEX_POINT('',#99839);
#9893=VERTEX_POINT('',#99846);
#9894=VERTEX_POINT('',#99848);
#9895=VERTEX_POINT('',#99852);
#9896=VERTEX_POINT('',#99856);
#9897=VERTEX_POINT('',#99863);
#9898=VERTEX_POINT('',#99866);
#9899=VERTEX_POINT('',#99870);
#9900=VERTEX_POINT('',#99874);
#9901=VERTEX_POINT('',#99877);
#9902=VERTEX_POINT('',#99881);
#9903=VERTEX_POINT('',#99885);
#9904=VERTEX_POINT('',#99888);
#9905=VERTEX_POINT('',#99892);
#9906=VERTEX_POINT('',#99895);
#9907=VERTEX_POINT('',#99899);
#9908=VERTEX_POINT('',#99902);
#9909=VERTEX_POINT('',#99906);
#9910=VERTEX_POINT('',#99912);
#9911=VERTEX_POINT('',#99914);
#9912=VERTEX_POINT('',#99918);
#9913=VERTEX_POINT('',#99922);
#9914=VERTEX_POINT('',#99929);
#9915=VERTEX_POINT('',#99932);
#9916=VERTEX_POINT('',#99935);
#9917=VERTEX_POINT('',#99939);
#9918=VERTEX_POINT('',#99942);
#9919=VERTEX_POINT('',#99946);
#9920=VERTEX_POINT('',#99952);
#9921=VERTEX_POINT('',#99955);
#9922=VERTEX_POINT('',#99958);
#9923=VERTEX_POINT('',#99962);
#9924=EDGE_CURVE('',#8043,#8044,#7457,.T.);
#9925=EDGE_CURVE('',#8044,#8045,#7458,.T.);
#9926=EDGE_CURVE('',#8045,#8044,#7459,.T.);
#9927=EDGE_CURVE('',#8043,#8046,#7460,.T.);
#9928=EDGE_CURVE('',#8046,#8047,#7461,.T.);
#9929=EDGE_CURVE('',#8047,#8048,#7462,.T.);
#9930=EDGE_CURVE('',#8048,#8049,#7463,.T.);
#9931=EDGE_CURVE('',#8049,#8050,#7464,.T.);
#9932=EDGE_CURVE('',#8050,#8051,#7465,.T.);
#9933=EDGE_CURVE('',#8051,#8052,#7466,.T.);
#9934=EDGE_CURVE('',#8052,#8053,#7467,.T.);
#9935=EDGE_CURVE('',#8053,#8054,#7468,.T.);
#9936=EDGE_CURVE('',#8054,#8055,#7469,.T.);
#9937=EDGE_CURVE('',#8055,#8043,#7470,.T.);
#9938=EDGE_CURVE('',#8045,#8056,#1980,.T.);
#9939=EDGE_CURVE('',#8057,#8056,#7471,.T.);
#9940=EDGE_CURVE('',#8056,#8057,#7472,.T.);
#9941=EDGE_CURVE('',#8058,#8059,#7473,.T.);
#9942=EDGE_CURVE('',#8059,#8060,#7474,.T.);
#9943=EDGE_CURVE('',#8060,#8061,#7475,.T.);
#9944=EDGE_CURVE('',#8061,#8062,#7476,.T.);
#9945=EDGE_CURVE('',#8062,#8063,#7477,.T.);
#9946=EDGE_CURVE('',#8063,#8064,#7478,.T.);
#9947=EDGE_CURVE('',#8064,#8065,#7479,.T.);
#9948=EDGE_CURVE('',#8065,#8066,#7480,.T.);
#9949=EDGE_CURVE('',#8066,#8067,#7481,.T.);
#9950=EDGE_CURVE('',#8067,#8068,#7482,.T.);
#9951=EDGE_CURVE('',#8068,#8069,#7483,.T.);
#9952=EDGE_CURVE('',#8069,#8070,#7484,.T.);
#9953=EDGE_CURVE('',#8070,#8071,#7485,.T.);
#9954=EDGE_CURVE('',#8071,#8072,#7486,.T.);
#9955=EDGE_CURVE('',#8072,#8073,#7487,.T.);
#9956=EDGE_CURVE('',#8073,#8074,#7488,.T.);
#9957=EDGE_CURVE('',#8074,#8075,#7489,.T.);
#9958=EDGE_CURVE('',#8075,#8076,#7490,.T.);
#9959=EDGE_CURVE('',#8076,#8077,#7491,.T.);
#9960=EDGE_CURVE('',#8077,#8078,#7492,.T.);
#9961=EDGE_CURVE('',#8078,#8079,#7493,.T.);
#9962=EDGE_CURVE('',#8079,#8080,#7494,.T.);
#9963=EDGE_CURVE('',#8080,#8081,#7495,.T.);
#9964=EDGE_CURVE('',#8081,#8082,#7496,.T.);
#9965=EDGE_CURVE('',#8082,#8083,#7497,.T.);
#9966=EDGE_CURVE('',#8083,#8084,#7498,.T.);
#9967=EDGE_CURVE('',#8084,#8085,#7499,.T.);
#9968=EDGE_CURVE('',#8085,#8086,#7500,.T.);
#9969=EDGE_CURVE('',#8086,#8087,#7501,.T.);
#9970=EDGE_CURVE('',#8087,#8088,#7502,.T.);
#9971=EDGE_CURVE('',#8088,#8089,#7503,.T.);
#9972=EDGE_CURVE('',#8089,#8090,#7504,.T.);
#9973=EDGE_CURVE('',#8090,#8091,#7505,.T.);
#9974=EDGE_CURVE('',#8091,#8092,#7506,.T.);
#9975=EDGE_CURVE('',#8092,#8093,#7507,.T.);
#9976=EDGE_CURVE('',#8093,#8094,#7508,.T.);
#9977=EDGE_CURVE('',#8094,#8095,#7509,.T.);
#9978=EDGE_CURVE('',#8095,#8096,#7510,.T.);
#9979=EDGE_CURVE('',#8096,#8097,#7511,.T.);
#9980=EDGE_CURVE('',#8097,#8098,#7512,.T.);
#9981=EDGE_CURVE('',#8098,#8099,#7513,.T.);
#9982=EDGE_CURVE('',#8099,#8100,#7514,.T.);
#9983=EDGE_CURVE('',#8100,#8101,#7515,.T.);
#9984=EDGE_CURVE('',#8101,#8102,#7516,.T.);
#9985=EDGE_CURVE('',#8102,#8103,#7517,.T.);
#9986=EDGE_CURVE('',#8103,#8104,#7518,.T.);
#9987=EDGE_CURVE('',#8104,#8105,#7519,.T.);
#9988=EDGE_CURVE('',#8105,#8106,#7520,.T.);
#9989=EDGE_CURVE('',#8106,#8107,#7521,.T.);
#9990=EDGE_CURVE('',#8107,#8108,#7522,.T.);
#9991=EDGE_CURVE('',#8108,#8109,#7523,.T.);
#9992=EDGE_CURVE('',#8109,#8110,#7524,.T.);
#9993=EDGE_CURVE('',#8110,#8111,#7525,.T.);
#9994=EDGE_CURVE('',#8111,#8112,#7526,.T.);
#9995=EDGE_CURVE('',#8112,#8113,#7527,.T.);
#9996=EDGE_CURVE('',#8113,#8114,#7528,.T.);
#9997=EDGE_CURVE('',#8114,#8115,#7529,.T.);
#9998=EDGE_CURVE('',#8115,#8116,#7530,.T.);
#9999=EDGE_CURVE('',#8116,#8117,#7531,.T.);
#10000=EDGE_CURVE('',#8117,#8118,#7532,.T.);
#10001=EDGE_CURVE('',#8118,#8119,#7533,.T.);
#10002=EDGE_CURVE('',#8119,#8120,#7534,.T.);
#10003=EDGE_CURVE('',#8120,#8121,#7535,.T.);
#10004=EDGE_CURVE('',#8121,#8122,#7536,.T.);
#10005=EDGE_CURVE('',#8122,#8123,#7537,.T.);
#10006=EDGE_CURVE('',#8123,#8124,#7538,.T.);
#10007=EDGE_CURVE('',#8124,#8125,#7539,.T.);
#10008=EDGE_CURVE('',#8125,#8058,#7540,.T.);
#10009=EDGE_CURVE('',#8126,#8127,#7541,.T.);
#10010=EDGE_CURVE('',#8128,#8126,#7542,.T.);
#10011=EDGE_CURVE('',#8129,#8128,#7543,.T.);
#10012=EDGE_CURVE('',#8130,#8129,#7544,.T.);
#10013=EDGE_CURVE('',#8131,#8130,#7545,.T.);
#10014=EDGE_CURVE('',#8132,#8131,#7546,.T.);
#10015=EDGE_CURVE('',#8133,#8132,#7547,.T.);
#10016=EDGE_CURVE('',#8134,#8133,#7548,.T.);
#10017=EDGE_CURVE('',#8135,#8134,#7549,.T.);
#10018=EDGE_CURVE('',#8136,#8135,#7550,.T.);
#10019=EDGE_CURVE('',#8127,#8136,#1811,.T.);
#10020=EDGE_CURVE('',#8137,#8138,#7551,.T.);
#10021=EDGE_CURVE('',#8139,#8137,#7552,.T.);
#10022=EDGE_CURVE('',#8138,#8139,#7553,.T.);
#10023=EDGE_CURVE('',#8140,#8141,#7554,.T.);
#10024=EDGE_CURVE('',#8142,#8141,#7555,.T.);
#10025=EDGE_CURVE('',#8142,#8143,#7556,.T.);
#10026=EDGE_CURVE('',#8143,#8144,#7557,.T.);
#10027=EDGE_CURVE('',#8145,#8144,#7558,.T.);
#10028=EDGE_CURVE('',#8145,#8146,#7559,.T.);
#10029=EDGE_CURVE('',#8147,#8146,#7560,.T.);
#10030=EDGE_CURVE('',#8147,#8148,#7561,.T.);
#10031=EDGE_CURVE('',#8149,#8148,#7562,.T.);
#10032=EDGE_CURVE('',#8149,#8140,#7563,.T.);
#10033=EDGE_CURVE('',#8150,#8151,#7564,.T.);
#10034=EDGE_CURVE('',#8152,#8150,#7565,.T.);
#10035=EDGE_CURVE('',#8151,#8152,#7566,.T.);
#10036=EDGE_CURVE('',#8153,#8057,#7567,.T.);
#10037=EDGE_CURVE('',#8153,#8154,#7568,.T.);
#10038=EDGE_CURVE('',#8154,#8155,#7569,.T.);
#10039=EDGE_CURVE('',#8155,#8156,#7570,.T.);
#10040=EDGE_CURVE('',#8156,#8157,#7571,.T.);
#10041=EDGE_CURVE('',#8157,#8158,#7572,.T.);
#10042=EDGE_CURVE('',#8158,#8159,#7573,.T.);
#10043=EDGE_CURVE('',#8159,#8160,#7574,.T.);
#10044=EDGE_CURVE('',#8160,#8161,#7575,.T.);
#10045=EDGE_CURVE('',#8161,#8162,#7576,.T.);
#10046=EDGE_CURVE('',#8162,#8163,#7577,.T.);
#10047=EDGE_CURVE('',#8163,#8153,#7578,.T.);
#10048=EDGE_CURVE('',#8164,#8165,#7579,.T.);
#10049=EDGE_CURVE('',#8166,#8164,#7580,.T.);
#10050=EDGE_CURVE('',#8167,#8166,#7581,.T.);
#10051=EDGE_CURVE('',#8168,#8167,#7582,.T.);
#10052=EDGE_CURVE('',#8169,#8168,#7583,.T.);
#10053=EDGE_CURVE('',#8170,#8169,#7584,.T.);
#10054=EDGE_CURVE('',#8171,#8170,#7585,.T.);
#10055=EDGE_CURVE('',#8172,#8171,#7586,.T.);
#10056=EDGE_CURVE('',#8173,#8172,#7587,.T.);
#10057=EDGE_CURVE('',#8174,#8173,#7588,.T.);
#10058=EDGE_CURVE('',#8175,#8174,#7589,.T.);
#10059=EDGE_CURVE('',#8176,#8175,#7590,.T.);
#10060=EDGE_CURVE('',#8177,#8176,#7591,.T.);
#10061=EDGE_CURVE('',#8178,#8177,#7592,.T.);
#10062=EDGE_CURVE('',#8179,#8178,#7593,.T.);
#10063=EDGE_CURVE('',#8180,#8179,#7594,.T.);
#10064=EDGE_CURVE('',#8181,#8180,#7595,.T.);
#10065=EDGE_CURVE('',#8182,#8181,#7596,.T.);
#10066=EDGE_CURVE('',#8183,#8182,#7597,.T.);
#10067=EDGE_CURVE('',#8184,#8183,#7598,.T.);
#10068=EDGE_CURVE('',#8185,#8184,#7599,.T.);
#10069=EDGE_CURVE('',#8186,#8185,#7600,.T.);
#10070=EDGE_CURVE('',#8187,#8186,#7601,.T.);
#10071=EDGE_CURVE('',#8188,#8187,#7602,.T.);
#10072=EDGE_CURVE('',#8189,#8188,#7603,.T.);
#10073=EDGE_CURVE('',#8190,#8189,#7604,.T.);
#10074=EDGE_CURVE('',#8191,#8190,#7605,.T.);
#10075=EDGE_CURVE('',#8192,#8191,#7606,.T.);
#10076=EDGE_CURVE('',#8193,#8192,#7607,.T.);
#10077=EDGE_CURVE('',#8194,#8193,#7608,.T.);
#10078=EDGE_CURVE('',#8195,#8194,#7609,.T.);
#10079=EDGE_CURVE('',#8196,#8195,#7610,.T.);
#10080=EDGE_CURVE('',#8197,#8196,#7611,.T.);
#10081=EDGE_CURVE('',#8198,#8197,#7612,.T.);
#10082=EDGE_CURVE('',#8199,#8198,#7613,.T.);
#10083=EDGE_CURVE('',#8200,#8199,#7614,.T.);
#10084=EDGE_CURVE('',#8201,#8200,#7615,.T.);
#10085=EDGE_CURVE('',#8202,#8201,#7616,.T.);
#10086=EDGE_CURVE('',#8203,#8202,#7617,.T.);
#10087=EDGE_CURVE('',#8204,#8203,#7618,.T.);
#10088=EDGE_CURVE('',#8205,#8204,#7619,.T.);
#10089=EDGE_CURVE('',#8206,#8205,#7620,.T.);
#10090=EDGE_CURVE('',#8207,#8206,#7621,.T.);
#10091=EDGE_CURVE('',#8208,#8207,#7622,.T.);
#10092=EDGE_CURVE('',#8209,#8208,#7623,.T.);
#10093=EDGE_CURVE('',#8210,#8209,#7624,.T.);
#10094=EDGE_CURVE('',#8211,#8210,#7625,.T.);
#10095=EDGE_CURVE('',#8212,#8211,#7626,.T.);
#10096=EDGE_CURVE('',#8213,#8212,#7627,.T.);
#10097=EDGE_CURVE('',#8214,#8213,#7628,.T.);
#10098=EDGE_CURVE('',#8215,#8214,#7629,.T.);
#10099=EDGE_CURVE('',#8216,#8215,#7630,.T.);
#10100=EDGE_CURVE('',#8217,#8216,#7631,.T.);
#10101=EDGE_CURVE('',#8218,#8217,#7632,.T.);
#10102=EDGE_CURVE('',#8219,#8218,#7633,.T.);
#10103=EDGE_CURVE('',#8220,#8219,#7634,.T.);
#10104=EDGE_CURVE('',#8221,#8220,#7635,.T.);
#10105=EDGE_CURVE('',#8222,#8221,#7636,.T.);
#10106=EDGE_CURVE('',#8223,#8222,#7637,.T.);
#10107=EDGE_CURVE('',#8224,#8223,#7638,.T.);
#10108=EDGE_CURVE('',#8225,#8224,#7639,.T.);
#10109=EDGE_CURVE('',#8226,#8225,#7640,.T.);
#10110=EDGE_CURVE('',#8227,#8226,#7641,.T.);
#10111=EDGE_CURVE('',#8228,#8227,#7642,.T.);
#10112=EDGE_CURVE('',#8229,#8228,#7643,.T.);
#10113=EDGE_CURVE('',#8230,#8229,#7644,.T.);
#10114=EDGE_CURVE('',#8231,#8230,#7645,.T.);
#10115=EDGE_CURVE('',#8165,#8231,#7646,.T.);
#10116=EDGE_CURVE('',#8232,#8233,#1812,.T.);
#10117=EDGE_CURVE('',#8234,#8232,#7647,.T.);
#10118=EDGE_CURVE('',#8235,#8234,#7648,.T.);
#10119=EDGE_CURVE('',#8236,#8235,#7649,.T.);
#10120=EDGE_CURVE('',#8237,#8236,#7650,.T.);
#10121=EDGE_CURVE('',#8238,#8237,#7651,.T.);
#10122=EDGE_CURVE('',#8239,#8238,#7652,.T.);
#10123=EDGE_CURVE('',#8240,#8239,#7653,.T.);
#10124=EDGE_CURVE('',#8241,#8240,#7654,.T.);
#10125=EDGE_CURVE('',#8242,#8241,#7655,.T.);
#10126=EDGE_CURVE('',#8233,#8242,#7656,.T.);
#10127=EDGE_CURVE('',#8243,#8244,#7657,.T.);
#10128=EDGE_CURVE('',#8245,#8243,#7658,.T.);
#10129=EDGE_CURVE('',#8244,#8245,#7659,.T.);
#10130=EDGE_CURVE('',#8246,#8247,#7660,.T.);
#10131=EDGE_CURVE('',#8248,#8246,#7661,.T.);
#10132=EDGE_CURVE('',#8247,#8248,#7662,.T.);
#10133=EDGE_CURVE('',#8127,#8249,#7663,.T.);
#10134=EDGE_CURVE('',#8249,#8250,#7664,.T.);
#10135=EDGE_CURVE('',#8250,#8249,#7665,.T.);
#10136=EDGE_CURVE('',#8250,#8251,#1981,.T.);
#10137=EDGE_CURVE('',#8252,#8251,#7666,.T.);
#10138=EDGE_CURVE('',#8251,#8252,#7667,.T.);
#10139=EDGE_CURVE('',#8233,#8252,#7668,.T.);
#10140=EDGE_CURVE('',#8151,#8253,#7669,.T.);
#10141=EDGE_CURVE('',#8253,#8254,#7670,.T.);
#10142=EDGE_CURVE('',#8254,#8253,#7671,.T.);
#10143=EDGE_CURVE('',#8254,#8255,#1982,.T.);
#10144=EDGE_CURVE('',#8256,#8255,#7672,.T.);
#10145=EDGE_CURVE('',#8255,#8256,#7673,.T.);
#10146=EDGE_CURVE('',#8247,#8256,#7674,.T.);
#10147=EDGE_CURVE('',#8138,#8257,#7675,.T.);
#10148=EDGE_CURVE('',#8257,#8258,#7676,.T.);
#10149=EDGE_CURVE('',#8258,#8257,#7677,.T.);
#10150=EDGE_CURVE('',#8258,#8259,#1983,.T.);
#10151=EDGE_CURVE('',#8260,#8259,#7678,.T.);
#10152=EDGE_CURVE('',#8259,#8260,#7679,.T.);
#10153=EDGE_CURVE('',#8244,#8260,#7680,.T.);
#10154=EDGE_CURVE('',#8149,#8261,#7681,.T.);
#10155=EDGE_CURVE('',#8148,#8262,#7682,.F.);
#10156=EDGE_CURVE('',#8262,#8261,#1984,.T.);
#10157=EDGE_CURVE('',#8146,#8263,#7683,.F.);
#10158=EDGE_CURVE('',#8263,#8262,#1985,.T.);
#10159=EDGE_CURVE('',#8144,#8264,#7684,.F.);
#10160=EDGE_CURVE('',#8264,#8263,#1986,.T.);
#10161=EDGE_CURVE('',#8261,#8264,#1987,.T.);
#10162=EDGE_CURVE('',#8083,#8208,#1988,.T.);
#10163=EDGE_CURVE('',#8082,#8209,#1989,.T.);
#10164=EDGE_CURVE('',#8081,#8210,#1990,.T.);
#10165=EDGE_CURVE('',#8080,#8265,#1991,.T.);
#10166=EDGE_CURVE('',#8265,#8211,#1992,.T.);
#10167=EDGE_CURVE('',#8079,#8266,#1993,.T.);
#10168=EDGE_CURVE('',#8266,#8212,#1994,.T.);
#10169=EDGE_CURVE('',#8078,#8213,#1995,.T.);
#10170=EDGE_CURVE('',#8077,#8214,#1996,.T.);
#10171=EDGE_CURVE('',#8076,#8215,#1997,.T.);
#10172=EDGE_CURVE('',#8075,#8216,#1998,.T.);
#10173=EDGE_CURVE('',#8074,#8267,#1999,.T.);
#10174=EDGE_CURVE('',#8267,#8217,#2000,.T.);
#10175=EDGE_CURVE('',#8073,#8268,#2001,.T.);
#10176=EDGE_CURVE('',#8268,#8218,#2002,.T.);
#10177=EDGE_CURVE('',#8072,#8269,#2003,.T.);
#10178=EDGE_CURVE('',#8269,#8219,#2004,.T.);
#10179=EDGE_CURVE('',#8071,#8220,#2005,.T.);
#10180=EDGE_CURVE('',#8070,#8221,#2006,.T.);
#10181=EDGE_CURVE('',#8091,#8270,#2007,.T.);
#10182=EDGE_CURVE('',#8090,#8201,#2008,.T.);
#10183=EDGE_CURVE('',#8270,#8200,#2009,.T.);
#10184=EDGE_CURVE('',#8089,#8202,#2010,.T.);
#10185=EDGE_CURVE('',#8088,#8203,#2011,.T.);
#10186=EDGE_CURVE('',#8087,#8204,#2012,.T.);
#10187=EDGE_CURVE('',#8086,#8205,#2013,.T.);
#10188=EDGE_CURVE('',#8085,#8206,#2014,.T.);
#10189=EDGE_CURVE('',#8098,#8193,#2015,.T.);
#10190=EDGE_CURVE('',#8097,#8194,#2016,.T.);
#10191=EDGE_CURVE('',#8096,#8195,#2017,.T.);
#10192=EDGE_CURVE('',#8095,#8196,#2018,.T.);
#10193=EDGE_CURVE('',#8094,#8197,#2019,.T.);
#10194=EDGE_CURVE('',#8093,#8271,#2020,.T.);
#10195=EDGE_CURVE('',#8271,#8198,#2021,.T.);
#10196=EDGE_CURVE('',#8092,#8199,#2022,.T.);
#10197=EDGE_CURVE('',#8113,#8178,#2023,.T.);
#10198=EDGE_CURVE('',#8112,#8272,#2024,.T.);
#10199=EDGE_CURVE('',#8272,#8179,#2025,.T.);
#10200=EDGE_CURVE('',#8111,#8273,#2026,.T.);
#10201=EDGE_CURVE('',#8273,#8180,#2027,.T.);
#10202=EDGE_CURVE('',#8110,#8274,#2028,.T.);
#10203=EDGE_CURVE('',#8274,#8181,#2029,.T.);
#10204=EDGE_CURVE('',#8109,#8182,#2030,.T.);
#10205=EDGE_CURVE('',#8108,#8183,#2031,.T.);
#10206=EDGE_CURVE('',#8107,#8184,#2032,.T.);
#10207=EDGE_CURVE('',#8106,#8185,#2033,.T.);
#10208=EDGE_CURVE('',#8105,#8275,#2034,.T.);
#10209=EDGE_CURVE('',#8275,#8186,#2035,.T.);
#10210=EDGE_CURVE('',#8104,#8276,#2036,.T.);
#10211=EDGE_CURVE('',#8276,#8187,#2037,.T.);
#10212=EDGE_CURVE('',#8103,#8188,#2038,.T.);
#10213=EDGE_CURVE('',#8102,#8189,#2039,.T.);
#10214=EDGE_CURVE('',#8101,#8190,#2040,.T.);
#10215=EDGE_CURVE('',#8100,#8191,#2041,.T.);
#10216=EDGE_CURVE('',#8125,#8277,#2042,.T.);
#10217=EDGE_CURVE('',#8124,#8167,#2043,.T.);
#10218=EDGE_CURVE('',#8277,#8166,#2044,.T.);
#10219=EDGE_CURVE('',#8123,#8168,#2045,.T.);
#10220=EDGE_CURVE('',#8122,#8169,#2046,.T.);
#10221=EDGE_CURVE('',#8121,#8170,#2047,.T.);
#10222=EDGE_CURVE('',#8120,#8171,#2048,.T.);
#10223=EDGE_CURVE('',#8119,#8172,#2049,.T.);
#10224=EDGE_CURVE('',#8118,#8173,#2050,.T.);
#10225=EDGE_CURVE('',#8117,#8174,#2051,.T.);
#10226=EDGE_CURVE('',#8116,#8175,#2052,.T.);
#10227=EDGE_CURVE('',#8115,#8176,#2053,.T.);
#10228=EDGE_CURVE('',#8114,#8177,#2054,.T.);
#10229=EDGE_CURVE('',#8069,#8222,#2055,.T.);
#10230=EDGE_CURVE('',#8068,#8223,#2056,.T.);
#10231=EDGE_CURVE('',#8067,#8224,#2057,.T.);
#10232=EDGE_CURVE('',#8066,#8225,#2058,.T.);
#10233=EDGE_CURVE('',#8065,#8226,#2059,.T.);
#10234=EDGE_CURVE('',#8064,#8227,#2060,.T.);
#10235=EDGE_CURVE('',#8063,#8228,#2061,.T.);
#10236=EDGE_CURVE('',#8062,#8229,#2062,.T.);
#10237=EDGE_CURVE('',#8061,#8230,#2063,.T.);
#10238=EDGE_CURVE('',#8060,#8231,#2064,.T.);
#10239=EDGE_CURVE('',#8059,#8278,#2065,.T.);
#10240=EDGE_CURVE('',#8278,#8165,#2066,.T.);
#10241=EDGE_CURVE('',#8058,#8164,#2067,.T.);
#10242=EDGE_CURVE('',#8099,#8192,#2068,.T.);
#10243=EDGE_CURVE('',#8084,#8207,#2069,.T.);
#10244=EDGE_CURVE('',#8279,#8280,#250,.T.);
#10245=EDGE_CURVE('',#8280,#8281,#251,.T.);
#10246=EDGE_CURVE('',#8281,#8282,#252,.T.);
#10247=EDGE_CURVE('',#8282,#8281,#253,.T.);
#10248=EDGE_CURVE('',#8280,#8279,#254,.T.);
#10249=EDGE_CURVE('',#8283,#8284,#255,.T.);
#10250=EDGE_CURVE('',#8284,#8283,#256,.T.);
#10251=EDGE_CURVE('',#8284,#8282,#2070,.T.);
#10252=EDGE_CURVE('',#8279,#8285,#2071,.T.);
#10253=EDGE_CURVE('',#8286,#8285,#257,.T.);
#10254=EDGE_CURVE('',#8285,#8286,#258,.T.);
#10255=EDGE_CURVE('',#8287,#8288,#259,.T.);
#10256=EDGE_CURVE('',#8288,#8289,#2072,.T.);
#10257=EDGE_CURVE('',#8289,#8290,#260,.T.);
#10258=EDGE_CURVE('',#8290,#8287,#2073,.T.);
#10259=EDGE_CURVE('',#8289,#8291,#261,.T.);
#10260=EDGE_CURVE('',#8291,#8290,#262,.T.);
#10261=EDGE_CURVE('',#8287,#8292,#263,.T.);
#10262=EDGE_CURVE('',#8292,#8288,#264,.T.);
#10263=EDGE_CURVE('',#8291,#8293,#2074,.T.);
#10264=EDGE_CURVE('',#8294,#8293,#265,.T.);
#10265=EDGE_CURVE('',#8294,#8290,#2075,.T.);
#10266=EDGE_CURVE('',#8289,#8295,#266,.T.);
#10267=EDGE_CURVE('',#8295,#8296,#267,.F.);
#10268=EDGE_CURVE('',#8296,#8291,#268,.T.);
#10269=EDGE_CURVE('',#8297,#8288,#269,.T.);
#10270=EDGE_CURVE('',#8295,#8297,#2076,.T.);
#10271=EDGE_CURVE('',#8294,#8298,#270,.T.);
#10272=EDGE_CURVE('',#8298,#8299,#2077,.T.);
#10273=EDGE_CURVE('',#8299,#8300,#271,.T.);
#10274=EDGE_CURVE('',#8300,#8294,#2078,.T.);
#10275=EDGE_CURVE('',#8299,#8301,#272,.T.);
#10276=EDGE_CURVE('',#8301,#8300,#273,.T.);
#10277=EDGE_CURVE('',#8293,#8298,#274,.T.);
#10278=EDGE_CURVE('',#8293,#8302,#275,.T.);
#10279=EDGE_CURVE('',#8303,#8302,#276,.T.);
#10280=EDGE_CURVE('',#8303,#8298,#277,.T.);
#10281=EDGE_CURVE('',#8287,#8300,#2079,.T.);
#10282=EDGE_CURVE('',#8304,#8305,#278,.T.);
#10283=EDGE_CURVE('',#8305,#8303,#2080,.T.);
#10284=EDGE_CURVE('',#8303,#8306,#279,.T.);
#10285=EDGE_CURVE('',#8306,#8304,#2081,.T.);
#10286=EDGE_CURVE('',#8302,#8306,#280,.T.);
#10287=EDGE_CURVE('',#8304,#8307,#281,.T.);
#10288=EDGE_CURVE('',#8307,#8305,#282,.T.);
#10289=EDGE_CURVE('',#8302,#8308,#2082,.T.);
#10290=EDGE_CURVE('',#8309,#8308,#283,.T.);
#10291=EDGE_CURVE('',#8309,#8306,#2083,.T.);
#10292=EDGE_CURVE('',#8299,#8305,#284,.T.);
#10293=EDGE_CURVE('',#8309,#8310,#285,.T.);
#10294=EDGE_CURVE('',#8310,#8311,#2084,.T.);
#10295=EDGE_CURVE('',#8311,#8312,#286,.T.);
#10296=EDGE_CURVE('',#8312,#8309,#2085,.T.);
#10297=EDGE_CURVE('',#8311,#8313,#287,.T.);
#10298=EDGE_CURVE('',#8313,#8312,#288,.T.);
#10299=EDGE_CURVE('',#8308,#8310,#289,.T.);
#10300=EDGE_CURVE('',#8308,#8314,#290,.T.);
#10301=EDGE_CURVE('',#8314,#8315,#291,.T.);
#10302=EDGE_CURVE('',#8315,#8310,#292,.T.);
#10303=EDGE_CURVE('',#8304,#8312,#2086,.T.);
#10304=EDGE_CURVE('',#8316,#8317,#293,.T.);
#10305=EDGE_CURVE('',#8317,#8318,#2087,.T.);
#10306=EDGE_CURVE('',#8318,#8319,#294,.T.);
#10307=EDGE_CURVE('',#8319,#8316,#2088,.T.);
#10308=EDGE_CURVE('',#8318,#8320,#295,.T.);
#10309=EDGE_CURVE('',#8320,#8319,#296,.T.);
#10310=EDGE_CURVE('',#8316,#8321,#297,.T.);
#10311=EDGE_CURVE('',#8321,#8317,#298,.T.);
#10312=EDGE_CURVE('',#8321,#8322,#299,.T.);
#10313=EDGE_CURVE('',#8323,#8322,#300,.T.);
#10314=EDGE_CURVE('',#8323,#8317,#301,.T.);
#10315=EDGE_CURVE('',#8316,#8324,#2089,.T.);
#10316=EDGE_CURVE('',#8325,#8324,#302,.T.);
#10317=EDGE_CURVE('',#8325,#8321,#2090,.T.);
#10318=EDGE_CURVE('',#8326,#8319,#2091,.T.);
#10319=EDGE_CURVE('',#8324,#8326,#2092,.T.);
#10320=EDGE_CURVE('',#8327,#8328,#303,.T.);
#10321=EDGE_CURVE('',#8328,#8323,#2093,.T.);
#10322=EDGE_CURVE('',#8323,#8329,#304,.T.);
#10323=EDGE_CURVE('',#8329,#8327,#2094,.T.);
#10324=EDGE_CURVE('',#8322,#8329,#305,.T.);
#10325=EDGE_CURVE('',#8327,#8330,#306,.T.);
#10326=EDGE_CURVE('',#8330,#8328,#307,.T.);
#10327=EDGE_CURVE('',#8322,#8331,#2095,.T.);
#10328=EDGE_CURVE('',#8332,#8331,#308,.T.);
#10329=EDGE_CURVE('',#8332,#8329,#2096,.T.);
#10330=EDGE_CURVE('',#8318,#8328,#309,.T.);
#10331=EDGE_CURVE('',#8333,#8333,#310,.T.);
#10332=EDGE_CURVE('',#8333,#8334,#311,.T.);
#10333=EDGE_CURVE('',#8334,#8335,#312,.T.);
#10334=EDGE_CURVE('',#8335,#8334,#313,.T.);
#10335=EDGE_CURVE('',#8336,#8337,#2097,.T.);
#10336=EDGE_CURVE('',#8338,#8336,#2098,.T.);
#10337=EDGE_CURVE('',#8339,#8338,#2099,.T.);
#10338=EDGE_CURVE('',#8340,#8339,#2100,.T.);
#10339=EDGE_CURVE('',#8341,#8340,#2101,.T.);
#10340=EDGE_CURVE('',#8342,#8341,#2102,.T.);
#10341=EDGE_CURVE('',#8343,#8342,#2103,.T.);
#10342=EDGE_CURVE('',#8344,#8343,#2104,.T.);
#10343=EDGE_CURVE('',#8345,#8344,#2105,.T.);
#10344=EDGE_CURVE('',#8346,#8345,#2106,.T.);
#10345=EDGE_CURVE('',#8347,#8346,#2107,.T.);
#10346=EDGE_CURVE('',#8348,#8347,#2108,.T.);
#10347=EDGE_CURVE('',#8349,#8348,#2109,.T.);
#10348=EDGE_CURVE('',#8350,#8349,#2110,.T.);
#10349=EDGE_CURVE('',#8351,#8350,#2111,.T.);
#10350=EDGE_CURVE('',#8352,#8351,#2112,.T.);
#10351=EDGE_CURVE('',#8353,#8352,#2113,.T.);
#10352=EDGE_CURVE('',#8354,#8353,#2114,.T.);
#10353=EDGE_CURVE('',#8355,#8354,#2115,.T.);
#10354=EDGE_CURVE('',#8356,#8355,#2116,.T.);
#10355=EDGE_CURVE('',#8357,#8356,#2117,.T.);
#10356=EDGE_CURVE('',#8358,#8357,#2118,.T.);
#10357=EDGE_CURVE('',#8359,#8358,#314,.T.);
#10358=EDGE_CURVE('',#8337,#8359,#2119,.T.);
#10359=EDGE_CURVE('',#8360,#8360,#315,.T.);
#10360=EDGE_CURVE('',#8361,#8362,#2120,.T.);
#10361=EDGE_CURVE('',#8363,#8361,#316,.T.);
#10362=EDGE_CURVE('',#8364,#8363,#2121,.T.);
#10363=EDGE_CURVE('',#8362,#8364,#317,.T.);
#10364=EDGE_CURVE('',#8365,#8330,#2122,.T.);
#10365=EDGE_CURVE('',#8366,#8365,#318,.T.);
#10366=EDGE_CURVE('',#8367,#8366,#2123,.T.);
#10367=EDGE_CURVE('',#8368,#8367,#319,.T.);
#10368=EDGE_CURVE('',#8369,#8368,#2124,.T.);
#10369=EDGE_CURVE('',#8370,#8369,#320,.T.);
#10370=EDGE_CURVE('',#8320,#8370,#2125,.T.);
#10371=EDGE_CURVE('',#8330,#8320,#321,.T.);
#10372=EDGE_CURVE('',#8371,#8371,#322,.T.);
#10373=EDGE_CURVE('',#8372,#8373,#323,.T.);
#10374=EDGE_CURVE('',#8374,#8372,#2126,.T.);
#10375=EDGE_CURVE('',#8292,#8374,#324,.T.);
#10376=EDGE_CURVE('',#8301,#8292,#2127,.T.);
#10377=EDGE_CURVE('',#8307,#8301,#325,.T.);
#10378=EDGE_CURVE('',#8313,#8307,#2128,.T.);
#10379=EDGE_CURVE('',#8375,#8313,#326,.T.);
#10380=EDGE_CURVE('',#8373,#8375,#2129,.T.);
#10381=EDGE_CURVE('',#8376,#8376,#327,.T.);
#10382=EDGE_CURVE('',#8335,#8377,#2130,.T.);
#10383=EDGE_CURVE('',#8378,#8377,#328,.T.);
#10384=EDGE_CURVE('',#8377,#8378,#329,.T.);
#10385=EDGE_CURVE('',#8360,#8379,#330,.T.);
#10386=EDGE_CURVE('',#8379,#8380,#331,.T.);
#10387=EDGE_CURVE('',#8380,#8379,#332,.T.);
#10388=EDGE_CURVE('',#8380,#8381,#2131,.T.);
#10389=EDGE_CURVE('',#8382,#8381,#333,.T.);
#10390=EDGE_CURVE('',#8381,#8382,#334,.T.);
#10391=EDGE_CURVE('',#8376,#8283,#335,.T.);
#10392=EDGE_CURVE('',#8362,#8383,#336,.T.);
#10393=EDGE_CURVE('',#8383,#8384,#2132,.T.);
#10394=EDGE_CURVE('',#8384,#8361,#337,.T.);
#10395=EDGE_CURVE('',#8385,#8363,#338,.T.);
#10396=EDGE_CURVE('',#8384,#8385,#339,.T.);
#10397=EDGE_CURVE('',#8386,#8364,#340,.T.);
#10398=EDGE_CURVE('',#8385,#8386,#2133,.T.);
#10399=EDGE_CURVE('',#8386,#8383,#341,.T.);
#10400=EDGE_CURVE('',#8384,#8387,#2134,.T.);
#10401=EDGE_CURVE('',#8388,#8387,#342,.T.);
#10402=EDGE_CURVE('',#8385,#8388,#2135,.T.);
#10403=EDGE_CURVE('',#8383,#8389,#2136,.T.);
#10404=EDGE_CURVE('',#8387,#8389,#2137,.T.);
#10405=EDGE_CURVE('',#8327,#8390,#2138,.T.);
#10406=EDGE_CURVE('',#8390,#8365,#343,.T.);
#10407=EDGE_CURVE('',#8326,#8370,#344,.T.);
#10408=EDGE_CURVE('',#8370,#8391,#345,.T.);
#10409=EDGE_CURVE('',#8391,#8326,#346,.T.);
#10410=EDGE_CURVE('',#8390,#8392,#347,.T.);
#10411=EDGE_CURVE('',#8392,#8365,#348,.T.);
#10412=EDGE_CURVE('',#8390,#8332,#2139,.T.);
#10413=EDGE_CURVE('',#8391,#8393,#2140,.T.);
#10414=EDGE_CURVE('',#8393,#8324,#349,.T.);
#10415=EDGE_CURVE('',#8369,#8394,#350,.F.);
#10416=EDGE_CURVE('',#8394,#8391,#351,.T.);
#10417=EDGE_CURVE('',#8395,#8336,#1813,.F.);
#10418=EDGE_CURVE('',#8337,#8396,#352,.T.);
#10419=EDGE_CURVE('',#8396,#8395,#2141,.T.);
#10420=EDGE_CURVE('',#8337,#8397,#353,.T.);
#10421=EDGE_CURVE('',#8397,#8396,#354,.T.);
#10422=EDGE_CURVE('',#8359,#8398,#355,.T.);
#10423=EDGE_CURVE('',#8398,#8397,#2142,.T.);
#10424=EDGE_CURVE('',#8399,#8400,#356,.F.);
#10425=EDGE_CURVE('',#8348,#8399,#357,.F.);
#10426=EDGE_CURVE('',#8400,#8348,#358,.F.);
#10427=EDGE_CURVE('',#8349,#8401,#359,.T.);
#10428=EDGE_CURVE('',#8401,#8402,#360,.T.);
#10429=EDGE_CURVE('',#8402,#8349,#361,.T.);
#10430=EDGE_CURVE('',#8399,#8401,#2143,.T.);
#10431=EDGE_CURVE('',#8403,#8404,#362,.F.);
#10432=EDGE_CURVE('',#8347,#8403,#363,.F.);
#10433=EDGE_CURVE('',#8404,#8347,#364,.F.);
#10434=EDGE_CURVE('',#8403,#8400,#2144,.T.);
#10435=EDGE_CURVE('',#8405,#8406,#365,.F.);
#10436=EDGE_CURVE('',#8346,#8405,#366,.F.);
#10437=EDGE_CURVE('',#8406,#8346,#367,.F.);
#10438=EDGE_CURVE('',#8405,#8404,#2145,.T.);
#10439=EDGE_CURVE('',#8345,#8407,#368,.T.);
#10440=EDGE_CURVE('',#8407,#8406,#2146,.T.);
#10441=EDGE_CURVE('',#8345,#8408,#369,.T.);
#10442=EDGE_CURVE('',#8408,#8407,#370,.T.);
#10443=EDGE_CURVE('',#8409,#8410,#371,.T.);
#10444=EDGE_CURVE('',#8410,#8405,#2147,.T.);
#10445=EDGE_CURVE('',#8406,#8409,#2148,.T.);
#10446=EDGE_CURVE('',#8409,#8411,#372,.T.);
#10447=EDGE_CURVE('',#8411,#8410,#373,.T.);
#10448=EDGE_CURVE('',#8412,#8413,#374,.T.);
#10449=EDGE_CURVE('',#8413,#8403,#2149,.T.);
#10450=EDGE_CURVE('',#8404,#8412,#2150,.T.);
#10451=EDGE_CURVE('',#8412,#8414,#375,.T.);
#10452=EDGE_CURVE('',#8414,#8413,#376,.T.);
#10453=EDGE_CURVE('',#8415,#8416,#377,.T.);
#10454=EDGE_CURVE('',#8416,#8399,#2151,.T.);
#10455=EDGE_CURVE('',#8400,#8415,#2152,.T.);
#10456=EDGE_CURVE('',#8415,#8417,#378,.T.);
#10457=EDGE_CURVE('',#8417,#8416,#379,.T.);
#10458=EDGE_CURVE('',#8415,#8413,#2153,.T.);
#10459=EDGE_CURVE('',#8412,#8410,#2154,.T.);
#10460=EDGE_CURVE('',#8411,#8414,#2155,.T.);
#10461=EDGE_CURVE('',#8409,#8418,#2156,.T.);
#10462=EDGE_CURVE('',#8419,#8418,#380,.T.);
#10463=EDGE_CURVE('',#8419,#8411,#2157,.T.);
#10464=EDGE_CURVE('',#8418,#8407,#2158,.T.);
#10465=EDGE_CURVE('',#8420,#8373,#381,.F.);
#10466=EDGE_CURVE('',#8421,#8420,#382,.F.);
#10467=EDGE_CURVE('',#8373,#8421,#383,.F.);
#10468=EDGE_CURVE('',#8422,#8423,#384,.T.);
#10469=EDGE_CURVE('',#8423,#8424,#385,.T.);
#10470=EDGE_CURVE('',#8424,#8422,#386,.T.);
#10471=EDGE_CURVE('',#8422,#8421,#2159,.T.);
#10472=EDGE_CURVE('',#8420,#8423,#2160,.T.);
#10473=EDGE_CURVE('',#8425,#8372,#387,.T.);
#10474=EDGE_CURVE('',#8421,#8425,#388,.T.);
#10475=EDGE_CURVE('',#8425,#8426,#389,.T.);
#10476=EDGE_CURVE('',#8426,#8372,#390,.T.);
#10477=EDGE_CURVE('',#8375,#8427,#391,.T.);
#10478=EDGE_CURVE('',#8427,#8420,#2161,.T.);
#10479=EDGE_CURVE('',#8311,#8428,#392,.T.);
#10480=EDGE_CURVE('',#8428,#8375,#393,.T.);
#10481=EDGE_CURVE('',#8297,#8374,#394,.T.);
#10482=EDGE_CURVE('',#8374,#8429,#395,.T.);
#10483=EDGE_CURVE('',#8429,#8297,#396,.T.);
#10484=EDGE_CURVE('',#8428,#8427,#397,.T.);
#10485=EDGE_CURVE('',#8424,#8430,#398,.T.);
#10486=EDGE_CURVE('',#8431,#8430,#399,.T.);
#10487=EDGE_CURVE('',#8431,#8422,#400,.T.);
#10488=EDGE_CURVE('',#8423,#8432,#2162,.T.);
#10489=EDGE_CURVE('',#8314,#8432,#401,.T.);
#10490=EDGE_CURVE('',#8314,#8424,#2163,.T.);
#10491=EDGE_CURVE('',#8432,#8427,#2164,.T.);
#10492=EDGE_CURVE('',#8428,#8315,#2165,.T.);
#10493=EDGE_CURVE('',#8315,#8432,#402,.T.);
#10494=EDGE_CURVE('',#8429,#8433,#2166,.T.);
#10495=EDGE_CURVE('',#8433,#8295,#403,.F.);
#10496=EDGE_CURVE('',#8371,#8434,#404,.T.);
#10497=EDGE_CURVE('',#8434,#8435,#405,.T.);
#10498=EDGE_CURVE('',#8435,#8434,#406,.T.);
#10499=EDGE_CURVE('',#8435,#8436,#2167,.T.);
#10500=EDGE_CURVE('',#8437,#8436,#407,.T.);
#10501=EDGE_CURVE('',#8436,#8437,#408,.T.);
#10502=EDGE_CURVE('',#8438,#8439,#409,.F.);
#10503=EDGE_CURVE('',#8344,#8438,#410,.F.);
#10504=EDGE_CURVE('',#8439,#8344,#411,.F.);
#10505=EDGE_CURVE('',#8438,#8408,#2168,.T.);
#10506=EDGE_CURVE('',#8440,#8441,#412,.F.);
#10507=EDGE_CURVE('',#8343,#8440,#413,.F.);
#10508=EDGE_CURVE('',#8441,#8343,#414,.F.);
#10509=EDGE_CURVE('',#8440,#8439,#2169,.T.);
#10510=EDGE_CURVE('',#8442,#8443,#415,.F.);
#10511=EDGE_CURVE('',#8342,#8442,#416,.F.);
#10512=EDGE_CURVE('',#8443,#8342,#417,.F.);
#10513=EDGE_CURVE('',#8442,#8441,#2170,.T.);
#10514=EDGE_CURVE('',#8444,#8445,#418,.F.);
#10515=EDGE_CURVE('',#8341,#8444,#419,.F.);
#10516=EDGE_CURVE('',#8445,#8341,#420,.F.);
#10517=EDGE_CURVE('',#8444,#8443,#2171,.T.);
#10518=EDGE_CURVE('',#8446,#8445,#2172,.T.);
#10519=EDGE_CURVE('',#8340,#8446,#1814,.T.);
#10520=EDGE_CURVE('',#8339,#8447,#1815,.T.);
#10521=EDGE_CURVE('',#8447,#8446,#2173,.T.);
#10522=EDGE_CURVE('',#8448,#8449,#421,.F.);
#10523=EDGE_CURVE('',#8338,#8448,#422,.F.);
#10524=EDGE_CURVE('',#8449,#8338,#423,.F.);
#10525=EDGE_CURVE('',#8448,#8447,#2174,.T.);
#10526=EDGE_CURVE('',#8395,#8449,#2175,.T.);
#10527=EDGE_CURVE('',#8450,#8451,#424,.T.);
#10528=EDGE_CURVE('',#8451,#8448,#2176,.T.);
#10529=EDGE_CURVE('',#8449,#8450,#2177,.T.);
#10530=EDGE_CURVE('',#8450,#8452,#425,.T.);
#10531=EDGE_CURVE('',#8452,#8451,#426,.T.);
#10532=EDGE_CURVE('',#8453,#8454,#427,.T.);
#10533=EDGE_CURVE('',#8454,#8444,#2178,.T.);
#10534=EDGE_CURVE('',#8445,#8453,#2179,.T.);
#10535=EDGE_CURVE('',#8453,#8455,#428,.T.);
#10536=EDGE_CURVE('',#8455,#8454,#429,.T.);
#10537=EDGE_CURVE('',#8456,#8457,#430,.T.);
#10538=EDGE_CURVE('',#8457,#8442,#2180,.T.);
#10539=EDGE_CURVE('',#8443,#8456,#2181,.T.);
#10540=EDGE_CURVE('',#8456,#8458,#431,.T.);
#10541=EDGE_CURVE('',#8458,#8457,#432,.T.);
#10542=EDGE_CURVE('',#8459,#8460,#433,.T.);
#10543=EDGE_CURVE('',#8460,#8440,#2182,.T.);
#10544=EDGE_CURVE('',#8441,#8459,#2183,.T.);
#10545=EDGE_CURVE('',#8459,#8461,#434,.T.);
#10546=EDGE_CURVE('',#8461,#8460,#435,.T.);
#10547=EDGE_CURVE('',#8462,#8463,#436,.T.);
#10548=EDGE_CURVE('',#8463,#8438,#2184,.T.);
#10549=EDGE_CURVE('',#8439,#8462,#2185,.T.);
#10550=EDGE_CURVE('',#8462,#8464,#437,.T.);
#10551=EDGE_CURVE('',#8464,#8463,#438,.T.);
#10552=EDGE_CURVE('',#8408,#8465,#2186,.T.);
#10553=EDGE_CURVE('',#8465,#8418,#439,.T.);
#10554=EDGE_CURVE('',#8465,#8419,#440,.T.);
#10555=EDGE_CURVE('',#8459,#8457,#2187,.T.);
#10556=EDGE_CURVE('',#8461,#8464,#2188,.T.);
#10557=EDGE_CURVE('',#8462,#8460,#2189,.T.);
#10558=EDGE_CURVE('',#8458,#8461,#2190,.T.);
#10559=EDGE_CURVE('',#8456,#8454,#2191,.T.);
#10560=EDGE_CURVE('',#8455,#8458,#2192,.T.);
#10561=EDGE_CURVE('',#8453,#8466,#2193,.T.);
#10562=EDGE_CURVE('',#8467,#8466,#1816,.T.);
#10563=EDGE_CURVE('',#8467,#8455,#2194,.T.);
#10564=EDGE_CURVE('',#8446,#8466,#2195,.T.);
#10565=EDGE_CURVE('',#8447,#8468,#2196,.T.);
#10566=EDGE_CURVE('',#8466,#8468,#2197,.T.);
#10567=EDGE_CURVE('',#8468,#8451,#2198,.T.);
#10568=EDGE_CURVE('',#8452,#8469,#2199,.T.);
#10569=EDGE_CURVE('',#8469,#8468,#1817,.T.);
#10570=EDGE_CURVE('',#8450,#8470,#2200,.T.);
#10571=EDGE_CURVE('',#8470,#8471,#1818,.F.);
#10572=EDGE_CURVE('',#8471,#8452,#2201,.T.);
#10573=EDGE_CURVE('',#8395,#8470,#2202,.T.);
#10574=EDGE_CURVE('',#8472,#8472,#441,.T.);
#10575=EDGE_CURVE('',#8472,#8437,#442,.T.);
#10576=EDGE_CURVE('',#8473,#8471,#2203,.T.);
#10577=EDGE_CURVE('',#8474,#8473,#2204,.T.);
#10578=EDGE_CURVE('',#8475,#8474,#443,.T.);
#10579=EDGE_CURVE('',#8476,#8475,#2205,.T.);
#10580=EDGE_CURVE('',#8477,#8476,#2206,.T.);
#10581=EDGE_CURVE('',#8478,#8477,#2207,.T.);
#10582=EDGE_CURVE('',#8479,#8478,#2208,.T.);
#10583=EDGE_CURVE('',#8480,#8479,#2209,.T.);
#10584=EDGE_CURVE('',#8481,#8480,#2210,.T.);
#10585=EDGE_CURVE('',#8482,#8481,#2211,.T.);
#10586=EDGE_CURVE('',#8483,#8482,#2212,.T.);
#10587=EDGE_CURVE('',#8484,#8483,#2213,.T.);
#10588=EDGE_CURVE('',#8417,#8484,#2214,.T.);
#10589=EDGE_CURVE('',#8414,#8417,#2215,.T.);
#10590=EDGE_CURVE('',#8464,#8419,#2216,.T.);
#10591=EDGE_CURVE('',#8469,#8467,#2217,.T.);
#10592=EDGE_CURVE('',#8485,#8325,#444,.T.);
#10593=EDGE_CURVE('',#8486,#8485,#2218,.T.);
#10594=EDGE_CURVE('',#8487,#8486,#445,.T.);
#10595=EDGE_CURVE('',#8488,#8487,#2219,.T.);
#10596=EDGE_CURVE('',#8331,#8488,#446,.T.);
#10597=EDGE_CURVE('',#8489,#8490,#2220,.T.);
#10598=EDGE_CURVE('',#8491,#8489,#447,.T.);
#10599=EDGE_CURVE('',#8492,#8491,#2221,.T.);
#10600=EDGE_CURVE('',#8490,#8492,#448,.T.);
#10601=EDGE_CURVE('',#8493,#8493,#449,.T.);
#10602=EDGE_CURVE('',#8430,#8296,#2222,.T.);
#10603=EDGE_CURVE('',#8494,#8494,#450,.T.);
#10604=EDGE_CURVE('',#8495,#8495,#451,.T.);
#10605=EDGE_CURVE('',#8296,#8433,#452,.F.);
#10606=EDGE_CURVE('',#8496,#8430,#453,.T.);
#10607=EDGE_CURVE('',#8433,#8496,#2223,.T.);
#10608=EDGE_CURVE('',#8426,#8429,#2224,.T.);
#10609=EDGE_CURVE('',#8425,#8431,#2225,.T.);
#10610=EDGE_CURVE('',#8431,#8496,#454,.T.);
#10611=EDGE_CURVE('',#8496,#8426,#2226,.T.);
#10612=EDGE_CURVE('',#8465,#8463,#2227,.T.);
#10613=EDGE_CURVE('',#8497,#8484,#455,.T.);
#10614=EDGE_CURVE('',#8484,#8498,#456,.T.);
#10615=EDGE_CURVE('',#8498,#8497,#457,.T.);
#10616=EDGE_CURVE('',#8497,#8416,#2228,.T.);
#10617=EDGE_CURVE('',#8401,#8497,#2229,.T.);
#10618=EDGE_CURVE('',#8498,#8402,#2230,.T.);
#10619=EDGE_CURVE('',#8394,#8499,#458,.F.);
#10620=EDGE_CURVE('',#8499,#8369,#459,.F.);
#10621=EDGE_CURVE('',#8500,#8501,#460,.F.);
#10622=EDGE_CURVE('',#8368,#8500,#461,.F.);
#10623=EDGE_CURVE('',#8501,#8368,#462,.F.);
#10624=EDGE_CURVE('',#8500,#8499,#2231,.T.);
#10625=EDGE_CURVE('',#8502,#8367,#463,.T.);
#10626=EDGE_CURVE('',#8367,#8503,#464,.T.);
#10627=EDGE_CURVE('',#8503,#8502,#465,.T.);
#10628=EDGE_CURVE('',#8502,#8501,#466,.T.);
#10629=EDGE_CURVE('',#8504,#8505,#467,.T.);
#10630=EDGE_CURVE('',#8505,#8500,#2232,.T.);
#10631=EDGE_CURVE('',#8501,#8504,#2233,.T.);
#10632=EDGE_CURVE('',#8504,#8486,#468,.T.);
#10633=EDGE_CURVE('',#8486,#8505,#469,.T.);
#10634=EDGE_CURVE('',#8506,#8507,#470,.T.);
#10635=EDGE_CURVE('',#8507,#8485,#471,.T.);
#10636=EDGE_CURVE('',#8485,#8506,#472,.T.);
#10637=EDGE_CURVE('',#8506,#8394,#2234,.T.);
#10638=EDGE_CURVE('',#8499,#8507,#2235,.T.);
#10639=EDGE_CURVE('',#8393,#8325,#473,.T.);
#10640=EDGE_CURVE('',#8393,#8506,#474,.T.);
#10641=EDGE_CURVE('',#8508,#8332,#475,.T.);
#10642=EDGE_CURVE('',#8331,#8508,#476,.T.);
#10643=EDGE_CURVE('',#8508,#8392,#2236,.T.);
#10644=EDGE_CURVE('',#8392,#8509,#477,.T.);
#10645=EDGE_CURVE('',#8509,#8366,#478,.T.);
#10646=EDGE_CURVE('',#8509,#8510,#479,.T.);
#10647=EDGE_CURVE('',#8510,#8366,#480,.T.);
#10648=EDGE_CURVE('',#8511,#8488,#481,.T.);
#10649=EDGE_CURVE('',#8511,#8508,#482,.T.);
#10650=EDGE_CURVE('',#8512,#8513,#483,.T.);
#10651=EDGE_CURVE('',#8513,#8487,#484,.T.);
#10652=EDGE_CURVE('',#8487,#8512,#485,.T.);
#10653=EDGE_CURVE('',#8503,#8513,#2237,.T.);
#10654=EDGE_CURVE('',#8512,#8502,#2238,.T.);
#10655=EDGE_CURVE('',#8510,#8503,#2239,.T.);
#10656=EDGE_CURVE('',#8509,#8511,#2240,.T.);
#10657=EDGE_CURVE('',#8511,#8514,#486,.T.);
#10658=EDGE_CURVE('',#8514,#8510,#2241,.T.);
#10659=EDGE_CURVE('',#8488,#8514,#487,.T.);
#10660=EDGE_CURVE('',#8513,#8514,#2242,.T.);
#10661=EDGE_CURVE('',#8515,#8473,#488,.T.);
#10662=EDGE_CURVE('',#8470,#8515,#2243,.T.);
#10663=EDGE_CURVE('',#8516,#8517,#489,.F.);
#10664=EDGE_CURVE('',#8357,#8516,#490,.F.);
#10665=EDGE_CURVE('',#8517,#8357,#491,.F.);
#10666=EDGE_CURVE('',#8358,#8518,#492,.T.);
#10667=EDGE_CURVE('',#8518,#8398,#493,.T.);
#10668=EDGE_CURVE('',#8516,#8518,#2244,.T.);
#10669=EDGE_CURVE('',#8519,#8517,#2245,.T.);
#10670=EDGE_CURVE('',#8356,#8519,#1819,.T.);
#10671=EDGE_CURVE('',#8520,#8521,#494,.F.);
#10672=EDGE_CURVE('',#8355,#8520,#495,.F.);
#10673=EDGE_CURVE('',#8521,#8355,#496,.F.);
#10674=EDGE_CURVE('',#8520,#8519,#2246,.T.);
#10675=EDGE_CURVE('',#8522,#8521,#2247,.T.);
#10676=EDGE_CURVE('',#8354,#8522,#1820,.T.);
#10677=EDGE_CURVE('',#8353,#8523,#1821,.T.);
#10678=EDGE_CURVE('',#8523,#8522,#2248,.T.);
#10679=EDGE_CURVE('',#8524,#8525,#497,.F.);
#10680=EDGE_CURVE('',#8352,#8524,#498,.F.);
#10681=EDGE_CURVE('',#8525,#8352,#499,.F.);
#10682=EDGE_CURVE('',#8524,#8523,#2249,.T.);
#10683=EDGE_CURVE('',#8526,#8527,#500,.F.);
#10684=EDGE_CURVE('',#8351,#8526,#501,.F.);
#10685=EDGE_CURVE('',#8527,#8351,#502,.F.);
#10686=EDGE_CURVE('',#8526,#8525,#2250,.T.);
#10687=EDGE_CURVE('',#8528,#8529,#503,.F.);
#10688=EDGE_CURVE('',#8350,#8528,#504,.F.);
#10689=EDGE_CURVE('',#8529,#8350,#505,.F.);
#10690=EDGE_CURVE('',#8528,#8527,#2251,.T.);
#10691=EDGE_CURVE('',#8402,#8529,#2252,.T.);
#10692=EDGE_CURVE('',#8530,#8531,#506,.T.);
#10693=EDGE_CURVE('',#8531,#8528,#2253,.T.);
#10694=EDGE_CURVE('',#8529,#8530,#2254,.T.);
#10695=EDGE_CURVE('',#8483,#8530,#507,.T.);
#10696=EDGE_CURVE('',#8530,#8498,#2255,.T.);
#10697=EDGE_CURVE('',#8532,#8533,#508,.T.);
#10698=EDGE_CURVE('',#8533,#8526,#2256,.T.);
#10699=EDGE_CURVE('',#8527,#8532,#2257,.T.);
#10700=EDGE_CURVE('',#8532,#8482,#509,.T.);
#10701=EDGE_CURVE('',#8482,#8533,#510,.T.);
#10702=EDGE_CURVE('',#8534,#8535,#511,.T.);
#10703=EDGE_CURVE('',#8535,#8524,#2258,.T.);
#10704=EDGE_CURVE('',#8525,#8534,#2259,.T.);
#10705=EDGE_CURVE('',#8534,#8481,#512,.T.);
#10706=EDGE_CURVE('',#8481,#8535,#513,.T.);
#10707=EDGE_CURVE('',#8536,#8537,#514,.T.);
#10708=EDGE_CURVE('',#8537,#8520,#2260,.T.);
#10709=EDGE_CURVE('',#8521,#8536,#2261,.T.);
#10710=EDGE_CURVE('',#8536,#8478,#515,.T.);
#10711=EDGE_CURVE('',#8478,#8537,#516,.T.);
#10712=EDGE_CURVE('',#8538,#8539,#517,.T.);
#10713=EDGE_CURVE('',#8539,#8516,#2262,.T.);
#10714=EDGE_CURVE('',#8517,#8538,#2263,.T.);
#10715=EDGE_CURVE('',#8538,#8476,#518,.T.);
#10716=EDGE_CURVE('',#8476,#8539,#519,.T.);
#10717=EDGE_CURVE('',#8397,#8540,#2264,.T.);
#10718=EDGE_CURVE('',#8540,#8515,#520,.T.);
#10719=EDGE_CURVE('',#8515,#8396,#2265,.T.);
#10720=EDGE_CURVE('',#8483,#8531,#521,.T.);
#10721=EDGE_CURVE('',#8540,#8473,#522,.T.);
#10722=EDGE_CURVE('',#8541,#8475,#523,.T.);
#10723=EDGE_CURVE('',#8541,#8539,#2266,.T.);
#10724=EDGE_CURVE('',#8538,#8542,#2267,.T.);
#10725=EDGE_CURVE('',#8477,#8542,#1822,.T.);
#10726=EDGE_CURVE('',#8519,#8542,#2268,.T.);
#10727=EDGE_CURVE('',#8542,#8537,#2269,.T.);
#10728=EDGE_CURVE('',#8536,#8543,#2270,.T.);
#10729=EDGE_CURVE('',#8479,#8543,#1823,.T.);
#10730=EDGE_CURVE('',#8522,#8543,#2271,.T.);
#10731=EDGE_CURVE('',#8523,#8544,#2272,.T.);
#10732=EDGE_CURVE('',#8543,#8544,#2273,.T.);
#10733=EDGE_CURVE('',#8544,#8535,#2274,.T.);
#10734=EDGE_CURVE('',#8480,#8544,#1824,.T.);
#10735=EDGE_CURVE('',#8534,#8533,#2275,.T.);
#10736=EDGE_CURVE('',#8532,#8531,#2276,.T.);
#10737=EDGE_CURVE('',#8540,#8545,#2277,.T.);
#10738=EDGE_CURVE('',#8545,#8474,#524,.T.);
#10739=EDGE_CURVE('',#8545,#8541,#525,.T.);
#10740=EDGE_CURVE('',#8518,#8541,#2278,.T.);
#10741=EDGE_CURVE('',#8398,#8545,#2279,.T.);
#10742=EDGE_CURVE('',#8504,#8512,#526,.T.);
#10743=EDGE_CURVE('',#8507,#8505,#2280,.T.);
#10744=EDGE_CURVE('',#8495,#8378,#527,.T.);
#10745=EDGE_CURVE('',#8490,#8387,#528,.T.);
#10746=EDGE_CURVE('',#8389,#8489,#529,.T.);
#10747=EDGE_CURVE('',#8546,#8491,#530,.T.);
#10748=EDGE_CURVE('',#8389,#8546,#531,.T.);
#10749=EDGE_CURVE('',#8388,#8492,#532,.T.);
#10750=EDGE_CURVE('',#8546,#8388,#2281,.T.);
#10751=EDGE_CURVE('',#8386,#8546,#2282,.T.);
#10752=EDGE_CURVE('',#8286,#8494,#533,.T.);
#10753=EDGE_CURVE('',#8547,#8548,#534,.T.);
#10754=EDGE_CURVE('',#8548,#8493,#535,.T.);
#10755=EDGE_CURVE('',#8548,#8547,#536,.T.);
#10756=EDGE_CURVE('',#8549,#8550,#537,.T.);
#10757=EDGE_CURVE('',#8550,#8549,#538,.T.);
#10758=EDGE_CURVE('',#8550,#8547,#2283,.T.);
#10759=EDGE_CURVE('',#8549,#8382,#539,.T.);
#10760=EDGE_CURVE('',#8551,#8552,#2284,.T.);
#10761=EDGE_CURVE('',#8552,#8553,#1825,.T.);
#10762=EDGE_CURVE('',#8553,#8554,#2285,.T.);
#10763=EDGE_CURVE('',#8554,#8551,#1826,.T.);
#10764=EDGE_CURVE('',#8555,#8553,#2286,.T.);
#10765=EDGE_CURVE('',#8552,#8556,#2287,.T.);
#10766=EDGE_CURVE('',#8555,#8556,#1827,.T.);
#10767=EDGE_CURVE('',#8557,#8551,#2288,.T.);
#10768=EDGE_CURVE('',#8554,#8558,#2289,.T.);
#10769=EDGE_CURVE('',#8558,#8557,#1828,.T.);
#10770=EDGE_CURVE('',#8556,#8557,#2290,.T.);
#10771=EDGE_CURVE('',#8558,#8555,#2291,.T.);
#10772=EDGE_CURVE('',#8559,#8554,#2292,.T.);
#10773=EDGE_CURVE('',#8560,#8559,#2293,.T.);
#10774=EDGE_CURVE('',#8560,#8558,#2294,.T.);
#10775=EDGE_CURVE('',#8561,#8553,#2295,.T.);
#10776=EDGE_CURVE('',#8559,#8561,#2296,.T.);
#10777=EDGE_CURVE('',#8562,#8563,#2297,.T.);
#10778=EDGE_CURVE('',#8564,#8562,#1829,.T.);
#10779=EDGE_CURVE('',#8565,#8564,#2298,.T.);
#10780=EDGE_CURVE('',#8566,#8565,#2299,.T.);
#10781=EDGE_CURVE('',#8567,#8566,#2300,.T.);
#10782=EDGE_CURVE('',#8567,#8563,#2301,.T.);
#10783=EDGE_CURVE('',#8568,#8562,#7685,.F.);
#10784=EDGE_CURVE('',#8563,#8569,#1830,.F.);
#10785=EDGE_CURVE('',#8569,#8568,#2302,.T.);
#10786=EDGE_CURVE('',#8570,#8571,#2303,.T.);
#10787=EDGE_CURVE('',#8571,#8572,#1831,.T.);
#10788=EDGE_CURVE('',#8572,#8560,#2304,.T.);
#10789=EDGE_CURVE('',#8570,#8560,#1832,.T.);
#10790=EDGE_CURVE('',#8573,#8574,#2305,.T.);
#10791=EDGE_CURVE('',#8574,#8559,#1833,.T.);
#10792=EDGE_CURVE('',#8561,#8573,#1834,.T.);
#10793=EDGE_CURVE('',#8574,#8570,#2306,.T.);
#10794=EDGE_CURVE('',#8571,#8573,#2307,.T.);
#10795=EDGE_CURVE('',#8561,#8572,#2308,.T.);
#10796=EDGE_CURVE('',#8572,#8555,#2309,.T.);
#10797=EDGE_CURVE('',#8575,#8576,#2310,.T.);
#10798=EDGE_CURVE('',#8577,#8575,#2311,.T.);
#10799=EDGE_CURVE('',#8577,#8578,#2312,.T.);
#10800=EDGE_CURVE('',#8579,#8578,#2313,.T.);
#10801=EDGE_CURVE('',#8580,#8579,#2314,.T.);
#10802=EDGE_CURVE('',#8576,#8580,#2315,.T.);
#10803=EDGE_CURVE('',#8581,#8575,#1835,.F.);
#10804=EDGE_CURVE('',#8576,#8582,#1836,.F.);
#10805=EDGE_CURVE('',#8582,#8581,#2316,.T.);
#10806=EDGE_CURVE('',#8583,#8584,#7686,.F.);
#10807=EDGE_CURVE('',#8584,#8585,#2317,.T.);
#10808=EDGE_CURVE('',#8585,#8586,#1837,.F.);
#10809=EDGE_CURVE('',#8586,#8583,#2318,.T.);
#10810=EDGE_CURVE('',#8587,#8584,#1838,.F.);
#10811=EDGE_CURVE('',#8588,#8587,#2319,.T.);
#10812=EDGE_CURVE('',#8589,#8588,#2320,.T.);
#10813=EDGE_CURVE('',#8589,#8585,#2321,.T.);
#10814=EDGE_CURVE('',#8590,#8591,#2322,.T.);
#10815=EDGE_CURVE('',#8591,#8592,#1839,.T.);
#10816=EDGE_CURVE('',#8592,#8593,#2323,.T.);
#10817=EDGE_CURVE('',#8593,#8590,#1840,.T.);
#10818=EDGE_CURVE('',#8594,#8592,#2324,.T.);
#10819=EDGE_CURVE('',#8591,#8595,#2325,.T.);
#10820=EDGE_CURVE('',#8594,#8595,#1841,.T.);
#10821=EDGE_CURVE('',#8596,#8590,#2326,.T.);
#10822=EDGE_CURVE('',#8593,#8597,#2327,.T.);
#10823=EDGE_CURVE('',#8597,#8596,#1842,.T.);
#10824=EDGE_CURVE('',#8595,#8596,#2328,.T.);
#10825=EDGE_CURVE('',#8597,#8594,#2329,.T.);
#10826=EDGE_CURVE('',#8598,#8593,#2330,.T.);
#10827=EDGE_CURVE('',#8599,#8598,#2331,.T.);
#10828=EDGE_CURVE('',#8599,#8597,#2332,.T.);
#10829=EDGE_CURVE('',#8600,#8592,#2333,.T.);
#10830=EDGE_CURVE('',#8598,#8600,#2334,.T.);
#10831=EDGE_CURVE('',#8586,#8601,#2335,.T.);
#10832=EDGE_CURVE('',#8602,#8601,#2336,.T.);
#10833=EDGE_CURVE('',#8603,#8602,#2337,.T.);
#10834=EDGE_CURVE('',#8603,#8604,#2338,.T.);
#10835=EDGE_CURVE('',#8583,#8604,#1843,.T.);
#10836=EDGE_CURVE('',#8605,#8579,#540,.T.);
#10837=EDGE_CURVE('',#8579,#8606,#541,.T.);
#10838=EDGE_CURVE('',#8606,#8605,#542,.T.);
#10839=EDGE_CURVE('',#8607,#8580,#1844,.F.);
#10840=EDGE_CURVE('',#8605,#8607,#2339,.T.);
#10841=EDGE_CURVE('',#8607,#8608,#2340,.T.);
#10842=EDGE_CURVE('',#8609,#8605,#2341,.T.);
#10843=EDGE_CURVE('',#8610,#8609,#2342,.T.);
#10844=EDGE_CURVE('',#8611,#8610,#2343,.T.);
#10845=EDGE_CURVE('',#8612,#8611,#2344,.T.);
#10846=EDGE_CURVE('',#8613,#8612,#2345,.T.);
#10847=EDGE_CURVE('',#8614,#8613,#2346,.T.);
#10848=EDGE_CURVE('',#8615,#8614,#2347,.T.);
#10849=EDGE_CURVE('',#8615,#8616,#2348,.T.);
#10850=EDGE_CURVE('',#8617,#8616,#2349,.T.);
#10851=EDGE_CURVE('',#8608,#8617,#2350,.T.);
#10852=EDGE_CURVE('',#8606,#8618,#2351,.T.);
#10853=EDGE_CURVE('',#8618,#8609,#1845,.T.);
#10854=EDGE_CURVE('',#8619,#8578,#1846,.T.);
#10855=EDGE_CURVE('',#8619,#8606,#2352,.T.);
#10856=EDGE_CURVE('',#8614,#8601,#1847,.T.);
#10857=EDGE_CURVE('',#8601,#8620,#2353,.T.);
#10858=EDGE_CURVE('',#8620,#8615,#1848,.T.);
#10859=EDGE_CURVE('',#8602,#8613,#543,.T.);
#10860=EDGE_CURVE('',#8613,#8621,#544,.T.);
#10861=EDGE_CURVE('',#8621,#8602,#545,.T.);
#10862=EDGE_CURVE('',#8620,#8622,#2354,.T.);
#10863=EDGE_CURVE('',#8622,#8623,#1849,.F.);
#10864=EDGE_CURVE('',#8623,#8615,#2355,.T.);
#10865=EDGE_CURVE('',#8623,#8624,#2356,.T.);
#10866=EDGE_CURVE('',#8616,#8624,#2357,.T.);
#10867=EDGE_CURVE('',#8581,#8625,#2358,.T.);
#10868=EDGE_CURVE('',#8625,#8577,#1850,.T.);
#10869=EDGE_CURVE('',#8625,#8626,#2359,.T.);
#10870=EDGE_CURVE('',#8626,#8627,#1851,.T.);
#10871=EDGE_CURVE('',#8627,#8577,#2360,.T.);
#10872=EDGE_CURVE('',#8626,#8628,#2361,.T.);
#10873=EDGE_CURVE('',#8628,#8629,#1852,.T.);
#10874=EDGE_CURVE('',#8629,#8627,#2362,.T.);
#10875=EDGE_CURVE('',#8630,#8631,#2363,.T.);
#10876=EDGE_CURVE('',#8631,#8632,#546,.T.);
#10877=EDGE_CURVE('',#8632,#8633,#2364,.T.);
#10878=EDGE_CURVE('',#8633,#8630,#1853,.T.);
#10879=EDGE_CURVE('',#8633,#8634,#2365,.T.);
#10880=EDGE_CURVE('',#8634,#8610,#1854,.T.);
#10881=EDGE_CURVE('',#8610,#8630,#2366,.T.);
#10882=EDGE_CURVE('',#8612,#8566,#547,.T.);
#10883=EDGE_CURVE('',#8566,#8635,#548,.T.);
#10884=EDGE_CURVE('',#8635,#8612,#549,.T.);
#10885=EDGE_CURVE('',#8611,#8567,#1855,.T.);
#10886=EDGE_CURVE('',#8634,#8567,#2367,.T.);
#10887=EDGE_CURVE('',#8636,#8632,#550,.T.);
#10888=EDGE_CURVE('',#8631,#8637,#551,.T.);
#10889=EDGE_CURVE('',#8637,#8636,#7687,.T.);
#10890=EDGE_CURVE('',#8628,#8636,#2368,.T.);
#10891=EDGE_CURVE('',#8637,#8629,#2369,.T.);
#10892=EDGE_CURVE('',#8627,#8638,#2370,.T.);
#10893=EDGE_CURVE('',#8578,#8638,#2371,.T.);
#10894=EDGE_CURVE('',#8629,#8639,#2372,.T.);
#10895=EDGE_CURVE('',#8638,#8639,#2373,.T.);
#10896=EDGE_CURVE('',#8637,#8640,#2374,.T.);
#10897=EDGE_CURVE('',#8639,#8640,#2375,.T.);
#10898=EDGE_CURVE('',#8631,#8641,#2376,.T.);
#10899=EDGE_CURVE('',#8640,#8641,#552,.T.);
#10900=EDGE_CURVE('',#8630,#8642,#2377,.T.);
#10901=EDGE_CURVE('',#8641,#8642,#2378,.T.);
#10902=EDGE_CURVE('',#8642,#8609,#2379,.T.);
#10903=EDGE_CURVE('',#8635,#8621,#2380,.T.);
#10904=EDGE_CURVE('',#8565,#8643,#1856,.T.);
#10905=EDGE_CURVE('',#8643,#8635,#2381,.T.);
#10906=EDGE_CURVE('',#8644,#8608,#1857,.F.);
#10907=EDGE_CURVE('',#8617,#8645,#553,.T.);
#10908=EDGE_CURVE('',#8645,#8644,#2382,.T.);
#10909=EDGE_CURVE('',#8617,#8646,#554,.T.);
#10910=EDGE_CURVE('',#8646,#8645,#555,.T.);
#10911=EDGE_CURVE('',#8647,#8616,#1858,.T.);
#10912=EDGE_CURVE('',#8647,#8646,#2383,.T.);
#10913=EDGE_CURVE('',#8648,#8589,#1859,.F.);
#10914=EDGE_CURVE('',#8588,#8649,#1860,.F.);
#10915=EDGE_CURVE('',#8649,#8648,#2384,.T.);
#10916=EDGE_CURVE('',#8650,#8651,#2385,.T.);
#10917=EDGE_CURVE('',#8651,#8652,#1861,.T.);
#10918=EDGE_CURVE('',#8652,#8599,#2386,.T.);
#10919=EDGE_CURVE('',#8650,#8599,#1862,.T.);
#10920=EDGE_CURVE('',#8653,#8654,#2387,.T.);
#10921=EDGE_CURVE('',#8654,#8598,#1863,.T.);
#10922=EDGE_CURVE('',#8600,#8653,#1864,.T.);
#10923=EDGE_CURVE('',#8654,#8650,#2388,.T.);
#10924=EDGE_CURVE('',#8651,#8653,#2389,.T.);
#10925=EDGE_CURVE('',#8600,#8652,#2390,.T.);
#10926=EDGE_CURVE('',#8652,#8594,#2391,.T.);
#10927=EDGE_CURVE('',#8655,#8645,#2392,.T.);
#10928=EDGE_CURVE('',#8656,#8655,#2393,.T.);
#10929=EDGE_CURVE('',#8648,#8656,#2394,.T.);
#10930=EDGE_CURVE('',#8644,#8649,#2395,.T.);
#10931=EDGE_CURVE('',#8657,#8658,#556,.T.);
#10932=EDGE_CURVE('',#8658,#8623,#2396,.T.);
#10933=EDGE_CURVE('',#8622,#8657,#2397,.T.);
#10934=EDGE_CURVE('',#8659,#8658,#557,.T.);
#10935=EDGE_CURVE('',#8657,#8660,#558,.T.);
#10936=EDGE_CURVE('',#8660,#8659,#7688,.T.);
#10937=EDGE_CURVE('',#8660,#8661,#2398,.T.);
#10938=EDGE_CURVE('',#8661,#8662,#1865,.T.);
#10939=EDGE_CURVE('',#8662,#8659,#2399,.T.);
#10940=EDGE_CURVE('',#8661,#8663,#2400,.T.);
#10941=EDGE_CURVE('',#8663,#8664,#1866,.T.);
#10942=EDGE_CURVE('',#8664,#8662,#2401,.T.);
#10943=EDGE_CURVE('',#8665,#8589,#2402,.T.);
#10944=EDGE_CURVE('',#8656,#8665,#1867,.T.);
#10945=EDGE_CURVE('',#8663,#8665,#2403,.T.);
#10946=EDGE_CURVE('',#8656,#8664,#2404,.T.);
#10947=EDGE_CURVE('',#8658,#8666,#2405,.T.);
#10948=EDGE_CURVE('',#8624,#8666,#2406,.T.);
#10949=EDGE_CURVE('',#8659,#8667,#2407,.T.);
#10950=EDGE_CURVE('',#8666,#8667,#559,.T.);
#10951=EDGE_CURVE('',#8662,#8668,#2408,.T.);
#10952=EDGE_CURVE('',#8667,#8668,#2409,.T.);
#10953=EDGE_CURVE('',#8664,#8669,#2410,.T.);
#10954=EDGE_CURVE('',#8668,#8669,#2411,.T.);
#10955=EDGE_CURVE('',#8669,#8655,#2412,.T.);
#10956=EDGE_CURVE('',#8618,#8670,#2413,.T.);
#10957=EDGE_CURVE('',#8670,#8642,#1868,.T.);
#10958=EDGE_CURVE('',#8641,#8671,#560,.T.);
#10959=EDGE_CURVE('',#8671,#8672,#561,.T.);
#10960=EDGE_CURVE('',#8672,#8640,#7689,.T.);
#10961=EDGE_CURVE('',#8670,#8671,#2414,.T.);
#10962=EDGE_CURVE('',#8672,#8673,#2415,.T.);
#10963=EDGE_CURVE('',#8673,#8639,#1869,.T.);
#10964=EDGE_CURVE('',#8673,#8674,#2416,.T.);
#10965=EDGE_CURVE('',#8674,#8638,#1870,.T.);
#10966=EDGE_CURVE('',#8674,#8619,#2417,.T.);
#10967=EDGE_CURVE('',#8675,#8675,#562,.T.);
#10968=EDGE_CURVE('',#8676,#8676,#563,.T.);
#10969=EDGE_CURVE('',#8677,#8677,#564,.T.);
#10970=EDGE_CURVE('',#8678,#8678,#565,.T.);
#10971=EDGE_CURVE('',#8678,#8679,#566,.T.);
#10972=EDGE_CURVE('',#8679,#8680,#567,.T.);
#10973=EDGE_CURVE('',#8680,#8679,#568,.T.);
#10974=EDGE_CURVE('',#8681,#8681,#569,.T.);
#10975=EDGE_CURVE('',#8680,#8682,#2418,.T.);
#10976=EDGE_CURVE('',#8682,#8682,#570,.T.);
#10977=EDGE_CURVE('',#8666,#8683,#571,.T.);
#10978=EDGE_CURVE('',#8683,#8684,#2419,.T.);
#10979=EDGE_CURVE('',#8684,#8624,#1871,.T.);
#10980=EDGE_CURVE('',#8684,#8647,#2420,.T.);
#10981=EDGE_CURVE('',#8646,#8685,#2421,.T.);
#10982=EDGE_CURVE('',#8685,#8655,#1872,.T.);
#10983=EDGE_CURVE('',#8685,#8686,#2422,.T.);
#10984=EDGE_CURVE('',#8686,#8669,#1873,.T.);
#10985=EDGE_CURVE('',#8686,#8687,#2423,.T.);
#10986=EDGE_CURVE('',#8687,#8668,#1874,.T.);
#10987=EDGE_CURVE('',#8687,#8688,#2424,.T.);
#10988=EDGE_CURVE('',#8688,#8667,#7690,.T.);
#10989=EDGE_CURVE('',#8688,#8683,#572,.T.);
#10990=EDGE_CURVE('',#8689,#8689,#573,.T.);
#10991=EDGE_CURVE('',#8690,#8690,#574,.T.);
#10992=EDGE_CURVE('',#8691,#8691,#575,.T.);
#10993=EDGE_CURVE('',#8692,#8692,#576,.T.);
#10994=EDGE_CURVE('',#8692,#8693,#577,.T.);
#10995=EDGE_CURVE('',#8693,#8694,#578,.T.);
#10996=EDGE_CURVE('',#8694,#8693,#579,.T.);
#10997=EDGE_CURVE('',#8695,#8695,#580,.T.);
#10998=EDGE_CURVE('',#8694,#8696,#2425,.T.);
#10999=EDGE_CURVE('',#8696,#8696,#581,.T.);
#11000=EDGE_CURVE('',#8695,#8697,#582,.T.);
#11001=EDGE_CURVE('',#8697,#8698,#583,.T.);
#11002=EDGE_CURVE('',#8698,#8697,#584,.T.);
#11003=EDGE_CURVE('',#8698,#8699,#2426,.T.);
#11004=EDGE_CURVE('',#8700,#8699,#585,.T.);
#11005=EDGE_CURVE('',#8699,#8700,#586,.T.);
#11006=EDGE_CURVE('',#8689,#8700,#587,.T.);
#11007=EDGE_CURVE('',#8681,#8701,#588,.T.);
#11008=EDGE_CURVE('',#8701,#8702,#589,.T.);
#11009=EDGE_CURVE('',#8702,#8701,#590,.T.);
#11010=EDGE_CURVE('',#8702,#8703,#2427,.T.);
#11011=EDGE_CURVE('',#8704,#8703,#591,.T.);
#11012=EDGE_CURVE('',#8703,#8704,#592,.T.);
#11013=EDGE_CURVE('',#8675,#8704,#593,.T.);
#11014=EDGE_CURVE('',#8691,#8705,#594,.T.);
#11015=EDGE_CURVE('',#8705,#8706,#595,.T.);
#11016=EDGE_CURVE('',#8706,#8705,#596,.T.);
#11017=EDGE_CURVE('',#8707,#8708,#597,.T.);
#11018=EDGE_CURVE('',#8708,#8707,#598,.T.);
#11019=EDGE_CURVE('',#8708,#8706,#2428,.T.);
#11020=EDGE_CURVE('',#8709,#8709,#599,.T.);
#11021=EDGE_CURVE('',#8709,#8707,#600,.T.);
#11022=EDGE_CURVE('',#8710,#8710,#601,.T.);
#11023=EDGE_CURVE('',#8677,#8711,#602,.T.);
#11024=EDGE_CURVE('',#8711,#8712,#603,.T.);
#11025=EDGE_CURVE('',#8712,#8711,#604,.T.);
#11026=EDGE_CURVE('',#8713,#8714,#605,.T.);
#11027=EDGE_CURVE('',#8714,#8713,#606,.T.);
#11028=EDGE_CURVE('',#8714,#8712,#2429,.T.);
#11029=EDGE_CURVE('',#8715,#8715,#607,.T.);
#11030=EDGE_CURVE('',#8715,#8713,#608,.T.);
#11031=EDGE_CURVE('',#8581,#8569,#2430,.T.);
#11032=EDGE_CURVE('',#8716,#8716,#609,.T.);
#11033=EDGE_CURVE('',#8690,#8717,#610,.T.);
#11034=EDGE_CURVE('',#8717,#8718,#611,.T.);
#11035=EDGE_CURVE('',#8718,#8717,#612,.T.);
#11036=EDGE_CURVE('',#8719,#8720,#613,.T.);
#11037=EDGE_CURVE('',#8720,#8719,#614,.T.);
#11038=EDGE_CURVE('',#8720,#8718,#2431,.T.);
#11039=EDGE_CURVE('',#8710,#8719,#615,.T.);
#11040=EDGE_CURVE('',#8676,#8721,#616,.T.);
#11041=EDGE_CURVE('',#8721,#8722,#617,.T.);
#11042=EDGE_CURVE('',#8722,#8721,#618,.T.);
#11043=EDGE_CURVE('',#8723,#8724,#619,.T.);
#11044=EDGE_CURVE('',#8724,#8723,#620,.T.);
#11045=EDGE_CURVE('',#8724,#8722,#2432,.T.);
#11046=EDGE_CURVE('',#8716,#8723,#621,.T.);
#11047=EDGE_CURVE('',#8725,#8725,#622,.T.);
#11048=EDGE_CURVE('',#8725,#8726,#623,.T.);
#11049=EDGE_CURVE('',#8726,#8727,#624,.T.);
#11050=EDGE_CURVE('',#8727,#8726,#625,.T.);
#11051=EDGE_CURVE('',#8728,#8729,#626,.T.);
#11052=EDGE_CURVE('',#8729,#8728,#627,.T.);
#11053=EDGE_CURVE('',#8729,#8727,#2433,.T.);
#11054=EDGE_CURVE('',#8730,#8731,#2434,.T.);
#11055=EDGE_CURVE('',#8730,#8582,#2435,.T.);
#11056=EDGE_CURVE('',#8644,#8580,#2436,.T.);
#11057=EDGE_CURVE('',#8732,#8587,#2437,.T.);
#11058=EDGE_CURVE('',#8731,#8732,#2438,.T.);
#11059=EDGE_CURVE('',#8733,#8733,#628,.T.);
#11060=EDGE_CURVE('',#8734,#8735,#2439,.T.);
#11061=EDGE_CURVE('',#8736,#8734,#2440,.T.);
#11062=EDGE_CURVE('',#8737,#8736,#2441,.T.);
#11063=EDGE_CURVE('',#8735,#8737,#2442,.T.);
#11064=EDGE_CURVE('',#8738,#8739,#2443,.T.);
#11065=EDGE_CURVE('',#8740,#8738,#2444,.T.);
#11066=EDGE_CURVE('',#8741,#8740,#2445,.T.);
#11067=EDGE_CURVE('',#8739,#8741,#2446,.T.);
#11068=EDGE_CURVE('',#8742,#8564,#2447,.T.);
#11069=EDGE_CURVE('',#8730,#8568,#1875,.T.);
#11070=EDGE_CURVE('',#8731,#8742,#1876,.T.);
#11071=EDGE_CURVE('',#8732,#8743,#1877,.T.);
#11072=EDGE_CURVE('',#8743,#8742,#2448,.T.);
#11073=EDGE_CURVE('',#8604,#8743,#2449,.T.);
#11074=EDGE_CURVE('',#8744,#8742,#2450,.T.);
#11075=EDGE_CURVE('',#8565,#8744,#2451,.T.);
#11076=EDGE_CURVE('',#8745,#8743,#2452,.T.);
#11077=EDGE_CURVE('',#8744,#8745,#2453,.T.);
#11078=EDGE_CURVE('',#8745,#8603,#2454,.T.);
#11079=EDGE_CURVE('',#8746,#8746,#629,.T.);
#11080=EDGE_CURVE('',#8746,#8728,#630,.T.);
#11081=EDGE_CURVE('',#8747,#8643,#2455,.T.);
#11082=EDGE_CURVE('',#8748,#8747,#2456,.T.);
#11083=EDGE_CURVE('',#8749,#8748,#2457,.T.);
#11084=EDGE_CURVE('',#8621,#8749,#2458,.T.);
#11085=EDGE_CURVE('',#8750,#8751,#2459,.T.);
#11086=EDGE_CURVE('',#8751,#8752,#2460,.T.);
#11087=EDGE_CURVE('',#8752,#8753,#2461,.T.);
#11088=EDGE_CURVE('',#8753,#8754,#2462,.T.);
#11089=EDGE_CURVE('',#8754,#8755,#2463,.T.);
#11090=EDGE_CURVE('',#8756,#8755,#2464,.T.);
#11091=EDGE_CURVE('',#8757,#8756,#2465,.T.);
#11092=EDGE_CURVE('',#8750,#8757,#2466,.T.);
#11093=EDGE_CURVE('',#8758,#8759,#2467,.T.);
#11094=EDGE_CURVE('',#8759,#8760,#2468,.T.);
#11095=EDGE_CURVE('',#8760,#8761,#2469,.T.);
#11096=EDGE_CURVE('',#8761,#8762,#2470,.T.);
#11097=EDGE_CURVE('',#8762,#8763,#2471,.T.);
#11098=EDGE_CURVE('',#8764,#8763,#2472,.T.);
#11099=EDGE_CURVE('',#8765,#8764,#2473,.T.);
#11100=EDGE_CURVE('',#8758,#8765,#2474,.T.);
#11101=EDGE_CURVE('',#8766,#8766,#631,.T.);
#11102=EDGE_CURVE('',#8747,#8744,#1878,.T.);
#11103=EDGE_CURVE('',#8748,#8745,#1879,.T.);
#11104=EDGE_CURVE('',#8749,#8603,#1880,.T.);
#11105=EDGE_CURVE('',#8766,#8767,#632,.T.);
#11106=EDGE_CURVE('',#8767,#8768,#633,.T.);
#11107=EDGE_CURVE('',#8768,#8767,#634,.T.);
#11108=EDGE_CURVE('',#8768,#8769,#2475,.T.);
#11109=EDGE_CURVE('',#8770,#8769,#635,.T.);
#11110=EDGE_CURVE('',#8769,#8770,#636,.T.);
#11111=EDGE_CURVE('',#8733,#8770,#637,.T.);
#11112=EDGE_CURVE('',#8739,#8771,#1881,.T.);
#11113=EDGE_CURVE('',#8771,#8772,#2476,.T.);
#11114=EDGE_CURVE('',#8772,#8738,#1882,.T.);
#11115=EDGE_CURVE('',#8773,#8771,#2477,.T.);
#11116=EDGE_CURVE('',#8773,#8741,#1883,.T.);
#11117=EDGE_CURVE('',#8772,#8774,#2478,.T.);
#11118=EDGE_CURVE('',#8774,#8740,#1884,.T.);
#11119=EDGE_CURVE('',#8774,#8773,#2479,.T.);
#11120=EDGE_CURVE('',#8775,#8772,#2480,.T.);
#11121=EDGE_CURVE('',#8776,#8775,#2481,.T.);
#11122=EDGE_CURVE('',#8776,#8774,#2482,.T.);
#11123=EDGE_CURVE('',#8777,#8771,#2483,.T.);
#11124=EDGE_CURVE('',#8775,#8777,#2484,.T.);
#11125=EDGE_CURVE('',#8777,#8758,#638,.F.);
#11126=EDGE_CURVE('',#8765,#8775,#1885,.T.);
#11127=EDGE_CURVE('',#8764,#8776,#1886,.T.);
#11128=EDGE_CURVE('',#8763,#8778,#639,.F.);
#11129=EDGE_CURVE('',#8778,#8776,#2485,.T.);
#11130=EDGE_CURVE('',#8778,#8773,#2486,.T.);
#11131=EDGE_CURVE('',#8735,#8779,#1887,.T.);
#11132=EDGE_CURVE('',#8779,#8780,#2487,.T.);
#11133=EDGE_CURVE('',#8780,#8734,#1888,.T.);
#11134=EDGE_CURVE('',#8781,#8779,#2488,.T.);
#11135=EDGE_CURVE('',#8781,#8737,#1889,.T.);
#11136=EDGE_CURVE('',#8780,#8782,#2489,.T.);
#11137=EDGE_CURVE('',#8782,#8736,#1890,.T.);
#11138=EDGE_CURVE('',#8782,#8781,#2490,.T.);
#11139=EDGE_CURVE('',#8783,#8780,#2491,.T.);
#11140=EDGE_CURVE('',#8784,#8783,#2492,.T.);
#11141=EDGE_CURVE('',#8784,#8782,#2493,.T.);
#11142=EDGE_CURVE('',#8785,#8779,#2494,.T.);
#11143=EDGE_CURVE('',#8783,#8785,#2495,.T.);
#11144=EDGE_CURVE('',#8785,#8750,#640,.F.);
#11145=EDGE_CURVE('',#8757,#8783,#1891,.T.);
#11146=EDGE_CURVE('',#8756,#8784,#1892,.T.);
#11147=EDGE_CURVE('',#8755,#8786,#641,.F.);
#11148=EDGE_CURVE('',#8786,#8784,#2496,.T.);
#11149=EDGE_CURVE('',#8786,#8781,#2497,.T.);
#11150=EDGE_CURVE('',#8787,#8788,#642,.T.);
#11151=EDGE_CURVE('',#8788,#8789,#2498,.T.);
#11152=EDGE_CURVE('',#8789,#8790,#643,.T.);
#11153=EDGE_CURVE('',#8790,#8791,#2499,.T.);
#11154=EDGE_CURVE('',#8791,#8792,#644,.T.);
#11155=EDGE_CURVE('',#8792,#8787,#2500,.T.);
#11156=EDGE_CURVE('',#8792,#8793,#645,.F.);
#11157=EDGE_CURVE('',#8793,#8794,#2501,.T.);
#11158=EDGE_CURVE('',#8794,#8787,#646,.T.);
#11159=EDGE_CURVE('',#8762,#8795,#2502,.T.);
#11160=EDGE_CURVE('',#8796,#8795,#647,.T.);
#11161=EDGE_CURVE('',#8796,#8797,#648,.T.);
#11162=EDGE_CURVE('',#8793,#8797,#2503,.T.);
#11163=EDGE_CURVE('',#8791,#8759,#2504,.T.);
#11164=EDGE_CURVE('',#8760,#8790,#2505,.T.);
#11165=EDGE_CURVE('',#8794,#8798,#2506,.T.);
#11166=EDGE_CURVE('',#8799,#8798,#649,.T.);
#11167=EDGE_CURVE('',#8800,#8799,#650,.T.);
#11168=EDGE_CURVE('',#8788,#8800,#2507,.T.);
#11169=EDGE_CURVE('',#8801,#8802,#651,.T.);
#11170=EDGE_CURVE('',#8802,#8800,#2508,.T.);
#11171=EDGE_CURVE('',#8799,#8796,#2509,.T.);
#11172=EDGE_CURVE('',#8795,#8801,#2510,.T.);
#11173=EDGE_CURVE('',#8802,#8789,#2511,.T.);
#11174=EDGE_CURVE('',#8761,#8801,#2512,.T.);
#11175=EDGE_CURVE('',#8798,#8797,#2513,.T.);
#11176=EDGE_CURVE('',#8803,#8804,#652,.T.);
#11177=EDGE_CURVE('',#8804,#8805,#2514,.T.);
#11178=EDGE_CURVE('',#8805,#8806,#653,.T.);
#11179=EDGE_CURVE('',#8806,#8807,#2515,.T.);
#11180=EDGE_CURVE('',#8807,#8808,#654,.T.);
#11181=EDGE_CURVE('',#8808,#8803,#2516,.T.);
#11182=EDGE_CURVE('',#8808,#8809,#655,.F.);
#11183=EDGE_CURVE('',#8809,#8810,#2517,.T.);
#11184=EDGE_CURVE('',#8810,#8803,#656,.T.);
#11185=EDGE_CURVE('',#8754,#8811,#2518,.T.);
#11186=EDGE_CURVE('',#8812,#8811,#657,.T.);
#11187=EDGE_CURVE('',#8812,#8813,#658,.T.);
#11188=EDGE_CURVE('',#8809,#8813,#2519,.T.);
#11189=EDGE_CURVE('',#8807,#8751,#2520,.T.);
#11190=EDGE_CURVE('',#8752,#8806,#2521,.T.);
#11191=EDGE_CURVE('',#8810,#8814,#2522,.T.);
#11192=EDGE_CURVE('',#8815,#8814,#659,.T.);
#11193=EDGE_CURVE('',#8816,#8815,#660,.T.);
#11194=EDGE_CURVE('',#8804,#8816,#2523,.T.);
#11195=EDGE_CURVE('',#8817,#8818,#661,.T.);
#11196=EDGE_CURVE('',#8818,#8816,#2524,.T.);
#11197=EDGE_CURVE('',#8815,#8812,#2525,.T.);
#11198=EDGE_CURVE('',#8811,#8817,#2526,.T.);
#11199=EDGE_CURVE('',#8818,#8805,#2527,.T.);
#11200=EDGE_CURVE('',#8753,#8817,#2528,.T.);
#11201=EDGE_CURVE('',#8814,#8813,#2529,.T.);
#11202=EDGE_CURVE('',#8819,#8820,#662,.F.);
#11203=EDGE_CURVE('',#8821,#8819,#663,.F.);
#11204=EDGE_CURVE('',#8820,#8821,#664,.F.);
#11205=EDGE_CURVE('',#8822,#8823,#665,.F.);
#11206=EDGE_CURVE('',#8824,#8822,#666,.F.);
#11207=EDGE_CURVE('',#8823,#8824,#667,.F.);
#11208=EDGE_CURVE('',#8825,#8826,#668,.T.);
#11209=EDGE_CURVE('',#8826,#8824,#2530,.T.);
#11210=EDGE_CURVE('',#8822,#8825,#2531,.T.);
#11211=EDGE_CURVE('',#8827,#8828,#669,.T.);
#11212=EDGE_CURVE('',#8828,#8823,#2532,.T.);
#11213=EDGE_CURVE('',#8824,#8827,#2533,.T.);
#11214=EDGE_CURVE('',#8819,#8822,#2534,.T.);
#11215=EDGE_CURVE('',#8823,#8821,#2535,.T.);
#11216=EDGE_CURVE('',#8829,#8830,#670,.F.);
#11217=EDGE_CURVE('',#8831,#8829,#671,.F.);
#11218=EDGE_CURVE('',#8830,#8831,#672,.F.);
#11219=EDGE_CURVE('',#8828,#8832,#673,.T.);
#11220=EDGE_CURVE('',#8832,#8831,#2536,.T.);
#11221=EDGE_CURVE('',#8829,#8828,#2537,.T.);
#11222=EDGE_CURVE('',#8833,#8830,#2538,.T.);
#11223=EDGE_CURVE('',#8831,#8834,#2539,.T.);
#11224=EDGE_CURVE('',#8834,#8833,#1893,.T.);
#11225=EDGE_CURVE('',#8835,#8819,#2540,.T.);
#11226=EDGE_CURVE('',#8820,#8836,#2541,.T.);
#11227=EDGE_CURVE('',#8836,#8835,#1894,.T.);
#11228=EDGE_CURVE('',#8837,#8838,#674,.F.);
#11229=EDGE_CURVE('',#8839,#8837,#675,.F.);
#11230=EDGE_CURVE('',#8838,#8839,#676,.F.);
#11231=EDGE_CURVE('',#8834,#8839,#2542,.T.);
#11232=EDGE_CURVE('',#8837,#8833,#2543,.T.);
#11233=EDGE_CURVE('',#8840,#8841,#677,.T.);
#11234=EDGE_CURVE('',#8841,#8838,#2544,.T.);
#11235=EDGE_CURVE('',#8839,#8840,#2545,.T.);
#11236=EDGE_CURVE('',#8842,#8843,#678,.F.);
#11237=EDGE_CURVE('',#8844,#8842,#679,.F.);
#11238=EDGE_CURVE('',#8843,#8844,#680,.F.);
#11239=EDGE_CURVE('',#8836,#8844,#2546,.T.);
#11240=EDGE_CURVE('',#8842,#8835,#2547,.T.);
#11241=EDGE_CURVE('',#8838,#8843,#2548,.T.);
#11242=EDGE_CURVE('',#8844,#8837,#2549,.T.);
#11243=EDGE_CURVE('',#8845,#8846,#681,.F.);
#11244=EDGE_CURVE('',#8847,#8845,#682,.F.);
#11245=EDGE_CURVE('',#8846,#8847,#683,.F.);
#11246=EDGE_CURVE('',#8848,#8849,#684,.F.);
#11247=EDGE_CURVE('',#8850,#8848,#685,.F.);
#11248=EDGE_CURVE('',#8849,#8850,#686,.F.);
#11249=EDGE_CURVE('',#8851,#8852,#687,.T.);
#11250=EDGE_CURVE('',#8852,#8850,#2550,.T.);
#11251=EDGE_CURVE('',#8848,#8851,#2551,.T.);
#11252=EDGE_CURVE('',#8853,#8854,#688,.F.);
#11253=EDGE_CURVE('',#8855,#8853,#689,.F.);
#11254=EDGE_CURVE('',#8854,#8855,#690,.F.);
#11255=EDGE_CURVE('',#8853,#8849,#2552,.T.);
#11256=EDGE_CURVE('',#8850,#8855,#2553,.T.);
#11257=EDGE_CURVE('',#8856,#8854,#2554,.T.);
#11258=EDGE_CURVE('',#8855,#8857,#2555,.T.);
#11259=EDGE_CURVE('',#8857,#8856,#1895,.T.);
#11260=EDGE_CURVE('',#8858,#8859,#691,.T.);
#11261=EDGE_CURVE('',#8859,#8860,#692,.T.);
#11262=EDGE_CURVE('',#8860,#8858,#693,.T.);
#11263=EDGE_CURVE('',#8858,#8853,#2556,.T.);
#11264=EDGE_CURVE('',#8854,#8859,#2557,.T.);
#11265=EDGE_CURVE('',#8857,#8847,#2558,.T.);
#11266=EDGE_CURVE('',#8845,#8856,#2559,.T.);
#11267=EDGE_CURVE('',#8861,#8862,#694,.T.);
#11268=EDGE_CURVE('',#8862,#8848,#2560,.T.);
#11269=EDGE_CURVE('',#8849,#8861,#2561,.T.);
#11270=EDGE_CURVE('',#8861,#8863,#695,.T.);
#11271=EDGE_CURVE('',#8863,#8862,#696,.T.);
#11272=EDGE_CURVE('',#8843,#8846,#2562,.T.);
#11273=EDGE_CURVE('',#8847,#8842,#2563,.T.);
#11274=EDGE_CURVE('',#8841,#8864,#697,.T.);
#11275=EDGE_CURVE('',#8864,#8845,#2564,.T.);
#11276=EDGE_CURVE('',#8846,#8841,#2565,.T.);
#11277=EDGE_CURVE('',#8830,#8820,#2566,.T.);
#11278=EDGE_CURVE('',#8821,#8829,#2567,.T.);
#11279=EDGE_CURVE('',#8851,#8865,#7691,.T.);
#11280=EDGE_CURVE('',#8865,#8866,#7692,.T.);
#11281=EDGE_CURVE('',#8866,#8852,#7693,.T.);
#11282=EDGE_CURVE('',#8840,#8864,#698,.T.);
#11283=EDGE_CURVE('',#8825,#8867,#699,.T.);
#11284=EDGE_CURVE('',#8867,#8865,#700,.T.);
#11285=EDGE_CURVE('',#8865,#8826,#7694,.T.);
#11286=EDGE_CURVE('',#8827,#8832,#701,.T.);
#11287=EDGE_CURVE('',#8833,#8836,#2568,.T.);
#11288=EDGE_CURVE('',#8827,#8862,#2569,.T.);
#11289=EDGE_CURVE('',#8868,#8868,#702,.T.);
#11290=EDGE_CURVE('',#8869,#8869,#703,.T.);
#11291=EDGE_CURVE('',#8861,#8858,#2570,.T.);
#11292=EDGE_CURVE('',#8860,#8863,#2571,.T.);
#11293=EDGE_CURVE('',#8863,#8832,#2572,.T.);
#11294=EDGE_CURVE('',#8859,#8870,#2573,.T.);
#11295=EDGE_CURVE('',#8870,#8871,#1896,.T.);
#11296=EDGE_CURVE('',#8871,#8860,#2574,.T.);
#11297=EDGE_CURVE('',#8840,#8871,#2575,.T.);
#11298=EDGE_CURVE('',#8870,#8864,#2576,.T.);
#11299=EDGE_CURVE('',#8856,#8870,#2577,.T.);
#11300=EDGE_CURVE('',#8872,#8872,#704,.T.);
#11301=EDGE_CURVE('',#8872,#8873,#705,.T.);
#11302=EDGE_CURVE('',#8873,#8873,#706,.T.);
#11303=EDGE_CURVE('',#8874,#8874,#707,.T.);
#11304=EDGE_CURVE('',#8874,#8872,#2578,.T.);
#11305=EDGE_CURVE('',#8875,#8875,#708,.T.);
#11306=EDGE_CURVE('',#8875,#8876,#709,.T.);
#11307=EDGE_CURVE('',#8876,#8876,#710,.T.);
#11308=EDGE_CURVE('',#8877,#8877,#711,.T.);
#11309=EDGE_CURVE('',#8876,#8878,#2579,.T.);
#11310=EDGE_CURVE('',#8879,#8878,#712,.T.);
#11311=EDGE_CURVE('',#8852,#8879,#713,.T.);
#11312=EDGE_CURVE('',#8880,#8825,#714,.T.);
#11313=EDGE_CURVE('',#8881,#8880,#715,.T.);
#11314=EDGE_CURVE('',#8882,#8881,#716,.T.);
#11315=EDGE_CURVE('',#8878,#8882,#717,.T.);
#11316=EDGE_CURVE('',#8883,#8883,#718,.T.);
#11317=EDGE_CURVE('',#8883,#8877,#719,.T.);
#11318=EDGE_CURVE('',#8869,#8884,#720,.T.);
#11319=EDGE_CURVE('',#8884,#8885,#721,.T.);
#11320=EDGE_CURVE('',#8885,#8884,#722,.T.);
#11321=EDGE_CURVE('',#8885,#8886,#2580,.T.);
#11322=EDGE_CURVE('',#8886,#8886,#723,.T.);
#11323=EDGE_CURVE('',#8868,#8887,#724,.T.);
#11324=EDGE_CURVE('',#8887,#8888,#725,.T.);
#11325=EDGE_CURVE('',#8888,#8887,#726,.T.);
#11326=EDGE_CURVE('',#8888,#8889,#2581,.T.);
#11327=EDGE_CURVE('',#8889,#8889,#727,.T.);
#11328=EDGE_CURVE('',#8890,#8891,#2582,.T.);
#11329=EDGE_CURVE('',#8891,#8892,#1897,.T.);
#11330=EDGE_CURVE('',#8892,#8893,#2583,.T.);
#11331=EDGE_CURVE('',#8893,#8890,#1898,.T.);
#11332=EDGE_CURVE('',#8879,#8894,#7695,.F.);
#11333=EDGE_CURVE('',#8894,#8892,#2584,.T.);
#11334=EDGE_CURVE('',#8891,#8879,#2585,.T.);
#11335=EDGE_CURVE('',#8882,#8895,#7696,.T.);
#11336=EDGE_CURVE('',#8882,#8890,#2586,.T.);
#11337=EDGE_CURVE('',#8893,#8895,#2587,.T.);
#11338=EDGE_CURVE('',#8895,#8894,#728,.T.);
#11339=EDGE_CURVE('',#8880,#8896,#7697,.F.);
#11340=EDGE_CURVE('',#8896,#8897,#729,.T.);
#11341=EDGE_CURVE('',#8881,#8897,#7698,.T.);
#11342=EDGE_CURVE('',#8898,#8881,#2588,.T.);
#11343=EDGE_CURVE('',#8899,#8898,#2589,.T.);
#11344=EDGE_CURVE('',#8880,#8899,#2590,.T.);
#11345=EDGE_CURVE('',#8899,#8900,#1899,.T.);
#11346=EDGE_CURVE('',#8900,#8896,#2591,.T.);
#11347=EDGE_CURVE('',#8897,#8901,#2592,.T.);
#11348=EDGE_CURVE('',#8901,#8898,#1900,.T.);
#11349=EDGE_CURVE('',#8901,#8900,#2593,.T.);
#11350=EDGE_CURVE('',#8902,#8902,#730,.T.);
#11351=EDGE_CURVE('',#8902,#8903,#731,.T.);
#11352=EDGE_CURVE('',#8903,#8903,#732,.T.);
#11353=EDGE_CURVE('',#8904,#8904,#733,.T.);
#11354=EDGE_CURVE('',#8905,#8905,#734,.T.);
#11355=EDGE_CURVE('',#8905,#8904,#735,.T.);
#11356=EDGE_CURVE('',#8906,#8906,#736,.T.);
#11357=EDGE_CURVE('',#8906,#8907,#737,.T.);
#11358=EDGE_CURVE('',#8907,#8907,#738,.T.);
#11359=EDGE_CURVE('',#8908,#8908,#739,.T.);
#11360=EDGE_CURVE('',#8909,#8909,#740,.T.);
#11361=EDGE_CURVE('',#8909,#8908,#741,.T.);
#11362=EDGE_CURVE('',#8910,#8910,#742,.T.);
#11363=EDGE_CURVE('',#8910,#8911,#743,.T.);
#11364=EDGE_CURVE('',#8911,#8911,#744,.T.);
#11365=EDGE_CURVE('',#8912,#8912,#745,.T.);
#11366=EDGE_CURVE('',#8913,#8913,#746,.T.);
#11367=EDGE_CURVE('',#8913,#8914,#2594,.T.);
#11368=EDGE_CURVE('',#8914,#8914,#747,.T.);
#11369=EDGE_CURVE('',#8913,#8912,#2595,.T.);
#11370=EDGE_CURVE('',#8915,#8916,#748,.T.);
#11371=EDGE_CURVE('',#8916,#8917,#2596,.T.);
#11372=EDGE_CURVE('',#8917,#8917,#749,.T.);
#11373=EDGE_CURVE('',#8916,#8915,#750,.T.);
#11374=EDGE_CURVE('',#8918,#8919,#751,.T.);
#11375=EDGE_CURVE('',#8919,#8918,#752,.T.);
#11376=EDGE_CURVE('',#8919,#8915,#2597,.T.);
#11377=EDGE_CURVE('',#8920,#8920,#753,.T.);
#11378=EDGE_CURVE('',#8918,#8921,#2598,.T.);
#11379=EDGE_CURVE('',#8921,#8921,#754,.T.);
#11380=EDGE_CURVE('',#8922,#8923,#755,.T.);
#11381=EDGE_CURVE('',#8923,#8924,#2599,.T.);
#11382=EDGE_CURVE('',#8924,#8925,#2600,.T.);
#11383=EDGE_CURVE('',#8925,#8926,#2601,.T.);
#11384=EDGE_CURVE('',#8926,#8927,#756,.T.);
#11385=EDGE_CURVE('',#8927,#8928,#2602,.T.);
#11386=EDGE_CURVE('',#8928,#8929,#2603,.T.);
#11387=EDGE_CURVE('',#8929,#8930,#2604,.T.);
#11388=EDGE_CURVE('',#8930,#8931,#757,.T.);
#11389=EDGE_CURVE('',#8931,#8932,#2605,.T.);
#11390=EDGE_CURVE('',#8932,#8933,#2606,.T.);
#11391=EDGE_CURVE('',#8933,#8934,#2607,.T.);
#11392=EDGE_CURVE('',#8934,#8935,#758,.T.);
#11393=EDGE_CURVE('',#8935,#8936,#2608,.T.);
#11394=EDGE_CURVE('',#8936,#8937,#2609,.T.);
#11395=EDGE_CURVE('',#8937,#8938,#2610,.T.);
#11396=EDGE_CURVE('',#8938,#8939,#759,.T.);
#11397=EDGE_CURVE('',#8939,#8940,#2611,.T.);
#11398=EDGE_CURVE('',#8940,#8941,#2612,.T.);
#11399=EDGE_CURVE('',#8941,#8942,#2613,.T.);
#11400=EDGE_CURVE('',#8942,#8943,#760,.T.);
#11401=EDGE_CURVE('',#8943,#8944,#2614,.T.);
#11402=EDGE_CURVE('',#8944,#8945,#2615,.T.);
#11403=EDGE_CURVE('',#8945,#8946,#2616,.T.);
#11404=EDGE_CURVE('',#8946,#8947,#761,.T.);
#11405=EDGE_CURVE('',#8947,#8948,#2617,.T.);
#11406=EDGE_CURVE('',#8948,#8949,#2618,.T.);
#11407=EDGE_CURVE('',#8949,#8950,#2619,.T.);
#11408=EDGE_CURVE('',#8950,#8951,#762,.T.);
#11409=EDGE_CURVE('',#8951,#8952,#2620,.T.);
#11410=EDGE_CURVE('',#8952,#8953,#2621,.T.);
#11411=EDGE_CURVE('',#8953,#8954,#2622,.T.);
#11412=EDGE_CURVE('',#8954,#8955,#763,.T.);
#11413=EDGE_CURVE('',#8955,#8956,#2623,.T.);
#11414=EDGE_CURVE('',#8956,#8957,#2624,.T.);
#11415=EDGE_CURVE('',#8957,#8958,#2625,.T.);
#11416=EDGE_CURVE('',#8958,#8959,#764,.T.);
#11417=EDGE_CURVE('',#8959,#8960,#2626,.T.);
#11418=EDGE_CURVE('',#8960,#8961,#2627,.T.);
#11419=EDGE_CURVE('',#8961,#8962,#2628,.T.);
#11420=EDGE_CURVE('',#8962,#8963,#765,.T.);
#11421=EDGE_CURVE('',#8963,#8964,#2629,.T.);
#11422=EDGE_CURVE('',#8964,#8965,#2630,.T.);
#11423=EDGE_CURVE('',#8965,#8966,#2631,.T.);
#11424=EDGE_CURVE('',#8966,#8967,#766,.T.);
#11425=EDGE_CURVE('',#8967,#8968,#2632,.T.);
#11426=EDGE_CURVE('',#8968,#8969,#2633,.T.);
#11427=EDGE_CURVE('',#8969,#8970,#2634,.T.);
#11428=EDGE_CURVE('',#8970,#8971,#767,.T.);
#11429=EDGE_CURVE('',#8971,#8972,#2635,.T.);
#11430=EDGE_CURVE('',#8972,#8973,#2636,.T.);
#11431=EDGE_CURVE('',#8973,#8974,#2637,.T.);
#11432=EDGE_CURVE('',#8974,#8975,#768,.T.);
#11433=EDGE_CURVE('',#8975,#8976,#2638,.T.);
#11434=EDGE_CURVE('',#8976,#8977,#2639,.T.);
#11435=EDGE_CURVE('',#8977,#8922,#2640,.T.);
#11436=EDGE_CURVE('',#8978,#8975,#2641,.T.);
#11437=EDGE_CURVE('',#8979,#8978,#2642,.T.);
#11438=EDGE_CURVE('',#8979,#8976,#2643,.T.);
#11439=EDGE_CURVE('',#8922,#8980,#2644,.T.);
#11440=EDGE_CURVE('',#8981,#8977,#2645,.T.);
#11441=EDGE_CURVE('',#8980,#8981,#2646,.T.);
#11442=EDGE_CURVE('',#8981,#8979,#2647,.T.);
#11443=EDGE_CURVE('',#8982,#8980,#769,.T.);
#11444=EDGE_CURVE('',#8982,#8923,#2648,.T.);
#11445=EDGE_CURVE('',#8983,#8982,#2649,.T.);
#11446=EDGE_CURVE('',#8983,#8924,#2650,.T.);
#11447=EDGE_CURVE('',#8926,#8984,#2651,.T.);
#11448=EDGE_CURVE('',#8985,#8925,#2652,.T.);
#11449=EDGE_CURVE('',#8984,#8985,#2653,.T.);
#11450=EDGE_CURVE('',#8985,#8983,#2654,.T.);
#11451=EDGE_CURVE('',#8986,#8984,#770,.T.);
#11452=EDGE_CURVE('',#8986,#8927,#2655,.T.);
#11453=EDGE_CURVE('',#8987,#8986,#2656,.T.);
#11454=EDGE_CURVE('',#8987,#8928,#2657,.T.);
#11455=EDGE_CURVE('',#8930,#8988,#2658,.T.);
#11456=EDGE_CURVE('',#8989,#8929,#2659,.T.);
#11457=EDGE_CURVE('',#8988,#8989,#2660,.T.);
#11458=EDGE_CURVE('',#8989,#8987,#2661,.T.);
#11459=EDGE_CURVE('',#8990,#8988,#771,.T.);
#11460=EDGE_CURVE('',#8990,#8931,#2662,.T.);
#11461=EDGE_CURVE('',#8991,#8990,#2663,.T.);
#11462=EDGE_CURVE('',#8991,#8932,#2664,.T.);
#11463=EDGE_CURVE('',#8934,#8992,#2665,.T.);
#11464=EDGE_CURVE('',#8993,#8933,#2666,.T.);
#11465=EDGE_CURVE('',#8992,#8993,#2667,.T.);
#11466=EDGE_CURVE('',#8993,#8991,#2668,.T.);
#11467=EDGE_CURVE('',#8994,#8992,#772,.T.);
#11468=EDGE_CURVE('',#8994,#8935,#2669,.T.);
#11469=EDGE_CURVE('',#8995,#8994,#2670,.T.);
#11470=EDGE_CURVE('',#8995,#8936,#2671,.T.);
#11471=EDGE_CURVE('',#8938,#8996,#2672,.T.);
#11472=EDGE_CURVE('',#8997,#8937,#2673,.T.);
#11473=EDGE_CURVE('',#8996,#8997,#2674,.T.);
#11474=EDGE_CURVE('',#8997,#8995,#2675,.T.);
#11475=EDGE_CURVE('',#8998,#8996,#773,.T.);
#11476=EDGE_CURVE('',#8998,#8939,#2676,.T.);
#11477=EDGE_CURVE('',#8999,#8998,#2677,.T.);
#11478=EDGE_CURVE('',#8999,#8940,#2678,.T.);
#11479=EDGE_CURVE('',#8942,#9000,#2679,.T.);
#11480=EDGE_CURVE('',#9001,#8941,#2680,.T.);
#11481=EDGE_CURVE('',#9000,#9001,#2681,.T.);
#11482=EDGE_CURVE('',#9001,#8999,#2682,.T.);
#11483=EDGE_CURVE('',#9002,#9000,#774,.T.);
#11484=EDGE_CURVE('',#9002,#8943,#2683,.T.);
#11485=EDGE_CURVE('',#9003,#9002,#2684,.T.);
#11486=EDGE_CURVE('',#9003,#8944,#2685,.T.);
#11487=EDGE_CURVE('',#8946,#9004,#2686,.T.);
#11488=EDGE_CURVE('',#9005,#8945,#2687,.T.);
#11489=EDGE_CURVE('',#9004,#9005,#2688,.T.);
#11490=EDGE_CURVE('',#9005,#9003,#2689,.T.);
#11491=EDGE_CURVE('',#9006,#9004,#775,.T.);
#11492=EDGE_CURVE('',#9006,#8947,#2690,.T.);
#11493=EDGE_CURVE('',#9007,#9006,#2691,.T.);
#11494=EDGE_CURVE('',#9007,#8948,#2692,.T.);
#11495=EDGE_CURVE('',#8950,#9008,#2693,.T.);
#11496=EDGE_CURVE('',#9009,#8949,#2694,.T.);
#11497=EDGE_CURVE('',#9008,#9009,#2695,.T.);
#11498=EDGE_CURVE('',#9009,#9007,#2696,.T.);
#11499=EDGE_CURVE('',#9010,#9008,#776,.T.);
#11500=EDGE_CURVE('',#9010,#8951,#2697,.T.);
#11501=EDGE_CURVE('',#9011,#9010,#2698,.T.);
#11502=EDGE_CURVE('',#9011,#8952,#2699,.T.);
#11503=EDGE_CURVE('',#8954,#9012,#2700,.T.);
#11504=EDGE_CURVE('',#9013,#8953,#2701,.T.);
#11505=EDGE_CURVE('',#9012,#9013,#2702,.T.);
#11506=EDGE_CURVE('',#9013,#9011,#2703,.T.);
#11507=EDGE_CURVE('',#9014,#9012,#777,.T.);
#11508=EDGE_CURVE('',#9014,#8955,#2704,.T.);
#11509=EDGE_CURVE('',#9015,#9014,#2705,.T.);
#11510=EDGE_CURVE('',#9015,#8956,#2706,.T.);
#11511=EDGE_CURVE('',#8958,#9016,#2707,.T.);
#11512=EDGE_CURVE('',#9017,#8957,#2708,.T.);
#11513=EDGE_CURVE('',#9016,#9017,#2709,.T.);
#11514=EDGE_CURVE('',#9017,#9015,#2710,.T.);
#11515=EDGE_CURVE('',#9018,#9016,#778,.T.);
#11516=EDGE_CURVE('',#9018,#8959,#2711,.T.);
#11517=EDGE_CURVE('',#9019,#9018,#2712,.T.);
#11518=EDGE_CURVE('',#9019,#8960,#2713,.T.);
#11519=EDGE_CURVE('',#8962,#9020,#2714,.T.);
#11520=EDGE_CURVE('',#9021,#8961,#2715,.T.);
#11521=EDGE_CURVE('',#9020,#9021,#2716,.T.);
#11522=EDGE_CURVE('',#9021,#9019,#2717,.T.);
#11523=EDGE_CURVE('',#9022,#9020,#779,.T.);
#11524=EDGE_CURVE('',#9022,#8963,#2718,.T.);
#11525=EDGE_CURVE('',#9023,#9022,#2719,.T.);
#11526=EDGE_CURVE('',#9023,#8964,#2720,.T.);
#11527=EDGE_CURVE('',#8966,#9024,#2721,.T.);
#11528=EDGE_CURVE('',#9025,#8965,#2722,.T.);
#11529=EDGE_CURVE('',#9024,#9025,#2723,.T.);
#11530=EDGE_CURVE('',#9025,#9023,#2724,.T.);
#11531=EDGE_CURVE('',#9026,#9024,#780,.T.);
#11532=EDGE_CURVE('',#9026,#8967,#2725,.T.);
#11533=EDGE_CURVE('',#9027,#9026,#2726,.T.);
#11534=EDGE_CURVE('',#9027,#8968,#2727,.T.);
#11535=EDGE_CURVE('',#8970,#9028,#2728,.T.);
#11536=EDGE_CURVE('',#9029,#8969,#2729,.T.);
#11537=EDGE_CURVE('',#9028,#9029,#2730,.T.);
#11538=EDGE_CURVE('',#9029,#9027,#2731,.T.);
#11539=EDGE_CURVE('',#9030,#9028,#781,.T.);
#11540=EDGE_CURVE('',#9030,#8971,#2732,.T.);
#11541=EDGE_CURVE('',#8974,#9031,#2733,.T.);
#11542=EDGE_CURVE('',#9032,#8973,#2734,.T.);
#11543=EDGE_CURVE('',#9031,#9032,#2735,.T.);
#11544=EDGE_CURVE('',#9033,#9030,#2736,.T.);
#11545=EDGE_CURVE('',#9033,#8972,#2737,.T.);
#11546=EDGE_CURVE('',#9032,#9033,#2738,.T.);
#11547=EDGE_CURVE('',#8978,#9031,#782,.T.);
#11548=EDGE_CURVE('',#9034,#9034,#783,.T.);
#11549=EDGE_CURVE('',#8920,#9034,#2739,.T.);
#11550=EDGE_CURVE('',#9035,#9036,#2740,.T.);
#11551=EDGE_CURVE('',#9037,#9035,#7699,.T.);
#11552=EDGE_CURVE('',#9038,#9037,#784,.T.);
#11553=EDGE_CURVE('',#9038,#9036,#7700,.T.);
#11554=EDGE_CURVE('',#9039,#9040,#2741,.T.);
#11555=EDGE_CURVE('',#9041,#9039,#7701,.T.);
#11556=EDGE_CURVE('',#9035,#9041,#7702,.T.);
#11557=EDGE_CURVE('',#9036,#9042,#7703,.T.);
#11558=EDGE_CURVE('',#9042,#9040,#7704,.T.);
#11559=EDGE_CURVE('',#9043,#9044,#2742,.T.);
#11560=EDGE_CURVE('',#9045,#9043,#7705,.T.);
#11561=EDGE_CURVE('',#9039,#9045,#7706,.T.);
#11562=EDGE_CURVE('',#9040,#9046,#7707,.T.);
#11563=EDGE_CURVE('',#9046,#9044,#7708,.T.);
#11564=EDGE_CURVE('',#9047,#9048,#2743,.T.);
#11565=EDGE_CURVE('',#9049,#9047,#7709,.T.);
#11566=EDGE_CURVE('',#9043,#9049,#7710,.T.);
#11567=EDGE_CURVE('',#9044,#9050,#7711,.T.);
#11568=EDGE_CURVE('',#9050,#9048,#7712,.T.);
#11569=EDGE_CURVE('',#9051,#9052,#2744,.T.);
#11570=EDGE_CURVE('',#9053,#9051,#7713,.T.);
#11571=EDGE_CURVE('',#9047,#9053,#7714,.T.);
#11572=EDGE_CURVE('',#9048,#9052,#7715,.T.);
#11573=EDGE_CURVE('',#9054,#9055,#2745,.T.);
#11574=EDGE_CURVE('',#9056,#9054,#7716,.T.);
#11575=EDGE_CURVE('',#9051,#9056,#7717,.T.);
#11576=EDGE_CURVE('',#9052,#9057,#7718,.T.);
#11577=EDGE_CURVE('',#9057,#9055,#7719,.T.);
#11578=EDGE_CURVE('',#9058,#9059,#2746,.T.);
#11579=EDGE_CURVE('',#9060,#9058,#7720,.T.);
#11580=EDGE_CURVE('',#9054,#9060,#7721,.T.);
#11581=EDGE_CURVE('',#9055,#9059,#7722,.T.);
#11582=EDGE_CURVE('',#9061,#9062,#2747,.T.);
#11583=EDGE_CURVE('',#9063,#9061,#7723,.T.);
#11584=EDGE_CURVE('',#9058,#9063,#7724,.T.);
#11585=EDGE_CURVE('',#9059,#9064,#7725,.T.);
#11586=EDGE_CURVE('',#9064,#9062,#7726,.T.);
#11587=EDGE_CURVE('',#9065,#9066,#2748,.T.);
#11588=EDGE_CURVE('',#9067,#9065,#7727,.T.);
#11589=EDGE_CURVE('',#9061,#9067,#7728,.T.);
#11590=EDGE_CURVE('',#9062,#9066,#7729,.T.);
#11591=EDGE_CURVE('',#9068,#9069,#2749,.T.);
#11592=EDGE_CURVE('',#9070,#9068,#7730,.T.);
#11593=EDGE_CURVE('',#9065,#9070,#7731,.T.);
#11594=EDGE_CURVE('',#9066,#9071,#7732,.T.);
#11595=EDGE_CURVE('',#9071,#9069,#7733,.T.);
#11596=EDGE_CURVE('',#9072,#9073,#2750,.T.);
#11597=EDGE_CURVE('',#9074,#9072,#7734,.T.);
#11598=EDGE_CURVE('',#9068,#9074,#7735,.T.);
#11599=EDGE_CURVE('',#9069,#9073,#7736,.T.);
#11600=EDGE_CURVE('',#9075,#9076,#2751,.T.);
#11601=EDGE_CURVE('',#9077,#9075,#7737,.T.);
#11602=EDGE_CURVE('',#9072,#9077,#7738,.T.);
#11603=EDGE_CURVE('',#9073,#9078,#7739,.T.);
#11604=EDGE_CURVE('',#9078,#9076,#7740,.T.);
#11605=EDGE_CURVE('',#9079,#9080,#2752,.T.);
#11606=EDGE_CURVE('',#9081,#9079,#7741,.T.);
#11607=EDGE_CURVE('',#9075,#9081,#7742,.T.);
#11608=EDGE_CURVE('',#9076,#9080,#7743,.T.);
#11609=EDGE_CURVE('',#9082,#9083,#2753,.T.);
#11610=EDGE_CURVE('',#9084,#9082,#7744,.T.);
#11611=EDGE_CURVE('',#9079,#9084,#7745,.T.);
#11612=EDGE_CURVE('',#9080,#9085,#7746,.T.);
#11613=EDGE_CURVE('',#9085,#9083,#7747,.T.);
#11614=EDGE_CURVE('',#9086,#9087,#2754,.T.);
#11615=EDGE_CURVE('',#9088,#9086,#7748,.T.);
#11616=EDGE_CURVE('',#9082,#9088,#7749,.T.);
#11617=EDGE_CURVE('',#9083,#9087,#7750,.T.);
#11618=EDGE_CURVE('',#9089,#9090,#2755,.T.);
#11619=EDGE_CURVE('',#9091,#9089,#7751,.T.);
#11620=EDGE_CURVE('',#9086,#9091,#7752,.T.);
#11621=EDGE_CURVE('',#9087,#9092,#7753,.T.);
#11622=EDGE_CURVE('',#9092,#9090,#7754,.T.);
#11623=EDGE_CURVE('',#9093,#9094,#2756,.T.);
#11624=EDGE_CURVE('',#9095,#9093,#7755,.T.);
#11625=EDGE_CURVE('',#9089,#9095,#7756,.T.);
#11626=EDGE_CURVE('',#9090,#9094,#7757,.T.);
#11627=EDGE_CURVE('',#9096,#9097,#2757,.T.);
#11628=EDGE_CURVE('',#9098,#9096,#7758,.T.);
#11629=EDGE_CURVE('',#9093,#9098,#7759,.T.);
#11630=EDGE_CURVE('',#9094,#9099,#7760,.T.);
#11631=EDGE_CURVE('',#9099,#9097,#7761,.T.);
#11632=EDGE_CURVE('',#9100,#9101,#2758,.T.);
#11633=EDGE_CURVE('',#9102,#9100,#7762,.T.);
#11634=EDGE_CURVE('',#9096,#9102,#7763,.T.);
#11635=EDGE_CURVE('',#9097,#9101,#7764,.T.);
#11636=EDGE_CURVE('',#9103,#9104,#2759,.T.);
#11637=EDGE_CURVE('',#9105,#9103,#7765,.T.);
#11638=EDGE_CURVE('',#9100,#9105,#7766,.T.);
#11639=EDGE_CURVE('',#9101,#9106,#7767,.T.);
#11640=EDGE_CURVE('',#9106,#9104,#7768,.T.);
#11641=EDGE_CURVE('',#9107,#9108,#2760,.T.);
#11642=EDGE_CURVE('',#9109,#9107,#7769,.T.);
#11643=EDGE_CURVE('',#9103,#9109,#7770,.T.);
#11644=EDGE_CURVE('',#9104,#9108,#7771,.T.);
#11645=EDGE_CURVE('',#9110,#9111,#2761,.T.);
#11646=EDGE_CURVE('',#9112,#9110,#7772,.T.);
#11647=EDGE_CURVE('',#9107,#9112,#7773,.T.);
#11648=EDGE_CURVE('',#9108,#9113,#7774,.T.);
#11649=EDGE_CURVE('',#9113,#9111,#7775,.T.);
#11650=EDGE_CURVE('',#9114,#9115,#2762,.T.);
#11651=EDGE_CURVE('',#9116,#9114,#7776,.T.);
#11652=EDGE_CURVE('',#9110,#9116,#7777,.T.);
#11653=EDGE_CURVE('',#9111,#9115,#7778,.T.);
#11654=EDGE_CURVE('',#9117,#9118,#2763,.T.);
#11655=EDGE_CURVE('',#9119,#9117,#7779,.T.);
#11656=EDGE_CURVE('',#9114,#9119,#7780,.T.);
#11657=EDGE_CURVE('',#9115,#9120,#7781,.T.);
#11658=EDGE_CURVE('',#9120,#9118,#7782,.T.);
#11659=EDGE_CURVE('',#9121,#9122,#2764,.T.);
#11660=EDGE_CURVE('',#9123,#9121,#7783,.T.);
#11661=EDGE_CURVE('',#9117,#9123,#7784,.T.);
#11662=EDGE_CURVE('',#9118,#9124,#7785,.T.);
#11663=EDGE_CURVE('',#9124,#9122,#7786,.T.);
#11664=EDGE_CURVE('',#9125,#9126,#2765,.T.);
#11665=EDGE_CURVE('',#9127,#9125,#7787,.T.);
#11666=EDGE_CURVE('',#9121,#9127,#7788,.T.);
#11667=EDGE_CURVE('',#9122,#9126,#7789,.T.);
#11668=EDGE_CURVE('',#9128,#9129,#2766,.T.);
#11669=EDGE_CURVE('',#9130,#9128,#7790,.T.);
#11670=EDGE_CURVE('',#9125,#9130,#7791,.T.);
#11671=EDGE_CURVE('',#9126,#9131,#7792,.T.);
#11672=EDGE_CURVE('',#9131,#9129,#7793,.T.);
#11673=EDGE_CURVE('',#9132,#9133,#2767,.T.);
#11674=EDGE_CURVE('',#9134,#9132,#7794,.T.);
#11675=EDGE_CURVE('',#9128,#9134,#7795,.T.);
#11676=EDGE_CURVE('',#9129,#9133,#7796,.T.);
#11677=EDGE_CURVE('',#9135,#9136,#2768,.T.);
#11678=EDGE_CURVE('',#9137,#9135,#7797,.T.);
#11679=EDGE_CURVE('',#9132,#9137,#7798,.T.);
#11680=EDGE_CURVE('',#9133,#9138,#7799,.T.);
#11681=EDGE_CURVE('',#9138,#9136,#7800,.T.);
#11682=EDGE_CURVE('',#9139,#9140,#2769,.T.);
#11683=EDGE_CURVE('',#9141,#9139,#7801,.T.);
#11684=EDGE_CURVE('',#9135,#9141,#7802,.T.);
#11685=EDGE_CURVE('',#9136,#9140,#7803,.T.);
#11686=EDGE_CURVE('',#9142,#9143,#2770,.T.);
#11687=EDGE_CURVE('',#9144,#9142,#7804,.T.);
#11688=EDGE_CURVE('',#9139,#9144,#7805,.T.);
#11689=EDGE_CURVE('',#9140,#9145,#7806,.T.);
#11690=EDGE_CURVE('',#9145,#9143,#7807,.T.);
#11691=EDGE_CURVE('',#9146,#9147,#2771,.T.);
#11692=EDGE_CURVE('',#9148,#9146,#7808,.T.);
#11693=EDGE_CURVE('',#9142,#9148,#7809,.T.);
#11694=EDGE_CURVE('',#9143,#9149,#7810,.T.);
#11695=EDGE_CURVE('',#9149,#9147,#7811,.T.);
#11696=EDGE_CURVE('',#9150,#9151,#2772,.T.);
#11697=EDGE_CURVE('',#9152,#9150,#7812,.T.);
#11698=EDGE_CURVE('',#9146,#9152,#7813,.T.);
#11699=EDGE_CURVE('',#9147,#9151,#7814,.T.);
#11700=EDGE_CURVE('',#9153,#9154,#2773,.T.);
#11701=EDGE_CURVE('',#9155,#9153,#7815,.T.);
#11702=EDGE_CURVE('',#9150,#9155,#7816,.T.);
#11703=EDGE_CURVE('',#9151,#9156,#7817,.T.);
#11704=EDGE_CURVE('',#9156,#9154,#7818,.T.);
#11705=EDGE_CURVE('',#9157,#9158,#2774,.T.);
#11706=EDGE_CURVE('',#9159,#9157,#7819,.T.);
#11707=EDGE_CURVE('',#9153,#9159,#7820,.T.);
#11708=EDGE_CURVE('',#9154,#9158,#7821,.T.);
#11709=EDGE_CURVE('',#9160,#9161,#2775,.T.);
#11710=EDGE_CURVE('',#9162,#9160,#7822,.T.);
#11711=EDGE_CURVE('',#9157,#9162,#7823,.T.);
#11712=EDGE_CURVE('',#9158,#9163,#7824,.T.);
#11713=EDGE_CURVE('',#9163,#9161,#7825,.T.);
#11714=EDGE_CURVE('',#9164,#9165,#2776,.T.);
#11715=EDGE_CURVE('',#9166,#9164,#7826,.T.);
#11716=EDGE_CURVE('',#9160,#9166,#7827,.T.);
#11717=EDGE_CURVE('',#9161,#9167,#7828,.T.);
#11718=EDGE_CURVE('',#9167,#9165,#7829,.T.);
#11719=EDGE_CURVE('',#9168,#9169,#2777,.T.);
#11720=EDGE_CURVE('',#9170,#9168,#7830,.T.);
#11721=EDGE_CURVE('',#9164,#9170,#7831,.T.);
#11722=EDGE_CURVE('',#9165,#9171,#7832,.T.);
#11723=EDGE_CURVE('',#9171,#9169,#7833,.T.);
#11724=EDGE_CURVE('',#9172,#9173,#2778,.T.);
#11725=EDGE_CURVE('',#9174,#9172,#7834,.T.);
#11726=EDGE_CURVE('',#9168,#9174,#7835,.T.);
#11727=EDGE_CURVE('',#9169,#9175,#7836,.T.);
#11728=EDGE_CURVE('',#9175,#9173,#7837,.T.);
#11729=EDGE_CURVE('',#9176,#9177,#7838,.T.);
#11730=EDGE_CURVE('',#9177,#9178,#785,.T.);
#11731=EDGE_CURVE('',#9178,#9179,#7839,.T.);
#11732=EDGE_CURVE('',#9179,#9180,#7840,.T.);
#11733=EDGE_CURVE('',#9180,#9181,#7841,.T.);
#11734=EDGE_CURVE('',#9181,#9182,#7842,.T.);
#11735=EDGE_CURVE('',#9182,#9183,#7843,.T.);
#11736=EDGE_CURVE('',#9183,#9184,#7844,.T.);
#11737=EDGE_CURVE('',#9184,#9185,#7845,.T.);
#11738=EDGE_CURVE('',#9185,#9186,#7846,.T.);
#11739=EDGE_CURVE('',#9186,#9187,#7847,.T.);
#11740=EDGE_CURVE('',#9187,#9188,#7848,.T.);
#11741=EDGE_CURVE('',#9188,#9189,#7849,.T.);
#11742=EDGE_CURVE('',#9189,#9190,#7850,.T.);
#11743=EDGE_CURVE('',#9190,#9191,#7851,.T.);
#11744=EDGE_CURVE('',#9191,#9192,#7852,.T.);
#11745=EDGE_CURVE('',#9192,#9193,#7853,.T.);
#11746=EDGE_CURVE('',#9193,#9194,#7854,.T.);
#11747=EDGE_CURVE('',#9194,#9195,#7855,.T.);
#11748=EDGE_CURVE('',#9195,#9196,#7856,.T.);
#11749=EDGE_CURVE('',#9196,#9197,#7857,.T.);
#11750=EDGE_CURVE('',#9197,#9198,#7858,.T.);
#11751=EDGE_CURVE('',#9198,#9199,#7859,.T.);
#11752=EDGE_CURVE('',#9199,#9200,#7860,.T.);
#11753=EDGE_CURVE('',#9200,#9201,#7861,.T.);
#11754=EDGE_CURVE('',#9201,#9202,#7862,.T.);
#11755=EDGE_CURVE('',#9202,#9203,#7863,.T.);
#11756=EDGE_CURVE('',#9203,#9204,#7864,.T.);
#11757=EDGE_CURVE('',#9204,#9205,#7865,.T.);
#11758=EDGE_CURVE('',#9205,#9206,#7866,.T.);
#11759=EDGE_CURVE('',#9206,#9207,#7867,.T.);
#11760=EDGE_CURVE('',#9207,#9208,#7868,.T.);
#11761=EDGE_CURVE('',#9208,#9209,#7869,.T.);
#11762=EDGE_CURVE('',#9209,#9210,#7870,.T.);
#11763=EDGE_CURVE('',#9210,#9211,#7871,.T.);
#11764=EDGE_CURVE('',#9211,#9212,#7872,.T.);
#11765=EDGE_CURVE('',#9212,#9213,#7873,.T.);
#11766=EDGE_CURVE('',#9213,#9214,#7874,.T.);
#11767=EDGE_CURVE('',#9214,#9215,#7875,.T.);
#11768=EDGE_CURVE('',#9215,#9216,#7876,.T.);
#11769=EDGE_CURVE('',#9216,#9217,#7877,.T.);
#11770=EDGE_CURVE('',#9217,#9218,#7878,.T.);
#11771=EDGE_CURVE('',#9219,#9218,#786,.F.);
#11772=EDGE_CURVE('',#9219,#9220,#7879,.T.);
#11773=EDGE_CURVE('',#9220,#9221,#7880,.T.);
#11774=EDGE_CURVE('',#9221,#9222,#7881,.T.);
#11775=EDGE_CURVE('',#9222,#9223,#7882,.T.);
#11776=EDGE_CURVE('',#9223,#9224,#7883,.T.);
#11777=EDGE_CURVE('',#9224,#9225,#7884,.T.);
#11778=EDGE_CURVE('',#9225,#9226,#7885,.T.);
#11779=EDGE_CURVE('',#9226,#9227,#7886,.T.);
#11780=EDGE_CURVE('',#9227,#9228,#7887,.T.);
#11781=EDGE_CURVE('',#9228,#9229,#7888,.T.);
#11782=EDGE_CURVE('',#9229,#9230,#7889,.T.);
#11783=EDGE_CURVE('',#9230,#9231,#7890,.T.);
#11784=EDGE_CURVE('',#9231,#9232,#7891,.T.);
#11785=EDGE_CURVE('',#9232,#9233,#7892,.T.);
#11786=EDGE_CURVE('',#9233,#9234,#7893,.T.);
#11787=EDGE_CURVE('',#9234,#9235,#7894,.T.);
#11788=EDGE_CURVE('',#9235,#9236,#7895,.T.);
#11789=EDGE_CURVE('',#9236,#9237,#7896,.T.);
#11790=EDGE_CURVE('',#9237,#9238,#7897,.T.);
#11791=EDGE_CURVE('',#9238,#9239,#7898,.T.);
#11792=EDGE_CURVE('',#9239,#9240,#7899,.T.);
#11793=EDGE_CURVE('',#9240,#9241,#7900,.T.);
#11794=EDGE_CURVE('',#9241,#9242,#7901,.T.);
#11795=EDGE_CURVE('',#9242,#9243,#7902,.T.);
#11796=EDGE_CURVE('',#9243,#9244,#7903,.T.);
#11797=EDGE_CURVE('',#9244,#9245,#7904,.T.);
#11798=EDGE_CURVE('',#9245,#9246,#7905,.T.);
#11799=EDGE_CURVE('',#9246,#9247,#7906,.T.);
#11800=EDGE_CURVE('',#9247,#9248,#7907,.T.);
#11801=EDGE_CURVE('',#9248,#9249,#7908,.T.);
#11802=EDGE_CURVE('',#9249,#9250,#7909,.T.);
#11803=EDGE_CURVE('',#9250,#9251,#7910,.T.);
#11804=EDGE_CURVE('',#9251,#9252,#7911,.T.);
#11805=EDGE_CURVE('',#9252,#9253,#7912,.T.);
#11806=EDGE_CURVE('',#9253,#9254,#7913,.T.);
#11807=EDGE_CURVE('',#9254,#9255,#7914,.T.);
#11808=EDGE_CURVE('',#9255,#9256,#7915,.T.);
#11809=EDGE_CURVE('',#9256,#9257,#7916,.T.);
#11810=EDGE_CURVE('',#9257,#9176,#7917,.T.);
#11811=EDGE_CURVE('',#9173,#9258,#7918,.T.);
#11812=EDGE_CURVE('',#9258,#9259,#7919,.T.);
#11813=EDGE_CURVE('',#9260,#9259,#787,.T.);
#11814=EDGE_CURVE('',#9261,#9260,#7920,.T.);
#11815=EDGE_CURVE('',#9172,#9261,#7921,.T.);
#11816=EDGE_CURVE('',#9262,#9262,#788,.T.);
#11817=EDGE_CURVE('',#9262,#9263,#2779,.T.);
#11818=EDGE_CURVE('',#9263,#9263,#789,.T.);
#11819=EDGE_CURVE('',#9264,#9265,#790,.F.);
#11820=EDGE_CURVE('',#9264,#9260,#7922,.T.);
#11821=EDGE_CURVE('',#9259,#9219,#7923,.T.);
#11822=EDGE_CURVE('',#9265,#9219,#791,.F.);
#11823=EDGE_CURVE('',#9218,#9264,#7924,.T.);
#11824=EDGE_CURVE('',#9037,#9178,#7925,.T.);
#11825=EDGE_CURVE('',#9178,#9266,#792,.T.);
#11826=EDGE_CURVE('',#9266,#9267,#793,.T.);
#11827=EDGE_CURVE('',#9267,#9038,#7926,.T.);
#11828=EDGE_CURVE('',#9267,#9177,#7927,.T.);
#11829=EDGE_CURVE('',#9268,#9268,#794,.T.);
#11830=EDGE_CURVE('',#9266,#9268,#2780,.T.);
#11831=EDGE_CURVE('',#9265,#9269,#2781,.T.);
#11832=EDGE_CURVE('',#9269,#9269,#795,.T.);
#11833=EDGE_CURVE('',#9270,#9270,#796,.T.);
#11834=EDGE_CURVE('',#9270,#9269,#2782,.T.);
#11835=EDGE_CURVE('',#9271,#9271,#797,.T.);
#11836=EDGE_CURVE('',#9272,#9272,#798,.T.);
#11837=EDGE_CURVE('',#9272,#9271,#2783,.T.);
#11838=EDGE_CURVE('',#9273,#9273,#799,.T.);
#11839=EDGE_CURVE('',#9274,#9274,#800,.T.);
#11840=EDGE_CURVE('',#9274,#9273,#2784,.T.);
#11841=EDGE_CURVE('',#9274,#9275,#2785,.T.);
#11842=EDGE_CURVE('',#9275,#9275,#801,.T.);
#11843=EDGE_CURVE('',#9276,#9277,#7928,.T.);
#11844=EDGE_CURVE('',#9276,#9278,#802,.T.);
#11845=EDGE_CURVE('',#9278,#9279,#7929,.F.);
#11846=EDGE_CURVE('',#9279,#9277,#803,.T.);
#11847=EDGE_CURVE('',#9277,#9279,#2786,.T.);
#11848=EDGE_CURVE('',#9280,#9281,#7930,.T.);
#11849=EDGE_CURVE('',#9280,#9282,#804,.T.);
#11850=EDGE_CURVE('',#9282,#9283,#7931,.F.);
#11851=EDGE_CURVE('',#9283,#9284,#7932,.F.);
#11852=EDGE_CURVE('',#9284,#9281,#805,.T.);
#11853=EDGE_CURVE('',#9284,#9285,#2787,.T.);
#11854=EDGE_CURVE('',#9285,#9281,#2788,.T.);
#11855=EDGE_CURVE('',#9286,#9287,#806,.T.);
#11856=EDGE_CURVE('',#9288,#9287,#7933,.T.);
#11857=EDGE_CURVE('',#9289,#9288,#7934,.T.);
#11858=EDGE_CURVE('',#9289,#9290,#807,.T.);
#11859=EDGE_CURVE('',#9290,#9286,#7935,.T.);
#11860=EDGE_CURVE('',#9291,#9286,#2789,.T.);
#11861=EDGE_CURVE('',#9290,#9292,#2790,.T.);
#11862=EDGE_CURVE('',#9292,#9291,#7936,.T.);
#11863=EDGE_CURVE('',#9292,#9293,#808,.T.);
#11864=EDGE_CURVE('',#9293,#9294,#7937,.F.);
#11865=EDGE_CURVE('',#9294,#9295,#7938,.F.);
#11866=EDGE_CURVE('',#9295,#9291,#809,.T.);
#11867=EDGE_CURVE('',#9295,#9287,#2791,.T.);
#11868=EDGE_CURVE('',#9296,#9297,#7939,.T.);
#11869=EDGE_CURVE('',#9296,#9298,#810,.T.);
#11870=EDGE_CURVE('',#9298,#9299,#7940,.F.);
#11871=EDGE_CURVE('',#9299,#9300,#811,.T.);
#11872=EDGE_CURVE('',#9297,#9300,#7941,.T.);
#11873=EDGE_CURVE('',#9301,#9299,#2792,.T.);
#11874=EDGE_CURVE('',#9301,#9300,#2793,.T.);
#11875=EDGE_CURVE('',#9302,#9303,#812,.F.);
#11876=EDGE_CURVE('',#9303,#9304,#2794,.T.);
#11877=EDGE_CURVE('',#9304,#9305,#813,.F.);
#11878=EDGE_CURVE('',#9305,#9302,#2795,.T.);
#11879=EDGE_CURVE('',#9306,#9303,#2796,.T.);
#11880=EDGE_CURVE('',#9307,#9306,#2797,.T.);
#11881=EDGE_CURVE('',#9304,#9307,#2798,.T.);
#11882=EDGE_CURVE('',#9306,#9308,#1901,.F.);
#11883=EDGE_CURVE('',#9308,#9309,#2799,.T.);
#11884=EDGE_CURVE('',#9309,#9307,#814,.F.);
#11885=EDGE_CURVE('',#9310,#9308,#2800,.T.);
#11886=EDGE_CURVE('',#9311,#9310,#815,.F.);
#11887=EDGE_CURVE('',#9311,#9312,#2801,.T.);
#11888=EDGE_CURVE('',#9313,#9312,#816,.F.);
#11889=EDGE_CURVE('',#9314,#9313,#2802,.T.);
#11890=EDGE_CURVE('',#9315,#9314,#817,.T.);
#11891=EDGE_CURVE('',#9316,#9315,#2803,.T.);
#11892=EDGE_CURVE('',#9316,#9317,#818,.T.);
#11893=EDGE_CURVE('',#9317,#9318,#2804,.T.);
#11894=EDGE_CURVE('',#9319,#9318,#819,.F.);
#11895=EDGE_CURVE('',#9320,#9319,#2805,.T.);
#11896=EDGE_CURVE('',#9321,#9320,#2806,.T.);
#11897=EDGE_CURVE('',#9321,#9322,#2807,.T.);
#11898=EDGE_CURVE('',#9288,#9322,#2808,.T.);
#11899=EDGE_CURVE('',#9323,#9294,#2809,.T.);
#11900=EDGE_CURVE('',#9309,#9323,#2810,.T.);
#11901=EDGE_CURVE('',#9319,#9324,#7942,.F.);
#11902=EDGE_CURVE('',#9324,#9325,#820,.F.);
#11903=EDGE_CURVE('',#9325,#9326,#2811,.T.);
#11904=EDGE_CURVE('',#9326,#9320,#1902,.T.);
#11905=EDGE_CURVE('',#9326,#9327,#2812,.T.);
#11906=EDGE_CURVE('',#9327,#9321,#821,.F.);
#11907=EDGE_CURVE('',#9328,#9329,#2813,.T.);
#11908=EDGE_CURVE('',#9329,#9330,#1903,.T.);
#11909=EDGE_CURVE('',#9330,#9331,#7943,.T.);
#11910=EDGE_CURVE('',#9332,#9331,#1904,.T.);
#11911=EDGE_CURVE('',#9332,#9333,#2814,.T.);
#11912=EDGE_CURVE('',#9334,#9333,#7944,.T.);
#11913=EDGE_CURVE('',#9334,#9335,#2815,.T.);
#11914=EDGE_CURVE('',#9335,#9336,#1905,.F.);
#11915=EDGE_CURVE('',#9336,#9337,#1906,.T.);
#11916=EDGE_CURVE('',#9337,#9338,#2816,.T.);
#11917=EDGE_CURVE('',#9338,#9339,#1907,.T.);
#11918=EDGE_CURVE('',#9339,#9340,#2817,.T.);
#11919=EDGE_CURVE('',#9340,#9341,#1908,.T.);
#11920=EDGE_CURVE('',#9341,#9342,#2818,.T.);
#11921=EDGE_CURVE('',#9342,#9328,#1909,.T.);
#11922=EDGE_CURVE('',#9332,#9343,#2819,.T.);
#11923=EDGE_CURVE('',#9343,#9344,#2820,.T.);
#11924=EDGE_CURVE('',#9333,#9344,#2821,.T.);
#11925=EDGE_CURVE('',#9345,#9334,#1910,.F.);
#11926=EDGE_CURVE('',#9345,#9346,#2822,.T.);
#11927=EDGE_CURVE('',#9335,#9346,#2823,.T.);
#11928=EDGE_CURVE('',#9347,#9341,#2824,.T.);
#11929=EDGE_CURVE('',#9347,#9348,#822,.T.);
#11930=EDGE_CURVE('',#9348,#9342,#2825,.T.);
#11931=EDGE_CURVE('',#9349,#9337,#2826,.T.);
#11932=EDGE_CURVE('',#9350,#9349,#2827,.T.);
#11933=EDGE_CURVE('',#9351,#9350,#2828,.T.);
#11934=EDGE_CURVE('',#9351,#9352,#823,.T.);
#11935=EDGE_CURVE('',#9352,#9353,#2829,.T.);
#11936=EDGE_CURVE('',#9353,#9354,#2830,.T.);
#11937=EDGE_CURVE('',#9354,#9355,#824,.T.);
#11938=EDGE_CURVE('',#9355,#9338,#2831,.T.);
#11939=EDGE_CURVE('',#9356,#9357,#2832,.T.);
#11940=EDGE_CURVE('',#9358,#9357,#2833,.T.);
#11941=EDGE_CURVE('',#9359,#9358,#2834,.T.);
#11942=EDGE_CURVE('',#9360,#9359,#2835,.T.);
#11943=EDGE_CURVE('',#9356,#9360,#2836,.T.);
#11944=EDGE_CURVE('',#9361,#9362,#2837,.T.);
#11945=EDGE_CURVE('',#9363,#9362,#825,.T.);
#11946=EDGE_CURVE('',#9363,#9364,#2838,.T.);
#11947=EDGE_CURVE('',#9364,#9359,#826,.T.);
#11948=EDGE_CURVE('',#9358,#9361,#1911,.T.);
#11949=EDGE_CURVE('',#9331,#9362,#7945,.T.);
#11950=EDGE_CURVE('',#9365,#9330,#827,.T.);
#11951=EDGE_CURVE('',#9363,#9365,#828,.T.);
#11952=EDGE_CURVE('',#9329,#9366,#1912,.T.);
#11953=EDGE_CURVE('',#9366,#9367,#2839,.T.);
#11954=EDGE_CURVE('',#9367,#9350,#1913,.T.);
#11955=EDGE_CURVE('',#9368,#9349,#829,.T.);
#11956=EDGE_CURVE('',#9368,#9365,#2840,.T.);
#11957=EDGE_CURVE('',#9369,#9370,#830,.T.);
#11958=EDGE_CURVE('',#9370,#9324,#2841,.T.);
#11959=EDGE_CURVE('',#9318,#9369,#2842,.T.);
#11960=EDGE_CURVE('',#9371,#9369,#831,.T.);
#11961=EDGE_CURVE('',#9369,#9372,#2843,.T.);
#11962=EDGE_CURVE('',#9372,#9373,#832,.T.);
#11963=EDGE_CURVE('',#9373,#9371,#2844,.T.);
#11964=EDGE_CURVE('',#9374,#9316,#7946,.T.);
#11965=EDGE_CURVE('',#9374,#9375,#2845,.T.);
#11966=EDGE_CURVE('',#9375,#9372,#833,.T.);
#11967=EDGE_CURVE('',#9372,#9317,#2846,.T.);
#11968=EDGE_CURVE('',#9375,#9373,#834,.T.);
#11969=EDGE_CURVE('',#9371,#9370,#835,.T.);
#11970=EDGE_CURVE('',#9376,#9370,#2847,.T.);
#11971=EDGE_CURVE('',#9376,#9377,#2848,.T.);
#11972=EDGE_CURVE('',#9378,#9377,#2849,.T.);
#11973=EDGE_CURVE('',#9325,#9378,#2850,.T.);
#11974=EDGE_CURVE('',#9371,#9379,#2851,.T.);
#11975=EDGE_CURVE('',#9379,#9376,#1914,.F.);
#11976=EDGE_CURVE('',#9364,#9373,#2852,.T.);
#11977=EDGE_CURVE('',#9380,#9363,#2853,.T.);
#11978=EDGE_CURVE('',#9381,#9380,#2854,.T.);
#11979=EDGE_CURVE('',#9382,#9381,#2855,.T.);
#11980=EDGE_CURVE('',#9383,#9382,#2856,.T.);
#11981=EDGE_CURVE('',#9384,#9383,#2857,.T.);
#11982=EDGE_CURVE('',#9379,#9384,#2858,.T.);
#11983=EDGE_CURVE('',#9375,#9385,#2859,.T.);
#11984=EDGE_CURVE('',#9385,#9364,#836,.T.);
#11985=EDGE_CURVE('',#9386,#9374,#837,.F.);
#11986=EDGE_CURVE('',#9387,#9386,#2860,.T.);
#11987=EDGE_CURVE('',#9388,#9387,#2861,.T.);
#11988=EDGE_CURVE('',#9385,#9388,#2862,.T.);
#11989=EDGE_CURVE('',#9389,#9315,#838,.T.);
#11990=EDGE_CURVE('',#9314,#9390,#839,.T.);
#11991=EDGE_CURVE('',#9390,#9389,#840,.T.);
#11992=EDGE_CURVE('',#9391,#9392,#841,.F.);
#11993=EDGE_CURVE('',#9392,#9390,#2863,.T.);
#11994=EDGE_CURVE('',#9313,#9391,#7947,.F.);
#11995=EDGE_CURVE('',#9389,#9386,#2864,.T.);
#11996=EDGE_CURVE('',#9392,#9393,#2865,.T.);
#11997=EDGE_CURVE('',#9394,#9393,#842,.F.);
#11998=EDGE_CURVE('',#9395,#9394,#2866,.T.);
#11999=EDGE_CURVE('',#9390,#9395,#2867,.T.);
#12000=EDGE_CURVE('',#9396,#9397,#843,.T.);
#12001=EDGE_CURVE('',#9397,#9398,#7948,.T.);
#12002=EDGE_CURVE('',#9398,#9399,#844,.T.);
#12003=EDGE_CURVE('',#9396,#9399,#7949,.T.);
#12004=EDGE_CURVE('',#9399,#9398,#2868,.T.);
#12005=EDGE_CURVE('',#9397,#9396,#2869,.T.);
#12006=EDGE_CURVE('',#9400,#9276,#2870,.T.);
#12007=EDGE_CURVE('',#9401,#9400,#845,.T.);
#12008=EDGE_CURVE('',#9298,#9401,#2871,.T.);
#12009=EDGE_CURVE('',#9402,#9296,#7950,.F.);
#12010=EDGE_CURVE('',#9402,#9403,#846,.T.);
#12011=EDGE_CURVE('',#9293,#9403,#7951,.F.);
#12012=EDGE_CURVE('',#9292,#9399,#2872,.T.);
#12013=EDGE_CURVE('',#9398,#9290,#2873,.T.);
#12014=EDGE_CURVE('',#9404,#9289,#7952,.F.);
#12015=EDGE_CURVE('',#9404,#9405,#847,.T.);
#12016=EDGE_CURVE('',#9282,#9405,#7953,.F.);
#12017=EDGE_CURVE('',#9406,#9280,#2874,.T.);
#12018=EDGE_CURVE('',#9407,#9406,#848,.T.);
#12019=EDGE_CURVE('',#9278,#9407,#2875,.T.);
#12020=EDGE_CURVE('',#9408,#9408,#849,.T.);
#12021=EDGE_CURVE('',#9408,#9409,#850,.T.);
#12022=EDGE_CURVE('',#9409,#9410,#851,.T.);
#12023=EDGE_CURVE('',#9410,#9409,#852,.T.);
#12024=EDGE_CURVE('',#9411,#9412,#7954,.T.);
#12025=EDGE_CURVE('',#9412,#9411,#7955,.T.);
#12026=EDGE_CURVE('',#9412,#9410,#2876,.T.);
#12027=EDGE_CURVE('',#9413,#9411,#7956,.T.);
#12028=EDGE_CURVE('',#9413,#9413,#7957,.T.);
#12029=EDGE_CURVE('',#9414,#9395,#853,.T.);
#12030=EDGE_CURVE('',#9415,#9414,#7958,.T.);
#12031=EDGE_CURVE('',#9416,#9415,#854,.T.);
#12032=EDGE_CURVE('',#9389,#9416,#2877,.T.);
#12033=EDGE_CURVE('',#9417,#9417,#855,.T.);
#12034=EDGE_CURVE('',#9417,#9418,#856,.T.);
#12035=EDGE_CURVE('',#9418,#9418,#857,.T.);
#12036=EDGE_CURVE('',#9310,#9419,#7959,.T.);
#12037=EDGE_CURVE('',#9306,#9420,#2878,.T.);
#12038=EDGE_CURVE('',#9419,#9420,#858,.T.);
#12039=EDGE_CURVE('',#9421,#9422,#859,.T.);
#12040=EDGE_CURVE('',#9422,#9423,#2879,.T.);
#12041=EDGE_CURVE('',#9423,#9424,#860,.T.);
#12042=EDGE_CURVE('',#9424,#9421,#2880,.T.);
#12043=EDGE_CURVE('',#9425,#9423,#861,.T.);
#12044=EDGE_CURVE('',#9423,#9368,#2881,.T.);
#12045=EDGE_CURVE('',#9368,#9426,#862,.T.);
#12046=EDGE_CURVE('',#9426,#9425,#2882,.T.);
#12047=EDGE_CURVE('',#9425,#9424,#863,.T.);
#12048=EDGE_CURVE('',#9349,#9426,#864,.T.);
#12049=EDGE_CURVE('',#9365,#9422,#2883,.T.);
#12050=EDGE_CURVE('',#9422,#9380,#865,.T.);
#12051=EDGE_CURVE('',#9421,#9380,#866,.T.);
#12052=EDGE_CURVE('',#9427,#9367,#1915,.T.);
#12053=EDGE_CURVE('',#9427,#9428,#2884,.T.);
#12054=EDGE_CURVE('',#9428,#9429,#7960,.T.);
#12055=EDGE_CURVE('',#9429,#9351,#7961,.T.);
#12056=EDGE_CURVE('',#9430,#9366,#1916,.T.);
#12057=EDGE_CURVE('',#9430,#9427,#2885,.T.);
#12058=EDGE_CURVE('',#9328,#9431,#1917,.F.);
#12059=EDGE_CURVE('',#9431,#9430,#2886,.T.);
#12060=EDGE_CURVE('',#9356,#9336,#1918,.T.);
#12061=EDGE_CURVE('',#9432,#9360,#867,.T.);
#12062=EDGE_CURVE('',#9432,#9426,#2887,.T.);
#12063=EDGE_CURVE('',#9433,#9433,#868,.T.);
#12064=EDGE_CURVE('',#9433,#9429,#2888,.T.);
#12065=EDGE_CURVE('',#9428,#9434,#2889,.T.);
#12066=EDGE_CURVE('',#9434,#9435,#869,.T.);
#12067=EDGE_CURVE('',#9435,#9348,#2890,.T.);
#12068=EDGE_CURVE('',#9436,#9347,#7962,.T.);
#12069=EDGE_CURVE('',#9436,#9437,#2891,.T.);
#12070=EDGE_CURVE('',#9437,#9438,#870,.T.);
#12071=EDGE_CURVE('',#9438,#9355,#2892,.T.);
#12072=EDGE_CURVE('',#9354,#9439,#2893,.T.);
#12073=EDGE_CURVE('',#9439,#9440,#871,.T.);
#12074=EDGE_CURVE('',#9440,#9352,#2894,.T.);
#12075=EDGE_CURVE('',#9441,#9442,#1919,.T.);
#12076=EDGE_CURVE('',#9441,#9345,#2895,.T.);
#12077=EDGE_CURVE('',#9333,#9443,#2896,.T.);
#12078=EDGE_CURVE('',#9443,#9444,#7963,.T.);
#12079=EDGE_CURVE('',#9444,#9445,#2897,.T.);
#12080=EDGE_CURVE('',#9445,#9446,#7964,.F.);
#12081=EDGE_CURVE('',#9446,#9442,#7965,.F.);
#12082=EDGE_CURVE('',#9447,#9447,#872,.T.);
#12083=EDGE_CURVE('',#9447,#9448,#2898,.T.);
#12084=EDGE_CURVE('',#9449,#9448,#873,.T.);
#12085=EDGE_CURVE('',#9449,#9444,#2899,.T.);
#12086=EDGE_CURVE('',#9443,#9450,#2900,.T.);
#12087=EDGE_CURVE('',#9448,#9450,#874,.T.);
#12088=EDGE_CURVE('',#9383,#9451,#875,.T.);
#12089=EDGE_CURVE('',#9451,#9452,#2901,.T.);
#12090=EDGE_CURVE('',#9452,#9384,#876,.T.);
#12091=EDGE_CURVE('',#9453,#9383,#877,.T.);
#12092=EDGE_CURVE('',#9382,#9454,#1920,.F.);
#12093=EDGE_CURVE('',#9454,#9453,#2902,.T.);
#12094=EDGE_CURVE('',#9453,#9451,#878,.T.);
#12095=EDGE_CURVE('',#9455,#9452,#879,.T.);
#12096=EDGE_CURVE('',#9452,#9456,#2903,.T.);
#12097=EDGE_CURVE('',#9456,#9322,#1921,.F.);
#12098=EDGE_CURVE('',#9322,#9455,#2904,.T.);
#12099=EDGE_CURVE('',#9455,#9384,#880,.T.);
#12100=EDGE_CURVE('',#9455,#9376,#2905,.T.);
#12101=EDGE_CURVE('',#9327,#9457,#2906,.T.);
#12102=EDGE_CURVE('',#9458,#9457,#881,.F.);
#12103=EDGE_CURVE('',#9459,#9458,#2907,.T.);
#12104=EDGE_CURVE('',#9460,#9459,#2908,.T.);
#12105=EDGE_CURVE('',#9461,#9460,#2909,.T.);
#12106=EDGE_CURVE('',#9462,#9461,#882,.T.);
#12107=EDGE_CURVE('',#9463,#9462,#883,.T.);
#12108=EDGE_CURVE('',#9377,#9463,#2910,.T.);
#12109=EDGE_CURVE('',#9464,#9464,#884,.T.);
#12110=EDGE_CURVE('',#9465,#9466,#885,.T.);
#12111=EDGE_CURVE('',#9466,#9467,#886,.T.);
#12112=EDGE_CURVE('',#9467,#9468,#887,.T.);
#12113=EDGE_CURVE('',#9468,#9467,#888,.T.);
#12114=EDGE_CURVE('',#9466,#9469,#889,.T.);
#12115=EDGE_CURVE('',#9469,#9465,#7966,.T.);
#12116=EDGE_CURVE('',#9469,#9470,#2911,.T.);
#12117=EDGE_CURVE('',#9471,#9470,#1922,.F.);
#12118=EDGE_CURVE('',#9471,#9472,#2912,.T.);
#12119=EDGE_CURVE('',#9473,#9472,#890,.T.);
#12120=EDGE_CURVE('',#9473,#9465,#2913,.T.);
#12121=EDGE_CURVE('',#9474,#9474,#891,.T.);
#12122=EDGE_CURVE('',#9474,#9468,#2914,.T.);
#12123=EDGE_CURVE('',#9475,#9475,#892,.T.);
#12124=EDGE_CURVE('',#9475,#9476,#893,.T.);
#12125=EDGE_CURVE('',#9476,#9477,#894,.T.);
#12126=EDGE_CURVE('',#9477,#9476,#895,.T.);
#12127=EDGE_CURVE('',#9478,#9478,#896,.T.);
#12128=EDGE_CURVE('',#9478,#9477,#2915,.T.);
#12129=EDGE_CURVE('',#9470,#9454,#2916,.T.);
#12130=EDGE_CURVE('',#9453,#9473,#2917,.T.);
#12131=EDGE_CURVE('',#9464,#9478,#897,.T.);
#12132=EDGE_CURVE('',#9462,#9474,#898,.T.);
#12133=EDGE_CURVE('',#9461,#9463,#7967,.T.);
#12134=EDGE_CURVE('',#9479,#9460,#899,.T.);
#12135=EDGE_CURVE('',#9479,#9480,#2918,.T.);
#12136=EDGE_CURVE('',#9480,#9377,#1923,.F.);
#12137=EDGE_CURVE('',#9457,#9481,#2919,.T.);
#12138=EDGE_CURVE('',#9481,#9482,#900,.F.);
#12139=EDGE_CURVE('',#9482,#9458,#2920,.T.);
#12140=EDGE_CURVE('',#9481,#9326,#2921,.T.);
#12141=EDGE_CURVE('',#9456,#9404,#2922,.T.);
#12142=EDGE_CURVE('',#9483,#9451,#2923,.T.);
#12143=EDGE_CURVE('',#9484,#9483,#2924,.T.);
#12144=EDGE_CURVE('',#9485,#9484,#2925,.T.);
#12145=EDGE_CURVE('',#9405,#9485,#2926,.T.);
#12146=EDGE_CURVE('',#9485,#9459,#1924,.F.);
#12147=EDGE_CURVE('',#9459,#9283,#2927,.T.);
#12148=EDGE_CURVE('',#9285,#9482,#2928,.T.);
#12149=EDGE_CURVE('',#9484,#9460,#901,.T.);
#12150=EDGE_CURVE('',#9479,#9484,#902,.T.);
#12151=EDGE_CURVE('',#9483,#9472,#903,.T.);
#12152=EDGE_CURVE('',#9472,#9479,#2929,.T.);
#12153=EDGE_CURVE('',#9473,#9483,#904,.T.);
#12154=EDGE_CURVE('',#9486,#9432,#2930,.T.);
#12155=EDGE_CURVE('',#9486,#9416,#2931,.T.);
#12156=EDGE_CURVE('',#9487,#9415,#905,.T.);
#12157=EDGE_CURVE('',#9414,#9487,#906,.T.);
#12158=EDGE_CURVE('',#9488,#9394,#2932,.T.);
#12159=EDGE_CURVE('',#9489,#9488,#2933,.T.);
#12160=EDGE_CURVE('',#9489,#9490,#2934,.T.);
#12161=EDGE_CURVE('',#9491,#9490,#907,.T.);
#12162=EDGE_CURVE('',#9491,#9492,#2935,.T.);
#12163=EDGE_CURVE('',#9493,#9492,#2936,.T.);
#12164=EDGE_CURVE('',#9494,#9493,#2937,.T.);
#12165=EDGE_CURVE('',#9495,#9494,#2938,.T.);
#12166=EDGE_CURVE('',#9496,#9495,#2939,.T.);
#12167=EDGE_CURVE('',#9497,#9496,#2940,.T.);
#12168=EDGE_CURVE('',#9498,#9497,#2941,.T.);
#12169=EDGE_CURVE('',#9498,#9400,#2942,.T.);
#12170=EDGE_CURVE('',#9407,#9499,#2943,.T.);
#12171=EDGE_CURVE('',#9500,#9499,#2944,.T.);
#12172=EDGE_CURVE('',#9480,#9500,#2945,.T.);
#12173=EDGE_CURVE('',#9501,#9471,#2946,.T.);
#12174=EDGE_CURVE('',#9425,#9501,#2947,.T.);
#12175=EDGE_CURVE('',#9502,#9503,#2948,.T.);
#12176=EDGE_CURVE('',#9504,#9502,#2949,.T.);
#12177=EDGE_CURVE('',#9505,#9504,#2950,.T.);
#12178=EDGE_CURVE('',#9503,#9505,#2951,.T.);
#12179=EDGE_CURVE('',#9506,#9507,#2952,.T.);
#12180=EDGE_CURVE('',#9508,#9506,#2953,.T.);
#12181=EDGE_CURVE('',#9509,#9508,#908,.T.);
#12182=EDGE_CURVE('',#9510,#9509,#2954,.T.);
#12183=EDGE_CURVE('',#9511,#9510,#2955,.T.);
#12184=EDGE_CURVE('',#9507,#9511,#2956,.T.);
#12185=EDGE_CURVE('',#9512,#9512,#909,.T.);
#12186=EDGE_CURVE('',#9513,#9513,#910,.T.);
#12187=EDGE_CURVE('',#9381,#9514,#1925,.F.);
#12188=EDGE_CURVE('',#9514,#9454,#2957,.T.);
#12189=EDGE_CURVE('',#9421,#9514,#2958,.T.);
#12190=EDGE_CURVE('',#9515,#9516,#911,.T.);
#12191=EDGE_CURVE('',#9516,#9433,#912,.T.);
#12192=EDGE_CURVE('',#9516,#9517,#913,.T.);
#12193=EDGE_CURVE('',#9517,#9515,#7968,.T.);
#12194=EDGE_CURVE('',#9501,#9518,#1926,.F.);
#12195=EDGE_CURVE('',#9518,#9515,#2959,.T.);
#12196=EDGE_CURVE('',#9517,#9424,#2960,.T.);
#12197=EDGE_CURVE('',#9431,#9519,#2961,.T.);
#12198=EDGE_CURVE('',#9519,#9520,#2962,.T.);
#12199=EDGE_CURVE('',#9430,#9520,#2963,.T.);
#12200=EDGE_CURVE('',#9340,#9521,#1927,.F.);
#12201=EDGE_CURVE('',#9521,#9436,#2964,.T.);
#12202=EDGE_CURVE('',#9521,#9522,#2965,.T.);
#12203=EDGE_CURVE('',#9522,#9437,#2966,.T.);
#12204=EDGE_CURVE('',#9339,#9523,#1928,.F.);
#12205=EDGE_CURVE('',#9523,#9521,#2967,.T.);
#12206=EDGE_CURVE('',#9523,#9524,#2968,.T.);
#12207=EDGE_CURVE('',#9524,#9522,#2969,.T.);
#12208=EDGE_CURVE('',#9335,#9442,#2970,.T.);
#12209=EDGE_CURVE('',#9446,#9525,#1929,.F.);
#12210=EDGE_CURVE('',#9525,#9357,#1930,.T.);
#12211=EDGE_CURVE('',#9346,#9441,#2971,.T.);
#12212=EDGE_CURVE('',#9385,#9359,#914,.T.);
#12213=EDGE_CURVE('',#9361,#9525,#1931,.F.);
#12214=EDGE_CURVE('',#9445,#9332,#2972,.T.);
#12215=EDGE_CURVE('',#9388,#9360,#915,.T.);
#12216=EDGE_CURVE('',#9432,#9388,#916,.T.);
#12217=EDGE_CURVE('',#9387,#9486,#917,.F.);
#12218=EDGE_CURVE('',#9403,#9526,#2973,.T.);
#12219=EDGE_CURVE('',#9526,#9323,#1932,.F.);
#12220=EDGE_CURVE('',#9526,#9527,#2974,.T.);
#12221=EDGE_CURVE('',#9528,#9402,#2975,.T.);
#12222=EDGE_CURVE('',#9529,#9528,#2976,.T.);
#12223=EDGE_CURVE('',#9530,#9529,#2977,.T.);
#12224=EDGE_CURVE('',#9531,#9530,#2978,.T.);
#12225=EDGE_CURVE('',#9527,#9531,#2979,.T.);
#12226=EDGE_CURVE('',#9532,#9528,#1933,.F.);
#12227=EDGE_CURVE('',#9297,#9532,#2980,.T.);
#12228=EDGE_CURVE('',#9533,#9533,#918,.T.);
#12229=EDGE_CURVE('',#9533,#9534,#919,.T.);
#12230=EDGE_CURVE('',#9534,#9534,#920,.T.);
#12231=EDGE_CURVE('',#9535,#9536,#921,.T.);
#12232=EDGE_CURVE('',#9536,#9535,#922,.T.);
#12233=EDGE_CURVE('',#9536,#9534,#2981,.T.);
#12234=EDGE_CURVE('',#9537,#9538,#923,.T.);
#12235=EDGE_CURVE('',#9539,#9537,#2982,.T.);
#12236=EDGE_CURVE('',#9540,#9539,#2983,.T.);
#12237=EDGE_CURVE('',#9541,#9540,#2984,.T.);
#12238=EDGE_CURVE('',#9542,#9541,#2985,.T.);
#12239=EDGE_CURVE('',#9543,#9542,#2986,.T.);
#12240=EDGE_CURVE('',#9538,#9543,#924,.T.);
#12241=EDGE_CURVE('',#9538,#9544,#925,.T.);
#12242=EDGE_CURVE('',#9544,#9544,#926,.T.);
#12243=EDGE_CURVE('',#9543,#9537,#7969,.T.);
#12244=EDGE_CURVE('',#9542,#9494,#927,.T.);
#12245=EDGE_CURVE('',#9539,#9493,#1934,.F.);
#12246=EDGE_CURVE('',#9545,#9546,#928,.T.);
#12247=EDGE_CURVE('',#9546,#9545,#929,.T.);
#12248=EDGE_CURVE('',#9546,#9544,#2987,.T.);
#12249=EDGE_CURVE('',#9514,#9518,#2988,.T.);
#12250=EDGE_CURVE('',#9547,#9547,#930,.T.);
#12251=EDGE_CURVE('',#9470,#9518,#2989,.T.);
#12252=EDGE_CURVE('',#9500,#9378,#1935,.F.);
#12253=EDGE_CURVE('',#9499,#9548,#931,.T.);
#12254=EDGE_CURVE('',#9548,#9378,#2990,.T.);
#12255=EDGE_CURVE('',#9406,#9548,#2991,.T.);
#12256=EDGE_CURVE('',#9549,#9498,#932,.T.);
#12257=EDGE_CURVE('',#9497,#9550,#1936,.F.);
#12258=EDGE_CURVE('',#9550,#9549,#2992,.T.);
#12259=EDGE_CURVE('',#9302,#9301,#2993,.T.);
#12260=EDGE_CURVE('',#9401,#9549,#2994,.T.);
#12261=EDGE_CURVE('',#9550,#9420,#2995,.T.);
#12262=EDGE_CURVE('',#9496,#9551,#1937,.F.);
#12263=EDGE_CURVE('',#9551,#9550,#2996,.T.);
#12264=EDGE_CURVE('',#9551,#9552,#2997,.T.);
#12265=EDGE_CURVE('',#9553,#9552,#2998,.T.);
#12266=EDGE_CURVE('',#9419,#9553,#2999,.T.);
#12267=EDGE_CURVE('',#9492,#9554,#933,.F.);
#12268=EDGE_CURVE('',#9554,#9539,#3000,.T.);
#12269=EDGE_CURVE('',#9554,#9555,#3001,.T.);
#12270=EDGE_CURVE('',#9540,#9555,#3002,.T.);
#12271=EDGE_CURVE('',#9505,#9556,#1938,.F.);
#12272=EDGE_CURVE('',#9556,#9557,#3003,.T.);
#12273=EDGE_CURVE('',#9557,#9503,#1939,.F.);
#12274=EDGE_CURVE('',#9556,#9558,#3004,.T.);
#12275=EDGE_CURVE('',#9558,#9559,#3005,.T.);
#12276=EDGE_CURVE('',#9559,#9560,#934,.T.);
#12277=EDGE_CURVE('',#9560,#9561,#3006,.T.);
#12278=EDGE_CURVE('',#9557,#9561,#3007,.T.);
#12279=EDGE_CURVE('',#9502,#9562,#1940,.F.);
#12280=EDGE_CURVE('',#9562,#9563,#3008,.T.);
#12281=EDGE_CURVE('',#9563,#9504,#1941,.F.);
#12282=EDGE_CURVE('',#9562,#9564,#3009,.T.);
#12283=EDGE_CURVE('',#9564,#9565,#3010,.T.);
#12284=EDGE_CURVE('',#9565,#9566,#935,.T.);
#12285=EDGE_CURVE('',#9566,#9567,#3011,.T.);
#12286=EDGE_CURVE('',#9563,#9567,#3012,.T.);
#12287=EDGE_CURVE('',#9511,#9568,#1942,.F.);
#12288=EDGE_CURVE('',#9568,#9569,#3013,.T.);
#12289=EDGE_CURVE('',#9569,#9507,#1943,.F.);
#12290=EDGE_CURVE('',#9568,#9570,#3014,.T.);
#12291=EDGE_CURVE('',#9570,#9571,#3015,.T.);
#12292=EDGE_CURVE('',#9571,#9572,#936,.T.);
#12293=EDGE_CURVE('',#9572,#9573,#3016,.T.);
#12294=EDGE_CURVE('',#9569,#9573,#3017,.T.);
#12295=EDGE_CURVE('',#9509,#9574,#7970,.T.);
#12296=EDGE_CURVE('',#9574,#9508,#7971,.T.);
#12297=EDGE_CURVE('',#9506,#9575,#1944,.F.);
#12298=EDGE_CURVE('',#9575,#9576,#3018,.T.);
#12299=EDGE_CURVE('',#9576,#9510,#1945,.F.);
#12300=EDGE_CURVE('',#9575,#9577,#3019,.T.);
#12301=EDGE_CURVE('',#9577,#9578,#3020,.T.);
#12302=EDGE_CURVE('',#9578,#9579,#937,.T.);
#12303=EDGE_CURVE('',#9579,#9580,#3021,.T.);
#12304=EDGE_CURVE('',#9576,#9580,#3022,.T.);
#12305=EDGE_CURVE('',#9574,#9581,#938,.T.);
#12306=EDGE_CURVE('',#9581,#9582,#939,.T.);
#12307=EDGE_CURVE('',#9582,#9581,#940,.T.);
#12308=EDGE_CURVE('',#9569,#9575,#3023,.T.);
#12309=EDGE_CURVE('',#9573,#9577,#3024,.T.);
#12310=EDGE_CURVE('',#9576,#9568,#3025,.T.);
#12311=EDGE_CURVE('',#9580,#9570,#3026,.T.);
#12312=EDGE_CURVE('',#9557,#9562,#3027,.T.);
#12313=EDGE_CURVE('',#9561,#9564,#3028,.T.);
#12314=EDGE_CURVE('',#9563,#9556,#3029,.T.);
#12315=EDGE_CURVE('',#9567,#9558,#3030,.T.);
#12316=EDGE_CURVE('',#9513,#9583,#941,.T.);
#12317=EDGE_CURVE('',#9583,#9584,#942,.T.);
#12318=EDGE_CURVE('',#9584,#9583,#943,.T.);
#12319=EDGE_CURVE('',#9584,#9585,#3031,.T.);
#12320=EDGE_CURVE('',#9585,#9585,#944,.T.);
#12321=EDGE_CURVE('',#9512,#9586,#945,.T.);
#12322=EDGE_CURVE('',#9586,#9587,#946,.T.);
#12323=EDGE_CURVE('',#9587,#9586,#947,.T.);
#12324=EDGE_CURVE('',#9587,#9588,#3032,.T.);
#12325=EDGE_CURVE('',#9588,#9588,#948,.T.);
#12326=EDGE_CURVE('',#9582,#9589,#3033,.T.);
#12327=EDGE_CURVE('',#9589,#9589,#949,.T.);
#12328=EDGE_CURVE('',#9590,#9590,#950,.T.);
#12329=EDGE_CURVE('',#9590,#9487,#951,.T.);
#12330=EDGE_CURVE('',#9591,#9592,#952,.T.);
#12331=EDGE_CURVE('',#9592,#9545,#953,.T.);
#12332=EDGE_CURVE('',#9592,#9593,#954,.T.);
#12333=EDGE_CURVE('',#9593,#9591,#7972,.T.);
#12334=EDGE_CURVE('',#9593,#9551,#3034,.T.);
#12335=EDGE_CURVE('',#9594,#9495,#955,.T.);
#12336=EDGE_CURVE('',#9594,#9591,#3035,.T.);
#12337=EDGE_CURVE('',#9595,#9595,#956,.T.);
#12338=EDGE_CURVE('',#9595,#9535,#957,.T.);
#12339=EDGE_CURVE('',#9532,#9594,#3036,.T.);
#12340=EDGE_CURVE('',#9532,#9305,#3037,.T.);
#12341=EDGE_CURVE('',#9596,#9323,#3038,.T.);
#12342=EDGE_CURVE('',#9552,#9596,#3039,.T.);
#12343=EDGE_CURVE('',#9494,#9530,#958,.T.);
#12344=EDGE_CURVE('',#9529,#9495,#959,.T.);
#12345=EDGE_CURVE('',#9594,#9529,#960,.T.);
#12346=EDGE_CURVE('',#9542,#9530,#961,.T.);
#12347=EDGE_CURVE('',#9541,#9531,#962,.T.);
#12348=EDGE_CURVE('',#9596,#9597,#963,.T.);
#12349=EDGE_CURVE('',#9597,#9598,#3040,.T.);
#12350=EDGE_CURVE('',#9598,#9552,#1946,.F.);
#12351=EDGE_CURVE('',#9527,#9596,#964,.T.);
#12352=EDGE_CURVE('',#9527,#9597,#965,.T.);
#12353=EDGE_CURVE('',#9598,#9599,#3041,.T.);
#12354=EDGE_CURVE('',#9600,#9597,#3042,.T.);
#12355=EDGE_CURVE('',#9601,#9600,#3043,.T.);
#12356=EDGE_CURVE('',#9602,#9601,#3044,.T.);
#12357=EDGE_CURVE('',#9602,#9603,#3045,.T.);
#12358=EDGE_CURVE('',#9604,#9603,#966,.T.);
#12359=EDGE_CURVE('',#9604,#9605,#3046,.T.);
#12360=EDGE_CURVE('',#9606,#9605,#3047,.T.);
#12361=EDGE_CURVE('',#9607,#9606,#3048,.T.);
#12362=EDGE_CURVE('',#9599,#9607,#3049,.T.);
#12363=EDGE_CURVE('',#9600,#9531,#967,.T.);
#12364=EDGE_CURVE('',#9608,#9609,#968,.T.);
#12365=EDGE_CURVE('',#9609,#9391,#3050,.T.);
#12366=EDGE_CURVE('',#9312,#9608,#3051,.T.);
#12367=EDGE_CURVE('',#9607,#9608,#969,.T.);
#12368=EDGE_CURVE('',#9608,#9610,#3052,.T.);
#12369=EDGE_CURVE('',#9610,#9599,#970,.T.);
#12370=EDGE_CURVE('',#9553,#9610,#971,.T.);
#12371=EDGE_CURVE('',#9610,#9311,#3053,.T.);
#12372=EDGE_CURVE('',#9553,#9599,#972,.T.);
#12373=EDGE_CURVE('',#9607,#9609,#973,.T.);
#12374=EDGE_CURVE('',#9611,#9609,#3054,.T.);
#12375=EDGE_CURVE('',#9612,#9611,#3055,.T.);
#12376=EDGE_CURVE('',#9393,#9612,#3056,.T.);
#12377=EDGE_CURVE('',#9606,#9611,#974,.T.);
#12378=EDGE_CURVE('',#9600,#9541,#975,.T.);
#12379=EDGE_CURVE('',#9540,#9601,#1947,.F.);
#12380=EDGE_CURVE('',#9613,#9613,#976,.T.);
#12381=EDGE_CURVE('',#9613,#9614,#977,.T.);
#12382=EDGE_CURVE('',#9614,#9615,#978,.T.);
#12383=EDGE_CURVE('',#9615,#9614,#979,.T.);
#12384=EDGE_CURVE('',#9615,#9616,#3057,.T.);
#12385=EDGE_CURVE('',#9617,#9616,#7973,.T.);
#12386=EDGE_CURVE('',#9618,#9617,#980,.T.);
#12387=EDGE_CURVE('',#9618,#9619,#3058,.T.);
#12388=EDGE_CURVE('',#9619,#9620,#981,.T.);
#12389=EDGE_CURVE('',#9620,#9621,#3059,.T.);
#12390=EDGE_CURVE('',#9622,#9621,#982,.T.);
#12391=EDGE_CURVE('',#9623,#9622,#7974,.T.);
#12392=EDGE_CURVE('',#9623,#9624,#3060,.T.);
#12393=EDGE_CURVE('',#9624,#9625,#983,.T.);
#12394=EDGE_CURVE('',#9625,#9626,#3061,.T.);
#12395=EDGE_CURVE('',#9627,#9626,#7975,.T.);
#12396=EDGE_CURVE('',#9628,#9627,#7976,.T.);
#12397=EDGE_CURVE('',#9628,#9629,#3062,.T.);
#12398=EDGE_CURVE('',#9629,#9630,#984,.T.);
#12399=EDGE_CURVE('',#9630,#9631,#3063,.T.);
#12400=EDGE_CURVE('',#9616,#9631,#7977,.T.);
#12401=EDGE_CURVE('',#9603,#9491,#3064,.T.);
#12402=EDGE_CURVE('',#9555,#9602,#985,.F.);
#12403=EDGE_CURVE('',#9632,#9632,#986,.T.);
#12404=EDGE_CURVE('',#9633,#9634,#1948,.T.);
#12405=EDGE_CURVE('',#9634,#9617,#3065,.T.);
#12406=EDGE_CURVE('',#9631,#9635,#3066,.T.);
#12407=EDGE_CURVE('',#9635,#9633,#1949,.F.);
#12408=EDGE_CURVE('',#9630,#9636,#3067,.T.);
#12409=EDGE_CURVE('',#9635,#9636,#3068,.T.);
#12410=EDGE_CURVE('',#9637,#9634,#3069,.T.);
#12411=EDGE_CURVE('',#9622,#9637,#987,.T.);
#12412=EDGE_CURVE('',#9621,#9638,#3070,.T.);
#12413=EDGE_CURVE('',#9638,#9618,#3071,.T.);
#12414=EDGE_CURVE('',#9639,#9640,#3072,.T.);
#12415=EDGE_CURVE('',#9641,#9640,#3073,.T.);
#12416=EDGE_CURVE('',#9641,#9642,#3074,.T.);
#12417=EDGE_CURVE('',#9639,#9642,#3075,.T.);
#12418=EDGE_CURVE('',#9643,#9644,#1950,.T.);
#12419=EDGE_CURVE('',#9644,#9645,#3076,.T.);
#12420=EDGE_CURVE('',#9645,#9646,#1951,.T.);
#12421=EDGE_CURVE('',#9647,#9646,#1952,.T.);
#12422=EDGE_CURVE('',#9647,#9648,#3077,.T.);
#12423=EDGE_CURVE('',#9648,#9643,#1953,.F.);
#12424=EDGE_CURVE('',#9646,#9649,#1954,.T.);
#12425=EDGE_CURVE('',#9645,#9650,#3078,.T.);
#12426=EDGE_CURVE('',#9606,#9650,#988,.T.);
#12427=EDGE_CURVE('',#9605,#9641,#989,.T.);
#12428=EDGE_CURVE('',#9640,#9651,#1955,.T.);
#12429=EDGE_CURVE('',#9651,#9652,#1956,.T.);
#12430=EDGE_CURVE('',#9652,#9653,#3079,.T.);
#12431=EDGE_CURVE('',#9653,#9654,#1957,.T.);
#12432=EDGE_CURVE('',#9654,#9655,#3080,.T.);
#12433=EDGE_CURVE('',#9655,#9656,#1958,.T.);
#12434=EDGE_CURVE('',#9656,#9649,#3081,.T.);
#12435=EDGE_CURVE('',#9657,#9644,#3082,.T.);
#12436=EDGE_CURVE('',#9650,#9657,#3083,.T.);
#12437=EDGE_CURVE('',#9658,#9659,#3084,.T.);
#12438=EDGE_CURVE('',#9660,#9659,#3085,.T.);
#12439=EDGE_CURVE('',#9660,#9661,#3086,.T.);
#12440=EDGE_CURVE('',#9658,#9661,#3087,.T.);
#12441=EDGE_CURVE('',#9662,#9649,#3088,.T.);
#12442=EDGE_CURVE('',#9656,#9663,#3089,.T.);
#12443=EDGE_CURVE('',#9663,#9664,#990,.T.);
#12444=EDGE_CURVE('',#9662,#9664,#991,.T.);
#12445=EDGE_CURVE('',#9665,#9666,#1959,.T.);
#12446=EDGE_CURVE('',#9667,#9666,#1960,.T.);
#12447=EDGE_CURVE('',#9667,#9647,#3090,.T.);
#12448=EDGE_CURVE('',#9662,#9668,#7978,.T.);
#12449=EDGE_CURVE('',#9668,#9669,#3091,.T.);
#12450=EDGE_CURVE('',#9669,#9670,#1961,.T.);
#12451=EDGE_CURVE('',#9670,#9665,#3092,.T.);
#12452=EDGE_CURVE('',#9666,#9659,#1962,.T.);
#12453=EDGE_CURVE('',#9666,#9671,#1963,.F.);
#12454=EDGE_CURVE('',#9671,#9628,#3093,.T.);
#12455=EDGE_CURVE('',#9627,#9672,#3094,.T.);
#12456=EDGE_CURVE('',#9672,#9660,#1964,.T.);
#12457=EDGE_CURVE('',#9665,#9652,#3095,.T.);
#12458=EDGE_CURVE('',#9651,#9673,#1965,.F.);
#12459=EDGE_CURVE('',#9673,#9671,#3096,.T.);
#12460=EDGE_CURVE('',#9670,#9653,#3097,.T.);
#12461=EDGE_CURVE('',#9674,#9669,#1966,.F.);
#12462=EDGE_CURVE('',#9674,#9675,#3098,.T.);
#12463=EDGE_CURVE('',#9675,#9676,#3099,.T.);
#12464=EDGE_CURVE('',#9677,#9676,#3100,.T.);
#12465=EDGE_CURVE('',#9654,#9677,#1967,.F.);
#12466=EDGE_CURVE('',#9668,#9678,#992,.T.);
#12467=EDGE_CURVE('',#9678,#9674,#3101,.T.);
#12468=EDGE_CURVE('',#9679,#9672,#1968,.F.);
#12469=EDGE_CURVE('',#9679,#9680,#3102,.T.);
#12470=EDGE_CURVE('',#9680,#9681,#3103,.T.);
#12471=EDGE_CURVE('',#9682,#9681,#3104,.T.);
#12472=EDGE_CURVE('',#9683,#9682,#1969,.F.);
#12473=EDGE_CURVE('',#9661,#9683,#1970,.T.);
#12474=EDGE_CURVE('',#9626,#9679,#3105,.T.);
#12475=EDGE_CURVE('',#9612,#9488,#993,.T.);
#12476=EDGE_CURVE('',#9611,#9650,#994,.T.);
#12477=EDGE_CURVE('',#9657,#9612,#995,.T.);
#12478=EDGE_CURVE('',#9657,#9488,#996,.T.);
#12479=EDGE_CURVE('',#9639,#9633,#1971,.T.);
#12480=EDGE_CURVE('',#9642,#9489,#997,.T.);
#12481=EDGE_CURVE('',#9658,#9643,#1972,.T.);
#12482=EDGE_CURVE('',#9683,#9684,#3106,.T.);
#12483=EDGE_CURVE('',#9684,#9637,#7979,.T.);
#12484=EDGE_CURVE('',#9490,#9604,#3107,.T.);
#12485=EDGE_CURVE('',#9547,#9447,#998,.T.);
#12486=EDGE_CURVE('',#9450,#9685,#7980,.F.);
#12487=EDGE_CURVE('',#9685,#9686,#999,.T.);
#12488=EDGE_CURVE('',#9686,#9449,#7981,.F.);
#12489=EDGE_CURVE('',#9344,#9685,#3108,.T.);
#12490=EDGE_CURVE('',#9687,#9343,#3109,.T.);
#12491=EDGE_CURVE('',#9686,#9687,#3110,.T.);
#12492=EDGE_CURVE('',#9445,#9687,#3111,.T.);
#12493=EDGE_CURVE('',#9623,#9684,#1000,.T.);
#12494=EDGE_CURVE('',#9682,#9623,#3112,.T.);
#12495=EDGE_CURVE('',#9688,#9655,#1973,.F.);
#12496=EDGE_CURVE('',#9688,#9689,#3113,.T.);
#12497=EDGE_CURVE('',#9689,#9690,#3114,.T.);
#12498=EDGE_CURVE('',#9691,#9690,#7982,.F.);
#12499=EDGE_CURVE('',#9663,#9691,#3115,.T.);
#12500=EDGE_CURVE('',#9677,#9688,#3116,.T.);
#12501=EDGE_CURVE('',#9673,#9692,#3117,.T.);
#12502=EDGE_CURVE('',#9692,#9693,#3118,.T.);
#12503=EDGE_CURVE('',#9671,#9693,#3119,.T.);
#12504=EDGE_CURVE('',#9635,#9673,#3120,.T.);
#12505=EDGE_CURVE('',#9636,#9692,#3121,.T.);
#12506=EDGE_CURVE('',#9648,#9667,#3122,.T.);
#12507=EDGE_CURVE('',#9648,#9694,#3123,.T.);
#12508=EDGE_CURVE('',#9694,#9695,#3124,.T.);
#12509=EDGE_CURVE('',#9667,#9695,#3125,.T.);
#12510=EDGE_CURVE('',#9681,#9624,#3126,.T.);
#12511=EDGE_CURVE('',#9632,#9696,#1001,.T.);
#12512=EDGE_CURVE('',#9696,#9697,#1002,.T.);
#12513=EDGE_CURVE('',#9697,#9696,#1003,.T.);
#12514=EDGE_CURVE('',#9697,#9698,#3127,.T.);
#12515=EDGE_CURVE('',#9699,#9698,#1004,.T.);
#12516=EDGE_CURVE('',#9699,#9678,#3128,.T.);
#12517=EDGE_CURVE('',#9664,#9678,#7983,.T.);
#12518=EDGE_CURVE('',#9698,#9691,#1005,.T.);
#12519=EDGE_CURVE('',#9676,#9689,#3129,.T.);
#12520=EDGE_CURVE('',#9690,#9700,#1006,.T.);
#12521=EDGE_CURVE('',#9700,#9699,#7984,.F.);
#12522=EDGE_CURVE('',#9700,#9675,#3130,.T.);
#12523=EDGE_CURVE('',#9625,#9680,#3131,.T.);
#12524=EDGE_CURVE('',#9620,#9701,#3132,.T.);
#12525=EDGE_CURVE('',#9638,#9701,#3133,.T.);
#12526=EDGE_CURVE('',#9701,#9619,#3134,.T.);
#12527=EDGE_CURVE('',#9693,#9629,#3135,.T.);
#12528=EDGE_CURVE('',#9647,#9702,#3136,.T.);
#12529=EDGE_CURVE('',#9702,#9694,#3137,.T.);
#12530=EDGE_CURVE('',#9695,#9702,#3138,.T.);
#12531=EDGE_CURVE('',#9438,#9524,#3139,.T.);
#12532=EDGE_CURVE('',#9440,#9703,#3140,.T.);
#12533=EDGE_CURVE('',#9353,#9703,#3141,.T.);
#12534=EDGE_CURVE('',#9703,#9439,#3142,.T.);
#12535=EDGE_CURVE('',#9427,#9704,#3143,.T.);
#12536=EDGE_CURVE('',#9704,#9434,#3144,.T.);
#12537=EDGE_CURVE('',#9520,#9704,#3145,.T.);
#12538=EDGE_CURVE('',#9435,#9519,#3146,.T.);
#12539=EDGE_CURVE('',#9572,#9578,#3147,.T.);
#12540=EDGE_CURVE('',#9579,#9571,#3148,.T.);
#12541=EDGE_CURVE('',#9560,#9565,#3149,.T.);
#12542=EDGE_CURVE('',#9566,#9559,#3150,.T.);
#12543=EDGE_CURVE('',#9705,#9706,#7985,.T.);
#12544=EDGE_CURVE('',#9706,#9705,#3151,.T.);
#12545=EDGE_CURVE('',#9705,#9707,#7986,.T.);
#12546=EDGE_CURVE('',#9707,#9708,#7987,.T.);
#12547=EDGE_CURVE('',#9708,#9709,#7988,.T.);
#12548=EDGE_CURVE('',#9709,#9710,#7989,.T.);
#12549=EDGE_CURVE('',#9710,#9711,#7990,.T.);
#12550=EDGE_CURVE('',#9711,#9706,#7991,.T.);
#12551=EDGE_CURVE('',#9712,#9713,#7992,.T.);
#12552=EDGE_CURVE('',#9713,#9712,#3152,.T.);
#12553=EDGE_CURVE('',#9714,#9712,#7993,.T.);
#12554=EDGE_CURVE('',#9715,#9714,#7994,.T.);
#12555=EDGE_CURVE('',#9715,#9716,#7995,.T.);
#12556=EDGE_CURVE('',#9717,#9716,#7996,.T.);
#12557=EDGE_CURVE('',#9718,#9717,#7997,.T.);
#12558=EDGE_CURVE('',#9713,#9718,#7998,.T.);
#12559=EDGE_CURVE('',#9711,#9714,#7999,.T.);
#12560=EDGE_CURVE('',#9707,#9718,#8000,.T.);
#12561=EDGE_CURVE('',#9709,#9708,#8001,.T.);
#12562=EDGE_CURVE('',#9716,#9715,#8002,.T.);
#12563=EDGE_CURVE('',#9719,#9719,#1007,.T.);
#12564=EDGE_CURVE('',#9719,#9720,#1008,.T.);
#12565=EDGE_CURVE('',#9720,#9721,#1009,.T.);
#12566=EDGE_CURVE('',#9721,#9720,#1010,.T.);
#12567=EDGE_CURVE('',#9721,#9722,#3153,.T.);
#12568=EDGE_CURVE('',#9723,#9722,#1011,.T.);
#12569=EDGE_CURVE('',#9722,#9723,#1012,.T.);
#12570=EDGE_CURVE('',#9724,#9724,#1013,.T.);
#12571=EDGE_CURVE('',#9723,#9725,#1014,.T.);
#12572=EDGE_CURVE('',#9725,#9725,#1015,.T.);
#12573=EDGE_CURVE('',#9726,#9726,#1016,.T.);
#12574=EDGE_CURVE('',#9727,#9728,#1017,.T.);
#12575=EDGE_CURVE('',#9728,#9729,#1018,.T.);
#12576=EDGE_CURVE('',#9729,#9729,#1019,.T.);
#12577=EDGE_CURVE('',#9728,#9727,#1020,.T.);
#12578=EDGE_CURVE('',#9730,#9730,#1021,.T.);
#12579=EDGE_CURVE('',#9726,#9727,#3154,.T.);
#12580=EDGE_CURVE('',#9730,#9731,#1022,.T.);
#12581=EDGE_CURVE('',#9731,#9732,#1023,.T.);
#12582=EDGE_CURVE('',#9732,#9731,#1024,.T.);
#12583=EDGE_CURVE('',#9732,#9733,#3155,.T.);
#12584=EDGE_CURVE('',#9733,#9733,#1025,.T.);
#12585=EDGE_CURVE('',#9734,#9735,#1026,.T.);
#12586=EDGE_CURVE('',#9735,#9736,#3156,.T.);
#12587=EDGE_CURVE('',#9736,#9737,#1027,.T.);
#12588=EDGE_CURVE('',#9737,#9734,#3157,.T.);
#12589=EDGE_CURVE('',#9738,#9738,#1028,.T.);
#12590=EDGE_CURVE('',#9738,#9739,#1029,.T.);
#12591=EDGE_CURVE('',#9739,#9740,#1030,.T.);
#12592=EDGE_CURVE('',#9740,#9739,#1031,.T.);
#12593=EDGE_CURVE('',#9740,#9741,#3158,.T.);
#12594=EDGE_CURVE('',#9742,#9741,#1032,.T.);
#12595=EDGE_CURVE('',#9741,#9742,#1033,.T.);
#12596=EDGE_CURVE('',#9742,#9724,#1034,.T.);
#12597=EDGE_CURVE('',#9743,#9744,#3159,.T.);
#12598=EDGE_CURVE('',#9744,#9745,#1974,.T.);
#12599=EDGE_CURVE('',#9745,#9746,#3160,.T.);
#12600=EDGE_CURVE('',#9746,#9743,#1975,.T.);
#12601=EDGE_CURVE('',#9747,#9745,#3161,.T.);
#12602=EDGE_CURVE('',#9744,#9748,#3162,.T.);
#12603=EDGE_CURVE('',#9748,#9747,#1976,.T.);
#12604=EDGE_CURVE('',#9749,#9743,#3163,.T.);
#12605=EDGE_CURVE('',#9746,#9750,#3164,.T.);
#12606=EDGE_CURVE('',#9750,#9749,#1977,.T.);
#12607=EDGE_CURVE('',#9748,#9749,#3165,.T.);
#12608=EDGE_CURVE('',#9750,#9747,#3166,.T.);
#12609=EDGE_CURVE('',#9735,#9744,#3167,.T.);
#12610=EDGE_CURVE('',#9748,#9734,#3168,.T.);
#12611=EDGE_CURVE('',#9743,#9736,#3169,.T.);
#12612=EDGE_CURVE('',#9751,#9752,#3170,.T.);
#12613=EDGE_CURVE('',#9752,#9753,#3171,.T.);
#12614=EDGE_CURVE('',#9753,#9754,#3172,.T.);
#12615=EDGE_CURVE('',#9754,#9751,#3173,.T.);
#12616=EDGE_CURVE('',#9751,#9755,#3174,.T.);
#12617=EDGE_CURVE('',#9755,#9756,#3175,.T.);
#12618=EDGE_CURVE('',#9752,#9756,#3176,.T.);
#12619=EDGE_CURVE('',#9754,#9757,#3177,.T.);
#12620=EDGE_CURVE('',#9757,#9755,#3178,.T.);
#12621=EDGE_CURVE('',#9753,#9758,#3179,.T.);
#12622=EDGE_CURVE('',#9758,#9757,#3180,.T.);
#12623=EDGE_CURVE('',#9756,#9758,#3181,.T.);
#12624=EDGE_CURVE('',#9737,#9749,#3182,.T.);
#12625=EDGE_CURVE('',#9759,#9760,#1035,.T.);
#12626=EDGE_CURVE('',#9760,#9761,#3183,.T.);
#12627=EDGE_CURVE('',#9761,#9762,#1036,.T.);
#12628=EDGE_CURVE('',#9762,#9759,#3184,.T.);
#12629=EDGE_CURVE('',#9763,#9764,#1037,.T.);
#12630=EDGE_CURVE('',#9764,#9765,#3185,.T.);
#12631=EDGE_CURVE('',#9765,#9761,#1038,.T.);
#12632=EDGE_CURVE('',#9761,#9763,#3186,.T.);
#12633=EDGE_CURVE('',#9766,#9763,#1039,.T.);
#12634=EDGE_CURVE('',#9763,#9767,#3187,.T.);
#12635=EDGE_CURVE('',#9767,#9768,#1040,.T.);
#12636=EDGE_CURVE('',#9768,#9766,#3188,.T.);
#12637=EDGE_CURVE('',#9760,#9769,#1041,.T.);
#12638=EDGE_CURVE('',#9769,#9770,#3189,.T.);
#12639=EDGE_CURVE('',#9770,#9767,#1042,.T.);
#12640=EDGE_CURVE('',#9767,#9760,#3190,.T.);
#12641=EDGE_CURVE('',#9770,#9768,#1043,.T.);
#12642=EDGE_CURVE('',#9766,#9764,#1044,.T.);
#12643=EDGE_CURVE('',#9765,#9762,#1045,.T.);
#12644=EDGE_CURVE('',#9759,#9769,#1046,.T.);
#12645=EDGE_CURVE('',#9766,#9771,#3191,.T.);
#12646=EDGE_CURVE('',#9771,#9772,#1047,.T.);
#12647=EDGE_CURVE('',#9772,#9764,#3192,.T.);
#12648=EDGE_CURVE('',#9773,#9768,#3193,.T.);
#12649=EDGE_CURVE('',#9771,#9773,#3194,.T.);
#12650=EDGE_CURVE('',#9770,#9774,#3195,.T.);
#12651=EDGE_CURVE('',#9774,#9773,#1048,.T.);
#12652=EDGE_CURVE('',#9775,#9769,#3196,.T.);
#12653=EDGE_CURVE('',#9776,#9775,#8003,.T.);
#12654=EDGE_CURVE('',#9777,#9776,#3197,.T.);
#12655=EDGE_CURVE('',#9774,#9777,#8004,.T.);
#12656=EDGE_CURVE('',#9778,#9778,#1049,.T.);
#12657=EDGE_CURVE('',#9779,#9779,#1050,.T.);
#12658=EDGE_CURVE('',#9759,#9780,#3198,.T.);
#12659=EDGE_CURVE('',#9780,#9775,#1051,.T.);
#12660=EDGE_CURVE('',#9781,#9780,#1052,.T.);
#12661=EDGE_CURVE('',#9780,#9782,#3199,.T.);
#12662=EDGE_CURVE('',#9782,#9783,#1053,.T.);
#12663=EDGE_CURVE('',#9783,#9781,#3200,.T.);
#12664=EDGE_CURVE('',#9781,#9775,#1054,.T.);
#12665=EDGE_CURVE('',#9765,#9784,#3201,.T.);
#12666=EDGE_CURVE('',#9784,#9782,#1055,.T.);
#12667=EDGE_CURVE('',#9782,#9762,#3202,.T.);
#12668=EDGE_CURVE('',#9784,#9783,#1056,.T.);
#12669=EDGE_CURVE('',#9781,#9785,#8005,.T.);
#12670=EDGE_CURVE('',#9776,#9785,#1057,.T.);
#12671=EDGE_CURVE('',#9786,#9783,#8006,.T.);
#12672=EDGE_CURVE('',#9787,#9786,#8007,.T.);
#12673=EDGE_CURVE('',#9788,#9787,#8008,.T.);
#12674=EDGE_CURVE('',#9789,#9788,#8009,.T.);
#12675=EDGE_CURVE('',#9790,#9789,#1058,.T.);
#12676=EDGE_CURVE('',#9790,#9791,#3203,.T.);
#12677=EDGE_CURVE('',#9792,#9791,#8010,.T.);
#12678=EDGE_CURVE('',#9793,#9792,#8011,.T.);
#12679=EDGE_CURVE('',#9794,#9793,#8012,.T.);
#12680=EDGE_CURVE('',#9785,#9794,#8013,.T.);
#12681=EDGE_CURVE('',#9784,#9795,#8014,.T.);
#12682=EDGE_CURVE('',#9786,#9795,#1059,.T.);
#12683=EDGE_CURVE('',#9796,#9772,#8015,.T.);
#12684=EDGE_CURVE('',#9795,#9796,#3204,.T.);
#12685=EDGE_CURVE('',#9797,#9797,#1060,.T.);
#12686=EDGE_CURVE('',#9798,#9798,#1061,.T.);
#12687=EDGE_CURVE('',#9773,#9799,#1062,.T.);
#12688=EDGE_CURVE('',#9799,#9800,#3205,.T.);
#12689=EDGE_CURVE('',#9800,#9771,#1063,.T.);
#12690=EDGE_CURVE('',#9774,#9799,#1064,.T.);
#12691=EDGE_CURVE('',#9800,#9772,#1065,.T.);
#12692=EDGE_CURVE('',#9800,#9801,#8016,.T.);
#12693=EDGE_CURVE('',#9796,#9801,#1066,.T.);
#12694=EDGE_CURVE('',#9802,#9799,#8017,.T.);
#12695=EDGE_CURVE('',#9803,#9802,#8018,.T.);
#12696=EDGE_CURVE('',#9804,#9803,#8019,.T.);
#12697=EDGE_CURVE('',#9805,#9804,#8020,.T.);
#12698=EDGE_CURVE('',#9806,#9805,#8021,.T.);
#12699=EDGE_CURVE('',#9807,#9806,#3206,.T.);
#12700=EDGE_CURVE('',#9808,#9807,#1067,.T.);
#12701=EDGE_CURVE('',#9809,#9808,#8022,.T.);
#12702=EDGE_CURVE('',#9810,#9809,#8023,.T.);
#12703=EDGE_CURVE('',#9801,#9810,#8024,.T.);
#12704=EDGE_CURVE('',#9777,#9802,#1068,.T.);
#12705=EDGE_CURVE('',#9777,#9811,#8025,.T.);
#12706=EDGE_CURVE('',#9811,#9803,#1069,.T.);
#12707=EDGE_CURVE('',#9812,#9804,#1070,.T.);
#12708=EDGE_CURVE('',#9811,#9812,#8026,.T.);
#12709=EDGE_CURVE('',#9812,#9813,#8027,.T.);
#12710=EDGE_CURVE('',#9813,#9805,#1071,.T.);
#12711=EDGE_CURVE('',#9813,#9814,#8028,.T.);
#12712=EDGE_CURVE('',#9814,#9806,#8029,.T.);
#12713=EDGE_CURVE('',#9814,#9815,#3207,.T.);
#12714=EDGE_CURVE('',#9815,#9816,#1072,.T.);
#12715=EDGE_CURVE('',#9816,#9806,#3208,.T.);
#12716=EDGE_CURVE('',#9817,#9818,#1073,.T.);
#12717=EDGE_CURVE('',#9818,#9816,#1074,.T.);
#12718=EDGE_CURVE('',#9815,#9817,#1075,.T.);
#12719=EDGE_CURVE('',#9791,#9818,#3209,.T.);
#12720=EDGE_CURVE('',#9817,#9819,#3210,.T.);
#12721=EDGE_CURVE('',#9819,#9791,#8030,.T.);
#12722=EDGE_CURVE('',#9792,#9820,#1076,.T.);
#12723=EDGE_CURVE('',#9820,#9821,#8031,.T.);
#12724=EDGE_CURVE('',#9821,#9793,#1077,.T.);
#12725=EDGE_CURVE('',#9819,#9820,#8032,.T.);
#12726=EDGE_CURVE('',#9822,#9794,#1078,.T.);
#12727=EDGE_CURVE('',#9821,#9822,#8033,.T.);
#12728=EDGE_CURVE('',#9822,#9776,#8034,.T.);
#12729=EDGE_CURVE('',#9823,#9816,#3211,.T.);
#12730=EDGE_CURVE('',#9823,#9824,#3212,.T.);
#12731=EDGE_CURVE('',#9824,#9825,#1079,.T.);
#12732=EDGE_CURVE('',#9825,#9826,#3213,.T.);
#12733=EDGE_CURVE('',#9826,#9827,#1978,.T.);
#12734=EDGE_CURVE('',#9827,#9828,#8035,.T.);
#12735=EDGE_CURVE('',#9828,#9807,#8036,.T.);
#12736=EDGE_CURVE('',#9829,#9818,#3214,.T.);
#12737=EDGE_CURVE('',#9829,#9823,#1080,.T.);
#12738=EDGE_CURVE('',#9830,#9790,#8037,.F.);
#12739=EDGE_CURVE('',#9831,#9830,#8038,.F.);
#12740=EDGE_CURVE('',#9832,#9831,#1979,.F.);
#12741=EDGE_CURVE('',#9832,#9833,#3215,.T.);
#12742=EDGE_CURVE('',#9833,#9834,#1081,.T.);
#12743=EDGE_CURVE('',#9834,#9829,#3216,.T.);
#12744=EDGE_CURVE('',#9831,#9788,#1082,.T.);
#12745=EDGE_CURVE('',#9787,#9835,#1083,.T.);
#12746=EDGE_CURVE('',#9835,#9832,#8039,.T.);
#12747=EDGE_CURVE('',#9830,#9789,#1084,.T.);
#12748=EDGE_CURVE('',#9795,#9835,#8040,.T.);
#12749=EDGE_CURVE('',#9836,#9796,#8041,.T.);
#12750=EDGE_CURVE('',#9836,#9835,#3217,.T.);
#12751=EDGE_CURVE('',#9826,#9836,#8042,.T.);
#12752=EDGE_CURVE('',#9836,#9810,#1085,.T.);
#12753=EDGE_CURVE('',#9809,#9827,#1086,.T.);
#12754=EDGE_CURVE('',#9808,#9828,#1087,.T.);
#12755=EDGE_CURVE('',#9833,#9825,#3218,.T.);
#12756=EDGE_CURVE('',#9824,#9834,#3219,.T.);
#12757=EDGE_CURVE('',#9837,#9837,#1088,.T.);
#12758=EDGE_CURVE('',#9838,#9838,#1089,.T.);
#12759=EDGE_CURVE('',#9797,#9839,#1090,.T.);
#12760=EDGE_CURVE('',#9839,#9840,#1091,.T.);
#12761=EDGE_CURVE('',#9840,#9839,#1092,.T.);
#12762=EDGE_CURVE('',#9840,#9841,#3220,.T.);
#12763=EDGE_CURVE('',#9842,#9841,#1093,.T.);
#12764=EDGE_CURVE('',#9841,#9842,#1094,.T.);
#12765=EDGE_CURVE('',#9778,#9842,#1095,.T.);
#12766=EDGE_CURVE('',#9837,#9843,#1096,.T.);
#12767=EDGE_CURVE('',#9843,#9844,#1097,.T.);
#12768=EDGE_CURVE('',#9844,#9843,#1098,.T.);
#12769=EDGE_CURVE('',#9844,#9845,#3221,.T.);
#12770=EDGE_CURVE('',#9846,#9845,#1099,.T.);
#12771=EDGE_CURVE('',#9845,#9846,#1100,.T.);
#12772=EDGE_CURVE('',#9847,#9847,#1101,.T.);
#12773=EDGE_CURVE('',#9847,#9846,#1102,.T.);
#12774=EDGE_CURVE('',#9820,#9813,#3222,.T.);
#12775=EDGE_CURVE('',#9848,#9848,#1103,.T.);
#12776=EDGE_CURVE('',#9798,#9849,#1104,.T.);
#12777=EDGE_CURVE('',#9849,#9850,#1105,.T.);
#12778=EDGE_CURVE('',#9850,#9849,#1106,.T.);
#12779=EDGE_CURVE('',#9850,#9851,#3223,.T.);
#12780=EDGE_CURVE('',#9852,#9851,#1107,.T.);
#12781=EDGE_CURVE('',#9851,#9852,#1108,.T.);
#12782=EDGE_CURVE('',#9779,#9852,#1109,.T.);
#12783=EDGE_CURVE('',#9838,#9853,#1110,.T.);
#12784=EDGE_CURVE('',#9853,#9854,#1111,.T.);
#12785=EDGE_CURVE('',#9854,#9853,#1112,.T.);
#12786=EDGE_CURVE('',#9854,#9855,#3224,.T.);
#12787=EDGE_CURVE('',#9856,#9855,#1113,.T.);
#12788=EDGE_CURVE('',#9855,#9856,#1114,.T.);
#12789=EDGE_CURVE('',#9848,#9856,#1115,.T.);
#12790=EDGE_CURVE('',#9812,#9821,#3225,.T.);
#12791=EDGE_CURVE('',#9822,#9811,#3226,.T.);
#12792=EDGE_CURVE('',#9857,#9857,#1116,.T.);
#12793=EDGE_CURVE('',#9858,#9858,#1117,.T.);
#12794=EDGE_CURVE('',#9859,#9859,#1118,.T.);
#12795=EDGE_CURVE('',#9859,#9857,#3227,.T.);
#12796=EDGE_CURVE('',#9860,#9860,#1119,.T.);
#12797=EDGE_CURVE('',#9860,#9861,#3228,.T.);
#12798=EDGE_CURVE('',#9861,#9861,#1120,.T.);
#12799=EDGE_CURVE('',#9862,#9862,#1121,.T.);
#12800=EDGE_CURVE('',#9862,#9863,#3229,.T.);
#12801=EDGE_CURVE('',#9863,#9863,#1122,.T.);
#12802=EDGE_CURVE('',#9864,#9864,#1123,.T.);
#12803=EDGE_CURVE('',#9864,#9865,#3230,.T.);
#12804=EDGE_CURVE('',#9865,#9865,#1124,.T.);
#12805=EDGE_CURVE('',#9866,#9866,#1125,.T.);
#12806=EDGE_CURVE('',#9867,#9867,#1126,.T.);
#12807=EDGE_CURVE('',#9867,#9868,#3231,.T.);
#12808=EDGE_CURVE('',#9868,#9868,#1127,.T.);
#12809=EDGE_CURVE('',#9869,#9869,#1128,.T.);
#12810=EDGE_CURVE('',#9869,#9870,#3232,.T.);
#12811=EDGE_CURVE('',#9870,#9870,#1129,.T.);
#12812=EDGE_CURVE('',#9871,#9871,#1130,.T.);
#12813=EDGE_CURVE('',#9872,#9872,#1131,.T.);
#12814=EDGE_CURVE('',#9873,#9873,#1132,.T.);
#12815=EDGE_CURVE('',#9873,#9874,#3233,.T.);
#12816=EDGE_CURVE('',#9874,#9874,#1133,.T.);
#12817=EDGE_CURVE('',#9875,#9875,#1134,.T.);
#12818=EDGE_CURVE('',#9875,#9876,#3234,.T.);
#12819=EDGE_CURVE('',#9876,#9876,#1135,.T.);
#12820=EDGE_CURVE('',#9877,#9877,#1136,.T.);
#12821=EDGE_CURVE('',#9877,#9878,#3235,.T.);
#12822=EDGE_CURVE('',#9878,#9878,#1137,.T.);
#12823=EDGE_CURVE('',#9879,#9879,#1138,.T.);
#12824=EDGE_CURVE('',#9879,#9880,#3236,.T.);
#12825=EDGE_CURVE('',#9880,#9880,#1139,.T.);
#12826=EDGE_CURVE('',#9880,#9881,#3237,.T.);
#12827=EDGE_CURVE('',#9881,#9881,#1140,.T.);
#12828=EDGE_CURVE('',#9882,#9882,#1141,.T.);
#12829=EDGE_CURVE('',#9882,#9872,#3238,.T.);
#12830=EDGE_CURVE('',#9882,#9871,#3239,.T.);
#12831=EDGE_CURVE('',#9858,#9866,#3240,.T.);
#12832=EDGE_CURVE('',#9883,#9883,#1142,.T.);
#12833=EDGE_CURVE('',#9883,#9884,#3241,.T.);
#12834=EDGE_CURVE('',#9884,#9884,#1143,.T.);
#12835=EDGE_CURVE('',#9885,#9885,#1144,.T.);
#12836=EDGE_CURVE('',#9885,#9883,#3242,.T.);
#12837=EDGE_CURVE('',#9885,#9886,#3243,.T.);
#12838=EDGE_CURVE('',#9886,#9886,#1145,.T.);
#12839=EDGE_CURVE('',#9887,#9887,#1146,.T.);
#12840=EDGE_CURVE('',#9888,#9888,#1147,.T.);
#12841=EDGE_CURVE('',#9888,#9887,#3244,.T.);
#12842=EDGE_CURVE('',#9889,#9889,#1148,.T.);
#12843=EDGE_CURVE('',#9889,#9890,#3245,.T.);
#12844=EDGE_CURVE('',#9890,#9890,#1149,.T.);
#12845=EDGE_CURVE('',#9891,#9891,#1150,.T.);
#12846=EDGE_CURVE('',#9891,#9889,#3246,.T.);
#12847=EDGE_CURVE('',#9891,#9892,#3247,.T.);
#12848=EDGE_CURVE('',#9892,#9892,#1151,.T.);
#12849=EDGE_CURVE('',#9893,#9893,#1152,.T.);
#12850=EDGE_CURVE('',#9893,#9894,#3248,.T.);
#12851=EDGE_CURVE('',#9894,#9894,#1153,.T.);
#12852=EDGE_CURVE('',#9895,#9895,#1154,.T.);
#12853=EDGE_CURVE('',#9895,#9893,#3249,.T.);
#12854=EDGE_CURVE('',#9895,#9896,#3250,.T.);
#12855=EDGE_CURVE('',#9896,#9896,#1155,.T.);
#12856=EDGE_CURVE('',#9897,#9897,#1156,.T.);
#12857=EDGE_CURVE('',#9898,#9898,#1157,.T.);
#12858=EDGE_CURVE('',#9898,#9897,#3251,.T.);
#12859=EDGE_CURVE('',#9899,#9899,#1158,.T.);
#12860=EDGE_CURVE('',#9899,#9898,#3252,.T.);
#12861=EDGE_CURVE('',#9900,#9900,#1159,.T.);
#12862=EDGE_CURVE('',#9901,#9901,#1160,.T.);
#12863=EDGE_CURVE('',#9901,#9900,#3253,.T.);
#12864=EDGE_CURVE('',#9901,#9902,#3254,.T.);
#12865=EDGE_CURVE('',#9902,#9902,#1161,.T.);
#12866=EDGE_CURVE('',#9903,#9903,#1162,.T.);
#12867=EDGE_CURVE('',#9904,#9904,#1163,.T.);
#12868=EDGE_CURVE('',#9904,#9903,#3255,.T.);
#12869=EDGE_CURVE('',#9905,#9905,#1164,.T.);
#12870=EDGE_CURVE('',#9906,#9906,#1165,.T.);
#12871=EDGE_CURVE('',#9906,#9905,#3256,.T.);
#12872=EDGE_CURVE('',#9907,#9907,#1166,.T.);
#12873=EDGE_CURVE('',#9908,#9908,#1167,.T.);
#12874=EDGE_CURVE('',#9908,#9907,#3257,.T.);
#12875=EDGE_CURVE('',#9908,#9909,#3258,.T.);
#12876=EDGE_CURVE('',#9909,#9909,#1168,.T.);
#12877=EDGE_CURVE('',#9910,#9910,#1169,.T.);
#12878=EDGE_CURVE('',#9910,#9911,#3259,.T.);
#12879=EDGE_CURVE('',#9911,#9911,#1170,.T.);
#12880=EDGE_CURVE('',#9912,#9912,#1171,.T.);
#12881=EDGE_CURVE('',#9912,#9910,#3260,.T.);
#12882=EDGE_CURVE('',#9912,#9913,#3261,.T.);
#12883=EDGE_CURVE('',#9913,#9913,#1172,.T.);
#12884=EDGE_CURVE('',#9914,#9914,#1173,.T.);
#12885=EDGE_CURVE('',#9915,#9915,#1174,.T.);
#12886=EDGE_CURVE('',#9916,#9916,#1175,.T.);
#12887=EDGE_CURVE('',#9916,#9915,#3262,.T.);
#12888=EDGE_CURVE('',#9917,#9917,#1176,.T.);
#12889=EDGE_CURVE('',#9918,#9918,#1177,.T.);
#12890=EDGE_CURVE('',#9918,#9917,#3263,.T.);
#12891=EDGE_CURVE('',#9918,#9919,#3264,.T.);
#12892=EDGE_CURVE('',#9919,#9919,#1178,.T.);
#12893=EDGE_CURVE('',#9920,#9920,#1179,.T.);
#12894=EDGE_CURVE('',#9921,#9921,#1180,.T.);
#12895=EDGE_CURVE('',#9922,#9922,#1181,.T.);
#12896=EDGE_CURVE('',#9922,#9921,#3265,.T.);
#12897=EDGE_CURVE('',#9922,#9923,#3266,.T.);
#12898=EDGE_CURVE('',#9923,#9923,#1182,.T.);
#12899=ORIENTED_EDGE('',*,*,#9924,.T.);
#12900=ORIENTED_EDGE('',*,*,#9925,.T.);
#12901=ORIENTED_EDGE('',*,*,#9926,.T.);
#12902=ORIENTED_EDGE('',*,*,#9924,.F.);
#12903=ORIENTED_EDGE('',*,*,#9927,.T.);
#12904=ORIENTED_EDGE('',*,*,#9928,.T.);
#12905=ORIENTED_EDGE('',*,*,#9929,.T.);
#12906=ORIENTED_EDGE('',*,*,#9930,.T.);
#12907=ORIENTED_EDGE('',*,*,#9931,.T.);
#12908=ORIENTED_EDGE('',*,*,#9932,.T.);
#12909=ORIENTED_EDGE('',*,*,#9933,.T.);
#12910=ORIENTED_EDGE('',*,*,#9934,.T.);
#12911=ORIENTED_EDGE('',*,*,#9935,.T.);
#12912=ORIENTED_EDGE('',*,*,#9936,.T.);
#12913=ORIENTED_EDGE('',*,*,#9937,.T.);
#12914=ORIENTED_EDGE('',*,*,#9925,.F.);
#12915=ORIENTED_EDGE('',*,*,#9926,.F.);
#12916=ORIENTED_EDGE('',*,*,#9938,.T.);
#12917=ORIENTED_EDGE('',*,*,#9939,.F.);
#12918=ORIENTED_EDGE('',*,*,#9940,.F.);
#12919=ORIENTED_EDGE('',*,*,#9938,.F.);
#12920=ORIENTED_EDGE('',*,*,#9941,.T.);
#12921=ORIENTED_EDGE('',*,*,#9942,.T.);
#12922=ORIENTED_EDGE('',*,*,#9943,.T.);
#12923=ORIENTED_EDGE('',*,*,#9944,.T.);
#12924=ORIENTED_EDGE('',*,*,#9945,.T.);
#12925=ORIENTED_EDGE('',*,*,#9946,.T.);
#12926=ORIENTED_EDGE('',*,*,#9947,.T.);
#12927=ORIENTED_EDGE('',*,*,#9948,.T.);
#12928=ORIENTED_EDGE('',*,*,#9949,.T.);
#12929=ORIENTED_EDGE('',*,*,#9950,.T.);
#12930=ORIENTED_EDGE('',*,*,#9951,.T.);
#12931=ORIENTED_EDGE('',*,*,#9952,.T.);
#12932=ORIENTED_EDGE('',*,*,#9953,.T.);
#12933=ORIENTED_EDGE('',*,*,#9954,.T.);
#12934=ORIENTED_EDGE('',*,*,#9955,.T.);
#12935=ORIENTED_EDGE('',*,*,#9956,.T.);
#12936=ORIENTED_EDGE('',*,*,#9957,.T.);
#12937=ORIENTED_EDGE('',*,*,#9958,.T.);
#12938=ORIENTED_EDGE('',*,*,#9959,.T.);
#12939=ORIENTED_EDGE('',*,*,#9960,.T.);
#12940=ORIENTED_EDGE('',*,*,#9961,.T.);
#12941=ORIENTED_EDGE('',*,*,#9962,.T.);
#12942=ORIENTED_EDGE('',*,*,#9963,.T.);
#12943=ORIENTED_EDGE('',*,*,#9964,.T.);
#12944=ORIENTED_EDGE('',*,*,#9965,.T.);
#12945=ORIENTED_EDGE('',*,*,#9966,.T.);
#12946=ORIENTED_EDGE('',*,*,#9967,.T.);
#12947=ORIENTED_EDGE('',*,*,#9968,.T.);
#12948=ORIENTED_EDGE('',*,*,#9969,.T.);
#12949=ORIENTED_EDGE('',*,*,#9970,.T.);
#12950=ORIENTED_EDGE('',*,*,#9971,.T.);
#12951=ORIENTED_EDGE('',*,*,#9972,.T.);
#12952=ORIENTED_EDGE('',*,*,#9973,.T.);
#12953=ORIENTED_EDGE('',*,*,#9974,.T.);
#12954=ORIENTED_EDGE('',*,*,#9975,.T.);
#12955=ORIENTED_EDGE('',*,*,#9976,.T.);
#12956=ORIENTED_EDGE('',*,*,#9977,.T.);
#12957=ORIENTED_EDGE('',*,*,#9978,.T.);
#12958=ORIENTED_EDGE('',*,*,#9979,.T.);
#12959=ORIENTED_EDGE('',*,*,#9980,.T.);
#12960=ORIENTED_EDGE('',*,*,#9981,.T.);
#12961=ORIENTED_EDGE('',*,*,#9982,.T.);
#12962=ORIENTED_EDGE('',*,*,#9983,.T.);
#12963=ORIENTED_EDGE('',*,*,#9984,.T.);
#12964=ORIENTED_EDGE('',*,*,#9985,.T.);
#12965=ORIENTED_EDGE('',*,*,#9986,.T.);
#12966=ORIENTED_EDGE('',*,*,#9987,.T.);
#12967=ORIENTED_EDGE('',*,*,#9988,.T.);
#12968=ORIENTED_EDGE('',*,*,#9989,.T.);
#12969=ORIENTED_EDGE('',*,*,#9990,.T.);
#12970=ORIENTED_EDGE('',*,*,#9991,.T.);
#12971=ORIENTED_EDGE('',*,*,#9992,.T.);
#12972=ORIENTED_EDGE('',*,*,#9993,.T.);
#12973=ORIENTED_EDGE('',*,*,#9994,.T.);
#12974=ORIENTED_EDGE('',*,*,#9995,.T.);
#12975=ORIENTED_EDGE('',*,*,#9996,.T.);
#12976=ORIENTED_EDGE('',*,*,#9997,.T.);
#12977=ORIENTED_EDGE('',*,*,#9998,.T.);
#12978=ORIENTED_EDGE('',*,*,#9999,.T.);
#12979=ORIENTED_EDGE('',*,*,#10000,.T.);
#12980=ORIENTED_EDGE('',*,*,#10001,.T.);
#12981=ORIENTED_EDGE('',*,*,#10002,.T.);
#12982=ORIENTED_EDGE('',*,*,#10003,.T.);
#12983=ORIENTED_EDGE('',*,*,#10004,.T.);
#12984=ORIENTED_EDGE('',*,*,#10005,.T.);
#12985=ORIENTED_EDGE('',*,*,#10006,.T.);
#12986=ORIENTED_EDGE('',*,*,#10007,.T.);
#12987=ORIENTED_EDGE('',*,*,#10008,.T.);
#12988=ORIENTED_EDGE('',*,*,#10009,.F.);
#12989=ORIENTED_EDGE('',*,*,#10010,.F.);
#12990=ORIENTED_EDGE('',*,*,#10011,.F.);
#12991=ORIENTED_EDGE('',*,*,#10012,.F.);
#12992=ORIENTED_EDGE('',*,*,#10013,.F.);
#12993=ORIENTED_EDGE('',*,*,#10014,.F.);
#12994=ORIENTED_EDGE('',*,*,#10015,.F.);
#12995=ORIENTED_EDGE('',*,*,#10016,.F.);
#12996=ORIENTED_EDGE('',*,*,#10017,.F.);
#12997=ORIENTED_EDGE('',*,*,#10018,.F.);
#12998=ORIENTED_EDGE('',*,*,#10019,.F.);
#12999=ORIENTED_EDGE('',*,*,#10020,.F.);
#13000=ORIENTED_EDGE('',*,*,#10021,.F.);
#13001=ORIENTED_EDGE('',*,*,#10022,.F.);
#13002=ORIENTED_EDGE('',*,*,#10023,.T.);
#13003=ORIENTED_EDGE('',*,*,#10024,.F.);
#13004=ORIENTED_EDGE('',*,*,#10025,.T.);
#13005=ORIENTED_EDGE('',*,*,#10026,.T.);
#13006=ORIENTED_EDGE('',*,*,#10027,.F.);
#13007=ORIENTED_EDGE('',*,*,#10028,.T.);
#13008=ORIENTED_EDGE('',*,*,#10029,.F.);
#13009=ORIENTED_EDGE('',*,*,#10030,.T.);
#13010=ORIENTED_EDGE('',*,*,#10031,.F.);
#13011=ORIENTED_EDGE('',*,*,#10032,.T.);
#13012=ORIENTED_EDGE('',*,*,#10033,.F.);
#13013=ORIENTED_EDGE('',*,*,#10034,.F.);
#13014=ORIENTED_EDGE('',*,*,#10035,.F.);
#13015=ORIENTED_EDGE('',*,*,#9937,.F.);
#13016=ORIENTED_EDGE('',*,*,#9936,.F.);
#13017=ORIENTED_EDGE('',*,*,#9935,.F.);
#13018=ORIENTED_EDGE('',*,*,#9934,.F.);
#13019=ORIENTED_EDGE('',*,*,#9933,.F.);
#13020=ORIENTED_EDGE('',*,*,#9932,.F.);
#13021=ORIENTED_EDGE('',*,*,#9931,.F.);
#13022=ORIENTED_EDGE('',*,*,#9930,.F.);
#13023=ORIENTED_EDGE('',*,*,#9929,.F.);
#13024=ORIENTED_EDGE('',*,*,#9928,.F.);
#13025=ORIENTED_EDGE('',*,*,#9927,.F.);
#13026=ORIENTED_EDGE('',*,*,#10036,.T.);
#13027=ORIENTED_EDGE('',*,*,#9939,.T.);
#13028=ORIENTED_EDGE('',*,*,#9940,.T.);
#13029=ORIENTED_EDGE('',*,*,#10036,.F.);
#13030=ORIENTED_EDGE('',*,*,#10037,.T.);
#13031=ORIENTED_EDGE('',*,*,#10038,.T.);
#13032=ORIENTED_EDGE('',*,*,#10039,.T.);
#13033=ORIENTED_EDGE('',*,*,#10040,.T.);
#13034=ORIENTED_EDGE('',*,*,#10041,.T.);
#13035=ORIENTED_EDGE('',*,*,#10042,.T.);
#13036=ORIENTED_EDGE('',*,*,#10043,.T.);
#13037=ORIENTED_EDGE('',*,*,#10044,.T.);
#13038=ORIENTED_EDGE('',*,*,#10045,.T.);
#13039=ORIENTED_EDGE('',*,*,#10046,.T.);
#13040=ORIENTED_EDGE('',*,*,#10047,.T.);
#13041=ORIENTED_EDGE('',*,*,#10048,.F.);
#13042=ORIENTED_EDGE('',*,*,#10049,.F.);
#13043=ORIENTED_EDGE('',*,*,#10050,.F.);
#13044=ORIENTED_EDGE('',*,*,#10051,.F.);
#13045=ORIENTED_EDGE('',*,*,#10052,.F.);
#13046=ORIENTED_EDGE('',*,*,#10053,.F.);
#13047=ORIENTED_EDGE('',*,*,#10054,.F.);
#13048=ORIENTED_EDGE('',*,*,#10055,.F.);
#13049=ORIENTED_EDGE('',*,*,#10056,.F.);
#13050=ORIENTED_EDGE('',*,*,#10057,.F.);
#13051=ORIENTED_EDGE('',*,*,#10058,.F.);
#13052=ORIENTED_EDGE('',*,*,#10059,.F.);
#13053=ORIENTED_EDGE('',*,*,#10060,.F.);
#13054=ORIENTED_EDGE('',*,*,#10061,.F.);
#13055=ORIENTED_EDGE('',*,*,#10062,.F.);
#13056=ORIENTED_EDGE('',*,*,#10063,.F.);
#13057=ORIENTED_EDGE('',*,*,#10064,.F.);
#13058=ORIENTED_EDGE('',*,*,#10065,.F.);
#13059=ORIENTED_EDGE('',*,*,#10066,.F.);
#13060=ORIENTED_EDGE('',*,*,#10067,.F.);
#13061=ORIENTED_EDGE('',*,*,#10068,.F.);
#13062=ORIENTED_EDGE('',*,*,#10069,.F.);
#13063=ORIENTED_EDGE('',*,*,#10070,.F.);
#13064=ORIENTED_EDGE('',*,*,#10071,.F.);
#13065=ORIENTED_EDGE('',*,*,#10072,.F.);
#13066=ORIENTED_EDGE('',*,*,#10073,.F.);
#13067=ORIENTED_EDGE('',*,*,#10074,.F.);
#13068=ORIENTED_EDGE('',*,*,#10075,.F.);
#13069=ORIENTED_EDGE('',*,*,#10076,.F.);
#13070=ORIENTED_EDGE('',*,*,#10077,.F.);
#13071=ORIENTED_EDGE('',*,*,#10078,.F.);
#13072=ORIENTED_EDGE('',*,*,#10079,.F.);
#13073=ORIENTED_EDGE('',*,*,#10080,.F.);
#13074=ORIENTED_EDGE('',*,*,#10081,.F.);
#13075=ORIENTED_EDGE('',*,*,#10082,.F.);
#13076=ORIENTED_EDGE('',*,*,#10083,.F.);
#13077=ORIENTED_EDGE('',*,*,#10084,.F.);
#13078=ORIENTED_EDGE('',*,*,#10085,.F.);
#13079=ORIENTED_EDGE('',*,*,#10086,.F.);
#13080=ORIENTED_EDGE('',*,*,#10087,.F.);
#13081=ORIENTED_EDGE('',*,*,#10088,.F.);
#13082=ORIENTED_EDGE('',*,*,#10089,.F.);
#13083=ORIENTED_EDGE('',*,*,#10090,.F.);
#13084=ORIENTED_EDGE('',*,*,#10091,.F.);
#13085=ORIENTED_EDGE('',*,*,#10092,.F.);
#13086=ORIENTED_EDGE('',*,*,#10093,.F.);
#13087=ORIENTED_EDGE('',*,*,#10094,.F.);
#13088=ORIENTED_EDGE('',*,*,#10095,.F.);
#13089=ORIENTED_EDGE('',*,*,#10096,.F.);
#13090=ORIENTED_EDGE('',*,*,#10097,.F.);
#13091=ORIENTED_EDGE('',*,*,#10098,.F.);
#13092=ORIENTED_EDGE('',*,*,#10099,.F.);
#13093=ORIENTED_EDGE('',*,*,#10100,.F.);
#13094=ORIENTED_EDGE('',*,*,#10101,.F.);
#13095=ORIENTED_EDGE('',*,*,#10102,.F.);
#13096=ORIENTED_EDGE('',*,*,#10103,.F.);
#13097=ORIENTED_EDGE('',*,*,#10104,.F.);
#13098=ORIENTED_EDGE('',*,*,#10105,.F.);
#13099=ORIENTED_EDGE('',*,*,#10106,.F.);
#13100=ORIENTED_EDGE('',*,*,#10107,.F.);
#13101=ORIENTED_EDGE('',*,*,#10108,.F.);
#13102=ORIENTED_EDGE('',*,*,#10109,.F.);
#13103=ORIENTED_EDGE('',*,*,#10110,.F.);
#13104=ORIENTED_EDGE('',*,*,#10111,.F.);
#13105=ORIENTED_EDGE('',*,*,#10112,.F.);
#13106=ORIENTED_EDGE('',*,*,#10113,.F.);
#13107=ORIENTED_EDGE('',*,*,#10114,.F.);
#13108=ORIENTED_EDGE('',*,*,#10115,.F.);
#13109=ORIENTED_EDGE('',*,*,#10116,.F.);
#13110=ORIENTED_EDGE('',*,*,#10117,.F.);
#13111=ORIENTED_EDGE('',*,*,#10118,.F.);
#13112=ORIENTED_EDGE('',*,*,#10119,.F.);
#13113=ORIENTED_EDGE('',*,*,#10120,.F.);
#13114=ORIENTED_EDGE('',*,*,#10121,.F.);
#13115=ORIENTED_EDGE('',*,*,#10122,.F.);
#13116=ORIENTED_EDGE('',*,*,#10123,.F.);
#13117=ORIENTED_EDGE('',*,*,#10124,.F.);
#13118=ORIENTED_EDGE('',*,*,#10125,.F.);
#13119=ORIENTED_EDGE('',*,*,#10126,.F.);
#13120=ORIENTED_EDGE('',*,*,#10127,.F.);
#13121=ORIENTED_EDGE('',*,*,#10128,.F.);
#13122=ORIENTED_EDGE('',*,*,#10129,.F.);
#13123=ORIENTED_EDGE('',*,*,#10130,.F.);
#13124=ORIENTED_EDGE('',*,*,#10131,.F.);
#13125=ORIENTED_EDGE('',*,*,#10132,.F.);
#13126=ORIENTED_EDGE('',*,*,#10047,.F.);
#13127=ORIENTED_EDGE('',*,*,#10046,.F.);
#13128=ORIENTED_EDGE('',*,*,#10045,.F.);
#13129=ORIENTED_EDGE('',*,*,#10044,.F.);
#13130=ORIENTED_EDGE('',*,*,#10043,.F.);
#13131=ORIENTED_EDGE('',*,*,#10042,.F.);
#13132=ORIENTED_EDGE('',*,*,#10041,.F.);
#13133=ORIENTED_EDGE('',*,*,#10040,.F.);
#13134=ORIENTED_EDGE('',*,*,#10039,.F.);
#13135=ORIENTED_EDGE('',*,*,#10038,.F.);
#13136=ORIENTED_EDGE('',*,*,#10037,.F.);
#13137=ORIENTED_EDGE('',*,*,#10133,.T.);
#13138=ORIENTED_EDGE('',*,*,#10134,.T.);
#13139=ORIENTED_EDGE('',*,*,#10135,.T.);
#13140=ORIENTED_EDGE('',*,*,#10133,.F.);
#13141=ORIENTED_EDGE('',*,*,#10019,.T.);
#13142=ORIENTED_EDGE('',*,*,#10018,.T.);
#13143=ORIENTED_EDGE('',*,*,#10017,.T.);
#13144=ORIENTED_EDGE('',*,*,#10016,.T.);
#13145=ORIENTED_EDGE('',*,*,#10015,.T.);
#13146=ORIENTED_EDGE('',*,*,#10014,.T.);
#13147=ORIENTED_EDGE('',*,*,#10013,.T.);
#13148=ORIENTED_EDGE('',*,*,#10012,.T.);
#13149=ORIENTED_EDGE('',*,*,#10011,.T.);
#13150=ORIENTED_EDGE('',*,*,#10010,.T.);
#13151=ORIENTED_EDGE('',*,*,#10009,.T.);
#13152=ORIENTED_EDGE('',*,*,#10134,.F.);
#13153=ORIENTED_EDGE('',*,*,#10135,.F.);
#13154=ORIENTED_EDGE('',*,*,#10136,.T.);
#13155=ORIENTED_EDGE('',*,*,#10137,.F.);
#13156=ORIENTED_EDGE('',*,*,#10138,.F.);
#13157=ORIENTED_EDGE('',*,*,#10136,.F.);
#13158=ORIENTED_EDGE('',*,*,#10139,.T.);
#13159=ORIENTED_EDGE('',*,*,#10137,.T.);
#13160=ORIENTED_EDGE('',*,*,#10138,.T.);
#13161=ORIENTED_EDGE('',*,*,#10139,.F.);
#13162=ORIENTED_EDGE('',*,*,#10126,.T.);
#13163=ORIENTED_EDGE('',*,*,#10125,.T.);
#13164=ORIENTED_EDGE('',*,*,#10124,.T.);
#13165=ORIENTED_EDGE('',*,*,#10123,.T.);
#13166=ORIENTED_EDGE('',*,*,#10122,.T.);
#13167=ORIENTED_EDGE('',*,*,#10121,.T.);
#13168=ORIENTED_EDGE('',*,*,#10120,.T.);
#13169=ORIENTED_EDGE('',*,*,#10119,.T.);
#13170=ORIENTED_EDGE('',*,*,#10118,.T.);
#13171=ORIENTED_EDGE('',*,*,#10117,.T.);
#13172=ORIENTED_EDGE('',*,*,#10116,.T.);
#13173=ORIENTED_EDGE('',*,*,#10140,.T.);
#13174=ORIENTED_EDGE('',*,*,#10141,.T.);
#13175=ORIENTED_EDGE('',*,*,#10142,.T.);
#13176=ORIENTED_EDGE('',*,*,#10140,.F.);
#13177=ORIENTED_EDGE('',*,*,#10035,.T.);
#13178=ORIENTED_EDGE('',*,*,#10034,.T.);
#13179=ORIENTED_EDGE('',*,*,#10033,.T.);
#13180=ORIENTED_EDGE('',*,*,#10141,.F.);
#13181=ORIENTED_EDGE('',*,*,#10142,.F.);
#13182=ORIENTED_EDGE('',*,*,#10143,.T.);
#13183=ORIENTED_EDGE('',*,*,#10144,.F.);
#13184=ORIENTED_EDGE('',*,*,#10145,.F.);
#13185=ORIENTED_EDGE('',*,*,#10143,.F.);
#13186=ORIENTED_EDGE('',*,*,#10146,.T.);
#13187=ORIENTED_EDGE('',*,*,#10144,.T.);
#13188=ORIENTED_EDGE('',*,*,#10145,.T.);
#13189=ORIENTED_EDGE('',*,*,#10146,.F.);
#13190=ORIENTED_EDGE('',*,*,#10132,.T.);
#13191=ORIENTED_EDGE('',*,*,#10131,.T.);
#13192=ORIENTED_EDGE('',*,*,#10130,.T.);
#13193=ORIENTED_EDGE('',*,*,#10147,.T.);
#13194=ORIENTED_EDGE('',*,*,#10148,.T.);
#13195=ORIENTED_EDGE('',*,*,#10149,.T.);
#13196=ORIENTED_EDGE('',*,*,#10147,.F.);
#13197=ORIENTED_EDGE('',*,*,#10022,.T.);
#13198=ORIENTED_EDGE('',*,*,#10021,.T.);
#13199=ORIENTED_EDGE('',*,*,#10020,.T.);
#13200=ORIENTED_EDGE('',*,*,#10148,.F.);
#13201=ORIENTED_EDGE('',*,*,#10149,.F.);
#13202=ORIENTED_EDGE('',*,*,#10150,.T.);
#13203=ORIENTED_EDGE('',*,*,#10151,.F.);
#13204=ORIENTED_EDGE('',*,*,#10152,.F.);
#13205=ORIENTED_EDGE('',*,*,#10150,.F.);
#13206=ORIENTED_EDGE('',*,*,#10153,.T.);
#13207=ORIENTED_EDGE('',*,*,#10151,.T.);
#13208=ORIENTED_EDGE('',*,*,#10152,.T.);
#13209=ORIENTED_EDGE('',*,*,#10153,.F.);
#13210=ORIENTED_EDGE('',*,*,#10129,.T.);
#13211=ORIENTED_EDGE('',*,*,#10128,.T.);
#13212=ORIENTED_EDGE('',*,*,#10127,.T.);
#13213=ORIENTED_EDGE('',*,*,#10154,.F.);
#13214=ORIENTED_EDGE('',*,*,#10031,.T.);
#13215=ORIENTED_EDGE('',*,*,#10155,.T.);
#13216=ORIENTED_EDGE('',*,*,#10156,.T.);
#13217=ORIENTED_EDGE('',*,*,#10029,.T.);
#13218=ORIENTED_EDGE('',*,*,#10157,.T.);
#13219=ORIENTED_EDGE('',*,*,#10158,.T.);
#13220=ORIENTED_EDGE('',*,*,#10155,.F.);
#13221=ORIENTED_EDGE('',*,*,#10030,.F.);
#13222=ORIENTED_EDGE('',*,*,#10027,.T.);
#13223=ORIENTED_EDGE('',*,*,#10159,.T.);
#13224=ORIENTED_EDGE('',*,*,#10160,.T.);
#13225=ORIENTED_EDGE('',*,*,#10157,.F.);
#13226=ORIENTED_EDGE('',*,*,#10028,.F.);
#13227=ORIENTED_EDGE('',*,*,#10024,.T.);
#13228=ORIENTED_EDGE('',*,*,#10023,.F.);
#13229=ORIENTED_EDGE('',*,*,#10032,.F.);
#13230=ORIENTED_EDGE('',*,*,#10154,.T.);
#13231=ORIENTED_EDGE('',*,*,#10161,.T.);
#13232=ORIENTED_EDGE('',*,*,#10159,.F.);
#13233=ORIENTED_EDGE('',*,*,#10026,.F.);
#13234=ORIENTED_EDGE('',*,*,#10025,.F.);
#13235=ORIENTED_EDGE('',*,*,#10156,.F.);
#13236=ORIENTED_EDGE('',*,*,#10158,.F.);
#13237=ORIENTED_EDGE('',*,*,#10160,.F.);
#13238=ORIENTED_EDGE('',*,*,#10161,.F.);
#13239=ORIENTED_EDGE('',*,*,#10162,.F.);
#13240=ORIENTED_EDGE('',*,*,#9965,.F.);
#13241=ORIENTED_EDGE('',*,*,#10163,.T.);
#13242=ORIENTED_EDGE('',*,*,#10092,.T.);
#13243=ORIENTED_EDGE('',*,*,#10163,.F.);
#13244=ORIENTED_EDGE('',*,*,#9964,.F.);
#13245=ORIENTED_EDGE('',*,*,#10164,.T.);
#13246=ORIENTED_EDGE('',*,*,#10093,.T.);
#13247=ORIENTED_EDGE('',*,*,#10164,.F.);
#13248=ORIENTED_EDGE('',*,*,#9963,.F.);
#13249=ORIENTED_EDGE('',*,*,#10165,.T.);
#13250=ORIENTED_EDGE('',*,*,#10166,.T.);
#13251=ORIENTED_EDGE('',*,*,#10094,.T.);
#13252=ORIENTED_EDGE('',*,*,#10165,.F.);
#13253=ORIENTED_EDGE('',*,*,#9962,.F.);
#13254=ORIENTED_EDGE('',*,*,#10167,.T.);
#13255=ORIENTED_EDGE('',*,*,#10168,.T.);
#13256=ORIENTED_EDGE('',*,*,#10095,.T.);
#13257=ORIENTED_EDGE('',*,*,#10166,.F.);
#13258=ORIENTED_EDGE('',*,*,#10167,.F.);
#13259=ORIENTED_EDGE('',*,*,#9961,.F.);
#13260=ORIENTED_EDGE('',*,*,#10169,.T.);
#13261=ORIENTED_EDGE('',*,*,#10096,.T.);
#13262=ORIENTED_EDGE('',*,*,#10168,.F.);
#13263=ORIENTED_EDGE('',*,*,#10169,.F.);
#13264=ORIENTED_EDGE('',*,*,#9960,.F.);
#13265=ORIENTED_EDGE('',*,*,#10170,.T.);
#13266=ORIENTED_EDGE('',*,*,#10097,.T.);
#13267=ORIENTED_EDGE('',*,*,#10170,.F.);
#13268=ORIENTED_EDGE('',*,*,#9959,.F.);
#13269=ORIENTED_EDGE('',*,*,#10171,.T.);
#13270=ORIENTED_EDGE('',*,*,#10098,.T.);
#13271=ORIENTED_EDGE('',*,*,#10171,.F.);
#13272=ORIENTED_EDGE('',*,*,#9958,.F.);
#13273=ORIENTED_EDGE('',*,*,#10172,.T.);
#13274=ORIENTED_EDGE('',*,*,#10099,.T.);
#13275=ORIENTED_EDGE('',*,*,#10172,.F.);
#13276=ORIENTED_EDGE('',*,*,#9957,.F.);
#13277=ORIENTED_EDGE('',*,*,#10173,.T.);
#13278=ORIENTED_EDGE('',*,*,#10174,.T.);
#13279=ORIENTED_EDGE('',*,*,#10100,.T.);
#13280=ORIENTED_EDGE('',*,*,#10173,.F.);
#13281=ORIENTED_EDGE('',*,*,#9956,.F.);
#13282=ORIENTED_EDGE('',*,*,#10175,.T.);
#13283=ORIENTED_EDGE('',*,*,#10176,.T.);
#13284=ORIENTED_EDGE('',*,*,#10101,.T.);
#13285=ORIENTED_EDGE('',*,*,#10174,.F.);
#13286=ORIENTED_EDGE('',*,*,#10175,.F.);
#13287=ORIENTED_EDGE('',*,*,#9955,.F.);
#13288=ORIENTED_EDGE('',*,*,#10177,.T.);
#13289=ORIENTED_EDGE('',*,*,#10178,.T.);
#13290=ORIENTED_EDGE('',*,*,#10102,.T.);
#13291=ORIENTED_EDGE('',*,*,#10176,.F.);
#13292=ORIENTED_EDGE('',*,*,#10177,.F.);
#13293=ORIENTED_EDGE('',*,*,#9954,.F.);
#13294=ORIENTED_EDGE('',*,*,#10179,.T.);
#13295=ORIENTED_EDGE('',*,*,#10103,.T.);
#13296=ORIENTED_EDGE('',*,*,#10178,.F.);
#13297=ORIENTED_EDGE('',*,*,#10179,.F.);
#13298=ORIENTED_EDGE('',*,*,#9953,.F.);
#13299=ORIENTED_EDGE('',*,*,#10180,.T.);
#13300=ORIENTED_EDGE('',*,*,#10104,.T.);
#13301=ORIENTED_EDGE('',*,*,#10181,.F.);
#13302=ORIENTED_EDGE('',*,*,#9973,.F.);
#13303=ORIENTED_EDGE('',*,*,#10182,.T.);
#13304=ORIENTED_EDGE('',*,*,#10084,.T.);
#13305=ORIENTED_EDGE('',*,*,#10183,.F.);
#13306=ORIENTED_EDGE('',*,*,#10182,.F.);
#13307=ORIENTED_EDGE('',*,*,#9972,.F.);
#13308=ORIENTED_EDGE('',*,*,#10184,.T.);
#13309=ORIENTED_EDGE('',*,*,#10085,.T.);
#13310=ORIENTED_EDGE('',*,*,#10184,.F.);
#13311=ORIENTED_EDGE('',*,*,#9971,.F.);
#13312=ORIENTED_EDGE('',*,*,#10185,.T.);
#13313=ORIENTED_EDGE('',*,*,#10086,.T.);
#13314=ORIENTED_EDGE('',*,*,#10185,.F.);
#13315=ORIENTED_EDGE('',*,*,#9970,.F.);
#13316=ORIENTED_EDGE('',*,*,#10186,.T.);
#13317=ORIENTED_EDGE('',*,*,#10087,.T.);
#13318=ORIENTED_EDGE('',*,*,#10186,.F.);
#13319=ORIENTED_EDGE('',*,*,#9969,.F.);
#13320=ORIENTED_EDGE('',*,*,#10187,.T.);
#13321=ORIENTED_EDGE('',*,*,#10088,.T.);
#13322=ORIENTED_EDGE('',*,*,#10187,.F.);
#13323=ORIENTED_EDGE('',*,*,#9968,.F.);
#13324=ORIENTED_EDGE('',*,*,#10188,.T.);
#13325=ORIENTED_EDGE('',*,*,#10089,.T.);
#13326=ORIENTED_EDGE('',*,*,#10189,.F.);
#13327=ORIENTED_EDGE('',*,*,#9980,.F.);
#13328=ORIENTED_EDGE('',*,*,#10190,.T.);
#13329=ORIENTED_EDGE('',*,*,#10077,.T.);
#13330=ORIENTED_EDGE('',*,*,#10190,.F.);
#13331=ORIENTED_EDGE('',*,*,#9979,.F.);
#13332=ORIENTED_EDGE('',*,*,#10191,.T.);
#13333=ORIENTED_EDGE('',*,*,#10078,.T.);
#13334=ORIENTED_EDGE('',*,*,#10191,.F.);
#13335=ORIENTED_EDGE('',*,*,#9978,.F.);
#13336=ORIENTED_EDGE('',*,*,#10192,.T.);
#13337=ORIENTED_EDGE('',*,*,#10079,.T.);
#13338=ORIENTED_EDGE('',*,*,#10192,.F.);
#13339=ORIENTED_EDGE('',*,*,#9977,.F.);
#13340=ORIENTED_EDGE('',*,*,#10193,.T.);
#13341=ORIENTED_EDGE('',*,*,#10080,.T.);
#13342=ORIENTED_EDGE('',*,*,#10193,.F.);
#13343=ORIENTED_EDGE('',*,*,#9976,.F.);
#13344=ORIENTED_EDGE('',*,*,#10194,.T.);
#13345=ORIENTED_EDGE('',*,*,#10195,.T.);
#13346=ORIENTED_EDGE('',*,*,#10081,.T.);
#13347=ORIENTED_EDGE('',*,*,#10194,.F.);
#13348=ORIENTED_EDGE('',*,*,#9975,.F.);
#13349=ORIENTED_EDGE('',*,*,#10196,.T.);
#13350=ORIENTED_EDGE('',*,*,#10082,.T.);
#13351=ORIENTED_EDGE('',*,*,#10195,.F.);
#13352=ORIENTED_EDGE('',*,*,#10197,.F.);
#13353=ORIENTED_EDGE('',*,*,#9995,.F.);
#13354=ORIENTED_EDGE('',*,*,#10198,.T.);
#13355=ORIENTED_EDGE('',*,*,#10199,.T.);
#13356=ORIENTED_EDGE('',*,*,#10062,.T.);
#13357=ORIENTED_EDGE('',*,*,#10198,.F.);
#13358=ORIENTED_EDGE('',*,*,#9994,.F.);
#13359=ORIENTED_EDGE('',*,*,#10200,.T.);
#13360=ORIENTED_EDGE('',*,*,#10201,.T.);
#13361=ORIENTED_EDGE('',*,*,#10063,.T.);
#13362=ORIENTED_EDGE('',*,*,#10199,.F.);
#13363=ORIENTED_EDGE('',*,*,#10200,.F.);
#13364=ORIENTED_EDGE('',*,*,#9993,.F.);
#13365=ORIENTED_EDGE('',*,*,#10202,.T.);
#13366=ORIENTED_EDGE('',*,*,#10203,.T.);
#13367=ORIENTED_EDGE('',*,*,#10064,.T.);
#13368=ORIENTED_EDGE('',*,*,#10201,.F.);
#13369=ORIENTED_EDGE('',*,*,#10202,.F.);
#13370=ORIENTED_EDGE('',*,*,#9992,.F.);
#13371=ORIENTED_EDGE('',*,*,#10204,.T.);
#13372=ORIENTED_EDGE('',*,*,#10065,.T.);
#13373=ORIENTED_EDGE('',*,*,#10203,.F.);
#13374=ORIENTED_EDGE('',*,*,#10204,.F.);
#13375=ORIENTED_EDGE('',*,*,#9991,.F.);
#13376=ORIENTED_EDGE('',*,*,#10205,.T.);
#13377=ORIENTED_EDGE('',*,*,#10066,.T.);
#13378=ORIENTED_EDGE('',*,*,#10205,.F.);
#13379=ORIENTED_EDGE('',*,*,#9990,.F.);
#13380=ORIENTED_EDGE('',*,*,#10206,.T.);
#13381=ORIENTED_EDGE('',*,*,#10067,.T.);
#13382=ORIENTED_EDGE('',*,*,#10206,.F.);
#13383=ORIENTED_EDGE('',*,*,#9989,.F.);
#13384=ORIENTED_EDGE('',*,*,#10207,.T.);
#13385=ORIENTED_EDGE('',*,*,#10068,.T.);
#13386=ORIENTED_EDGE('',*,*,#10207,.F.);
#13387=ORIENTED_EDGE('',*,*,#9988,.F.);
#13388=ORIENTED_EDGE('',*,*,#10208,.T.);
#13389=ORIENTED_EDGE('',*,*,#10209,.T.);
#13390=ORIENTED_EDGE('',*,*,#10069,.T.);
#13391=ORIENTED_EDGE('',*,*,#10208,.F.);
#13392=ORIENTED_EDGE('',*,*,#9987,.F.);
#13393=ORIENTED_EDGE('',*,*,#10210,.T.);
#13394=ORIENTED_EDGE('',*,*,#10211,.T.);
#13395=ORIENTED_EDGE('',*,*,#10070,.T.);
#13396=ORIENTED_EDGE('',*,*,#10209,.F.);
#13397=ORIENTED_EDGE('',*,*,#10210,.F.);
#13398=ORIENTED_EDGE('',*,*,#9986,.F.);
#13399=ORIENTED_EDGE('',*,*,#10212,.T.);
#13400=ORIENTED_EDGE('',*,*,#10071,.T.);
#13401=ORIENTED_EDGE('',*,*,#10211,.F.);
#13402=ORIENTED_EDGE('',*,*,#10212,.F.);
#13403=ORIENTED_EDGE('',*,*,#9985,.F.);
#13404=ORIENTED_EDGE('',*,*,#10213,.T.);
#13405=ORIENTED_EDGE('',*,*,#10072,.T.);
#13406=ORIENTED_EDGE('',*,*,#10213,.F.);
#13407=ORIENTED_EDGE('',*,*,#9984,.F.);
#13408=ORIENTED_EDGE('',*,*,#10214,.T.);
#13409=ORIENTED_EDGE('',*,*,#10073,.T.);
#13410=ORIENTED_EDGE('',*,*,#10214,.F.);
#13411=ORIENTED_EDGE('',*,*,#9983,.F.);
#13412=ORIENTED_EDGE('',*,*,#10215,.T.);
#13413=ORIENTED_EDGE('',*,*,#10074,.T.);
#13414=ORIENTED_EDGE('',*,*,#10216,.F.);
#13415=ORIENTED_EDGE('',*,*,#10007,.F.);
#13416=ORIENTED_EDGE('',*,*,#10217,.T.);
#13417=ORIENTED_EDGE('',*,*,#10050,.T.);
#13418=ORIENTED_EDGE('',*,*,#10218,.F.);
#13419=ORIENTED_EDGE('',*,*,#10217,.F.);
#13420=ORIENTED_EDGE('',*,*,#10006,.F.);
#13421=ORIENTED_EDGE('',*,*,#10219,.T.);
#13422=ORIENTED_EDGE('',*,*,#10051,.T.);
#13423=ORIENTED_EDGE('',*,*,#10219,.F.);
#13424=ORIENTED_EDGE('',*,*,#10005,.F.);
#13425=ORIENTED_EDGE('',*,*,#10220,.T.);
#13426=ORIENTED_EDGE('',*,*,#10052,.T.);
#13427=ORIENTED_EDGE('',*,*,#10220,.F.);
#13428=ORIENTED_EDGE('',*,*,#10004,.F.);
#13429=ORIENTED_EDGE('',*,*,#10221,.T.);
#13430=ORIENTED_EDGE('',*,*,#10053,.T.);
#13431=ORIENTED_EDGE('',*,*,#10221,.F.);
#13432=ORIENTED_EDGE('',*,*,#10003,.F.);
#13433=ORIENTED_EDGE('',*,*,#10222,.T.);
#13434=ORIENTED_EDGE('',*,*,#10054,.T.);
#13435=ORIENTED_EDGE('',*,*,#10222,.F.);
#13436=ORIENTED_EDGE('',*,*,#10002,.F.);
#13437=ORIENTED_EDGE('',*,*,#10223,.T.);
#13438=ORIENTED_EDGE('',*,*,#10055,.T.);
#13439=ORIENTED_EDGE('',*,*,#10223,.F.);
#13440=ORIENTED_EDGE('',*,*,#10001,.F.);
#13441=ORIENTED_EDGE('',*,*,#10224,.T.);
#13442=ORIENTED_EDGE('',*,*,#10056,.T.);
#13443=ORIENTED_EDGE('',*,*,#10224,.F.);
#13444=ORIENTED_EDGE('',*,*,#10000,.F.);
#13445=ORIENTED_EDGE('',*,*,#10225,.T.);
#13446=ORIENTED_EDGE('',*,*,#10057,.T.);
#13447=ORIENTED_EDGE('',*,*,#10225,.F.);
#13448=ORIENTED_EDGE('',*,*,#9999,.F.);
#13449=ORIENTED_EDGE('',*,*,#10226,.T.);
#13450=ORIENTED_EDGE('',*,*,#10058,.T.);
#13451=ORIENTED_EDGE('',*,*,#10226,.F.);
#13452=ORIENTED_EDGE('',*,*,#9998,.F.);
#13453=ORIENTED_EDGE('',*,*,#10227,.T.);
#13454=ORIENTED_EDGE('',*,*,#10059,.T.);
#13455=ORIENTED_EDGE('',*,*,#10227,.F.);
#13456=ORIENTED_EDGE('',*,*,#9997,.F.);
#13457=ORIENTED_EDGE('',*,*,#10228,.T.);
#13458=ORIENTED_EDGE('',*,*,#10060,.T.);
#13459=ORIENTED_EDGE('',*,*,#10229,.F.);
#13460=ORIENTED_EDGE('',*,*,#9951,.F.);
#13461=ORIENTED_EDGE('',*,*,#10230,.T.);
#13462=ORIENTED_EDGE('',*,*,#10106,.T.);
#13463=ORIENTED_EDGE('',*,*,#10230,.F.);
#13464=ORIENTED_EDGE('',*,*,#9950,.F.);
#13465=ORIENTED_EDGE('',*,*,#10231,.T.);
#13466=ORIENTED_EDGE('',*,*,#10107,.T.);
#13467=ORIENTED_EDGE('',*,*,#10231,.F.);
#13468=ORIENTED_EDGE('',*,*,#9949,.F.);
#13469=ORIENTED_EDGE('',*,*,#10232,.T.);
#13470=ORIENTED_EDGE('',*,*,#10108,.T.);
#13471=ORIENTED_EDGE('',*,*,#10232,.F.);
#13472=ORIENTED_EDGE('',*,*,#9948,.F.);
#13473=ORIENTED_EDGE('',*,*,#10233,.T.);
#13474=ORIENTED_EDGE('',*,*,#10109,.T.);
#13475=ORIENTED_EDGE('',*,*,#10233,.F.);
#13476=ORIENTED_EDGE('',*,*,#9947,.F.);
#13477=ORIENTED_EDGE('',*,*,#10234,.T.);
#13478=ORIENTED_EDGE('',*,*,#10110,.T.);
#13479=ORIENTED_EDGE('',*,*,#10234,.F.);
#13480=ORIENTED_EDGE('',*,*,#9946,.F.);
#13481=ORIENTED_EDGE('',*,*,#10235,.T.);
#13482=ORIENTED_EDGE('',*,*,#10111,.T.);
#13483=ORIENTED_EDGE('',*,*,#10235,.F.);
#13484=ORIENTED_EDGE('',*,*,#9945,.F.);
#13485=ORIENTED_EDGE('',*,*,#10236,.T.);
#13486=ORIENTED_EDGE('',*,*,#10112,.T.);
#13487=ORIENTED_EDGE('',*,*,#10236,.F.);
#13488=ORIENTED_EDGE('',*,*,#9944,.F.);
#13489=ORIENTED_EDGE('',*,*,#10237,.T.);
#13490=ORIENTED_EDGE('',*,*,#10113,.T.);
#13491=ORIENTED_EDGE('',*,*,#10237,.F.);
#13492=ORIENTED_EDGE('',*,*,#9943,.F.);
#13493=ORIENTED_EDGE('',*,*,#10238,.T.);
#13494=ORIENTED_EDGE('',*,*,#10114,.T.);
#13495=ORIENTED_EDGE('',*,*,#10238,.F.);
#13496=ORIENTED_EDGE('',*,*,#9942,.F.);
#13497=ORIENTED_EDGE('',*,*,#10239,.T.);
#13498=ORIENTED_EDGE('',*,*,#10240,.T.);
#13499=ORIENTED_EDGE('',*,*,#10115,.T.);
#13500=ORIENTED_EDGE('',*,*,#10239,.F.);
#13501=ORIENTED_EDGE('',*,*,#9941,.F.);
#13502=ORIENTED_EDGE('',*,*,#10241,.T.);
#13503=ORIENTED_EDGE('',*,*,#10048,.T.);
#13504=ORIENTED_EDGE('',*,*,#10240,.F.);
#13505=ORIENTED_EDGE('',*,*,#10229,.T.);
#13506=ORIENTED_EDGE('',*,*,#10105,.T.);
#13507=ORIENTED_EDGE('',*,*,#10180,.F.);
#13508=ORIENTED_EDGE('',*,*,#9952,.F.);
#13509=ORIENTED_EDGE('',*,*,#10216,.T.);
#13510=ORIENTED_EDGE('',*,*,#10218,.T.);
#13511=ORIENTED_EDGE('',*,*,#10049,.T.);
#13512=ORIENTED_EDGE('',*,*,#10241,.F.);
#13513=ORIENTED_EDGE('',*,*,#10008,.F.);
#13514=ORIENTED_EDGE('',*,*,#10197,.T.);
#13515=ORIENTED_EDGE('',*,*,#10061,.T.);
#13516=ORIENTED_EDGE('',*,*,#10228,.F.);
#13517=ORIENTED_EDGE('',*,*,#9996,.F.);
#13518=ORIENTED_EDGE('',*,*,#9982,.F.);
#13519=ORIENTED_EDGE('',*,*,#10242,.T.);
#13520=ORIENTED_EDGE('',*,*,#10075,.T.);
#13521=ORIENTED_EDGE('',*,*,#10215,.F.);
#13522=ORIENTED_EDGE('',*,*,#10189,.T.);
#13523=ORIENTED_EDGE('',*,*,#10076,.T.);
#13524=ORIENTED_EDGE('',*,*,#10242,.F.);
#13525=ORIENTED_EDGE('',*,*,#9981,.F.);
#13526=ORIENTED_EDGE('',*,*,#10181,.T.);
#13527=ORIENTED_EDGE('',*,*,#10183,.T.);
#13528=ORIENTED_EDGE('',*,*,#10083,.T.);
#13529=ORIENTED_EDGE('',*,*,#10196,.F.);
#13530=ORIENTED_EDGE('',*,*,#9974,.F.);
#13531=ORIENTED_EDGE('',*,*,#9967,.F.);
#13532=ORIENTED_EDGE('',*,*,#10243,.T.);
#13533=ORIENTED_EDGE('',*,*,#10090,.T.);
#13534=ORIENTED_EDGE('',*,*,#10188,.F.);
#13535=ORIENTED_EDGE('',*,*,#10162,.T.);
#13536=ORIENTED_EDGE('',*,*,#10091,.T.);
#13537=ORIENTED_EDGE('',*,*,#10243,.F.);
#13538=ORIENTED_EDGE('',*,*,#9966,.F.);
#13539=ORIENTED_EDGE('',*,*,#10244,.T.);
#13540=ORIENTED_EDGE('',*,*,#10245,.T.);
#13541=ORIENTED_EDGE('',*,*,#10246,.T.);
#13542=ORIENTED_EDGE('',*,*,#10247,.T.);
#13543=ORIENTED_EDGE('',*,*,#10245,.F.);
#13544=ORIENTED_EDGE('',*,*,#10248,.T.);
#13545=ORIENTED_EDGE('',*,*,#10249,.F.);
#13546=ORIENTED_EDGE('',*,*,#10250,.F.);
#13547=ORIENTED_EDGE('',*,*,#10251,.T.);
#13548=ORIENTED_EDGE('',*,*,#10246,.F.);
#13549=ORIENTED_EDGE('',*,*,#10247,.F.);
#13550=ORIENTED_EDGE('',*,*,#10251,.F.);
#13551=ORIENTED_EDGE('',*,*,#10244,.F.);
#13552=ORIENTED_EDGE('',*,*,#10252,.T.);
#13553=ORIENTED_EDGE('',*,*,#10253,.F.);
#13554=ORIENTED_EDGE('',*,*,#10254,.F.);
#13555=ORIENTED_EDGE('',*,*,#10252,.F.);
#13556=ORIENTED_EDGE('',*,*,#10248,.F.);
#13557=ORIENTED_EDGE('',*,*,#10255,.T.);
#13558=ORIENTED_EDGE('',*,*,#10256,.T.);
#13559=ORIENTED_EDGE('',*,*,#10257,.T.);
#13560=ORIENTED_EDGE('',*,*,#10258,.T.);
#13561=ORIENTED_EDGE('',*,*,#10257,.F.);
#13562=ORIENTED_EDGE('',*,*,#10259,.T.);
#13563=ORIENTED_EDGE('',*,*,#10260,.T.);
#13564=ORIENTED_EDGE('',*,*,#10255,.F.);
#13565=ORIENTED_EDGE('',*,*,#10261,.T.);
#13566=ORIENTED_EDGE('',*,*,#10262,.T.);
#13567=ORIENTED_EDGE('',*,*,#10260,.F.);
#13568=ORIENTED_EDGE('',*,*,#10263,.T.);
#13569=ORIENTED_EDGE('',*,*,#10264,.F.);
#13570=ORIENTED_EDGE('',*,*,#10265,.T.);
#13571=ORIENTED_EDGE('',*,*,#10259,.F.);
#13572=ORIENTED_EDGE('',*,*,#10266,.T.);
#13573=ORIENTED_EDGE('',*,*,#10267,.T.);
#13574=ORIENTED_EDGE('',*,*,#10268,.T.);
#13575=ORIENTED_EDGE('',*,*,#10256,.F.);
#13576=ORIENTED_EDGE('',*,*,#10269,.F.);
#13577=ORIENTED_EDGE('',*,*,#10270,.F.);
#13578=ORIENTED_EDGE('',*,*,#10266,.F.);
#13579=ORIENTED_EDGE('',*,*,#10271,.T.);
#13580=ORIENTED_EDGE('',*,*,#10272,.T.);
#13581=ORIENTED_EDGE('',*,*,#10273,.T.);
#13582=ORIENTED_EDGE('',*,*,#10274,.T.);
#13583=ORIENTED_EDGE('',*,*,#10273,.F.);
#13584=ORIENTED_EDGE('',*,*,#10275,.T.);
#13585=ORIENTED_EDGE('',*,*,#10276,.T.);
#13586=ORIENTED_EDGE('',*,*,#10271,.F.);
#13587=ORIENTED_EDGE('',*,*,#10264,.T.);
#13588=ORIENTED_EDGE('',*,*,#10277,.T.);
#13589=ORIENTED_EDGE('',*,*,#10277,.F.);
#13590=ORIENTED_EDGE('',*,*,#10278,.T.);
#13591=ORIENTED_EDGE('',*,*,#10279,.F.);
#13592=ORIENTED_EDGE('',*,*,#10280,.T.);
#13593=ORIENTED_EDGE('',*,*,#10258,.F.);
#13594=ORIENTED_EDGE('',*,*,#10265,.F.);
#13595=ORIENTED_EDGE('',*,*,#10274,.F.);
#13596=ORIENTED_EDGE('',*,*,#10281,.F.);
#13597=ORIENTED_EDGE('',*,*,#10282,.T.);
#13598=ORIENTED_EDGE('',*,*,#10283,.T.);
#13599=ORIENTED_EDGE('',*,*,#10284,.T.);
#13600=ORIENTED_EDGE('',*,*,#10285,.T.);
#13601=ORIENTED_EDGE('',*,*,#10284,.F.);
#13602=ORIENTED_EDGE('',*,*,#10279,.T.);
#13603=ORIENTED_EDGE('',*,*,#10286,.T.);
#13604=ORIENTED_EDGE('',*,*,#10282,.F.);
#13605=ORIENTED_EDGE('',*,*,#10287,.T.);
#13606=ORIENTED_EDGE('',*,*,#10288,.T.);
#13607=ORIENTED_EDGE('',*,*,#10286,.F.);
#13608=ORIENTED_EDGE('',*,*,#10289,.T.);
#13609=ORIENTED_EDGE('',*,*,#10290,.F.);
#13610=ORIENTED_EDGE('',*,*,#10291,.T.);
#13611=ORIENTED_EDGE('',*,*,#10272,.F.);
#13612=ORIENTED_EDGE('',*,*,#10280,.F.);
#13613=ORIENTED_EDGE('',*,*,#10283,.F.);
#13614=ORIENTED_EDGE('',*,*,#10292,.F.);
#13615=ORIENTED_EDGE('',*,*,#10293,.T.);
#13616=ORIENTED_EDGE('',*,*,#10294,.T.);
#13617=ORIENTED_EDGE('',*,*,#10295,.T.);
#13618=ORIENTED_EDGE('',*,*,#10296,.T.);
#13619=ORIENTED_EDGE('',*,*,#10295,.F.);
#13620=ORIENTED_EDGE('',*,*,#10297,.T.);
#13621=ORIENTED_EDGE('',*,*,#10298,.T.);
#13622=ORIENTED_EDGE('',*,*,#10293,.F.);
#13623=ORIENTED_EDGE('',*,*,#10290,.T.);
#13624=ORIENTED_EDGE('',*,*,#10299,.T.);
#13625=ORIENTED_EDGE('',*,*,#10299,.F.);
#13626=ORIENTED_EDGE('',*,*,#10300,.T.);
#13627=ORIENTED_EDGE('',*,*,#10301,.T.);
#13628=ORIENTED_EDGE('',*,*,#10302,.T.);
#13629=ORIENTED_EDGE('',*,*,#10285,.F.);
#13630=ORIENTED_EDGE('',*,*,#10291,.F.);
#13631=ORIENTED_EDGE('',*,*,#10296,.F.);
#13632=ORIENTED_EDGE('',*,*,#10303,.F.);
#13633=ORIENTED_EDGE('',*,*,#10304,.T.);
#13634=ORIENTED_EDGE('',*,*,#10305,.T.);
#13635=ORIENTED_EDGE('',*,*,#10306,.T.);
#13636=ORIENTED_EDGE('',*,*,#10307,.T.);
#13637=ORIENTED_EDGE('',*,*,#10306,.F.);
#13638=ORIENTED_EDGE('',*,*,#10308,.T.);
#13639=ORIENTED_EDGE('',*,*,#10309,.T.);
#13640=ORIENTED_EDGE('',*,*,#10304,.F.);
#13641=ORIENTED_EDGE('',*,*,#10310,.T.);
#13642=ORIENTED_EDGE('',*,*,#10311,.T.);
#13643=ORIENTED_EDGE('',*,*,#10311,.F.);
#13644=ORIENTED_EDGE('',*,*,#10312,.T.);
#13645=ORIENTED_EDGE('',*,*,#10313,.F.);
#13646=ORIENTED_EDGE('',*,*,#10314,.T.);
#13647=ORIENTED_EDGE('',*,*,#10310,.F.);
#13648=ORIENTED_EDGE('',*,*,#10315,.T.);
#13649=ORIENTED_EDGE('',*,*,#10316,.F.);
#13650=ORIENTED_EDGE('',*,*,#10317,.T.);
#13651=ORIENTED_EDGE('',*,*,#10307,.F.);
#13652=ORIENTED_EDGE('',*,*,#10318,.F.);
#13653=ORIENTED_EDGE('',*,*,#10319,.F.);
#13654=ORIENTED_EDGE('',*,*,#10315,.F.);
#13655=ORIENTED_EDGE('',*,*,#10320,.T.);
#13656=ORIENTED_EDGE('',*,*,#10321,.T.);
#13657=ORIENTED_EDGE('',*,*,#10322,.T.);
#13658=ORIENTED_EDGE('',*,*,#10323,.T.);
#13659=ORIENTED_EDGE('',*,*,#10322,.F.);
#13660=ORIENTED_EDGE('',*,*,#10313,.T.);
#13661=ORIENTED_EDGE('',*,*,#10324,.T.);
#13662=ORIENTED_EDGE('',*,*,#10320,.F.);
#13663=ORIENTED_EDGE('',*,*,#10325,.T.);
#13664=ORIENTED_EDGE('',*,*,#10326,.T.);
#13665=ORIENTED_EDGE('',*,*,#10324,.F.);
#13666=ORIENTED_EDGE('',*,*,#10327,.T.);
#13667=ORIENTED_EDGE('',*,*,#10328,.F.);
#13668=ORIENTED_EDGE('',*,*,#10329,.T.);
#13669=ORIENTED_EDGE('',*,*,#10305,.F.);
#13670=ORIENTED_EDGE('',*,*,#10314,.F.);
#13671=ORIENTED_EDGE('',*,*,#10321,.F.);
#13672=ORIENTED_EDGE('',*,*,#10330,.F.);
#13673=ORIENTED_EDGE('',*,*,#10331,.T.);
#13674=ORIENTED_EDGE('',*,*,#10332,.T.);
#13675=ORIENTED_EDGE('',*,*,#10333,.T.);
#13676=ORIENTED_EDGE('',*,*,#10334,.T.);
#13677=ORIENTED_EDGE('',*,*,#10332,.F.);
#13678=ORIENTED_EDGE('',*,*,#10335,.F.);
#13679=ORIENTED_EDGE('',*,*,#10336,.F.);
#13680=ORIENTED_EDGE('',*,*,#10337,.F.);
#13681=ORIENTED_EDGE('',*,*,#10338,.F.);
#13682=ORIENTED_EDGE('',*,*,#10339,.F.);
#13683=ORIENTED_EDGE('',*,*,#10340,.F.);
#13684=ORIENTED_EDGE('',*,*,#10341,.F.);
#13685=ORIENTED_EDGE('',*,*,#10342,.F.);
#13686=ORIENTED_EDGE('',*,*,#10343,.F.);
#13687=ORIENTED_EDGE('',*,*,#10344,.F.);
#13688=ORIENTED_EDGE('',*,*,#10345,.F.);
#13689=ORIENTED_EDGE('',*,*,#10346,.F.);
#13690=ORIENTED_EDGE('',*,*,#10347,.F.);
#13691=ORIENTED_EDGE('',*,*,#10348,.F.);
#13692=ORIENTED_EDGE('',*,*,#10349,.F.);
#13693=ORIENTED_EDGE('',*,*,#10350,.F.);
#13694=ORIENTED_EDGE('',*,*,#10351,.F.);
#13695=ORIENTED_EDGE('',*,*,#10352,.F.);
#13696=ORIENTED_EDGE('',*,*,#10353,.F.);
#13697=ORIENTED_EDGE('',*,*,#10354,.F.);
#13698=ORIENTED_EDGE('',*,*,#10355,.F.);
#13699=ORIENTED_EDGE('',*,*,#10356,.F.);
#13700=ORIENTED_EDGE('',*,*,#10357,.F.);
#13701=ORIENTED_EDGE('',*,*,#10358,.F.);
#13702=ORIENTED_EDGE('',*,*,#10359,.F.);
#13703=ORIENTED_EDGE('',*,*,#10360,.F.);
#13704=ORIENTED_EDGE('',*,*,#10361,.F.);
#13705=ORIENTED_EDGE('',*,*,#10362,.F.);
#13706=ORIENTED_EDGE('',*,*,#10363,.F.);
#13707=ORIENTED_EDGE('',*,*,#10364,.F.);
#13708=ORIENTED_EDGE('',*,*,#10365,.F.);
#13709=ORIENTED_EDGE('',*,*,#10366,.F.);
#13710=ORIENTED_EDGE('',*,*,#10367,.F.);
#13711=ORIENTED_EDGE('',*,*,#10368,.F.);
#13712=ORIENTED_EDGE('',*,*,#10369,.F.);
#13713=ORIENTED_EDGE('',*,*,#10370,.F.);
#13714=ORIENTED_EDGE('',*,*,#10371,.F.);
#13715=ORIENTED_EDGE('',*,*,#10372,.F.);
#13716=ORIENTED_EDGE('',*,*,#10373,.F.);
#13717=ORIENTED_EDGE('',*,*,#10374,.F.);
#13718=ORIENTED_EDGE('',*,*,#10375,.F.);
#13719=ORIENTED_EDGE('',*,*,#10376,.F.);
#13720=ORIENTED_EDGE('',*,*,#10377,.F.);
#13721=ORIENTED_EDGE('',*,*,#10378,.F.);
#13722=ORIENTED_EDGE('',*,*,#10379,.F.);
#13723=ORIENTED_EDGE('',*,*,#10380,.F.);
#13724=ORIENTED_EDGE('',*,*,#10381,.F.);
#13725=ORIENTED_EDGE('',*,*,#10331,.F.);
#13726=ORIENTED_EDGE('',*,*,#10334,.F.);
#13727=ORIENTED_EDGE('',*,*,#10382,.T.);
#13728=ORIENTED_EDGE('',*,*,#10383,.F.);
#13729=ORIENTED_EDGE('',*,*,#10384,.F.);
#13730=ORIENTED_EDGE('',*,*,#10382,.F.);
#13731=ORIENTED_EDGE('',*,*,#10333,.F.);
#13732=ORIENTED_EDGE('',*,*,#10359,.T.);
#13733=ORIENTED_EDGE('',*,*,#10385,.T.);
#13734=ORIENTED_EDGE('',*,*,#10386,.T.);
#13735=ORIENTED_EDGE('',*,*,#10387,.T.);
#13736=ORIENTED_EDGE('',*,*,#10385,.F.);
#13737=ORIENTED_EDGE('',*,*,#10387,.F.);
#13738=ORIENTED_EDGE('',*,*,#10388,.T.);
#13739=ORIENTED_EDGE('',*,*,#10389,.F.);
#13740=ORIENTED_EDGE('',*,*,#10390,.F.);
#13741=ORIENTED_EDGE('',*,*,#10388,.F.);
#13742=ORIENTED_EDGE('',*,*,#10386,.F.);
#13743=ORIENTED_EDGE('',*,*,#10381,.T.);
#13744=ORIENTED_EDGE('',*,*,#10391,.T.);
#13745=ORIENTED_EDGE('',*,*,#10249,.T.);
#13746=ORIENTED_EDGE('',*,*,#10250,.T.);
#13747=ORIENTED_EDGE('',*,*,#10391,.F.);
#13748=ORIENTED_EDGE('',*,*,#10392,.T.);
#13749=ORIENTED_EDGE('',*,*,#10393,.T.);
#13750=ORIENTED_EDGE('',*,*,#10394,.T.);
#13751=ORIENTED_EDGE('',*,*,#10360,.T.);
#13752=ORIENTED_EDGE('',*,*,#10395,.T.);
#13753=ORIENTED_EDGE('',*,*,#10361,.T.);
#13754=ORIENTED_EDGE('',*,*,#10394,.F.);
#13755=ORIENTED_EDGE('',*,*,#10396,.T.);
#13756=ORIENTED_EDGE('',*,*,#10397,.T.);
#13757=ORIENTED_EDGE('',*,*,#10362,.T.);
#13758=ORIENTED_EDGE('',*,*,#10395,.F.);
#13759=ORIENTED_EDGE('',*,*,#10398,.T.);
#13760=ORIENTED_EDGE('',*,*,#10392,.F.);
#13761=ORIENTED_EDGE('',*,*,#10363,.T.);
#13762=ORIENTED_EDGE('',*,*,#10397,.F.);
#13763=ORIENTED_EDGE('',*,*,#10399,.T.);
#13764=ORIENTED_EDGE('',*,*,#10396,.F.);
#13765=ORIENTED_EDGE('',*,*,#10400,.T.);
#13766=ORIENTED_EDGE('',*,*,#10401,.F.);
#13767=ORIENTED_EDGE('',*,*,#10402,.F.);
#13768=ORIENTED_EDGE('',*,*,#10393,.F.);
#13769=ORIENTED_EDGE('',*,*,#10403,.T.);
#13770=ORIENTED_EDGE('',*,*,#10404,.F.);
#13771=ORIENTED_EDGE('',*,*,#10400,.F.);
#13772=ORIENTED_EDGE('',*,*,#10325,.F.);
#13773=ORIENTED_EDGE('',*,*,#10405,.T.);
#13774=ORIENTED_EDGE('',*,*,#10406,.T.);
#13775=ORIENTED_EDGE('',*,*,#10364,.T.);
#13776=ORIENTED_EDGE('',*,*,#10308,.F.);
#13777=ORIENTED_EDGE('',*,*,#10330,.T.);
#13778=ORIENTED_EDGE('',*,*,#10326,.F.);
#13779=ORIENTED_EDGE('',*,*,#10371,.T.);
#13780=ORIENTED_EDGE('',*,*,#10407,.T.);
#13781=ORIENTED_EDGE('',*,*,#10408,.T.);
#13782=ORIENTED_EDGE('',*,*,#10409,.T.);
#13783=ORIENTED_EDGE('',*,*,#10309,.F.);
#13784=ORIENTED_EDGE('',*,*,#10370,.T.);
#13785=ORIENTED_EDGE('',*,*,#10407,.F.);
#13786=ORIENTED_EDGE('',*,*,#10318,.T.);
#13787=ORIENTED_EDGE('',*,*,#10406,.F.);
#13788=ORIENTED_EDGE('',*,*,#10410,.T.);
#13789=ORIENTED_EDGE('',*,*,#10411,.T.);
#13790=ORIENTED_EDGE('',*,*,#10323,.F.);
#13791=ORIENTED_EDGE('',*,*,#10329,.F.);
#13792=ORIENTED_EDGE('',*,*,#10412,.F.);
#13793=ORIENTED_EDGE('',*,*,#10405,.F.);
#13794=ORIENTED_EDGE('',*,*,#10409,.F.);
#13795=ORIENTED_EDGE('',*,*,#10413,.T.);
#13796=ORIENTED_EDGE('',*,*,#10414,.T.);
#13797=ORIENTED_EDGE('',*,*,#10319,.T.);
#13798=ORIENTED_EDGE('',*,*,#10408,.F.);
#13799=ORIENTED_EDGE('',*,*,#10369,.T.);
#13800=ORIENTED_EDGE('',*,*,#10415,.T.);
#13801=ORIENTED_EDGE('',*,*,#10416,.T.);
#13802=ORIENTED_EDGE('',*,*,#10417,.T.);
#13803=ORIENTED_EDGE('',*,*,#10335,.T.);
#13804=ORIENTED_EDGE('',*,*,#10418,.T.);
#13805=ORIENTED_EDGE('',*,*,#10419,.T.);
#13806=ORIENTED_EDGE('',*,*,#10418,.F.);
#13807=ORIENTED_EDGE('',*,*,#10420,.T.);
#13808=ORIENTED_EDGE('',*,*,#10421,.T.);
#13809=ORIENTED_EDGE('',*,*,#10420,.F.);
#13810=ORIENTED_EDGE('',*,*,#10358,.T.);
#13811=ORIENTED_EDGE('',*,*,#10422,.T.);
#13812=ORIENTED_EDGE('',*,*,#10423,.T.);
#13813=ORIENTED_EDGE('',*,*,#10424,.F.);
#13814=ORIENTED_EDGE('',*,*,#10425,.F.);
#13815=ORIENTED_EDGE('',*,*,#10426,.F.);
#13816=ORIENTED_EDGE('',*,*,#10427,.T.);
#13817=ORIENTED_EDGE('',*,*,#10428,.T.);
#13818=ORIENTED_EDGE('',*,*,#10429,.T.);
#13819=ORIENTED_EDGE('',*,*,#10427,.F.);
#13820=ORIENTED_EDGE('',*,*,#10347,.T.);
#13821=ORIENTED_EDGE('',*,*,#10425,.T.);
#13822=ORIENTED_EDGE('',*,*,#10430,.T.);
#13823=ORIENTED_EDGE('',*,*,#10431,.F.);
#13824=ORIENTED_EDGE('',*,*,#10432,.F.);
#13825=ORIENTED_EDGE('',*,*,#10433,.F.);
#13826=ORIENTED_EDGE('',*,*,#10432,.T.);
#13827=ORIENTED_EDGE('',*,*,#10434,.T.);
#13828=ORIENTED_EDGE('',*,*,#10426,.T.);
#13829=ORIENTED_EDGE('',*,*,#10346,.T.);
#13830=ORIENTED_EDGE('',*,*,#10435,.F.);
#13831=ORIENTED_EDGE('',*,*,#10436,.F.);
#13832=ORIENTED_EDGE('',*,*,#10437,.F.);
#13833=ORIENTED_EDGE('',*,*,#10436,.T.);
#13834=ORIENTED_EDGE('',*,*,#10438,.T.);
#13835=ORIENTED_EDGE('',*,*,#10433,.T.);
#13836=ORIENTED_EDGE('',*,*,#10345,.T.);
#13837=ORIENTED_EDGE('',*,*,#10439,.T.);
#13838=ORIENTED_EDGE('',*,*,#10440,.T.);
#13839=ORIENTED_EDGE('',*,*,#10437,.T.);
#13840=ORIENTED_EDGE('',*,*,#10344,.T.);
#13841=ORIENTED_EDGE('',*,*,#10439,.F.);
#13842=ORIENTED_EDGE('',*,*,#10441,.T.);
#13843=ORIENTED_EDGE('',*,*,#10442,.T.);
#13844=ORIENTED_EDGE('',*,*,#10443,.T.);
#13845=ORIENTED_EDGE('',*,*,#10444,.T.);
#13846=ORIENTED_EDGE('',*,*,#10435,.T.);
#13847=ORIENTED_EDGE('',*,*,#10445,.T.);
#13848=ORIENTED_EDGE('',*,*,#10443,.F.);
#13849=ORIENTED_EDGE('',*,*,#10446,.T.);
#13850=ORIENTED_EDGE('',*,*,#10447,.T.);
#13851=ORIENTED_EDGE('',*,*,#10448,.T.);
#13852=ORIENTED_EDGE('',*,*,#10449,.T.);
#13853=ORIENTED_EDGE('',*,*,#10431,.T.);
#13854=ORIENTED_EDGE('',*,*,#10450,.T.);
#13855=ORIENTED_EDGE('',*,*,#10448,.F.);
#13856=ORIENTED_EDGE('',*,*,#10451,.T.);
#13857=ORIENTED_EDGE('',*,*,#10452,.T.);
#13858=ORIENTED_EDGE('',*,*,#10453,.T.);
#13859=ORIENTED_EDGE('',*,*,#10454,.T.);
#13860=ORIENTED_EDGE('',*,*,#10424,.T.);
#13861=ORIENTED_EDGE('',*,*,#10455,.T.);
#13862=ORIENTED_EDGE('',*,*,#10453,.F.);
#13863=ORIENTED_EDGE('',*,*,#10456,.T.);
#13864=ORIENTED_EDGE('',*,*,#10457,.T.);
#13865=ORIENTED_EDGE('',*,*,#10455,.F.);
#13866=ORIENTED_EDGE('',*,*,#10434,.F.);
#13867=ORIENTED_EDGE('',*,*,#10449,.F.);
#13868=ORIENTED_EDGE('',*,*,#10458,.F.);
#13869=ORIENTED_EDGE('',*,*,#10450,.F.);
#13870=ORIENTED_EDGE('',*,*,#10438,.F.);
#13871=ORIENTED_EDGE('',*,*,#10444,.F.);
#13872=ORIENTED_EDGE('',*,*,#10459,.F.);
#13873=ORIENTED_EDGE('',*,*,#10451,.F.);
#13874=ORIENTED_EDGE('',*,*,#10459,.T.);
#13875=ORIENTED_EDGE('',*,*,#10447,.F.);
#13876=ORIENTED_EDGE('',*,*,#10460,.T.);
#13877=ORIENTED_EDGE('',*,*,#10446,.F.);
#13878=ORIENTED_EDGE('',*,*,#10461,.T.);
#13879=ORIENTED_EDGE('',*,*,#10462,.F.);
#13880=ORIENTED_EDGE('',*,*,#10463,.T.);
#13881=ORIENTED_EDGE('',*,*,#10445,.F.);
#13882=ORIENTED_EDGE('',*,*,#10440,.F.);
#13883=ORIENTED_EDGE('',*,*,#10464,.F.);
#13884=ORIENTED_EDGE('',*,*,#10461,.F.);
#13885=ORIENTED_EDGE('',*,*,#10465,.F.);
#13886=ORIENTED_EDGE('',*,*,#10466,.F.);
#13887=ORIENTED_EDGE('',*,*,#10467,.F.);
#13888=ORIENTED_EDGE('',*,*,#10468,.T.);
#13889=ORIENTED_EDGE('',*,*,#10469,.T.);
#13890=ORIENTED_EDGE('',*,*,#10470,.T.);
#13891=ORIENTED_EDGE('',*,*,#10468,.F.);
#13892=ORIENTED_EDGE('',*,*,#10471,.T.);
#13893=ORIENTED_EDGE('',*,*,#10466,.T.);
#13894=ORIENTED_EDGE('',*,*,#10472,.T.);
#13895=ORIENTED_EDGE('',*,*,#10473,.T.);
#13896=ORIENTED_EDGE('',*,*,#10373,.T.);
#13897=ORIENTED_EDGE('',*,*,#10467,.T.);
#13898=ORIENTED_EDGE('',*,*,#10474,.T.);
#13899=ORIENTED_EDGE('',*,*,#10473,.F.);
#13900=ORIENTED_EDGE('',*,*,#10475,.T.);
#13901=ORIENTED_EDGE('',*,*,#10476,.T.);
#13902=ORIENTED_EDGE('',*,*,#10477,.T.);
#13903=ORIENTED_EDGE('',*,*,#10478,.T.);
#13904=ORIENTED_EDGE('',*,*,#10465,.T.);
#13905=ORIENTED_EDGE('',*,*,#10380,.T.);
#13906=ORIENTED_EDGE('',*,*,#10297,.F.);
#13907=ORIENTED_EDGE('',*,*,#10479,.T.);
#13908=ORIENTED_EDGE('',*,*,#10480,.T.);
#13909=ORIENTED_EDGE('',*,*,#10379,.T.);
#13910=ORIENTED_EDGE('',*,*,#10287,.F.);
#13911=ORIENTED_EDGE('',*,*,#10303,.T.);
#13912=ORIENTED_EDGE('',*,*,#10298,.F.);
#13913=ORIENTED_EDGE('',*,*,#10378,.T.);
#13914=ORIENTED_EDGE('',*,*,#10275,.F.);
#13915=ORIENTED_EDGE('',*,*,#10292,.T.);
#13916=ORIENTED_EDGE('',*,*,#10288,.F.);
#13917=ORIENTED_EDGE('',*,*,#10377,.T.);
#13918=ORIENTED_EDGE('',*,*,#10261,.F.);
#13919=ORIENTED_EDGE('',*,*,#10281,.T.);
#13920=ORIENTED_EDGE('',*,*,#10276,.F.);
#13921=ORIENTED_EDGE('',*,*,#10376,.T.);
#13922=ORIENTED_EDGE('',*,*,#10481,.T.);
#13923=ORIENTED_EDGE('',*,*,#10482,.T.);
#13924=ORIENTED_EDGE('',*,*,#10483,.T.);
#13925=ORIENTED_EDGE('',*,*,#10262,.F.);
#13926=ORIENTED_EDGE('',*,*,#10375,.T.);
#13927=ORIENTED_EDGE('',*,*,#10481,.F.);
#13928=ORIENTED_EDGE('',*,*,#10269,.T.);
#13929=ORIENTED_EDGE('',*,*,#10480,.F.);
#13930=ORIENTED_EDGE('',*,*,#10484,.T.);
#13931=ORIENTED_EDGE('',*,*,#10477,.F.);
#13932=ORIENTED_EDGE('',*,*,#10470,.F.);
#13933=ORIENTED_EDGE('',*,*,#10485,.T.);
#13934=ORIENTED_EDGE('',*,*,#10486,.F.);
#13935=ORIENTED_EDGE('',*,*,#10487,.T.);
#13936=ORIENTED_EDGE('',*,*,#10469,.F.);
#13937=ORIENTED_EDGE('',*,*,#10488,.T.);
#13938=ORIENTED_EDGE('',*,*,#10489,.F.);
#13939=ORIENTED_EDGE('',*,*,#10490,.T.);
#13940=ORIENTED_EDGE('',*,*,#10472,.F.);
#13941=ORIENTED_EDGE('',*,*,#10478,.F.);
#13942=ORIENTED_EDGE('',*,*,#10491,.F.);
#13943=ORIENTED_EDGE('',*,*,#10488,.F.);
#13944=ORIENTED_EDGE('',*,*,#10484,.F.);
#13945=ORIENTED_EDGE('',*,*,#10492,.T.);
#13946=ORIENTED_EDGE('',*,*,#10493,.T.);
#13947=ORIENTED_EDGE('',*,*,#10491,.T.);
#13948=ORIENTED_EDGE('',*,*,#10294,.F.);
#13949=ORIENTED_EDGE('',*,*,#10302,.F.);
#13950=ORIENTED_EDGE('',*,*,#10492,.F.);
#13951=ORIENTED_EDGE('',*,*,#10479,.F.);
#13952=ORIENTED_EDGE('',*,*,#10483,.F.);
#13953=ORIENTED_EDGE('',*,*,#10494,.T.);
#13954=ORIENTED_EDGE('',*,*,#10495,.T.);
#13955=ORIENTED_EDGE('',*,*,#10270,.T.);
#13956=ORIENTED_EDGE('',*,*,#10372,.T.);
#13957=ORIENTED_EDGE('',*,*,#10496,.T.);
#13958=ORIENTED_EDGE('',*,*,#10497,.T.);
#13959=ORIENTED_EDGE('',*,*,#10498,.T.);
#13960=ORIENTED_EDGE('',*,*,#10496,.F.);
#13961=ORIENTED_EDGE('',*,*,#10498,.F.);
#13962=ORIENTED_EDGE('',*,*,#10499,.T.);
#13963=ORIENTED_EDGE('',*,*,#10500,.F.);
#13964=ORIENTED_EDGE('',*,*,#10501,.F.);
#13965=ORIENTED_EDGE('',*,*,#10499,.F.);
#13966=ORIENTED_EDGE('',*,*,#10497,.F.);
#13967=ORIENTED_EDGE('',*,*,#10502,.F.);
#13968=ORIENTED_EDGE('',*,*,#10503,.F.);
#13969=ORIENTED_EDGE('',*,*,#10504,.F.);
#13970=ORIENTED_EDGE('',*,*,#10441,.F.);
#13971=ORIENTED_EDGE('',*,*,#10343,.T.);
#13972=ORIENTED_EDGE('',*,*,#10503,.T.);
#13973=ORIENTED_EDGE('',*,*,#10505,.T.);
#13974=ORIENTED_EDGE('',*,*,#10506,.F.);
#13975=ORIENTED_EDGE('',*,*,#10507,.F.);
#13976=ORIENTED_EDGE('',*,*,#10508,.F.);
#13977=ORIENTED_EDGE('',*,*,#10507,.T.);
#13978=ORIENTED_EDGE('',*,*,#10509,.T.);
#13979=ORIENTED_EDGE('',*,*,#10504,.T.);
#13980=ORIENTED_EDGE('',*,*,#10342,.T.);
#13981=ORIENTED_EDGE('',*,*,#10510,.F.);
#13982=ORIENTED_EDGE('',*,*,#10511,.F.);
#13983=ORIENTED_EDGE('',*,*,#10512,.F.);
#13984=ORIENTED_EDGE('',*,*,#10511,.T.);
#13985=ORIENTED_EDGE('',*,*,#10513,.T.);
#13986=ORIENTED_EDGE('',*,*,#10508,.T.);
#13987=ORIENTED_EDGE('',*,*,#10341,.T.);
#13988=ORIENTED_EDGE('',*,*,#10514,.F.);
#13989=ORIENTED_EDGE('',*,*,#10515,.F.);
#13990=ORIENTED_EDGE('',*,*,#10516,.F.);
#13991=ORIENTED_EDGE('',*,*,#10515,.T.);
#13992=ORIENTED_EDGE('',*,*,#10517,.T.);
#13993=ORIENTED_EDGE('',*,*,#10512,.T.);
#13994=ORIENTED_EDGE('',*,*,#10340,.T.);
#13995=ORIENTED_EDGE('',*,*,#10518,.T.);
#13996=ORIENTED_EDGE('',*,*,#10516,.T.);
#13997=ORIENTED_EDGE('',*,*,#10339,.T.);
#13998=ORIENTED_EDGE('',*,*,#10519,.T.);
#13999=ORIENTED_EDGE('',*,*,#10338,.T.);
#14000=ORIENTED_EDGE('',*,*,#10520,.T.);
#14001=ORIENTED_EDGE('',*,*,#10521,.T.);
#14002=ORIENTED_EDGE('',*,*,#10519,.F.);
#14003=ORIENTED_EDGE('',*,*,#10522,.F.);
#14004=ORIENTED_EDGE('',*,*,#10523,.F.);
#14005=ORIENTED_EDGE('',*,*,#10524,.F.);
#14006=ORIENTED_EDGE('',*,*,#10337,.T.);
#14007=ORIENTED_EDGE('',*,*,#10523,.T.);
#14008=ORIENTED_EDGE('',*,*,#10525,.T.);
#14009=ORIENTED_EDGE('',*,*,#10520,.F.);
#14010=ORIENTED_EDGE('',*,*,#10526,.T.);
#14011=ORIENTED_EDGE('',*,*,#10524,.T.);
#14012=ORIENTED_EDGE('',*,*,#10336,.T.);
#14013=ORIENTED_EDGE('',*,*,#10417,.F.);
#14014=ORIENTED_EDGE('',*,*,#10527,.T.);
#14015=ORIENTED_EDGE('',*,*,#10528,.T.);
#14016=ORIENTED_EDGE('',*,*,#10522,.T.);
#14017=ORIENTED_EDGE('',*,*,#10529,.T.);
#14018=ORIENTED_EDGE('',*,*,#10527,.F.);
#14019=ORIENTED_EDGE('',*,*,#10530,.T.);
#14020=ORIENTED_EDGE('',*,*,#10531,.T.);
#14021=ORIENTED_EDGE('',*,*,#10532,.T.);
#14022=ORIENTED_EDGE('',*,*,#10533,.T.);
#14023=ORIENTED_EDGE('',*,*,#10514,.T.);
#14024=ORIENTED_EDGE('',*,*,#10534,.T.);
#14025=ORIENTED_EDGE('',*,*,#10532,.F.);
#14026=ORIENTED_EDGE('',*,*,#10535,.T.);
#14027=ORIENTED_EDGE('',*,*,#10536,.T.);
#14028=ORIENTED_EDGE('',*,*,#10537,.T.);
#14029=ORIENTED_EDGE('',*,*,#10538,.T.);
#14030=ORIENTED_EDGE('',*,*,#10510,.T.);
#14031=ORIENTED_EDGE('',*,*,#10539,.T.);
#14032=ORIENTED_EDGE('',*,*,#10537,.F.);
#14033=ORIENTED_EDGE('',*,*,#10540,.T.);
#14034=ORIENTED_EDGE('',*,*,#10541,.T.);
#14035=ORIENTED_EDGE('',*,*,#10542,.T.);
#14036=ORIENTED_EDGE('',*,*,#10543,.T.);
#14037=ORIENTED_EDGE('',*,*,#10506,.T.);
#14038=ORIENTED_EDGE('',*,*,#10544,.T.);
#14039=ORIENTED_EDGE('',*,*,#10542,.F.);
#14040=ORIENTED_EDGE('',*,*,#10545,.T.);
#14041=ORIENTED_EDGE('',*,*,#10546,.T.);
#14042=ORIENTED_EDGE('',*,*,#10547,.T.);
#14043=ORIENTED_EDGE('',*,*,#10548,.T.);
#14044=ORIENTED_EDGE('',*,*,#10502,.T.);
#14045=ORIENTED_EDGE('',*,*,#10549,.T.);
#14046=ORIENTED_EDGE('',*,*,#10547,.F.);
#14047=ORIENTED_EDGE('',*,*,#10550,.T.);
#14048=ORIENTED_EDGE('',*,*,#10551,.T.);
#14049=ORIENTED_EDGE('',*,*,#10442,.F.);
#14050=ORIENTED_EDGE('',*,*,#10552,.T.);
#14051=ORIENTED_EDGE('',*,*,#10553,.T.);
#14052=ORIENTED_EDGE('',*,*,#10464,.T.);
#14053=ORIENTED_EDGE('',*,*,#10553,.F.);
#14054=ORIENTED_EDGE('',*,*,#10554,.T.);
#14055=ORIENTED_EDGE('',*,*,#10462,.T.);
#14056=ORIENTED_EDGE('',*,*,#10544,.F.);
#14057=ORIENTED_EDGE('',*,*,#10513,.F.);
#14058=ORIENTED_EDGE('',*,*,#10538,.F.);
#14059=ORIENTED_EDGE('',*,*,#10555,.F.);
#14060=ORIENTED_EDGE('',*,*,#10546,.F.);
#14061=ORIENTED_EDGE('',*,*,#10556,.T.);
#14062=ORIENTED_EDGE('',*,*,#10550,.F.);
#14063=ORIENTED_EDGE('',*,*,#10557,.T.);
#14064=ORIENTED_EDGE('',*,*,#10545,.F.);
#14065=ORIENTED_EDGE('',*,*,#10555,.T.);
#14066=ORIENTED_EDGE('',*,*,#10541,.F.);
#14067=ORIENTED_EDGE('',*,*,#10558,.T.);
#14068=ORIENTED_EDGE('',*,*,#10539,.F.);
#14069=ORIENTED_EDGE('',*,*,#10517,.F.);
#14070=ORIENTED_EDGE('',*,*,#10533,.F.);
#14071=ORIENTED_EDGE('',*,*,#10559,.F.);
#14072=ORIENTED_EDGE('',*,*,#10540,.F.);
#14073=ORIENTED_EDGE('',*,*,#10559,.T.);
#14074=ORIENTED_EDGE('',*,*,#10536,.F.);
#14075=ORIENTED_EDGE('',*,*,#10560,.T.);
#14076=ORIENTED_EDGE('',*,*,#10535,.F.);
#14077=ORIENTED_EDGE('',*,*,#10561,.T.);
#14078=ORIENTED_EDGE('',*,*,#10562,.F.);
#14079=ORIENTED_EDGE('',*,*,#10563,.T.);
#14080=ORIENTED_EDGE('',*,*,#10534,.F.);
#14081=ORIENTED_EDGE('',*,*,#10518,.F.);
#14082=ORIENTED_EDGE('',*,*,#10564,.T.);
#14083=ORIENTED_EDGE('',*,*,#10561,.F.);
#14084=ORIENTED_EDGE('',*,*,#10521,.F.);
#14085=ORIENTED_EDGE('',*,*,#10565,.T.);
#14086=ORIENTED_EDGE('',*,*,#10566,.F.);
#14087=ORIENTED_EDGE('',*,*,#10564,.F.);
#14088=ORIENTED_EDGE('',*,*,#10525,.F.);
#14089=ORIENTED_EDGE('',*,*,#10528,.F.);
#14090=ORIENTED_EDGE('',*,*,#10567,.F.);
#14091=ORIENTED_EDGE('',*,*,#10565,.F.);
#14092=ORIENTED_EDGE('',*,*,#10531,.F.);
#14093=ORIENTED_EDGE('',*,*,#10568,.T.);
#14094=ORIENTED_EDGE('',*,*,#10569,.T.);
#14095=ORIENTED_EDGE('',*,*,#10567,.T.);
#14096=ORIENTED_EDGE('',*,*,#10530,.F.);
#14097=ORIENTED_EDGE('',*,*,#10570,.T.);
#14098=ORIENTED_EDGE('',*,*,#10571,.T.);
#14099=ORIENTED_EDGE('',*,*,#10572,.T.);
#14100=ORIENTED_EDGE('',*,*,#10529,.F.);
#14101=ORIENTED_EDGE('',*,*,#10526,.F.);
#14102=ORIENTED_EDGE('',*,*,#10573,.T.);
#14103=ORIENTED_EDGE('',*,*,#10570,.F.);
#14104=ORIENTED_EDGE('',*,*,#10574,.T.);
#14105=ORIENTED_EDGE('',*,*,#10575,.T.);
#14106=ORIENTED_EDGE('',*,*,#10500,.T.);
#14107=ORIENTED_EDGE('',*,*,#10501,.T.);
#14108=ORIENTED_EDGE('',*,*,#10575,.F.);
#14109=ORIENTED_EDGE('',*,*,#10576,.F.);
#14110=ORIENTED_EDGE('',*,*,#10577,.F.);
#14111=ORIENTED_EDGE('',*,*,#10578,.F.);
#14112=ORIENTED_EDGE('',*,*,#10579,.F.);
#14113=ORIENTED_EDGE('',*,*,#10580,.F.);
#14114=ORIENTED_EDGE('',*,*,#10581,.F.);
#14115=ORIENTED_EDGE('',*,*,#10582,.F.);
#14116=ORIENTED_EDGE('',*,*,#10583,.F.);
#14117=ORIENTED_EDGE('',*,*,#10584,.F.);
#14118=ORIENTED_EDGE('',*,*,#10585,.F.);
#14119=ORIENTED_EDGE('',*,*,#10586,.F.);
#14120=ORIENTED_EDGE('',*,*,#10587,.F.);
#14121=ORIENTED_EDGE('',*,*,#10588,.F.);
#14122=ORIENTED_EDGE('',*,*,#10589,.F.);
#14123=ORIENTED_EDGE('',*,*,#10460,.F.);
#14124=ORIENTED_EDGE('',*,*,#10463,.F.);
#14125=ORIENTED_EDGE('',*,*,#10590,.F.);
#14126=ORIENTED_EDGE('',*,*,#10556,.F.);
#14127=ORIENTED_EDGE('',*,*,#10558,.F.);
#14128=ORIENTED_EDGE('',*,*,#10560,.F.);
#14129=ORIENTED_EDGE('',*,*,#10563,.F.);
#14130=ORIENTED_EDGE('',*,*,#10591,.F.);
#14131=ORIENTED_EDGE('',*,*,#10568,.F.);
#14132=ORIENTED_EDGE('',*,*,#10572,.F.);
#14133=ORIENTED_EDGE('',*,*,#10592,.F.);
#14134=ORIENTED_EDGE('',*,*,#10593,.F.);
#14135=ORIENTED_EDGE('',*,*,#10594,.F.);
#14136=ORIENTED_EDGE('',*,*,#10595,.F.);
#14137=ORIENTED_EDGE('',*,*,#10596,.F.);
#14138=ORIENTED_EDGE('',*,*,#10327,.F.);
#14139=ORIENTED_EDGE('',*,*,#10312,.F.);
#14140=ORIENTED_EDGE('',*,*,#10317,.F.);
#14141=ORIENTED_EDGE('',*,*,#10597,.F.);
#14142=ORIENTED_EDGE('',*,*,#10598,.F.);
#14143=ORIENTED_EDGE('',*,*,#10599,.F.);
#14144=ORIENTED_EDGE('',*,*,#10600,.F.);
#14145=ORIENTED_EDGE('',*,*,#10601,.F.);
#14146=ORIENTED_EDGE('',*,*,#10300,.F.);
#14147=ORIENTED_EDGE('',*,*,#10289,.F.);
#14148=ORIENTED_EDGE('',*,*,#10278,.F.);
#14149=ORIENTED_EDGE('',*,*,#10263,.F.);
#14150=ORIENTED_EDGE('',*,*,#10268,.F.);
#14151=ORIENTED_EDGE('',*,*,#10602,.F.);
#14152=ORIENTED_EDGE('',*,*,#10485,.F.);
#14153=ORIENTED_EDGE('',*,*,#10490,.F.);
#14154=ORIENTED_EDGE('',*,*,#10603,.F.);
#14155=ORIENTED_EDGE('',*,*,#10604,.F.);
#14156=ORIENTED_EDGE('',*,*,#10574,.F.);
#14157=ORIENTED_EDGE('',*,*,#10495,.F.);
#14158=ORIENTED_EDGE('',*,*,#10605,.F.);
#14159=ORIENTED_EDGE('',*,*,#10267,.F.);
#14160=ORIENTED_EDGE('',*,*,#10606,.T.);
#14161=ORIENTED_EDGE('',*,*,#10602,.T.);
#14162=ORIENTED_EDGE('',*,*,#10605,.T.);
#14163=ORIENTED_EDGE('',*,*,#10607,.T.);
#14164=ORIENTED_EDGE('',*,*,#10476,.F.);
#14165=ORIENTED_EDGE('',*,*,#10608,.T.);
#14166=ORIENTED_EDGE('',*,*,#10482,.F.);
#14167=ORIENTED_EDGE('',*,*,#10374,.T.);
#14168=ORIENTED_EDGE('',*,*,#10475,.F.);
#14169=ORIENTED_EDGE('',*,*,#10609,.T.);
#14170=ORIENTED_EDGE('',*,*,#10610,.T.);
#14171=ORIENTED_EDGE('',*,*,#10611,.T.);
#14172=ORIENTED_EDGE('',*,*,#10610,.F.);
#14173=ORIENTED_EDGE('',*,*,#10486,.T.);
#14174=ORIENTED_EDGE('',*,*,#10606,.F.);
#14175=ORIENTED_EDGE('',*,*,#10301,.F.);
#14176=ORIENTED_EDGE('',*,*,#10489,.T.);
#14177=ORIENTED_EDGE('',*,*,#10493,.F.);
#14178=ORIENTED_EDGE('',*,*,#10471,.F.);
#14179=ORIENTED_EDGE('',*,*,#10487,.F.);
#14180=ORIENTED_EDGE('',*,*,#10609,.F.);
#14181=ORIENTED_EDGE('',*,*,#10474,.F.);
#14182=ORIENTED_EDGE('',*,*,#10607,.F.);
#14183=ORIENTED_EDGE('',*,*,#10494,.F.);
#14184=ORIENTED_EDGE('',*,*,#10608,.F.);
#14185=ORIENTED_EDGE('',*,*,#10611,.F.);
#14186=ORIENTED_EDGE('',*,*,#10591,.T.);
#14187=ORIENTED_EDGE('',*,*,#10562,.T.);
#14188=ORIENTED_EDGE('',*,*,#10566,.T.);
#14189=ORIENTED_EDGE('',*,*,#10569,.F.);
#14190=ORIENTED_EDGE('',*,*,#10551,.F.);
#14191=ORIENTED_EDGE('',*,*,#10590,.T.);
#14192=ORIENTED_EDGE('',*,*,#10554,.F.);
#14193=ORIENTED_EDGE('',*,*,#10612,.T.);
#14194=ORIENTED_EDGE('',*,*,#10456,.F.);
#14195=ORIENTED_EDGE('',*,*,#10458,.T.);
#14196=ORIENTED_EDGE('',*,*,#10452,.F.);
#14197=ORIENTED_EDGE('',*,*,#10589,.T.);
#14198=ORIENTED_EDGE('',*,*,#10613,.T.);
#14199=ORIENTED_EDGE('',*,*,#10614,.T.);
#14200=ORIENTED_EDGE('',*,*,#10615,.T.);
#14201=ORIENTED_EDGE('',*,*,#10457,.F.);
#14202=ORIENTED_EDGE('',*,*,#10588,.T.);
#14203=ORIENTED_EDGE('',*,*,#10613,.F.);
#14204=ORIENTED_EDGE('',*,*,#10616,.T.);
#14205=ORIENTED_EDGE('',*,*,#10543,.F.);
#14206=ORIENTED_EDGE('',*,*,#10557,.F.);
#14207=ORIENTED_EDGE('',*,*,#10549,.F.);
#14208=ORIENTED_EDGE('',*,*,#10509,.F.);
#14209=ORIENTED_EDGE('',*,*,#10548,.F.);
#14210=ORIENTED_EDGE('',*,*,#10612,.F.);
#14211=ORIENTED_EDGE('',*,*,#10552,.F.);
#14212=ORIENTED_EDGE('',*,*,#10505,.F.);
#14213=ORIENTED_EDGE('',*,*,#10454,.F.);
#14214=ORIENTED_EDGE('',*,*,#10616,.F.);
#14215=ORIENTED_EDGE('',*,*,#10617,.F.);
#14216=ORIENTED_EDGE('',*,*,#10430,.F.);
#14217=ORIENTED_EDGE('',*,*,#10428,.F.);
#14218=ORIENTED_EDGE('',*,*,#10617,.T.);
#14219=ORIENTED_EDGE('',*,*,#10615,.F.);
#14220=ORIENTED_EDGE('',*,*,#10618,.T.);
#14221=ORIENTED_EDGE('',*,*,#10619,.F.);
#14222=ORIENTED_EDGE('',*,*,#10415,.F.);
#14223=ORIENTED_EDGE('',*,*,#10620,.F.);
#14224=ORIENTED_EDGE('',*,*,#10621,.F.);
#14225=ORIENTED_EDGE('',*,*,#10622,.F.);
#14226=ORIENTED_EDGE('',*,*,#10623,.F.);
#14227=ORIENTED_EDGE('',*,*,#10620,.T.);
#14228=ORIENTED_EDGE('',*,*,#10368,.T.);
#14229=ORIENTED_EDGE('',*,*,#10622,.T.);
#14230=ORIENTED_EDGE('',*,*,#10624,.T.);
#14231=ORIENTED_EDGE('',*,*,#10625,.T.);
#14232=ORIENTED_EDGE('',*,*,#10626,.T.);
#14233=ORIENTED_EDGE('',*,*,#10627,.T.);
#14234=ORIENTED_EDGE('',*,*,#10625,.F.);
#14235=ORIENTED_EDGE('',*,*,#10628,.T.);
#14236=ORIENTED_EDGE('',*,*,#10623,.T.);
#14237=ORIENTED_EDGE('',*,*,#10367,.T.);
#14238=ORIENTED_EDGE('',*,*,#10629,.T.);
#14239=ORIENTED_EDGE('',*,*,#10630,.T.);
#14240=ORIENTED_EDGE('',*,*,#10621,.T.);
#14241=ORIENTED_EDGE('',*,*,#10631,.T.);
#14242=ORIENTED_EDGE('',*,*,#10629,.F.);
#14243=ORIENTED_EDGE('',*,*,#10632,.T.);
#14244=ORIENTED_EDGE('',*,*,#10633,.T.);
#14245=ORIENTED_EDGE('',*,*,#10634,.T.);
#14246=ORIENTED_EDGE('',*,*,#10635,.T.);
#14247=ORIENTED_EDGE('',*,*,#10636,.T.);
#14248=ORIENTED_EDGE('',*,*,#10634,.F.);
#14249=ORIENTED_EDGE('',*,*,#10637,.T.);
#14250=ORIENTED_EDGE('',*,*,#10619,.T.);
#14251=ORIENTED_EDGE('',*,*,#10638,.T.);
#14252=ORIENTED_EDGE('',*,*,#10414,.F.);
#14253=ORIENTED_EDGE('',*,*,#10639,.T.);
#14254=ORIENTED_EDGE('',*,*,#10316,.T.);
#14255=ORIENTED_EDGE('',*,*,#10413,.F.);
#14256=ORIENTED_EDGE('',*,*,#10416,.F.);
#14257=ORIENTED_EDGE('',*,*,#10637,.F.);
#14258=ORIENTED_EDGE('',*,*,#10640,.F.);
#14259=ORIENTED_EDGE('',*,*,#10639,.F.);
#14260=ORIENTED_EDGE('',*,*,#10640,.T.);
#14261=ORIENTED_EDGE('',*,*,#10636,.F.);
#14262=ORIENTED_EDGE('',*,*,#10592,.T.);
#14263=ORIENTED_EDGE('',*,*,#10641,.T.);
#14264=ORIENTED_EDGE('',*,*,#10328,.T.);
#14265=ORIENTED_EDGE('',*,*,#10642,.T.);
#14266=ORIENTED_EDGE('',*,*,#10410,.F.);
#14267=ORIENTED_EDGE('',*,*,#10412,.T.);
#14268=ORIENTED_EDGE('',*,*,#10641,.F.);
#14269=ORIENTED_EDGE('',*,*,#10643,.T.);
#14270=ORIENTED_EDGE('',*,*,#10411,.F.);
#14271=ORIENTED_EDGE('',*,*,#10644,.T.);
#14272=ORIENTED_EDGE('',*,*,#10645,.T.);
#14273=ORIENTED_EDGE('',*,*,#10365,.T.);
#14274=ORIENTED_EDGE('',*,*,#10645,.F.);
#14275=ORIENTED_EDGE('',*,*,#10646,.T.);
#14276=ORIENTED_EDGE('',*,*,#10647,.T.);
#14277=ORIENTED_EDGE('',*,*,#10642,.F.);
#14278=ORIENTED_EDGE('',*,*,#10596,.T.);
#14279=ORIENTED_EDGE('',*,*,#10648,.F.);
#14280=ORIENTED_EDGE('',*,*,#10649,.T.);
#14281=ORIENTED_EDGE('',*,*,#10650,.T.);
#14282=ORIENTED_EDGE('',*,*,#10651,.T.);
#14283=ORIENTED_EDGE('',*,*,#10652,.T.);
#14284=ORIENTED_EDGE('',*,*,#10627,.F.);
#14285=ORIENTED_EDGE('',*,*,#10653,.T.);
#14286=ORIENTED_EDGE('',*,*,#10650,.F.);
#14287=ORIENTED_EDGE('',*,*,#10654,.T.);
#14288=ORIENTED_EDGE('',*,*,#10626,.F.);
#14289=ORIENTED_EDGE('',*,*,#10366,.T.);
#14290=ORIENTED_EDGE('',*,*,#10647,.F.);
#14291=ORIENTED_EDGE('',*,*,#10655,.T.);
#14292=ORIENTED_EDGE('',*,*,#10646,.F.);
#14293=ORIENTED_EDGE('',*,*,#10656,.T.);
#14294=ORIENTED_EDGE('',*,*,#10657,.T.);
#14295=ORIENTED_EDGE('',*,*,#10658,.T.);
#14296=ORIENTED_EDGE('',*,*,#10657,.F.);
#14297=ORIENTED_EDGE('',*,*,#10648,.T.);
#14298=ORIENTED_EDGE('',*,*,#10659,.T.);
#14299=ORIENTED_EDGE('',*,*,#10653,.F.);
#14300=ORIENTED_EDGE('',*,*,#10655,.F.);
#14301=ORIENTED_EDGE('',*,*,#10658,.F.);
#14302=ORIENTED_EDGE('',*,*,#10660,.F.);
#14303=ORIENTED_EDGE('',*,*,#10643,.F.);
#14304=ORIENTED_EDGE('',*,*,#10649,.F.);
#14305=ORIENTED_EDGE('',*,*,#10656,.F.);
#14306=ORIENTED_EDGE('',*,*,#10644,.F.);
#14307=ORIENTED_EDGE('',*,*,#10661,.T.);
#14308=ORIENTED_EDGE('',*,*,#10576,.T.);
#14309=ORIENTED_EDGE('',*,*,#10571,.F.);
#14310=ORIENTED_EDGE('',*,*,#10662,.T.);
#14311=ORIENTED_EDGE('',*,*,#10663,.F.);
#14312=ORIENTED_EDGE('',*,*,#10664,.F.);
#14313=ORIENTED_EDGE('',*,*,#10665,.F.);
#14314=ORIENTED_EDGE('',*,*,#10666,.T.);
#14315=ORIENTED_EDGE('',*,*,#10667,.T.);
#14316=ORIENTED_EDGE('',*,*,#10422,.F.);
#14317=ORIENTED_EDGE('',*,*,#10357,.T.);
#14318=ORIENTED_EDGE('',*,*,#10664,.T.);
#14319=ORIENTED_EDGE('',*,*,#10668,.T.);
#14320=ORIENTED_EDGE('',*,*,#10666,.F.);
#14321=ORIENTED_EDGE('',*,*,#10356,.T.);
#14322=ORIENTED_EDGE('',*,*,#10669,.T.);
#14323=ORIENTED_EDGE('',*,*,#10665,.T.);
#14324=ORIENTED_EDGE('',*,*,#10355,.T.);
#14325=ORIENTED_EDGE('',*,*,#10670,.T.);
#14326=ORIENTED_EDGE('',*,*,#10671,.F.);
#14327=ORIENTED_EDGE('',*,*,#10672,.F.);
#14328=ORIENTED_EDGE('',*,*,#10673,.F.);
#14329=ORIENTED_EDGE('',*,*,#10354,.T.);
#14330=ORIENTED_EDGE('',*,*,#10672,.T.);
#14331=ORIENTED_EDGE('',*,*,#10674,.T.);
#14332=ORIENTED_EDGE('',*,*,#10670,.F.);
#14333=ORIENTED_EDGE('',*,*,#10675,.T.);
#14334=ORIENTED_EDGE('',*,*,#10673,.T.);
#14335=ORIENTED_EDGE('',*,*,#10353,.T.);
#14336=ORIENTED_EDGE('',*,*,#10676,.T.);
#14337=ORIENTED_EDGE('',*,*,#10352,.T.);
#14338=ORIENTED_EDGE('',*,*,#10677,.T.);
#14339=ORIENTED_EDGE('',*,*,#10678,.T.);
#14340=ORIENTED_EDGE('',*,*,#10676,.F.);
#14341=ORIENTED_EDGE('',*,*,#10679,.F.);
#14342=ORIENTED_EDGE('',*,*,#10680,.F.);
#14343=ORIENTED_EDGE('',*,*,#10681,.F.);
#14344=ORIENTED_EDGE('',*,*,#10351,.T.);
#14345=ORIENTED_EDGE('',*,*,#10680,.T.);
#14346=ORIENTED_EDGE('',*,*,#10682,.T.);
#14347=ORIENTED_EDGE('',*,*,#10677,.F.);
#14348=ORIENTED_EDGE('',*,*,#10683,.F.);
#14349=ORIENTED_EDGE('',*,*,#10684,.F.);
#14350=ORIENTED_EDGE('',*,*,#10685,.F.);
#14351=ORIENTED_EDGE('',*,*,#10684,.T.);
#14352=ORIENTED_EDGE('',*,*,#10686,.T.);
#14353=ORIENTED_EDGE('',*,*,#10681,.T.);
#14354=ORIENTED_EDGE('',*,*,#10350,.T.);
#14355=ORIENTED_EDGE('',*,*,#10687,.F.);
#14356=ORIENTED_EDGE('',*,*,#10688,.F.);
#14357=ORIENTED_EDGE('',*,*,#10689,.F.);
#14358=ORIENTED_EDGE('',*,*,#10688,.T.);
#14359=ORIENTED_EDGE('',*,*,#10690,.T.);
#14360=ORIENTED_EDGE('',*,*,#10685,.T.);
#14361=ORIENTED_EDGE('',*,*,#10349,.T.);
#14362=ORIENTED_EDGE('',*,*,#10429,.F.);
#14363=ORIENTED_EDGE('',*,*,#10691,.T.);
#14364=ORIENTED_EDGE('',*,*,#10689,.T.);
#14365=ORIENTED_EDGE('',*,*,#10348,.T.);
#14366=ORIENTED_EDGE('',*,*,#10692,.T.);
#14367=ORIENTED_EDGE('',*,*,#10693,.T.);
#14368=ORIENTED_EDGE('',*,*,#10687,.T.);
#14369=ORIENTED_EDGE('',*,*,#10694,.T.);
#14370=ORIENTED_EDGE('',*,*,#10614,.F.);
#14371=ORIENTED_EDGE('',*,*,#10587,.T.);
#14372=ORIENTED_EDGE('',*,*,#10695,.T.);
#14373=ORIENTED_EDGE('',*,*,#10696,.T.);
#14374=ORIENTED_EDGE('',*,*,#10697,.T.);
#14375=ORIENTED_EDGE('',*,*,#10698,.T.);
#14376=ORIENTED_EDGE('',*,*,#10683,.T.);
#14377=ORIENTED_EDGE('',*,*,#10699,.T.);
#14378=ORIENTED_EDGE('',*,*,#10697,.F.);
#14379=ORIENTED_EDGE('',*,*,#10700,.T.);
#14380=ORIENTED_EDGE('',*,*,#10701,.T.);
#14381=ORIENTED_EDGE('',*,*,#10702,.T.);
#14382=ORIENTED_EDGE('',*,*,#10703,.T.);
#14383=ORIENTED_EDGE('',*,*,#10679,.T.);
#14384=ORIENTED_EDGE('',*,*,#10704,.T.);
#14385=ORIENTED_EDGE('',*,*,#10702,.F.);
#14386=ORIENTED_EDGE('',*,*,#10705,.T.);
#14387=ORIENTED_EDGE('',*,*,#10706,.T.);
#14388=ORIENTED_EDGE('',*,*,#10707,.T.);
#14389=ORIENTED_EDGE('',*,*,#10708,.T.);
#14390=ORIENTED_EDGE('',*,*,#10671,.T.);
#14391=ORIENTED_EDGE('',*,*,#10709,.T.);
#14392=ORIENTED_EDGE('',*,*,#10707,.F.);
#14393=ORIENTED_EDGE('',*,*,#10710,.T.);
#14394=ORIENTED_EDGE('',*,*,#10711,.T.);
#14395=ORIENTED_EDGE('',*,*,#10712,.T.);
#14396=ORIENTED_EDGE('',*,*,#10713,.T.);
#14397=ORIENTED_EDGE('',*,*,#10663,.T.);
#14398=ORIENTED_EDGE('',*,*,#10714,.T.);
#14399=ORIENTED_EDGE('',*,*,#10712,.F.);
#14400=ORIENTED_EDGE('',*,*,#10715,.T.);
#14401=ORIENTED_EDGE('',*,*,#10716,.T.);
#14402=ORIENTED_EDGE('',*,*,#10421,.F.);
#14403=ORIENTED_EDGE('',*,*,#10717,.T.);
#14404=ORIENTED_EDGE('',*,*,#10718,.T.);
#14405=ORIENTED_EDGE('',*,*,#10719,.T.);
#14406=ORIENTED_EDGE('',*,*,#10695,.F.);
#14407=ORIENTED_EDGE('',*,*,#10720,.T.);
#14408=ORIENTED_EDGE('',*,*,#10692,.F.);
#14409=ORIENTED_EDGE('',*,*,#10718,.F.);
#14410=ORIENTED_EDGE('',*,*,#10721,.T.);
#14411=ORIENTED_EDGE('',*,*,#10661,.F.);
#14412=ORIENTED_EDGE('',*,*,#10716,.F.);
#14413=ORIENTED_EDGE('',*,*,#10579,.T.);
#14414=ORIENTED_EDGE('',*,*,#10722,.F.);
#14415=ORIENTED_EDGE('',*,*,#10723,.T.);
#14416=ORIENTED_EDGE('',*,*,#10715,.F.);
#14417=ORIENTED_EDGE('',*,*,#10724,.T.);
#14418=ORIENTED_EDGE('',*,*,#10725,.F.);
#14419=ORIENTED_EDGE('',*,*,#10580,.T.);
#14420=ORIENTED_EDGE('',*,*,#10714,.F.);
#14421=ORIENTED_EDGE('',*,*,#10669,.F.);
#14422=ORIENTED_EDGE('',*,*,#10726,.T.);
#14423=ORIENTED_EDGE('',*,*,#10724,.F.);
#14424=ORIENTED_EDGE('',*,*,#10674,.F.);
#14425=ORIENTED_EDGE('',*,*,#10708,.F.);
#14426=ORIENTED_EDGE('',*,*,#10727,.F.);
#14427=ORIENTED_EDGE('',*,*,#10726,.F.);
#14428=ORIENTED_EDGE('',*,*,#10711,.F.);
#14429=ORIENTED_EDGE('',*,*,#10581,.T.);
#14430=ORIENTED_EDGE('',*,*,#10725,.T.);
#14431=ORIENTED_EDGE('',*,*,#10727,.T.);
#14432=ORIENTED_EDGE('',*,*,#10710,.F.);
#14433=ORIENTED_EDGE('',*,*,#10728,.T.);
#14434=ORIENTED_EDGE('',*,*,#10729,.F.);
#14435=ORIENTED_EDGE('',*,*,#10582,.T.);
#14436=ORIENTED_EDGE('',*,*,#10709,.F.);
#14437=ORIENTED_EDGE('',*,*,#10675,.F.);
#14438=ORIENTED_EDGE('',*,*,#10730,.T.);
#14439=ORIENTED_EDGE('',*,*,#10728,.F.);
#14440=ORIENTED_EDGE('',*,*,#10678,.F.);
#14441=ORIENTED_EDGE('',*,*,#10731,.T.);
#14442=ORIENTED_EDGE('',*,*,#10732,.F.);
#14443=ORIENTED_EDGE('',*,*,#10730,.F.);
#14444=ORIENTED_EDGE('',*,*,#10682,.F.);
#14445=ORIENTED_EDGE('',*,*,#10703,.F.);
#14446=ORIENTED_EDGE('',*,*,#10733,.F.);
#14447=ORIENTED_EDGE('',*,*,#10731,.F.);
#14448=ORIENTED_EDGE('',*,*,#10706,.F.);
#14449=ORIENTED_EDGE('',*,*,#10584,.T.);
#14450=ORIENTED_EDGE('',*,*,#10734,.T.);
#14451=ORIENTED_EDGE('',*,*,#10733,.T.);
#14452=ORIENTED_EDGE('',*,*,#10704,.F.);
#14453=ORIENTED_EDGE('',*,*,#10686,.F.);
#14454=ORIENTED_EDGE('',*,*,#10698,.F.);
#14455=ORIENTED_EDGE('',*,*,#10735,.F.);
#14456=ORIENTED_EDGE('',*,*,#10705,.F.);
#14457=ORIENTED_EDGE('',*,*,#10735,.T.);
#14458=ORIENTED_EDGE('',*,*,#10701,.F.);
#14459=ORIENTED_EDGE('',*,*,#10585,.T.);
#14460=ORIENTED_EDGE('',*,*,#10699,.F.);
#14461=ORIENTED_EDGE('',*,*,#10690,.F.);
#14462=ORIENTED_EDGE('',*,*,#10693,.F.);
#14463=ORIENTED_EDGE('',*,*,#10736,.F.);
#14464=ORIENTED_EDGE('',*,*,#10700,.F.);
#14465=ORIENTED_EDGE('',*,*,#10736,.T.);
#14466=ORIENTED_EDGE('',*,*,#10720,.F.);
#14467=ORIENTED_EDGE('',*,*,#10586,.T.);
#14468=ORIENTED_EDGE('',*,*,#10691,.F.);
#14469=ORIENTED_EDGE('',*,*,#10618,.F.);
#14470=ORIENTED_EDGE('',*,*,#10696,.F.);
#14471=ORIENTED_EDGE('',*,*,#10694,.F.);
#14472=ORIENTED_EDGE('',*,*,#10583,.T.);
#14473=ORIENTED_EDGE('',*,*,#10729,.T.);
#14474=ORIENTED_EDGE('',*,*,#10732,.T.);
#14475=ORIENTED_EDGE('',*,*,#10734,.F.);
#14476=ORIENTED_EDGE('',*,*,#10721,.F.);
#14477=ORIENTED_EDGE('',*,*,#10737,.T.);
#14478=ORIENTED_EDGE('',*,*,#10738,.T.);
#14479=ORIENTED_EDGE('',*,*,#10577,.T.);
#14480=ORIENTED_EDGE('',*,*,#10722,.T.);
#14481=ORIENTED_EDGE('',*,*,#10578,.T.);
#14482=ORIENTED_EDGE('',*,*,#10738,.F.);
#14483=ORIENTED_EDGE('',*,*,#10739,.T.);
#14484=ORIENTED_EDGE('',*,*,#10713,.F.);
#14485=ORIENTED_EDGE('',*,*,#10723,.F.);
#14486=ORIENTED_EDGE('',*,*,#10740,.F.);
#14487=ORIENTED_EDGE('',*,*,#10668,.F.);
#14488=ORIENTED_EDGE('',*,*,#10667,.F.);
#14489=ORIENTED_EDGE('',*,*,#10740,.T.);
#14490=ORIENTED_EDGE('',*,*,#10739,.F.);
#14491=ORIENTED_EDGE('',*,*,#10741,.F.);
#14492=ORIENTED_EDGE('',*,*,#10423,.F.);
#14493=ORIENTED_EDGE('',*,*,#10741,.T.);
#14494=ORIENTED_EDGE('',*,*,#10737,.F.);
#14495=ORIENTED_EDGE('',*,*,#10717,.F.);
#14496=ORIENTED_EDGE('',*,*,#10651,.F.);
#14497=ORIENTED_EDGE('',*,*,#10660,.T.);
#14498=ORIENTED_EDGE('',*,*,#10659,.F.);
#14499=ORIENTED_EDGE('',*,*,#10595,.T.);
#14500=ORIENTED_EDGE('',*,*,#10632,.F.);
#14501=ORIENTED_EDGE('',*,*,#10742,.T.);
#14502=ORIENTED_EDGE('',*,*,#10652,.F.);
#14503=ORIENTED_EDGE('',*,*,#10594,.T.);
#14504=ORIENTED_EDGE('',*,*,#10633,.F.);
#14505=ORIENTED_EDGE('',*,*,#10593,.T.);
#14506=ORIENTED_EDGE('',*,*,#10635,.F.);
#14507=ORIENTED_EDGE('',*,*,#10743,.T.);
#14508=ORIENTED_EDGE('',*,*,#10628,.F.);
#14509=ORIENTED_EDGE('',*,*,#10654,.F.);
#14510=ORIENTED_EDGE('',*,*,#10742,.F.);
#14511=ORIENTED_EDGE('',*,*,#10631,.F.);
#14512=ORIENTED_EDGE('',*,*,#10630,.F.);
#14513=ORIENTED_EDGE('',*,*,#10743,.F.);
#14514=ORIENTED_EDGE('',*,*,#10638,.F.);
#14515=ORIENTED_EDGE('',*,*,#10624,.F.);
#14516=ORIENTED_EDGE('',*,*,#10604,.T.);
#14517=ORIENTED_EDGE('',*,*,#10744,.T.);
#14518=ORIENTED_EDGE('',*,*,#10383,.T.);
#14519=ORIENTED_EDGE('',*,*,#10384,.T.);
#14520=ORIENTED_EDGE('',*,*,#10744,.F.);
#14521=ORIENTED_EDGE('',*,*,#10745,.T.);
#14522=ORIENTED_EDGE('',*,*,#10404,.T.);
#14523=ORIENTED_EDGE('',*,*,#10746,.T.);
#14524=ORIENTED_EDGE('',*,*,#10597,.T.);
#14525=ORIENTED_EDGE('',*,*,#10747,.T.);
#14526=ORIENTED_EDGE('',*,*,#10598,.T.);
#14527=ORIENTED_EDGE('',*,*,#10746,.F.);
#14528=ORIENTED_EDGE('',*,*,#10748,.T.);
#14529=ORIENTED_EDGE('',*,*,#10749,.T.);
#14530=ORIENTED_EDGE('',*,*,#10599,.T.);
#14531=ORIENTED_EDGE('',*,*,#10747,.F.);
#14532=ORIENTED_EDGE('',*,*,#10750,.T.);
#14533=ORIENTED_EDGE('',*,*,#10745,.F.);
#14534=ORIENTED_EDGE('',*,*,#10600,.T.);
#14535=ORIENTED_EDGE('',*,*,#10749,.F.);
#14536=ORIENTED_EDGE('',*,*,#10401,.T.);
#14537=ORIENTED_EDGE('',*,*,#10399,.F.);
#14538=ORIENTED_EDGE('',*,*,#10751,.T.);
#14539=ORIENTED_EDGE('',*,*,#10748,.F.);
#14540=ORIENTED_EDGE('',*,*,#10403,.F.);
#14541=ORIENTED_EDGE('',*,*,#10253,.T.);
#14542=ORIENTED_EDGE('',*,*,#10254,.T.);
#14543=ORIENTED_EDGE('',*,*,#10752,.T.);
#14544=ORIENTED_EDGE('',*,*,#10603,.T.);
#14545=ORIENTED_EDGE('',*,*,#10752,.F.);
#14546=ORIENTED_EDGE('',*,*,#10753,.T.);
#14547=ORIENTED_EDGE('',*,*,#10754,.T.);
#14548=ORIENTED_EDGE('',*,*,#10601,.T.);
#14549=ORIENTED_EDGE('',*,*,#10754,.F.);
#14550=ORIENTED_EDGE('',*,*,#10755,.T.);
#14551=ORIENTED_EDGE('',*,*,#10756,.F.);
#14552=ORIENTED_EDGE('',*,*,#10757,.F.);
#14553=ORIENTED_EDGE('',*,*,#10758,.T.);
#14554=ORIENTED_EDGE('',*,*,#10755,.F.);
#14555=ORIENTED_EDGE('',*,*,#10753,.F.);
#14556=ORIENTED_EDGE('',*,*,#10758,.F.);
#14557=ORIENTED_EDGE('',*,*,#10756,.T.);
#14558=ORIENTED_EDGE('',*,*,#10757,.T.);
#14559=ORIENTED_EDGE('',*,*,#10759,.T.);
#14560=ORIENTED_EDGE('',*,*,#10389,.T.);
#14561=ORIENTED_EDGE('',*,*,#10390,.T.);
#14562=ORIENTED_EDGE('',*,*,#10759,.F.);
#14563=ORIENTED_EDGE('',*,*,#10398,.F.);
#14564=ORIENTED_EDGE('',*,*,#10402,.T.);
#14565=ORIENTED_EDGE('',*,*,#10750,.F.);
#14566=ORIENTED_EDGE('',*,*,#10751,.F.);
#14567=ORIENTED_EDGE('',*,*,#10419,.F.);
#14568=ORIENTED_EDGE('',*,*,#10719,.F.);
#14569=ORIENTED_EDGE('',*,*,#10662,.F.);
#14570=ORIENTED_EDGE('',*,*,#10573,.F.);
#14571=ORIENTED_EDGE('',*,*,#10760,.T.);
#14572=ORIENTED_EDGE('',*,*,#10761,.T.);
#14573=ORIENTED_EDGE('',*,*,#10762,.T.);
#14574=ORIENTED_EDGE('',*,*,#10763,.T.);
#14575=ORIENTED_EDGE('',*,*,#10764,.T.);
#14576=ORIENTED_EDGE('',*,*,#10761,.F.);
#14577=ORIENTED_EDGE('',*,*,#10765,.T.);
#14578=ORIENTED_EDGE('',*,*,#10766,.F.);
#14579=ORIENTED_EDGE('',*,*,#10767,.T.);
#14580=ORIENTED_EDGE('',*,*,#10763,.F.);
#14581=ORIENTED_EDGE('',*,*,#10768,.T.);
#14582=ORIENTED_EDGE('',*,*,#10769,.T.);
#14583=ORIENTED_EDGE('',*,*,#10770,.T.);
#14584=ORIENTED_EDGE('',*,*,#10769,.F.);
#14585=ORIENTED_EDGE('',*,*,#10771,.T.);
#14586=ORIENTED_EDGE('',*,*,#10766,.T.);
#14587=ORIENTED_EDGE('',*,*,#10768,.F.);
#14588=ORIENTED_EDGE('',*,*,#10772,.F.);
#14589=ORIENTED_EDGE('',*,*,#10773,.F.);
#14590=ORIENTED_EDGE('',*,*,#10774,.T.);
#14591=ORIENTED_EDGE('',*,*,#10762,.F.);
#14592=ORIENTED_EDGE('',*,*,#10775,.F.);
#14593=ORIENTED_EDGE('',*,*,#10776,.F.);
#14594=ORIENTED_EDGE('',*,*,#10772,.T.);
#14595=ORIENTED_EDGE('',*,*,#10777,.F.);
#14596=ORIENTED_EDGE('',*,*,#10778,.F.);
#14597=ORIENTED_EDGE('',*,*,#10779,.F.);
#14598=ORIENTED_EDGE('',*,*,#10780,.F.);
#14599=ORIENTED_EDGE('',*,*,#10781,.F.);
#14600=ORIENTED_EDGE('',*,*,#10782,.T.);
#14601=ORIENTED_EDGE('',*,*,#10760,.F.);
#14602=ORIENTED_EDGE('',*,*,#10767,.F.);
#14603=ORIENTED_EDGE('',*,*,#10770,.F.);
#14604=ORIENTED_EDGE('',*,*,#10765,.F.);
#14605=ORIENTED_EDGE('',*,*,#10783,.T.);
#14606=ORIENTED_EDGE('',*,*,#10777,.T.);
#14607=ORIENTED_EDGE('',*,*,#10784,.T.);
#14608=ORIENTED_EDGE('',*,*,#10785,.T.);
#14609=ORIENTED_EDGE('',*,*,#10786,.T.);
#14610=ORIENTED_EDGE('',*,*,#10787,.T.);
#14611=ORIENTED_EDGE('',*,*,#10788,.T.);
#14612=ORIENTED_EDGE('',*,*,#10789,.F.);
#14613=ORIENTED_EDGE('',*,*,#10790,.T.);
#14614=ORIENTED_EDGE('',*,*,#10791,.T.);
#14615=ORIENTED_EDGE('',*,*,#10776,.T.);
#14616=ORIENTED_EDGE('',*,*,#10792,.T.);
#14617=ORIENTED_EDGE('',*,*,#10773,.T.);
#14618=ORIENTED_EDGE('',*,*,#10791,.F.);
#14619=ORIENTED_EDGE('',*,*,#10793,.T.);
#14620=ORIENTED_EDGE('',*,*,#10789,.T.);
#14621=ORIENTED_EDGE('',*,*,#10794,.T.);
#14622=ORIENTED_EDGE('',*,*,#10792,.F.);
#14623=ORIENTED_EDGE('',*,*,#10795,.T.);
#14624=ORIENTED_EDGE('',*,*,#10787,.F.);
#14625=ORIENTED_EDGE('',*,*,#10764,.F.);
#14626=ORIENTED_EDGE('',*,*,#10796,.F.);
#14627=ORIENTED_EDGE('',*,*,#10795,.F.);
#14628=ORIENTED_EDGE('',*,*,#10775,.T.);
#14629=ORIENTED_EDGE('',*,*,#10797,.F.);
#14630=ORIENTED_EDGE('',*,*,#10798,.F.);
#14631=ORIENTED_EDGE('',*,*,#10799,.T.);
#14632=ORIENTED_EDGE('',*,*,#10800,.F.);
#14633=ORIENTED_EDGE('',*,*,#10801,.F.);
#14634=ORIENTED_EDGE('',*,*,#10802,.F.);
#14635=ORIENTED_EDGE('',*,*,#10790,.F.);
#14636=ORIENTED_EDGE('',*,*,#10794,.F.);
#14637=ORIENTED_EDGE('',*,*,#10786,.F.);
#14638=ORIENTED_EDGE('',*,*,#10793,.F.);
#14639=ORIENTED_EDGE('',*,*,#10803,.T.);
#14640=ORIENTED_EDGE('',*,*,#10797,.T.);
#14641=ORIENTED_EDGE('',*,*,#10804,.T.);
#14642=ORIENTED_EDGE('',*,*,#10805,.T.);
#14643=ORIENTED_EDGE('',*,*,#10806,.T.);
#14644=ORIENTED_EDGE('',*,*,#10807,.T.);
#14645=ORIENTED_EDGE('',*,*,#10808,.T.);
#14646=ORIENTED_EDGE('',*,*,#10809,.T.);
#14647=ORIENTED_EDGE('',*,*,#10807,.F.);
#14648=ORIENTED_EDGE('',*,*,#10810,.F.);
#14649=ORIENTED_EDGE('',*,*,#10811,.F.);
#14650=ORIENTED_EDGE('',*,*,#10812,.F.);
#14651=ORIENTED_EDGE('',*,*,#10813,.T.);
#14652=ORIENTED_EDGE('',*,*,#10814,.T.);
#14653=ORIENTED_EDGE('',*,*,#10815,.T.);
#14654=ORIENTED_EDGE('',*,*,#10816,.T.);
#14655=ORIENTED_EDGE('',*,*,#10817,.T.);
#14656=ORIENTED_EDGE('',*,*,#10818,.T.);
#14657=ORIENTED_EDGE('',*,*,#10815,.F.);
#14658=ORIENTED_EDGE('',*,*,#10819,.T.);
#14659=ORIENTED_EDGE('',*,*,#10820,.F.);
#14660=ORIENTED_EDGE('',*,*,#10821,.T.);
#14661=ORIENTED_EDGE('',*,*,#10817,.F.);
#14662=ORIENTED_EDGE('',*,*,#10822,.T.);
#14663=ORIENTED_EDGE('',*,*,#10823,.T.);
#14664=ORIENTED_EDGE('',*,*,#10824,.T.);
#14665=ORIENTED_EDGE('',*,*,#10823,.F.);
#14666=ORIENTED_EDGE('',*,*,#10825,.T.);
#14667=ORIENTED_EDGE('',*,*,#10820,.T.);
#14668=ORIENTED_EDGE('',*,*,#10822,.F.);
#14669=ORIENTED_EDGE('',*,*,#10826,.F.);
#14670=ORIENTED_EDGE('',*,*,#10827,.F.);
#14671=ORIENTED_EDGE('',*,*,#10828,.T.);
#14672=ORIENTED_EDGE('',*,*,#10816,.F.);
#14673=ORIENTED_EDGE('',*,*,#10829,.F.);
#14674=ORIENTED_EDGE('',*,*,#10830,.F.);
#14675=ORIENTED_EDGE('',*,*,#10826,.T.);
#14676=ORIENTED_EDGE('',*,*,#10809,.F.);
#14677=ORIENTED_EDGE('',*,*,#10831,.T.);
#14678=ORIENTED_EDGE('',*,*,#10832,.F.);
#14679=ORIENTED_EDGE('',*,*,#10833,.F.);
#14680=ORIENTED_EDGE('',*,*,#10834,.T.);
#14681=ORIENTED_EDGE('',*,*,#10835,.F.);
#14682=ORIENTED_EDGE('',*,*,#10814,.F.);
#14683=ORIENTED_EDGE('',*,*,#10821,.F.);
#14684=ORIENTED_EDGE('',*,*,#10824,.F.);
#14685=ORIENTED_EDGE('',*,*,#10819,.F.);
#14686=ORIENTED_EDGE('',*,*,#10836,.T.);
#14687=ORIENTED_EDGE('',*,*,#10837,.T.);
#14688=ORIENTED_EDGE('',*,*,#10838,.T.);
#14689=ORIENTED_EDGE('',*,*,#10839,.T.);
#14690=ORIENTED_EDGE('',*,*,#10801,.T.);
#14691=ORIENTED_EDGE('',*,*,#10836,.F.);
#14692=ORIENTED_EDGE('',*,*,#10840,.T.);
#14693=ORIENTED_EDGE('',*,*,#10841,.F.);
#14694=ORIENTED_EDGE('',*,*,#10840,.F.);
#14695=ORIENTED_EDGE('',*,*,#10842,.F.);
#14696=ORIENTED_EDGE('',*,*,#10843,.F.);
#14697=ORIENTED_EDGE('',*,*,#10844,.F.);
#14698=ORIENTED_EDGE('',*,*,#10845,.F.);
#14699=ORIENTED_EDGE('',*,*,#10846,.F.);
#14700=ORIENTED_EDGE('',*,*,#10847,.F.);
#14701=ORIENTED_EDGE('',*,*,#10848,.F.);
#14702=ORIENTED_EDGE('',*,*,#10849,.T.);
#14703=ORIENTED_EDGE('',*,*,#10850,.F.);
#14704=ORIENTED_EDGE('',*,*,#10851,.F.);
#14705=ORIENTED_EDGE('',*,*,#10838,.F.);
#14706=ORIENTED_EDGE('',*,*,#10852,.T.);
#14707=ORIENTED_EDGE('',*,*,#10853,.T.);
#14708=ORIENTED_EDGE('',*,*,#10842,.T.);
#14709=ORIENTED_EDGE('',*,*,#10837,.F.);
#14710=ORIENTED_EDGE('',*,*,#10800,.T.);
#14711=ORIENTED_EDGE('',*,*,#10854,.F.);
#14712=ORIENTED_EDGE('',*,*,#10855,.T.);
#14713=ORIENTED_EDGE('',*,*,#10848,.T.);
#14714=ORIENTED_EDGE('',*,*,#10856,.T.);
#14715=ORIENTED_EDGE('',*,*,#10857,.T.);
#14716=ORIENTED_EDGE('',*,*,#10858,.T.);
#14717=ORIENTED_EDGE('',*,*,#10859,.T.);
#14718=ORIENTED_EDGE('',*,*,#10860,.T.);
#14719=ORIENTED_EDGE('',*,*,#10861,.T.);
#14720=ORIENTED_EDGE('',*,*,#10847,.T.);
#14721=ORIENTED_EDGE('',*,*,#10859,.F.);
#14722=ORIENTED_EDGE('',*,*,#10832,.T.);
#14723=ORIENTED_EDGE('',*,*,#10856,.F.);
#14724=ORIENTED_EDGE('',*,*,#10862,.T.);
#14725=ORIENTED_EDGE('',*,*,#10863,.T.);
#14726=ORIENTED_EDGE('',*,*,#10864,.T.);
#14727=ORIENTED_EDGE('',*,*,#10858,.F.);
#14728=ORIENTED_EDGE('',*,*,#10864,.F.);
#14729=ORIENTED_EDGE('',*,*,#10865,.T.);
#14730=ORIENTED_EDGE('',*,*,#10866,.F.);
#14731=ORIENTED_EDGE('',*,*,#10849,.F.);
#14732=ORIENTED_EDGE('',*,*,#10798,.T.);
#14733=ORIENTED_EDGE('',*,*,#10803,.F.);
#14734=ORIENTED_EDGE('',*,*,#10867,.T.);
#14735=ORIENTED_EDGE('',*,*,#10868,.T.);
#14736=ORIENTED_EDGE('',*,*,#10869,.T.);
#14737=ORIENTED_EDGE('',*,*,#10870,.T.);
#14738=ORIENTED_EDGE('',*,*,#10871,.T.);
#14739=ORIENTED_EDGE('',*,*,#10868,.F.);
#14740=ORIENTED_EDGE('',*,*,#10872,.T.);
#14741=ORIENTED_EDGE('',*,*,#10873,.T.);
#14742=ORIENTED_EDGE('',*,*,#10874,.T.);
#14743=ORIENTED_EDGE('',*,*,#10870,.F.);
#14744=ORIENTED_EDGE('',*,*,#10875,.T.);
#14745=ORIENTED_EDGE('',*,*,#10876,.T.);
#14746=ORIENTED_EDGE('',*,*,#10877,.T.);
#14747=ORIENTED_EDGE('',*,*,#10878,.T.);
#14748=ORIENTED_EDGE('',*,*,#10879,.T.);
#14749=ORIENTED_EDGE('',*,*,#10880,.T.);
#14750=ORIENTED_EDGE('',*,*,#10881,.T.);
#14751=ORIENTED_EDGE('',*,*,#10878,.F.);
#14752=ORIENTED_EDGE('',*,*,#10882,.T.);
#14753=ORIENTED_EDGE('',*,*,#10883,.T.);
#14754=ORIENTED_EDGE('',*,*,#10884,.T.);
#14755=ORIENTED_EDGE('',*,*,#10781,.T.);
#14756=ORIENTED_EDGE('',*,*,#10882,.F.);
#14757=ORIENTED_EDGE('',*,*,#10845,.T.);
#14758=ORIENTED_EDGE('',*,*,#10885,.T.);
#14759=ORIENTED_EDGE('',*,*,#10886,.T.);
#14760=ORIENTED_EDGE('',*,*,#10885,.F.);
#14761=ORIENTED_EDGE('',*,*,#10844,.T.);
#14762=ORIENTED_EDGE('',*,*,#10880,.F.);
#14763=ORIENTED_EDGE('',*,*,#10887,.T.);
#14764=ORIENTED_EDGE('',*,*,#10876,.F.);
#14765=ORIENTED_EDGE('',*,*,#10888,.T.);
#14766=ORIENTED_EDGE('',*,*,#10889,.T.);
#14767=ORIENTED_EDGE('',*,*,#10890,.T.);
#14768=ORIENTED_EDGE('',*,*,#10889,.F.);
#14769=ORIENTED_EDGE('',*,*,#10891,.T.);
#14770=ORIENTED_EDGE('',*,*,#10873,.F.);
#14771=ORIENTED_EDGE('',*,*,#10871,.F.);
#14772=ORIENTED_EDGE('',*,*,#10892,.T.);
#14773=ORIENTED_EDGE('',*,*,#10893,.F.);
#14774=ORIENTED_EDGE('',*,*,#10799,.F.);
#14775=ORIENTED_EDGE('',*,*,#10874,.F.);
#14776=ORIENTED_EDGE('',*,*,#10894,.T.);
#14777=ORIENTED_EDGE('',*,*,#10895,.F.);
#14778=ORIENTED_EDGE('',*,*,#10892,.F.);
#14779=ORIENTED_EDGE('',*,*,#10891,.F.);
#14780=ORIENTED_EDGE('',*,*,#10896,.T.);
#14781=ORIENTED_EDGE('',*,*,#10897,.F.);
#14782=ORIENTED_EDGE('',*,*,#10894,.F.);
#14783=ORIENTED_EDGE('',*,*,#10888,.F.);
#14784=ORIENTED_EDGE('',*,*,#10898,.T.);
#14785=ORIENTED_EDGE('',*,*,#10899,.F.);
#14786=ORIENTED_EDGE('',*,*,#10896,.F.);
#14787=ORIENTED_EDGE('',*,*,#10875,.F.);
#14788=ORIENTED_EDGE('',*,*,#10900,.T.);
#14789=ORIENTED_EDGE('',*,*,#10901,.F.);
#14790=ORIENTED_EDGE('',*,*,#10898,.F.);
#14791=ORIENTED_EDGE('',*,*,#10881,.F.);
#14792=ORIENTED_EDGE('',*,*,#10843,.T.);
#14793=ORIENTED_EDGE('',*,*,#10902,.F.);
#14794=ORIENTED_EDGE('',*,*,#10900,.F.);
#14795=ORIENTED_EDGE('',*,*,#10860,.F.);
#14796=ORIENTED_EDGE('',*,*,#10846,.T.);
#14797=ORIENTED_EDGE('',*,*,#10884,.F.);
#14798=ORIENTED_EDGE('',*,*,#10903,.T.);
#14799=ORIENTED_EDGE('',*,*,#10883,.F.);
#14800=ORIENTED_EDGE('',*,*,#10780,.T.);
#14801=ORIENTED_EDGE('',*,*,#10904,.T.);
#14802=ORIENTED_EDGE('',*,*,#10905,.T.);
#14803=ORIENTED_EDGE('',*,*,#10906,.T.);
#14804=ORIENTED_EDGE('',*,*,#10851,.T.);
#14805=ORIENTED_EDGE('',*,*,#10907,.T.);
#14806=ORIENTED_EDGE('',*,*,#10908,.T.);
#14807=ORIENTED_EDGE('',*,*,#10907,.F.);
#14808=ORIENTED_EDGE('',*,*,#10909,.T.);
#14809=ORIENTED_EDGE('',*,*,#10910,.T.);
#14810=ORIENTED_EDGE('',*,*,#10909,.F.);
#14811=ORIENTED_EDGE('',*,*,#10850,.T.);
#14812=ORIENTED_EDGE('',*,*,#10911,.F.);
#14813=ORIENTED_EDGE('',*,*,#10912,.T.);
#14814=ORIENTED_EDGE('',*,*,#10913,.T.);
#14815=ORIENTED_EDGE('',*,*,#10812,.T.);
#14816=ORIENTED_EDGE('',*,*,#10914,.T.);
#14817=ORIENTED_EDGE('',*,*,#10915,.T.);
#14818=ORIENTED_EDGE('',*,*,#10916,.T.);
#14819=ORIENTED_EDGE('',*,*,#10917,.T.);
#14820=ORIENTED_EDGE('',*,*,#10918,.T.);
#14821=ORIENTED_EDGE('',*,*,#10919,.F.);
#14822=ORIENTED_EDGE('',*,*,#10920,.T.);
#14823=ORIENTED_EDGE('',*,*,#10921,.T.);
#14824=ORIENTED_EDGE('',*,*,#10830,.T.);
#14825=ORIENTED_EDGE('',*,*,#10922,.T.);
#14826=ORIENTED_EDGE('',*,*,#10827,.T.);
#14827=ORIENTED_EDGE('',*,*,#10921,.F.);
#14828=ORIENTED_EDGE('',*,*,#10923,.T.);
#14829=ORIENTED_EDGE('',*,*,#10919,.T.);
#14830=ORIENTED_EDGE('',*,*,#10924,.T.);
#14831=ORIENTED_EDGE('',*,*,#10922,.F.);
#14832=ORIENTED_EDGE('',*,*,#10925,.T.);
#14833=ORIENTED_EDGE('',*,*,#10917,.F.);
#14834=ORIENTED_EDGE('',*,*,#10818,.F.);
#14835=ORIENTED_EDGE('',*,*,#10926,.F.);
#14836=ORIENTED_EDGE('',*,*,#10925,.F.);
#14837=ORIENTED_EDGE('',*,*,#10829,.T.);
#14838=ORIENTED_EDGE('',*,*,#10908,.F.);
#14839=ORIENTED_EDGE('',*,*,#10927,.F.);
#14840=ORIENTED_EDGE('',*,*,#10928,.F.);
#14841=ORIENTED_EDGE('',*,*,#10929,.F.);
#14842=ORIENTED_EDGE('',*,*,#10915,.F.);
#14843=ORIENTED_EDGE('',*,*,#10930,.F.);
#14844=ORIENTED_EDGE('',*,*,#10920,.F.);
#14845=ORIENTED_EDGE('',*,*,#10924,.F.);
#14846=ORIENTED_EDGE('',*,*,#10916,.F.);
#14847=ORIENTED_EDGE('',*,*,#10923,.F.);
#14848=ORIENTED_EDGE('',*,*,#10931,.T.);
#14849=ORIENTED_EDGE('',*,*,#10932,.T.);
#14850=ORIENTED_EDGE('',*,*,#10863,.F.);
#14851=ORIENTED_EDGE('',*,*,#10933,.T.);
#14852=ORIENTED_EDGE('',*,*,#10934,.T.);
#14853=ORIENTED_EDGE('',*,*,#10931,.F.);
#14854=ORIENTED_EDGE('',*,*,#10935,.T.);
#14855=ORIENTED_EDGE('',*,*,#10936,.T.);
#14856=ORIENTED_EDGE('',*,*,#10937,.T.);
#14857=ORIENTED_EDGE('',*,*,#10938,.T.);
#14858=ORIENTED_EDGE('',*,*,#10939,.T.);
#14859=ORIENTED_EDGE('',*,*,#10936,.F.);
#14860=ORIENTED_EDGE('',*,*,#10940,.T.);
#14861=ORIENTED_EDGE('',*,*,#10941,.T.);
#14862=ORIENTED_EDGE('',*,*,#10942,.T.);
#14863=ORIENTED_EDGE('',*,*,#10938,.F.);
#14864=ORIENTED_EDGE('',*,*,#10943,.T.);
#14865=ORIENTED_EDGE('',*,*,#10913,.F.);
#14866=ORIENTED_EDGE('',*,*,#10929,.T.);
#14867=ORIENTED_EDGE('',*,*,#10944,.T.);
#14868=ORIENTED_EDGE('',*,*,#10945,.T.);
#14869=ORIENTED_EDGE('',*,*,#10944,.F.);
#14870=ORIENTED_EDGE('',*,*,#10946,.T.);
#14871=ORIENTED_EDGE('',*,*,#10941,.F.);
#14872=ORIENTED_EDGE('',*,*,#10932,.F.);
#14873=ORIENTED_EDGE('',*,*,#10947,.T.);
#14874=ORIENTED_EDGE('',*,*,#10948,.F.);
#14875=ORIENTED_EDGE('',*,*,#10865,.F.);
#14876=ORIENTED_EDGE('',*,*,#10934,.F.);
#14877=ORIENTED_EDGE('',*,*,#10949,.T.);
#14878=ORIENTED_EDGE('',*,*,#10950,.F.);
#14879=ORIENTED_EDGE('',*,*,#10947,.F.);
#14880=ORIENTED_EDGE('',*,*,#10939,.F.);
#14881=ORIENTED_EDGE('',*,*,#10951,.T.);
#14882=ORIENTED_EDGE('',*,*,#10952,.F.);
#14883=ORIENTED_EDGE('',*,*,#10949,.F.);
#14884=ORIENTED_EDGE('',*,*,#10942,.F.);
#14885=ORIENTED_EDGE('',*,*,#10953,.T.);
#14886=ORIENTED_EDGE('',*,*,#10954,.F.);
#14887=ORIENTED_EDGE('',*,*,#10951,.F.);
#14888=ORIENTED_EDGE('',*,*,#10946,.F.);
#14889=ORIENTED_EDGE('',*,*,#10928,.T.);
#14890=ORIENTED_EDGE('',*,*,#10955,.F.);
#14891=ORIENTED_EDGE('',*,*,#10953,.F.);
#14892=ORIENTED_EDGE('',*,*,#10956,.T.);
#14893=ORIENTED_EDGE('',*,*,#10957,.T.);
#14894=ORIENTED_EDGE('',*,*,#10902,.T.);
#14895=ORIENTED_EDGE('',*,*,#10853,.F.);
#14896=ORIENTED_EDGE('',*,*,#10899,.T.);
#14897=ORIENTED_EDGE('',*,*,#10958,.T.);
#14898=ORIENTED_EDGE('',*,*,#10959,.T.);
#14899=ORIENTED_EDGE('',*,*,#10960,.T.);
#14900=ORIENTED_EDGE('',*,*,#10961,.T.);
#14901=ORIENTED_EDGE('',*,*,#10958,.F.);
#14902=ORIENTED_EDGE('',*,*,#10901,.T.);
#14903=ORIENTED_EDGE('',*,*,#10957,.F.);
#14904=ORIENTED_EDGE('',*,*,#10897,.T.);
#14905=ORIENTED_EDGE('',*,*,#10960,.F.);
#14906=ORIENTED_EDGE('',*,*,#10962,.T.);
#14907=ORIENTED_EDGE('',*,*,#10963,.T.);
#14908=ORIENTED_EDGE('',*,*,#10895,.T.);
#14909=ORIENTED_EDGE('',*,*,#10963,.F.);
#14910=ORIENTED_EDGE('',*,*,#10964,.T.);
#14911=ORIENTED_EDGE('',*,*,#10965,.T.);
#14912=ORIENTED_EDGE('',*,*,#10893,.T.);
#14913=ORIENTED_EDGE('',*,*,#10965,.F.);
#14914=ORIENTED_EDGE('',*,*,#10966,.T.);
#14915=ORIENTED_EDGE('',*,*,#10854,.T.);
#14916=ORIENTED_EDGE('',*,*,#10959,.F.);
#14917=ORIENTED_EDGE('',*,*,#10961,.F.);
#14918=ORIENTED_EDGE('',*,*,#10956,.F.);
#14919=ORIENTED_EDGE('',*,*,#10852,.F.);
#14920=ORIENTED_EDGE('',*,*,#10855,.F.);
#14921=ORIENTED_EDGE('',*,*,#10966,.F.);
#14922=ORIENTED_EDGE('',*,*,#10964,.F.);
#14923=ORIENTED_EDGE('',*,*,#10962,.F.);
#14924=ORIENTED_EDGE('',*,*,#10967,.F.);
#14925=ORIENTED_EDGE('',*,*,#10968,.F.);
#14926=ORIENTED_EDGE('',*,*,#10969,.F.);
#14927=ORIENTED_EDGE('',*,*,#10970,.T.);
#14928=ORIENTED_EDGE('',*,*,#10971,.T.);
#14929=ORIENTED_EDGE('',*,*,#10972,.T.);
#14930=ORIENTED_EDGE('',*,*,#10973,.T.);
#14931=ORIENTED_EDGE('',*,*,#10971,.F.);
#14932=ORIENTED_EDGE('',*,*,#10970,.F.);
#14933=ORIENTED_EDGE('',*,*,#10974,.F.);
#14934=ORIENTED_EDGE('',*,*,#10973,.F.);
#14935=ORIENTED_EDGE('',*,*,#10975,.T.);
#14936=ORIENTED_EDGE('',*,*,#10976,.F.);
#14937=ORIENTED_EDGE('',*,*,#10975,.F.);
#14938=ORIENTED_EDGE('',*,*,#10972,.F.);
#14939=ORIENTED_EDGE('',*,*,#10948,.T.);
#14940=ORIENTED_EDGE('',*,*,#10977,.T.);
#14941=ORIENTED_EDGE('',*,*,#10978,.T.);
#14942=ORIENTED_EDGE('',*,*,#10979,.T.);
#14943=ORIENTED_EDGE('',*,*,#10980,.T.);
#14944=ORIENTED_EDGE('',*,*,#10911,.T.);
#14945=ORIENTED_EDGE('',*,*,#10866,.T.);
#14946=ORIENTED_EDGE('',*,*,#10979,.F.);
#14947=ORIENTED_EDGE('',*,*,#10910,.F.);
#14948=ORIENTED_EDGE('',*,*,#10981,.T.);
#14949=ORIENTED_EDGE('',*,*,#10982,.T.);
#14950=ORIENTED_EDGE('',*,*,#10927,.T.);
#14951=ORIENTED_EDGE('',*,*,#10955,.T.);
#14952=ORIENTED_EDGE('',*,*,#10982,.F.);
#14953=ORIENTED_EDGE('',*,*,#10983,.T.);
#14954=ORIENTED_EDGE('',*,*,#10984,.T.);
#14955=ORIENTED_EDGE('',*,*,#10954,.T.);
#14956=ORIENTED_EDGE('',*,*,#10984,.F.);
#14957=ORIENTED_EDGE('',*,*,#10985,.T.);
#14958=ORIENTED_EDGE('',*,*,#10986,.T.);
#14959=ORIENTED_EDGE('',*,*,#10952,.T.);
#14960=ORIENTED_EDGE('',*,*,#10986,.F.);
#14961=ORIENTED_EDGE('',*,*,#10987,.T.);
#14962=ORIENTED_EDGE('',*,*,#10988,.T.);
#14963=ORIENTED_EDGE('',*,*,#10989,.T.);
#14964=ORIENTED_EDGE('',*,*,#10977,.F.);
#14965=ORIENTED_EDGE('',*,*,#10950,.T.);
#14966=ORIENTED_EDGE('',*,*,#10988,.F.);
#14967=ORIENTED_EDGE('',*,*,#10978,.F.);
#14968=ORIENTED_EDGE('',*,*,#10989,.F.);
#14969=ORIENTED_EDGE('',*,*,#10987,.F.);
#14970=ORIENTED_EDGE('',*,*,#10985,.F.);
#14971=ORIENTED_EDGE('',*,*,#10983,.F.);
#14972=ORIENTED_EDGE('',*,*,#10981,.F.);
#14973=ORIENTED_EDGE('',*,*,#10912,.F.);
#14974=ORIENTED_EDGE('',*,*,#10980,.F.);
#14975=ORIENTED_EDGE('',*,*,#10990,.F.);
#14976=ORIENTED_EDGE('',*,*,#10991,.F.);
#14977=ORIENTED_EDGE('',*,*,#10992,.F.);
#14978=ORIENTED_EDGE('',*,*,#10993,.T.);
#14979=ORIENTED_EDGE('',*,*,#10994,.T.);
#14980=ORIENTED_EDGE('',*,*,#10995,.T.);
#14981=ORIENTED_EDGE('',*,*,#10996,.T.);
#14982=ORIENTED_EDGE('',*,*,#10994,.F.);
#14983=ORIENTED_EDGE('',*,*,#10993,.F.);
#14984=ORIENTED_EDGE('',*,*,#10997,.F.);
#14985=ORIENTED_EDGE('',*,*,#10996,.F.);
#14986=ORIENTED_EDGE('',*,*,#10998,.T.);
#14987=ORIENTED_EDGE('',*,*,#10999,.F.);
#14988=ORIENTED_EDGE('',*,*,#10998,.F.);
#14989=ORIENTED_EDGE('',*,*,#10995,.F.);
#14990=ORIENTED_EDGE('',*,*,#10997,.T.);
#14991=ORIENTED_EDGE('',*,*,#11000,.T.);
#14992=ORIENTED_EDGE('',*,*,#11001,.T.);
#14993=ORIENTED_EDGE('',*,*,#11002,.T.);
#14994=ORIENTED_EDGE('',*,*,#11000,.F.);
#14995=ORIENTED_EDGE('',*,*,#11002,.F.);
#14996=ORIENTED_EDGE('',*,*,#11003,.T.);
#14997=ORIENTED_EDGE('',*,*,#11004,.F.);
#14998=ORIENTED_EDGE('',*,*,#11005,.F.);
#14999=ORIENTED_EDGE('',*,*,#11003,.F.);
#15000=ORIENTED_EDGE('',*,*,#11001,.F.);
#15001=ORIENTED_EDGE('',*,*,#10990,.T.);
#15002=ORIENTED_EDGE('',*,*,#11006,.T.);
#15003=ORIENTED_EDGE('',*,*,#11004,.T.);
#15004=ORIENTED_EDGE('',*,*,#11005,.T.);
#15005=ORIENTED_EDGE('',*,*,#11006,.F.);
#15006=ORIENTED_EDGE('',*,*,#10974,.T.);
#15007=ORIENTED_EDGE('',*,*,#11007,.T.);
#15008=ORIENTED_EDGE('',*,*,#11008,.T.);
#15009=ORIENTED_EDGE('',*,*,#11009,.T.);
#15010=ORIENTED_EDGE('',*,*,#11007,.F.);
#15011=ORIENTED_EDGE('',*,*,#11009,.F.);
#15012=ORIENTED_EDGE('',*,*,#11010,.T.);
#15013=ORIENTED_EDGE('',*,*,#11011,.F.);
#15014=ORIENTED_EDGE('',*,*,#11012,.F.);
#15015=ORIENTED_EDGE('',*,*,#11010,.F.);
#15016=ORIENTED_EDGE('',*,*,#11008,.F.);
#15017=ORIENTED_EDGE('',*,*,#10967,.T.);
#15018=ORIENTED_EDGE('',*,*,#11013,.T.);
#15019=ORIENTED_EDGE('',*,*,#11011,.T.);
#15020=ORIENTED_EDGE('',*,*,#11012,.T.);
#15021=ORIENTED_EDGE('',*,*,#11013,.F.);
#15022=ORIENTED_EDGE('',*,*,#10992,.T.);
#15023=ORIENTED_EDGE('',*,*,#11014,.T.);
#15024=ORIENTED_EDGE('',*,*,#11015,.T.);
#15025=ORIENTED_EDGE('',*,*,#11016,.T.);
#15026=ORIENTED_EDGE('',*,*,#11014,.F.);
#15027=ORIENTED_EDGE('',*,*,#11017,.F.);
#15028=ORIENTED_EDGE('',*,*,#11018,.F.);
#15029=ORIENTED_EDGE('',*,*,#11019,.T.);
#15030=ORIENTED_EDGE('',*,*,#11015,.F.);
#15031=ORIENTED_EDGE('',*,*,#11016,.F.);
#15032=ORIENTED_EDGE('',*,*,#11019,.F.);
#15033=ORIENTED_EDGE('',*,*,#11020,.T.);
#15034=ORIENTED_EDGE('',*,*,#11021,.T.);
#15035=ORIENTED_EDGE('',*,*,#11017,.T.);
#15036=ORIENTED_EDGE('',*,*,#11018,.T.);
#15037=ORIENTED_EDGE('',*,*,#11021,.F.);
#15038=ORIENTED_EDGE('',*,*,#10857,.F.);
#15039=ORIENTED_EDGE('',*,*,#10831,.F.);
#15040=ORIENTED_EDGE('',*,*,#10808,.F.);
#15041=ORIENTED_EDGE('',*,*,#10813,.F.);
#15042=ORIENTED_EDGE('',*,*,#10943,.F.);
#15043=ORIENTED_EDGE('',*,*,#10945,.F.);
#15044=ORIENTED_EDGE('',*,*,#10940,.F.);
#15045=ORIENTED_EDGE('',*,*,#10937,.F.);
#15046=ORIENTED_EDGE('',*,*,#10935,.F.);
#15047=ORIENTED_EDGE('',*,*,#10933,.F.);
#15048=ORIENTED_EDGE('',*,*,#10862,.F.);
#15049=ORIENTED_EDGE('',*,*,#11022,.F.);
#15050=ORIENTED_EDGE('',*,*,#10999,.T.);
#15051=ORIENTED_EDGE('',*,*,#11020,.F.);
#15052=ORIENTED_EDGE('',*,*,#10969,.T.);
#15053=ORIENTED_EDGE('',*,*,#11023,.T.);
#15054=ORIENTED_EDGE('',*,*,#11024,.T.);
#15055=ORIENTED_EDGE('',*,*,#11025,.T.);
#15056=ORIENTED_EDGE('',*,*,#11023,.F.);
#15057=ORIENTED_EDGE('',*,*,#11026,.F.);
#15058=ORIENTED_EDGE('',*,*,#11027,.F.);
#15059=ORIENTED_EDGE('',*,*,#11028,.T.);
#15060=ORIENTED_EDGE('',*,*,#11024,.F.);
#15061=ORIENTED_EDGE('',*,*,#11025,.F.);
#15062=ORIENTED_EDGE('',*,*,#11028,.F.);
#15063=ORIENTED_EDGE('',*,*,#11029,.T.);
#15064=ORIENTED_EDGE('',*,*,#11030,.T.);
#15065=ORIENTED_EDGE('',*,*,#11026,.T.);
#15066=ORIENTED_EDGE('',*,*,#11027,.T.);
#15067=ORIENTED_EDGE('',*,*,#11030,.F.);
#15068=ORIENTED_EDGE('',*,*,#10867,.F.);
#15069=ORIENTED_EDGE('',*,*,#11031,.T.);
#15070=ORIENTED_EDGE('',*,*,#10784,.F.);
#15071=ORIENTED_EDGE('',*,*,#10782,.F.);
#15072=ORIENTED_EDGE('',*,*,#10886,.F.);
#15073=ORIENTED_EDGE('',*,*,#10879,.F.);
#15074=ORIENTED_EDGE('',*,*,#10877,.F.);
#15075=ORIENTED_EDGE('',*,*,#10887,.F.);
#15076=ORIENTED_EDGE('',*,*,#10890,.F.);
#15077=ORIENTED_EDGE('',*,*,#10872,.F.);
#15078=ORIENTED_EDGE('',*,*,#10869,.F.);
#15079=ORIENTED_EDGE('',*,*,#11032,.F.);
#15080=ORIENTED_EDGE('',*,*,#10976,.T.);
#15081=ORIENTED_EDGE('',*,*,#11029,.F.);
#15082=ORIENTED_EDGE('',*,*,#10991,.T.);
#15083=ORIENTED_EDGE('',*,*,#11033,.T.);
#15084=ORIENTED_EDGE('',*,*,#11034,.T.);
#15085=ORIENTED_EDGE('',*,*,#11035,.T.);
#15086=ORIENTED_EDGE('',*,*,#11033,.F.);
#15087=ORIENTED_EDGE('',*,*,#11036,.F.);
#15088=ORIENTED_EDGE('',*,*,#11037,.F.);
#15089=ORIENTED_EDGE('',*,*,#11038,.T.);
#15090=ORIENTED_EDGE('',*,*,#11034,.F.);
#15091=ORIENTED_EDGE('',*,*,#11035,.F.);
#15092=ORIENTED_EDGE('',*,*,#11038,.F.);
#15093=ORIENTED_EDGE('',*,*,#11022,.T.);
#15094=ORIENTED_EDGE('',*,*,#11039,.T.);
#15095=ORIENTED_EDGE('',*,*,#11036,.T.);
#15096=ORIENTED_EDGE('',*,*,#11037,.T.);
#15097=ORIENTED_EDGE('',*,*,#11039,.F.);
#15098=ORIENTED_EDGE('',*,*,#10968,.T.);
#15099=ORIENTED_EDGE('',*,*,#11040,.T.);
#15100=ORIENTED_EDGE('',*,*,#11041,.T.);
#15101=ORIENTED_EDGE('',*,*,#11042,.T.);
#15102=ORIENTED_EDGE('',*,*,#11040,.F.);
#15103=ORIENTED_EDGE('',*,*,#11043,.F.);
#15104=ORIENTED_EDGE('',*,*,#11044,.F.);
#15105=ORIENTED_EDGE('',*,*,#11045,.T.);
#15106=ORIENTED_EDGE('',*,*,#11041,.F.);
#15107=ORIENTED_EDGE('',*,*,#11042,.F.);
#15108=ORIENTED_EDGE('',*,*,#11045,.F.);
#15109=ORIENTED_EDGE('',*,*,#11032,.T.);
#15110=ORIENTED_EDGE('',*,*,#11046,.T.);
#15111=ORIENTED_EDGE('',*,*,#11043,.T.);
#15112=ORIENTED_EDGE('',*,*,#11044,.T.);
#15113=ORIENTED_EDGE('',*,*,#11046,.F.);
#15114=ORIENTED_EDGE('',*,*,#11047,.T.);
#15115=ORIENTED_EDGE('',*,*,#11048,.T.);
#15116=ORIENTED_EDGE('',*,*,#11049,.T.);
#15117=ORIENTED_EDGE('',*,*,#11050,.T.);
#15118=ORIENTED_EDGE('',*,*,#11048,.F.);
#15119=ORIENTED_EDGE('',*,*,#11051,.F.);
#15120=ORIENTED_EDGE('',*,*,#11052,.F.);
#15121=ORIENTED_EDGE('',*,*,#11053,.T.);
#15122=ORIENTED_EDGE('',*,*,#11049,.F.);
#15123=ORIENTED_EDGE('',*,*,#11050,.F.);
#15124=ORIENTED_EDGE('',*,*,#11053,.F.);
#15125=ORIENTED_EDGE('',*,*,#11054,.F.);
#15126=ORIENTED_EDGE('',*,*,#11055,.T.);
#15127=ORIENTED_EDGE('',*,*,#10804,.F.);
#15128=ORIENTED_EDGE('',*,*,#10802,.T.);
#15129=ORIENTED_EDGE('',*,*,#11056,.F.);
#15130=ORIENTED_EDGE('',*,*,#10930,.T.);
#15131=ORIENTED_EDGE('',*,*,#10914,.F.);
#15132=ORIENTED_EDGE('',*,*,#10811,.T.);
#15133=ORIENTED_EDGE('',*,*,#11057,.F.);
#15134=ORIENTED_EDGE('',*,*,#11058,.F.);
#15135=ORIENTED_EDGE('',*,*,#11059,.F.);
#15136=ORIENTED_EDGE('',*,*,#11060,.F.);
#15137=ORIENTED_EDGE('',*,*,#11061,.F.);
#15138=ORIENTED_EDGE('',*,*,#11062,.F.);
#15139=ORIENTED_EDGE('',*,*,#11063,.F.);
#15140=ORIENTED_EDGE('',*,*,#11064,.F.);
#15141=ORIENTED_EDGE('',*,*,#11065,.F.);
#15142=ORIENTED_EDGE('',*,*,#11066,.F.);
#15143=ORIENTED_EDGE('',*,*,#11067,.F.);
#15144=ORIENTED_EDGE('',*,*,#11047,.F.);
#15145=ORIENTED_EDGE('',*,*,#11068,.T.);
#15146=ORIENTED_EDGE('',*,*,#10778,.T.);
#15147=ORIENTED_EDGE('',*,*,#10783,.F.);
#15148=ORIENTED_EDGE('',*,*,#11069,.F.);
#15149=ORIENTED_EDGE('',*,*,#11054,.T.);
#15150=ORIENTED_EDGE('',*,*,#11070,.T.);
#15151=ORIENTED_EDGE('',*,*,#11058,.T.);
#15152=ORIENTED_EDGE('',*,*,#11071,.T.);
#15153=ORIENTED_EDGE('',*,*,#11072,.T.);
#15154=ORIENTED_EDGE('',*,*,#11070,.F.);
#15155=ORIENTED_EDGE('',*,*,#11057,.T.);
#15156=ORIENTED_EDGE('',*,*,#10810,.T.);
#15157=ORIENTED_EDGE('',*,*,#10806,.F.);
#15158=ORIENTED_EDGE('',*,*,#10835,.T.);
#15159=ORIENTED_EDGE('',*,*,#11073,.T.);
#15160=ORIENTED_EDGE('',*,*,#11071,.F.);
#15161=ORIENTED_EDGE('',*,*,#11068,.F.);
#15162=ORIENTED_EDGE('',*,*,#11074,.F.);
#15163=ORIENTED_EDGE('',*,*,#11075,.F.);
#15164=ORIENTED_EDGE('',*,*,#10779,.T.);
#15165=ORIENTED_EDGE('',*,*,#11072,.F.);
#15166=ORIENTED_EDGE('',*,*,#11076,.F.);
#15167=ORIENTED_EDGE('',*,*,#11077,.F.);
#15168=ORIENTED_EDGE('',*,*,#11074,.T.);
#15169=ORIENTED_EDGE('',*,*,#11073,.F.);
#15170=ORIENTED_EDGE('',*,*,#10834,.F.);
#15171=ORIENTED_EDGE('',*,*,#11078,.F.);
#15172=ORIENTED_EDGE('',*,*,#11076,.T.);
#15173=ORIENTED_EDGE('',*,*,#10841,.T.);
#15174=ORIENTED_EDGE('',*,*,#10906,.F.);
#15175=ORIENTED_EDGE('',*,*,#11056,.T.);
#15176=ORIENTED_EDGE('',*,*,#10839,.F.);
#15177=ORIENTED_EDGE('',*,*,#11079,.T.);
#15178=ORIENTED_EDGE('',*,*,#11080,.T.);
#15179=ORIENTED_EDGE('',*,*,#11051,.T.);
#15180=ORIENTED_EDGE('',*,*,#11052,.T.);
#15181=ORIENTED_EDGE('',*,*,#11080,.F.);
#15182=ORIENTED_EDGE('',*,*,#10905,.F.);
#15183=ORIENTED_EDGE('',*,*,#11081,.F.);
#15184=ORIENTED_EDGE('',*,*,#11082,.F.);
#15185=ORIENTED_EDGE('',*,*,#11083,.F.);
#15186=ORIENTED_EDGE('',*,*,#11084,.F.);
#15187=ORIENTED_EDGE('',*,*,#10903,.F.);
#15188=ORIENTED_EDGE('',*,*,#11085,.T.);
#15189=ORIENTED_EDGE('',*,*,#11086,.T.);
#15190=ORIENTED_EDGE('',*,*,#11087,.T.);
#15191=ORIENTED_EDGE('',*,*,#11088,.T.);
#15192=ORIENTED_EDGE('',*,*,#11089,.T.);
#15193=ORIENTED_EDGE('',*,*,#11090,.F.);
#15194=ORIENTED_EDGE('',*,*,#11091,.F.);
#15195=ORIENTED_EDGE('',*,*,#11092,.F.);
#15196=ORIENTED_EDGE('',*,*,#11093,.T.);
#15197=ORIENTED_EDGE('',*,*,#11094,.T.);
#15198=ORIENTED_EDGE('',*,*,#11095,.T.);
#15199=ORIENTED_EDGE('',*,*,#11096,.T.);
#15200=ORIENTED_EDGE('',*,*,#11097,.T.);
#15201=ORIENTED_EDGE('',*,*,#11098,.F.);
#15202=ORIENTED_EDGE('',*,*,#11099,.F.);
#15203=ORIENTED_EDGE('',*,*,#11100,.F.);
#15204=ORIENTED_EDGE('',*,*,#11101,.F.);
#15205=ORIENTED_EDGE('',*,*,#11079,.F.);
#15206=ORIENTED_EDGE('',*,*,#11082,.T.);
#15207=ORIENTED_EDGE('',*,*,#11102,.T.);
#15208=ORIENTED_EDGE('',*,*,#11077,.T.);
#15209=ORIENTED_EDGE('',*,*,#11103,.F.);
#15210=ORIENTED_EDGE('',*,*,#11081,.T.);
#15211=ORIENTED_EDGE('',*,*,#10904,.F.);
#15212=ORIENTED_EDGE('',*,*,#11075,.T.);
#15213=ORIENTED_EDGE('',*,*,#11102,.F.);
#15214=ORIENTED_EDGE('',*,*,#10861,.F.);
#15215=ORIENTED_EDGE('',*,*,#11084,.T.);
#15216=ORIENTED_EDGE('',*,*,#11104,.T.);
#15217=ORIENTED_EDGE('',*,*,#10833,.T.);
#15218=ORIENTED_EDGE('',*,*,#11078,.T.);
#15219=ORIENTED_EDGE('',*,*,#11104,.F.);
#15220=ORIENTED_EDGE('',*,*,#11083,.T.);
#15221=ORIENTED_EDGE('',*,*,#11103,.T.);
#15222=ORIENTED_EDGE('',*,*,#11101,.T.);
#15223=ORIENTED_EDGE('',*,*,#11105,.T.);
#15224=ORIENTED_EDGE('',*,*,#11106,.T.);
#15225=ORIENTED_EDGE('',*,*,#11107,.T.);
#15226=ORIENTED_EDGE('',*,*,#11105,.F.);
#15227=ORIENTED_EDGE('',*,*,#11107,.F.);
#15228=ORIENTED_EDGE('',*,*,#11108,.T.);
#15229=ORIENTED_EDGE('',*,*,#11109,.F.);
#15230=ORIENTED_EDGE('',*,*,#11110,.F.);
#15231=ORIENTED_EDGE('',*,*,#11108,.F.);
#15232=ORIENTED_EDGE('',*,*,#11106,.F.);
#15233=ORIENTED_EDGE('',*,*,#11059,.T.);
#15234=ORIENTED_EDGE('',*,*,#11111,.T.);
#15235=ORIENTED_EDGE('',*,*,#11109,.T.);
#15236=ORIENTED_EDGE('',*,*,#11110,.T.);
#15237=ORIENTED_EDGE('',*,*,#11111,.F.);
#15238=ORIENTED_EDGE('',*,*,#11064,.T.);
#15239=ORIENTED_EDGE('',*,*,#11112,.T.);
#15240=ORIENTED_EDGE('',*,*,#11113,.T.);
#15241=ORIENTED_EDGE('',*,*,#11114,.T.);
#15242=ORIENTED_EDGE('',*,*,#11115,.T.);
#15243=ORIENTED_EDGE('',*,*,#11112,.F.);
#15244=ORIENTED_EDGE('',*,*,#11067,.T.);
#15245=ORIENTED_EDGE('',*,*,#11116,.F.);
#15246=ORIENTED_EDGE('',*,*,#11065,.T.);
#15247=ORIENTED_EDGE('',*,*,#11114,.F.);
#15248=ORIENTED_EDGE('',*,*,#11117,.T.);
#15249=ORIENTED_EDGE('',*,*,#11118,.T.);
#15250=ORIENTED_EDGE('',*,*,#11066,.T.);
#15251=ORIENTED_EDGE('',*,*,#11118,.F.);
#15252=ORIENTED_EDGE('',*,*,#11119,.T.);
#15253=ORIENTED_EDGE('',*,*,#11116,.T.);
#15254=ORIENTED_EDGE('',*,*,#11117,.F.);
#15255=ORIENTED_EDGE('',*,*,#11120,.F.);
#15256=ORIENTED_EDGE('',*,*,#11121,.F.);
#15257=ORIENTED_EDGE('',*,*,#11122,.T.);
#15258=ORIENTED_EDGE('',*,*,#11113,.F.);
#15259=ORIENTED_EDGE('',*,*,#11123,.F.);
#15260=ORIENTED_EDGE('',*,*,#11124,.F.);
#15261=ORIENTED_EDGE('',*,*,#11120,.T.);
#15262=ORIENTED_EDGE('',*,*,#11124,.T.);
#15263=ORIENTED_EDGE('',*,*,#11125,.T.);
#15264=ORIENTED_EDGE('',*,*,#11100,.T.);
#15265=ORIENTED_EDGE('',*,*,#11126,.T.);
#15266=ORIENTED_EDGE('',*,*,#11121,.T.);
#15267=ORIENTED_EDGE('',*,*,#11126,.F.);
#15268=ORIENTED_EDGE('',*,*,#11099,.T.);
#15269=ORIENTED_EDGE('',*,*,#11127,.T.);
#15270=ORIENTED_EDGE('',*,*,#11098,.T.);
#15271=ORIENTED_EDGE('',*,*,#11128,.T.);
#15272=ORIENTED_EDGE('',*,*,#11129,.T.);
#15273=ORIENTED_EDGE('',*,*,#11127,.F.);
#15274=ORIENTED_EDGE('',*,*,#11119,.F.);
#15275=ORIENTED_EDGE('',*,*,#11122,.F.);
#15276=ORIENTED_EDGE('',*,*,#11129,.F.);
#15277=ORIENTED_EDGE('',*,*,#11130,.T.);
#15278=ORIENTED_EDGE('',*,*,#11060,.T.);
#15279=ORIENTED_EDGE('',*,*,#11131,.T.);
#15280=ORIENTED_EDGE('',*,*,#11132,.T.);
#15281=ORIENTED_EDGE('',*,*,#11133,.T.);
#15282=ORIENTED_EDGE('',*,*,#11134,.T.);
#15283=ORIENTED_EDGE('',*,*,#11131,.F.);
#15284=ORIENTED_EDGE('',*,*,#11063,.T.);
#15285=ORIENTED_EDGE('',*,*,#11135,.F.);
#15286=ORIENTED_EDGE('',*,*,#11061,.T.);
#15287=ORIENTED_EDGE('',*,*,#11133,.F.);
#15288=ORIENTED_EDGE('',*,*,#11136,.T.);
#15289=ORIENTED_EDGE('',*,*,#11137,.T.);
#15290=ORIENTED_EDGE('',*,*,#11062,.T.);
#15291=ORIENTED_EDGE('',*,*,#11137,.F.);
#15292=ORIENTED_EDGE('',*,*,#11138,.T.);
#15293=ORIENTED_EDGE('',*,*,#11135,.T.);
#15294=ORIENTED_EDGE('',*,*,#11136,.F.);
#15295=ORIENTED_EDGE('',*,*,#11139,.F.);
#15296=ORIENTED_EDGE('',*,*,#11140,.F.);
#15297=ORIENTED_EDGE('',*,*,#11141,.T.);
#15298=ORIENTED_EDGE('',*,*,#11132,.F.);
#15299=ORIENTED_EDGE('',*,*,#11142,.F.);
#15300=ORIENTED_EDGE('',*,*,#11143,.F.);
#15301=ORIENTED_EDGE('',*,*,#11139,.T.);
#15302=ORIENTED_EDGE('',*,*,#11143,.T.);
#15303=ORIENTED_EDGE('',*,*,#11144,.T.);
#15304=ORIENTED_EDGE('',*,*,#11092,.T.);
#15305=ORIENTED_EDGE('',*,*,#11145,.T.);
#15306=ORIENTED_EDGE('',*,*,#11140,.T.);
#15307=ORIENTED_EDGE('',*,*,#11145,.F.);
#15308=ORIENTED_EDGE('',*,*,#11091,.T.);
#15309=ORIENTED_EDGE('',*,*,#11146,.T.);
#15310=ORIENTED_EDGE('',*,*,#11090,.T.);
#15311=ORIENTED_EDGE('',*,*,#11147,.T.);
#15312=ORIENTED_EDGE('',*,*,#11148,.T.);
#15313=ORIENTED_EDGE('',*,*,#11146,.F.);
#15314=ORIENTED_EDGE('',*,*,#11138,.F.);
#15315=ORIENTED_EDGE('',*,*,#11141,.F.);
#15316=ORIENTED_EDGE('',*,*,#11148,.F.);
#15317=ORIENTED_EDGE('',*,*,#11149,.T.);
#15318=ORIENTED_EDGE('',*,*,#11150,.T.);
#15319=ORIENTED_EDGE('',*,*,#11151,.T.);
#15320=ORIENTED_EDGE('',*,*,#11152,.T.);
#15321=ORIENTED_EDGE('',*,*,#11153,.T.);
#15322=ORIENTED_EDGE('',*,*,#11154,.T.);
#15323=ORIENTED_EDGE('',*,*,#11155,.T.);
#15324=ORIENTED_EDGE('',*,*,#11155,.F.);
#15325=ORIENTED_EDGE('',*,*,#11156,.T.);
#15326=ORIENTED_EDGE('',*,*,#11157,.T.);
#15327=ORIENTED_EDGE('',*,*,#11158,.T.);
#15328=ORIENTED_EDGE('',*,*,#11115,.F.);
#15329=ORIENTED_EDGE('',*,*,#11130,.F.);
#15330=ORIENTED_EDGE('',*,*,#11128,.F.);
#15331=ORIENTED_EDGE('',*,*,#11097,.F.);
#15332=ORIENTED_EDGE('',*,*,#11159,.T.);
#15333=ORIENTED_EDGE('',*,*,#11160,.F.);
#15334=ORIENTED_EDGE('',*,*,#11161,.T.);
#15335=ORIENTED_EDGE('',*,*,#11162,.F.);
#15336=ORIENTED_EDGE('',*,*,#11156,.F.);
#15337=ORIENTED_EDGE('',*,*,#11154,.F.);
#15338=ORIENTED_EDGE('',*,*,#11163,.T.);
#15339=ORIENTED_EDGE('',*,*,#11093,.F.);
#15340=ORIENTED_EDGE('',*,*,#11125,.F.);
#15341=ORIENTED_EDGE('',*,*,#11123,.T.);
#15342=ORIENTED_EDGE('',*,*,#11153,.F.);
#15343=ORIENTED_EDGE('',*,*,#11164,.F.);
#15344=ORIENTED_EDGE('',*,*,#11094,.F.);
#15345=ORIENTED_EDGE('',*,*,#11163,.F.);
#15346=ORIENTED_EDGE('',*,*,#11150,.F.);
#15347=ORIENTED_EDGE('',*,*,#11158,.F.);
#15348=ORIENTED_EDGE('',*,*,#11165,.T.);
#15349=ORIENTED_EDGE('',*,*,#11166,.F.);
#15350=ORIENTED_EDGE('',*,*,#11167,.F.);
#15351=ORIENTED_EDGE('',*,*,#11168,.F.);
#15352=ORIENTED_EDGE('',*,*,#11169,.T.);
#15353=ORIENTED_EDGE('',*,*,#11170,.T.);
#15354=ORIENTED_EDGE('',*,*,#11167,.T.);
#15355=ORIENTED_EDGE('',*,*,#11171,.T.);
#15356=ORIENTED_EDGE('',*,*,#11160,.T.);
#15357=ORIENTED_EDGE('',*,*,#11172,.T.);
#15358=ORIENTED_EDGE('',*,*,#11151,.F.);
#15359=ORIENTED_EDGE('',*,*,#11168,.T.);
#15360=ORIENTED_EDGE('',*,*,#11170,.F.);
#15361=ORIENTED_EDGE('',*,*,#11173,.T.);
#15362=ORIENTED_EDGE('',*,*,#11152,.F.);
#15363=ORIENTED_EDGE('',*,*,#11173,.F.);
#15364=ORIENTED_EDGE('',*,*,#11169,.F.);
#15365=ORIENTED_EDGE('',*,*,#11174,.F.);
#15366=ORIENTED_EDGE('',*,*,#11095,.F.);
#15367=ORIENTED_EDGE('',*,*,#11164,.T.);
#15368=ORIENTED_EDGE('',*,*,#11172,.F.);
#15369=ORIENTED_EDGE('',*,*,#11159,.F.);
#15370=ORIENTED_EDGE('',*,*,#11096,.F.);
#15371=ORIENTED_EDGE('',*,*,#11174,.T.);
#15372=ORIENTED_EDGE('',*,*,#11171,.F.);
#15373=ORIENTED_EDGE('',*,*,#11166,.T.);
#15374=ORIENTED_EDGE('',*,*,#11175,.T.);
#15375=ORIENTED_EDGE('',*,*,#11161,.F.);
#15376=ORIENTED_EDGE('',*,*,#11176,.T.);
#15377=ORIENTED_EDGE('',*,*,#11177,.T.);
#15378=ORIENTED_EDGE('',*,*,#11178,.T.);
#15379=ORIENTED_EDGE('',*,*,#11179,.T.);
#15380=ORIENTED_EDGE('',*,*,#11180,.T.);
#15381=ORIENTED_EDGE('',*,*,#11181,.T.);
#15382=ORIENTED_EDGE('',*,*,#11181,.F.);
#15383=ORIENTED_EDGE('',*,*,#11182,.T.);
#15384=ORIENTED_EDGE('',*,*,#11183,.T.);
#15385=ORIENTED_EDGE('',*,*,#11184,.T.);
#15386=ORIENTED_EDGE('',*,*,#11134,.F.);
#15387=ORIENTED_EDGE('',*,*,#11149,.F.);
#15388=ORIENTED_EDGE('',*,*,#11147,.F.);
#15389=ORIENTED_EDGE('',*,*,#11089,.F.);
#15390=ORIENTED_EDGE('',*,*,#11185,.T.);
#15391=ORIENTED_EDGE('',*,*,#11186,.F.);
#15392=ORIENTED_EDGE('',*,*,#11187,.T.);
#15393=ORIENTED_EDGE('',*,*,#11188,.F.);
#15394=ORIENTED_EDGE('',*,*,#11182,.F.);
#15395=ORIENTED_EDGE('',*,*,#11180,.F.);
#15396=ORIENTED_EDGE('',*,*,#11189,.T.);
#15397=ORIENTED_EDGE('',*,*,#11085,.F.);
#15398=ORIENTED_EDGE('',*,*,#11144,.F.);
#15399=ORIENTED_EDGE('',*,*,#11142,.T.);
#15400=ORIENTED_EDGE('',*,*,#11179,.F.);
#15401=ORIENTED_EDGE('',*,*,#11190,.F.);
#15402=ORIENTED_EDGE('',*,*,#11086,.F.);
#15403=ORIENTED_EDGE('',*,*,#11189,.F.);
#15404=ORIENTED_EDGE('',*,*,#11176,.F.);
#15405=ORIENTED_EDGE('',*,*,#11184,.F.);
#15406=ORIENTED_EDGE('',*,*,#11191,.T.);
#15407=ORIENTED_EDGE('',*,*,#11192,.F.);
#15408=ORIENTED_EDGE('',*,*,#11193,.F.);
#15409=ORIENTED_EDGE('',*,*,#11194,.F.);
#15410=ORIENTED_EDGE('',*,*,#11195,.T.);
#15411=ORIENTED_EDGE('',*,*,#11196,.T.);
#15412=ORIENTED_EDGE('',*,*,#11193,.T.);
#15413=ORIENTED_EDGE('',*,*,#11197,.T.);
#15414=ORIENTED_EDGE('',*,*,#11186,.T.);
#15415=ORIENTED_EDGE('',*,*,#11198,.T.);
#15416=ORIENTED_EDGE('',*,*,#11177,.F.);
#15417=ORIENTED_EDGE('',*,*,#11194,.T.);
#15418=ORIENTED_EDGE('',*,*,#11196,.F.);
#15419=ORIENTED_EDGE('',*,*,#11199,.T.);
#15420=ORIENTED_EDGE('',*,*,#11178,.F.);
#15421=ORIENTED_EDGE('',*,*,#11199,.F.);
#15422=ORIENTED_EDGE('',*,*,#11195,.F.);
#15423=ORIENTED_EDGE('',*,*,#11200,.F.);
#15424=ORIENTED_EDGE('',*,*,#11087,.F.);
#15425=ORIENTED_EDGE('',*,*,#11190,.T.);
#15426=ORIENTED_EDGE('',*,*,#11198,.F.);
#15427=ORIENTED_EDGE('',*,*,#11185,.F.);
#15428=ORIENTED_EDGE('',*,*,#11088,.F.);
#15429=ORIENTED_EDGE('',*,*,#11200,.T.);
#15430=ORIENTED_EDGE('',*,*,#11197,.F.);
#15431=ORIENTED_EDGE('',*,*,#11192,.T.);
#15432=ORIENTED_EDGE('',*,*,#11201,.T.);
#15433=ORIENTED_EDGE('',*,*,#11187,.F.);
#15434=ORIENTED_EDGE('',*,*,#11183,.F.);
#15435=ORIENTED_EDGE('',*,*,#11188,.T.);
#15436=ORIENTED_EDGE('',*,*,#11201,.F.);
#15437=ORIENTED_EDGE('',*,*,#11191,.F.);
#15438=ORIENTED_EDGE('',*,*,#11157,.F.);
#15439=ORIENTED_EDGE('',*,*,#11162,.T.);
#15440=ORIENTED_EDGE('',*,*,#11175,.F.);
#15441=ORIENTED_EDGE('',*,*,#11165,.F.);
#15442=ORIENTED_EDGE('',*,*,#10771,.F.);
#15443=ORIENTED_EDGE('',*,*,#10774,.F.);
#15444=ORIENTED_EDGE('',*,*,#10788,.F.);
#15445=ORIENTED_EDGE('',*,*,#10796,.T.);
#15446=ORIENTED_EDGE('',*,*,#10785,.F.);
#15447=ORIENTED_EDGE('',*,*,#11031,.F.);
#15448=ORIENTED_EDGE('',*,*,#10805,.F.);
#15449=ORIENTED_EDGE('',*,*,#11055,.F.);
#15450=ORIENTED_EDGE('',*,*,#11069,.T.);
#15451=ORIENTED_EDGE('',*,*,#10825,.F.);
#15452=ORIENTED_EDGE('',*,*,#10828,.F.);
#15453=ORIENTED_EDGE('',*,*,#10918,.F.);
#15454=ORIENTED_EDGE('',*,*,#10926,.T.);
#15455=ORIENTED_EDGE('',*,*,#11202,.F.);
#15456=ORIENTED_EDGE('',*,*,#11203,.F.);
#15457=ORIENTED_EDGE('',*,*,#11204,.F.);
#15458=ORIENTED_EDGE('',*,*,#11205,.F.);
#15459=ORIENTED_EDGE('',*,*,#11206,.F.);
#15460=ORIENTED_EDGE('',*,*,#11207,.F.);
#15461=ORIENTED_EDGE('',*,*,#11208,.T.);
#15462=ORIENTED_EDGE('',*,*,#11209,.T.);
#15463=ORIENTED_EDGE('',*,*,#11206,.T.);
#15464=ORIENTED_EDGE('',*,*,#11210,.T.);
#15465=ORIENTED_EDGE('',*,*,#11211,.T.);
#15466=ORIENTED_EDGE('',*,*,#11212,.T.);
#15467=ORIENTED_EDGE('',*,*,#11207,.T.);
#15468=ORIENTED_EDGE('',*,*,#11213,.T.);
#15469=ORIENTED_EDGE('',*,*,#11203,.T.);
#15470=ORIENTED_EDGE('',*,*,#11214,.T.);
#15471=ORIENTED_EDGE('',*,*,#11205,.T.);
#15472=ORIENTED_EDGE('',*,*,#11215,.T.);
#15473=ORIENTED_EDGE('',*,*,#11216,.F.);
#15474=ORIENTED_EDGE('',*,*,#11217,.F.);
#15475=ORIENTED_EDGE('',*,*,#11218,.F.);
#15476=ORIENTED_EDGE('',*,*,#11219,.T.);
#15477=ORIENTED_EDGE('',*,*,#11220,.T.);
#15478=ORIENTED_EDGE('',*,*,#11217,.T.);
#15479=ORIENTED_EDGE('',*,*,#11221,.T.);
#15480=ORIENTED_EDGE('',*,*,#11222,.T.);
#15481=ORIENTED_EDGE('',*,*,#11218,.T.);
#15482=ORIENTED_EDGE('',*,*,#11223,.T.);
#15483=ORIENTED_EDGE('',*,*,#11224,.T.);
#15484=ORIENTED_EDGE('',*,*,#11225,.T.);
#15485=ORIENTED_EDGE('',*,*,#11202,.T.);
#15486=ORIENTED_EDGE('',*,*,#11226,.T.);
#15487=ORIENTED_EDGE('',*,*,#11227,.T.);
#15488=ORIENTED_EDGE('',*,*,#11228,.F.);
#15489=ORIENTED_EDGE('',*,*,#11229,.F.);
#15490=ORIENTED_EDGE('',*,*,#11230,.F.);
#15491=ORIENTED_EDGE('',*,*,#11231,.T.);
#15492=ORIENTED_EDGE('',*,*,#11229,.T.);
#15493=ORIENTED_EDGE('',*,*,#11232,.T.);
#15494=ORIENTED_EDGE('',*,*,#11224,.F.);
#15495=ORIENTED_EDGE('',*,*,#11233,.T.);
#15496=ORIENTED_EDGE('',*,*,#11234,.T.);
#15497=ORIENTED_EDGE('',*,*,#11230,.T.);
#15498=ORIENTED_EDGE('',*,*,#11235,.T.);
#15499=ORIENTED_EDGE('',*,*,#11236,.F.);
#15500=ORIENTED_EDGE('',*,*,#11237,.F.);
#15501=ORIENTED_EDGE('',*,*,#11238,.F.);
#15502=ORIENTED_EDGE('',*,*,#11239,.T.);
#15503=ORIENTED_EDGE('',*,*,#11237,.T.);
#15504=ORIENTED_EDGE('',*,*,#11240,.T.);
#15505=ORIENTED_EDGE('',*,*,#11227,.F.);
#15506=ORIENTED_EDGE('',*,*,#11228,.T.);
#15507=ORIENTED_EDGE('',*,*,#11241,.T.);
#15508=ORIENTED_EDGE('',*,*,#11238,.T.);
#15509=ORIENTED_EDGE('',*,*,#11242,.T.);
#15510=ORIENTED_EDGE('',*,*,#11243,.F.);
#15511=ORIENTED_EDGE('',*,*,#11244,.F.);
#15512=ORIENTED_EDGE('',*,*,#11245,.F.);
#15513=ORIENTED_EDGE('',*,*,#11246,.F.);
#15514=ORIENTED_EDGE('',*,*,#11247,.F.);
#15515=ORIENTED_EDGE('',*,*,#11248,.F.);
#15516=ORIENTED_EDGE('',*,*,#11249,.T.);
#15517=ORIENTED_EDGE('',*,*,#11250,.T.);
#15518=ORIENTED_EDGE('',*,*,#11247,.T.);
#15519=ORIENTED_EDGE('',*,*,#11251,.T.);
#15520=ORIENTED_EDGE('',*,*,#11252,.F.);
#15521=ORIENTED_EDGE('',*,*,#11253,.F.);
#15522=ORIENTED_EDGE('',*,*,#11254,.F.);
#15523=ORIENTED_EDGE('',*,*,#11253,.T.);
#15524=ORIENTED_EDGE('',*,*,#11255,.T.);
#15525=ORIENTED_EDGE('',*,*,#11248,.T.);
#15526=ORIENTED_EDGE('',*,*,#11256,.T.);
#15527=ORIENTED_EDGE('',*,*,#11257,.T.);
#15528=ORIENTED_EDGE('',*,*,#11254,.T.);
#15529=ORIENTED_EDGE('',*,*,#11258,.T.);
#15530=ORIENTED_EDGE('',*,*,#11259,.T.);
#15531=ORIENTED_EDGE('',*,*,#11260,.T.);
#15532=ORIENTED_EDGE('',*,*,#11261,.T.);
#15533=ORIENTED_EDGE('',*,*,#11262,.T.);
#15534=ORIENTED_EDGE('',*,*,#11260,.F.);
#15535=ORIENTED_EDGE('',*,*,#11263,.T.);
#15536=ORIENTED_EDGE('',*,*,#11252,.T.);
#15537=ORIENTED_EDGE('',*,*,#11264,.T.);
#15538=ORIENTED_EDGE('',*,*,#11265,.T.);
#15539=ORIENTED_EDGE('',*,*,#11244,.T.);
#15540=ORIENTED_EDGE('',*,*,#11266,.T.);
#15541=ORIENTED_EDGE('',*,*,#11259,.F.);
#15542=ORIENTED_EDGE('',*,*,#11267,.T.);
#15543=ORIENTED_EDGE('',*,*,#11268,.T.);
#15544=ORIENTED_EDGE('',*,*,#11246,.T.);
#15545=ORIENTED_EDGE('',*,*,#11269,.T.);
#15546=ORIENTED_EDGE('',*,*,#11267,.F.);
#15547=ORIENTED_EDGE('',*,*,#11270,.T.);
#15548=ORIENTED_EDGE('',*,*,#11271,.T.);
#15549=ORIENTED_EDGE('',*,*,#11236,.T.);
#15550=ORIENTED_EDGE('',*,*,#11272,.T.);
#15551=ORIENTED_EDGE('',*,*,#11245,.T.);
#15552=ORIENTED_EDGE('',*,*,#11273,.T.);
#15553=ORIENTED_EDGE('',*,*,#11274,.T.);
#15554=ORIENTED_EDGE('',*,*,#11275,.T.);
#15555=ORIENTED_EDGE('',*,*,#11243,.T.);
#15556=ORIENTED_EDGE('',*,*,#11276,.T.);
#15557=ORIENTED_EDGE('',*,*,#11216,.T.);
#15558=ORIENTED_EDGE('',*,*,#11277,.T.);
#15559=ORIENTED_EDGE('',*,*,#11204,.T.);
#15560=ORIENTED_EDGE('',*,*,#11278,.T.);
#15561=ORIENTED_EDGE('',*,*,#11249,.F.);
#15562=ORIENTED_EDGE('',*,*,#11279,.T.);
#15563=ORIENTED_EDGE('',*,*,#11280,.T.);
#15564=ORIENTED_EDGE('',*,*,#11281,.T.);
#15565=ORIENTED_EDGE('',*,*,#11233,.F.);
#15566=ORIENTED_EDGE('',*,*,#11282,.T.);
#15567=ORIENTED_EDGE('',*,*,#11274,.F.);
#15568=ORIENTED_EDGE('',*,*,#11208,.F.);
#15569=ORIENTED_EDGE('',*,*,#11283,.T.);
#15570=ORIENTED_EDGE('',*,*,#11284,.T.);
#15571=ORIENTED_EDGE('',*,*,#11285,.T.);
#15572=ORIENTED_EDGE('',*,*,#11211,.F.);
#15573=ORIENTED_EDGE('',*,*,#11286,.T.);
#15574=ORIENTED_EDGE('',*,*,#11219,.F.);
#15575=ORIENTED_EDGE('',*,*,#11232,.F.);
#15576=ORIENTED_EDGE('',*,*,#11242,.F.);
#15577=ORIENTED_EDGE('',*,*,#11239,.F.);
#15578=ORIENTED_EDGE('',*,*,#11287,.F.);
#15579=ORIENTED_EDGE('',*,*,#11213,.F.);
#15580=ORIENTED_EDGE('',*,*,#11209,.F.);
#15581=ORIENTED_EDGE('',*,*,#11285,.F.);
#15582=ORIENTED_EDGE('',*,*,#11279,.F.);
#15583=ORIENTED_EDGE('',*,*,#11251,.F.);
#15584=ORIENTED_EDGE('',*,*,#11268,.F.);
#15585=ORIENTED_EDGE('',*,*,#11288,.F.);
#15586=ORIENTED_EDGE('',*,*,#11289,.F.);
#15587=ORIENTED_EDGE('',*,*,#11290,.F.);
#15588=ORIENTED_EDGE('',*,*,#11269,.F.);
#15589=ORIENTED_EDGE('',*,*,#11255,.F.);
#15590=ORIENTED_EDGE('',*,*,#11263,.F.);
#15591=ORIENTED_EDGE('',*,*,#11291,.F.);
#15592=ORIENTED_EDGE('',*,*,#11270,.F.);
#15593=ORIENTED_EDGE('',*,*,#11291,.T.);
#15594=ORIENTED_EDGE('',*,*,#11262,.F.);
#15595=ORIENTED_EDGE('',*,*,#11292,.T.);
#15596=ORIENTED_EDGE('',*,*,#11212,.F.);
#15597=ORIENTED_EDGE('',*,*,#11221,.F.);
#15598=ORIENTED_EDGE('',*,*,#11278,.F.);
#15599=ORIENTED_EDGE('',*,*,#11215,.F.);
#15600=ORIENTED_EDGE('',*,*,#11234,.F.);
#15601=ORIENTED_EDGE('',*,*,#11276,.F.);
#15602=ORIENTED_EDGE('',*,*,#11272,.F.);
#15603=ORIENTED_EDGE('',*,*,#11241,.F.);
#15604=ORIENTED_EDGE('',*,*,#11286,.F.);
#15605=ORIENTED_EDGE('',*,*,#11288,.T.);
#15606=ORIENTED_EDGE('',*,*,#11271,.F.);
#15607=ORIENTED_EDGE('',*,*,#11293,.T.);
#15608=ORIENTED_EDGE('',*,*,#11261,.F.);
#15609=ORIENTED_EDGE('',*,*,#11294,.T.);
#15610=ORIENTED_EDGE('',*,*,#11295,.T.);
#15611=ORIENTED_EDGE('',*,*,#11296,.T.);
#15612=ORIENTED_EDGE('',*,*,#11282,.F.);
#15613=ORIENTED_EDGE('',*,*,#11297,.T.);
#15614=ORIENTED_EDGE('',*,*,#11295,.F.);
#15615=ORIENTED_EDGE('',*,*,#11298,.T.);
#15616=ORIENTED_EDGE('',*,*,#11257,.F.);
#15617=ORIENTED_EDGE('',*,*,#11299,.T.);
#15618=ORIENTED_EDGE('',*,*,#11294,.F.);
#15619=ORIENTED_EDGE('',*,*,#11264,.F.);
#15620=ORIENTED_EDGE('',*,*,#11300,.T.);
#15621=ORIENTED_EDGE('',*,*,#11301,.T.);
#15622=ORIENTED_EDGE('',*,*,#11302,.T.);
#15623=ORIENTED_EDGE('',*,*,#11301,.F.);
#15624=ORIENTED_EDGE('',*,*,#11303,.F.);
#15625=ORIENTED_EDGE('',*,*,#11304,.T.);
#15626=ORIENTED_EDGE('',*,*,#11300,.F.);
#15627=ORIENTED_EDGE('',*,*,#11304,.F.);
#15628=ORIENTED_EDGE('',*,*,#11305,.T.);
#15629=ORIENTED_EDGE('',*,*,#11306,.T.);
#15630=ORIENTED_EDGE('',*,*,#11307,.T.);
#15631=ORIENTED_EDGE('',*,*,#11306,.F.);
#15632=ORIENTED_EDGE('',*,*,#11305,.F.);
#15633=ORIENTED_EDGE('',*,*,#11308,.F.);
#15634=ORIENTED_EDGE('',*,*,#11307,.F.);
#15635=ORIENTED_EDGE('',*,*,#11309,.T.);
#15636=ORIENTED_EDGE('',*,*,#11310,.F.);
#15637=ORIENTED_EDGE('',*,*,#11311,.F.);
#15638=ORIENTED_EDGE('',*,*,#11281,.F.);
#15639=ORIENTED_EDGE('',*,*,#11280,.F.);
#15640=ORIENTED_EDGE('',*,*,#11284,.F.);
#15641=ORIENTED_EDGE('',*,*,#11283,.F.);
#15642=ORIENTED_EDGE('',*,*,#11312,.F.);
#15643=ORIENTED_EDGE('',*,*,#11313,.F.);
#15644=ORIENTED_EDGE('',*,*,#11314,.F.);
#15645=ORIENTED_EDGE('',*,*,#11315,.F.);
#15646=ORIENTED_EDGE('',*,*,#11309,.F.);
#15647=ORIENTED_EDGE('',*,*,#11316,.T.);
#15648=ORIENTED_EDGE('',*,*,#11317,.T.);
#15649=ORIENTED_EDGE('',*,*,#11308,.T.);
#15650=ORIENTED_EDGE('',*,*,#11317,.F.);
#15651=ORIENTED_EDGE('',*,*,#11290,.T.);
#15652=ORIENTED_EDGE('',*,*,#11318,.T.);
#15653=ORIENTED_EDGE('',*,*,#11319,.T.);
#15654=ORIENTED_EDGE('',*,*,#11320,.T.);
#15655=ORIENTED_EDGE('',*,*,#11318,.F.);
#15656=ORIENTED_EDGE('',*,*,#11320,.F.);
#15657=ORIENTED_EDGE('',*,*,#11321,.T.);
#15658=ORIENTED_EDGE('',*,*,#11322,.T.);
#15659=ORIENTED_EDGE('',*,*,#11321,.F.);
#15660=ORIENTED_EDGE('',*,*,#11319,.F.);
#15661=ORIENTED_EDGE('',*,*,#11289,.T.);
#15662=ORIENTED_EDGE('',*,*,#11323,.T.);
#15663=ORIENTED_EDGE('',*,*,#11324,.T.);
#15664=ORIENTED_EDGE('',*,*,#11325,.T.);
#15665=ORIENTED_EDGE('',*,*,#11323,.F.);
#15666=ORIENTED_EDGE('',*,*,#11325,.F.);
#15667=ORIENTED_EDGE('',*,*,#11326,.T.);
#15668=ORIENTED_EDGE('',*,*,#11327,.T.);
#15669=ORIENTED_EDGE('',*,*,#11326,.F.);
#15670=ORIENTED_EDGE('',*,*,#11324,.F.);
#15671=ORIENTED_EDGE('',*,*,#11328,.T.);
#15672=ORIENTED_EDGE('',*,*,#11329,.T.);
#15673=ORIENTED_EDGE('',*,*,#11330,.T.);
#15674=ORIENTED_EDGE('',*,*,#11331,.T.);
#15675=ORIENTED_EDGE('',*,*,#11332,.T.);
#15676=ORIENTED_EDGE('',*,*,#11333,.T.);
#15677=ORIENTED_EDGE('',*,*,#11329,.F.);
#15678=ORIENTED_EDGE('',*,*,#11334,.T.);
#15679=ORIENTED_EDGE('',*,*,#11335,.F.);
#15680=ORIENTED_EDGE('',*,*,#11336,.T.);
#15681=ORIENTED_EDGE('',*,*,#11331,.F.);
#15682=ORIENTED_EDGE('',*,*,#11337,.T.);
#15683=ORIENTED_EDGE('',*,*,#11310,.T.);
#15684=ORIENTED_EDGE('',*,*,#11315,.T.);
#15685=ORIENTED_EDGE('',*,*,#11335,.T.);
#15686=ORIENTED_EDGE('',*,*,#11338,.T.);
#15687=ORIENTED_EDGE('',*,*,#11332,.F.);
#15688=ORIENTED_EDGE('',*,*,#11339,.T.);
#15689=ORIENTED_EDGE('',*,*,#11340,.T.);
#15690=ORIENTED_EDGE('',*,*,#11341,.F.);
#15691=ORIENTED_EDGE('',*,*,#11313,.T.);
#15692=ORIENTED_EDGE('',*,*,#11250,.F.);
#15693=ORIENTED_EDGE('',*,*,#11311,.T.);
#15694=ORIENTED_EDGE('',*,*,#11334,.F.);
#15695=ORIENTED_EDGE('',*,*,#11328,.F.);
#15696=ORIENTED_EDGE('',*,*,#11336,.F.);
#15697=ORIENTED_EDGE('',*,*,#11314,.T.);
#15698=ORIENTED_EDGE('',*,*,#11342,.F.);
#15699=ORIENTED_EDGE('',*,*,#11343,.F.);
#15700=ORIENTED_EDGE('',*,*,#11344,.F.);
#15701=ORIENTED_EDGE('',*,*,#11312,.T.);
#15702=ORIENTED_EDGE('',*,*,#11210,.F.);
#15703=ORIENTED_EDGE('',*,*,#11214,.F.);
#15704=ORIENTED_EDGE('',*,*,#11225,.F.);
#15705=ORIENTED_EDGE('',*,*,#11240,.F.);
#15706=ORIENTED_EDGE('',*,*,#11273,.F.);
#15707=ORIENTED_EDGE('',*,*,#11265,.F.);
#15708=ORIENTED_EDGE('',*,*,#11258,.F.);
#15709=ORIENTED_EDGE('',*,*,#11256,.F.);
#15710=ORIENTED_EDGE('',*,*,#11344,.T.);
#15711=ORIENTED_EDGE('',*,*,#11345,.T.);
#15712=ORIENTED_EDGE('',*,*,#11346,.T.);
#15713=ORIENTED_EDGE('',*,*,#11339,.F.);
#15714=ORIENTED_EDGE('',*,*,#11347,.T.);
#15715=ORIENTED_EDGE('',*,*,#11348,.T.);
#15716=ORIENTED_EDGE('',*,*,#11342,.T.);
#15717=ORIENTED_EDGE('',*,*,#11341,.T.);
#15718=ORIENTED_EDGE('',*,*,#11343,.T.);
#15719=ORIENTED_EDGE('',*,*,#11348,.F.);
#15720=ORIENTED_EDGE('',*,*,#11349,.T.);
#15721=ORIENTED_EDGE('',*,*,#11345,.F.);
#15722=ORIENTED_EDGE('',*,*,#11350,.T.);
#15723=ORIENTED_EDGE('',*,*,#11351,.T.);
#15724=ORIENTED_EDGE('',*,*,#11352,.T.);
#15725=ORIENTED_EDGE('',*,*,#11351,.F.);
#15726=ORIENTED_EDGE('',*,*,#11337,.F.);
#15727=ORIENTED_EDGE('',*,*,#11330,.F.);
#15728=ORIENTED_EDGE('',*,*,#11333,.F.);
#15729=ORIENTED_EDGE('',*,*,#11338,.F.);
#15730=ORIENTED_EDGE('',*,*,#11353,.F.);
#15731=ORIENTED_EDGE('',*,*,#11352,.F.);
#15732=ORIENTED_EDGE('',*,*,#11354,.T.);
#15733=ORIENTED_EDGE('',*,*,#11355,.T.);
#15734=ORIENTED_EDGE('',*,*,#11353,.T.);
#15735=ORIENTED_EDGE('',*,*,#11355,.F.);
#15736=ORIENTED_EDGE('',*,*,#11356,.T.);
#15737=ORIENTED_EDGE('',*,*,#11357,.T.);
#15738=ORIENTED_EDGE('',*,*,#11358,.T.);
#15739=ORIENTED_EDGE('',*,*,#11357,.F.);
#15740=ORIENTED_EDGE('',*,*,#11349,.F.);
#15741=ORIENTED_EDGE('',*,*,#11347,.F.);
#15742=ORIENTED_EDGE('',*,*,#11340,.F.);
#15743=ORIENTED_EDGE('',*,*,#11346,.F.);
#15744=ORIENTED_EDGE('',*,*,#11359,.F.);
#15745=ORIENTED_EDGE('',*,*,#11358,.F.);
#15746=ORIENTED_EDGE('',*,*,#11360,.T.);
#15747=ORIENTED_EDGE('',*,*,#11361,.T.);
#15748=ORIENTED_EDGE('',*,*,#11359,.T.);
#15749=ORIENTED_EDGE('',*,*,#11361,.F.);
#15750=ORIENTED_EDGE('',*,*,#11362,.T.);
#15751=ORIENTED_EDGE('',*,*,#11363,.T.);
#15752=ORIENTED_EDGE('',*,*,#11364,.T.);
#15753=ORIENTED_EDGE('',*,*,#11363,.F.);
#15754=ORIENTED_EDGE('',*,*,#11364,.F.);
#15755=ORIENTED_EDGE('',*,*,#11302,.F.);
#15756=ORIENTED_EDGE('',*,*,#11360,.F.);
#15757=ORIENTED_EDGE('',*,*,#11356,.F.);
#15758=ORIENTED_EDGE('',*,*,#11354,.F.);
#15759=ORIENTED_EDGE('',*,*,#11350,.F.);
#15760=ORIENTED_EDGE('',*,*,#11327,.F.);
#15761=ORIENTED_EDGE('',*,*,#11322,.F.);
#15762=ORIENTED_EDGE('',*,*,#11316,.F.);
#15763=ORIENTED_EDGE('',*,*,#11362,.F.);
#15764=ORIENTED_EDGE('',*,*,#11303,.T.);
#15765=ORIENTED_EDGE('',*,*,#11365,.F.);
#15766=ORIENTED_EDGE('',*,*,#11366,.T.);
#15767=ORIENTED_EDGE('',*,*,#11367,.T.);
#15768=ORIENTED_EDGE('',*,*,#11368,.T.);
#15769=ORIENTED_EDGE('',*,*,#11367,.F.);
#15770=ORIENTED_EDGE('',*,*,#11366,.F.);
#15771=ORIENTED_EDGE('',*,*,#11369,.T.);
#15772=ORIENTED_EDGE('',*,*,#11365,.T.);
#15773=ORIENTED_EDGE('',*,*,#11369,.F.);
#15774=ORIENTED_EDGE('',*,*,#11220,.F.);
#15775=ORIENTED_EDGE('',*,*,#11293,.F.);
#15776=ORIENTED_EDGE('',*,*,#11292,.F.);
#15777=ORIENTED_EDGE('',*,*,#11296,.F.);
#15778=ORIENTED_EDGE('',*,*,#11297,.F.);
#15779=ORIENTED_EDGE('',*,*,#11235,.F.);
#15780=ORIENTED_EDGE('',*,*,#11231,.F.);
#15781=ORIENTED_EDGE('',*,*,#11223,.F.);
#15782=ORIENTED_EDGE('',*,*,#11368,.F.);
#15783=ORIENTED_EDGE('',*,*,#11275,.F.);
#15784=ORIENTED_EDGE('',*,*,#11298,.F.);
#15785=ORIENTED_EDGE('',*,*,#11299,.F.);
#15786=ORIENTED_EDGE('',*,*,#11266,.F.);
#15787=ORIENTED_EDGE('',*,*,#11222,.F.);
#15788=ORIENTED_EDGE('',*,*,#11287,.T.);
#15789=ORIENTED_EDGE('',*,*,#11226,.F.);
#15790=ORIENTED_EDGE('',*,*,#11277,.F.);
#15791=ORIENTED_EDGE('',*,*,#11370,.T.);
#15792=ORIENTED_EDGE('',*,*,#11371,.T.);
#15793=ORIENTED_EDGE('',*,*,#11372,.T.);
#15794=ORIENTED_EDGE('',*,*,#11371,.F.);
#15795=ORIENTED_EDGE('',*,*,#11373,.T.);
#15796=ORIENTED_EDGE('',*,*,#11374,.F.);
#15797=ORIENTED_EDGE('',*,*,#11375,.F.);
#15798=ORIENTED_EDGE('',*,*,#11376,.T.);
#15799=ORIENTED_EDGE('',*,*,#11373,.F.);
#15800=ORIENTED_EDGE('',*,*,#11370,.F.);
#15801=ORIENTED_EDGE('',*,*,#11376,.F.);
#15802=ORIENTED_EDGE('',*,*,#11372,.F.);
#15803=ORIENTED_EDGE('',*,*,#11377,.T.);
#15804=ORIENTED_EDGE('',*,*,#11374,.T.);
#15805=ORIENTED_EDGE('',*,*,#11375,.T.);
#15806=ORIENTED_EDGE('',*,*,#11378,.T.);
#15807=ORIENTED_EDGE('',*,*,#11379,.T.);
#15808=ORIENTED_EDGE('',*,*,#11378,.F.);
#15809=ORIENTED_EDGE('',*,*,#11379,.F.);
#15810=ORIENTED_EDGE('',*,*,#11380,.T.);
#15811=ORIENTED_EDGE('',*,*,#11381,.T.);
#15812=ORIENTED_EDGE('',*,*,#11382,.T.);
#15813=ORIENTED_EDGE('',*,*,#11383,.T.);
#15814=ORIENTED_EDGE('',*,*,#11384,.T.);
#15815=ORIENTED_EDGE('',*,*,#11385,.T.);
#15816=ORIENTED_EDGE('',*,*,#11386,.T.);
#15817=ORIENTED_EDGE('',*,*,#11387,.T.);
#15818=ORIENTED_EDGE('',*,*,#11388,.T.);
#15819=ORIENTED_EDGE('',*,*,#11389,.T.);
#15820=ORIENTED_EDGE('',*,*,#11390,.T.);
#15821=ORIENTED_EDGE('',*,*,#11391,.T.);
#15822=ORIENTED_EDGE('',*,*,#11392,.T.);
#15823=ORIENTED_EDGE('',*,*,#11393,.T.);
#15824=ORIENTED_EDGE('',*,*,#11394,.T.);
#15825=ORIENTED_EDGE('',*,*,#11395,.T.);
#15826=ORIENTED_EDGE('',*,*,#11396,.T.);
#15827=ORIENTED_EDGE('',*,*,#11397,.T.);
#15828=ORIENTED_EDGE('',*,*,#11398,.T.);
#15829=ORIENTED_EDGE('',*,*,#11399,.T.);
#15830=ORIENTED_EDGE('',*,*,#11400,.T.);
#15831=ORIENTED_EDGE('',*,*,#11401,.T.);
#15832=ORIENTED_EDGE('',*,*,#11402,.T.);
#15833=ORIENTED_EDGE('',*,*,#11403,.T.);
#15834=ORIENTED_EDGE('',*,*,#11404,.T.);
#15835=ORIENTED_EDGE('',*,*,#11405,.T.);
#15836=ORIENTED_EDGE('',*,*,#11406,.T.);
#15837=ORIENTED_EDGE('',*,*,#11407,.T.);
#15838=ORIENTED_EDGE('',*,*,#11408,.T.);
#15839=ORIENTED_EDGE('',*,*,#11409,.T.);
#15840=ORIENTED_EDGE('',*,*,#11410,.T.);
#15841=ORIENTED_EDGE('',*,*,#11411,.T.);
#15842=ORIENTED_EDGE('',*,*,#11412,.T.);
#15843=ORIENTED_EDGE('',*,*,#11413,.T.);
#15844=ORIENTED_EDGE('',*,*,#11414,.T.);
#15845=ORIENTED_EDGE('',*,*,#11415,.T.);
#15846=ORIENTED_EDGE('',*,*,#11416,.T.);
#15847=ORIENTED_EDGE('',*,*,#11417,.T.);
#15848=ORIENTED_EDGE('',*,*,#11418,.T.);
#15849=ORIENTED_EDGE('',*,*,#11419,.T.);
#15850=ORIENTED_EDGE('',*,*,#11420,.T.);
#15851=ORIENTED_EDGE('',*,*,#11421,.T.);
#15852=ORIENTED_EDGE('',*,*,#11422,.T.);
#15853=ORIENTED_EDGE('',*,*,#11423,.T.);
#15854=ORIENTED_EDGE('',*,*,#11424,.T.);
#15855=ORIENTED_EDGE('',*,*,#11425,.T.);
#15856=ORIENTED_EDGE('',*,*,#11426,.T.);
#15857=ORIENTED_EDGE('',*,*,#11427,.T.);
#15858=ORIENTED_EDGE('',*,*,#11428,.T.);
#15859=ORIENTED_EDGE('',*,*,#11429,.T.);
#15860=ORIENTED_EDGE('',*,*,#11430,.T.);
#15861=ORIENTED_EDGE('',*,*,#11431,.T.);
#15862=ORIENTED_EDGE('',*,*,#11432,.T.);
#15863=ORIENTED_EDGE('',*,*,#11433,.T.);
#15864=ORIENTED_EDGE('',*,*,#11434,.T.);
#15865=ORIENTED_EDGE('',*,*,#11435,.T.);
#15866=ORIENTED_EDGE('',*,*,#11436,.F.);
#15867=ORIENTED_EDGE('',*,*,#11437,.F.);
#15868=ORIENTED_EDGE('',*,*,#11438,.T.);
#15869=ORIENTED_EDGE('',*,*,#11433,.F.);
#15870=ORIENTED_EDGE('',*,*,#11439,.F.);
#15871=ORIENTED_EDGE('',*,*,#11435,.F.);
#15872=ORIENTED_EDGE('',*,*,#11440,.F.);
#15873=ORIENTED_EDGE('',*,*,#11441,.F.);
#15874=ORIENTED_EDGE('',*,*,#11442,.F.);
#15875=ORIENTED_EDGE('',*,*,#11440,.T.);
#15876=ORIENTED_EDGE('',*,*,#11434,.F.);
#15877=ORIENTED_EDGE('',*,*,#11438,.F.);
#15878=ORIENTED_EDGE('',*,*,#11439,.T.);
#15879=ORIENTED_EDGE('',*,*,#11443,.F.);
#15880=ORIENTED_EDGE('',*,*,#11444,.T.);
#15881=ORIENTED_EDGE('',*,*,#11380,.F.);
#15882=ORIENTED_EDGE('',*,*,#11444,.F.);
#15883=ORIENTED_EDGE('',*,*,#11445,.F.);
#15884=ORIENTED_EDGE('',*,*,#11446,.T.);
#15885=ORIENTED_EDGE('',*,*,#11381,.F.);
#15886=ORIENTED_EDGE('',*,*,#11447,.F.);
#15887=ORIENTED_EDGE('',*,*,#11383,.F.);
#15888=ORIENTED_EDGE('',*,*,#11448,.F.);
#15889=ORIENTED_EDGE('',*,*,#11449,.F.);
#15890=ORIENTED_EDGE('',*,*,#11450,.F.);
#15891=ORIENTED_EDGE('',*,*,#11448,.T.);
#15892=ORIENTED_EDGE('',*,*,#11382,.F.);
#15893=ORIENTED_EDGE('',*,*,#11446,.F.);
#15894=ORIENTED_EDGE('',*,*,#11447,.T.);
#15895=ORIENTED_EDGE('',*,*,#11451,.F.);
#15896=ORIENTED_EDGE('',*,*,#11452,.T.);
#15897=ORIENTED_EDGE('',*,*,#11384,.F.);
#15898=ORIENTED_EDGE('',*,*,#11452,.F.);
#15899=ORIENTED_EDGE('',*,*,#11453,.F.);
#15900=ORIENTED_EDGE('',*,*,#11454,.T.);
#15901=ORIENTED_EDGE('',*,*,#11385,.F.);
#15902=ORIENTED_EDGE('',*,*,#11455,.F.);
#15903=ORIENTED_EDGE('',*,*,#11387,.F.);
#15904=ORIENTED_EDGE('',*,*,#11456,.F.);
#15905=ORIENTED_EDGE('',*,*,#11457,.F.);
#15906=ORIENTED_EDGE('',*,*,#11458,.F.);
#15907=ORIENTED_EDGE('',*,*,#11456,.T.);
#15908=ORIENTED_EDGE('',*,*,#11386,.F.);
#15909=ORIENTED_EDGE('',*,*,#11454,.F.);
#15910=ORIENTED_EDGE('',*,*,#11455,.T.);
#15911=ORIENTED_EDGE('',*,*,#11459,.F.);
#15912=ORIENTED_EDGE('',*,*,#11460,.T.);
#15913=ORIENTED_EDGE('',*,*,#11388,.F.);
#15914=ORIENTED_EDGE('',*,*,#11460,.F.);
#15915=ORIENTED_EDGE('',*,*,#11461,.F.);
#15916=ORIENTED_EDGE('',*,*,#11462,.T.);
#15917=ORIENTED_EDGE('',*,*,#11389,.F.);
#15918=ORIENTED_EDGE('',*,*,#11463,.F.);
#15919=ORIENTED_EDGE('',*,*,#11391,.F.);
#15920=ORIENTED_EDGE('',*,*,#11464,.F.);
#15921=ORIENTED_EDGE('',*,*,#11465,.F.);
#15922=ORIENTED_EDGE('',*,*,#11466,.F.);
#15923=ORIENTED_EDGE('',*,*,#11464,.T.);
#15924=ORIENTED_EDGE('',*,*,#11390,.F.);
#15925=ORIENTED_EDGE('',*,*,#11462,.F.);
#15926=ORIENTED_EDGE('',*,*,#11463,.T.);
#15927=ORIENTED_EDGE('',*,*,#11467,.F.);
#15928=ORIENTED_EDGE('',*,*,#11468,.T.);
#15929=ORIENTED_EDGE('',*,*,#11392,.F.);
#15930=ORIENTED_EDGE('',*,*,#11468,.F.);
#15931=ORIENTED_EDGE('',*,*,#11469,.F.);
#15932=ORIENTED_EDGE('',*,*,#11470,.T.);
#15933=ORIENTED_EDGE('',*,*,#11393,.F.);
#15934=ORIENTED_EDGE('',*,*,#11471,.F.);
#15935=ORIENTED_EDGE('',*,*,#11395,.F.);
#15936=ORIENTED_EDGE('',*,*,#11472,.F.);
#15937=ORIENTED_EDGE('',*,*,#11473,.F.);
#15938=ORIENTED_EDGE('',*,*,#11474,.F.);
#15939=ORIENTED_EDGE('',*,*,#11472,.T.);
#15940=ORIENTED_EDGE('',*,*,#11394,.F.);
#15941=ORIENTED_EDGE('',*,*,#11470,.F.);
#15942=ORIENTED_EDGE('',*,*,#11471,.T.);
#15943=ORIENTED_EDGE('',*,*,#11475,.F.);
#15944=ORIENTED_EDGE('',*,*,#11476,.T.);
#15945=ORIENTED_EDGE('',*,*,#11396,.F.);
#15946=ORIENTED_EDGE('',*,*,#11476,.F.);
#15947=ORIENTED_EDGE('',*,*,#11477,.F.);
#15948=ORIENTED_EDGE('',*,*,#11478,.T.);
#15949=ORIENTED_EDGE('',*,*,#11397,.F.);
#15950=ORIENTED_EDGE('',*,*,#11479,.F.);
#15951=ORIENTED_EDGE('',*,*,#11399,.F.);
#15952=ORIENTED_EDGE('',*,*,#11480,.F.);
#15953=ORIENTED_EDGE('',*,*,#11481,.F.);
#15954=ORIENTED_EDGE('',*,*,#11482,.F.);
#15955=ORIENTED_EDGE('',*,*,#11480,.T.);
#15956=ORIENTED_EDGE('',*,*,#11398,.F.);
#15957=ORIENTED_EDGE('',*,*,#11478,.F.);
#15958=ORIENTED_EDGE('',*,*,#11479,.T.);
#15959=ORIENTED_EDGE('',*,*,#11483,.F.);
#15960=ORIENTED_EDGE('',*,*,#11484,.T.);
#15961=ORIENTED_EDGE('',*,*,#11400,.F.);
#15962=ORIENTED_EDGE('',*,*,#11484,.F.);
#15963=ORIENTED_EDGE('',*,*,#11485,.F.);
#15964=ORIENTED_EDGE('',*,*,#11486,.T.);
#15965=ORIENTED_EDGE('',*,*,#11401,.F.);
#15966=ORIENTED_EDGE('',*,*,#11487,.F.);
#15967=ORIENTED_EDGE('',*,*,#11403,.F.);
#15968=ORIENTED_EDGE('',*,*,#11488,.F.);
#15969=ORIENTED_EDGE('',*,*,#11489,.F.);
#15970=ORIENTED_EDGE('',*,*,#11490,.F.);
#15971=ORIENTED_EDGE('',*,*,#11488,.T.);
#15972=ORIENTED_EDGE('',*,*,#11402,.F.);
#15973=ORIENTED_EDGE('',*,*,#11486,.F.);
#15974=ORIENTED_EDGE('',*,*,#11487,.T.);
#15975=ORIENTED_EDGE('',*,*,#11491,.F.);
#15976=ORIENTED_EDGE('',*,*,#11492,.T.);
#15977=ORIENTED_EDGE('',*,*,#11404,.F.);
#15978=ORIENTED_EDGE('',*,*,#11492,.F.);
#15979=ORIENTED_EDGE('',*,*,#11493,.F.);
#15980=ORIENTED_EDGE('',*,*,#11494,.T.);
#15981=ORIENTED_EDGE('',*,*,#11405,.F.);
#15982=ORIENTED_EDGE('',*,*,#11495,.F.);
#15983=ORIENTED_EDGE('',*,*,#11407,.F.);
#15984=ORIENTED_EDGE('',*,*,#11496,.F.);
#15985=ORIENTED_EDGE('',*,*,#11497,.F.);
#15986=ORIENTED_EDGE('',*,*,#11498,.F.);
#15987=ORIENTED_EDGE('',*,*,#11496,.T.);
#15988=ORIENTED_EDGE('',*,*,#11406,.F.);
#15989=ORIENTED_EDGE('',*,*,#11494,.F.);
#15990=ORIENTED_EDGE('',*,*,#11495,.T.);
#15991=ORIENTED_EDGE('',*,*,#11499,.F.);
#15992=ORIENTED_EDGE('',*,*,#11500,.T.);
#15993=ORIENTED_EDGE('',*,*,#11408,.F.);
#15994=ORIENTED_EDGE('',*,*,#11500,.F.);
#15995=ORIENTED_EDGE('',*,*,#11501,.F.);
#15996=ORIENTED_EDGE('',*,*,#11502,.T.);
#15997=ORIENTED_EDGE('',*,*,#11409,.F.);
#15998=ORIENTED_EDGE('',*,*,#11503,.F.);
#15999=ORIENTED_EDGE('',*,*,#11411,.F.);
#16000=ORIENTED_EDGE('',*,*,#11504,.F.);
#16001=ORIENTED_EDGE('',*,*,#11505,.F.);
#16002=ORIENTED_EDGE('',*,*,#11506,.F.);
#16003=ORIENTED_EDGE('',*,*,#11504,.T.);
#16004=ORIENTED_EDGE('',*,*,#11410,.F.);
#16005=ORIENTED_EDGE('',*,*,#11502,.F.);
#16006=ORIENTED_EDGE('',*,*,#11503,.T.);
#16007=ORIENTED_EDGE('',*,*,#11507,.F.);
#16008=ORIENTED_EDGE('',*,*,#11508,.T.);
#16009=ORIENTED_EDGE('',*,*,#11412,.F.);
#16010=ORIENTED_EDGE('',*,*,#11508,.F.);
#16011=ORIENTED_EDGE('',*,*,#11509,.F.);
#16012=ORIENTED_EDGE('',*,*,#11510,.T.);
#16013=ORIENTED_EDGE('',*,*,#11413,.F.);
#16014=ORIENTED_EDGE('',*,*,#11511,.F.);
#16015=ORIENTED_EDGE('',*,*,#11415,.F.);
#16016=ORIENTED_EDGE('',*,*,#11512,.F.);
#16017=ORIENTED_EDGE('',*,*,#11513,.F.);
#16018=ORIENTED_EDGE('',*,*,#11514,.F.);
#16019=ORIENTED_EDGE('',*,*,#11512,.T.);
#16020=ORIENTED_EDGE('',*,*,#11414,.F.);
#16021=ORIENTED_EDGE('',*,*,#11510,.F.);
#16022=ORIENTED_EDGE('',*,*,#11511,.T.);
#16023=ORIENTED_EDGE('',*,*,#11515,.F.);
#16024=ORIENTED_EDGE('',*,*,#11516,.T.);
#16025=ORIENTED_EDGE('',*,*,#11416,.F.);
#16026=ORIENTED_EDGE('',*,*,#11516,.F.);
#16027=ORIENTED_EDGE('',*,*,#11517,.F.);
#16028=ORIENTED_EDGE('',*,*,#11518,.T.);
#16029=ORIENTED_EDGE('',*,*,#11417,.F.);
#16030=ORIENTED_EDGE('',*,*,#11519,.F.);
#16031=ORIENTED_EDGE('',*,*,#11419,.F.);
#16032=ORIENTED_EDGE('',*,*,#11520,.F.);
#16033=ORIENTED_EDGE('',*,*,#11521,.F.);
#16034=ORIENTED_EDGE('',*,*,#11522,.F.);
#16035=ORIENTED_EDGE('',*,*,#11520,.T.);
#16036=ORIENTED_EDGE('',*,*,#11418,.F.);
#16037=ORIENTED_EDGE('',*,*,#11518,.F.);
#16038=ORIENTED_EDGE('',*,*,#11519,.T.);
#16039=ORIENTED_EDGE('',*,*,#11523,.F.);
#16040=ORIENTED_EDGE('',*,*,#11524,.T.);
#16041=ORIENTED_EDGE('',*,*,#11420,.F.);
#16042=ORIENTED_EDGE('',*,*,#11524,.F.);
#16043=ORIENTED_EDGE('',*,*,#11525,.F.);
#16044=ORIENTED_EDGE('',*,*,#11526,.T.);
#16045=ORIENTED_EDGE('',*,*,#11421,.F.);
#16046=ORIENTED_EDGE('',*,*,#11527,.F.);
#16047=ORIENTED_EDGE('',*,*,#11423,.F.);
#16048=ORIENTED_EDGE('',*,*,#11528,.F.);
#16049=ORIENTED_EDGE('',*,*,#11529,.F.);
#16050=ORIENTED_EDGE('',*,*,#11530,.F.);
#16051=ORIENTED_EDGE('',*,*,#11528,.T.);
#16052=ORIENTED_EDGE('',*,*,#11422,.F.);
#16053=ORIENTED_EDGE('',*,*,#11526,.F.);
#16054=ORIENTED_EDGE('',*,*,#11527,.T.);
#16055=ORIENTED_EDGE('',*,*,#11531,.F.);
#16056=ORIENTED_EDGE('',*,*,#11532,.T.);
#16057=ORIENTED_EDGE('',*,*,#11424,.F.);
#16058=ORIENTED_EDGE('',*,*,#11532,.F.);
#16059=ORIENTED_EDGE('',*,*,#11533,.F.);
#16060=ORIENTED_EDGE('',*,*,#11534,.T.);
#16061=ORIENTED_EDGE('',*,*,#11425,.F.);
#16062=ORIENTED_EDGE('',*,*,#11535,.F.);
#16063=ORIENTED_EDGE('',*,*,#11427,.F.);
#16064=ORIENTED_EDGE('',*,*,#11536,.F.);
#16065=ORIENTED_EDGE('',*,*,#11537,.F.);
#16066=ORIENTED_EDGE('',*,*,#11538,.F.);
#16067=ORIENTED_EDGE('',*,*,#11536,.T.);
#16068=ORIENTED_EDGE('',*,*,#11426,.F.);
#16069=ORIENTED_EDGE('',*,*,#11534,.F.);
#16070=ORIENTED_EDGE('',*,*,#11535,.T.);
#16071=ORIENTED_EDGE('',*,*,#11539,.F.);
#16072=ORIENTED_EDGE('',*,*,#11540,.T.);
#16073=ORIENTED_EDGE('',*,*,#11428,.F.);
#16074=ORIENTED_EDGE('',*,*,#11541,.F.);
#16075=ORIENTED_EDGE('',*,*,#11431,.F.);
#16076=ORIENTED_EDGE('',*,*,#11542,.F.);
#16077=ORIENTED_EDGE('',*,*,#11543,.F.);
#16078=ORIENTED_EDGE('',*,*,#11540,.F.);
#16079=ORIENTED_EDGE('',*,*,#11544,.F.);
#16080=ORIENTED_EDGE('',*,*,#11545,.T.);
#16081=ORIENTED_EDGE('',*,*,#11429,.F.);
#16082=ORIENTED_EDGE('',*,*,#11546,.F.);
#16083=ORIENTED_EDGE('',*,*,#11542,.T.);
#16084=ORIENTED_EDGE('',*,*,#11430,.F.);
#16085=ORIENTED_EDGE('',*,*,#11545,.F.);
#16086=ORIENTED_EDGE('',*,*,#11437,.T.);
#16087=ORIENTED_EDGE('',*,*,#11547,.T.);
#16088=ORIENTED_EDGE('',*,*,#11543,.T.);
#16089=ORIENTED_EDGE('',*,*,#11546,.T.);
#16090=ORIENTED_EDGE('',*,*,#11544,.T.);
#16091=ORIENTED_EDGE('',*,*,#11539,.T.);
#16092=ORIENTED_EDGE('',*,*,#11537,.T.);
#16093=ORIENTED_EDGE('',*,*,#11538,.T.);
#16094=ORIENTED_EDGE('',*,*,#11533,.T.);
#16095=ORIENTED_EDGE('',*,*,#11531,.T.);
#16096=ORIENTED_EDGE('',*,*,#11529,.T.);
#16097=ORIENTED_EDGE('',*,*,#11530,.T.);
#16098=ORIENTED_EDGE('',*,*,#11525,.T.);
#16099=ORIENTED_EDGE('',*,*,#11523,.T.);
#16100=ORIENTED_EDGE('',*,*,#11521,.T.);
#16101=ORIENTED_EDGE('',*,*,#11522,.T.);
#16102=ORIENTED_EDGE('',*,*,#11517,.T.);
#16103=ORIENTED_EDGE('',*,*,#11515,.T.);
#16104=ORIENTED_EDGE('',*,*,#11513,.T.);
#16105=ORIENTED_EDGE('',*,*,#11514,.T.);
#16106=ORIENTED_EDGE('',*,*,#11509,.T.);
#16107=ORIENTED_EDGE('',*,*,#11507,.T.);
#16108=ORIENTED_EDGE('',*,*,#11505,.T.);
#16109=ORIENTED_EDGE('',*,*,#11506,.T.);
#16110=ORIENTED_EDGE('',*,*,#11501,.T.);
#16111=ORIENTED_EDGE('',*,*,#11499,.T.);
#16112=ORIENTED_EDGE('',*,*,#11497,.T.);
#16113=ORIENTED_EDGE('',*,*,#11498,.T.);
#16114=ORIENTED_EDGE('',*,*,#11493,.T.);
#16115=ORIENTED_EDGE('',*,*,#11491,.T.);
#16116=ORIENTED_EDGE('',*,*,#11489,.T.);
#16117=ORIENTED_EDGE('',*,*,#11490,.T.);
#16118=ORIENTED_EDGE('',*,*,#11485,.T.);
#16119=ORIENTED_EDGE('',*,*,#11483,.T.);
#16120=ORIENTED_EDGE('',*,*,#11481,.T.);
#16121=ORIENTED_EDGE('',*,*,#11482,.T.);
#16122=ORIENTED_EDGE('',*,*,#11477,.T.);
#16123=ORIENTED_EDGE('',*,*,#11475,.T.);
#16124=ORIENTED_EDGE('',*,*,#11473,.T.);
#16125=ORIENTED_EDGE('',*,*,#11474,.T.);
#16126=ORIENTED_EDGE('',*,*,#11469,.T.);
#16127=ORIENTED_EDGE('',*,*,#11467,.T.);
#16128=ORIENTED_EDGE('',*,*,#11465,.T.);
#16129=ORIENTED_EDGE('',*,*,#11466,.T.);
#16130=ORIENTED_EDGE('',*,*,#11461,.T.);
#16131=ORIENTED_EDGE('',*,*,#11459,.T.);
#16132=ORIENTED_EDGE('',*,*,#11457,.T.);
#16133=ORIENTED_EDGE('',*,*,#11458,.T.);
#16134=ORIENTED_EDGE('',*,*,#11453,.T.);
#16135=ORIENTED_EDGE('',*,*,#11451,.T.);
#16136=ORIENTED_EDGE('',*,*,#11449,.T.);
#16137=ORIENTED_EDGE('',*,*,#11450,.T.);
#16138=ORIENTED_EDGE('',*,*,#11445,.T.);
#16139=ORIENTED_EDGE('',*,*,#11443,.T.);
#16140=ORIENTED_EDGE('',*,*,#11441,.T.);
#16141=ORIENTED_EDGE('',*,*,#11442,.T.);
#16142=ORIENTED_EDGE('',*,*,#11548,.F.);
#16143=ORIENTED_EDGE('',*,*,#11436,.T.);
#16144=ORIENTED_EDGE('',*,*,#11432,.F.);
#16145=ORIENTED_EDGE('',*,*,#11541,.T.);
#16146=ORIENTED_EDGE('',*,*,#11547,.F.);
#16147=ORIENTED_EDGE('',*,*,#11377,.F.);
#16148=ORIENTED_EDGE('',*,*,#11549,.T.);
#16149=ORIENTED_EDGE('',*,*,#11548,.T.);
#16150=ORIENTED_EDGE('',*,*,#11549,.F.);
#16151=ORIENTED_EDGE('',*,*,#11550,.F.);
#16152=ORIENTED_EDGE('',*,*,#11551,.F.);
#16153=ORIENTED_EDGE('',*,*,#11552,.F.);
#16154=ORIENTED_EDGE('',*,*,#11553,.T.);
#16155=ORIENTED_EDGE('',*,*,#11554,.F.);
#16156=ORIENTED_EDGE('',*,*,#11555,.F.);
#16157=ORIENTED_EDGE('',*,*,#11556,.F.);
#16158=ORIENTED_EDGE('',*,*,#11550,.T.);
#16159=ORIENTED_EDGE('',*,*,#11557,.T.);
#16160=ORIENTED_EDGE('',*,*,#11558,.T.);
#16161=ORIENTED_EDGE('',*,*,#11559,.F.);
#16162=ORIENTED_EDGE('',*,*,#11560,.F.);
#16163=ORIENTED_EDGE('',*,*,#11561,.F.);
#16164=ORIENTED_EDGE('',*,*,#11554,.T.);
#16165=ORIENTED_EDGE('',*,*,#11562,.T.);
#16166=ORIENTED_EDGE('',*,*,#11563,.T.);
#16167=ORIENTED_EDGE('',*,*,#11564,.F.);
#16168=ORIENTED_EDGE('',*,*,#11565,.F.);
#16169=ORIENTED_EDGE('',*,*,#11566,.F.);
#16170=ORIENTED_EDGE('',*,*,#11559,.T.);
#16171=ORIENTED_EDGE('',*,*,#11567,.T.);
#16172=ORIENTED_EDGE('',*,*,#11568,.T.);
#16173=ORIENTED_EDGE('',*,*,#11569,.F.);
#16174=ORIENTED_EDGE('',*,*,#11570,.F.);
#16175=ORIENTED_EDGE('',*,*,#11571,.F.);
#16176=ORIENTED_EDGE('',*,*,#11564,.T.);
#16177=ORIENTED_EDGE('',*,*,#11572,.T.);
#16178=ORIENTED_EDGE('',*,*,#11573,.F.);
#16179=ORIENTED_EDGE('',*,*,#11574,.F.);
#16180=ORIENTED_EDGE('',*,*,#11575,.F.);
#16181=ORIENTED_EDGE('',*,*,#11569,.T.);
#16182=ORIENTED_EDGE('',*,*,#11576,.T.);
#16183=ORIENTED_EDGE('',*,*,#11577,.T.);
#16184=ORIENTED_EDGE('',*,*,#11578,.F.);
#16185=ORIENTED_EDGE('',*,*,#11579,.F.);
#16186=ORIENTED_EDGE('',*,*,#11580,.F.);
#16187=ORIENTED_EDGE('',*,*,#11573,.T.);
#16188=ORIENTED_EDGE('',*,*,#11581,.T.);
#16189=ORIENTED_EDGE('',*,*,#11582,.F.);
#16190=ORIENTED_EDGE('',*,*,#11583,.F.);
#16191=ORIENTED_EDGE('',*,*,#11584,.F.);
#16192=ORIENTED_EDGE('',*,*,#11578,.T.);
#16193=ORIENTED_EDGE('',*,*,#11585,.T.);
#16194=ORIENTED_EDGE('',*,*,#11586,.T.);
#16195=ORIENTED_EDGE('',*,*,#11587,.F.);
#16196=ORIENTED_EDGE('',*,*,#11588,.F.);
#16197=ORIENTED_EDGE('',*,*,#11589,.F.);
#16198=ORIENTED_EDGE('',*,*,#11582,.T.);
#16199=ORIENTED_EDGE('',*,*,#11590,.T.);
#16200=ORIENTED_EDGE('',*,*,#11591,.F.);
#16201=ORIENTED_EDGE('',*,*,#11592,.F.);
#16202=ORIENTED_EDGE('',*,*,#11593,.F.);
#16203=ORIENTED_EDGE('',*,*,#11587,.T.);
#16204=ORIENTED_EDGE('',*,*,#11594,.T.);
#16205=ORIENTED_EDGE('',*,*,#11595,.T.);
#16206=ORIENTED_EDGE('',*,*,#11596,.F.);
#16207=ORIENTED_EDGE('',*,*,#11597,.F.);
#16208=ORIENTED_EDGE('',*,*,#11598,.F.);
#16209=ORIENTED_EDGE('',*,*,#11591,.T.);
#16210=ORIENTED_EDGE('',*,*,#11599,.T.);
#16211=ORIENTED_EDGE('',*,*,#11600,.F.);
#16212=ORIENTED_EDGE('',*,*,#11601,.F.);
#16213=ORIENTED_EDGE('',*,*,#11602,.F.);
#16214=ORIENTED_EDGE('',*,*,#11596,.T.);
#16215=ORIENTED_EDGE('',*,*,#11603,.T.);
#16216=ORIENTED_EDGE('',*,*,#11604,.T.);
#16217=ORIENTED_EDGE('',*,*,#11605,.F.);
#16218=ORIENTED_EDGE('',*,*,#11606,.F.);
#16219=ORIENTED_EDGE('',*,*,#11607,.F.);
#16220=ORIENTED_EDGE('',*,*,#11600,.T.);
#16221=ORIENTED_EDGE('',*,*,#11608,.T.);
#16222=ORIENTED_EDGE('',*,*,#11609,.F.);
#16223=ORIENTED_EDGE('',*,*,#11610,.F.);
#16224=ORIENTED_EDGE('',*,*,#11611,.F.);
#16225=ORIENTED_EDGE('',*,*,#11605,.T.);
#16226=ORIENTED_EDGE('',*,*,#11612,.T.);
#16227=ORIENTED_EDGE('',*,*,#11613,.T.);
#16228=ORIENTED_EDGE('',*,*,#11614,.F.);
#16229=ORIENTED_EDGE('',*,*,#11615,.F.);
#16230=ORIENTED_EDGE('',*,*,#11616,.F.);
#16231=ORIENTED_EDGE('',*,*,#11609,.T.);
#16232=ORIENTED_EDGE('',*,*,#11617,.T.);
#16233=ORIENTED_EDGE('',*,*,#11618,.F.);
#16234=ORIENTED_EDGE('',*,*,#11619,.F.);
#16235=ORIENTED_EDGE('',*,*,#11620,.F.);
#16236=ORIENTED_EDGE('',*,*,#11614,.T.);
#16237=ORIENTED_EDGE('',*,*,#11621,.T.);
#16238=ORIENTED_EDGE('',*,*,#11622,.T.);
#16239=ORIENTED_EDGE('',*,*,#11623,.F.);
#16240=ORIENTED_EDGE('',*,*,#11624,.F.);
#16241=ORIENTED_EDGE('',*,*,#11625,.F.);
#16242=ORIENTED_EDGE('',*,*,#11618,.T.);
#16243=ORIENTED_EDGE('',*,*,#11626,.T.);
#16244=ORIENTED_EDGE('',*,*,#11627,.F.);
#16245=ORIENTED_EDGE('',*,*,#11628,.F.);
#16246=ORIENTED_EDGE('',*,*,#11629,.F.);
#16247=ORIENTED_EDGE('',*,*,#11623,.T.);
#16248=ORIENTED_EDGE('',*,*,#11630,.T.);
#16249=ORIENTED_EDGE('',*,*,#11631,.T.);
#16250=ORIENTED_EDGE('',*,*,#11632,.F.);
#16251=ORIENTED_EDGE('',*,*,#11633,.F.);
#16252=ORIENTED_EDGE('',*,*,#11634,.F.);
#16253=ORIENTED_EDGE('',*,*,#11627,.T.);
#16254=ORIENTED_EDGE('',*,*,#11635,.T.);
#16255=ORIENTED_EDGE('',*,*,#11636,.F.);
#16256=ORIENTED_EDGE('',*,*,#11637,.F.);
#16257=ORIENTED_EDGE('',*,*,#11638,.F.);
#16258=ORIENTED_EDGE('',*,*,#11632,.T.);
#16259=ORIENTED_EDGE('',*,*,#11639,.T.);
#16260=ORIENTED_EDGE('',*,*,#11640,.T.);
#16261=ORIENTED_EDGE('',*,*,#11641,.F.);
#16262=ORIENTED_EDGE('',*,*,#11642,.F.);
#16263=ORIENTED_EDGE('',*,*,#11643,.F.);
#16264=ORIENTED_EDGE('',*,*,#11636,.T.);
#16265=ORIENTED_EDGE('',*,*,#11644,.T.);
#16266=ORIENTED_EDGE('',*,*,#11645,.F.);
#16267=ORIENTED_EDGE('',*,*,#11646,.F.);
#16268=ORIENTED_EDGE('',*,*,#11647,.F.);
#16269=ORIENTED_EDGE('',*,*,#11641,.T.);
#16270=ORIENTED_EDGE('',*,*,#11648,.T.);
#16271=ORIENTED_EDGE('',*,*,#11649,.T.);
#16272=ORIENTED_EDGE('',*,*,#11650,.F.);
#16273=ORIENTED_EDGE('',*,*,#11651,.F.);
#16274=ORIENTED_EDGE('',*,*,#11652,.F.);
#16275=ORIENTED_EDGE('',*,*,#11645,.T.);
#16276=ORIENTED_EDGE('',*,*,#11653,.T.);
#16277=ORIENTED_EDGE('',*,*,#11654,.F.);
#16278=ORIENTED_EDGE('',*,*,#11655,.F.);
#16279=ORIENTED_EDGE('',*,*,#11656,.F.);
#16280=ORIENTED_EDGE('',*,*,#11650,.T.);
#16281=ORIENTED_EDGE('',*,*,#11657,.T.);
#16282=ORIENTED_EDGE('',*,*,#11658,.T.);
#16283=ORIENTED_EDGE('',*,*,#11659,.F.);
#16284=ORIENTED_EDGE('',*,*,#11660,.F.);
#16285=ORIENTED_EDGE('',*,*,#11661,.F.);
#16286=ORIENTED_EDGE('',*,*,#11654,.T.);
#16287=ORIENTED_EDGE('',*,*,#11662,.T.);
#16288=ORIENTED_EDGE('',*,*,#11663,.T.);
#16289=ORIENTED_EDGE('',*,*,#11664,.F.);
#16290=ORIENTED_EDGE('',*,*,#11665,.F.);
#16291=ORIENTED_EDGE('',*,*,#11666,.F.);
#16292=ORIENTED_EDGE('',*,*,#11659,.T.);
#16293=ORIENTED_EDGE('',*,*,#11667,.T.);
#16294=ORIENTED_EDGE('',*,*,#11668,.F.);
#16295=ORIENTED_EDGE('',*,*,#11669,.F.);
#16296=ORIENTED_EDGE('',*,*,#11670,.F.);
#16297=ORIENTED_EDGE('',*,*,#11664,.T.);
#16298=ORIENTED_EDGE('',*,*,#11671,.T.);
#16299=ORIENTED_EDGE('',*,*,#11672,.T.);
#16300=ORIENTED_EDGE('',*,*,#11673,.F.);
#16301=ORIENTED_EDGE('',*,*,#11674,.F.);
#16302=ORIENTED_EDGE('',*,*,#11675,.F.);
#16303=ORIENTED_EDGE('',*,*,#11668,.T.);
#16304=ORIENTED_EDGE('',*,*,#11676,.T.);
#16305=ORIENTED_EDGE('',*,*,#11677,.F.);
#16306=ORIENTED_EDGE('',*,*,#11678,.F.);
#16307=ORIENTED_EDGE('',*,*,#11679,.F.);
#16308=ORIENTED_EDGE('',*,*,#11673,.T.);
#16309=ORIENTED_EDGE('',*,*,#11680,.T.);
#16310=ORIENTED_EDGE('',*,*,#11681,.T.);
#16311=ORIENTED_EDGE('',*,*,#11682,.F.);
#16312=ORIENTED_EDGE('',*,*,#11683,.F.);
#16313=ORIENTED_EDGE('',*,*,#11684,.F.);
#16314=ORIENTED_EDGE('',*,*,#11677,.T.);
#16315=ORIENTED_EDGE('',*,*,#11685,.T.);
#16316=ORIENTED_EDGE('',*,*,#11686,.F.);
#16317=ORIENTED_EDGE('',*,*,#11687,.F.);
#16318=ORIENTED_EDGE('',*,*,#11688,.F.);
#16319=ORIENTED_EDGE('',*,*,#11682,.T.);
#16320=ORIENTED_EDGE('',*,*,#11689,.T.);
#16321=ORIENTED_EDGE('',*,*,#11690,.T.);
#16322=ORIENTED_EDGE('',*,*,#11691,.F.);
#16323=ORIENTED_EDGE('',*,*,#11692,.F.);
#16324=ORIENTED_EDGE('',*,*,#11693,.F.);
#16325=ORIENTED_EDGE('',*,*,#11686,.T.);
#16326=ORIENTED_EDGE('',*,*,#11694,.T.);
#16327=ORIENTED_EDGE('',*,*,#11695,.T.);
#16328=ORIENTED_EDGE('',*,*,#11696,.F.);
#16329=ORIENTED_EDGE('',*,*,#11697,.F.);
#16330=ORIENTED_EDGE('',*,*,#11698,.F.);
#16331=ORIENTED_EDGE('',*,*,#11691,.T.);
#16332=ORIENTED_EDGE('',*,*,#11699,.T.);
#16333=ORIENTED_EDGE('',*,*,#11700,.F.);
#16334=ORIENTED_EDGE('',*,*,#11701,.F.);
#16335=ORIENTED_EDGE('',*,*,#11702,.F.);
#16336=ORIENTED_EDGE('',*,*,#11696,.T.);
#16337=ORIENTED_EDGE('',*,*,#11703,.T.);
#16338=ORIENTED_EDGE('',*,*,#11704,.T.);
#16339=ORIENTED_EDGE('',*,*,#11705,.F.);
#16340=ORIENTED_EDGE('',*,*,#11706,.F.);
#16341=ORIENTED_EDGE('',*,*,#11707,.F.);
#16342=ORIENTED_EDGE('',*,*,#11700,.T.);
#16343=ORIENTED_EDGE('',*,*,#11708,.T.);
#16344=ORIENTED_EDGE('',*,*,#11709,.F.);
#16345=ORIENTED_EDGE('',*,*,#11710,.F.);
#16346=ORIENTED_EDGE('',*,*,#11711,.F.);
#16347=ORIENTED_EDGE('',*,*,#11705,.T.);
#16348=ORIENTED_EDGE('',*,*,#11712,.T.);
#16349=ORIENTED_EDGE('',*,*,#11713,.T.);
#16350=ORIENTED_EDGE('',*,*,#11714,.F.);
#16351=ORIENTED_EDGE('',*,*,#11715,.F.);
#16352=ORIENTED_EDGE('',*,*,#11716,.F.);
#16353=ORIENTED_EDGE('',*,*,#11709,.T.);
#16354=ORIENTED_EDGE('',*,*,#11717,.T.);
#16355=ORIENTED_EDGE('',*,*,#11718,.T.);
#16356=ORIENTED_EDGE('',*,*,#11719,.F.);
#16357=ORIENTED_EDGE('',*,*,#11720,.F.);
#16358=ORIENTED_EDGE('',*,*,#11721,.F.);
#16359=ORIENTED_EDGE('',*,*,#11714,.T.);
#16360=ORIENTED_EDGE('',*,*,#11722,.T.);
#16361=ORIENTED_EDGE('',*,*,#11723,.T.);
#16362=ORIENTED_EDGE('',*,*,#11724,.F.);
#16363=ORIENTED_EDGE('',*,*,#11725,.F.);
#16364=ORIENTED_EDGE('',*,*,#11726,.F.);
#16365=ORIENTED_EDGE('',*,*,#11719,.T.);
#16366=ORIENTED_EDGE('',*,*,#11727,.T.);
#16367=ORIENTED_EDGE('',*,*,#11728,.T.);
#16368=ORIENTED_EDGE('',*,*,#11729,.T.);
#16369=ORIENTED_EDGE('',*,*,#11730,.T.);
#16370=ORIENTED_EDGE('',*,*,#11731,.T.);
#16371=ORIENTED_EDGE('',*,*,#11732,.T.);
#16372=ORIENTED_EDGE('',*,*,#11733,.T.);
#16373=ORIENTED_EDGE('',*,*,#11734,.T.);
#16374=ORIENTED_EDGE('',*,*,#11735,.T.);
#16375=ORIENTED_EDGE('',*,*,#11736,.T.);
#16376=ORIENTED_EDGE('',*,*,#11737,.T.);
#16377=ORIENTED_EDGE('',*,*,#11738,.T.);
#16378=ORIENTED_EDGE('',*,*,#11739,.T.);
#16379=ORIENTED_EDGE('',*,*,#11740,.T.);
#16380=ORIENTED_EDGE('',*,*,#11741,.T.);
#16381=ORIENTED_EDGE('',*,*,#11742,.T.);
#16382=ORIENTED_EDGE('',*,*,#11743,.T.);
#16383=ORIENTED_EDGE('',*,*,#11744,.T.);
#16384=ORIENTED_EDGE('',*,*,#11745,.T.);
#16385=ORIENTED_EDGE('',*,*,#11746,.T.);
#16386=ORIENTED_EDGE('',*,*,#11747,.T.);
#16387=ORIENTED_EDGE('',*,*,#11748,.T.);
#16388=ORIENTED_EDGE('',*,*,#11749,.T.);
#16389=ORIENTED_EDGE('',*,*,#11750,.T.);
#16390=ORIENTED_EDGE('',*,*,#11751,.T.);
#16391=ORIENTED_EDGE('',*,*,#11752,.T.);
#16392=ORIENTED_EDGE('',*,*,#11753,.T.);
#16393=ORIENTED_EDGE('',*,*,#11754,.T.);
#16394=ORIENTED_EDGE('',*,*,#11755,.T.);
#16395=ORIENTED_EDGE('',*,*,#11756,.T.);
#16396=ORIENTED_EDGE('',*,*,#11757,.T.);
#16397=ORIENTED_EDGE('',*,*,#11758,.T.);
#16398=ORIENTED_EDGE('',*,*,#11759,.T.);
#16399=ORIENTED_EDGE('',*,*,#11760,.T.);
#16400=ORIENTED_EDGE('',*,*,#11761,.T.);
#16401=ORIENTED_EDGE('',*,*,#11762,.T.);
#16402=ORIENTED_EDGE('',*,*,#11763,.T.);
#16403=ORIENTED_EDGE('',*,*,#11764,.T.);
#16404=ORIENTED_EDGE('',*,*,#11765,.T.);
#16405=ORIENTED_EDGE('',*,*,#11766,.T.);
#16406=ORIENTED_EDGE('',*,*,#11767,.T.);
#16407=ORIENTED_EDGE('',*,*,#11768,.T.);
#16408=ORIENTED_EDGE('',*,*,#11769,.T.);
#16409=ORIENTED_EDGE('',*,*,#11770,.T.);
#16410=ORIENTED_EDGE('',*,*,#11771,.F.);
#16411=ORIENTED_EDGE('',*,*,#11772,.T.);
#16412=ORIENTED_EDGE('',*,*,#11773,.T.);
#16413=ORIENTED_EDGE('',*,*,#11774,.T.);
#16414=ORIENTED_EDGE('',*,*,#11775,.T.);
#16415=ORIENTED_EDGE('',*,*,#11776,.T.);
#16416=ORIENTED_EDGE('',*,*,#11777,.T.);
#16417=ORIENTED_EDGE('',*,*,#11778,.T.);
#16418=ORIENTED_EDGE('',*,*,#11779,.T.);
#16419=ORIENTED_EDGE('',*,*,#11780,.T.);
#16420=ORIENTED_EDGE('',*,*,#11781,.T.);
#16421=ORIENTED_EDGE('',*,*,#11782,.T.);
#16422=ORIENTED_EDGE('',*,*,#11783,.T.);
#16423=ORIENTED_EDGE('',*,*,#11784,.T.);
#16424=ORIENTED_EDGE('',*,*,#11785,.T.);
#16425=ORIENTED_EDGE('',*,*,#11786,.T.);
#16426=ORIENTED_EDGE('',*,*,#11787,.T.);
#16427=ORIENTED_EDGE('',*,*,#11788,.T.);
#16428=ORIENTED_EDGE('',*,*,#11789,.T.);
#16429=ORIENTED_EDGE('',*,*,#11790,.T.);
#16430=ORIENTED_EDGE('',*,*,#11791,.T.);
#16431=ORIENTED_EDGE('',*,*,#11792,.T.);
#16432=ORIENTED_EDGE('',*,*,#11793,.T.);
#16433=ORIENTED_EDGE('',*,*,#11794,.T.);
#16434=ORIENTED_EDGE('',*,*,#11795,.T.);
#16435=ORIENTED_EDGE('',*,*,#11796,.T.);
#16436=ORIENTED_EDGE('',*,*,#11797,.T.);
#16437=ORIENTED_EDGE('',*,*,#11798,.T.);
#16438=ORIENTED_EDGE('',*,*,#11799,.T.);
#16439=ORIENTED_EDGE('',*,*,#11800,.T.);
#16440=ORIENTED_EDGE('',*,*,#11801,.T.);
#16441=ORIENTED_EDGE('',*,*,#11802,.T.);
#16442=ORIENTED_EDGE('',*,*,#11803,.T.);
#16443=ORIENTED_EDGE('',*,*,#11804,.T.);
#16444=ORIENTED_EDGE('',*,*,#11805,.T.);
#16445=ORIENTED_EDGE('',*,*,#11806,.T.);
#16446=ORIENTED_EDGE('',*,*,#11807,.T.);
#16447=ORIENTED_EDGE('',*,*,#11808,.T.);
#16448=ORIENTED_EDGE('',*,*,#11809,.T.);
#16449=ORIENTED_EDGE('',*,*,#11810,.T.);
#16450=ORIENTED_EDGE('',*,*,#11724,.T.);
#16451=ORIENTED_EDGE('',*,*,#11811,.T.);
#16452=ORIENTED_EDGE('',*,*,#11812,.T.);
#16453=ORIENTED_EDGE('',*,*,#11813,.F.);
#16454=ORIENTED_EDGE('',*,*,#11814,.F.);
#16455=ORIENTED_EDGE('',*,*,#11815,.F.);
#16456=ORIENTED_EDGE('',*,*,#11816,.F.);
#16457=ORIENTED_EDGE('',*,*,#11817,.T.);
#16458=ORIENTED_EDGE('',*,*,#11818,.T.);
#16459=ORIENTED_EDGE('',*,*,#11817,.F.);
#16460=ORIENTED_EDGE('',*,*,#11818,.F.);
#16461=ORIENTED_EDGE('',*,*,#11819,.F.);
#16462=ORIENTED_EDGE('',*,*,#11820,.T.);
#16463=ORIENTED_EDGE('',*,*,#11813,.T.);
#16464=ORIENTED_EDGE('',*,*,#11821,.T.);
#16465=ORIENTED_EDGE('',*,*,#11822,.F.);
#16466=ORIENTED_EDGE('',*,*,#11820,.F.);
#16467=ORIENTED_EDGE('',*,*,#11823,.F.);
#16468=ORIENTED_EDGE('',*,*,#11770,.F.);
#16469=ORIENTED_EDGE('',*,*,#11769,.F.);
#16470=ORIENTED_EDGE('',*,*,#11768,.F.);
#16471=ORIENTED_EDGE('',*,*,#11767,.F.);
#16472=ORIENTED_EDGE('',*,*,#11766,.F.);
#16473=ORIENTED_EDGE('',*,*,#11765,.F.);
#16474=ORIENTED_EDGE('',*,*,#11764,.F.);
#16475=ORIENTED_EDGE('',*,*,#11763,.F.);
#16476=ORIENTED_EDGE('',*,*,#11762,.F.);
#16477=ORIENTED_EDGE('',*,*,#11761,.F.);
#16478=ORIENTED_EDGE('',*,*,#11760,.F.);
#16479=ORIENTED_EDGE('',*,*,#11759,.F.);
#16480=ORIENTED_EDGE('',*,*,#11758,.F.);
#16481=ORIENTED_EDGE('',*,*,#11757,.F.);
#16482=ORIENTED_EDGE('',*,*,#11756,.F.);
#16483=ORIENTED_EDGE('',*,*,#11755,.F.);
#16484=ORIENTED_EDGE('',*,*,#11754,.F.);
#16485=ORIENTED_EDGE('',*,*,#11753,.F.);
#16486=ORIENTED_EDGE('',*,*,#11752,.F.);
#16487=ORIENTED_EDGE('',*,*,#11751,.F.);
#16488=ORIENTED_EDGE('',*,*,#11750,.F.);
#16489=ORIENTED_EDGE('',*,*,#11749,.F.);
#16490=ORIENTED_EDGE('',*,*,#11748,.F.);
#16491=ORIENTED_EDGE('',*,*,#11747,.F.);
#16492=ORIENTED_EDGE('',*,*,#11746,.F.);
#16493=ORIENTED_EDGE('',*,*,#11745,.F.);
#16494=ORIENTED_EDGE('',*,*,#11744,.F.);
#16495=ORIENTED_EDGE('',*,*,#11743,.F.);
#16496=ORIENTED_EDGE('',*,*,#11742,.F.);
#16497=ORIENTED_EDGE('',*,*,#11741,.F.);
#16498=ORIENTED_EDGE('',*,*,#11740,.F.);
#16499=ORIENTED_EDGE('',*,*,#11739,.F.);
#16500=ORIENTED_EDGE('',*,*,#11738,.F.);
#16501=ORIENTED_EDGE('',*,*,#11737,.F.);
#16502=ORIENTED_EDGE('',*,*,#11736,.F.);
#16503=ORIENTED_EDGE('',*,*,#11735,.F.);
#16504=ORIENTED_EDGE('',*,*,#11734,.F.);
#16505=ORIENTED_EDGE('',*,*,#11733,.F.);
#16506=ORIENTED_EDGE('',*,*,#11732,.F.);
#16507=ORIENTED_EDGE('',*,*,#11731,.F.);
#16508=ORIENTED_EDGE('',*,*,#11824,.F.);
#16509=ORIENTED_EDGE('',*,*,#11551,.T.);
#16510=ORIENTED_EDGE('',*,*,#11556,.T.);
#16511=ORIENTED_EDGE('',*,*,#11555,.T.);
#16512=ORIENTED_EDGE('',*,*,#11561,.T.);
#16513=ORIENTED_EDGE('',*,*,#11560,.T.);
#16514=ORIENTED_EDGE('',*,*,#11566,.T.);
#16515=ORIENTED_EDGE('',*,*,#11565,.T.);
#16516=ORIENTED_EDGE('',*,*,#11571,.T.);
#16517=ORIENTED_EDGE('',*,*,#11570,.T.);
#16518=ORIENTED_EDGE('',*,*,#11575,.T.);
#16519=ORIENTED_EDGE('',*,*,#11574,.T.);
#16520=ORIENTED_EDGE('',*,*,#11580,.T.);
#16521=ORIENTED_EDGE('',*,*,#11579,.T.);
#16522=ORIENTED_EDGE('',*,*,#11584,.T.);
#16523=ORIENTED_EDGE('',*,*,#11583,.T.);
#16524=ORIENTED_EDGE('',*,*,#11589,.T.);
#16525=ORIENTED_EDGE('',*,*,#11588,.T.);
#16526=ORIENTED_EDGE('',*,*,#11593,.T.);
#16527=ORIENTED_EDGE('',*,*,#11592,.T.);
#16528=ORIENTED_EDGE('',*,*,#11598,.T.);
#16529=ORIENTED_EDGE('',*,*,#11597,.T.);
#16530=ORIENTED_EDGE('',*,*,#11602,.T.);
#16531=ORIENTED_EDGE('',*,*,#11601,.T.);
#16532=ORIENTED_EDGE('',*,*,#11607,.T.);
#16533=ORIENTED_EDGE('',*,*,#11606,.T.);
#16534=ORIENTED_EDGE('',*,*,#11611,.T.);
#16535=ORIENTED_EDGE('',*,*,#11610,.T.);
#16536=ORIENTED_EDGE('',*,*,#11616,.T.);
#16537=ORIENTED_EDGE('',*,*,#11615,.T.);
#16538=ORIENTED_EDGE('',*,*,#11620,.T.);
#16539=ORIENTED_EDGE('',*,*,#11619,.T.);
#16540=ORIENTED_EDGE('',*,*,#11625,.T.);
#16541=ORIENTED_EDGE('',*,*,#11624,.T.);
#16542=ORIENTED_EDGE('',*,*,#11629,.T.);
#16543=ORIENTED_EDGE('',*,*,#11628,.T.);
#16544=ORIENTED_EDGE('',*,*,#11634,.T.);
#16545=ORIENTED_EDGE('',*,*,#11633,.T.);
#16546=ORIENTED_EDGE('',*,*,#11638,.T.);
#16547=ORIENTED_EDGE('',*,*,#11637,.T.);
#16548=ORIENTED_EDGE('',*,*,#11643,.T.);
#16549=ORIENTED_EDGE('',*,*,#11642,.T.);
#16550=ORIENTED_EDGE('',*,*,#11647,.T.);
#16551=ORIENTED_EDGE('',*,*,#11646,.T.);
#16552=ORIENTED_EDGE('',*,*,#11652,.T.);
#16553=ORIENTED_EDGE('',*,*,#11651,.T.);
#16554=ORIENTED_EDGE('',*,*,#11656,.T.);
#16555=ORIENTED_EDGE('',*,*,#11655,.T.);
#16556=ORIENTED_EDGE('',*,*,#11661,.T.);
#16557=ORIENTED_EDGE('',*,*,#11660,.T.);
#16558=ORIENTED_EDGE('',*,*,#11666,.T.);
#16559=ORIENTED_EDGE('',*,*,#11665,.T.);
#16560=ORIENTED_EDGE('',*,*,#11670,.T.);
#16561=ORIENTED_EDGE('',*,*,#11669,.T.);
#16562=ORIENTED_EDGE('',*,*,#11675,.T.);
#16563=ORIENTED_EDGE('',*,*,#11674,.T.);
#16564=ORIENTED_EDGE('',*,*,#11679,.T.);
#16565=ORIENTED_EDGE('',*,*,#11678,.T.);
#16566=ORIENTED_EDGE('',*,*,#11684,.T.);
#16567=ORIENTED_EDGE('',*,*,#11683,.T.);
#16568=ORIENTED_EDGE('',*,*,#11688,.T.);
#16569=ORIENTED_EDGE('',*,*,#11687,.T.);
#16570=ORIENTED_EDGE('',*,*,#11693,.T.);
#16571=ORIENTED_EDGE('',*,*,#11692,.T.);
#16572=ORIENTED_EDGE('',*,*,#11698,.T.);
#16573=ORIENTED_EDGE('',*,*,#11697,.T.);
#16574=ORIENTED_EDGE('',*,*,#11702,.T.);
#16575=ORIENTED_EDGE('',*,*,#11701,.T.);
#16576=ORIENTED_EDGE('',*,*,#11707,.T.);
#16577=ORIENTED_EDGE('',*,*,#11706,.T.);
#16578=ORIENTED_EDGE('',*,*,#11711,.T.);
#16579=ORIENTED_EDGE('',*,*,#11710,.T.);
#16580=ORIENTED_EDGE('',*,*,#11716,.T.);
#16581=ORIENTED_EDGE('',*,*,#11715,.T.);
#16582=ORIENTED_EDGE('',*,*,#11721,.T.);
#16583=ORIENTED_EDGE('',*,*,#11720,.T.);
#16584=ORIENTED_EDGE('',*,*,#11726,.T.);
#16585=ORIENTED_EDGE('',*,*,#11725,.T.);
#16586=ORIENTED_EDGE('',*,*,#11815,.T.);
#16587=ORIENTED_EDGE('',*,*,#11814,.T.);
#16588=ORIENTED_EDGE('',*,*,#11825,.T.);
#16589=ORIENTED_EDGE('',*,*,#11826,.T.);
#16590=ORIENTED_EDGE('',*,*,#11827,.T.);
#16591=ORIENTED_EDGE('',*,*,#11552,.T.);
#16592=ORIENTED_EDGE('',*,*,#11824,.T.);
#16593=ORIENTED_EDGE('',*,*,#11821,.F.);
#16594=ORIENTED_EDGE('',*,*,#11812,.F.);
#16595=ORIENTED_EDGE('',*,*,#11811,.F.);
#16596=ORIENTED_EDGE('',*,*,#11728,.F.);
#16597=ORIENTED_EDGE('',*,*,#11727,.F.);
#16598=ORIENTED_EDGE('',*,*,#11723,.F.);
#16599=ORIENTED_EDGE('',*,*,#11722,.F.);
#16600=ORIENTED_EDGE('',*,*,#11718,.F.);
#16601=ORIENTED_EDGE('',*,*,#11717,.F.);
#16602=ORIENTED_EDGE('',*,*,#11713,.F.);
#16603=ORIENTED_EDGE('',*,*,#11712,.F.);
#16604=ORIENTED_EDGE('',*,*,#11708,.F.);
#16605=ORIENTED_EDGE('',*,*,#11704,.F.);
#16606=ORIENTED_EDGE('',*,*,#11703,.F.);
#16607=ORIENTED_EDGE('',*,*,#11699,.F.);
#16608=ORIENTED_EDGE('',*,*,#11695,.F.);
#16609=ORIENTED_EDGE('',*,*,#11694,.F.);
#16610=ORIENTED_EDGE('',*,*,#11690,.F.);
#16611=ORIENTED_EDGE('',*,*,#11689,.F.);
#16612=ORIENTED_EDGE('',*,*,#11685,.F.);
#16613=ORIENTED_EDGE('',*,*,#11681,.F.);
#16614=ORIENTED_EDGE('',*,*,#11680,.F.);
#16615=ORIENTED_EDGE('',*,*,#11676,.F.);
#16616=ORIENTED_EDGE('',*,*,#11672,.F.);
#16617=ORIENTED_EDGE('',*,*,#11671,.F.);
#16618=ORIENTED_EDGE('',*,*,#11667,.F.);
#16619=ORIENTED_EDGE('',*,*,#11663,.F.);
#16620=ORIENTED_EDGE('',*,*,#11662,.F.);
#16621=ORIENTED_EDGE('',*,*,#11658,.F.);
#16622=ORIENTED_EDGE('',*,*,#11657,.F.);
#16623=ORIENTED_EDGE('',*,*,#11653,.F.);
#16624=ORIENTED_EDGE('',*,*,#11649,.F.);
#16625=ORIENTED_EDGE('',*,*,#11648,.F.);
#16626=ORIENTED_EDGE('',*,*,#11644,.F.);
#16627=ORIENTED_EDGE('',*,*,#11640,.F.);
#16628=ORIENTED_EDGE('',*,*,#11639,.F.);
#16629=ORIENTED_EDGE('',*,*,#11635,.F.);
#16630=ORIENTED_EDGE('',*,*,#11631,.F.);
#16631=ORIENTED_EDGE('',*,*,#11630,.F.);
#16632=ORIENTED_EDGE('',*,*,#11626,.F.);
#16633=ORIENTED_EDGE('',*,*,#11622,.F.);
#16634=ORIENTED_EDGE('',*,*,#11621,.F.);
#16635=ORIENTED_EDGE('',*,*,#11617,.F.);
#16636=ORIENTED_EDGE('',*,*,#11613,.F.);
#16637=ORIENTED_EDGE('',*,*,#11612,.F.);
#16638=ORIENTED_EDGE('',*,*,#11608,.F.);
#16639=ORIENTED_EDGE('',*,*,#11604,.F.);
#16640=ORIENTED_EDGE('',*,*,#11603,.F.);
#16641=ORIENTED_EDGE('',*,*,#11599,.F.);
#16642=ORIENTED_EDGE('',*,*,#11595,.F.);
#16643=ORIENTED_EDGE('',*,*,#11594,.F.);
#16644=ORIENTED_EDGE('',*,*,#11590,.F.);
#16645=ORIENTED_EDGE('',*,*,#11586,.F.);
#16646=ORIENTED_EDGE('',*,*,#11585,.F.);
#16647=ORIENTED_EDGE('',*,*,#11581,.F.);
#16648=ORIENTED_EDGE('',*,*,#11577,.F.);
#16649=ORIENTED_EDGE('',*,*,#11576,.F.);
#16650=ORIENTED_EDGE('',*,*,#11572,.F.);
#16651=ORIENTED_EDGE('',*,*,#11568,.F.);
#16652=ORIENTED_EDGE('',*,*,#11567,.F.);
#16653=ORIENTED_EDGE('',*,*,#11563,.F.);
#16654=ORIENTED_EDGE('',*,*,#11562,.F.);
#16655=ORIENTED_EDGE('',*,*,#11558,.F.);
#16656=ORIENTED_EDGE('',*,*,#11557,.F.);
#16657=ORIENTED_EDGE('',*,*,#11553,.F.);
#16658=ORIENTED_EDGE('',*,*,#11827,.F.);
#16659=ORIENTED_EDGE('',*,*,#11828,.T.);
#16660=ORIENTED_EDGE('',*,*,#11729,.F.);
#16661=ORIENTED_EDGE('',*,*,#11810,.F.);
#16662=ORIENTED_EDGE('',*,*,#11809,.F.);
#16663=ORIENTED_EDGE('',*,*,#11808,.F.);
#16664=ORIENTED_EDGE('',*,*,#11807,.F.);
#16665=ORIENTED_EDGE('',*,*,#11806,.F.);
#16666=ORIENTED_EDGE('',*,*,#11805,.F.);
#16667=ORIENTED_EDGE('',*,*,#11804,.F.);
#16668=ORIENTED_EDGE('',*,*,#11803,.F.);
#16669=ORIENTED_EDGE('',*,*,#11802,.F.);
#16670=ORIENTED_EDGE('',*,*,#11801,.F.);
#16671=ORIENTED_EDGE('',*,*,#11800,.F.);
#16672=ORIENTED_EDGE('',*,*,#11799,.F.);
#16673=ORIENTED_EDGE('',*,*,#11798,.F.);
#16674=ORIENTED_EDGE('',*,*,#11797,.F.);
#16675=ORIENTED_EDGE('',*,*,#11796,.F.);
#16676=ORIENTED_EDGE('',*,*,#11795,.F.);
#16677=ORIENTED_EDGE('',*,*,#11794,.F.);
#16678=ORIENTED_EDGE('',*,*,#11793,.F.);
#16679=ORIENTED_EDGE('',*,*,#11792,.F.);
#16680=ORIENTED_EDGE('',*,*,#11791,.F.);
#16681=ORIENTED_EDGE('',*,*,#11790,.F.);
#16682=ORIENTED_EDGE('',*,*,#11789,.F.);
#16683=ORIENTED_EDGE('',*,*,#11788,.F.);
#16684=ORIENTED_EDGE('',*,*,#11787,.F.);
#16685=ORIENTED_EDGE('',*,*,#11786,.F.);
#16686=ORIENTED_EDGE('',*,*,#11785,.F.);
#16687=ORIENTED_EDGE('',*,*,#11784,.F.);
#16688=ORIENTED_EDGE('',*,*,#11783,.F.);
#16689=ORIENTED_EDGE('',*,*,#11782,.F.);
#16690=ORIENTED_EDGE('',*,*,#11781,.F.);
#16691=ORIENTED_EDGE('',*,*,#11780,.F.);
#16692=ORIENTED_EDGE('',*,*,#11779,.F.);
#16693=ORIENTED_EDGE('',*,*,#11778,.F.);
#16694=ORIENTED_EDGE('',*,*,#11777,.F.);
#16695=ORIENTED_EDGE('',*,*,#11776,.F.);
#16696=ORIENTED_EDGE('',*,*,#11775,.F.);
#16697=ORIENTED_EDGE('',*,*,#11774,.F.);
#16698=ORIENTED_EDGE('',*,*,#11773,.F.);
#16699=ORIENTED_EDGE('',*,*,#11772,.F.);
#16700=ORIENTED_EDGE('',*,*,#11829,.F.);
#16701=ORIENTED_EDGE('',*,*,#11816,.T.);
#16702=ORIENTED_EDGE('',*,*,#11828,.F.);
#16703=ORIENTED_EDGE('',*,*,#11826,.F.);
#16704=ORIENTED_EDGE('',*,*,#11830,.T.);
#16705=ORIENTED_EDGE('',*,*,#11829,.T.);
#16706=ORIENTED_EDGE('',*,*,#11830,.F.);
#16707=ORIENTED_EDGE('',*,*,#11825,.F.);
#16708=ORIENTED_EDGE('',*,*,#11730,.F.);
#16709=ORIENTED_EDGE('',*,*,#11819,.T.);
#16710=ORIENTED_EDGE('',*,*,#11831,.T.);
#16711=ORIENTED_EDGE('',*,*,#11832,.F.);
#16712=ORIENTED_EDGE('',*,*,#11831,.F.);
#16713=ORIENTED_EDGE('',*,*,#11822,.T.);
#16714=ORIENTED_EDGE('',*,*,#11771,.T.);
#16715=ORIENTED_EDGE('',*,*,#11823,.T.);
#16716=ORIENTED_EDGE('',*,*,#11833,.F.);
#16717=ORIENTED_EDGE('',*,*,#11834,.T.);
#16718=ORIENTED_EDGE('',*,*,#11832,.T.);
#16719=ORIENTED_EDGE('',*,*,#11834,.F.);
#16720=ORIENTED_EDGE('',*,*,#11835,.F.);
#16721=ORIENTED_EDGE('',*,*,#11833,.T.);
#16722=ORIENTED_EDGE('',*,*,#11836,.F.);
#16723=ORIENTED_EDGE('',*,*,#11837,.T.);
#16724=ORIENTED_EDGE('',*,*,#11835,.T.);
#16725=ORIENTED_EDGE('',*,*,#11837,.F.);
#16726=ORIENTED_EDGE('',*,*,#11836,.T.);
#16727=ORIENTED_EDGE('',*,*,#11838,.F.);
#16728=ORIENTED_EDGE('',*,*,#11839,.F.);
#16729=ORIENTED_EDGE('',*,*,#11840,.T.);
#16730=ORIENTED_EDGE('',*,*,#11838,.T.);
#16731=ORIENTED_EDGE('',*,*,#11840,.F.);
#16732=ORIENTED_EDGE('',*,*,#11839,.T.);
#16733=ORIENTED_EDGE('',*,*,#11841,.T.);
#16734=ORIENTED_EDGE('',*,*,#11842,.F.);
#16735=ORIENTED_EDGE('',*,*,#11841,.F.);
#16736=ORIENTED_EDGE('',*,*,#11842,.T.);
#16737=ORIENTED_EDGE('',*,*,#11843,.F.);
#16738=ORIENTED_EDGE('',*,*,#11844,.T.);
#16739=ORIENTED_EDGE('',*,*,#11845,.T.);
#16740=ORIENTED_EDGE('',*,*,#11846,.T.);
#16741=ORIENTED_EDGE('',*,*,#11846,.F.);
#16742=ORIENTED_EDGE('',*,*,#11847,.F.);
#16743=ORIENTED_EDGE('',*,*,#11848,.F.);
#16744=ORIENTED_EDGE('',*,*,#11849,.T.);
#16745=ORIENTED_EDGE('',*,*,#11850,.T.);
#16746=ORIENTED_EDGE('',*,*,#11851,.T.);
#16747=ORIENTED_EDGE('',*,*,#11852,.T.);
#16748=ORIENTED_EDGE('',*,*,#11852,.F.);
#16749=ORIENTED_EDGE('',*,*,#11853,.T.);
#16750=ORIENTED_EDGE('',*,*,#11854,.T.);
#16751=ORIENTED_EDGE('',*,*,#11855,.T.);
#16752=ORIENTED_EDGE('',*,*,#11856,.F.);
#16753=ORIENTED_EDGE('',*,*,#11857,.F.);
#16754=ORIENTED_EDGE('',*,*,#11858,.T.);
#16755=ORIENTED_EDGE('',*,*,#11859,.T.);
#16756=ORIENTED_EDGE('',*,*,#11860,.T.);
#16757=ORIENTED_EDGE('',*,*,#11859,.F.);
#16758=ORIENTED_EDGE('',*,*,#11861,.T.);
#16759=ORIENTED_EDGE('',*,*,#11862,.T.);
#16760=ORIENTED_EDGE('',*,*,#11863,.T.);
#16761=ORIENTED_EDGE('',*,*,#11864,.T.);
#16762=ORIENTED_EDGE('',*,*,#11865,.T.);
#16763=ORIENTED_EDGE('',*,*,#11866,.T.);
#16764=ORIENTED_EDGE('',*,*,#11862,.F.);
#16765=ORIENTED_EDGE('',*,*,#11855,.F.);
#16766=ORIENTED_EDGE('',*,*,#11860,.F.);
#16767=ORIENTED_EDGE('',*,*,#11866,.F.);
#16768=ORIENTED_EDGE('',*,*,#11867,.T.);
#16769=ORIENTED_EDGE('',*,*,#11868,.F.);
#16770=ORIENTED_EDGE('',*,*,#11869,.T.);
#16771=ORIENTED_EDGE('',*,*,#11870,.T.);
#16772=ORIENTED_EDGE('',*,*,#11871,.T.);
#16773=ORIENTED_EDGE('',*,*,#11872,.F.);
#16774=ORIENTED_EDGE('',*,*,#11871,.F.);
#16775=ORIENTED_EDGE('',*,*,#11873,.F.);
#16776=ORIENTED_EDGE('',*,*,#11874,.T.);
#16777=ORIENTED_EDGE('',*,*,#11875,.T.);
#16778=ORIENTED_EDGE('',*,*,#11876,.T.);
#16779=ORIENTED_EDGE('',*,*,#11877,.T.);
#16780=ORIENTED_EDGE('',*,*,#11878,.T.);
#16781=ORIENTED_EDGE('',*,*,#11876,.F.);
#16782=ORIENTED_EDGE('',*,*,#11879,.F.);
#16783=ORIENTED_EDGE('',*,*,#11880,.F.);
#16784=ORIENTED_EDGE('',*,*,#11881,.F.);
#16785=ORIENTED_EDGE('',*,*,#11882,.T.);
#16786=ORIENTED_EDGE('',*,*,#11883,.T.);
#16787=ORIENTED_EDGE('',*,*,#11884,.T.);
#16788=ORIENTED_EDGE('',*,*,#11880,.T.);
#16789=ORIENTED_EDGE('',*,*,#11883,.F.);
#16790=ORIENTED_EDGE('',*,*,#11885,.F.);
#16791=ORIENTED_EDGE('',*,*,#11886,.F.);
#16792=ORIENTED_EDGE('',*,*,#11887,.T.);
#16793=ORIENTED_EDGE('',*,*,#11888,.F.);
#16794=ORIENTED_EDGE('',*,*,#11889,.F.);
#16795=ORIENTED_EDGE('',*,*,#11890,.F.);
#16796=ORIENTED_EDGE('',*,*,#11891,.F.);
#16797=ORIENTED_EDGE('',*,*,#11892,.T.);
#16798=ORIENTED_EDGE('',*,*,#11893,.T.);
#16799=ORIENTED_EDGE('',*,*,#11894,.F.);
#16800=ORIENTED_EDGE('',*,*,#11895,.F.);
#16801=ORIENTED_EDGE('',*,*,#11896,.F.);
#16802=ORIENTED_EDGE('',*,*,#11897,.T.);
#16803=ORIENTED_EDGE('',*,*,#11898,.F.);
#16804=ORIENTED_EDGE('',*,*,#11856,.T.);
#16805=ORIENTED_EDGE('',*,*,#11867,.F.);
#16806=ORIENTED_EDGE('',*,*,#11865,.F.);
#16807=ORIENTED_EDGE('',*,*,#11899,.F.);
#16808=ORIENTED_EDGE('',*,*,#11900,.F.);
#16809=ORIENTED_EDGE('',*,*,#11895,.T.);
#16810=ORIENTED_EDGE('',*,*,#11901,.T.);
#16811=ORIENTED_EDGE('',*,*,#11902,.T.);
#16812=ORIENTED_EDGE('',*,*,#11903,.T.);
#16813=ORIENTED_EDGE('',*,*,#11904,.T.);
#16814=ORIENTED_EDGE('',*,*,#11905,.T.);
#16815=ORIENTED_EDGE('',*,*,#11906,.T.);
#16816=ORIENTED_EDGE('',*,*,#11896,.T.);
#16817=ORIENTED_EDGE('',*,*,#11904,.F.);
#16818=ORIENTED_EDGE('',*,*,#11907,.T.);
#16819=ORIENTED_EDGE('',*,*,#11908,.T.);
#16820=ORIENTED_EDGE('',*,*,#11909,.T.);
#16821=ORIENTED_EDGE('',*,*,#11910,.F.);
#16822=ORIENTED_EDGE('',*,*,#11911,.T.);
#16823=ORIENTED_EDGE('',*,*,#11912,.F.);
#16824=ORIENTED_EDGE('',*,*,#11913,.T.);
#16825=ORIENTED_EDGE('',*,*,#11914,.T.);
#16826=ORIENTED_EDGE('',*,*,#11915,.T.);
#16827=ORIENTED_EDGE('',*,*,#11916,.T.);
#16828=ORIENTED_EDGE('',*,*,#11917,.T.);
#16829=ORIENTED_EDGE('',*,*,#11918,.T.);
#16830=ORIENTED_EDGE('',*,*,#11919,.T.);
#16831=ORIENTED_EDGE('',*,*,#11920,.T.);
#16832=ORIENTED_EDGE('',*,*,#11921,.T.);
#16833=ORIENTED_EDGE('',*,*,#11911,.F.);
#16834=ORIENTED_EDGE('',*,*,#11922,.T.);
#16835=ORIENTED_EDGE('',*,*,#11923,.T.);
#16836=ORIENTED_EDGE('',*,*,#11924,.F.);
#16837=ORIENTED_EDGE('',*,*,#11913,.F.);
#16838=ORIENTED_EDGE('',*,*,#11925,.F.);
#16839=ORIENTED_EDGE('',*,*,#11926,.T.);
#16840=ORIENTED_EDGE('',*,*,#11927,.F.);
#16841=ORIENTED_EDGE('',*,*,#11920,.F.);
#16842=ORIENTED_EDGE('',*,*,#11928,.F.);
#16843=ORIENTED_EDGE('',*,*,#11929,.T.);
#16844=ORIENTED_EDGE('',*,*,#11930,.T.);
#16845=ORIENTED_EDGE('',*,*,#11916,.F.);
#16846=ORIENTED_EDGE('',*,*,#11931,.F.);
#16847=ORIENTED_EDGE('',*,*,#11932,.F.);
#16848=ORIENTED_EDGE('',*,*,#11933,.F.);
#16849=ORIENTED_EDGE('',*,*,#11934,.T.);
#16850=ORIENTED_EDGE('',*,*,#11935,.T.);
#16851=ORIENTED_EDGE('',*,*,#11936,.T.);
#16852=ORIENTED_EDGE('',*,*,#11937,.T.);
#16853=ORIENTED_EDGE('',*,*,#11938,.T.);
#16854=ORIENTED_EDGE('',*,*,#11939,.T.);
#16855=ORIENTED_EDGE('',*,*,#11940,.F.);
#16856=ORIENTED_EDGE('',*,*,#11941,.F.);
#16857=ORIENTED_EDGE('',*,*,#11942,.F.);
#16858=ORIENTED_EDGE('',*,*,#11943,.F.);
#16859=ORIENTED_EDGE('',*,*,#11944,.T.);
#16860=ORIENTED_EDGE('',*,*,#11945,.F.);
#16861=ORIENTED_EDGE('',*,*,#11946,.T.);
#16862=ORIENTED_EDGE('',*,*,#11947,.T.);
#16863=ORIENTED_EDGE('',*,*,#11941,.T.);
#16864=ORIENTED_EDGE('',*,*,#11948,.T.);
#16865=ORIENTED_EDGE('',*,*,#11949,.F.);
#16866=ORIENTED_EDGE('',*,*,#11909,.F.);
#16867=ORIENTED_EDGE('',*,*,#11950,.F.);
#16868=ORIENTED_EDGE('',*,*,#11951,.F.);
#16869=ORIENTED_EDGE('',*,*,#11945,.T.);
#16870=ORIENTED_EDGE('',*,*,#11908,.F.);
#16871=ORIENTED_EDGE('',*,*,#11952,.T.);
#16872=ORIENTED_EDGE('',*,*,#11953,.T.);
#16873=ORIENTED_EDGE('',*,*,#11954,.T.);
#16874=ORIENTED_EDGE('',*,*,#11932,.T.);
#16875=ORIENTED_EDGE('',*,*,#11955,.F.);
#16876=ORIENTED_EDGE('',*,*,#11956,.T.);
#16877=ORIENTED_EDGE('',*,*,#11950,.T.);
#16878=ORIENTED_EDGE('',*,*,#11957,.T.);
#16879=ORIENTED_EDGE('',*,*,#11958,.T.);
#16880=ORIENTED_EDGE('',*,*,#11901,.F.);
#16881=ORIENTED_EDGE('',*,*,#11894,.T.);
#16882=ORIENTED_EDGE('',*,*,#11959,.T.);
#16883=ORIENTED_EDGE('',*,*,#11960,.T.);
#16884=ORIENTED_EDGE('',*,*,#11961,.T.);
#16885=ORIENTED_EDGE('',*,*,#11962,.T.);
#16886=ORIENTED_EDGE('',*,*,#11963,.T.);
#16887=ORIENTED_EDGE('',*,*,#11964,.F.);
#16888=ORIENTED_EDGE('',*,*,#11965,.T.);
#16889=ORIENTED_EDGE('',*,*,#11966,.T.);
#16890=ORIENTED_EDGE('',*,*,#11967,.T.);
#16891=ORIENTED_EDGE('',*,*,#11892,.F.);
#16892=ORIENTED_EDGE('',*,*,#11966,.F.);
#16893=ORIENTED_EDGE('',*,*,#11968,.T.);
#16894=ORIENTED_EDGE('',*,*,#11962,.F.);
#16895=ORIENTED_EDGE('',*,*,#11960,.F.);
#16896=ORIENTED_EDGE('',*,*,#11969,.T.);
#16897=ORIENTED_EDGE('',*,*,#11957,.F.);
#16898=ORIENTED_EDGE('',*,*,#11958,.F.);
#16899=ORIENTED_EDGE('',*,*,#11970,.F.);
#16900=ORIENTED_EDGE('',*,*,#11971,.T.);
#16901=ORIENTED_EDGE('',*,*,#11972,.F.);
#16902=ORIENTED_EDGE('',*,*,#11973,.F.);
#16903=ORIENTED_EDGE('',*,*,#11902,.F.);
#16904=ORIENTED_EDGE('',*,*,#11969,.F.);
#16905=ORIENTED_EDGE('',*,*,#11974,.T.);
#16906=ORIENTED_EDGE('',*,*,#11975,.T.);
#16907=ORIENTED_EDGE('',*,*,#11970,.T.);
#16908=ORIENTED_EDGE('',*,*,#11963,.F.);
#16909=ORIENTED_EDGE('',*,*,#11976,.F.);
#16910=ORIENTED_EDGE('',*,*,#11946,.F.);
#16911=ORIENTED_EDGE('',*,*,#11977,.F.);
#16912=ORIENTED_EDGE('',*,*,#11978,.F.);
#16913=ORIENTED_EDGE('',*,*,#11979,.F.);
#16914=ORIENTED_EDGE('',*,*,#11980,.F.);
#16915=ORIENTED_EDGE('',*,*,#11981,.F.);
#16916=ORIENTED_EDGE('',*,*,#11982,.F.);
#16917=ORIENTED_EDGE('',*,*,#11974,.F.);
#16918=ORIENTED_EDGE('',*,*,#11968,.F.);
#16919=ORIENTED_EDGE('',*,*,#11983,.T.);
#16920=ORIENTED_EDGE('',*,*,#11984,.T.);
#16921=ORIENTED_EDGE('',*,*,#11976,.T.);
#16922=ORIENTED_EDGE('',*,*,#11965,.F.);
#16923=ORIENTED_EDGE('',*,*,#11985,.F.);
#16924=ORIENTED_EDGE('',*,*,#11986,.F.);
#16925=ORIENTED_EDGE('',*,*,#11987,.F.);
#16926=ORIENTED_EDGE('',*,*,#11988,.F.);
#16927=ORIENTED_EDGE('',*,*,#11983,.F.);
#16928=ORIENTED_EDGE('',*,*,#11989,.T.);
#16929=ORIENTED_EDGE('',*,*,#11890,.T.);
#16930=ORIENTED_EDGE('',*,*,#11990,.T.);
#16931=ORIENTED_EDGE('',*,*,#11991,.T.);
#16932=ORIENTED_EDGE('',*,*,#11992,.T.);
#16933=ORIENTED_EDGE('',*,*,#11993,.T.);
#16934=ORIENTED_EDGE('',*,*,#11990,.F.);
#16935=ORIENTED_EDGE('',*,*,#11889,.T.);
#16936=ORIENTED_EDGE('',*,*,#11994,.T.);
#16937=ORIENTED_EDGE('',*,*,#11985,.T.);
#16938=ORIENTED_EDGE('',*,*,#11964,.T.);
#16939=ORIENTED_EDGE('',*,*,#11891,.T.);
#16940=ORIENTED_EDGE('',*,*,#11989,.F.);
#16941=ORIENTED_EDGE('',*,*,#11995,.T.);
#16942=ORIENTED_EDGE('',*,*,#11993,.F.);
#16943=ORIENTED_EDGE('',*,*,#11996,.T.);
#16944=ORIENTED_EDGE('',*,*,#11997,.F.);
#16945=ORIENTED_EDGE('',*,*,#11998,.F.);
#16946=ORIENTED_EDGE('',*,*,#11999,.F.);
#16947=ORIENTED_EDGE('',*,*,#12000,.T.);
#16948=ORIENTED_EDGE('',*,*,#12001,.T.);
#16949=ORIENTED_EDGE('',*,*,#12002,.T.);
#16950=ORIENTED_EDGE('',*,*,#12003,.F.);
#16951=ORIENTED_EDGE('',*,*,#12004,.T.);
#16952=ORIENTED_EDGE('',*,*,#12001,.F.);
#16953=ORIENTED_EDGE('',*,*,#12005,.T.);
#16954=ORIENTED_EDGE('',*,*,#12003,.T.);
#16955=ORIENTED_EDGE('',*,*,#12006,.F.);
#16956=ORIENTED_EDGE('',*,*,#12007,.F.);
#16957=ORIENTED_EDGE('',*,*,#12008,.F.);
#16958=ORIENTED_EDGE('',*,*,#11869,.F.);
#16959=ORIENTED_EDGE('',*,*,#12009,.F.);
#16960=ORIENTED_EDGE('',*,*,#12010,.T.);
#16961=ORIENTED_EDGE('',*,*,#12011,.F.);
#16962=ORIENTED_EDGE('',*,*,#11863,.F.);
#16963=ORIENTED_EDGE('',*,*,#12012,.T.);
#16964=ORIENTED_EDGE('',*,*,#12002,.F.);
#16965=ORIENTED_EDGE('',*,*,#12013,.T.);
#16966=ORIENTED_EDGE('',*,*,#11858,.F.);
#16967=ORIENTED_EDGE('',*,*,#12014,.F.);
#16968=ORIENTED_EDGE('',*,*,#12015,.T.);
#16969=ORIENTED_EDGE('',*,*,#12016,.F.);
#16970=ORIENTED_EDGE('',*,*,#11849,.F.);
#16971=ORIENTED_EDGE('',*,*,#12017,.F.);
#16972=ORIENTED_EDGE('',*,*,#12018,.F.);
#16973=ORIENTED_EDGE('',*,*,#12019,.F.);
#16974=ORIENTED_EDGE('',*,*,#11844,.F.);
#16975=ORIENTED_EDGE('',*,*,#12000,.F.);
#16976=ORIENTED_EDGE('',*,*,#12005,.F.);
#16977=ORIENTED_EDGE('',*,*,#12020,.F.);
#16978=ORIENTED_EDGE('',*,*,#12020,.T.);
#16979=ORIENTED_EDGE('',*,*,#12021,.T.);
#16980=ORIENTED_EDGE('',*,*,#12022,.T.);
#16981=ORIENTED_EDGE('',*,*,#12023,.T.);
#16982=ORIENTED_EDGE('',*,*,#12021,.F.);
#16983=ORIENTED_EDGE('',*,*,#12024,.F.);
#16984=ORIENTED_EDGE('',*,*,#12025,.F.);
#16985=ORIENTED_EDGE('',*,*,#12026,.T.);
#16986=ORIENTED_EDGE('',*,*,#12022,.F.);
#16987=ORIENTED_EDGE('',*,*,#12023,.F.);
#16988=ORIENTED_EDGE('',*,*,#12026,.F.);
#16989=ORIENTED_EDGE('',*,*,#12027,.T.);
#16990=ORIENTED_EDGE('',*,*,#12024,.T.);
#16991=ORIENTED_EDGE('',*,*,#12025,.T.);
#16992=ORIENTED_EDGE('',*,*,#12027,.F.);
#16993=ORIENTED_EDGE('',*,*,#12028,.T.);
#16994=ORIENTED_EDGE('',*,*,#11991,.F.);
#16995=ORIENTED_EDGE('',*,*,#11999,.T.);
#16996=ORIENTED_EDGE('',*,*,#12029,.F.);
#16997=ORIENTED_EDGE('',*,*,#12030,.F.);
#16998=ORIENTED_EDGE('',*,*,#12031,.F.);
#16999=ORIENTED_EDGE('',*,*,#12032,.F.);
#17000=ORIENTED_EDGE('',*,*,#12028,.F.);
#17001=ORIENTED_EDGE('',*,*,#12033,.T.);
#17002=ORIENTED_EDGE('',*,*,#12034,.T.);
#17003=ORIENTED_EDGE('',*,*,#12035,.T.);
#17004=ORIENTED_EDGE('',*,*,#12034,.F.);
#17005=ORIENTED_EDGE('',*,*,#12033,.F.);
#17006=ORIENTED_EDGE('',*,*,#12036,.F.);
#17007=ORIENTED_EDGE('',*,*,#11885,.T.);
#17008=ORIENTED_EDGE('',*,*,#11882,.F.);
#17009=ORIENTED_EDGE('',*,*,#12037,.T.);
#17010=ORIENTED_EDGE('',*,*,#12038,.F.);
#17011=ORIENTED_EDGE('',*,*,#12039,.T.);
#17012=ORIENTED_EDGE('',*,*,#12040,.T.);
#17013=ORIENTED_EDGE('',*,*,#12041,.T.);
#17014=ORIENTED_EDGE('',*,*,#12042,.T.);
#17015=ORIENTED_EDGE('',*,*,#12043,.T.);
#17016=ORIENTED_EDGE('',*,*,#12044,.T.);
#17017=ORIENTED_EDGE('',*,*,#12045,.T.);
#17018=ORIENTED_EDGE('',*,*,#12046,.T.);
#17019=ORIENTED_EDGE('',*,*,#12043,.F.);
#17020=ORIENTED_EDGE('',*,*,#12047,.T.);
#17021=ORIENTED_EDGE('',*,*,#12041,.F.);
#17022=ORIENTED_EDGE('',*,*,#11955,.T.);
#17023=ORIENTED_EDGE('',*,*,#12048,.T.);
#17024=ORIENTED_EDGE('',*,*,#12045,.F.);
#17025=ORIENTED_EDGE('',*,*,#11951,.T.);
#17026=ORIENTED_EDGE('',*,*,#12049,.T.);
#17027=ORIENTED_EDGE('',*,*,#12050,.T.);
#17028=ORIENTED_EDGE('',*,*,#11977,.T.);
#17029=ORIENTED_EDGE('',*,*,#12039,.F.);
#17030=ORIENTED_EDGE('',*,*,#12051,.T.);
#17031=ORIENTED_EDGE('',*,*,#12050,.F.);
#17032=ORIENTED_EDGE('',*,*,#11954,.F.);
#17033=ORIENTED_EDGE('',*,*,#12052,.F.);
#17034=ORIENTED_EDGE('',*,*,#12053,.T.);
#17035=ORIENTED_EDGE('',*,*,#12054,.T.);
#17036=ORIENTED_EDGE('',*,*,#12055,.T.);
#17037=ORIENTED_EDGE('',*,*,#11933,.T.);
#17038=ORIENTED_EDGE('',*,*,#11953,.F.);
#17039=ORIENTED_EDGE('',*,*,#12056,.F.);
#17040=ORIENTED_EDGE('',*,*,#12057,.T.);
#17041=ORIENTED_EDGE('',*,*,#12052,.T.);
#17042=ORIENTED_EDGE('',*,*,#11907,.F.);
#17043=ORIENTED_EDGE('',*,*,#12058,.T.);
#17044=ORIENTED_EDGE('',*,*,#12059,.T.);
#17045=ORIENTED_EDGE('',*,*,#12056,.T.);
#17046=ORIENTED_EDGE('',*,*,#11952,.F.);
#17047=ORIENTED_EDGE('',*,*,#12040,.F.);
#17048=ORIENTED_EDGE('',*,*,#12049,.F.);
#17049=ORIENTED_EDGE('',*,*,#11956,.F.);
#17050=ORIENTED_EDGE('',*,*,#12044,.F.);
#17051=ORIENTED_EDGE('',*,*,#12060,.F.);
#17052=ORIENTED_EDGE('',*,*,#11943,.T.);
#17053=ORIENTED_EDGE('',*,*,#12061,.F.);
#17054=ORIENTED_EDGE('',*,*,#12062,.T.);
#17055=ORIENTED_EDGE('',*,*,#12048,.F.);
#17056=ORIENTED_EDGE('',*,*,#11931,.T.);
#17057=ORIENTED_EDGE('',*,*,#11915,.F.);
#17058=ORIENTED_EDGE('',*,*,#12063,.F.);
#17059=ORIENTED_EDGE('',*,*,#12064,.T.);
#17060=ORIENTED_EDGE('',*,*,#12054,.F.);
#17061=ORIENTED_EDGE('',*,*,#12065,.T.);
#17062=ORIENTED_EDGE('',*,*,#12066,.T.);
#17063=ORIENTED_EDGE('',*,*,#12067,.T.);
#17064=ORIENTED_EDGE('',*,*,#11929,.F.);
#17065=ORIENTED_EDGE('',*,*,#12068,.F.);
#17066=ORIENTED_EDGE('',*,*,#12069,.T.);
#17067=ORIENTED_EDGE('',*,*,#12070,.T.);
#17068=ORIENTED_EDGE('',*,*,#12071,.T.);
#17069=ORIENTED_EDGE('',*,*,#11937,.F.);
#17070=ORIENTED_EDGE('',*,*,#12072,.T.);
#17071=ORIENTED_EDGE('',*,*,#12073,.T.);
#17072=ORIENTED_EDGE('',*,*,#12074,.T.);
#17073=ORIENTED_EDGE('',*,*,#11934,.F.);
#17074=ORIENTED_EDGE('',*,*,#12055,.F.);
#17075=ORIENTED_EDGE('',*,*,#12064,.F.);
#17076=ORIENTED_EDGE('',*,*,#12075,.F.);
#17077=ORIENTED_EDGE('',*,*,#12076,.T.);
#17078=ORIENTED_EDGE('',*,*,#11925,.T.);
#17079=ORIENTED_EDGE('',*,*,#11912,.T.);
#17080=ORIENTED_EDGE('',*,*,#12077,.T.);
#17081=ORIENTED_EDGE('',*,*,#12078,.T.);
#17082=ORIENTED_EDGE('',*,*,#12079,.T.);
#17083=ORIENTED_EDGE('',*,*,#12080,.T.);
#17084=ORIENTED_EDGE('',*,*,#12081,.T.);
#17085=ORIENTED_EDGE('',*,*,#12082,.F.);
#17086=ORIENTED_EDGE('',*,*,#12083,.T.);
#17087=ORIENTED_EDGE('',*,*,#12084,.F.);
#17088=ORIENTED_EDGE('',*,*,#12085,.T.);
#17089=ORIENTED_EDGE('',*,*,#12078,.F.);
#17090=ORIENTED_EDGE('',*,*,#12086,.T.);
#17091=ORIENTED_EDGE('',*,*,#12087,.F.);
#17092=ORIENTED_EDGE('',*,*,#12083,.F.);
#17093=ORIENTED_EDGE('',*,*,#12088,.T.);
#17094=ORIENTED_EDGE('',*,*,#12089,.T.);
#17095=ORIENTED_EDGE('',*,*,#12090,.T.);
#17096=ORIENTED_EDGE('',*,*,#11981,.T.);
#17097=ORIENTED_EDGE('',*,*,#12091,.T.);
#17098=ORIENTED_EDGE('',*,*,#11980,.T.);
#17099=ORIENTED_EDGE('',*,*,#12092,.T.);
#17100=ORIENTED_EDGE('',*,*,#12093,.T.);
#17101=ORIENTED_EDGE('',*,*,#12091,.F.);
#17102=ORIENTED_EDGE('',*,*,#12094,.T.);
#17103=ORIENTED_EDGE('',*,*,#12088,.F.);
#17104=ORIENTED_EDGE('',*,*,#12095,.T.);
#17105=ORIENTED_EDGE('',*,*,#12096,.T.);
#17106=ORIENTED_EDGE('',*,*,#12097,.T.);
#17107=ORIENTED_EDGE('',*,*,#12098,.T.);
#17108=ORIENTED_EDGE('',*,*,#12095,.F.);
#17109=ORIENTED_EDGE('',*,*,#12099,.T.);
#17110=ORIENTED_EDGE('',*,*,#12090,.F.);
#17111=ORIENTED_EDGE('',*,*,#12099,.F.);
#17112=ORIENTED_EDGE('',*,*,#12100,.T.);
#17113=ORIENTED_EDGE('',*,*,#11975,.F.);
#17114=ORIENTED_EDGE('',*,*,#11982,.T.);
#17115=ORIENTED_EDGE('',*,*,#12098,.F.);
#17116=ORIENTED_EDGE('',*,*,#11897,.F.);
#17117=ORIENTED_EDGE('',*,*,#11906,.F.);
#17118=ORIENTED_EDGE('',*,*,#12101,.T.);
#17119=ORIENTED_EDGE('',*,*,#12102,.F.);
#17120=ORIENTED_EDGE('',*,*,#12103,.F.);
#17121=ORIENTED_EDGE('',*,*,#12104,.F.);
#17122=ORIENTED_EDGE('',*,*,#12105,.F.);
#17123=ORIENTED_EDGE('',*,*,#12106,.F.);
#17124=ORIENTED_EDGE('',*,*,#12107,.F.);
#17125=ORIENTED_EDGE('',*,*,#12108,.F.);
#17126=ORIENTED_EDGE('',*,*,#11971,.F.);
#17127=ORIENTED_EDGE('',*,*,#12100,.F.);
#17128=ORIENTED_EDGE('',*,*,#12109,.F.);
#17129=ORIENTED_EDGE('',*,*,#12110,.T.);
#17130=ORIENTED_EDGE('',*,*,#12111,.T.);
#17131=ORIENTED_EDGE('',*,*,#12112,.T.);
#17132=ORIENTED_EDGE('',*,*,#12113,.T.);
#17133=ORIENTED_EDGE('',*,*,#12111,.F.);
#17134=ORIENTED_EDGE('',*,*,#12114,.T.);
#17135=ORIENTED_EDGE('',*,*,#12115,.T.);
#17136=ORIENTED_EDGE('',*,*,#12115,.F.);
#17137=ORIENTED_EDGE('',*,*,#12116,.T.);
#17138=ORIENTED_EDGE('',*,*,#12117,.F.);
#17139=ORIENTED_EDGE('',*,*,#12118,.T.);
#17140=ORIENTED_EDGE('',*,*,#12119,.F.);
#17141=ORIENTED_EDGE('',*,*,#12120,.T.);
#17142=ORIENTED_EDGE('',*,*,#12121,.F.);
#17143=ORIENTED_EDGE('',*,*,#12122,.T.);
#17144=ORIENTED_EDGE('',*,*,#12112,.F.);
#17145=ORIENTED_EDGE('',*,*,#12113,.F.);
#17146=ORIENTED_EDGE('',*,*,#12122,.F.);
#17147=ORIENTED_EDGE('',*,*,#12123,.T.);
#17148=ORIENTED_EDGE('',*,*,#12124,.T.);
#17149=ORIENTED_EDGE('',*,*,#12125,.T.);
#17150=ORIENTED_EDGE('',*,*,#12126,.T.);
#17151=ORIENTED_EDGE('',*,*,#12124,.F.);
#17152=ORIENTED_EDGE('',*,*,#12127,.F.);
#17153=ORIENTED_EDGE('',*,*,#12128,.T.);
#17154=ORIENTED_EDGE('',*,*,#12125,.F.);
#17155=ORIENTED_EDGE('',*,*,#12126,.F.);
#17156=ORIENTED_EDGE('',*,*,#12128,.F.);
#17157=ORIENTED_EDGE('',*,*,#12093,.F.);
#17158=ORIENTED_EDGE('',*,*,#12129,.F.);
#17159=ORIENTED_EDGE('',*,*,#12116,.F.);
#17160=ORIENTED_EDGE('',*,*,#12114,.F.);
#17161=ORIENTED_EDGE('',*,*,#12110,.F.);
#17162=ORIENTED_EDGE('',*,*,#12120,.F.);
#17163=ORIENTED_EDGE('',*,*,#12130,.F.);
#17164=ORIENTED_EDGE('',*,*,#12123,.F.);
#17165=ORIENTED_EDGE('',*,*,#12109,.T.);
#17166=ORIENTED_EDGE('',*,*,#12131,.T.);
#17167=ORIENTED_EDGE('',*,*,#12127,.T.);
#17168=ORIENTED_EDGE('',*,*,#12131,.F.);
#17169=ORIENTED_EDGE('',*,*,#12107,.T.);
#17170=ORIENTED_EDGE('',*,*,#12132,.T.);
#17171=ORIENTED_EDGE('',*,*,#12121,.T.);
#17172=ORIENTED_EDGE('',*,*,#12132,.F.);
#17173=ORIENTED_EDGE('',*,*,#12106,.T.);
#17174=ORIENTED_EDGE('',*,*,#12133,.T.);
#17175=ORIENTED_EDGE('',*,*,#12133,.F.);
#17176=ORIENTED_EDGE('',*,*,#12105,.T.);
#17177=ORIENTED_EDGE('',*,*,#12134,.F.);
#17178=ORIENTED_EDGE('',*,*,#12135,.T.);
#17179=ORIENTED_EDGE('',*,*,#12136,.T.);
#17180=ORIENTED_EDGE('',*,*,#12108,.T.);
#17181=ORIENTED_EDGE('',*,*,#12102,.T.);
#17182=ORIENTED_EDGE('',*,*,#12137,.T.);
#17183=ORIENTED_EDGE('',*,*,#12138,.T.);
#17184=ORIENTED_EDGE('',*,*,#12139,.T.);
#17185=ORIENTED_EDGE('',*,*,#11905,.F.);
#17186=ORIENTED_EDGE('',*,*,#12140,.F.);
#17187=ORIENTED_EDGE('',*,*,#12137,.F.);
#17188=ORIENTED_EDGE('',*,*,#12101,.F.);
#17189=ORIENTED_EDGE('',*,*,#12141,.T.);
#17190=ORIENTED_EDGE('',*,*,#12014,.T.);
#17191=ORIENTED_EDGE('',*,*,#11857,.T.);
#17192=ORIENTED_EDGE('',*,*,#11898,.T.);
#17193=ORIENTED_EDGE('',*,*,#12097,.F.);
#17194=ORIENTED_EDGE('',*,*,#12089,.F.);
#17195=ORIENTED_EDGE('',*,*,#12142,.F.);
#17196=ORIENTED_EDGE('',*,*,#12143,.F.);
#17197=ORIENTED_EDGE('',*,*,#12144,.F.);
#17198=ORIENTED_EDGE('',*,*,#12145,.F.);
#17199=ORIENTED_EDGE('',*,*,#12015,.F.);
#17200=ORIENTED_EDGE('',*,*,#12141,.F.);
#17201=ORIENTED_EDGE('',*,*,#12096,.F.);
#17202=ORIENTED_EDGE('',*,*,#12146,.T.);
#17203=ORIENTED_EDGE('',*,*,#12147,.T.);
#17204=ORIENTED_EDGE('',*,*,#11850,.F.);
#17205=ORIENTED_EDGE('',*,*,#12016,.T.);
#17206=ORIENTED_EDGE('',*,*,#12145,.T.);
#17207=ORIENTED_EDGE('',*,*,#12139,.F.);
#17208=ORIENTED_EDGE('',*,*,#12148,.F.);
#17209=ORIENTED_EDGE('',*,*,#11853,.F.);
#17210=ORIENTED_EDGE('',*,*,#11851,.F.);
#17211=ORIENTED_EDGE('',*,*,#12147,.F.);
#17212=ORIENTED_EDGE('',*,*,#12103,.T.);
#17213=ORIENTED_EDGE('',*,*,#12149,.T.);
#17214=ORIENTED_EDGE('',*,*,#12104,.T.);
#17215=ORIENTED_EDGE('',*,*,#12146,.F.);
#17216=ORIENTED_EDGE('',*,*,#12144,.T.);
#17217=ORIENTED_EDGE('',*,*,#12150,.T.);
#17218=ORIENTED_EDGE('',*,*,#12143,.T.);
#17219=ORIENTED_EDGE('',*,*,#12151,.T.);
#17220=ORIENTED_EDGE('',*,*,#12152,.T.);
#17221=ORIENTED_EDGE('',*,*,#12150,.F.);
#17222=ORIENTED_EDGE('',*,*,#12134,.T.);
#17223=ORIENTED_EDGE('',*,*,#12149,.F.);
#17224=ORIENTED_EDGE('',*,*,#12094,.F.);
#17225=ORIENTED_EDGE('',*,*,#12130,.T.);
#17226=ORIENTED_EDGE('',*,*,#12153,.T.);
#17227=ORIENTED_EDGE('',*,*,#12142,.T.);
#17228=ORIENTED_EDGE('',*,*,#12153,.F.);
#17229=ORIENTED_EDGE('',*,*,#12119,.T.);
#17230=ORIENTED_EDGE('',*,*,#12151,.F.);
#17231=ORIENTED_EDGE('',*,*,#12046,.F.);
#17232=ORIENTED_EDGE('',*,*,#12062,.F.);
#17233=ORIENTED_EDGE('',*,*,#12154,.F.);
#17234=ORIENTED_EDGE('',*,*,#12155,.T.);
#17235=ORIENTED_EDGE('',*,*,#12031,.T.);
#17236=ORIENTED_EDGE('',*,*,#12156,.F.);
#17237=ORIENTED_EDGE('',*,*,#12157,.F.);
#17238=ORIENTED_EDGE('',*,*,#12029,.T.);
#17239=ORIENTED_EDGE('',*,*,#11998,.T.);
#17240=ORIENTED_EDGE('',*,*,#12158,.F.);
#17241=ORIENTED_EDGE('',*,*,#12159,.F.);
#17242=ORIENTED_EDGE('',*,*,#12160,.T.);
#17243=ORIENTED_EDGE('',*,*,#12161,.F.);
#17244=ORIENTED_EDGE('',*,*,#12162,.T.);
#17245=ORIENTED_EDGE('',*,*,#12163,.F.);
#17246=ORIENTED_EDGE('',*,*,#12164,.F.);
#17247=ORIENTED_EDGE('',*,*,#12165,.F.);
#17248=ORIENTED_EDGE('',*,*,#12166,.F.);
#17249=ORIENTED_EDGE('',*,*,#12167,.F.);
#17250=ORIENTED_EDGE('',*,*,#12168,.F.);
#17251=ORIENTED_EDGE('',*,*,#12169,.T.);
#17252=ORIENTED_EDGE('',*,*,#12006,.T.);
#17253=ORIENTED_EDGE('',*,*,#11843,.T.);
#17254=ORIENTED_EDGE('',*,*,#11847,.T.);
#17255=ORIENTED_EDGE('',*,*,#11845,.F.);
#17256=ORIENTED_EDGE('',*,*,#12019,.T.);
#17257=ORIENTED_EDGE('',*,*,#12170,.T.);
#17258=ORIENTED_EDGE('',*,*,#12171,.F.);
#17259=ORIENTED_EDGE('',*,*,#12172,.F.);
#17260=ORIENTED_EDGE('',*,*,#12135,.F.);
#17261=ORIENTED_EDGE('',*,*,#12152,.F.);
#17262=ORIENTED_EDGE('',*,*,#12118,.F.);
#17263=ORIENTED_EDGE('',*,*,#12173,.F.);
#17264=ORIENTED_EDGE('',*,*,#12174,.F.);
#17265=ORIENTED_EDGE('',*,*,#12175,.F.);
#17266=ORIENTED_EDGE('',*,*,#12176,.F.);
#17267=ORIENTED_EDGE('',*,*,#12177,.F.);
#17268=ORIENTED_EDGE('',*,*,#12178,.F.);
#17269=ORIENTED_EDGE('',*,*,#12179,.F.);
#17270=ORIENTED_EDGE('',*,*,#12180,.F.);
#17271=ORIENTED_EDGE('',*,*,#12181,.F.);
#17272=ORIENTED_EDGE('',*,*,#12182,.F.);
#17273=ORIENTED_EDGE('',*,*,#12183,.F.);
#17274=ORIENTED_EDGE('',*,*,#12184,.F.);
#17275=ORIENTED_EDGE('',*,*,#12185,.F.);
#17276=ORIENTED_EDGE('',*,*,#12186,.F.);
#17277=ORIENTED_EDGE('',*,*,#11979,.T.);
#17278=ORIENTED_EDGE('',*,*,#12187,.T.);
#17279=ORIENTED_EDGE('',*,*,#12188,.T.);
#17280=ORIENTED_EDGE('',*,*,#12092,.F.);
#17281=ORIENTED_EDGE('',*,*,#12051,.F.);
#17282=ORIENTED_EDGE('',*,*,#12189,.T.);
#17283=ORIENTED_EDGE('',*,*,#12187,.F.);
#17284=ORIENTED_EDGE('',*,*,#11978,.T.);
#17285=ORIENTED_EDGE('',*,*,#12190,.T.);
#17286=ORIENTED_EDGE('',*,*,#12191,.T.);
#17287=ORIENTED_EDGE('',*,*,#12063,.T.);
#17288=ORIENTED_EDGE('',*,*,#12191,.F.);
#17289=ORIENTED_EDGE('',*,*,#12192,.T.);
#17290=ORIENTED_EDGE('',*,*,#12193,.T.);
#17291=ORIENTED_EDGE('',*,*,#12047,.F.);
#17292=ORIENTED_EDGE('',*,*,#12174,.T.);
#17293=ORIENTED_EDGE('',*,*,#12194,.T.);
#17294=ORIENTED_EDGE('',*,*,#12195,.T.);
#17295=ORIENTED_EDGE('',*,*,#12193,.F.);
#17296=ORIENTED_EDGE('',*,*,#12196,.T.);
#17297=ORIENTED_EDGE('',*,*,#12059,.F.);
#17298=ORIENTED_EDGE('',*,*,#12197,.T.);
#17299=ORIENTED_EDGE('',*,*,#12198,.T.);
#17300=ORIENTED_EDGE('',*,*,#12199,.F.);
#17301=ORIENTED_EDGE('',*,*,#11919,.F.);
#17302=ORIENTED_EDGE('',*,*,#12200,.T.);
#17303=ORIENTED_EDGE('',*,*,#12201,.T.);
#17304=ORIENTED_EDGE('',*,*,#12068,.T.);
#17305=ORIENTED_EDGE('',*,*,#11928,.T.);
#17306=ORIENTED_EDGE('',*,*,#12201,.F.);
#17307=ORIENTED_EDGE('',*,*,#12202,.T.);
#17308=ORIENTED_EDGE('',*,*,#12203,.T.);
#17309=ORIENTED_EDGE('',*,*,#12069,.F.);
#17310=ORIENTED_EDGE('',*,*,#11918,.F.);
#17311=ORIENTED_EDGE('',*,*,#12204,.T.);
#17312=ORIENTED_EDGE('',*,*,#12205,.T.);
#17313=ORIENTED_EDGE('',*,*,#12200,.F.);
#17314=ORIENTED_EDGE('',*,*,#12205,.F.);
#17315=ORIENTED_EDGE('',*,*,#12206,.T.);
#17316=ORIENTED_EDGE('',*,*,#12207,.T.);
#17317=ORIENTED_EDGE('',*,*,#12202,.F.);
#17318=ORIENTED_EDGE('',*,*,#12208,.T.);
#17319=ORIENTED_EDGE('',*,*,#12081,.F.);
#17320=ORIENTED_EDGE('',*,*,#12209,.T.);
#17321=ORIENTED_EDGE('',*,*,#12210,.T.);
#17322=ORIENTED_EDGE('',*,*,#11939,.F.);
#17323=ORIENTED_EDGE('',*,*,#12060,.T.);
#17324=ORIENTED_EDGE('',*,*,#11914,.F.);
#17325=ORIENTED_EDGE('',*,*,#12208,.F.);
#17326=ORIENTED_EDGE('',*,*,#11927,.T.);
#17327=ORIENTED_EDGE('',*,*,#12211,.T.);
#17328=ORIENTED_EDGE('',*,*,#12075,.T.);
#17329=ORIENTED_EDGE('',*,*,#11984,.F.);
#17330=ORIENTED_EDGE('',*,*,#12212,.T.);
#17331=ORIENTED_EDGE('',*,*,#11947,.F.);
#17332=ORIENTED_EDGE('',*,*,#11944,.F.);
#17333=ORIENTED_EDGE('',*,*,#12213,.T.);
#17334=ORIENTED_EDGE('',*,*,#12209,.F.);
#17335=ORIENTED_EDGE('',*,*,#12080,.F.);
#17336=ORIENTED_EDGE('',*,*,#12214,.T.);
#17337=ORIENTED_EDGE('',*,*,#11910,.T.);
#17338=ORIENTED_EDGE('',*,*,#11949,.T.);
#17339=ORIENTED_EDGE('',*,*,#12210,.F.);
#17340=ORIENTED_EDGE('',*,*,#12213,.F.);
#17341=ORIENTED_EDGE('',*,*,#11948,.F.);
#17342=ORIENTED_EDGE('',*,*,#11940,.T.);
#17343=ORIENTED_EDGE('',*,*,#12212,.F.);
#17344=ORIENTED_EDGE('',*,*,#11988,.T.);
#17345=ORIENTED_EDGE('',*,*,#12215,.T.);
#17346=ORIENTED_EDGE('',*,*,#11942,.T.);
#17347=ORIENTED_EDGE('',*,*,#12216,.T.);
#17348=ORIENTED_EDGE('',*,*,#11987,.T.);
#17349=ORIENTED_EDGE('',*,*,#12217,.T.);
#17350=ORIENTED_EDGE('',*,*,#12154,.T.);
#17351=ORIENTED_EDGE('',*,*,#12216,.F.);
#17352=ORIENTED_EDGE('',*,*,#12061,.T.);
#17353=ORIENTED_EDGE('',*,*,#12215,.F.);
#17354=ORIENTED_EDGE('',*,*,#12011,.T.);
#17355=ORIENTED_EDGE('',*,*,#12218,.T.);
#17356=ORIENTED_EDGE('',*,*,#12219,.T.);
#17357=ORIENTED_EDGE('',*,*,#11899,.T.);
#17358=ORIENTED_EDGE('',*,*,#11864,.F.);
#17359=ORIENTED_EDGE('',*,*,#12220,.F.);
#17360=ORIENTED_EDGE('',*,*,#12218,.F.);
#17361=ORIENTED_EDGE('',*,*,#12010,.F.);
#17362=ORIENTED_EDGE('',*,*,#12221,.F.);
#17363=ORIENTED_EDGE('',*,*,#12222,.F.);
#17364=ORIENTED_EDGE('',*,*,#12223,.F.);
#17365=ORIENTED_EDGE('',*,*,#12224,.F.);
#17366=ORIENTED_EDGE('',*,*,#12225,.F.);
#17367=ORIENTED_EDGE('',*,*,#12226,.T.);
#17368=ORIENTED_EDGE('',*,*,#12221,.T.);
#17369=ORIENTED_EDGE('',*,*,#12009,.T.);
#17370=ORIENTED_EDGE('',*,*,#11868,.T.);
#17371=ORIENTED_EDGE('',*,*,#12227,.T.);
#17372=ORIENTED_EDGE('',*,*,#12228,.T.);
#17373=ORIENTED_EDGE('',*,*,#12229,.T.);
#17374=ORIENTED_EDGE('',*,*,#12230,.T.);
#17375=ORIENTED_EDGE('',*,*,#12229,.F.);
#17376=ORIENTED_EDGE('',*,*,#12231,.F.);
#17377=ORIENTED_EDGE('',*,*,#12232,.F.);
#17378=ORIENTED_EDGE('',*,*,#12233,.T.);
#17379=ORIENTED_EDGE('',*,*,#12230,.F.);
#17380=ORIENTED_EDGE('',*,*,#12233,.F.);
#17381=ORIENTED_EDGE('',*,*,#12234,.F.);
#17382=ORIENTED_EDGE('',*,*,#12235,.F.);
#17383=ORIENTED_EDGE('',*,*,#12236,.F.);
#17384=ORIENTED_EDGE('',*,*,#12237,.F.);
#17385=ORIENTED_EDGE('',*,*,#12238,.F.);
#17386=ORIENTED_EDGE('',*,*,#12239,.F.);
#17387=ORIENTED_EDGE('',*,*,#12240,.F.);
#17388=ORIENTED_EDGE('',*,*,#12228,.F.);
#17389=ORIENTED_EDGE('',*,*,#12234,.T.);
#17390=ORIENTED_EDGE('',*,*,#12241,.T.);
#17391=ORIENTED_EDGE('',*,*,#12242,.T.);
#17392=ORIENTED_EDGE('',*,*,#12241,.F.);
#17393=ORIENTED_EDGE('',*,*,#12240,.T.);
#17394=ORIENTED_EDGE('',*,*,#12243,.T.);
#17395=ORIENTED_EDGE('',*,*,#12243,.F.);
#17396=ORIENTED_EDGE('',*,*,#12239,.T.);
#17397=ORIENTED_EDGE('',*,*,#12244,.T.);
#17398=ORIENTED_EDGE('',*,*,#12164,.T.);
#17399=ORIENTED_EDGE('',*,*,#12245,.F.);
#17400=ORIENTED_EDGE('',*,*,#12235,.T.);
#17401=ORIENTED_EDGE('',*,*,#12246,.F.);
#17402=ORIENTED_EDGE('',*,*,#12247,.F.);
#17403=ORIENTED_EDGE('',*,*,#12248,.T.);
#17404=ORIENTED_EDGE('',*,*,#12242,.F.);
#17405=ORIENTED_EDGE('',*,*,#12248,.F.);
#17406=ORIENTED_EDGE('',*,*,#12042,.F.);
#17407=ORIENTED_EDGE('',*,*,#12196,.F.);
#17408=ORIENTED_EDGE('',*,*,#12192,.F.);
#17409=ORIENTED_EDGE('',*,*,#12190,.F.);
#17410=ORIENTED_EDGE('',*,*,#12195,.F.);
#17411=ORIENTED_EDGE('',*,*,#12249,.F.);
#17412=ORIENTED_EDGE('',*,*,#12189,.F.);
#17413=ORIENTED_EDGE('',*,*,#12250,.F.);
#17414=ORIENTED_EDGE('',*,*,#12117,.T.);
#17415=ORIENTED_EDGE('',*,*,#12251,.T.);
#17416=ORIENTED_EDGE('',*,*,#12194,.F.);
#17417=ORIENTED_EDGE('',*,*,#12173,.T.);
#17418=ORIENTED_EDGE('',*,*,#12188,.F.);
#17419=ORIENTED_EDGE('',*,*,#12249,.T.);
#17420=ORIENTED_EDGE('',*,*,#12251,.F.);
#17421=ORIENTED_EDGE('',*,*,#12129,.T.);
#17422=ORIENTED_EDGE('',*,*,#12252,.T.);
#17423=ORIENTED_EDGE('',*,*,#11972,.T.);
#17424=ORIENTED_EDGE('',*,*,#12136,.F.);
#17425=ORIENTED_EDGE('',*,*,#12172,.T.);
#17426=ORIENTED_EDGE('',*,*,#12253,.T.);
#17427=ORIENTED_EDGE('',*,*,#12254,.T.);
#17428=ORIENTED_EDGE('',*,*,#12252,.F.);
#17429=ORIENTED_EDGE('',*,*,#12171,.T.);
#17430=ORIENTED_EDGE('',*,*,#12253,.F.);
#17431=ORIENTED_EDGE('',*,*,#12170,.F.);
#17432=ORIENTED_EDGE('',*,*,#12018,.T.);
#17433=ORIENTED_EDGE('',*,*,#12255,.T.);
#17434=ORIENTED_EDGE('',*,*,#12256,.T.);
#17435=ORIENTED_EDGE('',*,*,#12168,.T.);
#17436=ORIENTED_EDGE('',*,*,#12257,.T.);
#17437=ORIENTED_EDGE('',*,*,#12258,.T.);
#17438=ORIENTED_EDGE('',*,*,#12037,.F.);
#17439=ORIENTED_EDGE('',*,*,#11879,.T.);
#17440=ORIENTED_EDGE('',*,*,#11875,.F.);
#17441=ORIENTED_EDGE('',*,*,#12259,.T.);
#17442=ORIENTED_EDGE('',*,*,#11873,.T.);
#17443=ORIENTED_EDGE('',*,*,#11870,.F.);
#17444=ORIENTED_EDGE('',*,*,#12008,.T.);
#17445=ORIENTED_EDGE('',*,*,#12260,.T.);
#17446=ORIENTED_EDGE('',*,*,#12258,.F.);
#17447=ORIENTED_EDGE('',*,*,#12261,.T.);
#17448=ORIENTED_EDGE('',*,*,#12262,.T.);
#17449=ORIENTED_EDGE('',*,*,#12263,.T.);
#17450=ORIENTED_EDGE('',*,*,#12257,.F.);
#17451=ORIENTED_EDGE('',*,*,#12167,.T.);
#17452=ORIENTED_EDGE('',*,*,#12263,.F.);
#17453=ORIENTED_EDGE('',*,*,#12264,.T.);
#17454=ORIENTED_EDGE('',*,*,#12265,.F.);
#17455=ORIENTED_EDGE('',*,*,#12266,.F.);
#17456=ORIENTED_EDGE('',*,*,#12038,.T.);
#17457=ORIENTED_EDGE('',*,*,#12261,.F.);
#17458=ORIENTED_EDGE('',*,*,#12267,.T.);
#17459=ORIENTED_EDGE('',*,*,#12268,.T.);
#17460=ORIENTED_EDGE('',*,*,#12245,.T.);
#17461=ORIENTED_EDGE('',*,*,#12163,.T.);
#17462=ORIENTED_EDGE('',*,*,#12268,.F.);
#17463=ORIENTED_EDGE('',*,*,#12269,.T.);
#17464=ORIENTED_EDGE('',*,*,#12270,.F.);
#17465=ORIENTED_EDGE('',*,*,#12236,.T.);
#17466=ORIENTED_EDGE('',*,*,#12271,.T.);
#17467=ORIENTED_EDGE('',*,*,#12272,.T.);
#17468=ORIENTED_EDGE('',*,*,#12273,.T.);
#17469=ORIENTED_EDGE('',*,*,#12178,.T.);
#17470=ORIENTED_EDGE('',*,*,#12272,.F.);
#17471=ORIENTED_EDGE('',*,*,#12274,.T.);
#17472=ORIENTED_EDGE('',*,*,#12275,.T.);
#17473=ORIENTED_EDGE('',*,*,#12276,.T.);
#17474=ORIENTED_EDGE('',*,*,#12277,.T.);
#17475=ORIENTED_EDGE('',*,*,#12278,.F.);
#17476=ORIENTED_EDGE('',*,*,#12279,.T.);
#17477=ORIENTED_EDGE('',*,*,#12280,.T.);
#17478=ORIENTED_EDGE('',*,*,#12281,.T.);
#17479=ORIENTED_EDGE('',*,*,#12176,.T.);
#17480=ORIENTED_EDGE('',*,*,#12280,.F.);
#17481=ORIENTED_EDGE('',*,*,#12282,.T.);
#17482=ORIENTED_EDGE('',*,*,#12283,.T.);
#17483=ORIENTED_EDGE('',*,*,#12284,.T.);
#17484=ORIENTED_EDGE('',*,*,#12285,.T.);
#17485=ORIENTED_EDGE('',*,*,#12286,.F.);
#17486=ORIENTED_EDGE('',*,*,#12287,.T.);
#17487=ORIENTED_EDGE('',*,*,#12288,.T.);
#17488=ORIENTED_EDGE('',*,*,#12289,.T.);
#17489=ORIENTED_EDGE('',*,*,#12184,.T.);
#17490=ORIENTED_EDGE('',*,*,#12288,.F.);
#17491=ORIENTED_EDGE('',*,*,#12290,.T.);
#17492=ORIENTED_EDGE('',*,*,#12291,.T.);
#17493=ORIENTED_EDGE('',*,*,#12292,.T.);
#17494=ORIENTED_EDGE('',*,*,#12293,.T.);
#17495=ORIENTED_EDGE('',*,*,#12294,.F.);
#17496=ORIENTED_EDGE('',*,*,#12295,.T.);
#17497=ORIENTED_EDGE('',*,*,#12296,.T.);
#17498=ORIENTED_EDGE('',*,*,#12180,.T.);
#17499=ORIENTED_EDGE('',*,*,#12297,.T.);
#17500=ORIENTED_EDGE('',*,*,#12298,.T.);
#17501=ORIENTED_EDGE('',*,*,#12299,.T.);
#17502=ORIENTED_EDGE('',*,*,#12182,.T.);
#17503=ORIENTED_EDGE('',*,*,#12298,.F.);
#17504=ORIENTED_EDGE('',*,*,#12300,.T.);
#17505=ORIENTED_EDGE('',*,*,#12301,.T.);
#17506=ORIENTED_EDGE('',*,*,#12302,.T.);
#17507=ORIENTED_EDGE('',*,*,#12303,.T.);
#17508=ORIENTED_EDGE('',*,*,#12304,.F.);
#17509=ORIENTED_EDGE('',*,*,#12295,.F.);
#17510=ORIENTED_EDGE('',*,*,#12181,.T.);
#17511=ORIENTED_EDGE('',*,*,#12296,.F.);
#17512=ORIENTED_EDGE('',*,*,#12305,.T.);
#17513=ORIENTED_EDGE('',*,*,#12306,.T.);
#17514=ORIENTED_EDGE('',*,*,#12307,.T.);
#17515=ORIENTED_EDGE('',*,*,#12305,.F.);
#17516=ORIENTED_EDGE('',*,*,#12308,.T.);
#17517=ORIENTED_EDGE('',*,*,#12297,.F.);
#17518=ORIENTED_EDGE('',*,*,#12179,.T.);
#17519=ORIENTED_EDGE('',*,*,#12289,.F.);
#17520=ORIENTED_EDGE('',*,*,#12308,.F.);
#17521=ORIENTED_EDGE('',*,*,#12294,.T.);
#17522=ORIENTED_EDGE('',*,*,#12309,.T.);
#17523=ORIENTED_EDGE('',*,*,#12300,.F.);
#17524=ORIENTED_EDGE('',*,*,#12310,.T.);
#17525=ORIENTED_EDGE('',*,*,#12287,.F.);
#17526=ORIENTED_EDGE('',*,*,#12183,.T.);
#17527=ORIENTED_EDGE('',*,*,#12299,.F.);
#17528=ORIENTED_EDGE('',*,*,#12310,.F.);
#17529=ORIENTED_EDGE('',*,*,#12304,.T.);
#17530=ORIENTED_EDGE('',*,*,#12311,.T.);
#17531=ORIENTED_EDGE('',*,*,#12290,.F.);
#17532=ORIENTED_EDGE('',*,*,#12312,.T.);
#17533=ORIENTED_EDGE('',*,*,#12279,.F.);
#17534=ORIENTED_EDGE('',*,*,#12175,.T.);
#17535=ORIENTED_EDGE('',*,*,#12273,.F.);
#17536=ORIENTED_EDGE('',*,*,#12312,.F.);
#17537=ORIENTED_EDGE('',*,*,#12278,.T.);
#17538=ORIENTED_EDGE('',*,*,#12313,.T.);
#17539=ORIENTED_EDGE('',*,*,#12282,.F.);
#17540=ORIENTED_EDGE('',*,*,#12314,.T.);
#17541=ORIENTED_EDGE('',*,*,#12271,.F.);
#17542=ORIENTED_EDGE('',*,*,#12177,.T.);
#17543=ORIENTED_EDGE('',*,*,#12281,.F.);
#17544=ORIENTED_EDGE('',*,*,#12314,.F.);
#17545=ORIENTED_EDGE('',*,*,#12286,.T.);
#17546=ORIENTED_EDGE('',*,*,#12315,.T.);
#17547=ORIENTED_EDGE('',*,*,#12274,.F.);
#17548=ORIENTED_EDGE('',*,*,#12186,.T.);
#17549=ORIENTED_EDGE('',*,*,#12316,.T.);
#17550=ORIENTED_EDGE('',*,*,#12317,.T.);
#17551=ORIENTED_EDGE('',*,*,#12318,.T.);
#17552=ORIENTED_EDGE('',*,*,#12316,.F.);
#17553=ORIENTED_EDGE('',*,*,#12318,.F.);
#17554=ORIENTED_EDGE('',*,*,#12319,.T.);
#17555=ORIENTED_EDGE('',*,*,#12320,.T.);
#17556=ORIENTED_EDGE('',*,*,#12319,.F.);
#17557=ORIENTED_EDGE('',*,*,#12317,.F.);
#17558=ORIENTED_EDGE('',*,*,#12185,.T.);
#17559=ORIENTED_EDGE('',*,*,#12321,.T.);
#17560=ORIENTED_EDGE('',*,*,#12322,.T.);
#17561=ORIENTED_EDGE('',*,*,#12323,.T.);
#17562=ORIENTED_EDGE('',*,*,#12321,.F.);
#17563=ORIENTED_EDGE('',*,*,#12323,.F.);
#17564=ORIENTED_EDGE('',*,*,#12324,.T.);
#17565=ORIENTED_EDGE('',*,*,#12325,.T.);
#17566=ORIENTED_EDGE('',*,*,#12324,.F.);
#17567=ORIENTED_EDGE('',*,*,#12322,.F.);
#17568=ORIENTED_EDGE('',*,*,#12307,.F.);
#17569=ORIENTED_EDGE('',*,*,#12326,.T.);
#17570=ORIENTED_EDGE('',*,*,#12327,.T.);
#17571=ORIENTED_EDGE('',*,*,#12326,.F.);
#17572=ORIENTED_EDGE('',*,*,#12306,.F.);
#17573=ORIENTED_EDGE('',*,*,#12328,.T.);
#17574=ORIENTED_EDGE('',*,*,#12329,.T.);
#17575=ORIENTED_EDGE('',*,*,#12156,.T.);
#17576=ORIENTED_EDGE('',*,*,#12030,.T.);
#17577=ORIENTED_EDGE('',*,*,#12157,.T.);
#17578=ORIENTED_EDGE('',*,*,#12329,.F.);
#17579=ORIENTED_EDGE('',*,*,#12330,.T.);
#17580=ORIENTED_EDGE('',*,*,#12331,.T.);
#17581=ORIENTED_EDGE('',*,*,#12246,.T.);
#17582=ORIENTED_EDGE('',*,*,#12247,.T.);
#17583=ORIENTED_EDGE('',*,*,#12331,.F.);
#17584=ORIENTED_EDGE('',*,*,#12332,.T.);
#17585=ORIENTED_EDGE('',*,*,#12333,.T.);
#17586=ORIENTED_EDGE('',*,*,#12333,.F.);
#17587=ORIENTED_EDGE('',*,*,#12334,.T.);
#17588=ORIENTED_EDGE('',*,*,#12262,.F.);
#17589=ORIENTED_EDGE('',*,*,#12166,.T.);
#17590=ORIENTED_EDGE('',*,*,#12335,.F.);
#17591=ORIENTED_EDGE('',*,*,#12336,.T.);
#17592=ORIENTED_EDGE('',*,*,#12337,.T.);
#17593=ORIENTED_EDGE('',*,*,#12338,.T.);
#17594=ORIENTED_EDGE('',*,*,#12231,.T.);
#17595=ORIENTED_EDGE('',*,*,#12232,.T.);
#17596=ORIENTED_EDGE('',*,*,#12338,.F.);
#17597=ORIENTED_EDGE('',*,*,#12330,.F.);
#17598=ORIENTED_EDGE('',*,*,#12336,.F.);
#17599=ORIENTED_EDGE('',*,*,#12339,.F.);
#17600=ORIENTED_EDGE('',*,*,#12340,.T.);
#17601=ORIENTED_EDGE('',*,*,#11877,.F.);
#17602=ORIENTED_EDGE('',*,*,#11881,.T.);
#17603=ORIENTED_EDGE('',*,*,#11884,.F.);
#17604=ORIENTED_EDGE('',*,*,#11900,.T.);
#17605=ORIENTED_EDGE('',*,*,#12341,.F.);
#17606=ORIENTED_EDGE('',*,*,#12342,.F.);
#17607=ORIENTED_EDGE('',*,*,#12264,.F.);
#17608=ORIENTED_EDGE('',*,*,#12334,.F.);
#17609=ORIENTED_EDGE('',*,*,#12332,.F.);
#17610=ORIENTED_EDGE('',*,*,#12337,.F.);
#17611=ORIENTED_EDGE('',*,*,#12343,.T.);
#17612=ORIENTED_EDGE('',*,*,#12223,.T.);
#17613=ORIENTED_EDGE('',*,*,#12344,.T.);
#17614=ORIENTED_EDGE('',*,*,#12165,.T.);
#17615=ORIENTED_EDGE('',*,*,#12345,.T.);
#17616=ORIENTED_EDGE('',*,*,#12222,.T.);
#17617=ORIENTED_EDGE('',*,*,#12226,.F.);
#17618=ORIENTED_EDGE('',*,*,#12339,.T.);
#17619=ORIENTED_EDGE('',*,*,#12345,.F.);
#17620=ORIENTED_EDGE('',*,*,#12335,.T.);
#17621=ORIENTED_EDGE('',*,*,#12344,.F.);
#17622=ORIENTED_EDGE('',*,*,#12244,.F.);
#17623=ORIENTED_EDGE('',*,*,#12346,.T.);
#17624=ORIENTED_EDGE('',*,*,#12343,.F.);
#17625=ORIENTED_EDGE('',*,*,#12346,.F.);
#17626=ORIENTED_EDGE('',*,*,#12238,.T.);
#17627=ORIENTED_EDGE('',*,*,#12347,.T.);
#17628=ORIENTED_EDGE('',*,*,#12224,.T.);
#17629=ORIENTED_EDGE('',*,*,#12348,.T.);
#17630=ORIENTED_EDGE('',*,*,#12349,.T.);
#17631=ORIENTED_EDGE('',*,*,#12350,.T.);
#17632=ORIENTED_EDGE('',*,*,#12342,.T.);
#17633=ORIENTED_EDGE('',*,*,#12351,.T.);
#17634=ORIENTED_EDGE('',*,*,#12341,.T.);
#17635=ORIENTED_EDGE('',*,*,#12219,.F.);
#17636=ORIENTED_EDGE('',*,*,#12220,.T.);
#17637=ORIENTED_EDGE('',*,*,#12351,.F.);
#17638=ORIENTED_EDGE('',*,*,#12352,.T.);
#17639=ORIENTED_EDGE('',*,*,#12348,.F.);
#17640=ORIENTED_EDGE('',*,*,#12353,.F.);
#17641=ORIENTED_EDGE('',*,*,#12349,.F.);
#17642=ORIENTED_EDGE('',*,*,#12354,.F.);
#17643=ORIENTED_EDGE('',*,*,#12355,.F.);
#17644=ORIENTED_EDGE('',*,*,#12356,.F.);
#17645=ORIENTED_EDGE('',*,*,#12357,.T.);
#17646=ORIENTED_EDGE('',*,*,#12358,.F.);
#17647=ORIENTED_EDGE('',*,*,#12359,.T.);
#17648=ORIENTED_EDGE('',*,*,#12360,.F.);
#17649=ORIENTED_EDGE('',*,*,#12361,.F.);
#17650=ORIENTED_EDGE('',*,*,#12362,.F.);
#17651=ORIENTED_EDGE('',*,*,#12352,.F.);
#17652=ORIENTED_EDGE('',*,*,#12225,.T.);
#17653=ORIENTED_EDGE('',*,*,#12363,.F.);
#17654=ORIENTED_EDGE('',*,*,#12354,.T.);
#17655=ORIENTED_EDGE('',*,*,#12364,.T.);
#17656=ORIENTED_EDGE('',*,*,#12365,.T.);
#17657=ORIENTED_EDGE('',*,*,#11994,.F.);
#17658=ORIENTED_EDGE('',*,*,#11888,.T.);
#17659=ORIENTED_EDGE('',*,*,#12366,.T.);
#17660=ORIENTED_EDGE('',*,*,#12367,.T.);
#17661=ORIENTED_EDGE('',*,*,#12368,.T.);
#17662=ORIENTED_EDGE('',*,*,#12369,.T.);
#17663=ORIENTED_EDGE('',*,*,#12362,.T.);
#17664=ORIENTED_EDGE('',*,*,#12370,.T.);
#17665=ORIENTED_EDGE('',*,*,#12371,.T.);
#17666=ORIENTED_EDGE('',*,*,#11886,.T.);
#17667=ORIENTED_EDGE('',*,*,#12036,.T.);
#17668=ORIENTED_EDGE('',*,*,#12266,.T.);
#17669=ORIENTED_EDGE('',*,*,#12370,.F.);
#17670=ORIENTED_EDGE('',*,*,#12372,.T.);
#17671=ORIENTED_EDGE('',*,*,#12369,.F.);
#17672=ORIENTED_EDGE('',*,*,#12367,.F.);
#17673=ORIENTED_EDGE('',*,*,#12373,.T.);
#17674=ORIENTED_EDGE('',*,*,#12364,.F.);
#17675=ORIENTED_EDGE('',*,*,#12365,.F.);
#17676=ORIENTED_EDGE('',*,*,#12374,.F.);
#17677=ORIENTED_EDGE('',*,*,#12375,.F.);
#17678=ORIENTED_EDGE('',*,*,#12376,.F.);
#17679=ORIENTED_EDGE('',*,*,#11996,.F.);
#17680=ORIENTED_EDGE('',*,*,#11992,.F.);
#17681=ORIENTED_EDGE('',*,*,#12373,.F.);
#17682=ORIENTED_EDGE('',*,*,#12361,.T.);
#17683=ORIENTED_EDGE('',*,*,#12377,.T.);
#17684=ORIENTED_EDGE('',*,*,#12374,.T.);
#17685=ORIENTED_EDGE('',*,*,#12372,.F.);
#17686=ORIENTED_EDGE('',*,*,#12265,.T.);
#17687=ORIENTED_EDGE('',*,*,#12350,.F.);
#17688=ORIENTED_EDGE('',*,*,#12353,.T.);
#17689=ORIENTED_EDGE('',*,*,#12378,.T.);
#17690=ORIENTED_EDGE('',*,*,#12237,.T.);
#17691=ORIENTED_EDGE('',*,*,#12379,.T.);
#17692=ORIENTED_EDGE('',*,*,#12355,.T.);
#17693=ORIENTED_EDGE('',*,*,#12378,.F.);
#17694=ORIENTED_EDGE('',*,*,#12363,.T.);
#17695=ORIENTED_EDGE('',*,*,#12347,.F.);
#17696=ORIENTED_EDGE('',*,*,#12380,.T.);
#17697=ORIENTED_EDGE('',*,*,#12381,.T.);
#17698=ORIENTED_EDGE('',*,*,#12382,.T.);
#17699=ORIENTED_EDGE('',*,*,#12383,.T.);
#17700=ORIENTED_EDGE('',*,*,#12381,.F.);
#17701=ORIENTED_EDGE('',*,*,#12383,.F.);
#17702=ORIENTED_EDGE('',*,*,#12384,.T.);
#17703=ORIENTED_EDGE('',*,*,#12385,.F.);
#17704=ORIENTED_EDGE('',*,*,#12386,.F.);
#17705=ORIENTED_EDGE('',*,*,#12387,.T.);
#17706=ORIENTED_EDGE('',*,*,#12388,.T.);
#17707=ORIENTED_EDGE('',*,*,#12389,.T.);
#17708=ORIENTED_EDGE('',*,*,#12390,.F.);
#17709=ORIENTED_EDGE('',*,*,#12391,.F.);
#17710=ORIENTED_EDGE('',*,*,#12392,.T.);
#17711=ORIENTED_EDGE('',*,*,#12393,.T.);
#17712=ORIENTED_EDGE('',*,*,#12394,.T.);
#17713=ORIENTED_EDGE('',*,*,#12395,.F.);
#17714=ORIENTED_EDGE('',*,*,#12396,.F.);
#17715=ORIENTED_EDGE('',*,*,#12397,.T.);
#17716=ORIENTED_EDGE('',*,*,#12398,.T.);
#17717=ORIENTED_EDGE('',*,*,#12399,.T.);
#17718=ORIENTED_EDGE('',*,*,#12400,.F.);
#17719=ORIENTED_EDGE('',*,*,#12384,.F.);
#17720=ORIENTED_EDGE('',*,*,#12382,.F.);
#17721=ORIENTED_EDGE('',*,*,#12401,.F.);
#17722=ORIENTED_EDGE('',*,*,#12357,.F.);
#17723=ORIENTED_EDGE('',*,*,#12402,.F.);
#17724=ORIENTED_EDGE('',*,*,#12269,.F.);
#17725=ORIENTED_EDGE('',*,*,#12267,.F.);
#17726=ORIENTED_EDGE('',*,*,#12162,.F.);
#17727=ORIENTED_EDGE('',*,*,#12403,.F.);
#17728=ORIENTED_EDGE('',*,*,#12380,.F.);
#17729=ORIENTED_EDGE('',*,*,#12402,.T.);
#17730=ORIENTED_EDGE('',*,*,#12356,.T.);
#17731=ORIENTED_EDGE('',*,*,#12379,.F.);
#17732=ORIENTED_EDGE('',*,*,#12270,.T.);
#17733=ORIENTED_EDGE('',*,*,#12366,.F.);
#17734=ORIENTED_EDGE('',*,*,#11887,.F.);
#17735=ORIENTED_EDGE('',*,*,#12371,.F.);
#17736=ORIENTED_EDGE('',*,*,#12368,.F.);
#17737=ORIENTED_EDGE('',*,*,#12404,.T.);
#17738=ORIENTED_EDGE('',*,*,#12405,.T.);
#17739=ORIENTED_EDGE('',*,*,#12385,.T.);
#17740=ORIENTED_EDGE('',*,*,#12400,.T.);
#17741=ORIENTED_EDGE('',*,*,#12406,.T.);
#17742=ORIENTED_EDGE('',*,*,#12407,.T.);
#17743=ORIENTED_EDGE('',*,*,#12406,.F.);
#17744=ORIENTED_EDGE('',*,*,#12399,.F.);
#17745=ORIENTED_EDGE('',*,*,#12408,.T.);
#17746=ORIENTED_EDGE('',*,*,#12409,.F.);
#17747=ORIENTED_EDGE('',*,*,#12405,.F.);
#17748=ORIENTED_EDGE('',*,*,#12410,.F.);
#17749=ORIENTED_EDGE('',*,*,#12411,.F.);
#17750=ORIENTED_EDGE('',*,*,#12390,.T.);
#17751=ORIENTED_EDGE('',*,*,#12412,.T.);
#17752=ORIENTED_EDGE('',*,*,#12413,.T.);
#17753=ORIENTED_EDGE('',*,*,#12386,.T.);
#17754=ORIENTED_EDGE('',*,*,#12414,.T.);
#17755=ORIENTED_EDGE('',*,*,#12415,.F.);
#17756=ORIENTED_EDGE('',*,*,#12416,.T.);
#17757=ORIENTED_EDGE('',*,*,#12417,.F.);
#17758=ORIENTED_EDGE('',*,*,#12418,.T.);
#17759=ORIENTED_EDGE('',*,*,#12419,.T.);
#17760=ORIENTED_EDGE('',*,*,#12420,.T.);
#17761=ORIENTED_EDGE('',*,*,#12421,.F.);
#17762=ORIENTED_EDGE('',*,*,#12422,.T.);
#17763=ORIENTED_EDGE('',*,*,#12423,.T.);
#17764=ORIENTED_EDGE('',*,*,#12424,.F.);
#17765=ORIENTED_EDGE('',*,*,#12420,.F.);
#17766=ORIENTED_EDGE('',*,*,#12425,.T.);
#17767=ORIENTED_EDGE('',*,*,#12426,.F.);
#17768=ORIENTED_EDGE('',*,*,#12360,.T.);
#17769=ORIENTED_EDGE('',*,*,#12427,.T.);
#17770=ORIENTED_EDGE('',*,*,#12415,.T.);
#17771=ORIENTED_EDGE('',*,*,#12428,.T.);
#17772=ORIENTED_EDGE('',*,*,#12429,.T.);
#17773=ORIENTED_EDGE('',*,*,#12430,.T.);
#17774=ORIENTED_EDGE('',*,*,#12431,.T.);
#17775=ORIENTED_EDGE('',*,*,#12432,.T.);
#17776=ORIENTED_EDGE('',*,*,#12433,.T.);
#17777=ORIENTED_EDGE('',*,*,#12434,.T.);
#17778=ORIENTED_EDGE('',*,*,#12419,.F.);
#17779=ORIENTED_EDGE('',*,*,#12435,.F.);
#17780=ORIENTED_EDGE('',*,*,#12436,.F.);
#17781=ORIENTED_EDGE('',*,*,#12425,.F.);
#17782=ORIENTED_EDGE('',*,*,#12437,.T.);
#17783=ORIENTED_EDGE('',*,*,#12438,.F.);
#17784=ORIENTED_EDGE('',*,*,#12439,.T.);
#17785=ORIENTED_EDGE('',*,*,#12440,.F.);
#17786=ORIENTED_EDGE('',*,*,#12441,.T.);
#17787=ORIENTED_EDGE('',*,*,#12434,.F.);
#17788=ORIENTED_EDGE('',*,*,#12442,.T.);
#17789=ORIENTED_EDGE('',*,*,#12443,.T.);
#17790=ORIENTED_EDGE('',*,*,#12444,.F.);
#17791=ORIENTED_EDGE('',*,*,#12445,.T.);
#17792=ORIENTED_EDGE('',*,*,#12446,.F.);
#17793=ORIENTED_EDGE('',*,*,#12447,.T.);
#17794=ORIENTED_EDGE('',*,*,#12421,.T.);
#17795=ORIENTED_EDGE('',*,*,#12424,.T.);
#17796=ORIENTED_EDGE('',*,*,#12441,.F.);
#17797=ORIENTED_EDGE('',*,*,#12448,.T.);
#17798=ORIENTED_EDGE('',*,*,#12449,.T.);
#17799=ORIENTED_EDGE('',*,*,#12450,.T.);
#17800=ORIENTED_EDGE('',*,*,#12451,.T.);
#17801=ORIENTED_EDGE('',*,*,#12452,.F.);
#17802=ORIENTED_EDGE('',*,*,#12453,.T.);
#17803=ORIENTED_EDGE('',*,*,#12454,.T.);
#17804=ORIENTED_EDGE('',*,*,#12396,.T.);
#17805=ORIENTED_EDGE('',*,*,#12455,.T.);
#17806=ORIENTED_EDGE('',*,*,#12456,.T.);
#17807=ORIENTED_EDGE('',*,*,#12438,.T.);
#17808=ORIENTED_EDGE('',*,*,#12445,.F.);
#17809=ORIENTED_EDGE('',*,*,#12457,.T.);
#17810=ORIENTED_EDGE('',*,*,#12429,.F.);
#17811=ORIENTED_EDGE('',*,*,#12458,.T.);
#17812=ORIENTED_EDGE('',*,*,#12459,.T.);
#17813=ORIENTED_EDGE('',*,*,#12453,.F.);
#17814=ORIENTED_EDGE('',*,*,#12451,.F.);
#17815=ORIENTED_EDGE('',*,*,#12460,.T.);
#17816=ORIENTED_EDGE('',*,*,#12430,.F.);
#17817=ORIENTED_EDGE('',*,*,#12457,.F.);
#17818=ORIENTED_EDGE('',*,*,#12450,.F.);
#17819=ORIENTED_EDGE('',*,*,#12461,.F.);
#17820=ORIENTED_EDGE('',*,*,#12462,.T.);
#17821=ORIENTED_EDGE('',*,*,#12463,.T.);
#17822=ORIENTED_EDGE('',*,*,#12464,.F.);
#17823=ORIENTED_EDGE('',*,*,#12465,.F.);
#17824=ORIENTED_EDGE('',*,*,#12431,.F.);
#17825=ORIENTED_EDGE('',*,*,#12460,.F.);
#17826=ORIENTED_EDGE('',*,*,#12449,.F.);
#17827=ORIENTED_EDGE('',*,*,#12466,.T.);
#17828=ORIENTED_EDGE('',*,*,#12467,.T.);
#17829=ORIENTED_EDGE('',*,*,#12461,.T.);
#17830=ORIENTED_EDGE('',*,*,#12456,.F.);
#17831=ORIENTED_EDGE('',*,*,#12468,.F.);
#17832=ORIENTED_EDGE('',*,*,#12469,.T.);
#17833=ORIENTED_EDGE('',*,*,#12470,.T.);
#17834=ORIENTED_EDGE('',*,*,#12471,.F.);
#17835=ORIENTED_EDGE('',*,*,#12472,.F.);
#17836=ORIENTED_EDGE('',*,*,#12473,.F.);
#17837=ORIENTED_EDGE('',*,*,#12439,.F.);
#17838=ORIENTED_EDGE('',*,*,#12455,.F.);
#17839=ORIENTED_EDGE('',*,*,#12395,.T.);
#17840=ORIENTED_EDGE('',*,*,#12474,.T.);
#17841=ORIENTED_EDGE('',*,*,#12468,.T.);
#17842=ORIENTED_EDGE('',*,*,#12475,.T.);
#17843=ORIENTED_EDGE('',*,*,#12158,.T.);
#17844=ORIENTED_EDGE('',*,*,#11997,.T.);
#17845=ORIENTED_EDGE('',*,*,#12376,.T.);
#17846=ORIENTED_EDGE('',*,*,#12476,.T.);
#17847=ORIENTED_EDGE('',*,*,#12436,.T.);
#17848=ORIENTED_EDGE('',*,*,#12477,.T.);
#17849=ORIENTED_EDGE('',*,*,#12375,.T.);
#17850=ORIENTED_EDGE('',*,*,#12477,.F.);
#17851=ORIENTED_EDGE('',*,*,#12478,.T.);
#17852=ORIENTED_EDGE('',*,*,#12475,.F.);
#17853=ORIENTED_EDGE('',*,*,#12377,.F.);
#17854=ORIENTED_EDGE('',*,*,#12426,.T.);
#17855=ORIENTED_EDGE('',*,*,#12476,.F.);
#17856=ORIENTED_EDGE('',*,*,#12479,.F.);
#17857=ORIENTED_EDGE('',*,*,#12417,.T.);
#17858=ORIENTED_EDGE('',*,*,#12480,.T.);
#17859=ORIENTED_EDGE('',*,*,#12159,.T.);
#17860=ORIENTED_EDGE('',*,*,#12478,.F.);
#17861=ORIENTED_EDGE('',*,*,#12435,.T.);
#17862=ORIENTED_EDGE('',*,*,#12418,.F.);
#17863=ORIENTED_EDGE('',*,*,#12481,.F.);
#17864=ORIENTED_EDGE('',*,*,#12440,.T.);
#17865=ORIENTED_EDGE('',*,*,#12473,.T.);
#17866=ORIENTED_EDGE('',*,*,#12482,.T.);
#17867=ORIENTED_EDGE('',*,*,#12483,.T.);
#17868=ORIENTED_EDGE('',*,*,#12410,.T.);
#17869=ORIENTED_EDGE('',*,*,#12404,.F.);
#17870=ORIENTED_EDGE('',*,*,#12161,.T.);
#17871=ORIENTED_EDGE('',*,*,#12484,.T.);
#17872=ORIENTED_EDGE('',*,*,#12358,.T.);
#17873=ORIENTED_EDGE('',*,*,#12401,.T.);
#17874=ORIENTED_EDGE('',*,*,#12484,.F.);
#17875=ORIENTED_EDGE('',*,*,#12160,.F.);
#17876=ORIENTED_EDGE('',*,*,#12480,.F.);
#17877=ORIENTED_EDGE('',*,*,#12416,.F.);
#17878=ORIENTED_EDGE('',*,*,#12427,.F.);
#17879=ORIENTED_EDGE('',*,*,#12359,.F.);
#17880=ORIENTED_EDGE('',*,*,#12250,.T.);
#17881=ORIENTED_EDGE('',*,*,#12485,.T.);
#17882=ORIENTED_EDGE('',*,*,#12082,.T.);
#17883=ORIENTED_EDGE('',*,*,#12485,.F.);
#17884=ORIENTED_EDGE('',*,*,#12486,.T.);
#17885=ORIENTED_EDGE('',*,*,#12487,.T.);
#17886=ORIENTED_EDGE('',*,*,#12488,.T.);
#17887=ORIENTED_EDGE('',*,*,#12084,.T.);
#17888=ORIENTED_EDGE('',*,*,#12087,.T.);
#17889=ORIENTED_EDGE('',*,*,#12487,.F.);
#17890=ORIENTED_EDGE('',*,*,#12489,.F.);
#17891=ORIENTED_EDGE('',*,*,#11923,.F.);
#17892=ORIENTED_EDGE('',*,*,#12490,.F.);
#17893=ORIENTED_EDGE('',*,*,#12491,.F.);
#17894=ORIENTED_EDGE('',*,*,#12214,.F.);
#17895=ORIENTED_EDGE('',*,*,#12492,.T.);
#17896=ORIENTED_EDGE('',*,*,#12490,.T.);
#17897=ORIENTED_EDGE('',*,*,#11922,.F.);
#17898=ORIENTED_EDGE('',*,*,#12079,.F.);
#17899=ORIENTED_EDGE('',*,*,#12085,.F.);
#17900=ORIENTED_EDGE('',*,*,#12488,.F.);
#17901=ORIENTED_EDGE('',*,*,#12491,.T.);
#17902=ORIENTED_EDGE('',*,*,#12492,.F.);
#17903=ORIENTED_EDGE('',*,*,#12077,.F.);
#17904=ORIENTED_EDGE('',*,*,#11924,.T.);
#17905=ORIENTED_EDGE('',*,*,#12489,.T.);
#17906=ORIENTED_EDGE('',*,*,#12486,.F.);
#17907=ORIENTED_EDGE('',*,*,#12086,.F.);
#17908=ORIENTED_EDGE('',*,*,#12483,.F.);
#17909=ORIENTED_EDGE('',*,*,#12493,.F.);
#17910=ORIENTED_EDGE('',*,*,#12391,.T.);
#17911=ORIENTED_EDGE('',*,*,#12411,.T.);
#17912=ORIENTED_EDGE('',*,*,#12482,.F.);
#17913=ORIENTED_EDGE('',*,*,#12472,.T.);
#17914=ORIENTED_EDGE('',*,*,#12494,.T.);
#17915=ORIENTED_EDGE('',*,*,#12493,.T.);
#17916=ORIENTED_EDGE('',*,*,#12433,.F.);
#17917=ORIENTED_EDGE('',*,*,#12495,.F.);
#17918=ORIENTED_EDGE('',*,*,#12496,.T.);
#17919=ORIENTED_EDGE('',*,*,#12497,.T.);
#17920=ORIENTED_EDGE('',*,*,#12498,.F.);
#17921=ORIENTED_EDGE('',*,*,#12499,.F.);
#17922=ORIENTED_EDGE('',*,*,#12442,.F.);
#17923=ORIENTED_EDGE('',*,*,#12432,.F.);
#17924=ORIENTED_EDGE('',*,*,#12465,.T.);
#17925=ORIENTED_EDGE('',*,*,#12500,.T.);
#17926=ORIENTED_EDGE('',*,*,#12495,.T.);
#17927=ORIENTED_EDGE('',*,*,#12459,.F.);
#17928=ORIENTED_EDGE('',*,*,#12501,.T.);
#17929=ORIENTED_EDGE('',*,*,#12502,.T.);
#17930=ORIENTED_EDGE('',*,*,#12503,.F.);
#17931=ORIENTED_EDGE('',*,*,#12428,.F.);
#17932=ORIENTED_EDGE('',*,*,#12414,.F.);
#17933=ORIENTED_EDGE('',*,*,#12479,.T.);
#17934=ORIENTED_EDGE('',*,*,#12407,.F.);
#17935=ORIENTED_EDGE('',*,*,#12504,.T.);
#17936=ORIENTED_EDGE('',*,*,#12458,.F.);
#17937=ORIENTED_EDGE('',*,*,#12504,.F.);
#17938=ORIENTED_EDGE('',*,*,#12409,.T.);
#17939=ORIENTED_EDGE('',*,*,#12505,.T.);
#17940=ORIENTED_EDGE('',*,*,#12501,.F.);
#17941=ORIENTED_EDGE('',*,*,#12506,.T.);
#17942=ORIENTED_EDGE('',*,*,#12446,.T.);
#17943=ORIENTED_EDGE('',*,*,#12452,.T.);
#17944=ORIENTED_EDGE('',*,*,#12437,.F.);
#17945=ORIENTED_EDGE('',*,*,#12481,.T.);
#17946=ORIENTED_EDGE('',*,*,#12423,.F.);
#17947=ORIENTED_EDGE('',*,*,#12506,.F.);
#17948=ORIENTED_EDGE('',*,*,#12507,.T.);
#17949=ORIENTED_EDGE('',*,*,#12508,.T.);
#17950=ORIENTED_EDGE('',*,*,#12509,.F.);
#17951=ORIENTED_EDGE('',*,*,#12494,.F.);
#17952=ORIENTED_EDGE('',*,*,#12471,.T.);
#17953=ORIENTED_EDGE('',*,*,#12510,.T.);
#17954=ORIENTED_EDGE('',*,*,#12392,.F.);
#17955=ORIENTED_EDGE('',*,*,#12403,.T.);
#17956=ORIENTED_EDGE('',*,*,#12511,.T.);
#17957=ORIENTED_EDGE('',*,*,#12512,.T.);
#17958=ORIENTED_EDGE('',*,*,#12513,.T.);
#17959=ORIENTED_EDGE('',*,*,#12511,.F.);
#17960=ORIENTED_EDGE('',*,*,#12513,.F.);
#17961=ORIENTED_EDGE('',*,*,#12514,.T.);
#17962=ORIENTED_EDGE('',*,*,#12515,.F.);
#17963=ORIENTED_EDGE('',*,*,#12516,.T.);
#17964=ORIENTED_EDGE('',*,*,#12517,.F.);
#17965=ORIENTED_EDGE('',*,*,#12443,.F.);
#17966=ORIENTED_EDGE('',*,*,#12499,.T.);
#17967=ORIENTED_EDGE('',*,*,#12518,.F.);
#17968=ORIENTED_EDGE('',*,*,#12514,.F.);
#17969=ORIENTED_EDGE('',*,*,#12512,.F.);
#17970=ORIENTED_EDGE('',*,*,#12500,.F.);
#17971=ORIENTED_EDGE('',*,*,#12464,.T.);
#17972=ORIENTED_EDGE('',*,*,#12519,.T.);
#17973=ORIENTED_EDGE('',*,*,#12496,.F.);
#17974=ORIENTED_EDGE('',*,*,#12448,.F.);
#17975=ORIENTED_EDGE('',*,*,#12444,.T.);
#17976=ORIENTED_EDGE('',*,*,#12517,.T.);
#17977=ORIENTED_EDGE('',*,*,#12466,.F.);
#17978=ORIENTED_EDGE('',*,*,#12498,.T.);
#17979=ORIENTED_EDGE('',*,*,#12520,.T.);
#17980=ORIENTED_EDGE('',*,*,#12521,.T.);
#17981=ORIENTED_EDGE('',*,*,#12515,.T.);
#17982=ORIENTED_EDGE('',*,*,#12518,.T.);
#17983=ORIENTED_EDGE('',*,*,#12520,.F.);
#17984=ORIENTED_EDGE('',*,*,#12497,.F.);
#17985=ORIENTED_EDGE('',*,*,#12519,.F.);
#17986=ORIENTED_EDGE('',*,*,#12463,.F.);
#17987=ORIENTED_EDGE('',*,*,#12522,.F.);
#17988=ORIENTED_EDGE('',*,*,#12467,.F.);
#17989=ORIENTED_EDGE('',*,*,#12516,.F.);
#17990=ORIENTED_EDGE('',*,*,#12521,.F.);
#17991=ORIENTED_EDGE('',*,*,#12522,.T.);
#17992=ORIENTED_EDGE('',*,*,#12462,.F.);
#17993=ORIENTED_EDGE('',*,*,#12393,.F.);
#17994=ORIENTED_EDGE('',*,*,#12510,.F.);
#17995=ORIENTED_EDGE('',*,*,#12470,.F.);
#17996=ORIENTED_EDGE('',*,*,#12523,.F.);
#17997=ORIENTED_EDGE('',*,*,#12474,.F.);
#17998=ORIENTED_EDGE('',*,*,#12394,.F.);
#17999=ORIENTED_EDGE('',*,*,#12523,.T.);
#18000=ORIENTED_EDGE('',*,*,#12469,.F.);
#18001=ORIENTED_EDGE('',*,*,#12389,.F.);
#18002=ORIENTED_EDGE('',*,*,#12524,.T.);
#18003=ORIENTED_EDGE('',*,*,#12525,.F.);
#18004=ORIENTED_EDGE('',*,*,#12412,.F.);
#18005=ORIENTED_EDGE('',*,*,#12387,.F.);
#18006=ORIENTED_EDGE('',*,*,#12413,.F.);
#18007=ORIENTED_EDGE('',*,*,#12525,.T.);
#18008=ORIENTED_EDGE('',*,*,#12526,.T.);
#18009=ORIENTED_EDGE('',*,*,#12388,.F.);
#18010=ORIENTED_EDGE('',*,*,#12526,.F.);
#18011=ORIENTED_EDGE('',*,*,#12524,.F.);
#18012=ORIENTED_EDGE('',*,*,#12454,.F.);
#18013=ORIENTED_EDGE('',*,*,#12503,.T.);
#18014=ORIENTED_EDGE('',*,*,#12527,.T.);
#18015=ORIENTED_EDGE('',*,*,#12397,.F.);
#18016=ORIENTED_EDGE('',*,*,#12398,.F.);
#18017=ORIENTED_EDGE('',*,*,#12527,.F.);
#18018=ORIENTED_EDGE('',*,*,#12502,.F.);
#18019=ORIENTED_EDGE('',*,*,#12505,.F.);
#18020=ORIENTED_EDGE('',*,*,#12408,.F.);
#18021=ORIENTED_EDGE('',*,*,#12422,.F.);
#18022=ORIENTED_EDGE('',*,*,#12528,.T.);
#18023=ORIENTED_EDGE('',*,*,#12529,.T.);
#18024=ORIENTED_EDGE('',*,*,#12507,.F.);
#18025=ORIENTED_EDGE('',*,*,#12447,.F.);
#18026=ORIENTED_EDGE('',*,*,#12509,.T.);
#18027=ORIENTED_EDGE('',*,*,#12530,.T.);
#18028=ORIENTED_EDGE('',*,*,#12528,.F.);
#18029=ORIENTED_EDGE('',*,*,#12530,.F.);
#18030=ORIENTED_EDGE('',*,*,#12508,.F.);
#18031=ORIENTED_EDGE('',*,*,#12529,.F.);
#18032=ORIENTED_EDGE('',*,*,#12070,.F.);
#18033=ORIENTED_EDGE('',*,*,#12203,.F.);
#18034=ORIENTED_EDGE('',*,*,#12207,.F.);
#18035=ORIENTED_EDGE('',*,*,#12531,.F.);
#18036=ORIENTED_EDGE('',*,*,#11917,.F.);
#18037=ORIENTED_EDGE('',*,*,#11938,.F.);
#18038=ORIENTED_EDGE('',*,*,#12071,.F.);
#18039=ORIENTED_EDGE('',*,*,#12531,.T.);
#18040=ORIENTED_EDGE('',*,*,#12206,.F.);
#18041=ORIENTED_EDGE('',*,*,#12204,.F.);
#18042=ORIENTED_EDGE('',*,*,#12074,.F.);
#18043=ORIENTED_EDGE('',*,*,#12532,.T.);
#18044=ORIENTED_EDGE('',*,*,#12533,.F.);
#18045=ORIENTED_EDGE('',*,*,#11935,.F.);
#18046=ORIENTED_EDGE('',*,*,#12072,.F.);
#18047=ORIENTED_EDGE('',*,*,#11936,.F.);
#18048=ORIENTED_EDGE('',*,*,#12533,.T.);
#18049=ORIENTED_EDGE('',*,*,#12534,.T.);
#18050=ORIENTED_EDGE('',*,*,#12073,.F.);
#18051=ORIENTED_EDGE('',*,*,#12534,.F.);
#18052=ORIENTED_EDGE('',*,*,#12532,.F.);
#18053=ORIENTED_EDGE('',*,*,#12053,.F.);
#18054=ORIENTED_EDGE('',*,*,#12535,.T.);
#18055=ORIENTED_EDGE('',*,*,#12536,.T.);
#18056=ORIENTED_EDGE('',*,*,#12065,.F.);
#18057=ORIENTED_EDGE('',*,*,#12057,.F.);
#18058=ORIENTED_EDGE('',*,*,#12199,.T.);
#18059=ORIENTED_EDGE('',*,*,#12537,.T.);
#18060=ORIENTED_EDGE('',*,*,#12535,.F.);
#18061=ORIENTED_EDGE('',*,*,#11921,.F.);
#18062=ORIENTED_EDGE('',*,*,#11930,.F.);
#18063=ORIENTED_EDGE('',*,*,#12067,.F.);
#18064=ORIENTED_EDGE('',*,*,#12538,.T.);
#18065=ORIENTED_EDGE('',*,*,#12197,.F.);
#18066=ORIENTED_EDGE('',*,*,#12058,.F.);
#18067=ORIENTED_EDGE('',*,*,#12066,.F.);
#18068=ORIENTED_EDGE('',*,*,#12536,.F.);
#18069=ORIENTED_EDGE('',*,*,#12537,.F.);
#18070=ORIENTED_EDGE('',*,*,#12198,.F.);
#18071=ORIENTED_EDGE('',*,*,#12538,.F.);
#18072=ORIENTED_EDGE('',*,*,#12076,.F.);
#18073=ORIENTED_EDGE('',*,*,#12211,.F.);
#18074=ORIENTED_EDGE('',*,*,#11926,.F.);
#18075=ORIENTED_EDGE('',*,*,#12328,.F.);
#18076=ORIENTED_EDGE('',*,*,#12035,.F.);
#18077=ORIENTED_EDGE('',*,*,#12327,.F.);
#18078=ORIENTED_EDGE('',*,*,#12325,.F.);
#18079=ORIENTED_EDGE('',*,*,#12320,.F.);
#18080=ORIENTED_EDGE('',*,*,#12302,.F.);
#18081=ORIENTED_EDGE('',*,*,#12539,.F.);
#18082=ORIENTED_EDGE('',*,*,#12292,.F.);
#18083=ORIENTED_EDGE('',*,*,#12540,.F.);
#18084=ORIENTED_EDGE('',*,*,#12284,.F.);
#18085=ORIENTED_EDGE('',*,*,#12541,.F.);
#18086=ORIENTED_EDGE('',*,*,#12276,.F.);
#18087=ORIENTED_EDGE('',*,*,#12542,.F.);
#18088=ORIENTED_EDGE('',*,*,#12541,.T.);
#18089=ORIENTED_EDGE('',*,*,#12283,.F.);
#18090=ORIENTED_EDGE('',*,*,#12313,.F.);
#18091=ORIENTED_EDGE('',*,*,#12277,.F.);
#18092=ORIENTED_EDGE('',*,*,#12539,.T.);
#18093=ORIENTED_EDGE('',*,*,#12301,.F.);
#18094=ORIENTED_EDGE('',*,*,#12309,.F.);
#18095=ORIENTED_EDGE('',*,*,#12293,.F.);
#18096=ORIENTED_EDGE('',*,*,#12542,.T.);
#18097=ORIENTED_EDGE('',*,*,#12275,.F.);
#18098=ORIENTED_EDGE('',*,*,#12315,.F.);
#18099=ORIENTED_EDGE('',*,*,#12285,.F.);
#18100=ORIENTED_EDGE('',*,*,#12540,.T.);
#18101=ORIENTED_EDGE('',*,*,#12291,.F.);
#18102=ORIENTED_EDGE('',*,*,#12311,.F.);
#18103=ORIENTED_EDGE('',*,*,#12303,.F.);
#18104=ORIENTED_EDGE('',*,*,#11878,.F.);
#18105=ORIENTED_EDGE('',*,*,#12340,.F.);
#18106=ORIENTED_EDGE('',*,*,#12227,.F.);
#18107=ORIENTED_EDGE('',*,*,#11872,.T.);
#18108=ORIENTED_EDGE('',*,*,#11874,.F.);
#18109=ORIENTED_EDGE('',*,*,#12259,.F.);
#18110=ORIENTED_EDGE('',*,*,#11959,.F.);
#18111=ORIENTED_EDGE('',*,*,#11893,.F.);
#18112=ORIENTED_EDGE('',*,*,#11967,.F.);
#18113=ORIENTED_EDGE('',*,*,#11961,.F.);
#18114=ORIENTED_EDGE('',*,*,#11903,.F.);
#18115=ORIENTED_EDGE('',*,*,#11973,.T.);
#18116=ORIENTED_EDGE('',*,*,#12254,.F.);
#18117=ORIENTED_EDGE('',*,*,#12255,.F.);
#18118=ORIENTED_EDGE('',*,*,#12017,.T.);
#18119=ORIENTED_EDGE('',*,*,#11848,.T.);
#18120=ORIENTED_EDGE('',*,*,#11854,.F.);
#18121=ORIENTED_EDGE('',*,*,#12148,.T.);
#18122=ORIENTED_EDGE('',*,*,#12138,.F.);
#18123=ORIENTED_EDGE('',*,*,#12140,.T.);
#18124=ORIENTED_EDGE('',*,*,#11861,.F.);
#18125=ORIENTED_EDGE('',*,*,#12013,.F.);
#18126=ORIENTED_EDGE('',*,*,#12004,.F.);
#18127=ORIENTED_EDGE('',*,*,#12012,.F.);
#18128=ORIENTED_EDGE('',*,*,#12256,.F.);
#18129=ORIENTED_EDGE('',*,*,#12260,.F.);
#18130=ORIENTED_EDGE('',*,*,#12007,.T.);
#18131=ORIENTED_EDGE('',*,*,#12169,.F.);
#18132=ORIENTED_EDGE('',*,*,#11995,.F.);
#18133=ORIENTED_EDGE('',*,*,#12032,.T.);
#18134=ORIENTED_EDGE('',*,*,#12155,.F.);
#18135=ORIENTED_EDGE('',*,*,#12217,.F.);
#18136=ORIENTED_EDGE('',*,*,#11986,.T.);
#18137=ORIENTED_EDGE('',*,*,#12543,.F.);
#18138=ORIENTED_EDGE('',*,*,#12544,.F.);
#18139=ORIENTED_EDGE('',*,*,#12544,.T.);
#18140=ORIENTED_EDGE('',*,*,#12545,.T.);
#18141=ORIENTED_EDGE('',*,*,#12546,.T.);
#18142=ORIENTED_EDGE('',*,*,#12547,.T.);
#18143=ORIENTED_EDGE('',*,*,#12548,.T.);
#18144=ORIENTED_EDGE('',*,*,#12549,.T.);
#18145=ORIENTED_EDGE('',*,*,#12550,.T.);
#18146=ORIENTED_EDGE('',*,*,#12551,.F.);
#18147=ORIENTED_EDGE('',*,*,#12552,.F.);
#18148=ORIENTED_EDGE('',*,*,#12552,.T.);
#18149=ORIENTED_EDGE('',*,*,#12553,.F.);
#18150=ORIENTED_EDGE('',*,*,#12554,.F.);
#18151=ORIENTED_EDGE('',*,*,#12555,.T.);
#18152=ORIENTED_EDGE('',*,*,#12556,.F.);
#18153=ORIENTED_EDGE('',*,*,#12557,.F.);
#18154=ORIENTED_EDGE('',*,*,#12558,.F.);
#18155=ORIENTED_EDGE('',*,*,#12543,.T.);
#18156=ORIENTED_EDGE('',*,*,#12550,.F.);
#18157=ORIENTED_EDGE('',*,*,#12559,.T.);
#18158=ORIENTED_EDGE('',*,*,#12553,.T.);
#18159=ORIENTED_EDGE('',*,*,#12551,.T.);
#18160=ORIENTED_EDGE('',*,*,#12558,.T.);
#18161=ORIENTED_EDGE('',*,*,#12560,.F.);
#18162=ORIENTED_EDGE('',*,*,#12545,.F.);
#18163=ORIENTED_EDGE('',*,*,#12547,.F.);
#18164=ORIENTED_EDGE('',*,*,#12561,.F.);
#18165=ORIENTED_EDGE('',*,*,#12555,.F.);
#18166=ORIENTED_EDGE('',*,*,#12562,.F.);
#18167=ORIENTED_EDGE('',*,*,#12561,.T.);
#18168=ORIENTED_EDGE('',*,*,#12546,.F.);
#18169=ORIENTED_EDGE('',*,*,#12560,.T.);
#18170=ORIENTED_EDGE('',*,*,#12557,.T.);
#18171=ORIENTED_EDGE('',*,*,#12556,.T.);
#18172=ORIENTED_EDGE('',*,*,#12562,.T.);
#18173=ORIENTED_EDGE('',*,*,#12554,.T.);
#18174=ORIENTED_EDGE('',*,*,#12559,.F.);
#18175=ORIENTED_EDGE('',*,*,#12549,.F.);
#18176=ORIENTED_EDGE('',*,*,#12548,.F.);
#18177=ORIENTED_EDGE('',*,*,#12563,.T.);
#18178=ORIENTED_EDGE('',*,*,#12564,.T.);
#18179=ORIENTED_EDGE('',*,*,#12565,.T.);
#18180=ORIENTED_EDGE('',*,*,#12566,.T.);
#18181=ORIENTED_EDGE('',*,*,#12564,.F.);
#18182=ORIENTED_EDGE('',*,*,#12566,.F.);
#18183=ORIENTED_EDGE('',*,*,#12567,.T.);
#18184=ORIENTED_EDGE('',*,*,#12568,.F.);
#18185=ORIENTED_EDGE('',*,*,#12569,.F.);
#18186=ORIENTED_EDGE('',*,*,#12567,.F.);
#18187=ORIENTED_EDGE('',*,*,#12565,.F.);
#18188=ORIENTED_EDGE('',*,*,#12570,.F.);
#18189=ORIENTED_EDGE('',*,*,#12563,.F.);
#18190=ORIENTED_EDGE('',*,*,#12568,.T.);
#18191=ORIENTED_EDGE('',*,*,#12569,.T.);
#18192=ORIENTED_EDGE('',*,*,#12571,.T.);
#18193=ORIENTED_EDGE('',*,*,#12572,.T.);
#18194=ORIENTED_EDGE('',*,*,#12571,.F.);
#18195=ORIENTED_EDGE('',*,*,#12573,.T.);
#18196=ORIENTED_EDGE('',*,*,#12572,.F.);
#18197=ORIENTED_EDGE('',*,*,#12574,.T.);
#18198=ORIENTED_EDGE('',*,*,#12575,.T.);
#18199=ORIENTED_EDGE('',*,*,#12576,.T.);
#18200=ORIENTED_EDGE('',*,*,#12575,.F.);
#18201=ORIENTED_EDGE('',*,*,#12577,.T.);
#18202=ORIENTED_EDGE('',*,*,#12578,.F.);
#18203=ORIENTED_EDGE('',*,*,#12576,.F.);
#18204=ORIENTED_EDGE('',*,*,#12573,.F.);
#18205=ORIENTED_EDGE('',*,*,#12579,.T.);
#18206=ORIENTED_EDGE('',*,*,#12577,.F.);
#18207=ORIENTED_EDGE('',*,*,#12574,.F.);
#18208=ORIENTED_EDGE('',*,*,#12579,.F.);
#18209=ORIENTED_EDGE('',*,*,#12578,.T.);
#18210=ORIENTED_EDGE('',*,*,#12580,.T.);
#18211=ORIENTED_EDGE('',*,*,#12581,.T.);
#18212=ORIENTED_EDGE('',*,*,#12582,.T.);
#18213=ORIENTED_EDGE('',*,*,#12580,.F.);
#18214=ORIENTED_EDGE('',*,*,#12582,.F.);
#18215=ORIENTED_EDGE('',*,*,#12583,.T.);
#18216=ORIENTED_EDGE('',*,*,#12584,.T.);
#18217=ORIENTED_EDGE('',*,*,#12583,.F.);
#18218=ORIENTED_EDGE('',*,*,#12581,.F.);
#18219=ORIENTED_EDGE('',*,*,#12585,.T.);
#18220=ORIENTED_EDGE('',*,*,#12586,.T.);
#18221=ORIENTED_EDGE('',*,*,#12587,.T.);
#18222=ORIENTED_EDGE('',*,*,#12588,.T.);
#18223=ORIENTED_EDGE('',*,*,#12589,.T.);
#18224=ORIENTED_EDGE('',*,*,#12590,.T.);
#18225=ORIENTED_EDGE('',*,*,#12591,.T.);
#18226=ORIENTED_EDGE('',*,*,#12592,.T.);
#18227=ORIENTED_EDGE('',*,*,#12590,.F.);
#18228=ORIENTED_EDGE('',*,*,#12592,.F.);
#18229=ORIENTED_EDGE('',*,*,#12593,.T.);
#18230=ORIENTED_EDGE('',*,*,#12594,.F.);
#18231=ORIENTED_EDGE('',*,*,#12595,.F.);
#18232=ORIENTED_EDGE('',*,*,#12593,.F.);
#18233=ORIENTED_EDGE('',*,*,#12591,.F.);
#18234=ORIENTED_EDGE('',*,*,#12589,.F.);
#18235=ORIENTED_EDGE('',*,*,#12584,.F.);
#18236=ORIENTED_EDGE('',*,*,#12594,.T.);
#18237=ORIENTED_EDGE('',*,*,#12595,.T.);
#18238=ORIENTED_EDGE('',*,*,#12596,.T.);
#18239=ORIENTED_EDGE('',*,*,#12570,.T.);
#18240=ORIENTED_EDGE('',*,*,#12596,.F.);
#18241=ORIENTED_EDGE('',*,*,#12597,.T.);
#18242=ORIENTED_EDGE('',*,*,#12598,.T.);
#18243=ORIENTED_EDGE('',*,*,#12599,.T.);
#18244=ORIENTED_EDGE('',*,*,#12600,.T.);
#18245=ORIENTED_EDGE('',*,*,#12601,.T.);
#18246=ORIENTED_EDGE('',*,*,#12598,.F.);
#18247=ORIENTED_EDGE('',*,*,#12602,.T.);
#18248=ORIENTED_EDGE('',*,*,#12603,.T.);
#18249=ORIENTED_EDGE('',*,*,#12604,.T.);
#18250=ORIENTED_EDGE('',*,*,#12600,.F.);
#18251=ORIENTED_EDGE('',*,*,#12605,.T.);
#18252=ORIENTED_EDGE('',*,*,#12606,.T.);
#18253=ORIENTED_EDGE('',*,*,#12607,.T.);
#18254=ORIENTED_EDGE('',*,*,#12606,.F.);
#18255=ORIENTED_EDGE('',*,*,#12608,.T.);
#18256=ORIENTED_EDGE('',*,*,#12603,.F.);
#18257=ORIENTED_EDGE('',*,*,#12602,.F.);
#18258=ORIENTED_EDGE('',*,*,#12609,.F.);
#18259=ORIENTED_EDGE('',*,*,#12585,.F.);
#18260=ORIENTED_EDGE('',*,*,#12610,.F.);
#18261=ORIENTED_EDGE('',*,*,#12597,.F.);
#18262=ORIENTED_EDGE('',*,*,#12611,.T.);
#18263=ORIENTED_EDGE('',*,*,#12586,.F.);
#18264=ORIENTED_EDGE('',*,*,#12609,.T.);
#18265=ORIENTED_EDGE('',*,*,#12599,.F.);
#18266=ORIENTED_EDGE('',*,*,#12601,.F.);
#18267=ORIENTED_EDGE('',*,*,#12608,.F.);
#18268=ORIENTED_EDGE('',*,*,#12605,.F.);
#18269=ORIENTED_EDGE('',*,*,#12612,.T.);
#18270=ORIENTED_EDGE('',*,*,#12613,.T.);
#18271=ORIENTED_EDGE('',*,*,#12614,.T.);
#18272=ORIENTED_EDGE('',*,*,#12615,.T.);
#18273=ORIENTED_EDGE('',*,*,#12612,.F.);
#18274=ORIENTED_EDGE('',*,*,#12616,.T.);
#18275=ORIENTED_EDGE('',*,*,#12617,.T.);
#18276=ORIENTED_EDGE('',*,*,#12618,.F.);
#18277=ORIENTED_EDGE('',*,*,#12615,.F.);
#18278=ORIENTED_EDGE('',*,*,#12619,.T.);
#18279=ORIENTED_EDGE('',*,*,#12620,.T.);
#18280=ORIENTED_EDGE('',*,*,#12616,.F.);
#18281=ORIENTED_EDGE('',*,*,#12614,.F.);
#18282=ORIENTED_EDGE('',*,*,#12621,.T.);
#18283=ORIENTED_EDGE('',*,*,#12622,.T.);
#18284=ORIENTED_EDGE('',*,*,#12619,.F.);
#18285=ORIENTED_EDGE('',*,*,#12613,.F.);
#18286=ORIENTED_EDGE('',*,*,#12618,.T.);
#18287=ORIENTED_EDGE('',*,*,#12623,.T.);
#18288=ORIENTED_EDGE('',*,*,#12621,.F.);
#18289=ORIENTED_EDGE('',*,*,#12623,.F.);
#18290=ORIENTED_EDGE('',*,*,#12617,.F.);
#18291=ORIENTED_EDGE('',*,*,#12620,.F.);
#18292=ORIENTED_EDGE('',*,*,#12622,.F.);
#18293=ORIENTED_EDGE('',*,*,#12604,.F.);
#18294=ORIENTED_EDGE('',*,*,#12624,.F.);
#18295=ORIENTED_EDGE('',*,*,#12587,.F.);
#18296=ORIENTED_EDGE('',*,*,#12611,.F.);
#18297=ORIENTED_EDGE('',*,*,#12607,.F.);
#18298=ORIENTED_EDGE('',*,*,#12610,.T.);
#18299=ORIENTED_EDGE('',*,*,#12588,.F.);
#18300=ORIENTED_EDGE('',*,*,#12624,.T.);
#18301=ORIENTED_EDGE('',*,*,#12625,.T.);
#18302=ORIENTED_EDGE('',*,*,#12626,.T.);
#18303=ORIENTED_EDGE('',*,*,#12627,.T.);
#18304=ORIENTED_EDGE('',*,*,#12628,.T.);
#18305=ORIENTED_EDGE('',*,*,#12629,.T.);
#18306=ORIENTED_EDGE('',*,*,#12630,.T.);
#18307=ORIENTED_EDGE('',*,*,#12631,.T.);
#18308=ORIENTED_EDGE('',*,*,#12632,.T.);
#18309=ORIENTED_EDGE('',*,*,#12633,.T.);
#18310=ORIENTED_EDGE('',*,*,#12634,.T.);
#18311=ORIENTED_EDGE('',*,*,#12635,.T.);
#18312=ORIENTED_EDGE('',*,*,#12636,.T.);
#18313=ORIENTED_EDGE('',*,*,#12637,.T.);
#18314=ORIENTED_EDGE('',*,*,#12638,.T.);
#18315=ORIENTED_EDGE('',*,*,#12639,.T.);
#18316=ORIENTED_EDGE('',*,*,#12640,.T.);
#18317=ORIENTED_EDGE('',*,*,#12639,.F.);
#18318=ORIENTED_EDGE('',*,*,#12641,.T.);
#18319=ORIENTED_EDGE('',*,*,#12635,.F.);
#18320=ORIENTED_EDGE('',*,*,#12633,.F.);
#18321=ORIENTED_EDGE('',*,*,#12642,.T.);
#18322=ORIENTED_EDGE('',*,*,#12629,.F.);
#18323=ORIENTED_EDGE('',*,*,#12631,.F.);
#18324=ORIENTED_EDGE('',*,*,#12643,.T.);
#18325=ORIENTED_EDGE('',*,*,#12627,.F.);
#18326=ORIENTED_EDGE('',*,*,#12625,.F.);
#18327=ORIENTED_EDGE('',*,*,#12644,.T.);
#18328=ORIENTED_EDGE('',*,*,#12637,.F.);
#18329=ORIENTED_EDGE('',*,*,#12642,.F.);
#18330=ORIENTED_EDGE('',*,*,#12645,.T.);
#18331=ORIENTED_EDGE('',*,*,#12646,.T.);
#18332=ORIENTED_EDGE('',*,*,#12647,.T.);
#18333=ORIENTED_EDGE('',*,*,#12636,.F.);
#18334=ORIENTED_EDGE('',*,*,#12648,.F.);
#18335=ORIENTED_EDGE('',*,*,#12649,.F.);
#18336=ORIENTED_EDGE('',*,*,#12645,.F.);
#18337=ORIENTED_EDGE('',*,*,#12641,.F.);
#18338=ORIENTED_EDGE('',*,*,#12650,.T.);
#18339=ORIENTED_EDGE('',*,*,#12651,.T.);
#18340=ORIENTED_EDGE('',*,*,#12648,.T.);
#18341=ORIENTED_EDGE('',*,*,#12638,.F.);
#18342=ORIENTED_EDGE('',*,*,#12652,.F.);
#18343=ORIENTED_EDGE('',*,*,#12653,.F.);
#18344=ORIENTED_EDGE('',*,*,#12654,.F.);
#18345=ORIENTED_EDGE('',*,*,#12655,.F.);
#18346=ORIENTED_EDGE('',*,*,#12650,.F.);
#18347=ORIENTED_EDGE('',*,*,#12656,.F.);
#18348=ORIENTED_EDGE('',*,*,#12657,.F.);
#18349=ORIENTED_EDGE('',*,*,#12626,.F.);
#18350=ORIENTED_EDGE('',*,*,#12640,.F.);
#18351=ORIENTED_EDGE('',*,*,#12634,.F.);
#18352=ORIENTED_EDGE('',*,*,#12632,.F.);
#18353=ORIENTED_EDGE('',*,*,#12644,.F.);
#18354=ORIENTED_EDGE('',*,*,#12658,.T.);
#18355=ORIENTED_EDGE('',*,*,#12659,.T.);
#18356=ORIENTED_EDGE('',*,*,#12652,.T.);
#18357=ORIENTED_EDGE('',*,*,#12660,.T.);
#18358=ORIENTED_EDGE('',*,*,#12661,.T.);
#18359=ORIENTED_EDGE('',*,*,#12662,.T.);
#18360=ORIENTED_EDGE('',*,*,#12663,.T.);
#18361=ORIENTED_EDGE('',*,*,#12660,.F.);
#18362=ORIENTED_EDGE('',*,*,#12664,.T.);
#18363=ORIENTED_EDGE('',*,*,#12659,.F.);
#18364=ORIENTED_EDGE('',*,*,#12643,.F.);
#18365=ORIENTED_EDGE('',*,*,#12665,.T.);
#18366=ORIENTED_EDGE('',*,*,#12666,.T.);
#18367=ORIENTED_EDGE('',*,*,#12667,.T.);
#18368=ORIENTED_EDGE('',*,*,#12666,.F.);
#18369=ORIENTED_EDGE('',*,*,#12668,.T.);
#18370=ORIENTED_EDGE('',*,*,#12662,.F.);
#18371=ORIENTED_EDGE('',*,*,#12664,.F.);
#18372=ORIENTED_EDGE('',*,*,#12669,.T.);
#18373=ORIENTED_EDGE('',*,*,#12670,.F.);
#18374=ORIENTED_EDGE('',*,*,#12653,.T.);
#18375=ORIENTED_EDGE('',*,*,#12663,.F.);
#18376=ORIENTED_EDGE('',*,*,#12671,.F.);
#18377=ORIENTED_EDGE('',*,*,#12672,.F.);
#18378=ORIENTED_EDGE('',*,*,#12673,.F.);
#18379=ORIENTED_EDGE('',*,*,#12674,.F.);
#18380=ORIENTED_EDGE('',*,*,#12675,.F.);
#18381=ORIENTED_EDGE('',*,*,#12676,.T.);
#18382=ORIENTED_EDGE('',*,*,#12677,.F.);
#18383=ORIENTED_EDGE('',*,*,#12678,.F.);
#18384=ORIENTED_EDGE('',*,*,#12679,.F.);
#18385=ORIENTED_EDGE('',*,*,#12680,.F.);
#18386=ORIENTED_EDGE('',*,*,#12669,.F.);
#18387=ORIENTED_EDGE('',*,*,#12668,.F.);
#18388=ORIENTED_EDGE('',*,*,#12681,.T.);
#18389=ORIENTED_EDGE('',*,*,#12682,.F.);
#18390=ORIENTED_EDGE('',*,*,#12671,.T.);
#18391=ORIENTED_EDGE('',*,*,#12630,.F.);
#18392=ORIENTED_EDGE('',*,*,#12647,.F.);
#18393=ORIENTED_EDGE('',*,*,#12683,.F.);
#18394=ORIENTED_EDGE('',*,*,#12684,.F.);
#18395=ORIENTED_EDGE('',*,*,#12681,.F.);
#18396=ORIENTED_EDGE('',*,*,#12665,.F.);
#18397=ORIENTED_EDGE('',*,*,#12685,.F.);
#18398=ORIENTED_EDGE('',*,*,#12686,.F.);
#18399=ORIENTED_EDGE('',*,*,#12687,.T.);
#18400=ORIENTED_EDGE('',*,*,#12688,.T.);
#18401=ORIENTED_EDGE('',*,*,#12689,.T.);
#18402=ORIENTED_EDGE('',*,*,#12649,.T.);
#18403=ORIENTED_EDGE('',*,*,#12651,.F.);
#18404=ORIENTED_EDGE('',*,*,#12690,.T.);
#18405=ORIENTED_EDGE('',*,*,#12687,.F.);
#18406=ORIENTED_EDGE('',*,*,#12689,.F.);
#18407=ORIENTED_EDGE('',*,*,#12691,.T.);
#18408=ORIENTED_EDGE('',*,*,#12646,.F.);
#18409=ORIENTED_EDGE('',*,*,#12691,.F.);
#18410=ORIENTED_EDGE('',*,*,#12692,.T.);
#18411=ORIENTED_EDGE('',*,*,#12693,.F.);
#18412=ORIENTED_EDGE('',*,*,#12683,.T.);
#18413=ORIENTED_EDGE('',*,*,#12688,.F.);
#18414=ORIENTED_EDGE('',*,*,#12694,.F.);
#18415=ORIENTED_EDGE('',*,*,#12695,.F.);
#18416=ORIENTED_EDGE('',*,*,#12696,.F.);
#18417=ORIENTED_EDGE('',*,*,#12697,.F.);
#18418=ORIENTED_EDGE('',*,*,#12698,.F.);
#18419=ORIENTED_EDGE('',*,*,#12699,.F.);
#18420=ORIENTED_EDGE('',*,*,#12700,.F.);
#18421=ORIENTED_EDGE('',*,*,#12701,.F.);
#18422=ORIENTED_EDGE('',*,*,#12702,.F.);
#18423=ORIENTED_EDGE('',*,*,#12703,.F.);
#18424=ORIENTED_EDGE('',*,*,#12692,.F.);
#18425=ORIENTED_EDGE('',*,*,#12690,.F.);
#18426=ORIENTED_EDGE('',*,*,#12655,.T.);
#18427=ORIENTED_EDGE('',*,*,#12704,.T.);
#18428=ORIENTED_EDGE('',*,*,#12694,.T.);
#18429=ORIENTED_EDGE('',*,*,#12704,.F.);
#18430=ORIENTED_EDGE('',*,*,#12705,.T.);
#18431=ORIENTED_EDGE('',*,*,#12706,.T.);
#18432=ORIENTED_EDGE('',*,*,#12695,.T.);
#18433=ORIENTED_EDGE('',*,*,#12707,.T.);
#18434=ORIENTED_EDGE('',*,*,#12696,.T.);
#18435=ORIENTED_EDGE('',*,*,#12706,.F.);
#18436=ORIENTED_EDGE('',*,*,#12708,.T.);
#18437=ORIENTED_EDGE('',*,*,#12707,.F.);
#18438=ORIENTED_EDGE('',*,*,#12709,.T.);
#18439=ORIENTED_EDGE('',*,*,#12710,.T.);
#18440=ORIENTED_EDGE('',*,*,#12697,.T.);
#18441=ORIENTED_EDGE('',*,*,#12698,.T.);
#18442=ORIENTED_EDGE('',*,*,#12710,.F.);
#18443=ORIENTED_EDGE('',*,*,#12711,.T.);
#18444=ORIENTED_EDGE('',*,*,#12712,.T.);
#18445=ORIENTED_EDGE('',*,*,#12713,.T.);
#18446=ORIENTED_EDGE('',*,*,#12714,.T.);
#18447=ORIENTED_EDGE('',*,*,#12715,.T.);
#18448=ORIENTED_EDGE('',*,*,#12712,.F.);
#18449=ORIENTED_EDGE('',*,*,#12716,.T.);
#18450=ORIENTED_EDGE('',*,*,#12717,.T.);
#18451=ORIENTED_EDGE('',*,*,#12714,.F.);
#18452=ORIENTED_EDGE('',*,*,#12718,.T.);
#18453=ORIENTED_EDGE('',*,*,#12719,.T.);
#18454=ORIENTED_EDGE('',*,*,#12716,.F.);
#18455=ORIENTED_EDGE('',*,*,#12720,.T.);
#18456=ORIENTED_EDGE('',*,*,#12721,.T.);
#18457=ORIENTED_EDGE('',*,*,#12722,.T.);
#18458=ORIENTED_EDGE('',*,*,#12723,.T.);
#18459=ORIENTED_EDGE('',*,*,#12724,.T.);
#18460=ORIENTED_EDGE('',*,*,#12678,.T.);
#18461=ORIENTED_EDGE('',*,*,#12725,.T.);
#18462=ORIENTED_EDGE('',*,*,#12722,.F.);
#18463=ORIENTED_EDGE('',*,*,#12677,.T.);
#18464=ORIENTED_EDGE('',*,*,#12721,.F.);
#18465=ORIENTED_EDGE('',*,*,#12726,.T.);
#18466=ORIENTED_EDGE('',*,*,#12679,.T.);
#18467=ORIENTED_EDGE('',*,*,#12724,.F.);
#18468=ORIENTED_EDGE('',*,*,#12727,.T.);
#18469=ORIENTED_EDGE('',*,*,#12726,.F.);
#18470=ORIENTED_EDGE('',*,*,#12728,.T.);
#18471=ORIENTED_EDGE('',*,*,#12670,.T.);
#18472=ORIENTED_EDGE('',*,*,#12680,.T.);
#18473=ORIENTED_EDGE('',*,*,#12715,.F.);
#18474=ORIENTED_EDGE('',*,*,#12729,.F.);
#18475=ORIENTED_EDGE('',*,*,#12730,.T.);
#18476=ORIENTED_EDGE('',*,*,#12731,.T.);
#18477=ORIENTED_EDGE('',*,*,#12732,.T.);
#18478=ORIENTED_EDGE('',*,*,#12733,.T.);
#18479=ORIENTED_EDGE('',*,*,#12734,.T.);
#18480=ORIENTED_EDGE('',*,*,#12735,.T.);
#18481=ORIENTED_EDGE('',*,*,#12699,.T.);
#18482=ORIENTED_EDGE('',*,*,#12717,.F.);
#18483=ORIENTED_EDGE('',*,*,#12736,.F.);
#18484=ORIENTED_EDGE('',*,*,#12737,.T.);
#18485=ORIENTED_EDGE('',*,*,#12729,.T.);
#18486=ORIENTED_EDGE('',*,*,#12719,.F.);
#18487=ORIENTED_EDGE('',*,*,#12676,.F.);
#18488=ORIENTED_EDGE('',*,*,#12738,.F.);
#18489=ORIENTED_EDGE('',*,*,#12739,.F.);
#18490=ORIENTED_EDGE('',*,*,#12740,.F.);
#18491=ORIENTED_EDGE('',*,*,#12741,.T.);
#18492=ORIENTED_EDGE('',*,*,#12742,.T.);
#18493=ORIENTED_EDGE('',*,*,#12743,.T.);
#18494=ORIENTED_EDGE('',*,*,#12736,.T.);
#18495=ORIENTED_EDGE('',*,*,#12628,.F.);
#18496=ORIENTED_EDGE('',*,*,#12667,.F.);
#18497=ORIENTED_EDGE('',*,*,#12661,.F.);
#18498=ORIENTED_EDGE('',*,*,#12658,.F.);
#18499=ORIENTED_EDGE('',*,*,#12740,.T.);
#18500=ORIENTED_EDGE('',*,*,#12744,.T.);
#18501=ORIENTED_EDGE('',*,*,#12673,.T.);
#18502=ORIENTED_EDGE('',*,*,#12745,.T.);
#18503=ORIENTED_EDGE('',*,*,#12746,.T.);
#18504=ORIENTED_EDGE('',*,*,#12739,.T.);
#18505=ORIENTED_EDGE('',*,*,#12747,.T.);
#18506=ORIENTED_EDGE('',*,*,#12674,.T.);
#18507=ORIENTED_EDGE('',*,*,#12744,.F.);
#18508=ORIENTED_EDGE('',*,*,#12738,.T.);
#18509=ORIENTED_EDGE('',*,*,#12675,.T.);
#18510=ORIENTED_EDGE('',*,*,#12747,.F.);
#18511=ORIENTED_EDGE('',*,*,#12682,.T.);
#18512=ORIENTED_EDGE('',*,*,#12748,.T.);
#18513=ORIENTED_EDGE('',*,*,#12745,.F.);
#18514=ORIENTED_EDGE('',*,*,#12672,.T.);
#18515=ORIENTED_EDGE('',*,*,#12748,.F.);
#18516=ORIENTED_EDGE('',*,*,#12684,.T.);
#18517=ORIENTED_EDGE('',*,*,#12749,.F.);
#18518=ORIENTED_EDGE('',*,*,#12750,.T.);
#18519=ORIENTED_EDGE('',*,*,#12733,.F.);
#18520=ORIENTED_EDGE('',*,*,#12751,.T.);
#18521=ORIENTED_EDGE('',*,*,#12752,.T.);
#18522=ORIENTED_EDGE('',*,*,#12702,.T.);
#18523=ORIENTED_EDGE('',*,*,#12753,.T.);
#18524=ORIENTED_EDGE('',*,*,#12752,.F.);
#18525=ORIENTED_EDGE('',*,*,#12749,.T.);
#18526=ORIENTED_EDGE('',*,*,#12693,.T.);
#18527=ORIENTED_EDGE('',*,*,#12703,.T.);
#18528=ORIENTED_EDGE('',*,*,#12734,.F.);
#18529=ORIENTED_EDGE('',*,*,#12753,.F.);
#18530=ORIENTED_EDGE('',*,*,#12701,.T.);
#18531=ORIENTED_EDGE('',*,*,#12754,.T.);
#18532=ORIENTED_EDGE('',*,*,#12735,.F.);
#18533=ORIENTED_EDGE('',*,*,#12754,.F.);
#18534=ORIENTED_EDGE('',*,*,#12700,.T.);
#18535=ORIENTED_EDGE('',*,*,#12742,.F.);
#18536=ORIENTED_EDGE('',*,*,#12755,.T.);
#18537=ORIENTED_EDGE('',*,*,#12731,.F.);
#18538=ORIENTED_EDGE('',*,*,#12756,.T.);
#18539=ORIENTED_EDGE('',*,*,#12743,.F.);
#18540=ORIENTED_EDGE('',*,*,#12756,.F.);
#18541=ORIENTED_EDGE('',*,*,#12730,.F.);
#18542=ORIENTED_EDGE('',*,*,#12737,.F.);
#18543=ORIENTED_EDGE('',*,*,#12757,.F.);
#18544=ORIENTED_EDGE('',*,*,#12758,.F.);
#18545=ORIENTED_EDGE('',*,*,#12685,.T.);
#18546=ORIENTED_EDGE('',*,*,#12759,.T.);
#18547=ORIENTED_EDGE('',*,*,#12760,.T.);
#18548=ORIENTED_EDGE('',*,*,#12761,.T.);
#18549=ORIENTED_EDGE('',*,*,#12759,.F.);
#18550=ORIENTED_EDGE('',*,*,#12761,.F.);
#18551=ORIENTED_EDGE('',*,*,#12762,.T.);
#18552=ORIENTED_EDGE('',*,*,#12763,.F.);
#18553=ORIENTED_EDGE('',*,*,#12764,.F.);
#18554=ORIENTED_EDGE('',*,*,#12762,.F.);
#18555=ORIENTED_EDGE('',*,*,#12760,.F.);
#18556=ORIENTED_EDGE('',*,*,#12656,.T.);
#18557=ORIENTED_EDGE('',*,*,#12765,.T.);
#18558=ORIENTED_EDGE('',*,*,#12763,.T.);
#18559=ORIENTED_EDGE('',*,*,#12764,.T.);
#18560=ORIENTED_EDGE('',*,*,#12765,.F.);
#18561=ORIENTED_EDGE('',*,*,#12757,.T.);
#18562=ORIENTED_EDGE('',*,*,#12766,.T.);
#18563=ORIENTED_EDGE('',*,*,#12767,.T.);
#18564=ORIENTED_EDGE('',*,*,#12768,.T.);
#18565=ORIENTED_EDGE('',*,*,#12766,.F.);
#18566=ORIENTED_EDGE('',*,*,#12768,.F.);
#18567=ORIENTED_EDGE('',*,*,#12769,.T.);
#18568=ORIENTED_EDGE('',*,*,#12770,.F.);
#18569=ORIENTED_EDGE('',*,*,#12771,.F.);
#18570=ORIENTED_EDGE('',*,*,#12769,.F.);
#18571=ORIENTED_EDGE('',*,*,#12767,.F.);
#18572=ORIENTED_EDGE('',*,*,#12772,.T.);
#18573=ORIENTED_EDGE('',*,*,#12773,.T.);
#18574=ORIENTED_EDGE('',*,*,#12770,.T.);
#18575=ORIENTED_EDGE('',*,*,#12771,.T.);
#18576=ORIENTED_EDGE('',*,*,#12773,.F.);
#18577=ORIENTED_EDGE('',*,*,#12711,.F.);
#18578=ORIENTED_EDGE('',*,*,#12774,.F.);
#18579=ORIENTED_EDGE('',*,*,#12725,.F.);
#18580=ORIENTED_EDGE('',*,*,#12720,.F.);
#18581=ORIENTED_EDGE('',*,*,#12718,.F.);
#18582=ORIENTED_EDGE('',*,*,#12713,.F.);
#18583=ORIENTED_EDGE('',*,*,#12775,.F.);
#18584=ORIENTED_EDGE('',*,*,#12772,.F.);
#18585=ORIENTED_EDGE('',*,*,#12686,.T.);
#18586=ORIENTED_EDGE('',*,*,#12776,.T.);
#18587=ORIENTED_EDGE('',*,*,#12777,.T.);
#18588=ORIENTED_EDGE('',*,*,#12778,.T.);
#18589=ORIENTED_EDGE('',*,*,#12776,.F.);
#18590=ORIENTED_EDGE('',*,*,#12778,.F.);
#18591=ORIENTED_EDGE('',*,*,#12779,.T.);
#18592=ORIENTED_EDGE('',*,*,#12780,.F.);
#18593=ORIENTED_EDGE('',*,*,#12781,.F.);
#18594=ORIENTED_EDGE('',*,*,#12779,.F.);
#18595=ORIENTED_EDGE('',*,*,#12777,.F.);
#18596=ORIENTED_EDGE('',*,*,#12657,.T.);
#18597=ORIENTED_EDGE('',*,*,#12782,.T.);
#18598=ORIENTED_EDGE('',*,*,#12780,.T.);
#18599=ORIENTED_EDGE('',*,*,#12781,.T.);
#18600=ORIENTED_EDGE('',*,*,#12782,.F.);
#18601=ORIENTED_EDGE('',*,*,#12758,.T.);
#18602=ORIENTED_EDGE('',*,*,#12783,.T.);
#18603=ORIENTED_EDGE('',*,*,#12784,.T.);
#18604=ORIENTED_EDGE('',*,*,#12785,.T.);
#18605=ORIENTED_EDGE('',*,*,#12783,.F.);
#18606=ORIENTED_EDGE('',*,*,#12785,.F.);
#18607=ORIENTED_EDGE('',*,*,#12786,.T.);
#18608=ORIENTED_EDGE('',*,*,#12787,.F.);
#18609=ORIENTED_EDGE('',*,*,#12788,.F.);
#18610=ORIENTED_EDGE('',*,*,#12786,.F.);
#18611=ORIENTED_EDGE('',*,*,#12784,.F.);
#18612=ORIENTED_EDGE('',*,*,#12775,.T.);
#18613=ORIENTED_EDGE('',*,*,#12789,.T.);
#18614=ORIENTED_EDGE('',*,*,#12787,.T.);
#18615=ORIENTED_EDGE('',*,*,#12788,.T.);
#18616=ORIENTED_EDGE('',*,*,#12789,.F.);
#18617=ORIENTED_EDGE('',*,*,#12746,.F.);
#18618=ORIENTED_EDGE('',*,*,#12750,.F.);
#18619=ORIENTED_EDGE('',*,*,#12751,.F.);
#18620=ORIENTED_EDGE('',*,*,#12732,.F.);
#18621=ORIENTED_EDGE('',*,*,#12755,.F.);
#18622=ORIENTED_EDGE('',*,*,#12741,.F.);
#18623=ORIENTED_EDGE('',*,*,#12709,.F.);
#18624=ORIENTED_EDGE('',*,*,#12790,.T.);
#18625=ORIENTED_EDGE('',*,*,#12723,.F.);
#18626=ORIENTED_EDGE('',*,*,#12774,.T.);
#18627=ORIENTED_EDGE('',*,*,#12705,.F.);
#18628=ORIENTED_EDGE('',*,*,#12654,.T.);
#18629=ORIENTED_EDGE('',*,*,#12728,.F.);
#18630=ORIENTED_EDGE('',*,*,#12791,.T.);
#18631=ORIENTED_EDGE('',*,*,#12708,.F.);
#18632=ORIENTED_EDGE('',*,*,#12791,.F.);
#18633=ORIENTED_EDGE('',*,*,#12727,.F.);
#18634=ORIENTED_EDGE('',*,*,#12790,.F.);
#18635=ORIENTED_EDGE('',*,*,#12792,.F.);
#18636=ORIENTED_EDGE('',*,*,#12793,.T.);
#18637=ORIENTED_EDGE('',*,*,#12794,.F.);
#18638=ORIENTED_EDGE('',*,*,#12795,.T.);
#18639=ORIENTED_EDGE('',*,*,#12792,.T.);
#18640=ORIENTED_EDGE('',*,*,#12795,.F.);
#18641=ORIENTED_EDGE('',*,*,#12796,.F.);
#18642=ORIENTED_EDGE('',*,*,#12797,.T.);
#18643=ORIENTED_EDGE('',*,*,#12798,.T.);
#18644=ORIENTED_EDGE('',*,*,#12797,.F.);
#18645=ORIENTED_EDGE('',*,*,#12798,.F.);
#18646=ORIENTED_EDGE('',*,*,#12799,.T.);
#18647=ORIENTED_EDGE('',*,*,#12799,.F.);
#18648=ORIENTED_EDGE('',*,*,#12800,.T.);
#18649=ORIENTED_EDGE('',*,*,#12801,.F.);
#18650=ORIENTED_EDGE('',*,*,#12800,.F.);
#18651=ORIENTED_EDGE('',*,*,#12801,.T.);
#18652=ORIENTED_EDGE('',*,*,#12794,.T.);
#18653=ORIENTED_EDGE('',*,*,#12802,.F.);
#18654=ORIENTED_EDGE('',*,*,#12803,.T.);
#18655=ORIENTED_EDGE('',*,*,#12804,.F.);
#18656=ORIENTED_EDGE('',*,*,#12803,.F.);
#18657=ORIENTED_EDGE('',*,*,#12802,.T.);
#18658=ORIENTED_EDGE('',*,*,#12805,.F.);
#18659=ORIENTED_EDGE('',*,*,#12806,.F.);
#18660=ORIENTED_EDGE('',*,*,#12807,.T.);
#18661=ORIENTED_EDGE('',*,*,#12808,.T.);
#18662=ORIENTED_EDGE('',*,*,#12807,.F.);
#18663=ORIENTED_EDGE('',*,*,#12809,.T.);
#18664=ORIENTED_EDGE('',*,*,#12808,.F.);
#18665=ORIENTED_EDGE('',*,*,#12809,.F.);
#18666=ORIENTED_EDGE('',*,*,#12810,.T.);
#18667=ORIENTED_EDGE('',*,*,#12811,.F.);
#18668=ORIENTED_EDGE('',*,*,#12810,.F.);
#18669=ORIENTED_EDGE('',*,*,#12812,.T.);
#18670=ORIENTED_EDGE('',*,*,#12811,.T.);
#18671=ORIENTED_EDGE('',*,*,#12813,.F.);
#18672=ORIENTED_EDGE('',*,*,#12814,.T.);
#18673=ORIENTED_EDGE('',*,*,#12814,.F.);
#18674=ORIENTED_EDGE('',*,*,#12815,.T.);
#18675=ORIENTED_EDGE('',*,*,#12816,.T.);
#18676=ORIENTED_EDGE('',*,*,#12815,.F.);
#18677=ORIENTED_EDGE('',*,*,#12817,.F.);
#18678=ORIENTED_EDGE('',*,*,#12816,.F.);
#18679=ORIENTED_EDGE('',*,*,#12817,.T.);
#18680=ORIENTED_EDGE('',*,*,#12818,.T.);
#18681=ORIENTED_EDGE('',*,*,#12819,.T.);
#18682=ORIENTED_EDGE('',*,*,#12818,.F.);
#18683=ORIENTED_EDGE('',*,*,#12819,.F.);
#18684=ORIENTED_EDGE('',*,*,#12820,.T.);
#18685=ORIENTED_EDGE('',*,*,#12820,.F.);
#18686=ORIENTED_EDGE('',*,*,#12821,.T.);
#18687=ORIENTED_EDGE('',*,*,#12822,.T.);
#18688=ORIENTED_EDGE('',*,*,#12821,.F.);
#18689=ORIENTED_EDGE('',*,*,#12823,.F.);
#18690=ORIENTED_EDGE('',*,*,#12822,.F.);
#18691=ORIENTED_EDGE('',*,*,#12823,.T.);
#18692=ORIENTED_EDGE('',*,*,#12824,.T.);
#18693=ORIENTED_EDGE('',*,*,#12825,.T.);
#18694=ORIENTED_EDGE('',*,*,#12824,.F.);
#18695=ORIENTED_EDGE('',*,*,#12825,.F.);
#18696=ORIENTED_EDGE('',*,*,#12826,.T.);
#18697=ORIENTED_EDGE('',*,*,#12827,.T.);
#18698=ORIENTED_EDGE('',*,*,#12826,.F.);
#18699=ORIENTED_EDGE('',*,*,#12828,.F.);
#18700=ORIENTED_EDGE('',*,*,#12829,.T.);
#18701=ORIENTED_EDGE('',*,*,#12813,.T.);
#18702=ORIENTED_EDGE('',*,*,#12829,.F.);
#18703=ORIENTED_EDGE('',*,*,#12828,.T.);
#18704=ORIENTED_EDGE('',*,*,#12830,.T.);
#18705=ORIENTED_EDGE('',*,*,#12812,.F.);
#18706=ORIENTED_EDGE('',*,*,#12830,.F.);
#18707=ORIENTED_EDGE('',*,*,#12806,.T.);
#18708=ORIENTED_EDGE('',*,*,#12804,.T.);
#18709=ORIENTED_EDGE('',*,*,#12793,.F.);
#18710=ORIENTED_EDGE('',*,*,#12831,.T.);
#18711=ORIENTED_EDGE('',*,*,#12805,.T.);
#18712=ORIENTED_EDGE('',*,*,#12831,.F.);
#18713=ORIENTED_EDGE('',*,*,#12827,.F.);
#18714=ORIENTED_EDGE('',*,*,#12796,.T.);
#18715=ORIENTED_EDGE('',*,*,#12832,.F.);
#18716=ORIENTED_EDGE('',*,*,#12833,.T.);
#18717=ORIENTED_EDGE('',*,*,#12834,.T.);
#18718=ORIENTED_EDGE('',*,*,#12833,.F.);
#18719=ORIENTED_EDGE('',*,*,#12835,.F.);
#18720=ORIENTED_EDGE('',*,*,#12836,.T.);
#18721=ORIENTED_EDGE('',*,*,#12832,.T.);
#18722=ORIENTED_EDGE('',*,*,#12836,.F.);
#18723=ORIENTED_EDGE('',*,*,#12835,.T.);
#18724=ORIENTED_EDGE('',*,*,#12837,.T.);
#18725=ORIENTED_EDGE('',*,*,#12838,.F.);
#18726=ORIENTED_EDGE('',*,*,#12837,.F.);
#18727=ORIENTED_EDGE('',*,*,#12838,.T.);
#18728=ORIENTED_EDGE('',*,*,#12839,.F.);
#18729=ORIENTED_EDGE('',*,*,#12840,.F.);
#18730=ORIENTED_EDGE('',*,*,#12841,.T.);
#18731=ORIENTED_EDGE('',*,*,#12839,.T.);
#18732=ORIENTED_EDGE('',*,*,#12841,.F.);
#18733=ORIENTED_EDGE('',*,*,#12834,.F.);
#18734=ORIENTED_EDGE('',*,*,#12840,.T.);
#18735=ORIENTED_EDGE('',*,*,#12842,.F.);
#18736=ORIENTED_EDGE('',*,*,#12843,.T.);
#18737=ORIENTED_EDGE('',*,*,#12844,.T.);
#18738=ORIENTED_EDGE('',*,*,#12843,.F.);
#18739=ORIENTED_EDGE('',*,*,#12845,.F.);
#18740=ORIENTED_EDGE('',*,*,#12846,.T.);
#18741=ORIENTED_EDGE('',*,*,#12842,.T.);
#18742=ORIENTED_EDGE('',*,*,#12846,.F.);
#18743=ORIENTED_EDGE('',*,*,#12845,.T.);
#18744=ORIENTED_EDGE('',*,*,#12847,.T.);
#18745=ORIENTED_EDGE('',*,*,#12848,.F.);
#18746=ORIENTED_EDGE('',*,*,#12847,.F.);
#18747=ORIENTED_EDGE('',*,*,#12848,.T.);
#18748=ORIENTED_EDGE('',*,*,#12844,.F.);
#18749=ORIENTED_EDGE('',*,*,#12849,.F.);
#18750=ORIENTED_EDGE('',*,*,#12850,.T.);
#18751=ORIENTED_EDGE('',*,*,#12851,.T.);
#18752=ORIENTED_EDGE('',*,*,#12850,.F.);
#18753=ORIENTED_EDGE('',*,*,#12852,.F.);
#18754=ORIENTED_EDGE('',*,*,#12853,.T.);
#18755=ORIENTED_EDGE('',*,*,#12849,.T.);
#18756=ORIENTED_EDGE('',*,*,#12853,.F.);
#18757=ORIENTED_EDGE('',*,*,#12852,.T.);
#18758=ORIENTED_EDGE('',*,*,#12854,.T.);
#18759=ORIENTED_EDGE('',*,*,#12855,.F.);
#18760=ORIENTED_EDGE('',*,*,#12854,.F.);
#18761=ORIENTED_EDGE('',*,*,#12855,.T.);
#18762=ORIENTED_EDGE('',*,*,#12851,.F.);
#18763=ORIENTED_EDGE('',*,*,#12856,.F.);
#18764=ORIENTED_EDGE('',*,*,#12857,.F.);
#18765=ORIENTED_EDGE('',*,*,#12858,.T.);
#18766=ORIENTED_EDGE('',*,*,#12856,.T.);
#18767=ORIENTED_EDGE('',*,*,#12858,.F.);
#18768=ORIENTED_EDGE('',*,*,#12859,.F.);
#18769=ORIENTED_EDGE('',*,*,#12860,.T.);
#18770=ORIENTED_EDGE('',*,*,#12857,.T.);
#18771=ORIENTED_EDGE('',*,*,#12860,.F.);
#18772=ORIENTED_EDGE('',*,*,#12861,.F.);
#18773=ORIENTED_EDGE('',*,*,#12859,.T.);
#18774=ORIENTED_EDGE('',*,*,#12862,.F.);
#18775=ORIENTED_EDGE('',*,*,#12863,.T.);
#18776=ORIENTED_EDGE('',*,*,#12861,.T.);
#18777=ORIENTED_EDGE('',*,*,#12863,.F.);
#18778=ORIENTED_EDGE('',*,*,#12862,.T.);
#18779=ORIENTED_EDGE('',*,*,#12864,.T.);
#18780=ORIENTED_EDGE('',*,*,#12865,.F.);
#18781=ORIENTED_EDGE('',*,*,#12864,.F.);
#18782=ORIENTED_EDGE('',*,*,#12865,.T.);
#18783=ORIENTED_EDGE('',*,*,#12866,.F.);
#18784=ORIENTED_EDGE('',*,*,#12867,.F.);
#18785=ORIENTED_EDGE('',*,*,#12868,.T.);
#18786=ORIENTED_EDGE('',*,*,#12866,.T.);
#18787=ORIENTED_EDGE('',*,*,#12868,.F.);
#18788=ORIENTED_EDGE('',*,*,#12867,.T.);
#18789=ORIENTED_EDGE('',*,*,#12869,.F.);
#18790=ORIENTED_EDGE('',*,*,#12870,.F.);
#18791=ORIENTED_EDGE('',*,*,#12871,.T.);
#18792=ORIENTED_EDGE('',*,*,#12869,.T.);
#18793=ORIENTED_EDGE('',*,*,#12871,.F.);
#18794=ORIENTED_EDGE('',*,*,#12872,.F.);
#18795=ORIENTED_EDGE('',*,*,#12870,.T.);
#18796=ORIENTED_EDGE('',*,*,#12873,.F.);
#18797=ORIENTED_EDGE('',*,*,#12874,.T.);
#18798=ORIENTED_EDGE('',*,*,#12872,.T.);
#18799=ORIENTED_EDGE('',*,*,#12874,.F.);
#18800=ORIENTED_EDGE('',*,*,#12873,.T.);
#18801=ORIENTED_EDGE('',*,*,#12875,.T.);
#18802=ORIENTED_EDGE('',*,*,#12876,.F.);
#18803=ORIENTED_EDGE('',*,*,#12875,.F.);
#18804=ORIENTED_EDGE('',*,*,#12876,.T.);
#18805=ORIENTED_EDGE('',*,*,#12877,.F.);
#18806=ORIENTED_EDGE('',*,*,#12878,.T.);
#18807=ORIENTED_EDGE('',*,*,#12879,.T.);
#18808=ORIENTED_EDGE('',*,*,#12878,.F.);
#18809=ORIENTED_EDGE('',*,*,#12880,.F.);
#18810=ORIENTED_EDGE('',*,*,#12881,.T.);
#18811=ORIENTED_EDGE('',*,*,#12877,.T.);
#18812=ORIENTED_EDGE('',*,*,#12881,.F.);
#18813=ORIENTED_EDGE('',*,*,#12880,.T.);
#18814=ORIENTED_EDGE('',*,*,#12882,.T.);
#18815=ORIENTED_EDGE('',*,*,#12883,.F.);
#18816=ORIENTED_EDGE('',*,*,#12882,.F.);
#18817=ORIENTED_EDGE('',*,*,#12883,.T.);
#18818=ORIENTED_EDGE('',*,*,#12879,.F.);
#18819=ORIENTED_EDGE('',*,*,#12884,.F.);
#18820=ORIENTED_EDGE('',*,*,#12884,.T.);
#18821=ORIENTED_EDGE('',*,*,#12885,.F.);
#18822=ORIENTED_EDGE('',*,*,#12886,.F.);
#18823=ORIENTED_EDGE('',*,*,#12887,.T.);
#18824=ORIENTED_EDGE('',*,*,#12885,.T.);
#18825=ORIENTED_EDGE('',*,*,#12887,.F.);
#18826=ORIENTED_EDGE('',*,*,#12888,.F.);
#18827=ORIENTED_EDGE('',*,*,#12886,.T.);
#18828=ORIENTED_EDGE('',*,*,#12889,.F.);
#18829=ORIENTED_EDGE('',*,*,#12890,.T.);
#18830=ORIENTED_EDGE('',*,*,#12888,.T.);
#18831=ORIENTED_EDGE('',*,*,#12890,.F.);
#18832=ORIENTED_EDGE('',*,*,#12889,.T.);
#18833=ORIENTED_EDGE('',*,*,#12891,.T.);
#18834=ORIENTED_EDGE('',*,*,#12892,.F.);
#18835=ORIENTED_EDGE('',*,*,#12891,.F.);
#18836=ORIENTED_EDGE('',*,*,#12892,.T.);
#18837=ORIENTED_EDGE('',*,*,#12893,.F.);
#18838=ORIENTED_EDGE('',*,*,#12893,.T.);
#18839=ORIENTED_EDGE('',*,*,#12894,.F.);
#18840=ORIENTED_EDGE('',*,*,#12895,.F.);
#18841=ORIENTED_EDGE('',*,*,#12896,.T.);
#18842=ORIENTED_EDGE('',*,*,#12894,.T.);
#18843=ORIENTED_EDGE('',*,*,#12896,.F.);
#18844=ORIENTED_EDGE('',*,*,#12895,.T.);
#18845=ORIENTED_EDGE('',*,*,#12897,.T.);
#18846=ORIENTED_EDGE('',*,*,#12898,.F.);
#18847=ORIENTED_EDGE('',*,*,#12897,.F.);
#18848=ORIENTED_EDGE('',*,*,#12898,.T.);
#18849=B_SPLINE_SURFACE_WITH_KNOTS('',3,3,((#28196,#28197,#28198,#28199,
#28200,#28201,#28202,#28203,#28204,#28205,#28206,#28207,#28208,#28209,#28210,
#28211,#28212,#28213,#28214,#28215,#28216,#28217,#28218,#28219,#28220,#28221,
#28222,#28223,#28224,#28225,#28226,#28227,#28228,#28229,#28230,#28231,#28232,
#28233,#28234,#28235,#28236,#28237,#28238,#28239,#28240),(#28241,#28242,
#28243,#28244,#28245,#28246,#28247,#28248,#28249,#28250,#28251,#28252,#28253,
#28254,#28255,#28256,#28257,#28258,#28259,#28260,#28261,#28262,#28263,#28264,
#28265,#28266,#28267,#28268,#28269,#28270,#28271,#28272,#28273,#28274,#28275,
#28276,#28277,#28278,#28279,#28280,#28281,#28282,#28283,#28284,#28285),
(#28286,#28287,#28288,#28289,#28290,#28291,#28292,#28293,#28294,#28295,
#28296,#28297,#28298,#28299,#28300,#28301,#28302,#28303,#28304,#28305,#28306,
#28307,#28308,#28309,#28310,#28311,#28312,#28313,#28314,#28315,#28316,#28317,
#28318,#28319,#28320,#28321,#28322,#28323,#28324,#28325,#28326,#28327,#28328,
#28329,#28330),(#28331,#28332,#28333,#28334,#28335,#28336,#28337,#28338,
#28339,#28340,#28341,#28342,#28343,#28344,#28345,#28346,#28347,#28348,#28349,
#28350,#28351,#28352,#28353,#28354,#28355,#28356,#28357,#28358,#28359,#28360,
#28361,#28362,#28363,#28364,#28365,#28366,#28367,#28368,#28369,#28370,#28371,
#28372,#28373,#28374,#28375),(#28376,#28377,#28378,#28379,#28380,#28381,
#28382,#28383,#28384,#28385,#28386,#28387,#28388,#28389,#28390,#28391,#28392,
#28393,#28394,#28395,#28396,#28397,#28398,#28399,#28400,#28401,#28402,#28403,
#28404,#28405,#28406,#28407,#28408,#28409,#28410,#28411,#28412,#28413,#28414,
#28415,#28416,#28417,#28418,#28419,#28420),(#28421,#28422,#28423,#28424,
#28425,#28426,#28427,#28428,#28429,#28430,#28431,#28432,#28433,#28434,#28435,
#28436,#28437,#28438,#28439,#28440,#28441,#28442,#28443,#28444,#28445,#28446,
#28447,#28448,#28449,#28450,#28451,#28452,#28453,#28454,#28455,#28456,#28457,
#28458,#28459,#28460,#28461,#28462,#28463,#28464,#28465)),.UNSPECIFIED.,
 .F.,.T.,.F.,(4,1,1,4),(4,2,2,2,2,1,1,2,2,1,2,1,1,1,2,1,1,1,2,1,1,1,1,1,
1,1,1,1,1,2,1,1,4),(0.,0.285714285714286,0.571428571428571,1.00025096923236),
(-13.0076216717983,-12.6762562420903,-11.8531689108674,-11.05258106389,
-10.1188927640438,-8.47830334468407,-7.04278760274435,-6.83771392532439,
-5.90055842268743,-5.54885349043522,-5.09666143468238,-4.98988621289018,
-4.88311099109797,-4.50939771482526,-4.24245966034475,-3.88978669781647,
-3.67818292029951,-3.43131184652972,-3.11390618025428,-3.0769781504351,
-2.96619406097756,-2.81848194170084,-2.7076978522433,-2.5230577031474,-1.93220922604053,
-1.78449710676381,-1.74756907694463,-1.34136074893366,-1.04593651038022,
-0.750512271826782,-0.60979122085926,-0.469070169891739,0.),
 .UNSPECIFIED.);
#18850=B_SPLINE_SURFACE_WITH_KNOTS('',3,3,((#28856,#28857,#28858,#28859,
#28860,#28861,#28862,#28863,#28864,#28865,#28866,#28867,#28868,#28869,#28870,
#28871,#28872,#28873,#28874,#28875,#28876,#28877,#28878,#28879,#28880,#28881,
#28882,#28883,#28884,#28885,#28886,#28887,#28888,#28889,#28890,#28891,#28892,
#28893,#28894,#28895,#28896,#28897,#28898,#28899,#28900,#28901,#28902,#28903,
#28904,#28905,#28906,#28907,#28908,#28909,#28910,#28911,#28912,#28913,#28914,
#28915,#28916,#28917,#28918,#28919,#28920,#28921,#28922,#28923,#28924,#28925,
#28926,#28927,#28928,#28929,#28930,#28931,#28932,#28933,#28934,#28935,#28936,
#28937,#28938,#28939,#28940,#28941,#28942,#28943,#28944,#28945,#28946,#28947,
#28948,#28949,#28950,#28951,#28952,#28953,#28954,#28955,#28956,#28957,#28958,
#28959,#28960,#28961,#28962,#28963,#28964,#28965,#28966,#28967,#28968,#28969,
#28970,#28971,#28972,#28973,#28974,#28975,#28976,#28977,#28978,#28979,#28980,
#28981,#28982,#28983,#28984,#28985,#28986,#28987,#28988,#28989,#28990,#28991,
#28992,#28993,#28994,#28995,#28996,#28997,#28998,#28999),(#29000,#29001,
#29002,#29003,#29004,#29005,#29006,#29007,#29008,#29009,#29010,#29011,#29012,
#29013,#29014,#29015,#29016,#29017,#29018,#29019,#29020,#29021,#29022,#29023,
#29024,#29025,#29026,#29027,#29028,#29029,#29030,#29031,#29032,#29033,#29034,
#29035,#29036,#29037,#29038,#29039,#29040,#29041,#29042,#29043,#29044,#29045,
#29046,#29047,#29048,#29049,#29050,#29051,#29052,#29053,#29054,#29055,#29056,
#29057,#29058,#29059,#29060,#29061,#29062,#29063,#29064,#29065,#29066,#29067,
#29068,#29069,#29070,#29071,#29072,#29073,#29074,#29075,#29076,#29077,#29078,
#29079,#29080,#29081,#29082,#29083,#29084,#29085,#29086,#29087,#29088,#29089,
#29090,#29091,#29092,#29093,#29094,#29095,#29096,#29097,#29098,#29099,#29100,
#29101,#29102,#29103,#29104,#29105,#29106,#29107,#29108,#29109,#29110,#29111,
#29112,#29113,#29114,#29115,#29116,#29117,#29118,#29119,#29120,#29121,#29122,
#29123,#29124,#29125,#29126,#29127,#29128,#29129,#29130,#29131,#29132,#29133,
#29134,#29135,#29136,#29137,#29138,#29139,#29140,#29141,#29142,#29143),
(#29144,#29145,#29146,#29147,#29148,#29149,#29150,#29151,#29152,#29153,
#29154,#29155,#29156,#29157,#29158,#29159,#29160,#29161,#29162,#29163,#29164,
#29165,#29166,#29167,#29168,#29169,#29170,#29171,#29172,#29173,#29174,#29175,
#29176,#29177,#29178,#29179,#29180,#29181,#29182,#29183,#29184,#29185,#29186,
#29187,#29188,#29189,#29190,#29191,#29192,#29193,#29194,#29195,#29196,#29197,
#29198,#29199,#29200,#29201,#29202,#29203,#29204,#29205,#29206,#29207,#29208,
#29209,#29210,#29211,#29212,#29213,#29214,#29215,#29216,#29217,#29218,#29219,
#29220,#29221,#29222,#29223,#29224,#29225,#29226,#29227,#29228,#29229,#29230,
#29231,#29232,#29233,#29234,#29235,#29236,#29237,#29238,#29239,#29240,#29241,
#29242,#29243,#29244,#29245,#29246,#29247,#29248,#29249,#29250,#29251,#29252,
#29253,#29254,#29255,#29256,#29257,#29258,#29259,#29260,#29261,#29262,#29263,
#29264,#29265,#29266,#29267,#29268,#29269,#29270,#29271,#29272,#29273,#29274,
#29275,#29276,#29277,#29278,#29279,#29280,#29281,#29282,#29283,#29284,#29285,
#29286,#29287),(#29288,#29289,#29290,#29291,#29292,#29293,#29294,#29295,
#29296,#29297,#29298,#29299,#29300,#29301,#29302,#29303,#29304,#29305,#29306,
#29307,#29308,#29309,#29310,#29311,#29312,#29313,#29314,#29315,#29316,#29317,
#29318,#29319,#29320,#29321,#29322,#29323,#29324,#29325,#29326,#29327,#29328,
#29329,#29330,#29331,#29332,#29333,#29334,#29335,#29336,#29337,#29338,#29339,
#29340,#29341,#29342,#29343,#29344,#29345,#29346,#29347,#29348,#29349,#29350,
#29351,#29352,#29353,#29354,#29355,#29356,#29357,#29358,#29359,#29360,#29361,
#29362,#29363,#29364,#29365,#29366,#29367,#29368,#29369,#29370,#29371,#29372,
#29373,#29374,#29375,#29376,#29377,#29378,#29379,#29380,#29381,#29382,#29383,
#29384,#29385,#29386,#29387,#29388,#29389,#29390,#29391,#29392,#29393,#29394,
#29395,#29396,#29397,#29398,#29399,#29400,#29401,#29402,#29403,#29404,#29405,
#29406,#29407,#29408,#29409,#29410,#29411,#29412,#29413,#29414,#29415,#29416,
#29417,#29418,#29419,#29420,#29421,#29422,#29423,#29424,#29425,#29426,#29427,
#29428,#29429,#29430,#29431),(#29432,#29433,#29434,#29435,#29436,#29437,
#29438,#29439,#29440,#29441,#29442,#29443,#29444,#29445,#29446,#29447,#29448,
#29449,#29450,#29451,#29452,#29453,#29454,#29455,#29456,#29457,#29458,#29459,
#29460,#29461,#29462,#29463,#29464,#29465,#29466,#29467,#29468,#29469,#29470,
#29471,#29472,#29473,#29474,#29475,#29476,#29477,#29478,#29479,#29480,#29481,
#29482,#29483,#29484,#29485,#29486,#29487,#29488,#29489,#29490,#29491,#29492,
#29493,#29494,#29495,#29496,#29497,#29498,#29499,#29500,#29501,#29502,#29503,
#29504,#29505,#29506,#29507,#29508,#29509,#29510,#29511,#29512,#29513,#29514,
#29515,#29516,#29517,#29518,#29519,#29520,#29521,#29522,#29523,#29524,#29525,
#29526,#29527,#29528,#29529,#29530,#29531,#29532,#29533,#29534,#29535,#29536,
#29537,#29538,#29539,#29540,#29541,#29542,#29543,#29544,#29545,#29546,#29547,
#29548,#29549,#29550,#29551,#29552,#29553,#29554,#29555,#29556,#29557,#29558,
#29559,#29560,#29561,#29562,#29563,#29564,#29565,#29566,#29567,#29568,#29569,
#29570,#29571,#29572,#29573,#29574,#29575),(#29576,#29577,#29578,#29579,
#29580,#29581,#29582,#29583,#29584,#29585,#29586,#29587,#29588,#29589,#29590,
#29591,#29592,#29593,#29594,#29595,#29596,#29597,#29598,#29599,#29600,#29601,
#29602,#29603,#29604,#29605,#29606,#29607,#29608,#29609,#29610,#29611,#29612,
#29613,#29614,#29615,#29616,#29617,#29618,#29619,#29620,#29621,#29622,#29623,
#29624,#29625,#29626,#29627,#29628,#29629,#29630,#29631,#29632,#29633,#29634,
#29635,#29636,#29637,#29638,#29639,#29640,#29641,#29642,#29643,#29644,#29645,
#29646,#29647,#29648,#29649,#29650,#29651,#29652,#29653,#29654,#29655,#29656,
#29657,#29658,#29659,#29660,#29661,#29662,#29663,#29664,#29665,#29666,#29667,
#29668,#29669,#29670,#29671,#29672,#29673,#29674,#29675,#29676,#29677,#29678,
#29679,#29680,#29681,#29682,#29683,#29684,#29685,#29686,#29687,#29688,#29689,
#29690,#29691,#29692,#29693,#29694,#29695,#29696,#29697,#29698,#29699,#29700,
#29701,#29702,#29703,#29704,#29705,#29706,#29707,#29708,#29709,#29710,#29711,
#29712,#29713,#29714,#29715,#29716,#29717,#29718,#29719),(#29720,#29721,
#29722,#29723,#29724,#29725,#29726,#29727,#29728,#29729,#29730,#29731,#29732,
#29733,#29734,#29735,#29736,#29737,#29738,#29739,#29740,#29741,#29742,#29743,
#29744,#29745,#29746,#29747,#29748,#29749,#29750,#29751,#29752,#29753,#29754,
#29755,#29756,#29757,#29758,#29759,#29760,#29761,#29762,#29763,#29764,#29765,
#29766,#29767,#29768,#29769,#29770,#29771,#29772,#29773,#29774,#29775,#29776,
#29777,#29778,#29779,#29780,#29781,#29782,#29783,#29784,#29785,#29786,#29787,
#29788,#29789,#29790,#29791,#29792,#29793,#29794,#29795,#29796,#29797,#29798,
#29799,#29800,#29801,#29802,#29803,#29804,#29805,#29806,#29807,#29808,#29809,
#29810,#29811,#29812,#29813,#29814,#29815,#29816,#29817,#29818,#29819,#29820,
#29821,#29822,#29823,#29824,#29825,#29826,#29827,#29828,#29829,#29830,#29831,
#29832,#29833,#29834,#29835,#29836,#29837,#29838,#29839,#29840,#29841,#29842,
#29843,#29844,#29845,#29846,#29847,#29848,#29849,#29850,#29851,#29852,#29853,
#29854,#29855,#29856,#29857,#29858,#29859,#29860,#29861,#29862,#29863),
(#29864,#29865,#29866,#29867,#29868,#29869,#29870,#29871,#29872,#29873,
#29874,#29875,#29876,#29877,#29878,#29879,#29880,#29881,#29882,#29883,#29884,
#29885,#29886,#29887,#29888,#29889,#29890,#29891,#29892,#29893,#29894,#29895,
#29896,#29897,#29898,#29899,#29900,#29901,#29902,#29903,#29904,#29905,#29906,
#29907,#29908,#29909,#29910,#29911,#29912,#29913,#29914,#29915,#29916,#29917,
#29918,#29919,#29920,#29921,#29922,#29923,#29924,#29925,#29926,#29927,#29928,
#29929,#29930,#29931,#29932,#29933,#29934,#29935,#29936,#29937,#29938,#29939,
#29940,#29941,#29942,#29943,#29944,#29945,#29946,#29947,#29948,#29949,#29950,
#29951,#29952,#29953,#29954,#29955,#29956,#29957,#29958,#29959,#29960,#29961,
#29962,#29963,#29964,#29965,#29966,#29967,#29968,#29969,#29970,#29971,#29972,
#29973,#29974,#29975,#29976,#29977,#29978,#29979,#29980,#29981,#29982,#29983,
#29984,#29985,#29986,#29987,#29988,#29989,#29990,#29991,#29992,#29993,#29994,
#29995,#29996,#29997,#29998,#29999,#30000,#30001,#30002,#30003,#30004,#30005,
#30006,#30007),(#30008,#30009,#30010,#30011,#30012,#30013,#30014,#30015,
#30016,#30017,#30018,#30019,#30020,#30021,#30022,#30023,#30024,#30025,#30026,
#30027,#30028,#30029,#30030,#30031,#30032,#30033,#30034,#30035,#30036,#30037,
#30038,#30039,#30040,#30041,#30042,#30043,#30044,#30045,#30046,#30047,#30048,
#30049,#30050,#30051,#30052,#30053,#30054,#30055,#30056,#30057,#30058,#30059,
#30060,#30061,#30062,#30063,#30064,#30065,#30066,#30067,#30068,#30069,#30070,
#30071,#30072,#30073,#30074,#30075,#30076,#30077,#30078,#30079,#30080,#30081,
#30082,#30083,#30084,#30085,#30086,#30087,#30088,#30089,#30090,#30091,#30092,
#30093,#30094,#30095,#30096,#30097,#30098,#30099,#30100,#30101,#30102,#30103,
#30104,#30105,#30106,#30107,#30108,#30109,#30110,#30111,#30112,#30113,#30114,
#30115,#30116,#30117,#30118,#30119,#30120,#30121,#30122,#30123,#30124,#30125,
#30126,#30127,#30128,#30129,#30130,#30131,#30132,#30133,#30134,#30135,#30136,
#30137,#30138,#30139,#30140,#30141,#30142,#30143,#30144,#30145,#30146,#30147,
#30148,#30149,#30150,#30151),(#30152,#30153,#30154,#30155,#30156,#30157,
#30158,#30159,#30160,#30161,#30162,#30163,#30164,#30165,#30166,#30167,#30168,
#30169,#30170,#30171,#30172,#30173,#30174,#30175,#30176,#30177,#30178,#30179,
#30180,#30181,#30182,#30183,#30184,#30185,#30186,#30187,#30188,#30189,#30190,
#30191,#30192,#30193,#30194,#30195,#30196,#30197,#30198,#30199,#30200,#30201,
#30202,#30203,#30204,#30205,#30206,#30207,#30208,#30209,#30210,#30211,#30212,
#30213,#30214,#30215,#30216,#30217,#30218,#30219,#30220,#30221,#30222,#30223,
#30224,#30225,#30226,#30227,#30228,#30229,#30230,#30231,#30232,#30233,#30234,
#30235,#30236,#30237,#30238,#30239,#30240,#30241,#30242,#30243,#30244,#30245,
#30246,#30247,#30248,#30249,#30250,#30251,#30252,#30253,#30254,#30255,#30256,
#30257,#30258,#30259,#30260,#30261,#30262,#30263,#30264,#30265,#30266,#30267,
#30268,#30269,#30270,#30271,#30272,#30273,#30274,#30275,#30276,#30277,#30278,
#30279,#30280,#30281,#30282,#30283,#30284,#30285,#30286,#30287,#30288,#30289,
#30290,#30291,#30292,#30293,#30294,#30295),(#30296,#30297,#30298,#30299,
#30300,#30301,#30302,#30303,#30304,#30305,#30306,#30307,#30308,#30309,#30310,
#30311,#30312,#30313,#30314,#30315,#30316,#30317,#30318,#30319,#30320,#30321,
#30322,#30323,#30324,#30325,#30326,#30327,#30328,#30329,#30330,#30331,#30332,
#30333,#30334,#30335,#30336,#30337,#30338,#30339,#30340,#30341,#30342,#30343,
#30344,#30345,#30346,#30347,#30348,#30349,#30350,#30351,#30352,#30353,#30354,
#30355,#30356,#30357,#30358,#30359,#30360,#30361,#30362,#30363,#30364,#30365,
#30366,#30367,#30368,#30369,#30370,#30371,#30372,#30373,#30374,#30375,#30376,
#30377,#30378,#30379,#30380,#30381,#30382,#30383,#30384,#30385,#30386,#30387,
#30388,#30389,#30390,#30391,#30392,#30393,#30394,#30395,#30396,#30397,#30398,
#30399,#30400,#30401,#30402,#30403,#30404,#30405,#30406,#30407,#30408,#30409,
#30410,#30411,#30412,#30413,#30414,#30415,#30416,#30417,#30418,#30419,#30420,
#30421,#30422,#30423,#30424,#30425,#30426,#30427,#30428,#30429,#30430,#30431,
#30432,#30433,#30434,#30435,#30436,#30437,#30438,#30439),(#30440,#30441,
#30442,#30443,#30444,#30445,#30446,#30447,#30448,#30449,#30450,#30451,#30452,
#30453,#30454,#30455,#30456,#30457,#30458,#30459,#30460,#30461,#30462,#30463,
#30464,#30465,#30466,#30467,#30468,#30469,#30470,#30471,#30472,#30473,#30474,
#30475,#30476,#30477,#30478,#30479,#30480,#30481,#30482,#30483,#30484,#30485,
#30486,#30487,#30488,#30489,#30490,#30491,#30492,#30493,#30494,#30495,#30496,
#30497,#30498,#30499,#30500,#30501,#30502,#30503,#30504,#30505,#30506,#30507,
#30508,#30509,#30510,#30511,#30512,#30513,#30514,#30515,#30516,#30517,#30518,
#30519,#30520,#30521,#30522,#30523,#30524,#30525,#30526,#30527,#30528,#30529,
#30530,#30531,#30532,#30533,#30534,#30535,#30536,#30537,#30538,#30539,#30540,
#30541,#30542,#30543,#30544,#30545,#30546,#30547,#30548,#30549,#30550,#30551,
#30552,#30553,#30554,#30555,#30556,#30557,#30558,#30559,#30560,#30561,#30562,
#30563,#30564,#30565,#30566,#30567,#30568,#30569,#30570,#30571,#30572,#30573,
#30574,#30575,#30576,#30577,#30578,#30579,#30580,#30581,#30582,#30583),
(#30584,#30585,#30586,#30587,#30588,#30589,#30590,#30591,#30592,#30593,
#30594,#30595,#30596,#30597,#30598,#30599,#30600,#30601,#30602,#30603,#30604,
#30605,#30606,#30607,#30608,#30609,#30610,#30611,#30612,#30613,#30614,#30615,
#30616,#30617,#30618,#30619,#30620,#30621,#30622,#30623,#30624,#30625,#30626,
#30627,#30628,#30629,#30630,#30631,#30632,#30633,#30634,#30635,#30636,#30637,
#30638,#30639,#30640,#30641,#30642,#30643,#30644,#30645,#30646,#30647,#30648,
#30649,#30650,#30651,#30652,#30653,#30654,#30655,#30656,#30657,#30658,#30659,
#30660,#30661,#30662,#30663,#30664,#30665,#30666,#30667,#30668,#30669,#30670,
#30671,#30672,#30673,#30674,#30675,#30676,#30677,#30678,#30679,#30680,#30681,
#30682,#30683,#30684,#30685,#30686,#30687,#30688,#30689,#30690,#30691,#30692,
#30693,#30694,#30695,#30696,#30697,#30698,#30699,#30700,#30701,#30702,#30703,
#30704,#30705,#30706,#30707,#30708,#30709,#30710,#30711,#30712,#30713,#30714,
#30715,#30716,#30717,#30718,#30719,#30720,#30721,#30722,#30723,#30724,#30725,
#30726,#30727),(#30728,#30729,#30730,#30731,#30732,#30733,#30734,#30735,
#30736,#30737,#30738,#30739,#30740,#30741,#30742,#30743,#30744,#30745,#30746,
#30747,#30748,#30749,#30750,#30751,#30752,#30753,#30754,#30755,#30756,#30757,
#30758,#30759,#30760,#30761,#30762,#30763,#30764,#30765,#30766,#30767,#30768,
#30769,#30770,#30771,#30772,#30773,#30774,#30775,#30776,#30777,#30778,#30779,
#30780,#30781,#30782,#30783,#30784,#30785,#30786,#30787,#30788,#30789,#30790,
#30791,#30792,#30793,#30794,#30795,#30796,#30797,#30798,#30799,#30800,#30801,
#30802,#30803,#30804,#30805,#30806,#30807,#30808,#30809,#30810,#30811,#30812,
#30813,#30814,#30815,#30816,#30817,#30818,#30819,#30820,#30821,#30822,#30823,
#30824,#30825,#30826,#30827,#30828,#30829,#30830,#30831,#30832,#30833,#30834,
#30835,#30836,#30837,#30838,#30839,#30840,#30841,#30842,#30843,#30844,#30845,
#30846,#30847,#30848,#30849,#30850,#30851,#30852,#30853,#30854,#30855,#30856,
#30857,#30858,#30859,#30860,#30861,#30862,#30863,#30864,#30865,#30866,#30867,
#30868,#30869,#30870,#30871),(#30872,#30873,#30874,#30875,#30876,#30877,
#30878,#30879,#30880,#30881,#30882,#30883,#30884,#30885,#30886,#30887,#30888,
#30889,#30890,#30891,#30892,#30893,#30894,#30895,#30896,#30897,#30898,#30899,
#30900,#30901,#30902,#30903,#30904,#30905,#30906,#30907,#30908,#30909,#30910,
#30911,#30912,#30913,#30914,#30915,#30916,#30917,#30918,#30919,#30920,#30921,
#30922,#30923,#30924,#30925,#30926,#30927,#30928,#30929,#30930,#30931,#30932,
#30933,#30934,#30935,#30936,#30937,#30938,#30939,#30940,#30941,#30942,#30943,
#30944,#30945,#30946,#30947,#30948,#30949,#30950,#30951,#30952,#30953,#30954,
#30955,#30956,#30957,#30958,#30959,#30960,#30961,#30962,#30963,#30964,#30965,
#30966,#30967,#30968,#30969,#30970,#30971,#30972,#30973,#30974,#30975,#30976,
#30977,#30978,#30979,#30980,#30981,#30982,#30983,#30984,#30985,#30986,#30987,
#30988,#30989,#30990,#30991,#30992,#30993,#30994,#30995,#30996,#30997,#30998,
#30999,#31000,#31001,#31002,#31003,#31004,#31005,#31006,#31007,#31008,#31009,
#31010,#31011,#31012,#31013,#31014,#31015),(#31016,#31017,#31018,#31019,
#31020,#31021,#31022,#31023,#31024,#31025,#31026,#31027,#31028,#31029,#31030,
#31031,#31032,#31033,#31034,#31035,#31036,#31037,#31038,#31039,#31040,#31041,
#31042,#31043,#31044,#31045,#31046,#31047,#31048,#31049,#31050,#31051,#31052,
#31053,#31054,#31055,#31056,#31057,#31058,#31059,#31060,#31061,#31062,#31063,
#31064,#31065,#31066,#31067,#31068,#31069,#31070,#31071,#31072,#31073,#31074,
#31075,#31076,#31077,#31078,#31079,#31080,#31081,#31082,#31083,#31084,#31085,
#31086,#31087,#31088,#31089,#31090,#31091,#31092,#31093,#31094,#31095,#31096,
#31097,#31098,#31099,#31100,#31101,#31102,#31103,#31104,#31105,#31106,#31107,
#31108,#31109,#31110,#31111,#31112,#31113,#31114,#31115,#31116,#31117,#31118,
#31119,#31120,#31121,#31122,#31123,#31124,#31125,#31126,#31127,#31128,#31129,
#31130,#31131,#31132,#31133,#31134,#31135,#31136,#31137,#31138,#31139,#31140,
#31141,#31142,#31143,#31144,#31145,#31146,#31147,#31148,#31149,#31150,#31151,
#31152,#31153,#31154,#31155,#31156,#31157,#31158,#31159),(#31160,#31161,
#31162,#31163,#31164,#31165,#31166,#31167,#31168,#31169,#31170,#31171,#31172,
#31173,#31174,#31175,#31176,#31177,#31178,#31179,#31180,#31181,#31182,#31183,
#31184,#31185,#31186,#31187,#31188,#31189,#31190,#31191,#31192,#31193,#31194,
#31195,#31196,#31197,#31198,#31199,#31200,#31201,#31202,#31203,#31204,#31205,
#31206,#31207,#31208,#31209,#31210,#31211,#31212,#31213,#31214,#31215,#31216,
#31217,#31218,#31219,#31220,#31221,#31222,#31223,#31224,#31225,#31226,#31227,
#31228,#31229,#31230,#31231,#31232,#31233,#31234,#31235,#31236,#31237,#31238,
#31239,#31240,#31241,#31242,#31243,#31244,#31245,#31246,#31247,#31248,#31249,
#31250,#31251,#31252,#31253,#31254,#31255,#31256,#31257,#31258,#31259,#31260,
#31261,#31262,#31263,#31264,#31265,#31266,#31267,#31268,#31269,#31270,#31271,
#31272,#31273,#31274,#31275,#31276,#31277,#31278,#31279,#31280,#31281,#31282,
#31283,#31284,#31285,#31286,#31287,#31288,#31289,#31290,#31291,#31292,#31293,
#31294,#31295,#31296,#31297,#31298,#31299,#31300,#31301,#31302,#31303),
(#31304,#31305,#31306,#31307,#31308,#31309,#31310,#31311,#31312,#31313,
#31314,#31315,#31316,#31317,#31318,#31319,#31320,#31321,#31322,#31323,#31324,
#31325,#31326,#31327,#31328,#31329,#31330,#31331,#31332,#31333,#31334,#31335,
#31336,#31337,#31338,#31339,#31340,#31341,#31342,#31343,#31344,#31345,#31346,
#31347,#31348,#31349,#31350,#31351,#31352,#31353,#31354,#31355,#31356,#31357,
#31358,#31359,#31360,#31361,#31362,#31363,#31364,#31365,#31366,#31367,#31368,
#31369,#31370,#31371,#31372,#31373,#31374,#31375,#31376,#31377,#31378,#31379,
#31380,#31381,#31382,#31383,#31384,#31385,#31386,#31387,#31388,#31389,#31390,
#31391,#31392,#31393,#31394,#31395,#31396,#31397,#31398,#31399,#31400,#31401,
#31402,#31403,#31404,#31405,#31406,#31407,#31408,#31409,#31410,#31411,#31412,
#31413,#31414,#31415,#31416,#31417,#31418,#31419,#31420,#31421,#31422,#31423,
#31424,#31425,#31426,#31427,#31428,#31429,#31430,#31431,#31432,#31433,#31434,
#31435,#31436,#31437,#31438,#31439,#31440,#31441,#31442,#31443,#31444,#31445,
#31446,#31447),(#31448,#31449,#31450,#31451,#31452,#31453,#31454,#31455,
#31456,#31457,#31458,#31459,#31460,#31461,#31462,#31463,#31464,#31465,#31466,
#31467,#31468,#31469,#31470,#31471,#31472,#31473,#31474,#31475,#31476,#31477,
#31478,#31479,#31480,#31481,#31482,#31483,#31484,#31485,#31486,#31487,#31488,
#31489,#31490,#31491,#31492,#31493,#31494,#31495,#31496,#31497,#31498,#31499,
#31500,#31501,#31502,#31503,#31504,#31505,#31506,#31507,#31508,#31509,#31510,
#31511,#31512,#31513,#31514,#31515,#31516,#31517,#31518,#31519,#31520,#31521,
#31522,#31523,#31524,#31525,#31526,#31527,#31528,#31529,#31530,#31531,#31532,
#31533,#31534,#31535,#31536,#31537,#31538,#31539,#31540,#31541,#31542,#31543,
#31544,#31545,#31546,#31547,#31548,#31549,#31550,#31551,#31552,#31553,#31554,
#31555,#31556,#31557,#31558,#31559,#31560,#31561,#31562,#31563,#31564,#31565,
#31566,#31567,#31568,#31569,#31570,#31571,#31572,#31573,#31574,#31575,#31576,
#31577,#31578,#31579,#31580,#31581,#31582,#31583,#31584,#31585,#31586,#31587,
#31588,#31589,#31590,#31591),(#31592,#31593,#31594,#31595,#31596,#31597,
#31598,#31599,#31600,#31601,#31602,#31603,#31604,#31605,#31606,#31607,#31608,
#31609,#31610,#31611,#31612,#31613,#31614,#31615,#31616,#31617,#31618,#31619,
#31620,#31621,#31622,#31623,#31624,#31625,#31626,#31627,#31628,#31629,#31630,
#31631,#31632,#31633,#31634,#31635,#31636,#31637,#31638,#31639,#31640,#31641,
#31642,#31643,#31644,#31645,#31646,#31647,#31648,#31649,#31650,#31651,#31652,
#31653,#31654,#31655,#31656,#31657,#31658,#31659,#31660,#31661,#31662,#31663,
#31664,#31665,#31666,#31667,#31668,#31669,#31670,#31671,#31672,#31673,#31674,
#31675,#31676,#31677,#31678,#31679,#31680,#31681,#31682,#31683,#31684,#31685,
#31686,#31687,#31688,#31689,#31690,#31691,#31692,#31693,#31694,#31695,#31696,
#31697,#31698,#31699,#31700,#31701,#31702,#31703,#31704,#31705,#31706,#31707,
#31708,#31709,#31710,#31711,#31712,#31713,#31714,#31715,#31716,#31717,#31718,
#31719,#31720,#31721,#31722,#31723,#31724,#31725,#31726,#31727,#31728,#31729,
#31730,#31731,#31732,#31733,#31734,#31735),(#31736,#31737,#31738,#31739,
#31740,#31741,#31742,#31743,#31744,#31745,#31746,#31747,#31748,#31749,#31750,
#31751,#31752,#31753,#31754,#31755,#31756,#31757,#31758,#31759,#31760,#31761,
#31762,#31763,#31764,#31765,#31766,#31767,#31768,#31769,#31770,#31771,#31772,
#31773,#31774,#31775,#31776,#31777,#31778,#31779,#31780,#31781,#31782,#31783,
#31784,#31785,#31786,#31787,#31788,#31789,#31790,#31791,#31792,#31793,#31794,
#31795,#31796,#31797,#31798,#31799,#31800,#31801,#31802,#31803,#31804,#31805,
#31806,#31807,#31808,#31809,#31810,#31811,#31812,#31813,#31814,#31815,#31816,
#31817,#31818,#31819,#31820,#31821,#31822,#31823,#31824,#31825,#31826,#31827,
#31828,#31829,#31830,#31831,#31832,#31833,#31834,#31835,#31836,#31837,#31838,
#31839,#31840,#31841,#31842,#31843,#31844,#31845,#31846,#31847,#31848,#31849,
#31850,#31851,#31852,#31853,#31854,#31855,#31856,#31857,#31858,#31859,#31860,
#31861,#31862,#31863,#31864,#31865,#31866,#31867,#31868,#31869,#31870,#31871,
#31872,#31873,#31874,#31875,#31876,#31877,#31878,#31879),(#31880,#31881,
#31882,#31883,#31884,#31885,#31886,#31887,#31888,#31889,#31890,#31891,#31892,
#31893,#31894,#31895,#31896,#31897,#31898,#31899,#31900,#31901,#31902,#31903,
#31904,#31905,#31906,#31907,#31908,#31909,#31910,#31911,#31912,#31913,#31914,
#31915,#31916,#31917,#31918,#31919,#31920,#31921,#31922,#31923,#31924,#31925,
#31926,#31927,#31928,#31929,#31930,#31931,#31932,#31933,#31934,#31935,#31936,
#31937,#31938,#31939,#31940,#31941,#31942,#31943,#31944,#31945,#31946,#31947,
#31948,#31949,#31950,#31951,#31952,#31953,#31954,#31955,#31956,#31957,#31958,
#31959,#31960,#31961,#31962,#31963,#31964,#31965,#31966,#31967,#31968,#31969,
#31970,#31971,#31972,#31973,#31974,#31975,#31976,#31977,#31978,#31979,#31980,
#31981,#31982,#31983,#31984,#31985,#31986,#31987,#31988,#31989,#31990,#31991,
#31992,#31993,#31994,#31995,#31996,#31997,#31998,#31999,#32000,#32001,#32002,
#32003,#32004,#32005,#32006,#32007,#32008,#32009,#32010,#32011,#32012,#32013,
#32014,#32015,#32016,#32017,#32018,#32019,#32020,#32021,#32022,#32023),
(#32024,#32025,#32026,#32027,#32028,#32029,#32030,#32031,#32032,#32033,
#32034,#32035,#32036,#32037,#32038,#32039,#32040,#32041,#32042,#32043,#32044,
#32045,#32046,#32047,#32048,#32049,#32050,#32051,#32052,#32053,#32054,#32055,
#32056,#32057,#32058,#32059,#32060,#32061,#32062,#32063,#32064,#32065,#32066,
#32067,#32068,#32069,#32070,#32071,#32072,#32073,#32074,#32075,#32076,#32077,
#32078,#32079,#32080,#32081,#32082,#32083,#32084,#32085,#32086,#32087,#32088,
#32089,#32090,#32091,#32092,#32093,#32094,#32095,#32096,#32097,#32098,#32099,
#32100,#32101,#32102,#32103,#32104,#32105,#32106,#32107,#32108,#32109,#32110,
#32111,#32112,#32113,#32114,#32115,#32116,#32117,#32118,#32119,#32120,#32121,
#32122,#32123,#32124,#32125,#32126,#32127,#32128,#32129,#32130,#32131,#32132,
#32133,#32134,#32135,#32136,#32137,#32138,#32139,#32140,#32141,#32142,#32143,
#32144,#32145,#32146,#32147,#32148,#32149,#32150,#32151,#32152,#32153,#32154,
#32155,#32156,#32157,#32158,#32159,#32160,#32161,#32162,#32163,#32164,#32165,
#32166,#32167),(#32168,#32169,#32170,#32171,#32172,#32173,#32174,#32175,
#32176,#32177,#32178,#32179,#32180,#32181,#32182,#32183,#32184,#32185,#32186,
#32187,#32188,#32189,#32190,#32191,#32192,#32193,#32194,#32195,#32196,#32197,
#32198,#32199,#32200,#32201,#32202,#32203,#32204,#32205,#32206,#32207,#32208,
#32209,#32210,#32211,#32212,#32213,#32214,#32215,#32216,#32217,#32218,#32219,
#32220,#32221,#32222,#32223,#32224,#32225,#32226,#32227,#32228,#32229,#32230,
#32231,#32232,#32233,#32234,#32235,#32236,#32237,#32238,#32239,#32240,#32241,
#32242,#32243,#32244,#32245,#32246,#32247,#32248,#32249,#32250,#32251,#32252,
#32253,#32254,#32255,#32256,#32257,#32258,#32259,#32260,#32261,#32262,#32263,
#32264,#32265,#32266,#32267,#32268,#32269,#32270,#32271,#32272,#32273,#32274,
#32275,#32276,#32277,#32278,#32279,#32280,#32281,#32282,#32283,#32284,#32285,
#32286,#32287,#32288,#32289,#32290,#32291,#32292,#32293,#32294,#32295,#32296,
#32297,#32298,#32299,#32300,#32301,#32302,#32303,#32304,#32305,#32306,#32307,
#32308,#32309,#32310,#32311),(#32312,#32313,#32314,#32315,#32316,#32317,
#32318,#32319,#32320,#32321,#32322,#32323,#32324,#32325,#32326,#32327,#32328,
#32329,#32330,#32331,#32332,#32333,#32334,#32335,#32336,#32337,#32338,#32339,
#32340,#32341,#32342,#32343,#32344,#32345,#32346,#32347,#32348,#32349,#32350,
#32351,#32352,#32353,#32354,#32355,#32356,#32357,#32358,#32359,#32360,#32361,
#32362,#32363,#32364,#32365,#32366,#32367,#32368,#32369,#32370,#32371,#32372,
#32373,#32374,#32375,#32376,#32377,#32378,#32379,#32380,#32381,#32382,#32383,
#32384,#32385,#32386,#32387,#32388,#32389,#32390,#32391,#32392,#32393,#32394,
#32395,#32396,#32397,#32398,#32399,#32400,#32401,#32402,#32403,#32404,#32405,
#32406,#32407,#32408,#32409,#32410,#32411,#32412,#32413,#32414,#32415,#32416,
#32417,#32418,#32419,#32420,#32421,#32422,#32423,#32424,#32425,#32426,#32427,
#32428,#32429,#32430,#32431,#32432,#32433,#32434,#32435,#32436,#32437,#32438,
#32439,#32440,#32441,#32442,#32443,#32444,#32445,#32446,#32447,#32448,#32449,
#32450,#32451,#32452,#32453,#32454,#32455),(#32456,#32457,#32458,#32459,
#32460,#32461,#32462,#32463,#32464,#32465,#32466,#32467,#32468,#32469,#32470,
#32471,#32472,#32473,#32474,#32475,#32476,#32477,#32478,#32479,#32480,#32481,
#32482,#32483,#32484,#32485,#32486,#32487,#32488,#32489,#32490,#32491,#32492,
#32493,#32494,#32495,#32496,#32497,#32498,#32499,#32500,#32501,#32502,#32503,
#32504,#32505,#32506,#32507,#32508,#32509,#32510,#32511,#32512,#32513,#32514,
#32515,#32516,#32517,#32518,#32519,#32520,#32521,#32522,#32523,#32524,#32525,
#32526,#32527,#32528,#32529,#32530,#32531,#32532,#32533,#32534,#32535,#32536,
#32537,#32538,#32539,#32540,#32541,#32542,#32543,#32544,#32545,#32546,#32547,
#32548,#32549,#32550,#32551,#32552,#32553,#32554,#32555,#32556,#32557,#32558,
#32559,#32560,#32561,#32562,#32563,#32564,#32565,#32566,#32567,#32568,#32569,
#32570,#32571,#32572,#32573,#32574,#32575,#32576,#32577,#32578,#32579,#32580,
#32581,#32582,#32583,#32584,#32585,#32586,#32587,#32588,#32589,#32590,#32591,
#32592,#32593,#32594,#32595,#32596,#32597,#32598,#32599),(#32600,#32601,
#32602,#32603,#32604,#32605,#32606,#32607,#32608,#32609,#32610,#32611,#32612,
#32613,#32614,#32615,#32616,#32617,#32618,#32619,#32620,#32621,#32622,#32623,
#32624,#32625,#32626,#32627,#32628,#32629,#32630,#32631,#32632,#32633,#32634,
#32635,#32636,#32637,#32638,#32639,#32640,#32641,#32642,#32643,#32644,#32645,
#32646,#32647,#32648,#32649,#32650,#32651,#32652,#32653,#32654,#32655,#32656,
#32657,#32658,#32659,#32660,#32661,#32662,#32663,#32664,#32665,#32666,#32667,
#32668,#32669,#32670,#32671,#32672,#32673,#32674,#32675,#32676,#32677,#32678,
#32679,#32680,#32681,#32682,#32683,#32684,#32685,#32686,#32687,#32688,#32689,
#32690,#32691,#32692,#32693,#32694,#32695,#32696,#32697,#32698,#32699,#32700,
#32701,#32702,#32703,#32704,#32705,#32706,#32707,#32708,#32709,#32710,#32711,
#32712,#32713,#32714,#32715,#32716,#32717,#32718,#32719,#32720,#32721,#32722,
#32723,#32724,#32725,#32726,#32727,#32728,#32729,#32730,#32731,#32732,#32733,
#32734,#32735,#32736,#32737,#32738,#32739,#32740,#32741,#32742,#32743),
(#32744,#32745,#32746,#32747,#32748,#32749,#32750,#32751,#32752,#32753,
#32754,#32755,#32756,#32757,#32758,#32759,#32760,#32761,#32762,#32763,#32764,
#32765,#32766,#32767,#32768,#32769,#32770,#32771,#32772,#32773,#32774,#32775,
#32776,#32777,#32778,#32779,#32780,#32781,#32782,#32783,#32784,#32785,#32786,
#32787,#32788,#32789,#32790,#32791,#32792,#32793,#32794,#32795,#32796,#32797,
#32798,#32799,#32800,#32801,#32802,#32803,#32804,#32805,#32806,#32807,#32808,
#32809,#32810,#32811,#32812,#32813,#32814,#32815,#32816,#32817,#32818,#32819,
#32820,#32821,#32822,#32823,#32824,#32825,#32826,#32827,#32828,#32829,#32830,
#32831,#32832,#32833,#32834,#32835,#32836,#32837,#32838,#32839,#32840,#32841,
#32842,#32843,#32844,#32845,#32846,#32847,#32848,#32849,#32850,#32851,#32852,
#32853,#32854,#32855,#32856,#32857,#32858,#32859,#32860,#32861,#32862,#32863,
#32864,#32865,#32866,#32867,#32868,#32869,#32870,#32871,#32872,#32873,#32874,
#32875,#32876,#32877,#32878,#32879,#32880,#32881,#32882,#32883,#32884,#32885,
#32886,#32887),(#32888,#32889,#32890,#32891,#32892,#32893,#32894,#32895,
#32896,#32897,#32898,#32899,#32900,#32901,#32902,#32903,#32904,#32905,#32906,
#32907,#32908,#32909,#32910,#32911,#32912,#32913,#32914,#32915,#32916,#32917,
#32918,#32919,#32920,#32921,#32922,#32923,#32924,#32925,#32926,#32927,#32928,
#32929,#32930,#32931,#32932,#32933,#32934,#32935,#32936,#32937,#32938,#32939,
#32940,#32941,#32942,#32943,#32944,#32945,#32946,#32947,#32948,#32949,#32950,
#32951,#32952,#32953,#32954,#32955,#32956,#32957,#32958,#32959,#32960,#32961,
#32962,#32963,#32964,#32965,#32966,#32967,#32968,#32969,#32970,#32971,#32972,
#32973,#32974,#32975,#32976,#32977,#32978,#32979,#32980,#32981,#32982,#32983,
#32984,#32985,#32986,#32987,#32988,#32989,#32990,#32991,#32992,#32993,#32994,
#32995,#32996,#32997,#32998,#32999,#33000,#33001,#33002,#33003,#33004,#33005,
#33006,#33007,#33008,#33009,#33010,#33011,#33012,#33013,#33014,#33015,#33016,
#33017,#33018,#33019,#33020,#33021,#33022,#33023,#33024,#33025,#33026,#33027,
#33028,#33029,#33030,#33031),(#33032,#33033,#33034,#33035,#33036,#33037,
#33038,#33039,#33040,#33041,#33042,#33043,#33044,#33045,#33046,#33047,#33048,
#33049,#33050,#33051,#33052,#33053,#33054,#33055,#33056,#33057,#33058,#33059,
#33060,#33061,#33062,#33063,#33064,#33065,#33066,#33067,#33068,#33069,#33070,
#33071,#33072,#33073,#33074,#33075,#33076,#33077,#33078,#33079,#33080,#33081,
#33082,#33083,#33084,#33085,#33086,#33087,#33088,#33089,#33090,#33091,#33092,
#33093,#33094,#33095,#33096,#33097,#33098,#33099,#33100,#33101,#33102,#33103,
#33104,#33105,#33106,#33107,#33108,#33109,#33110,#33111,#33112,#33113,#33114,
#33115,#33116,#33117,#33118,#33119,#33120,#33121,#33122,#33123,#33124,#33125,
#33126,#33127,#33128,#33129,#33130,#33131,#33132,#33133,#33134,#33135,#33136,
#33137,#33138,#33139,#33140,#33141,#33142,#33143,#33144,#33145,#33146,#33147,
#33148,#33149,#33150,#33151,#33152,#33153,#33154,#33155,#33156,#33157,#33158,
#33159,#33160,#33161,#33162,#33163,#33164,#33165,#33166,#33167,#33168,#33169,
#33170,#33171,#33172,#33173,#33174,#33175),(#33176,#33177,#33178,#33179,
#33180,#33181,#33182,#33183,#33184,#33185,#33186,#33187,#33188,#33189,#33190,
#33191,#33192,#33193,#33194,#33195,#33196,#33197,#33198,#33199,#33200,#33201,
#33202,#33203,#33204,#33205,#33206,#33207,#33208,#33209,#33210,#33211,#33212,
#33213,#33214,#33215,#33216,#33217,#33218,#33219,#33220,#33221,#33222,#33223,
#33224,#33225,#33226,#33227,#33228,#33229,#33230,#33231,#33232,#33233,#33234,
#33235,#33236,#33237,#33238,#33239,#33240,#33241,#33242,#33243,#33244,#33245,
#33246,#33247,#33248,#33249,#33250,#33251,#33252,#33253,#33254,#33255,#33256,
#33257,#33258,#33259,#33260,#33261,#33262,#33263,#33264,#33265,#33266,#33267,
#33268,#33269,#33270,#33271,#33272,#33273,#33274,#33275,#33276,#33277,#33278,
#33279,#33280,#33281,#33282,#33283,#33284,#33285,#33286,#33287,#33288,#33289,
#33290,#33291,#33292,#33293,#33294,#33295,#33296,#33297,#33298,#33299,#33300,
#33301,#33302,#33303,#33304,#33305,#33306,#33307,#33308,#33309,#33310,#33311,
#33312,#33313,#33314,#33315,#33316,#33317,#33318,#33319),(#33320,#33321,
#33322,#33323,#33324,#33325,#33326,#33327,#33328,#33329,#33330,#33331,#33332,
#33333,#33334,#33335,#33336,#33337,#33338,#33339,#33340,#33341,#33342,#33343,
#33344,#33345,#33346,#33347,#33348,#33349,#33350,#33351,#33352,#33353,#33354,
#33355,#33356,#33357,#33358,#33359,#33360,#33361,#33362,#33363,#33364,#33365,
#33366,#33367,#33368,#33369,#33370,#33371,#33372,#33373,#33374,#33375,#33376,
#33377,#33378,#33379,#33380,#33381,#33382,#33383,#33384,#33385,#33386,#33387,
#33388,#33389,#33390,#33391,#33392,#33393,#33394,#33395,#33396,#33397,#33398,
#33399,#33400,#33401,#33402,#33403,#33404,#33405,#33406,#33407,#33408,#33409,
#33410,#33411,#33412,#33413,#33414,#33415,#33416,#33417,#33418,#33419,#33420,
#33421,#33422,#33423,#33424,#33425,#33426,#33427,#33428,#33429,#33430,#33431,
#33432,#33433,#33434,#33435,#33436,#33437,#33438,#33439,#33440,#33441,#33442,
#33443,#33444,#33445,#33446,#33447,#33448,#33449,#33450,#33451,#33452,#33453,
#33454,#33455,#33456,#33457,#33458,#33459,#33460,#33461,#33462,#33463),
(#33464,#33465,#33466,#33467,#33468,#33469,#33470,#33471,#33472,#33473,
#33474,#33475,#33476,#33477,#33478,#33479,#33480,#33481,#33482,#33483,#33484,
#33485,#33486,#33487,#33488,#33489,#33490,#33491,#33492,#33493,#33494,#33495,
#33496,#33497,#33498,#33499,#33500,#33501,#33502,#33503,#33504,#33505,#33506,
#33507,#33508,#33509,#33510,#33511,#33512,#33513,#33514,#33515,#33516,#33517,
#33518,#33519,#33520,#33521,#33522,#33523,#33524,#33525,#33526,#33527,#33528,
#33529,#33530,#33531,#33532,#33533,#33534,#33535,#33536,#33537,#33538,#33539,
#33540,#33541,#33542,#33543,#33544,#33545,#33546,#33547,#33548,#33549,#33550,
#33551,#33552,#33553,#33554,#33555,#33556,#33557,#33558,#33559,#33560,#33561,
#33562,#33563,#33564,#33565,#33566,#33567,#33568,#33569,#33570,#33571,#33572,
#33573,#33574,#33575,#33576,#33577,#33578,#33579,#33580,#33581,#33582,#33583,
#33584,#33585,#33586,#33587,#33588,#33589,#33590,#33591,#33592,#33593,#33594,
#33595,#33596,#33597,#33598,#33599,#33600,#33601,#33602,#33603,#33604,#33605,
#33606,#33607),(#33608,#33609,#33610,#33611,#33612,#33613,#33614,#33615,
#33616,#33617,#33618,#33619,#33620,#33621,#33622,#33623,#33624,#33625,#33626,
#33627,#33628,#33629,#33630,#33631,#33632,#33633,#33634,#33635,#33636,#33637,
#33638,#33639,#33640,#33641,#33642,#33643,#33644,#33645,#33646,#33647,#33648,
#33649,#33650,#33651,#33652,#33653,#33654,#33655,#33656,#33657,#33658,#33659,
#33660,#33661,#33662,#33663,#33664,#33665,#33666,#33667,#33668,#33669,#33670,
#33671,#33672,#33673,#33674,#33675,#33676,#33677,#33678,#33679,#33680,#33681,
#33682,#33683,#33684,#33685,#33686,#33687,#33688,#33689,#33690,#33691,#33692,
#33693,#33694,#33695,#33696,#33697,#33698,#33699,#33700,#33701,#33702,#33703,
#33704,#33705,#33706,#33707,#33708,#33709,#33710,#33711,#33712,#33713,#33714,
#33715,#33716,#33717,#33718,#33719,#33720,#33721,#33722,#33723,#33724,#33725,
#33726,#33727,#33728,#33729,#33730,#33731,#33732,#33733,#33734,#33735,#33736,
#33737,#33738,#33739,#33740,#33741,#33742,#33743,#33744,#33745,#33746,#33747,
#33748,#33749,#33750,#33751),(#33752,#33753,#33754,#33755,#33756,#33757,
#33758,#33759,#33760,#33761,#33762,#33763,#33764,#33765,#33766,#33767,#33768,
#33769,#33770,#33771,#33772,#33773,#33774,#33775,#33776,#33777,#33778,#33779,
#33780,#33781,#33782,#33783,#33784,#33785,#33786,#33787,#33788,#33789,#33790,
#33791,#33792,#33793,#33794,#33795,#33796,#33797,#33798,#33799,#33800,#33801,
#33802,#33803,#33804,#33805,#33806,#33807,#33808,#33809,#33810,#33811,#33812,
#33813,#33814,#33815,#33816,#33817,#33818,#33819,#33820,#33821,#33822,#33823,
#33824,#33825,#33826,#33827,#33828,#33829,#33830,#33831,#33832,#33833,#33834,
#33835,#33836,#33837,#33838,#33839,#33840,#33841,#33842,#33843,#33844,#33845,
#33846,#33847,#33848,#33849,#33850,#33851,#33852,#33853,#33854,#33855,#33856,
#33857,#33858,#33859,#33860,#33861,#33862,#33863,#33864,#33865,#33866,#33867,
#33868,#33869,#33870,#33871,#33872,#33873,#33874,#33875,#33876,#33877,#33878,
#33879,#33880,#33881,#33882,#33883,#33884,#33885,#33886,#33887,#33888,#33889,
#33890,#33891,#33892,#33893,#33894,#33895),(#33896,#33897,#33898,#33899,
#33900,#33901,#33902,#33903,#33904,#33905,#33906,#33907,#33908,#33909,#33910,
#33911,#33912,#33913,#33914,#33915,#33916,#33917,#33918,#33919,#33920,#33921,
#33922,#33923,#33924,#33925,#33926,#33927,#33928,#33929,#33930,#33931,#33932,
#33933,#33934,#33935,#33936,#33937,#33938,#33939,#33940,#33941,#33942,#33943,
#33944,#33945,#33946,#33947,#33948,#33949,#33950,#33951,#33952,#33953,#33954,
#33955,#33956,#33957,#33958,#33959,#33960,#33961,#33962,#33963,#33964,#33965,
#33966,#33967,#33968,#33969,#33970,#33971,#33972,#33973,#33974,#33975,#33976,
#33977,#33978,#33979,#33980,#33981,#33982,#33983,#33984,#33985,#33986,#33987,
#33988,#33989,#33990,#33991,#33992,#33993,#33994,#33995,#33996,#33997,#33998,
#33999,#34000,#34001,#34002,#34003,#34004,#34005,#34006,#34007,#34008,#34009,
#34010,#34011,#34012,#34013,#34014,#34015,#34016,#34017,#34018,#34019,#34020,
#34021,#34022,#34023,#34024,#34025,#34026,#34027,#34028,#34029,#34030,#34031,
#34032,#34033,#34034,#34035,#34036,#34037,#34038,#34039),(#34040,#34041,
#34042,#34043,#34044,#34045,#34046,#34047,#34048,#34049,#34050,#34051,#34052,
#34053,#34054,#34055,#34056,#34057,#34058,#34059,#34060,#34061,#34062,#34063,
#34064,#34065,#34066,#34067,#34068,#34069,#34070,#34071,#34072,#34073,#34074,
#34075,#34076,#34077,#34078,#34079,#34080,#34081,#34082,#34083,#34084,#34085,
#34086,#34087,#34088,#34089,#34090,#34091,#34092,#34093,#34094,#34095,#34096,
#34097,#34098,#34099,#34100,#34101,#34102,#34103,#34104,#34105,#34106,#34107,
#34108,#34109,#34110,#34111,#34112,#34113,#34114,#34115,#34116,#34117,#34118,
#34119,#34120,#34121,#34122,#34123,#34124,#34125,#34126,#34127,#34128,#34129,
#34130,#34131,#34132,#34133,#34134,#34135,#34136,#34137,#34138,#34139,#34140,
#34141,#34142,#34143,#34144,#34145,#34146,#34147,#34148,#34149,#34150,#34151,
#34152,#34153,#34154,#34155,#34156,#34157,#34158,#34159,#34160,#34161,#34162,
#34163,#34164,#34165,#34166,#34167,#34168,#34169,#34170,#34171,#34172,#34173,
#34174,#34175,#34176,#34177,#34178,#34179,#34180,#34181,#34182,#34183),
(#34184,#34185,#34186,#34187,#34188,#34189,#34190,#34191,#34192,#34193,
#34194,#34195,#34196,#34197,#34198,#34199,#34200,#34201,#34202,#34203,#34204,
#34205,#34206,#34207,#34208,#34209,#34210,#34211,#34212,#34213,#34214,#34215,
#34216,#34217,#34218,#34219,#34220,#34221,#34222,#34223,#34224,#34225,#34226,
#34227,#34228,#34229,#34230,#34231,#34232,#34233,#34234,#34235,#34236,#34237,
#34238,#34239,#34240,#34241,#34242,#34243,#34244,#34245,#34246,#34247,#34248,
#34249,#34250,#34251,#34252,#34253,#34254,#34255,#34256,#34257,#34258,#34259,
#34260,#34261,#34262,#34263,#34264,#34265,#34266,#34267,#34268,#34269,#34270,
#34271,#34272,#34273,#34274,#34275,#34276,#34277,#34278,#34279,#34280,#34281,
#34282,#34283,#34284,#34285,#34286,#34287,#34288,#34289,#34290,#34291,#34292,
#34293,#34294,#34295,#34296,#34297,#34298,#34299,#34300,#34301,#34302,#34303,
#34304,#34305,#34306,#34307,#34308,#34309,#34310,#34311,#34312,#34313,#34314,
#34315,#34316,#34317,#34318,#34319,#34320,#34321,#34322,#34323,#34324,#34325,
#34326,#34327),(#34328,#34329,#34330,#34331,#34332,#34333,#34334,#34335,
#34336,#34337,#34338,#34339,#34340,#34341,#34342,#34343,#34344,#34345,#34346,
#34347,#34348,#34349,#34350,#34351,#34352,#34353,#34354,#34355,#34356,#34357,
#34358,#34359,#34360,#34361,#34362,#34363,#34364,#34365,#34366,#34367,#34368,
#34369,#34370,#34371,#34372,#34373,#34374,#34375,#34376,#34377,#34378,#34379,
#34380,#34381,#34382,#34383,#34384,#34385,#34386,#34387,#34388,#34389,#34390,
#34391,#34392,#34393,#34394,#34395,#34396,#34397,#34398,#34399,#34400,#34401,
#34402,#34403,#34404,#34405,#34406,#34407,#34408,#34409,#34410,#34411,#34412,
#34413,#34414,#34415,#34416,#34417,#34418,#34419,#34420,#34421,#34422,#34423,
#34424,#34425,#34426,#34427,#34428,#34429,#34430,#34431,#34432,#34433,#34434,
#34435,#34436,#34437,#34438,#34439,#34440,#34441,#34442,#34443,#34444,#34445,
#34446,#34447,#34448,#34449,#34450,#34451,#34452,#34453,#34454,#34455,#34456,
#34457,#34458,#34459,#34460,#34461,#34462,#34463,#34464,#34465,#34466,#34467,
#34468,#34469,#34470,#34471),(#34472,#34473,#34474,#34475,#34476,#34477,
#34478,#34479,#34480,#34481,#34482,#34483,#34484,#34485,#34486,#34487,#34488,
#34489,#34490,#34491,#34492,#34493,#34494,#34495,#34496,#34497,#34498,#34499,
#34500,#34501,#34502,#34503,#34504,#34505,#34506,#34507,#34508,#34509,#34510,
#34511,#34512,#34513,#34514,#34515,#34516,#34517,#34518,#34519,#34520,#34521,
#34522,#34523,#34524,#34525,#34526,#34527,#34528,#34529,#34530,#34531,#34532,
#34533,#34534,#34535,#34536,#34537,#34538,#34539,#34540,#34541,#34542,#34543,
#34544,#34545,#34546,#34547,#34548,#34549,#34550,#34551,#34552,#34553,#34554,
#34555,#34556,#34557,#34558,#34559,#34560,#34561,#34562,#34563,#34564,#34565,
#34566,#34567,#34568,#34569,#34570,#34571,#34572,#34573,#34574,#34575,#34576,
#34577,#34578,#34579,#34580,#34581,#34582,#34583,#34584,#34585,#34586,#34587,
#34588,#34589,#34590,#34591,#34592,#34593,#34594,#34595,#34596,#34597,#34598,
#34599,#34600,#34601,#34602,#34603,#34604,#34605,#34606,#34607,#34608,#34609,
#34610,#34611,#34612,#34613,#34614,#34615),(#34616,#34617,#34618,#34619,
#34620,#34621,#34622,#34623,#34624,#34625,#34626,#34627,#34628,#34629,#34630,
#34631,#34632,#34633,#34634,#34635,#34636,#34637,#34638,#34639,#34640,#34641,
#34642,#34643,#34644,#34645,#34646,#34647,#34648,#34649,#34650,#34651,#34652,
#34653,#34654,#34655,#34656,#34657,#34658,#34659,#34660,#34661,#34662,#34663,
#34664,#34665,#34666,#34667,#34668,#34669,#34670,#34671,#34672,#34673,#34674,
#34675,#34676,#34677,#34678,#34679,#34680,#34681,#34682,#34683,#34684,#34685,
#34686,#34687,#34688,#34689,#34690,#34691,#34692,#34693,#34694,#34695,#34696,
#34697,#34698,#34699,#34700,#34701,#34702,#34703,#34704,#34705,#34706,#34707,
#34708,#34709,#34710,#34711,#34712,#34713,#34714,#34715,#34716,#34717,#34718,
#34719,#34720,#34721,#34722,#34723,#34724,#34725,#34726,#34727,#34728,#34729,
#34730,#34731,#34732,#34733,#34734,#34735,#34736,#34737,#34738,#34739,#34740,
#34741,#34742,#34743,#34744,#34745,#34746,#34747,#34748,#34749,#34750,#34751,
#34752,#34753,#34754,#34755,#34756,#34757,#34758,#34759),(#34760,#34761,
#34762,#34763,#34764,#34765,#34766,#34767,#34768,#34769,#34770,#34771,#34772,
#34773,#34774,#34775,#34776,#34777,#34778,#34779,#34780,#34781,#34782,#34783,
#34784,#34785,#34786,#34787,#34788,#34789,#34790,#34791,#34792,#34793,#34794,
#34795,#34796,#34797,#34798,#34799,#34800,#34801,#34802,#34803,#34804,#34805,
#34806,#34807,#34808,#34809,#34810,#34811,#34812,#34813,#34814,#34815,#34816,
#34817,#34818,#34819,#34820,#34821,#34822,#34823,#34824,#34825,#34826,#34827,
#34828,#34829,#34830,#34831,#34832,#34833,#34834,#34835,#34836,#34837,#34838,
#34839,#34840,#34841,#34842,#34843,#34844,#34845,#34846,#34847,#34848,#34849,
#34850,#34851,#34852,#34853,#34854,#34855,#34856,#34857,#34858,#34859,#34860,
#34861,#34862,#34863,#34864,#34865,#34866,#34867,#34868,#34869,#34870,#34871,
#34872,#34873,#34874,#34875,#34876,#34877,#34878,#34879,#34880,#34881,#34882,
#34883,#34884,#34885,#34886,#34887,#34888,#34889,#34890,#34891,#34892,#34893,
#34894,#34895,#34896,#34897,#34898,#34899,#34900,#34901,#34902,#34903),
(#34904,#34905,#34906,#34907,#34908,#34909,#34910,#34911,#34912,#34913,
#34914,#34915,#34916,#34917,#34918,#34919,#34920,#34921,#34922,#34923,#34924,
#34925,#34926,#34927,#34928,#34929,#34930,#34931,#34932,#34933,#34934,#34935,
#34936,#34937,#34938,#34939,#34940,#34941,#34942,#34943,#34944,#34945,#34946,
#34947,#34948,#34949,#34950,#34951,#34952,#34953,#34954,#34955,#34956,#34957,
#34958,#34959,#34960,#34961,#34962,#34963,#34964,#34965,#34966,#34967,#34968,
#34969,#34970,#34971,#34972,#34973,#34974,#34975,#34976,#34977,#34978,#34979,
#34980,#34981,#34982,#34983,#34984,#34985,#34986,#34987,#34988,#34989,#34990,
#34991,#34992,#34993,#34994,#34995,#34996,#34997,#34998,#34999,#35000,#35001,
#35002,#35003,#35004,#35005,#35006,#35007,#35008,#35009,#35010,#35011,#35012,
#35013,#35014,#35015,#35016,#35017,#35018,#35019,#35020,#35021,#35022,#35023,
#35024,#35025,#35026,#35027,#35028,#35029,#35030,#35031,#35032,#35033,#35034,
#35035,#35036,#35037,#35038,#35039,#35040,#35041,#35042,#35043,#35044,#35045,
#35046,#35047),(#35048,#35049,#35050,#35051,#35052,#35053,#35054,#35055,
#35056,#35057,#35058,#35059,#35060,#35061,#35062,#35063,#35064,#35065,#35066,
#35067,#35068,#35069,#35070,#35071,#35072,#35073,#35074,#35075,#35076,#35077,
#35078,#35079,#35080,#35081,#35082,#35083,#35084,#35085,#35086,#35087,#35088,
#35089,#35090,#35091,#35092,#35093,#35094,#35095,#35096,#35097,#35098,#35099,
#35100,#35101,#35102,#35103,#35104,#35105,#35106,#35107,#35108,#35109,#35110,
#35111,#35112,#35113,#35114,#35115,#35116,#35117,#35118,#35119,#35120,#35121,
#35122,#35123,#35124,#35125,#35126,#35127,#35128,#35129,#35130,#35131,#35132,
#35133,#35134,#35135,#35136,#35137,#35138,#35139,#35140,#35141,#35142,#35143,
#35144,#35145,#35146,#35147,#35148,#35149,#35150,#35151,#35152,#35153,#35154,
#35155,#35156,#35157,#35158,#35159,#35160,#35161,#35162,#35163,#35164,#35165,
#35166,#35167,#35168,#35169,#35170,#35171,#35172,#35173,#35174,#35175,#35176,
#35177,#35178,#35179,#35180,#35181,#35182,#35183,#35184,#35185,#35186,#35187,
#35188,#35189,#35190,#35191),(#35192,#35193,#35194,#35195,#35196,#35197,
#35198,#35199,#35200,#35201,#35202,#35203,#35204,#35205,#35206,#35207,#35208,
#35209,#35210,#35211,#35212,#35213,#35214,#35215,#35216,#35217,#35218,#35219,
#35220,#35221,#35222,#35223,#35224,#35225,#35226,#35227,#35228,#35229,#35230,
#35231,#35232,#35233,#35234,#35235,#35236,#35237,#35238,#35239,#35240,#35241,
#35242,#35243,#35244,#35245,#35246,#35247,#35248,#35249,#35250,#35251,#35252,
#35253,#35254,#35255,#35256,#35257,#35258,#35259,#35260,#35261,#35262,#35263,
#35264,#35265,#35266,#35267,#35268,#35269,#35270,#35271,#35272,#35273,#35274,
#35275,#35276,#35277,#35278,#35279,#35280,#35281,#35282,#35283,#35284,#35285,
#35286,#35287,#35288,#35289,#35290,#35291,#35292,#35293,#35294,#35295,#35296,
#35297,#35298,#35299,#35300,#35301,#35302,#35303,#35304,#35305,#35306,#35307,
#35308,#35309,#35310,#35311,#35312,#35313,#35314,#35315,#35316,#35317,#35318,
#35319,#35320,#35321,#35322,#35323,#35324,#35325,#35326,#35327,#35328,#35329,
#35330,#35331,#35332,#35333,#35334,#35335),(#35336,#35337,#35338,#35339,
#35340,#35341,#35342,#35343,#35344,#35345,#35346,#35347,#35348,#35349,#35350,
#35351,#35352,#35353,#35354,#35355,#35356,#35357,#35358,#35359,#35360,#35361,
#35362,#35363,#35364,#35365,#35366,#35367,#35368,#35369,#35370,#35371,#35372,
#35373,#35374,#35375,#35376,#35377,#35378,#35379,#35380,#35381,#35382,#35383,
#35384,#35385,#35386,#35387,#35388,#35389,#35390,#35391,#35392,#35393,#35394,
#35395,#35396,#35397,#35398,#35399,#35400,#35401,#35402,#35403,#35404,#35405,
#35406,#35407,#35408,#35409,#35410,#35411,#35412,#35413,#35414,#35415,#35416,
#35417,#35418,#35419,#35420,#35421,#35422,#35423,#35424,#35425,#35426,#35427,
#35428,#35429,#35430,#35431,#35432,#35433,#35434,#35435,#35436,#35437,#35438,
#35439,#35440,#35441,#35442,#35443,#35444,#35445,#35446,#35447,#35448,#35449,
#35450,#35451,#35452,#35453,#35454,#35455,#35456,#35457,#35458,#35459,#35460,
#35461,#35462,#35463,#35464,#35465,#35466,#35467,#35468,#35469,#35470,#35471,
#35472,#35473,#35474,#35475,#35476,#35477,#35478,#35479),(#35480,#35481,
#35482,#35483,#35484,#35485,#35486,#35487,#35488,#35489,#35490,#35491,#35492,
#35493,#35494,#35495,#35496,#35497,#35498,#35499,#35500,#35501,#35502,#35503,
#35504,#35505,#35506,#35507,#35508,#35509,#35510,#35511,#35512,#35513,#35514,
#35515,#35516,#35517,#35518,#35519,#35520,#35521,#35522,#35523,#35524,#35525,
#35526,#35527,#35528,#35529,#35530,#35531,#35532,#35533,#35534,#35535,#35536,
#35537,#35538,#35539,#35540,#35541,#35542,#35543,#35544,#35545,#35546,#35547,
#35548,#35549,#35550,#35551,#35552,#35553,#35554,#35555,#35556,#35557,#35558,
#35559,#35560,#35561,#35562,#35563,#35564,#35565,#35566,#35567,#35568,#35569,
#35570,#35571,#35572,#35573,#35574,#35575,#35576,#35577,#35578,#35579,#35580,
#35581,#35582,#35583,#35584,#35585,#35586,#35587,#35588,#35589,#35590,#35591,
#35592,#35593,#35594,#35595,#35596,#35597,#35598,#35599,#35600,#35601,#35602,
#35603,#35604,#35605,#35606,#35607,#35608,#35609,#35610,#35611,#35612,#35613,
#35614,#35615,#35616,#35617,#35618,#35619,#35620,#35621,#35622,#35623),
(#35624,#35625,#35626,#35627,#35628,#35629,#35630,#35631,#35632,#35633,
#35634,#35635,#35636,#35637,#35638,#35639,#35640,#35641,#35642,#35643,#35644,
#35645,#35646,#35647,#35648,#35649,#35650,#35651,#35652,#35653,#35654,#35655,
#35656,#35657,#35658,#35659,#35660,#35661,#35662,#35663,#35664,#35665,#35666,
#35667,#35668,#35669,#35670,#35671,#35672,#35673,#35674,#35675,#35676,#35677,
#35678,#35679,#35680,#35681,#35682,#35683,#35684,#35685,#35686,#35687,#35688,
#35689,#35690,#35691,#35692,#35693,#35694,#35695,#35696,#35697,#35698,#35699,
#35700,#35701,#35702,#35703,#35704,#35705,#35706,#35707,#35708,#35709,#35710,
#35711,#35712,#35713,#35714,#35715,#35716,#35717,#35718,#35719,#35720,#35721,
#35722,#35723,#35724,#35725,#35726,#35727,#35728,#35729,#35730,#35731,#35732,
#35733,#35734,#35735,#35736,#35737,#35738,#35739,#35740,#35741,#35742,#35743,
#35744,#35745,#35746,#35747,#35748,#35749,#35750,#35751,#35752,#35753,#35754,
#35755,#35756,#35757,#35758,#35759,#35760,#35761,#35762,#35763,#35764,#35765,
#35766,#35767),(#35768,#35769,#35770,#35771,#35772,#35773,#35774,#35775,
#35776,#35777,#35778,#35779,#35780,#35781,#35782,#35783,#35784,#35785,#35786,
#35787,#35788,#35789,#35790,#35791,#35792,#35793,#35794,#35795,#35796,#35797,
#35798,#35799,#35800,#35801,#35802,#35803,#35804,#35805,#35806,#35807,#35808,
#35809,#35810,#35811,#35812,#35813,#35814,#35815,#35816,#35817,#35818,#35819,
#35820,#35821,#35822,#35823,#35824,#35825,#35826,#35827,#35828,#35829,#35830,
#35831,#35832,#35833,#35834,#35835,#35836,#35837,#35838,#35839,#35840,#35841,
#35842,#35843,#35844,#35845,#35846,#35847,#35848,#35849,#35850,#35851,#35852,
#35853,#35854,#35855,#35856,#35857,#35858,#35859,#35860,#35861,#35862,#35863,
#35864,#35865,#35866,#35867,#35868,#35869,#35870,#35871,#35872,#35873,#35874,
#35875,#35876,#35877,#35878,#35879,#35880,#35881,#35882,#35883,#35884,#35885,
#35886,#35887,#35888,#35889,#35890,#35891,#35892,#35893,#35894,#35895,#35896,
#35897,#35898,#35899,#35900,#35901,#35902,#35903,#35904,#35905,#35906,#35907,
#35908,#35909,#35910,#35911),(#35912,#35913,#35914,#35915,#35916,#35917,
#35918,#35919,#35920,#35921,#35922,#35923,#35924,#35925,#35926,#35927,#35928,
#35929,#35930,#35931,#35932,#35933,#35934,#35935,#35936,#35937,#35938,#35939,
#35940,#35941,#35942,#35943,#35944,#35945,#35946,#35947,#35948,#35949,#35950,
#35951,#35952,#35953,#35954,#35955,#35956,#35957,#35958,#35959,#35960,#35961,
#35962,#35963,#35964,#35965,#35966,#35967,#35968,#35969,#35970,#35971,#35972,
#35973,#35974,#35975,#35976,#35977,#35978,#35979,#35980,#35981,#35982,#35983,
#35984,#35985,#35986,#35987,#35988,#35989,#35990,#35991,#35992,#35993,#35994,
#35995,#35996,#35997,#35998,#35999,#36000,#36001,#36002,#36003,#36004,#36005,
#36006,#36007,#36008,#36009,#36010,#36011,#36012,#36013,#36014,#36015,#36016,
#36017,#36018,#36019,#36020,#36021,#36022,#36023,#36024,#36025,#36026,#36027,
#36028,#36029,#36030,#36031,#36032,#36033,#36034,#36035,#36036,#36037,#36038,
#36039,#36040,#36041,#36042,#36043,#36044,#36045,#36046,#36047,#36048,#36049,
#36050,#36051,#36052,#36053,#36054,#36055),(#36056,#36057,#36058,#36059,
#36060,#36061,#36062,#36063,#36064,#36065,#36066,#36067,#36068,#36069,#36070,
#36071,#36072,#36073,#36074,#36075,#36076,#36077,#36078,#36079,#36080,#36081,
#36082,#36083,#36084,#36085,#36086,#36087,#36088,#36089,#36090,#36091,#36092,
#36093,#36094,#36095,#36096,#36097,#36098,#36099,#36100,#36101,#36102,#36103,
#36104,#36105,#36106,#36107,#36108,#36109,#36110,#36111,#36112,#36113,#36114,
#36115,#36116,#36117,#36118,#36119,#36120,#36121,#36122,#36123,#36124,#36125,
#36126,#36127,#36128,#36129,#36130,#36131,#36132,#36133,#36134,#36135,#36136,
#36137,#36138,#36139,#36140,#36141,#36142,#36143,#36144,#36145,#36146,#36147,
#36148,#36149,#36150,#36151,#36152,#36153,#36154,#36155,#36156,#36157,#36158,
#36159,#36160,#36161,#36162,#36163,#36164,#36165,#36166,#36167,#36168,#36169,
#36170,#36171,#36172,#36173,#36174,#36175,#36176,#36177,#36178,#36179,#36180,
#36181,#36182,#36183,#36184,#36185,#36186,#36187,#36188,#36189,#36190,#36191,
#36192,#36193,#36194,#36195,#36196,#36197,#36198,#36199),(#36200,#36201,
#36202,#36203,#36204,#36205,#36206,#36207,#36208,#36209,#36210,#36211,#36212,
#36213,#36214,#36215,#36216,#36217,#36218,#36219,#36220,#36221,#36222,#36223,
#36224,#36225,#36226,#36227,#36228,#36229,#36230,#36231,#36232,#36233,#36234,
#36235,#36236,#36237,#36238,#36239,#36240,#36241,#36242,#36243,#36244,#36245,
#36246,#36247,#36248,#36249,#36250,#36251,#36252,#36253,#36254,#36255,#36256,
#36257,#36258,#36259,#36260,#36261,#36262,#36263,#36264,#36265,#36266,#36267,
#36268,#36269,#36270,#36271,#36272,#36273,#36274,#36275,#36276,#36277,#36278,
#36279,#36280,#36281,#36282,#36283,#36284,#36285,#36286,#36287,#36288,#36289,
#36290,#36291,#36292,#36293,#36294,#36295,#36296,#36297,#36298,#36299,#36300,
#36301,#36302,#36303,#36304,#36305,#36306,#36307,#36308,#36309,#36310,#36311,
#36312,#36313,#36314,#36315,#36316,#36317,#36318,#36319,#36320,#36321,#36322,
#36323,#36324,#36325,#36326,#36327,#36328,#36329,#36330,#36331,#36332,#36333,
#36334,#36335,#36336,#36337,#36338,#36339,#36340,#36341,#36342,#36343),
(#36344,#36345,#36346,#36347,#36348,#36349,#36350,#36351,#36352,#36353,
#36354,#36355,#36356,#36357,#36358,#36359,#36360,#36361,#36362,#36363,#36364,
#36365,#36366,#36367,#36368,#36369,#36370,#36371,#36372,#36373,#36374,#36375,
#36376,#36377,#36378,#36379,#36380,#36381,#36382,#36383,#36384,#36385,#36386,
#36387,#36388,#36389,#36390,#36391,#36392,#36393,#36394,#36395,#36396,#36397,
#36398,#36399,#36400,#36401,#36402,#36403,#36404,#36405,#36406,#36407,#36408,
#36409,#36410,#36411,#36412,#36413,#36414,#36415,#36416,#36417,#36418,#36419,
#36420,#36421,#36422,#36423,#36424,#36425,#36426,#36427,#36428,#36429,#36430,
#36431,#36432,#36433,#36434,#36435,#36436,#36437,#36438,#36439,#36440,#36441,
#36442,#36443,#36444,#36445,#36446,#36447,#36448,#36449,#36450,#36451,#36452,
#36453,#36454,#36455,#36456,#36457,#36458,#36459,#36460,#36461,#36462,#36463,
#36464,#36465,#36466,#36467,#36468,#36469,#36470,#36471,#36472,#36473,#36474,
#36475,#36476,#36477,#36478,#36479,#36480,#36481,#36482,#36483,#36484,#36485,
#36486,#36487),(#36488,#36489,#36490,#36491,#36492,#36493,#36494,#36495,
#36496,#36497,#36498,#36499,#36500,#36501,#36502,#36503,#36504,#36505,#36506,
#36507,#36508,#36509,#36510,#36511,#36512,#36513,#36514,#36515,#36516,#36517,
#36518,#36519,#36520,#36521,#36522,#36523,#36524,#36525,#36526,#36527,#36528,
#36529,#36530,#36531,#36532,#36533,#36534,#36535,#36536,#36537,#36538,#36539,
#36540,#36541,#36542,#36543,#36544,#36545,#36546,#36547,#36548,#36549,#36550,
#36551,#36552,#36553,#36554,#36555,#36556,#36557,#36558,#36559,#36560,#36561,
#36562,#36563,#36564,#36565,#36566,#36567,#36568,#36569,#36570,#36571,#36572,
#36573,#36574,#36575,#36576,#36577,#36578,#36579,#36580,#36581,#36582,#36583,
#36584,#36585,#36586,#36587,#36588,#36589,#36590,#36591,#36592,#36593,#36594,
#36595,#36596,#36597,#36598,#36599,#36600,#36601,#36602,#36603,#36604,#36605,
#36606,#36607,#36608,#36609,#36610,#36611,#36612,#36613,#36614,#36615,#36616,
#36617,#36618,#36619,#36620,#36621,#36622,#36623,#36624,#36625,#36626,#36627,
#36628,#36629,#36630,#36631),(#36632,#36633,#36634,#36635,#36636,#36637,
#36638,#36639,#36640,#36641,#36642,#36643,#36644,#36645,#36646,#36647,#36648,
#36649,#36650,#36651,#36652,#36653,#36654,#36655,#36656,#36657,#36658,#36659,
#36660,#36661,#36662,#36663,#36664,#36665,#36666,#36667,#36668,#36669,#36670,
#36671,#36672,#36673,#36674,#36675,#36676,#36677,#36678,#36679,#36680,#36681,
#36682,#36683,#36684,#36685,#36686,#36687,#36688,#36689,#36690,#36691,#36692,
#36693,#36694,#36695,#36696,#36697,#36698,#36699,#36700,#36701,#36702,#36703,
#36704,#36705,#36706,#36707,#36708,#36709,#36710,#36711,#36712,#36713,#36714,
#36715,#36716,#36717,#36718,#36719,#36720,#36721,#36722,#36723,#36724,#36725,
#36726,#36727,#36728,#36729,#36730,#36731,#36732,#36733,#36734,#36735,#36736,
#36737,#36738,#36739,#36740,#36741,#36742,#36743,#36744,#36745,#36746,#36747,
#36748,#36749,#36750,#36751,#36752,#36753,#36754,#36755,#36756,#36757,#36758,
#36759,#36760,#36761,#36762,#36763,#36764,#36765,#36766,#36767,#36768,#36769,
#36770,#36771,#36772,#36773,#36774,#36775),(#36776,#36777,#36778,#36779,
#36780,#36781,#36782,#36783,#36784,#36785,#36786,#36787,#36788,#36789,#36790,
#36791,#36792,#36793,#36794,#36795,#36796,#36797,#36798,#36799,#36800,#36801,
#36802,#36803,#36804,#36805,#36806,#36807,#36808,#36809,#36810,#36811,#36812,
#36813,#36814,#36815,#36816,#36817,#36818,#36819,#36820,#36821,#36822,#36823,
#36824,#36825,#36826,#36827,#36828,#36829,#36830,#36831,#36832,#36833,#36834,
#36835,#36836,#36837,#36838,#36839,#36840,#36841,#36842,#36843,#36844,#36845,
#36846,#36847,#36848,#36849,#36850,#36851,#36852,#36853,#36854,#36855,#36856,
#36857,#36858,#36859,#36860,#36861,#36862,#36863,#36864,#36865,#36866,#36867,
#36868,#36869,#36870,#36871,#36872,#36873,#36874,#36875,#36876,#36877,#36878,
#36879,#36880,#36881,#36882,#36883,#36884,#36885,#36886,#36887,#36888,#36889,
#36890,#36891,#36892,#36893,#36894,#36895,#36896,#36897,#36898,#36899,#36900,
#36901,#36902,#36903,#36904,#36905,#36906,#36907,#36908,#36909,#36910,#36911,
#36912,#36913,#36914,#36915,#36916,#36917,#36918,#36919),(#36920,#36921,
#36922,#36923,#36924,#36925,#36926,#36927,#36928,#36929,#36930,#36931,#36932,
#36933,#36934,#36935,#36936,#36937,#36938,#36939,#36940,#36941,#36942,#36943,
#36944,#36945,#36946,#36947,#36948,#36949,#36950,#36951,#36952,#36953,#36954,
#36955,#36956,#36957,#36958,#36959,#36960,#36961,#36962,#36963,#36964,#36965,
#36966,#36967,#36968,#36969,#36970,#36971,#36972,#36973,#36974,#36975,#36976,
#36977,#36978,#36979,#36980,#36981,#36982,#36983,#36984,#36985,#36986,#36987,
#36988,#36989,#36990,#36991,#36992,#36993,#36994,#36995,#36996,#36997,#36998,
#36999,#37000,#37001,#37002,#37003,#37004,#37005,#37006,#37007,#37008,#37009,
#37010,#37011,#37012,#37013,#37014,#37015,#37016,#37017,#37018,#37019,#37020,
#37021,#37022,#37023,#37024,#37025,#37026,#37027,#37028,#37029,#37030,#37031,
#37032,#37033,#37034,#37035,#37036,#37037,#37038,#37039,#37040,#37041,#37042,
#37043,#37044,#37045,#37046,#37047,#37048,#37049,#37050,#37051,#37052,#37053,
#37054,#37055,#37056,#37057,#37058,#37059,#37060,#37061,#37062,#37063),
(#37064,#37065,#37066,#37067,#37068,#37069,#37070,#37071,#37072,#37073,
#37074,#37075,#37076,#37077,#37078,#37079,#37080,#37081,#37082,#37083,#37084,
#37085,#37086,#37087,#37088,#37089,#37090,#37091,#37092,#37093,#37094,#37095,
#37096,#37097,#37098,#37099,#37100,#37101,#37102,#37103,#37104,#37105,#37106,
#37107,#37108,#37109,#37110,#37111,#37112,#37113,#37114,#37115,#37116,#37117,
#37118,#37119,#37120,#37121,#37122,#37123,#37124,#37125,#37126,#37127,#37128,
#37129,#37130,#37131,#37132,#37133,#37134,#37135,#37136,#37137,#37138,#37139,
#37140,#37141,#37142,#37143,#37144,#37145,#37146,#37147,#37148,#37149,#37150,
#37151,#37152,#37153,#37154,#37155,#37156,#37157,#37158,#37159,#37160,#37161,
#37162,#37163,#37164,#37165,#37166,#37167,#37168,#37169,#37170,#37171,#37172,
#37173,#37174,#37175,#37176,#37177,#37178,#37179,#37180,#37181,#37182,#37183,
#37184,#37185,#37186,#37187,#37188,#37189,#37190,#37191,#37192,#37193,#37194,
#37195,#37196,#37197,#37198,#37199,#37200,#37201,#37202,#37203,#37204,#37205,
#37206,#37207),(#37208,#37209,#37210,#37211,#37212,#37213,#37214,#37215,
#37216,#37217,#37218,#37219,#37220,#37221,#37222,#37223,#37224,#37225,#37226,
#37227,#37228,#37229,#37230,#37231,#37232,#37233,#37234,#37235,#37236,#37237,
#37238,#37239,#37240,#37241,#37242,#37243,#37244,#37245,#37246,#37247,#37248,
#37249,#37250,#37251,#37252,#37253,#37254,#37255,#37256,#37257,#37258,#37259,
#37260,#37261,#37262,#37263,#37264,#37265,#37266,#37267,#37268,#37269,#37270,
#37271,#37272,#37273,#37274,#37275,#37276,#37277,#37278,#37279,#37280,#37281,
#37282,#37283,#37284,#37285,#37286,#37287,#37288,#37289,#37290,#37291,#37292,
#37293,#37294,#37295,#37296,#37297,#37298,#37299,#37300,#37301,#37302,#37303,
#37304,#37305,#37306,#37307,#37308,#37309,#37310,#37311,#37312,#37313,#37314,
#37315,#37316,#37317,#37318,#37319,#37320,#37321,#37322,#37323,#37324,#37325,
#37326,#37327,#37328,#37329,#37330,#37331,#37332,#37333,#37334,#37335,#37336,
#37337,#37338,#37339,#37340,#37341,#37342,#37343,#37344,#37345,#37346,#37347,
#37348,#37349,#37350,#37351),(#37352,#37353,#37354,#37355,#37356,#37357,
#37358,#37359,#37360,#37361,#37362,#37363,#37364,#37365,#37366,#37367,#37368,
#37369,#37370,#37371,#37372,#37373,#37374,#37375,#37376,#37377,#37378,#37379,
#37380,#37381,#37382,#37383,#37384,#37385,#37386,#37387,#37388,#37389,#37390,
#37391,#37392,#37393,#37394,#37395,#37396,#37397,#37398,#37399,#37400,#37401,
#37402,#37403,#37404,#37405,#37406,#37407,#37408,#37409,#37410,#37411,#37412,
#37413,#37414,#37415,#37416,#37417,#37418,#37419,#37420,#37421,#37422,#37423,
#37424,#37425,#37426,#37427,#37428,#37429,#37430,#37431,#37432,#37433,#37434,
#37435,#37436,#37437,#37438,#37439,#37440,#37441,#37442,#37443,#37444,#37445,
#37446,#37447,#37448,#37449,#37450,#37451,#37452,#37453,#37454,#37455,#37456,
#37457,#37458,#37459,#37460,#37461,#37462,#37463,#37464,#37465,#37466,#37467,
#37468,#37469,#37470,#37471,#37472,#37473,#37474,#37475,#37476,#37477,#37478,
#37479,#37480,#37481,#37482,#37483,#37484,#37485,#37486,#37487,#37488,#37489,
#37490,#37491,#37492,#37493,#37494,#37495),(#37496,#37497,#37498,#37499,
#37500,#37501,#37502,#37503,#37504,#37505,#37506,#37507,#37508,#37509,#37510,
#37511,#37512,#37513,#37514,#37515,#37516,#37517,#37518,#37519,#37520,#37521,
#37522,#37523,#37524,#37525,#37526,#37527,#37528,#37529,#37530,#37531,#37532,
#37533,#37534,#37535,#37536,#37537,#37538,#37539,#37540,#37541,#37542,#37543,
#37544,#37545,#37546,#37547,#37548,#37549,#37550,#37551,#37552,#37553,#37554,
#37555,#37556,#37557,#37558,#37559,#37560,#37561,#37562,#37563,#37564,#37565,
#37566,#37567,#37568,#37569,#37570,#37571,#37572,#37573,#37574,#37575,#37576,
#37577,#37578,#37579,#37580,#37581,#37582,#37583,#37584,#37585,#37586,#37587,
#37588,#37589,#37590,#37591,#37592,#37593,#37594,#37595,#37596,#37597,#37598,
#37599,#37600,#37601,#37602,#37603,#37604,#37605,#37606,#37607,#37608,#37609,
#37610,#37611,#37612,#37613,#37614,#37615,#37616,#37617,#37618,#37619,#37620,
#37621,#37622,#37623,#37624,#37625,#37626,#37627,#37628,#37629,#37630,#37631,
#37632,#37633,#37634,#37635,#37636,#37637,#37638,#37639),(#37640,#37641,
#37642,#37643,#37644,#37645,#37646,#37647,#37648,#37649,#37650,#37651,#37652,
#37653,#37654,#37655,#37656,#37657,#37658,#37659,#37660,#37661,#37662,#37663,
#37664,#37665,#37666,#37667,#37668,#37669,#37670,#37671,#37672,#37673,#37674,
#37675,#37676,#37677,#37678,#37679,#37680,#37681,#37682,#37683,#37684,#37685,
#37686,#37687,#37688,#37689,#37690,#37691,#37692,#37693,#37694,#37695,#37696,
#37697,#37698,#37699,#37700,#37701,#37702,#37703,#37704,#37705,#37706,#37707,
#37708,#37709,#37710,#37711,#37712,#37713,#37714,#37715,#37716,#37717,#37718,
#37719,#37720,#37721,#37722,#37723,#37724,#37725,#37726,#37727,#37728,#37729,
#37730,#37731,#37732,#37733,#37734,#37735,#37736,#37737,#37738,#37739,#37740,
#37741,#37742,#37743,#37744,#37745,#37746,#37747,#37748,#37749,#37750,#37751,
#37752,#37753,#37754,#37755,#37756,#37757,#37758,#37759,#37760,#37761,#37762,
#37763,#37764,#37765,#37766,#37767,#37768,#37769,#37770,#37771,#37772,#37773,
#37774,#37775,#37776,#37777,#37778,#37779,#37780,#37781,#37782,#37783),
(#37784,#37785,#37786,#37787,#37788,#37789,#37790,#37791,#37792,#37793,
#37794,#37795,#37796,#37797,#37798,#37799,#37800,#37801,#37802,#37803,#37804,
#37805,#37806,#37807,#37808,#37809,#37810,#37811,#37812,#37813,#37814,#37815,
#37816,#37817,#37818,#37819,#37820,#37821,#37822,#37823,#37824,#37825,#37826,
#37827,#37828,#37829,#37830,#37831,#37832,#37833,#37834,#37835,#37836,#37837,
#37838,#37839,#37840,#37841,#37842,#37843,#37844,#37845,#37846,#37847,#37848,
#37849,#37850,#37851,#37852,#37853,#37854,#37855,#37856,#37857,#37858,#37859,
#37860,#37861,#37862,#37863,#37864,#37865,#37866,#37867,#37868,#37869,#37870,
#37871,#37872,#37873,#37874,#37875,#37876,#37877,#37878,#37879,#37880,#37881,
#37882,#37883,#37884,#37885,#37886,#37887,#37888,#37889,#37890,#37891,#37892,
#37893,#37894,#37895,#37896,#37897,#37898,#37899,#37900,#37901,#37902,#37903,
#37904,#37905,#37906,#37907,#37908,#37909,#37910,#37911,#37912,#37913,#37914,
#37915,#37916,#37917,#37918,#37919,#37920,#37921,#37922,#37923,#37924,#37925,
#37926,#37927),(#37928,#37929,#37930,#37931,#37932,#37933,#37934,#37935,
#37936,#37937,#37938,#37939,#37940,#37941,#37942,#37943,#37944,#37945,#37946,
#37947,#37948,#37949,#37950,#37951,#37952,#37953,#37954,#37955,#37956,#37957,
#37958,#37959,#37960,#37961,#37962,#37963,#37964,#37965,#37966,#37967,#37968,
#37969,#37970,#37971,#37972,#37973,#37974,#37975,#37976,#37977,#37978,#37979,
#37980,#37981,#37982,#37983,#37984,#37985,#37986,#37987,#37988,#37989,#37990,
#37991,#37992,#37993,#37994,#37995,#37996,#37997,#37998,#37999,#38000,#38001,
#38002,#38003,#38004,#38005,#38006,#38007,#38008,#38009,#38010,#38011,#38012,
#38013,#38014,#38015,#38016,#38017,#38018,#38019,#38020,#38021,#38022,#38023,
#38024,#38025,#38026,#38027,#38028,#38029,#38030,#38031,#38032,#38033,#38034,
#38035,#38036,#38037,#38038,#38039,#38040,#38041,#38042,#38043,#38044,#38045,
#38046,#38047,#38048,#38049,#38050,#38051,#38052,#38053,#38054,#38055,#38056,
#38057,#38058,#38059,#38060,#38061,#38062,#38063,#38064,#38065,#38066,#38067,
#38068,#38069,#38070,#38071),(#38072,#38073,#38074,#38075,#38076,#38077,
#38078,#38079,#38080,#38081,#38082,#38083,#38084,#38085,#38086,#38087,#38088,
#38089,#38090,#38091,#38092,#38093,#38094,#38095,#38096,#38097,#38098,#38099,
#38100,#38101,#38102,#38103,#38104,#38105,#38106,#38107,#38108,#38109,#38110,
#38111,#38112,#38113,#38114,#38115,#38116,#38117,#38118,#38119,#38120,#38121,
#38122,#38123,#38124,#38125,#38126,#38127,#38128,#38129,#38130,#38131,#38132,
#38133,#38134,#38135,#38136,#38137,#38138,#38139,#38140,#38141,#38142,#38143,
#38144,#38145,#38146,#38147,#38148,#38149,#38150,#38151,#38152,#38153,#38154,
#38155,#38156,#38157,#38158,#38159,#38160,#38161,#38162,#38163,#38164,#38165,
#38166,#38167,#38168,#38169,#38170,#38171,#38172,#38173,#38174,#38175,#38176,
#38177,#38178,#38179,#38180,#38181,#38182,#38183,#38184,#38185,#38186,#38187,
#38188,#38189,#38190,#38191,#38192,#38193,#38194,#38195,#38196,#38197,#38198,
#38199,#38200,#38201,#38202,#38203,#38204,#38205,#38206,#38207,#38208,#38209,
#38210,#38211,#38212,#38213,#38214,#38215),(#38216,#38217,#38218,#38219,
#38220,#38221,#38222,#38223,#38224,#38225,#38226,#38227,#38228,#38229,#38230,
#38231,#38232,#38233,#38234,#38235,#38236,#38237,#38238,#38239,#38240,#38241,
#38242,#38243,#38244,#38245,#38246,#38247,#38248,#38249,#38250,#38251,#38252,
#38253,#38254,#38255,#38256,#38257,#38258,#38259,#38260,#38261,#38262,#38263,
#38264,#38265,#38266,#38267,#38268,#38269,#38270,#38271,#38272,#38273,#38274,
#38275,#38276,#38277,#38278,#38279,#38280,#38281,#38282,#38283,#38284,#38285,
#38286,#38287,#38288,#38289,#38290,#38291,#38292,#38293,#38294,#38295,#38296,
#38297,#38298,#38299,#38300,#38301,#38302,#38303,#38304,#38305,#38306,#38307,
#38308,#38309,#38310,#38311,#38312,#38313,#38314,#38315,#38316,#38317,#38318,
#38319,#38320,#38321,#38322,#38323,#38324,#38325,#38326,#38327,#38328,#38329,
#38330,#38331,#38332,#38333,#38334,#38335,#38336,#38337,#38338,#38339,#38340,
#38341,#38342,#38343,#38344,#38345,#38346,#38347,#38348,#38349,#38350,#38351,
#38352,#38353,#38354,#38355,#38356,#38357,#38358,#38359),(#38360,#38361,
#38362,#38363,#38364,#38365,#38366,#38367,#38368,#38369,#38370,#38371,#38372,
#38373,#38374,#38375,#38376,#38377,#38378,#38379,#38380,#38381,#38382,#38383,
#38384,#38385,#38386,#38387,#38388,#38389,#38390,#38391,#38392,#38393,#38394,
#38395,#38396,#38397,#38398,#38399,#38400,#38401,#38402,#38403,#38404,#38405,
#38406,#38407,#38408,#38409,#38410,#38411,#38412,#38413,#38414,#38415,#38416,
#38417,#38418,#38419,#38420,#38421,#38422,#38423,#38424,#38425,#38426,#38427,
#38428,#38429,#38430,#38431,#38432,#38433,#38434,#38435,#38436,#38437,#38438,
#38439,#38440,#38441,#38442,#38443,#38444,#38445,#38446,#38447,#38448,#38449,
#38450,#38451,#38452,#38453,#38454,#38455,#38456,#38457,#38458,#38459,#38460,
#38461,#38462,#38463,#38464,#38465,#38466,#38467,#38468,#38469,#38470,#38471,
#38472,#38473,#38474,#38475,#38476,#38477,#38478,#38479,#38480,#38481,#38482,
#38483,#38484,#38485,#38486,#38487,#38488,#38489,#38490,#38491,#38492,#38493,
#38494,#38495,#38496,#38497,#38498,#38499,#38500,#38501,#38502,#38503),
(#38504,#38505,#38506,#38507,#38508,#38509,#38510,#38511,#38512,#38513,
#38514,#38515,#38516,#38517,#38518,#38519,#38520,#38521,#38522,#38523,#38524,
#38525,#38526,#38527,#38528,#38529,#38530,#38531,#38532,#38533,#38534,#38535,
#38536,#38537,#38538,#38539,#38540,#38541,#38542,#38543,#38544,#38545,#38546,
#38547,#38548,#38549,#38550,#38551,#38552,#38553,#38554,#38555,#38556,#38557,
#38558,#38559,#38560,#38561,#38562,#38563,#38564,#38565,#38566,#38567,#38568,
#38569,#38570,#38571,#38572,#38573,#38574,#38575,#38576,#38577,#38578,#38579,
#38580,#38581,#38582,#38583,#38584,#38585,#38586,#38587,#38588,#38589,#38590,
#38591,#38592,#38593,#38594,#38595,#38596,#38597,#38598,#38599,#38600,#38601,
#38602,#38603,#38604,#38605,#38606,#38607,#38608,#38609,#38610,#38611,#38612,
#38613,#38614,#38615,#38616,#38617,#38618,#38619,#38620,#38621,#38622,#38623,
#38624,#38625,#38626,#38627,#38628,#38629,#38630,#38631,#38632,#38633,#38634,
#38635,#38636,#38637,#38638,#38639,#38640,#38641,#38642,#38643,#38644,#38645,
#38646,#38647)),.UNSPECIFIED.,.F.,.F.,.F.,(4,1,1,1,1,1,1,1,1,1,1,1,1,1,
1,1,1,1,1,1,1,1,1,1,1,1,1,1,1,1,1,1,1,1,1,1,1,1,1,1,1,1,1,1,1,1,1,1,1,1,
1,1,1,1,1,1,1,1,1,1,1,1,1,1,1,4),(4,2,1,1,2,1,1,1,2,1,1,1,2,1,1,1,1,2,1,
1,1,1,1,1,1,2,1,1,1,1,1,1,1,2,1,1,1,1,1,1,1,1,2,1,1,1,1,1,1,1,1,1,1,1,2,
1,1,1,1,1,2,1,1,1,1,1,1,1,1,2,1,1,1,1,2,1,1,1,1,1,1,1,1,1,1,1,2,1,1,1,1,
1,2,1,1,1,1,2,1,1,1,1,1,1,1,1,1,1,1,1,1,2,1,1,1,1,2,1,1,1,1,1,2,4),(0.0268159196746105,
0.0437158964674566,0.0606153077094141,0.0775147189513715,0.094414130193329,
0.111313541435286,0.128212952677244,0.145112363919201,0.162011775161159,
0.178911186403116,0.195810597645074,0.212710008887031,0.229609420128989,
0.246508831370946,0.254958536991925,0.263408242612904,0.280307653854861,
0.297207065096819,0.308473339258124,0.319739613419429,0.331005887580734,
0.342272161742039,0.353538435903344,0.364804710064649,0.387337258387259,
0.398603532548564,0.409869806709869,0.421136080871174,0.432402355032479,
0.454934903355088,0.466201177516393,0.477467451677698,0.488733725839003,
0.500000000000308,0.511266274161613,0.522532548322918,0.545065096645528,
0.556331370806833,0.567597644968138,0.584497056210096,0.601396467452053,
0.618295878694011,0.635195289935968,0.652094701177926,0.668994112419883,
0.677443818040862,0.685893523661841,0.694343229282819,0.702792934903798,
0.719692346145756,0.736591757387713,0.745041463008692,0.75349116862967,
0.770390579871628,0.787289991113585,0.804189402355543,0.8210888135975,0.837988224839458,
0.854887636081415,0.871787047323373,0.88868645856533,0.905585869807288,
0.922485281049245,0.939384692291203,0.95628410353316,0.973184071869037),
(0.0960305811261702,0.0972154775043869,0.109378606187391,0.121541734870394,
0.145867992236401,0.151993923775347,0.158119855314292,0.170371718392183,
0.194875444547964,0.200989580746302,0.207103716944641,0.219331989341318,
0.243788534134673,0.246827927163601,0.24986732019253,0.255946106250386,
0.2681036783661,0.292418822597527,0.293959106599555,0.295499390601583,0.29857995860564,
0.304741094613752,0.310902230621865,0.317063366629978,0.329385638646203,
0.341707910662428,0.344790082003921,0.347872253345414,0.354036596028399,
0.36636528139437,0.37869396676034,0.384858309443326,0.387940480784818,0.391022652126311,
0.392583125212554,0.394143598298796,0.397264544471281,0.403506436816251,
0.422232113851161,0.428474006196132,0.434715898541102,0.437836844713587,
0.440957790886072,0.442498863959882,0.444039937033693,0.447122083181315,
0.448663156255125,0.450204229328936,0.450974765865841,0.451745302402747,
0.453286375476557,0.4594506677718,0.465614960067043,0.477943544657529,0.490272129248014,
0.493311253959715,0.496350378671415,0.502428628094816,0.514585126941617,
0.526741625788419,0.53889812463522,0.540417366609575,0.541936608583929,
0.544975092532638,0.551052060430056,0.563205996224891,0.569282964122308,
0.575359932019726,0.581436899917144,0.587513867814562,0.590576684581802,
0.593639501349043,0.599765134883524,0.612016401952486,0.636518936090411,
0.639559223907375,0.642599511724338,0.645639799541302,0.648680087358265,
0.654760662992193,0.66084123862612,0.666921814260047,0.669962102077011,
0.673002389893974,0.676042677710938,0.679082965527902,0.685163541161829,
0.688226234079092,0.691288926996354,0.697414312830879,0.70966508449993,
0.72191585616898,0.734166627838031,0.737264704064826,0.740362780291622,
0.746558932745213,0.758951237652395,0.783735847466759,0.785338745832564,
0.78694164419837,0.790147440929981,0.796559034393203,0.809382221319647,
0.815793814782869,0.822205408246091,0.823808306611897,0.825411204977702,
0.828617001709314,0.830219900075119,0.831021349258022,0.831822798440925,
0.835028595172536,0.838457852551916,0.841887109931297,0.848745624690058,
0.86246265420758,0.889896713242625,0.893337440953794,0.896778168664963,
0.9036596240873,0.910541079509638,0.917422534931976,0.944948356621327,0.967478850977141),
 .UNSPECIFIED.);
#18851=B_SPLINE_SURFACE_WITH_KNOTS('',3,3,((#41157,#41158,#41159,#41160,
#41161,#41162,#41163,#41164,#41165,#41166,#41167,#41168,#41169,#41170,#41171,
#41172,#41173,#41174,#41175,#41176,#41177,#41178,#41179,#41180,#41181,#41182,
#41183,#41184,#41185,#41186,#41187,#41188,#41189,#41190,#41191,#41192,#41193,
#41194,#41195,#41196,#41197),(#41198,#41199,#41200,#41201,#41202,#41203,
#41204,#41205,#41206,#41207,#41208,#41209,#41210,#41211,#41212,#41213,#41214,
#41215,#41216,#41217,#41218,#41219,#41220,#41221,#41222,#41223,#41224,#41225,
#41226,#41227,#41228,#41229,#41230,#41231,#41232,#41233,#41234,#41235,#41236,
#41237,#41238),(#41239,#41240,#41241,#41242,#41243,#41244,#41245,#41246,
#41247,#41248,#41249,#41250,#41251,#41252,#41253,#41254,#41255,#41256,#41257,
#41258,#41259,#41260,#41261,#41262,#41263,#41264,#41265,#41266,#41267,#41268,
#41269,#41270,#41271,#41272,#41273,#41274,#41275,#41276,#41277,#41278,#41279),
(#41280,#41281,#41282,#41283,#41284,#41285,#41286,#41287,#41288,#41289,
#41290,#41291,#41292,#41293,#41294,#41295,#41296,#41297,#41298,#41299,#41300,
#41301,#41302,#41303,#41304,#41305,#41306,#41307,#41308,#41309,#41310,#41311,
#41312,#41313,#41314,#41315,#41316,#41317,#41318,#41319,#41320),(#41321,
#41322,#41323,#41324,#41325,#41326,#41327,#41328,#41329,#41330,#41331,#41332,
#41333,#41334,#41335,#41336,#41337,#41338,#41339,#41340,#41341,#41342,#41343,
#41344,#41345,#41346,#41347,#41348,#41349,#41350,#41351,#41352,#41353,#41354,
#41355,#41356,#41357,#41358,#41359,#41360,#41361)),.UNSPECIFIED.,.F.,.T.,
 .F.,(4,1,4),(4,1,1,1,2,1,1,1,1,2,1,1,1,2,1,1,1,2,2,1,2,2,2,2,1,2,1,1,4),
(0.,0.571428571428571,1.),(-9.55960092302324,-9.1896794456085,-8.81975796819377,
-8.44983649077903,-8.0799150133643,-8.03266253512535,-7.98541005688641,
-7.89090510040853,-7.70189518745276,-7.32387536154123,-7.17881214312514,
-7.03374892470906,-6.88868570629297,-6.74362248787689,-6.67050437063,-6.59738625338311,
-6.45115001888933,-6.15867754990177,-5.47160541199434,-4.26766323501505,
-3.06372105803577,-2.37819810334092,-1.79056374069951,-1.18667868852568,
-0.800342864550781,-0.414007040575882,-0.310505280431912,-0.207003520287941,
0.),.UNSPECIFIED.);
#18852=B_SPLINE_SURFACE_WITH_KNOTS('',3,3,((#41541,#41542,#41543,#41544,
#41545,#41546,#41547,#41548,#41549,#41550,#41551,#41552,#41553,#41554,#41555,
#41556,#41557,#41558,#41559,#41560,#41561,#41562,#41563,#41564,#41565,#41566,
#41567,#41568,#41569,#41570,#41571,#41572,#41573,#41574,#41575,#41576,#41577,
#41578,#41579,#41580,#41581,#41582,#41583,#41584,#41585,#41586,#41587,#41588,
#41589,#41590,#41591,#41592,#41593,#41594,#41595,#41596,#41597,#41598,#41599,
#41600,#41601,#41602,#41603,#41604,#41605,#41606,#41607,#41608,#41609,#41610,
#41611,#41612,#41613,#41614,#41615,#41616,#41617,#41618,#41619,#41620,#41621,
#41622,#41623,#41624,#41625,#41626,#41627,#41628,#41629,#41630,#41631,#41632,
#41633,#41634,#41635,#41636,#41637,#41638,#41639,#41640,#41641,#41642,#41643,
#41644,#41645,#41646,#41647,#41648,#41649,#41650,#41651,#41652,#41653,#41654,
#41655,#41656,#41657,#41658,#41659,#41660,#41661,#41662,#41663,#41664,#41665,
#41666,#41667,#41668,#41669,#41670,#41671,#41672,#41673,#41674,#41675,#41676,
#41677,#41678,#41679,#41680,#41681,#41682,#41683,#41684),(#41685,#41686,
#41687,#41688,#41689,#41690,#41691,#41692,#41693,#41694,#41695,#41696,#41697,
#41698,#41699,#41700,#41701,#41702,#41703,#41704,#41705,#41706,#41707,#41708,
#41709,#41710,#41711,#41712,#41713,#41714,#41715,#41716,#41717,#41718,#41719,
#41720,#41721,#41722,#41723,#41724,#41725,#41726,#41727,#41728,#41729,#41730,
#41731,#41732,#41733,#41734,#41735,#41736,#41737,#41738,#41739,#41740,#41741,
#41742,#41743,#41744,#41745,#41746,#41747,#41748,#41749,#41750,#41751,#41752,
#41753,#41754,#41755,#41756,#41757,#41758,#41759,#41760,#41761,#41762,#41763,
#41764,#41765,#41766,#41767,#41768,#41769,#41770,#41771,#41772,#41773,#41774,
#41775,#41776,#41777,#41778,#41779,#41780,#41781,#41782,#41783,#41784,#41785,
#41786,#41787,#41788,#41789,#41790,#41791,#41792,#41793,#41794,#41795,#41796,
#41797,#41798,#41799,#41800,#41801,#41802,#41803,#41804,#41805,#41806,#41807,
#41808,#41809,#41810,#41811,#41812,#41813,#41814,#41815,#41816,#41817,#41818,
#41819,#41820,#41821,#41822,#41823,#41824,#41825,#41826,#41827,#41828),
(#41829,#41830,#41831,#41832,#41833,#41834,#41835,#41836,#41837,#41838,
#41839,#41840,#41841,#41842,#41843,#41844,#41845,#41846,#41847,#41848,#41849,
#41850,#41851,#41852,#41853,#41854,#41855,#41856,#41857,#41858,#41859,#41860,
#41861,#41862,#41863,#41864,#41865,#41866,#41867,#41868,#41869,#41870,#41871,
#41872,#41873,#41874,#41875,#41876,#41877,#41878,#41879,#41880,#41881,#41882,
#41883,#41884,#41885,#41886,#41887,#41888,#41889,#41890,#41891,#41892,#41893,
#41894,#41895,#41896,#41897,#41898,#41899,#41900,#41901,#41902,#41903,#41904,
#41905,#41906,#41907,#41908,#41909,#41910,#41911,#41912,#41913,#41914,#41915,
#41916,#41917,#41918,#41919,#41920,#41921,#41922,#41923,#41924,#41925,#41926,
#41927,#41928,#41929,#41930,#41931,#41932,#41933,#41934,#41935,#41936,#41937,
#41938,#41939,#41940,#41941,#41942,#41943,#41944,#41945,#41946,#41947,#41948,
#41949,#41950,#41951,#41952,#41953,#41954,#41955,#41956,#41957,#41958,#41959,
#41960,#41961,#41962,#41963,#41964,#41965,#41966,#41967,#41968,#41969,#41970,
#41971,#41972),(#41973,#41974,#41975,#41976,#41977,#41978,#41979,#41980,
#41981,#41982,#41983,#41984,#41985,#41986,#41987,#41988,#41989,#41990,#41991,
#41992,#41993,#41994,#41995,#41996,#41997,#41998,#41999,#42000,#42001,#42002,
#42003,#42004,#42005,#42006,#42007,#42008,#42009,#42010,#42011,#42012,#42013,
#42014,#42015,#42016,#42017,#42018,#42019,#42020,#42021,#42022,#42023,#42024,
#42025,#42026,#42027,#42028,#42029,#42030,#42031,#42032,#42033,#42034,#42035,
#42036,#42037,#42038,#42039,#42040,#42041,#42042,#42043,#42044,#42045,#42046,
#42047,#42048,#42049,#42050,#42051,#42052,#42053,#42054,#42055,#42056,#42057,
#42058,#42059,#42060,#42061,#42062,#42063,#42064,#42065,#42066,#42067,#42068,
#42069,#42070,#42071,#42072,#42073,#42074,#42075,#42076,#42077,#42078,#42079,
#42080,#42081,#42082,#42083,#42084,#42085,#42086,#42087,#42088,#42089,#42090,
#42091,#42092,#42093,#42094,#42095,#42096,#42097,#42098,#42099,#42100,#42101,
#42102,#42103,#42104,#42105,#42106,#42107,#42108,#42109,#42110,#42111,#42112,
#42113,#42114,#42115,#42116),(#42117,#42118,#42119,#42120,#42121,#42122,
#42123,#42124,#42125,#42126,#42127,#42128,#42129,#42130,#42131,#42132,#42133,
#42134,#42135,#42136,#42137,#42138,#42139,#42140,#42141,#42142,#42143,#42144,
#42145,#42146,#42147,#42148,#42149,#42150,#42151,#42152,#42153,#42154,#42155,
#42156,#42157,#42158,#42159,#42160,#42161,#42162,#42163,#42164,#42165,#42166,
#42167,#42168,#42169,#42170,#42171,#42172,#42173,#42174,#42175,#42176,#42177,
#42178,#42179,#42180,#42181,#42182,#42183,#42184,#42185,#42186,#42187,#42188,
#42189,#42190,#42191,#42192,#42193,#42194,#42195,#42196,#42197,#42198,#42199,
#42200,#42201,#42202,#42203,#42204,#42205,#42206,#42207,#42208,#42209,#42210,
#42211,#42212,#42213,#42214,#42215,#42216,#42217,#42218,#42219,#42220,#42221,
#42222,#42223,#42224,#42225,#42226,#42227,#42228,#42229,#42230,#42231,#42232,
#42233,#42234,#42235,#42236,#42237,#42238,#42239,#42240,#42241,#42242,#42243,
#42244,#42245,#42246,#42247,#42248,#42249,#42250,#42251,#42252,#42253,#42254,
#42255,#42256,#42257,#42258,#42259,#42260),(#42261,#42262,#42263,#42264,
#42265,#42266,#42267,#42268,#42269,#42270,#42271,#42272,#42273,#42274,#42275,
#42276,#42277,#42278,#42279,#42280,#42281,#42282,#42283,#42284,#42285,#42286,
#42287,#42288,#42289,#42290,#42291,#42292,#42293,#42294,#42295,#42296,#42297,
#42298,#42299,#42300,#42301,#42302,#42303,#42304,#42305,#42306,#42307,#42308,
#42309,#42310,#42311,#42312,#42313,#42314,#42315,#42316,#42317,#42318,#42319,
#42320,#42321,#42322,#42323,#42324,#42325,#42326,#42327,#42328,#42329,#42330,
#42331,#42332,#42333,#42334,#42335,#42336,#42337,#42338,#42339,#42340,#42341,
#42342,#42343,#42344,#42345,#42346,#42347,#42348,#42349,#42350,#42351,#42352,
#42353,#42354,#42355,#42356,#42357,#42358,#42359,#42360,#42361,#42362,#42363,
#42364,#42365,#42366,#42367,#42368,#42369,#42370,#42371,#42372,#42373,#42374,
#42375,#42376,#42377,#42378,#42379,#42380,#42381,#42382,#42383,#42384,#42385,
#42386,#42387,#42388,#42389,#42390,#42391,#42392,#42393,#42394,#42395,#42396,
#42397,#42398,#42399,#42400,#42401,#42402,#42403,#42404),(#42405,#42406,
#42407,#42408,#42409,#42410,#42411,#42412,#42413,#42414,#42415,#42416,#42417,
#42418,#42419,#42420,#42421,#42422,#42423,#42424,#42425,#42426,#42427,#42428,
#42429,#42430,#42431,#42432,#42433,#42434,#42435,#42436,#42437,#42438,#42439,
#42440,#42441,#42442,#42443,#42444,#42445,#42446,#42447,#42448,#42449,#42450,
#42451,#42452,#42453,#42454,#42455,#42456,#42457,#42458,#42459,#42460,#42461,
#42462,#42463,#42464,#42465,#42466,#42467,#42468,#42469,#42470,#42471,#42472,
#42473,#42474,#42475,#42476,#42477,#42478,#42479,#42480,#42481,#42482,#42483,
#42484,#42485,#42486,#42487,#42488,#42489,#42490,#42491,#42492,#42493,#42494,
#42495,#42496,#42497,#42498,#42499,#42500,#42501,#42502,#42503,#42504,#42505,
#42506,#42507,#42508,#42509,#42510,#42511,#42512,#42513,#42514,#42515,#42516,
#42517,#42518,#42519,#42520,#42521,#42522,#42523,#42524,#42525,#42526,#42527,
#42528,#42529,#42530,#42531,#42532,#42533,#42534,#42535,#42536,#42537,#42538,
#42539,#42540,#42541,#42542,#42543,#42544,#42545,#42546,#42547,#42548),
(#42549,#42550,#42551,#42552,#42553,#42554,#42555,#42556,#42557,#42558,
#42559,#42560,#42561,#42562,#42563,#42564,#42565,#42566,#42567,#42568,#42569,
#42570,#42571,#42572,#42573,#42574,#42575,#42576,#42577,#42578,#42579,#42580,
#42581,#42582,#42583,#42584,#42585,#42586,#42587,#42588,#42589,#42590,#42591,
#42592,#42593,#42594,#42595,#42596,#42597,#42598,#42599,#42600,#42601,#42602,
#42603,#42604,#42605,#42606,#42607,#42608,#42609,#42610,#42611,#42612,#42613,
#42614,#42615,#42616,#42617,#42618,#42619,#42620,#42621,#42622,#42623,#42624,
#42625,#42626,#42627,#42628,#42629,#42630,#42631,#42632,#42633,#42634,#42635,
#42636,#42637,#42638,#42639,#42640,#42641,#42642,#42643,#42644,#42645,#42646,
#42647,#42648,#42649,#42650,#42651,#42652,#42653,#42654,#42655,#42656,#42657,
#42658,#42659,#42660,#42661,#42662,#42663,#42664,#42665,#42666,#42667,#42668,
#42669,#42670,#42671,#42672,#42673,#42674,#42675,#42676,#42677,#42678,#42679,
#42680,#42681,#42682,#42683,#42684,#42685,#42686,#42687,#42688,#42689,#42690,
#42691,#42692),(#42693,#42694,#42695,#42696,#42697,#42698,#42699,#42700,
#42701,#42702,#42703,#42704,#42705,#42706,#42707,#42708,#42709,#42710,#42711,
#42712,#42713,#42714,#42715,#42716,#42717,#42718,#42719,#42720,#42721,#42722,
#42723,#42724,#42725,#42726,#42727,#42728,#42729,#42730,#42731,#42732,#42733,
#42734,#42735,#42736,#42737,#42738,#42739,#42740,#42741,#42742,#42743,#42744,
#42745,#42746,#42747,#42748,#42749,#42750,#42751,#42752,#42753,#42754,#42755,
#42756,#42757,#42758,#42759,#42760,#42761,#42762,#42763,#42764,#42765,#42766,
#42767,#42768,#42769,#42770,#42771,#42772,#42773,#42774,#42775,#42776,#42777,
#42778,#42779,#42780,#42781,#42782,#42783,#42784,#42785,#42786,#42787,#42788,
#42789,#42790,#42791,#42792,#42793,#42794,#42795,#42796,#42797,#42798,#42799,
#42800,#42801,#42802,#42803,#42804,#42805,#42806,#42807,#42808,#42809,#42810,
#42811,#42812,#42813,#42814,#42815,#42816,#42817,#42818,#42819,#42820,#42821,
#42822,#42823,#42824,#42825,#42826,#42827,#42828,#42829,#42830,#42831,#42832,
#42833,#42834,#42835,#42836),(#42837,#42838,#42839,#42840,#42841,#42842,
#42843,#42844,#42845,#42846,#42847,#42848,#42849,#42850,#42851,#42852,#42853,
#42854,#42855,#42856,#42857,#42858,#42859,#42860,#42861,#42862,#42863,#42864,
#42865,#42866,#42867,#42868,#42869,#42870,#42871,#42872,#42873,#42874,#42875,
#42876,#42877,#42878,#42879,#42880,#42881,#42882,#42883,#42884,#42885,#42886,
#42887,#42888,#42889,#42890,#42891,#42892,#42893,#42894,#42895,#42896,#42897,
#42898,#42899,#42900,#42901,#42902,#42903,#42904,#42905,#42906,#42907,#42908,
#42909,#42910,#42911,#42912,#42913,#42914,#42915,#42916,#42917,#42918,#42919,
#42920,#42921,#42922,#42923,#42924,#42925,#42926,#42927,#42928,#42929,#42930,
#42931,#42932,#42933,#42934,#42935,#42936,#42937,#42938,#42939,#42940,#42941,
#42942,#42943,#42944,#42945,#42946,#42947,#42948,#42949,#42950,#42951,#42952,
#42953,#42954,#42955,#42956,#42957,#42958,#42959,#42960,#42961,#42962,#42963,
#42964,#42965,#42966,#42967,#42968,#42969,#42970,#42971,#42972,#42973,#42974,
#42975,#42976,#42977,#42978,#42979,#42980),(#42981,#42982,#42983,#42984,
#42985,#42986,#42987,#42988,#42989,#42990,#42991,#42992,#42993,#42994,#42995,
#42996,#42997,#42998,#42999,#43000,#43001,#43002,#43003,#43004,#43005,#43006,
#43007,#43008,#43009,#43010,#43011,#43012,#43013,#43014,#43015,#43016,#43017,
#43018,#43019,#43020,#43021,#43022,#43023,#43024,#43025,#43026,#43027,#43028,
#43029,#43030,#43031,#43032,#43033,#43034,#43035,#43036,#43037,#43038,#43039,
#43040,#43041,#43042,#43043,#43044,#43045,#43046,#43047,#43048,#43049,#43050,
#43051,#43052,#43053,#43054,#43055,#43056,#43057,#43058,#43059,#43060,#43061,
#43062,#43063,#43064,#43065,#43066,#43067,#43068,#43069,#43070,#43071,#43072,
#43073,#43074,#43075,#43076,#43077,#43078,#43079,#43080,#43081,#43082,#43083,
#43084,#43085,#43086,#43087,#43088,#43089,#43090,#43091,#43092,#43093,#43094,
#43095,#43096,#43097,#43098,#43099,#43100,#43101,#43102,#43103,#43104,#43105,
#43106,#43107,#43108,#43109,#43110,#43111,#43112,#43113,#43114,#43115,#43116,
#43117,#43118,#43119,#43120,#43121,#43122,#43123,#43124),(#43125,#43126,
#43127,#43128,#43129,#43130,#43131,#43132,#43133,#43134,#43135,#43136,#43137,
#43138,#43139,#43140,#43141,#43142,#43143,#43144,#43145,#43146,#43147,#43148,
#43149,#43150,#43151,#43152,#43153,#43154,#43155,#43156,#43157,#43158,#43159,
#43160,#43161,#43162,#43163,#43164,#43165,#43166,#43167,#43168,#43169,#43170,
#43171,#43172,#43173,#43174,#43175,#43176,#43177,#43178,#43179,#43180,#43181,
#43182,#43183,#43184,#43185,#43186,#43187,#43188,#43189,#43190,#43191,#43192,
#43193,#43194,#43195,#43196,#43197,#43198,#43199,#43200,#43201,#43202,#43203,
#43204,#43205,#43206,#43207,#43208,#43209,#43210,#43211,#43212,#43213,#43214,
#43215,#43216,#43217,#43218,#43219,#43220,#43221,#43222,#43223,#43224,#43225,
#43226,#43227,#43228,#43229,#43230,#43231,#43232,#43233,#43234,#43235,#43236,
#43237,#43238,#43239,#43240,#43241,#43242,#43243,#43244,#43245,#43246,#43247,
#43248,#43249,#43250,#43251,#43252,#43253,#43254,#43255,#43256,#43257,#43258,
#43259,#43260,#43261,#43262,#43263,#43264,#43265,#43266,#43267,#43268),
(#43269,#43270,#43271,#43272,#43273,#43274,#43275,#43276,#43277,#43278,
#43279,#43280,#43281,#43282,#43283,#43284,#43285,#43286,#43287,#43288,#43289,
#43290,#43291,#43292,#43293,#43294,#43295,#43296,#43297,#43298,#43299,#43300,
#43301,#43302,#43303,#43304,#43305,#43306,#43307,#43308,#43309,#43310,#43311,
#43312,#43313,#43314,#43315,#43316,#43317,#43318,#43319,#43320,#43321,#43322,
#43323,#43324,#43325,#43326,#43327,#43328,#43329,#43330,#43331,#43332,#43333,
#43334,#43335,#43336,#43337,#43338,#43339,#43340,#43341,#43342,#43343,#43344,
#43345,#43346,#43347,#43348,#43349,#43350,#43351,#43352,#43353,#43354,#43355,
#43356,#43357,#43358,#43359,#43360,#43361,#43362,#43363,#43364,#43365,#43366,
#43367,#43368,#43369,#43370,#43371,#43372,#43373,#43374,#43375,#43376,#43377,
#43378,#43379,#43380,#43381,#43382,#43383,#43384,#43385,#43386,#43387,#43388,
#43389,#43390,#43391,#43392,#43393,#43394,#43395,#43396,#43397,#43398,#43399,
#43400,#43401,#43402,#43403,#43404,#43405,#43406,#43407,#43408,#43409,#43410,
#43411,#43412),(#43413,#43414,#43415,#43416,#43417,#43418,#43419,#43420,
#43421,#43422,#43423,#43424,#43425,#43426,#43427,#43428,#43429,#43430,#43431,
#43432,#43433,#43434,#43435,#43436,#43437,#43438,#43439,#43440,#43441,#43442,
#43443,#43444,#43445,#43446,#43447,#43448,#43449,#43450,#43451,#43452,#43453,
#43454,#43455,#43456,#43457,#43458,#43459,#43460,#43461,#43462,#43463,#43464,
#43465,#43466,#43467,#43468,#43469,#43470,#43471,#43472,#43473,#43474,#43475,
#43476,#43477,#43478,#43479,#43480,#43481,#43482,#43483,#43484,#43485,#43486,
#43487,#43488,#43489,#43490,#43491,#43492,#43493,#43494,#43495,#43496,#43497,
#43498,#43499,#43500,#43501,#43502,#43503,#43504,#43505,#43506,#43507,#43508,
#43509,#43510,#43511,#43512,#43513,#43514,#43515,#43516,#43517,#43518,#43519,
#43520,#43521,#43522,#43523,#43524,#43525,#43526,#43527,#43528,#43529,#43530,
#43531,#43532,#43533,#43534,#43535,#43536,#43537,#43538,#43539,#43540,#43541,
#43542,#43543,#43544,#43545,#43546,#43547,#43548,#43549,#43550,#43551,#43552,
#43553,#43554,#43555,#43556),(#43557,#43558,#43559,#43560,#43561,#43562,
#43563,#43564,#43565,#43566,#43567,#43568,#43569,#43570,#43571,#43572,#43573,
#43574,#43575,#43576,#43577,#43578,#43579,#43580,#43581,#43582,#43583,#43584,
#43585,#43586,#43587,#43588,#43589,#43590,#43591,#43592,#43593,#43594,#43595,
#43596,#43597,#43598,#43599,#43600,#43601,#43602,#43603,#43604,#43605,#43606,
#43607,#43608,#43609,#43610,#43611,#43612,#43613,#43614,#43615,#43616,#43617,
#43618,#43619,#43620,#43621,#43622,#43623,#43624,#43625,#43626,#43627,#43628,
#43629,#43630,#43631,#43632,#43633,#43634,#43635,#43636,#43637,#43638,#43639,
#43640,#43641,#43642,#43643,#43644,#43645,#43646,#43647,#43648,#43649,#43650,
#43651,#43652,#43653,#43654,#43655,#43656,#43657,#43658,#43659,#43660,#43661,
#43662,#43663,#43664,#43665,#43666,#43667,#43668,#43669,#43670,#43671,#43672,
#43673,#43674,#43675,#43676,#43677,#43678,#43679,#43680,#43681,#43682,#43683,
#43684,#43685,#43686,#43687,#43688,#43689,#43690,#43691,#43692,#43693,#43694,
#43695,#43696,#43697,#43698,#43699,#43700),(#43701,#43702,#43703,#43704,
#43705,#43706,#43707,#43708,#43709,#43710,#43711,#43712,#43713,#43714,#43715,
#43716,#43717,#43718,#43719,#43720,#43721,#43722,#43723,#43724,#43725,#43726,
#43727,#43728,#43729,#43730,#43731,#43732,#43733,#43734,#43735,#43736,#43737,
#43738,#43739,#43740,#43741,#43742,#43743,#43744,#43745,#43746,#43747,#43748,
#43749,#43750,#43751,#43752,#43753,#43754,#43755,#43756,#43757,#43758,#43759,
#43760,#43761,#43762,#43763,#43764,#43765,#43766,#43767,#43768,#43769,#43770,
#43771,#43772,#43773,#43774,#43775,#43776,#43777,#43778,#43779,#43780,#43781,
#43782,#43783,#43784,#43785,#43786,#43787,#43788,#43789,#43790,#43791,#43792,
#43793,#43794,#43795,#43796,#43797,#43798,#43799,#43800,#43801,#43802,#43803,
#43804,#43805,#43806,#43807,#43808,#43809,#43810,#43811,#43812,#43813,#43814,
#43815,#43816,#43817,#43818,#43819,#43820,#43821,#43822,#43823,#43824,#43825,
#43826,#43827,#43828,#43829,#43830,#43831,#43832,#43833,#43834,#43835,#43836,
#43837,#43838,#43839,#43840,#43841,#43842,#43843,#43844),(#43845,#43846,
#43847,#43848,#43849,#43850,#43851,#43852,#43853,#43854,#43855,#43856,#43857,
#43858,#43859,#43860,#43861,#43862,#43863,#43864,#43865,#43866,#43867,#43868,
#43869,#43870,#43871,#43872,#43873,#43874,#43875,#43876,#43877,#43878,#43879,
#43880,#43881,#43882,#43883,#43884,#43885,#43886,#43887,#43888,#43889,#43890,
#43891,#43892,#43893,#43894,#43895,#43896,#43897,#43898,#43899,#43900,#43901,
#43902,#43903,#43904,#43905,#43906,#43907,#43908,#43909,#43910,#43911,#43912,
#43913,#43914,#43915,#43916,#43917,#43918,#43919,#43920,#43921,#43922,#43923,
#43924,#43925,#43926,#43927,#43928,#43929,#43930,#43931,#43932,#43933,#43934,
#43935,#43936,#43937,#43938,#43939,#43940,#43941,#43942,#43943,#43944,#43945,
#43946,#43947,#43948,#43949,#43950,#43951,#43952,#43953,#43954,#43955,#43956,
#43957,#43958,#43959,#43960,#43961,#43962,#43963,#43964,#43965,#43966,#43967,
#43968,#43969,#43970,#43971,#43972,#43973,#43974,#43975,#43976,#43977,#43978,
#43979,#43980,#43981,#43982,#43983,#43984,#43985,#43986,#43987,#43988),
(#43989,#43990,#43991,#43992,#43993,#43994,#43995,#43996,#43997,#43998,
#43999,#44000,#44001,#44002,#44003,#44004,#44005,#44006,#44007,#44008,#44009,
#44010,#44011,#44012,#44013,#44014,#44015,#44016,#44017,#44018,#44019,#44020,
#44021,#44022,#44023,#44024,#44025,#44026,#44027,#44028,#44029,#44030,#44031,
#44032,#44033,#44034,#44035,#44036,#44037,#44038,#44039,#44040,#44041,#44042,
#44043,#44044,#44045,#44046,#44047,#44048,#44049,#44050,#44051,#44052,#44053,
#44054,#44055,#44056,#44057,#44058,#44059,#44060,#44061,#44062,#44063,#44064,
#44065,#44066,#44067,#44068,#44069,#44070,#44071,#44072,#44073,#44074,#44075,
#44076,#44077,#44078,#44079,#44080,#44081,#44082,#44083,#44084,#44085,#44086,
#44087,#44088,#44089,#44090,#44091,#44092,#44093,#44094,#44095,#44096,#44097,
#44098,#44099,#44100,#44101,#44102,#44103,#44104,#44105,#44106,#44107,#44108,
#44109,#44110,#44111,#44112,#44113,#44114,#44115,#44116,#44117,#44118,#44119,
#44120,#44121,#44122,#44123,#44124,#44125,#44126,#44127,#44128,#44129,#44130,
#44131,#44132),(#44133,#44134,#44135,#44136,#44137,#44138,#44139,#44140,
#44141,#44142,#44143,#44144,#44145,#44146,#44147,#44148,#44149,#44150,#44151,
#44152,#44153,#44154,#44155,#44156,#44157,#44158,#44159,#44160,#44161,#44162,
#44163,#44164,#44165,#44166,#44167,#44168,#44169,#44170,#44171,#44172,#44173,
#44174,#44175,#44176,#44177,#44178,#44179,#44180,#44181,#44182,#44183,#44184,
#44185,#44186,#44187,#44188,#44189,#44190,#44191,#44192,#44193,#44194,#44195,
#44196,#44197,#44198,#44199,#44200,#44201,#44202,#44203,#44204,#44205,#44206,
#44207,#44208,#44209,#44210,#44211,#44212,#44213,#44214,#44215,#44216,#44217,
#44218,#44219,#44220,#44221,#44222,#44223,#44224,#44225,#44226,#44227,#44228,
#44229,#44230,#44231,#44232,#44233,#44234,#44235,#44236,#44237,#44238,#44239,
#44240,#44241,#44242,#44243,#44244,#44245,#44246,#44247,#44248,#44249,#44250,
#44251,#44252,#44253,#44254,#44255,#44256,#44257,#44258,#44259,#44260,#44261,
#44262,#44263,#44264,#44265,#44266,#44267,#44268,#44269,#44270,#44271,#44272,
#44273,#44274,#44275,#44276),(#44277,#44278,#44279,#44280,#44281,#44282,
#44283,#44284,#44285,#44286,#44287,#44288,#44289,#44290,#44291,#44292,#44293,
#44294,#44295,#44296,#44297,#44298,#44299,#44300,#44301,#44302,#44303,#44304,
#44305,#44306,#44307,#44308,#44309,#44310,#44311,#44312,#44313,#44314,#44315,
#44316,#44317,#44318,#44319,#44320,#44321,#44322,#44323,#44324,#44325,#44326,
#44327,#44328,#44329,#44330,#44331,#44332,#44333,#44334,#44335,#44336,#44337,
#44338,#44339,#44340,#44341,#44342,#44343,#44344,#44345,#44346,#44347,#44348,
#44349,#44350,#44351,#44352,#44353,#44354,#44355,#44356,#44357,#44358,#44359,
#44360,#44361,#44362,#44363,#44364,#44365,#44366,#44367,#44368,#44369,#44370,
#44371,#44372,#44373,#44374,#44375,#44376,#44377,#44378,#44379,#44380,#44381,
#44382,#44383,#44384,#44385,#44386,#44387,#44388,#44389,#44390,#44391,#44392,
#44393,#44394,#44395,#44396,#44397,#44398,#44399,#44400,#44401,#44402,#44403,
#44404,#44405,#44406,#44407,#44408,#44409,#44410,#44411,#44412,#44413,#44414,
#44415,#44416,#44417,#44418,#44419,#44420),(#44421,#44422,#44423,#44424,
#44425,#44426,#44427,#44428,#44429,#44430,#44431,#44432,#44433,#44434,#44435,
#44436,#44437,#44438,#44439,#44440,#44441,#44442,#44443,#44444,#44445,#44446,
#44447,#44448,#44449,#44450,#44451,#44452,#44453,#44454,#44455,#44456,#44457,
#44458,#44459,#44460,#44461,#44462,#44463,#44464,#44465,#44466,#44467,#44468,
#44469,#44470,#44471,#44472,#44473,#44474,#44475,#44476,#44477,#44478,#44479,
#44480,#44481,#44482,#44483,#44484,#44485,#44486,#44487,#44488,#44489,#44490,
#44491,#44492,#44493,#44494,#44495,#44496,#44497,#44498,#44499,#44500,#44501,
#44502,#44503,#44504,#44505,#44506,#44507,#44508,#44509,#44510,#44511,#44512,
#44513,#44514,#44515,#44516,#44517,#44518,#44519,#44520,#44521,#44522,#44523,
#44524,#44525,#44526,#44527,#44528,#44529,#44530,#44531,#44532,#44533,#44534,
#44535,#44536,#44537,#44538,#44539,#44540,#44541,#44542,#44543,#44544,#44545,
#44546,#44547,#44548,#44549,#44550,#44551,#44552,#44553,#44554,#44555,#44556,
#44557,#44558,#44559,#44560,#44561,#44562,#44563,#44564),(#44565,#44566,
#44567,#44568,#44569,#44570,#44571,#44572,#44573,#44574,#44575,#44576,#44577,
#44578,#44579,#44580,#44581,#44582,#44583,#44584,#44585,#44586,#44587,#44588,
#44589,#44590,#44591,#44592,#44593,#44594,#44595,#44596,#44597,#44598,#44599,
#44600,#44601,#44602,#44603,#44604,#44605,#44606,#44607,#44608,#44609,#44610,
#44611,#44612,#44613,#44614,#44615,#44616,#44617,#44618,#44619,#44620,#44621,
#44622,#44623,#44624,#44625,#44626,#44627,#44628,#44629,#44630,#44631,#44632,
#44633,#44634,#44635,#44636,#44637,#44638,#44639,#44640,#44641,#44642,#44643,
#44644,#44645,#44646,#44647,#44648,#44649,#44650,#44651,#44652,#44653,#44654,
#44655,#44656,#44657,#44658,#44659,#44660,#44661,#44662,#44663,#44664,#44665,
#44666,#44667,#44668,#44669,#44670,#44671,#44672,#44673,#44674,#44675,#44676,
#44677,#44678,#44679,#44680,#44681,#44682,#44683,#44684,#44685,#44686,#44687,
#44688,#44689,#44690,#44691,#44692,#44693,#44694,#44695,#44696,#44697,#44698,
#44699,#44700,#44701,#44702,#44703,#44704,#44705,#44706,#44707,#44708),
(#44709,#44710,#44711,#44712,#44713,#44714,#44715,#44716,#44717,#44718,
#44719,#44720,#44721,#44722,#44723,#44724,#44725,#44726,#44727,#44728,#44729,
#44730,#44731,#44732,#44733,#44734,#44735,#44736,#44737,#44738,#44739,#44740,
#44741,#44742,#44743,#44744,#44745,#44746,#44747,#44748,#44749,#44750,#44751,
#44752,#44753,#44754,#44755,#44756,#44757,#44758,#44759,#44760,#44761,#44762,
#44763,#44764,#44765,#44766,#44767,#44768,#44769,#44770,#44771,#44772,#44773,
#44774,#44775,#44776,#44777,#44778,#44779,#44780,#44781,#44782,#44783,#44784,
#44785,#44786,#44787,#44788,#44789,#44790,#44791,#44792,#44793,#44794,#44795,
#44796,#44797,#44798,#44799,#44800,#44801,#44802,#44803,#44804,#44805,#44806,
#44807,#44808,#44809,#44810,#44811,#44812,#44813,#44814,#44815,#44816,#44817,
#44818,#44819,#44820,#44821,#44822,#44823,#44824,#44825,#44826,#44827,#44828,
#44829,#44830,#44831,#44832,#44833,#44834,#44835,#44836,#44837,#44838,#44839,
#44840,#44841,#44842,#44843,#44844,#44845,#44846,#44847,#44848,#44849,#44850,
#44851,#44852),(#44853,#44854,#44855,#44856,#44857,#44858,#44859,#44860,
#44861,#44862,#44863,#44864,#44865,#44866,#44867,#44868,#44869,#44870,#44871,
#44872,#44873,#44874,#44875,#44876,#44877,#44878,#44879,#44880,#44881,#44882,
#44883,#44884,#44885,#44886,#44887,#44888,#44889,#44890,#44891,#44892,#44893,
#44894,#44895,#44896,#44897,#44898,#44899,#44900,#44901,#44902,#44903,#44904,
#44905,#44906,#44907,#44908,#44909,#44910,#44911,#44912,#44913,#44914,#44915,
#44916,#44917,#44918,#44919,#44920,#44921,#44922,#44923,#44924,#44925,#44926,
#44927,#44928,#44929,#44930,#44931,#44932,#44933,#44934,#44935,#44936,#44937,
#44938,#44939,#44940,#44941,#44942,#44943,#44944,#44945,#44946,#44947,#44948,
#44949,#44950,#44951,#44952,#44953,#44954,#44955,#44956,#44957,#44958,#44959,
#44960,#44961,#44962,#44963,#44964,#44965,#44966,#44967,#44968,#44969,#44970,
#44971,#44972,#44973,#44974,#44975,#44976,#44977,#44978,#44979,#44980,#44981,
#44982,#44983,#44984,#44985,#44986,#44987,#44988,#44989,#44990,#44991,#44992,
#44993,#44994,#44995,#44996),(#44997,#44998,#44999,#45000,#45001,#45002,
#45003,#45004,#45005,#45006,#45007,#45008,#45009,#45010,#45011,#45012,#45013,
#45014,#45015,#45016,#45017,#45018,#45019,#45020,#45021,#45022,#45023,#45024,
#45025,#45026,#45027,#45028,#45029,#45030,#45031,#45032,#45033,#45034,#45035,
#45036,#45037,#45038,#45039,#45040,#45041,#45042,#45043,#45044,#45045,#45046,
#45047,#45048,#45049,#45050,#45051,#45052,#45053,#45054,#45055,#45056,#45057,
#45058,#45059,#45060,#45061,#45062,#45063,#45064,#45065,#45066,#45067,#45068,
#45069,#45070,#45071,#45072,#45073,#45074,#45075,#45076,#45077,#45078,#45079,
#45080,#45081,#45082,#45083,#45084,#45085,#45086,#45087,#45088,#45089,#45090,
#45091,#45092,#45093,#45094,#45095,#45096,#45097,#45098,#45099,#45100,#45101,
#45102,#45103,#45104,#45105,#45106,#45107,#45108,#45109,#45110,#45111,#45112,
#45113,#45114,#45115,#45116,#45117,#45118,#45119,#45120,#45121,#45122,#45123,
#45124,#45125,#45126,#45127,#45128,#45129,#45130,#45131,#45132,#45133,#45134,
#45135,#45136,#45137,#45138,#45139,#45140),(#45141,#45142,#45143,#45144,
#45145,#45146,#45147,#45148,#45149,#45150,#45151,#45152,#45153,#45154,#45155,
#45156,#45157,#45158,#45159,#45160,#45161,#45162,#45163,#45164,#45165,#45166,
#45167,#45168,#45169,#45170,#45171,#45172,#45173,#45174,#45175,#45176,#45177,
#45178,#45179,#45180,#45181,#45182,#45183,#45184,#45185,#45186,#45187,#45188,
#45189,#45190,#45191,#45192,#45193,#45194,#45195,#45196,#45197,#45198,#45199,
#45200,#45201,#45202,#45203,#45204,#45205,#45206,#45207,#45208,#45209,#45210,
#45211,#45212,#45213,#45214,#45215,#45216,#45217,#45218,#45219,#45220,#45221,
#45222,#45223,#45224,#45225,#45226,#45227,#45228,#45229,#45230,#45231,#45232,
#45233,#45234,#45235,#45236,#45237,#45238,#45239,#45240,#45241,#45242,#45243,
#45244,#45245,#45246,#45247,#45248,#45249,#45250,#45251,#45252,#45253,#45254,
#45255,#45256,#45257,#45258,#45259,#45260,#45261,#45262,#45263,#45264,#45265,
#45266,#45267,#45268,#45269,#45270,#45271,#45272,#45273,#45274,#45275,#45276,
#45277,#45278,#45279,#45280,#45281,#45282,#45283,#45284),(#45285,#45286,
#45287,#45288,#45289,#45290,#45291,#45292,#45293,#45294,#45295,#45296,#45297,
#45298,#45299,#45300,#45301,#45302,#45303,#45304,#45305,#45306,#45307,#45308,
#45309,#45310,#45311,#45312,#45313,#45314,#45315,#45316,#45317,#45318,#45319,
#45320,#45321,#45322,#45323,#45324,#45325,#45326,#45327,#45328,#45329,#45330,
#45331,#45332,#45333,#45334,#45335,#45336,#45337,#45338,#45339,#45340,#45341,
#45342,#45343,#45344,#45345,#45346,#45347,#45348,#45349,#45350,#45351,#45352,
#45353,#45354,#45355,#45356,#45357,#45358,#45359,#45360,#45361,#45362,#45363,
#45364,#45365,#45366,#45367,#45368,#45369,#45370,#45371,#45372,#45373,#45374,
#45375,#45376,#45377,#45378,#45379,#45380,#45381,#45382,#45383,#45384,#45385,
#45386,#45387,#45388,#45389,#45390,#45391,#45392,#45393,#45394,#45395,#45396,
#45397,#45398,#45399,#45400,#45401,#45402,#45403,#45404,#45405,#45406,#45407,
#45408,#45409,#45410,#45411,#45412,#45413,#45414,#45415,#45416,#45417,#45418,
#45419,#45420,#45421,#45422,#45423,#45424,#45425,#45426,#45427,#45428),
(#45429,#45430,#45431,#45432,#45433,#45434,#45435,#45436,#45437,#45438,
#45439,#45440,#45441,#45442,#45443,#45444,#45445,#45446,#45447,#45448,#45449,
#45450,#45451,#45452,#45453,#45454,#45455,#45456,#45457,#45458,#45459,#45460,
#45461,#45462,#45463,#45464,#45465,#45466,#45467,#45468,#45469,#45470,#45471,
#45472,#45473,#45474,#45475,#45476,#45477,#45478,#45479,#45480,#45481,#45482,
#45483,#45484,#45485,#45486,#45487,#45488,#45489,#45490,#45491,#45492,#45493,
#45494,#45495,#45496,#45497,#45498,#45499,#45500,#45501,#45502,#45503,#45504,
#45505,#45506,#45507,#45508,#45509,#45510,#45511,#45512,#45513,#45514,#45515,
#45516,#45517,#45518,#45519,#45520,#45521,#45522,#45523,#45524,#45525,#45526,
#45527,#45528,#45529,#45530,#45531,#45532,#45533,#45534,#45535,#45536,#45537,
#45538,#45539,#45540,#45541,#45542,#45543,#45544,#45545,#45546,#45547,#45548,
#45549,#45550,#45551,#45552,#45553,#45554,#45555,#45556,#45557,#45558,#45559,
#45560,#45561,#45562,#45563,#45564,#45565,#45566,#45567,#45568,#45569,#45570,
#45571,#45572),(#45573,#45574,#45575,#45576,#45577,#45578,#45579,#45580,
#45581,#45582,#45583,#45584,#45585,#45586,#45587,#45588,#45589,#45590,#45591,
#45592,#45593,#45594,#45595,#45596,#45597,#45598,#45599,#45600,#45601,#45602,
#45603,#45604,#45605,#45606,#45607,#45608,#45609,#45610,#45611,#45612,#45613,
#45614,#45615,#45616,#45617,#45618,#45619,#45620,#45621,#45622,#45623,#45624,
#45625,#45626,#45627,#45628,#45629,#45630,#45631,#45632,#45633,#45634,#45635,
#45636,#45637,#45638,#45639,#45640,#45641,#45642,#45643,#45644,#45645,#45646,
#45647,#45648,#45649,#45650,#45651,#45652,#45653,#45654,#45655,#45656,#45657,
#45658,#45659,#45660,#45661,#45662,#45663,#45664,#45665,#45666,#45667,#45668,
#45669,#45670,#45671,#45672,#45673,#45674,#45675,#45676,#45677,#45678,#45679,
#45680,#45681,#45682,#45683,#45684,#45685,#45686,#45687,#45688,#45689,#45690,
#45691,#45692,#45693,#45694,#45695,#45696,#45697,#45698,#45699,#45700,#45701,
#45702,#45703,#45704,#45705,#45706,#45707,#45708,#45709,#45710,#45711,#45712,
#45713,#45714,#45715,#45716),(#45717,#45718,#45719,#45720,#45721,#45722,
#45723,#45724,#45725,#45726,#45727,#45728,#45729,#45730,#45731,#45732,#45733,
#45734,#45735,#45736,#45737,#45738,#45739,#45740,#45741,#45742,#45743,#45744,
#45745,#45746,#45747,#45748,#45749,#45750,#45751,#45752,#45753,#45754,#45755,
#45756,#45757,#45758,#45759,#45760,#45761,#45762,#45763,#45764,#45765,#45766,
#45767,#45768,#45769,#45770,#45771,#45772,#45773,#45774,#45775,#45776,#45777,
#45778,#45779,#45780,#45781,#45782,#45783,#45784,#45785,#45786,#45787,#45788,
#45789,#45790,#45791,#45792,#45793,#45794,#45795,#45796,#45797,#45798,#45799,
#45800,#45801,#45802,#45803,#45804,#45805,#45806,#45807,#45808,#45809,#45810,
#45811,#45812,#45813,#45814,#45815,#45816,#45817,#45818,#45819,#45820,#45821,
#45822,#45823,#45824,#45825,#45826,#45827,#45828,#45829,#45830,#45831,#45832,
#45833,#45834,#45835,#45836,#45837,#45838,#45839,#45840,#45841,#45842,#45843,
#45844,#45845,#45846,#45847,#45848,#45849,#45850,#45851,#45852,#45853,#45854,
#45855,#45856,#45857,#45858,#45859,#45860),(#45861,#45862,#45863,#45864,
#45865,#45866,#45867,#45868,#45869,#45870,#45871,#45872,#45873,#45874,#45875,
#45876,#45877,#45878,#45879,#45880,#45881,#45882,#45883,#45884,#45885,#45886,
#45887,#45888,#45889,#45890,#45891,#45892,#45893,#45894,#45895,#45896,#45897,
#45898,#45899,#45900,#45901,#45902,#45903,#45904,#45905,#45906,#45907,#45908,
#45909,#45910,#45911,#45912,#45913,#45914,#45915,#45916,#45917,#45918,#45919,
#45920,#45921,#45922,#45923,#45924,#45925,#45926,#45927,#45928,#45929,#45930,
#45931,#45932,#45933,#45934,#45935,#45936,#45937,#45938,#45939,#45940,#45941,
#45942,#45943,#45944,#45945,#45946,#45947,#45948,#45949,#45950,#45951,#45952,
#45953,#45954,#45955,#45956,#45957,#45958,#45959,#45960,#45961,#45962,#45963,
#45964,#45965,#45966,#45967,#45968,#45969,#45970,#45971,#45972,#45973,#45974,
#45975,#45976,#45977,#45978,#45979,#45980,#45981,#45982,#45983,#45984,#45985,
#45986,#45987,#45988,#45989,#45990,#45991,#45992,#45993,#45994,#45995,#45996,
#45997,#45998,#45999,#46000,#46001,#46002,#46003,#46004),(#46005,#46006,
#46007,#46008,#46009,#46010,#46011,#46012,#46013,#46014,#46015,#46016,#46017,
#46018,#46019,#46020,#46021,#46022,#46023,#46024,#46025,#46026,#46027,#46028,
#46029,#46030,#46031,#46032,#46033,#46034,#46035,#46036,#46037,#46038,#46039,
#46040,#46041,#46042,#46043,#46044,#46045,#46046,#46047,#46048,#46049,#46050,
#46051,#46052,#46053,#46054,#46055,#46056,#46057,#46058,#46059,#46060,#46061,
#46062,#46063,#46064,#46065,#46066,#46067,#46068,#46069,#46070,#46071,#46072,
#46073,#46074,#46075,#46076,#46077,#46078,#46079,#46080,#46081,#46082,#46083,
#46084,#46085,#46086,#46087,#46088,#46089,#46090,#46091,#46092,#46093,#46094,
#46095,#46096,#46097,#46098,#46099,#46100,#46101,#46102,#46103,#46104,#46105,
#46106,#46107,#46108,#46109,#46110,#46111,#46112,#46113,#46114,#46115,#46116,
#46117,#46118,#46119,#46120,#46121,#46122,#46123,#46124,#46125,#46126,#46127,
#46128,#46129,#46130,#46131,#46132,#46133,#46134,#46135,#46136,#46137,#46138,
#46139,#46140,#46141,#46142,#46143,#46144,#46145,#46146,#46147,#46148),
(#46149,#46150,#46151,#46152,#46153,#46154,#46155,#46156,#46157,#46158,
#46159,#46160,#46161,#46162,#46163,#46164,#46165,#46166,#46167,#46168,#46169,
#46170,#46171,#46172,#46173,#46174,#46175,#46176,#46177,#46178,#46179,#46180,
#46181,#46182,#46183,#46184,#46185,#46186,#46187,#46188,#46189,#46190,#46191,
#46192,#46193,#46194,#46195,#46196,#46197,#46198,#46199,#46200,#46201,#46202,
#46203,#46204,#46205,#46206,#46207,#46208,#46209,#46210,#46211,#46212,#46213,
#46214,#46215,#46216,#46217,#46218,#46219,#46220,#46221,#46222,#46223,#46224,
#46225,#46226,#46227,#46228,#46229,#46230,#46231,#46232,#46233,#46234,#46235,
#46236,#46237,#46238,#46239,#46240,#46241,#46242,#46243,#46244,#46245,#46246,
#46247,#46248,#46249,#46250,#46251,#46252,#46253,#46254,#46255,#46256,#46257,
#46258,#46259,#46260,#46261,#46262,#46263,#46264,#46265,#46266,#46267,#46268,
#46269,#46270,#46271,#46272,#46273,#46274,#46275,#46276,#46277,#46278,#46279,
#46280,#46281,#46282,#46283,#46284,#46285,#46286,#46287,#46288,#46289,#46290,
#46291,#46292),(#46293,#46294,#46295,#46296,#46297,#46298,#46299,#46300,
#46301,#46302,#46303,#46304,#46305,#46306,#46307,#46308,#46309,#46310,#46311,
#46312,#46313,#46314,#46315,#46316,#46317,#46318,#46319,#46320,#46321,#46322,
#46323,#46324,#46325,#46326,#46327,#46328,#46329,#46330,#46331,#46332,#46333,
#46334,#46335,#46336,#46337,#46338,#46339,#46340,#46341,#46342,#46343,#46344,
#46345,#46346,#46347,#46348,#46349,#46350,#46351,#46352,#46353,#46354,#46355,
#46356,#46357,#46358,#46359,#46360,#46361,#46362,#46363,#46364,#46365,#46366,
#46367,#46368,#46369,#46370,#46371,#46372,#46373,#46374,#46375,#46376,#46377,
#46378,#46379,#46380,#46381,#46382,#46383,#46384,#46385,#46386,#46387,#46388,
#46389,#46390,#46391,#46392,#46393,#46394,#46395,#46396,#46397,#46398,#46399,
#46400,#46401,#46402,#46403,#46404,#46405,#46406,#46407,#46408,#46409,#46410,
#46411,#46412,#46413,#46414,#46415,#46416,#46417,#46418,#46419,#46420,#46421,
#46422,#46423,#46424,#46425,#46426,#46427,#46428,#46429,#46430,#46431,#46432,
#46433,#46434,#46435,#46436),(#46437,#46438,#46439,#46440,#46441,#46442,
#46443,#46444,#46445,#46446,#46447,#46448,#46449,#46450,#46451,#46452,#46453,
#46454,#46455,#46456,#46457,#46458,#46459,#46460,#46461,#46462,#46463,#46464,
#46465,#46466,#46467,#46468,#46469,#46470,#46471,#46472,#46473,#46474,#46475,
#46476,#46477,#46478,#46479,#46480,#46481,#46482,#46483,#46484,#46485,#46486,
#46487,#46488,#46489,#46490,#46491,#46492,#46493,#46494,#46495,#46496,#46497,
#46498,#46499,#46500,#46501,#46502,#46503,#46504,#46505,#46506,#46507,#46508,
#46509,#46510,#46511,#46512,#46513,#46514,#46515,#46516,#46517,#46518,#46519,
#46520,#46521,#46522,#46523,#46524,#46525,#46526,#46527,#46528,#46529,#46530,
#46531,#46532,#46533,#46534,#46535,#46536,#46537,#46538,#46539,#46540,#46541,
#46542,#46543,#46544,#46545,#46546,#46547,#46548,#46549,#46550,#46551,#46552,
#46553,#46554,#46555,#46556,#46557,#46558,#46559,#46560,#46561,#46562,#46563,
#46564,#46565,#46566,#46567,#46568,#46569,#46570,#46571,#46572,#46573,#46574,
#46575,#46576,#46577,#46578,#46579,#46580),(#46581,#46582,#46583,#46584,
#46585,#46586,#46587,#46588,#46589,#46590,#46591,#46592,#46593,#46594,#46595,
#46596,#46597,#46598,#46599,#46600,#46601,#46602,#46603,#46604,#46605,#46606,
#46607,#46608,#46609,#46610,#46611,#46612,#46613,#46614,#46615,#46616,#46617,
#46618,#46619,#46620,#46621,#46622,#46623,#46624,#46625,#46626,#46627,#46628,
#46629,#46630,#46631,#46632,#46633,#46634,#46635,#46636,#46637,#46638,#46639,
#46640,#46641,#46642,#46643,#46644,#46645,#46646,#46647,#46648,#46649,#46650,
#46651,#46652,#46653,#46654,#46655,#46656,#46657,#46658,#46659,#46660,#46661,
#46662,#46663,#46664,#46665,#46666,#46667,#46668,#46669,#46670,#46671,#46672,
#46673,#46674,#46675,#46676,#46677,#46678,#46679,#46680,#46681,#46682,#46683,
#46684,#46685,#46686,#46687,#46688,#46689,#46690,#46691,#46692,#46693,#46694,
#46695,#46696,#46697,#46698,#46699,#46700,#46701,#46702,#46703,#46704,#46705,
#46706,#46707,#46708,#46709,#46710,#46711,#46712,#46713,#46714,#46715,#46716,
#46717,#46718,#46719,#46720,#46721,#46722,#46723,#46724),(#46725,#46726,
#46727,#46728,#46729,#46730,#46731,#46732,#46733,#46734,#46735,#46736,#46737,
#46738,#46739,#46740,#46741,#46742,#46743,#46744,#46745,#46746,#46747,#46748,
#46749,#46750,#46751,#46752,#46753,#46754,#46755,#46756,#46757,#46758,#46759,
#46760,#46761,#46762,#46763,#46764,#46765,#46766,#46767,#46768,#46769,#46770,
#46771,#46772,#46773,#46774,#46775,#46776,#46777,#46778,#46779,#46780,#46781,
#46782,#46783,#46784,#46785,#46786,#46787,#46788,#46789,#46790,#46791,#46792,
#46793,#46794,#46795,#46796,#46797,#46798,#46799,#46800,#46801,#46802,#46803,
#46804,#46805,#46806,#46807,#46808,#46809,#46810,#46811,#46812,#46813,#46814,
#46815,#46816,#46817,#46818,#46819,#46820,#46821,#46822,#46823,#46824,#46825,
#46826,#46827,#46828,#46829,#46830,#46831,#46832,#46833,#46834,#46835,#46836,
#46837,#46838,#46839,#46840,#46841,#46842,#46843,#46844,#46845,#46846,#46847,
#46848,#46849,#46850,#46851,#46852,#46853,#46854,#46855,#46856,#46857,#46858,
#46859,#46860,#46861,#46862,#46863,#46864,#46865,#46866,#46867,#46868),
(#46869,#46870,#46871,#46872,#46873,#46874,#46875,#46876,#46877,#46878,
#46879,#46880,#46881,#46882,#46883,#46884,#46885,#46886,#46887,#46888,#46889,
#46890,#46891,#46892,#46893,#46894,#46895,#46896,#46897,#46898,#46899,#46900,
#46901,#46902,#46903,#46904,#46905,#46906,#46907,#46908,#46909,#46910,#46911,
#46912,#46913,#46914,#46915,#46916,#46917,#46918,#46919,#46920,#46921,#46922,
#46923,#46924,#46925,#46926,#46927,#46928,#46929,#46930,#46931,#46932,#46933,
#46934,#46935,#46936,#46937,#46938,#46939,#46940,#46941,#46942,#46943,#46944,
#46945,#46946,#46947,#46948,#46949,#46950,#46951,#46952,#46953,#46954,#46955,
#46956,#46957,#46958,#46959,#46960,#46961,#46962,#46963,#46964,#46965,#46966,
#46967,#46968,#46969,#46970,#46971,#46972,#46973,#46974,#46975,#46976,#46977,
#46978,#46979,#46980,#46981,#46982,#46983,#46984,#46985,#46986,#46987,#46988,
#46989,#46990,#46991,#46992,#46993,#46994,#46995,#46996,#46997,#46998,#46999,
#47000,#47001,#47002,#47003,#47004,#47005,#47006,#47007,#47008,#47009,#47010,
#47011,#47012),(#47013,#47014,#47015,#47016,#47017,#47018,#47019,#47020,
#47021,#47022,#47023,#47024,#47025,#47026,#47027,#47028,#47029,#47030,#47031,
#47032,#47033,#47034,#47035,#47036,#47037,#47038,#47039,#47040,#47041,#47042,
#47043,#47044,#47045,#47046,#47047,#47048,#47049,#47050,#47051,#47052,#47053,
#47054,#47055,#47056,#47057,#47058,#47059,#47060,#47061,#47062,#47063,#47064,
#47065,#47066,#47067,#47068,#47069,#47070,#47071,#47072,#47073,#47074,#47075,
#47076,#47077,#47078,#47079,#47080,#47081,#47082,#47083,#47084,#47085,#47086,
#47087,#47088,#47089,#47090,#47091,#47092,#47093,#47094,#47095,#47096,#47097,
#47098,#47099,#47100,#47101,#47102,#47103,#47104,#47105,#47106,#47107,#47108,
#47109,#47110,#47111,#47112,#47113,#47114,#47115,#47116,#47117,#47118,#47119,
#47120,#47121,#47122,#47123,#47124,#47125,#47126,#47127,#47128,#47129,#47130,
#47131,#47132,#47133,#47134,#47135,#47136,#47137,#47138,#47139,#47140,#47141,
#47142,#47143,#47144,#47145,#47146,#47147,#47148,#47149,#47150,#47151,#47152,
#47153,#47154,#47155,#47156),(#47157,#47158,#47159,#47160,#47161,#47162,
#47163,#47164,#47165,#47166,#47167,#47168,#47169,#47170,#47171,#47172,#47173,
#47174,#47175,#47176,#47177,#47178,#47179,#47180,#47181,#47182,#47183,#47184,
#47185,#47186,#47187,#47188,#47189,#47190,#47191,#47192,#47193,#47194,#47195,
#47196,#47197,#47198,#47199,#47200,#47201,#47202,#47203,#47204,#47205,#47206,
#47207,#47208,#47209,#47210,#47211,#47212,#47213,#47214,#47215,#47216,#47217,
#47218,#47219,#47220,#47221,#47222,#47223,#47224,#47225,#47226,#47227,#47228,
#47229,#47230,#47231,#47232,#47233,#47234,#47235,#47236,#47237,#47238,#47239,
#47240,#47241,#47242,#47243,#47244,#47245,#47246,#47247,#47248,#47249,#47250,
#47251,#47252,#47253,#47254,#47255,#47256,#47257,#47258,#47259,#47260,#47261,
#47262,#47263,#47264,#47265,#47266,#47267,#47268,#47269,#47270,#47271,#47272,
#47273,#47274,#47275,#47276,#47277,#47278,#47279,#47280,#47281,#47282,#47283,
#47284,#47285,#47286,#47287,#47288,#47289,#47290,#47291,#47292,#47293,#47294,
#47295,#47296,#47297,#47298,#47299,#47300),(#47301,#47302,#47303,#47304,
#47305,#47306,#47307,#47308,#47309,#47310,#47311,#47312,#47313,#47314,#47315,
#47316,#47317,#47318,#47319,#47320,#47321,#47322,#47323,#47324,#47325,#47326,
#47327,#47328,#47329,#47330,#47331,#47332,#47333,#47334,#47335,#47336,#47337,
#47338,#47339,#47340,#47341,#47342,#47343,#47344,#47345,#47346,#47347,#47348,
#47349,#47350,#47351,#47352,#47353,#47354,#47355,#47356,#47357,#47358,#47359,
#47360,#47361,#47362,#47363,#47364,#47365,#47366,#47367,#47368,#47369,#47370,
#47371,#47372,#47373,#47374,#47375,#47376,#47377,#47378,#47379,#47380,#47381,
#47382,#47383,#47384,#47385,#47386,#47387,#47388,#47389,#47390,#47391,#47392,
#47393,#47394,#47395,#47396,#47397,#47398,#47399,#47400,#47401,#47402,#47403,
#47404,#47405,#47406,#47407,#47408,#47409,#47410,#47411,#47412,#47413,#47414,
#47415,#47416,#47417,#47418,#47419,#47420,#47421,#47422,#47423,#47424,#47425,
#47426,#47427,#47428,#47429,#47430,#47431,#47432,#47433,#47434,#47435,#47436,
#47437,#47438,#47439,#47440,#47441,#47442,#47443,#47444),(#47445,#47446,
#47447,#47448,#47449,#47450,#47451,#47452,#47453,#47454,#47455,#47456,#47457,
#47458,#47459,#47460,#47461,#47462,#47463,#47464,#47465,#47466,#47467,#47468,
#47469,#47470,#47471,#47472,#47473,#47474,#47475,#47476,#47477,#47478,#47479,
#47480,#47481,#47482,#47483,#47484,#47485,#47486,#47487,#47488,#47489,#47490,
#47491,#47492,#47493,#47494,#47495,#47496,#47497,#47498,#47499,#47500,#47501,
#47502,#47503,#47504,#47505,#47506,#47507,#47508,#47509,#47510,#47511,#47512,
#47513,#47514,#47515,#47516,#47517,#47518,#47519,#47520,#47521,#47522,#47523,
#47524,#47525,#47526,#47527,#47528,#47529,#47530,#47531,#47532,#47533,#47534,
#47535,#47536,#47537,#47538,#47539,#47540,#47541,#47542,#47543,#47544,#47545,
#47546,#47547,#47548,#47549,#47550,#47551,#47552,#47553,#47554,#47555,#47556,
#47557,#47558,#47559,#47560,#47561,#47562,#47563,#47564,#47565,#47566,#47567,
#47568,#47569,#47570,#47571,#47572,#47573,#47574,#47575,#47576,#47577,#47578,
#47579,#47580,#47581,#47582,#47583,#47584,#47585,#47586,#47587,#47588),
(#47589,#47590,#47591,#47592,#47593,#47594,#47595,#47596,#47597,#47598,
#47599,#47600,#47601,#47602,#47603,#47604,#47605,#47606,#47607,#47608,#47609,
#47610,#47611,#47612,#47613,#47614,#47615,#47616,#47617,#47618,#47619,#47620,
#47621,#47622,#47623,#47624,#47625,#47626,#47627,#47628,#47629,#47630,#47631,
#47632,#47633,#47634,#47635,#47636,#47637,#47638,#47639,#47640,#47641,#47642,
#47643,#47644,#47645,#47646,#47647,#47648,#47649,#47650,#47651,#47652,#47653,
#47654,#47655,#47656,#47657,#47658,#47659,#47660,#47661,#47662,#47663,#47664,
#47665,#47666,#47667,#47668,#47669,#47670,#47671,#47672,#47673,#47674,#47675,
#47676,#47677,#47678,#47679,#47680,#47681,#47682,#47683,#47684,#47685,#47686,
#47687,#47688,#47689,#47690,#47691,#47692,#47693,#47694,#47695,#47696,#47697,
#47698,#47699,#47700,#47701,#47702,#47703,#47704,#47705,#47706,#47707,#47708,
#47709,#47710,#47711,#47712,#47713,#47714,#47715,#47716,#47717,#47718,#47719,
#47720,#47721,#47722,#47723,#47724,#47725,#47726,#47727,#47728,#47729,#47730,
#47731,#47732),(#47733,#47734,#47735,#47736,#47737,#47738,#47739,#47740,
#47741,#47742,#47743,#47744,#47745,#47746,#47747,#47748,#47749,#47750,#47751,
#47752,#47753,#47754,#47755,#47756,#47757,#47758,#47759,#47760,#47761,#47762,
#47763,#47764,#47765,#47766,#47767,#47768,#47769,#47770,#47771,#47772,#47773,
#47774,#47775,#47776,#47777,#47778,#47779,#47780,#47781,#47782,#47783,#47784,
#47785,#47786,#47787,#47788,#47789,#47790,#47791,#47792,#47793,#47794,#47795,
#47796,#47797,#47798,#47799,#47800,#47801,#47802,#47803,#47804,#47805,#47806,
#47807,#47808,#47809,#47810,#47811,#47812,#47813,#47814,#47815,#47816,#47817,
#47818,#47819,#47820,#47821,#47822,#47823,#47824,#47825,#47826,#47827,#47828,
#47829,#47830,#47831,#47832,#47833,#47834,#47835,#47836,#47837,#47838,#47839,
#47840,#47841,#47842,#47843,#47844,#47845,#47846,#47847,#47848,#47849,#47850,
#47851,#47852,#47853,#47854,#47855,#47856,#47857,#47858,#47859,#47860,#47861,
#47862,#47863,#47864,#47865,#47866,#47867,#47868,#47869,#47870,#47871,#47872,
#47873,#47874,#47875,#47876),(#47877,#47878,#47879,#47880,#47881,#47882,
#47883,#47884,#47885,#47886,#47887,#47888,#47889,#47890,#47891,#47892,#47893,
#47894,#47895,#47896,#47897,#47898,#47899,#47900,#47901,#47902,#47903,#47904,
#47905,#47906,#47907,#47908,#47909,#47910,#47911,#47912,#47913,#47914,#47915,
#47916,#47917,#47918,#47919,#47920,#47921,#47922,#47923,#47924,#47925,#47926,
#47927,#47928,#47929,#47930,#47931,#47932,#47933,#47934,#47935,#47936,#47937,
#47938,#47939,#47940,#47941,#47942,#47943,#47944,#47945,#47946,#47947,#47948,
#47949,#47950,#47951,#47952,#47953,#47954,#47955,#47956,#47957,#47958,#47959,
#47960,#47961,#47962,#47963,#47964,#47965,#47966,#47967,#47968,#47969,#47970,
#47971,#47972,#47973,#47974,#47975,#47976,#47977,#47978,#47979,#47980,#47981,
#47982,#47983,#47984,#47985,#47986,#47987,#47988,#47989,#47990,#47991,#47992,
#47993,#47994,#47995,#47996,#47997,#47998,#47999,#48000,#48001,#48002,#48003,
#48004,#48005,#48006,#48007,#48008,#48009,#48010,#48011,#48012,#48013,#48014,
#48015,#48016,#48017,#48018,#48019,#48020),(#48021,#48022,#48023,#48024,
#48025,#48026,#48027,#48028,#48029,#48030,#48031,#48032,#48033,#48034,#48035,
#48036,#48037,#48038,#48039,#48040,#48041,#48042,#48043,#48044,#48045,#48046,
#48047,#48048,#48049,#48050,#48051,#48052,#48053,#48054,#48055,#48056,#48057,
#48058,#48059,#48060,#48061,#48062,#48063,#48064,#48065,#48066,#48067,#48068,
#48069,#48070,#48071,#48072,#48073,#48074,#48075,#48076,#48077,#48078,#48079,
#48080,#48081,#48082,#48083,#48084,#48085,#48086,#48087,#48088,#48089,#48090,
#48091,#48092,#48093,#48094,#48095,#48096,#48097,#48098,#48099,#48100,#48101,
#48102,#48103,#48104,#48105,#48106,#48107,#48108,#48109,#48110,#48111,#48112,
#48113,#48114,#48115,#48116,#48117,#48118,#48119,#48120,#48121,#48122,#48123,
#48124,#48125,#48126,#48127,#48128,#48129,#48130,#48131,#48132,#48133,#48134,
#48135,#48136,#48137,#48138,#48139,#48140,#48141,#48142,#48143,#48144,#48145,
#48146,#48147,#48148,#48149,#48150,#48151,#48152,#48153,#48154,#48155,#48156,
#48157,#48158,#48159,#48160,#48161,#48162,#48163,#48164),(#48165,#48166,
#48167,#48168,#48169,#48170,#48171,#48172,#48173,#48174,#48175,#48176,#48177,
#48178,#48179,#48180,#48181,#48182,#48183,#48184,#48185,#48186,#48187,#48188,
#48189,#48190,#48191,#48192,#48193,#48194,#48195,#48196,#48197,#48198,#48199,
#48200,#48201,#48202,#48203,#48204,#48205,#48206,#48207,#48208,#48209,#48210,
#48211,#48212,#48213,#48214,#48215,#48216,#48217,#48218,#48219,#48220,#48221,
#48222,#48223,#48224,#48225,#48226,#48227,#48228,#48229,#48230,#48231,#48232,
#48233,#48234,#48235,#48236,#48237,#48238,#48239,#48240,#48241,#48242,#48243,
#48244,#48245,#48246,#48247,#48248,#48249,#48250,#48251,#48252,#48253,#48254,
#48255,#48256,#48257,#48258,#48259,#48260,#48261,#48262,#48263,#48264,#48265,
#48266,#48267,#48268,#48269,#48270,#48271,#48272,#48273,#48274,#48275,#48276,
#48277,#48278,#48279,#48280,#48281,#48282,#48283,#48284,#48285,#48286,#48287,
#48288,#48289,#48290,#48291,#48292,#48293,#48294,#48295,#48296,#48297,#48298,
#48299,#48300,#48301,#48302,#48303,#48304,#48305,#48306,#48307,#48308),
(#48309,#48310,#48311,#48312,#48313,#48314,#48315,#48316,#48317,#48318,
#48319,#48320,#48321,#48322,#48323,#48324,#48325,#48326,#48327,#48328,#48329,
#48330,#48331,#48332,#48333,#48334,#48335,#48336,#48337,#48338,#48339,#48340,
#48341,#48342,#48343,#48344,#48345,#48346,#48347,#48348,#48349,#48350,#48351,
#48352,#48353,#48354,#48355,#48356,#48357,#48358,#48359,#48360,#48361,#48362,
#48363,#48364,#48365,#48366,#48367,#48368,#48369,#48370,#48371,#48372,#48373,
#48374,#48375,#48376,#48377,#48378,#48379,#48380,#48381,#48382,#48383,#48384,
#48385,#48386,#48387,#48388,#48389,#48390,#48391,#48392,#48393,#48394,#48395,
#48396,#48397,#48398,#48399,#48400,#48401,#48402,#48403,#48404,#48405,#48406,
#48407,#48408,#48409,#48410,#48411,#48412,#48413,#48414,#48415,#48416,#48417,
#48418,#48419,#48420,#48421,#48422,#48423,#48424,#48425,#48426,#48427,#48428,
#48429,#48430,#48431,#48432,#48433,#48434,#48435,#48436,#48437,#48438,#48439,
#48440,#48441,#48442,#48443,#48444,#48445,#48446,#48447,#48448,#48449,#48450,
#48451,#48452),(#48453,#48454,#48455,#48456,#48457,#48458,#48459,#48460,
#48461,#48462,#48463,#48464,#48465,#48466,#48467,#48468,#48469,#48470,#48471,
#48472,#48473,#48474,#48475,#48476,#48477,#48478,#48479,#48480,#48481,#48482,
#48483,#48484,#48485,#48486,#48487,#48488,#48489,#48490,#48491,#48492,#48493,
#48494,#48495,#48496,#48497,#48498,#48499,#48500,#48501,#48502,#48503,#48504,
#48505,#48506,#48507,#48508,#48509,#48510,#48511,#48512,#48513,#48514,#48515,
#48516,#48517,#48518,#48519,#48520,#48521,#48522,#48523,#48524,#48525,#48526,
#48527,#48528,#48529,#48530,#48531,#48532,#48533,#48534,#48535,#48536,#48537,
#48538,#48539,#48540,#48541,#48542,#48543,#48544,#48545,#48546,#48547,#48548,
#48549,#48550,#48551,#48552,#48553,#48554,#48555,#48556,#48557,#48558,#48559,
#48560,#48561,#48562,#48563,#48564,#48565,#48566,#48567,#48568,#48569,#48570,
#48571,#48572,#48573,#48574,#48575,#48576,#48577,#48578,#48579,#48580,#48581,
#48582,#48583,#48584,#48585,#48586,#48587,#48588,#48589,#48590,#48591,#48592,
#48593,#48594,#48595,#48596),(#48597,#48598,#48599,#48600,#48601,#48602,
#48603,#48604,#48605,#48606,#48607,#48608,#48609,#48610,#48611,#48612,#48613,
#48614,#48615,#48616,#48617,#48618,#48619,#48620,#48621,#48622,#48623,#48624,
#48625,#48626,#48627,#48628,#48629,#48630,#48631,#48632,#48633,#48634,#48635,
#48636,#48637,#48638,#48639,#48640,#48641,#48642,#48643,#48644,#48645,#48646,
#48647,#48648,#48649,#48650,#48651,#48652,#48653,#48654,#48655,#48656,#48657,
#48658,#48659,#48660,#48661,#48662,#48663,#48664,#48665,#48666,#48667,#48668,
#48669,#48670,#48671,#48672,#48673,#48674,#48675,#48676,#48677,#48678,#48679,
#48680,#48681,#48682,#48683,#48684,#48685,#48686,#48687,#48688,#48689,#48690,
#48691,#48692,#48693,#48694,#48695,#48696,#48697,#48698,#48699,#48700,#48701,
#48702,#48703,#48704,#48705,#48706,#48707,#48708,#48709,#48710,#48711,#48712,
#48713,#48714,#48715,#48716,#48717,#48718,#48719,#48720,#48721,#48722,#48723,
#48724,#48725,#48726,#48727,#48728,#48729,#48730,#48731,#48732,#48733,#48734,
#48735,#48736,#48737,#48738,#48739,#48740),(#48741,#48742,#48743,#48744,
#48745,#48746,#48747,#48748,#48749,#48750,#48751,#48752,#48753,#48754,#48755,
#48756,#48757,#48758,#48759,#48760,#48761,#48762,#48763,#48764,#48765,#48766,
#48767,#48768,#48769,#48770,#48771,#48772,#48773,#48774,#48775,#48776,#48777,
#48778,#48779,#48780,#48781,#48782,#48783,#48784,#48785,#48786,#48787,#48788,
#48789,#48790,#48791,#48792,#48793,#48794,#48795,#48796,#48797,#48798,#48799,
#48800,#48801,#48802,#48803,#48804,#48805,#48806,#48807,#48808,#48809,#48810,
#48811,#48812,#48813,#48814,#48815,#48816,#48817,#48818,#48819,#48820,#48821,
#48822,#48823,#48824,#48825,#48826,#48827,#48828,#48829,#48830,#48831,#48832,
#48833,#48834,#48835,#48836,#48837,#48838,#48839,#48840,#48841,#48842,#48843,
#48844,#48845,#48846,#48847,#48848,#48849,#48850,#48851,#48852,#48853,#48854,
#48855,#48856,#48857,#48858,#48859,#48860,#48861,#48862,#48863,#48864,#48865,
#48866,#48867,#48868,#48869,#48870,#48871,#48872,#48873,#48874,#48875,#48876,
#48877,#48878,#48879,#48880,#48881,#48882,#48883,#48884),(#48885,#48886,
#48887,#48888,#48889,#48890,#48891,#48892,#48893,#48894,#48895,#48896,#48897,
#48898,#48899,#48900,#48901,#48902,#48903,#48904,#48905,#48906,#48907,#48908,
#48909,#48910,#48911,#48912,#48913,#48914,#48915,#48916,#48917,#48918,#48919,
#48920,#48921,#48922,#48923,#48924,#48925,#48926,#48927,#48928,#48929,#48930,
#48931,#48932,#48933,#48934,#48935,#48936,#48937,#48938,#48939,#48940,#48941,
#48942,#48943,#48944,#48945,#48946,#48947,#48948,#48949,#48950,#48951,#48952,
#48953,#48954,#48955,#48956,#48957,#48958,#48959,#48960,#48961,#48962,#48963,
#48964,#48965,#48966,#48967,#48968,#48969,#48970,#48971,#48972,#48973,#48974,
#48975,#48976,#48977,#48978,#48979,#48980,#48981,#48982,#48983,#48984,#48985,
#48986,#48987,#48988,#48989,#48990,#48991,#48992,#48993,#48994,#48995,#48996,
#48997,#48998,#48999,#49000,#49001,#49002,#49003,#49004,#49005,#49006,#49007,
#49008,#49009,#49010,#49011,#49012,#49013,#49014,#49015,#49016,#49017,#49018,
#49019,#49020,#49021,#49022,#49023,#49024,#49025,#49026,#49027,#49028),
(#49029,#49030,#49031,#49032,#49033,#49034,#49035,#49036,#49037,#49038,
#49039,#49040,#49041,#49042,#49043,#49044,#49045,#49046,#49047,#49048,#49049,
#49050,#49051,#49052,#49053,#49054,#49055,#49056,#49057,#49058,#49059,#49060,
#49061,#49062,#49063,#49064,#49065,#49066,#49067,#49068,#49069,#49070,#49071,
#49072,#49073,#49074,#49075,#49076,#49077,#49078,#49079,#49080,#49081,#49082,
#49083,#49084,#49085,#49086,#49087,#49088,#49089,#49090,#49091,#49092,#49093,
#49094,#49095,#49096,#49097,#49098,#49099,#49100,#49101,#49102,#49103,#49104,
#49105,#49106,#49107,#49108,#49109,#49110,#49111,#49112,#49113,#49114,#49115,
#49116,#49117,#49118,#49119,#49120,#49121,#49122,#49123,#49124,#49125,#49126,
#49127,#49128,#49129,#49130,#49131,#49132,#49133,#49134,#49135,#49136,#49137,
#49138,#49139,#49140,#49141,#49142,#49143,#49144,#49145,#49146,#49147,#49148,
#49149,#49150,#49151,#49152,#49153,#49154,#49155,#49156,#49157,#49158,#49159,
#49160,#49161,#49162,#49163,#49164,#49165,#49166,#49167,#49168,#49169,#49170,
#49171,#49172),(#49173,#49174,#49175,#49176,#49177,#49178,#49179,#49180,
#49181,#49182,#49183,#49184,#49185,#49186,#49187,#49188,#49189,#49190,#49191,
#49192,#49193,#49194,#49195,#49196,#49197,#49198,#49199,#49200,#49201,#49202,
#49203,#49204,#49205,#49206,#49207,#49208,#49209,#49210,#49211,#49212,#49213,
#49214,#49215,#49216,#49217,#49218,#49219,#49220,#49221,#49222,#49223,#49224,
#49225,#49226,#49227,#49228,#49229,#49230,#49231,#49232,#49233,#49234,#49235,
#49236,#49237,#49238,#49239,#49240,#49241,#49242,#49243,#49244,#49245,#49246,
#49247,#49248,#49249,#49250,#49251,#49252,#49253,#49254,#49255,#49256,#49257,
#49258,#49259,#49260,#49261,#49262,#49263,#49264,#49265,#49266,#49267,#49268,
#49269,#49270,#49271,#49272,#49273,#49274,#49275,#49276,#49277,#49278,#49279,
#49280,#49281,#49282,#49283,#49284,#49285,#49286,#49287,#49288,#49289,#49290,
#49291,#49292,#49293,#49294,#49295,#49296,#49297,#49298,#49299,#49300,#49301,
#49302,#49303,#49304,#49305,#49306,#49307,#49308,#49309,#49310,#49311,#49312,
#49313,#49314,#49315,#49316),(#49317,#49318,#49319,#49320,#49321,#49322,
#49323,#49324,#49325,#49326,#49327,#49328,#49329,#49330,#49331,#49332,#49333,
#49334,#49335,#49336,#49337,#49338,#49339,#49340,#49341,#49342,#49343,#49344,
#49345,#49346,#49347,#49348,#49349,#49350,#49351,#49352,#49353,#49354,#49355,
#49356,#49357,#49358,#49359,#49360,#49361,#49362,#49363,#49364,#49365,#49366,
#49367,#49368,#49369,#49370,#49371,#49372,#49373,#49374,#49375,#49376,#49377,
#49378,#49379,#49380,#49381,#49382,#49383,#49384,#49385,#49386,#49387,#49388,
#49389,#49390,#49391,#49392,#49393,#49394,#49395,#49396,#49397,#49398,#49399,
#49400,#49401,#49402,#49403,#49404,#49405,#49406,#49407,#49408,#49409,#49410,
#49411,#49412,#49413,#49414,#49415,#49416,#49417,#49418,#49419,#49420,#49421,
#49422,#49423,#49424,#49425,#49426,#49427,#49428,#49429,#49430,#49431,#49432,
#49433,#49434,#49435,#49436,#49437,#49438,#49439,#49440,#49441,#49442,#49443,
#49444,#49445,#49446,#49447,#49448,#49449,#49450,#49451,#49452,#49453,#49454,
#49455,#49456,#49457,#49458,#49459,#49460),(#49461,#49462,#49463,#49464,
#49465,#49466,#49467,#49468,#49469,#49470,#49471,#49472,#49473,#49474,#49475,
#49476,#49477,#49478,#49479,#49480,#49481,#49482,#49483,#49484,#49485,#49486,
#49487,#49488,#49489,#49490,#49491,#49492,#49493,#49494,#49495,#49496,#49497,
#49498,#49499,#49500,#49501,#49502,#49503,#49504,#49505,#49506,#49507,#49508,
#49509,#49510,#49511,#49512,#49513,#49514,#49515,#49516,#49517,#49518,#49519,
#49520,#49521,#49522,#49523,#49524,#49525,#49526,#49527,#49528,#49529,#49530,
#49531,#49532,#49533,#49534,#49535,#49536,#49537,#49538,#49539,#49540,#49541,
#49542,#49543,#49544,#49545,#49546,#49547,#49548,#49549,#49550,#49551,#49552,
#49553,#49554,#49555,#49556,#49557,#49558,#49559,#49560,#49561,#49562,#49563,
#49564,#49565,#49566,#49567,#49568,#49569,#49570,#49571,#49572,#49573,#49574,
#49575,#49576,#49577,#49578,#49579,#49580,#49581,#49582,#49583,#49584,#49585,
#49586,#49587,#49588,#49589,#49590,#49591,#49592,#49593,#49594,#49595,#49596,
#49597,#49598,#49599,#49600,#49601,#49602,#49603,#49604),(#49605,#49606,
#49607,#49608,#49609,#49610,#49611,#49612,#49613,#49614,#49615,#49616,#49617,
#49618,#49619,#49620,#49621,#49622,#49623,#49624,#49625,#49626,#49627,#49628,
#49629,#49630,#49631,#49632,#49633,#49634,#49635,#49636,#49637,#49638,#49639,
#49640,#49641,#49642,#49643,#49644,#49645,#49646,#49647,#49648,#49649,#49650,
#49651,#49652,#49653,#49654,#49655,#49656,#49657,#49658,#49659,#49660,#49661,
#49662,#49663,#49664,#49665,#49666,#49667,#49668,#49669,#49670,#49671,#49672,
#49673,#49674,#49675,#49676,#49677,#49678,#49679,#49680,#49681,#49682,#49683,
#49684,#49685,#49686,#49687,#49688,#49689,#49690,#49691,#49692,#49693,#49694,
#49695,#49696,#49697,#49698,#49699,#49700,#49701,#49702,#49703,#49704,#49705,
#49706,#49707,#49708,#49709,#49710,#49711,#49712,#49713,#49714,#49715,#49716,
#49717,#49718,#49719,#49720,#49721,#49722,#49723,#49724,#49725,#49726,#49727,
#49728,#49729,#49730,#49731,#49732,#49733,#49734,#49735,#49736,#49737,#49738,
#49739,#49740,#49741,#49742,#49743,#49744,#49745,#49746,#49747,#49748),
(#49749,#49750,#49751,#49752,#49753,#49754,#49755,#49756,#49757,#49758,
#49759,#49760,#49761,#49762,#49763,#49764,#49765,#49766,#49767,#49768,#49769,
#49770,#49771,#49772,#49773,#49774,#49775,#49776,#49777,#49778,#49779,#49780,
#49781,#49782,#49783,#49784,#49785,#49786,#49787,#49788,#49789,#49790,#49791,
#49792,#49793,#49794,#49795,#49796,#49797,#49798,#49799,#49800,#49801,#49802,
#49803,#49804,#49805,#49806,#49807,#49808,#49809,#49810,#49811,#49812,#49813,
#49814,#49815,#49816,#49817,#49818,#49819,#49820,#49821,#49822,#49823,#49824,
#49825,#49826,#49827,#49828,#49829,#49830,#49831,#49832,#49833,#49834,#49835,
#49836,#49837,#49838,#49839,#49840,#49841,#49842,#49843,#49844,#49845,#49846,
#49847,#49848,#49849,#49850,#49851,#49852,#49853,#49854,#49855,#49856,#49857,
#49858,#49859,#49860,#49861,#49862,#49863,#49864,#49865,#49866,#49867,#49868,
#49869,#49870,#49871,#49872,#49873,#49874,#49875,#49876,#49877,#49878,#49879,
#49880,#49881,#49882,#49883,#49884,#49885,#49886,#49887,#49888,#49889,#49890,
#49891,#49892),(#49893,#49894,#49895,#49896,#49897,#49898,#49899,#49900,
#49901,#49902,#49903,#49904,#49905,#49906,#49907,#49908,#49909,#49910,#49911,
#49912,#49913,#49914,#49915,#49916,#49917,#49918,#49919,#49920,#49921,#49922,
#49923,#49924,#49925,#49926,#49927,#49928,#49929,#49930,#49931,#49932,#49933,
#49934,#49935,#49936,#49937,#49938,#49939,#49940,#49941,#49942,#49943,#49944,
#49945,#49946,#49947,#49948,#49949,#49950,#49951,#49952,#49953,#49954,#49955,
#49956,#49957,#49958,#49959,#49960,#49961,#49962,#49963,#49964,#49965,#49966,
#49967,#49968,#49969,#49970,#49971,#49972,#49973,#49974,#49975,#49976,#49977,
#49978,#49979,#49980,#49981,#49982,#49983,#49984,#49985,#49986,#49987,#49988,
#49989,#49990,#49991,#49992,#49993,#49994,#49995,#49996,#49997,#49998,#49999,
#50000,#50001,#50002,#50003,#50004,#50005,#50006,#50007,#50008,#50009,#50010,
#50011,#50012,#50013,#50014,#50015,#50016,#50017,#50018,#50019,#50020,#50021,
#50022,#50023,#50024,#50025,#50026,#50027,#50028,#50029,#50030,#50031,#50032,
#50033,#50034,#50035,#50036),(#50037,#50038,#50039,#50040,#50041,#50042,
#50043,#50044,#50045,#50046,#50047,#50048,#50049,#50050,#50051,#50052,#50053,
#50054,#50055,#50056,#50057,#50058,#50059,#50060,#50061,#50062,#50063,#50064,
#50065,#50066,#50067,#50068,#50069,#50070,#50071,#50072,#50073,#50074,#50075,
#50076,#50077,#50078,#50079,#50080,#50081,#50082,#50083,#50084,#50085,#50086,
#50087,#50088,#50089,#50090,#50091,#50092,#50093,#50094,#50095,#50096,#50097,
#50098,#50099,#50100,#50101,#50102,#50103,#50104,#50105,#50106,#50107,#50108,
#50109,#50110,#50111,#50112,#50113,#50114,#50115,#50116,#50117,#50118,#50119,
#50120,#50121,#50122,#50123,#50124,#50125,#50126,#50127,#50128,#50129,#50130,
#50131,#50132,#50133,#50134,#50135,#50136,#50137,#50138,#50139,#50140,#50141,
#50142,#50143,#50144,#50145,#50146,#50147,#50148,#50149,#50150,#50151,#50152,
#50153,#50154,#50155,#50156,#50157,#50158,#50159,#50160,#50161,#50162,#50163,
#50164,#50165,#50166,#50167,#50168,#50169,#50170,#50171,#50172,#50173,#50174,
#50175,#50176,#50177,#50178,#50179,#50180),(#50181,#50182,#50183,#50184,
#50185,#50186,#50187,#50188,#50189,#50190,#50191,#50192,#50193,#50194,#50195,
#50196,#50197,#50198,#50199,#50200,#50201,#50202,#50203,#50204,#50205,#50206,
#50207,#50208,#50209,#50210,#50211,#50212,#50213,#50214,#50215,#50216,#50217,
#50218,#50219,#50220,#50221,#50222,#50223,#50224,#50225,#50226,#50227,#50228,
#50229,#50230,#50231,#50232,#50233,#50234,#50235,#50236,#50237,#50238,#50239,
#50240,#50241,#50242,#50243,#50244,#50245,#50246,#50247,#50248,#50249,#50250,
#50251,#50252,#50253,#50254,#50255,#50256,#50257,#50258,#50259,#50260,#50261,
#50262,#50263,#50264,#50265,#50266,#50267,#50268,#50269,#50270,#50271,#50272,
#50273,#50274,#50275,#50276,#50277,#50278,#50279,#50280,#50281,#50282,#50283,
#50284,#50285,#50286,#50287,#50288,#50289,#50290,#50291,#50292,#50293,#50294,
#50295,#50296,#50297,#50298,#50299,#50300,#50301,#50302,#50303,#50304,#50305,
#50306,#50307,#50308,#50309,#50310,#50311,#50312,#50313,#50314,#50315,#50316,
#50317,#50318,#50319,#50320,#50321,#50322,#50323,#50324),(#50325,#50326,
#50327,#50328,#50329,#50330,#50331,#50332,#50333,#50334,#50335,#50336,#50337,
#50338,#50339,#50340,#50341,#50342,#50343,#50344,#50345,#50346,#50347,#50348,
#50349,#50350,#50351,#50352,#50353,#50354,#50355,#50356,#50357,#50358,#50359,
#50360,#50361,#50362,#50363,#50364,#50365,#50366,#50367,#50368,#50369,#50370,
#50371,#50372,#50373,#50374,#50375,#50376,#50377,#50378,#50379,#50380,#50381,
#50382,#50383,#50384,#50385,#50386,#50387,#50388,#50389,#50390,#50391,#50392,
#50393,#50394,#50395,#50396,#50397,#50398,#50399,#50400,#50401,#50402,#50403,
#50404,#50405,#50406,#50407,#50408,#50409,#50410,#50411,#50412,#50413,#50414,
#50415,#50416,#50417,#50418,#50419,#50420,#50421,#50422,#50423,#50424,#50425,
#50426,#50427,#50428,#50429,#50430,#50431,#50432,#50433,#50434,#50435,#50436,
#50437,#50438,#50439,#50440,#50441,#50442,#50443,#50444,#50445,#50446,#50447,
#50448,#50449,#50450,#50451,#50452,#50453,#50454,#50455,#50456,#50457,#50458,
#50459,#50460,#50461,#50462,#50463,#50464,#50465,#50466,#50467,#50468),
(#50469,#50470,#50471,#50472,#50473,#50474,#50475,#50476,#50477,#50478,
#50479,#50480,#50481,#50482,#50483,#50484,#50485,#50486,#50487,#50488,#50489,
#50490,#50491,#50492,#50493,#50494,#50495,#50496,#50497,#50498,#50499,#50500,
#50501,#50502,#50503,#50504,#50505,#50506,#50507,#50508,#50509,#50510,#50511,
#50512,#50513,#50514,#50515,#50516,#50517,#50518,#50519,#50520,#50521,#50522,
#50523,#50524,#50525,#50526,#50527,#50528,#50529,#50530,#50531,#50532,#50533,
#50534,#50535,#50536,#50537,#50538,#50539,#50540,#50541,#50542,#50543,#50544,
#50545,#50546,#50547,#50548,#50549,#50550,#50551,#50552,#50553,#50554,#50555,
#50556,#50557,#50558,#50559,#50560,#50561,#50562,#50563,#50564,#50565,#50566,
#50567,#50568,#50569,#50570,#50571,#50572,#50573,#50574,#50575,#50576,#50577,
#50578,#50579,#50580,#50581,#50582,#50583,#50584,#50585,#50586,#50587,#50588,
#50589,#50590,#50591,#50592,#50593,#50594,#50595,#50596,#50597,#50598,#50599,
#50600,#50601,#50602,#50603,#50604,#50605,#50606,#50607,#50608,#50609,#50610,
#50611,#50612),(#50613,#50614,#50615,#50616,#50617,#50618,#50619,#50620,
#50621,#50622,#50623,#50624,#50625,#50626,#50627,#50628,#50629,#50630,#50631,
#50632,#50633,#50634,#50635,#50636,#50637,#50638,#50639,#50640,#50641,#50642,
#50643,#50644,#50645,#50646,#50647,#50648,#50649,#50650,#50651,#50652,#50653,
#50654,#50655,#50656,#50657,#50658,#50659,#50660,#50661,#50662,#50663,#50664,
#50665,#50666,#50667,#50668,#50669,#50670,#50671,#50672,#50673,#50674,#50675,
#50676,#50677,#50678,#50679,#50680,#50681,#50682,#50683,#50684,#50685,#50686,
#50687,#50688,#50689,#50690,#50691,#50692,#50693,#50694,#50695,#50696,#50697,
#50698,#50699,#50700,#50701,#50702,#50703,#50704,#50705,#50706,#50707,#50708,
#50709,#50710,#50711,#50712,#50713,#50714,#50715,#50716,#50717,#50718,#50719,
#50720,#50721,#50722,#50723,#50724,#50725,#50726,#50727,#50728,#50729,#50730,
#50731,#50732,#50733,#50734,#50735,#50736,#50737,#50738,#50739,#50740,#50741,
#50742,#50743,#50744,#50745,#50746,#50747,#50748,#50749,#50750,#50751,#50752,
#50753,#50754,#50755,#50756),(#50757,#50758,#50759,#50760,#50761,#50762,
#50763,#50764,#50765,#50766,#50767,#50768,#50769,#50770,#50771,#50772,#50773,
#50774,#50775,#50776,#50777,#50778,#50779,#50780,#50781,#50782,#50783,#50784,
#50785,#50786,#50787,#50788,#50789,#50790,#50791,#50792,#50793,#50794,#50795,
#50796,#50797,#50798,#50799,#50800,#50801,#50802,#50803,#50804,#50805,#50806,
#50807,#50808,#50809,#50810,#50811,#50812,#50813,#50814,#50815,#50816,#50817,
#50818,#50819,#50820,#50821,#50822,#50823,#50824,#50825,#50826,#50827,#50828,
#50829,#50830,#50831,#50832,#50833,#50834,#50835,#50836,#50837,#50838,#50839,
#50840,#50841,#50842,#50843,#50844,#50845,#50846,#50847,#50848,#50849,#50850,
#50851,#50852,#50853,#50854,#50855,#50856,#50857,#50858,#50859,#50860,#50861,
#50862,#50863,#50864,#50865,#50866,#50867,#50868,#50869,#50870,#50871,#50872,
#50873,#50874,#50875,#50876,#50877,#50878,#50879,#50880,#50881,#50882,#50883,
#50884,#50885,#50886,#50887,#50888,#50889,#50890,#50891,#50892,#50893,#50894,
#50895,#50896,#50897,#50898,#50899,#50900),(#50901,#50902,#50903,#50904,
#50905,#50906,#50907,#50908,#50909,#50910,#50911,#50912,#50913,#50914,#50915,
#50916,#50917,#50918,#50919,#50920,#50921,#50922,#50923,#50924,#50925,#50926,
#50927,#50928,#50929,#50930,#50931,#50932,#50933,#50934,#50935,#50936,#50937,
#50938,#50939,#50940,#50941,#50942,#50943,#50944,#50945,#50946,#50947,#50948,
#50949,#50950,#50951,#50952,#50953,#50954,#50955,#50956,#50957,#50958,#50959,
#50960,#50961,#50962,#50963,#50964,#50965,#50966,#50967,#50968,#50969,#50970,
#50971,#50972,#50973,#50974,#50975,#50976,#50977,#50978,#50979,#50980,#50981,
#50982,#50983,#50984,#50985,#50986,#50987,#50988,#50989,#50990,#50991,#50992,
#50993,#50994,#50995,#50996,#50997,#50998,#50999,#51000,#51001,#51002,#51003,
#51004,#51005,#51006,#51007,#51008,#51009,#51010,#51011,#51012,#51013,#51014,
#51015,#51016,#51017,#51018,#51019,#51020,#51021,#51022,#51023,#51024,#51025,
#51026,#51027,#51028,#51029,#51030,#51031,#51032,#51033,#51034,#51035,#51036,
#51037,#51038,#51039,#51040,#51041,#51042,#51043,#51044),(#51045,#51046,
#51047,#51048,#51049,#51050,#51051,#51052,#51053,#51054,#51055,#51056,#51057,
#51058,#51059,#51060,#51061,#51062,#51063,#51064,#51065,#51066,#51067,#51068,
#51069,#51070,#51071,#51072,#51073,#51074,#51075,#51076,#51077,#51078,#51079,
#51080,#51081,#51082,#51083,#51084,#51085,#51086,#51087,#51088,#51089,#51090,
#51091,#51092,#51093,#51094,#51095,#51096,#51097,#51098,#51099,#51100,#51101,
#51102,#51103,#51104,#51105,#51106,#51107,#51108,#51109,#51110,#51111,#51112,
#51113,#51114,#51115,#51116,#51117,#51118,#51119,#51120,#51121,#51122,#51123,
#51124,#51125,#51126,#51127,#51128,#51129,#51130,#51131,#51132,#51133,#51134,
#51135,#51136,#51137,#51138,#51139,#51140,#51141,#51142,#51143,#51144,#51145,
#51146,#51147,#51148,#51149,#51150,#51151,#51152,#51153,#51154,#51155,#51156,
#51157,#51158,#51159,#51160,#51161,#51162,#51163,#51164,#51165,#51166,#51167,
#51168,#51169,#51170,#51171,#51172,#51173,#51174,#51175,#51176,#51177,#51178,
#51179,#51180,#51181,#51182,#51183,#51184,#51185,#51186,#51187,#51188),
(#51189,#51190,#51191,#51192,#51193,#51194,#51195,#51196,#51197,#51198,
#51199,#51200,#51201,#51202,#51203,#51204,#51205,#51206,#51207,#51208,#51209,
#51210,#51211,#51212,#51213,#51214,#51215,#51216,#51217,#51218,#51219,#51220,
#51221,#51222,#51223,#51224,#51225,#51226,#51227,#51228,#51229,#51230,#51231,
#51232,#51233,#51234,#51235,#51236,#51237,#51238,#51239,#51240,#51241,#51242,
#51243,#51244,#51245,#51246,#51247,#51248,#51249,#51250,#51251,#51252,#51253,
#51254,#51255,#51256,#51257,#51258,#51259,#51260,#51261,#51262,#51263,#51264,
#51265,#51266,#51267,#51268,#51269,#51270,#51271,#51272,#51273,#51274,#51275,
#51276,#51277,#51278,#51279,#51280,#51281,#51282,#51283,#51284,#51285,#51286,
#51287,#51288,#51289,#51290,#51291,#51292,#51293,#51294,#51295,#51296,#51297,
#51298,#51299,#51300,#51301,#51302,#51303,#51304,#51305,#51306,#51307,#51308,
#51309,#51310,#51311,#51312,#51313,#51314,#51315,#51316,#51317,#51318,#51319,
#51320,#51321,#51322,#51323,#51324,#51325,#51326,#51327,#51328,#51329,#51330,
#51331,#51332),(#51333,#51334,#51335,#51336,#51337,#51338,#51339,#51340,
#51341,#51342,#51343,#51344,#51345,#51346,#51347,#51348,#51349,#51350,#51351,
#51352,#51353,#51354,#51355,#51356,#51357,#51358,#51359,#51360,#51361,#51362,
#51363,#51364,#51365,#51366,#51367,#51368,#51369,#51370,#51371,#51372,#51373,
#51374,#51375,#51376,#51377,#51378,#51379,#51380,#51381,#51382,#51383,#51384,
#51385,#51386,#51387,#51388,#51389,#51390,#51391,#51392,#51393,#51394,#51395,
#51396,#51397,#51398,#51399,#51400,#51401,#51402,#51403,#51404,#51405,#51406,
#51407,#51408,#51409,#51410,#51411,#51412,#51413,#51414,#51415,#51416,#51417,
#51418,#51419,#51420,#51421,#51422,#51423,#51424,#51425,#51426,#51427,#51428,
#51429,#51430,#51431,#51432,#51433,#51434,#51435,#51436,#51437,#51438,#51439,
#51440,#51441,#51442,#51443,#51444,#51445,#51446,#51447,#51448,#51449,#51450,
#51451,#51452,#51453,#51454,#51455,#51456,#51457,#51458,#51459,#51460,#51461,
#51462,#51463,#51464,#51465,#51466,#51467,#51468,#51469,#51470,#51471,#51472,
#51473,#51474,#51475,#51476),(#51477,#51478,#51479,#51480,#51481,#51482,
#51483,#51484,#51485,#51486,#51487,#51488,#51489,#51490,#51491,#51492,#51493,
#51494,#51495,#51496,#51497,#51498,#51499,#51500,#51501,#51502,#51503,#51504,
#51505,#51506,#51507,#51508,#51509,#51510,#51511,#51512,#51513,#51514,#51515,
#51516,#51517,#51518,#51519,#51520,#51521,#51522,#51523,#51524,#51525,#51526,
#51527,#51528,#51529,#51530,#51531,#51532,#51533,#51534,#51535,#51536,#51537,
#51538,#51539,#51540,#51541,#51542,#51543,#51544,#51545,#51546,#51547,#51548,
#51549,#51550,#51551,#51552,#51553,#51554,#51555,#51556,#51557,#51558,#51559,
#51560,#51561,#51562,#51563,#51564,#51565,#51566,#51567,#51568,#51569,#51570,
#51571,#51572,#51573,#51574,#51575,#51576,#51577,#51578,#51579,#51580,#51581,
#51582,#51583,#51584,#51585,#51586,#51587,#51588,#51589,#51590,#51591,#51592,
#51593,#51594,#51595,#51596,#51597,#51598,#51599,#51600,#51601,#51602,#51603,
#51604,#51605,#51606,#51607,#51608,#51609,#51610,#51611,#51612,#51613,#51614,
#51615,#51616,#51617,#51618,#51619,#51620),(#51621,#51622,#51623,#51624,
#51625,#51626,#51627,#51628,#51629,#51630,#51631,#51632,#51633,#51634,#51635,
#51636,#51637,#51638,#51639,#51640,#51641,#51642,#51643,#51644,#51645,#51646,
#51647,#51648,#51649,#51650,#51651,#51652,#51653,#51654,#51655,#51656,#51657,
#51658,#51659,#51660,#51661,#51662,#51663,#51664,#51665,#51666,#51667,#51668,
#51669,#51670,#51671,#51672,#51673,#51674,#51675,#51676,#51677,#51678,#51679,
#51680,#51681,#51682,#51683,#51684,#51685,#51686,#51687,#51688,#51689,#51690,
#51691,#51692,#51693,#51694,#51695,#51696,#51697,#51698,#51699,#51700,#51701,
#51702,#51703,#51704,#51705,#51706,#51707,#51708,#51709,#51710,#51711,#51712,
#51713,#51714,#51715,#51716,#51717,#51718,#51719,#51720,#51721,#51722,#51723,
#51724,#51725,#51726,#51727,#51728,#51729,#51730,#51731,#51732,#51733,#51734,
#51735,#51736,#51737,#51738,#51739,#51740,#51741,#51742,#51743,#51744,#51745,
#51746,#51747,#51748,#51749,#51750,#51751,#51752,#51753,#51754,#51755,#51756,
#51757,#51758,#51759,#51760,#51761,#51762,#51763,#51764),(#51765,#51766,
#51767,#51768,#51769,#51770,#51771,#51772,#51773,#51774,#51775,#51776,#51777,
#51778,#51779,#51780,#51781,#51782,#51783,#51784,#51785,#51786,#51787,#51788,
#51789,#51790,#51791,#51792,#51793,#51794,#51795,#51796,#51797,#51798,#51799,
#51800,#51801,#51802,#51803,#51804,#51805,#51806,#51807,#51808,#51809,#51810,
#51811,#51812,#51813,#51814,#51815,#51816,#51817,#51818,#51819,#51820,#51821,
#51822,#51823,#51824,#51825,#51826,#51827,#51828,#51829,#51830,#51831,#51832,
#51833,#51834,#51835,#51836,#51837,#51838,#51839,#51840,#51841,#51842,#51843,
#51844,#51845,#51846,#51847,#51848,#51849,#51850,#51851,#51852,#51853,#51854,
#51855,#51856,#51857,#51858,#51859,#51860,#51861,#51862,#51863,#51864,#51865,
#51866,#51867,#51868,#51869,#51870,#51871,#51872,#51873,#51874,#51875,#51876,
#51877,#51878,#51879,#51880,#51881,#51882,#51883,#51884,#51885,#51886,#51887,
#51888,#51889,#51890,#51891,#51892,#51893,#51894,#51895,#51896,#51897,#51898,
#51899,#51900,#51901,#51902,#51903,#51904,#51905,#51906,#51907,#51908),
(#51909,#51910,#51911,#51912,#51913,#51914,#51915,#51916,#51917,#51918,
#51919,#51920,#51921,#51922,#51923,#51924,#51925,#51926,#51927,#51928,#51929,
#51930,#51931,#51932,#51933,#51934,#51935,#51936,#51937,#51938,#51939,#51940,
#51941,#51942,#51943,#51944,#51945,#51946,#51947,#51948,#51949,#51950,#51951,
#51952,#51953,#51954,#51955,#51956,#51957,#51958,#51959,#51960,#51961,#51962,
#51963,#51964,#51965,#51966,#51967,#51968,#51969,#51970,#51971,#51972,#51973,
#51974,#51975,#51976,#51977,#51978,#51979,#51980,#51981,#51982,#51983,#51984,
#51985,#51986,#51987,#51988,#51989,#51990,#51991,#51992,#51993,#51994,#51995,
#51996,#51997,#51998,#51999,#52000,#52001,#52002,#52003,#52004,#52005,#52006,
#52007,#52008,#52009,#52010,#52011,#52012,#52013,#52014,#52015,#52016,#52017,
#52018,#52019,#52020,#52021,#52022,#52023,#52024,#52025,#52026,#52027,#52028,
#52029,#52030,#52031,#52032,#52033,#52034,#52035,#52036,#52037,#52038,#52039,
#52040,#52041,#52042,#52043,#52044,#52045,#52046,#52047,#52048,#52049,#52050,
#52051,#52052),(#52053,#52054,#52055,#52056,#52057,#52058,#52059,#52060,
#52061,#52062,#52063,#52064,#52065,#52066,#52067,#52068,#52069,#52070,#52071,
#52072,#52073,#52074,#52075,#52076,#52077,#52078,#52079,#52080,#52081,#52082,
#52083,#52084,#52085,#52086,#52087,#52088,#52089,#52090,#52091,#52092,#52093,
#52094,#52095,#52096,#52097,#52098,#52099,#52100,#52101,#52102,#52103,#52104,
#52105,#52106,#52107,#52108,#52109,#52110,#52111,#52112,#52113,#52114,#52115,
#52116,#52117,#52118,#52119,#52120,#52121,#52122,#52123,#52124,#52125,#52126,
#52127,#52128,#52129,#52130,#52131,#52132,#52133,#52134,#52135,#52136,#52137,
#52138,#52139,#52140,#52141,#52142,#52143,#52144,#52145,#52146,#52147,#52148,
#52149,#52150,#52151,#52152,#52153,#52154,#52155,#52156,#52157,#52158,#52159,
#52160,#52161,#52162,#52163,#52164,#52165,#52166,#52167,#52168,#52169,#52170,
#52171,#52172,#52173,#52174,#52175,#52176,#52177,#52178,#52179,#52180,#52181,
#52182,#52183,#52184,#52185,#52186,#52187,#52188,#52189,#52190,#52191,#52192,
#52193,#52194,#52195,#52196),(#52197,#52198,#52199,#52200,#52201,#52202,
#52203,#52204,#52205,#52206,#52207,#52208,#52209,#52210,#52211,#52212,#52213,
#52214,#52215,#52216,#52217,#52218,#52219,#52220,#52221,#52222,#52223,#52224,
#52225,#52226,#52227,#52228,#52229,#52230,#52231,#52232,#52233,#52234,#52235,
#52236,#52237,#52238,#52239,#52240,#52241,#52242,#52243,#52244,#52245,#52246,
#52247,#52248,#52249,#52250,#52251,#52252,#52253,#52254,#52255,#52256,#52257,
#52258,#52259,#52260,#52261,#52262,#52263,#52264,#52265,#52266,#52267,#52268,
#52269,#52270,#52271,#52272,#52273,#52274,#52275,#52276,#52277,#52278,#52279,
#52280,#52281,#52282,#52283,#52284,#52285,#52286,#52287,#52288,#52289,#52290,
#52291,#52292,#52293,#52294,#52295,#52296,#52297,#52298,#52299,#52300,#52301,
#52302,#52303,#52304,#52305,#52306,#52307,#52308,#52309,#52310,#52311,#52312,
#52313,#52314,#52315,#52316,#52317,#52318,#52319,#52320,#52321,#52322,#52323,
#52324,#52325,#52326,#52327,#52328,#52329,#52330,#52331,#52332,#52333,#52334,
#52335,#52336,#52337,#52338,#52339,#52340)),.UNSPECIFIED.,.F.,.F.,.F.,(4,
1,1,1,1,1,1,1,1,1,1,1,1,1,1,1,1,1,1,1,1,1,1,1,1,1,1,1,1,1,1,1,1,1,1,1,1,
1,1,1,1,1,1,1,1,1,1,1,1,1,1,1,1,1,1,1,1,1,1,1,1,1,1,1,1,1,1,1,1,1,1,1,4),
(4,2,1,1,2,1,1,1,2,1,1,1,1,2,1,1,1,1,2,1,1,1,1,1,1,1,2,1,1,1,1,1,1,1,2,
1,1,1,1,1,1,1,1,2,1,1,1,1,1,1,1,1,1,1,1,1,2,1,1,1,1,1,2,1,1,1,1,1,1,1,2,
1,1,1,1,2,1,1,1,1,1,1,1,1,1,1,2,1,1,1,1,1,2,1,1,1,1,2,1,1,1,1,1,1,1,1,1,
1,1,1,1,2,1,1,1,1,2,1,1,1,1,1,2,4),(0.0268156772007072,0.0437158964674566,
0.0606153077094141,0.0775147189513715,0.094414130193329,0.111313541435286,
0.115538394245776,0.119763247056265,0.128212952677244,0.145112363919201,
0.162011775161159,0.178911186403116,0.195810597645074,0.212710008887031,
0.229609420128989,0.238059125749968,0.246508831370946,0.263408242612904,
0.271857948233882,0.280307653854861,0.284532506665351,0.28875735947584,
0.297207065096819,0.308473339258124,0.319739613419429,0.331005887580734,
0.336639024661386,0.342272161742039,0.353538435903344,0.364804710064649,
0.387337258387259,0.398603532548564,0.409869806709869,0.421136080871174,
0.432402355032479,0.454934903355088,0.466201177516393,0.477467451677698,
0.500000000000308,0.511266274161613,0.522532548322918,0.545065096645528,
0.567597644968138,0.584497056210096,0.601396467452053,0.618295878694011,
0.635195289935968,0.643644995556947,0.652094701177926,0.668994112419883,
0.677443818040862,0.685893523661841,0.702792934903798,0.719692346145756,
0.728142051766734,0.736591757387713,0.75349116862967,0.770390579871628,
0.787289991113585,0.804189402355543,0.8210888135975,0.837988224839458,0.854887636081415,
0.871787047323373,0.880236752944352,0.884461605754841,0.88868645856533,
0.897136164186309,0.905585869807288,0.922485281049245,0.939384692291203,
0.95628410353316,0.973183514775118),(0.0960305811261704,0.0972154775043869,
0.109378606187391,0.121541734870394,0.145867992236401,0.151993923775347,
0.158119855314292,0.170371718392183,0.194875444547964,0.200989580746302,
0.207103716944641,0.219331989341318,0.231560261737996,0.243788534134673,
0.246827927163601,0.24986732019253,0.255946106250386,0.2681036783661,0.292418822597527,
0.293959106599555,0.295499390601583,0.29857995860564,0.304741094613752,
0.310902230621865,0.317063366629978,0.329385638646203,0.341707910662428,
0.344790082003921,0.347872253345414,0.354036596028399,0.36636528139437,
0.37869396676034,0.384858309443326,0.387940480784818,0.391022652126311,
0.392583125212554,0.394143598298796,0.397264544471281,0.403506436816251,
0.415990221506191,0.428474006196132,0.431594952368617,0.434715898541102,
0.440957790886072,0.442498863959882,0.444039937033693,0.447122083181315,
0.448663156255125,0.450204229328936,0.450974765865841,0.451745302402747,
0.452515838939652,0.452901107208105,0.453286375476557,0.465614960067043,
0.477943544657529,0.490272129248014,0.493311253959715,0.496350378671415,
0.502428628094816,0.514585126941617,0.526741625788419,0.53889812463522,
0.540417366609575,0.541936608583929,0.544975092532638,0.551052060430056,
0.563205996224891,0.575359932019726,0.581436899917144,0.587513867814562,
0.590576684581802,0.593639501349043,0.599765134883524,0.612016401952486,
0.636518936090411,0.642599511724338,0.645639799541302,0.648680087358265,
0.654760662992193,0.66084123862612,0.666921814260047,0.669962102077011,
0.673002389893974,0.676042677710938,0.679082965527902,0.685163541161829,
0.688226234079092,0.691288926996354,0.697414312830879,0.70966508449993,
0.72191585616898,0.734166627838031,0.737264704064826,0.740362780291622,
0.746558932745213,0.758951237652395,0.783735847466759,0.785338745832564,
0.78694164419837,0.790147440929981,0.796559034393203,0.809382221319647,
0.815793814782869,0.822205408246091,0.823808306611897,0.825411204977702,
0.828617001709314,0.830219900075119,0.831021349258022,0.831822798440925,
0.835028595172536,0.838457852551916,0.841887109931297,0.848745624690058,
0.86246265420758,0.889896713242625,0.893337440953794,0.896778168664963,
0.9036596240873,0.910541079509638,0.917422534931976,0.944948356621327,0.967478850977141),
 .UNSPECIFIED.);
#18853=B_SPLINE_SURFACE_WITH_KNOTS('',3,3,((#55216,#55217,#55218,#55219,
#55220,#55221,#55222,#55223,#55224,#55225,#55226,#55227,#55228,#55229,#55230,
#55231,#55232,#55233,#55234,#55235,#55236,#55237,#55238,#55239,#55240,#55241,
#55242,#55243,#55244,#55245,#55246,#55247,#55248,#55249,#55250,#55251,#55252,
#55253,#55254,#55255,#55256,#55257,#55258,#55259,#55260,#55261),(#55262,
#55263,#55264,#55265,#55266,#55267,#55268,#55269,#55270,#55271,#55272,#55273,
#55274,#55275,#55276,#55277,#55278,#55279,#55280,#55281,#55282,#55283,#55284,
#55285,#55286,#55287,#55288,#55289,#55290,#55291,#55292,#55293,#55294,#55295,
#55296,#55297,#55298,#55299,#55300,#55301,#55302,#55303,#55304,#55305,#55306,
#55307),(#55308,#55309,#55310,#55311,#55312,#55313,#55314,#55315,#55316,
#55317,#55318,#55319,#55320,#55321,#55322,#55323,#55324,#55325,#55326,#55327,
#55328,#55329,#55330,#55331,#55332,#55333,#55334,#55335,#55336,#55337,#55338,
#55339,#55340,#55341,#55342,#55343,#55344,#55345,#55346,#55347,#55348,#55349,
#55350,#55351,#55352,#55353),(#55354,#55355,#55356,#55357,#55358,#55359,
#55360,#55361,#55362,#55363,#55364,#55365,#55366,#55367,#55368,#55369,#55370,
#55371,#55372,#55373,#55374,#55375,#55376,#55377,#55378,#55379,#55380,#55381,
#55382,#55383,#55384,#55385,#55386,#55387,#55388,#55389,#55390,#55391,#55392,
#55393,#55394,#55395,#55396,#55397,#55398,#55399),(#55400,#55401,#55402,
#55403,#55404,#55405,#55406,#55407,#55408,#55409,#55410,#55411,#55412,#55413,
#55414,#55415,#55416,#55417,#55418,#55419,#55420,#55421,#55422,#55423,#55424,
#55425,#55426,#55427,#55428,#55429,#55430,#55431,#55432,#55433,#55434,#55435,
#55436,#55437,#55438,#55439,#55440,#55441,#55442,#55443,#55444,#55445),
(#55446,#55447,#55448,#55449,#55450,#55451,#55452,#55453,#55454,#55455,
#55456,#55457,#55458,#55459,#55460,#55461,#55462,#55463,#55464,#55465,#55466,
#55467,#55468,#55469,#55470,#55471,#55472,#55473,#55474,#55475,#55476,#55477,
#55478,#55479,#55480,#55481,#55482,#55483,#55484,#55485,#55486,#55487,#55488,
#55489,#55490,#55491)),.UNSPECIFIED.,.F.,.T.,.F.,(4,1,1,4),(4,2,1,2,1,1,
1,1,1,1,2,1,1,1,1,2,1,1,2,1,1,1,1,2,1,2,1,1,1,2,1,2,2,4),(-0.00142384579029664,
0.285714285714286,0.571428571428571,1.),(-9.19419977830157,-8.92020082022876,
-8.53897544224619,-8.15775006426363,-7.94884017932526,-7.73993029438688,
-7.32211052451013,-7.11320063957175,-6.79983581216419,-6.695380869695,-6.48647098475663,
-6.38692241757501,-6.28737385039339,-6.08827671603015,-5.73985673089448,
-5.69008244730366,-5.46391696776057,-5.23775148821748,-5.08697450185542,
-5.0692256166783,-5.01597896114694,-4.94498342043847,-4.80299233902153,
-4.51901017618764,-4.27069680674408,-3.85684119100481,-3.05948850905774,
-2.69705547180907,-1.68224296751281,-1.53726975261334,-1.28960453962952,
-0.876829184656479,-0.308773384377632,0.),.UNSPECIFIED.);
#18854=B_SPLINE_SURFACE_WITH_KNOTS('',3,3,((#55772,#55773,#55774,#55775,
#55776,#55777,#55778,#55779,#55780,#55781,#55782,#55783,#55784,#55785,#55786,
#55787,#55788,#55789,#55790,#55791,#55792,#55793,#55794,#55795,#55796,#55797,
#55798,#55799,#55800,#55801,#55802,#55803,#55804,#55805,#55806,#55807,#55808,
#55809),(#55810,#55811,#55812,#55813,#55814,#55815,#55816,#55817,#55818,
#55819,#55820,#55821,#55822,#55823,#55824,#55825,#55826,#55827,#55828,#55829,
#55830,#55831,#55832,#55833,#55834,#55835,#55836,#55837,#55838,#55839,#55840,
#55841,#55842,#55843,#55844,#55845,#55846,#55847),(#55848,#55849,#55850,
#55851,#55852,#55853,#55854,#55855,#55856,#55857,#55858,#55859,#55860,#55861,
#55862,#55863,#55864,#55865,#55866,#55867,#55868,#55869,#55870,#55871,#55872,
#55873,#55874,#55875,#55876,#55877,#55878,#55879,#55880,#55881,#55882,#55883,
#55884,#55885),(#55886,#55887,#55888,#55889,#55890,#55891,#55892,#55893,
#55894,#55895,#55896,#55897,#55898,#55899,#55900,#55901,#55902,#55903,#55904,
#55905,#55906,#55907,#55908,#55909,#55910,#55911,#55912,#55913,#55914,#55915,
#55916,#55917,#55918,#55919,#55920,#55921,#55922,#55923),(#55924,#55925,
#55926,#55927,#55928,#55929,#55930,#55931,#55932,#55933,#55934,#55935,#55936,
#55937,#55938,#55939,#55940,#55941,#55942,#55943,#55944,#55945,#55946,#55947,
#55948,#55949,#55950,#55951,#55952,#55953,#55954,#55955,#55956,#55957,#55958,
#55959,#55960,#55961)),.UNSPECIFIED.,.F.,.T.,.F.,(4,1,4),(4,2,2,2,1,2,2,
2,1,1,1,2,1,2,1,1,1,1,1,1,1,2,1,1,2,4),(0.,0.571428571428571,1.),(-9.1649736818217,
-8.85500373849296,-8.29205753853133,-7.63533633256183,-6.48172574214371,
-5.32811515172559,-4.66932841177279,-4.10834838496996,-4.03861769654365,
-3.96888700811733,-3.8294256312647,-3.55050287755944,-3.18769596354942,
-2.82488904953941,-2.76816872685197,-2.71144840416452,-2.59800775878964,
-2.37112646803988,-1.91736388654036,-1.46360130504084,-1.23672001429108,
-1.00983872354131,-0.824618171658037,-0.639397619774759,-0.268956516008204,
0.),.UNSPECIFIED.);
#18855=B_SPLINE_SURFACE_WITH_KNOTS('',3,3,((#55967,#55968,#55969,#55970,
#55971,#55972,#55973,#55974,#55975,#55976,#55977,#55978,#55979,#55980,#55981,
#55982,#55983),(#55984,#55985,#55986,#55987,#55988,#55989,#55990,#55991,
#55992,#55993,#55994,#55995,#55996,#55997,#55998,#55999,#56000),(#56001,
#56002,#56003,#56004,#56005,#56006,#56007,#56008,#56009,#56010,#56011,#56012,
#56013,#56014,#56015,#56016,#56017),(#56018,#56019,#56020,#56021,#56022,
#56023,#56024,#56025,#56026,#56027,#56028,#56029,#56030,#56031,#56032,#56033,
#56034),(#56035,#56036,#56037,#56038,#56039,#56040,#56041,#56042,#56043,
#56044,#56045,#56046,#56047,#56048,#56049,#56050,#56051)),.UNSPECIFIED.,
 .F.,.T.,.F.,(4,1,4),(4,1,1,2,1,1,1,1,1,1,1,2,4),(0.,0.571428571428571,
1.00001445338435),(-1.29174070129165,-1.21783674573549,-1.07002883462318,
-0.922220923510859,-0.795342097926536,-0.753049156065094,-0.668463272342212,
-0.583877388619329,-0.414705621173564,-0.330119737450682,-0.245533853727799,
-0.076362086282034,0.),.UNSPECIFIED.);
#18856=B_SPLINE_SURFACE_WITH_KNOTS('',3,3,((#56103,#56104,#56105,#56106,
#56107,#56108,#56109,#56110,#56111,#56112,#56113,#56114,#56115,#56116,#56117),
(#56118,#56119,#56120,#56121,#56122,#56123,#56124,#56125,#56126,#56127,
#56128,#56129,#56130,#56131,#56132),(#56133,#56134,#56135,#56136,#56137,
#56138,#56139,#56140,#56141,#56142,#56143,#56144,#56145,#56146,#56147),
(#56148,#56149,#56150,#56151,#56152,#56153,#56154,#56155,#56156,#56157,
#56158,#56159,#56160,#56161,#56162),(#56163,#56164,#56165,#56166,#56167,
#56168,#56169,#56170,#56171,#56172,#56173,#56174,#56175,#56176,#56177)),
 .UNSPECIFIED.,.F.,.T.,.F.,(4,1,4),(4,2,1,1,1,1,1,2,1,1,4),(0.,0.571428571428571,
1.),(-1.2915881661436,-1.18065640410841,-1.01148719643655,-0.842317988764689,
-0.757733384928759,-0.673148781092829,-0.50397957342097,-0.334810365749111,
-0.234367256024377,-0.133924146299644,0.),.UNSPECIFIED.);
#18857=B_SPLINE_SURFACE_WITH_KNOTS('',3,3,((#56183,#56184,#56185,#56186,
#56187,#56188,#56189,#56190,#56191,#56192,#56193,#56194,#56195,#56196,#56197,
#56198,#56199,#56200,#56201,#56202,#56203,#56204,#56205),(#56206,#56207,
#56208,#56209,#56210,#56211,#56212,#56213,#56214,#56215,#56216,#56217,#56218,
#56219,#56220,#56221,#56222,#56223,#56224,#56225,#56226,#56227,#56228),
(#56229,#56230,#56231,#56232,#56233,#56234,#56235,#56236,#56237,#56238,
#56239,#56240,#56241,#56242,#56243,#56244,#56245,#56246,#56247,#56248,#56249,
#56250,#56251),(#56252,#56253,#56254,#56255,#56256,#56257,#56258,#56259,
#56260,#56261,#56262,#56263,#56264,#56265,#56266,#56267,#56268,#56269,#56270,
#56271,#56272,#56273,#56274),(#56275,#56276,#56277,#56278,#56279,#56280,
#56281,#56282,#56283,#56284,#56285,#56286,#56287,#56288,#56289,#56290,#56291,
#56292,#56293,#56294,#56295,#56296,#56297)),.UNSPECIFIED.,.F.,.T.,.F.,(4,
1,4),(4,1,1,1,1,2,1,1,1,1,1,1,1,1,1,2,1,1,4),(0.,0.571428571428571,1.00007865727904),
(-1.29193145083568,-1.18863906797729,-1.0853466851189,-0.982054302260506,
-0.878761919402114,-0.775469536543723,-0.720593698815789,-0.665717861087855,
-0.555966185631988,-0.44621451017612,-0.336462834720253,-0.309024915856286,
-0.281586996992319,-0.254149078128352,-0.240430118696369,-0.226711159264386,
-0.181368927411508,-0.136026695558631,0.),.UNSPECIFIED.);
#18858=B_SPLINE_SURFACE_WITH_KNOTS('',3,3,((#56420,#56421,#56422,#56423,
#56424,#56425,#56426,#56427,#56428,#56429,#56430,#56431,#56432,#56433,#56434,
#56435,#56436,#56437,#56438),(#56439,#56440,#56441,#56442,#56443,#56444,
#56445,#56446,#56447,#56448,#56449,#56450,#56451,#56452,#56453,#56454,#56455,
#56456,#56457),(#56458,#56459,#56460,#56461,#56462,#56463,#56464,#56465,
#56466,#56467,#56468,#56469,#56470,#56471,#56472,#56473,#56474,#56475,#56476),
(#56477,#56478,#56479,#56480,#56481,#56482,#56483,#56484,#56485,#56486,
#56487,#56488,#56489,#56490,#56491,#56492,#56493,#56494,#56495),(#56496,
#56497,#56498,#56499,#56500,#56501,#56502,#56503,#56504,#56505,#56506,#56507,
#56508,#56509,#56510,#56511,#56512,#56513,#56514)),.UNSPECIFIED.,.F.,.T.,
 .F.,(4,1,4),(4,1,2,1,1,1,1,1,2,1,1,1,1,1,4),(0.,0.571428571428571,1.),
(-1.29158374785677,-1.19032888736264,-1.03844659662145,-0.983576456101594,
-0.928706315581737,-0.818966034542023,-0.709225753502309,-0.599485472462595,
-0.489745191422881,-0.440770672280593,-0.391796153138305,-0.293847114853729,
-0.195898076569152,-0.0979490382845762,0.),.UNSPECIFIED.);
#18859=B_SPLINE_SURFACE_WITH_KNOTS('',3,3,((#56520,#56521,#56522,#56523,
#56524,#56525,#56526,#56527),(#56528,#56529,#56530,#56531,#56532,#56533,
#56534,#56535),(#56536,#56537,#56538,#56539,#56540,#56541,#56542,#56543),
(#56544,#56545,#56546,#56547,#56548,#56549,#56550,#56551)),
 .UNSPECIFIED.,.F.,.F.,.F.,(4,4),(4,2,2,4),(0.,1.),(-0.32931292451793,-0.275040863381023,
0.328202711224253,0.329193263838381),.UNSPECIFIED.);
#18860=B_SPLINE_SURFACE_WITH_KNOTS('',3,3,((#56577,#56578,#56579,#56580,
#56581),(#56582,#56583,#56584,#56585,#56586),(#56587,#56588,#56589,#56590,
#56591),(#56592,#56593,#56594,#56595,#56596)),.UNSPECIFIED.,.F.,.F.,.F.,
(4,4),(4,1,4),(0.,1.),(-0.299498223131783,-0.0164065923085981,0.361048915455649),
 .UNSPECIFIED.);
#18861=B_SPLINE_SURFACE_WITH_KNOTS('',3,3,((#56607,#56608,#56609,#56610,
#56611,#56612,#56613,#56614,#56615,#56616,#56617,#56618,#56619,#56620,#56621,
#56622,#56623),(#56624,#56625,#56626,#56627,#56628,#56629,#56630,#56631,
#56632,#56633,#56634,#56635,#56636,#56637,#56638,#56639,#56640),(#56641,
#56642,#56643,#56644,#56645,#56646,#56647,#56648,#56649,#56650,#56651,#56652,
#56653,#56654,#56655,#56656,#56657),(#56658,#56659,#56660,#56661,#56662,
#56663,#56664,#56665,#56666,#56667,#56668,#56669,#56670,#56671,#56672,#56673,
#56674)),.UNSPECIFIED.,.F.,.F.,.F.,(4,4),(4,2,1,1,1,1,1,1,1,1,1,2,4),(0.,
1.),(-0.297794025374421,-0.296794638674619,-0.236399107412475,-0.17600357615033,
-0.115608044888186,-0.0552125136260416,0.00518301763610282,0.0655785488982472,
0.125974080160392,0.186369611422536,0.24676514268468,0.307160673946825,
0.361386326815235),.UNSPECIFIED.);
#18862=B_SPLINE_SURFACE_WITH_KNOTS('',3,3,((#56689,#56690,#56691,#56692,
#56693,#56694,#56695,#56696,#56697),(#56698,#56699,#56700,#56701,#56702,
#56703,#56704,#56705,#56706),(#56707,#56708,#56709,#56710,#56711,#56712,
#56713,#56714,#56715),(#56716,#56717,#56718,#56719,#56720,#56721,#56722,
#56723,#56724)),.UNSPECIFIED.,.F.,.F.,.F.,(4,4),(4,2,1,2,4),(-4.7316025546104E-6,
1.00000473160542),(-0.330176451776112,-0.314286281116363,-0.0628601143819659,
0.314279135719629,0.330169461918646),.UNSPECIFIED.);
#18863=B_SPLINE_SURFACE_WITH_KNOTS('',3,3,((#56727,#56728,#56729,#56730),
(#56731,#56732,#56733,#56734),(#56735,#56736,#56737,#56738),(#56739,#56740,
#56741,#56742),(#56743,#56744,#56745,#56746),(#56747,#56748,#56749,#56750)),
 .UNSPECIFIED.,.F.,.F.,.F.,(4,1,1,4),(4,4),(-0.799336073509661,-0.594771590871585,
-0.39020710823351,-0.0833603842763964),(-0.204000152442369,0.204),
 .UNSPECIFIED.);
#18864=B_SPLINE_SURFACE_WITH_KNOTS('',3,3,((#56753,#56754,#56755,#56756),
(#56757,#56758,#56759,#56760),(#56761,#56762,#56763,#56764),(#56765,#56766,
#56767,#56768),(#56769,#56770,#56771,#56772),(#56773,#56774,#56775,#56776)),
 .UNSPECIFIED.,.F.,.F.,.F.,(4,1,1,4),(4,4),(-1.96312962658784,-1.63061718285122,
-1.46436096098291,-0.799336073509661),(-0.204,0.204048008019707),
 .UNSPECIFIED.);
#18865=B_SPLINE_SURFACE_WITH_KNOTS('',3,3,((#56778,#56779,#56780,#56781),
(#56782,#56783,#56784,#56785),(#56786,#56787,#56788,#56789),(#56790,#56791,
#56792,#56793),(#56794,#56795,#56796,#56797),(#56798,#56799,#56800,#56801)),
 .UNSPECIFIED.,.F.,.F.,.F.,(4,1,1,4),(4,4),(-3.17329134625142,-3.0004111005852,
-2.65465060925274,-1.96312962658784),(-0.204,0.204),.UNSPECIFIED.);
#18866=B_SPLINE_SURFACE_WITH_KNOTS('',3,3,((#56805,#56806,#56807,#56808),
(#56809,#56810,#56811,#56812),(#56813,#56814,#56815,#56816),(#56817,#56818,
#56819,#56820),(#56821,#56822,#56823,#56824),(#56825,#56826,#56827,#56828)),
 .UNSPECIFIED.,.F.,.F.,.F.,(4,1,1,4),(4,4),(-4.08237667107798,-3.69276867472374,
-3.43303001048758,-3.17329134625142),(-0.204,0.204),.UNSPECIFIED.);
#18867=B_SPLINE_SURFACE_WITH_KNOTS('',3,3,((#56832,#56833,#56834,#56835),
(#56836,#56837,#56838,#56839),(#56840,#56841,#56842,#56843),(#56844,#56845,
#56846,#56847),(#56848,#56849,#56850,#56851),(#56852,#56853,#56854,#56855)),
 .UNSPECIFIED.,.F.,.F.,.F.,(4,1,1,4),(4,4),(-5.24964463690696,-5.08288401419063,
-4.74938156648641,-4.08236727834706),(-0.204,0.204009400954156),
 .UNSPECIFIED.);
#18868=B_SPLINE_SURFACE_WITH_KNOTS('',3,3,((#56857,#56858,#56859,#56860),
(#56861,#56862,#56863,#56864),(#56865,#56866,#56867,#56868),(#56869,#56870,
#56871,#56872),(#56873,#56874,#56875,#56876),(#56877,#56878,#56879,#56880),
(#56881,#56882,#56883,#56884)),.UNSPECIFIED.,.F.,.F.,.F.,(4,1,1,1,4),(4,
4),(-6.31492341312625,-6.01055536310239,-5.85837133809046,-5.5540032880666,
-5.24963523804274),(-0.204,0.204),.UNSPECIFIED.);
#18869=B_SPLINE_SURFACE_WITH_KNOTS('',3,3,((#56886,#56887,#56888,#56889),
(#56890,#56891,#56892,#56893),(#56894,#56895,#56896,#56897),(#56898,#56899,
#56900,#56901),(#56902,#56903,#56904,#56905),(#56906,#56907,#56908,#56909),
(#56910,#56911,#56912,#56913),(#56914,#56915,#56916,#56917),(#56918,#56919,
#56920,#56921),(#56922,#56923,#56924,#56925)),.UNSPECIFIED.,.F.,.F.,.F.,
(4,1,1,1,1,1,1,4),(4,4),(-7.69657954651299,-7.30181972429585,-7.10444046206193,
-6.90706119982801,-6.80837156871105,-6.70968193759409,-6.51230267536017,
-6.31492211537695),(-0.204,0.204001297749304),.UNSPECIFIED.);
#18870=B_SPLINE_SURFACE_WITH_KNOTS('',3,3,((#56927,#56928,#56929,#56930),
(#56931,#56932,#56933,#56934),(#56935,#56936,#56937,#56938),(#56939,#56940,
#56941,#56942),(#56943,#56944,#56945,#56946),(#56947,#56948,#56949,#56950),
(#56951,#56952,#56953,#56954),(#56955,#56956,#56957,#56958),(#56959,#56960,
#56961,#56962)),.UNSPECIFIED.,.F.,.F.,.F.,(4,1,1,1,1,1,4),(4,4),(-10.2944961530174,
-9.9233650238383,-9.5522338946592,-9.18110276548009,-8.43884050712189,-8.06770937794279,
-7.69657824876369),(-0.204,0.204),.UNSPECIFIED.);
#18871=B_SPLINE_SURFACE_WITH_KNOTS('',3,3,((#56964,#56965,#56966,#56967),
(#56968,#56969,#56970,#56971),(#56972,#56973,#56974,#56975),(#56976,#56977,
#56978,#56979),(#56980,#56981,#56982,#56983),(#56984,#56985,#56986,#56987),
(#56988,#56989,#56990,#56991),(#56992,#56993,#56994,#56995)),
 .UNSPECIFIED.,.F.,.F.,.F.,(4,1,1,1,1,4),(4,4),(-11.9813316832122,-11.8608434310554,
-11.7403551788986,-11.2584021702716,-10.7764491616445,-10.2944961530174),
(-0.204,0.204),.UNSPECIFIED.);
#18872=B_SPLINE_SURFACE_WITH_KNOTS('',3,3,((#56999,#57000,#57001,#57002),
(#57003,#57004,#57005,#57006),(#57007,#57008,#57009,#57010),(#57011,#57012,
#57013,#57014),(#57015,#57016,#57017,#57018),(#57019,#57020,#57021,#57022),
(#57023,#57024,#57025,#57026),(#57027,#57028,#57029,#57030),(#57031,#57032,
#57033,#57034),(#57035,#57036,#57037,#57038)),.UNSPECIFIED.,.F.,.F.,.F.,
(4,1,1,1,1,1,1,4),(4,4),(-16.6980910490008,-16.0242682824596,-14.6766227493771,
-14.0027999828359,-13.3289772162947,-12.6551544497534,-12.3182430664828,
-11.9813316832122),(-0.204,0.204),.UNSPECIFIED.);
#18873=B_SPLINE_SURFACE_WITH_KNOTS('',3,3,((#57042,#57043,#57044,#57045),
(#57046,#57047,#57048,#57049),(#57050,#57051,#57052,#57053),(#57054,#57055,
#57056,#57057),(#57058,#57059,#57060,#57061),(#57062,#57063,#57064,#57065),
(#57066,#57067,#57068,#57069),(#57070,#57071,#57072,#57073),(#57074,#57075,
#57076,#57077)),.UNSPECIFIED.,.F.,.F.,.F.,(4,1,1,1,1,1,4),(4,4),(-21.7463678506673,
-21.0251854504292,-19.5828206499531,-18.861638249715,-18.140455849477,-17.4192734492389,
-16.6980910490008),(-0.204,0.204),.UNSPECIFIED.);
#18874=B_SPLINE_SURFACE_WITH_KNOTS('',3,3,((#57081,#57082,#57083,#57084),
(#57085,#57086,#57087,#57088),(#57089,#57090,#57091,#57092),(#57093,#57094,
#57095,#57096),(#57097,#57098,#57099,#57100),(#57101,#57102,#57103,#57104),
(#57105,#57106,#57107,#57108)),.UNSPECIFIED.,.F.,.F.,.F.,(4,1,1,1,4),(4,
4),(-25.4580188592258,-24.3975168143727,-23.8672870216316,-22.8068274361495,
-21.7463253912963),(-0.204042459371017,0.204),.UNSPECIFIED.);
#18875=B_SPLINE_SURFACE_WITH_KNOTS('',3,3,((#57110,#57111,#57112,#57113),
(#57114,#57115,#57116,#57117),(#57118,#57119,#57120,#57121),(#57122,#57123,
#57124,#57125),(#57126,#57127,#57128,#57129)),.UNSPECIFIED.,.F.,.F.,.F.,
(4,1,4),(4,4),(-27.614177239717,-26.6900911654903,-25.4579763998548),(-0.204,
0.204044923106431),.UNSPECIFIED.);
#18876=B_SPLINE_SURFACE_WITH_KNOTS('',3,3,((#57131,#57132,#57133,#57134),
(#57135,#57136,#57137,#57138),(#57139,#57140,#57141,#57142),(#57143,#57144,
#57145,#57146),(#57147,#57148,#57149,#57150),(#57151,#57152,#57153,#57154),
(#57155,#57156,#57157,#57158),(#57159,#57160,#57161,#57162),(#57163,#57164,
#57165,#57166)),.UNSPECIFIED.,.F.,.F.,.F.,(4,1,1,1,1,1,4),(4,4),(4.87949017123957,
5.11201692992118,5.57705083698662,5.80956779051934,6.04208474405206,6.27460169758478,
6.507128569875),(-0.204009919306124,0.204),.UNSPECIFIED.);
#18877=B_SPLINE_SURFACE_WITH_KNOTS('',3,3,((#57171,#57172,#57173,#57174),
(#57175,#57176,#57177,#57178),(#57179,#57180,#57181,#57182),(#57183,#57184,
#57185,#57186),(#57187,#57188,#57189,#57190),(#57191,#57192,#57193,#57194),
(#57195,#57196,#57197,#57198)),.UNSPECIFIED.,.F.,.F.,.F.,(4,1,1,1,4),(4,
4),(2.69094642325915,3.62889794602885,4.25419896120866,4.56684946879856,
4.87949997638846),(-0.204,0.204),.UNSPECIFIED.);
#18878=B_SPLINE_SURFACE_WITH_KNOTS('',3,3,((#57200,#57201,#57202,#57203),
(#57204,#57205,#57206,#57207),(#57208,#57209,#57210,#57211),(#57212,#57213,
#57214,#57215),(#57216,#57217,#57218,#57219),(#57220,#57221,#57222,#57223),
(#57224,#57225,#57226,#57227),(#57228,#57229,#57230,#57231),(#57232,#57233,
#57234,#57235),(#57236,#57237,#57238,#57239)),.UNSPECIFIED.,.F.,.F.,.F.,
(4,1,1,1,1,1,1,4),(4,4),(1.28453619636216,1.68637707337851,1.88729094335464,
1.93751941084867,1.9877478783427,2.08820481333076,2.28911868330689,2.69095954767691),
(-0.204,0.204013137504486),.UNSPECIFIED.);
#18879=B_SPLINE_SURFACE_WITH_KNOTS('',3,3,((#57241,#57242,#57243,#57244),
(#57245,#57246,#57247,#57248),(#57249,#57250,#57251,#57252),(#57253,#57254,
#57255,#57256),(#57257,#57258,#57259,#57260),(#57261,#57262,#57263,#57264),
(#57265,#57266,#57267,#57268)),.UNSPECIFIED.,.F.,.F.,.F.,(4,1,1,1,4),(4,
4),(0.675577463735769,0.762573445120124,0.936565407888833,1.11055737065754,
1.28454933342625),(-0.204,0.204),.UNSPECIFIED.);
#18880=B_SPLINE_SURFACE_WITH_KNOTS('',3,3,((#57270,#57271,#57272,#57273),
(#57274,#57275,#57276,#57277),(#57278,#57279,#57280,#57281),(#57282,#57283,
#57284,#57285),(#57286,#57287,#57288,#57289),(#57290,#57291,#57292,#57293)),
 .UNSPECIFIED.,.F.,.F.,.F.,(4,1,1,4),(4,4),(0.0412699530886637,0.222500670416408,
0.403731387744152,0.675577463735769),(-0.204,0.204),.UNSPECIFIED.);
#18881=B_SPLINE_SURFACE_WITH_KNOTS('',3,3,((#57295,#57296,#57297,#57298),
(#57299,#57300,#57301,#57302),(#57303,#57304,#57305,#57306),(#57307,#57308,
#57309,#57310)),.UNSPECIFIED.,.F.,.F.,.F.,(4,4),(4,4),(0.,0.0412699530886637),
(-0.204,0.204),.UNSPECIFIED.);
#18882=B_SPLINE_SURFACE_WITH_KNOTS('',3,3,((#57312,#57313,#57314,#57315),
(#57316,#57317,#57318,#57319),(#57320,#57321,#57322,#57323),(#57324,#57325,
#57326,#57327),(#57328,#57329,#57330,#57331),(#57332,#57333,#57334,#57335)),
 .UNSPECIFIED.,.F.,.F.,.F.,(4,1,1,4),(4,4),(8.77692550510397,9.17723620667681,
9.97785760982251,11.5791004161139),(-0.204,0.204000856547217),
 .UNSPECIFIED.);
#18883=B_SPLINE_SURFACE_WITH_KNOTS('',3,3,((#57338,#57339,#57340,#57341),
(#57342,#57343,#57344,#57345),(#57346,#57347,#57348,#57349),(#57350,#57351,
#57352,#57353),(#57354,#57355,#57356,#57357)),.UNSPECIFIED.,.F.,.F.,.F.,
(4,1,4),(4,4),(6.63337020876143,7.5520367643368,8.77692550510397),(-0.204,
0.204),.UNSPECIFIED.);
#18884=B_SPLINE_SURFACE_WITH_KNOTS('',3,3,((#57359,#57360,#57361,#57362),
(#57363,#57364,#57365,#57366),(#57367,#57368,#57369,#57370),(#57371,#57372,
#57373,#57374),(#57375,#57376,#57377,#57378)),.UNSPECIFIED.,.F.,.F.,.F.,
(4,1,4),(4,4),(4.69944989998284,5.80455488046634,6.63338808485148),(-0.204017876090052,
0.204),.UNSPECIFIED.);
#18885=B_SPLINE_SURFACE_WITH_KNOTS('',3,3,((#57380,#57381,#57382,#57383),
(#57384,#57385,#57386,#57387),(#57388,#57389,#57390,#57391),(#57392,#57393,
#57394,#57395),(#57396,#57397,#57398,#57399),(#57400,#57401,#57402,#57403),
(#57404,#57405,#57406,#57407)),.UNSPECIFIED.,.F.,.F.,.F.,(4,1,1,1,4),(4,
4),(3.61161161838824,4.07783568596737,4.23324370849375,4.54405975354651,
4.69946777607289),(-0.204,0.204015895391734),.UNSPECIFIED.);
#18886=B_SPLINE_SURFACE_WITH_KNOTS('',3,3,((#57409,#57410,#57411,#57412),
(#57413,#57414,#57415,#57416),(#57417,#57418,#57419,#57420),(#57421,#57422,
#57423,#57424),(#57425,#57426,#57427,#57428),(#57429,#57430,#57431,#57432),
(#57433,#57434,#57435,#57436),(#57437,#57438,#57439,#57440),(#57441,#57442,
#57443,#57444),(#57445,#57446,#57447,#57448)),.UNSPECIFIED.,.F.,.F.,.F.,
(4,1,1,1,1,1,1,4),(4,4),(1.96419346040493,2.1995405412518,2.43488572077454,
2.67023090029728,2.90557607982002,3.14092125934276,3.3762664388655,3.61161352768816),
(-0.204001604230681,0.204001909299916),.UNSPECIFIED.);
#18887=B_SPLINE_SURFACE_WITH_KNOTS('',3,3,((#57452,#57453,#57454,#57455),
(#57456,#57457,#57458,#57459),(#57460,#57461,#57462,#57463),(#57464,#57465,
#57466,#57467),(#57468,#57469,#57470,#57471),(#57472,#57473,#57474,#57475),
(#57476,#57477,#57478,#57479),(#57480,#57481,#57482,#57483),(#57484,#57485,
#57486,#57487),(#57488,#57489,#57490,#57491),(#57492,#57493,#57494,#57495)),
 .UNSPECIFIED.,.F.,.F.,.F.,(4,1,1,1,1,1,1,1,4),(4,4),(-3.27331145294747E-6,
0.561198674779733,0.701498343474666,0.841798012169599,0.982097680864532,
1.12239734955947,1.40299668694933,1.6835960243392,1.96419863537987),(-0.204,
0.204003273650805),.UNSPECIFIED.);
#18888=B_SPLINE_SURFACE_WITH_KNOTS('',3,3,((#57497,#57498,#57499,#57500),
(#57501,#57502,#57503,#57504),(#57505,#57506,#57507,#57508),(#57509,#57510,
#57511,#57512),(#57513,#57514,#57515,#57516),(#57517,#57518,#57519,#57520),
(#57521,#57522,#57523,#57524),(#57525,#57526,#57527,#57528),(#57529,#57530,
#57531,#57532)),.UNSPECIFIED.,.F.,.F.,.F.,(4,1,1,1,1,1,4),(4,4),(-1.10870576037865,
-1.01091721837057,-0.913128676362484,-0.815340134354398,-0.766445863350356,
-0.619763050338228,-0.424185966322057),(-0.204,0.204),.UNSPECIFIED.);
#18889=B_SPLINE_SURFACE_WITH_KNOTS('',3,3,((#57537,#57538,#57539,#57540),
(#57541,#57542,#57543,#57544),(#57545,#57546,#57547,#57548),(#57549,#57550,
#57551,#57552),(#57553,#57554,#57555,#57556),(#57557,#57558,#57559,#57560),
(#57561,#57562,#57563,#57564),(#57565,#57566,#57567,#57568),(#57569,#57570,
#57571,#57572),(#57573,#57574,#57575,#57576)),.UNSPECIFIED.,.F.,.F.,.F.,
(4,1,1,1,1,1,1,4),(4,4),(-2.04907351897734,-1.91473526774895,-1.64605876529219,
-1.5117205140638,-1.37738226283542,-1.24304401160704,-1.17587488599285,
-1.10870576037865),(-0.204,0.204),.UNSPECIFIED.);
#18890=B_SPLINE_SURFACE_WITH_KNOTS('',3,3,((#57580,#57581,#57582,#57583),
(#57584,#57585,#57586,#57587),(#57588,#57589,#57590,#57591),(#57592,#57593,
#57594,#57595),(#57596,#57597,#57598,#57599),(#57600,#57601,#57602,#57603),
(#57604,#57605,#57606,#57607),(#57608,#57609,#57610,#57611),(#57612,#57613,
#57614,#57615),(#57616,#57617,#57618,#57619),(#57620,#57621,#57622,#57623)),
 .UNSPECIFIED.,.F.,.F.,.F.,(4,1,1,1,1,1,1,1,4),(4,4),(-3.79500150868533,
-3.54558322444133,-3.04674665595333,-2.92203751383133,-2.79732837170933,
-2.67261922958733,-2.54791008746534,-2.29849180322134,-2.04907351897734),
(-0.204,0.204),.UNSPECIFIED.);
#18891=B_SPLINE_SURFACE_WITH_KNOTS('',3,3,((#57627,#57628,#57629,#57630),
(#57631,#57632,#57633,#57634),(#57635,#57636,#57637,#57638),(#57639,#57640,
#57641,#57642),(#57643,#57644,#57645,#57646),(#57647,#57648,#57649,#57650),
(#57651,#57652,#57653,#57654),(#57655,#57656,#57657,#57658),(#57659,#57660,
#57661,#57662),(#57663,#57664,#57665,#57666),(#57667,#57668,#57669,#57670)),
 .UNSPECIFIED.,.F.,.F.,.F.,(4,1,1,1,1,1,1,1,4),(4,4),(-7.37894121078442,
-6.86694230253758,-5.84296203792017,-4.81898177330275,-4.56298670714839,
-4.46698855734051,-4.30699164099404,-4.05099657483969,-3.7949926101359),
(-0.204,0.204008898549431),.UNSPECIFIED.);
#18892=B_SPLINE_SURFACE_WITH_KNOTS('',3,3,((#57672,#57673,#57674,#57675),
(#57676,#57677,#57678,#57679),(#57680,#57681,#57682,#57683),(#57684,#57685,
#57686,#57687),(#57688,#57689,#57690,#57691),(#57692,#57693,#57694,#57695),
(#57696,#57697,#57698,#57699),(#57700,#57701,#57702,#57703)),
 .UNSPECIFIED.,.F.,.F.,.F.,(4,1,1,1,1,4),(4,4),(-13.6209874915031,-10.9458199140635,
-10.0540980442592,-9.16237617445491,-8.2706543046506,-7.3789298003802),
(-0.204,0.20400263446609),.UNSPECIFIED.);
#18893=B_SPLINE_SURFACE_WITH_KNOTS('',3,3,((#57705,#57706,#57707,#57708),
(#57709,#57710,#57711,#57712),(#57713,#57714,#57715,#57716),(#57717,#57718,
#57719,#57720),(#57721,#57722,#57723,#57724),(#57725,#57726,#57727,#57728),
(#57729,#57730,#57731,#57732),(#57733,#57734,#57735,#57736)),
 .UNSPECIFIED.,.F.,.F.,.F.,(4,1,1,1,1,4),(4,4),(-20.9230961620266,-17.7936201740765,
-15.7073028487765,-14.6641441861265,-14.1425648548015,-13.6209855234765),
(-0.204,0.204),.UNSPECIFIED.);
#18894=B_SPLINE_SURFACE_WITH_KNOTS('',3,3,((#57738,#57739,#57740,#57741),
(#57742,#57743,#57744,#57745),(#57746,#57747,#57748,#57749),(#57750,#57751,
#57752,#57753),(#57754,#57755,#57756,#57757),(#57758,#57759,#57760,#57761),
(#57762,#57763,#57764,#57765),(#57766,#57767,#57768,#57769)),
 .UNSPECIFIED.,.F.,.F.,.F.,(4,1,1,1,1,4),(4,4),(-29.2787346184417,-28.085071981811,
-25.6977467085495,-24.5040840719188,-23.310421435288,-20.9230961620266),
(-0.204,0.204),.UNSPECIFIED.);
#18895=B_SPLINE_SURFACE_WITH_KNOTS('',3,3,((#57771,#57772,#57773,#57774),
(#57775,#57776,#57777,#57778),(#57779,#57780,#57781,#57782),(#57783,#57784,
#57785,#57786),(#57787,#57788,#57789,#57790),(#57791,#57792,#57793,#57794),
(#57795,#57796,#57797,#57798)),.UNSPECIFIED.,.F.,.F.,.F.,(4,1,1,1,4),(4,
4),(-35.1303495878619,-33.4584584867811,-31.7865689394453,-30.9506241657775,
-29.2787331702972),(-0.204001840580079,0.204),.UNSPECIFIED.);
#18896=B_SPLINE_SURFACE_WITH_KNOTS('',3,3,((#57802,#57803,#57804,#57805),
(#57806,#57807,#57808,#57809),(#57810,#57811,#57812,#57813),(#57814,#57815,
#57816,#57817),(#57818,#57819,#57820,#57821),(#57822,#57823,#57824,#57825),
(#57826,#57827,#57828,#57829),(#57830,#57831,#57832,#57833),(#57834,#57835,
#57836,#57837)),.UNSPECIFIED.,.F.,.F.,.F.,(4,1,1,1,1,1,4),(4,4),(-40.4542048267256,
-38.9331028859802,-38.1725519156075,-37.4120009452349,-36.6514499748622,
-35.8908990044895,-35.1303480341168),(-0.204,0.204),.UNSPECIFIED.);
#18897=B_SPLINE_SURFACE_WITH_KNOTS('',3,3,((#57841,#57842,#57843,#57844),
(#57845,#57846,#57847,#57848),(#57849,#57850,#57851,#57852),(#57853,#57854,
#57855,#57856),(#57857,#57858,#57859,#57860),(#57861,#57862,#57863,#57864),
(#57865,#57866,#57867,#57868),(#57869,#57870,#57871,#57872)),
 .UNSPECIFIED.,.F.,.F.,.F.,(4,1,1,1,1,4),(4,4),(-52.0762703289969,-47.0953817384218,
-43.7747932825737,-42.1144990546496,-41.2843519406876,-40.4541989180265),
(-0.204,0.204005908699072),.UNSPECIFIED.);
#18898=B_SPLINE_SURFACE_WITH_KNOTS('',3,3,((#57874,#57875,#57876,#57877),
(#57878,#57879,#57880,#57881),(#57882,#57883,#57884,#57885),(#57886,#57887,
#57888,#57889),(#57890,#57891,#57892,#57893)),.UNSPECIFIED.,.F.,.F.,.F.,
(4,1,4),(4,4),(-66.1031756239825,-60.0916422517874,-52.076264422194),(-0.204,
0.204),.UNSPECIFIED.);
#18899=B_SPLINE_SURFACE_WITH_KNOTS('',3,3,((#57895,#57896,#57897,#57898),
(#57899,#57900,#57901,#57902),(#57903,#57904,#57905,#57906),(#57907,#57908,
#57909,#57910)),.UNSPECIFIED.,.F.,.F.,.F.,(4,4),(4,4),(-75.2949305236969,
-66.1031756239825),(-0.204,0.204),.UNSPECIFIED.);
#18900=B_SPLINE_SURFACE_WITH_KNOTS('',3,3,((#57912,#57913,#57914,#57915),
(#57916,#57917,#57918,#57919),(#57920,#57921,#57922,#57923),(#57924,#57925,
#57926,#57927)),.UNSPECIFIED.,.F.,.F.,.F.,(4,4),(4,4),(-76.3862538744791,
-75.2949305236969),(-0.204,0.204000226653285),.UNSPECIFIED.);
#18901=B_SPLINE_SURFACE_WITH_KNOTS('',3,3,((#57929,#57930,#57931,#57932),
(#57933,#57934,#57935,#57936),(#57937,#57938,#57939,#57940),(#57941,#57942,
#57943,#57944),(#57945,#57946,#57947,#57948),(#57949,#57950,#57951,#57952),
(#57953,#57954,#57955,#57956),(#57957,#57958,#57959,#57960)),
 .UNSPECIFIED.,.F.,.F.,.F.,(4,1,1,1,1,4),(4,4),(2.10086200096182,2.11383027239681,
2.12678492441379,2.13973957643076,2.15269422844774,2.19157180391669),(-0.204,
0.204013619418013),.UNSPECIFIED.);
#18902=B_SPLINE_SURFACE_WITH_KNOTS('',3,3,((#57965,#57966,#57967,#57968),
(#57969,#57970,#57971,#57972),(#57973,#57974,#57975,#57976),(#57977,#57978,
#57979,#57980),(#57981,#57982,#57983,#57984),(#57985,#57986,#57987,#57988),
(#57989,#57990,#57991,#57992),(#57993,#57994,#57995,#57996),(#57997,#57998,
#57999,#58000)),.UNSPECIFIED.,.F.,.F.,.F.,(4,1,1,1,1,1,4),(4,4),(2.03661045158091,
2.0549719283806,2.06415266678044,2.07333340518029,2.08251414358014,2.09169488197998,
2.10087562037983),(-0.204,0.204),.UNSPECIFIED.);
#18903=B_SPLINE_SURFACE_WITH_KNOTS('',3,3,((#58002,#58003,#58004,#58005),
(#58006,#58007,#58008,#58009),(#58010,#58011,#58012,#58013),(#58014,#58015,
#58016,#58017),(#58018,#58019,#58020,#58021),(#58022,#58023,#58024,#58025),
(#58026,#58027,#58028,#58029),(#58030,#58031,#58032,#58033)),
 .UNSPECIFIED.,.F.,.F.,.F.,(4,1,1,1,1,4),(4,4),(1.96650114296421,1.97401285460172,
1.97651675848088,1.98653237399755,2.00656360503089,2.03661045158091),(-0.204,
0.204),.UNSPECIFIED.);
#18904=B_SPLINE_SURFACE_WITH_KNOTS('',3,3,((#58035,#58036,#58037,#58038),
(#58039,#58040,#58041,#58042),(#58043,#58044,#58045,#58046),(#58047,#58048,
#58049,#58050)),.UNSPECIFIED.,.F.,.F.,.F.,(4,4),(4,4),(1.9008556588209,
1.96650114296421),(-0.204000199215518,0.204),.UNSPECIFIED.);
#18905=B_SPLINE_SURFACE_WITH_KNOTS('',3,3,((#58052,#58053,#58054,#58055),
(#58056,#58057,#58058,#58059),(#58060,#58061,#58062,#58063),(#58064,#58065,
#58066,#58067),(#58068,#58069,#58070,#58071),(#58072,#58073,#58074,#58075),
(#58076,#58077,#58078,#58079),(#58080,#58081,#58082,#58083),(#58084,#58085,
#58086,#58087)),.UNSPECIFIED.,.F.,.F.,.F.,(4,1,1,1,1,1,4),(4,4),(1.82758018188507,
1.83805116497033,1.84328487279121,1.85898599625385,1.87992082753738,1.89038824317914,
1.9008592262644),(-0.204,0.204003567443499),.UNSPECIFIED.);
#18906=B_SPLINE_SURFACE_WITH_KNOTS('',3,3,((#58089,#58090,#58091,#58092),
(#58093,#58094,#58095,#58096),(#58097,#58098,#58099,#58100),(#58101,#58102,
#58103,#58104),(#58105,#58106,#58107,#58108),(#58109,#58110,#58111,#58112)),
 .UNSPECIFIED.,.F.,.F.,.F.,(4,1,1,4),(4,4),(1.80197179046417,1.80928949299685,
1.8129483442632,1.82758374932857),(-0.204,0.204000646491389),
 .UNSPECIFIED.);
#18907=B_SPLINE_SURFACE_WITH_KNOTS('',3,3,((#58114,#58115,#58116,#58117),
(#58118,#58119,#58120,#58121),(#58122,#58123,#58124,#58125),(#58126,#58127,
#58128,#58129),(#58130,#58131,#58132,#58133),(#58134,#58135,#58136,#58137),
(#58138,#58139,#58140,#58141),(#58142,#58143,#58144,#58145),(#58146,#58147,
#58148,#58149),(#58150,#58151,#58152,#58153),(#58154,#58155,#58156,#58157),
(#58158,#58159,#58160,#58161)),.UNSPECIFIED.,.F.,.F.,.F.,(4,1,1,1,1,1,1,
1,1,4),(4,4),(1.56845471413357,1.60181606521468,1.66853464029784,1.70189392783942,
1.735253215381,1.7435930372664,1.75193285915179,1.76861250292259,1.78529214669338,
1.8019738540036),(-0.204001877008512,0.204002063539524),.UNSPECIFIED.);
#18908=B_SPLINE_SURFACE_WITH_KNOTS('',3,3,((#58163,#58164,#58165,#58166),
(#58167,#58168,#58169,#58170),(#58171,#58172,#58173,#58174),(#58175,#58176,
#58177,#58178),(#58179,#58180,#58181,#58182),(#58183,#58184,#58185,#58186),
(#58187,#58188,#58189,#58190)),.UNSPECIFIED.,.F.,.F.,.F.,(4,1,1,1,4),(4,
4),(1.43249195629979,1.45191550221026,1.4616272751655,1.4907625940312,1.56845677767309),
(-0.204,0.204),.UNSPECIFIED.);
#18909=B_SPLINE_SURFACE_WITH_KNOTS('',3,3,((#58192,#58193,#58194,#58195),
(#58196,#58197,#58198,#58199),(#58200,#58201,#58202,#58203),(#58204,#58205,
#58206,#58207),(#58208,#58209,#58210,#58211),(#58212,#58213,#58214,#58215),
(#58216,#58217,#58218,#58219),(#58220,#58221,#58222,#58223)),
 .UNSPECIFIED.,.F.,.F.,.F.,(4,1,1,1,1,4),(4,4),(1.26182357380732,1.33496716630409,
1.35934836380302,1.38372956130194,1.3959201600514,1.43249195629979),(-0.204,
0.204),.UNSPECIFIED.);
#18910=B_SPLINE_SURFACE_WITH_KNOTS('',3,3,((#58225,#58226,#58227,#58228),
(#58229,#58230,#58231,#58232),(#58233,#58234,#58235,#58236),(#58237,#58238,
#58239,#58240),(#58241,#58242,#58243,#58244),(#58245,#58246,#58247,#58248),
(#58249,#58250,#58251,#58252),(#58253,#58254,#58255,#58256),(#58257,#58258,
#58259,#58260),(#58261,#58262,#58263,#58264),(#58265,#58266,#58267,#58268),
(#58269,#58270,#58271,#58272),(#58273,#58274,#58275,#58276),(#58277,#58278,
#58279,#58280),(#58281,#58282,#58283,#58284),(#58285,#58286,#58287,#58288)),
 .UNSPECIFIED.,.F.,.F.,.F.,(4,1,1,1,1,1,1,1,1,1,1,1,1,4),(4,4),(0.756789029878484,
0.828970599685942,0.901112762039505,0.919148302627896,0.937183843216286,
0.973254924393068,1.00932600556985,1.02736154615824,1.03637931645244,1.04539708674663,
1.11753924910019,1.18968141145376,1.22575249263054,1.26186298126122),(-0.204039407453895,
0.204016158273927),.UNSPECIFIED.);
#18911=B_SPLINE_SURFACE_WITH_KNOTS('',3,3,((#58290,#58291,#58292,#58293),
(#58294,#58295,#58296,#58297),(#58298,#58299,#58300,#58301),(#58302,#58303,
#58304,#58305),(#58306,#58307,#58308,#58309),(#58310,#58311,#58312,#58313),
(#58314,#58315,#58316,#58317),(#58318,#58319,#58320,#58321),(#58322,#58323,
#58324,#58325),(#58326,#58327,#58328,#58329)),.UNSPECIFIED.,.F.,.F.,.F.,
(4,1,1,1,1,1,1,4),(4,4),(0.,0.21623669638068,0.324355044571019,0.432473392761359,
0.540591740951699,0.648710089142039,0.702769263237209,0.756836420205482),
(-0.204,0.204007982873103),.UNSPECIFIED.);
#18912=B_SPLINE_SURFACE_WITH_KNOTS('',3,3,((#58331,#58332,#58333,#58334),
(#58335,#58336,#58337,#58338),(#58339,#58340,#58341,#58342),(#58343,#58344,
#58345,#58346),(#58347,#58348,#58349,#58350),(#58351,#58352,#58353,#58354),
(#58355,#58356,#58357,#58358),(#58359,#58360,#58361,#58362),(#58363,#58364,
#58365,#58366)),.UNSPECIFIED.,.F.,.F.,.F.,(4,1,1,1,1,1,4),(4,4),(13.8978590689825,
14.2193450517567,14.862262798083,15.1837216712462,15.5051805444094,15.8266394175726,
16.1481253792677),(-0.204025631400802,0.204027109611016),.UNSPECIFIED.);
#18913=B_SPLINE_SURFACE_WITH_KNOTS('',3,3,((#58369,#58370,#58371,#58372),
(#58373,#58374,#58375,#58376),(#58377,#58378,#58379,#58380),(#58381,#58382,
#58383,#58384),(#58385,#58386,#58387,#58388),(#58389,#58390,#58391,#58392)),
 .UNSPECIFIED.,.F.,.F.,.F.,(4,1,1,4),(4,4),(12.3501192806041,13.0134488895805,
13.455667534087,13.8978877785644),(-0.204,0.204001642216694),
 .UNSPECIFIED.);
#18914=B_SPLINE_SURFACE_WITH_KNOTS('',3,3,((#58394,#58395,#58396,#58397),
(#58398,#58399,#58400,#58401),(#58402,#58403,#58404,#58405),(#58406,#58407,
#58408,#58409),(#58410,#58411,#58412,#58413),(#58414,#58415,#58416,#58417),
(#58418,#58419,#58420,#58421),(#58422,#58423,#58424,#58425),(#58426,#58427,
#58428,#58429)),.UNSPECIFIED.,.F.,.F.,.F.,(4,1,1,1,1,1,4),(4,4),(10.8793710892452,
11.0894782083274,11.2995853274097,11.5096924464919,11.7197995655741,11.9299066846563,
12.3501209228208),(-0.204,0.204),.UNSPECIFIED.);
#18915=B_SPLINE_SURFACE_WITH_KNOTS('',3,3,((#58431,#58432,#58433,#58434),
(#58435,#58436,#58437,#58438),(#58439,#58440,#58441,#58442),(#58443,#58444,
#58445,#58446),(#58447,#58448,#58449,#58450),(#58451,#58452,#58453,#58454),
(#58455,#58456,#58457,#58458),(#58459,#58460,#58461,#58462),(#58463,#58464,
#58465,#58466)),.UNSPECIFIED.,.F.,.F.,.F.,(4,1,1,1,1,1,4),(4,4),(7.9278984945301,
8.77117777664964,9.19281643916875,9.61445510168786,10.036093764207,10.4577324267261,
10.8793730468907),(-0.204,0.204031354795924),.UNSPECIFIED.);
#18916=B_SPLINE_SURFACE_WITH_KNOTS('',3,3,((#58468,#58469,#58470,#58471),
(#58472,#58473,#58474,#58475),(#58476,#58477,#58478,#58479),(#58480,#58481,
#58482,#58483)),.UNSPECIFIED.,.F.,.F.,.F.,(4,4),(4,4),(6.94071132372615,
7.92790045161141),(-0.204,0.20400038518575),.UNSPECIFIED.);
#18917=B_SPLINE_SURFACE_WITH_KNOTS('',3,3,((#58485,#58486,#58487,#58488),
(#58489,#58490,#58491,#58492),(#58493,#58494,#58495,#58496),(#58497,#58498,
#58499,#58500),(#58501,#58502,#58503,#58504),(#58505,#58506,#58507,#58508),
(#58509,#58510,#58511,#58512),(#58513,#58514,#58515,#58516),(#58517,#58518,
#58519,#58520),(#58521,#58522,#58523,#58524),(#58525,#58526,#58527,#58528),
(#58529,#58530,#58531,#58532)),.UNSPECIFIED.,.F.,.F.,.F.,(4,1,1,1,1,1,1,
1,1,4),(4,4),(4.48918216137468,4.66429138725693,4.75184600019805,4.83940061313917,
5.53983751666817,5.89005596843266,6.06516519431491,6.24027442019716,6.59049287196166,
6.94071132372615),(-0.204,0.204015052160367),.UNSPECIFIED.);
#18918=B_SPLINE_SURFACE_WITH_KNOTS('',3,3,((#58534,#58535,#58536,#58537),
(#58538,#58539,#58540,#58541),(#58542,#58543,#58544,#58545),(#58546,#58547,
#58548,#58549)),.UNSPECIFIED.,.F.,.F.,.F.,(4,4),(4,4),(3.57654770812807,
4.48918216137468),(-0.204,0.204),.UNSPECIFIED.);
#18919=B_SPLINE_SURFACE_WITH_KNOTS('',3,3,((#58551,#58552,#58553,#58554),
(#58555,#58556,#58557,#58558),(#58559,#58560,#58561,#58562),(#58563,#58564,
#58565,#58566),(#58567,#58568,#58569,#58570),(#58571,#58572,#58573,#58574)),
 .UNSPECIFIED.,.F.,.F.,.F.,(4,1,1,4),(4,4),(2.87518401914012,3.17576845727781,
3.37615808270294,3.57654770812807),(-0.204,0.204),.UNSPECIFIED.);
#18920=B_SPLINE_SURFACE_WITH_KNOTS('',3,3,((#58576,#58577,#58578,#58579),
(#58580,#58581,#58582,#58583),(#58584,#58585,#58586,#58587),(#58588,#58589,
#58590,#58591),(#58592,#58593,#58594,#58595),(#58596,#58597,#58598,#58599),
(#58600,#58601,#58602,#58603),(#58604,#58605,#58606,#58607)),
 .UNSPECIFIED.,.F.,.F.,.F.,(4,1,1,1,1,4),(4,4),(2.26956600807314,2.44259972552085,
2.5291165842447,2.61563344296856,2.70215030169241,2.87518401914012),(-0.204,
0.204),.UNSPECIFIED.);
#18921=B_SPLINE_SURFACE_WITH_KNOTS('',3,3,((#58609,#58610,#58611,#58612),
(#58613,#58614,#58615,#58616),(#58617,#58618,#58619,#58620),(#58621,#58622,
#58623,#58624),(#58625,#58626,#58627,#58628),(#58629,#58630,#58631,#58632),
(#58633,#58634,#58635,#58636),(#58637,#58638,#58639,#58640),(#58641,#58642,
#58643,#58644)),.UNSPECIFIED.,.F.,.F.,.F.,(4,1,1,1,1,1,4),(4,4),(1.46286168120391,
1.57811142102339,1.80859628337331,1.92383871454827,2.03908114572322,2.15432357689818,
2.26957331671767),(-0.204,0.204007308644527),.UNSPECIFIED.);
#18922=B_SPLINE_SURFACE_WITH_KNOTS('',3,3,((#58648,#58649,#58650,#58651),
(#58652,#58653,#58654,#58655),(#58656,#58657,#58658,#58659),(#58660,#58661,
#58662,#58663),(#58664,#58665,#58666,#58667),(#58668,#58669,#58670,#58671),
(#58672,#58673,#58674,#58675),(#58676,#58677,#58678,#58679),(#58680,#58681,
#58682,#58683)),.UNSPECIFIED.,.F.,.F.,.F.,(4,1,1,1,1,1,4),(4,4),(0.,0.208981284264062,
0.626943852792187,0.835925137056249,1.04490642132031,1.25388770558437,1.46286898984844),
(-0.204,0.204),.UNSPECIFIED.);
#18923=B_SPLINE_SURFACE_WITH_KNOTS('',3,3,((#58685,#58686,#58687,#58688),
(#58689,#58690,#58691,#58692),(#58693,#58694,#58695,#58696),(#58697,#58698,
#58699,#58700),(#58701,#58702,#58703,#58704),(#58705,#58706,#58707,#58708),
(#58709,#58710,#58711,#58712),(#58713,#58714,#58715,#58716)),
 .UNSPECIFIED.,.F.,.F.,.F.,(4,1,1,1,1,4),(4,4),(16.1480982907358,17.1122318399124,
17.4336096896379,17.7549875393634,17.9156764642262,18.3977432388145),(-0.204,
0.204),.UNSPECIFIED.);
#18924=B_SPLINE_SURFACE_WITH_KNOTS('',3,3,((#58717,#58718,#58719,#58720),
(#58721,#58722,#58723,#58724),(#58725,#58726,#58727,#58728),(#58729,#58730,
#58731,#58732),(#58733,#58734,#58735,#58736),(#58737,#58738,#58739,#58740),
(#58741,#58742,#58743,#58744),(#58745,#58746,#58747,#58748),(#58749,#58750,
#58751,#58752),(#58753,#58754,#58755,#58756),(#58757,#58758,#58759,#58760)),
 .UNSPECIFIED.,.F.,.F.,.F.,(4,1,1,1,1,1,1,1,4),(4,4),(2.19155818449868,
2.25090656855756,2.280580760587,2.31025495261644,2.32509204863116,2.33992914464588,
2.36960333667532,2.48830010479308,2.60699687291084),(-0.204,0.204),
 .UNSPECIFIED.);
#18925=B_SPLINE_SURFACE_WITH_KNOTS('',3,3,((#58761,#58762,#58763,#58764),
(#58765,#58766,#58767,#58768),(#58769,#58770,#58771,#58772),(#58773,#58774,
#58775,#58776)),.UNSPECIFIED.,.F.,.F.,.F.,(4,4),(4,4),(-0.424185966322057,
0.),(-0.204,0.204),.UNSPECIFIED.);
#18926=B_SPLINE_SURFACE_WITH_KNOTS('',3,3,((#58777,#58778,#58779,#58780),
(#58781,#58782,#58783,#58784),(#58785,#58786,#58787,#58788),(#58789,#58790,
#58791,#58792),(#58793,#58794,#58795,#58796),(#58797,#58798,#58799,#58800),
(#58801,#58802,#58803,#58804),(#58805,#58806,#58807,#58808),(#58809,#58810,
#58811,#58812),(#58813,#58814,#58815,#58816),(#58817,#58818,#58819,#58820),
(#58821,#58822,#58823,#58824),(#58825,#58826,#58827,#58828),(#58829,#58830,
#58831,#58832),(#58833,#58834,#58835,#58836),(#58837,#58838,#58839,#58840),
(#58841,#58842,#58843,#58844),(#58845,#58846,#58847,#58848)),
 .UNSPECIFIED.,.F.,.F.,.F.,(4,1,1,1,1,1,1,1,1,1,1,1,1,1,1,4),(4,4),(0.,
0.0536833715747986,0.107366743149597,0.161050114724396,0.214733486299194,
0.228154329192894,0.241575172086594,0.268416857873993,0.322100229448792,
0.37578360102359,0.429466972598389,0.509992029960587,0.590517087322785,
0.644200458897583,0.697883830472382,0.75156720204718),(-0.204,0.204),
 .UNSPECIFIED.);
#18927=B_SPLINE_SURFACE_WITH_KNOTS('',3,3,((#58850,#58851,#58852,#58853),
(#58854,#58855,#58856,#58857),(#58858,#58859,#58860,#58861),(#58862,#58863,
#58864,#58865)),.UNSPECIFIED.,.F.,.F.,.F.,(4,4),(4,4),(11.5791004161139,
11.7855397152994),(-0.204,0.20400006877991),.UNSPECIFIED.);
#18928=B_SPLINE_SURFACE_WITH_KNOTS('',3,3,((#58866,#58867,#58868,#58869),
(#58870,#58871,#58872,#58873),(#58874,#58875,#58876,#58877),(#58878,#58879,
#58880,#58881),(#58882,#58883,#58884,#58885),(#58886,#58887,#58888,#58889),
(#58890,#58891,#58892,#58893),(#58894,#58895,#58896,#58897),(#58898,#58899,
#58900,#58901),(#58902,#58903,#58904,#58905),(#58906,#58907,#58908,#58909),
(#58910,#58911,#58912,#58913),(#58914,#58915,#58916,#58917)),
 .UNSPECIFIED.,.F.,.F.,.F.,(4,1,1,1,1,1,1,1,1,1,4),(4,4),(6.50711619353453,
6.712779658626,6.91844066613449,6.96985591801162,7.02127116988874,7.22693217739724,
7.32976268115149,7.48400843678286,7.53542368865998,7.74108469616848,7.94674816125994),
(-0.204002457582968,0.204),.UNSPECIFIED.);
#18929=B_SPLINE_SURFACE_WITH_KNOTS('',3,3,((#58918,#58919,#58920,#58921,
#58922),(#58923,#58924,#58925,#58926,#58927),(#58928,#58929,#58930,#58931,
#58932),(#58933,#58934,#58935,#58936,#58937),(#58938,#58939,#58940,#58941,
#58942),(#58943,#58944,#58945,#58946,#58947),(#58948,#58949,#58950,#58951,
#58952),(#58953,#58954,#58955,#58956,#58957),(#58958,#58959,#58960,#58961,
#58962),(#58963,#58964,#58965,#58966,#58967),(#58968,#58969,#58970,#58971,
#58972),(#58973,#58974,#58975,#58976,#58977),(#58978,#58979,#58980,#58981,
#58982),(#58983,#58984,#58985,#58986,#58987),(#58988,#58989,#58990,#58991,
#58992),(#58993,#58994,#58995,#58996,#58997),(#58998,#58999,#59000,#59001,
#59002),(#59003,#59004,#59005,#59006,#59007),(#59008,#59009,#59010,#59011,
#59012),(#59013,#59014,#59015,#59016,#59017),(#59018,#59019,#59020,#59021,
#59022),(#59023,#59024,#59025,#59026,#59027),(#59028,#59029,#59030,#59031,
#59032),(#59033,#59034,#59035,#59036,#59037),(#59038,#59039,#59040,#59041,
#59042),(#59043,#59044,#59045,#59046,#59047)),.UNSPECIFIED.,.F.,.F.,.F.,
(4,1,1,1,1,1,1,1,1,1,1,1,1,1,1,1,1,1,1,1,1,1,1,4),(4,1,4),(0.,0.0539979975781232,
0.107995995156246,0.215991990312493,0.269989987890616,0.323987985468739,
0.377985983046862,0.431983980624985,0.458982979414047,0.472482478808578,
0.485981978203109,0.49948147759764,0.51298097699217,0.519730726689436,0.521418164113752,
0.526480476386701,0.529855351235334,0.533230226083967,0.536605100932599,
0.538292538356915,0.539979975781232,0.593977973359355,0.647975970937478,
0.755971966093725),(-0.204000260274416,-0.0291428571428571,0.204),
 .UNSPECIFIED.);
#18930=B_SPLINE_SURFACE_WITH_KNOTS('',3,3,((#59049,#59050,#59051,#59052),
(#59053,#59054,#59055,#59056),(#59057,#59058,#59059,#59060),(#59061,#59062,
#59063,#59064)),.UNSPECIFIED.,.F.,.F.,.F.,(4,4),(4,4),(-0.0833603842763964,
0.),(-0.204,0.204),.UNSPECIFIED.);
#18931=B_SPLINE_SURFACE_WITH_KNOTS('',3,3,((#61280,#61281,#61282,#61283,
#61284,#61285,#61286,#61287),(#61288,#61289,#61290,#61291,#61292,#61293,
#61294,#61295),(#61296,#61297,#61298,#61299,#61300,#61301,#61302,#61303),
(#61304,#61305,#61306,#61307,#61308,#61309,#61310,#61311),(#61312,#61313,
#61314,#61315,#61316,#61317,#61318,#61319)),.UNSPECIFIED.,.F.,.F.,.F.,(4,
1,4),(4,2,1,1,4),(-0.00184352937430784,0.571428571428571,1.),(-1.32899011332275,
-1.3277635388384,-1.06297443065277,-0.974711394590892,-0.884839152512737),
 .UNSPECIFIED.);
#18932=B_SPLINE_SURFACE_WITH_KNOTS('',3,3,((#61347,#61348,#61349,#61350,
#61351,#61352),(#61353,#61354,#61355,#61356,#61357,#61358),(#61359,#61360,
#61361,#61362,#61363,#61364),(#61365,#61366,#61367,#61368,#61369,#61370),
(#61371,#61372,#61373,#61374,#61375,#61376)),.UNSPECIFIED.,.F.,.F.,.F.,
(4,1,4),(4,2,4),(-0.0048972902445563,0.571428571428571,1.),(-0.446212470553937,
0.,0.00122657448435937),.UNSPECIFIED.);
#18933=B_SPLINE_SURFACE_WITH_KNOTS('',3,3,((#88758,#88759,#88760,#88761,
#88762,#88763,#88764,#88765,#88766,#88767,#88768,#88769,#88770,#88771,#88772,
#88773,#88774,#88775,#88776,#88777,#88778,#88779,#88780,#88781,#88782,#88783,
#88784,#88785,#88786,#88787,#88788,#88789,#88790,#88791,#88792,#88793,#88794,
#88795,#88796,#88797,#88798,#88799,#88800,#88801,#88802,#88803,#88804,#88805,
#88806,#88807,#88808,#88809,#88810,#88811,#88812,#88813,#88814,#88815,#88816,
#88817,#88818,#88819,#88820,#88821,#88822,#88823,#88824,#88825,#88826,#88827,
#88828,#88829,#88830,#88831,#88832,#88833,#88834,#88835,#88836,#88837,#88838,
#88839,#88840,#88841,#88842,#88843,#88844,#88845,#88846,#88847,#88848,#88849,
#88850,#88851,#88852,#88853,#88854,#88855,#88856,#88857,#88858,#88859,#88860,
#88861,#88862,#88863,#88864,#88865,#88866,#88867,#88868,#88869,#88870,#88871,
#88872,#88873,#88874,#88875,#88876,#88877,#88878,#88879,#88880,#88881,#88882,
#88883,#88884,#88885,#88886,#88887,#88888,#88889,#88890,#88891,#88892,#88893,
#88894,#88895,#88896,#88897,#88898,#88899,#88900,#88901,#88902,#88903,#88904,
#88905,#88906,#88907,#88908,#88909,#88910,#88911,#88912,#88913,#88914,#88915,
#88916,#88917,#88918,#88919,#88920,#88921,#88922,#88923,#88924,#88925,#88926,
#88927,#88928,#88929,#88930,#88931,#88932,#88933,#88934,#88935,#88936,#88937,
#88938,#88939,#88940,#88941,#88942,#88943,#88944,#88945,#88946,#88947,#88948,
#88949,#88950,#88951,#88952,#88953,#88954,#88955,#88956,#88957,#88958,#88959,
#88960,#88961,#88962,#88963,#88964,#88965,#88966,#88967,#88968,#88969,#88970,
#88971,#88972,#88973,#88974,#88975,#88976,#88977,#88978,#88979,#88980,#88981,
#88982,#88983,#88984,#88985,#88986,#88987,#88988,#88989,#88990,#88991,#88992,
#88993,#88994,#88995,#88996,#88997,#88998,#88999,#89000,#89001,#89002,#89003,
#89004,#89005,#89006,#89007),(#89008,#89009,#89010,#89011,#89012,#89013,
#89014,#89015,#89016,#89017,#89018,#89019,#89020,#89021,#89022,#89023,#89024,
#89025,#89026,#89027,#89028,#89029,#89030,#89031,#89032,#89033,#89034,#89035,
#89036,#89037,#89038,#89039,#89040,#89041,#89042,#89043,#89044,#89045,#89046,
#89047,#89048,#89049,#89050,#89051,#89052,#89053,#89054,#89055,#89056,#89057,
#89058,#89059,#89060,#89061,#89062,#89063,#89064,#89065,#89066,#89067,#89068,
#89069,#89070,#89071,#89072,#89073,#89074,#89075,#89076,#89077,#89078,#89079,
#89080,#89081,#89082,#89083,#89084,#89085,#89086,#89087,#89088,#89089,#89090,
#89091,#89092,#89093,#89094,#89095,#89096,#89097,#89098,#89099,#89100,#89101,
#89102,#89103,#89104,#89105,#89106,#89107,#89108,#89109,#89110,#89111,#89112,
#89113,#89114,#89115,#89116,#89117,#89118,#89119,#89120,#89121,#89122,#89123,
#89124,#89125,#89126,#89127,#89128,#89129,#89130,#89131,#89132,#89133,#89134,
#89135,#89136,#89137,#89138,#89139,#89140,#89141,#89142,#89143,#89144,#89145,
#89146,#89147,#89148,#89149,#89150,#89151,#89152,#89153,#89154,#89155,#89156,
#89157,#89158,#89159,#89160,#89161,#89162,#89163,#89164,#89165,#89166,#89167,
#89168,#89169,#89170,#89171,#89172,#89173,#89174,#89175,#89176,#89177,#89178,
#89179,#89180,#89181,#89182,#89183,#89184,#89185,#89186,#89187,#89188,#89189,
#89190,#89191,#89192,#89193,#89194,#89195,#89196,#89197,#89198,#89199,#89200,
#89201,#89202,#89203,#89204,#89205,#89206,#89207,#89208,#89209,#89210,#89211,
#89212,#89213,#89214,#89215,#89216,#89217,#89218,#89219,#89220,#89221,#89222,
#89223,#89224,#89225,#89226,#89227,#89228,#89229,#89230,#89231,#89232,#89233,
#89234,#89235,#89236,#89237,#89238,#89239,#89240,#89241,#89242,#89243,#89244,
#89245,#89246,#89247,#89248,#89249,#89250,#89251,#89252,#89253,#89254,#89255,
#89256,#89257),(#89258,#89259,#89260,#89261,#89262,#89263,#89264,#89265,
#89266,#89267,#89268,#89269,#89270,#89271,#89272,#89273,#89274,#89275,#89276,
#89277,#89278,#89279,#89280,#89281,#89282,#89283,#89284,#89285,#89286,#89287,
#89288,#89289,#89290,#89291,#89292,#89293,#89294,#89295,#89296,#89297,#89298,
#89299,#89300,#89301,#89302,#89303,#89304,#89305,#89306,#89307,#89308,#89309,
#89310,#89311,#89312,#89313,#89314,#89315,#89316,#89317,#89318,#89319,#89320,
#89321,#89322,#89323,#89324,#89325,#89326,#89327,#89328,#89329,#89330,#89331,
#89332,#89333,#89334,#89335,#89336,#89337,#89338,#89339,#89340,#89341,#89342,
#89343,#89344,#89345,#89346,#89347,#89348,#89349,#89350,#89351,#89352,#89353,
#89354,#89355,#89356,#89357,#89358,#89359,#89360,#89361,#89362,#89363,#89364,
#89365,#89366,#89367,#89368,#89369,#89370,#89371,#89372,#89373,#89374,#89375,
#89376,#89377,#89378,#89379,#89380,#89381,#89382,#89383,#89384,#89385,#89386,
#89387,#89388,#89389,#89390,#89391,#89392,#89393,#89394,#89395,#89396,#89397,
#89398,#89399,#89400,#89401,#89402,#89403,#89404,#89405,#89406,#89407,#89408,
#89409,#89410,#89411,#89412,#89413,#89414,#89415,#89416,#89417,#89418,#89419,
#89420,#89421,#89422,#89423,#89424,#89425,#89426,#89427,#89428,#89429,#89430,
#89431,#89432,#89433,#89434,#89435,#89436,#89437,#89438,#89439,#89440,#89441,
#89442,#89443,#89444,#89445,#89446,#89447,#89448,#89449,#89450,#89451,#89452,
#89453,#89454,#89455,#89456,#89457,#89458,#89459,#89460,#89461,#89462,#89463,
#89464,#89465,#89466,#89467,#89468,#89469,#89470,#89471,#89472,#89473,#89474,
#89475,#89476,#89477,#89478,#89479,#89480,#89481,#89482,#89483,#89484,#89485,
#89486,#89487,#89488,#89489,#89490,#89491,#89492,#89493,#89494,#89495,#89496,
#89497,#89498,#89499,#89500,#89501,#89502,#89503,#89504,#89505,#89506,#89507),
(#89508,#89509,#89510,#89511,#89512,#89513,#89514,#89515,#89516,#89517,
#89518,#89519,#89520,#89521,#89522,#89523,#89524,#89525,#89526,#89527,#89528,
#89529,#89530,#89531,#89532,#89533,#89534,#89535,#89536,#89537,#89538,#89539,
#89540,#89541,#89542,#89543,#89544,#89545,#89546,#89547,#89548,#89549,#89550,
#89551,#89552,#89553,#89554,#89555,#89556,#89557,#89558,#89559,#89560,#89561,
#89562,#89563,#89564,#89565,#89566,#89567,#89568,#89569,#89570,#89571,#89572,
#89573,#89574,#89575,#89576,#89577,#89578,#89579,#89580,#89581,#89582,#89583,
#89584,#89585,#89586,#89587,#89588,#89589,#89590,#89591,#89592,#89593,#89594,
#89595,#89596,#89597,#89598,#89599,#89600,#89601,#89602,#89603,#89604,#89605,
#89606,#89607,#89608,#89609,#89610,#89611,#89612,#89613,#89614,#89615,#89616,
#89617,#89618,#89619,#89620,#89621,#89622,#89623,#89624,#89625,#89626,#89627,
#89628,#89629,#89630,#89631,#89632,#89633,#89634,#89635,#89636,#89637,#89638,
#89639,#89640,#89641,#89642,#89643,#89644,#89645,#89646,#89647,#89648,#89649,
#89650,#89651,#89652,#89653,#89654,#89655,#89656,#89657,#89658,#89659,#89660,
#89661,#89662,#89663,#89664,#89665,#89666,#89667,#89668,#89669,#89670,#89671,
#89672,#89673,#89674,#89675,#89676,#89677,#89678,#89679,#89680,#89681,#89682,
#89683,#89684,#89685,#89686,#89687,#89688,#89689,#89690,#89691,#89692,#89693,
#89694,#89695,#89696,#89697,#89698,#89699,#89700,#89701,#89702,#89703,#89704,
#89705,#89706,#89707,#89708,#89709,#89710,#89711,#89712,#89713,#89714,#89715,
#89716,#89717,#89718,#89719,#89720,#89721,#89722,#89723,#89724,#89725,#89726,
#89727,#89728,#89729,#89730,#89731,#89732,#89733,#89734,#89735,#89736,#89737,
#89738,#89739,#89740,#89741,#89742,#89743,#89744,#89745,#89746,#89747,#89748,
#89749,#89750,#89751,#89752,#89753,#89754,#89755,#89756,#89757)),
 .UNSPECIFIED.,.F.,.F.,.F.,(4,4),(4,1,1,1,1,1,1,1,1,1,1,1,1,1,1,1,1,1,1,
1,1,1,1,1,1,1,1,1,1,1,1,1,1,1,1,1,1,1,1,1,1,1,1,1,1,1,1,1,1,1,1,1,1,1,1,
1,1,1,1,1,1,1,1,1,1,1,1,1,1,1,1,1,1,1,1,1,1,1,1,1,1,1,1,1,1,1,1,1,1,1,1,
1,1,1,1,1,1,1,1,1,1,1,1,1,1,1,1,1,1,1,1,1,1,1,1,1,1,1,1,1,1,1,1,1,1,1,1,
1,1,1,1,1,1,1,1,1,1,1,1,1,1,1,1,1,1,1,1,1,1,1,1,1,1,1,1,1,1,1,1,1,1,1,1,
1,1,1,1,1,1,1,1,1,1,1,1,1,1,1,1,1,1,1,1,1,1,1,1,1,1,1,1,1,1,1,1,1,1,1,1,
1,1,1,1,1,1,1,1,1,1,1,1,1,1,1,1,1,1,1,1,1,1,1,1,1,1,1,1,1,1,1,1,1,1,1,1,
1,1,1,1,1,1,1,1,1,1,1,1,4),(-0.000536156821677024,0.0823575402511902),(8.31473274985828,
9.31424788838504,10.3137630269118,11.3132781654386,12.3127933039653,13.3123084424921,
14.3118235810189,15.3113387195456,16.3108538580724,17.3103689965991,18.3098841351259,
19.3093992736527,20.3089144121794,21.3084295507062,22.307944689233,23.3074598277597,
24.3069749662865,25.3064901048132,26.30600524334,27.3055203818668,28.3050355203935,
29.3045506589203,30.3040657974471,31.3035809359738,32.3030960745006,33.3026112130273,
34.3021263515541,35.3016414900809,36.3011566286076,37.3006717671344,38.3001869056612,
39.2997020441879,40.2992171827147,41.2987323212414,42.2982474597682,43.297762598295,
44.2972777368217,45.2967928753485,46.2963080138753,47.295823152402,48.2953382909288,
49.2948534294556,50.2943685679823,51.2938837065091,52.2933988450358,53.2929139835626,
54.2924291220894,55.2919442606161,56.2914593991429,57.2909745376696,58.2904896761964,
59.2900048147232,60.2895199532499,61.2890350917767,62.2885502303035,63.2880653688302,
64.287580507357,65.2870956458838,66.2866107844105,67.2861259229373,68.285641061464,
69.2851561999908,70.2846713385176,71.2841864770443,72.2837016155711,73.2832167540979,
74.2827318926246,75.2822470311514,76.2817621696781,77.2812773082049,78.2807924467317,
79.2803075852584,80.2798227237852,81.2793378623119,82.2788530008387,83.2783681393655,
84.2778832778922,85.277398416419,86.2769135549458,87.2764286934725,88.2759438319993,
89.2754589705261,90.2749741090528,91.2744892475796,92.2740043861063,93.2735195246331,
94.2730346631599,95.2725498016866,96.2720649402134,97.2715800787402,98.2710952172669,
99.2706103557937,100.27012549432,101.269640632847,102.269155771374,103.268670909901,
104.268186048427,105.267701186954,106.267216325481,107.266731464008,108.266246602535,
109.265761741061,110.265276879588,111.264792018115,112.264307156642,113.263822295168,
114.263337433695,115.262852572222,116.262367710749,117.261882849275,118.261397987802,
119.260913126329,120.260428264856,121.259943403382,122.259458541909,123.258973680436,
124.258488818963,125.25800395749,126.257519096016,127.257034234543,128.25654937307,
129.256064511597,130.255579650123,131.25509478865,132.254609927177,133.254125065704,
134.25364020423,135.253155342757,136.252670481284,137.252185619811,138.251700758337,
139.251215896864,140.250731035391,141.250246173918,142.249761312444,143.249276450971,
144.248791589498,145.248306728025,146.247821866552,147.247337005078,148.246852143605,
149.246367282132,150.245882420659,151.245397559185,152.244912697712,153.244427836239,
154.243942974766,155.243458113292,156.242973251819,157.242488390346,158.242003528873,
159.241518667399,160.241033805926,161.240548944453,162.24006408298,163.239579221506,
164.239094360033,165.23860949856,166.238124637087,167.237639775614,168.23715491414,
169.236670052667,170.236185191194,171.235700329721,172.235215468247,173.234730606774,
174.234245745301,175.233760883828,176.233276022354,177.232791160881,178.232306299408,
179.231821437935,180.231336576461,181.230851714988,182.230366853515,183.229881992042,
184.229397130569,185.228912269095,186.228427407622,187.227942546149,188.227457684676,
189.226972823202,190.226487961729,191.226003100256,192.225518238783,193.225033377309,
194.224548515836,195.224063654363,196.22357879289,197.223093931416,198.222609069943,
199.22212420847,200.221639346997,201.221154485523,202.22066962405,203.220184762577,
204.219699901104,205.219215039631,206.218730178157,207.218245316684,208.217760455211,
209.217275593738,210.216790732264,211.216305870791,212.215821009318,213.215336147845,
214.214851286371,215.214366424898,216.213881563425,217.213396701952,218.212911840478,
219.212426979005,220.211942117532,221.211457256059,222.210972394585,223.210487533112,
224.210002671639,225.209517810166,226.209032948693,227.208548087219,228.208063225746,
229.207578364273,230.2070935028,231.206608641326,232.206123779853,233.20563891838,
234.205154056907,235.204669195433,236.20418433396,237.203699472487,238.203214611014,
239.20272974954,240.202244888067,241.201760026594,242.201275165121,243.200790303647,
244.200305442174,245.199820580701,246.199335719228,247.198850857755,248.198365996281,
249.197881134808,250.197396273335,251.196911411862,252.196426550388,253.195941688915,
254.195456827442,255.194971965969),.UNSPECIFIED.);
#18934=B_SPLINE_SURFACE_WITH_KNOTS('',3,3,((#89946,#89947,#89948,#89949,
#89950,#89951,#89952,#89953,#89954,#89955,#89956,#89957,#89958,#89959,#89960,
#89961,#89962,#89963,#89964,#89965,#89966,#89967,#89968,#89969,#89970,#89971,
#89972,#89973,#89974,#89975,#89976,#89977,#89978,#89979,#89980,#89981,#89982,
#89983,#89984,#89985,#89986,#89987,#89988,#89989,#89990,#89991,#89992,#89993,
#89994,#89995,#89996,#89997,#89998,#89999,#90000,#90001,#90002,#90003,#90004,
#90005,#90006,#90007,#90008,#90009,#90010,#90011,#90012,#90013,#90014,#90015,
#90016,#90017,#90018,#90019,#90020,#90021,#90022,#90023,#90024,#90025,#90026,
#90027,#90028,#90029,#90030,#90031,#90032,#90033,#90034,#90035,#90036,#90037,
#90038,#90039,#90040,#90041,#90042,#90043,#90044,#90045,#90046,#90047,#90048,
#90049,#90050,#90051,#90052,#90053,#90054,#90055,#90056,#90057,#90058,#90059,
#90060,#90061,#90062,#90063,#90064,#90065,#90066,#90067,#90068,#90069,#90070,
#90071,#90072,#90073,#90074,#90075,#90076,#90077,#90078,#90079,#90080,#90081,
#90082,#90083,#90084,#90085,#90086,#90087,#90088,#90089,#90090,#90091,#90092,
#90093,#90094,#90095,#90096,#90097,#90098,#90099,#90100,#90101,#90102,#90103,
#90104,#90105,#90106,#90107,#90108,#90109,#90110,#90111,#90112,#90113,#90114,
#90115,#90116,#90117,#90118,#90119,#90120,#90121,#90122,#90123,#90124,#90125,
#90126,#90127,#90128,#90129,#90130,#90131,#90132,#90133,#90134,#90135,#90136,
#90137,#90138,#90139,#90140,#90141,#90142,#90143,#90144,#90145,#90146,#90147,
#90148,#90149,#90150,#90151,#90152,#90153,#90154,#90155,#90156,#90157,#90158,
#90159,#90160,#90161,#90162,#90163,#90164,#90165,#90166,#90167,#90168,#90169,
#90170,#90171,#90172,#90173,#90174,#90175,#90176,#90177,#90178,#90179,#90180,
#90181,#90182,#90183,#90184,#90185,#90186,#90187,#90188,#90189,#90190,#90191,
#90192,#90193,#90194,#90195),(#90196,#90197,#90198,#90199,#90200,#90201,
#90202,#90203,#90204,#90205,#90206,#90207,#90208,#90209,#90210,#90211,#90212,
#90213,#90214,#90215,#90216,#90217,#90218,#90219,#90220,#90221,#90222,#90223,
#90224,#90225,#90226,#90227,#90228,#90229,#90230,#90231,#90232,#90233,#90234,
#90235,#90236,#90237,#90238,#90239,#90240,#90241,#90242,#90243,#90244,#90245,
#90246,#90247,#90248,#90249,#90250,#90251,#90252,#90253,#90254,#90255,#90256,
#90257,#90258,#90259,#90260,#90261,#90262,#90263,#90264,#90265,#90266,#90267,
#90268,#90269,#90270,#90271,#90272,#90273,#90274,#90275,#90276,#90277,#90278,
#90279,#90280,#90281,#90282,#90283,#90284,#90285,#90286,#90287,#90288,#90289,
#90290,#90291,#90292,#90293,#90294,#90295,#90296,#90297,#90298,#90299,#90300,
#90301,#90302,#90303,#90304,#90305,#90306,#90307,#90308,#90309,#90310,#90311,
#90312,#90313,#90314,#90315,#90316,#90317,#90318,#90319,#90320,#90321,#90322,
#90323,#90324,#90325,#90326,#90327,#90328,#90329,#90330,#90331,#90332,#90333,
#90334,#90335,#90336,#90337,#90338,#90339,#90340,#90341,#90342,#90343,#90344,
#90345,#90346,#90347,#90348,#90349,#90350,#90351,#90352,#90353,#90354,#90355,
#90356,#90357,#90358,#90359,#90360,#90361,#90362,#90363,#90364,#90365,#90366,
#90367,#90368,#90369,#90370,#90371,#90372,#90373,#90374,#90375,#90376,#90377,
#90378,#90379,#90380,#90381,#90382,#90383,#90384,#90385,#90386,#90387,#90388,
#90389,#90390,#90391,#90392,#90393,#90394,#90395,#90396,#90397,#90398,#90399,
#90400,#90401,#90402,#90403,#90404,#90405,#90406,#90407,#90408,#90409,#90410,
#90411,#90412,#90413,#90414,#90415,#90416,#90417,#90418,#90419,#90420,#90421,
#90422,#90423,#90424,#90425,#90426,#90427,#90428,#90429,#90430,#90431,#90432,
#90433,#90434,#90435,#90436,#90437,#90438,#90439,#90440,#90441,#90442,#90443,
#90444,#90445),(#90446,#90447,#90448,#90449,#90450,#90451,#90452,#90453,
#90454,#90455,#90456,#90457,#90458,#90459,#90460,#90461,#90462,#90463,#90464,
#90465,#90466,#90467,#90468,#90469,#90470,#90471,#90472,#90473,#90474,#90475,
#90476,#90477,#90478,#90479,#90480,#90481,#90482,#90483,#90484,#90485,#90486,
#90487,#90488,#90489,#90490,#90491,#90492,#90493,#90494,#90495,#90496,#90497,
#90498,#90499,#90500,#90501,#90502,#90503,#90504,#90505,#90506,#90507,#90508,
#90509,#90510,#90511,#90512,#90513,#90514,#90515,#90516,#90517,#90518,#90519,
#90520,#90521,#90522,#90523,#90524,#90525,#90526,#90527,#90528,#90529,#90530,
#90531,#90532,#90533,#90534,#90535,#90536,#90537,#90538,#90539,#90540,#90541,
#90542,#90543,#90544,#90545,#90546,#90547,#90548,#90549,#90550,#90551,#90552,
#90553,#90554,#90555,#90556,#90557,#90558,#90559,#90560,#90561,#90562,#90563,
#90564,#90565,#90566,#90567,#90568,#90569,#90570,#90571,#90572,#90573,#90574,
#90575,#90576,#90577,#90578,#90579,#90580,#90581,#90582,#90583,#90584,#90585,
#90586,#90587,#90588,#90589,#90590,#90591,#90592,#90593,#90594,#90595,#90596,
#90597,#90598,#90599,#90600,#90601,#90602,#90603,#90604,#90605,#90606,#90607,
#90608,#90609,#90610,#90611,#90612,#90613,#90614,#90615,#90616,#90617,#90618,
#90619,#90620,#90621,#90622,#90623,#90624,#90625,#90626,#90627,#90628,#90629,
#90630,#90631,#90632,#90633,#90634,#90635,#90636,#90637,#90638,#90639,#90640,
#90641,#90642,#90643,#90644,#90645,#90646,#90647,#90648,#90649,#90650,#90651,
#90652,#90653,#90654,#90655,#90656,#90657,#90658,#90659,#90660,#90661,#90662,
#90663,#90664,#90665,#90666,#90667,#90668,#90669,#90670,#90671,#90672,#90673,
#90674,#90675,#90676,#90677,#90678,#90679,#90680,#90681,#90682,#90683,#90684,
#90685,#90686,#90687,#90688,#90689,#90690,#90691,#90692,#90693,#90694,#90695),
(#90696,#90697,#90698,#90699,#90700,#90701,#90702,#90703,#90704,#90705,
#90706,#90707,#90708,#90709,#90710,#90711,#90712,#90713,#90714,#90715,#90716,
#90717,#90718,#90719,#90720,#90721,#90722,#90723,#90724,#90725,#90726,#90727,
#90728,#90729,#90730,#90731,#90732,#90733,#90734,#90735,#90736,#90737,#90738,
#90739,#90740,#90741,#90742,#90743,#90744,#90745,#90746,#90747,#90748,#90749,
#90750,#90751,#90752,#90753,#90754,#90755,#90756,#90757,#90758,#90759,#90760,
#90761,#90762,#90763,#90764,#90765,#90766,#90767,#90768,#90769,#90770,#90771,
#90772,#90773,#90774,#90775,#90776,#90777,#90778,#90779,#90780,#90781,#90782,
#90783,#90784,#90785,#90786,#90787,#90788,#90789,#90790,#90791,#90792,#90793,
#90794,#90795,#90796,#90797,#90798,#90799,#90800,#90801,#90802,#90803,#90804,
#90805,#90806,#90807,#90808,#90809,#90810,#90811,#90812,#90813,#90814,#90815,
#90816,#90817,#90818,#90819,#90820,#90821,#90822,#90823,#90824,#90825,#90826,
#90827,#90828,#90829,#90830,#90831,#90832,#90833,#90834,#90835,#90836,#90837,
#90838,#90839,#90840,#90841,#90842,#90843,#90844,#90845,#90846,#90847,#90848,
#90849,#90850,#90851,#90852,#90853,#90854,#90855,#90856,#90857,#90858,#90859,
#90860,#90861,#90862,#90863,#90864,#90865,#90866,#90867,#90868,#90869,#90870,
#90871,#90872,#90873,#90874,#90875,#90876,#90877,#90878,#90879,#90880,#90881,
#90882,#90883,#90884,#90885,#90886,#90887,#90888,#90889,#90890,#90891,#90892,
#90893,#90894,#90895,#90896,#90897,#90898,#90899,#90900,#90901,#90902,#90903,
#90904,#90905,#90906,#90907,#90908,#90909,#90910,#90911,#90912,#90913,#90914,
#90915,#90916,#90917,#90918,#90919,#90920,#90921,#90922,#90923,#90924,#90925,
#90926,#90927,#90928,#90929,#90930,#90931,#90932,#90933,#90934,#90935,#90936,
#90937,#90938,#90939,#90940,#90941,#90942,#90943,#90944,#90945)),
 .UNSPECIFIED.,.F.,.F.,.F.,(4,4),(4,1,1,1,1,1,1,1,1,1,1,1,1,1,1,1,1,1,1,
1,1,1,1,1,1,1,1,1,1,1,1,1,1,1,1,1,1,1,1,1,1,1,1,1,1,1,1,1,1,1,1,1,1,1,1,
1,1,1,1,1,1,1,1,1,1,1,1,1,1,1,1,1,1,1,1,1,1,1,1,1,1,1,1,1,1,1,1,1,1,1,1,
1,1,1,1,1,1,1,1,1,1,1,1,1,1,1,1,1,1,1,1,1,1,1,1,1,1,1,1,1,1,1,1,1,1,1,1,
1,1,1,1,1,1,1,1,1,1,1,1,1,1,1,1,1,1,1,1,1,1,1,1,1,1,1,1,1,1,1,1,1,1,1,1,
1,1,1,1,1,1,1,1,1,1,1,1,1,1,1,1,1,1,1,1,1,1,1,1,1,1,1,1,1,1,1,1,1,1,1,1,
1,1,1,1,1,1,1,1,1,1,1,1,1,1,1,1,1,1,1,1,1,1,1,1,1,1,1,1,1,1,1,1,1,1,1,1,
1,1,1,1,1,1,1,1,1,1,1,1,4),(-0.000330323912087073,0.0826817882439028),(11.6145450452496,
12.6147293662818,13.6142445048086,14.6137596433353,15.6132747818621,16.6127899203889,
17.6123050589156,18.6118201974424,19.6113353359692,20.6108504744959,21.6103656130227,
22.6098807515494,23.6093958900762,24.608911028603,25.6084261671297,26.6079413056565,
27.6074564441833,28.60697158271,29.6064867212368,30.6060018597635,31.6055169982903,
32.6050321368171,33.6045472753438,34.6040624138706,35.6035775523974,36.6030926909241,
37.6026078294509,38.6021229679776,39.6016381065044,40.6011532450312,41.6006683835579,
42.6001835220847,43.5996986606115,44.5992137991382,45.598728937665,46.5982440761917,
47.5977592147185,48.5972743532453,49.596789491772,50.5963046302988,51.5958197688256,
52.5953349073523,53.5948500458791,54.5943651844058,55.5938803229326,56.5933954614594,
57.5929105999861,58.5924257385129,59.5919408770397,60.5914560155664,61.5909711540932,
62.5904862926199,63.5900014311467,64.5895165696735,65.5890317082002,66.588546846727,
67.5880619852538,68.5875771237805,69.5870922623073,70.5866074008341,71.5861225393608,
72.5856376778876,73.5851528164143,74.5846679549411,75.5841830934679,76.5836982319946,
77.5832133705214,78.5827285090482,79.5822436475749,80.5817587861017,81.5812739246284,
82.5807890631552,83.580304201682,84.5798193402087,85.5793344787355,86.5788496172623,
87.578364755789,88.5778798943158,89.5773950328425,90.5769101713693,91.5764253098961,
92.5759404484228,93.5754555869496,94.5749707254764,95.5744858640031,96.5740010025299,
97.5735161410566,98.5730312795834,99.5725464181102,100.572061556637,101.571576695164,
102.57109183369,103.570606972217,104.570122110744,105.569637249271,106.569152387798,
107.568667526324,108.568182664851,109.567697803378,110.567212941905,111.566728080431,
112.566243218958,113.565758357485,114.565273496012,115.564788634538,116.564303773065,
117.563818911592,118.563334050119,119.562849188645,120.562364327172,121.561879465699,
122.561394604226,123.560909742752,124.560424881279,125.559940019806,126.559455158333,
127.55897029686,128.558485435386,129.558000573913,130.55751571244,131.557030850967,
132.556545989493,133.55606112802,134.555576266547,135.555091405074,136.5546065436,
137.554121682127,138.553636820654,139.553151959181,140.552667097707,141.552182236234,
142.551697374761,143.551212513288,144.550727651814,145.550242790341,146.549757928868,
147.549273067395,148.548788205922,149.548303344448,150.547818482975,151.547333621502,
152.546848760029,153.546363898555,154.545879037082,155.545394175609,156.544909314136,
157.544424452662,158.543939591189,159.543454729716,160.542969868243,161.542485006769,
162.542000145296,163.541515283823,164.54103042235,165.540545560876,166.540060699403,
167.53957583793,168.539090976457,169.538606114984,170.53812125351,171.537636392037,
172.537151530564,173.536666669091,174.536181807617,175.535696946144,176.535212084671,
177.534727223198,178.534242361724,179.533757500251,180.533272638778,181.532787777305,
182.532302915831,183.531818054358,184.531333192885,185.530848331412,186.530363469939,
187.529878608465,188.529393746992,189.528908885519,190.528424024046,191.527939162572,
192.527454301099,193.526969439626,194.526484578153,195.525999716679,196.525514855206,
197.525029993733,198.52454513226,199.524060270786,200.523575409313,201.52309054784,
202.522605686367,203.522120824893,204.52163596342,205.521151101947,206.520666240474,
207.520181379001,208.519696517527,209.519211656054,210.518726794581,211.518241933108,
212.517757071634,213.517272210161,214.516787348688,215.516302487215,216.515817625741,
217.515332764268,218.514847902795,219.514363041322,220.513878179848,221.513393318375,
222.512908456902,223.512423595429,224.511938733956,225.511453872482,226.510969011009,
227.510484149536,228.509999288063,229.509514426589,230.509029565116,231.508544703643,
232.50805984217,233.507574980696,234.507090119223,235.50660525775,236.506120396277,
237.505635534803,238.50515067333,239.504665811857,240.504180950384,241.50369608891,
242.503211227437,243.502726365964,244.502241504491,245.501756643018,246.501271781544,
247.500786920071,248.500302058598,249.499817197125,250.499332335651,251.498847474178,
252.498362612705,253.497877751232,254.497392889758,255.496908028285,256.496423166812,
257.495938305339,258.495453443865),.UNSPECIFIED.);
#18935=B_SPLINE_SURFACE_WITH_KNOTS('',3,3,((#91656,#91657,#91658,#91659,
#91660,#91661,#91662,#91663,#91664,#91665,#91666,#91667,#91668,#91669,#91670,
#91671,#91672,#91673),(#91674,#91675,#91676,#91677,#91678,#91679,#91680,
#91681,#91682,#91683,#91684,#91685,#91686,#91687,#91688,#91689,#91690,#91691),
(#91692,#91693,#91694,#91695,#91696,#91697,#91698,#91699,#91700,#91701,
#91702,#91703,#91704,#91705,#91706,#91707,#91708,#91709),(#91710,#91711,
#91712,#91713,#91714,#91715,#91716,#91717,#91718,#91719,#91720,#91721,#91722,
#91723,#91724,#91725,#91726,#91727),(#91728,#91729,#91730,#91731,#91732,
#91733,#91734,#91735,#91736,#91737,#91738,#91739,#91740,#91741,#91742,#91743,
#91744,#91745),(#91746,#91747,#91748,#91749,#91750,#91751,#91752,#91753,
#91754,#91755,#91756,#91757,#91758,#91759,#91760,#91761,#91762,#91763)),
 .UNSPECIFIED.,.F.,.T.,.F.,(4,1,1,4),(4,1,1,1,1,1,1,1,1,1,1,1,1,1,1,4),
(0.,0.285714285714286,0.571428571428571,1.),(0.,0.177176435663881,0.354352871327763,
0.531529306991644,0.708705742655525,0.885882178319406,1.06305861398329,
1.18117623775921,1.29929386153513,1.41741148531105,1.65364673286289,1.77176435663881,
1.94894079230269,2.12611722796658,2.30329366363046,2.48047009929434),
 .UNSPECIFIED.);
#18936=B_SPLINE_SURFACE_WITH_KNOTS('',3,3,((#93381,#93382,#93383,#93384,
#93385,#93386,#93387,#93388,#93389,#93390,#93391,#93392,#93393,#93394,#93395,
#93396,#93397,#93398,#93399,#93400,#93401,#93402,#93403,#93404,#93405,#93406,
#93407,#93408,#93409,#93410,#93411,#93412,#93413,#93414,#93415,#93416,#93417,
#93418,#93419,#93420,#93421,#93422,#93423,#93424,#93425,#93426,#93427,#93428,
#93429,#93430,#93431,#93432,#93433,#93434,#93435,#93436,#93437,#93438,#93439,
#93440,#93441,#93442,#93443,#93444,#93445,#93446,#93447,#93448,#93449,#93450,
#93451,#93452,#93453,#93454,#93455,#93456,#93457,#93458,#93459,#93460,#93461,
#93462,#93463,#93464,#93465,#93466,#93467,#93468,#93469,#93470,#93471,#93472,
#93473,#93474,#93475,#93476,#93477,#93478,#93479,#93480,#93481,#93482,#93483,
#93484,#93485,#93486,#93487,#93488,#93489,#93490),(#93491,#93492,#93493,
#93494,#93495,#93496,#93497,#93498,#93499,#93500,#93501,#93502,#93503,#93504,
#93505,#93506,#93507,#93508,#93509,#93510,#93511,#93512,#93513,#93514,#93515,
#93516,#93517,#93518,#93519,#93520,#93521,#93522,#93523,#93524,#93525,#93526,
#93527,#93528,#93529,#93530,#93531,#93532,#93533,#93534,#93535,#93536,#93537,
#93538,#93539,#93540,#93541,#93542,#93543,#93544,#93545,#93546,#93547,#93548,
#93549,#93550,#93551,#93552,#93553,#93554,#93555,#93556,#93557,#93558,#93559,
#93560,#93561,#93562,#93563,#93564,#93565,#93566,#93567,#93568,#93569,#93570,
#93571,#93572,#93573,#93574,#93575,#93576,#93577,#93578,#93579,#93580,#93581,
#93582,#93583,#93584,#93585,#93586,#93587,#93588,#93589,#93590,#93591,#93592,
#93593,#93594,#93595,#93596,#93597,#93598,#93599,#93600),(#93601,#93602,
#93603,#93604,#93605,#93606,#93607,#93608,#93609,#93610,#93611,#93612,#93613,
#93614,#93615,#93616,#93617,#93618,#93619,#93620,#93621,#93622,#93623,#93624,
#93625,#93626,#93627,#93628,#93629,#93630,#93631,#93632,#93633,#93634,#93635,
#93636,#93637,#93638,#93639,#93640,#93641,#93642,#93643,#93644,#93645,#93646,
#93647,#93648,#93649,#93650,#93651,#93652,#93653,#93654,#93655,#93656,#93657,
#93658,#93659,#93660,#93661,#93662,#93663,#93664,#93665,#93666,#93667,#93668,
#93669,#93670,#93671,#93672,#93673,#93674,#93675,#93676,#93677,#93678,#93679,
#93680,#93681,#93682,#93683,#93684,#93685,#93686,#93687,#93688,#93689,#93690,
#93691,#93692,#93693,#93694,#93695,#93696,#93697,#93698,#93699,#93700,#93701,
#93702,#93703,#93704,#93705,#93706,#93707,#93708,#93709,#93710),(#93711,
#93712,#93713,#93714,#93715,#93716,#93717,#93718,#93719,#93720,#93721,#93722,
#93723,#93724,#93725,#93726,#93727,#93728,#93729,#93730,#93731,#93732,#93733,
#93734,#93735,#93736,#93737,#93738,#93739,#93740,#93741,#93742,#93743,#93744,
#93745,#93746,#93747,#93748,#93749,#93750,#93751,#93752,#93753,#93754,#93755,
#93756,#93757,#93758,#93759,#93760,#93761,#93762,#93763,#93764,#93765,#93766,
#93767,#93768,#93769,#93770,#93771,#93772,#93773,#93774,#93775,#93776,#93777,
#93778,#93779,#93780,#93781,#93782,#93783,#93784,#93785,#93786,#93787,#93788,
#93789,#93790,#93791,#93792,#93793,#93794,#93795,#93796,#93797,#93798,#93799,
#93800,#93801,#93802,#93803,#93804,#93805,#93806,#93807,#93808,#93809,#93810,
#93811,#93812,#93813,#93814,#93815,#93816,#93817,#93818,#93819,#93820),
(#93821,#93822,#93823,#93824,#93825,#93826,#93827,#93828,#93829,#93830,
#93831,#93832,#93833,#93834,#93835,#93836,#93837,#93838,#93839,#93840,#93841,
#93842,#93843,#93844,#93845,#93846,#93847,#93848,#93849,#93850,#93851,#93852,
#93853,#93854,#93855,#93856,#93857,#93858,#93859,#93860,#93861,#93862,#93863,
#93864,#93865,#93866,#93867,#93868,#93869,#93870,#93871,#93872,#93873,#93874,
#93875,#93876,#93877,#93878,#93879,#93880,#93881,#93882,#93883,#93884,#93885,
#93886,#93887,#93888,#93889,#93890,#93891,#93892,#93893,#93894,#93895,#93896,
#93897,#93898,#93899,#93900,#93901,#93902,#93903,#93904,#93905,#93906,#93907,
#93908,#93909,#93910,#93911,#93912,#93913,#93914,#93915,#93916,#93917,#93918,
#93919,#93920,#93921,#93922,#93923,#93924,#93925,#93926,#93927,#93928,#93929,
#93930),(#93931,#93932,#93933,#93934,#93935,#93936,#93937,#93938,#93939,
#93940,#93941,#93942,#93943,#93944,#93945,#93946,#93947,#93948,#93949,#93950,
#93951,#93952,#93953,#93954,#93955,#93956,#93957,#93958,#93959,#93960,#93961,
#93962,#93963,#93964,#93965,#93966,#93967,#93968,#93969,#93970,#93971,#93972,
#93973,#93974,#93975,#93976,#93977,#93978,#93979,#93980,#93981,#93982,#93983,
#93984,#93985,#93986,#93987,#93988,#93989,#93990,#93991,#93992,#93993,#93994,
#93995,#93996,#93997,#93998,#93999,#94000,#94001,#94002,#94003,#94004,#94005,
#94006,#94007,#94008,#94009,#94010,#94011,#94012,#94013,#94014,#94015,#94016,
#94017,#94018,#94019,#94020,#94021,#94022,#94023,#94024,#94025,#94026,#94027,
#94028,#94029,#94030,#94031,#94032,#94033,#94034,#94035,#94036,#94037,#94038,
#94039,#94040),(#94041,#94042,#94043,#94044,#94045,#94046,#94047,#94048,
#94049,#94050,#94051,#94052,#94053,#94054,#94055,#94056,#94057,#94058,#94059,
#94060,#94061,#94062,#94063,#94064,#94065,#94066,#94067,#94068,#94069,#94070,
#94071,#94072,#94073,#94074,#94075,#94076,#94077,#94078,#94079,#94080,#94081,
#94082,#94083,#94084,#94085,#94086,#94087,#94088,#94089,#94090,#94091,#94092,
#94093,#94094,#94095,#94096,#94097,#94098,#94099,#94100,#94101,#94102,#94103,
#94104,#94105,#94106,#94107,#94108,#94109,#94110,#94111,#94112,#94113,#94114,
#94115,#94116,#94117,#94118,#94119,#94120,#94121,#94122,#94123,#94124,#94125,
#94126,#94127,#94128,#94129,#94130,#94131,#94132,#94133,#94134,#94135,#94136,
#94137,#94138,#94139,#94140,#94141,#94142,#94143,#94144,#94145,#94146,#94147,
#94148,#94149,#94150),(#94151,#94152,#94153,#94154,#94155,#94156,#94157,
#94158,#94159,#94160,#94161,#94162,#94163,#94164,#94165,#94166,#94167,#94168,
#94169,#94170,#94171,#94172,#94173,#94174,#94175,#94176,#94177,#94178,#94179,
#94180,#94181,#94182,#94183,#94184,#94185,#94186,#94187,#94188,#94189,#94190,
#94191,#94192,#94193,#94194,#94195,#94196,#94197,#94198,#94199,#94200,#94201,
#94202,#94203,#94204,#94205,#94206,#94207,#94208,#94209,#94210,#94211,#94212,
#94213,#94214,#94215,#94216,#94217,#94218,#94219,#94220,#94221,#94222,#94223,
#94224,#94225,#94226,#94227,#94228,#94229,#94230,#94231,#94232,#94233,#94234,
#94235,#94236,#94237,#94238,#94239,#94240,#94241,#94242,#94243,#94244,#94245,
#94246,#94247,#94248,#94249,#94250,#94251,#94252,#94253,#94254,#94255,#94256,
#94257,#94258,#94259,#94260),(#94261,#94262,#94263,#94264,#94265,#94266,
#94267,#94268,#94269,#94270,#94271,#94272,#94273,#94274,#94275,#94276,#94277,
#94278,#94279,#94280,#94281,#94282,#94283,#94284,#94285,#94286,#94287,#94288,
#94289,#94290,#94291,#94292,#94293,#94294,#94295,#94296,#94297,#94298,#94299,
#94300,#94301,#94302,#94303,#94304,#94305,#94306,#94307,#94308,#94309,#94310,
#94311,#94312,#94313,#94314,#94315,#94316,#94317,#94318,#94319,#94320,#94321,
#94322,#94323,#94324,#94325,#94326,#94327,#94328,#94329,#94330,#94331,#94332,
#94333,#94334,#94335,#94336,#94337,#94338,#94339,#94340,#94341,#94342,#94343,
#94344,#94345,#94346,#94347,#94348,#94349,#94350,#94351,#94352,#94353,#94354,
#94355,#94356,#94357,#94358,#94359,#94360,#94361,#94362,#94363,#94364,#94365,
#94366,#94367,#94368,#94369,#94370),(#94371,#94372,#94373,#94374,#94375,
#94376,#94377,#94378,#94379,#94380,#94381,#94382,#94383,#94384,#94385,#94386,
#94387,#94388,#94389,#94390,#94391,#94392,#94393,#94394,#94395,#94396,#94397,
#94398,#94399,#94400,#94401,#94402,#94403,#94404,#94405,#94406,#94407,#94408,
#94409,#94410,#94411,#94412,#94413,#94414,#94415,#94416,#94417,#94418,#94419,
#94420,#94421,#94422,#94423,#94424,#94425,#94426,#94427,#94428,#94429,#94430,
#94431,#94432,#94433,#94434,#94435,#94436,#94437,#94438,#94439,#94440,#94441,
#94442,#94443,#94444,#94445,#94446,#94447,#94448,#94449,#94450,#94451,#94452,
#94453,#94454,#94455,#94456,#94457,#94458,#94459,#94460,#94461,#94462,#94463,
#94464,#94465,#94466,#94467,#94468,#94469,#94470,#94471,#94472,#94473,#94474,
#94475,#94476,#94477,#94478,#94479,#94480)),.UNSPECIFIED.,.F.,.F.,.F.,(4,
1,1,1,1,1,1,4),(4,1,1,1,1,1,1,1,1,1,1,1,1,1,1,1,1,1,1,1,1,1,1,1,1,1,1,1,
1,1,1,1,1,1,1,1,1,1,1,1,1,1,1,1,1,1,1,1,1,1,1,1,1,1,1,1,1,1,1,1,1,1,1,1,
1,1,1,1,1,1,1,1,1,1,1,1,1,1,1,1,1,1,1,1,1,1,1,1,1,1,1,1,1,1,1,1,1,1,1,1,
1,1,1,1,1,1,1,4),(-2.15967935518058,-1.67714812064519,-1.20351419577799,
-0.729880270910797,-0.2562463460436,0.217387578823596,0.691021503690793,
1.17374330931374),(-0.00388260537544204,0.00892857142857143,0.0178571428571429,
0.0267857142857143,0.0357142857142857,0.0446428571428571,0.0535714285714286,
0.0625,0.0714285714285714,0.0803571428571428,0.0892857142857143,0.0982142857142857,
0.107142857142857,0.116071428571429,0.125,0.133928571428571,0.142857142857143,
0.154761904761905,0.166666666666667,0.178571428571429,0.19047619047619,
0.202380952380952,0.214285714285714,0.222222222222222,0.23015873015873,
0.238095238095238,0.25,0.261904761904762,0.273809523809524,0.285714285714286,
0.297619047619048,0.30952380952381,0.321428571428571,0.333333333333333,
0.341269841269841,0.349206349206349,0.357142857142857,0.365079365079365,
0.375661375661376,0.380952380952381,0.388888888888889,0.396825396825397,
0.404761904761905,0.416666666666667,0.428571428571429,0.43452380952381,
0.44047619047619,0.452380952380952,0.46031746031746,0.468253968253968,0.476190476190476,
0.481481481481481,0.492063492063492,0.5,0.507936507936508,0.515873015873016,
0.523809523809524,0.535714285714286,0.547619047619048,0.55952380952381,
0.571428571428571,0.583333333333333,0.595238095238095,0.607142857142857,
0.619047619047619,0.626984126984127,0.634920634920635,0.642857142857143,
0.650793650793651,0.658730158730159,0.666666666666667,0.674603174603175,
0.682539682539683,0.69047619047619,0.702380952380952,0.708333333333333,
0.714285714285714,0.723214285714286,0.732142857142857,0.741071428571428,
0.75,0.761904761904762,0.773809523809524,0.785714285714286,0.794642857142857,
0.803571428571428,0.8125,0.821428571428571,0.830357142857143,0.839285714285714,
0.848214285714286,0.857142857142857,0.866071428571429,0.875,0.883928571428571,
0.892857142857143,0.901785714285714,0.910714285714286,0.919642857142857,
0.928571428571429,0.9375,0.946428571428571,0.955357142857143,0.964285714285714,
0.973214285714286,0.982142857142857,0.991071428571429,1.00388260537544),
 .UNSPECIFIED.);
#18937=B_SPLINE_SURFACE_WITH_KNOTS('',3,3,((#96921,#96922,#96923,#96924,
#96925,#96926,#96927,#96928,#96929,#96930,#96931,#96932,#96933,#96934,#96935,
#96936,#96937,#96938,#96939,#96940,#96941,#96942,#96943,#96944,#96945,#96946,
#96947,#96948,#96949,#96950,#96951,#96952,#96953,#96954,#96955,#96956,#96957,
#96958,#96959,#96960,#96961,#96962,#96963,#96964,#96965,#96966,#96967,#96968,
#96969,#96970,#96971,#96972,#96973,#96974,#96975,#96976,#96977,#96978,#96979,
#96980,#96981,#96982,#96983,#96984,#96985,#96986,#96987,#96988,#96989,#96990,
#96991,#96992,#96993,#96994,#96995,#96996,#96997,#96998,#96999,#97000,#97001,
#97002,#97003,#97004,#97005,#97006,#97007,#97008,#97009,#97010,#97011,#97012,
#97013,#97014,#97015,#97016,#97017,#97018,#97019,#97020,#97021,#97022,#97023,
#97024,#97025,#97026,#97027),(#97028,#97029,#97030,#97031,#97032,#97033,
#97034,#97035,#97036,#97037,#97038,#97039,#97040,#97041,#97042,#97043,#97044,
#97045,#97046,#97047,#97048,#97049,#97050,#97051,#97052,#97053,#97054,#97055,
#97056,#97057,#97058,#97059,#97060,#97061,#97062,#97063,#97064,#97065,#97066,
#97067,#97068,#97069,#97070,#97071,#97072,#97073,#97074,#97075,#97076,#97077,
#97078,#97079,#97080,#97081,#97082,#97083,#97084,#97085,#97086,#97087,#97088,
#97089,#97090,#97091,#97092,#97093,#97094,#97095,#97096,#97097,#97098,#97099,
#97100,#97101,#97102,#97103,#97104,#97105,#97106,#97107,#97108,#97109,#97110,
#97111,#97112,#97113,#97114,#97115,#97116,#97117,#97118,#97119,#97120,#97121,
#97122,#97123,#97124,#97125,#97126,#97127,#97128,#97129,#97130,#97131,#97132,
#97133,#97134),(#97135,#97136,#97137,#97138,#97139,#97140,#97141,#97142,
#97143,#97144,#97145,#97146,#97147,#97148,#97149,#97150,#97151,#97152,#97153,
#97154,#97155,#97156,#97157,#97158,#97159,#97160,#97161,#97162,#97163,#97164,
#97165,#97166,#97167,#97168,#97169,#97170,#97171,#97172,#97173,#97174,#97175,
#97176,#97177,#97178,#97179,#97180,#97181,#97182,#97183,#97184,#97185,#97186,
#97187,#97188,#97189,#97190,#97191,#97192,#97193,#97194,#97195,#97196,#97197,
#97198,#97199,#97200,#97201,#97202,#97203,#97204,#97205,#97206,#97207,#97208,
#97209,#97210,#97211,#97212,#97213,#97214,#97215,#97216,#97217,#97218,#97219,
#97220,#97221,#97222,#97223,#97224,#97225,#97226,#97227,#97228,#97229,#97230,
#97231,#97232,#97233,#97234,#97235,#97236,#97237,#97238,#97239,#97240,#97241),
(#97242,#97243,#97244,#97245,#97246,#97247,#97248,#97249,#97250,#97251,
#97252,#97253,#97254,#97255,#97256,#97257,#97258,#97259,#97260,#97261,#97262,
#97263,#97264,#97265,#97266,#97267,#97268,#97269,#97270,#97271,#97272,#97273,
#97274,#97275,#97276,#97277,#97278,#97279,#97280,#97281,#97282,#97283,#97284,
#97285,#97286,#97287,#97288,#97289,#97290,#97291,#97292,#97293,#97294,#97295,
#97296,#97297,#97298,#97299,#97300,#97301,#97302,#97303,#97304,#97305,#97306,
#97307,#97308,#97309,#97310,#97311,#97312,#97313,#97314,#97315,#97316,#97317,
#97318,#97319,#97320,#97321,#97322,#97323,#97324,#97325,#97326,#97327,#97328,
#97329,#97330,#97331,#97332,#97333,#97334,#97335,#97336,#97337,#97338,#97339,
#97340,#97341,#97342,#97343,#97344,#97345,#97346,#97347,#97348),(#97349,
#97350,#97351,#97352,#97353,#97354,#97355,#97356,#97357,#97358,#97359,#97360,
#97361,#97362,#97363,#97364,#97365,#97366,#97367,#97368,#97369,#97370,#97371,
#97372,#97373,#97374,#97375,#97376,#97377,#97378,#97379,#97380,#97381,#97382,
#97383,#97384,#97385,#97386,#97387,#97388,#97389,#97390,#97391,#97392,#97393,
#97394,#97395,#97396,#97397,#97398,#97399,#97400,#97401,#97402,#97403,#97404,
#97405,#97406,#97407,#97408,#97409,#97410,#97411,#97412,#97413,#97414,#97415,
#97416,#97417,#97418,#97419,#97420,#97421,#97422,#97423,#97424,#97425,#97426,
#97427,#97428,#97429,#97430,#97431,#97432,#97433,#97434,#97435,#97436,#97437,
#97438,#97439,#97440,#97441,#97442,#97443,#97444,#97445,#97446,#97447,#97448,
#97449,#97450,#97451,#97452,#97453,#97454,#97455),(#97456,#97457,#97458,
#97459,#97460,#97461,#97462,#97463,#97464,#97465,#97466,#97467,#97468,#97469,
#97470,#97471,#97472,#97473,#97474,#97475,#97476,#97477,#97478,#97479,#97480,
#97481,#97482,#97483,#97484,#97485,#97486,#97487,#97488,#97489,#97490,#97491,
#97492,#97493,#97494,#97495,#97496,#97497,#97498,#97499,#97500,#97501,#97502,
#97503,#97504,#97505,#97506,#97507,#97508,#97509,#97510,#97511,#97512,#97513,
#97514,#97515,#97516,#97517,#97518,#97519,#97520,#97521,#97522,#97523,#97524,
#97525,#97526,#97527,#97528,#97529,#97530,#97531,#97532,#97533,#97534,#97535,
#97536,#97537,#97538,#97539,#97540,#97541,#97542,#97543,#97544,#97545,#97546,
#97547,#97548,#97549,#97550,#97551,#97552,#97553,#97554,#97555,#97556,#97557,
#97558,#97559,#97560,#97561,#97562),(#97563,#97564,#97565,#97566,#97567,
#97568,#97569,#97570,#97571,#97572,#97573,#97574,#97575,#97576,#97577,#97578,
#97579,#97580,#97581,#97582,#97583,#97584,#97585,#97586,#97587,#97588,#97589,
#97590,#97591,#97592,#97593,#97594,#97595,#97596,#97597,#97598,#97599,#97600,
#97601,#97602,#97603,#97604,#97605,#97606,#97607,#97608,#97609,#97610,#97611,
#97612,#97613,#97614,#97615,#97616,#97617,#97618,#97619,#97620,#97621,#97622,
#97623,#97624,#97625,#97626,#97627,#97628,#97629,#97630,#97631,#97632,#97633,
#97634,#97635,#97636,#97637,#97638,#97639,#97640,#97641,#97642,#97643,#97644,
#97645,#97646,#97647,#97648,#97649,#97650,#97651,#97652,#97653,#97654,#97655,
#97656,#97657,#97658,#97659,#97660,#97661,#97662,#97663,#97664,#97665,#97666,
#97667,#97668,#97669)),.UNSPECIFIED.,.F.,.F.,.F.,(4,1,1,1,4),(4,1,1,1,1,
1,1,1,1,1,1,1,1,1,1,1,1,1,1,1,1,1,1,1,1,1,1,1,1,1,1,1,1,1,1,1,1,1,1,1,1,
1,1,1,1,1,1,1,1,1,1,1,1,1,1,1,1,1,1,1,1,1,1,1,1,1,1,1,1,1,1,1,1,1,1,1,1,
1,1,1,1,1,1,1,1,1,1,1,1,1,1,1,1,1,1,1,1,1,1,1,1,1,1,1,4),(1.16465542855799,
1.80060139279568,2.43654735703337,3.28447530935028,4.1324032616672),(0.,
0.00892857142857143,0.0178571428571429,0.0267857142857143,0.0357142857142857,
0.0446428571428571,0.0535714285714286,0.0625,0.0714285714285714,0.0803571428571428,
0.0892857142857143,0.0982142857142857,0.107142857142857,0.116071428571429,
0.125,0.133928571428571,0.142857142857143,0.154761904761905,0.166666666666667,
0.178571428571429,0.19047619047619,0.202380952380952,0.214285714285714,
0.222222222222222,0.23015873015873,0.238095238095238,0.25,0.261904761904762,
0.273809523809524,0.285714285714286,0.297619047619048,0.30952380952381,
0.321428571428571,0.327380952380952,0.333333333333333,0.345238095238095,
0.357142857142857,0.369047619047619,0.380952380952381,0.392857142857143,
0.404761904761905,0.416666666666667,0.422619047619048,0.428571428571429,
0.44047619047619,0.452380952380952,0.46031746031746,0.468253968253968,0.476190476190476,
0.481481481481481,0.492063492063492,0.5,0.507936507936508,0.515873015873016,
0.523809523809524,0.535714285714286,0.547619047619048,0.55952380952381,
0.571428571428571,0.583333333333333,0.595238095238095,0.607142857142857,
0.619047619047619,0.626984126984127,0.634920634920635,0.642857142857143,
0.650793650793651,0.658730158730159,0.666666666666667,0.672619047619048,
0.678571428571429,0.69047619047619,0.702380952380952,0.714285714285714,
0.726190476190476,0.738095238095238,0.746031746031746,0.753968253968254,
0.761904761904762,0.76984126984127,0.777777777777778,0.785714285714286,
0.793650793650794,0.801587301587302,0.809523809523809,0.821428571428571,
0.833333333333333,0.845238095238095,0.857142857142857,0.866071428571429,
0.875,0.883928571428571,0.892857142857143,0.901785714285714,0.910714285714286,
0.919642857142857,0.928571428571429,0.9375,0.946428571428571,0.955357142857143,
0.964285714285714,0.973214285714286,0.982142857142857,0.991071428571429,
1.),.UNSPECIFIED.);
#18938=B_SPLINE_SURFACE_WITH_KNOTS('',3,3,((#97942,#97943,#97944,#97945,
#97946,#97947,#97948,#97949,#97950,#97951,#97952,#97953,#97954,#97955,#97956,
#97957,#97958,#97959,#97960,#97961,#97962,#97963,#97964,#97965,#97966,#97967,
#97968,#97969),(#97970,#97971,#97972,#97973,#97974,#97975,#97976,#97977,
#97978,#97979,#97980,#97981,#97982,#97983,#97984,#97985,#97986,#97987,#97988,
#97989,#97990,#97991,#97992,#97993,#97994,#97995,#97996,#97997),(#97998,
#97999,#98000,#98001,#98002,#98003,#98004,#98005,#98006,#98007,#98008,#98009,
#98010,#98011,#98012,#98013,#98014,#98015,#98016,#98017,#98018,#98019,#98020,
#98021,#98022,#98023,#98024,#98025),(#98026,#98027,#98028,#98029,#98030,
#98031,#98032,#98033,#98034,#98035,#98036,#98037,#98038,#98039,#98040,#98041,
#98042,#98043,#98044,#98045,#98046,#98047,#98048,#98049,#98050,#98051,#98052,
#98053),(#98054,#98055,#98056,#98057,#98058,#98059,#98060,#98061,#98062,
#98063,#98064,#98065,#98066,#98067,#98068,#98069,#98070,#98071,#98072,#98073,
#98074,#98075,#98076,#98077,#98078,#98079,#98080,#98081)),.UNSPECIFIED.,
 .F.,.F.,.F.,(4,1,4),(4,1,1,1,1,1,1,1,1,1,1,1,1,1,1,1,1,1,1,1,1,1,1,1,1,
4),(0.,0.5,1.),(3.41679525229117E-14,0.241483590676928,0.482967181353822,
0.96593436270761,1.2074179533845,1.4489015440614,1.69038513473829,1.81112693007674,
1.87149782774596,1.90168327658057,1.93186872541519,2.05261052075363,2.11298141842286,
2.17335231609208,2.2337232137613,2.29409411143053,2.35446500909975,2.41483590676897,
2.53557770210742,2.65631949744587,2.77706129278432,2.89780308812276,3.01854488346121,
3.13928667879966,3.2600284741381,3.38077026947655),.UNSPECIFIED.);
#18939=B_SPLINE_SURFACE_WITH_KNOTS('',5,1,((#98112,#98113),(#98114,#98115),
(#98116,#98117),(#98118,#98119),(#98120,#98121),(#98122,#98123),(#98124,
#98125),(#98126,#98127),(#98128,#98129),(#98130,#98131),(#98132,#98133),
(#98134,#98135),(#98136,#98137),(#98138,#98139),(#98140,#98141),(#98142,
#98143),(#98144,#98145),(#98146,#98147),(#98148,#98149),(#98150,#98151),
(#98152,#98153),(#98154,#98155),(#98156,#98157),(#98158,#98159),(#98160,
#98161),(#98162,#98163),(#98164,#98165),(#98166,#98167),(#98168,#98169),
(#98170,#98171),(#98172,#98173),(#98174,#98175),(#98176,#98177),(#98178,
#98179),(#98180,#98181),(#98182,#98183),(#98184,#98185),(#98186,#98187),
(#98188,#98189),(#98190,#98191),(#98192,#98193),(#98194,#98195),(#98196,
#98197),(#98198,#98199),(#98200,#98201),(#98202,#98203),(#98204,#98205),
(#98206,#98207),(#98208,#98209),(#98210,#98211),(#98212,#98213),(#98214,
#98215),(#98216,#98217),(#98218,#98219),(#98220,#98221),(#98222,#98223),
(#98224,#98225),(#98226,#98227),(#98228,#98229),(#98230,#98231),(#98232,
#98233),(#98234,#98235),(#98236,#98237),(#98238,#98239),(#98240,#98241),
(#98242,#98243),(#98244,#98245),(#98246,#98247),(#98248,#98249),(#98250,
#98251)),.UNSPECIFIED.,.F.,.F.,.F.,(6,1,1,1,1,1,1,1,1,1,1,1,1,1,1,1,1,1,
1,1,1,1,1,1,1,1,1,1,1,1,1,1,1,1,1,1,1,1,1,1,1,1,1,1,1,1,1,1,1,1,1,1,1,1,
1,1,1,1,1,1,1,1,1,1,1,6),(2,2),(0.,0.0153846153846154,0.0307692307692308,
0.0461538461538462,0.0615384615384615,0.0769230769230769,0.0923076923076923,
0.107692307692308,0.123076923076923,0.138461538461538,0.153846153846154,
0.169230769230769,0.184615384615385,0.2,0.215384615384615,0.230769230769231,
0.246153846153846,0.261538461538462,0.276923076923077,0.292307692307692,
0.307692307692308,0.323076923076923,0.338461538461538,0.353846153846154,
0.369230769230769,0.384615384615385,0.4,0.415384615384615,0.430769230769231,
0.446153846153846,0.461538461538462,0.476923076923077,0.492307692307692,
0.507692307692308,0.523076923076923,0.538461538461538,0.553846153846154,
0.569230769230769,0.584615384615384,0.6,0.615384615384615,0.63076923076923,
0.646153846153846,0.661538461538461,0.676923076923076,0.692307692307692,
0.707692307692307,0.723076923076922,0.738461538461538,0.753846153846153,
0.769230769230768,0.784615384615384,0.799999999999999,0.815384615384614,
0.83076923076923,0.846153846153845,0.86153846153846,0.876923076923076,0.892307692307691,
0.907692307692306,0.923076923076922,0.938461538461537,0.953846153846152,
0.969230769230768,0.984615384615383,1.),(0.,1.4688),.UNSPECIFIED.);
#18940=B_SPLINE_SURFACE_WITH_KNOTS('',3,3,((#98351,#98352,#98353,#98354,
#98355,#98356,#98357,#98358,#98359,#98360,#98361,#98362,#98363,#98364,#98365,
#98366,#98367,#98368,#98369,#98370,#98371,#98372,#98373,#98374,#98375,#98376,
#98377),(#98378,#98379,#98380,#98381,#98382,#98383,#98384,#98385,#98386,
#98387,#98388,#98389,#98390,#98391,#98392,#98393,#98394,#98395,#98396,#98397,
#98398,#98399,#98400,#98401,#98402,#98403,#98404),(#98405,#98406,#98407,
#98408,#98409,#98410,#98411,#98412,#98413,#98414,#98415,#98416,#98417,#98418,
#98419,#98420,#98421,#98422,#98423,#98424,#98425,#98426,#98427,#98428,#98429,
#98430,#98431),(#98432,#98433,#98434,#98435,#98436,#98437,#98438,#98439,
#98440,#98441,#98442,#98443,#98444,#98445,#98446,#98447,#98448,#98449,#98450,
#98451,#98452,#98453,#98454,#98455,#98456,#98457,#98458),(#98459,#98460,
#98461,#98462,#98463,#98464,#98465,#98466,#98467,#98468,#98469,#98470,#98471,
#98472,#98473,#98474,#98475,#98476,#98477,#98478,#98479,#98480,#98481,#98482,
#98483,#98484,#98485)),.UNSPECIFIED.,.F.,.F.,.F.,(4,1,4),(4,1,1,1,1,1,1,
1,1,1,1,1,1,1,1,1,1,1,1,1,1,1,1,1,4),(0.,0.5,1.),(0.00128107289438891,0.0623100798183742,
0.12333908674236,0.24539710059033,0.367455114438301,0.489513128286272,0.611571142134242,
0.733629155982213,0.855687169830184,0.977745183678154,1.03877419060214,
1.09980319752612,1.16083220445011,1.1913467079121,1.2218612113741,1.34391922522207,
1.46597723907004,1.71009326676598,1.83215128061395,1.95420929446192,2.19832532215786,
2.4424413498538,2.93067340524569,3.17478943294163,3.41890546063757),
 .UNSPECIFIED.);
#18941=B_SPLINE_SURFACE_WITH_KNOTS('',3,3,((#98561,#98562,#98563,#98564,
#98565,#98566,#98567,#98568,#98569,#98570,#98571,#98572,#98573,#98574,#98575,
#98576,#98577,#98578,#98579,#98580,#98581,#98582,#98583,#98584,#98585,#98586,
#98587,#98588,#98589),(#98590,#98591,#98592,#98593,#98594,#98595,#98596,
#98597,#98598,#98599,#98600,#98601,#98602,#98603,#98604,#98605,#98606,#98607,
#98608,#98609,#98610,#98611,#98612,#98613,#98614,#98615,#98616,#98617,#98618),
(#98619,#98620,#98621,#98622,#98623,#98624,#98625,#98626,#98627,#98628,
#98629,#98630,#98631,#98632,#98633,#98634,#98635,#98636,#98637,#98638,#98639,
#98640,#98641,#98642,#98643,#98644,#98645,#98646,#98647),(#98648,#98649,
#98650,#98651,#98652,#98653,#98654,#98655,#98656,#98657,#98658,#98659,#98660,
#98661,#98662,#98663,#98664,#98665,#98666,#98667,#98668,#98669,#98670,#98671,
#98672,#98673,#98674,#98675,#98676),(#98677,#98678,#98679,#98680,#98681,
#98682,#98683,#98684,#98685,#98686,#98687,#98688,#98689,#98690,#98691,#98692,
#98693,#98694,#98695,#98696,#98697,#98698,#98699,#98700,#98701,#98702,#98703,
#98704,#98705)),.UNSPECIFIED.,.F.,.F.,.F.,(4,1,4),(4,1,1,1,1,1,1,1,1,1,
1,1,1,1,1,1,1,1,1,1,1,1,1,1,1,1,4),(0.,0.5,1.),(0.,0.244116027696041,0.488232055392083,
0.976464110784166,1.22058013848021,1.46469616617625,1.70881219387229,1.83087020772031,
1.89189921464432,1.95292822156833,2.07498623541635,2.13601524234036,2.19704424926437,
2.25807325618838,2.28858775965039,2.31910226311239,2.3801312700364,2.44116027696041,
2.56321829080843,2.68527630465646,2.80733431850448,2.9293923323525,3.05145034620052,
3.17350836004854,3.29556637389656,3.35659538082057,3.41762438774458),
 .UNSPECIFIED.);
#18942=B_SPLINE_SURFACE_WITH_KNOTS('',5,1,((#98737,#98738),(#98739,#98740),
(#98741,#98742),(#98743,#98744),(#98745,#98746),(#98747,#98748),(#98749,
#98750),(#98751,#98752),(#98753,#98754),(#98755,#98756),(#98757,#98758),
(#98759,#98760),(#98761,#98762),(#98763,#98764),(#98765,#98766),(#98767,
#98768),(#98769,#98770),(#98771,#98772),(#98773,#98774),(#98775,#98776),
(#98777,#98778),(#98779,#98780),(#98781,#98782),(#98783,#98784),(#98785,
#98786),(#98787,#98788),(#98789,#98790),(#98791,#98792),(#98793,#98794),
(#98795,#98796),(#98797,#98798),(#98799,#98800),(#98801,#98802),(#98803,
#98804),(#98805,#98806),(#98807,#98808),(#98809,#98810),(#98811,#98812),
(#98813,#98814),(#98815,#98816),(#98817,#98818),(#98819,#98820),(#98821,
#98822),(#98823,#98824),(#98825,#98826),(#98827,#98828),(#98829,#98830),
(#98831,#98832),(#98833,#98834),(#98835,#98836),(#98837,#98838),(#98839,
#98840),(#98841,#98842),(#98843,#98844),(#98845,#98846),(#98847,#98848),
(#98849,#98850),(#98851,#98852),(#98853,#98854),(#98855,#98856),(#98857,
#98858),(#98859,#98860),(#98861,#98862),(#98863,#98864),(#98865,#98866),
(#98867,#98868),(#98869,#98870),(#98871,#98872),(#98873,#98874),(#98875,
#98876)),.UNSPECIFIED.,.F.,.F.,.F.,(6,1,1,1,1,1,1,1,1,1,1,1,1,1,1,1,1,1,
1,1,1,1,1,1,1,1,1,1,1,1,1,1,1,1,1,1,1,1,1,1,1,1,1,1,1,1,1,1,1,1,1,1,1,1,
1,1,1,1,1,1,1,1,1,1,1,6),(2,2),(0.,0.0153846153846154,0.0307692307692308,
0.0461538461538462,0.0615384615384615,0.0769230769230769,0.0923076923076923,
0.107692307692308,0.123076923076923,0.138461538461538,0.153846153846154,
0.169230769230769,0.184615384615385,0.2,0.215384615384615,0.230769230769231,
0.246153846153846,0.261538461538462,0.276923076923077,0.292307692307692,
0.307692307692308,0.323076923076923,0.338461538461538,0.353846153846154,
0.369230769230769,0.384615384615385,0.4,0.415384615384615,0.430769230769231,
0.446153846153846,0.461538461538462,0.476923076923077,0.492307692307692,
0.507692307692308,0.523076923076923,0.538461538461538,0.553846153846154,
0.569230769230769,0.584615384615384,0.6,0.615384615384615,0.63076923076923,
0.646153846153846,0.661538461538461,0.676923076923076,0.692307692307692,
0.707692307692307,0.723076923076922,0.738461538461538,0.753846153846153,
0.769230769230768,0.784615384615384,0.799999999999999,0.815384615384614,
0.83076923076923,0.846153846153845,0.86153846153846,0.876923076923076,0.892307692307691,
0.907692307692306,0.923076923076922,0.938461538461537,0.953846153846152,
0.969230769230768,0.984615384615383,1.),(0.,1.4688),.UNSPECIFIED.);
#18943=B_SPLINE_SURFACE_WITH_KNOTS('',3,3,((#98984,#98985,#98986,#98987,
#98988,#98989,#98990,#98991,#98992,#98993,#98994,#98995,#98996,#98997,#98998,
#98999,#99000,#99001,#99002,#99003,#99004,#99005,#99006,#99007,#99008,#99009),
(#99010,#99011,#99012,#99013,#99014,#99015,#99016,#99017,#99018,#99019,
#99020,#99021,#99022,#99023,#99024,#99025,#99026,#99027,#99028,#99029,#99030,
#99031,#99032,#99033,#99034,#99035),(#99036,#99037,#99038,#99039,#99040,
#99041,#99042,#99043,#99044,#99045,#99046,#99047,#99048,#99049,#99050,#99051,
#99052,#99053,#99054,#99055,#99056,#99057,#99058,#99059,#99060,#99061),
(#99062,#99063,#99064,#99065,#99066,#99067,#99068,#99069,#99070,#99071,
#99072,#99073,#99074,#99075,#99076,#99077,#99078,#99079,#99080,#99081,#99082,
#99083,#99084,#99085,#99086,#99087),(#99088,#99089,#99090,#99091,#99092,
#99093,#99094,#99095,#99096,#99097,#99098,#99099,#99100,#99101,#99102,#99103,
#99104,#99105,#99106,#99107,#99108,#99109,#99110,#99111,#99112,#99113)),
 .UNSPECIFIED.,.F.,.F.,.F.,(4,1,4),(4,1,1,1,1,1,1,1,1,1,1,1,1,1,1,1,1,1,
1,1,1,1,1,4),(0.,0.5,1.),(0.00128110943246098,0.1220229047709,0.242764700109339,
0.363506495447778,0.484248290786216,0.604990086124655,0.725731881463094,
0.846473676801533,0.906844574470752,0.967215472139972,1.02758636980919,
1.08795726747841,1.14832816514763,1.20869906281685,1.26906996048607,1.32944085815529,
1.45018265349373,1.6916662441706,1.93314983484748,2.17463342552436,2.41611701620124,
2.89908419755499,3.14056778823187,3.38205137890875),.UNSPECIFIED.);
#18944=B_SPLINE_SURFACE_WITH_KNOTS('',3,3,((#99115,#99116,#99117,#99118),
(#99119,#99120,#99121,#99122),(#99123,#99124,#99125,#99126),(#99127,#99128,
#99129,#99130),(#99131,#99132,#99133,#99134)),.UNSPECIFIED.,.F.,.F.,.F.,
(4,1,4),(4,4),(0.,0.5,1.),(0.,0.0900415523927057),.UNSPECIFIED.);
#18945=B_SPLINE_SURFACE_WITH_KNOTS('',3,3,((#99141,#99142,#99143,#99144),
(#99145,#99146,#99147,#99148),(#99149,#99150,#99151,#99152),(#99153,#99154,
#99155,#99156),(#99157,#99158,#99159,#99160)),.UNSPECIFIED.,.F.,.F.,.F.,
(4,1,4),(4,4),(0.,0.5,1.00033317135741),(-0.000333171357409007,0.325047276078282),
 .UNSPECIFIED.);
#18946=B_SPLINE_SURFACE_WITH_KNOTS('',3,3,((#99167,#99168,#99169,#99170),
(#99171,#99172,#99173,#99174),(#99175,#99176,#99177,#99178),(#99179,#99180,
#99181,#99182),(#99183,#99184,#99185,#99186)),.UNSPECIFIED.,.F.,.F.,.F.,
(4,1,4),(4,4),(0.,0.5,1.),(0.,0.0523713743724485),.UNSPECIFIED.);
#18947=B_SPLINE_SURFACE_WITH_KNOTS('',3,3,((#99193,#99194,#99195,#99196,
#99197,#99198),(#99199,#99200,#99201,#99202,#99203,#99204),(#99205,#99206,
#99207,#99208,#99209,#99210),(#99211,#99212,#99213,#99214,#99215,#99216),
(#99217,#99218,#99219,#99220,#99221,#99222)),.UNSPECIFIED.,.F.,.F.,.F.,
(4,1,4),(4,2,4),(0.,0.5,1.),(1.22307313571325E-14,0.0771338280521436,0.0784358874721452),
 .UNSPECIFIED.);
#18948=B_SPLINE_SURFACE_WITH_KNOTS('',3,3,((#99278,#99279,#99280,#99281),
(#99282,#99283,#99284,#99285),(#99286,#99287,#99288,#99289),(#99290,#99291,
#99292,#99293),(#99294,#99295,#99296,#99297)),.UNSPECIFIED.,.F.,.F.,.F.,
(4,1,4),(4,4),(0.,0.5,1.),(0.,0.0523726503223924),.UNSPECIFIED.);
#18949=B_SPLINE_SURFACE_WITH_KNOTS('',3,3,((#99306,#99307,#99308,#99309,
#99310,#99311),(#99312,#99313,#99314,#99315,#99316,#99317),(#99318,#99319,
#99320,#99321,#99322,#99323),(#99324,#99325,#99326,#99327,#99328,#99329),
(#99330,#99331,#99332,#99333,#99334,#99335)),.UNSPECIFIED.,.F.,.F.,.F.,
(4,1,4),(4,2,4),(0.,0.5,1.),(-0.00130205941990691,0.,0.0771338280522776),
 .UNSPECIFIED.);
#18950=B_SPLINE_SURFACE_WITH_KNOTS('',3,3,((#99342,#99343,#99344,#99345),
(#99346,#99347,#99348,#99349),(#99350,#99351,#99352,#99353),(#99354,#99355,
#99356,#99357),(#99358,#99359,#99360,#99361)),.UNSPECIFIED.,.F.,.F.,.F.,
(4,1,4),(4,4),(0.,0.5,1.00033317136049),(-0.000333171360490094,0.325047276081303),
 .UNSPECIFIED.);
#18951=B_SPLINE_SURFACE_WITH_KNOTS('',3,3,((#99368,#99369,#99370,#99371),
(#99372,#99373,#99374,#99375),(#99376,#99377,#99378,#99379),(#99380,#99381,
#99382,#99383),(#99384,#99385,#99386,#99387)),.UNSPECIFIED.,.F.,.F.,.F.,
(4,1,4),(4,4),(0.,0.5,1.),(0.,0.0900393973869889),.UNSPECIFIED.);
#18952=B_SPLINE_SURFACE_WITH_KNOTS('',3,3,((#99457,#99458,#99459,#99460),
(#99461,#99462,#99463,#99464),(#99465,#99466,#99467,#99468),(#99469,#99470,
#99471,#99472),(#99473,#99474,#99475,#99476)),.UNSPECIFIED.,.F.,.F.,.F.,
(4,1,4),(4,4),(0.,0.5,1.),(0.,0.324683822128034),.UNSPECIFIED.);
#18953=B_SPLINE_SURFACE_WITH_KNOTS('',3,3,((#99484,#99485,#99486,#99487),
(#99488,#99489,#99490,#99491),(#99492,#99493,#99494,#99495),(#99496,#99497,
#99498,#99499),(#99500,#99501,#99502,#99503)),.UNSPECIFIED.,.F.,.F.,.F.,
(4,1,4),(4,4),(-4.89933240562015E-5,0.309230284442149,0.721537330365014),
(-4.89933240562015E-5,0.0862352312336272),.UNSPECIFIED.);
#18954=B_SPLINE_SURFACE_WITH_KNOTS('',3,3,((#99505,#99506,#99507,#99508),
(#99509,#99510,#99511,#99512),(#99513,#99514,#99515,#99516),(#99517,#99518,
#99519,#99520)),.UNSPECIFIED.,.F.,.F.,.F.,(4,4),(4,4),(0.640913278958594,
1.),(3.45512125000871E-14,0.0441554944102273),.UNSPECIFIED.);
#18955=B_SPLINE_SURFACE_WITH_KNOTS('',3,3,((#99521,#99522,#99523,#99524),
(#99525,#99526,#99527,#99528),(#99529,#99530,#99531,#99532),(#99533,#99534,
#99535,#99536),(#99537,#99538,#99539,#99540)),.UNSPECIFIED.,.F.,.F.,.F.,
(4,1,4),(4,4),(-4.01713313415748E-5,0.5,1.),(-4.01713313414375E-5,0.0546115211509691),
 .UNSPECIFIED.);
#18956=B_SPLINE_SURFACE_WITH_KNOTS('',3,3,((#99552,#99553,#99554,#99555),
(#99556,#99557,#99558,#99559),(#99560,#99561,#99562,#99563),(#99564,#99565,
#99566,#99567),(#99568,#99569,#99570,#99571)),.UNSPECIFIED.,.F.,.F.,.F.,
(4,1,4),(4,4),(0.,0.5,1.),(0.,0.324683822128098),.UNSPECIFIED.);
#18957=B_SPLINE_SURFACE_WITH_KNOTS('',3,3,((#99578,#99579,#99580,#99581),
(#99582,#99583,#99584,#99585),(#99586,#99587,#99588,#99589),(#99590,#99591,
#99592,#99593),(#99594,#99595,#99596,#99597)),.UNSPECIFIED.,.F.,.F.,.F.,
(4,1,4),(4,4),(-4.017133134979E-5,0.5,1.),(-4.01713313514047E-5,0.0546115211509732),
 .UNSPECIFIED.);
#18958=B_SPLINE_SURFACE_WITH_KNOTS('',3,3,((#99598,#99599,#99600,#99601),
(#99602,#99603,#99604,#99605),(#99606,#99607,#99608,#99609),(#99610,#99611,
#99612,#99613),(#99614,#99615,#99616,#99617)),.UNSPECIFIED.,.F.,.F.,.F.,
(4,1,4),(4,4),(-4.89933240230808E-5,0.309230284442265,0.721537330365286),
(-4.89933240233201E-5,0.0862352312335747),.UNSPECIFIED.);
#18959=B_SPLINE_SURFACE_WITH_KNOTS('',3,3,((#99619,#99620,#99621,#99622),
(#99623,#99624,#99625,#99626),(#99627,#99628,#99629,#99630),(#99631,#99632,
#99633,#99634)),.UNSPECIFIED.,.F.,.F.,.F.,(4,4),(4,4),(0.640913278953462,
1.),(-1.2330723644364E-15,0.0441554944100176),.UNSPECIFIED.);
#18960=ADVANCED_FACE('',(#5026),#18849,.F.);
#18961=ADVANCED_FACE('',(#5027),#4554,.F.);
#18962=ADVANCED_FACE('',(#5028,#1694,#1695,#1696,#1697,#1698),#18850,.F.);
#18963=ADVANCED_FACE('',(#5029),#18851,.F.);
#18964=ADVANCED_FACE('',(#5030,#1699,#1700,#1701,#1702),#18852,.T.);
#18965=ADVANCED_FACE('',(#5031),#18853,.F.);
#18966=ADVANCED_FACE('',(#5032),#4555,.F.);
#18967=ADVANCED_FACE('',(#5033),#18854,.F.);
#18968=ADVANCED_FACE('',(#5034),#18855,.F.);
#18969=ADVANCED_FACE('',(#5035),#4556,.F.);
#18970=ADVANCED_FACE('',(#5036),#18856,.F.);
#18971=ADVANCED_FACE('',(#5037),#18857,.F.);
#18972=ADVANCED_FACE('',(#5038),#4557,.F.);
#18973=ADVANCED_FACE('',(#5039),#18858,.F.);
#18974=ADVANCED_FACE('',(#5040),#18859,.F.);
#18975=ADVANCED_FACE('',(#5041),#18860,.F.);
#18976=ADVANCED_FACE('',(#5042),#18861,.F.);
#18977=ADVANCED_FACE('',(#5043),#18862,.F.);
#18978=ADVANCED_FACE('',(#5044),#1363,.F.);
#18979=ADVANCED_FACE('',(#5045),#18863,.F.);
#18980=ADVANCED_FACE('',(#5046),#18864,.F.);
#18981=ADVANCED_FACE('',(#5047),#18865,.F.);
#18982=ADVANCED_FACE('',(#5048),#18866,.F.);
#18983=ADVANCED_FACE('',(#5049),#18867,.F.);
#18984=ADVANCED_FACE('',(#5050),#18868,.F.);
#18985=ADVANCED_FACE('',(#5051),#18869,.F.);
#18986=ADVANCED_FACE('',(#5052),#18870,.F.);
#18987=ADVANCED_FACE('',(#5053),#18871,.F.);
#18988=ADVANCED_FACE('',(#5054),#18872,.F.);
#18989=ADVANCED_FACE('',(#5055),#18873,.F.);
#18990=ADVANCED_FACE('',(#5056),#18874,.F.);
#18991=ADVANCED_FACE('',(#5057),#18875,.F.);
#18992=ADVANCED_FACE('',(#5058),#18876,.F.);
#18993=ADVANCED_FACE('',(#5059),#18877,.F.);
#18994=ADVANCED_FACE('',(#5060),#18878,.F.);
#18995=ADVANCED_FACE('',(#5061),#18879,.F.);
#18996=ADVANCED_FACE('',(#5062),#18880,.F.);
#18997=ADVANCED_FACE('',(#5063),#18881,.F.);
#18998=ADVANCED_FACE('',(#5064),#18882,.F.);
#18999=ADVANCED_FACE('',(#5065),#18883,.F.);
#19000=ADVANCED_FACE('',(#5066),#18884,.F.);
#19001=ADVANCED_FACE('',(#5067),#18885,.F.);
#19002=ADVANCED_FACE('',(#5068),#18886,.F.);
#19003=ADVANCED_FACE('',(#5069),#18887,.F.);
#19004=ADVANCED_FACE('',(#5070),#18888,.F.);
#19005=ADVANCED_FACE('',(#5071),#18889,.F.);
#19006=ADVANCED_FACE('',(#5072),#18890,.F.);
#19007=ADVANCED_FACE('',(#5073),#18891,.F.);
#19008=ADVANCED_FACE('',(#5074),#18892,.F.);
#19009=ADVANCED_FACE('',(#5075),#18893,.F.);
#19010=ADVANCED_FACE('',(#5076),#18894,.F.);
#19011=ADVANCED_FACE('',(#5077),#18895,.F.);
#19012=ADVANCED_FACE('',(#5078),#18896,.F.);
#19013=ADVANCED_FACE('',(#5079),#18897,.F.);
#19014=ADVANCED_FACE('',(#5080),#18898,.F.);
#19015=ADVANCED_FACE('',(#5081),#18899,.F.);
#19016=ADVANCED_FACE('',(#5082),#18900,.F.);
#19017=ADVANCED_FACE('',(#5083),#18901,.F.);
#19018=ADVANCED_FACE('',(#5084),#18902,.F.);
#19019=ADVANCED_FACE('',(#5085),#18903,.F.);
#19020=ADVANCED_FACE('',(#5086),#18904,.F.);
#19021=ADVANCED_FACE('',(#5087),#18905,.F.);
#19022=ADVANCED_FACE('',(#5088),#18906,.F.);
#19023=ADVANCED_FACE('',(#5089),#18907,.F.);
#19024=ADVANCED_FACE('',(#5090),#18908,.F.);
#19025=ADVANCED_FACE('',(#5091),#18909,.F.);
#19026=ADVANCED_FACE('',(#5092),#18910,.F.);
#19027=ADVANCED_FACE('',(#5093),#18911,.F.);
#19028=ADVANCED_FACE('',(#5094),#18912,.F.);
#19029=ADVANCED_FACE('',(#5095),#18913,.F.);
#19030=ADVANCED_FACE('',(#5096),#18914,.F.);
#19031=ADVANCED_FACE('',(#5097),#18915,.F.);
#19032=ADVANCED_FACE('',(#5098),#18916,.F.);
#19033=ADVANCED_FACE('',(#5099),#18917,.F.);
#19034=ADVANCED_FACE('',(#5100),#18918,.F.);
#19035=ADVANCED_FACE('',(#5101),#18919,.F.);
#19036=ADVANCED_FACE('',(#5102),#18920,.F.);
#19037=ADVANCED_FACE('',(#5103),#18921,.F.);
#19038=ADVANCED_FACE('',(#5104),#18922,.F.);
#19039=ADVANCED_FACE('',(#5105),#18923,.F.);
#19040=ADVANCED_FACE('',(#5106),#18924,.F.);
#19041=ADVANCED_FACE('',(#5107),#18925,.F.);
#19042=ADVANCED_FACE('',(#5108),#18926,.F.);
#19043=ADVANCED_FACE('',(#5109),#18927,.F.);
#19044=ADVANCED_FACE('',(#5110),#18928,.F.);
#19045=ADVANCED_FACE('',(#5111),#18929,.F.);
#19046=ADVANCED_FACE('',(#5112),#18930,.F.);
#19047=ADVANCED_FACE('',(#5113),#1183,.T.);
#19048=ADVANCED_FACE('',(#5114),#4558,.F.);
#19049=ADVANCED_FACE('',(#5115),#227,.F.);
#19050=ADVANCED_FACE('',(#5116),#4559,.T.);
#19051=ADVANCED_FACE('',(#5117),#117,.T.);
#19052=ADVANCED_FACE('',(#5118),#118,.T.);
#19053=ADVANCED_FACE('',(#5119),#4560,.T.);
#19054=ADVANCED_FACE('',(#5120),#1184,.T.);
#19055=ADVANCED_FACE('',(#5121),#4561,.F.);
#19056=ADVANCED_FACE('',(#5122),#4562,.T.);
#19057=ADVANCED_FACE('',(#5123),#119,.T.);
#19058=ADVANCED_FACE('',(#5124),#120,.T.);
#19059=ADVANCED_FACE('',(#5125),#1185,.T.);
#19060=ADVANCED_FACE('',(#5126),#1364,.F.);
#19061=ADVANCED_FACE('',(#5127),#4563,.T.);
#19062=ADVANCED_FACE('',(#5128),#121,.T.);
#19063=ADVANCED_FACE('',(#5129),#122,.T.);
#19064=ADVANCED_FACE('',(#5130),#4564,.T.);
#19065=ADVANCED_FACE('',(#5131),#4565,.F.);
#19066=ADVANCED_FACE('',(#5132),#4566,.T.);
#19067=ADVANCED_FACE('',(#5133),#123,.T.);
#19068=ADVANCED_FACE('',(#5134),#124,.T.);
#19069=ADVANCED_FACE('',(#5135),#1186,.T.);
#19070=ADVANCED_FACE('',(#5136),#1365,.F.);
#19071=ADVANCED_FACE('',(#5137),#4567,.T.);
#19072=ADVANCED_FACE('',(#5138),#125,.T.);
#19073=ADVANCED_FACE('',(#5139),#126,.T.);
#19074=ADVANCED_FACE('',(#5140),#1187,.T.);
#19075=ADVANCED_FACE('',(#5141),#4568,.T.);
#19076=ADVANCED_FACE('',(#5142),#1366,.F.);
#19077=ADVANCED_FACE('',(#5143),#4569,.T.);
#19078=ADVANCED_FACE('',(#5144),#127,.T.);
#19079=ADVANCED_FACE('',(#5145),#128,.T.);
#19080=ADVANCED_FACE('',(#5146),#4570,.T.);
#19081=ADVANCED_FACE('',(#5147),#4571,.F.);
#19082=ADVANCED_FACE('',(#5148),#1188,.T.);
#19083=ADVANCED_FACE('',(#5149,#1703,#1704,#1705,#1706,#1707,#1708,#1709),
#1367,.F.);
#19084=ADVANCED_FACE('',(#5150),#4572,.F.);
#19085=ADVANCED_FACE('',(#5151),#1189,.T.);
#19086=ADVANCED_FACE('',(#5152),#4573,.F.);
#19087=ADVANCED_FACE('',(#5153),#1190,.T.);
#19088=ADVANCED_FACE('',(#5154),#4574,.T.);
#19089=ADVANCED_FACE('',(#5155),#1191,.T.);
#19090=ADVANCED_FACE('',(#5156),#4575,.T.);
#19091=ADVANCED_FACE('',(#5157),#1192,.T.);
#19092=ADVANCED_FACE('',(#5158),#4576,.F.);
#19093=ADVANCED_FACE('',(#5159),#1368,.F.);
#19094=ADVANCED_FACE('',(#5160),#4577,.T.);
#19095=ADVANCED_FACE('',(#5161),#1193,.T.);
#19096=ADVANCED_FACE('',(#5162),#129,.T.);
#19097=ADVANCED_FACE('',(#5163),#4578,.T.);
#19098=ADVANCED_FACE('',(#5164),#130,.T.);
#19099=ADVANCED_FACE('',(#5165),#1369,.F.);
#19100=ADVANCED_FACE('',(#5166),#4579,.T.);
#19101=ADVANCED_FACE('',(#5167),#1194,.T.);
#19102=ADVANCED_FACE('',(#5168),#4580,.T.);
#19103=ADVANCED_FACE('',(#5169),#131,.T.);
#19104=ADVANCED_FACE('',(#5170),#4581,.T.);
#19105=ADVANCED_FACE('',(#5171),#132,.T.);
#19106=ADVANCED_FACE('',(#5172),#133,.T.);
#19107=ADVANCED_FACE('',(#5173),#4582,.T.);
#19108=ADVANCED_FACE('',(#5174),#134,.T.);
#19109=ADVANCED_FACE('',(#5175),#4583,.T.);
#19110=ADVANCED_FACE('',(#5176),#135,.T.);
#19111=ADVANCED_FACE('',(#5177),#4584,.T.);
#19112=ADVANCED_FACE('',(#5178),#4585,.T.);
#19113=ADVANCED_FACE('',(#5179),#136,.T.);
#19114=ADVANCED_FACE('',(#5180),#4586,.T.);
#19115=ADVANCED_FACE('',(#5181),#137,.T.);
#19116=ADVANCED_FACE('',(#5182),#4587,.T.);
#19117=ADVANCED_FACE('',(#5183),#138,.T.);
#19118=ADVANCED_FACE('',(#5184),#4588,.T.);
#19119=ADVANCED_FACE('',(#5185),#139,.T.);
#19120=ADVANCED_FACE('',(#5186),#1370,.T.);
#19121=ADVANCED_FACE('',(#5187),#1371,.T.);
#19122=ADVANCED_FACE('',(#5188),#4589,.T.);
#19123=ADVANCED_FACE('',(#5189),#4590,.T.);
#19124=ADVANCED_FACE('',(#5190),#1372,.T.);
#19125=ADVANCED_FACE('',(#5191),#140,.T.);
#19126=ADVANCED_FACE('',(#5192),#141,.T.);
#19127=ADVANCED_FACE('',(#5193),#4591,.T.);
#19128=ADVANCED_FACE('',(#5194),#1195,.T.);
#19129=ADVANCED_FACE('',(#5195),#142,.T.);
#19130=ADVANCED_FACE('',(#5196),#4592,.T.);
#19131=ADVANCED_FACE('',(#5197),#1196,.T.);
#19132=ADVANCED_FACE('',(#5198),#4593,.T.);
#19133=ADVANCED_FACE('',(#5199),#1197,.T.);
#19134=ADVANCED_FACE('',(#5200),#4594,.T.);
#19135=ADVANCED_FACE('',(#5201),#143,.T.);
#19136=ADVANCED_FACE('',(#5202),#1198,.T.);
#19137=ADVANCED_FACE('',(#5203),#144,.T.);
#19138=ADVANCED_FACE('',(#5204),#1199,.T.);
#19139=ADVANCED_FACE('',(#5205),#4595,.T.);
#19140=ADVANCED_FACE('',(#5206),#1373,.F.);
#19141=ADVANCED_FACE('',(#5207),#4596,.T.);
#19142=ADVANCED_FACE('',(#5208),#4597,.F.);
#19143=ADVANCED_FACE('',(#5209),#4598,.T.);
#19144=ADVANCED_FACE('',(#5210),#1200,.T.);
#19145=ADVANCED_FACE('',(#5211),#4599,.F.);
#19146=ADVANCED_FACE('',(#5212),#145,.T.);
#19147=ADVANCED_FACE('',(#5213),#4600,.T.);
#19148=ADVANCED_FACE('',(#5214),#146,.T.);
#19149=ADVANCED_FACE('',(#5215),#4601,.T.);
#19150=ADVANCED_FACE('',(#5216),#147,.T.);
#19151=ADVANCED_FACE('',(#5217),#4602,.T.);
#19152=ADVANCED_FACE('',(#5218),#148,.T.);
#19153=ADVANCED_FACE('',(#5219),#4603,.T.);
#19154=ADVANCED_FACE('',(#5220),#4604,.T.);
#19155=ADVANCED_FACE('',(#5221),#4605,.T.);
#19156=ADVANCED_FACE('',(#5222),#149,.T.);
#19157=ADVANCED_FACE('',(#5223),#4606,.T.);
#19158=ADVANCED_FACE('',(#5224),#4607,.T.);
#19159=ADVANCED_FACE('',(#5225),#4608,.T.);
#19160=ADVANCED_FACE('',(#5226),#150,.T.);
#19161=ADVANCED_FACE('',(#5227),#4609,.T.);
#19162=ADVANCED_FACE('',(#5228),#151,.T.);
#19163=ADVANCED_FACE('',(#5229),#4610,.T.);
#19164=ADVANCED_FACE('',(#5230),#152,.T.);
#19165=ADVANCED_FACE('',(#5231),#4611,.T.);
#19166=ADVANCED_FACE('',(#5232),#153,.T.);
#19167=ADVANCED_FACE('',(#5233),#4612,.T.);
#19168=ADVANCED_FACE('',(#5234),#154,.T.);
#19169=ADVANCED_FACE('',(#5235),#4613,.T.);
#19170=ADVANCED_FACE('',(#5236),#155,.T.);
#19171=ADVANCED_FACE('',(#5237),#1374,.T.);
#19172=ADVANCED_FACE('',(#5238),#4614,.T.);
#19173=ADVANCED_FACE('',(#5239),#4615,.T.);
#19174=ADVANCED_FACE('',(#5240),#1375,.T.);
#19175=ADVANCED_FACE('',(#5241),#4616,.T.);
#19176=ADVANCED_FACE('',(#5242),#4617,.T.);
#19177=ADVANCED_FACE('',(#5243),#1376,.T.);
#19178=ADVANCED_FACE('',(#5244),#1377,.T.);
#19179=ADVANCED_FACE('',(#5245),#1378,.T.);
#19180=ADVANCED_FACE('',(#5246),#4618,.T.);
#19181=ADVANCED_FACE('',(#5247),#4619,.T.);
#19182=ADVANCED_FACE('',(#5248),#1379,.T.);
#19183=ADVANCED_FACE('',(#5249),#1201,.T.);
#19184=ADVANCED_FACE('',(#5250,#1710,#1711,#1712,#1713,#1714,#1715,#1716),
#1380,.T.);
#19185=ADVANCED_FACE('',(#5251),#156,.T.);
#19186=ADVANCED_FACE('',(#5252),#4620,.T.);
#19187=ADVANCED_FACE('',(#5253),#4621,.T.);
#19188=ADVANCED_FACE('',(#5254),#4622,.T.);
#19189=ADVANCED_FACE('',(#5255),#157,.T.);
#19190=ADVANCED_FACE('',(#5256),#158,.T.);
#19191=ADVANCED_FACE('',(#5257),#4623,.F.);
#19192=ADVANCED_FACE('',(#5258),#1381,.F.);
#19193=ADVANCED_FACE('',(#5259),#4624,.T.);
#19194=ADVANCED_FACE('',(#5260),#4625,.T.);
#19195=ADVANCED_FACE('',(#5261),#4626,.T.);
#19196=ADVANCED_FACE('',(#5262),#159,.T.);
#19197=ADVANCED_FACE('',(#5263),#4627,.T.);
#19198=ADVANCED_FACE('',(#5264),#1382,.T.);
#19199=ADVANCED_FACE('',(#5265),#1383,.T.);
#19200=ADVANCED_FACE('',(#5266),#1384,.T.);
#19201=ADVANCED_FACE('',(#5267),#4628,.T.);
#19202=ADVANCED_FACE('',(#5268),#160,.T.);
#19203=ADVANCED_FACE('',(#5269),#161,.T.);
#19204=ADVANCED_FACE('',(#5270),#4629,.T.);
#19205=ADVANCED_FACE('',(#5271),#162,.T.);
#19206=ADVANCED_FACE('',(#5272),#1202,.T.);
#19207=ADVANCED_FACE('',(#5273),#4630,.T.);
#19208=ADVANCED_FACE('',(#5274),#163,.T.);
#19209=ADVANCED_FACE('',(#5275),#164,.T.);
#19210=ADVANCED_FACE('',(#5276),#4631,.T.);
#19211=ADVANCED_FACE('',(#5277),#165,.T.);
#19212=ADVANCED_FACE('',(#5278),#4632,.F.);
#19213=ADVANCED_FACE('',(#5279),#1203,.T.);
#19214=ADVANCED_FACE('',(#5280),#166,.T.);
#19215=ADVANCED_FACE('',(#5281),#4633,.T.);
#19216=ADVANCED_FACE('',(#5282),#1204,.T.);
#19217=ADVANCED_FACE('',(#5283),#167,.T.);
#19218=ADVANCED_FACE('',(#5284),#1205,.T.);
#19219=ADVANCED_FACE('',(#5285),#168,.T.);
#19220=ADVANCED_FACE('',(#5286),#4634,.T.);
#19221=ADVANCED_FACE('',(#5287),#4635,.T.);
#19222=ADVANCED_FACE('',(#5288),#4636,.T.);
#19223=ADVANCED_FACE('',(#5289),#169,.T.);
#19224=ADVANCED_FACE('',(#5290),#1385,.F.);
#19225=ADVANCED_FACE('',(#5291),#4637,.F.);
#19226=ADVANCED_FACE('',(#5292),#4638,.T.);
#19227=ADVANCED_FACE('',(#5293),#170,.T.);
#19228=ADVANCED_FACE('',(#5294),#1206,.T.);
#19229=ADVANCED_FACE('',(#5295),#4639,.T.);
#19230=ADVANCED_FACE('',(#5296),#4640,.T.);
#19231=ADVANCED_FACE('',(#5297),#171,.T.);
#19232=ADVANCED_FACE('',(#5298),#4641,.T.);
#19233=ADVANCED_FACE('',(#5299),#4642,.T.);
#19234=ADVANCED_FACE('',(#5300),#4643,.T.);
#19235=ADVANCED_FACE('',(#5301),#172,.T.);
#19236=ADVANCED_FACE('',(#5302),#4644,.T.);
#19237=ADVANCED_FACE('',(#5303),#173,.T.);
#19238=ADVANCED_FACE('',(#5304),#4645,.T.);
#19239=ADVANCED_FACE('',(#5305),#174,.T.);
#19240=ADVANCED_FACE('',(#5306),#4646,.T.);
#19241=ADVANCED_FACE('',(#5307),#4647,.T.);
#19242=ADVANCED_FACE('',(#5308),#4648,.T.);
#19243=ADVANCED_FACE('',(#5309),#4649,.T.);
#19244=ADVANCED_FACE('',(#5310),#4650,.T.);
#19245=ADVANCED_FACE('',(#5311),#175,.T.);
#19246=ADVANCED_FACE('',(#5312),#4651,.T.);
#19247=ADVANCED_FACE('',(#5313),#176,.T.);
#19248=ADVANCED_FACE('',(#5314),#4652,.T.);
#19249=ADVANCED_FACE('',(#5315),#177,.T.);
#19250=ADVANCED_FACE('',(#5316),#4653,.T.);
#19251=ADVANCED_FACE('',(#5317),#178,.T.);
#19252=ADVANCED_FACE('',(#5318),#4654,.T.);
#19253=ADVANCED_FACE('',(#5319),#179,.T.);
#19254=ADVANCED_FACE('',(#5320),#180,.T.);
#19255=ADVANCED_FACE('',(#5321),#4655,.T.);
#19256=ADVANCED_FACE('',(#5322),#4656,.T.);
#19257=ADVANCED_FACE('',(#5323),#1386,.T.);
#19258=ADVANCED_FACE('',(#5324),#1387,.T.);
#19259=ADVANCED_FACE('',(#5325),#4657,.T.);
#19260=ADVANCED_FACE('',(#5326),#4658,.T.);
#19261=ADVANCED_FACE('',(#5327),#1388,.T.);
#19262=ADVANCED_FACE('',(#5328),#1389,.T.);
#19263=ADVANCED_FACE('',(#5329),#1390,.T.);
#19264=ADVANCED_FACE('',(#5330),#4659,.T.);
#19265=ADVANCED_FACE('',(#5331),#1391,.T.);
#19266=ADVANCED_FACE('',(#5332),#4660,.T.);
#19267=ADVANCED_FACE('',(#5333),#1392,.T.);
#19268=ADVANCED_FACE('',(#5334),#4661,.T.);
#19269=ADVANCED_FACE('',(#5335),#1393,.T.);
#19270=ADVANCED_FACE('',(#5336),#4662,.T.);
#19271=ADVANCED_FACE('',(#5337),#4663,.T.);
#19272=ADVANCED_FACE('',(#5338),#1207,.T.);
#19273=ADVANCED_FACE('',(#5339),#1394,.T.);
#19274=ADVANCED_FACE('',(#5340),#4664,.F.);
#19275=ADVANCED_FACE('',(#5341),#1395,.T.);
#19276=ADVANCED_FACE('',(#5342),#4665,.T.);
#19277=ADVANCED_FACE('',(#5343),#1208,.T.);
#19278=ADVANCED_FACE('',(#5344),#4666,.T.);
#19279=ADVANCED_FACE('',(#5345),#4667,.F.);
#19280=ADVANCED_FACE('',(#5346),#1396,.F.);
#19281=ADVANCED_FACE('',(#5347),#1209,.T.);
#19282=ADVANCED_FACE('',(#5348),#4668,.T.);
#19283=ADVANCED_FACE('',(#5349),#1210,.T.);
#19284=ADVANCED_FACE('',(#5350),#4669,.T.);
#19285=ADVANCED_FACE('',(#5351),#1211,.T.);
#19286=ADVANCED_FACE('',(#5352),#4670,.F.);
#19287=ADVANCED_FACE('',(#5353),#1212,.T.);
#19288=ADVANCED_FACE('',(#5354),#1213,.T.);
#19289=ADVANCED_FACE('',(#5355),#228,.F.);
#19290=ADVANCED_FACE('',(#5356),#1214,.T.);
#19291=ADVANCED_FACE('',(#5357),#1397,.F.);
#19292=ADVANCED_FACE('',(#5358),#1398,.T.);
#19293=ADVANCED_FACE('',(#5359),#4671,.T.);
#19294=ADVANCED_FACE('',(#5360),#4672,.T.);
#19295=ADVANCED_FACE('',(#5361),#4673,.T.);
#19296=ADVANCED_FACE('',(#5362),#4674,.T.);
#19297=ADVANCED_FACE('',(#5363),#1399,.F.);
#19298=ADVANCED_FACE('',(#5364),#1400,.F.);
#19299=ADVANCED_FACE('',(#5365,#1717),#1401,.T.);
#19300=ADVANCED_FACE('',(#5366),#4675,.T.);
#19301=ADVANCED_FACE('',(#5367),#4676,.T.);
#19302=ADVANCED_FACE('',(#5368),#4677,.T.);
#19303=ADVANCED_FACE('',(#5369),#4678,.T.);
#19304=ADVANCED_FACE('',(#5370),#4679,.T.);
#19305=ADVANCED_FACE('',(#5371),#1402,.F.);
#19306=ADVANCED_FACE('',(#5372,#1718),#1403,.T.);
#19307=ADVANCED_FACE('',(#5373),#4680,.T.);
#19308=ADVANCED_FACE('',(#5374),#4681,.T.);
#19309=ADVANCED_FACE('',(#5375),#1404,.T.);
#19310=ADVANCED_FACE('',(#5376),#4682,.T.);
#19311=ADVANCED_FACE('',(#5377),#4683,.T.);
#19312=ADVANCED_FACE('',(#5378),#4684,.T.);
#19313=ADVANCED_FACE('',(#5379),#4685,.T.);
#19314=ADVANCED_FACE('',(#5380),#1405,.F.);
#19315=ADVANCED_FACE('',(#5381),#1406,.F.);
#19316=ADVANCED_FACE('',(#5382,#1719),#1407,.T.);
#19317=ADVANCED_FACE('',(#5383),#181,.T.);
#19318=ADVANCED_FACE('',(#5384),#4686,.T.);
#19319=ADVANCED_FACE('',(#5385),#1408,.T.);
#19320=ADVANCED_FACE('',(#5386),#4687,.T.);
#19321=ADVANCED_FACE('',(#5387),#4688,.T.);
#19322=ADVANCED_FACE('',(#5388),#4689,.T.);
#19323=ADVANCED_FACE('',(#5389),#182,.T.);
#19324=ADVANCED_FACE('',(#5390),#4690,.T.);
#19325=ADVANCED_FACE('',(#5391),#4691,.T.);
#19326=ADVANCED_FACE('',(#5392),#1409,.T.);
#19327=ADVANCED_FACE('',(#5393),#4692,.T.);
#19328=ADVANCED_FACE('',(#5394),#4693,.T.);
#19329=ADVANCED_FACE('',(#5395),#4694,.T.);
#19330=ADVANCED_FACE('',(#5396),#4695,.T.);
#19331=ADVANCED_FACE('',(#5397),#4696,.T.);
#19332=ADVANCED_FACE('',(#5398),#183,.T.);
#19333=ADVANCED_FACE('',(#5399),#4697,.T.);
#19334=ADVANCED_FACE('',(#5400),#4698,.T.);
#19335=ADVANCED_FACE('',(#5401),#1215,.T.);
#19336=ADVANCED_FACE('',(#5402),#4699,.T.);
#19337=ADVANCED_FACE('',(#5403),#1410,.T.);
#19338=ADVANCED_FACE('',(#5404),#1411,.T.);
#19339=ADVANCED_FACE('',(#5405),#1412,.T.);
#19340=ADVANCED_FACE('',(#5406),#4700,.T.);
#19341=ADVANCED_FACE('',(#5407),#1413,.T.);
#19342=ADVANCED_FACE('',(#5408),#1414,.T.);
#19343=ADVANCED_FACE('',(#5409),#4701,.T.);
#19344=ADVANCED_FACE('',(#5410),#4702,.T.);
#19345=ADVANCED_FACE('',(#5411),#4703,.T.);
#19346=ADVANCED_FACE('',(#5412),#184,.T.);
#19347=ADVANCED_FACE('',(#5413),#4704,.T.);
#19348=ADVANCED_FACE('',(#5414),#4705,.T.);
#19349=ADVANCED_FACE('',(#5415),#4706,.T.);
#19350=ADVANCED_FACE('',(#5416),#4707,.T.);
#19351=ADVANCED_FACE('',(#5417),#4708,.T.);
#19352=ADVANCED_FACE('',(#5418),#4709,.T.);
#19353=ADVANCED_FACE('',(#5419),#1415,.F.);
#19354=ADVANCED_FACE('',(#5420,#1720),#1416,.F.);
#19355=ADVANCED_FACE('',(#5421),#4710,.T.);
#19356=ADVANCED_FACE('',(#5422),#1216,.T.);
#19357=ADVANCED_FACE('',(#5423),#4711,.T.);
#19358=ADVANCED_FACE('',(#5424),#4712,.T.);
#19359=ADVANCED_FACE('',(#5425),#4713,.T.);
#19360=ADVANCED_FACE('',(#5426),#4714,.T.);
#19361=ADVANCED_FACE('',(#5427),#1417,.T.);
#19362=ADVANCED_FACE('',(#5428),#4715,.T.);
#19363=ADVANCED_FACE('',(#5429),#1418,.T.);
#19364=ADVANCED_FACE('',(#5430),#1419,.T.);
#19365=ADVANCED_FACE('',(#5431),#1420,.T.);
#19366=ADVANCED_FACE('',(#5432),#4716,.T.);
#19367=ADVANCED_FACE('',(#5433),#1217,.T.);
#19368=ADVANCED_FACE('',(#5434),#4717,.T.);
#19369=ADVANCED_FACE('',(#5435),#4718,.T.);
#19370=ADVANCED_FACE('',(#5436),#4719,.T.);
#19371=ADVANCED_FACE('',(#5437),#4720,.T.);
#19372=ADVANCED_FACE('',(#5438,#1721,#1722,#1723),#1421,.T.);
#19373=ADVANCED_FACE('',(#5439),#1218,.T.);
#19374=ADVANCED_FACE('',(#5440,#1724),#1422,.F.);
#19375=ADVANCED_FACE('',(#5441),#4721,.T.);
#19376=ADVANCED_FACE('',(#5442),#4722,.T.);
#19377=ADVANCED_FACE('',(#5443),#4723,.T.);
#19378=ADVANCED_FACE('',(#5444),#4724,.T.);
#19379=ADVANCED_FACE('',(#5445),#4725,.T.);
#19380=ADVANCED_FACE('',(#5446),#4726,.T.);
#19381=ADVANCED_FACE('',(#5447),#4727,.T.);
#19382=ADVANCED_FACE('',(#5448),#1219,.T.);
#19383=ADVANCED_FACE('',(#5449,#1725,#1726,#1727),#1423,.T.);
#19384=ADVANCED_FACE('',(#5450),#1220,.T.);
#19385=ADVANCED_FACE('',(#5451,#1728),#1424,.F.);
#19386=ADVANCED_FACE('',(#5452),#4728,.T.);
#19387=ADVANCED_FACE('',(#5453),#1221,.T.);
#19388=ADVANCED_FACE('',(#5454),#4729,.F.);
#19389=ADVANCED_FACE('',(#5455),#1222,.T.);
#19390=ADVANCED_FACE('',(#5456),#1223,.T.);
#19391=ADVANCED_FACE('',(#5457),#4730,.F.);
#19392=ADVANCED_FACE('',(#5458),#1224,.T.);
#19393=ADVANCED_FACE('',(#5459),#1225,.T.);
#19394=ADVANCED_FACE('',(#5460),#4731,.F.);
#19395=ADVANCED_FACE('',(#5461),#1226,.T.);
#19396=ADVANCED_FACE('',(#5462,#1729,#1730,#1731),#1425,.F.);
#19397=ADVANCED_FACE('',(#5463),#1227,.T.);
#19398=ADVANCED_FACE('',(#5464),#4732,.F.);
#19399=ADVANCED_FACE('',(#5465),#1228,.T.);
#19400=ADVANCED_FACE('',(#5466,#1732,#1733,#1734),#1426,.F.);
#19401=ADVANCED_FACE('',(#5467),#1229,.T.);
#19402=ADVANCED_FACE('',(#5468),#4733,.F.);
#19403=ADVANCED_FACE('',(#5469),#1230,.T.);
#19404=ADVANCED_FACE('',(#5470),#1231,.T.);
#19405=ADVANCED_FACE('',(#5471),#4734,.F.);
#19406=ADVANCED_FACE('',(#5472),#1232,.T.);
#19407=ADVANCED_FACE('',(#5473),#1233,.T.);
#19408=ADVANCED_FACE('',(#5474),#4735,.F.);
#19409=ADVANCED_FACE('',(#5475,#1735,#1736,#1737,#1738),#1427,.T.);
#19410=ADVANCED_FACE('',(#5476),#4736,.T.);
#19411=ADVANCED_FACE('',(#5477),#4737,.T.);
#19412=ADVANCED_FACE('',(#5478),#4738,.T.);
#19413=ADVANCED_FACE('',(#5479),#1428,.T.);
#19414=ADVANCED_FACE('',(#5480),#1429,.T.);
#19415=ADVANCED_FACE('',(#5481),#1430,.T.);
#19416=ADVANCED_FACE('',(#5482),#4739,.T.);
#19417=ADVANCED_FACE('',(#5483),#1234,.T.);
#19418=ADVANCED_FACE('',(#5484,#1739,#1740,#1741,#1742),#1431,.F.);
#19419=ADVANCED_FACE('',(#5485),#4740,.T.);
#19420=ADVANCED_FACE('',(#5486),#4741,.T.);
#19421=ADVANCED_FACE('',(#5487),#4742,.T.);
#19422=ADVANCED_FACE('',(#5488),#4743,.T.);
#19423=ADVANCED_FACE('',(#5489),#1235,.T.);
#19424=ADVANCED_FACE('',(#5490),#4744,.F.);
#19425=ADVANCED_FACE('',(#5491),#1236,.T.);
#19426=ADVANCED_FACE('',(#5492),#4745,.T.);
#19427=ADVANCED_FACE('',(#5493),#4746,.T.);
#19428=ADVANCED_FACE('',(#5494),#4747,.T.);
#19429=ADVANCED_FACE('',(#5495),#4748,.T.);
#19430=ADVANCED_FACE('',(#5496),#1432,.F.);
#19431=ADVANCED_FACE('',(#5497),#1433,.F.);
#19432=ADVANCED_FACE('',(#5498),#4749,.T.);
#19433=ADVANCED_FACE('',(#5499),#4750,.T.);
#19434=ADVANCED_FACE('',(#5500),#4751,.T.);
#19435=ADVANCED_FACE('',(#5501),#1434,.F.);
#19436=ADVANCED_FACE('',(#5502),#4752,.T.);
#19437=ADVANCED_FACE('',(#5503),#4753,.T.);
#19438=ADVANCED_FACE('',(#5504),#4754,.T.);
#19439=ADVANCED_FACE('',(#5505),#4755,.T.);
#19440=ADVANCED_FACE('',(#5506),#1435,.F.);
#19441=ADVANCED_FACE('',(#5507),#1436,.F.);
#19442=ADVANCED_FACE('',(#5508),#4756,.T.);
#19443=ADVANCED_FACE('',(#5509),#4757,.T.);
#19444=ADVANCED_FACE('',(#5510),#4758,.T.);
#19445=ADVANCED_FACE('',(#5511),#1437,.F.);
#19446=ADVANCED_FACE('',(#5512),#4759,.T.);
#19447=ADVANCED_FACE('',(#5513),#4760,.T.);
#19448=ADVANCED_FACE('',(#5514),#1438,.F.);
#19449=ADVANCED_FACE('',(#5515),#1439,.T.);
#19450=ADVANCED_FACE('',(#5516),#1440,.T.);
#19451=ADVANCED_FACE('',(#5517),#4761,.T.);
#19452=ADVANCED_FACE('',(#5518),#1441,.T.);
#19453=ADVANCED_FACE('',(#5519),#1442,.T.);
#19454=ADVANCED_FACE('',(#5520),#1443,.T.);
#19455=ADVANCED_FACE('',(#5521),#4762,.T.);
#19456=ADVANCED_FACE('',(#5522),#4763,.T.);
#19457=ADVANCED_FACE('',(#5523),#4764,.T.);
#19458=ADVANCED_FACE('',(#5524),#1444,.F.);
#19459=ADVANCED_FACE('',(#5525),#1445,.T.);
#19460=ADVANCED_FACE('',(#5526),#1446,.T.);
#19461=ADVANCED_FACE('',(#5527),#4765,.T.);
#19462=ADVANCED_FACE('',(#5528),#1447,.T.);
#19463=ADVANCED_FACE('',(#5529),#1448,.T.);
#19464=ADVANCED_FACE('',(#5530),#1449,.T.);
#19465=ADVANCED_FACE('',(#5531),#4766,.T.);
#19466=ADVANCED_FACE('',(#5532),#1450,.T.);
#19467=ADVANCED_FACE('',(#5533),#1451,.T.);
#19468=ADVANCED_FACE('',(#5534),#1452,.F.);
#19469=ADVANCED_FACE('',(#5535),#1453,.T.);
#19470=ADVANCED_FACE('',(#5536),#1454,.F.);
#19471=ADVANCED_FACE('',(#5537),#185,.T.);
#19472=ADVANCED_FACE('',(#5538),#186,.T.);
#19473=ADVANCED_FACE('',(#5539),#4767,.T.);
#19474=ADVANCED_FACE('',(#5540),#4768,.T.);
#19475=ADVANCED_FACE('',(#5541),#4769,.T.);
#19476=ADVANCED_FACE('',(#5542),#187,.T.);
#19477=ADVANCED_FACE('',(#5543),#4770,.T.);
#19478=ADVANCED_FACE('',(#5544),#4771,.T.);
#19479=ADVANCED_FACE('',(#5545),#4772,.T.);
#19480=ADVANCED_FACE('',(#5546),#188,.T.);
#19481=ADVANCED_FACE('',(#5547),#4773,.T.);
#19482=ADVANCED_FACE('',(#5548),#4774,.T.);
#19483=ADVANCED_FACE('',(#5549),#189,.T.);
#19484=ADVANCED_FACE('',(#5550),#4775,.T.);
#19485=ADVANCED_FACE('',(#5551),#4776,.T.);
#19486=ADVANCED_FACE('',(#5552),#190,.T.);
#19487=ADVANCED_FACE('',(#5553),#191,.T.);
#19488=ADVANCED_FACE('',(#5554),#4777,.T.);
#19489=ADVANCED_FACE('',(#5555),#192,.T.);
#19490=ADVANCED_FACE('',(#5556),#4778,.T.);
#19491=ADVANCED_FACE('',(#5557),#4779,.T.);
#19492=ADVANCED_FACE('',(#5558),#193,.T.);
#19493=ADVANCED_FACE('',(#5559),#4780,.T.);
#19494=ADVANCED_FACE('',(#5560),#4781,.T.);
#19495=ADVANCED_FACE('',(#5561),#4782,.T.);
#19496=ADVANCED_FACE('',(#5562),#194,.T.);
#19497=ADVANCED_FACE('',(#5563),#4783,.T.);
#19498=ADVANCED_FACE('',(#5564),#4784,.T.);
#19499=ADVANCED_FACE('',(#5565),#4785,.T.);
#19500=ADVANCED_FACE('',(#5566),#18931,.F.);
#19501=ADVANCED_FACE('',(#5567),#195,.T.);
#19502=ADVANCED_FACE('',(#5568),#18932,.F.);
#19503=ADVANCED_FACE('',(#5569),#196,.T.);
#19504=ADVANCED_FACE('',(#5570),#1455,.T.);
#19505=ADVANCED_FACE('',(#5571,#1743,#1744),#1456,.F.);
#19506=ADVANCED_FACE('',(#5572),#1457,.T.);
#19507=ADVANCED_FACE('',(#5573),#4786,.T.);
#19508=ADVANCED_FACE('',(#5574),#1458,.T.);
#19509=ADVANCED_FACE('',(#5575),#1459,.T.);
#19510=ADVANCED_FACE('',(#5576),#4787,.T.);
#19511=ADVANCED_FACE('',(#5577),#4788,.T.);
#19512=ADVANCED_FACE('',(#5578),#4789,.T.);
#19513=ADVANCED_FACE('',(#5579),#1460,.T.);
#19514=ADVANCED_FACE('',(#5580),#1237,.T.);
#19515=ADVANCED_FACE('',(#5581),#4790,.F.);
#19516=ADVANCED_FACE('',(#5582),#1238,.T.);
#19517=ADVANCED_FACE('',(#5583,#1745),#1461,.T.);
#19518=ADVANCED_FACE('',(#5584),#4791,.T.);
#19519=ADVANCED_FACE('',(#5585),#1239,.T.);
#19520=ADVANCED_FACE('',(#5586),#1240,.T.);
#19521=ADVANCED_FACE('',(#5587),#4792,.F.);
#19522=ADVANCED_FACE('',(#5588),#1241,.T.);
#19523=ADVANCED_FACE('',(#5589),#4793,.F.);
#19524=ADVANCED_FACE('',(#5590),#4794,.T.);
#19525=ADVANCED_FACE('',(#5591),#4795,.T.);
#19526=ADVANCED_FACE('',(#5592),#4796,.T.);
#19527=ADVANCED_FACE('',(#5593),#1242,.T.);
#19528=ADVANCED_FACE('',(#5594),#1243,.T.);
#19529=ADVANCED_FACE('',(#5595),#1462,.T.);
#19530=ADVANCED_FACE('',(#5596),#4797,.T.);
#19531=ADVANCED_FACE('',(#5597),#4798,.T.);
#19532=ADVANCED_FACE('',(#5598),#4799,.T.);
#19533=ADVANCED_FACE('',(#5599),#1244,.T.);
#19534=ADVANCED_FACE('',(#5600,#1746,#1747),#1463,.T.);
#19535=ADVANCED_FACE('',(#5601),#1245,.T.);
#19536=ADVANCED_FACE('',(#5602),#1246,.T.);
#19537=ADVANCED_FACE('',(#5603,#1748,#1749),#1464,.T.);
#19538=ADVANCED_FACE('',(#5604),#1247,.T.);
#19539=ADVANCED_FACE('',(#5605),#1248,.T.);
#19540=ADVANCED_FACE('',(#5606,#1750),#1465,.T.);
#19541=ADVANCED_FACE('',(#5607),#1466,.T.);
#19542=ADVANCED_FACE('',(#5608),#1467,.T.);
#19543=ADVANCED_FACE('',(#5609),#1468,.T.);
#19544=ADVANCED_FACE('',(#5610),#1469,.T.);
#19545=ADVANCED_FACE('',(#5611),#1470,.F.);
#19546=ADVANCED_FACE('',(#5612),#1471,.F.);
#19547=ADVANCED_FACE('',(#5613,#1751),#1472,.T.);
#19548=ADVANCED_FACE('',(#5614,#1752),#1473,.T.);
#19549=ADVANCED_FACE('',(#5615),#229,.F.);
#19550=ADVANCED_FACE('',(#5616),#4800,.F.);
#19551=ADVANCED_FACE('',(#5617,#1753),#1474,.T.);
#19552=ADVANCED_FACE('',(#5618),#1475,.T.);
#19553=ADVANCED_FACE('',(#5619),#1476,.T.);
#19554=ADVANCED_FACE('',(#5620),#230,.T.);
#19555=ADVANCED_FACE('',(#5621),#4801,.T.);
#19556=ADVANCED_FACE('',(#5622,#1754),#1477,.T.);
#19557=ADVANCED_FACE('',(#5623),#231,.T.);
#19558=ADVANCED_FACE('',(#5624,#1755),#1478,.T.);
#19559=ADVANCED_FACE('',(#5625),#1479,.T.);
#19560=ADVANCED_FACE('',(#5626),#1480,.T.);
#19561=ADVANCED_FACE('',(#5627),#1481,.T.);
#19562=ADVANCED_FACE('',(#5628),#4802,.F.);
#19563=ADVANCED_FACE('',(#5629),#1482,.T.);
#19564=ADVANCED_FACE('',(#5630),#1483,.T.);
#19565=ADVANCED_FACE('',(#5631),#1484,.T.);
#19566=ADVANCED_FACE('',(#5632),#4803,.F.);
#19567=ADVANCED_FACE('',(#5633),#1485,.T.);
#19568=ADVANCED_FACE('',(#5634),#1486,.T.);
#19569=ADVANCED_FACE('',(#5635),#1487,.T.);
#19570=ADVANCED_FACE('',(#5636),#4804,.F.);
#19571=ADVANCED_FACE('',(#5637),#1488,.T.);
#19572=ADVANCED_FACE('',(#5638),#1489,.T.);
#19573=ADVANCED_FACE('',(#5639),#1490,.T.);
#19574=ADVANCED_FACE('',(#5640),#4805,.F.);
#19575=ADVANCED_FACE('',(#5641),#1491,.T.);
#19576=ADVANCED_FACE('',(#5642),#1492,.T.);
#19577=ADVANCED_FACE('',(#5643),#1493,.T.);
#19578=ADVANCED_FACE('',(#5644),#4806,.F.);
#19579=ADVANCED_FACE('',(#5645),#1494,.T.);
#19580=ADVANCED_FACE('',(#5646),#1495,.T.);
#19581=ADVANCED_FACE('',(#5647),#1496,.T.);
#19582=ADVANCED_FACE('',(#5648),#4807,.F.);
#19583=ADVANCED_FACE('',(#5649),#1497,.T.);
#19584=ADVANCED_FACE('',(#5650),#1498,.T.);
#19585=ADVANCED_FACE('',(#5651),#1499,.T.);
#19586=ADVANCED_FACE('',(#5652),#4808,.F.);
#19587=ADVANCED_FACE('',(#5653),#1500,.T.);
#19588=ADVANCED_FACE('',(#5654),#1501,.T.);
#19589=ADVANCED_FACE('',(#5655),#1502,.T.);
#19590=ADVANCED_FACE('',(#5656),#4809,.F.);
#19591=ADVANCED_FACE('',(#5657),#1503,.T.);
#19592=ADVANCED_FACE('',(#5658),#1504,.T.);
#19593=ADVANCED_FACE('',(#5659),#1505,.T.);
#19594=ADVANCED_FACE('',(#5660),#4810,.F.);
#19595=ADVANCED_FACE('',(#5661),#1506,.T.);
#19596=ADVANCED_FACE('',(#5662),#1507,.T.);
#19597=ADVANCED_FACE('',(#5663),#1508,.T.);
#19598=ADVANCED_FACE('',(#5664),#4811,.F.);
#19599=ADVANCED_FACE('',(#5665),#1509,.T.);
#19600=ADVANCED_FACE('',(#5666),#1510,.T.);
#19601=ADVANCED_FACE('',(#5667),#1511,.T.);
#19602=ADVANCED_FACE('',(#5668),#4812,.F.);
#19603=ADVANCED_FACE('',(#5669),#1512,.T.);
#19604=ADVANCED_FACE('',(#5670),#1513,.T.);
#19605=ADVANCED_FACE('',(#5671),#1514,.T.);
#19606=ADVANCED_FACE('',(#5672),#4813,.F.);
#19607=ADVANCED_FACE('',(#5673),#1515,.T.);
#19608=ADVANCED_FACE('',(#5674),#1516,.T.);
#19609=ADVANCED_FACE('',(#5675),#1517,.T.);
#19610=ADVANCED_FACE('',(#5676),#4814,.F.);
#19611=ADVANCED_FACE('',(#5677),#1518,.T.);
#19612=ADVANCED_FACE('',(#5678),#1519,.T.);
#19613=ADVANCED_FACE('',(#5679),#1520,.T.);
#19614=ADVANCED_FACE('',(#5680,#1756),#1521,.T.);
#19615=ADVANCED_FACE('',(#5681),#4815,.F.);
#19616=ADVANCED_FACE('',(#5682),#4816,.F.);
#19617=ADVANCED_FACE('',(#5683),#4817,.T.);
#19618=ADVANCED_FACE('',(#5684),#4818,.T.);
#19619=ADVANCED_FACE('',(#5685),#4819,.T.);
#19620=ADVANCED_FACE('',(#5686),#4820,.T.);
#19621=ADVANCED_FACE('',(#5687),#4821,.T.);
#19622=ADVANCED_FACE('',(#5688),#4822,.T.);
#19623=ADVANCED_FACE('',(#5689),#4823,.T.);
#19624=ADVANCED_FACE('',(#5690),#4824,.T.);
#19625=ADVANCED_FACE('',(#5691),#4825,.T.);
#19626=ADVANCED_FACE('',(#5692),#4826,.T.);
#19627=ADVANCED_FACE('',(#5693),#4827,.T.);
#19628=ADVANCED_FACE('',(#5694),#4828,.T.);
#19629=ADVANCED_FACE('',(#5695),#4829,.T.);
#19630=ADVANCED_FACE('',(#5696),#4830,.T.);
#19631=ADVANCED_FACE('',(#5697),#4831,.T.);
#19632=ADVANCED_FACE('',(#5698),#4832,.T.);
#19633=ADVANCED_FACE('',(#5699),#4833,.T.);
#19634=ADVANCED_FACE('',(#5700),#4834,.T.);
#19635=ADVANCED_FACE('',(#5701),#4835,.T.);
#19636=ADVANCED_FACE('',(#5702),#4836,.T.);
#19637=ADVANCED_FACE('',(#5703),#4837,.T.);
#19638=ADVANCED_FACE('',(#5704),#4838,.T.);
#19639=ADVANCED_FACE('',(#5705),#4839,.T.);
#19640=ADVANCED_FACE('',(#5706),#4840,.T.);
#19641=ADVANCED_FACE('',(#5707),#4841,.T.);
#19642=ADVANCED_FACE('',(#5708),#4842,.T.);
#19643=ADVANCED_FACE('',(#5709),#4843,.T.);
#19644=ADVANCED_FACE('',(#5710),#4844,.T.);
#19645=ADVANCED_FACE('',(#5711),#4845,.T.);
#19646=ADVANCED_FACE('',(#5712),#4846,.T.);
#19647=ADVANCED_FACE('',(#5713),#4847,.T.);
#19648=ADVANCED_FACE('',(#5714),#4848,.T.);
#19649=ADVANCED_FACE('',(#5715),#4849,.T.);
#19650=ADVANCED_FACE('',(#5716),#4850,.T.);
#19651=ADVANCED_FACE('',(#5717),#4851,.T.);
#19652=ADVANCED_FACE('',(#5718),#4852,.T.);
#19653=ADVANCED_FACE('',(#5719),#4853,.T.);
#19654=ADVANCED_FACE('',(#5720),#4854,.T.);
#19655=ADVANCED_FACE('',(#5721),#4855,.T.);
#19656=ADVANCED_FACE('',(#5722),#4856,.T.);
#19657=ADVANCED_FACE('',(#5723),#4857,.T.);
#19658=ADVANCED_FACE('',(#5724),#4858,.F.);
#19659=ADVANCED_FACE('',(#5725),#1522,.F.);
#19660=ADVANCED_FACE('',(#5726),#1523,.F.);
#19661=ADVANCED_FACE('',(#5727),#18933,.F.);
#19662=ADVANCED_FACE('',(#5728),#1524,.T.);
#19663=ADVANCED_FACE('',(#5729),#18934,.F.);
#19664=ADVANCED_FACE('',(#5730,#1757),#1525,.T.);
#19665=ADVANCED_FACE('',(#5731),#232,.T.);
#19666=ADVANCED_FACE('',(#5732),#233,.T.);
#19667=ADVANCED_FACE('',(#5733),#4859,.T.);
#19668=ADVANCED_FACE('',(#5734,#1758),#1526,.T.);
#19669=ADVANCED_FACE('',(#5735),#4860,.T.);
#19670=ADVANCED_FACE('',(#5736,#1759),#1527,.T.);
#19671=ADVANCED_FACE('',(#5737),#4861,.T.);
#19672=ADVANCED_FACE('',(#5738),#234,.T.);
#19673=ADVANCED_FACE('',(#5739),#1528,.T.);
#19674=ADVANCED_FACE('',(#5740),#1249,.T.);
#19675=ADVANCED_FACE('',(#5741),#1529,.F.);
#19676=ADVANCED_FACE('',(#5742),#1250,.T.);
#19677=ADVANCED_FACE('',(#5743),#1530,.F.);
#19678=ADVANCED_FACE('',(#5744),#1251,.T.);
#19679=ADVANCED_FACE('',(#5745),#4862,.T.);
#19680=ADVANCED_FACE('',(#5746),#1252,.T.);
#19681=ADVANCED_FACE('',(#5747),#1531,.F.);
#19682=ADVANCED_FACE('',(#5748),#1253,.T.);
#19683=ADVANCED_FACE('',(#5749),#1532,.F.);
#19684=ADVANCED_FACE('',(#5750),#4863,.T.);
#19685=ADVANCED_FACE('',(#5751),#1533,.T.);
#19686=ADVANCED_FACE('',(#5752),#4864,.T.);
#19687=ADVANCED_FACE('',(#5753),#1534,.F.);
#19688=ADVANCED_FACE('',(#5754),#4865,.T.);
#19689=ADVANCED_FACE('',(#5755),#4866,.T.);
#19690=ADVANCED_FACE('',(#5756),#4867,.T.);
#19691=ADVANCED_FACE('',(#5757),#1535,.F.);
#19692=ADVANCED_FACE('',(#5758),#1536,.F.);
#19693=ADVANCED_FACE('',(#5759),#1537,.T.);
#19694=ADVANCED_FACE('',(#5760),#1538,.T.);
#19695=ADVANCED_FACE('',(#5761),#1539,.T.);
#19696=ADVANCED_FACE('',(#5762),#4868,.T.);
#19697=ADVANCED_FACE('',(#5763),#197,.T.);
#19698=ADVANCED_FACE('',(#5764),#4869,.T.);
#19699=ADVANCED_FACE('',(#5765),#4870,.T.);
#19700=ADVANCED_FACE('',(#5766),#4871,.T.);
#19701=ADVANCED_FACE('',(#5767),#4872,.T.);
#19702=ADVANCED_FACE('',(#5768),#198,.T.);
#19703=ADVANCED_FACE('',(#5769),#199,.T.);
#19704=ADVANCED_FACE('',(#5770),#1540,.T.);
#19705=ADVANCED_FACE('',(#5771),#4873,.T.);
#19706=ADVANCED_FACE('',(#5772),#1541,.F.);
#19707=ADVANCED_FACE('',(#5773),#4874,.T.);
#19708=ADVANCED_FACE('',(#5774),#1542,.T.);
#19709=ADVANCED_FACE('',(#5775),#1254,.T.);
#19710=ADVANCED_FACE('',(#5776),#4875,.T.);
#19711=ADVANCED_FACE('',(#5777),#4876,.T.);
#19712=ADVANCED_FACE('',(#5778),#1543,.T.);
#19713=ADVANCED_FACE('',(#5779),#1255,.T.);
#19714=ADVANCED_FACE('',(#5780),#4877,.T.);
#19715=ADVANCED_FACE('',(#5781),#4878,.T.);
#19716=ADVANCED_FACE('',(#5782,#1760),#1544,.T.);
#19717=ADVANCED_FACE('',(#5783),#1256,.T.);
#19718=ADVANCED_FACE('',(#5784),#4879,.F.);
#19719=ADVANCED_FACE('',(#5785),#18935,.F.);
#19720=ADVANCED_FACE('',(#5786,#1761),#4880,.T.);
#19721=ADVANCED_FACE('',(#5787),#1257,.T.);
#19722=ADVANCED_FACE('',(#5788),#1545,.T.);
#19723=ADVANCED_FACE('',(#5789),#4881,.T.);
#19724=ADVANCED_FACE('',(#5790),#4882,.T.);
#19725=ADVANCED_FACE('',(#5791),#4883,.T.);
#19726=ADVANCED_FACE('',(#5792),#200,.T.);
#19727=ADVANCED_FACE('',(#5793),#201,.T.);
#19728=ADVANCED_FACE('',(#5794),#4884,.T.);
#19729=ADVANCED_FACE('',(#5795),#202,.T.);
#19730=ADVANCED_FACE('',(#5796),#4885,.T.);
#19731=ADVANCED_FACE('',(#5797),#4886,.T.);
#19732=ADVANCED_FACE('',(#5798),#4887,.T.);
#19733=ADVANCED_FACE('',(#5799),#1546,.T.);
#19734=ADVANCED_FACE('',(#5800),#4888,.T.);
#19735=ADVANCED_FACE('',(#5801),#4889,.F.);
#19736=ADVANCED_FACE('',(#5802),#4890,.T.);
#19737=ADVANCED_FACE('',(#5803),#4891,.F.);
#19738=ADVANCED_FACE('',(#5804),#4892,.T.);
#19739=ADVANCED_FACE('',(#5805),#4893,.T.);
#19740=ADVANCED_FACE('',(#5806),#203,.T.);
#19741=ADVANCED_FACE('',(#5807),#4894,.T.);
#19742=ADVANCED_FACE('',(#5808),#204,.T.);
#19743=ADVANCED_FACE('',(#5809),#4895,.T.);
#19744=ADVANCED_FACE('',(#5810,#1762),#1547,.T.);
#19745=ADVANCED_FACE('',(#5811),#1258,.T.);
#19746=ADVANCED_FACE('',(#5812),#4896,.T.);
#19747=ADVANCED_FACE('',(#5813),#4897,.F.);
#19748=ADVANCED_FACE('',(#5814),#1259,.T.);
#19749=ADVANCED_FACE('',(#5815),#4898,.F.);
#19750=ADVANCED_FACE('',(#5816,#1763),#1548,.T.);
#19751=ADVANCED_FACE('',(#5817),#1260,.T.);
#19752=ADVANCED_FACE('',(#5818),#1261,.T.);
#19753=ADVANCED_FACE('',(#5819),#4899,.T.);
#19754=ADVANCED_FACE('',(#5820),#4900,.T.);
#19755=ADVANCED_FACE('',(#5821),#1549,.T.);
#19756=ADVANCED_FACE('',(#5822),#4901,.T.);
#19757=ADVANCED_FACE('',(#5823),#1550,.T.);
#19758=ADVANCED_FACE('',(#5824),#4902,.T.);
#19759=ADVANCED_FACE('',(#5825),#1551,.T.);
#19760=ADVANCED_FACE('',(#5826),#4903,.T.);
#19761=ADVANCED_FACE('',(#5827),#4904,.T.);
#19762=ADVANCED_FACE('',(#5828),#205,.T.);
#19763=ADVANCED_FACE('',(#5829),#4905,.T.);
#19764=ADVANCED_FACE('',(#5830),#206,.T.);
#19765=ADVANCED_FACE('',(#5831,#1764,#1765,#1766,#1767),#1552,.T.);
#19766=ADVANCED_FACE('',(#5832),#4906,.T.);
#19767=ADVANCED_FACE('',(#5833),#4907,.T.);
#19768=ADVANCED_FACE('',(#5834),#1262,.T.);
#19769=ADVANCED_FACE('',(#5835),#4908,.T.);
#19770=ADVANCED_FACE('',(#5836),#1553,.F.);
#19771=ADVANCED_FACE('',(#5837),#4909,.T.);
#19772=ADVANCED_FACE('',(#5838),#1554,.F.);
#19773=ADVANCED_FACE('',(#5839),#4910,.T.);
#19774=ADVANCED_FACE('',(#5840),#1555,.F.);
#19775=ADVANCED_FACE('',(#5841),#4911,.T.);
#19776=ADVANCED_FACE('',(#5842),#1556,.F.);
#19777=ADVANCED_FACE('',(#5843),#207,.T.);
#19778=ADVANCED_FACE('',(#5844),#4912,.T.);
#19779=ADVANCED_FACE('',(#5845),#4913,.T.);
#19780=ADVANCED_FACE('',(#5846),#4914,.T.);
#19781=ADVANCED_FACE('',(#5847),#4915,.T.);
#19782=ADVANCED_FACE('',(#5848),#208,.T.);
#19783=ADVANCED_FACE('',(#5849),#4916,.T.);
#19784=ADVANCED_FACE('',(#5850),#1557,.T.);
#19785=ADVANCED_FACE('',(#5851),#4917,.T.);
#19786=ADVANCED_FACE('',(#5852),#1263,.T.);
#19787=ADVANCED_FACE('',(#5853),#4918,.F.);
#19788=ADVANCED_FACE('',(#5854,#1768),#1558,.T.);
#19789=ADVANCED_FACE('',(#5855),#1264,.T.);
#19790=ADVANCED_FACE('',(#5856),#4919,.T.);
#19791=ADVANCED_FACE('',(#5857),#4920,.F.);
#19792=ADVANCED_FACE('',(#5858,#1769),#1559,.T.);
#19793=ADVANCED_FACE('',(#5859),#4921,.T.);
#19794=ADVANCED_FACE('',(#5860),#1560,.T.);
#19795=ADVANCED_FACE('',(#5861),#4922,.T.);
#19796=ADVANCED_FACE('',(#5862),#4923,.T.);
#19797=ADVANCED_FACE('',(#5863),#1561,.T.);
#19798=ADVANCED_FACE('',(#5864),#4924,.T.);
#19799=ADVANCED_FACE('',(#5865),#1562,.T.);
#19800=ADVANCED_FACE('',(#5866),#4925,.T.);
#19801=ADVANCED_FACE('',(#5867),#1563,.T.);
#19802=ADVANCED_FACE('',(#5868),#4926,.T.);
#19803=ADVANCED_FACE('',(#5869),#1564,.T.);
#19804=ADVANCED_FACE('',(#5870),#4927,.T.);
#19805=ADVANCED_FACE('',(#5871),#1565,.F.);
#19806=ADVANCED_FACE('',(#5872),#4928,.T.);
#19807=ADVANCED_FACE('',(#5873),#1566,.F.);
#19808=ADVANCED_FACE('',(#5874),#4929,.T.);
#19809=ADVANCED_FACE('',(#5875),#1567,.F.);
#19810=ADVANCED_FACE('',(#5876),#4930,.T.);
#19811=ADVANCED_FACE('',(#5877),#1568,.F.);
#19812=ADVANCED_FACE('',(#5878),#1265,.T.);
#19813=ADVANCED_FACE('',(#5879),#4931,.T.);
#19814=ADVANCED_FACE('',(#5880),#1569,.F.);
#19815=ADVANCED_FACE('',(#5881),#4932,.T.);
#19816=ADVANCED_FACE('',(#5882),#1570,.F.);
#19817=ADVANCED_FACE('',(#5883),#4933,.T.);
#19818=ADVANCED_FACE('',(#5884),#1571,.F.);
#19819=ADVANCED_FACE('',(#5885),#4934,.T.);
#19820=ADVANCED_FACE('',(#5886),#1572,.F.);
#19821=ADVANCED_FACE('',(#5887),#1266,.T.);
#19822=ADVANCED_FACE('',(#5888),#4935,.F.);
#19823=ADVANCED_FACE('',(#5889),#1267,.T.);
#19824=ADVANCED_FACE('',(#5890),#4936,.F.);
#19825=ADVANCED_FACE('',(#5891),#4937,.F.);
#19826=ADVANCED_FACE('',(#5892),#1268,.T.);
#19827=ADVANCED_FACE('',(#5893),#1269,.T.);
#19828=ADVANCED_FACE('',(#5894),#4938,.T.);
#19829=ADVANCED_FACE('',(#5895),#1270,.T.);
#19830=ADVANCED_FACE('',(#5896,#1770),#1573,.T.);
#19831=ADVANCED_FACE('',(#5897),#4939,.T.);
#19832=ADVANCED_FACE('',(#5898),#4940,.T.);
#19833=ADVANCED_FACE('',(#5899),#209,.T.);
#19834=ADVANCED_FACE('',(#5900),#210,.T.);
#19835=ADVANCED_FACE('',(#5901),#4941,.T.);
#19836=ADVANCED_FACE('',(#5902),#4942,.T.);
#19837=ADVANCED_FACE('',(#5903),#4943,.T.);
#19838=ADVANCED_FACE('',(#5904),#211,.T.);
#19839=ADVANCED_FACE('',(#5905),#1574,.F.);
#19840=ADVANCED_FACE('',(#5906),#4944,.T.);
#19841=ADVANCED_FACE('',(#5907),#4945,.T.);
#19842=ADVANCED_FACE('',(#5908),#4946,.T.);
#19843=ADVANCED_FACE('',(#5909),#4947,.T.);
#19844=ADVANCED_FACE('',(#5910),#212,.T.);
#19845=ADVANCED_FACE('',(#5911),#213,.T.);
#19846=ADVANCED_FACE('',(#5912),#1575,.T.);
#19847=ADVANCED_FACE('',(#5913),#4948,.T.);
#19848=ADVANCED_FACE('',(#5914),#4949,.T.);
#19849=ADVANCED_FACE('',(#5915),#4950,.T.);
#19850=ADVANCED_FACE('',(#5916),#214,.T.);
#19851=ADVANCED_FACE('',(#5917),#1271,.T.);
#19852=ADVANCED_FACE('',(#5918),#4951,.F.);
#19853=ADVANCED_FACE('',(#5919,#1771,#1772),#1576,.T.);
#19854=ADVANCED_FACE('',(#5920),#4952,.T.);
#19855=ADVANCED_FACE('',(#5921),#1577,.T.);
#19856=ADVANCED_FACE('',(#5922),#4953,.T.);
#19857=ADVANCED_FACE('',(#5923),#1578,.F.);
#19858=ADVANCED_FACE('',(#5924),#1579,.T.);
#19859=ADVANCED_FACE('',(#5925),#1580,.T.);
#19860=ADVANCED_FACE('',(#5926),#4954,.T.);
#19861=ADVANCED_FACE('',(#5927),#4955,.T.);
#19862=ADVANCED_FACE('',(#5928),#1581,.T.);
#19863=ADVANCED_FACE('',(#5929),#1582,.T.);
#19864=ADVANCED_FACE('',(#5930),#1583,.T.);
#19865=ADVANCED_FACE('',(#5931),#4956,.T.);
#19866=ADVANCED_FACE('',(#5932),#4957,.T.);
#19867=ADVANCED_FACE('',(#5933),#4958,.T.);
#19868=ADVANCED_FACE('',(#5934),#1584,.T.);
#19869=ADVANCED_FACE('',(#5935),#1585,.F.);
#19870=ADVANCED_FACE('',(#5936),#4959,.T.);
#19871=ADVANCED_FACE('',(#5937),#1586,.F.);
#19872=ADVANCED_FACE('',(#5938),#4960,.T.);
#19873=ADVANCED_FACE('',(#5939),#4961,.T.);
#19874=ADVANCED_FACE('',(#5940),#4962,.T.);
#19875=ADVANCED_FACE('',(#5941),#215,.T.);
#19876=ADVANCED_FACE('',(#5942),#216,.T.);
#19877=ADVANCED_FACE('',(#5943),#4963,.T.);
#19878=ADVANCED_FACE('',(#5944),#4964,.T.);
#19879=ADVANCED_FACE('',(#5945),#1587,.T.);
#19880=ADVANCED_FACE('',(#5946),#1272,.T.);
#19881=ADVANCED_FACE('',(#5947),#1273,.T.);
#19882=ADVANCED_FACE('',(#5948),#1588,.F.);
#19883=ADVANCED_FACE('',(#5949),#1589,.F.);
#19884=ADVANCED_FACE('',(#5950),#1590,.F.);
#19885=ADVANCED_FACE('',(#5951),#1591,.F.);
#19886=ADVANCED_FACE('',(#5952),#115,.F.);
#19887=ADVANCED_FACE('',(#5953),#4965,.T.);
#19888=ADVANCED_FACE('',(#5954),#1592,.F.);
#19889=ADVANCED_FACE('',(#5955),#4966,.T.);
#19890=ADVANCED_FACE('',(#5956),#1593,.F.);
#19891=ADVANCED_FACE('',(#5957),#4967,.T.);
#19892=ADVANCED_FACE('',(#5958),#1594,.F.);
#19893=ADVANCED_FACE('',(#5959),#4968,.T.);
#19894=ADVANCED_FACE('',(#5960),#1595,.F.);
#19895=ADVANCED_FACE('',(#5961),#1596,.F.);
#19896=ADVANCED_FACE('',(#5962),#1274,.T.);
#19897=ADVANCED_FACE('',(#5963),#4969,.F.);
#19898=ADVANCED_FACE('',(#5964),#1597,.F.);
#19899=ADVANCED_FACE('',(#5965),#116,.F.);
#19900=ADVANCED_FACE('',(#5966),#1275,.T.);
#19901=ADVANCED_FACE('',(#5967),#1598,.F.);
#19902=ADVANCED_FACE('',(#5968),#1599,.F.);
#19903=ADVANCED_FACE('',(#5969),#1600,.F.);
#19904=ADVANCED_FACE('',(#5970),#1601,.F.);
#19905=ADVANCED_FACE('',(#5971),#1602,.F.);
#19906=ADVANCED_FACE('',(#5972),#1603,.F.);
#19907=ADVANCED_FACE('',(#5973),#1604,.F.);
#19908=ADVANCED_FACE('',(#5974),#1605,.F.);
#19909=ADVANCED_FACE('',(#5975),#1606,.F.);
#19910=ADVANCED_FACE('',(#5976),#1607,.F.);
#19911=ADVANCED_FACE('',(#5977),#1608,.F.);
#19912=ADVANCED_FACE('',(#5978),#1609,.F.);
#19913=ADVANCED_FACE('',(#5979),#1610,.F.);
#19914=ADVANCED_FACE('',(#5980),#1611,.F.);
#19915=ADVANCED_FACE('',(#5981),#1612,.F.);
#19916=ADVANCED_FACE('',(#5982),#1613,.F.);
#19917=ADVANCED_FACE('',(#5983),#1614,.F.);
#19918=ADVANCED_FACE('',(#5984),#1615,.F.);
#19919=ADVANCED_FACE('',(#5985),#1616,.F.);
#19920=ADVANCED_FACE('',(#5986),#1617,.F.);
#19921=ADVANCED_FACE('',(#5987),#1618,.F.);
#19922=ADVANCED_FACE('',(#5988),#1619,.F.);
#19923=ADVANCED_FACE('',(#5989,#1773),#1620,.T.);
#19924=ADVANCED_FACE('',(#5990),#1621,.T.);
#19925=ADVANCED_FACE('',(#5991),#1622,.T.);
#19926=ADVANCED_FACE('',(#5992),#1623,.T.);
#19927=ADVANCED_FACE('',(#5993),#4970,.T.);
#19928=ADVANCED_FACE('',(#5994),#4971,.T.);
#19929=ADVANCED_FACE('',(#5995),#1624,.F.);
#19930=ADVANCED_FACE('',(#5996),#1625,.F.);
#19931=ADVANCED_FACE('',(#5997),#1626,.F.);
#19932=ADVANCED_FACE('',(#5998),#1627,.F.);
#19933=ADVANCED_FACE('',(#5999),#1628,.T.);
#19934=ADVANCED_FACE('',(#6000),#1629,.T.);
#19935=ADVANCED_FACE('',(#6001),#1630,.T.);
#19936=ADVANCED_FACE('',(#6002),#1631,.F.);
#19937=ADVANCED_FACE('',(#6003),#1632,.T.);
#19938=ADVANCED_FACE('',(#6004),#1633,.T.);
#19939=ADVANCED_FACE('',(#6005),#1634,.T.);
#19940=ADVANCED_FACE('',(#6006),#1635,.T.);
#19941=ADVANCED_FACE('',(#6007),#1636,.F.);
#19942=ADVANCED_FACE('',(#6008),#1637,.F.);
#19943=ADVANCED_FACE('',(#6009,#1774,#1775),#18936,.T.);
#19944=ADVANCED_FACE('',(#6010),#18937,.T.);
#19945=ADVANCED_FACE('',(#6011),#1276,.T.);
#19946=ADVANCED_FACE('',(#6012),#4972,.F.);
#19947=ADVANCED_FACE('',(#6013,#1776),#1638,.T.);
#19948=ADVANCED_FACE('',(#6014),#1277,.T.);
#19949=ADVANCED_FACE('',(#6015,#1777),#1639,.T.);
#19950=ADVANCED_FACE('',(#6016),#1278,.T.);
#19951=ADVANCED_FACE('',(#6017,#1778),#1640,.T.);
#19952=ADVANCED_FACE('',(#6018),#4973,.F.);
#19953=ADVANCED_FACE('',(#6019),#1279,.T.);
#19954=ADVANCED_FACE('',(#6020,#1779),#4974,.T.);
#19955=ADVANCED_FACE('',(#6021),#1280,.T.);
#19956=ADVANCED_FACE('',(#6022),#4975,.T.);
#19957=ADVANCED_FACE('',(#6023,#1780),#1641,.T.);
#19958=ADVANCED_FACE('',(#6024),#1281,.T.);
#19959=ADVANCED_FACE('',(#6025),#4976,.T.);
#19960=ADVANCED_FACE('',(#6026),#4977,.T.);
#19961=ADVANCED_FACE('',(#6027),#4978,.T.);
#19962=ADVANCED_FACE('',(#6028),#4979,.T.);
#19963=ADVANCED_FACE('',(#6029),#1642,.T.);
#19964=ADVANCED_FACE('',(#6030),#1643,.F.);
#19965=ADVANCED_FACE('',(#6031,#1781),#1644,.T.);
#19966=ADVANCED_FACE('',(#6032),#1645,.F.);
#19967=ADVANCED_FACE('',(#6033),#1646,.F.);
#19968=ADVANCED_FACE('',(#6034),#1647,.F.);
#19969=ADVANCED_FACE('',(#6035),#1648,.F.);
#19970=ADVANCED_FACE('',(#6036),#1649,.F.);
#19971=ADVANCED_FACE('',(#6037),#1650,.T.);
#19972=ADVANCED_FACE('',(#6038),#1651,.T.);
#19973=ADVANCED_FACE('',(#6039),#4980,.T.);
#19974=ADVANCED_FACE('',(#6040),#4981,.T.);
#19975=ADVANCED_FACE('',(#6041),#4982,.T.);
#19976=ADVANCED_FACE('',(#6042),#4983,.T.);
#19977=ADVANCED_FACE('',(#6043),#217,.T.);
#19978=ADVANCED_FACE('',(#6044),#218,.T.);
#19979=ADVANCED_FACE('',(#6045),#219,.T.);
#19980=ADVANCED_FACE('',(#6046),#220,.T.);
#19981=ADVANCED_FACE('',(#6047),#4984,.T.);
#19982=ADVANCED_FACE('',(#6048),#1652,.T.);
#19983=ADVANCED_FACE('',(#6049),#4985,.T.);
#19984=ADVANCED_FACE('',(#6050,#1782,#1783),#1653,.T.);
#19985=ADVANCED_FACE('',(#6051),#1654,.T.);
#19986=ADVANCED_FACE('',(#6052),#4986,.T.);
#19987=ADVANCED_FACE('',(#6053),#4987,.T.);
#19988=ADVANCED_FACE('',(#6054),#221,.T.);
#19989=ADVANCED_FACE('',(#6055),#4988,.T.);
#19990=ADVANCED_FACE('',(#6056),#222,.T.);
#19991=ADVANCED_FACE('',(#6057),#18938,.F.);
#19992=ADVANCED_FACE('',(#6058),#18939,.T.);
#19993=ADVANCED_FACE('',(#6059),#18940,.F.);
#19994=ADVANCED_FACE('',(#6060,#1784,#1785),#1655,.T.);
#19995=ADVANCED_FACE('',(#6061),#4989,.T.);
#19996=ADVANCED_FACE('',(#6062),#223,.T.);
#19997=ADVANCED_FACE('',(#6063),#224,.T.);
#19998=ADVANCED_FACE('',(#6064),#18941,.F.);
#19999=ADVANCED_FACE('',(#6065),#18942,.T.);
#20000=ADVANCED_FACE('',(#6066),#18943,.F.);
#20001=ADVANCED_FACE('',(#6067),#18944,.F.);
#20002=ADVANCED_FACE('',(#6068),#18945,.F.);
#20003=ADVANCED_FACE('',(#6069),#18946,.F.);
#20004=ADVANCED_FACE('',(#6070),#18947,.F.);
#20005=ADVANCED_FACE('',(#6071),#4990,.T.);
#20006=ADVANCED_FACE('',(#6072),#1282,.T.);
#20007=ADVANCED_FACE('',(#6073),#4991,.T.);
#20008=ADVANCED_FACE('',(#6074),#18948,.F.);
#20009=ADVANCED_FACE('',(#6075),#18949,.F.);
#20010=ADVANCED_FACE('',(#6076),#18950,.F.);
#20011=ADVANCED_FACE('',(#6077),#18951,.F.);
#20012=ADVANCED_FACE('',(#6078),#1656,.T.);
#20013=ADVANCED_FACE('',(#6079),#4992,.T.);
#20014=ADVANCED_FACE('',(#6080),#1657,.T.);
#20015=ADVANCED_FACE('',(#6081),#1658,.T.);
#20016=ADVANCED_FACE('',(#6082),#18952,.F.);
#20017=ADVANCED_FACE('',(#6083),#18953,.F.);
#20018=ADVANCED_FACE('',(#6084),#18954,.F.);
#20019=ADVANCED_FACE('',(#6085),#18955,.F.);
#20020=ADVANCED_FACE('',(#6086),#4993,.T.);
#20021=ADVANCED_FACE('',(#6087),#18956,.F.);
#20022=ADVANCED_FACE('',(#6088),#18957,.F.);
#20023=ADVANCED_FACE('',(#6089),#18958,.F.);
#20024=ADVANCED_FACE('',(#6090),#18959,.F.);
#20025=ADVANCED_FACE('',(#6091),#4994,.F.);
#20026=ADVANCED_FACE('',(#6092,#1786,#1787),#1659,.T.);
#20027=ADVANCED_FACE('',(#6093),#1283,.T.);
#20028=ADVANCED_FACE('',(#6094),#4995,.F.);
#20029=ADVANCED_FACE('',(#6095),#1284,.T.);
#20030=ADVANCED_FACE('',(#6096),#1285,.T.);
#20031=ADVANCED_FACE('',(#6097),#4996,.F.);
#20032=ADVANCED_FACE('',(#6098),#1286,.T.);
#20033=ADVANCED_FACE('',(#6099,#1788,#1789),#1660,.T.);
#20034=ADVANCED_FACE('',(#6100),#1287,.T.);
#20035=ADVANCED_FACE('',(#6101),#4997,.F.);
#20036=ADVANCED_FACE('',(#6102),#1288,.T.);
#20037=ADVANCED_FACE('',(#6103),#1289,.T.);
#20038=ADVANCED_FACE('',(#6104),#4998,.F.);
#20039=ADVANCED_FACE('',(#6105),#1290,.T.);
#20040=ADVANCED_FACE('',(#6106),#1661,.T.);
#20041=ADVANCED_FACE('',(#6107),#4999,.T.);
#20042=ADVANCED_FACE('',(#6108),#5000,.F.);
#20043=ADVANCED_FACE('',(#6109),#1662,.T.);
#20044=ADVANCED_FACE('',(#6110,#1790),#1663,.T.);
#20045=ADVANCED_FACE('',(#6111),#5001,.T.);
#20046=ADVANCED_FACE('',(#6112),#5002,.F.);
#20047=ADVANCED_FACE('',(#6113,#1791),#1664,.F.);
#20048=ADVANCED_FACE('',(#6114),#5003,.T.);
#20049=ADVANCED_FACE('',(#6115,#1792),#1665,.T.);
#20050=ADVANCED_FACE('',(#6116),#5004,.T.);
#20051=ADVANCED_FACE('',(#6117,#1793),#1666,.T.);
#20052=ADVANCED_FACE('',(#6118),#5005,.T.);
#20053=ADVANCED_FACE('',(#6119,#1794),#1667,.F.);
#20054=ADVANCED_FACE('',(#6120),#5006,.F.);
#20055=ADVANCED_FACE('',(#6121,#1795),#1668,.T.);
#20056=ADVANCED_FACE('',(#6122,#1796),#1669,.F.);
#20057=ADVANCED_FACE('',(#6123),#5007,.T.);
#20058=ADVANCED_FACE('',(#6124,#1797),#1670,.F.);
#20059=ADVANCED_FACE('',(#6125),#5008,.T.);
#20060=ADVANCED_FACE('',(#6126,#1798),#1671,.F.);
#20061=ADVANCED_FACE('',(#6127),#5009,.T.);
#20062=ADVANCED_FACE('',(#6128,#1799),#1672,.F.);
#20063=ADVANCED_FACE('',(#6129),#5010,.T.);
#20064=ADVANCED_FACE('',(#6130),#235,.T.);
#20065=ADVANCED_FACE('',(#6131),#5011,.T.);
#20066=ADVANCED_FACE('',(#6132),#236,.T.);
#20067=ADVANCED_FACE('',(#6133,#1800),#1673,.T.);
#20068=ADVANCED_FACE('',(#6134),#5012,.F.);
#20069=ADVANCED_FACE('',(#6135,#1801),#1674,.T.);
#20070=ADVANCED_FACE('',(#6136),#237,.T.);
#20071=ADVANCED_FACE('',(#6137),#5013,.T.);
#20072=ADVANCED_FACE('',(#6138),#238,.T.);
#20073=ADVANCED_FACE('',(#6139,#1802),#1675,.T.);
#20074=ADVANCED_FACE('',(#6140),#5014,.F.);
#20075=ADVANCED_FACE('',(#6141,#1803),#1676,.T.);
#20076=ADVANCED_FACE('',(#6142),#239,.T.);
#20077=ADVANCED_FACE('',(#6143),#5015,.T.);
#20078=ADVANCED_FACE('',(#6144),#240,.T.);
#20079=ADVANCED_FACE('',(#6145),#1677,.T.);
#20080=ADVANCED_FACE('',(#6146),#1678,.T.);
#20081=ADVANCED_FACE('',(#6147),#241,.T.);
#20082=ADVANCED_FACE('',(#6148),#5016,.T.);
#20083=ADVANCED_FACE('',(#6149),#242,.T.);
#20084=ADVANCED_FACE('',(#6150),#1679,.T.);
#20085=ADVANCED_FACE('',(#6151),#1680,.T.);
#20086=ADVANCED_FACE('',(#6152),#1681,.T.);
#20087=ADVANCED_FACE('',(#6153),#243,.T.);
#20088=ADVANCED_FACE('',(#6154),#5017,.T.);
#20089=ADVANCED_FACE('',(#6155,#1804),#1682,.T.);
#20090=ADVANCED_FACE('',(#6156),#5018,.T.);
#20091=ADVANCED_FACE('',(#6157),#244,.T.);
#20092=ADVANCED_FACE('',(#6158,#1805),#1683,.T.);
#20093=ADVANCED_FACE('',(#6159),#5019,.T.);
#20094=ADVANCED_FACE('',(#6160,#1806),#1684,.T.);
#20095=ADVANCED_FACE('',(#6161),#5020,.T.);
#20096=ADVANCED_FACE('',(#6162,#1807),#1685,.T.);
#20097=ADVANCED_FACE('',(#6163),#5021,.T.);
#20098=ADVANCED_FACE('',(#6164),#245,.T.);
#20099=ADVANCED_FACE('',(#6165),#1686,.T.);
#20100=ADVANCED_FACE('',(#6166),#246,.T.);
#20101=ADVANCED_FACE('',(#6167),#5022,.T.);
#20102=ADVANCED_FACE('',(#6168),#247,.T.);
#20103=ADVANCED_FACE('',(#6169),#1687,.T.);
#20104=ADVANCED_FACE('',(#6170),#1688,.T.);
#20105=ADVANCED_FACE('',(#6171),#225,.T.);
#20106=ADVANCED_FACE('',(#6172,#1808),#1689,.T.);
#20107=ADVANCED_FACE('',(#6173),#5023,.T.);
#20108=ADVANCED_FACE('',(#6174,#1809),#1690,.T.);
#20109=ADVANCED_FACE('',(#6175),#5024,.T.);
#20110=ADVANCED_FACE('',(#6176),#248,.T.);
#20111=ADVANCED_FACE('',(#6177),#1691,.T.);
#20112=ADVANCED_FACE('',(#6178),#226,.T.);
#20113=ADVANCED_FACE('',(#6179,#1810),#1692,.T.);
#20114=ADVANCED_FACE('',(#6180),#5025,.T.);
#20115=ADVANCED_FACE('',(#6181),#249,.T.);
#20116=ADVANCED_FACE('',(#6182),#1693,.T.);
#20117=CLOSED_SHELL('',(#18960,#18961,#18962,#18963,#18964,#18965,#18966,
#18967,#18968,#18969,#18970,#18971,#18972,#18973,#18974,#18975,#18976,#18977,
#18978,#18979,#18980,#18981,#18982,#18983,#18984,#18985,#18986,#18987,#18988,
#18989,#18990,#18991,#18992,#18993,#18994,#18995,#18996,#18997,#18998,#18999,
#19000,#19001,#19002,#19003,#19004,#19005,#19006,#19007,#19008,#19009,#19010,
#19011,#19012,#19013,#19014,#19015,#19016,#19017,#19018,#19019,#19020,#19021,
#19022,#19023,#19024,#19025,#19026,#19027,#19028,#19029,#19030,#19031,#19032,
#19033,#19034,#19035,#19036,#19037,#19038,#19039,#19040,#19041,#19042,#19043,
#19044,#19045,#19046));
#20118=CLOSED_SHELL('',(#19047,#19048,#19049,#19050,#19051,#19052,#19053,
#19054,#19055,#19056,#19057,#19058,#19059,#19060,#19061,#19062,#19063,#19064,
#19065,#19066,#19067,#19068,#19069,#19070,#19071,#19072,#19073,#19074,#19075,
#19076,#19077,#19078,#19079,#19080,#19081,#19082,#19083,#19084,#19085,#19086,
#19087,#19088,#19089,#19090,#19091,#19092,#19093,#19094,#19095,#19096,#19097,
#19098,#19099,#19100,#19101,#19102,#19103,#19104,#19105,#19106,#19107,#19108,
#19109,#19110,#19111,#19112,#19113,#19114,#19115,#19116,#19117,#19118,#19119,
#19120,#19121,#19122,#19123,#19124,#19125,#19126,#19127,#19128,#19129,#19130,
#19131,#19132,#19133,#19134,#19135,#19136,#19137,#19138,#19139,#19140,#19141,
#19142,#19143,#19144,#19145,#19146,#19147,#19148,#19149,#19150,#19151,#19152,
#19153,#19154,#19155,#19156,#19157,#19158,#19159,#19160,#19161,#19162,#19163,
#19164,#19165,#19166,#19167,#19168,#19169,#19170,#19171,#19172,#19173,#19174,
#19175,#19176,#19177,#19178,#19179,#19180,#19181,#19182,#19183,#19184,#19185,
#19186,#19187,#19188,#19189,#19190,#19191,#19192,#19193,#19194,#19195,#19196,
#19197,#19198,#19199,#19200,#19201,#19202,#19203,#19204,#19205,#19206,#19207,
#19208,#19209,#19210,#19211,#19212,#19213,#19214,#19215,#19216,#19217,#19218,
#19219,#19220,#19221,#19222,#19223,#19224,#19225,#19226,#19227,#19228,#19229,
#19230,#19231,#19232,#19233,#19234,#19235,#19236,#19237,#19238,#19239,#19240,
#19241,#19242,#19243,#19244,#19245,#19246,#19247,#19248,#19249,#19250,#19251,
#19252,#19253,#19254,#19255,#19256,#19257,#19258,#19259,#19260,#19261,#19262,
#19263,#19264,#19265,#19266,#19267,#19268,#19269,#19270,#19271,#19272,#19273,
#19274,#19275,#19276,#19277,#19278,#19279,#19280,#19281,#19282,#19283,#19284,
#19285,#19286,#19287,#19288,#19289,#19290,#19291,#19292));
#20119=CLOSED_SHELL('',(#19293,#19294,#19295,#19296,#19297,#19298,#19299,
#19300,#19301,#19302,#19303,#19304,#19305,#19306,#19307,#19308,#19309,#19310,
#19311,#19312,#19313,#19314,#19315,#19316,#19317,#19318,#19319,#19320,#19321,
#19322,#19323,#19324,#19325,#19326,#19327,#19328,#19329,#19330,#19331,#19332,
#19333,#19334,#19335,#19336,#19337,#19338,#19339,#19340,#19341,#19342,#19343,
#19344,#19345,#19346,#19347,#19348,#19349,#19350,#19351,#19352,#19353,#19354,
#19355,#19356,#19357,#19358,#19359,#19360,#19361,#19362,#19363,#19364,#19365,
#19366,#19367,#19368,#19369,#19370,#19371,#19372,#19373,#19374,#19375,#19376,
#19377,#19378,#19379,#19380,#19381,#19382,#19383,#19384,#19385,#19386,#19387,
#19388,#19389,#19390,#19391,#19392,#19393,#19394,#19395,#19396,#19397,#19398,
#19399,#19400,#19401,#19402,#19403,#19404,#19405,#19406,#19407,#19408,#19409,
#19410,#19411,#19412,#19413,#19414,#19415,#19416,#19417,#19418,#19419,#19420,
#19421,#19422,#19423,#19424,#19425,#19426,#19427,#19428,#19429,#19430,#19431,
#19432,#19433,#19434,#19435,#19436,#19437,#19438,#19439,#19440,#19441,#19442,
#19443,#19444,#19445,#19446,#19447,#19448,#19449,#19450,#19451,#19452,#19453,
#19454,#19455,#19456,#19457,#19458,#19459,#19460,#19461,#19462,#19463,#19464,
#19465,#19466,#19467,#19468,#19469,#19470));
#20120=CLOSED_SHELL('',(#19471,#19472,#19473,#19474,#19475,#19476,#19477,
#19478,#19479,#19480,#19481,#19482,#19483,#19484,#19485,#19486,#19487,#19488,
#19489,#19490,#19491,#19492,#19493,#19494,#19495,#19496,#19497,#19498,#19499,
#19500,#19501,#19502,#19503,#19504,#19505,#19506,#19507,#19508,#19509,#19510,
#19511,#19512,#19513,#19514,#19515,#19516,#19517,#19518,#19519,#19520,#19521,
#19522,#19523,#19524,#19525,#19526,#19527,#19528,#19529,#19530,#19531,#19532,
#19533,#19534,#19535,#19536,#19537,#19538,#19539,#19540,#19541,#19542,#19543,
#19544,#19545,#19546,#19547,#19548,#19549,#19550,#19551,#19552,#19553));
#20121=CLOSED_SHELL('',(#19554,#19555,#19556,#19557,#19558,#19559,#19560,
#19561,#19562,#19563,#19564,#19565,#19566,#19567,#19568,#19569,#19570,#19571,
#19572,#19573,#19574,#19575,#19576,#19577,#19578,#19579,#19580,#19581,#19582,
#19583,#19584,#19585,#19586,#19587,#19588,#19589,#19590,#19591,#19592,#19593,
#19594,#19595,#19596,#19597,#19598,#19599,#19600,#19601,#19602,#19603,#19604,
#19605,#19606,#19607,#19608,#19609,#19610,#19611,#19612,#19613,#19614,#19615,
#19616));
#20122=CLOSED_SHELL('',(#19617,#19618,#19619,#19620,#19621,#19622,#19623,
#19624,#19625,#19626,#19627,#19628,#19629,#19630,#19631,#19632,#19633,#19634,
#19635,#19636,#19637,#19638,#19639,#19640,#19641,#19642,#19643,#19644,#19645,
#19646,#19647,#19648,#19649,#19650,#19651,#19652,#19653,#19654,#19655,#19656,
#19657,#19658,#19659,#19660,#19661,#19662,#19663,#19664,#19665,#19666,#19667,
#19668,#19669,#19670,#19671,#19672,#19673));
#20123=CLOSED_SHELL('',(#19674,#19675,#19676,#19677,#19678,#19679,#19680,
#19681,#19682,#19683,#19684,#19685,#19686,#19687,#19688,#19689,#19690,#19691,
#19692,#19693,#19694,#19695,#19696,#19697,#19698,#19699,#19700,#19701,#19702,
#19703,#19704,#19705,#19706,#19707,#19708,#19709,#19710,#19711,#19712,#19713,
#19714,#19715,#19716,#19717,#19718,#19719,#19720,#19721,#19722,#19723,#19724,
#19725,#19726,#19727,#19728,#19729,#19730,#19731,#19732,#19733,#19734,#19735,
#19736,#19737,#19738,#19739,#19740,#19741,#19742,#19743,#19744,#19745,#19746,
#19747,#19748,#19749,#19750,#19751,#19752,#19753,#19754,#19755,#19756,#19757,
#19758,#19759,#19760,#19761,#19762,#19763,#19764,#19765,#19766,#19767,#19768,
#19769,#19770,#19771,#19772,#19773,#19774,#19775,#19776,#19777,#19778,#19779,
#19780,#19781,#19782,#19783,#19784,#19785,#19786,#19787,#19788,#19789,#19790,
#19791,#19792,#19793,#19794,#19795,#19796,#19797,#19798,#19799,#19800,#19801,
#19802,#19803,#19804,#19805,#19806,#19807,#19808,#19809,#19810,#19811,#19812,
#19813,#19814,#19815,#19816,#19817,#19818,#19819,#19820,#19821,#19822,#19823,
#19824,#19825,#19826,#19827,#19828,#19829,#19830,#19831,#19832,#19833,#19834,
#19835,#19836,#19837,#19838,#19839,#19840,#19841,#19842,#19843,#19844,#19845,
#19846,#19847,#19848,#19849,#19850,#19851,#19852,#19853,#19854,#19855,#19856,
#19857,#19858,#19859,#19860,#19861,#19862,#19863,#19864,#19865,#19866,#19867,
#19868,#19869,#19870,#19871,#19872,#19873,#19874,#19875,#19876,#19877,#19878,
#19879,#19880,#19881,#19882,#19883,#19884,#19885,#19886,#19887,#19888,#19889,
#19890,#19891,#19892,#19893,#19894,#19895,#19896,#19897,#19898,#19899,#19900,
#19901,#19902,#19903,#19904,#19905,#19906,#19907,#19908,#19909,#19910,#19911,
#19912,#19913,#19914,#19915,#19916,#19917,#19918,#19919,#19920,#19921,#19922,
#19923,#19924,#19925,#19926,#19927,#19928,#19929,#19930,#19931,#19932,#19933,
#19934,#19935,#19936,#19937,#19938));
#20124=CLOSED_SHELL('',(#19939,#19940,#19941,#19942,#19943,#19944));
#20125=CLOSED_SHELL('',(#19945,#19946,#19947,#19948,#19949,#19950,#19951,
#19952,#19953,#19954,#19955,#19956,#19957,#19958,#19959,#19960,#19961,#19962,
#19963,#19964,#19965,#19966,#19967,#19968,#19969,#19970,#19971,#19972));
#20126=CLOSED_SHELL('',(#19973,#19974,#19975,#19976,#19977,#19978,#19979,
#19980,#19981,#19982,#19983,#19984,#19985,#19986,#19987,#19988,#19989,#19990,
#19991,#19992,#19993,#19994,#19995,#19996,#19997,#19998,#19999,#20000,#20001,
#20002,#20003,#20004,#20005,#20006,#20007,#20008,#20009,#20010,#20011,#20012,
#20013,#20014,#20015,#20016,#20017,#20018,#20019,#20020,#20021,#20022,#20023,
#20024,#20025,#20026,#20027,#20028,#20029,#20030,#20031,#20032,#20033,#20034,
#20035,#20036,#20037,#20038,#20039,#20040,#20041,#20042,#20043));
#20127=CLOSED_SHELL('',(#20044,#20045,#20046,#20047,#20048,#20049,#20050,
#20051,#20052,#20053,#20054,#20055,#20056,#20057,#20058,#20059,#20060,#20061,
#20062,#20063,#20064,#20065,#20066,#20067,#20068,#20069));
#20128=CLOSED_SHELL('',(#20070,#20071,#20072,#20073,#20074,#20075));
#20129=CLOSED_SHELL('',(#20076,#20077,#20078,#20079,#20080));
#20130=CLOSED_SHELL('',(#20081,#20082,#20083,#20084,#20085));
#20131=CLOSED_SHELL('',(#20086,#20087,#20088,#20089,#20090,#20091,#20092,
#20093,#20094,#20095,#20096,#20097,#20098,#20099));
#20132=CLOSED_SHELL('',(#20100,#20101,#20102,#20103,#20104));
#20133=CLOSED_SHELL('',(#20105,#20106,#20107,#20108,#20109,#20110,#20111));
#20134=CLOSED_SHELL('',(#20112,#20113,#20114,#20115,#20116));
#20135=DERIVED_UNIT_ELEMENT(#20171,1.);
#20136=DERIVED_UNIT_ELEMENT(#100033,-3.);
#20137=DERIVED_UNIT_ELEMENT(#20171,1.);
#20138=DERIVED_UNIT_ELEMENT(#100033,-3.);
#20139=DERIVED_UNIT_ELEMENT(#20171,1.);
#20140=DERIVED_UNIT_ELEMENT(#100033,-3.);
#20141=DERIVED_UNIT_ELEMENT(#20171,1.);
#20142=DERIVED_UNIT_ELEMENT(#100033,-3.);
#20143=DERIVED_UNIT_ELEMENT(#20171,1.);
#20144=DERIVED_UNIT_ELEMENT(#100033,-3.);
#20145=DERIVED_UNIT_ELEMENT(#20171,1.);
#20146=DERIVED_UNIT_ELEMENT(#100033,-3.);
#20147=DERIVED_UNIT_ELEMENT(#20171,1.);
#20148=DERIVED_UNIT_ELEMENT(#100033,-3.);
#20149=DERIVED_UNIT_ELEMENT(#20171,1.);
#20150=DERIVED_UNIT_ELEMENT(#100033,-3.);
#20151=DERIVED_UNIT_ELEMENT(#20171,1.);
#20152=DERIVED_UNIT_ELEMENT(#100033,-3.);
#20153=DERIVED_UNIT_ELEMENT(#20171,1.);
#20154=DERIVED_UNIT_ELEMENT(#100033,-3.);
#20155=DERIVED_UNIT_ELEMENT(#20171,1.);
#20156=DERIVED_UNIT_ELEMENT(#100033,-3.);
#20157=DERIVED_UNIT_ELEMENT(#20171,1.);
#20158=DERIVED_UNIT_ELEMENT(#100033,-3.);
#20159=DERIVED_UNIT_ELEMENT(#20171,1.);
#20160=DERIVED_UNIT_ELEMENT(#100033,-3.);
#20161=DERIVED_UNIT_ELEMENT(#20171,1.);
#20162=DERIVED_UNIT_ELEMENT(#100033,-3.);
#20163=DERIVED_UNIT_ELEMENT(#20171,1.);
#20164=DERIVED_UNIT_ELEMENT(#100033,-3.);
#20165=DERIVED_UNIT_ELEMENT(#20171,1.);
#20166=DERIVED_UNIT_ELEMENT(#100033,-3.);
#20167=DERIVED_UNIT_ELEMENT(#20171,1.);
#20168=DERIVED_UNIT_ELEMENT(#100033,-3.);
#20169=DERIVED_UNIT_ELEMENT(#20171,1.);
#20170=DERIVED_UNIT_ELEMENT(#100033,-3.);
#20171=(
MASS_UNIT()
NAMED_UNIT(*)
SI_UNIT(.KILO.,.GRAM.)
);
#20172=DERIVED_UNIT((#20135,#20136));
#20173=DERIVED_UNIT((#20137,#20138));
#20174=DERIVED_UNIT((#20139,#20140));
#20175=DERIVED_UNIT((#20141,#20142));
#20176=DERIVED_UNIT((#20143,#20144));
#20177=DERIVED_UNIT((#20145,#20146));
#20178=DERIVED_UNIT((#20147,#20148));
#20179=DERIVED_UNIT((#20149,#20150));
#20180=DERIVED_UNIT((#20151,#20152));
#20181=DERIVED_UNIT((#20153,#20154));
#20182=DERIVED_UNIT((#20155,#20156));
#20183=DERIVED_UNIT((#20157,#20158));
#20184=DERIVED_UNIT((#20159,#20160));
#20185=DERIVED_UNIT((#20161,#20162));
#20186=DERIVED_UNIT((#20163,#20164));
#20187=DERIVED_UNIT((#20165,#20166));
#20188=DERIVED_UNIT((#20167,#20168));
#20189=DERIVED_UNIT((#20169,#20170));
#20190=MEASURE_REPRESENTATION_ITEM('density measure',
POSITIVE_RATIO_MEASURE(7850.),#20172);
#20191=MEASURE_REPRESENTATION_ITEM('density measure',
POSITIVE_RATIO_MEASURE(7850.),#20173);
#20192=MEASURE_REPRESENTATION_ITEM('density measure',
POSITIVE_RATIO_MEASURE(7850.),#20174);
#20193=MEASURE_REPRESENTATION_ITEM('density measure',
POSITIVE_RATIO_MEASURE(7850.),#20175);
#20194=MEASURE_REPRESENTATION_ITEM('density measure',
POSITIVE_RATIO_MEASURE(7850.),#20176);
#20195=MEASURE_REPRESENTATION_ITEM('density measure',
POSITIVE_RATIO_MEASURE(7850.),#20177);
#20196=MEASURE_REPRESENTATION_ITEM('density measure',
POSITIVE_RATIO_MEASURE(7850.),#20178);
#20197=MEASURE_REPRESENTATION_ITEM('density measure',
POSITIVE_RATIO_MEASURE(7850.),#20179);
#20198=MEASURE_REPRESENTATION_ITEM('density measure',
POSITIVE_RATIO_MEASURE(7850.),#20180);
#20199=MEASURE_REPRESENTATION_ITEM('density measure',
POSITIVE_RATIO_MEASURE(7850.),#20181);
#20200=MEASURE_REPRESENTATION_ITEM('density measure',
POSITIVE_RATIO_MEASURE(7850.),#20182);
#20201=MEASURE_REPRESENTATION_ITEM('density measure',
POSITIVE_RATIO_MEASURE(7850.),#20183);
#20202=MEASURE_REPRESENTATION_ITEM('density measure',
POSITIVE_RATIO_MEASURE(7850.),#20184);
#20203=MEASURE_REPRESENTATION_ITEM('density measure',
POSITIVE_RATIO_MEASURE(7850.),#20185);
#20204=MEASURE_REPRESENTATION_ITEM('density measure',
POSITIVE_RATIO_MEASURE(7850.),#20186);
#20205=MEASURE_REPRESENTATION_ITEM('density measure',
POSITIVE_RATIO_MEASURE(7850.),#20187);
#20206=MEASURE_REPRESENTATION_ITEM('density measure',
POSITIVE_RATIO_MEASURE(7850.),#20188);
#20207=MEASURE_REPRESENTATION_ITEM('density measure',
POSITIVE_RATIO_MEASURE(7850.),#20189);
#20208=PROPERTY_DEFINITION_REPRESENTATION(#20298,#20244);
#20209=PROPERTY_DEFINITION_REPRESENTATION(#20299,#20245);
#20210=PROPERTY_DEFINITION_REPRESENTATION(#20300,#20246);
#20211=PROPERTY_DEFINITION_REPRESENTATION(#20301,#20247);
#20212=PROPERTY_DEFINITION_REPRESENTATION(#20302,#20248);
#20213=PROPERTY_DEFINITION_REPRESENTATION(#20303,#20249);
#20214=PROPERTY_DEFINITION_REPRESENTATION(#20304,#20250);
#20215=PROPERTY_DEFINITION_REPRESENTATION(#20305,#20251);
#20216=PROPERTY_DEFINITION_REPRESENTATION(#20306,#20252);
#20217=PROPERTY_DEFINITION_REPRESENTATION(#20307,#20253);
#20218=PROPERTY_DEFINITION_REPRESENTATION(#20308,#20254);
#20219=PROPERTY_DEFINITION_REPRESENTATION(#20309,#20255);
#20220=PROPERTY_DEFINITION_REPRESENTATION(#20310,#20256);
#20221=PROPERTY_DEFINITION_REPRESENTATION(#20311,#20257);
#20222=PROPERTY_DEFINITION_REPRESENTATION(#20312,#20258);
#20223=PROPERTY_DEFINITION_REPRESENTATION(#20313,#20259);
#20224=PROPERTY_DEFINITION_REPRESENTATION(#20314,#20260);
#20225=PROPERTY_DEFINITION_REPRESENTATION(#20315,#20261);
#20226=PROPERTY_DEFINITION_REPRESENTATION(#20316,#20262);
#20227=PROPERTY_DEFINITION_REPRESENTATION(#20317,#20263);
#20228=PROPERTY_DEFINITION_REPRESENTATION(#20318,#20264);
#20229=PROPERTY_DEFINITION_REPRESENTATION(#20319,#20265);
#20230=PROPERTY_DEFINITION_REPRESENTATION(#20320,#20266);
#20231=PROPERTY_DEFINITION_REPRESENTATION(#20321,#20267);
#20232=PROPERTY_DEFINITION_REPRESENTATION(#20322,#20268);
#20233=PROPERTY_DEFINITION_REPRESENTATION(#20323,#20269);
#20234=PROPERTY_DEFINITION_REPRESENTATION(#20324,#20270);
#20235=PROPERTY_DEFINITION_REPRESENTATION(#20325,#20271);
#20236=PROPERTY_DEFINITION_REPRESENTATION(#20326,#20272);
#20237=PROPERTY_DEFINITION_REPRESENTATION(#20327,#20273);
#20238=PROPERTY_DEFINITION_REPRESENTATION(#20328,#20274);
#20239=PROPERTY_DEFINITION_REPRESENTATION(#20329,#20275);
#20240=PROPERTY_DEFINITION_REPRESENTATION(#20330,#20276);
#20241=PROPERTY_DEFINITION_REPRESENTATION(#20331,#20277);
#20242=PROPERTY_DEFINITION_REPRESENTATION(#20332,#20278);
#20243=PROPERTY_DEFINITION_REPRESENTATION(#20333,#20279);
#20244=REPRESENTATION('material name',(#20280),#100013);
#20245=REPRESENTATION('density',(#20190),#100013);
#20246=REPRESENTATION('material name',(#20281),#100014);
#20247=REPRESENTATION('density',(#20191),#100014);
#20248=REPRESENTATION('material name',(#20282),#100015);
#20249=REPRESENTATION('density',(#20192),#100015);
#20250=REPRESENTATION('material name',(#20283),#100016);
#20251=REPRESENTATION('density',(#20193),#100016);
#20252=REPRESENTATION('material name',(#20284),#100017);
#20253=REPRESENTATION('density',(#20194),#100017);
#20254=REPRESENTATION('material name',(#20285),#100018);
#20255=REPRESENTATION('density',(#20195),#100018);
#20256=REPRESENTATION('material name',(#20286),#100019);
#20257=REPRESENTATION('density',(#20196),#100019);
#20258=REPRESENTATION('material name',(#20287),#100020);
#20259=REPRESENTATION('density',(#20197),#100020);
#20260=REPRESENTATION('material name',(#20288),#100021);
#20261=REPRESENTATION('density',(#20198),#100021);
#20262=REPRESENTATION('material name',(#20289),#100022);
#20263=REPRESENTATION('density',(#20199),#100022);
#20264=REPRESENTATION('material name',(#20290),#100023);
#20265=REPRESENTATION('density',(#20200),#100023);
#20266=REPRESENTATION('material name',(#20291),#100024);
#20267=REPRESENTATION('density',(#20201),#100024);
#20268=REPRESENTATION('material name',(#20292),#100025);
#20269=REPRESENTATION('density',(#20202),#100025);
#20270=REPRESENTATION('material name',(#20293),#100026);
#20271=REPRESENTATION('density',(#20203),#100026);
#20272=REPRESENTATION('material name',(#20294),#100027);
#20273=REPRESENTATION('density',(#20204),#100027);
#20274=REPRESENTATION('material name',(#20295),#100028);
#20275=REPRESENTATION('density',(#20205),#100028);
#20276=REPRESENTATION('material name',(#20296),#100029);
#20277=REPRESENTATION('density',(#20206),#100029);
#20278=REPRESENTATION('material name',(#20297),#100030);
#20279=REPRESENTATION('density',(#20207),#100030);
#20280=DESCRIPTIVE_REPRESENTATION_ITEM('Steel','Steel');
#20281=DESCRIPTIVE_REPRESENTATION_ITEM('Steel','Steel');
#20282=DESCRIPTIVE_REPRESENTATION_ITEM('Steel','Steel');
#20283=DESCRIPTIVE_REPRESENTATION_ITEM('Steel','Steel');
#20284=DESCRIPTIVE_REPRESENTATION_ITEM('Steel','Steel');
#20285=DESCRIPTIVE_REPRESENTATION_ITEM('Steel','Steel');
#20286=DESCRIPTIVE_REPRESENTATION_ITEM('Steel','Steel');
#20287=DESCRIPTIVE_REPRESENTATION_ITEM('Steel','Steel');
#20288=DESCRIPTIVE_REPRESENTATION_ITEM('Steel','Steel');
#20289=DESCRIPTIVE_REPRESENTATION_ITEM('Steel','Steel');
#20290=DESCRIPTIVE_REPRESENTATION_ITEM('Steel','Steel');
#20291=DESCRIPTIVE_REPRESENTATION_ITEM('Steel','Steel');
#20292=DESCRIPTIVE_REPRESENTATION_ITEM('Steel','Steel');
#20293=DESCRIPTIVE_REPRESENTATION_ITEM('Steel','Steel');
#20294=DESCRIPTIVE_REPRESENTATION_ITEM('Steel','Steel');
#20295=DESCRIPTIVE_REPRESENTATION_ITEM('Steel','Steel');
#20296=DESCRIPTIVE_REPRESENTATION_ITEM('Steel','Steel');
#20297=DESCRIPTIVE_REPRESENTATION_ITEM('Steel','Steel');
#20298=PROPERTY_DEFINITION('material property','material name',#100121);
#20299=PROPERTY_DEFINITION('material property','density of part',#100121);
#20300=PROPERTY_DEFINITION('material property','material name',#100122);
#20301=PROPERTY_DEFINITION('material property','density of part',#100122);
#20302=PROPERTY_DEFINITION('material property','material name',#100123);
#20303=PROPERTY_DEFINITION('material property','density of part',#100123);
#20304=PROPERTY_DEFINITION('material property','material name',#100124);
#20305=PROPERTY_DEFINITION('material property','density of part',#100124);
#20306=PROPERTY_DEFINITION('material property','material name',#100125);
#20307=PROPERTY_DEFINITION('material property','density of part',#100125);
#20308=PROPERTY_DEFINITION('material property','material name',#100126);
#20309=PROPERTY_DEFINITION('material property','density of part',#100126);
#20310=PROPERTY_DEFINITION('material property','material name',#100127);
#20311=PROPERTY_DEFINITION('material property','density of part',#100127);
#20312=PROPERTY_DEFINITION('material property','material name',#100128);
#20313=PROPERTY_DEFINITION('material property','density of part',#100128);
#20314=PROPERTY_DEFINITION('material property','material name',#100129);
#20315=PROPERTY_DEFINITION('material property','density of part',#100129);
#20316=PROPERTY_DEFINITION('material property','material name',#100130);
#20317=PROPERTY_DEFINITION('material property','density of part',#100130);
#20318=PROPERTY_DEFINITION('material property','material name',#100131);
#20319=PROPERTY_DEFINITION('material property','density of part',#100131);
#20320=PROPERTY_DEFINITION('material property','material name',#100132);
#20321=PROPERTY_DEFINITION('material property','density of part',#100132);
#20322=PROPERTY_DEFINITION('material property','material name',#100133);
#20323=PROPERTY_DEFINITION('material property','density of part',#100133);
#20324=PROPERTY_DEFINITION('material property','material name',#100134);
#20325=PROPERTY_DEFINITION('material property','density of part',#100134);
#20326=PROPERTY_DEFINITION('material property','material name',#100135);
#20327=PROPERTY_DEFINITION('material property','density of part',#100135);
#20328=PROPERTY_DEFINITION('material property','material name',#100136);
#20329=PROPERTY_DEFINITION('material property','density of part',#100136);
#20330=PROPERTY_DEFINITION('material property','material name',#100137);
#20331=PROPERTY_DEFINITION('material property','density of part',#100137);
#20332=PROPERTY_DEFINITION('material property','material name',#100138);
#20333=PROPERTY_DEFINITION('material property','density of part',#100138);
#20334=AXIS2_PLACEMENT_3D('',#28194,#22525,#22526);
#20335=AXIS2_PLACEMENT_3D('',#28195,#22527,#22528);
#20336=AXIS2_PLACEMENT_3D('',#28807,#22529,#22530);
#20337=AXIS2_PLACEMENT_3D('',#40840,#22532,#22533);
#20338=AXIS2_PLACEMENT_3D('',#54981,#22534,#22535);
#20339=AXIS2_PLACEMENT_3D('',#55726,#22536,#22537);
#20340=AXIS2_PLACEMENT_3D('',#56080,#22539,#22540);
#20341=AXIS2_PLACEMENT_3D('',#56332,#22542,#22543);
#20342=AXIS2_PLACEMENT_3D('',#56726,#22549,#22550);
#20343=AXIS2_PLACEMENT_3D('',#59065,#22633,#22634);
#20344=AXIS2_PLACEMENT_3D('',#59066,#22635,#22636);
#20345=AXIS2_PLACEMENT_3D('',#59069,#22637,#22638);
#20346=AXIS2_PLACEMENT_3D('',#59071,#22639,#22640);
#20347=AXIS2_PLACEMENT_3D('',#59073,#22641,#22642);
#20348=AXIS2_PLACEMENT_3D('',#59074,#22643,#22644);
#20349=AXIS2_PLACEMENT_3D('',#59075,#22645,#22646);
#20350=AXIS2_PLACEMENT_3D('',#59076,#22647,#22648);
#20351=AXIS2_PLACEMENT_3D('',#59079,#22649,#22650);
#20352=AXIS2_PLACEMENT_3D('',#59080,#22651,#22652);
#20353=AXIS2_PLACEMENT_3D('',#59082,#22654,#22655);
#20354=AXIS2_PLACEMENT_3D('',#59086,#22657,#22658);
#20355=AXIS2_PLACEMENT_3D('',#59087,#22659,#22660);
#20356=AXIS2_PLACEMENT_3D('',#59088,#22661,#22662);
#20357=AXIS2_PLACEMENT_3D('',#59091,#22663,#22664);
#20358=AXIS2_PLACEMENT_3D('',#59095,#22666,#22667);
#20359=AXIS2_PLACEMENT_3D('',#59097,#22669,#22670);
#20360=AXIS2_PLACEMENT_3D('',#59099,#22671,#22672);
#20361=AXIS2_PLACEMENT_3D('',#59100,#22673,#22674);
#20362=AXIS2_PLACEMENT_3D('',#59101,#22675,#22676);
#20363=AXIS2_PLACEMENT_3D('',#59103,#22677,#22678);
#20364=AXIS2_PLACEMENT_3D('',#59104,#22679,#22680);
#20365=AXIS2_PLACEMENT_3D('',#59105,#22681,#22682);
#20366=AXIS2_PLACEMENT_3D('',#59109,#22684,#22685);
#20367=AXIS2_PLACEMENT_3D('',#59111,#22687,#22688);
#20368=AXIS2_PLACEMENT_3D('',#59113,#22689,#22690);
#20369=AXIS2_PLACEMENT_3D('',#59115,#22691,#22692);
#20370=AXIS2_PLACEMENT_3D('',#59116,#22693,#22694);
#20371=AXIS2_PLACEMENT_3D('',#59117,#22695,#22696);
#20372=AXIS2_PLACEMENT_3D('',#59119,#22697,#22698);
#20373=AXIS2_PLACEMENT_3D('',#59121,#22700,#22701);
#20374=AXIS2_PLACEMENT_3D('',#59123,#22702,#22703);
#20375=AXIS2_PLACEMENT_3D('',#59127,#22705,#22706);
#20376=AXIS2_PLACEMENT_3D('',#59129,#22708,#22709);
#20377=AXIS2_PLACEMENT_3D('',#59131,#22710,#22711);
#20378=AXIS2_PLACEMENT_3D('',#59132,#22712,#22713);
#20379=AXIS2_PLACEMENT_3D('',#59133,#22714,#22715);
#20380=AXIS2_PLACEMENT_3D('',#59134,#22716,#22717);
#20381=AXIS2_PLACEMENT_3D('',#59135,#22718,#22719);
#20382=AXIS2_PLACEMENT_3D('',#59137,#22720,#22721);
#20383=AXIS2_PLACEMENT_3D('',#59139,#22722,#22723);
#20384=AXIS2_PLACEMENT_3D('',#59140,#22724,#22725);
#20385=AXIS2_PLACEMENT_3D('',#59141,#22726,#22727);
#20386=AXIS2_PLACEMENT_3D('',#59143,#22729,#22730);
#20387=AXIS2_PLACEMENT_3D('',#59146,#22731,#22732);
#20388=AXIS2_PLACEMENT_3D('',#59149,#22734,#22735);
#20389=AXIS2_PLACEMENT_3D('',#59151,#22737,#22738);
#20390=AXIS2_PLACEMENT_3D('',#59152,#22739,#22740);
#20391=AXIS2_PLACEMENT_3D('',#59153,#22741,#22742);
#20392=AXIS2_PLACEMENT_3D('',#59155,#22743,#22744);
#20393=AXIS2_PLACEMENT_3D('',#59156,#22745,#22746);
#20394=AXIS2_PLACEMENT_3D('',#59157,#22747,#22748);
#20395=AXIS2_PLACEMENT_3D('',#59161,#22750,#22751);
#20396=AXIS2_PLACEMENT_3D('',#59163,#22753,#22754);
#20397=AXIS2_PLACEMENT_3D('',#59164,#22755,#22756);
#20398=AXIS2_PLACEMENT_3D('',#59165,#22757,#22758);
#20399=AXIS2_PLACEMENT_3D('',#59167,#22759,#22760);
#20400=AXIS2_PLACEMENT_3D('',#59171,#22762,#22763);
#20401=AXIS2_PLACEMENT_3D('',#59173,#22765,#22766);
#20402=AXIS2_PLACEMENT_3D('',#59175,#22767,#22768);
#20403=AXIS2_PLACEMENT_3D('',#59176,#22769,#22770);
#20404=AXIS2_PLACEMENT_3D('',#59177,#22771,#22772);
#20405=AXIS2_PLACEMENT_3D('',#59178,#22773,#22774);
#20406=AXIS2_PLACEMENT_3D('',#59179,#22775,#22776);
#20407=AXIS2_PLACEMENT_3D('',#59181,#22777,#22778);
#20408=AXIS2_PLACEMENT_3D('',#59183,#22779,#22780);
#20409=AXIS2_PLACEMENT_3D('',#59184,#22781,#22782);
#20410=AXIS2_PLACEMENT_3D('',#59185,#22783,#22784);
#20411=AXIS2_PLACEMENT_3D('',#59187,#22786,#22787);
#20412=AXIS2_PLACEMENT_3D('',#59190,#22788,#22789);
#20413=AXIS2_PLACEMENT_3D('',#59194,#22791,#22792);
#20414=AXIS2_PLACEMENT_3D('',#59196,#22794,#22795);
#20415=AXIS2_PLACEMENT_3D('',#59198,#22796,#22797);
#20416=AXIS2_PLACEMENT_3D('',#59199,#22798,#22799);
#20417=AXIS2_PLACEMENT_3D('',#59200,#22800,#22801);
#20418=AXIS2_PLACEMENT_3D('',#59202,#22802,#22803);
#20419=AXIS2_PLACEMENT_3D('',#59203,#22804,#22805);
#20420=AXIS2_PLACEMENT_3D('',#59204,#22806,#22807);
#20421=AXIS2_PLACEMENT_3D('',#59206,#22808,#22809);
#20422=AXIS2_PLACEMENT_3D('',#59208,#22810,#22811);
#20423=AXIS2_PLACEMENT_3D('',#59209,#22812,#22813);
#20424=AXIS2_PLACEMENT_3D('',#59210,#22814,#22815);
#20425=AXIS2_PLACEMENT_3D('',#59214,#22817,#22818);
#20426=AXIS2_PLACEMENT_3D('',#59216,#22820,#22821);
#20427=AXIS2_PLACEMENT_3D('',#59220,#22824,#22825);
#20428=AXIS2_PLACEMENT_3D('',#59223,#22826,#22827);
#20429=AXIS2_PLACEMENT_3D('',#59226,#22829,#22830);
#20430=AXIS2_PLACEMENT_3D('',#59228,#22832,#22833);
#20431=AXIS2_PLACEMENT_3D('',#59229,#22834,#22835);
#20432=AXIS2_PLACEMENT_3D('',#59230,#22836,#22837);
#20433=AXIS2_PLACEMENT_3D('',#59232,#22838,#22839);
#20434=AXIS2_PLACEMENT_3D('',#59233,#22840,#22841);
#20435=AXIS2_PLACEMENT_3D('',#59234,#22842,#22843);
#20436=AXIS2_PLACEMENT_3D('',#59238,#22845,#22846);
#20437=AXIS2_PLACEMENT_3D('',#59240,#22848,#22849);
#20438=AXIS2_PLACEMENT_3D('',#59241,#22850,#22851);
#20439=AXIS2_PLACEMENT_3D('',#59242,#22852,#22853);
#20440=AXIS2_PLACEMENT_3D('',#59244,#22854,#22855);
#20441=AXIS2_PLACEMENT_3D('',#59246,#22856,#22857);
#20442=AXIS2_PLACEMENT_3D('',#59248,#22858,#22859);
#20443=AXIS2_PLACEMENT_3D('',#59249,#22860,#22861);
#20444=AXIS2_PLACEMENT_3D('',#59250,#22862,#22863);
#20445=AXIS2_PLACEMENT_3D('',#59297,#22886,#22887);
#20446=AXIS2_PLACEMENT_3D('',#59300,#22889,#22890);
#20447=AXIS2_PLACEMENT_3D('',#59305,#22892,#22893);
#20448=AXIS2_PLACEMENT_3D('',#59308,#22895,#22896);
#20449=AXIS2_PLACEMENT_3D('',#59312,#22898,#22899);
#20450=AXIS2_PLACEMENT_3D('',#59316,#22901,#22902);
#20451=AXIS2_PLACEMENT_3D('',#59320,#22904,#22905);
#20452=AXIS2_PLACEMENT_3D('',#59322,#22907,#22908);
#20453=AXIS2_PLACEMENT_3D('',#59324,#22909,#22910);
#20454=AXIS2_PLACEMENT_3D('',#59327,#22911,#22912);
#20455=AXIS2_PLACEMENT_3D('',#59330,#22914,#22915);
#20456=AXIS2_PLACEMENT_3D('',#59332,#22917,#22918);
#20457=AXIS2_PLACEMENT_3D('',#59335,#22920,#22921);
#20458=AXIS2_PLACEMENT_3D('',#59338,#22923,#22924);
#20459=AXIS2_PLACEMENT_3D('',#59339,#22925,#22926);
#20460=AXIS2_PLACEMENT_3D('',#59343,#22928,#22929);
#20461=AXIS2_PLACEMENT_3D('',#59344,#22930,#22931);
#20462=AXIS2_PLACEMENT_3D('',#59345,#22932,#22933);
#20463=AXIS2_PLACEMENT_3D('',#59347,#22934,#22935);
#20464=AXIS2_PLACEMENT_3D('',#59349,#22936,#22937);
#20465=AXIS2_PLACEMENT_3D('',#59350,#22938,#22939);
#20466=AXIS2_PLACEMENT_3D('',#59351,#22940,#22941);
#20467=AXIS2_PLACEMENT_3D('',#59355,#22943,#22944);
#20468=AXIS2_PLACEMENT_3D('',#59356,#22945,#22946);
#20469=AXIS2_PLACEMENT_3D('',#59357,#22947,#22948);
#20470=AXIS2_PLACEMENT_3D('',#59358,#22949,#22950);
#20471=AXIS2_PLACEMENT_3D('',#59359,#22951,#22952);
#20472=AXIS2_PLACEMENT_3D('',#59361,#22953,#22954);
#20473=AXIS2_PLACEMENT_3D('',#59364,#22956,#22957);
#20474=AXIS2_PLACEMENT_3D('',#59365,#22958,#22959);
#20475=AXIS2_PLACEMENT_3D('',#59367,#22960,#22961);
#20476=AXIS2_PLACEMENT_3D('',#59368,#22962,#22963);
#20477=AXIS2_PLACEMENT_3D('',#59369,#22964,#22965);
#20478=AXIS2_PLACEMENT_3D('',#59371,#22966,#22967);
#20479=AXIS2_PLACEMENT_3D('',#59373,#22969,#22970);
#20480=AXIS2_PLACEMENT_3D('',#59374,#22971,#22972);
#20481=AXIS2_PLACEMENT_3D('',#59375,#22973,#22974);
#20482=AXIS2_PLACEMENT_3D('',#59379,#22976,#22977);
#20483=AXIS2_PLACEMENT_3D('',#59381,#22979,#22980);
#20484=AXIS2_PLACEMENT_3D('',#59385,#22983,#22984);
#20485=AXIS2_PLACEMENT_3D('',#59388,#22986,#22987);
#20486=AXIS2_PLACEMENT_3D('',#59389,#22988,#22989);
#20487=AXIS2_PLACEMENT_3D('',#59390,#22990,#22991);
#20488=AXIS2_PLACEMENT_3D('',#59391,#22992,#22993);
#20489=AXIS2_PLACEMENT_3D('',#59393,#22994,#22995);
#20490=AXIS2_PLACEMENT_3D('',#59394,#22996,#22997);
#20491=AXIS2_PLACEMENT_3D('',#59395,#22998,#22999);
#20492=AXIS2_PLACEMENT_3D('',#59396,#23000,#23001);
#20493=AXIS2_PLACEMENT_3D('',#59398,#23002,#23003);
#20494=AXIS2_PLACEMENT_3D('',#59399,#23004,#23005);
#20495=AXIS2_PLACEMENT_3D('',#59400,#23006,#23007);
#20496=AXIS2_PLACEMENT_3D('',#59402,#23009,#23010);
#20497=AXIS2_PLACEMENT_3D('',#59405,#23012,#23013);
#20498=AXIS2_PLACEMENT_3D('',#59406,#23014,#23015);
#20499=AXIS2_PLACEMENT_3D('',#59408,#23016,#23017);
#20500=AXIS2_PLACEMENT_3D('',#59409,#23018,#23019);
#20501=AXIS2_PLACEMENT_3D('',#59410,#23020,#23021);
#20502=AXIS2_PLACEMENT_3D('',#59412,#23022,#23023);
#20503=AXIS2_PLACEMENT_3D('',#59414,#23024,#23025);
#20504=AXIS2_PLACEMENT_3D('',#59416,#23027,#23028);
#20505=AXIS2_PLACEMENT_3D('',#59418,#23029,#23030);
#20506=AXIS2_PLACEMENT_3D('',#59419,#23031,#23032);
#20507=AXIS2_PLACEMENT_3D('',#59420,#23033,#23034);
#20508=AXIS2_PLACEMENT_3D('',#59422,#23035,#23036);
#20509=AXIS2_PLACEMENT_3D('',#59424,#23038,#23039);
#20510=AXIS2_PLACEMENT_3D('',#59427,#23040,#23041);
#20511=AXIS2_PLACEMENT_3D('',#59428,#23042,#23043);
#20512=AXIS2_PLACEMENT_3D('',#59429,#23044,#23045);
#20513=AXIS2_PLACEMENT_3D('',#59430,#23046,#23047);
#20514=AXIS2_PLACEMENT_3D('',#59432,#23048,#23049);
#20515=AXIS2_PLACEMENT_3D('',#59434,#23050,#23051);
#20516=AXIS2_PLACEMENT_3D('',#59435,#23052,#23053);
#20517=AXIS2_PLACEMENT_3D('',#59436,#23054,#23055);
#20518=AXIS2_PLACEMENT_3D('',#59438,#23057,#23058);
#20519=AXIS2_PLACEMENT_3D('',#59441,#23059,#23060);
#20520=AXIS2_PLACEMENT_3D('',#59442,#23061,#23062);
#20521=AXIS2_PLACEMENT_3D('',#59443,#23063,#23064);
#20522=AXIS2_PLACEMENT_3D('',#59444,#23065,#23066);
#20523=AXIS2_PLACEMENT_3D('',#59446,#23068,#23069);
#20524=AXIS2_PLACEMENT_3D('',#59449,#23070,#23071);
#20525=AXIS2_PLACEMENT_3D('',#59450,#23072,#23073);
#20526=AXIS2_PLACEMENT_3D('',#59451,#23074,#23075);
#20527=AXIS2_PLACEMENT_3D('',#59452,#23076,#23077);
#20528=AXIS2_PLACEMENT_3D('',#59454,#23079,#23080);
#20529=AXIS2_PLACEMENT_3D('',#59456,#23081,#23082);
#20530=AXIS2_PLACEMENT_3D('',#59458,#23084,#23085);
#20531=AXIS2_PLACEMENT_3D('',#59460,#23086,#23087);
#20532=AXIS2_PLACEMENT_3D('',#59461,#23088,#23089);
#20533=AXIS2_PLACEMENT_3D('',#59462,#23090,#23091);
#20534=AXIS2_PLACEMENT_3D('',#59465,#23092,#23093);
#20535=AXIS2_PLACEMENT_3D('',#59468,#23096,#23097);
#20536=AXIS2_PLACEMENT_3D('',#59470,#23098,#23099);
#20537=AXIS2_PLACEMENT_3D('',#59471,#23100,#23101);
#20538=AXIS2_PLACEMENT_3D('',#59472,#23102,#23103);
#20539=AXIS2_PLACEMENT_3D('',#59475,#23104,#23105);
#20540=AXIS2_PLACEMENT_3D('',#59478,#23108,#23109);
#20541=AXIS2_PLACEMENT_3D('',#59480,#23110,#23111);
#20542=AXIS2_PLACEMENT_3D('',#59481,#23112,#23113);
#20543=AXIS2_PLACEMENT_3D('',#59482,#23114,#23115);
#20544=AXIS2_PLACEMENT_3D('',#59485,#23116,#23117);
#20545=AXIS2_PLACEMENT_3D('',#59488,#23120,#23121);
#20546=AXIS2_PLACEMENT_3D('',#59490,#23122,#23123);
#20547=AXIS2_PLACEMENT_3D('',#59491,#23124,#23125);
#20548=AXIS2_PLACEMENT_3D('',#59492,#23126,#23127);
#20549=AXIS2_PLACEMENT_3D('',#59494,#23129,#23130);
#20550=AXIS2_PLACEMENT_3D('',#59496,#23132,#23133);
#20551=AXIS2_PLACEMENT_3D('',#59498,#23135,#23136);
#20552=AXIS2_PLACEMENT_3D('',#59502,#23138,#23139);
#20553=AXIS2_PLACEMENT_3D('',#59504,#23141,#23142);
#20554=AXIS2_PLACEMENT_3D('',#59506,#23144,#23145);
#20555=AXIS2_PLACEMENT_3D('',#59508,#23146,#23147);
#20556=AXIS2_PLACEMENT_3D('',#59510,#23148,#23149);
#20557=AXIS2_PLACEMENT_3D('',#59511,#23150,#23151);
#20558=AXIS2_PLACEMENT_3D('',#59512,#23152,#23153);
#20559=AXIS2_PLACEMENT_3D('',#59515,#23154,#23155);
#20560=AXIS2_PLACEMENT_3D('',#59517,#23156,#23157);
#20561=AXIS2_PLACEMENT_3D('',#59518,#23158,#23159);
#20562=AXIS2_PLACEMENT_3D('',#59519,#23160,#23161);
#20563=AXIS2_PLACEMENT_3D('',#59522,#23164,#23165);
#20564=AXIS2_PLACEMENT_3D('',#59524,#23166,#23167);
#20565=AXIS2_PLACEMENT_3D('',#59525,#23168,#23169);
#20566=AXIS2_PLACEMENT_3D('',#59526,#23170,#23171);
#20567=AXIS2_PLACEMENT_3D('',#59528,#23172,#23173);
#20568=AXIS2_PLACEMENT_3D('',#59529,#23174,#23175);
#20569=AXIS2_PLACEMENT_3D('',#59530,#23176,#23177);
#20570=AXIS2_PLACEMENT_3D('',#59532,#23178,#23179);
#20571=AXIS2_PLACEMENT_3D('',#59534,#23181,#23182);
#20572=AXIS2_PLACEMENT_3D('',#59536,#23183,#23184);
#20573=AXIS2_PLACEMENT_3D('',#59537,#23185,#23186);
#20574=AXIS2_PLACEMENT_3D('',#59538,#23187,#23188);
#20575=AXIS2_PLACEMENT_3D('',#59539,#23189,#23190);
#20576=AXIS2_PLACEMENT_3D('',#59540,#23191,#23192);
#20577=AXIS2_PLACEMENT_3D('',#59541,#23193,#23194);
#20578=AXIS2_PLACEMENT_3D('',#59542,#23195,#23196);
#20579=AXIS2_PLACEMENT_3D('',#59544,#23197,#23198);
#20580=AXIS2_PLACEMENT_3D('',#59545,#23199,#23200);
#20581=AXIS2_PLACEMENT_3D('',#59546,#23201,#23202);
#20582=AXIS2_PLACEMENT_3D('',#59547,#23203,#23204);
#20583=AXIS2_PLACEMENT_3D('',#59548,#23205,#23206);
#20584=AXIS2_PLACEMENT_3D('',#59549,#23207,#23208);
#20585=AXIS2_PLACEMENT_3D('',#59551,#23209,#23210);
#20586=AXIS2_PLACEMENT_3D('',#59553,#23211,#23212);
#20587=AXIS2_PLACEMENT_3D('',#59554,#23213,#23214);
#20588=AXIS2_PLACEMENT_3D('',#59555,#23215,#23216);
#20589=AXIS2_PLACEMENT_3D('',#59558,#23218,#23219);
#20590=AXIS2_PLACEMENT_3D('',#59560,#23221,#23222);
#20591=AXIS2_PLACEMENT_3D('',#59562,#23224,#23225);
#20592=AXIS2_PLACEMENT_3D('',#59564,#23227,#23228);
#20593=AXIS2_PLACEMENT_3D('',#59565,#23229,#23230);
#20594=AXIS2_PLACEMENT_3D('',#59566,#23231,#23232);
#20595=AXIS2_PLACEMENT_3D('',#59569,#23234,#23235);
#20596=AXIS2_PLACEMENT_3D('',#59570,#23236,#23237);
#20597=AXIS2_PLACEMENT_3D('',#59572,#23238,#23239);
#20598=AXIS2_PLACEMENT_3D('',#59574,#23240,#23241);
#20599=AXIS2_PLACEMENT_3D('',#59575,#23242,#23243);
#20600=AXIS2_PLACEMENT_3D('',#59576,#23244,#23245);
#20601=AXIS2_PLACEMENT_3D('',#59580,#23247,#23248);
#20602=AXIS2_PLACEMENT_3D('',#59581,#23249,#23250);
#20603=AXIS2_PLACEMENT_3D('',#59582,#23251,#23252);
#20604=AXIS2_PLACEMENT_3D('',#59585,#23253,#23254);
#20605=AXIS2_PLACEMENT_3D('',#59586,#23255,#23256);
#20606=AXIS2_PLACEMENT_3D('',#59587,#23257,#23258);
#20607=AXIS2_PLACEMENT_3D('',#59588,#23259,#23260);
#20608=AXIS2_PLACEMENT_3D('',#59590,#23262,#23263);
#20609=AXIS2_PLACEMENT_3D('',#59593,#23264,#23265);
#20610=AXIS2_PLACEMENT_3D('',#59594,#23266,#23267);
#20611=AXIS2_PLACEMENT_3D('',#59595,#23268,#23269);
#20612=AXIS2_PLACEMENT_3D('',#59596,#23270,#23271);
#20613=AXIS2_PLACEMENT_3D('',#59598,#23273,#23274);
#20614=AXIS2_PLACEMENT_3D('',#59601,#23275,#23276);
#20615=AXIS2_PLACEMENT_3D('',#59602,#23277,#23278);
#20616=AXIS2_PLACEMENT_3D('',#59603,#23279,#23280);
#20617=AXIS2_PLACEMENT_3D('',#59604,#23281,#23282);
#20618=AXIS2_PLACEMENT_3D('',#59606,#23284,#23285);
#20619=AXIS2_PLACEMENT_3D('',#59609,#23286,#23287);
#20620=AXIS2_PLACEMENT_3D('',#59610,#23288,#23289);
#20621=AXIS2_PLACEMENT_3D('',#59611,#23290,#23291);
#20622=AXIS2_PLACEMENT_3D('',#59612,#23292,#23293);
#20623=AXIS2_PLACEMENT_3D('',#59614,#23295,#23296);
#20624=AXIS2_PLACEMENT_3D('',#59617,#23298,#23299);
#20625=AXIS2_PLACEMENT_3D('',#59618,#23300,#23301);
#20626=AXIS2_PLACEMENT_3D('',#59620,#23302,#23303);
#20627=AXIS2_PLACEMENT_3D('',#59622,#23305,#23306);
#20628=AXIS2_PLACEMENT_3D('',#59625,#23307,#23308);
#20629=AXIS2_PLACEMENT_3D('',#59626,#23309,#23310);
#20630=AXIS2_PLACEMENT_3D('',#59627,#23311,#23312);
#20631=AXIS2_PLACEMENT_3D('',#59628,#23313,#23314);
#20632=AXIS2_PLACEMENT_3D('',#59630,#23316,#23317);
#20633=AXIS2_PLACEMENT_3D('',#59632,#23319,#23320);
#20634=AXIS2_PLACEMENT_3D('',#59635,#23321,#23322);
#20635=AXIS2_PLACEMENT_3D('',#59638,#23325,#23326);
#20636=AXIS2_PLACEMENT_3D('',#59640,#23327,#23328);
#20637=AXIS2_PLACEMENT_3D('',#59641,#23329,#23330);
#20638=AXIS2_PLACEMENT_3D('',#59642,#23331,#23332);
#20639=AXIS2_PLACEMENT_3D('',#59645,#23333,#23334);
#20640=AXIS2_PLACEMENT_3D('',#59648,#23337,#23338);
#20641=AXIS2_PLACEMENT_3D('',#59650,#23339,#23340);
#20642=AXIS2_PLACEMENT_3D('',#59651,#23341,#23342);
#20643=AXIS2_PLACEMENT_3D('',#59652,#23343,#23344);
#20644=AXIS2_PLACEMENT_3D('',#59655,#23345,#23346);
#20645=AXIS2_PLACEMENT_3D('',#59658,#23349,#23350);
#20646=AXIS2_PLACEMENT_3D('',#59660,#23351,#23352);
#20647=AXIS2_PLACEMENT_3D('',#59661,#23353,#23354);
#20648=AXIS2_PLACEMENT_3D('',#59662,#23355,#23356);
#20649=AXIS2_PLACEMENT_3D('',#59665,#23357,#23358);
#20650=AXIS2_PLACEMENT_3D('',#59668,#23361,#23362);
#20651=AXIS2_PLACEMENT_3D('',#59670,#23363,#23364);
#20652=AXIS2_PLACEMENT_3D('',#59671,#23365,#23366);
#20653=AXIS2_PLACEMENT_3D('',#59672,#23367,#23368);
#20654=AXIS2_PLACEMENT_3D('',#59675,#23369,#23370);
#20655=AXIS2_PLACEMENT_3D('',#59678,#23373,#23374);
#20656=AXIS2_PLACEMENT_3D('',#59680,#23375,#23376);
#20657=AXIS2_PLACEMENT_3D('',#59681,#23377,#23378);
#20658=AXIS2_PLACEMENT_3D('',#59682,#23379,#23380);
#20659=AXIS2_PLACEMENT_3D('',#59685,#23382,#23383);
#20660=AXIS2_PLACEMENT_3D('',#59686,#23384,#23385);
#20661=AXIS2_PLACEMENT_3D('',#59687,#23386,#23387);
#20662=AXIS2_PLACEMENT_3D('',#59688,#23388,#23389);
#20663=AXIS2_PLACEMENT_3D('',#59690,#23391,#23392);
#20664=AXIS2_PLACEMENT_3D('',#59693,#23395,#23396);
#20665=AXIS2_PLACEMENT_3D('',#59695,#23398,#23399);
#20666=AXIS2_PLACEMENT_3D('',#59697,#23401,#23402);
#20667=AXIS2_PLACEMENT_3D('',#59699,#23404,#23405);
#20668=AXIS2_PLACEMENT_3D('',#59703,#23407,#23408);
#20669=AXIS2_PLACEMENT_3D('',#59705,#23410,#23411);
#20670=AXIS2_PLACEMENT_3D('',#59707,#23413,#23414);
#20671=AXIS2_PLACEMENT_3D('',#59711,#23417,#23418);
#20672=AXIS2_PLACEMENT_3D('',#59713,#23420,#23421);
#20673=AXIS2_PLACEMENT_3D('',#59716,#23423,#23424);
#20674=AXIS2_PLACEMENT_3D('',#59717,#23425,#23426);
#20675=AXIS2_PLACEMENT_3D('',#59721,#23428,#23429);
#20676=AXIS2_PLACEMENT_3D('',#59723,#23431,#23432);
#20677=AXIS2_PLACEMENT_3D('',#59725,#23434,#23435);
#20678=AXIS2_PLACEMENT_3D('',#59727,#23436,#23437);
#20679=AXIS2_PLACEMENT_3D('',#59728,#23438,#23439);
#20680=AXIS2_PLACEMENT_3D('',#59729,#23440,#23441);
#20681=AXIS2_PLACEMENT_3D('',#59735,#23444,#23445);
#20682=AXIS2_PLACEMENT_3D('',#59759,#23459,#23460);
#20683=AXIS2_PLACEMENT_3D('',#59763,#23462,#23463);
#20684=AXIS2_PLACEMENT_3D('',#59766,#23465,#23466);
#20685=AXIS2_PLACEMENT_3D('',#59771,#23468,#23469);
#20686=AXIS2_PLACEMENT_3D('',#59774,#23471,#23472);
#20687=AXIS2_PLACEMENT_3D('',#59776,#23473,#23474);
#20688=AXIS2_PLACEMENT_3D('',#59779,#23476,#23477);
#20689=AXIS2_PLACEMENT_3D('',#59781,#23478,#23479);
#20690=AXIS2_PLACEMENT_3D('',#59782,#23480,#23481);
#20691=AXIS2_PLACEMENT_3D('',#59783,#23482,#23483);
#20692=AXIS2_PLACEMENT_3D('',#59784,#23484,#23485);
#20693=AXIS2_PLACEMENT_3D('',#59786,#23486,#23487);
#20694=AXIS2_PLACEMENT_3D('',#59788,#23489,#23490);
#20695=AXIS2_PLACEMENT_3D('',#59790,#23492,#23493);
#20696=AXIS2_PLACEMENT_3D('',#59792,#23495,#23496);
#20697=AXIS2_PLACEMENT_3D('',#59794,#23498,#23499);
#20698=AXIS2_PLACEMENT_3D('',#59795,#23500,#23501);
#20699=AXIS2_PLACEMENT_3D('',#59796,#23502,#23503);
#20700=AXIS2_PLACEMENT_3D('',#59797,#23504,#23505);
#20701=AXIS2_PLACEMENT_3D('',#59798,#23506,#23507);
#20702=AXIS2_PLACEMENT_3D('',#59799,#23508,#23509);
#20703=AXIS2_PLACEMENT_3D('',#59801,#23511,#23512);
#20704=AXIS2_PLACEMENT_3D('',#59802,#23513,#23514);
#20705=AXIS2_PLACEMENT_3D('',#59804,#23515,#23516);
#20706=AXIS2_PLACEMENT_3D('',#59806,#23517,#23518);
#20707=AXIS2_PLACEMENT_3D('',#59807,#23519,#23520);
#20708=AXIS2_PLACEMENT_3D('',#59808,#23521,#23522);
#20709=AXIS2_PLACEMENT_3D('',#59810,#23524,#23525);
#20710=AXIS2_PLACEMENT_3D('',#59811,#23526,#23527);
#20711=AXIS2_PLACEMENT_3D('',#59812,#23528,#23529);
#20712=AXIS2_PLACEMENT_3D('',#59814,#23531,#23532);
#20713=AXIS2_PLACEMENT_3D('',#59816,#23534,#23535);
#20714=AXIS2_PLACEMENT_3D('',#59818,#23536,#23537);
#20715=AXIS2_PLACEMENT_3D('',#59819,#23538,#23539);
#20716=AXIS2_PLACEMENT_3D('',#59820,#23540,#23541);
#20717=AXIS2_PLACEMENT_3D('',#59823,#23542,#23543);
#20718=AXIS2_PLACEMENT_3D('',#59824,#23544,#23545);
#20719=AXIS2_PLACEMENT_3D('',#59825,#23546,#23547);
#20720=AXIS2_PLACEMENT_3D('',#59826,#23548,#23549);
#20721=AXIS2_PLACEMENT_3D('',#59828,#23551,#23552);
#20722=AXIS2_PLACEMENT_3D('',#59830,#23553,#23554);
#20723=AXIS2_PLACEMENT_3D('',#59832,#23555,#23556);
#20724=AXIS2_PLACEMENT_3D('',#59833,#23557,#23558);
#20725=AXIS2_PLACEMENT_3D('',#59834,#23559,#23560);
#20726=AXIS2_PLACEMENT_3D('',#59835,#23561,#23562);
#20727=AXIS2_PLACEMENT_3D('',#59836,#23563,#23564);
#20728=AXIS2_PLACEMENT_3D('',#59839,#23565,#23566);
#20729=AXIS2_PLACEMENT_3D('',#59842,#23569,#23570);
#20730=AXIS2_PLACEMENT_3D('',#59843,#23571,#23572);
#20731=AXIS2_PLACEMENT_3D('',#59844,#23573,#23574);
#20732=AXIS2_PLACEMENT_3D('',#59845,#23575,#23576);
#20733=AXIS2_PLACEMENT_3D('',#59848,#23577,#23578);
#20734=AXIS2_PLACEMENT_3D('',#59849,#23579,#23580);
#20735=AXIS2_PLACEMENT_3D('',#59850,#23581,#23582);
#20736=AXIS2_PLACEMENT_3D('',#59851,#23583,#23584);
#20737=AXIS2_PLACEMENT_3D('',#59854,#23587,#23588);
#20738=AXIS2_PLACEMENT_3D('',#59855,#23589,#23590);
#20739=AXIS2_PLACEMENT_3D('',#59856,#23591,#23592);
#20740=AXIS2_PLACEMENT_3D('',#59857,#23593,#23594);
#20741=AXIS2_PLACEMENT_3D('',#59858,#23595,#23596);
#20742=AXIS2_PLACEMENT_3D('',#59859,#23597,#23598);
#20743=AXIS2_PLACEMENT_3D('',#59861,#23599,#23600);
#20744=AXIS2_PLACEMENT_3D('',#59862,#23601,#23602);
#20745=AXIS2_PLACEMENT_3D('',#59863,#23603,#23604);
#20746=AXIS2_PLACEMENT_3D('',#59865,#23606,#23607);
#20747=AXIS2_PLACEMENT_3D('',#59867,#23608,#23609);
#20748=AXIS2_PLACEMENT_3D('',#59868,#23610,#23611);
#20749=AXIS2_PLACEMENT_3D('',#59869,#23612,#23613);
#20750=AXIS2_PLACEMENT_3D('',#59871,#23614,#23615);
#20751=AXIS2_PLACEMENT_3D('',#59872,#23616,#23617);
#20752=AXIS2_PLACEMENT_3D('',#59873,#23618,#23619);
#20753=AXIS2_PLACEMENT_3D('',#59875,#23620,#23621);
#20754=AXIS2_PLACEMENT_3D('',#59876,#23622,#23623);
#20755=AXIS2_PLACEMENT_3D('',#59877,#23624,#23625);
#20756=AXIS2_PLACEMENT_3D('',#59880,#23626,#23627);
#20757=AXIS2_PLACEMENT_3D('',#59881,#23628,#23629);
#20758=AXIS2_PLACEMENT_3D('',#59882,#23630,#23631);
#20759=AXIS2_PLACEMENT_3D('',#59883,#23632,#23633);
#20760=AXIS2_PLACEMENT_3D('',#59886,#23636,#23637);
#20761=AXIS2_PLACEMENT_3D('',#59888,#23639,#23640);
#20762=AXIS2_PLACEMENT_3D('',#59891,#23642,#23643);
#20763=AXIS2_PLACEMENT_3D('',#59893,#23645,#23646);
#20764=AXIS2_PLACEMENT_3D('',#59894,#23647,#23648);
#20765=AXIS2_PLACEMENT_3D('',#59895,#23649,#23650);
#20766=AXIS2_PLACEMENT_3D('',#59897,#23652,#23653);
#20767=AXIS2_PLACEMENT_3D('',#59898,#23654,#23655);
#20768=AXIS2_PLACEMENT_3D('',#59900,#23656,#23657);
#20769=AXIS2_PLACEMENT_3D('',#59902,#23659,#23660);
#20770=AXIS2_PLACEMENT_3D('',#59905,#23661,#23662);
#20771=AXIS2_PLACEMENT_3D('',#59906,#23663,#23664);
#20772=AXIS2_PLACEMENT_3D('',#59907,#23665,#23666);
#20773=AXIS2_PLACEMENT_3D('',#59908,#23667,#23668);
#20774=AXIS2_PLACEMENT_3D('',#59910,#23669,#23670);
#20775=AXIS2_PLACEMENT_3D('',#59911,#23671,#23672);
#20776=AXIS2_PLACEMENT_3D('',#59912,#23673,#23674);
#20777=AXIS2_PLACEMENT_3D('',#59914,#23676,#23677);
#20778=AXIS2_PLACEMENT_3D('',#59917,#23679,#23680);
#20779=AXIS2_PLACEMENT_3D('',#59918,#23681,#23682);
#20780=AXIS2_PLACEMENT_3D('',#59921,#23683,#23684);
#20781=AXIS2_PLACEMENT_3D('',#59922,#23685,#23686);
#20782=AXIS2_PLACEMENT_3D('',#59923,#23687,#23688);
#20783=AXIS2_PLACEMENT_3D('',#59924,#23689,#23690);
#20784=AXIS2_PLACEMENT_3D('',#59926,#23692,#23693);
#20785=AXIS2_PLACEMENT_3D('',#59929,#23695,#23696);
#20786=AXIS2_PLACEMENT_3D('',#59930,#23697,#23698);
#20787=AXIS2_PLACEMENT_3D('',#59932,#23699,#23700);
#20788=AXIS2_PLACEMENT_3D('',#59934,#23702,#23703);
#20789=AXIS2_PLACEMENT_3D('',#59937,#23704,#23705);
#20790=AXIS2_PLACEMENT_3D('',#59938,#23706,#23707);
#20791=AXIS2_PLACEMENT_3D('',#59939,#23708,#23709);
#20792=AXIS2_PLACEMENT_3D('',#59940,#23710,#23711);
#20793=AXIS2_PLACEMENT_3D('',#59942,#23713,#23714);
#20794=AXIS2_PLACEMENT_3D('',#59945,#23715,#23716);
#20795=AXIS2_PLACEMENT_3D('',#59946,#23717,#23718);
#20796=AXIS2_PLACEMENT_3D('',#59947,#23719,#23720);
#20797=AXIS2_PLACEMENT_3D('',#59948,#23721,#23722);
#20798=AXIS2_PLACEMENT_3D('',#59950,#23724,#23725);
#20799=AXIS2_PLACEMENT_3D('',#59953,#23726,#23727);
#20800=AXIS2_PLACEMENT_3D('',#59954,#23728,#23729);
#20801=AXIS2_PLACEMENT_3D('',#59955,#23730,#23731);
#20802=AXIS2_PLACEMENT_3D('',#59956,#23732,#23733);
#20803=AXIS2_PLACEMENT_3D('',#59958,#23735,#23736);
#20804=AXIS2_PLACEMENT_3D('',#59960,#23738,#23739);
#20805=AXIS2_PLACEMENT_3D('',#59963,#23740,#23741);
#20806=AXIS2_PLACEMENT_3D('',#59966,#23744,#23745);
#20807=AXIS2_PLACEMENT_3D('',#59967,#23746,#23747);
#20808=AXIS2_PLACEMENT_3D('',#59969,#23749,#23750);
#20809=AXIS2_PLACEMENT_3D('',#59972,#23751,#23752);
#20810=AXIS2_PLACEMENT_3D('',#59975,#23755,#23756);
#20811=AXIS2_PLACEMENT_3D('',#59976,#23757,#23758);
#20812=AXIS2_PLACEMENT_3D('',#59977,#23759,#23760);
#20813=AXIS2_PLACEMENT_3D('',#59978,#23761,#23762);
#20814=AXIS2_PLACEMENT_3D('',#59981,#23763,#23764);
#20815=AXIS2_PLACEMENT_3D('',#59984,#23767,#23768);
#20816=AXIS2_PLACEMENT_3D('',#59985,#23769,#23770);
#20817=AXIS2_PLACEMENT_3D('',#59986,#23771,#23772);
#20818=AXIS2_PLACEMENT_3D('',#59987,#23773,#23774);
#20819=AXIS2_PLACEMENT_3D('',#59990,#23775,#23776);
#20820=AXIS2_PLACEMENT_3D('',#59993,#23779,#23780);
#20821=AXIS2_PLACEMENT_3D('',#59994,#23781,#23782);
#20822=AXIS2_PLACEMENT_3D('',#59995,#23783,#23784);
#20823=AXIS2_PLACEMENT_3D('',#59996,#23785,#23786);
#20824=AXIS2_PLACEMENT_3D('',#59999,#23787,#23788);
#20825=AXIS2_PLACEMENT_3D('',#60002,#23791,#23792);
#20826=AXIS2_PLACEMENT_3D('',#60003,#23793,#23794);
#20827=AXIS2_PLACEMENT_3D('',#60004,#23795,#23796);
#20828=AXIS2_PLACEMENT_3D('',#60005,#23797,#23798);
#20829=AXIS2_PLACEMENT_3D('',#60008,#23800,#23801);
#20830=AXIS2_PLACEMENT_3D('',#60010,#23803,#23804);
#20831=AXIS2_PLACEMENT_3D('',#60011,#23805,#23806);
#20832=AXIS2_PLACEMENT_3D('',#60012,#23807,#23808);
#20833=AXIS2_PLACEMENT_3D('',#60013,#23809,#23810);
#20834=AXIS2_PLACEMENT_3D('',#60014,#23811,#23812);
#20835=AXIS2_PLACEMENT_3D('',#60016,#23813,#23814);
#20836=AXIS2_PLACEMENT_3D('',#60018,#23816,#23817);
#20837=AXIS2_PLACEMENT_3D('',#60021,#23819,#23820);
#20838=AXIS2_PLACEMENT_3D('',#60022,#23821,#23822);
#20839=AXIS2_PLACEMENT_3D('',#60024,#23824,#23825);
#20840=AXIS2_PLACEMENT_3D('',#60026,#23827,#23828);
#20841=AXIS2_PLACEMENT_3D('',#60027,#23829,#23830);
#20842=AXIS2_PLACEMENT_3D('',#60030,#23832,#23833);
#20843=AXIS2_PLACEMENT_3D('',#60031,#23834,#23835);
#20844=AXIS2_PLACEMENT_3D('',#60033,#23837,#23838);
#20845=AXIS2_PLACEMENT_3D('',#60037,#23841,#23842);
#20846=AXIS2_PLACEMENT_3D('',#60039,#23844,#23845);
#20847=AXIS2_PLACEMENT_3D('',#60040,#23846,#23847);
#20848=AXIS2_PLACEMENT_3D('',#60041,#23848,#23849);
#20849=AXIS2_PLACEMENT_3D('',#60043,#23851,#23852);
#20850=AXIS2_PLACEMENT_3D('',#60044,#23853,#23854);
#20851=AXIS2_PLACEMENT_3D('',#60046,#23856,#23857);
#20852=AXIS2_PLACEMENT_3D('',#60047,#23858,#23859);
#20853=AXIS2_PLACEMENT_3D('',#60048,#23860,#23861);
#20854=AXIS2_PLACEMENT_3D('',#60049,#23862,#23863);
#20855=AXIS2_PLACEMENT_3D('',#60052,#23865,#23866);
#20856=AXIS2_PLACEMENT_3D('',#60053,#23867,#23868);
#20857=AXIS2_PLACEMENT_3D('',#60054,#23869,#23870);
#20858=AXIS2_PLACEMENT_3D('',#60055,#23871,#23872);
#20859=AXIS2_PLACEMENT_3D('',#60057,#23874,#23875);
#20860=AXIS2_PLACEMENT_3D('',#60059,#23877,#23878);
#20861=AXIS2_PLACEMENT_3D('',#60060,#23879,#23880);
#20862=AXIS2_PLACEMENT_3D('',#60061,#23881,#23882);
#20863=AXIS2_PLACEMENT_3D('',#60062,#23883,#23884);
#20864=AXIS2_PLACEMENT_3D('',#60063,#23885,#23886);
#20865=AXIS2_PLACEMENT_3D('',#60065,#23888,#23889);
#20866=AXIS2_PLACEMENT_3D('',#60066,#23890,#23891);
#20867=AXIS2_PLACEMENT_3D('',#60067,#23892,#23893);
#20868=AXIS2_PLACEMENT_3D('',#60068,#23894,#23895);
#20869=AXIS2_PLACEMENT_3D('',#60069,#23896,#23897);
#20870=AXIS2_PLACEMENT_3D('',#60070,#23898,#23899);
#20871=AXIS2_PLACEMENT_3D('',#60071,#23900,#23901);
#20872=AXIS2_PLACEMENT_3D('',#60072,#23902,#23903);
#20873=AXIS2_PLACEMENT_3D('',#60074,#23904,#23905);
#20874=AXIS2_PLACEMENT_3D('',#60075,#23906,#23907);
#20875=AXIS2_PLACEMENT_3D('',#60076,#23908,#23909);
#20876=AXIS2_PLACEMENT_3D('',#60077,#23910,#23911);
#20877=AXIS2_PLACEMENT_3D('',#60079,#23913,#23914);
#20878=AXIS2_PLACEMENT_3D('',#60080,#23915,#23916);
#20879=AXIS2_PLACEMENT_3D('',#60082,#23918,#23919);
#20880=AXIS2_PLACEMENT_3D('',#60083,#23920,#23921);
#20881=AXIS2_PLACEMENT_3D('',#60084,#23922,#23923);
#20882=AXIS2_PLACEMENT_3D('',#60087,#23924,#23925);
#20883=AXIS2_PLACEMENT_3D('',#60088,#23926,#23927);
#20884=AXIS2_PLACEMENT_3D('',#60089,#23928,#23929);
#20885=AXIS2_PLACEMENT_3D('',#60090,#23930,#23931);
#20886=AXIS2_PLACEMENT_3D('',#60093,#23932,#23933);
#20887=AXIS2_PLACEMENT_3D('',#60094,#23934,#23935);
#20888=AXIS2_PLACEMENT_3D('',#60096,#23937,#23938);
#20889=AXIS2_PLACEMENT_3D('',#60097,#23939,#23940);
#20890=AXIS2_PLACEMENT_3D('',#60098,#23941,#23942);
#20891=AXIS2_PLACEMENT_3D('',#60099,#23943,#23944);
#20892=AXIS2_PLACEMENT_3D('',#60100,#23945,#23946);
#20893=AXIS2_PLACEMENT_3D('',#60101,#23947,#23948);
#20894=AXIS2_PLACEMENT_3D('',#60106,#23950,#23951);
#20895=AXIS2_PLACEMENT_3D('',#60109,#23953,#23954);
#20896=AXIS2_PLACEMENT_3D('',#60110,#23955,#23956);
#20897=AXIS2_PLACEMENT_3D('',#60115,#23959,#23960);
#20898=AXIS2_PLACEMENT_3D('',#60116,#23961,#23962);
#20899=AXIS2_PLACEMENT_3D('',#60121,#23965,#23966);
#20900=AXIS2_PLACEMENT_3D('',#60122,#23967,#23968);
#20901=AXIS2_PLACEMENT_3D('',#60125,#23971,#23972);
#20902=AXIS2_PLACEMENT_3D('',#60131,#23976,#23977);
#20903=AXIS2_PLACEMENT_3D('',#60135,#23980,#23981);
#20904=AXIS2_PLACEMENT_3D('',#60140,#23983,#23984);
#20905=AXIS2_PLACEMENT_3D('',#60148,#23989,#23990);
#20906=AXIS2_PLACEMENT_3D('',#60167,#23991,#23992);
#20907=AXIS2_PLACEMENT_3D('',#60169,#23994,#23995);
#20908=AXIS2_PLACEMENT_3D('',#60174,#23997,#23998);
#20909=AXIS2_PLACEMENT_3D('',#60176,#24000,#24001);
#20910=AXIS2_PLACEMENT_3D('',#60177,#24002,#24003);
#20911=AXIS2_PLACEMENT_3D('',#60181,#24005,#24006);
#20912=AXIS2_PLACEMENT_3D('',#60182,#24007,#24008);
#20913=AXIS2_PLACEMENT_3D('',#60183,#24009,#24010);
#20914=AXIS2_PLACEMENT_3D('',#60185,#24012,#24013);
#20915=AXIS2_PLACEMENT_3D('',#60188,#24016,#24017);
#20916=AXIS2_PLACEMENT_3D('',#60190,#24019,#24020);
#20917=AXIS2_PLACEMENT_3D('',#60203,#24027,#24028);
#20918=AXIS2_PLACEMENT_3D('',#60205,#24029,#24030);
#20919=AXIS2_PLACEMENT_3D('',#60207,#24031,#24032);
#20920=AXIS2_PLACEMENT_3D('',#60209,#24034,#24035);
#20921=AXIS2_PLACEMENT_3D('',#60231,#24037,#24038);
#20922=AXIS2_PLACEMENT_3D('',#60233,#24040,#24041);
#20923=AXIS2_PLACEMENT_3D('',#60235,#24042,#24043);
#20924=AXIS2_PLACEMENT_3D('',#60241,#24047,#24048);
#20925=AXIS2_PLACEMENT_3D('',#60246,#24050,#24051);
#20926=AXIS2_PLACEMENT_3D('',#60249,#24053,#24054);
#20927=AXIS2_PLACEMENT_3D('',#60250,#24055,#24056);
#20928=AXIS2_PLACEMENT_3D('',#60255,#24059,#24060);
#20929=AXIS2_PLACEMENT_3D('',#60256,#24061,#24062);
#20930=AXIS2_PLACEMENT_3D('',#60261,#24065,#24066);
#20931=AXIS2_PLACEMENT_3D('',#60262,#24067,#24068);
#20932=AXIS2_PLACEMENT_3D('',#60265,#24071,#24072);
#20933=AXIS2_PLACEMENT_3D('',#60271,#24076,#24077);
#20934=AXIS2_PLACEMENT_3D('',#60275,#24080,#24081);
#20935=AXIS2_PLACEMENT_3D('',#60284,#24086,#24087);
#20936=AXIS2_PLACEMENT_3D('',#60285,#24088,#24089);
#20937=AXIS2_PLACEMENT_3D('',#60287,#24090,#24091);
#20938=AXIS2_PLACEMENT_3D('',#60289,#24092,#24093);
#20939=AXIS2_PLACEMENT_3D('',#60290,#24094,#24095);
#20940=AXIS2_PLACEMENT_3D('',#60291,#24096,#24097);
#20941=AXIS2_PLACEMENT_3D('',#60293,#24098,#24099);
#20942=AXIS2_PLACEMENT_3D('',#60295,#24101,#24102);
#20943=AXIS2_PLACEMENT_3D('',#60317,#24114,#24115);
#20944=AXIS2_PLACEMENT_3D('',#60320,#24117,#24118);
#20945=AXIS2_PLACEMENT_3D('',#60321,#24119,#24120);
#20946=AXIS2_PLACEMENT_3D('',#60323,#24121,#24122);
#20947=AXIS2_PLACEMENT_3D('',#60325,#24124,#24125);
#20948=AXIS2_PLACEMENT_3D('',#60326,#24126,#24127);
#20949=AXIS2_PLACEMENT_3D('',#60329,#24129,#24130);
#20950=AXIS2_PLACEMENT_3D('',#60330,#24131,#24132);
#20951=AXIS2_PLACEMENT_3D('',#60331,#24133,#24134);
#20952=AXIS2_PLACEMENT_3D('',#60333,#24135,#24136);
#20953=AXIS2_PLACEMENT_3D('',#60334,#24137,#24138);
#20954=AXIS2_PLACEMENT_3D('',#60335,#24139,#24140);
#20955=AXIS2_PLACEMENT_3D('',#60336,#24141,#24142);
#20956=AXIS2_PLACEMENT_3D('',#60340,#24144,#24145);
#20957=AXIS2_PLACEMENT_3D('',#60342,#24147,#24148);
#20958=AXIS2_PLACEMENT_3D('',#60346,#24151,#24152);
#20959=AXIS2_PLACEMENT_3D('',#60349,#24154,#24155);
#20960=AXIS2_PLACEMENT_3D('',#60350,#24156,#24157);
#20961=AXIS2_PLACEMENT_3D('',#60354,#24159,#24160);
#20962=AXIS2_PLACEMENT_3D('',#60356,#24162,#24163);
#20963=AXIS2_PLACEMENT_3D('',#60360,#24165,#24166);
#20964=AXIS2_PLACEMENT_3D('',#60362,#24168,#24169);
#20965=AXIS2_PLACEMENT_3D('',#60367,#24171,#24172);
#20966=AXIS2_PLACEMENT_3D('',#60370,#24174,#24175);
#20967=AXIS2_PLACEMENT_3D('',#60371,#24176,#24177);
#20968=AXIS2_PLACEMENT_3D('',#60374,#24179,#24180);
#20969=AXIS2_PLACEMENT_3D('',#60376,#24182,#24183);
#20970=AXIS2_PLACEMENT_3D('',#60377,#24184,#24185);
#20971=AXIS2_PLACEMENT_3D('',#60379,#24186,#24187);
#20972=AXIS2_PLACEMENT_3D('',#60380,#24188,#24189);
#20973=AXIS2_PLACEMENT_3D('',#60381,#24190,#24191);
#20974=AXIS2_PLACEMENT_3D('',#60382,#24192,#24193);
#20975=AXIS2_PLACEMENT_3D('',#60383,#24194,#24195);
#20976=AXIS2_PLACEMENT_3D('',#60385,#24197,#24198);
#20977=AXIS2_PLACEMENT_3D('',#60387,#24199,#24200);
#20978=AXIS2_PLACEMENT_3D('',#60389,#24201,#24202);
#20979=AXIS2_PLACEMENT_3D('',#60418,#24203,#24204);
#20980=AXIS2_PLACEMENT_3D('',#60421,#24207,#24208);
#20981=AXIS2_PLACEMENT_3D('',#60425,#24211,#24212);
#20982=AXIS2_PLACEMENT_3D('',#60429,#24215,#24216);
#20983=AXIS2_PLACEMENT_3D('',#60433,#24219,#24220);
#20984=AXIS2_PLACEMENT_3D('',#60436,#24222,#24223);
#20985=AXIS2_PLACEMENT_3D('',#60437,#24224,#24225);
#20986=AXIS2_PLACEMENT_3D('',#60441,#24228,#24229);
#20987=AXIS2_PLACEMENT_3D('',#60443,#24231,#24232);
#20988=AXIS2_PLACEMENT_3D('',#60445,#24234,#24235);
#20989=AXIS2_PLACEMENT_3D('',#60447,#24236,#24237);
#20990=AXIS2_PLACEMENT_3D('',#60449,#24239,#24240);
#20991=AXIS2_PLACEMENT_3D('',#60451,#24241,#24242);
#20992=AXIS2_PLACEMENT_3D('',#60453,#24243,#24244);
#20993=AXIS2_PLACEMENT_3D('',#60455,#24246,#24247);
#20994=AXIS2_PLACEMENT_3D('',#60457,#24248,#24249);
#20995=AXIS2_PLACEMENT_3D('',#60458,#24250,#24251);
#20996=AXIS2_PLACEMENT_3D('',#60459,#24252,#24253);
#20997=AXIS2_PLACEMENT_3D('',#60461,#24254,#24255);
#20998=AXIS2_PLACEMENT_3D('',#60463,#24257,#24258);
#20999=AXIS2_PLACEMENT_3D('',#60465,#24259,#24260);
#21000=AXIS2_PLACEMENT_3D('',#60467,#24261,#24262);
#21001=AXIS2_PLACEMENT_3D('',#60469,#24264,#24265);
#21002=AXIS2_PLACEMENT_3D('',#60474,#24267,#24268);
#21003=AXIS2_PLACEMENT_3D('',#60476,#24270,#24271);
#21004=AXIS2_PLACEMENT_3D('',#60477,#24272,#24273);
#21005=AXIS2_PLACEMENT_3D('',#60481,#24275,#24276);
#21006=AXIS2_PLACEMENT_3D('',#60482,#24277,#24278);
#21007=AXIS2_PLACEMENT_3D('',#60483,#24279,#24280);
#21008=AXIS2_PLACEMENT_3D('',#60485,#24282,#24283);
#21009=AXIS2_PLACEMENT_3D('',#60488,#24286,#24287);
#21010=AXIS2_PLACEMENT_3D('',#60490,#24289,#24290);
#21011=AXIS2_PLACEMENT_3D('',#60497,#24295,#24296);
#21012=AXIS2_PLACEMENT_3D('',#60500,#24297,#24298);
#21013=AXIS2_PLACEMENT_3D('',#60503,#24301,#24302);
#21014=AXIS2_PLACEMENT_3D('',#60505,#24303,#24304);
#21015=AXIS2_PLACEMENT_3D('',#60507,#24305,#24306);
#21016=AXIS2_PLACEMENT_3D('',#60536,#24307,#24308);
#21017=AXIS2_PLACEMENT_3D('',#60540,#24310,#24311);
#21018=AXIS2_PLACEMENT_3D('',#60542,#24313,#24314);
#21019=AXIS2_PLACEMENT_3D('',#60546,#24316,#24317);
#21020=AXIS2_PLACEMENT_3D('',#60548,#24319,#24320);
#21021=AXIS2_PLACEMENT_3D('',#60551,#24322,#24323);
#21022=AXIS2_PLACEMENT_3D('',#60552,#24324,#24325);
#21023=AXIS2_PLACEMENT_3D('',#60555,#24328,#24329);
#21024=AXIS2_PLACEMENT_3D('',#60559,#24332,#24333);
#21025=AXIS2_PLACEMENT_3D('',#60562,#24335,#24336);
#21026=AXIS2_PLACEMENT_3D('',#60563,#24337,#24338);
#21027=AXIS2_PLACEMENT_3D('',#60567,#24341,#24342);
#21028=AXIS2_PLACEMENT_3D('',#60571,#24345,#24346);
#21029=AXIS2_PLACEMENT_3D('',#60573,#24348,#24349);
#21030=AXIS2_PLACEMENT_3D('',#60576,#24351,#24352);
#21031=AXIS2_PLACEMENT_3D('',#60577,#24353,#24354);
#21032=AXIS2_PLACEMENT_3D('',#60579,#24355,#24356);
#21033=AXIS2_PLACEMENT_3D('',#60581,#24357,#24358);
#21034=AXIS2_PLACEMENT_3D('',#60610,#24359,#24360);
#21035=AXIS2_PLACEMENT_3D('',#60612,#24362,#24363);
#21036=AXIS2_PLACEMENT_3D('',#60615,#24365,#24366);
#21037=AXIS2_PLACEMENT_3D('',#60616,#24367,#24368);
#21038=AXIS2_PLACEMENT_3D('',#60619,#24370,#24371);
#21039=AXIS2_PLACEMENT_3D('',#60620,#24372,#24373);
#21040=AXIS2_PLACEMENT_3D('',#60622,#24375,#24376);
#21041=AXIS2_PLACEMENT_3D('',#60624,#24377,#24378);
#21042=AXIS2_PLACEMENT_3D('',#60626,#24379,#24380);
#21043=AXIS2_PLACEMENT_3D('',#60628,#24381,#24382);
#21044=AXIS2_PLACEMENT_3D('',#60629,#24383,#24384);
#21045=AXIS2_PLACEMENT_3D('',#60631,#24385,#24386);
#21046=AXIS2_PLACEMENT_3D('',#60633,#24387,#24388);
#21047=AXIS2_PLACEMENT_3D('',#60635,#24389,#24390);
#21048=AXIS2_PLACEMENT_3D('',#60636,#24391,#24392);
#21049=AXIS2_PLACEMENT_3D('',#60637,#24393,#24394);
#21050=AXIS2_PLACEMENT_3D('',#60639,#24395,#24396);
#21051=AXIS2_PLACEMENT_3D('',#60640,#24397,#24398);
#21052=AXIS2_PLACEMENT_3D('',#60643,#24400,#24401);
#21053=AXIS2_PLACEMENT_3D('',#60644,#24402,#24403);
#21054=AXIS2_PLACEMENT_3D('',#60646,#24404,#24405);
#21055=AXIS2_PLACEMENT_3D('',#60649,#24407,#24408);
#21056=AXIS2_PLACEMENT_3D('',#60650,#24409,#24410);
#21057=AXIS2_PLACEMENT_3D('',#60652,#24412,#24413);
#21058=AXIS2_PLACEMENT_3D('',#60655,#24415,#24416);
#21059=AXIS2_PLACEMENT_3D('',#60656,#24417,#24418);
#21060=AXIS2_PLACEMENT_3D('',#60659,#24420,#24421);
#21061=AXIS2_PLACEMENT_3D('',#60660,#24422,#24423);
#21062=AXIS2_PLACEMENT_3D('',#60663,#24425,#24426);
#21063=AXIS2_PLACEMENT_3D('',#60664,#24427,#24428);
#21064=AXIS2_PLACEMENT_3D('',#60695,#24430,#24431);
#21065=AXIS2_PLACEMENT_3D('',#60696,#24432,#24433);
#21066=AXIS2_PLACEMENT_3D('',#60697,#24434,#24435);
#21067=AXIS2_PLACEMENT_3D('',#60699,#24436,#24437);
#21068=AXIS2_PLACEMENT_3D('',#60701,#24438,#24439);
#21069=AXIS2_PLACEMENT_3D('',#60703,#24440,#24441);
#21070=AXIS2_PLACEMENT_3D('',#60704,#24442,#24443);
#21071=AXIS2_PLACEMENT_3D('',#60706,#24444,#24445);
#21072=AXIS2_PLACEMENT_3D('',#60708,#24446,#24447);
#21073=AXIS2_PLACEMENT_3D('',#60710,#24448,#24449);
#21074=AXIS2_PLACEMENT_3D('',#60711,#24450,#24451);
#21075=AXIS2_PLACEMENT_3D('',#60712,#24452,#24453);
#21076=AXIS2_PLACEMENT_3D('',#60714,#24454,#24455);
#21077=AXIS2_PLACEMENT_3D('',#60715,#24456,#24457);
#21078=AXIS2_PLACEMENT_3D('',#60718,#24459,#24460);
#21079=AXIS2_PLACEMENT_3D('',#60719,#24461,#24462);
#21080=AXIS2_PLACEMENT_3D('',#60721,#24463,#24464);
#21081=AXIS2_PLACEMENT_3D('',#60723,#24465,#24466);
#21082=AXIS2_PLACEMENT_3D('',#60724,#24467,#24468);
#21083=AXIS2_PLACEMENT_3D('',#60725,#24469,#24470);
#21084=AXIS2_PLACEMENT_3D('',#60729,#24472,#24473);
#21085=AXIS2_PLACEMENT_3D('',#60730,#24474,#24475);
#21086=AXIS2_PLACEMENT_3D('',#60731,#24476,#24477);
#21087=AXIS2_PLACEMENT_3D('',#60732,#24478,#24479);
#21088=AXIS2_PLACEMENT_3D('',#60733,#24480,#24481);
#21089=AXIS2_PLACEMENT_3D('',#60735,#24482,#24483);
#21090=AXIS2_PLACEMENT_3D('',#60737,#24484,#24485);
#21091=AXIS2_PLACEMENT_3D('',#60738,#24486,#24487);
#21092=AXIS2_PLACEMENT_3D('',#60739,#24488,#24489);
#21093=AXIS2_PLACEMENT_3D('',#60743,#24491,#24492);
#21094=AXIS2_PLACEMENT_3D('',#60744,#24493,#24494);
#21095=AXIS2_PLACEMENT_3D('',#60745,#24495,#24496);
#21096=AXIS2_PLACEMENT_3D('',#60746,#24497,#24498);
#21097=AXIS2_PLACEMENT_3D('',#60747,#24499,#24500);
#21098=AXIS2_PLACEMENT_3D('',#60749,#24501,#24502);
#21099=AXIS2_PLACEMENT_3D('',#60751,#24503,#24504);
#21100=AXIS2_PLACEMENT_3D('',#60752,#24505,#24506);
#21101=AXIS2_PLACEMENT_3D('',#60753,#24507,#24508);
#21102=AXIS2_PLACEMENT_3D('',#60756,#24509,#24510);
#21103=AXIS2_PLACEMENT_3D('',#60757,#24511,#24512);
#21104=AXIS2_PLACEMENT_3D('',#60759,#24514,#24515);
#21105=AXIS2_PLACEMENT_3D('',#60761,#24516,#24517);
#21106=AXIS2_PLACEMENT_3D('',#60762,#24518,#24519);
#21107=AXIS2_PLACEMENT_3D('',#60763,#24520,#24521);
#21108=AXIS2_PLACEMENT_3D('',#60765,#24522,#24523);
#21109=AXIS2_PLACEMENT_3D('',#60766,#24524,#24525);
#21110=AXIS2_PLACEMENT_3D('',#60768,#24526,#24527);
#21111=AXIS2_PLACEMENT_3D('',#60770,#24528,#24529);
#21112=AXIS2_PLACEMENT_3D('',#60771,#24530,#24531);
#21113=AXIS2_PLACEMENT_3D('',#60772,#24532,#24533);
#21114=AXIS2_PLACEMENT_3D('',#60775,#24534,#24535);
#21115=AXIS2_PLACEMENT_3D('',#60776,#24536,#24537);
#21116=AXIS2_PLACEMENT_3D('',#60778,#24539,#24540);
#21117=AXIS2_PLACEMENT_3D('',#60780,#24541,#24542);
#21118=AXIS2_PLACEMENT_3D('',#60781,#24543,#24544);
#21119=AXIS2_PLACEMENT_3D('',#60782,#24545,#24546);
#21120=AXIS2_PLACEMENT_3D('',#60785,#24548,#24549);
#21121=AXIS2_PLACEMENT_3D('',#60786,#24550,#24551);
#21122=AXIS2_PLACEMENT_3D('',#60788,#24552,#24553);
#21123=AXIS2_PLACEMENT_3D('',#60790,#24554,#24555);
#21124=AXIS2_PLACEMENT_3D('',#60791,#24556,#24557);
#21125=AXIS2_PLACEMENT_3D('',#60792,#24558,#24559);
#21126=AXIS2_PLACEMENT_3D('',#60795,#24560,#24561);
#21127=AXIS2_PLACEMENT_3D('',#60796,#24562,#24563);
#21128=AXIS2_PLACEMENT_3D('',#60798,#24565,#24566);
#21129=AXIS2_PLACEMENT_3D('',#60799,#24567,#24568);
#21130=AXIS2_PLACEMENT_3D('',#60800,#24569,#24570);
#21131=AXIS2_PLACEMENT_3D('',#60802,#24571,#24572);
#21132=AXIS2_PLACEMENT_3D('',#60804,#24573,#24574);
#21133=AXIS2_PLACEMENT_3D('',#60805,#24575,#24576);
#21134=AXIS2_PLACEMENT_3D('',#60806,#24577,#24578);
#21135=AXIS2_PLACEMENT_3D('',#60809,#24579,#24580);
#21136=AXIS2_PLACEMENT_3D('',#60810,#24581,#24582);
#21137=AXIS2_PLACEMENT_3D('',#60812,#24584,#24585);
#21138=AXIS2_PLACEMENT_3D('',#60813,#24586,#24587);
#21139=AXIS2_PLACEMENT_3D('',#60814,#24588,#24589);
#21140=AXIS2_PLACEMENT_3D('',#60816,#24590,#24591);
#21141=AXIS2_PLACEMENT_3D('',#60818,#24592,#24593);
#21142=AXIS2_PLACEMENT_3D('',#60820,#24594,#24595);
#21143=AXIS2_PLACEMENT_3D('',#60821,#24596,#24597);
#21144=AXIS2_PLACEMENT_3D('',#60822,#24598,#24599);
#21145=AXIS2_PLACEMENT_3D('',#60825,#24600,#24601);
#21146=AXIS2_PLACEMENT_3D('',#60826,#24602,#24603);
#21147=AXIS2_PLACEMENT_3D('',#60828,#24605,#24606);
#21148=AXIS2_PLACEMENT_3D('',#60838,#24612,#24613);
#21149=AXIS2_PLACEMENT_3D('',#60855,#24622,#24623);
#21150=AXIS2_PLACEMENT_3D('',#60858,#24625,#24626);
#21151=AXIS2_PLACEMENT_3D('',#60859,#24627,#24628);
#21152=AXIS2_PLACEMENT_3D('',#60860,#24629,#24630);
#21153=AXIS2_PLACEMENT_3D('',#60862,#24631,#24632);
#21154=AXIS2_PLACEMENT_3D('',#60864,#24634,#24635);
#21155=AXIS2_PLACEMENT_3D('',#60866,#24637,#24638);
#21156=AXIS2_PLACEMENT_3D('',#60870,#24641,#24642);
#21157=AXIS2_PLACEMENT_3D('',#60874,#24645,#24646);
#21158=AXIS2_PLACEMENT_3D('',#60876,#24648,#24649);
#21159=AXIS2_PLACEMENT_3D('',#60877,#24650,#24651);
#21160=AXIS2_PLACEMENT_3D('',#60879,#24652,#24653);
#21161=AXIS2_PLACEMENT_3D('',#60880,#24654,#24655);
#21162=AXIS2_PLACEMENT_3D('',#60881,#24656,#24657);
#21163=AXIS2_PLACEMENT_3D('',#60922,#24678,#24679);
#21164=AXIS2_PLACEMENT_3D('',#60923,#24680,#24681);
#21165=AXIS2_PLACEMENT_3D('',#60924,#24682,#24683);
#21166=AXIS2_PLACEMENT_3D('',#60925,#24684,#24685);
#21167=AXIS2_PLACEMENT_3D('',#60926,#24686,#24687);
#21168=AXIS2_PLACEMENT_3D('',#60927,#24688,#24689);
#21169=AXIS2_PLACEMENT_3D('',#60928,#24690,#24691);
#21170=AXIS2_PLACEMENT_3D('',#60929,#24692,#24693);
#21171=AXIS2_PLACEMENT_3D('',#60930,#24694,#24695);
#21172=AXIS2_PLACEMENT_3D('',#60932,#24696,#24697);
#21173=AXIS2_PLACEMENT_3D('',#60934,#24698,#24699);
#21174=AXIS2_PLACEMENT_3D('',#60935,#24700,#24701);
#21175=AXIS2_PLACEMENT_3D('',#60936,#24702,#24703);
#21176=AXIS2_PLACEMENT_3D('',#60940,#24705,#24706);
#21177=AXIS2_PLACEMENT_3D('',#60941,#24707,#24708);
#21178=AXIS2_PLACEMENT_3D('',#60942,#24709,#24710);
#21179=AXIS2_PLACEMENT_3D('',#60943,#24711,#24712);
#21180=AXIS2_PLACEMENT_3D('',#60944,#24713,#24714);
#21181=AXIS2_PLACEMENT_3D('',#60946,#24715,#24716);
#21182=AXIS2_PLACEMENT_3D('',#60949,#24718,#24719);
#21183=AXIS2_PLACEMENT_3D('',#60950,#24720,#24721);
#21184=AXIS2_PLACEMENT_3D('',#60953,#24723,#24724);
#21185=AXIS2_PLACEMENT_3D('',#60954,#24725,#24726);
#21186=AXIS2_PLACEMENT_3D('',#60957,#24728,#24729);
#21187=AXIS2_PLACEMENT_3D('',#60958,#24730,#24731);
#21188=AXIS2_PLACEMENT_3D('',#60960,#24733,#24734);
#21189=AXIS2_PLACEMENT_3D('',#60966,#24738,#24739);
#21190=AXIS2_PLACEMENT_3D('',#60970,#24742,#24743);
#21191=AXIS2_PLACEMENT_3D('',#60971,#24744,#24745);
#21192=AXIS2_PLACEMENT_3D('',#60972,#24746,#24747);
#21193=AXIS2_PLACEMENT_3D('',#60973,#24748,#24749);
#21194=AXIS2_PLACEMENT_3D('',#60974,#24750,#24751);
#21195=AXIS2_PLACEMENT_3D('',#60975,#24752,#24753);
#21196=AXIS2_PLACEMENT_3D('',#60977,#24754,#24755);
#21197=AXIS2_PLACEMENT_3D('',#60979,#24757,#24758);
#21198=AXIS2_PLACEMENT_3D('',#60981,#24760,#24761);
#21199=AXIS2_PLACEMENT_3D('',#60983,#24762,#24763);
#21200=AXIS2_PLACEMENT_3D('',#60986,#24765,#24766);
#21201=AXIS2_PLACEMENT_3D('',#60987,#24767,#24768);
#21202=AXIS2_PLACEMENT_3D('',#60990,#24770,#24771);
#21203=AXIS2_PLACEMENT_3D('',#60991,#24772,#24773);
#21204=AXIS2_PLACEMENT_3D('',#60994,#24775,#24776);
#21205=AXIS2_PLACEMENT_3D('',#60995,#24777,#24778);
#21206=AXIS2_PLACEMENT_3D('',#60997,#24780,#24781);
#21207=AXIS2_PLACEMENT_3D('',#61003,#24785,#24786);
#21208=AXIS2_PLACEMENT_3D('',#61007,#24789,#24790);
#21209=AXIS2_PLACEMENT_3D('',#61008,#24791,#24792);
#21210=AXIS2_PLACEMENT_3D('',#61009,#24793,#24794);
#21211=AXIS2_PLACEMENT_3D('',#61010,#24795,#24796);
#21212=AXIS2_PLACEMENT_3D('',#61011,#24797,#24798);
#21213=AXIS2_PLACEMENT_3D('',#61012,#24799,#24800);
#21214=AXIS2_PLACEMENT_3D('',#61014,#24801,#24802);
#21215=AXIS2_PLACEMENT_3D('',#61016,#24804,#24805);
#21216=AXIS2_PLACEMENT_3D('',#61018,#24807,#24808);
#21217=AXIS2_PLACEMENT_3D('',#61021,#24809,#24810);
#21218=AXIS2_PLACEMENT_3D('',#61025,#24812,#24813);
#21219=AXIS2_PLACEMENT_3D('',#61029,#24815,#24816);
#21220=AXIS2_PLACEMENT_3D('',#61031,#24818,#24819);
#21221=AXIS2_PLACEMENT_3D('',#61033,#24820,#24821);
#21222=AXIS2_PLACEMENT_3D('',#61036,#24823,#24824);
#21223=AXIS2_PLACEMENT_3D('',#61037,#24825,#24826);
#21224=AXIS2_PLACEMENT_3D('',#61041,#24828,#24829);
#21225=AXIS2_PLACEMENT_3D('',#61043,#24830,#24831);
#21226=AXIS2_PLACEMENT_3D('',#61046,#24834,#24835);
#21227=AXIS2_PLACEMENT_3D('',#61048,#24837,#24838);
#21228=AXIS2_PLACEMENT_3D('',#61052,#24840,#24841);
#21229=AXIS2_PLACEMENT_3D('',#61054,#24842,#24843);
#21230=AXIS2_PLACEMENT_3D('',#61056,#24845,#24846);
#21231=AXIS2_PLACEMENT_3D('',#61059,#24847,#24848);
#21232=AXIS2_PLACEMENT_3D('',#61063,#24852,#24853);
#21233=AXIS2_PLACEMENT_3D('',#61065,#24855,#24856);
#21234=AXIS2_PLACEMENT_3D('',#61067,#24858,#24859);
#21235=AXIS2_PLACEMENT_3D('',#61068,#24860,#24861);
#21236=AXIS2_PLACEMENT_3D('',#61070,#24863,#24864);
#21237=AXIS2_PLACEMENT_3D('',#61073,#24865,#24866);
#21238=AXIS2_PLACEMENT_3D('',#61077,#24868,#24869);
#21239=AXIS2_PLACEMENT_3D('',#61081,#24871,#24872);
#21240=AXIS2_PLACEMENT_3D('',#61083,#24874,#24875);
#21241=AXIS2_PLACEMENT_3D('',#61085,#24876,#24877);
#21242=AXIS2_PLACEMENT_3D('',#61088,#24879,#24880);
#21243=AXIS2_PLACEMENT_3D('',#61089,#24881,#24882);
#21244=AXIS2_PLACEMENT_3D('',#61093,#24884,#24885);
#21245=AXIS2_PLACEMENT_3D('',#61095,#24886,#24887);
#21246=AXIS2_PLACEMENT_3D('',#61098,#24890,#24891);
#21247=AXIS2_PLACEMENT_3D('',#61100,#24893,#24894);
#21248=AXIS2_PLACEMENT_3D('',#61104,#24896,#24897);
#21249=AXIS2_PLACEMENT_3D('',#61106,#24898,#24899);
#21250=AXIS2_PLACEMENT_3D('',#61108,#24901,#24902);
#21251=AXIS2_PLACEMENT_3D('',#61111,#24903,#24904);
#21252=AXIS2_PLACEMENT_3D('',#61115,#24908,#24909);
#21253=AXIS2_PLACEMENT_3D('',#61117,#24911,#24912);
#21254=AXIS2_PLACEMENT_3D('',#61119,#24914,#24915);
#21255=AXIS2_PLACEMENT_3D('',#61120,#24916,#24917);
#21256=AXIS2_PLACEMENT_3D('',#61122,#24919,#24920);
#21257=AXIS2_PLACEMENT_3D('',#61123,#24921,#24922);
#21258=AXIS2_PLACEMENT_3D('',#61124,#24923,#24924);
#21259=AXIS2_PLACEMENT_3D('',#61125,#24925,#24926);
#21260=AXIS2_PLACEMENT_3D('',#61126,#24927,#24928);
#21261=AXIS2_PLACEMENT_3D('',#61127,#24929,#24930);
#21262=AXIS2_PLACEMENT_3D('',#61128,#24931,#24932);
#21263=AXIS2_PLACEMENT_3D('',#61131,#24933,#24934);
#21264=AXIS2_PLACEMENT_3D('',#61133,#24935,#24936);
#21265=AXIS2_PLACEMENT_3D('',#61134,#24937,#24938);
#21266=AXIS2_PLACEMENT_3D('',#61135,#24939,#24940);
#21267=AXIS2_PLACEMENT_3D('',#61138,#24941,#24942);
#21268=AXIS2_PLACEMENT_3D('',#61140,#24943,#24944);
#21269=AXIS2_PLACEMENT_3D('',#61141,#24945,#24946);
#21270=AXIS2_PLACEMENT_3D('',#61142,#24947,#24948);
#21271=AXIS2_PLACEMENT_3D('',#61145,#24949,#24950);
#21272=AXIS2_PLACEMENT_3D('',#61148,#24953,#24954);
#21273=AXIS2_PLACEMENT_3D('',#61151,#24955,#24956);
#21274=AXIS2_PLACEMENT_3D('',#61154,#24959,#24960);
#21275=AXIS2_PLACEMENT_3D('',#61157,#24963,#24964);
#21276=AXIS2_PLACEMENT_3D('',#61160,#24965,#24966);
#21277=AXIS2_PLACEMENT_3D('',#61162,#24967,#24968);
#21278=AXIS2_PLACEMENT_3D('',#61163,#24969,#24970);
#21279=AXIS2_PLACEMENT_3D('',#61164,#24971,#24972);
#21280=AXIS2_PLACEMENT_3D('',#61166,#24973,#24974);
#21281=AXIS2_PLACEMENT_3D('',#61169,#24977,#24978);
#21282=AXIS2_PLACEMENT_3D('',#61174,#24981,#24982);
#21283=AXIS2_PLACEMENT_3D('',#61175,#24983,#24984);
#21284=AXIS2_PLACEMENT_3D('',#61180,#24987,#24988);
#21285=AXIS2_PLACEMENT_3D('',#61181,#24989,#24990);
#21286=AXIS2_PLACEMENT_3D('',#61184,#24991,#24992);
#21287=AXIS2_PLACEMENT_3D('',#61186,#24993,#24994);
#21288=AXIS2_PLACEMENT_3D('',#61187,#24995,#24996);
#21289=AXIS2_PLACEMENT_3D('',#61188,#24997,#24998);
#21290=AXIS2_PLACEMENT_3D('',#61191,#25001,#25002);
#21291=AXIS2_PLACEMENT_3D('',#61194,#25003,#25004);
#21292=AXIS2_PLACEMENT_3D('',#61197,#25007,#25008);
#21293=AXIS2_PLACEMENT_3D('',#61200,#25009,#25010);
#21294=AXIS2_PLACEMENT_3D('',#61202,#25011,#25012);
#21295=AXIS2_PLACEMENT_3D('',#61203,#25013,#25014);
#21296=AXIS2_PLACEMENT_3D('',#61204,#25015,#25016);
#21297=AXIS2_PLACEMENT_3D('',#61207,#25019,#25020);
#21298=AXIS2_PLACEMENT_3D('',#61210,#25023,#25024);
#21299=AXIS2_PLACEMENT_3D('',#61213,#25025,#25026);
#21300=AXIS2_PLACEMENT_3D('',#61215,#25027,#25028);
#21301=AXIS2_PLACEMENT_3D('',#61216,#25029,#25030);
#21302=AXIS2_PLACEMENT_3D('',#61217,#25031,#25032);
#21303=AXIS2_PLACEMENT_3D('',#61220,#25033,#25034);
#21304=AXIS2_PLACEMENT_3D('',#61222,#25035,#25036);
#21305=AXIS2_PLACEMENT_3D('',#61223,#25037,#25038);
#21306=AXIS2_PLACEMENT_3D('',#61224,#25039,#25040);
#21307=AXIS2_PLACEMENT_3D('',#61227,#25041,#25042);
#21308=AXIS2_PLACEMENT_3D('',#61230,#25045,#25046);
#21309=AXIS2_PLACEMENT_3D('',#61233,#25047,#25048);
#21310=AXIS2_PLACEMENT_3D('',#61235,#25049,#25050);
#21311=AXIS2_PLACEMENT_3D('',#61236,#25051,#25052);
#21312=AXIS2_PLACEMENT_3D('',#61237,#25053,#25054);
#21313=AXIS2_PLACEMENT_3D('',#61240,#25057,#25058);
#21314=AXIS2_PLACEMENT_3D('',#61245,#25061,#25062);
#21315=AXIS2_PLACEMENT_3D('',#61246,#25063,#25064);
#21316=AXIS2_PLACEMENT_3D('',#61249,#25065,#25066);
#21317=AXIS2_PLACEMENT_3D('',#61251,#25067,#25068);
#21318=AXIS2_PLACEMENT_3D('',#61252,#25069,#25070);
#21319=AXIS2_PLACEMENT_3D('',#61253,#25071,#25072);
#21320=AXIS2_PLACEMENT_3D('',#61256,#25075,#25076);
#21321=AXIS2_PLACEMENT_3D('',#61259,#25079,#25080);
#21322=AXIS2_PLACEMENT_3D('',#61262,#25081,#25082);
#21323=AXIS2_PLACEMENT_3D('',#61265,#25085,#25086);
#21324=AXIS2_PLACEMENT_3D('',#61267,#25087,#25088);
#21325=AXIS2_PLACEMENT_3D('',#61268,#25089,#25090);
#21326=AXIS2_PLACEMENT_3D('',#61269,#25091,#25092);
#21327=AXIS2_PLACEMENT_3D('',#61272,#25095,#25096);
#21328=AXIS2_PLACEMENT_3D('',#61274,#25097,#25098);
#21329=AXIS2_PLACEMENT_3D('',#61277,#25101,#25102);
#21330=AXIS2_PLACEMENT_3D('',#61345,#25105,#25106);
#21331=AXIS2_PLACEMENT_3D('',#61346,#25107,#25108);
#21332=AXIS2_PLACEMENT_3D('',#61378,#25109,#25110);
#21333=AXIS2_PLACEMENT_3D('',#61379,#25111,#25112);
#21334=AXIS2_PLACEMENT_3D('',#61386,#25113,#25114);
#21335=AXIS2_PLACEMENT_3D('',#61387,#25115,#25116);
#21336=AXIS2_PLACEMENT_3D('',#61388,#25117,#25118);
#21337=AXIS2_PLACEMENT_3D('',#61390,#25120,#25121);
#21338=AXIS2_PLACEMENT_3D('',#61393,#25123,#25124);
#21339=AXIS2_PLACEMENT_3D('',#61395,#25125,#25126);
#21340=AXIS2_PLACEMENT_3D('',#61396,#25127,#25128);
#21341=AXIS2_PLACEMENT_3D('',#61398,#25130,#25131);
#21342=AXIS2_PLACEMENT_3D('',#61400,#25133,#25134);
#21343=AXIS2_PLACEMENT_3D('',#61401,#25135,#25136);
#21344=AXIS2_PLACEMENT_3D('',#61402,#25137,#25138);
#21345=AXIS2_PLACEMENT_3D('',#61404,#25140,#25141);
#21346=AXIS2_PLACEMENT_3D('',#61408,#25143,#25144);
#21347=AXIS2_PLACEMENT_3D('',#61410,#25146,#25147);
#21348=AXIS2_PLACEMENT_3D('',#61413,#25150,#25151);
#21349=AXIS2_PLACEMENT_3D('',#61415,#25153,#25154);
#21350=AXIS2_PLACEMENT_3D('',#61417,#25155,#25156);
#21351=AXIS2_PLACEMENT_3D('',#61419,#25157,#25158);
#21352=AXIS2_PLACEMENT_3D('',#61420,#25159,#25160);
#21353=AXIS2_PLACEMENT_3D('',#61421,#25161,#25162);
#21354=AXIS2_PLACEMENT_3D('',#61423,#25163,#25164);
#21355=AXIS2_PLACEMENT_3D('',#61425,#25166,#25167);
#21356=AXIS2_PLACEMENT_3D('',#61427,#25168,#25169);
#21357=AXIS2_PLACEMENT_3D('',#61429,#25170,#25171);
#21358=AXIS2_PLACEMENT_3D('',#61430,#25172,#25173);
#21359=AXIS2_PLACEMENT_3D('',#61431,#25174,#25175);
#21360=AXIS2_PLACEMENT_3D('',#61433,#25176,#25177);
#21361=AXIS2_PLACEMENT_3D('',#61434,#25178,#25179);
#21362=AXIS2_PLACEMENT_3D('',#61438,#25181,#25182);
#21363=AXIS2_PLACEMENT_3D('',#61439,#25183,#25184);
#21364=AXIS2_PLACEMENT_3D('',#61441,#25185,#25186);
#21365=AXIS2_PLACEMENT_3D('',#61443,#25187,#25188);
#21366=AXIS2_PLACEMENT_3D('',#61445,#25189,#25190);
#21367=AXIS2_PLACEMENT_3D('',#61446,#25191,#25192);
#21368=AXIS2_PLACEMENT_3D('',#61447,#25193,#25194);
#21369=AXIS2_PLACEMENT_3D('',#61449,#25195,#25196);
#21370=AXIS2_PLACEMENT_3D('',#61450,#25197,#25198);
#21371=AXIS2_PLACEMENT_3D('',#61451,#25199,#25200);
#21372=AXIS2_PLACEMENT_3D('',#61453,#25201,#25202);
#21373=AXIS2_PLACEMENT_3D('',#61455,#25203,#25204);
#21374=AXIS2_PLACEMENT_3D('',#61456,#25205,#25206);
#21375=AXIS2_PLACEMENT_3D('',#61457,#25207,#25208);
#21376=AXIS2_PLACEMENT_3D('',#61460,#25210,#25211);
#21377=AXIS2_PLACEMENT_3D('',#61461,#25212,#25213);
#21378=AXIS2_PLACEMENT_3D('',#61463,#25214,#25215);
#21379=AXIS2_PLACEMENT_3D('',#61465,#25216,#25217);
#21380=AXIS2_PLACEMENT_3D('',#61466,#25218,#25219);
#21381=AXIS2_PLACEMENT_3D('',#61467,#25220,#25221);
#21382=AXIS2_PLACEMENT_3D('',#61470,#25223,#25224);
#21383=AXIS2_PLACEMENT_3D('',#61471,#25225,#25226);
#21384=AXIS2_PLACEMENT_3D('',#61476,#25228,#25229);
#21385=AXIS2_PLACEMENT_3D('',#61479,#25231,#25232);
#21386=AXIS2_PLACEMENT_3D('',#61480,#25233,#25234);
#21387=AXIS2_PLACEMENT_3D('',#61498,#25237,#25238);
#21388=AXIS2_PLACEMENT_3D('',#61518,#25241,#25242);
#21389=AXIS2_PLACEMENT_3D('',#61519,#25243,#25244);
#21390=AXIS2_PLACEMENT_3D('',#61520,#25245,#25246);
#21391=AXIS2_PLACEMENT_3D('',#61537,#25247,#25248);
#21392=AXIS2_PLACEMENT_3D('',#61556,#25249,#25250);
#21393=AXIS2_PLACEMENT_3D('',#61562,#25254,#25255);
#21394=AXIS2_PLACEMENT_3D('',#61564,#25256,#25257);
#21395=AXIS2_PLACEMENT_3D('',#61566,#25259,#25260);
#21396=AXIS2_PLACEMENT_3D('',#61569,#25262,#25263);
#21397=AXIS2_PLACEMENT_3D('',#61570,#25264,#25265);
#21398=AXIS2_PLACEMENT_3D('',#61572,#25267,#25268);
#21399=AXIS2_PLACEMENT_3D('',#61574,#25269,#25270);
#21400=AXIS2_PLACEMENT_3D('',#61576,#25271,#25272);
#21401=AXIS2_PLACEMENT_3D('',#61577,#25273,#25274);
#21402=AXIS2_PLACEMENT_3D('',#61578,#25275,#25276);
#21403=AXIS2_PLACEMENT_3D('',#61580,#25277,#25278);
#21404=AXIS2_PLACEMENT_3D('',#61581,#25279,#25280);
#21405=AXIS2_PLACEMENT_3D('',#61583,#25281,#25282);
#21406=AXIS2_PLACEMENT_3D('',#61584,#25283,#25284);
#21407=AXIS2_PLACEMENT_3D('',#61585,#25285,#25286);
#21408=AXIS2_PLACEMENT_3D('',#61587,#25287,#25288);
#21409=AXIS2_PLACEMENT_3D('',#61589,#25289,#25290);
#21410=AXIS2_PLACEMENT_3D('',#61590,#25291,#25292);
#21411=AXIS2_PLACEMENT_3D('',#61591,#25293,#25294);
#21412=AXIS2_PLACEMENT_3D('',#61593,#25295,#25296);
#21413=AXIS2_PLACEMENT_3D('',#61594,#25297,#25298);
#21414=AXIS2_PLACEMENT_3D('',#61596,#25299,#25300);
#21415=AXIS2_PLACEMENT_3D('',#61597,#25301,#25302);
#21416=AXIS2_PLACEMENT_3D('',#61598,#25303,#25304);
#21417=AXIS2_PLACEMENT_3D('',#61600,#25305,#25306);
#21418=AXIS2_PLACEMENT_3D('',#61602,#25307,#25308);
#21419=AXIS2_PLACEMENT_3D('',#61603,#25309,#25310);
#21420=AXIS2_PLACEMENT_3D('',#61604,#25311,#25312);
#21421=AXIS2_PLACEMENT_3D('',#61605,#25313,#25314);
#21422=AXIS2_PLACEMENT_3D('',#61606,#25315,#25316);
#21423=AXIS2_PLACEMENT_3D('',#61607,#25317,#25318);
#21424=AXIS2_PLACEMENT_3D('',#61608,#25319,#25320);
#21425=AXIS2_PLACEMENT_3D('',#61609,#25321,#25322);
#21426=AXIS2_PLACEMENT_3D('',#61610,#25323,#25324);
#21427=AXIS2_PLACEMENT_3D('',#61611,#25325,#25326);
#21428=AXIS2_PLACEMENT_3D('',#61612,#25327,#25328);
#21429=AXIS2_PLACEMENT_3D('',#61614,#25329,#25330);
#21430=AXIS2_PLACEMENT_3D('',#61615,#25331,#25332);
#21431=AXIS2_PLACEMENT_3D('',#61617,#25333,#25334);
#21432=AXIS2_PLACEMENT_3D('',#61620,#25336,#25337);
#21433=AXIS2_PLACEMENT_3D('',#61621,#25338,#25339);
#21434=AXIS2_PLACEMENT_3D('',#61623,#25341,#25342);
#21435=AXIS2_PLACEMENT_3D('',#61624,#25343,#25344);
#21436=AXIS2_PLACEMENT_3D('',#61625,#25345,#25346);
#21437=AXIS2_PLACEMENT_3D('',#61626,#25347,#25348);
#21438=AXIS2_PLACEMENT_3D('',#61627,#25349,#25350);
#21439=AXIS2_PLACEMENT_3D('',#61630,#25351,#25352);
#21440=AXIS2_PLACEMENT_3D('',#61633,#25354,#25355);
#21441=AXIS2_PLACEMENT_3D('',#61634,#25356,#25357);
#21442=AXIS2_PLACEMENT_3D('',#61635,#25358,#25359);
#21443=AXIS2_PLACEMENT_3D('',#61638,#25360,#25361);
#21444=AXIS2_PLACEMENT_3D('',#61639,#25362,#25363);
#21445=AXIS2_PLACEMENT_3D('',#61641,#25365,#25366);
#21446=AXIS2_PLACEMENT_3D('',#61643,#25367,#25368);
#21447=AXIS2_PLACEMENT_3D('',#61644,#25369,#25370);
#21448=AXIS2_PLACEMENT_3D('',#61647,#25372,#25373);
#21449=AXIS2_PLACEMENT_3D('',#61648,#25374,#25375);
#21450=AXIS2_PLACEMENT_3D('',#61651,#25376,#25377);
#21451=AXIS2_PLACEMENT_3D('',#61659,#25381,#25382);
#21452=AXIS2_PLACEMENT_3D('',#61667,#25386,#25387);
#21453=AXIS2_PLACEMENT_3D('',#61675,#25391,#25392);
#21454=AXIS2_PLACEMENT_3D('',#61683,#25396,#25397);
#21455=AXIS2_PLACEMENT_3D('',#61691,#25401,#25402);
#21456=AXIS2_PLACEMENT_3D('',#61699,#25406,#25407);
#21457=AXIS2_PLACEMENT_3D('',#61707,#25411,#25412);
#21458=AXIS2_PLACEMENT_3D('',#61715,#25416,#25417);
#21459=AXIS2_PLACEMENT_3D('',#61723,#25421,#25422);
#21460=AXIS2_PLACEMENT_3D('',#61731,#25426,#25427);
#21461=AXIS2_PLACEMENT_3D('',#61739,#25431,#25432);
#21462=AXIS2_PLACEMENT_3D('',#61747,#25436,#25437);
#21463=AXIS2_PLACEMENT_3D('',#61755,#25441,#25442);
#21464=AXIS2_PLACEMENT_3D('',#61761,#25446,#25447);
#21465=AXIS2_PLACEMENT_3D('',#61767,#25451,#25452);
#21466=AXIS2_PLACEMENT_3D('',#61773,#25456,#25457);
#21467=AXIS2_PLACEMENT_3D('',#61775,#25459,#25460);
#21468=AXIS2_PLACEMENT_3D('',#61777,#25461,#25462);
#21469=AXIS2_PLACEMENT_3D('',#61779,#25464,#25465);
#21470=AXIS2_PLACEMENT_3D('',#61783,#25468,#25469);
#21471=AXIS2_PLACEMENT_3D('',#61789,#25473,#25474);
#21472=AXIS2_PLACEMENT_3D('',#61791,#25476,#25477);
#21473=AXIS2_PLACEMENT_3D('',#61793,#25478,#25479);
#21474=AXIS2_PLACEMENT_3D('',#61795,#25481,#25482);
#21475=AXIS2_PLACEMENT_3D('',#61799,#25485,#25486);
#21476=AXIS2_PLACEMENT_3D('',#61805,#25490,#25491);
#21477=AXIS2_PLACEMENT_3D('',#61807,#25493,#25494);
#21478=AXIS2_PLACEMENT_3D('',#61809,#25495,#25496);
#21479=AXIS2_PLACEMENT_3D('',#61811,#25498,#25499);
#21480=AXIS2_PLACEMENT_3D('',#61815,#25502,#25503);
#21481=AXIS2_PLACEMENT_3D('',#61821,#25507,#25508);
#21482=AXIS2_PLACEMENT_3D('',#61823,#25510,#25511);
#21483=AXIS2_PLACEMENT_3D('',#61825,#25512,#25513);
#21484=AXIS2_PLACEMENT_3D('',#61827,#25515,#25516);
#21485=AXIS2_PLACEMENT_3D('',#61831,#25519,#25520);
#21486=AXIS2_PLACEMENT_3D('',#61837,#25524,#25525);
#21487=AXIS2_PLACEMENT_3D('',#61839,#25527,#25528);
#21488=AXIS2_PLACEMENT_3D('',#61841,#25529,#25530);
#21489=AXIS2_PLACEMENT_3D('',#61843,#25532,#25533);
#21490=AXIS2_PLACEMENT_3D('',#61847,#25536,#25537);
#21491=AXIS2_PLACEMENT_3D('',#61853,#25541,#25542);
#21492=AXIS2_PLACEMENT_3D('',#61855,#25544,#25545);
#21493=AXIS2_PLACEMENT_3D('',#61857,#25546,#25547);
#21494=AXIS2_PLACEMENT_3D('',#61859,#25549,#25550);
#21495=AXIS2_PLACEMENT_3D('',#61863,#25553,#25554);
#21496=AXIS2_PLACEMENT_3D('',#61869,#25558,#25559);
#21497=AXIS2_PLACEMENT_3D('',#61871,#25561,#25562);
#21498=AXIS2_PLACEMENT_3D('',#61873,#25563,#25564);
#21499=AXIS2_PLACEMENT_3D('',#61875,#25566,#25567);
#21500=AXIS2_PLACEMENT_3D('',#61879,#25570,#25571);
#21501=AXIS2_PLACEMENT_3D('',#61885,#25575,#25576);
#21502=AXIS2_PLACEMENT_3D('',#61887,#25578,#25579);
#21503=AXIS2_PLACEMENT_3D('',#61889,#25580,#25581);
#21504=AXIS2_PLACEMENT_3D('',#61891,#25583,#25584);
#21505=AXIS2_PLACEMENT_3D('',#61895,#25587,#25588);
#21506=AXIS2_PLACEMENT_3D('',#61901,#25592,#25593);
#21507=AXIS2_PLACEMENT_3D('',#61903,#25595,#25596);
#21508=AXIS2_PLACEMENT_3D('',#61905,#25597,#25598);
#21509=AXIS2_PLACEMENT_3D('',#61907,#25600,#25601);
#21510=AXIS2_PLACEMENT_3D('',#61911,#25604,#25605);
#21511=AXIS2_PLACEMENT_3D('',#61917,#25609,#25610);
#21512=AXIS2_PLACEMENT_3D('',#61919,#25612,#25613);
#21513=AXIS2_PLACEMENT_3D('',#61921,#25614,#25615);
#21514=AXIS2_PLACEMENT_3D('',#61923,#25617,#25618);
#21515=AXIS2_PLACEMENT_3D('',#61927,#25621,#25622);
#21516=AXIS2_PLACEMENT_3D('',#61933,#25626,#25627);
#21517=AXIS2_PLACEMENT_3D('',#61935,#25629,#25630);
#21518=AXIS2_PLACEMENT_3D('',#61937,#25631,#25632);
#21519=AXIS2_PLACEMENT_3D('',#61939,#25634,#25635);
#21520=AXIS2_PLACEMENT_3D('',#61943,#25638,#25639);
#21521=AXIS2_PLACEMENT_3D('',#61949,#25643,#25644);
#21522=AXIS2_PLACEMENT_3D('',#61951,#25646,#25647);
#21523=AXIS2_PLACEMENT_3D('',#61953,#25648,#25649);
#21524=AXIS2_PLACEMENT_3D('',#61955,#25651,#25652);
#21525=AXIS2_PLACEMENT_3D('',#61959,#25655,#25656);
#21526=AXIS2_PLACEMENT_3D('',#61965,#25660,#25661);
#21527=AXIS2_PLACEMENT_3D('',#61967,#25663,#25664);
#21528=AXIS2_PLACEMENT_3D('',#61969,#25665,#25666);
#21529=AXIS2_PLACEMENT_3D('',#61971,#25668,#25669);
#21530=AXIS2_PLACEMENT_3D('',#61977,#25673,#25674);
#21531=AXIS2_PLACEMENT_3D('',#61981,#25677,#25678);
#21532=AXIS2_PLACEMENT_3D('',#61983,#25680,#25681);
#21533=AXIS2_PLACEMENT_3D('',#61984,#25682,#25683);
#21534=AXIS2_PLACEMENT_3D('',#61986,#25684,#25685);
#21535=AXIS2_PLACEMENT_3D('',#61987,#25686,#25687);
#21536=AXIS2_PLACEMENT_3D('',#61988,#25688,#25689);
#21537=AXIS2_PLACEMENT_3D('',#61990,#25691,#25692);
#21538=AXIS2_PLACEMENT_3D('',#61991,#25693,#25694);
#21539=AXIS2_PLACEMENT_3D('',#62106,#25696,#25697);
#21540=AXIS2_PLACEMENT_3D('',#62174,#25698,#25699);
#21541=AXIS2_PLACEMENT_3D('',#62604,#25701,#25702);
#21542=AXIS2_PLACEMENT_3D('',#63031,#25704,#25705);
#21543=AXIS2_PLACEMENT_3D('',#63487,#25707,#25708);
#21544=AXIS2_PLACEMENT_3D('',#63951,#25710,#25711);
#21545=AXIS2_PLACEMENT_3D('',#64294,#25713,#25714);
#21546=AXIS2_PLACEMENT_3D('',#64692,#25716,#25717);
#21547=AXIS2_PLACEMENT_3D('',#65025,#25719,#25720);
#21548=AXIS2_PLACEMENT_3D('',#65417,#25722,#25723);
#21549=AXIS2_PLACEMENT_3D('',#65800,#25725,#25726);
#21550=AXIS2_PLACEMENT_3D('',#66199,#25728,#25729);
#21551=AXIS2_PLACEMENT_3D('',#66755,#25731,#25732);
#21552=AXIS2_PLACEMENT_3D('',#67216,#25734,#25735);
#21553=AXIS2_PLACEMENT_3D('',#67746,#25737,#25738);
#21554=AXIS2_PLACEMENT_3D('',#68199,#25740,#25741);
#21555=AXIS2_PLACEMENT_3D('',#68738,#25743,#25744);
#21556=AXIS2_PLACEMENT_3D('',#69200,#25746,#25747);
#21557=AXIS2_PLACEMENT_3D('',#69711,#25749,#25750);
#21558=AXIS2_PLACEMENT_3D('',#70194,#25752,#25753);
#21559=AXIS2_PLACEMENT_3D('',#70658,#25755,#25756);
#21560=AXIS2_PLACEMENT_3D('',#71125,#25758,#25759);
#21561=AXIS2_PLACEMENT_3D('',#71589,#25761,#25762);
#21562=AXIS2_PLACEMENT_3D('',#72041,#25764,#25765);
#21563=AXIS2_PLACEMENT_3D('',#72527,#25767,#25768);
#21564=AXIS2_PLACEMENT_3D('',#72980,#25770,#25771);
#21565=AXIS2_PLACEMENT_3D('',#73453,#25773,#25774);
#21566=AXIS2_PLACEMENT_3D('',#73921,#25776,#25777);
#21567=AXIS2_PLACEMENT_3D('',#74393,#25779,#25780);
#21568=AXIS2_PLACEMENT_3D('',#74855,#25782,#25783);
#21569=AXIS2_PLACEMENT_3D('',#75315,#25785,#25786);
#21570=AXIS2_PLACEMENT_3D('',#75801,#25788,#25789);
#21571=AXIS2_PLACEMENT_3D('',#76258,#25791,#25792);
#21572=AXIS2_PLACEMENT_3D('',#76729,#25794,#25795);
#21573=AXIS2_PLACEMENT_3D('',#77191,#25797,#25798);
#21574=AXIS2_PLACEMENT_3D('',#77652,#25800,#25801);
#21575=AXIS2_PLACEMENT_3D('',#78089,#25803,#25804);
#21576=AXIS2_PLACEMENT_3D('',#78385,#25806,#25807);
#21577=AXIS2_PLACEMENT_3D('',#78745,#25809,#25810);
#21578=AXIS2_PLACEMENT_3D('',#79047,#25812,#25813);
#21579=AXIS2_PLACEMENT_3D('',#79124,#25814,#25815);
#21580=AXIS2_PLACEMENT_3D('',#84052,#25816,#25817);
#21581=AXIS2_PLACEMENT_3D('',#88373,#25818,#25819);
#21582=AXIS2_PLACEMENT_3D('',#88453,#25820,#25821);
#21583=AXIS2_PLACEMENT_3D('',#88558,#25822,#25823);
#21584=AXIS2_PLACEMENT_3D('',#88560,#25824,#25825);
#21585=AXIS2_PLACEMENT_3D('',#88563,#25827,#25828);
#21586=AXIS2_PLACEMENT_3D('',#88564,#25829,#25830);
#21587=AXIS2_PLACEMENT_3D('',#88565,#25831,#25832);
#21588=AXIS2_PLACEMENT_3D('',#88568,#25833,#25834);
#21589=AXIS2_PLACEMENT_3D('',#88757,#25835,#25836);
#21590=AXIS2_PLACEMENT_3D('',#89856,#25837,#25838);
#21591=AXIS2_PLACEMENT_3D('',#89858,#25839,#25840);
#21592=AXIS2_PLACEMENT_3D('',#89860,#25841,#25842);
#21593=AXIS2_PLACEMENT_3D('',#90950,#25843,#25844);
#21594=AXIS2_PLACEMENT_3D('',#90952,#25845,#25846);
#21595=AXIS2_PLACEMENT_3D('',#90953,#25847,#25848);
#21596=AXIS2_PLACEMENT_3D('',#90955,#25850,#25851);
#21597=AXIS2_PLACEMENT_3D('',#90958,#25853,#25854);
#21598=AXIS2_PLACEMENT_3D('',#90959,#25855,#25856);
#21599=AXIS2_PLACEMENT_3D('',#90961,#25857,#25858);
#21600=AXIS2_PLACEMENT_3D('',#90963,#25860,#25861);
#21601=AXIS2_PLACEMENT_3D('',#90965,#25862,#25863);
#21602=AXIS2_PLACEMENT_3D('',#90966,#25864,#25865);
#21603=AXIS2_PLACEMENT_3D('',#90968,#25866,#25867);
#21604=AXIS2_PLACEMENT_3D('',#90970,#25869,#25870);
#21605=AXIS2_PLACEMENT_3D('',#90972,#25871,#25872);
#21606=AXIS2_PLACEMENT_3D('',#90973,#25873,#25874);
#21607=AXIS2_PLACEMENT_3D('',#90975,#25875,#25876);
#21608=AXIS2_PLACEMENT_3D('',#90977,#25878,#25879);
#21609=AXIS2_PLACEMENT_3D('',#90980,#25881,#25882);
#21610=AXIS2_PLACEMENT_3D('',#90981,#25883,#25884);
#21611=AXIS2_PLACEMENT_3D('',#90982,#25885,#25886);
#21612=AXIS2_PLACEMENT_3D('',#90983,#25887,#25888);
#21613=AXIS2_PLACEMENT_3D('',#90997,#25889,#25890);
#21614=AXIS2_PLACEMENT_3D('',#91009,#25891,#25892);
#21615=AXIS2_PLACEMENT_3D('',#91010,#25893,#25894);
#21616=AXIS2_PLACEMENT_3D('',#91012,#25896,#25897);
#21617=AXIS2_PLACEMENT_3D('',#91028,#25898,#25899);
#21618=AXIS2_PLACEMENT_3D('',#91047,#25900,#25901);
#21619=AXIS2_PLACEMENT_3D('',#91048,#25902,#25903);
#21620=AXIS2_PLACEMENT_3D('',#91052,#25906,#25907);
#21621=AXIS2_PLACEMENT_3D('',#91055,#25908,#25909);
#21622=AXIS2_PLACEMENT_3D('',#91075,#25910,#25911);
#21623=AXIS2_PLACEMENT_3D('',#91104,#25912,#25913);
#21624=AXIS2_PLACEMENT_3D('',#91137,#25916,#25917);
#21625=AXIS2_PLACEMENT_3D('',#91139,#25918,#25919);
#21626=AXIS2_PLACEMENT_3D('',#91158,#25920,#25921);
#21627=AXIS2_PLACEMENT_3D('',#91159,#25922,#25923);
#21628=AXIS2_PLACEMENT_3D('',#91161,#25925,#25926);
#21629=AXIS2_PLACEMENT_3D('',#91173,#25927,#25928);
#21630=AXIS2_PLACEMENT_3D('',#91188,#25929,#25930);
#21631=AXIS2_PLACEMENT_3D('',#91197,#25931,#25932);
#21632=AXIS2_PLACEMENT_3D('',#91201,#25935,#25936);
#21633=AXIS2_PLACEMENT_3D('',#91204,#25937,#25938);
#21634=AXIS2_PLACEMENT_3D('',#91208,#25940,#25941);
#21635=AXIS2_PLACEMENT_3D('',#91210,#25943,#25944);
#21636=AXIS2_PLACEMENT_3D('',#91216,#25948,#25949);
#21637=AXIS2_PLACEMENT_3D('',#91218,#25950,#25951);
#21638=AXIS2_PLACEMENT_3D('',#91221,#25953,#25954);
#21639=AXIS2_PLACEMENT_3D('',#91222,#25955,#25956);
#21640=AXIS2_PLACEMENT_3D('',#91226,#25958,#25959);
#21641=AXIS2_PLACEMENT_3D('',#91230,#25961,#25962);
#21642=AXIS2_PLACEMENT_3D('',#91234,#25964,#25965);
#21643=AXIS2_PLACEMENT_3D('',#91238,#25967,#25968);
#21644=AXIS2_PLACEMENT_3D('',#91242,#25970,#25971);
#21645=AXIS2_PLACEMENT_3D('',#91253,#25978,#25979);
#21646=AXIS2_PLACEMENT_3D('',#91266,#25980,#25981);
#21647=AXIS2_PLACEMENT_3D('',#91269,#25983,#25984);
#21648=AXIS2_PLACEMENT_3D('',#91270,#25985,#25986);
#21649=AXIS2_PLACEMENT_3D('',#91273,#25988,#25989);
#21650=AXIS2_PLACEMENT_3D('',#91274,#25990,#25991);
#21651=AXIS2_PLACEMENT_3D('',#91279,#25993,#25994);
#21652=AXIS2_PLACEMENT_3D('',#91288,#25995,#25996);
#21653=AXIS2_PLACEMENT_3D('',#91314,#25999,#26000);
#21654=AXIS2_PLACEMENT_3D('',#91316,#26001,#26002);
#21655=AXIS2_PLACEMENT_3D('',#91320,#26004,#26005);
#21656=AXIS2_PLACEMENT_3D('',#91324,#26007,#26008);
#21657=AXIS2_PLACEMENT_3D('',#91327,#26010,#26011);
#21658=AXIS2_PLACEMENT_3D('',#91328,#26012,#26013);
#21659=AXIS2_PLACEMENT_3D('',#91334,#26017,#26018);
#21660=AXIS2_PLACEMENT_3D('',#91336,#26019,#26020);
#21661=AXIS2_PLACEMENT_3D('',#91340,#26023,#26024);
#21662=AXIS2_PLACEMENT_3D('',#91344,#26026,#26027);
#21663=AXIS2_PLACEMENT_3D('',#91346,#26029,#26030);
#21664=AXIS2_PLACEMENT_3D('',#91354,#26034,#26035);
#21665=AXIS2_PLACEMENT_3D('',#91360,#26038,#26039);
#21666=AXIS2_PLACEMENT_3D('',#91362,#26041,#26042);
#21667=AXIS2_PLACEMENT_3D('',#91373,#26048,#26049);
#21668=AXIS2_PLACEMENT_3D('',#91378,#26051,#26052);
#21669=AXIS2_PLACEMENT_3D('',#91381,#26054,#26055);
#21670=AXIS2_PLACEMENT_3D('',#91382,#26056,#26057);
#21671=AXIS2_PLACEMENT_3D('',#91383,#26058,#26059);
#21672=AXIS2_PLACEMENT_3D('',#91391,#26060,#26061);
#21673=AXIS2_PLACEMENT_3D('',#91392,#26062,#26063);
#21674=AXIS2_PLACEMENT_3D('',#91393,#26064,#26065);
#21675=AXIS2_PLACEMENT_3D('',#91395,#26066,#26067);
#21676=AXIS2_PLACEMENT_3D('',#91398,#26069,#26070);
#21677=AXIS2_PLACEMENT_3D('',#91400,#26071,#26072);
#21678=AXIS2_PLACEMENT_3D('',#91402,#26074,#26075);
#21679=AXIS2_PLACEMENT_3D('',#91405,#26076,#26077);
#21680=AXIS2_PLACEMENT_3D('',#91408,#26080,#26081);
#21681=AXIS2_PLACEMENT_3D('',#91410,#26082,#26083);
#21682=AXIS2_PLACEMENT_3D('',#91414,#26085,#26086);
#21683=AXIS2_PLACEMENT_3D('',#91416,#26088,#26089);
#21684=AXIS2_PLACEMENT_3D('',#91430,#26091,#26092);
#21685=AXIS2_PLACEMENT_3D('',#91432,#26094,#26095);
#21686=AXIS2_PLACEMENT_3D('',#91433,#26096,#26097);
#21687=AXIS2_PLACEMENT_3D('',#91434,#26098,#26099);
#21688=AXIS2_PLACEMENT_3D('',#91435,#26100,#26101);
#21689=AXIS2_PLACEMENT_3D('',#91436,#26102,#26103);
#21690=AXIS2_PLACEMENT_3D('',#91444,#26108,#26109);
#21691=AXIS2_PLACEMENT_3D('',#91447,#26111,#26112);
#21692=AXIS2_PLACEMENT_3D('',#91448,#26113,#26114);
#21693=AXIS2_PLACEMENT_3D('',#91461,#26122,#26123);
#21694=AXIS2_PLACEMENT_3D('',#91464,#26125,#26126);
#21695=AXIS2_PLACEMENT_3D('',#91465,#26127,#26128);
#21696=AXIS2_PLACEMENT_3D('',#91467,#26129,#26130);
#21697=AXIS2_PLACEMENT_3D('',#91473,#26134,#26135);
#21698=AXIS2_PLACEMENT_3D('',#91475,#26136,#26137);
#21699=AXIS2_PLACEMENT_3D('',#91477,#26138,#26139);
#21700=AXIS2_PLACEMENT_3D('',#91478,#26140,#26141);
#21701=AXIS2_PLACEMENT_3D('',#91479,#26142,#26143);
#21702=AXIS2_PLACEMENT_3D('',#91482,#26144,#26145);
#21703=AXIS2_PLACEMENT_3D('',#91494,#26147,#26148);
#21704=AXIS2_PLACEMENT_3D('',#91496,#26150,#26151);
#21705=AXIS2_PLACEMENT_3D('',#91500,#26153,#26154);
#21706=AXIS2_PLACEMENT_3D('',#91504,#26157,#26158);
#21707=AXIS2_PLACEMENT_3D('',#91507,#26159,#26160);
#21708=AXIS2_PLACEMENT_3D('',#91538,#26161,#26162);
#21709=AXIS2_PLACEMENT_3D('',#91567,#26163,#26164);
#21710=AXIS2_PLACEMENT_3D('',#91570,#26167,#26168);
#21711=AXIS2_PLACEMENT_3D('',#91574,#26170,#26171);
#21712=AXIS2_PLACEMENT_3D('',#91586,#26173,#26174);
#21713=AXIS2_PLACEMENT_3D('',#91607,#26177,#26178);
#21714=AXIS2_PLACEMENT_3D('',#91619,#26180,#26181);
#21715=AXIS2_PLACEMENT_3D('',#91621,#26183,#26184);
#21716=AXIS2_PLACEMENT_3D('',#91623,#26185,#26186);
#21717=AXIS2_PLACEMENT_3D('',#91624,#26187,#26188);
#21718=AXIS2_PLACEMENT_3D('',#91626,#26189,#26190);
#21719=AXIS2_PLACEMENT_3D('',#91628,#26191,#26192);
#21720=AXIS2_PLACEMENT_3D('',#91629,#26193,#26194);
#21721=AXIS2_PLACEMENT_3D('',#91630,#26195,#26196);
#21722=AXIS2_PLACEMENT_3D('',#91789,#26198,#26199);
#21723=AXIS2_PLACEMENT_3D('',#91791,#26200,#26201);
#21724=AXIS2_PLACEMENT_3D('',#91812,#26202,#26203);
#21725=AXIS2_PLACEMENT_3D('',#91814,#26205,#26206);
#21726=AXIS2_PLACEMENT_3D('',#91816,#26207,#26208);
#21727=AXIS2_PLACEMENT_3D('',#91818,#26209,#26210);
#21728=AXIS2_PLACEMENT_3D('',#91819,#26211,#26212);
#21729=AXIS2_PLACEMENT_3D('',#91820,#26213,#26214);
#21730=AXIS2_PLACEMENT_3D('',#91821,#26215,#26216);
#21731=AXIS2_PLACEMENT_3D('',#91835,#26218,#26219);
#21732=AXIS2_PLACEMENT_3D('',#91836,#26220,#26221);
#21733=AXIS2_PLACEMENT_3D('',#91839,#26222,#26223);
#21734=AXIS2_PLACEMENT_3D('',#91843,#26225,#26226);
#21735=AXIS2_PLACEMENT_3D('',#91845,#26228,#26229);
#21736=AXIS2_PLACEMENT_3D('',#91847,#26230,#26231);
#21737=AXIS2_PLACEMENT_3D('',#91850,#26233,#26234);
#21738=AXIS2_PLACEMENT_3D('',#91852,#26236,#26237);
#21739=AXIS2_PLACEMENT_3D('',#91853,#26238,#26239);
#21740=AXIS2_PLACEMENT_3D('',#91854,#26240,#26241);
#21741=AXIS2_PLACEMENT_3D('',#91855,#26242,#26243);
#21742=AXIS2_PLACEMENT_3D('',#91856,#26244,#26245);
#21743=AXIS2_PLACEMENT_3D('',#91858,#26247,#26248);
#21744=AXIS2_PLACEMENT_3D('',#91859,#26249,#26250);
#21745=AXIS2_PLACEMENT_3D('',#91860,#26251,#26252);
#21746=AXIS2_PLACEMENT_3D('',#91861,#26253,#26254);
#21747=AXIS2_PLACEMENT_3D('',#91863,#26255,#26256);
#21748=AXIS2_PLACEMENT_3D('',#91883,#26258,#26259);
#21749=AXIS2_PLACEMENT_3D('',#91885,#26260,#26261);
#21750=AXIS2_PLACEMENT_3D('',#91887,#26263,#26264);
#21751=AXIS2_PLACEMENT_3D('',#91889,#26265,#26266);
#21752=AXIS2_PLACEMENT_3D('',#91891,#26268,#26269);
#21753=AXIS2_PLACEMENT_3D('',#91892,#26270,#26271);
#21754=AXIS2_PLACEMENT_3D('',#91893,#26272,#26273);
#21755=AXIS2_PLACEMENT_3D('',#91895,#26274,#26275);
#21756=AXIS2_PLACEMENT_3D('',#91897,#26277,#26278);
#21757=AXIS2_PLACEMENT_3D('',#91899,#26279,#26280);
#21758=AXIS2_PLACEMENT_3D('',#91904,#26283,#26284);
#21759=AXIS2_PLACEMENT_3D('',#91920,#26287,#26288);
#21760=AXIS2_PLACEMENT_3D('',#91925,#26291,#26292);
#21761=AXIS2_PLACEMENT_3D('',#91927,#26294,#26295);
#21762=AXIS2_PLACEMENT_3D('',#91930,#26296,#26297);
#21763=AXIS2_PLACEMENT_3D('',#91978,#26301,#26302);
#21764=AXIS2_PLACEMENT_3D('',#91980,#26303,#26304);
#21765=AXIS2_PLACEMENT_3D('',#91984,#26306,#26307);
#21766=AXIS2_PLACEMENT_3D('',#91988,#26310,#26311);
#21767=AXIS2_PLACEMENT_3D('',#91989,#26312,#26313);
#21768=AXIS2_PLACEMENT_3D('',#91991,#26314,#26315);
#21769=AXIS2_PLACEMENT_3D('',#91994,#26317,#26318);
#21770=AXIS2_PLACEMENT_3D('',#91995,#26319,#26320);
#21771=AXIS2_PLACEMENT_3D('',#91997,#26321,#26322);
#21772=AXIS2_PLACEMENT_3D('',#91999,#26323,#26324);
#21773=AXIS2_PLACEMENT_3D('',#92001,#26326,#26327);
#21774=AXIS2_PLACEMENT_3D('',#92002,#26328,#26329);
#21775=AXIS2_PLACEMENT_3D('',#92003,#26330,#26331);
#21776=AXIS2_PLACEMENT_3D('',#92005,#26332,#26333);
#21777=AXIS2_PLACEMENT_3D('',#92008,#26335,#26336);
#21778=AXIS2_PLACEMENT_3D('',#92010,#26338,#26339);
#21779=AXIS2_PLACEMENT_3D('',#92011,#26340,#26341);
#21780=AXIS2_PLACEMENT_3D('',#92012,#26342,#26343);
#21781=AXIS2_PLACEMENT_3D('',#92014,#26345,#26346);
#21782=AXIS2_PLACEMENT_3D('',#92018,#26348,#26349);
#21783=AXIS2_PLACEMENT_3D('',#92026,#26353,#26354);
#21784=AXIS2_PLACEMENT_3D('',#92028,#26355,#26356);
#21785=AXIS2_PLACEMENT_3D('',#92031,#26358,#26359);
#21786=AXIS2_PLACEMENT_3D('',#92032,#26360,#26361);
#21787=AXIS2_PLACEMENT_3D('',#92035,#26362,#26363);
#21788=AXIS2_PLACEMENT_3D('',#92037,#26364,#26365);
#21789=AXIS2_PLACEMENT_3D('',#92039,#26366,#26367);
#21790=AXIS2_PLACEMENT_3D('',#92040,#26368,#26369);
#21791=AXIS2_PLACEMENT_3D('',#92042,#26370,#26371);
#21792=AXIS2_PLACEMENT_3D('',#92057,#26372,#26373);
#21793=AXIS2_PLACEMENT_3D('',#92061,#26375,#26376);
#21794=AXIS2_PLACEMENT_3D('',#92065,#26378,#26379);
#21795=AXIS2_PLACEMENT_3D('',#92067,#26381,#26382);
#21796=AXIS2_PLACEMENT_3D('',#92069,#26383,#26384);
#21797=AXIS2_PLACEMENT_3D('',#92071,#26386,#26387);
#21798=AXIS2_PLACEMENT_3D('',#92073,#26388,#26389);
#21799=AXIS2_PLACEMENT_3D('',#92075,#26390,#26391);
#21800=AXIS2_PLACEMENT_3D('',#92077,#26392,#26393);
#21801=AXIS2_PLACEMENT_3D('',#92078,#26394,#26395);
#21802=AXIS2_PLACEMENT_3D('',#92079,#26396,#26397);
#21803=AXIS2_PLACEMENT_3D('',#92081,#26398,#26399);
#21804=AXIS2_PLACEMENT_3D('',#92083,#26401,#26402);
#21805=AXIS2_PLACEMENT_3D('',#92086,#26405,#26406);
#21806=AXIS2_PLACEMENT_3D('',#92087,#26407,#26408);
#21807=AXIS2_PLACEMENT_3D('',#92088,#26409,#26410);
#21808=AXIS2_PLACEMENT_3D('',#92089,#26411,#26412);
#21809=AXIS2_PLACEMENT_3D('',#92104,#26413,#26414);
#21810=AXIS2_PLACEMENT_3D('',#92106,#26415,#26416);
#21811=AXIS2_PLACEMENT_3D('',#92109,#26418,#26419);
#21812=AXIS2_PLACEMENT_3D('',#92110,#26420,#26421);
#21813=AXIS2_PLACEMENT_3D('',#92114,#26423,#26424);
#21814=AXIS2_PLACEMENT_3D('',#92116,#26426,#26427);
#21815=AXIS2_PLACEMENT_3D('',#92118,#26429,#26430);
#21816=AXIS2_PLACEMENT_3D('',#92120,#26432,#26433);
#21817=AXIS2_PLACEMENT_3D('',#92128,#26438,#26439);
#21818=AXIS2_PLACEMENT_3D('',#92129,#26440,#26441);
#21819=AXIS2_PLACEMENT_3D('',#92131,#26443,#26444);
#21820=AXIS2_PLACEMENT_3D('',#92133,#26446,#26447);
#21821=AXIS2_PLACEMENT_3D('',#92134,#26448,#26449);
#21822=AXIS2_PLACEMENT_3D('',#92135,#26450,#26451);
#21823=AXIS2_PLACEMENT_3D('',#92136,#26452,#26453);
#21824=AXIS2_PLACEMENT_3D('',#92137,#26454,#26455);
#21825=AXIS2_PLACEMENT_3D('',#92139,#26457,#26458);
#21826=AXIS2_PLACEMENT_3D('',#92140,#26459,#26460);
#21827=AXIS2_PLACEMENT_3D('',#92141,#26461,#26462);
#21828=AXIS2_PLACEMENT_3D('',#92142,#26463,#26464);
#21829=AXIS2_PLACEMENT_3D('',#92143,#26465,#26466);
#21830=AXIS2_PLACEMENT_3D('',#92148,#26469,#26470);
#21831=AXIS2_PLACEMENT_3D('',#92149,#26471,#26472);
#21832=AXIS2_PLACEMENT_3D('',#92157,#26476,#26477);
#21833=AXIS2_PLACEMENT_3D('',#92195,#26497,#26498);
#21834=AXIS2_PLACEMENT_3D('',#92202,#26502,#26503);
#21835=AXIS2_PLACEMENT_3D('',#92204,#26504,#26505);
#21836=AXIS2_PLACEMENT_3D('',#92205,#26506,#26507);
#21837=AXIS2_PLACEMENT_3D('',#92207,#26508,#26509);
#21838=AXIS2_PLACEMENT_3D('',#92209,#26511,#26512);
#21839=AXIS2_PLACEMENT_3D('',#92211,#26514,#26515);
#21840=AXIS2_PLACEMENT_3D('',#92214,#26516,#26517);
#21841=AXIS2_PLACEMENT_3D('',#92215,#26518,#26519);
#21842=AXIS2_PLACEMENT_3D('',#92217,#26520,#26521);
#21843=AXIS2_PLACEMENT_3D('',#92232,#26522,#26523);
#21844=AXIS2_PLACEMENT_3D('',#92234,#26524,#26525);
#21845=AXIS2_PLACEMENT_3D('',#92237,#26528,#26529);
#21846=AXIS2_PLACEMENT_3D('',#92243,#26533,#26534);
#21847=AXIS2_PLACEMENT_3D('',#92245,#26535,#26536);
#21848=AXIS2_PLACEMENT_3D('',#92247,#26538,#26539);
#21849=AXIS2_PLACEMENT_3D('',#92251,#26542,#26543);
#21850=AXIS2_PLACEMENT_3D('',#92253,#26544,#26545);
#21851=AXIS2_PLACEMENT_3D('',#92255,#26547,#26548);
#21852=AXIS2_PLACEMENT_3D('',#92259,#26551,#26552);
#21853=AXIS2_PLACEMENT_3D('',#92262,#26554,#26555);
#21854=AXIS2_PLACEMENT_3D('',#92263,#26556,#26557);
#21855=AXIS2_PLACEMENT_3D('',#92264,#26558,#26559);
#21856=AXIS2_PLACEMENT_3D('',#92266,#26561,#26562);
#21857=AXIS2_PLACEMENT_3D('',#92267,#26563,#26564);
#21858=AXIS2_PLACEMENT_3D('',#92268,#26565,#26566);
#21859=AXIS2_PLACEMENT_3D('',#92269,#26567,#26568);
#21860=AXIS2_PLACEMENT_3D('',#92271,#26570,#26571);
#21861=AXIS2_PLACEMENT_3D('',#92272,#26572,#26573);
#21862=AXIS2_PLACEMENT_3D('',#92273,#26574,#26575);
#21863=AXIS2_PLACEMENT_3D('',#92274,#26576,#26577);
#21864=AXIS2_PLACEMENT_3D('',#92275,#26578,#26579);
#21865=AXIS2_PLACEMENT_3D('',#92276,#26580,#26581);
#21866=AXIS2_PLACEMENT_3D('',#92277,#26582,#26583);
#21867=AXIS2_PLACEMENT_3D('',#92278,#26584,#26585);
#21868=AXIS2_PLACEMENT_3D('',#92281,#26587,#26588);
#21869=AXIS2_PLACEMENT_3D('',#92282,#26589,#26590);
#21870=AXIS2_PLACEMENT_3D('',#92294,#26597,#26598);
#21871=AXIS2_PLACEMENT_3D('',#92296,#26599,#26600);
#21872=AXIS2_PLACEMENT_3D('',#92298,#26602,#26603);
#21873=AXIS2_PLACEMENT_3D('',#92300,#26604,#26605);
#21874=AXIS2_PLACEMENT_3D('',#92302,#26606,#26607);
#21875=AXIS2_PLACEMENT_3D('',#92303,#26608,#26609);
#21876=AXIS2_PLACEMENT_3D('',#92304,#26610,#26611);
#21877=AXIS2_PLACEMENT_3D('',#92307,#26612,#26613);
#21878=AXIS2_PLACEMENT_3D('',#92308,#26614,#26615);
#21879=AXIS2_PLACEMENT_3D('',#92310,#26617,#26618);
#21880=AXIS2_PLACEMENT_3D('',#92313,#26619,#26620);
#21881=AXIS2_PLACEMENT_3D('',#92324,#26626,#26627);
#21882=AXIS2_PLACEMENT_3D('',#92325,#26628,#26629);
#21883=AXIS2_PLACEMENT_3D('',#92327,#26630,#26631);
#21884=AXIS2_PLACEMENT_3D('',#92328,#26632,#26633);
#21885=AXIS2_PLACEMENT_3D('',#92343,#26634,#26635);
#21886=AXIS2_PLACEMENT_3D('',#92344,#26636,#26637);
#21887=AXIS2_PLACEMENT_3D('',#92345,#26638,#26639);
#21888=AXIS2_PLACEMENT_3D('',#92346,#26640,#26641);
#21889=AXIS2_PLACEMENT_3D('',#92349,#26642,#26643);
#21890=AXIS2_PLACEMENT_3D('',#92350,#26644,#26645);
#21891=AXIS2_PLACEMENT_3D('',#92352,#26647,#26648);
#21892=AXIS2_PLACEMENT_3D('',#92355,#26650,#26651);
#21893=AXIS2_PLACEMENT_3D('',#92356,#26652,#26653);
#21894=AXIS2_PLACEMENT_3D('',#92358,#26655,#26656);
#21895=AXIS2_PLACEMENT_3D('',#92359,#26657,#26658);
#21896=AXIS2_PLACEMENT_3D('',#92360,#26659,#26660);
#21897=AXIS2_PLACEMENT_3D('',#92361,#26661,#26662);
#21898=AXIS2_PLACEMENT_3D('',#92363,#26663,#26664);
#21899=AXIS2_PLACEMENT_3D('',#92365,#26666,#26667);
#21900=AXIS2_PLACEMENT_3D('',#92367,#26669,#26670);
#21901=AXIS2_PLACEMENT_3D('',#92369,#26671,#26672);
#21902=AXIS2_PLACEMENT_3D('',#92371,#26673,#26674);
#21903=AXIS2_PLACEMENT_3D('',#92373,#26676,#26677);
#21904=AXIS2_PLACEMENT_3D('',#92377,#26681,#26682);
#21905=AXIS2_PLACEMENT_3D('',#92379,#26683,#26684);
#21906=AXIS2_PLACEMENT_3D('',#92381,#26686,#26687);
#21907=AXIS2_PLACEMENT_3D('',#92387,#26691,#26692);
#21908=AXIS2_PLACEMENT_3D('',#92389,#26693,#26694);
#21909=AXIS2_PLACEMENT_3D('',#92391,#26696,#26697);
#21910=AXIS2_PLACEMENT_3D('',#92395,#26700,#26701);
#21911=AXIS2_PLACEMENT_3D('',#92397,#26702,#26703);
#21912=AXIS2_PLACEMENT_3D('',#92400,#26705,#26706);
#21913=AXIS2_PLACEMENT_3D('',#92401,#26707,#26708);
#21914=AXIS2_PLACEMENT_3D('',#92407,#26711,#26712);
#21915=AXIS2_PLACEMENT_3D('',#92411,#26715,#26716);
#21916=AXIS2_PLACEMENT_3D('',#92413,#26717,#26718);
#21917=AXIS2_PLACEMENT_3D('',#92416,#26720,#26721);
#21918=AXIS2_PLACEMENT_3D('',#92417,#26722,#26723);
#21919=AXIS2_PLACEMENT_3D('',#92423,#26726,#26727);
#21920=AXIS2_PLACEMENT_3D('',#92427,#26730,#26731);
#21921=AXIS2_PLACEMENT_3D('',#92429,#26732,#26733);
#21922=AXIS2_PLACEMENT_3D('',#92432,#26735,#26736);
#21923=AXIS2_PLACEMENT_3D('',#92433,#26737,#26738);
#21924=AXIS2_PLACEMENT_3D('',#92439,#26741,#26742);
#21925=AXIS2_PLACEMENT_3D('',#92443,#26745,#26746);
#21926=AXIS2_PLACEMENT_3D('',#92462,#26747,#26748);
#21927=AXIS2_PLACEMENT_3D('',#92465,#26750,#26751);
#21928=AXIS2_PLACEMENT_3D('',#92466,#26752,#26753);
#21929=AXIS2_PLACEMENT_3D('',#92472,#26756,#26757);
#21930=AXIS2_PLACEMENT_3D('',#92476,#26760,#26761);
#21931=AXIS2_PLACEMENT_3D('',#92478,#26762,#26763);
#21932=AXIS2_PLACEMENT_3D('',#92480,#26764,#26765);
#21933=AXIS2_PLACEMENT_3D('',#92481,#26766,#26767);
#21934=AXIS2_PLACEMENT_3D('',#92482,#26768,#26769);
#21935=AXIS2_PLACEMENT_3D('',#92484,#26771,#26772);
#21936=AXIS2_PLACEMENT_3D('',#92486,#26774,#26775);
#21937=AXIS2_PLACEMENT_3D('',#92488,#26777,#26778);
#21938=AXIS2_PLACEMENT_3D('',#92490,#26780,#26781);
#21939=AXIS2_PLACEMENT_3D('',#92492,#26783,#26784);
#21940=AXIS2_PLACEMENT_3D('',#92494,#26786,#26787);
#21941=AXIS2_PLACEMENT_3D('',#92496,#26789,#26790);
#21942=AXIS2_PLACEMENT_3D('',#92498,#26792,#26793);
#21943=AXIS2_PLACEMENT_3D('',#92500,#26794,#26795);
#21944=AXIS2_PLACEMENT_3D('',#92502,#26796,#26797);
#21945=AXIS2_PLACEMENT_3D('',#92503,#26798,#26799);
#21946=AXIS2_PLACEMENT_3D('',#92504,#26800,#26801);
#21947=AXIS2_PLACEMENT_3D('',#92507,#26803,#26804);
#21948=AXIS2_PLACEMENT_3D('',#92508,#26805,#26806);
#21949=AXIS2_PLACEMENT_3D('',#92510,#26807,#26808);
#21950=AXIS2_PLACEMENT_3D('',#92512,#26809,#26810);
#21951=AXIS2_PLACEMENT_3D('',#92513,#26811,#26812);
#21952=AXIS2_PLACEMENT_3D('',#92514,#26813,#26814);
#21953=AXIS2_PLACEMENT_3D('',#92517,#26816,#26817);
#21954=AXIS2_PLACEMENT_3D('',#92518,#26818,#26819);
#21955=AXIS2_PLACEMENT_3D('',#92521,#26821,#26822);
#21956=AXIS2_PLACEMENT_3D('',#92522,#26823,#26824);
#21957=AXIS2_PLACEMENT_3D('',#92524,#26825,#26826);
#21958=AXIS2_PLACEMENT_3D('',#92525,#26827,#26828);
#21959=AXIS2_PLACEMENT_3D('',#92526,#26829,#26830);
#21960=AXIS2_PLACEMENT_3D('',#92529,#26831,#26832);
#21961=AXIS2_PLACEMENT_3D('',#92530,#26833,#26834);
#21962=AXIS2_PLACEMENT_3D('',#92532,#26835,#26836);
#21963=AXIS2_PLACEMENT_3D('',#92547,#26837,#26838);
#21964=AXIS2_PLACEMENT_3D('',#92550,#26840,#26841);
#21965=AXIS2_PLACEMENT_3D('',#92552,#26843,#26844);
#21966=AXIS2_PLACEMENT_3D('',#92554,#26845,#26846);
#21967=AXIS2_PLACEMENT_3D('',#92555,#26847,#26848);
#21968=AXIS2_PLACEMENT_3D('',#92556,#26849,#26850);
#21969=AXIS2_PLACEMENT_3D('',#92562,#26855,#26856);
#21970=AXIS2_PLACEMENT_3D('',#92563,#26857,#26858);
#21971=AXIS2_PLACEMENT_3D('',#92564,#26859,#26860);
#21972=AXIS2_PLACEMENT_3D('',#92565,#26861,#26862);
#21973=AXIS2_PLACEMENT_3D('',#92566,#26863,#26864);
#21974=AXIS2_PLACEMENT_3D('',#92567,#26865,#26866);
#21975=AXIS2_PLACEMENT_3D('',#92568,#26867,#26868);
#21976=AXIS2_PLACEMENT_3D('',#92569,#26869,#26870);
#21977=AXIS2_PLACEMENT_3D('',#92570,#26871,#26872);
#21978=AXIS2_PLACEMENT_3D('',#92571,#26873,#26874);
#21979=AXIS2_PLACEMENT_3D('',#92572,#26875,#26876);
#21980=AXIS2_PLACEMENT_3D('',#92574,#26877,#26878);
#21981=AXIS2_PLACEMENT_3D('',#92577,#26880,#26881);
#21982=AXIS2_PLACEMENT_3D('',#92578,#26882,#26883);
#21983=AXIS2_PLACEMENT_3D('',#92579,#26884,#26885);
#21984=AXIS2_PLACEMENT_3D('',#92580,#26886,#26887);
#21985=AXIS2_PLACEMENT_3D('',#92581,#26888,#26889);
#21986=AXIS2_PLACEMENT_3D('',#92582,#26890,#26891);
#21987=AXIS2_PLACEMENT_3D('',#92594,#26897,#26898);
#21988=AXIS2_PLACEMENT_3D('',#92602,#26903,#26904);
#21989=AXIS2_PLACEMENT_3D('',#92603,#26905,#26906);
#21990=AXIS2_PLACEMENT_3D('',#92604,#26907,#26908);
#21991=AXIS2_PLACEMENT_3D('',#92607,#26909,#26910);
#21992=AXIS2_PLACEMENT_3D('',#92610,#26913,#26914);
#21993=AXIS2_PLACEMENT_3D('',#92611,#26915,#26916);
#21994=AXIS2_PLACEMENT_3D('',#92614,#26918,#26919);
#21995=AXIS2_PLACEMENT_3D('',#92615,#26920,#26921);
#21996=AXIS2_PLACEMENT_3D('',#92616,#26922,#26923);
#21997=AXIS2_PLACEMENT_3D('',#92618,#26925,#26926);
#21998=AXIS2_PLACEMENT_3D('',#92619,#26927,#26928);
#21999=AXIS2_PLACEMENT_3D('',#92620,#26929,#26930);
#22000=AXIS2_PLACEMENT_3D('',#92621,#26931,#26932);
#22001=AXIS2_PLACEMENT_3D('',#92622,#26933,#26934);
#22002=AXIS2_PLACEMENT_3D('',#92628,#26938,#26939);
#22003=AXIS2_PLACEMENT_3D('',#92629,#26940,#26941);
#22004=AXIS2_PLACEMENT_3D('',#92630,#26942,#26943);
#22005=AXIS2_PLACEMENT_3D('',#92631,#26944,#26945);
#22006=AXIS2_PLACEMENT_3D('',#92632,#26946,#26947);
#22007=AXIS2_PLACEMENT_3D('',#92633,#26948,#26949);
#22008=AXIS2_PLACEMENT_3D('',#92634,#26950,#26951);
#22009=AXIS2_PLACEMENT_3D('',#92635,#26952,#26953);
#22010=AXIS2_PLACEMENT_3D('',#92637,#26954,#26955);
#22011=AXIS2_PLACEMENT_3D('',#92639,#26956,#26957);
#22012=AXIS2_PLACEMENT_3D('',#92641,#26958,#26959);
#22013=AXIS2_PLACEMENT_3D('',#92642,#26960,#26961);
#22014=AXIS2_PLACEMENT_3D('',#92643,#26962,#26963);
#22015=AXIS2_PLACEMENT_3D('',#92654,#26965,#26966);
#22016=AXIS2_PLACEMENT_3D('',#92658,#26968,#26969);
#22017=AXIS2_PLACEMENT_3D('',#92662,#26971,#26972);
#22018=AXIS2_PLACEMENT_3D('',#92716,#26974,#26975);
#22019=AXIS2_PLACEMENT_3D('',#92746,#26978,#26979);
#22020=AXIS2_PLACEMENT_3D('',#92759,#26981,#26982);
#22021=AXIS2_PLACEMENT_3D('',#92761,#26984,#26985);
#22022=AXIS2_PLACEMENT_3D('',#92763,#26986,#26987);
#22023=AXIS2_PLACEMENT_3D('',#92764,#26988,#26989);
#22024=AXIS2_PLACEMENT_3D('',#92765,#26990,#26991);
#22025=AXIS2_PLACEMENT_3D('',#92766,#26992,#26993);
#22026=AXIS2_PLACEMENT_3D('',#92769,#26994,#26995);
#22027=AXIS2_PLACEMENT_3D('',#92773,#26998,#26999);
#22028=AXIS2_PLACEMENT_3D('',#92774,#27000,#27001);
#22029=AXIS2_PLACEMENT_3D('',#92778,#27004,#27005);
#22030=AXIS2_PLACEMENT_3D('',#92781,#27007,#27008);
#22031=AXIS2_PLACEMENT_3D('',#92785,#27011,#27012);
#22032=AXIS2_PLACEMENT_3D('',#92794,#27017,#27018);
#22033=AXIS2_PLACEMENT_3D('',#92797,#27019,#27020);
#22034=AXIS2_PLACEMENT_3D('',#92801,#27022,#27023);
#22035=AXIS2_PLACEMENT_3D('',#92803,#27024,#27025);
#22036=AXIS2_PLACEMENT_3D('',#92806,#27027,#27028);
#22037=AXIS2_PLACEMENT_3D('',#92807,#27029,#27030);
#22038=AXIS2_PLACEMENT_3D('',#92809,#27031,#27032);
#22039=AXIS2_PLACEMENT_3D('',#92812,#27034,#27035);
#22040=AXIS2_PLACEMENT_3D('',#92813,#27036,#27037);
#22041=AXIS2_PLACEMENT_3D('',#92815,#27038,#27039);
#22042=AXIS2_PLACEMENT_3D('',#92817,#27040,#27041);
#22043=AXIS2_PLACEMENT_3D('',#92821,#27043,#27044);
#22044=AXIS2_PLACEMENT_3D('',#92825,#27046,#27047);
#22045=AXIS2_PLACEMENT_3D('',#92827,#27049,#27050);
#22046=AXIS2_PLACEMENT_3D('',#92831,#27053,#27054);
#22047=AXIS2_PLACEMENT_3D('',#92840,#27059,#27060);
#22048=AXIS2_PLACEMENT_3D('',#92846,#27063,#27064);
#22049=AXIS2_PLACEMENT_3D('',#92847,#27065,#27066);
#22050=AXIS2_PLACEMENT_3D('',#92848,#27067,#27068);
#22051=AXIS2_PLACEMENT_3D('',#92851,#27069,#27070);
#22052=AXIS2_PLACEMENT_3D('',#92853,#27071,#27072);
#22053=AXIS2_PLACEMENT_3D('',#92875,#27075,#27076);
#22054=AXIS2_PLACEMENT_3D('',#92877,#27078,#27079);
#22055=AXIS2_PLACEMENT_3D('',#92878,#27080,#27081);
#22056=AXIS2_PLACEMENT_3D('',#92880,#27082,#27083);
#22057=AXIS2_PLACEMENT_3D('',#92884,#27086,#27087);
#22058=AXIS2_PLACEMENT_3D('',#92885,#27088,#27089);
#22059=AXIS2_PLACEMENT_3D('',#92888,#27091,#27092);
#22060=AXIS2_PLACEMENT_3D('',#92890,#27094,#27095);
#22061=AXIS2_PLACEMENT_3D('',#92892,#27097,#27098);
#22062=AXIS2_PLACEMENT_3D('',#92894,#27099,#27100);
#22063=AXIS2_PLACEMENT_3D('',#92901,#27104,#27105);
#22064=AXIS2_PLACEMENT_3D('',#92902,#27106,#27107);
#22065=AXIS2_PLACEMENT_3D('',#92904,#27108,#27109);
#22066=AXIS2_PLACEMENT_3D('',#92906,#27111,#27112);
#22067=AXIS2_PLACEMENT_3D('',#92908,#27113,#27114);
#22068=AXIS2_PLACEMENT_3D('',#92916,#27118,#27119);
#22069=AXIS2_PLACEMENT_3D('',#92917,#27120,#27121);
#22070=AXIS2_PLACEMENT_3D('',#92918,#27122,#27123);
#22071=AXIS2_PLACEMENT_3D('',#92920,#27125,#27126);
#22072=AXIS2_PLACEMENT_3D('',#92921,#27127,#27128);
#22073=AXIS2_PLACEMENT_3D('',#92922,#27129,#27130);
#22074=AXIS2_PLACEMENT_3D('',#92923,#27131,#27132);
#22075=AXIS2_PLACEMENT_3D('',#92924,#27133,#27134);
#22076=AXIS2_PLACEMENT_3D('',#92925,#27135,#27136);
#22077=AXIS2_PLACEMENT_3D('',#92926,#27137,#27138);
#22078=AXIS2_PLACEMENT_3D('',#92927,#27139,#27140);
#22079=AXIS2_PLACEMENT_3D('',#92928,#27141,#27142);
#22080=AXIS2_PLACEMENT_3D('',#92929,#27143,#27144);
#22081=AXIS2_PLACEMENT_3D('',#92930,#27145,#27146);
#22082=AXIS2_PLACEMENT_3D('',#92931,#27147,#27148);
#22083=AXIS2_PLACEMENT_3D('',#92956,#27150,#27151);
#22084=AXIS2_PLACEMENT_3D('',#92958,#27153,#27154);
#22085=AXIS2_PLACEMENT_3D('',#92959,#27155,#27156);
#22086=AXIS2_PLACEMENT_3D('',#92960,#27157,#27158);
#22087=AXIS2_PLACEMENT_3D('',#92961,#27159,#27160);
#22088=AXIS2_PLACEMENT_3D('',#92974,#27161,#27162);
#22089=AXIS2_PLACEMENT_3D('',#92985,#27163,#27164);
#22090=AXIS2_PLACEMENT_3D('',#92990,#27168,#27169);
#22091=AXIS2_PLACEMENT_3D('',#92992,#27171,#27172);
#22092=AXIS2_PLACEMENT_3D('',#92993,#27173,#27174);
#22093=AXIS2_PLACEMENT_3D('',#93003,#27175,#27176);
#22094=AXIS2_PLACEMENT_3D('',#93004,#27177,#27178);
#22095=AXIS2_PLACEMENT_3D('',#93006,#27180,#27181);
#22096=AXIS2_PLACEMENT_3D('',#93008,#27182,#27183);
#22097=AXIS2_PLACEMENT_3D('',#93025,#27187,#27188);
#22098=AXIS2_PLACEMENT_3D('',#93027,#27190,#27191);
#22099=AXIS2_PLACEMENT_3D('',#93033,#27195,#27196);
#22100=AXIS2_PLACEMENT_3D('',#93035,#27198,#27199);
#22101=AXIS2_PLACEMENT_3D('',#93037,#27201,#27202);
#22102=AXIS2_PLACEMENT_3D('',#93039,#27204,#27205);
#22103=AXIS2_PLACEMENT_3D('',#93045,#27209,#27210);
#22104=AXIS2_PLACEMENT_3D('',#93047,#27212,#27213);
#22105=AXIS2_PLACEMENT_3D('',#93049,#27214,#27215);
#22106=AXIS2_PLACEMENT_3D('',#93051,#27216,#27217);
#22107=AXIS2_PLACEMENT_3D('',#93052,#27218,#27219);
#22108=AXIS2_PLACEMENT_3D('',#93053,#27220,#27221);
#22109=AXIS2_PLACEMENT_3D('',#93057,#27223,#27224);
#22110=AXIS2_PLACEMENT_3D('',#93102,#27226,#27227);
#22111=AXIS2_PLACEMENT_3D('',#93103,#27228,#27229);
#22112=AXIS2_PLACEMENT_3D('',#93114,#27231,#27232);
#22113=AXIS2_PLACEMENT_3D('',#93116,#27233,#27234);
#22114=AXIS2_PLACEMENT_3D('',#93127,#27235,#27236);
#22115=AXIS2_PLACEMENT_3D('',#93129,#27238,#27239);
#22116=AXIS2_PLACEMENT_3D('',#93130,#27240,#27241);
#22117=AXIS2_PLACEMENT_3D('',#93132,#27243,#27244);
#22118=AXIS2_PLACEMENT_3D('',#93133,#27245,#27246);
#22119=AXIS2_PLACEMENT_3D('',#93137,#27249,#27250);
#22120=AXIS2_PLACEMENT_3D('',#93139,#27252,#27253);
#22121=AXIS2_PLACEMENT_3D('',#93140,#27254,#27255);
#22122=AXIS2_PLACEMENT_3D('',#93142,#27257,#27258);
#22123=AXIS2_PLACEMENT_3D('',#93143,#27259,#27260);
#22124=AXIS2_PLACEMENT_3D('',#93147,#27263,#27264);
#22125=AXIS2_PLACEMENT_3D('',#93149,#27266,#27267);
#22126=AXIS2_PLACEMENT_3D('',#93150,#27268,#27269);
#22127=AXIS2_PLACEMENT_3D('',#93152,#27271,#27272);
#22128=AXIS2_PLACEMENT_3D('',#93153,#27273,#27274);
#22129=AXIS2_PLACEMENT_3D('',#93157,#27277,#27278);
#22130=AXIS2_PLACEMENT_3D('',#93159,#27280,#27281);
#22131=AXIS2_PLACEMENT_3D('',#93160,#27282,#27283);
#22132=AXIS2_PLACEMENT_3D('',#93164,#27286,#27287);
#22133=AXIS2_PLACEMENT_3D('',#93166,#27289,#27290);
#22134=AXIS2_PLACEMENT_3D('',#93168,#27292,#27293);
#22135=AXIS2_PLACEMENT_3D('',#93169,#27294,#27295);
#22136=AXIS2_PLACEMENT_3D('',#93170,#27296,#27297);
#22137=AXIS2_PLACEMENT_3D('',#93171,#27298,#27299);
#22138=AXIS2_PLACEMENT_3D('',#93172,#27300,#27301);
#22139=AXIS2_PLACEMENT_3D('',#93173,#27302,#27303);
#22140=AXIS2_PLACEMENT_3D('',#93174,#27304,#27305);
#22141=AXIS2_PLACEMENT_3D('',#93177,#27308,#27309);
#22142=AXIS2_PLACEMENT_3D('',#93180,#27312,#27313);
#22143=AXIS2_PLACEMENT_3D('',#93181,#27314,#27315);
#22144=AXIS2_PLACEMENT_3D('',#93182,#27316,#27317);
#22145=AXIS2_PLACEMENT_3D('',#93183,#27318,#27319);
#22146=AXIS2_PLACEMENT_3D('',#93184,#27320,#27321);
#22147=AXIS2_PLACEMENT_3D('',#93185,#27322,#27323);
#22148=AXIS2_PLACEMENT_3D('',#93186,#27324,#27325);
#22149=AXIS2_PLACEMENT_3D('',#93187,#27326,#27327);
#22150=AXIS2_PLACEMENT_3D('',#93188,#27328,#27329);
#22151=AXIS2_PLACEMENT_3D('',#93189,#27330,#27331);
#22152=AXIS2_PLACEMENT_3D('',#93190,#27332,#27333);
#22153=AXIS2_PLACEMENT_3D('',#93191,#27334,#27335);
#22154=AXIS2_PLACEMENT_3D('',#93227,#27337,#27338);
#22155=AXIS2_PLACEMENT_3D('',#93285,#27339,#27340);
#22156=AXIS2_PLACEMENT_3D('',#93321,#27342,#27343);
#22157=AXIS2_PLACEMENT_3D('',#97670,#27344,#27345);
#22158=AXIS2_PLACEMENT_3D('',#97671,#27346,#27347);
#22159=AXIS2_PLACEMENT_3D('',#97673,#27348,#27349);
#22160=AXIS2_PLACEMENT_3D('',#97675,#27350,#27351);
#22161=AXIS2_PLACEMENT_3D('',#97677,#27352,#27353);
#22162=AXIS2_PLACEMENT_3D('',#97678,#27354,#27355);
#22163=AXIS2_PLACEMENT_3D('',#97679,#27356,#27357);
#22164=AXIS2_PLACEMENT_3D('',#97683,#27359,#27360);
#22165=AXIS2_PLACEMENT_3D('',#97684,#27361,#27362);
#22166=AXIS2_PLACEMENT_3D('',#97685,#27363,#27364);
#22167=AXIS2_PLACEMENT_3D('',#97687,#27365,#27366);
#22168=AXIS2_PLACEMENT_3D('',#97688,#27367,#27368);
#22169=AXIS2_PLACEMENT_3D('',#97690,#27369,#27370);
#22170=AXIS2_PLACEMENT_3D('',#97691,#27371,#27372);
#22171=AXIS2_PLACEMENT_3D('',#97692,#27373,#27374);
#22172=AXIS2_PLACEMENT_3D('',#97694,#27375,#27376);
#22173=AXIS2_PLACEMENT_3D('',#97695,#27377,#27378);
#22174=AXIS2_PLACEMENT_3D('',#97698,#27379,#27380);
#22175=AXIS2_PLACEMENT_3D('',#97700,#27381,#27382);
#22176=AXIS2_PLACEMENT_3D('',#97701,#27383,#27384);
#22177=AXIS2_PLACEMENT_3D('',#97702,#27385,#27386);
#22178=AXIS2_PLACEMENT_3D('',#97703,#27387,#27388);
#22179=AXIS2_PLACEMENT_3D('',#97705,#27389,#27390);
#22180=AXIS2_PLACEMENT_3D('',#97706,#27391,#27392);
#22181=AXIS2_PLACEMENT_3D('',#97708,#27394,#27395);
#22182=AXIS2_PLACEMENT_3D('',#97710,#27396,#27397);
#22183=AXIS2_PLACEMENT_3D('',#97712,#27398,#27399);
#22184=AXIS2_PLACEMENT_3D('',#97713,#27400,#27401);
#22185=AXIS2_PLACEMENT_3D('',#97714,#27402,#27403);
#22186=AXIS2_PLACEMENT_3D('',#97717,#27405,#27406);
#22187=AXIS2_PLACEMENT_3D('',#97720,#27407,#27408);
#22188=AXIS2_PLACEMENT_3D('',#97724,#27410,#27411);
#22189=AXIS2_PLACEMENT_3D('',#97726,#27413,#27414);
#22190=AXIS2_PLACEMENT_3D('',#97728,#27415,#27416);
#22191=AXIS2_PLACEMENT_3D('',#97730,#27417,#27418);
#22192=AXIS2_PLACEMENT_3D('',#97732,#27419,#27420);
#22193=AXIS2_PLACEMENT_3D('',#97733,#27421,#27422);
#22194=AXIS2_PLACEMENT_3D('',#97734,#27423,#27424);
#22195=AXIS2_PLACEMENT_3D('',#97738,#27426,#27427);
#22196=AXIS2_PLACEMENT_3D('',#97739,#27428,#27429);
#22197=AXIS2_PLACEMENT_3D('',#97740,#27430,#27431);
#22198=AXIS2_PLACEMENT_3D('',#97741,#27432,#27433);
#22199=AXIS2_PLACEMENT_3D('',#97742,#27434,#27435);
#22200=AXIS2_PLACEMENT_3D('',#97743,#27436,#27437);
#22201=AXIS2_PLACEMENT_3D('',#97748,#27439,#27440);
#22202=AXIS2_PLACEMENT_3D('',#97751,#27442,#27443);
#22203=AXIS2_PLACEMENT_3D('',#97752,#27444,#27445);
#22204=AXIS2_PLACEMENT_3D('',#97757,#27448,#27449);
#22205=AXIS2_PLACEMENT_3D('',#97758,#27450,#27451);
#22206=AXIS2_PLACEMENT_3D('',#97763,#27454,#27455);
#22207=AXIS2_PLACEMENT_3D('',#97764,#27456,#27457);
#22208=AXIS2_PLACEMENT_3D('',#97767,#27460,#27461);
#22209=AXIS2_PLACEMENT_3D('',#97770,#27464,#27465);
#22210=AXIS2_PLACEMENT_3D('',#97772,#27467,#27468);
#22211=AXIS2_PLACEMENT_3D('',#97781,#27473,#27474);
#22212=AXIS2_PLACEMENT_3D('',#97787,#27478,#27479);
#22213=AXIS2_PLACEMENT_3D('',#97791,#27482,#27483);
#22214=AXIS2_PLACEMENT_3D('',#97795,#27486,#27487);
#22215=AXIS2_PLACEMENT_3D('',#97797,#27489,#27490);
#22216=AXIS2_PLACEMENT_3D('',#97798,#27491,#27492);
#22217=AXIS2_PLACEMENT_3D('',#97800,#27494,#27495);
#22218=AXIS2_PLACEMENT_3D('',#97801,#27496,#27497);
#22219=AXIS2_PLACEMENT_3D('',#97802,#27498,#27499);
#22220=AXIS2_PLACEMENT_3D('',#97805,#27500,#27501);
#22221=AXIS2_PLACEMENT_3D('',#97809,#27503,#27504);
#22222=AXIS2_PLACEMENT_3D('',#97811,#27506,#27507);
#22223=AXIS2_PLACEMENT_3D('',#97814,#27508,#27509);
#22224=AXIS2_PLACEMENT_3D('',#97817,#27511,#27512);
#22225=AXIS2_PLACEMENT_3D('',#97819,#27514,#27515);
#22226=AXIS2_PLACEMENT_3D('',#97821,#27516,#27517);
#22227=AXIS2_PLACEMENT_3D('',#97825,#27519,#27520);
#22228=AXIS2_PLACEMENT_3D('',#97827,#27522,#27523);
#22229=AXIS2_PLACEMENT_3D('',#97829,#27524,#27525);
#22230=AXIS2_PLACEMENT_3D('',#97832,#27527,#27528);
#22231=AXIS2_PLACEMENT_3D('',#97834,#27530,#27531);
#22232=AXIS2_PLACEMENT_3D('',#97835,#27532,#27533);
#22233=AXIS2_PLACEMENT_3D('',#97836,#27534,#27535);
#22234=AXIS2_PLACEMENT_3D('',#97837,#27536,#27537);
#22235=AXIS2_PLACEMENT_3D('',#97838,#27538,#27539);
#22236=AXIS2_PLACEMENT_3D('',#97839,#27540,#27541);
#22237=AXIS2_PLACEMENT_3D('',#97840,#27542,#27543);
#22238=AXIS2_PLACEMENT_3D('',#97841,#27544,#27545);
#22239=AXIS2_PLACEMENT_3D('',#97842,#27546,#27547);
#22240=AXIS2_PLACEMENT_3D('',#97846,#27549,#27550);
#22241=AXIS2_PLACEMENT_3D('',#97848,#27552,#27553);
#22242=AXIS2_PLACEMENT_3D('',#97852,#27556,#27557);
#22243=AXIS2_PLACEMENT_3D('',#97855,#27559,#27560);
#22244=AXIS2_PLACEMENT_3D('',#97856,#27561,#27562);
#22245=AXIS2_PLACEMENT_3D('',#97917,#27565,#27566);
#22246=AXIS2_PLACEMENT_3D('',#97919,#27567,#27568);
#22247=AXIS2_PLACEMENT_3D('',#97920,#27569,#27570);
#22248=AXIS2_PLACEMENT_3D('',#97921,#27571,#27572);
#22249=AXIS2_PLACEMENT_3D('',#97924,#27574,#27575);
#22250=AXIS2_PLACEMENT_3D('',#97925,#27576,#27577);
#22251=AXIS2_PLACEMENT_3D('',#97927,#27578,#27579);
#22252=AXIS2_PLACEMENT_3D('',#97931,#27581,#27582);
#22253=AXIS2_PLACEMENT_3D('',#97933,#27584,#27585);
#22254=AXIS2_PLACEMENT_3D('',#97934,#27586,#27587);
#22255=AXIS2_PLACEMENT_3D('',#97935,#27588,#27589);
#22256=AXIS2_PLACEMENT_3D('',#97938,#27591,#27592);
#22257=AXIS2_PLACEMENT_3D('',#97940,#27594,#27595);
#22258=AXIS2_PLACEMENT_3D('',#97941,#27596,#27597);
#22259=AXIS2_PLACEMENT_3D('',#98111,#27598,#27599);
#22260=AXIS2_PLACEMENT_3D('',#98311,#27600,#27601);
#22261=AXIS2_PLACEMENT_3D('',#98514,#27603,#27604);
#22262=AXIS2_PLACEMENT_3D('',#98515,#27605,#27606);
#22263=AXIS2_PLACEMENT_3D('',#98548,#27608,#27609);
#22264=AXIS2_PLACEMENT_3D('',#98550,#27610,#27611);
#22265=AXIS2_PLACEMENT_3D('',#98551,#27612,#27613);
#22266=AXIS2_PLACEMENT_3D('',#98553,#27614,#27615);
#22267=AXIS2_PLACEMENT_3D('',#98556,#27617,#27618);
#22268=AXIS2_PLACEMENT_3D('',#98557,#27619,#27620);
#22269=AXIS2_PLACEMENT_3D('',#98558,#27621,#27622);
#22270=AXIS2_PLACEMENT_3D('',#98559,#27623,#27624);
#22271=AXIS2_PLACEMENT_3D('',#98560,#27625,#27626);
#22272=AXIS2_PLACEMENT_3D('',#98736,#27627,#27628);
#22273=AXIS2_PLACEMENT_3D('',#98954,#27630,#27631);
#22274=AXIS2_PLACEMENT_3D('',#99114,#27632,#27633);
#22275=AXIS2_PLACEMENT_3D('',#99140,#27634,#27635);
#22276=AXIS2_PLACEMENT_3D('',#99162,#27636,#27637);
#22277=AXIS2_PLACEMENT_3D('',#99192,#27638,#27639);
#22278=AXIS2_PLACEMENT_3D('',#99246,#27640,#27641);
#22279=AXIS2_PLACEMENT_3D('',#99250,#27643,#27644);
#22280=AXIS2_PLACEMENT_3D('',#99252,#27646,#27647);
#22281=AXIS2_PLACEMENT_3D('',#99255,#27648,#27649);
#22282=AXIS2_PLACEMENT_3D('',#99256,#27650,#27651);
#22283=AXIS2_PLACEMENT_3D('',#99257,#27652,#27653);
#22284=AXIS2_PLACEMENT_3D('',#99258,#27654,#27655);
#22285=AXIS2_PLACEMENT_3D('',#99299,#27658,#27659);
#22286=AXIS2_PLACEMENT_3D('',#99305,#27660,#27661);
#22287=AXIS2_PLACEMENT_3D('',#99363,#27662,#27663);
#22288=AXIS2_PLACEMENT_3D('',#99392,#27664,#27665);
#22289=AXIS2_PLACEMENT_3D('',#99398,#27668,#27669);
#22290=AXIS2_PLACEMENT_3D('',#99402,#27671,#27672);
#22291=AXIS2_PLACEMENT_3D('',#99424,#27673,#27674);
#22292=AXIS2_PLACEMENT_3D('',#99427,#27676,#27677);
#22293=AXIS2_PLACEMENT_3D('',#99428,#27678,#27679);
#22294=AXIS2_PLACEMENT_3D('',#99450,#27680,#27681);
#22295=AXIS2_PLACEMENT_3D('',#99454,#27683,#27684);
#22296=AXIS2_PLACEMENT_3D('',#99456,#27686,#27687);
#22297=AXIS2_PLACEMENT_3D('',#99477,#27688,#27689);
#22298=AXIS2_PLACEMENT_3D('',#99479,#27690,#27691);
#22299=AXIS2_PLACEMENT_3D('',#99504,#27692,#27693);
#22300=AXIS2_PLACEMENT_3D('',#99545,#27694,#27695);
#22301=AXIS2_PLACEMENT_3D('',#99576,#27697,#27698);
#22302=AXIS2_PLACEMENT_3D('',#99577,#27699,#27700);
#22303=AXIS2_PLACEMENT_3D('',#99618,#27701,#27702);
#22304=AXIS2_PLACEMENT_3D('',#99635,#27703,#27704);
#22305=AXIS2_PLACEMENT_3D('',#99638,#27707,#27708);
#22306=AXIS2_PLACEMENT_3D('',#99640,#27709,#27710);
#22307=AXIS2_PLACEMENT_3D('',#99642,#27711,#27712);
#22308=AXIS2_PLACEMENT_3D('',#99643,#27713,#27714);
#22309=AXIS2_PLACEMENT_3D('',#99645,#27715,#27716);
#22310=AXIS2_PLACEMENT_3D('',#99647,#27717,#27718);
#22311=AXIS2_PLACEMENT_3D('',#99648,#27719,#27720);
#22312=AXIS2_PLACEMENT_3D('',#99649,#27721,#27722);
#22313=AXIS2_PLACEMENT_3D('',#99653,#27724,#27725);
#22314=AXIS2_PLACEMENT_3D('',#99654,#27726,#27727);
#22315=AXIS2_PLACEMENT_3D('',#99655,#27728,#27729);
#22316=AXIS2_PLACEMENT_3D('',#99656,#27730,#27731);
#22317=AXIS2_PLACEMENT_3D('',#99657,#27732,#27733);
#22318=AXIS2_PLACEMENT_3D('',#99659,#27734,#27735);
#22319=AXIS2_PLACEMENT_3D('',#99661,#27736,#27737);
#22320=AXIS2_PLACEMENT_3D('',#99662,#27738,#27739);
#22321=AXIS2_PLACEMENT_3D('',#99663,#27740,#27741);
#22322=AXIS2_PLACEMENT_3D('',#99667,#27743,#27744);
#22323=AXIS2_PLACEMENT_3D('',#99668,#27745,#27746);
#22324=AXIS2_PLACEMENT_3D('',#99669,#27747,#27748);
#22325=AXIS2_PLACEMENT_3D('',#99671,#27749,#27750);
#22326=AXIS2_PLACEMENT_3D('',#99672,#27751,#27752);
#22327=AXIS2_PLACEMENT_3D('',#99673,#27753,#27754);
#22328=AXIS2_PLACEMENT_3D('',#99676,#27756,#27757);
#22329=AXIS2_PLACEMENT_3D('',#99677,#27758,#27759);
#22330=AXIS2_PLACEMENT_3D('',#99679,#27760,#27761);
#22331=AXIS2_PLACEMENT_3D('',#99681,#27762,#27763);
#22332=AXIS2_PLACEMENT_3D('',#99682,#27764,#27765);
#22333=AXIS2_PLACEMENT_3D('',#99683,#27766,#27767);
#22334=AXIS2_PLACEMENT_3D('',#99687,#27769,#27770);
#22335=AXIS2_PLACEMENT_3D('',#99688,#27771,#27772);
#22336=AXIS2_PLACEMENT_3D('',#99689,#27773,#27774);
#22337=AXIS2_PLACEMENT_3D('',#99690,#27775,#27776);
#22338=AXIS2_PLACEMENT_3D('',#99691,#27777,#27778);
#22339=AXIS2_PLACEMENT_3D('',#99693,#27779,#27780);
#22340=AXIS2_PLACEMENT_3D('',#99695,#27781,#27782);
#22341=AXIS2_PLACEMENT_3D('',#99696,#27783,#27784);
#22342=AXIS2_PLACEMENT_3D('',#99697,#27785,#27786);
#22343=AXIS2_PLACEMENT_3D('',#99701,#27788,#27789);
#22344=AXIS2_PLACEMENT_3D('',#99702,#27790,#27791);
#22345=AXIS2_PLACEMENT_3D('',#99703,#27792,#27793);
#22346=AXIS2_PLACEMENT_3D('',#99704,#27794,#27795);
#22347=AXIS2_PLACEMENT_3D('',#99705,#27796,#27797);
#22348=AXIS2_PLACEMENT_3D('',#99706,#27798,#27799);
#22349=AXIS2_PLACEMENT_3D('',#99708,#27801,#27802);
#22350=AXIS2_PLACEMENT_3D('',#99710,#27804,#27805);
#22351=AXIS2_PLACEMENT_3D('',#99711,#27806,#27807);
#22352=AXIS2_PLACEMENT_3D('',#99712,#27808,#27809);
#22353=AXIS2_PLACEMENT_3D('',#99714,#27810,#27811);
#22354=AXIS2_PLACEMENT_3D('',#99716,#27812,#27813);
#22355=AXIS2_PLACEMENT_3D('',#99717,#27814,#27815);
#22356=AXIS2_PLACEMENT_3D('',#99719,#27816,#27817);
#22357=AXIS2_PLACEMENT_3D('',#99721,#27819,#27820);
#22358=AXIS2_PLACEMENT_3D('',#99723,#27821,#27822);
#22359=AXIS2_PLACEMENT_3D('',#99726,#27824,#27825);
#22360=AXIS2_PLACEMENT_3D('',#99727,#27826,#27827);
#22361=AXIS2_PLACEMENT_3D('',#99729,#27828,#27829);
#22362=AXIS2_PLACEMENT_3D('',#99730,#27830,#27831);
#22363=AXIS2_PLACEMENT_3D('',#99733,#27833,#27834);
#22364=AXIS2_PLACEMENT_3D('',#99734,#27835,#27836);
#22365=AXIS2_PLACEMENT_3D('',#99735,#27837,#27838);
#22366=AXIS2_PLACEMENT_3D('',#99737,#27839,#27840);
#22367=AXIS2_PLACEMENT_3D('',#99740,#27842,#27843);
#22368=AXIS2_PLACEMENT_3D('',#99741,#27844,#27845);
#22369=AXIS2_PLACEMENT_3D('',#99743,#27846,#27847);
#22370=AXIS2_PLACEMENT_3D('',#99744,#27848,#27849);
#22371=AXIS2_PLACEMENT_3D('',#99746,#27850,#27851);
#22372=AXIS2_PLACEMENT_3D('',#99749,#27853,#27854);
#22373=AXIS2_PLACEMENT_3D('',#99750,#27855,#27856);
#22374=AXIS2_PLACEMENT_3D('',#99752,#27857,#27858);
#22375=AXIS2_PLACEMENT_3D('',#99753,#27859,#27860);
#22376=AXIS2_PLACEMENT_3D('',#99756,#27862,#27863);
#22377=AXIS2_PLACEMENT_3D('',#99757,#27864,#27865);
#22378=AXIS2_PLACEMENT_3D('',#99759,#27866,#27867);
#22379=AXIS2_PLACEMENT_3D('',#99760,#27868,#27869);
#22380=AXIS2_PLACEMENT_3D('',#99762,#27870,#27871);
#22381=AXIS2_PLACEMENT_3D('',#99764,#27872,#27873);
#22382=AXIS2_PLACEMENT_3D('',#99765,#27874,#27875);
#22383=AXIS2_PLACEMENT_3D('',#99768,#27877,#27878);
#22384=AXIS2_PLACEMENT_3D('',#99769,#27879,#27880);
#22385=AXIS2_PLACEMENT_3D('',#99771,#27881,#27882);
#22386=AXIS2_PLACEMENT_3D('',#99772,#27883,#27884);
#22387=AXIS2_PLACEMENT_3D('',#99775,#27886,#27887);
#22388=AXIS2_PLACEMENT_3D('',#99776,#27888,#27889);
#22389=AXIS2_PLACEMENT_3D('',#99778,#27890,#27891);
#22390=AXIS2_PLACEMENT_3D('',#99779,#27892,#27893);
#22391=AXIS2_PLACEMENT_3D('',#99782,#27895,#27896);
#22392=AXIS2_PLACEMENT_3D('',#99783,#27897,#27898);
#22393=AXIS2_PLACEMENT_3D('',#99785,#27899,#27900);
#22394=AXIS2_PLACEMENT_3D('',#99786,#27901,#27902);
#22395=AXIS2_PLACEMENT_3D('',#99789,#27904,#27905);
#22396=AXIS2_PLACEMENT_3D('',#99790,#27906,#27907);
#22397=AXIS2_PLACEMENT_3D('',#99793,#27909,#27910);
#22398=AXIS2_PLACEMENT_3D('',#99794,#27911,#27912);
#22399=AXIS2_PLACEMENT_3D('',#99796,#27913,#27914);
#22400=AXIS2_PLACEMENT_3D('',#99798,#27916,#27917);
#22401=AXIS2_PLACEMENT_3D('',#99800,#27919,#27920);
#22402=AXIS2_PLACEMENT_3D('',#99801,#27921,#27922);
#22403=AXIS2_PLACEMENT_3D('',#99803,#27924,#27925);
#22404=AXIS2_PLACEMENT_3D('',#99804,#27926,#27927);
#22405=AXIS2_PLACEMENT_3D('',#99805,#27928,#27929);
#22406=AXIS2_PLACEMENT_3D('',#99807,#27930,#27931);
#22407=AXIS2_PLACEMENT_3D('',#99810,#27933,#27934);
#22408=AXIS2_PLACEMENT_3D('',#99811,#27935,#27936);
#22409=AXIS2_PLACEMENT_3D('',#99813,#27937,#27938);
#22410=AXIS2_PLACEMENT_3D('',#99815,#27940,#27941);
#22411=AXIS2_PLACEMENT_3D('',#99818,#27943,#27944);
#22412=AXIS2_PLACEMENT_3D('',#99819,#27945,#27946);
#22413=AXIS2_PLACEMENT_3D('',#99821,#27947,#27948);
#22414=AXIS2_PLACEMENT_3D('',#99822,#27949,#27950);
#22415=AXIS2_PLACEMENT_3D('',#99824,#27951,#27952);
#22416=AXIS2_PLACEMENT_3D('',#99826,#27954,#27955);
#22417=AXIS2_PLACEMENT_3D('',#99827,#27956,#27957);
#22418=AXIS2_PLACEMENT_3D('',#99828,#27958,#27959);
#22419=AXIS2_PLACEMENT_3D('',#99830,#27960,#27961);
#22420=AXIS2_PLACEMENT_3D('',#99833,#27963,#27964);
#22421=AXIS2_PLACEMENT_3D('',#99834,#27965,#27966);
#22422=AXIS2_PLACEMENT_3D('',#99836,#27967,#27968);
#22423=AXIS2_PLACEMENT_3D('',#99838,#27970,#27971);
#22424=AXIS2_PLACEMENT_3D('',#99841,#27973,#27974);
#22425=AXIS2_PLACEMENT_3D('',#99842,#27975,#27976);
#22426=AXIS2_PLACEMENT_3D('',#99843,#27977,#27978);
#22427=AXIS2_PLACEMENT_3D('',#99844,#27979,#27980);
#22428=AXIS2_PLACEMENT_3D('',#99845,#27981,#27982);
#22429=AXIS2_PLACEMENT_3D('',#99847,#27983,#27984);
#22430=AXIS2_PLACEMENT_3D('',#99850,#27986,#27987);
#22431=AXIS2_PLACEMENT_3D('',#99851,#27988,#27989);
#22432=AXIS2_PLACEMENT_3D('',#99853,#27990,#27991);
#22433=AXIS2_PLACEMENT_3D('',#99855,#27993,#27994);
#22434=AXIS2_PLACEMENT_3D('',#99858,#27996,#27997);
#22435=AXIS2_PLACEMENT_3D('',#99859,#27998,#27999);
#22436=AXIS2_PLACEMENT_3D('',#99860,#28000,#28001);
#22437=AXIS2_PLACEMENT_3D('',#99861,#28002,#28003);
#22438=AXIS2_PLACEMENT_3D('',#99862,#28004,#28005);
#22439=AXIS2_PLACEMENT_3D('',#99864,#28006,#28007);
#22440=AXIS2_PLACEMENT_3D('',#99865,#28008,#28009);
#22441=AXIS2_PLACEMENT_3D('',#99867,#28010,#28011);
#22442=AXIS2_PLACEMENT_3D('',#99869,#28013,#28014);
#22443=AXIS2_PLACEMENT_3D('',#99871,#28015,#28016);
#22444=AXIS2_PLACEMENT_3D('',#99873,#28018,#28019);
#22445=AXIS2_PLACEMENT_3D('',#99875,#28020,#28021);
#22446=AXIS2_PLACEMENT_3D('',#99876,#28022,#28023);
#22447=AXIS2_PLACEMENT_3D('',#99878,#28024,#28025);
#22448=AXIS2_PLACEMENT_3D('',#99880,#28027,#28028);
#22449=AXIS2_PLACEMENT_3D('',#99883,#28030,#28031);
#22450=AXIS2_PLACEMENT_3D('',#99884,#28032,#28033);
#22451=AXIS2_PLACEMENT_3D('',#99886,#28034,#28035);
#22452=AXIS2_PLACEMENT_3D('',#99887,#28036,#28037);
#22453=AXIS2_PLACEMENT_3D('',#99889,#28038,#28039);
#22454=AXIS2_PLACEMENT_3D('',#99891,#28041,#28042);
#22455=AXIS2_PLACEMENT_3D('',#99893,#28043,#28044);
#22456=AXIS2_PLACEMENT_3D('',#99894,#28045,#28046);
#22457=AXIS2_PLACEMENT_3D('',#99896,#28047,#28048);
#22458=AXIS2_PLACEMENT_3D('',#99898,#28050,#28051);
#22459=AXIS2_PLACEMENT_3D('',#99900,#28052,#28053);
#22460=AXIS2_PLACEMENT_3D('',#99901,#28054,#28055);
#22461=AXIS2_PLACEMENT_3D('',#99903,#28056,#28057);
#22462=AXIS2_PLACEMENT_3D('',#99905,#28059,#28060);
#22463=AXIS2_PLACEMENT_3D('',#99908,#28062,#28063);
#22464=AXIS2_PLACEMENT_3D('',#99909,#28064,#28065);
#22465=AXIS2_PLACEMENT_3D('',#99910,#28066,#28067);
#22466=AXIS2_PLACEMENT_3D('',#99911,#28068,#28069);
#22467=AXIS2_PLACEMENT_3D('',#99913,#28070,#28071);
#22468=AXIS2_PLACEMENT_3D('',#99916,#28073,#28074);
#22469=AXIS2_PLACEMENT_3D('',#99917,#28075,#28076);
#22470=AXIS2_PLACEMENT_3D('',#99919,#28077,#28078);
#22471=AXIS2_PLACEMENT_3D('',#99921,#28080,#28081);
#22472=AXIS2_PLACEMENT_3D('',#99924,#28083,#28084);
#22473=AXIS2_PLACEMENT_3D('',#99925,#28085,#28086);
#22474=AXIS2_PLACEMENT_3D('',#99926,#28087,#28088);
#22475=AXIS2_PLACEMENT_3D('',#99927,#28089,#28090);
#22476=AXIS2_PLACEMENT_3D('',#99928,#28091,#28092);
#22477=AXIS2_PLACEMENT_3D('',#99930,#28093,#28094);
#22478=AXIS2_PLACEMENT_3D('',#99931,#28095,#28096);
#22479=AXIS2_PLACEMENT_3D('',#99933,#28097,#28098);
#22480=AXIS2_PLACEMENT_3D('',#99934,#28099,#28100);
#22481=AXIS2_PLACEMENT_3D('',#99936,#28101,#28102);
#22482=AXIS2_PLACEMENT_3D('',#99938,#28104,#28105);
#22483=AXIS2_PLACEMENT_3D('',#99940,#28106,#28107);
#22484=AXIS2_PLACEMENT_3D('',#99941,#28108,#28109);
#22485=AXIS2_PLACEMENT_3D('',#99943,#28110,#28111);
#22486=AXIS2_PLACEMENT_3D('',#99945,#28113,#28114);
#22487=AXIS2_PLACEMENT_3D('',#99948,#28116,#28117);
#22488=AXIS2_PLACEMENT_3D('',#99949,#28118,#28119);
#22489=AXIS2_PLACEMENT_3D('',#99950,#28120,#28121);
#22490=AXIS2_PLACEMENT_3D('',#99951,#28122,#28123);
#22491=AXIS2_PLACEMENT_3D('',#99953,#28124,#28125);
#22492=AXIS2_PLACEMENT_3D('',#99954,#28126,#28127);
#22493=AXIS2_PLACEMENT_3D('',#99956,#28128,#28129);
#22494=AXIS2_PLACEMENT_3D('',#99957,#28130,#28131);
#22495=AXIS2_PLACEMENT_3D('',#99959,#28132,#28133);
#22496=AXIS2_PLACEMENT_3D('',#99961,#28135,#28136);
#22497=AXIS2_PLACEMENT_3D('',#99964,#28138,#28139);
#22498=AXIS2_PLACEMENT_3D('',#99965,#28140,#28141);
#22499=AXIS2_PLACEMENT_3D('',#99966,#28142,#28143);
#22500=AXIS2_PLACEMENT_3D('',#99967,#28144,#28145);
#22501=AXIS2_PLACEMENT_3D('',#99968,#28146,#28147);
#22502=AXIS2_PLACEMENT_3D('',#99969,#28148,#28149);
#22503=AXIS2_PLACEMENT_3D('',#99970,#28150,#28151);
#22504=AXIS2_PLACEMENT_3D('',#99971,#28152,#28153);
#22505=AXIS2_PLACEMENT_3D('',#99972,#28154,#28155);
#22506=AXIS2_PLACEMENT_3D('',#99973,#28156,#28157);
#22507=AXIS2_PLACEMENT_3D('',#99974,#28158,#28159);
#22508=AXIS2_PLACEMENT_3D('',#99975,#28160,#28161);
#22509=AXIS2_PLACEMENT_3D('',#99976,#28162,#28163);
#22510=AXIS2_PLACEMENT_3D('',#99977,#28164,#28165);
#22511=AXIS2_PLACEMENT_3D('',#99978,#28166,#28167);
#22512=AXIS2_PLACEMENT_3D('',#99979,#28168,#28169);
#22513=AXIS2_PLACEMENT_3D('',#99980,#28170,#28171);
#22514=AXIS2_PLACEMENT_3D('',#99981,#28172,#28173);
#22515=AXIS2_PLACEMENT_3D('',#99982,#28174,#28175);
#22516=AXIS2_PLACEMENT_3D('',#99983,#28176,#28177);
#22517=AXIS2_PLACEMENT_3D('',#99984,#28178,#28179);
#22518=AXIS2_PLACEMENT_3D('',#99985,#28180,#28181);
#22519=AXIS2_PLACEMENT_3D('',#99986,#28182,#28183);
#22520=AXIS2_PLACEMENT_3D('',#99987,#28184,#28185);
#22521=AXIS2_PLACEMENT_3D('',#99988,#28186,#28187);
#22522=AXIS2_PLACEMENT_3D('',#99989,#28188,#28189);
#22523=AXIS2_PLACEMENT_3D('',#99990,#28190,#28191);
#22524=AXIS2_PLACEMENT_3D('',#99991,#28192,#28193);
#22525=DIRECTION('axis',(0.,0.,1.));
#22526=DIRECTION('refdir',(1.,0.,0.));
#22527=DIRECTION('axis',(0.,0.,1.));
#22528=DIRECTION('refdir',(1.,0.,0.));
#22529=DIRECTION('center_axis',(0.,1.,0.));
#22530=DIRECTION('ref_axis',(1.,0.,0.));
#22531=DIRECTION('',(0.,1.,0.));
#22532=DIRECTION('center_axis',(-0.0253793612844622,-0.999677881145026,
0.000148223423376537));
#22533=DIRECTION('ref_axis',(-0.178708422703468,0.00439108419345073,-0.983892279690437));
#22534=DIRECTION('center_axis',(0.0255908057683819,0.999672491941936,-0.000139695117279073));
#22535=DIRECTION('ref_axis',(0.172447171466502,-0.00427686176175424,0.985009482952664));
#22536=DIRECTION('center_axis',(0.,1.,0.));
#22537=DIRECTION('ref_axis',(1.,0.,0.));
#22538=DIRECTION('',(0.,1.,0.));
#22539=DIRECTION('center_axis',(0.,1.,0.));
#22540=DIRECTION('ref_axis',(1.,0.,0.));
#22541=DIRECTION('',(0.,1.,0.));
#22542=DIRECTION('center_axis',(0.,1.,0.));
#22543=DIRECTION('ref_axis',(1.,0.,0.));
#22544=DIRECTION('',(0.,1.,0.));
#22545=DIRECTION('',(0.,0.,1.));
#22546=DIRECTION('',(-1.,0.,0.));
#22547=DIRECTION('',(0.,0.,-1.));
#22548=DIRECTION('',(1.,0.,0.));
#22549=DIRECTION('center_axis',(0.,1.,0.));
#22550=DIRECTION('ref_axis',(0.,0.,1.));
#22551=DIRECTION('',(-0.00142981099856909,0.882946690327321,0.46947108290132));
#22552=DIRECTION('',(-0.00150687409113358,0.883971486149799,0.467538384525367));
#22553=DIRECTION('',(0.0093100859730185,0.921219118259289,0.388932717128236));
#22554=DIRECTION('',(0.11564262543821,0.977075605521038,0.178745753173203));
#22555=DIRECTION('',(0.11564262543821,0.977075605521038,0.178745753173203));
#22556=DIRECTION('',(0.312891528512139,0.948359943232815,0.0520798373345121));
#22557=DIRECTION('',(0.312891528512139,0.948359943232815,0.0520798373345121));
#22558=DIRECTION('',(0.373785927406222,0.925420377862593,0.0622993154836071));
#22559=DIRECTION('',(0.335603981569758,0.93950240830941,0.0685944045483549));
#22560=DIRECTION('',(0.300592335144719,0.950101339342829,0.0833768135107546));
#22561=DIRECTION('',(0.388156973132249,0.911806820751478,0.133949564537902));
#22562=DIRECTION('',(0.301315367899131,0.918801423299879,0.25497645697187));
#22563=DIRECTION('',(0.301315367899131,0.918801423299879,0.25497645697187));
#22564=DIRECTION('',(0.212309885750666,0.93297911113271,0.29064495626547));
#22565=DIRECTION('',(0.212309885750666,0.93297911113271,0.29064495626547));
#22566=DIRECTION('',(0.270714584418356,0.934862032394266,0.229666266941533));
#22567=DIRECTION('',(0.270714584418356,0.934862032394266,0.229666266941533));
#22568=DIRECTION('',(0.374046850555081,0.917657512959969,0.134140383546302));
#22569=DIRECTION('',(0.418654959254244,0.897085298745081,0.141301068174572));
#22570=DIRECTION('',(0.000960745570679864,0.997274324740366,0.0737766777619821));
#22571=DIRECTION('',(0.0202807143037105,0.975301639137796,0.219944095902709));
#22572=DIRECTION('',(0.000960745570679864,0.997274324740366,0.0737766777619821));
#22573=DIRECTION('',(0.0689297223974915,0.919692597369279,0.386541355762038));
#22574=DIRECTION('',(0.00418796611478942,0.889609932076628,0.456701904627557));
#22575=DIRECTION('',(-0.000115678535487473,0.883083285401883,0.469216258949211));
#22576=DIRECTION('',(0.000654370202600861,0.882947403819665,0.469471462271938));
#22577=DIRECTION('',(0.000647998298494371,0.882947407483268,0.469471464219905));
#22578=DIRECTION('',(-0.000654370203064388,0.882947403819657,0.469471462271951));
#22579=DIRECTION('',(0.000115678535825108,0.883083285401884,0.46921625894921));
#22580=DIRECTION('',(-0.00418796611441199,0.889609932076588,0.456701904627638));
#22581=DIRECTION('',(-0.0689297223978216,0.919692597369242,0.386541355762066));
#22582=DIRECTION('',(-0.0202807143037967,0.975301639137796,0.219944095902698));
#22583=DIRECTION('',(-0.000960745570720953,0.997274324740367,0.0737766777619683));
#22584=DIRECTION('',(-0.000960745570720953,0.997274324740367,0.0737766777619683));
#22585=DIRECTION('',(6.32891971479231E-15,0.999877709626058,-0.0156385994560964));
#22586=DIRECTION('',(-0.374046850567848,0.917657512954638,0.134140383547171));
#22587=DIRECTION('',(-0.270714584414742,0.934862032395629,0.229666266940246));
#22588=DIRECTION('',(-0.270714584414742,0.934862032395629,0.229666266940246));
#22589=DIRECTION('',(-0.21230988575075,0.932979111132764,0.290644956265237));
#22590=DIRECTION('',(-0.21230988575075,0.932979111132764,0.290644956265237));
#22591=DIRECTION('',(-0.301315367899016,0.918801423299914,0.254976456971879));
#22592=DIRECTION('',(-0.301315367899016,0.918801423299914,0.254976456971879));
#22593=DIRECTION('',(-0.38815697313222,0.911806820751496,0.133949564537858));
#22594=DIRECTION('',(-0.300592335144713,0.950101339342829,0.0833768135107739));
#22595=DIRECTION('',(-0.335603981569753,0.939502408309412,0.0685944045483639));
#22596=DIRECTION('',(-0.373785927406274,0.925420377862572,0.0622993154836042));
#22597=DIRECTION('',(-0.312891528512024,0.948359943232853,0.0520798373345141));
#22598=DIRECTION('',(-0.312891528512024,0.948359943232853,0.0520798373345141));
#22599=DIRECTION('',(-0.11564262543822,0.977075605521036,0.178745753173204));
#22600=DIRECTION('',(-0.11564262543822,0.977075605521036,0.178745753173204));
#22601=DIRECTION('',(-0.00931008597314742,0.921219118259316,0.38893271712817));
#22602=DIRECTION('',(0.00150687409148693,0.883971486149805,0.467538384525354));
#22603=DIRECTION('',(0.00142981099892595,0.882946690327321,0.469471082901318));
#22604=DIRECTION('',(0.00131186599430631,0.882946833085555,0.469471158807229));
#22605=DIRECTION('',(-0.215703315134032,0.969009134257414,-0.120388444486531));
#22606=DIRECTION('',(0.000191764460211616,0.999797893622117,-0.0201031125741501));
#22607=DIRECTION('',(-0.215703315134032,0.969009134257414,-0.120388444486531));
#22608=DIRECTION('',(-0.000711770826806861,0.99999974667456,-5.75375725464803E-6));
#22609=DIRECTION('',(0.0013619134070984,0.999999072594712,-1.25999984792182E-6));
#22610=DIRECTION('',(-0.00216662813574643,0.999997652852845,-3.36493555673733E-6));
#22611=DIRECTION('',(-0.0752475458844889,0.997164884342654,1.65004120863823E-5));
#22612=DIRECTION('',(-0.103899479420175,0.994587803073991,-1.23558909609556E-5));
#22613=DIRECTION('',(-0.137985609280151,0.990434122609957,-0.0004694693063891));
#22614=DIRECTION('',(-0.140950090121527,0.990013822946304,0.00238798450134629));
#22615=DIRECTION('',(-0.113368116257768,0.993551950546169,-0.00148046684130703));
#22616=DIRECTION('',(-0.481426420109111,0.851820335359678,0.206472076292778));
#22617=DIRECTION('',(-0.418654959263383,0.897085298741647,0.1413010681693));
#22618=DIRECTION('',(0.481426420119192,0.851820335353988,0.206472076292748));
#22619=DIRECTION('',(0.113368116259197,0.993551950546006,-0.00148046684129751));
#22620=DIRECTION('',(0.140950090121739,0.990013822946273,0.00238798450135761));
#22621=DIRECTION('',(0.13798560927957,0.990434122610038,-0.000469469306391179));
#22622=DIRECTION('',(0.103899479420036,0.994587803074006,-1.23558909597681E-5));
#22623=DIRECTION('',(0.0752475458845945,0.997164884342646,1.65004120770553E-5));
#22624=DIRECTION('',(0.00216662813568782,0.999997652852845,-3.36493555644336E-6));
#22625=DIRECTION('',(-0.00136191340713365,0.999999072594712,-1.25999984490252E-6));
#22626=DIRECTION('',(0.000711770826834646,0.99999974667456,-5.7537572588639E-6));
#22627=DIRECTION('',(-0.000191764460208702,0.999797893622118,-0.0201031125741359));
#22628=DIRECTION('',(0.215703315134029,0.969009134257416,-0.120388444486517));
#22629=DIRECTION('',(0.215703315134029,0.969009134257416,-0.120388444486517));
#22630=DIRECTION('',(-2.65900267047622E-15,0.999951816801407,-0.00981652054273898));
#22631=DIRECTION('',(-0.000647998298984417,0.882947407483259,0.46947146421992));
#22632=DIRECTION('',(-0.00131186599394202,0.882946833085558,0.469471158807223));
#22633=DIRECTION('axis',(0.,0.,1.));
#22634=DIRECTION('refdir',(1.,0.,0.));
#22635=DIRECTION('center_axis',(0.,-1.,0.));
#22636=DIRECTION('ref_axis',(0.,0.,-1.));
#22637=DIRECTION('center_axis',(0.,1.,1.15415719212674E-15));
#22638=DIRECTION('ref_axis',(1.,0.,0.));
#22639=DIRECTION('center_axis',(-1.,0.,0.));
#22640=DIRECTION('ref_axis',(0.,0.,1.));
#22641=DIRECTION('center_axis',(0.,-1.,0.));
#22642=DIRECTION('ref_axis',(1.,0.,0.));
#22643=DIRECTION('center_axis',(0.,-1.,0.));
#22644=DIRECTION('ref_axis',(1.,0.,0.));
#22645=DIRECTION('center_axis',(0.,1.,1.15415719212674E-15));
#22646=DIRECTION('ref_axis',(1.,0.,0.));
#22647=DIRECTION('center_axis',(0.,1.,0.));
#22648=DIRECTION('ref_axis',(1.,0.,0.));
#22649=DIRECTION('center_axis',(0.,1.,0.));
#22650=DIRECTION('ref_axis',(1.,0.,0.));
#22651=DIRECTION('center_axis',(0.,1.,0.));
#22652=DIRECTION('ref_axis',(1.,0.,0.));
#22653=DIRECTION('',(0.,1.,0.));
#22654=DIRECTION('center_axis',(0.,1.,0.));
#22655=DIRECTION('ref_axis',(1.,0.,0.));
#22656=DIRECTION('',(-0.707106781186547,0.707106781186548,8.65956056235493E-17));
#22657=DIRECTION('center_axis',(0.,-1.,0.));
#22658=DIRECTION('ref_axis',(1.,0.,0.));
#22659=DIRECTION('center_axis',(0.,-1.,0.));
#22660=DIRECTION('ref_axis',(1.,0.,0.));
#22661=DIRECTION('center_axis',(0.,1.,0.));
#22662=DIRECTION('ref_axis',(-0.796497710072376,0.,0.60464154492514));
#22663=DIRECTION('center_axis',(0.,1.,0.));
#22664=DIRECTION('ref_axis',(-1.,0.,0.));
#22665=DIRECTION('',(0.,1.,0.));
#22666=DIRECTION('center_axis',(0.,-1.,0.));
#22667=DIRECTION('ref_axis',(-0.268817204301075,0.,0.963191211894998));
#22668=DIRECTION('',(0.,-1.,0.));
#22669=DIRECTION('center_axis',(0.,0.,1.));
#22670=DIRECTION('ref_axis',(1.,0.,0.));
#22671=DIRECTION('center_axis',(-0.963191211894997,0.,-0.268817204301076));
#22672=DIRECTION('ref_axis',(0.268817204301076,0.,-0.963191211894997));
#22673=DIRECTION('center_axis',(0.,0.,1.));
#22674=DIRECTION('ref_axis',(-0.707106781186544,0.707106781186551,0.));
#22675=DIRECTION('center_axis',(0.,0.,1.));
#22676=DIRECTION('ref_axis',(1.,0.,0.));
#22677=DIRECTION('center_axis',(0.,0.,1.));
#22678=DIRECTION('ref_axis',(-0.707106781186544,-0.707106781186551,0.));
#22679=DIRECTION('center_axis',(-0.963191211894997,0.,-0.268817204301076));
#22680=DIRECTION('ref_axis',(0.268817204301076,0.,-0.963191211894997));
#22681=DIRECTION('center_axis',(0.,0.,1.));
#22682=DIRECTION('ref_axis',(-0.707106781186545,0.70710678118655,0.));
#22683=DIRECTION('',(0.,0.,-1.));
#22684=DIRECTION('center_axis',(0.,0.,-1.));
#22685=DIRECTION('ref_axis',(-0.707106781186544,0.707106781186551,0.));
#22686=DIRECTION('',(0.,0.,1.));
#22687=DIRECTION('center_axis',(0.,-1.,0.));
#22688=DIRECTION('ref_axis',(0.707106781186548,0.,0.707106781186547));
#22689=DIRECTION('center_axis',(0.,-1.,0.));
#22690=DIRECTION('ref_axis',(0.707106781186547,0.,0.707106781186547));
#22691=DIRECTION('center_axis',(-0.268817204301076,0.,-0.963191211894997));
#22692=DIRECTION('ref_axis',(0.963191211894997,0.,-0.268817204301076));
#22693=DIRECTION('center_axis',(0.,1.,0.));
#22694=DIRECTION('ref_axis',(0.707106781186547,0.,0.707106781186547));
#22695=DIRECTION('center_axis',(0.,1.,0.));
#22696=DIRECTION('ref_axis',(1.,0.,0.));
#22697=DIRECTION('center_axis',(0.,1.,0.));
#22698=DIRECTION('ref_axis',(0.826936230559385,0.,0.562295714538387));
#22699=DIRECTION('',(0.,-1.,0.));
#22700=DIRECTION('center_axis',(0.,-1.,0.));
#22701=DIRECTION('ref_axis',(-0.796497710072379,0.,-0.604641544925138));
#22702=DIRECTION('center_axis',(0.,-1.,0.));
#22703=DIRECTION('ref_axis',(-1.,0.,0.));
#22704=DIRECTION('',(0.,-1.,0.));
#22705=DIRECTION('center_axis',(0.,1.,0.));
#22706=DIRECTION('ref_axis',(-0.268817204301076,0.,-0.963191211894997));
#22707=DIRECTION('',(0.,1.,0.));
#22708=DIRECTION('center_axis',(0.,0.,1.));
#22709=DIRECTION('ref_axis',(1.,0.,0.));
#22710=DIRECTION('center_axis',(-0.963191211894997,0.,0.268817204301076));
#22711=DIRECTION('ref_axis',(0.268817204301076,0.,0.963191211894997));
#22712=DIRECTION('center_axis',(0.,0.,-1.));
#22713=DIRECTION('ref_axis',(-0.707106781186544,-0.707106781186551,0.));
#22714=DIRECTION('center_axis',(0.,0.,1.));
#22715=DIRECTION('ref_axis',(1.,0.,0.));
#22716=DIRECTION('center_axis',(-0.963191211894997,0.,0.268817204301076));
#22717=DIRECTION('ref_axis',(0.268817204301076,0.,0.963191211894997));
#22718=DIRECTION('center_axis',(0.,-1.,0.));
#22719=DIRECTION('ref_axis',(0.,0.,-1.));
#22720=DIRECTION('center_axis',(0.,1.,0.));
#22721=DIRECTION('ref_axis',(0.707106781186547,0.,-0.707106781186548));
#22722=DIRECTION('center_axis',(-0.268817204301076,0.,0.963191211894997));
#22723=DIRECTION('ref_axis',(-0.963191211894997,0.,-0.268817204301076));
#22724=DIRECTION('center_axis',(0.,-1.,0.));
#22725=DIRECTION('ref_axis',(0.707106781186547,0.,-0.707106781186548));
#22726=DIRECTION('center_axis',(1.,0.,0.));
#22727=DIRECTION('ref_axis',(0.,0.,-1.));
#22728=DIRECTION('',(0.,0.,-1.));
#22729=DIRECTION('center_axis',(0.,1.,0.));
#22730=DIRECTION('ref_axis',(0.60464154492514,0.,0.796497710072376));
#22731=DIRECTION('center_axis',(0.,1.,0.));
#22732=DIRECTION('ref_axis',(0.,0.,1.));
#22733=DIRECTION('',(0.,1.,0.));
#22734=DIRECTION('center_axis',(0.,-1.,0.));
#22735=DIRECTION('ref_axis',(0.963191211894997,0.,0.268817204301076));
#22736=DIRECTION('',(0.,-1.,0.));
#22737=DIRECTION('center_axis',(0.321470784124458,-0.846950546350565,0.423475273175289));
#22738=DIRECTION('ref_axis',(0.512101486820596,0.531671676917698,0.674594170712776));
#22739=DIRECTION('center_axis',(1.,0.,0.));
#22740=DIRECTION('ref_axis',(0.,0.707106781186551,0.707106781186544));
#22741=DIRECTION('center_axis',(-0.321470784124453,-0.846950546350573,-0.423475273175278));
#22742=DIRECTION('ref_axis',(0.512101486820604,-0.531671676917688,0.674594170712778));
#22743=DIRECTION('center_axis',(1.,0.,0.));
#22744=DIRECTION('ref_axis',(0.,-0.707106781186551,0.707106781186544));
#22745=DIRECTION('center_axis',(-0.268817204301076,0.,0.963191211894997));
#22746=DIRECTION('ref_axis',(-0.963191211894997,0.,-0.268817204301076));
#22747=DIRECTION('center_axis',(1.,0.,0.));
#22748=DIRECTION('ref_axis',(0.,0.707106781186553,0.707106781186542));
#22749=DIRECTION('',(-1.,0.,0.));
#22750=DIRECTION('center_axis',(-1.,0.,0.));
#22751=DIRECTION('ref_axis',(0.,0.707106781186551,0.707106781186544));
#22752=DIRECTION('',(1.,0.,0.));
#22753=DIRECTION('center_axis',(0.,1.,0.));
#22754=DIRECTION('ref_axis',(1.,0.,0.));
#22755=DIRECTION('center_axis',(0.,1.,0.));
#22756=DIRECTION('ref_axis',(0.707106781186547,0.,-0.707106781186548));
#22757=DIRECTION('center_axis',(0.,-1.,0.));
#22758=DIRECTION('ref_axis',(-0.604641544925143,0.,0.796497710072374));
#22759=DIRECTION('center_axis',(0.,-1.,0.));
#22760=DIRECTION('ref_axis',(0.,0.,1.));
#22761=DIRECTION('',(0.,-1.,0.));
#22762=DIRECTION('center_axis',(0.,1.,0.));
#22763=DIRECTION('ref_axis',(-0.963191211894998,0.,0.268817204301074));
#22764=DIRECTION('',(0.,1.,0.));
#22765=DIRECTION('center_axis',(0.321470784124453,-0.846950546350573,-0.423475273175278));
#22766=DIRECTION('ref_axis',(-0.512101486820604,-0.531671676917688,0.674594170712778));
#22767=DIRECTION('center_axis',(0.268817204301076,0.,0.963191211894997));
#22768=DIRECTION('ref_axis',(0.963191211894997,0.,-0.268817204301076));
#22769=DIRECTION('center_axis',(-1.,0.,0.));
#22770=DIRECTION('ref_axis',(0.,-0.707106781186551,0.707106781186544));
#22771=DIRECTION('center_axis',(-0.32147078412446,-0.84695054635057,0.423475273175279));
#22772=DIRECTION('ref_axis',(-0.512101486820602,0.531671676917693,0.674594170712776));
#22773=DIRECTION('center_axis',(0.268817204301076,0.,0.963191211894997));
#22774=DIRECTION('ref_axis',(0.963191211894997,0.,-0.268817204301076));
#22775=DIRECTION('center_axis',(0.,-1.,0.));
#22776=DIRECTION('ref_axis',(0.,0.,-1.));
#22777=DIRECTION('center_axis',(0.,1.,0.));
#22778=DIRECTION('ref_axis',(-0.562295714538387,0.,-0.826936230559385));
#22779=DIRECTION('center_axis',(-0.963191211894995,1.98964699753618E-15,
-0.268817204301083));
#22780=DIRECTION('ref_axis',(1.84149810182896E-30,1.,7.40148683083437E-15));
#22781=DIRECTION('center_axis',(0.,-1.,0.));
#22782=DIRECTION('ref_axis',(-0.562295714538387,0.,-0.826936230559385));
#22783=DIRECTION('center_axis',(0.,0.,-1.));
#22784=DIRECTION('ref_axis',(-1.,0.,0.));
#22785=DIRECTION('',(-1.,0.,0.));
#22786=DIRECTION('center_axis',(0.,-1.,0.));
#22787=DIRECTION('ref_axis',(0.604641544925143,0.,-0.796497710072374));
#22788=DIRECTION('center_axis',(0.,-1.,0.));
#22789=DIRECTION('ref_axis',(0.,0.,-1.));
#22790=DIRECTION('',(0.,-1.,0.));
#22791=DIRECTION('center_axis',(0.,1.,0.));
#22792=DIRECTION('ref_axis',(0.963191211894997,0.,-0.268817204301076));
#22793=DIRECTION('',(0.,1.,0.));
#22794=DIRECTION('center_axis',(-0.321470784124453,-0.846950546350573,0.423475273175278));
#22795=DIRECTION('ref_axis',(0.512101486820604,-0.531671676917688,-0.674594170712778));
#22796=DIRECTION('center_axis',(-0.268817204301076,0.,-0.963191211894997));
#22797=DIRECTION('ref_axis',(-0.963191211894997,0.,0.268817204301076));
#22798=DIRECTION('center_axis',(1.,0.,0.));
#22799=DIRECTION('ref_axis',(0.,-0.70710678118655,-0.707106781186545));
#22800=DIRECTION('center_axis',(0.321470784124459,-0.846950546350569,-0.423475273175281));
#22801=DIRECTION('ref_axis',(0.512101486820603,0.531671676917694,-0.674594170712774));
#22802=DIRECTION('center_axis',(1.,0.,0.));
#22803=DIRECTION('ref_axis',(0.,0.70710678118655,-0.707106781186545));
#22804=DIRECTION('center_axis',(-0.268817204301076,0.,-0.963191211894997));
#22805=DIRECTION('ref_axis',(-0.963191211894997,0.,0.268817204301076));
#22806=DIRECTION('center_axis',(0.,-1.,0.));
#22807=DIRECTION('ref_axis',(0.707106781186548,0.,0.707106781186547));
#22808=DIRECTION('center_axis',(0.,1.,0.));
#22809=DIRECTION('ref_axis',(0.707106781186547,0.,0.707106781186547));
#22810=DIRECTION('center_axis',(-0.963191211894997,0.,-0.268817204301078));
#22811=DIRECTION('ref_axis',(0.268817204301078,0.,-0.963191211894997));
#22812=DIRECTION('center_axis',(0.,-1.,0.));
#22813=DIRECTION('ref_axis',(0.707106781186547,0.,0.707106781186547));
#22814=DIRECTION('center_axis',(-1.,0.,0.));
#22815=DIRECTION('ref_axis',(0.,0.70710678118655,-0.707106781186545));
#22816=DIRECTION('',(-1.,0.,0.));
#22817=DIRECTION('center_axis',(-1.,0.,0.));
#22818=DIRECTION('ref_axis',(0.,0.70710678118655,-0.707106781186545));
#22819=DIRECTION('',(1.,0.,0.));
#22820=DIRECTION('center_axis',(0.,0.,1.));
#22821=DIRECTION('ref_axis',(1.,0.,0.));
#22822=DIRECTION('',(1.,0.,0.));
#22823=DIRECTION('',(0.,-1.,0.));
#22824=DIRECTION('center_axis',(0.,1.,0.));
#22825=DIRECTION('ref_axis',(-0.796497710072375,0.,0.604641544925142));
#22826=DIRECTION('center_axis',(0.,1.,0.));
#22827=DIRECTION('ref_axis',(-1.,0.,0.));
#22828=DIRECTION('',(0.,1.,0.));
#22829=DIRECTION('center_axis',(0.,-1.,0.));
#22830=DIRECTION('ref_axis',(-0.268817204301075,0.,0.963191211894998));
#22831=DIRECTION('',(0.,-1.,0.));
#22832=DIRECTION('center_axis',(0.,0.,1.));
#22833=DIRECTION('ref_axis',(1.,0.,0.));
#22834=DIRECTION('center_axis',(0.,0.,1.));
#22835=DIRECTION('ref_axis',(-0.707106781186544,0.707106781186551,0.));
#22836=DIRECTION('center_axis',(0.,0.,1.));
#22837=DIRECTION('ref_axis',(1.,0.,0.));
#22838=DIRECTION('center_axis',(0.,0.,1.));
#22839=DIRECTION('ref_axis',(-0.707106781186544,-0.707106781186551,0.));
#22840=DIRECTION('center_axis',(-0.963191211894998,0.,-0.268817204301074));
#22841=DIRECTION('ref_axis',(0.268817204301074,0.,-0.963191211894998));
#22842=DIRECTION('center_axis',(0.,0.,1.));
#22843=DIRECTION('ref_axis',(-0.707106781186542,0.707106781186553,0.));
#22844=DIRECTION('',(0.,0.,-1.));
#22845=DIRECTION('center_axis',(0.,0.,-1.));
#22846=DIRECTION('ref_axis',(-0.707106781186544,0.707106781186551,0.));
#22847=DIRECTION('',(0.,0.,1.));
#22848=DIRECTION('center_axis',(0.,1.,0.));
#22849=DIRECTION('ref_axis',(1.,0.,0.));
#22850=DIRECTION('center_axis',(0.,1.,0.));
#22851=DIRECTION('ref_axis',(0.707106781186547,0.,0.707106781186547));
#22852=DIRECTION('center_axis',(0.,1.,0.));
#22853=DIRECTION('ref_axis',(0.,0.,1.));
#22854=DIRECTION('center_axis',(0.,-1.,0.));
#22855=DIRECTION('ref_axis',(1.,0.,0.));
#22856=DIRECTION('center_axis',(-1.,0.,0.));
#22857=DIRECTION('ref_axis',(0.,0.,-1.));
#22858=DIRECTION('center_axis',(0.,1.,0.));
#22859=DIRECTION('ref_axis',(1.,0.,0.));
#22860=DIRECTION('center_axis',(0.,1.,0.));
#22861=DIRECTION('ref_axis',(1.,0.,0.));
#22862=DIRECTION('center_axis',(0.,1.,0.));
#22863=DIRECTION('ref_axis',(1.,0.,0.));
#22864=DIRECTION('',(0.707106781186548,0.,-0.707106781186547));
#22865=DIRECTION('',(0.,0.,-1.));
#22866=DIRECTION('',(1.,0.,0.));
#22867=DIRECTION('',(0.,0.,-1.));
#22868=DIRECTION('',(-1.,0.,0.));
#22869=DIRECTION('',(0.,0.,-1.));
#22870=DIRECTION('',(1.,0.,0.));
#22871=DIRECTION('',(0.707106781186547,0.,0.707106781186548));
#22872=DIRECTION('',(0.,0.,1.));
#22873=DIRECTION('',(-0.66436383882992,0.,0.74740931868366));
#22874=DIRECTION('',(-1.,0.,0.));
#22875=DIRECTION('',(-0.66436383882992,0.,-0.74740931868366));
#22876=DIRECTION('',(0.,0.,-1.));
#22877=DIRECTION('',(0.707106781186547,0.,-0.707106781186548));
#22878=DIRECTION('',(1.,0.,0.));
#22879=DIRECTION('',(0.,0.,1.));
#22880=DIRECTION('',(-1.,0.,0.));
#22881=DIRECTION('',(0.,0.,1.));
#22882=DIRECTION('',(1.,0.,0.));
#22883=DIRECTION('',(0.,0.,1.));
#22884=DIRECTION('',(0.707106781186548,0.,0.707106781186547));
#22885=DIRECTION('',(0.,0.,1.));
#22886=DIRECTION('center_axis',(0.,-1.,0.));
#22887=DIRECTION('ref_axis',(6.46422633350345E-16,0.,-1.));
#22888=DIRECTION('',(0.,0.,-1.));
#22889=DIRECTION('center_axis',(0.,-1.,0.));
#22890=DIRECTION('ref_axis',(1.,0.,0.));
#22891=DIRECTION('',(0.,0.,1.));
#22892=DIRECTION('center_axis',(0.,-1.,0.));
#22893=DIRECTION('ref_axis',(1.61616654811585E-15,0.,-1.));
#22894=DIRECTION('',(0.,0.,-1.));
#22895=DIRECTION('center_axis',(0.,-1.,0.));
#22896=DIRECTION('ref_axis',(1.49370186820111E-15,0.,1.));
#22897=DIRECTION('',(0.,0.,1.));
#22898=DIRECTION('center_axis',(0.,-1.,0.));
#22899=DIRECTION('ref_axis',(0.826936230559386,0.,-0.562295714538386));
#22900=DIRECTION('',(1.,0.,0.));
#22901=DIRECTION('center_axis',(0.,-1.,0.));
#22902=DIRECTION('ref_axis',(-0.826936230559385,0.,-0.562295714538387));
#22903=DIRECTION('',(0.,0.,-1.));
#22904=DIRECTION('center_axis',(0.,-1.,0.));
#22905=DIRECTION('ref_axis',(-0.707106781186547,0.,0.707106781186547));
#22906=DIRECTION('',(-1.,0.,0.));
#22907=DIRECTION('center_axis',(0.,-1.,0.));
#22908=DIRECTION('ref_axis',(0.707106781186547,0.,0.707106781186547));
#22909=DIRECTION('center_axis',(0.,-1.,0.));
#22910=DIRECTION('ref_axis',(1.,0.,0.));
#22911=DIRECTION('center_axis',(0.,-1.,0.));
#22912=DIRECTION('ref_axis',(-0.826936230559386,0.,0.562295714538386));
#22913=DIRECTION('',(-1.,0.,0.));
#22914=DIRECTION('center_axis',(0.,-1.,0.));
#22915=DIRECTION('ref_axis',(0.826936230559385,0.,0.562295714538387));
#22916=DIRECTION('',(0.,0.,1.));
#22917=DIRECTION('center_axis',(0.,-1.,0.));
#22918=DIRECTION('ref_axis',(0.707106781186547,0.,-0.707106781186548));
#22919=DIRECTION('',(1.,0.,0.));
#22920=DIRECTION('center_axis',(0.,-1.,0.));
#22921=DIRECTION('ref_axis',(-0.604641544925142,0.,-0.796497710072375));
#22922=DIRECTION('',(0.,0.,-1.));
#22923=DIRECTION('center_axis',(0.,-1.,0.));
#22924=DIRECTION('ref_axis',(1.,0.,0.));
#22925=DIRECTION('center_axis',(0.,1.,0.));
#22926=DIRECTION('ref_axis',(1.,0.,0.));
#22927=DIRECTION('',(0.,1.,0.));
#22928=DIRECTION('center_axis',(0.,-1.,0.));
#22929=DIRECTION('ref_axis',(1.,0.,0.));
#22930=DIRECTION('center_axis',(0.,-1.,0.));
#22931=DIRECTION('ref_axis',(1.,0.,0.));
#22932=DIRECTION('center_axis',(0.,1.,0.));
#22933=DIRECTION('ref_axis',(0.,0.,1.));
#22934=DIRECTION('center_axis',(-1.,0.,0.));
#22935=DIRECTION('ref_axis',(0.,0.,-1.));
#22936=DIRECTION('center_axis',(0.,1.,0.));
#22937=DIRECTION('ref_axis',(1.,0.,0.));
#22938=DIRECTION('center_axis',(0.,1.,0.));
#22939=DIRECTION('ref_axis',(1.,0.,0.));
#22940=DIRECTION('center_axis',(0.,1.,0.));
#22941=DIRECTION('ref_axis',(1.,0.,0.));
#22942=DIRECTION('',(0.,1.,0.));
#22943=DIRECTION('center_axis',(0.,-1.,0.));
#22944=DIRECTION('ref_axis',(1.,0.,0.));
#22945=DIRECTION('center_axis',(0.,-1.,0.));
#22946=DIRECTION('ref_axis',(1.,0.,0.));
#22947=DIRECTION('center_axis',(0.,1.,0.));
#22948=DIRECTION('ref_axis',(0.,0.,1.));
#22949=DIRECTION('center_axis',(-1.,0.,0.));
#22950=DIRECTION('ref_axis',(0.,0.,-1.));
#22951=DIRECTION('center_axis',(0.,0.,-1.));
#22952=DIRECTION('ref_axis',(-0.707106781186544,-0.707106781186551,0.));
#22953=DIRECTION('center_axis',(0.,0.,-1.));
#22954=DIRECTION('ref_axis',(0.,-1.,0.));
#22955=DIRECTION('',(0.,0.,-1.));
#22956=DIRECTION('center_axis',(0.,0.,1.));
#22957=DIRECTION('ref_axis',(-1.,0.,0.));
#22958=DIRECTION('center_axis',(0.,1.,0.));
#22959=DIRECTION('ref_axis',(1.65389215948551E-15,0.,-1.));
#22960=DIRECTION('center_axis',(0.,0.,-1.));
#22961=DIRECTION('ref_axis',(1.,0.,0.));
#22962=DIRECTION('center_axis',(0.,1.,0.));
#22963=DIRECTION('ref_axis',(1.61616654811585E-15,0.,-1.));
#22964=DIRECTION('center_axis',(0.,0.,1.));
#22965=DIRECTION('ref_axis',(0.707106781186544,-0.707106781186551,0.));
#22966=DIRECTION('center_axis',(0.,0.,-1.));
#22967=DIRECTION('ref_axis',(1.,0.,0.));
#22968=DIRECTION('',(0.,0.,1.));
#22969=DIRECTION('center_axis',(0.,1.,0.));
#22970=DIRECTION('ref_axis',(0.,0.,1.));
#22971=DIRECTION('center_axis',(0.,1.,0.));
#22972=DIRECTION('ref_axis',(1.49370186820111E-15,0.,1.));
#22973=DIRECTION('center_axis',(0.,1.,0.));
#22974=DIRECTION('ref_axis',(1.,0.,1.55493420815848E-15));
#22975=DIRECTION('',(0.,1.,0.));
#22976=DIRECTION('center_axis',(0.,-1.,0.));
#22977=DIRECTION('ref_axis',(1.61616654811585E-15,0.,-1.));
#22978=DIRECTION('',(0.,1.,0.));
#22979=DIRECTION('center_axis',(1.,0.,0.));
#22980=DIRECTION('ref_axis',(0.,0.,-1.));
#22981=DIRECTION('',(0.,1.,0.));
#22982=DIRECTION('',(0.,0.,1.));
#22983=DIRECTION('center_axis',(0.,0.,-1.));
#22984=DIRECTION('ref_axis',(-0.707106781186542,-0.707106781186553,0.));
#22985=DIRECTION('',(0.,0.,-1.));
#22986=DIRECTION('center_axis',(0.,0.,1.));
#22987=DIRECTION('ref_axis',(-1.,0.,0.));
#22988=DIRECTION('center_axis',(0.,1.,0.));
#22989=DIRECTION('ref_axis',(0.,0.,1.));
#22990=DIRECTION('center_axis',(0.321470784124453,-0.846950546350569,0.423475273175284));
#22991=DIRECTION('ref_axis',(-0.512101486820598,-0.531671676917694,-0.674594170712778));
#22992=DIRECTION('center_axis',(-1.,0.,0.));
#22993=DIRECTION('ref_axis',(0.,0.,-1.));
#22994=DIRECTION('center_axis',(0.268817204301076,0.,-0.963191211894997));
#22995=DIRECTION('ref_axis',(0.963191211894997,0.,0.268817204301076));
#22996=DIRECTION('center_axis',(0.,-1.,0.));
#22997=DIRECTION('ref_axis',(-0.60464154492514,0.,-0.796497710072376));
#22998=DIRECTION('center_axis',(1.,0.,0.));
#22999=DIRECTION('ref_axis',(0.,-0.70710678118655,-0.707106781186545));
#23000=DIRECTION('center_axis',(0.,0.,1.));
#23001=DIRECTION('ref_axis',(1.,0.,0.));
#23002=DIRECTION('center_axis',(0.,-1.,0.));
#23003=DIRECTION('ref_axis',(-0.796497710072374,0.,-0.604641544925144));
#23004=DIRECTION('center_axis',(-0.963191211894998,0.,0.268817204301074));
#23005=DIRECTION('ref_axis',(0.268817204301074,0.,0.963191211894998));
#23006=DIRECTION('center_axis',(1.,0.,0.));
#23007=DIRECTION('ref_axis',(0.,0.,-1.));
#23008=DIRECTION('',(0.,1.,0.));
#23009=DIRECTION('center_axis',(0.,1.,0.));
#23010=DIRECTION('ref_axis',(-0.60464154492514,0.,-0.796497710072376));
#23011=DIRECTION('',(0.,1.,0.));
#23012=DIRECTION('center_axis',(0.,-1.,0.));
#23013=DIRECTION('ref_axis',(-0.963191211894997,0.,-0.268817204301076));
#23014=DIRECTION('center_axis',(0.,1.,0.));
#23015=DIRECTION('ref_axis',(0.,0.,1.));
#23016=DIRECTION('center_axis',(0.963191211894997,0.,-0.268817204301076));
#23017=DIRECTION('ref_axis',(0.,-1.,0.));
#23018=DIRECTION('center_axis',(0.,1.,0.));
#23019=DIRECTION('ref_axis',(-0.707106781186547,0.,0.707106781186547));
#23020=DIRECTION('center_axis',(0.707106781186548,0.,-0.707106781186547));
#23021=DIRECTION('ref_axis',(0.500000000000001,-0.707106781186545,0.500000000000002));
#23022=DIRECTION('center_axis',(-0.382683432365091,0.,0.923879532511286));
#23023=DIRECTION('ref_axis',(0.923879532511286,6.94492722742783E-16,0.382683432365091));
#23024=DIRECTION('center_axis',(-0.707106781186548,0.,0.707106781186547));
#23025=DIRECTION('ref_axis',(0.,-1.,0.));
#23026=DIRECTION('',(-0.707106781186548,0.,0.707106781186547));
#23027=DIRECTION('center_axis',(0.,0.,1.));
#23028=DIRECTION('ref_axis',(1.,0.,0.));
#23029=DIRECTION('center_axis',(0.,0.,1.));
#23030=DIRECTION('ref_axis',(0.707106781186551,-0.707106781186544,0.));
#23031=DIRECTION('center_axis',(0.,-1.,0.));
#23032=DIRECTION('ref_axis',(0.923879532511287,0.,0.382683432365089));
#23033=DIRECTION('center_axis',(0.,0.,-1.));
#23034=DIRECTION('ref_axis',(0.70710678118655,-0.707106781186545,0.));
#23035=DIRECTION('center_axis',(0.,0.,1.));
#23036=DIRECTION('ref_axis',(0.,-1.,0.));
#23037=DIRECTION('',(0.,0.,1.));
#23038=DIRECTION('center_axis',(0.,0.,1.));
#23039=DIRECTION('ref_axis',(1.,0.,0.));
#23040=DIRECTION('center_axis',(0.,-1.,0.));
#23041=DIRECTION('ref_axis',(1.,0.,0.));
#23042=DIRECTION('center_axis',(2.96059473233375E-14,0.,-1.));
#23043=DIRECTION('ref_axis',(0.,-1.,0.));
#23044=DIRECTION('center_axis',(0.664363838829916,-4.91728020398219E-15,
0.747409318683663));
#23045=DIRECTION('ref_axis',(0.747409318683663,2.66054456061107E-31,-0.664363838829916));
#23046=DIRECTION('center_axis',(0.,0.,1.));
#23047=DIRECTION('ref_axis',(1.,0.,0.));
#23048=DIRECTION('center_axis',(0.,0.,1.));
#23049=DIRECTION('ref_axis',(-7.40148683083437E-15,-1.,0.));
#23050=DIRECTION('center_axis',(0.,-1.,0.));
#23051=DIRECTION('ref_axis',(0.923879532511288,0.,0.382683432365087));
#23052=DIRECTION('center_axis',(0.707106781186547,0.,-0.707106781186548));
#23053=DIRECTION('ref_axis',(0.500000000000006,-0.70710678118654,0.500000000000005));
#23054=DIRECTION('center_axis',(0.,0.,-1.));
#23055=DIRECTION('ref_axis',(0.707106781186547,-0.707106781186547,0.));
#23056=DIRECTION('',(0.,0.,1.));
#23057=DIRECTION('center_axis',(-0.196897064909128,-0.876918033036229,0.438459016518126));
#23058=DIRECTION('ref_axis',(0.359234778961065,-0.480639951872367,-0.799959755393309));
#23059=DIRECTION('center_axis',(0.,-1.,0.));
#23060=DIRECTION('ref_axis',(0.747409318683659,0.,-0.664363838829921));
#23061=DIRECTION('center_axis',(-0.664363838829928,0.,-0.747409318683652));
#23062=DIRECTION('ref_axis',(0.,-1.,0.));
#23063=DIRECTION('center_axis',(1.,7.40148683083437E-15,0.));
#23064=DIRECTION('ref_axis',(0.,0.,-1.));
#23065=DIRECTION('center_axis',(-0.66436383882992,0.,-0.74740931868366));
#23066=DIRECTION('ref_axis',(0.528498197563231,-0.70710678118655,-0.469776175611761));
#23067=DIRECTION('',(0.66436383882992,0.,0.74740931868366));
#23068=DIRECTION('center_axis',(0.196897064909139,-0.876918033036233,0.438459016518113));
#23069=DIRECTION('ref_axis',(-0.359234778961077,-0.48063995187236,-0.799959755393308));
#23070=DIRECTION('center_axis',(0.,-1.,0.));
#23071=DIRECTION('ref_axis',(0.,0.,-1.));
#23072=DIRECTION('center_axis',(-1.,0.,0.));
#23073=DIRECTION('ref_axis',(0.,-1.,0.));
#23074=DIRECTION('center_axis',(0.664363838829921,0.,-0.747409318683659));
#23075=DIRECTION('ref_axis',(-0.747409318683659,0.,-0.664363838829921));
#23076=DIRECTION('center_axis',(-1.,0.,0.));
#23077=DIRECTION('ref_axis',(0.,-0.707106781186542,-0.707106781186553));
#23078=DIRECTION('',(1.,0.,0.));
#23079=DIRECTION('center_axis',(-0.66436383882992,0.,0.74740931868366));
#23080=DIRECTION('ref_axis',(-0.528498197563231,-0.70710678118655,-0.469776175611761));
#23081=DIRECTION('center_axis',(0.664363838829924,0.,-0.747409318683656));
#23082=DIRECTION('ref_axis',(0.,-1.,0.));
#23083=DIRECTION('',(0.66436383882992,0.,-0.74740931868366));
#23084=DIRECTION('center_axis',(0.,0.,1.));
#23085=DIRECTION('ref_axis',(1.,0.,0.));
#23086=DIRECTION('center_axis',(0.,0.,-1.));
#23087=DIRECTION('ref_axis',(-0.707106781186547,-0.707106781186547,0.));
#23088=DIRECTION('center_axis',(0.,-1.,0.));
#23089=DIRECTION('ref_axis',(-0.934721701546419,0.,-0.355380557512882));
#23090=DIRECTION('center_axis',(0.,1.,0.));
#23091=DIRECTION('ref_axis',(-0.40965605156648,0.,-0.912240055804919));
#23092=DIRECTION('center_axis',(0.,-1.,0.));
#23093=DIRECTION('ref_axis',(-0.747409318683659,0.,-0.664363838829921));
#23094=DIRECTION('',(0.,-1.,0.));
#23095=DIRECTION('',(0.,1.,0.));
#23096=DIRECTION('center_axis',(-0.196897064909128,-0.876918033036235,-0.438459016518114));
#23097=DIRECTION('ref_axis',(-0.359234778961066,0.480639951872362,-0.799959755393312));
#23098=DIRECTION('center_axis',(0.66436383882992,0.,-0.74740931868366));
#23099=DIRECTION('ref_axis',(-0.528498197563228,0.707106781186555,-0.469776175611758));
#23100=DIRECTION('center_axis',(-1.,0.,0.));
#23101=DIRECTION('ref_axis',(0.,0.707106781186551,-0.707106781186544));
#23102=DIRECTION('center_axis',(0.,1.,0.));
#23103=DIRECTION('ref_axis',(0.40965605156648,0.,-0.912240055804919));
#23104=DIRECTION('center_axis',(0.,-1.,0.));
#23105=DIRECTION('ref_axis',(0.,0.,-1.));
#23106=DIRECTION('',(0.,-1.,0.));
#23107=DIRECTION('',(0.,1.,0.));
#23108=DIRECTION('center_axis',(0.196897064909128,-0.876918033036229,-0.438459016518126));
#23109=DIRECTION('ref_axis',(0.359234778961052,0.480639951872364,-0.799959755393317));
#23110=DIRECTION('center_axis',(1.,0.,0.));
#23111=DIRECTION('ref_axis',(0.,0.707106781186551,-0.707106781186544));
#23112=DIRECTION('center_axis',(-0.66436383882992,0.,-0.74740931868366));
#23113=DIRECTION('ref_axis',(0.528498197563224,0.70710678118656,-0.469776175611754));
#23114=DIRECTION('center_axis',(0.,1.,0.));
#23115=DIRECTION('ref_axis',(0.934721701546416,0.,-0.355380557512891));
#23116=DIRECTION('center_axis',(0.,-1.,0.));
#23117=DIRECTION('ref_axis',(0.747409318683655,0.,-0.664363838829925));
#23118=DIRECTION('',(0.,-1.,0.));
#23119=DIRECTION('',(0.,1.,0.));
#23120=DIRECTION('center_axis',(0.,0.,1.));
#23121=DIRECTION('ref_axis',(1.,0.,0.));
#23122=DIRECTION('center_axis',(0.66436383882992,0.,0.74740931868366));
#23123=DIRECTION('ref_axis',(0.528498197563228,0.707106781186555,-0.469776175611758));
#23124=DIRECTION('center_axis',(0.,0.,-1.));
#23125=DIRECTION('ref_axis',(0.707106781186544,0.707106781186551,0.));
#23126=DIRECTION('center_axis',(0.74740931868366,0.,-0.66436383882992));
#23127=DIRECTION('ref_axis',(-0.66436383882992,0.,-0.74740931868366));
#23128=DIRECTION('',(-0.66436383882992,0.,-0.74740931868366));
#23129=DIRECTION('center_axis',(0.,0.,-1.));
#23130=DIRECTION('ref_axis',(-1.,0.,0.));
#23131=DIRECTION('',(-1.,0.,0.));
#23132=DIRECTION('center_axis',(-1.,0.,0.));
#23133=DIRECTION('ref_axis',(0.,0.707106781186547,-0.707106781186547));
#23134=DIRECTION('',(1.,0.,0.));
#23135=DIRECTION('center_axis',(-0.66436383882992,0.,0.74740931868366));
#23136=DIRECTION('ref_axis',(-0.528498197563227,0.707106781186556,-0.469776175611757));
#23137=DIRECTION('',(-0.66436383882992,0.,0.74740931868366));
#23138=DIRECTION('center_axis',(-0.66436383882992,0.,0.74740931868366));
#23139=DIRECTION('ref_axis',(-0.528498197563228,0.707106781186555,-0.469776175611758));
#23140=DIRECTION('',(0.66436383882992,0.,-0.74740931868366));
#23141=DIRECTION('center_axis',(-0.74740931868366,0.,-0.66436383882992));
#23142=DIRECTION('ref_axis',(-0.66436383882992,0.,0.74740931868366));
#23143=DIRECTION('',(0.,-1.,0.));
#23144=DIRECTION('center_axis',(0.,0.,1.));
#23145=DIRECTION('ref_axis',(1.,0.,0.));
#23146=DIRECTION('center_axis',(0.,0.,1.));
#23147=DIRECTION('ref_axis',(1.,0.,0.));
#23148=DIRECTION('center_axis',(7.40148683083432E-15,-1.,-2.0656822580655E-15));
#23149=DIRECTION('ref_axis',(0.268817204301075,5.02404021851122E-31,0.963191211894998));
#23150=DIRECTION('center_axis',(0.963191211895,0.,-0.268817204301067));
#23151=DIRECTION('ref_axis',(0.,-1.,0.));
#23152=DIRECTION('center_axis',(0.,0.,1.));
#23153=DIRECTION('ref_axis',(1.,0.,0.));
#23154=DIRECTION('center_axis',(0.,1.,0.));
#23155=DIRECTION('ref_axis',(0.268817204301075,0.,0.963191211894998));
#23156=DIRECTION('center_axis',(0.,0.,1.));
#23157=DIRECTION('ref_axis',(0.707106781186544,0.707106781186551,0.));
#23158=DIRECTION('center_axis',(0.963191211894997,0.,-0.268817204301076));
#23159=DIRECTION('ref_axis',(-0.268817204301076,0.,-0.963191211894997));
#23160=DIRECTION('center_axis',(0.,-1.,0.));
#23161=DIRECTION('ref_axis',(0.796497710072375,0.,0.604641544925142));
#23162=DIRECTION('',(0.,-1.,0.));
#23163=DIRECTION('',(0.,1.,0.));
#23164=DIRECTION('center_axis',(0.,1.,0.));
#23165=DIRECTION('ref_axis',(0.,0.,1.));
#23166=DIRECTION('center_axis',(-0.268817204301074,1.78226176760406E-15,
0.963191211894998));
#23167=DIRECTION('ref_axis',(-0.963191211894998,7.01637702544147E-32,-0.268817204301074));
#23168=DIRECTION('center_axis',(0.,1.,0.));
#23169=DIRECTION('ref_axis',(-0.826936230559386,0.,0.562295714538386));
#23170=DIRECTION('center_axis',(0.321470784124458,-0.846950546350566,0.423475273175286));
#23171=DIRECTION('ref_axis',(-0.512101486820597,-0.531671676917699,-0.674594170712774));
#23172=DIRECTION('center_axis',(0.,-1.,0.));
#23173=DIRECTION('ref_axis',(-0.604641544925144,0.,-0.796497710072374));
#23174=DIRECTION('center_axis',(-1.,0.,0.));
#23175=DIRECTION('ref_axis',(0.,-0.70710678118655,-0.707106781186545));
#23176=DIRECTION('center_axis',(0.,0.,1.));
#23177=DIRECTION('ref_axis',(0.707106781186542,-0.707106781186553,0.));
#23178=DIRECTION('center_axis',(0.,0.,1.));
#23179=DIRECTION('ref_axis',(0.,-1.,0.));
#23180=DIRECTION('',(0.,0.,1.));
#23181=DIRECTION('center_axis',(0.,1.,0.));
#23182=DIRECTION('ref_axis',(-0.707106781186548,0.,-0.707106781186547));
#23183=DIRECTION('center_axis',(0.,1.,0.));
#23184=DIRECTION('ref_axis',(-0.604641544925142,0.,-0.796497710072375));
#23185=DIRECTION('center_axis',(-0.963191211894997,0.,-0.268817204301076));
#23186=DIRECTION('ref_axis',(0.268817204301076,0.,-0.963191211894997));
#23187=DIRECTION('center_axis',(-1.,0.,0.));
#23188=DIRECTION('ref_axis',(0.,-0.707106781186553,0.707106781186542));
#23189=DIRECTION('center_axis',(0.,1.,0.));
#23190=DIRECTION('ref_axis',(0.707106781186548,0.,-0.707106781186547));
#23191=DIRECTION('center_axis',(0.,0.,-1.));
#23192=DIRECTION('ref_axis',(-0.707106781186545,-0.70710678118655,0.));
#23193=DIRECTION('center_axis',(-0.321470784124458,-0.846950546350566,0.423475273175286));
#23194=DIRECTION('ref_axis',(0.512101486820597,-0.531671676917699,-0.674594170712774));
#23195=DIRECTION('center_axis',(-0.268817204301076,0.,-0.963191211894997));
#23196=DIRECTION('ref_axis',(0.963191211894997,0.,-0.268817204301076));
#23197=DIRECTION('center_axis',(1.,0.,0.));
#23198=DIRECTION('ref_axis',(0.,-0.70710678118655,-0.707106781186545));
#23199=DIRECTION('center_axis',(0.,-1.,0.));
#23200=DIRECTION('ref_axis',(0.60464154492514,0.,-0.796497710072376));
#23201=DIRECTION('center_axis',(0.,1.,0.));
#23202=DIRECTION('ref_axis',(0.,0.,1.));
#23203=DIRECTION('center_axis',(0.,0.,1.));
#23204=DIRECTION('ref_axis',(1.,0.,0.));
#23205=DIRECTION('center_axis',(0.,-1.,0.));
#23206=DIRECTION('ref_axis',(0.796497710072377,0.,-0.604641544925139));
#23207=DIRECTION('center_axis',(0.,-1.,0.));
#23208=DIRECTION('ref_axis',(-0.707106781186547,0.,0.707106781186548));
#23209=DIRECTION('center_axis',(0.,1.,0.));
#23210=DIRECTION('ref_axis',(-0.707106781186547,0.,0.707106781186547));
#23211=DIRECTION('center_axis',(0.268817204301076,0.,-0.963191211894997));
#23212=DIRECTION('ref_axis',(0.963191211894997,0.,0.268817204301076));
#23213=DIRECTION('center_axis',(0.,-1.,0.));
#23214=DIRECTION('ref_axis',(-0.707106781186547,0.,0.707106781186547));
#23215=DIRECTION('center_axis',(0.,0.,-1.));
#23216=DIRECTION('ref_axis',(0.707106781186542,0.707106781186553,0.));
#23217=DIRECTION('',(0.,0.,-1.));
#23218=DIRECTION('center_axis',(0.,0.,-1.));
#23219=DIRECTION('ref_axis',(0.707106781186544,0.707106781186551,0.));
#23220=DIRECTION('',(0.,0.,1.));
#23221=DIRECTION('center_axis',(-1.,0.,0.));
#23222=DIRECTION('ref_axis',(0.,0.,1.));
#23223=DIRECTION('',(0.,-1.,0.));
#23224=DIRECTION('center_axis',(0.,1.,0.));
#23225=DIRECTION('ref_axis',(0.796497710072378,0.,-0.604641544925139));
#23226=DIRECTION('',(0.,1.,0.));
#23227=DIRECTION('center_axis',(0.,-1.,0.));
#23228=DIRECTION('ref_axis',(0.268817204301081,0.,-0.963191211894996));
#23229=DIRECTION('center_axis',(0.,1.,0.));
#23230=DIRECTION('ref_axis',(-0.707106781186547,0.,-0.707106781186548));
#23231=DIRECTION('center_axis',(0.,-1.,0.));
#23232=DIRECTION('ref_axis',(0.60464154492514,0.,-0.796497710072376));
#23233=DIRECTION('',(0.,1.,0.));
#23234=DIRECTION('center_axis',(0.,1.,0.));
#23235=DIRECTION('ref_axis',(0.,0.,-1.));
#23236=DIRECTION('center_axis',(0.,1.,0.));
#23237=DIRECTION('ref_axis',(0.,0.,1.));
#23238=DIRECTION('center_axis',(-1.,0.,0.));
#23239=DIRECTION('ref_axis',(0.,0.,-1.));
#23240=DIRECTION('center_axis',(0.,1.,0.));
#23241=DIRECTION('ref_axis',(1.,0.,0.));
#23242=DIRECTION('center_axis',(0.,1.,0.));
#23243=DIRECTION('ref_axis',(1.,0.,0.));
#23244=DIRECTION('center_axis',(0.,1.,0.));
#23245=DIRECTION('ref_axis',(1.,0.,0.));
#23246=DIRECTION('',(0.,1.,0.));
#23247=DIRECTION('center_axis',(0.,-1.,0.));
#23248=DIRECTION('ref_axis',(1.,0.,0.));
#23249=DIRECTION('center_axis',(0.,-1.,0.));
#23250=DIRECTION('ref_axis',(1.,0.,0.));
#23251=DIRECTION('center_axis',(0.,0.,1.));
#23252=DIRECTION('ref_axis',(1.,0.,0.));
#23253=DIRECTION('center_axis',(0.,-1.,0.));
#23254=DIRECTION('ref_axis',(-1.,0.,0.));
#23255=DIRECTION('center_axis',(2.96059473233375E-14,0.,1.));
#23256=DIRECTION('ref_axis',(0.,-1.,0.));
#23257=DIRECTION('center_axis',(-0.707106781186544,3.14018491736755E-14,
-0.707106781186551));
#23258=DIRECTION('ref_axis',(-0.707106781186551,2.99807087075423E-31,0.707106781186544));
#23259=DIRECTION('center_axis',(0.,0.,1.));
#23260=DIRECTION('ref_axis',(-0.707106781186547,-0.707106781186547,0.));
#23261=DIRECTION('',(0.,0.,-1.));
#23262=DIRECTION('center_axis',(0.182143211721535,-0.879465224064607,-0.439732612032306));
#23263=DIRECTION('ref_axis',(-0.336556770590779,-0.475963149477974,0.812519920068741));
#23264=DIRECTION('center_axis',(0.,-1.,0.));
#23265=DIRECTION('ref_axis',(-0.707106781186548,0.,0.707106781186548));
#23266=DIRECTION('center_axis',(0.707106781186544,0.,0.707106781186551));
#23267=DIRECTION('ref_axis',(0.,-1.,0.));
#23268=DIRECTION('center_axis',(-1.,-7.40148683083437E-15,0.));
#23269=DIRECTION('ref_axis',(0.,0.,1.));
#23270=DIRECTION('center_axis',(0.707106781186547,0.,0.707106781186548));
#23271=DIRECTION('ref_axis',(-0.500000000000005,-0.70710678118654,0.500000000000005));
#23272=DIRECTION('',(-0.707106781186547,0.,-0.707106781186548));
#23273=DIRECTION('center_axis',(-0.408248290463862,-0.816496580927729,-0.408248290463859));
#23274=DIRECTION('ref_axis',(0.577350269189622,-0.577350269189622,0.577350269189634));
#23275=DIRECTION('center_axis',(0.,-1.,0.));
#23276=DIRECTION('ref_axis',(0.,0.,1.));
#23277=DIRECTION('center_axis',(1.,0.,0.));
#23278=DIRECTION('ref_axis',(0.,-1.,0.));
#23279=DIRECTION('center_axis',(0.,-1.48029736616687E-14,1.));
#23280=DIRECTION('ref_axis',(1.,0.,0.));
#23281=DIRECTION('center_axis',(1.,0.,0.));
#23282=DIRECTION('ref_axis',(0.,-0.707106781186542,0.707106781186553));
#23283=DIRECTION('',(-1.,0.,0.));
#23284=DIRECTION('center_axis',(-0.408248290463864,-0.816496580927728,0.408248290463858));
#23285=DIRECTION('ref_axis',(0.577350269189628,-0.577350269189628,-0.577350269189622));
#23286=DIRECTION('center_axis',(0.,-1.,0.));
#23287=DIRECTION('ref_axis',(1.,0.,0.));
#23288=DIRECTION('center_axis',(0.,0.,-1.));
#23289=DIRECTION('ref_axis',(0.,-1.,0.));
#23290=DIRECTION('center_axis',(1.,0.,0.));
#23291=DIRECTION('ref_axis',(0.,0.,-1.));
#23292=DIRECTION('center_axis',(0.,0.,-1.));
#23293=DIRECTION('ref_axis',(0.70710678118655,-0.707106781186545,0.));
#23294=DIRECTION('',(0.,0.,1.));
#23295=DIRECTION('center_axis',(-1.,0.,0.));
#23296=DIRECTION('ref_axis',(0.,-0.707106781186542,-0.707106781186553));
#23297=DIRECTION('',(1.,0.,0.));
#23298=DIRECTION('center_axis',(0.707106781186548,0.,0.707106781186548));
#23299=DIRECTION('ref_axis',(0.707106781186548,0.,-0.707106781186548));
#23300=DIRECTION('center_axis',(0.,0.,-1.));
#23301=DIRECTION('ref_axis',(0.70710678118655,-0.707106781186545,0.));
#23302=DIRECTION('center_axis',(-0.707106781186548,0.,0.707106781186548));
#23303=DIRECTION('ref_axis',(0.707106781186548,0.,0.707106781186548));
#23304=DIRECTION('',(0.,0.,1.));
#23305=DIRECTION('center_axis',(-0.816496580927727,-0.408248290463865,0.408248290463859));
#23306=DIRECTION('ref_axis',(0.577350269189626,-0.577350269189629,0.577350269189623));
#23307=DIRECTION('center_axis',(0.,-1.,0.));
#23308=DIRECTION('ref_axis',(0.,0.,1.));
#23309=DIRECTION('center_axis',(1.,0.,0.));
#23310=DIRECTION('ref_axis',(0.,-1.,0.));
#23311=DIRECTION('center_axis',(0.,7.40148683083437E-15,1.));
#23312=DIRECTION('ref_axis',(1.,0.,0.));
#23313=DIRECTION('center_axis',(1.,0.,0.));
#23314=DIRECTION('ref_axis',(0.,-0.707106781186547,0.707106781186547));
#23315=DIRECTION('',(-1.,0.,0.));
#23316=DIRECTION('center_axis',(0.,0.,-1.));
#23317=DIRECTION('ref_axis',(0.70710678118655,-0.707106781186545,0.));
#23318=DIRECTION('',(0.,0.,1.));
#23319=DIRECTION('center_axis',(0.,1.,0.));
#23320=DIRECTION('ref_axis',(0.707106781186545,0.,0.70710678118655));
#23321=DIRECTION('center_axis',(0.,-1.,0.));
#23322=DIRECTION('ref_axis',(1.,0.,0.));
#23323=DIRECTION('',(0.,-1.,0.));
#23324=DIRECTION('',(0.,1.,0.));
#23325=DIRECTION('center_axis',(-0.816496580927726,0.408248290463866,0.40824829046386));
#23326=DIRECTION('ref_axis',(0.577350269189626,0.577350269189629,0.577350269189623));
#23327=DIRECTION('center_axis',(0.,0.,1.));
#23328=DIRECTION('ref_axis',(0.707106781186544,0.707106781186551,0.));
#23329=DIRECTION('center_axis',(1.,0.,0.));
#23330=DIRECTION('ref_axis',(0.,0.707106781186551,0.707106781186544));
#23331=DIRECTION('center_axis',(0.,1.,0.));
#23332=DIRECTION('ref_axis',(0.707106781186545,0.,-0.70710678118655));
#23333=DIRECTION('center_axis',(0.,-1.,0.));
#23334=DIRECTION('ref_axis',(0.,0.,-1.));
#23335=DIRECTION('',(0.,-1.,0.));
#23336=DIRECTION('',(0.,1.,0.));
#23337=DIRECTION('center_axis',(0.408248290463864,-0.816496580927727,-0.408248290463861));
#23338=DIRECTION('ref_axis',(0.57735026918963,0.577350269189624,-0.577350269189624));
#23339=DIRECTION('center_axis',(1.,0.,0.));
#23340=DIRECTION('ref_axis',(0.,0.707106781186547,-0.707106781186547));
#23341=DIRECTION('center_axis',(0.,0.,-1.));
#23342=DIRECTION('ref_axis',(0.707106781186544,0.707106781186551,0.));
#23343=DIRECTION('center_axis',(0.,1.,0.));
#23344=DIRECTION('ref_axis',(0.707106781186555,0.,0.70710678118654));
#23345=DIRECTION('center_axis',(0.,-1.,0.));
#23346=DIRECTION('ref_axis',(1.,0.,0.));
#23347=DIRECTION('',(0.,-1.,0.));
#23348=DIRECTION('',(0.,1.,0.));
#23349=DIRECTION('center_axis',(0.408248290463861,-0.816496580927728,0.408248290463861));
#23350=DIRECTION('ref_axis',(0.577350269189622,0.577350269189622,0.577350269189634));
#23351=DIRECTION('center_axis',(0.,0.,1.));
#23352=DIRECTION('ref_axis',(0.707106781186544,0.707106781186551,0.));
#23353=DIRECTION('center_axis',(1.,0.,0.));
#23354=DIRECTION('ref_axis',(0.,0.707106781186551,0.707106781186544));
#23355=DIRECTION('center_axis',(0.,1.,0.));
#23356=DIRECTION('ref_axis',(-0.38268343236509,0.,0.923879532511287));
#23357=DIRECTION('center_axis',(0.,-1.,0.));
#23358=DIRECTION('ref_axis',(0.,0.,1.));
#23359=DIRECTION('',(0.,-1.,0.));
#23360=DIRECTION('',(0.,1.,0.));
#23361=DIRECTION('center_axis',(-0.182143211721524,-0.879465224064608,0.43973261203231));
#23362=DIRECTION('ref_axis',(-0.33655677059077,0.475963149477971,0.812519920068747));
#23363=DIRECTION('center_axis',(-1.,0.,0.));
#23364=DIRECTION('ref_axis',(0.,0.707106781186551,0.707106781186544));
#23365=DIRECTION('center_axis',(0.707106781186547,0.,0.707106781186548));
#23366=DIRECTION('ref_axis',(-0.500000000000004,0.707106781186542,0.500000000000004));
#23367=DIRECTION('center_axis',(0.,1.,0.));
#23368=DIRECTION('ref_axis',(-0.923879532511285,0.,0.382683432365094));
#23369=DIRECTION('center_axis',(0.,-1.,0.));
#23370=DIRECTION('ref_axis',(-0.707106781186548,0.,0.707106781186548));
#23371=DIRECTION('',(0.,-1.,0.));
#23372=DIRECTION('',(0.,1.,0.));
#23373=DIRECTION('center_axis',(0.,0.,1.));
#23374=DIRECTION('ref_axis',(1.,0.,0.));
#23375=DIRECTION('center_axis',(-0.707106781186547,0.,-0.707106781186548));
#23376=DIRECTION('ref_axis',(-0.500000000000006,0.70710678118654,0.500000000000005));
#23377=DIRECTION('center_axis',(0.,0.,1.));
#23378=DIRECTION('ref_axis',(-0.707106781186544,0.707106781186551,0.));
#23379=DIRECTION('center_axis',(0.,1.,0.));
#23380=DIRECTION('ref_axis',(-0.934721701546419,0.,-0.355380557512883));
#23381=DIRECTION('',(0.,1.,0.));
#23382=DIRECTION('center_axis',(0.,-1.,0.));
#23383=DIRECTION('ref_axis',(-1.,0.,0.));
#23384=DIRECTION('center_axis',(0.,0.,1.));
#23385=DIRECTION('ref_axis',(1.,0.,0.));
#23386=DIRECTION('center_axis',(0.,0.,-1.));
#23387=DIRECTION('ref_axis',(-0.707106781186544,0.707106781186551,0.));
#23388=DIRECTION('center_axis',(0.,0.,1.));
#23389=DIRECTION('ref_axis',(1.,0.,0.));
#23390=DIRECTION('',(1.,0.,0.));
#23391=DIRECTION('center_axis',(0.707106781186547,0.,0.707106781186548));
#23392=DIRECTION('ref_axis',(-0.500000000000002,0.707106781186545,0.500000000000001));
#23393=DIRECTION('',(-0.707106781186547,0.,-0.707106781186548));
#23394=DIRECTION('',(0.707106781186547,0.,0.707106781186548));
#23395=DIRECTION('center_axis',(1.,0.,0.));
#23396=DIRECTION('ref_axis',(0.,0.707106781186547,0.707106781186547));
#23397=DIRECTION('',(-1.,0.,0.));
#23398=DIRECTION('center_axis',(1.,0.,0.));
#23399=DIRECTION('ref_axis',(0.,0.,-1.));
#23400=DIRECTION('',(0.,0.,-1.));
#23401=DIRECTION('center_axis',(0.,0.,-1.));
#23402=DIRECTION('ref_axis',(0.707106781186545,0.70710678118655,0.));
#23403=DIRECTION('',(0.,0.,1.));
#23404=DIRECTION('center_axis',(-1.,0.,0.));
#23405=DIRECTION('ref_axis',(0.,0.707106781186547,-0.707106781186547));
#23406=DIRECTION('',(-1.,0.,0.));
#23407=DIRECTION('center_axis',(-0.707106781186548,0.,-0.707106781186548));
#23408=DIRECTION('ref_axis',(-0.707106781186548,0.,0.707106781186548));
#23409=DIRECTION('',(1.,0.,0.));
#23410=DIRECTION('center_axis',(0.,0.,-1.));
#23411=DIRECTION('ref_axis',(-1.,0.,0.));
#23412=DIRECTION('',(0.,1.,0.));
#23413=DIRECTION('center_axis',(1.,0.,0.));
#23414=DIRECTION('ref_axis',(0.,0.,-1.));
#23415=DIRECTION('',(0.,1.,0.));
#23416=DIRECTION('',(0.,0.,-1.));
#23417=DIRECTION('center_axis',(0.,0.,1.));
#23418=DIRECTION('ref_axis',(1.,0.,0.));
#23419=DIRECTION('',(1.,0.,0.));
#23420=DIRECTION('center_axis',(1.,0.,0.));
#23421=DIRECTION('ref_axis',(0.,0.707106781186553,0.707106781186542));
#23422=DIRECTION('',(-1.,0.,0.));
#23423=DIRECTION('center_axis',(0.707106781186548,0.,-0.707106781186548));
#23424=DIRECTION('ref_axis',(-0.707106781186548,0.,-0.707106781186548));
#23425=DIRECTION('center_axis',(0.,0.,-1.));
#23426=DIRECTION('ref_axis',(0.707106781186545,0.70710678118655,0.));
#23427=DIRECTION('',(0.,0.,-1.));
#23428=DIRECTION('center_axis',(0.382683432365085,0.,-0.923879532511289));
#23429=DIRECTION('ref_axis',(0.923879532511289,1.06845034268121E-16,0.382683432365085));
#23430=DIRECTION('',(0.,0.,1.));
#23431=DIRECTION('center_axis',(1.,0.,0.));
#23432=DIRECTION('ref_axis',(0.,0.,-1.));
#23433=DIRECTION('',(0.,1.,0.));
#23434=DIRECTION('center_axis',(0.,-1.,0.));
#23435=DIRECTION('ref_axis',(0.,0.,-1.));
#23436=DIRECTION('center_axis',(0.,1.,0.));
#23437=DIRECTION('ref_axis',(1.,0.,0.));
#23438=DIRECTION('center_axis',(-1.,0.,0.));
#23439=DIRECTION('ref_axis',(0.,0.,1.));
#23440=DIRECTION('center_axis',(0.,1.,0.));
#23441=DIRECTION('ref_axis',(1.,0.,0.));
#23442=DIRECTION('',(-0.707106781186548,0.,0.707106781186547));
#23443=DIRECTION('',(0.,0.,1.));
#23444=DIRECTION('center_axis',(0.,1.,0.));
#23445=DIRECTION('ref_axis',(6.46422633350345E-16,0.,-1.));
#23446=DIRECTION('',(0.,0.,-1.));
#23447=DIRECTION('',(-0.707106781186548,0.,-0.707106781186547));
#23448=DIRECTION('',(0.,0.,-1.));
#23449=DIRECTION('',(-1.,0.,0.));
#23450=DIRECTION('',(0.,0.,-1.));
#23451=DIRECTION('',(1.,0.,0.));
#23452=DIRECTION('',(0.,0.,-1.));
#23453=DIRECTION('',(-1.,0.,0.));
#23454=DIRECTION('',(-0.707106781186547,0.,0.707106781186548));
#23455=DIRECTION('',(0.,0.,1.));
#23456=DIRECTION('',(0.66436383882992,0.,0.74740931868366));
#23457=DIRECTION('',(0.,0.,-1.));
#23458=DIRECTION('',(0.,0.,1.));
#23459=DIRECTION('center_axis',(0.,1.,0.));
#23460=DIRECTION('ref_axis',(-0.707106781186547,0.,0.707106781186547));
#23461=DIRECTION('',(0.,0.,1.));
#23462=DIRECTION('center_axis',(0.,1.,0.));
#23463=DIRECTION('ref_axis',(-0.707106781186547,0.,-0.707106781186548));
#23464=DIRECTION('',(-1.,0.,0.));
#23465=DIRECTION('center_axis',(0.,1.,0.));
#23466=DIRECTION('ref_axis',(0.707106781186547,0.,-0.707106781186547));
#23467=DIRECTION('',(0.,0.,-1.));
#23468=DIRECTION('center_axis',(0.,1.,0.));
#23469=DIRECTION('ref_axis',(1.49370186820111E-15,0.,1.));
#23470=DIRECTION('',(0.,0.,1.));
#23471=DIRECTION('center_axis',(0.,1.,0.));
#23472=DIRECTION('ref_axis',(1.61616654811585E-15,0.,-1.));
#23473=DIRECTION('center_axis',(0.,1.,0.));
#23474=DIRECTION('ref_axis',(1.,0.,0.));
#23475=DIRECTION('',(1.,0.,0.));
#23476=DIRECTION('center_axis',(0.,1.,0.));
#23477=DIRECTION('ref_axis',(1.,0.,0.));
#23478=DIRECTION('center_axis',(0.,1.,0.));
#23479=DIRECTION('ref_axis',(1.,0.,0.));
#23480=DIRECTION('center_axis',(0.321470784124458,-0.846950546350566,-0.423475273175286));
#23481=DIRECTION('ref_axis',(0.512101486820597,0.531671676917699,-0.674594170712774));
#23482=DIRECTION('center_axis',(1.,0.,0.));
#23483=DIRECTION('ref_axis',(0.,1.,0.));
#23484=DIRECTION('center_axis',(-1.,0.,0.));
#23485=DIRECTION('ref_axis',(0.,0.70710678118655,-0.707106781186545));
#23486=DIRECTION('center_axis',(1.,0.,0.));
#23487=DIRECTION('ref_axis',(0.,0.,-1.));
#23488=DIRECTION('',(-1.,0.,0.));
#23489=DIRECTION('center_axis',(1.,0.,0.));
#23490=DIRECTION('ref_axis',(0.,-0.70710678118655,-0.707106781186545));
#23491=DIRECTION('',(1.,0.,0.));
#23492=DIRECTION('center_axis',(0.,1.,0.));
#23493=DIRECTION('ref_axis',(-0.604641544925143,0.,-0.796497710072374));
#23494=DIRECTION('',(0.,1.,0.));
#23495=DIRECTION('center_axis',(0.,-1.,0.));
#23496=DIRECTION('ref_axis',(-0.963191211894997,0.,-0.268817204301076));
#23497=DIRECTION('',(0.,-1.,0.));
#23498=DIRECTION('center_axis',(-0.321470784124459,-0.846950546350567,-0.423475273175284));
#23499=DIRECTION('ref_axis',(-0.512101486820603,0.531671676917699,-0.67459417071277));
#23500=DIRECTION('center_axis',(0.,0.,1.));
#23501=DIRECTION('ref_axis',(1.,0.,0.));
#23502=DIRECTION('center_axis',(0.,1.,0.));
#23503=DIRECTION('ref_axis',(-0.707106781186547,0.,0.707106781186548));
#23504=DIRECTION('center_axis',(0.,0.,1.));
#23505=DIRECTION('ref_axis',(1.,0.,0.));
#23506=DIRECTION('center_axis',(0.,0.,-1.));
#23507=DIRECTION('ref_axis',(0.707106781186545,0.70710678118655,0.));
#23508=DIRECTION('center_axis',(0.,0.,1.));
#23509=DIRECTION('ref_axis',(-0.707106781186542,0.707106781186553,0.));
#23510=DIRECTION('',(0.,0.,1.));
#23511=DIRECTION('center_axis',(-0.66436383882992,0.,-0.74740931868366));
#23512=DIRECTION('ref_axis',(0.528498197563227,0.707106781186556,-0.469776175611757));
#23513=DIRECTION('center_axis',(0.,0.,1.));
#23514=DIRECTION('ref_axis',(1.,0.,0.));
#23515=DIRECTION('center_axis',(0.,0.,1.));
#23516=DIRECTION('ref_axis',(1.,0.,0.));
#23517=DIRECTION('center_axis',(0.707106781186547,0.,-0.707106781186548));
#23518=DIRECTION('ref_axis',(0.500000000000006,0.70710678118654,0.500000000000005));
#23519=DIRECTION('center_axis',(0.,1.,0.));
#23520=DIRECTION('ref_axis',(0.923879532511288,0.,0.382683432365087));
#23521=DIRECTION('center_axis',(0.,0.,-1.));
#23522=DIRECTION('ref_axis',(0.707106781186542,0.707106781186553,0.));
#23523=DIRECTION('',(0.,0.,-1.));
#23524=DIRECTION('center_axis',(-0.707106781186548,0.,0.707106781186547));
#23525=DIRECTION('ref_axis',(0.707106781186547,0.,0.707106781186548));
#23526=DIRECTION('center_axis',(-1.,0.,0.));
#23527=DIRECTION('ref_axis',(0.,0.,1.));
#23528=DIRECTION('center_axis',(1.,0.,0.));
#23529=DIRECTION('ref_axis',(0.,0.,-1.));
#23530=DIRECTION('',(0.,1.,0.));
#23531=DIRECTION('center_axis',(0.,1.,0.));
#23532=DIRECTION('ref_axis',(0.923879532511291,0.,0.38268343236508));
#23533=DIRECTION('',(0.,-1.,0.));
#23534=DIRECTION('center_axis',(0.,0.,1.));
#23535=DIRECTION('ref_axis',(1.,0.,0.));
#23536=DIRECTION('center_axis',(7.40148683083437E-15,-1.,-2.06568225806552E-15));
#23537=DIRECTION('ref_axis',(0.268817204301075,-3.31042368671712E-30,0.963191211894998));
#23538=DIRECTION('center_axis',(0.,0.,1.));
#23539=DIRECTION('ref_axis',(1.,0.,0.));
#23540=DIRECTION('center_axis',(0.,0.,1.));
#23541=DIRECTION('ref_axis',(1.,0.,0.));
#23542=DIRECTION('center_axis',(0.,-1.,0.));
#23543=DIRECTION('ref_axis',(1.,0.,0.));
#23544=DIRECTION('center_axis',(0.,0.,-1.));
#23545=DIRECTION('ref_axis',(0.,-1.,0.));
#23546=DIRECTION('center_axis',(0.963191211894997,0.,0.268817204301076));
#23547=DIRECTION('ref_axis',(0.268817204301076,0.,-0.963191211894997));
#23548=DIRECTION('center_axis',(0.,0.,1.));
#23549=DIRECTION('ref_axis',(0.707106781186545,-0.70710678118655,0.));
#23550=DIRECTION('',(0.,0.,1.));
#23551=DIRECTION('center_axis',(0.321470784124458,-0.846950546350565,-0.423475273175289));
#23552=DIRECTION('ref_axis',(-0.512101486820596,-0.531671676917698,0.674594170712776));
#23553=DIRECTION('center_axis',(0.268817204301076,0.,0.963191211894997));
#23554=DIRECTION('ref_axis',(-0.963191211894997,0.,0.268817204301076));
#23555=DIRECTION('center_axis',(-1.,0.,0.));
#23556=DIRECTION('ref_axis',(0.,-0.707106781186551,0.707106781186544));
#23557=DIRECTION('center_axis',(0.,-1.,0.));
#23558=DIRECTION('ref_axis',(-0.604641544925141,0.,0.796497710072376));
#23559=DIRECTION('center_axis',(0.,1.,0.));
#23560=DIRECTION('ref_axis',(-0.707106781186548,0.,-0.707106781186547));
#23561=DIRECTION('center_axis',(0.,1.,0.));
#23562=DIRECTION('ref_axis',(-0.826936230559385,0.,-0.562295714538387));
#23563=DIRECTION('center_axis',(0.,1.,0.));
#23564=DIRECTION('ref_axis',(0.796497710072379,0.,-0.604641544925138));
#23565=DIRECTION('center_axis',(0.,-1.,0.));
#23566=DIRECTION('ref_axis',(0.268817204301076,0.,-0.963191211894997));
#23567=DIRECTION('',(0.,-1.,0.));
#23568=DIRECTION('',(0.,1.,0.));
#23569=DIRECTION('center_axis',(0.,0.,1.));
#23570=DIRECTION('ref_axis',(1.,0.,0.));
#23571=DIRECTION('center_axis',(0.963191211894997,0.,0.268817204301076));
#23572=DIRECTION('ref_axis',(-0.268817204301076,0.,0.963191211894997));
#23573=DIRECTION('center_axis',(0.,0.,-1.));
#23574=DIRECTION('ref_axis',(0.707106781186544,0.707106781186551,0.));
#23575=DIRECTION('center_axis',(0.,0.,1.));
#23576=DIRECTION('ref_axis',(1.,0.,0.));
#23577=DIRECTION('center_axis',(0.,1.,0.));
#23578=DIRECTION('ref_axis',(0.268817204301075,0.,0.963191211894998));
#23579=DIRECTION('center_axis',(0.,0.,1.));
#23580=DIRECTION('ref_axis',(0.707106781186544,0.707106781186551,0.));
#23581=DIRECTION('center_axis',(0.963191211894997,0.,-0.268817204301076));
#23582=DIRECTION('ref_axis',(-0.268817204301076,0.,-0.963191211894997));
#23583=DIRECTION('center_axis',(0.,-1.,0.));
#23584=DIRECTION('ref_axis',(0.796497710072376,0.,0.60464154492514));
#23585=DIRECTION('',(0.,-1.,0.));
#23586=DIRECTION('',(0.,1.,0.));
#23587=DIRECTION('center_axis',(-0.321470784124459,-0.846950546350567,-0.423475273175284));
#23588=DIRECTION('ref_axis',(-0.512101486820597,0.531671676917699,-0.674594170712774));
#23589=DIRECTION('center_axis',(0.268817204301076,0.,-0.963191211894997));
#23590=DIRECTION('ref_axis',(0.963191211894997,0.,0.268817204301076));
#23591=DIRECTION('center_axis',(0.,1.,0.));
#23592=DIRECTION('ref_axis',(-0.707106781186547,0.,0.707106781186547));
#23593=DIRECTION('center_axis',(0.,-1.,0.));
#23594=DIRECTION('ref_axis',(-0.707106781186547,0.,0.707106781186547));
#23595=DIRECTION('center_axis',(0.,-1.,0.));
#23596=DIRECTION('ref_axis',(-0.707106781186547,0.,0.707106781186548));
#23597=DIRECTION('center_axis',(0.,0.,1.));
#23598=DIRECTION('ref_axis',(1.,0.,0.));
#23599=DIRECTION('center_axis',(0.,1.,0.));
#23600=DIRECTION('ref_axis',(-0.268817204301076,0.,-0.963191211894997));
#23601=DIRECTION('center_axis',(-0.963191211894997,0.,0.268817204301077));
#23602=DIRECTION('ref_axis',(0.268817204301077,0.,0.963191211894997));
#23603=DIRECTION('center_axis',(0.,-1.,0.));
#23604=DIRECTION('ref_axis',(-0.796497710072374,0.,-0.604641544925143));
#23605=DIRECTION('',(0.,-1.,0.));
#23606=DIRECTION('center_axis',(0.,1.,0.));
#23607=DIRECTION('ref_axis',(0.707106781186548,0.,-0.707106781186547));
#23608=DIRECTION('center_axis',(0.,1.,0.));
#23609=DIRECTION('ref_axis',(0.826936230559386,0.,-0.562295714538385));
#23610=DIRECTION('center_axis',(0.268817204301074,0.,-0.963191211894998));
#23611=DIRECTION('ref_axis',(0.963191211894998,0.,0.268817204301074));
#23612=DIRECTION('center_axis',(-0.321470784124458,-0.846950546350565,-0.423475273175289));
#23613=DIRECTION('ref_axis',(0.512101486820605,-0.531671676917701,0.674594170712767));
#23614=DIRECTION('center_axis',(0.,-1.,0.));
#23615=DIRECTION('ref_axis',(0.604641544925144,0.,0.796497710072374));
#23616=DIRECTION('center_axis',(1.,0.,0.));
#23617=DIRECTION('ref_axis',(0.,-0.707106781186551,0.707106781186544));
#23618=DIRECTION('center_axis',(0.,-1.,0.));
#23619=DIRECTION('ref_axis',(0.,0.,-1.));
#23620=DIRECTION('center_axis',(-0.268817204301076,0.,0.963191211894997));
#23621=DIRECTION('ref_axis',(-0.963191211894997,0.,-0.268817204301076));
#23622=DIRECTION('center_axis',(0.,-1.,0.));
#23623=DIRECTION('ref_axis',(0.707106781186547,0.,-0.707106781186547));
#23624=DIRECTION('center_axis',(-0.321470784124458,-0.846950546350565,0.423475273175289));
#23625=DIRECTION('ref_axis',(-0.512101486820596,0.531671676917698,0.674594170712776));
#23626=DIRECTION('center_axis',(0.,1.,0.));
#23627=DIRECTION('ref_axis',(-0.963191211894998,0.,0.268817204301075));
#23628=DIRECTION('center_axis',(-1.,0.,0.));
#23629=DIRECTION('ref_axis',(0.,0.707106781186551,0.707106781186544));
#23630=DIRECTION('center_axis',(0.268817204301076,0.,0.963191211894997));
#23631=DIRECTION('ref_axis',(0.963191211894997,0.,-0.268817204301076));
#23632=DIRECTION('center_axis',(0.,-1.,0.));
#23633=DIRECTION('ref_axis',(-0.60464154492514,0.,0.796497710072376));
#23634=DIRECTION('',(0.,1.,0.));
#23635=DIRECTION('',(0.,-1.,0.));
#23636=DIRECTION('center_axis',(-1.,0.,0.));
#23637=DIRECTION('ref_axis',(0.,-0.707106781186553,0.707106781186542));
#23638=DIRECTION('',(-1.,0.,0.));
#23639=DIRECTION('center_axis',(0.,1.,0.));
#23640=DIRECTION('ref_axis',(0.604641544925143,0.,0.796497710072374));
#23641=DIRECTION('',(0.,1.,0.));
#23642=DIRECTION('center_axis',(0.,-1.,0.));
#23643=DIRECTION('ref_axis',(0.963191211894998,0.,0.268817204301074));
#23644=DIRECTION('',(0.,-1.,0.));
#23645=DIRECTION('center_axis',(0.32147078412446,-0.84695054635057,0.423475273175279));
#23646=DIRECTION('ref_axis',(0.512101486820602,0.531671676917693,0.674594170712776));
#23647=DIRECTION('center_axis',(1.,0.,0.));
#23648=DIRECTION('ref_axis',(0.,0.707106781186551,0.707106781186544));
#23649=DIRECTION('center_axis',(0.,0.,-1.));
#23650=DIRECTION('ref_axis',(-1.,0.,0.));
#23651=DIRECTION('',(1.,0.,0.));
#23652=DIRECTION('center_axis',(0.,1.,0.));
#23653=DIRECTION('ref_axis',(1.,0.,0.));
#23654=DIRECTION('center_axis',(0.707106781186548,0.,-0.707106781186547));
#23655=DIRECTION('ref_axis',(0.499999999999998,0.707106781186551,0.499999999999998));
#23656=DIRECTION('center_axis',(-0.707106781186548,0.,0.707106781186548));
#23657=DIRECTION('ref_axis',(0.707106781186547,0.,0.707106781186547));
#23658=DIRECTION('',(0.707106781186548,0.,-0.707106781186547));
#23659=DIRECTION('center_axis',(0.,0.,1.));
#23660=DIRECTION('ref_axis',(1.,0.,0.));
#23661=DIRECTION('center_axis',(0.,-1.,0.));
#23662=DIRECTION('ref_axis',(-1.,0.,0.));
#23663=DIRECTION('center_axis',(-3.70074341541718E-15,0.,1.));
#23664=DIRECTION('ref_axis',(0.,-1.,0.));
#23665=DIRECTION('center_axis',(-0.707106781186548,-2.61682076447296E-15,
-0.707106781186548));
#23666=DIRECTION('ref_axis',(-0.707106781186547,-1.53081335547773E-32,0.707106781186547));
#23667=DIRECTION('center_axis',(0.,1.,0.));
#23668=DIRECTION('ref_axis',(1.01064309961486E-15,0.,-1.));
#23669=DIRECTION('center_axis',(0.,0.,-1.));
#23670=DIRECTION('ref_axis',(0.,-1.,0.));
#23671=DIRECTION('center_axis',(0.,1.,0.));
#23672=DIRECTION('ref_axis',(6.46422633350345E-16,0.,-1.));
#23673=DIRECTION('center_axis',(0.,0.,1.));
#23674=DIRECTION('ref_axis',(-0.70710678118655,-0.707106781186545,0.));
#23675=DIRECTION('',(0.,0.,-1.));
#23676=DIRECTION('center_axis',(0.707106781186548,0.,0.707106781186547));
#23677=DIRECTION('ref_axis',(-0.500000000000001,-0.707106781186545,0.500000000000002));
#23678=DIRECTION('',(-0.707106781186548,0.,-0.707106781186547));
#23679=DIRECTION('center_axis',(-0.382683432365088,0.,-0.923879532511288));
#23680=DIRECTION('ref_axis',(-0.923879532511288,0.,0.382683432365088));
#23681=DIRECTION('center_axis',(0.408248290463864,-0.816496580927728,-0.408248290463858));
#23682=DIRECTION('ref_axis',(-0.577350269189628,-0.577350269189628,0.577350269189622));
#23683=DIRECTION('center_axis',(0.,-1.,0.));
#23684=DIRECTION('ref_axis',(-1.,0.,0.));
#23685=DIRECTION('center_axis',(0.,0.,1.));
#23686=DIRECTION('ref_axis',(0.,-1.,0.));
#23687=DIRECTION('center_axis',(-1.,0.,0.));
#23688=DIRECTION('ref_axis',(0.,0.,1.));
#23689=DIRECTION('center_axis',(0.,0.,1.));
#23690=DIRECTION('ref_axis',(-0.70710678118655,-0.707106781186545,0.));
#23691=DIRECTION('',(0.,0.,-1.));
#23692=DIRECTION('center_axis',(1.,0.,0.));
#23693=DIRECTION('ref_axis',(0.,-0.707106781186547,0.707106781186547));
#23694=DIRECTION('',(-1.,0.,0.));
#23695=DIRECTION('center_axis',(-0.707106781186548,0.,-0.707106781186548));
#23696=DIRECTION('ref_axis',(-0.707106781186548,0.,0.707106781186548));
#23697=DIRECTION('center_axis',(0.,0.,1.));
#23698=DIRECTION('ref_axis',(-0.70710678118655,-0.707106781186545,0.));
#23699=DIRECTION('center_axis',(0.707106781186548,0.,-0.707106781186548));
#23700=DIRECTION('ref_axis',(-0.707106781186548,0.,-0.707106781186548));
#23701=DIRECTION('',(0.,0.,-1.));
#23702=DIRECTION('center_axis',(0.408248290463864,-0.816496580927728,0.408248290463858));
#23703=DIRECTION('ref_axis',(-0.577350269189628,-0.577350269189628,-0.577350269189622));
#23704=DIRECTION('center_axis',(0.,-1.,0.));
#23705=DIRECTION('ref_axis',(0.,0.,-1.));
#23706=DIRECTION('center_axis',(-1.,0.,0.));
#23707=DIRECTION('ref_axis',(0.,-1.,0.));
#23708=DIRECTION('center_axis',(0.,0.,-1.));
#23709=DIRECTION('ref_axis',(-1.,0.,0.));
#23710=DIRECTION('center_axis',(-1.,0.,0.));
#23711=DIRECTION('ref_axis',(0.,-0.707106781186542,-0.707106781186553));
#23712=DIRECTION('',(1.,0.,0.));
#23713=DIRECTION('center_axis',(-0.816496580927727,0.408248290463865,-0.408248290463859));
#23714=DIRECTION('ref_axis',(-0.577350269189626,-0.577350269189629,0.577350269189623));
#23715=DIRECTION('center_axis',(0.,-1.,0.));
#23716=DIRECTION('ref_axis',(-1.,0.,0.));
#23717=DIRECTION('center_axis',(0.,0.,1.));
#23718=DIRECTION('ref_axis',(0.,-1.,0.));
#23719=DIRECTION('center_axis',(-1.,0.,0.));
#23720=DIRECTION('ref_axis',(0.,0.,1.));
#23721=DIRECTION('center_axis',(0.,0.,1.));
#23722=DIRECTION('ref_axis',(-0.70710678118655,-0.707106781186545,0.));
#23723=DIRECTION('',(0.,0.,-1.));
#23724=DIRECTION('center_axis',(-0.182143211721535,-0.879465224064607,-0.439732612032306));
#23725=DIRECTION('ref_axis',(0.33655677059079,-0.475963149477972,0.812519920068738));
#23726=DIRECTION('center_axis',(0.,-1.,0.));
#23727=DIRECTION('ref_axis',(0.,0.,1.));
#23728=DIRECTION('center_axis',(1.,0.,-7.40148683083442E-15));
#23729=DIRECTION('ref_axis',(0.,-1.,0.));
#23730=DIRECTION('center_axis',(-0.707106781186544,0.,0.707106781186551));
#23731=DIRECTION('ref_axis',(0.707106781186551,0.,0.707106781186544));
#23732=DIRECTION('center_axis',(1.,0.,0.));
#23733=DIRECTION('ref_axis',(0.,-0.707106781186542,0.707106781186553));
#23734=DIRECTION('',(-1.,0.,0.));
#23735=DIRECTION('center_axis',(0.707106781186547,0.,-0.707106781186548));
#23736=DIRECTION('ref_axis',(0.500000000000005,-0.70710678118654,0.500000000000005));
#23737=DIRECTION('',(-0.707106781186547,0.,0.707106781186548));
#23738=DIRECTION('center_axis',(0.,1.,0.));
#23739=DIRECTION('ref_axis',(0.38268343236509,0.,0.923879532511287));
#23740=DIRECTION('center_axis',(0.,-1.,0.));
#23741=DIRECTION('ref_axis',(0.707106781186551,0.,0.707106781186544));
#23742=DIRECTION('',(0.,-1.,0.));
#23743=DIRECTION('',(0.,1.,0.));
#23744=DIRECTION('center_axis',(0.707106781186547,0.,-0.707106781186548));
#23745=DIRECTION('ref_axis',(0.500000000000002,0.707106781186545,0.500000000000001));
#23746=DIRECTION('center_axis',(0.707106781186544,0.,-0.707106781186551));
#23747=DIRECTION('ref_axis',(0.,1.,0.));
#23748=DIRECTION('',(0.707106781186547,0.,-0.707106781186548));
#23749=DIRECTION('center_axis',(0.,1.,0.));
#23750=DIRECTION('ref_axis',(-0.707106781186545,0.,0.70710678118655));
#23751=DIRECTION('center_axis',(0.,-1.,0.));
#23752=DIRECTION('ref_axis',(0.,0.,1.));
#23753=DIRECTION('',(0.,-1.,0.));
#23754=DIRECTION('',(0.,1.,0.));
#23755=DIRECTION('center_axis',(-0.816496580927726,-0.408248290463866,-0.40824829046386));
#23756=DIRECTION('ref_axis',(-0.577350269189626,0.577350269189629,0.577350269189623));
#23757=DIRECTION('center_axis',(-1.,0.,0.));
#23758=DIRECTION('ref_axis',(0.,0.707106781186551,0.707106781186544));
#23759=DIRECTION('center_axis',(0.,0.,1.));
#23760=DIRECTION('ref_axis',(-0.707106781186544,0.707106781186551,0.));
#23761=DIRECTION('center_axis',(0.,1.,0.));
#23762=DIRECTION('ref_axis',(-0.707106781186545,0.,-0.70710678118655));
#23763=DIRECTION('center_axis',(0.,-1.,0.));
#23764=DIRECTION('ref_axis',(-1.,0.,0.));
#23765=DIRECTION('',(0.,-1.,0.));
#23766=DIRECTION('',(0.,1.,0.));
#23767=DIRECTION('center_axis',(-0.408248290463864,-0.816496580927727,-0.408248290463861));
#23768=DIRECTION('ref_axis',(-0.57735026918963,0.577350269189624,-0.577350269189624));
#23769=DIRECTION('center_axis',(0.,0.,-1.));
#23770=DIRECTION('ref_axis',(-0.707106781186544,0.707106781186551,0.));
#23771=DIRECTION('center_axis',(-1.,0.,0.));
#23772=DIRECTION('ref_axis',(0.,0.707106781186547,-0.707106781186547));
#23773=DIRECTION('center_axis',(0.,1.,0.));
#23774=DIRECTION('ref_axis',(-0.70710678118655,0.,0.707106781186545));
#23775=DIRECTION('center_axis',(0.,-1.,0.));
#23776=DIRECTION('ref_axis',(0.,0.,1.));
#23777=DIRECTION('',(0.,-1.,0.));
#23778=DIRECTION('',(0.,1.,0.));
#23779=DIRECTION('center_axis',(-0.408248290463864,-0.816496580927727,0.408248290463861));
#23780=DIRECTION('ref_axis',(-0.57735026918963,0.577350269189624,0.577350269189624));
#23781=DIRECTION('center_axis',(-1.,0.,0.));
#23782=DIRECTION('ref_axis',(0.,0.707106781186551,0.707106781186544));
#23783=DIRECTION('center_axis',(0.,0.,1.));
#23784=DIRECTION('ref_axis',(-0.707106781186544,0.707106781186551,0.));
#23785=DIRECTION('center_axis',(0.,1.,0.));
#23786=DIRECTION('ref_axis',(-0.923879532511286,0.,0.382683432365091));
#23787=DIRECTION('center_axis',(0.,-1.,0.));
#23788=DIRECTION('ref_axis',(-0.707106781186547,0.,0.707106781186547));
#23789=DIRECTION('',(0.,-1.,0.));
#23790=DIRECTION('',(0.,1.,0.));
#23791=DIRECTION('center_axis',(0.,0.,1.));
#23792=DIRECTION('ref_axis',(1.,0.,0.));
#23793=DIRECTION('center_axis',(-0.707106781186548,0.,-0.707106781186547));
#23794=DIRECTION('ref_axis',(-0.499999999999997,0.707106781186552,0.499999999999998));
#23795=DIRECTION('center_axis',(0.,0.,1.));
#23796=DIRECTION('ref_axis',(-0.707106781186545,0.70710678118655,0.));
#23797=DIRECTION('center_axis',(0.,1.,0.));
#23798=DIRECTION('ref_axis',(0.923879532511287,0.,0.382683432365088));
#23799=DIRECTION('',(0.,1.,0.));
#23800=DIRECTION('center_axis',(0.,-1.,0.));
#23801=DIRECTION('ref_axis',(1.,0.,0.));
#23802=DIRECTION('',(0.,-1.,0.));
#23803=DIRECTION('center_axis',(0.182143211721524,-0.879465224064608,0.43973261203231));
#23804=DIRECTION('ref_axis',(0.33655677059078,0.475963149477969,0.812519920068744));
#23805=DIRECTION('center_axis',(1.,0.,0.));
#23806=DIRECTION('ref_axis',(0.,0.707106781186551,0.707106781186544));
#23807=DIRECTION('center_axis',(0.,0.,1.));
#23808=DIRECTION('ref_axis',(1.,0.,0.));
#23809=DIRECTION('center_axis',(0.,0.,1.));
#23810=DIRECTION('ref_axis',(0.707106781186545,0.70710678118655,0.));
#23811=DIRECTION('center_axis',(0.,0.,1.));
#23812=DIRECTION('ref_axis',(-0.707106781186545,0.70710678118655,0.));
#23813=DIRECTION('center_axis',(0.,0.,-1.));
#23814=DIRECTION('ref_axis',(-1.,0.,0.));
#23815=DIRECTION('',(0.,0.,1.));
#23816=DIRECTION('center_axis',(0.707106781186548,0.,0.707106781186547));
#23817=DIRECTION('ref_axis',(-0.499999999999998,0.707106781186551,0.499999999999998));
#23818=DIRECTION('',(0.707106781186548,0.,0.707106781186547));
#23819=DIRECTION('center_axis',(0.382683432365088,0.,0.923879532511288));
#23820=DIRECTION('ref_axis',(0.923879532511288,0.,-0.382683432365088));
#23821=DIRECTION('center_axis',(-0.707106781186547,0.,0.707106781186548));
#23822=DIRECTION('ref_axis',(0.707106781186548,0.,0.707106781186547));
#23823=DIRECTION('',(0.,1.,0.));
#23824=DIRECTION('center_axis',(-1.,0.,0.));
#23825=DIRECTION('ref_axis',(0.,0.,1.));
#23826=DIRECTION('',(0.,0.,1.));
#23827=DIRECTION('center_axis',(0.,0.,1.));
#23828=DIRECTION('ref_axis',(-0.707106781186545,0.70710678118655,0.));
#23829=DIRECTION('center_axis',(1.,0.,0.));
#23830=DIRECTION('ref_axis',(0.,0.707106781186553,0.707106781186542));
#23831=DIRECTION('',(1.,0.,0.));
#23832=DIRECTION('center_axis',(0.707106781186548,0.,0.707106781186548));
#23833=DIRECTION('ref_axis',(0.707106781186548,0.,-0.707106781186548));
#23834=DIRECTION('center_axis',(0.,0.,1.));
#23835=DIRECTION('ref_axis',(1.,0.,0.));
#23836=DIRECTION('',(0.,1.,0.));
#23837=DIRECTION('center_axis',(-1.,0.,0.));
#23838=DIRECTION('ref_axis',(0.,0.,1.));
#23839=DIRECTION('',(0.,1.,0.));
#23840=DIRECTION('',(0.,0.,1.));
#23841=DIRECTION('center_axis',(0.,0.,-1.));
#23842=DIRECTION('ref_axis',(-1.,0.,0.));
#23843=DIRECTION('',(-1.,0.,0.));
#23844=DIRECTION('center_axis',(-1.,0.,0.));
#23845=DIRECTION('ref_axis',(0.,0.707106781186547,-0.707106781186547));
#23846=DIRECTION('center_axis',(-0.707106781186548,0.,0.707106781186548));
#23847=DIRECTION('ref_axis',(0.707106781186548,0.,0.707106781186548));
#23848=DIRECTION('center_axis',(-1.,0.,0.));
#23849=DIRECTION('ref_axis',(0.,0.,1.));
#23850=DIRECTION('',(0.,0.,1.));
#23851=DIRECTION('center_axis',(0.,0.,1.));
#23852=DIRECTION('ref_axis',(-0.707106781186545,0.70710678118655,0.));
#23853=DIRECTION('center_axis',(0.,0.,1.));
#23854=DIRECTION('ref_axis',(1.,0.,0.));
#23855=DIRECTION('',(1.,0.,0.));
#23856=DIRECTION('center_axis',(1.,0.,0.));
#23857=DIRECTION('ref_axis',(0.,0.707106781186547,0.707106781186547));
#23858=DIRECTION('center_axis',(0.707106781186548,0.,0.707106781186547));
#23859=DIRECTION('ref_axis',(0.707106781186547,0.,-0.707106781186548));
#23860=DIRECTION('center_axis',(0.,0.,1.));
#23861=DIRECTION('ref_axis',(-0.707106781186545,0.70710678118655,0.));
#23862=DIRECTION('center_axis',(0.,0.,-1.));
#23863=DIRECTION('ref_axis',(0.707106781186545,0.70710678118655,0.));
#23864=DIRECTION('',(0.,0.,-1.));
#23865=DIRECTION('center_axis',(0.,0.,1.));
#23866=DIRECTION('ref_axis',(1.,0.,0.));
#23867=DIRECTION('center_axis',(0.,-1.,0.));
#23868=DIRECTION('ref_axis',(0.,0.,-1.));
#23869=DIRECTION('center_axis',(0.,-1.,0.));
#23870=DIRECTION('ref_axis',(6.46422633350345E-16,0.,-1.));
#23871=DIRECTION('center_axis',(-1.,0.,0.));
#23872=DIRECTION('ref_axis',(0.,0.,1.));
#23873=DIRECTION('',(0.,1.,0.));
#23874=DIRECTION('center_axis',(0.,1.,0.));
#23875=DIRECTION('ref_axis',(1.,0.,5.85190293392977E-16));
#23876=DIRECTION('',(0.,1.,0.));
#23877=DIRECTION('center_axis',(1.,0.,0.));
#23878=DIRECTION('ref_axis',(0.,0.,-1.));
#23879=DIRECTION('center_axis',(1.,0.,0.));
#23880=DIRECTION('ref_axis',(0.,0.707106781186553,0.707106781186542));
#23881=DIRECTION('center_axis',(0.,-1.,0.));
#23882=DIRECTION('ref_axis',(0.,0.,-1.));
#23883=DIRECTION('center_axis',(0.,-1.,0.));
#23884=DIRECTION('ref_axis',(-0.707106781186547,0.,-0.707106781186548));
#23885=DIRECTION('center_axis',(0.,0.,-1.));
#23886=DIRECTION('ref_axis',(0.707106781186545,0.70710678118655,0.));
#23887=DIRECTION('',(0.,0.,-1.));
#23888=DIRECTION('center_axis',(0.,1.,0.));
#23889=DIRECTION('ref_axis',(-0.707106781186547,0.,-0.707106781186547));
#23890=DIRECTION('center_axis',(-1.,0.,0.));
#23891=DIRECTION('ref_axis',(0.,0.,1.));
#23892=DIRECTION('center_axis',(0.,-1.,0.));
#23893=DIRECTION('ref_axis',(0.,0.,-1.));
#23894=DIRECTION('center_axis',(-1.,0.,0.));
#23895=DIRECTION('ref_axis',(0.,0.,1.));
#23896=DIRECTION('center_axis',(0.,0.,1.));
#23897=DIRECTION('ref_axis',(-0.707106781186544,0.707106781186551,0.));
#23898=DIRECTION('center_axis',(0.,0.,1.));
#23899=DIRECTION('ref_axis',(0.,1.,0.));
#23900=DIRECTION('center_axis',(0.,0.,-1.));
#23901=DIRECTION('ref_axis',(-1.,0.,0.));
#23902=DIRECTION('center_axis',(0.,-1.,0.));
#23903=DIRECTION('ref_axis',(1.65389215948551E-15,0.,1.));
#23904=DIRECTION('center_axis',(0.,0.,1.));
#23905=DIRECTION('ref_axis',(1.,0.,0.));
#23906=DIRECTION('center_axis',(0.,-1.,0.));
#23907=DIRECTION('ref_axis',(1.49370186820111E-15,0.,1.));
#23908=DIRECTION('center_axis',(0.,0.,-1.));
#23909=DIRECTION('ref_axis',(0.707106781186544,0.707106781186551,0.));
#23910=DIRECTION('center_axis',(0.,0.,1.));
#23911=DIRECTION('ref_axis',(1.,0.,0.));
#23912=DIRECTION('',(0.,0.,-1.));
#23913=DIRECTION('center_axis',(0.,-1.,0.));
#23914=DIRECTION('ref_axis',(0.,0.,-1.));
#23915=DIRECTION('center_axis',(0.,1.,0.));
#23916=DIRECTION('ref_axis',(-1.,0.,1.55493420815848E-15));
#23917=DIRECTION('',(0.,1.,0.));
#23918=DIRECTION('center_axis',(0.,1.,0.));
#23919=DIRECTION('ref_axis',(0.,0.,1.));
#23920=DIRECTION('center_axis',(-1.,0.,0.));
#23921=DIRECTION('ref_axis',(0.,0.,-1.));
#23922=DIRECTION('center_axis',(0.,1.,0.));
#23923=DIRECTION('ref_axis',(0.,0.,1.));
#23924=DIRECTION('center_axis',(0.,-1.,0.));
#23925=DIRECTION('ref_axis',(1.,0.,0.));
#23926=DIRECTION('center_axis',(-1.,0.,0.));
#23927=DIRECTION('ref_axis',(0.,0.,-1.));
#23928=DIRECTION('center_axis',(0.,-1.,0.));
#23929=DIRECTION('ref_axis',(1.,0.,0.));
#23930=DIRECTION('center_axis',(0.,1.,0.));
#23931=DIRECTION('ref_axis',(1.,0.,0.));
#23932=DIRECTION('center_axis',(0.,1.,1.15415719212674E-15));
#23933=DIRECTION('ref_axis',(1.,0.,0.));
#23934=DIRECTION('center_axis',(0.,1.,1.15415719212674E-15));
#23935=DIRECTION('ref_axis',(1.,0.,0.));
#23936=DIRECTION('',(-0.707106781186547,0.707106781186548,8.65956056235493E-17));
#23937=DIRECTION('center_axis',(0.,-1.,0.));
#23938=DIRECTION('ref_axis',(0.,0.,-1.));
#23939=DIRECTION('center_axis',(-1.,0.,0.));
#23940=DIRECTION('ref_axis',(0.,0.,1.));
#23941=DIRECTION('center_axis',(-1.,0.,0.));
#23942=DIRECTION('ref_axis',(0.,0.,1.));
#23943=DIRECTION('center_axis',(0.707106781186547,0.,0.707106781186548));
#23944=DIRECTION('ref_axis',(0.707106781186548,0.,-0.707106781186547));
#23945=DIRECTION('axis',(0.,0.,1.));
#23946=DIRECTION('refdir',(1.,0.,0.));
#23947=DIRECTION('center_axis',(0.,1.,0.));
#23948=DIRECTION('ref_axis',(-0.707106781186548,0.,0.707106781186548));
#23949=DIRECTION('',(0.,-1.,0.));
#23950=DIRECTION('center_axis',(0.,0.707106781186548,-0.707106781186548));
#23951=DIRECTION('ref_axis',(0.,-0.707106781186548,-0.707106781186548));
#23952=DIRECTION('',(0.,1.,0.));
#23953=DIRECTION('center_axis',(0.,-0.707106781186548,-0.707106781186548));
#23954=DIRECTION('ref_axis',(0.,-0.707106781186548,0.707106781186548));
#23955=DIRECTION('center_axis',(0.,0.,-1.));
#23956=DIRECTION('ref_axis',(-0.707106781186548,0.707106781186548,0.));
#23957=DIRECTION('',(0.,0.,-1.));
#23958=DIRECTION('',(0.,0.,1.));
#23959=DIRECTION('center_axis',(0.,0.707106781186548,0.707106781186548));
#23960=DIRECTION('ref_axis',(0.,0.707106781186548,-0.707106781186548));
#23961=DIRECTION('center_axis',(0.,0.,1.));
#23962=DIRECTION('ref_axis',(-0.707106781186548,-0.707106781186548,0.));
#23963=DIRECTION('',(0.,0.,-1.));
#23964=DIRECTION('',(0.,0.,1.));
#23965=DIRECTION('center_axis',(0.,0.707106781186548,-0.707106781186548));
#23966=DIRECTION('ref_axis',(0.,-0.707106781186548,-0.707106781186548));
#23967=DIRECTION('center_axis',(0.,-1.,0.));
#23968=DIRECTION('ref_axis',(-0.70710678118654,0.,-0.707106781186555));
#23969=DIRECTION('',(0.,1.,0.));
#23970=DIRECTION('',(0.,-1.,0.));
#23971=DIRECTION('center_axis',(0.,1.,0.));
#23972=DIRECTION('ref_axis',(0.,0.,-1.));
#23973=DIRECTION('',(-1.,0.,0.));
#23974=DIRECTION('',(0.,0.,-1.));
#23975=DIRECTION('',(-1.,0.,0.));
#23976=DIRECTION('center_axis',(0.,0.,-1.));
#23977=DIRECTION('ref_axis',(0.,-1.,0.));
#23978=DIRECTION('',(-1.,0.,0.));
#23979=DIRECTION('',(0.,-1.,0.));
#23980=DIRECTION('center_axis',(-1.,0.,0.));
#23981=DIRECTION('ref_axis',(0.,0.,1.));
#23982=DIRECTION('',(0.,0.985211754819674,-0.171341174751248));
#23983=DIRECTION('center_axis',(1.,0.,0.));
#23984=DIRECTION('ref_axis',(0.,6.13317366673349E-17,-1.));
#23985=DIRECTION('',(0.,1.,0.));
#23986=DIRECTION('',(0.,0.,-1.));
#23987=DIRECTION('',(0.,-1.,0.));
#23988=DIRECTION('',(0.,0.,-1.));
#23989=DIRECTION('center_axis',(0.,0.985211754819675,-0.171341174751248));
#23990=DIRECTION('ref_axis',(-0.707106781186549,-0.121156506563076,-0.696649912737688));
#23991=DIRECTION('center_axis',(0.,1.,0.));
#23992=DIRECTION('ref_axis',(2.13633744986749E-15,0.,-1.));
#23993=DIRECTION('',(0.,-0.985211754819674,0.171341174751248));
#23994=DIRECTION('center_axis',(0.,1.,0.));
#23995=DIRECTION('ref_axis',(0.70710678118654,0.,-0.707106781186555));
#23996=DIRECTION('',(0.,-1.,0.));
#23997=DIRECTION('center_axis',(0.,0.707106781186548,0.707106781186548));
#23998=DIRECTION('ref_axis',(0.,-0.707106781186548,0.707106781186548));
#23999=DIRECTION('',(0.,1.,0.));
#24000=DIRECTION('center_axis',(0.,0.707106781186548,-0.707106781186548));
#24001=DIRECTION('ref_axis',(0.,0.707106781186548,0.707106781186548));
#24002=DIRECTION('center_axis',(0.,-1.,0.));
#24003=DIRECTION('ref_axis',(0.707106781186548,0.,0.707106781186548));
#24004=DIRECTION('',(0.,1.,0.));
#24005=DIRECTION('center_axis',(0.,-0.707106781186548,-0.707106781186548));
#24006=DIRECTION('ref_axis',(0.,0.707106781186548,-0.707106781186548));
#24007=DIRECTION('center_axis',(0.,0.707106781186548,-0.707106781186548));
#24008=DIRECTION('ref_axis',(0.,0.707106781186548,0.707106781186548));
#24009=DIRECTION('center_axis',(0.,0.,-1.));
#24010=DIRECTION('ref_axis',(0.707106781186548,-0.707106781186548,0.));
#24011=DIRECTION('',(0.,0.,1.));
#24012=DIRECTION('center_axis',(0.,0.,1.));
#24013=DIRECTION('ref_axis',(0.707106781186548,0.707106781186548,0.));
#24014=DIRECTION('',(0.,0.,-1.));
#24015=DIRECTION('',(0.,0.,1.));
#24016=DIRECTION('center_axis',(0.,-1.,0.));
#24017=DIRECTION('ref_axis',(0.,0.,1.));
#24018=DIRECTION('',(-1.,0.,0.));
#24019=DIRECTION('center_axis',(1.,0.,0.));
#24020=DIRECTION('ref_axis',(0.,0.,-1.));
#24021=DIRECTION('',(0.,-0.985211754819674,0.171341174751248));
#24022=DIRECTION('',(0.,0.,1.));
#24023=DIRECTION('',(0.,1.,0.));
#24024=DIRECTION('',(0.,0.,-1.));
#24025=DIRECTION('',(0.,1.,0.));
#24026=DIRECTION('',(0.,0.,1.));
#24027=DIRECTION('center_axis',(0.,0.985211754819675,-0.171341174751248));
#24028=DIRECTION('ref_axis',(0.707106781186549,-0.121156506563076,-0.696649912737688));
#24029=DIRECTION('center_axis',(0.,0.64368424916598,-0.76529117816399));
#24030=DIRECTION('ref_axis',(-1.99135285907852E-16,-0.76529117816399,-0.64368424916598));
#24031=DIRECTION('center_axis',(0.,-1.,0.));
#24032=DIRECTION('ref_axis',(-2.13633744986749E-15,0.,-1.));
#24033=DIRECTION('',(0.,0.985211754819674,-0.171341174751248));
#24034=DIRECTION('center_axis',(0.,-0.985211754819675,0.171341174751248));
#24035=DIRECTION('ref_axis',(0.707106781186549,-0.121156506563076,-0.696649912737688));
#24036=DIRECTION('',(0.,0.985211754819674,-0.171341174751248));
#24037=DIRECTION('center_axis',(0.,1.,0.));
#24038=DIRECTION('ref_axis',(-1.96543045387809E-15,0.,-1.));
#24039=DIRECTION('',(0.,-0.985211754819674,0.171341174751248));
#24040=DIRECTION('center_axis',(0.,-0.171341174751248,-0.985211754819675));
#24041=DIRECTION('ref_axis',(0.,0.985211754819675,-0.171341174751248));
#24042=DIRECTION('center_axis',(0.,0.171341174751248,0.985211754819675));
#24043=DIRECTION('ref_axis',(0.985636596769451,-0.166382691564751,0.0289361202721306));
#24044=DIRECTION('',(1.,0.,0.));
#24045=DIRECTION('',(0.,-0.985211754819674,0.171341174751248));
#24046=DIRECTION('',(1.,0.,0.));
#24047=DIRECTION('center_axis',(0.,1.,0.));
#24048=DIRECTION('ref_axis',(0.70710678118654,0.,-0.707106781186555));
#24049=DIRECTION('',(0.,-1.,0.));
#24050=DIRECTION('center_axis',(0.,0.707106781186548,0.707106781186548));
#24051=DIRECTION('ref_axis',(0.,-0.707106781186548,0.707106781186548));
#24052=DIRECTION('',(0.,1.,0.));
#24053=DIRECTION('center_axis',(0.,-0.707106781186548,0.707106781186548));
#24054=DIRECTION('ref_axis',(0.,-0.707106781186548,-0.707106781186548));
#24055=DIRECTION('center_axis',(0.,0.,1.));
#24056=DIRECTION('ref_axis',(0.707106781186548,0.707106781186548,0.));
#24057=DIRECTION('',(0.,0.,1.));
#24058=DIRECTION('',(0.,0.,-1.));
#24059=DIRECTION('center_axis',(0.,0.707106781186548,-0.707106781186548));
#24060=DIRECTION('ref_axis',(0.,0.707106781186548,0.707106781186548));
#24061=DIRECTION('center_axis',(0.,0.,-1.));
#24062=DIRECTION('ref_axis',(0.707106781186548,-0.707106781186548,0.));
#24063=DIRECTION('',(0.,0.,1.));
#24064=DIRECTION('',(0.,0.,-1.));
#24065=DIRECTION('center_axis',(0.,0.707106781186548,0.707106781186548));
#24066=DIRECTION('ref_axis',(0.,-0.707106781186548,0.707106781186548));
#24067=DIRECTION('center_axis',(0.,-1.,0.));
#24068=DIRECTION('ref_axis',(0.707106781186548,0.,0.707106781186548));
#24069=DIRECTION('',(0.,1.,0.));
#24070=DIRECTION('',(0.,-1.,0.));
#24071=DIRECTION('center_axis',(0.,1.,0.));
#24072=DIRECTION('ref_axis',(0.,0.,1.));
#24073=DIRECTION('',(1.,0.,0.));
#24074=DIRECTION('',(0.,0.,1.));
#24075=DIRECTION('',(1.,0.,0.));
#24076=DIRECTION('center_axis',(0.,0.,1.));
#24077=DIRECTION('ref_axis',(0.,-1.,0.));
#24078=DIRECTION('',(1.,0.,0.));
#24079=DIRECTION('',(0.,-1.,0.));
#24080=DIRECTION('center_axis',(1.,0.,0.));
#24081=DIRECTION('ref_axis',(0.,0.,-1.));
#24082=DIRECTION('',(0.,0.,1.));
#24083=DIRECTION('',(0.,1.,0.));
#24084=DIRECTION('',(0.,0.,1.));
#24085=DIRECTION('',(0.,1.,0.));
#24086=DIRECTION('center_axis',(-1.,0.,0.));
#24087=DIRECTION('ref_axis',(0.,6.13317366673349E-17,-1.));
#24088=DIRECTION('center_axis',(0.40824829046386,-0.816496580927729,0.40824829046386));
#24089=DIRECTION('ref_axis',(0.577350269189632,0.577350269189623,0.577350269189623));
#24090=DIRECTION('center_axis',(0.,1.,0.));
#24091=DIRECTION('ref_axis',(0.,0.,1.));
#24092=DIRECTION('center_axis',(0.,0.,1.));
#24093=DIRECTION('ref_axis',(0.707106781186545,0.70710678118655,0.));
#24094=DIRECTION('center_axis',(1.,0.,0.));
#24095=DIRECTION('ref_axis',(0.,0.707106781186542,0.707106781186553));
#24096=DIRECTION('center_axis',(0.,-1.,0.));
#24097=DIRECTION('ref_axis',(0.70710678118654,0.,0.707106781186555));
#24098=DIRECTION('center_axis',(0.707106781186548,-0.707106781186548,0.));
#24099=DIRECTION('ref_axis',(0.707106781186548,0.707106781186548,0.));
#24100=DIRECTION('',(0.,-1.,0.));
#24101=DIRECTION('center_axis',(0.,0.,1.));
#24102=DIRECTION('ref_axis',(1.,0.,0.));
#24103=DIRECTION('',(1.,0.,0.));
#24104=DIRECTION('',(1.,0.,0.));
#24105=DIRECTION('',(0.,1.,0.));
#24106=DIRECTION('',(-1.,0.,0.));
#24107=DIRECTION('',(0.,1.,0.));
#24108=DIRECTION('',(-1.,0.,0.));
#24109=DIRECTION('',(0.,-1.,0.));
#24110=DIRECTION('',(-1.,0.,0.));
#24111=DIRECTION('',(0.,1.,0.));
#24112=DIRECTION('',(1.,0.,0.));
#24113=DIRECTION('',(0.,1.,0.));
#24114=DIRECTION('center_axis',(1.,0.,0.));
#24115=DIRECTION('ref_axis',(0.,0.70710678118654,0.707106781186555));
#24116=DIRECTION('',(-1.,0.,0.));
#24117=DIRECTION('center_axis',(0.987087457637498,0.,0.160182243006963));
#24118=DIRECTION('ref_axis',(-0.160182243006963,0.,0.987087457637497));
#24119=DIRECTION('center_axis',(0.,0.,-1.));
#24120=DIRECTION('ref_axis',(0.707106781186548,0.707106781186548,0.));
#24121=DIRECTION('center_axis',(-0.707106781186548,0.,-0.707106781186548));
#24122=DIRECTION('ref_axis',(0.707106781186548,0.,-0.707106781186548));
#24123=DIRECTION('',(0.,0.,1.));
#24124=DIRECTION('center_axis',(1.,0.,0.));
#24125=DIRECTION('ref_axis',(0.,-0.70710678118654,0.707106781186555));
#24126=DIRECTION('center_axis',(0.707106781186546,0.707106781186549,0.));
#24127=DIRECTION('ref_axis',(-0.707106781186549,0.707106781186546,0.));
#24128=DIRECTION('',(1.,0.,0.));
#24129=DIRECTION('center_axis',(-0.987087457637496,-2.19177444557571E-14,
0.160182243006974));
#24130=DIRECTION('ref_axis',(-0.160182243006974,1.35063227020986E-13,-0.987087457637496));
#24131=DIRECTION('center_axis',(-0.408248290463859,-0.81649658092773,-0.408248290463859));
#24132=DIRECTION('ref_axis',(0.577350269189621,-0.577350269189618,0.577350269189638));
#24133=DIRECTION('center_axis',(0.,-1.,0.));
#24134=DIRECTION('ref_axis',(1.,0.,0.));
#24135=DIRECTION('center_axis',(1.,0.,0.));
#24136=DIRECTION('ref_axis',(0.,-0.707106781186542,0.707106781186553));
#24137=DIRECTION('center_axis',(0.,0.,1.));
#24138=DIRECTION('ref_axis',(0.707106781186549,-0.707106781186546,0.));
#24139=DIRECTION('center_axis',(0.,1.,0.));
#24140=DIRECTION('ref_axis',(0.707106781186555,0.,0.70710678118654));
#24141=DIRECTION('center_axis',(0.948683298050514,0.,-0.316227766016838));
#24142=DIRECTION('ref_axis',(0.223606797749977,-0.707106781186554,0.670820393249931));
#24143=DIRECTION('',(0.948683298050514,0.,-0.316227766016838));
#24144=DIRECTION('center_axis',(0.987087457637496,0.,-0.160182243006974));
#24145=DIRECTION('ref_axis',(0.160182243006974,3.42464757121206E-15,0.987087457637496));
#24146=DIRECTION('',(-0.948683298050514,0.,0.316227766016838));
#24147=DIRECTION('center_axis',(0.316227766016838,0.,0.948683298050514));
#24148=DIRECTION('ref_axis',(0.948683298050514,0.,-0.316227766016838));
#24149=DIRECTION('',(0.,1.,0.));
#24150=DIRECTION('',(0.948683298050514,0.,-0.316227766016838));
#24151=DIRECTION('center_axis',(0.,0.,1.));
#24152=DIRECTION('ref_axis',(0.707106781186548,-0.707106781186548,0.));
#24153=DIRECTION('',(0.,0.,-1.));
#24154=DIRECTION('center_axis',(0.707106781186548,0.,0.707106781186548));
#24155=DIRECTION('ref_axis',(0.707106781186548,0.,-0.707106781186548));
#24156=DIRECTION('center_axis',(1.,0.,0.));
#24157=DIRECTION('ref_axis',(0.,-0.707106781186548,-0.707106781186548));
#24158=DIRECTION('',(-1.,0.,0.));
#24159=DIRECTION('center_axis',(0.988554494713122,0.,-0.150864213723747));
#24160=DIRECTION('ref_axis',(-0.150864213723747,0.,-0.988554494713122));
#24161=DIRECTION('',(1.,0.,0.));
#24162=DIRECTION('center_axis',(0.95447997803503,0.,-0.298274993135947));
#24163=DIRECTION('ref_axis',(-0.210912270304798,-0.707106781186552,-0.674919264975352));
#24164=DIRECTION('',(-0.95447997803503,0.,0.298274993135947));
#24165=DIRECTION('center_axis',(0.855572029308621,0.,-0.517683786364541));
#24166=DIRECTION('ref_axis',(-0.517683786364541,0.,-0.855572029308621));
#24167=DIRECTION('',(0.95447997803503,0.,-0.298274993135947));
#24168=DIRECTION('center_axis',(-1.,0.,0.));
#24169=DIRECTION('ref_axis',(0.,-0.70710678118654,0.707106781186555));
#24170=DIRECTION('',(-1.,0.,0.));
#24171=DIRECTION('center_axis',(1.,0.,0.));
#24172=DIRECTION('ref_axis',(0.,0.,1.));
#24173=DIRECTION('',(1.,0.,0.));
#24174=DIRECTION('center_axis',(-0.987087457637498,0.,-0.160182243006963));
#24175=DIRECTION('ref_axis',(0.160182243006963,0.,-0.987087457637497));
#24176=DIRECTION('center_axis',(-0.948683298050514,0.,-0.316227766016838));
#24177=DIRECTION('ref_axis',(-0.223606797749977,-0.707106781186554,0.670820393249931));
#24178=DIRECTION('',(0.948683298050514,0.,0.316227766016838));
#24179=DIRECTION('center_axis',(-0.987087457637498,0.,-0.160182243006963));
#24180=DIRECTION('ref_axis',(-0.160182243006963,0.,0.987087457637497));
#24181=DIRECTION('',(-0.948683298050514,0.,-0.316227766016838));
#24182=DIRECTION('center_axis',(0.40824829046386,-0.81649658092773,-0.40824829046386));
#24183=DIRECTION('ref_axis',(-0.57735026918962,-0.577350269189619,0.577350269189638));
#24184=DIRECTION('center_axis',(0.,-1.,0.));
#24185=DIRECTION('ref_axis',(0.,0.,1.));
#24186=DIRECTION('center_axis',(0.,0.,1.));
#24187=DIRECTION('ref_axis',(-0.707106781186549,-0.707106781186546,0.));
#24188=DIRECTION('center_axis',(-1.,0.,0.));
#24189=DIRECTION('ref_axis',(0.,-0.707106781186542,0.707106781186553));
#24190=DIRECTION('center_axis',(0.,1.,0.));
#24191=DIRECTION('ref_axis',(-0.70710678118654,0.,0.707106781186555));
#24192=DIRECTION('center_axis',(0.707106781186546,-0.707106781186549,0.));
#24193=DIRECTION('ref_axis',(-0.707106781186549,-0.707106781186546,0.));
#24194=DIRECTION('center_axis',(-1.,0.,0.));
#24195=DIRECTION('ref_axis',(0.,-0.70710678118654,0.707106781186555));
#24196=DIRECTION('',(1.,0.,0.));
#24197=DIRECTION('center_axis',(0.,1.,0.));
#24198=DIRECTION('ref_axis',(-0.999898028249439,0.,-0.0142805147975766));
#24199=DIRECTION('center_axis',(0.,1.,0.));
#24200=DIRECTION('ref_axis',(-1.,0.,0.));
#24201=DIRECTION('center_axis',(0.,-1.,0.));
#24202=DIRECTION('ref_axis',(-1.,0.,0.));
#24203=DIRECTION('center_axis',(0.707106781186548,0.,-0.707106781186548));
#24204=DIRECTION('ref_axis',(-0.500000000000001,-0.707106781186546,-0.500000000000001));
#24205=DIRECTION('',(-0.707106781186547,0.,0.707106781186547));
#24206=DIRECTION('',(0.707106781186547,0.,-0.707106781186547));
#24207=DIRECTION('center_axis',(0.,0.,-1.));
#24208=DIRECTION('ref_axis',(-1.,0.,0.));
#24209=DIRECTION('',(0.,1.,0.));
#24210=DIRECTION('',(-1.,0.,0.));
#24211=DIRECTION('center_axis',(-0.298274993135947,0.,-0.95447997803503));
#24212=DIRECTION('ref_axis',(-0.95447997803503,0.,0.298274993135947));
#24213=DIRECTION('',(0.,1.,0.));
#24214=DIRECTION('',(-0.95447997803503,0.,0.298274993135947));
#24215=DIRECTION('center_axis',(-0.707106781186548,0.,-0.707106781186548));
#24216=DIRECTION('ref_axis',(-0.707106781186548,0.,0.707106781186548));
#24217=DIRECTION('',(0.,1.,0.));
#24218=DIRECTION('',(-0.707106781186547,0.,0.707106781186547));
#24219=DIRECTION('center_axis',(0.,1.,0.));
#24220=DIRECTION('ref_axis',(0.,0.,-1.));
#24221=DIRECTION('',(0.,1.,0.));
#24222=DIRECTION('center_axis',(0.,1.,0.));
#24223=DIRECTION('ref_axis',(-1.,0.,0.));
#24224=DIRECTION('center_axis',(0.,0.,1.));
#24225=DIRECTION('ref_axis',(1.,0.,0.));
#24226=DIRECTION('',(0.,1.,0.));
#24227=DIRECTION('',(1.,0.,0.));
#24228=DIRECTION('center_axis',(-0.316227766016838,0.,0.948683298050514));
#24229=DIRECTION('ref_axis',(0.948683298050514,0.,0.316227766016838));
#24230=DIRECTION('',(0.948683298050514,0.,0.316227766016838));
#24231=DIRECTION('center_axis',(1.,0.,0.));
#24232=DIRECTION('ref_axis',(0.,-0.707106781186539,0.707106781186556));
#24233=DIRECTION('',(1.,0.,0.));
#24234=DIRECTION('center_axis',(0.,0.,1.));
#24235=DIRECTION('ref_axis',(-0.707106781186548,-0.707106781186547,0.));
#24236=DIRECTION('center_axis',(-0.382683432365102,0.,0.923879532511282));
#24237=DIRECTION('ref_axis',(-0.923879532511282,0.,-0.382683432365102));
#24238=DIRECTION('',(0.,0.,1.));
#24239=DIRECTION('center_axis',(0.,1.,0.));
#24240=DIRECTION('ref_axis',(-0.70710678118654,0.,0.707106781186555));
#24241=DIRECTION('center_axis',(-0.707106781186547,-0.707106781186548,0.));
#24242=DIRECTION('ref_axis',(-0.707106781186548,0.707106781186547,0.));
#24243=DIRECTION('center_axis',(0.,-1.,0.));
#24244=DIRECTION('ref_axis',(0.,0.,1.));
#24245=DIRECTION('',(0.,-1.,0.));
#24246=DIRECTION('center_axis',(-0.40824829046386,-0.816496580927729,0.40824829046386));
#24247=DIRECTION('ref_axis',(-0.577350269189632,0.577350269189623,0.577350269189623));
#24248=DIRECTION('center_axis',(-1.,0.,0.));
#24249=DIRECTION('ref_axis',(0.,0.707106781186542,0.707106781186553));
#24250=DIRECTION('center_axis',(0.,0.,1.));
#24251=DIRECTION('ref_axis',(-0.707106781186545,0.70710678118655,0.));
#24252=DIRECTION('center_axis',(1.,0.,0.));
#24253=DIRECTION('ref_axis',(0.,0.70710678118654,0.707106781186555));
#24254=DIRECTION('center_axis',(0.987087457637498,-1.09588722278786E-14,
-0.160182243006963));
#24255=DIRECTION('ref_axis',(0.160182243006963,-6.7531613510494E-14,0.987087457637497));
#24256=DIRECTION('',(-1.,0.,0.));
#24257=DIRECTION('center_axis',(0.,0.985211754819675,-0.171341174751248));
#24258=DIRECTION('ref_axis',(-0.707106781186549,-0.121156506563076,-0.696649912737688));
#24259=DIRECTION('center_axis',(0.,0.64368424916598,-0.76529117816399));
#24260=DIRECTION('ref_axis',(1.99135285907852E-16,-0.76529117816399,-0.64368424916598));
#24261=DIRECTION('center_axis',(0.,-1.,0.));
#24262=DIRECTION('ref_axis',(2.13633744986749E-15,0.,-1.));
#24263=DIRECTION('',(0.,0.985211754819674,-0.171341174751248));
#24264=DIRECTION('center_axis',(0.,1.,0.));
#24265=DIRECTION('ref_axis',(-0.707106781186548,0.,0.707106781186548));
#24266=DIRECTION('',(0.,-1.,0.));
#24267=DIRECTION('center_axis',(0.,0.707106781186548,-0.707106781186548));
#24268=DIRECTION('ref_axis',(0.,-0.707106781186548,-0.707106781186548));
#24269=DIRECTION('',(0.,1.,0.));
#24270=DIRECTION('center_axis',(0.,0.707106781186548,0.707106781186548));
#24271=DIRECTION('ref_axis',(0.,0.707106781186548,-0.707106781186548));
#24272=DIRECTION('center_axis',(0.,-1.,0.));
#24273=DIRECTION('ref_axis',(-0.70710678118654,0.,-0.707106781186555));
#24274=DIRECTION('',(0.,1.,0.));
#24275=DIRECTION('center_axis',(0.,-0.707106781186548,0.707106781186548));
#24276=DIRECTION('ref_axis',(0.,0.707106781186548,0.707106781186548));
#24277=DIRECTION('center_axis',(0.,0.707106781186548,0.707106781186548));
#24278=DIRECTION('ref_axis',(0.,0.707106781186548,-0.707106781186548));
#24279=DIRECTION('center_axis',(0.,0.,1.));
#24280=DIRECTION('ref_axis',(-0.707106781186548,-0.707106781186548,0.));
#24281=DIRECTION('',(0.,0.,-1.));
#24282=DIRECTION('center_axis',(0.,0.,-1.));
#24283=DIRECTION('ref_axis',(-0.707106781186548,0.707106781186548,0.));
#24284=DIRECTION('',(0.,0.,1.));
#24285=DIRECTION('',(0.,0.,-1.));
#24286=DIRECTION('center_axis',(0.,-1.,0.));
#24287=DIRECTION('ref_axis',(0.,0.,-1.));
#24288=DIRECTION('',(1.,0.,0.));
#24289=DIRECTION('center_axis',(1.,0.,0.));
#24290=DIRECTION('ref_axis',(0.,0.,-1.));
#24291=DIRECTION('',(0.,0.,1.));
#24292=DIRECTION('',(0.,1.,0.));
#24293=DIRECTION('',(0.,0.,-1.));
#24294=DIRECTION('',(0.,0.,-1.));
#24295=DIRECTION('center_axis',(1.,0.,0.));
#24296=DIRECTION('ref_axis',(0.,-0.70710678118654,0.707106781186555));
#24297=DIRECTION('center_axis',(-1.,0.,0.));
#24298=DIRECTION('ref_axis',(0.,-1.,0.));
#24299=DIRECTION('',(-1.,0.,0.));
#24300=DIRECTION('',(1.,0.,0.));
#24301=DIRECTION('center_axis',(0.,1.,0.));
#24302=DIRECTION('ref_axis',(0.999898028249439,0.,-0.0142805147975766));
#24303=DIRECTION('center_axis',(0.,-1.,0.));
#24304=DIRECTION('ref_axis',(1.,0.,0.));
#24305=DIRECTION('center_axis',(0.,1.,0.));
#24306=DIRECTION('ref_axis',(1.,0.,0.));
#24307=DIRECTION('center_axis',(-0.707106781186548,0.,-0.707106781186548));
#24308=DIRECTION('ref_axis',(0.500000000000005,-0.707106781186541,-0.500000000000005));
#24309=DIRECTION('',(-0.707106781186547,0.,-0.707106781186547));
#24310=DIRECTION('center_axis',(0.855572029308629,0.,0.517683786364528));
#24311=DIRECTION('ref_axis',(-0.517683786364528,0.,0.855572029308629));
#24312=DIRECTION('',(0.707106781186547,0.,0.707106781186547));
#24313=DIRECTION('center_axis',(-0.95447997803503,0.,-0.298274993135947));
#24314=DIRECTION('ref_axis',(0.2109122703048,-0.707106781186545,-0.674919264975359));
#24315=DIRECTION('',(-0.95447997803503,0.,-0.298274993135947));
#24316=DIRECTION('center_axis',(0.988554494713119,0.,0.150864213723769));
#24317=DIRECTION('ref_axis',(-0.150864213723769,0.,0.988554494713118));
#24318=DIRECTION('',(0.95447997803503,0.,0.298274993135947));
#24319=DIRECTION('center_axis',(0.,0.,1.));
#24320=DIRECTION('ref_axis',(-0.707106781186544,-0.707106781186551,0.));
#24321=DIRECTION('',(0.,0.,1.));
#24322=DIRECTION('center_axis',(-0.70710678118655,0.,0.707106781186546));
#24323=DIRECTION('ref_axis',(-0.707106781186546,0.,-0.707106781186549));
#24324=DIRECTION('center_axis',(-1.,0.,0.));
#24325=DIRECTION('ref_axis',(0.,-0.707106781186548,-0.707106781186548));
#24326=DIRECTION('',(-1.,0.,0.));
#24327=DIRECTION('',(1.,0.,0.));
#24328=DIRECTION('center_axis',(0.,0.,1.));
#24329=DIRECTION('ref_axis',(1.,0.,0.));
#24330=DIRECTION('',(0.,1.,0.));
#24331=DIRECTION('',(1.,0.,0.));
#24332=DIRECTION('center_axis',(0.,1.,0.));
#24333=DIRECTION('ref_axis',(0.,0.,1.));
#24334=DIRECTION('',(0.,1.,0.));
#24335=DIRECTION('center_axis',(0.,1.,0.));
#24336=DIRECTION('ref_axis',(1.,0.,0.));
#24337=DIRECTION('center_axis',(0.707106781186548,0.,-0.707106781186548));
#24338=DIRECTION('ref_axis',(-0.707106781186548,0.,-0.707106781186548));
#24339=DIRECTION('',(0.,1.,0.));
#24340=DIRECTION('',(-0.707106781186547,0.,-0.707106781186547));
#24341=DIRECTION('center_axis',(0.298274993135947,0.,-0.95447997803503));
#24342=DIRECTION('ref_axis',(-0.95447997803503,0.,-0.298274993135947));
#24343=DIRECTION('',(0.,1.,0.));
#24344=DIRECTION('',(-0.95447997803503,0.,-0.298274993135947));
#24345=DIRECTION('center_axis',(0.,0.,-1.));
#24346=DIRECTION('ref_axis',(-1.,0.,0.));
#24347=DIRECTION('',(-1.,0.,0.));
#24348=DIRECTION('center_axis',(0.948683298050514,0.,0.316227766016838));
#24349=DIRECTION('ref_axis',(-0.223606797749977,0.707106781186554,0.670820393249931));
#24350=DIRECTION('',(-0.948683298050514,0.,-0.316227766016838));
#24351=DIRECTION('center_axis',(0.987087457637498,0.,0.160182243006963));
#24352=DIRECTION('ref_axis',(0.160182243006963,0.,-0.987087457637497));
#24353=DIRECTION('center_axis',(0.,1.,0.));
#24354=DIRECTION('ref_axis',(-0.999898028249439,0.,-0.0142805147975755));
#24355=DIRECTION('center_axis',(-1.,0.,0.));
#24356=DIRECTION('ref_axis',(0.,0.,1.));
#24357=DIRECTION('center_axis',(0.,-1.,0.));
#24358=DIRECTION('ref_axis',(-1.,0.,0.));
#24359=DIRECTION('center_axis',(1.,0.,0.));
#24360=DIRECTION('ref_axis',(0.,0.70710678118654,0.707106781186555));
#24361=DIRECTION('',(-1.,0.,0.));
#24362=DIRECTION('center_axis',(-0.707106781186548,0.,0.707106781186548));
#24363=DIRECTION('ref_axis',(-0.500000000000001,0.707106781186546,-0.500000000000001));
#24364=DIRECTION('',(0.707106781186547,0.,-0.707106781186547));
#24365=DIRECTION('center_axis',(-0.855572029308621,0.,0.517683786364541));
#24366=DIRECTION('ref_axis',(-0.517683786364541,0.,-0.855572029308621));
#24367=DIRECTION('center_axis',(-0.95447997803503,0.,0.298274993135947));
#24368=DIRECTION('ref_axis',(-0.210912270304798,0.707106781186552,-0.674919264975352));
#24369=DIRECTION('',(0.95447997803503,0.,-0.298274993135947));
#24370=DIRECTION('center_axis',(-0.988554494713122,0.,0.150864213723747));
#24371=DIRECTION('ref_axis',(-0.150864213723747,0.,-0.988554494713122));
#24372=DIRECTION('center_axis',(-1.,0.,0.));
#24373=DIRECTION('ref_axis',(0.,0.707106781186548,-0.707106781186548));
#24374=DIRECTION('',(1.,0.,0.));
#24375=DIRECTION('center_axis',(0.,1.,0.));
#24376=DIRECTION('ref_axis',(1.,0.,0.));
#24377=DIRECTION('center_axis',(0.,1.,0.));
#24378=DIRECTION('ref_axis',(1.,0.,0.));
#24379=DIRECTION('center_axis',(0.,1.,0.));
#24380=DIRECTION('ref_axis',(1.,0.,0.));
#24381=DIRECTION('center_axis',(0.,1.,0.));
#24382=DIRECTION('ref_axis',(1.,0.,0.));
#24383=DIRECTION('center_axis',(0.,-1.,0.));
#24384=DIRECTION('ref_axis',(0.,0.,-1.));
#24385=DIRECTION('center_axis',(0.,1.,0.));
#24386=DIRECTION('ref_axis',(1.,0.,0.));
#24387=DIRECTION('center_axis',(-1.,0.,0.));
#24388=DIRECTION('ref_axis',(0.,0.,1.));
#24389=DIRECTION('center_axis',(0.,-1.,0.));
#24390=DIRECTION('ref_axis',(1.,0.,0.));
#24391=DIRECTION('center_axis',(0.,-1.,0.));
#24392=DIRECTION('ref_axis',(1.,0.,0.));
#24393=DIRECTION('center_axis',(0.,1.,0.));
#24394=DIRECTION('ref_axis',(1.,0.,0.));
#24395=DIRECTION('center_axis',(0.,-1.,0.));
#24396=DIRECTION('ref_axis',(1.,0.,0.));
#24397=DIRECTION('center_axis',(0.,-1.,0.));
#24398=DIRECTION('ref_axis',(1.,0.,0.));
#24399=DIRECTION('',(0.,1.,0.));
#24400=DIRECTION('center_axis',(0.,1.,0.));
#24401=DIRECTION('ref_axis',(1.,0.,0.));
#24402=DIRECTION('center_axis',(1.,0.,0.));
#24403=DIRECTION('ref_axis',(0.,0.70710678118654,0.707106781186555));
#24404=DIRECTION('center_axis',(-1.,0.,0.));
#24405=DIRECTION('ref_axis',(0.,0.,1.));
#24406=DIRECTION('',(-1.,0.,0.));
#24407=DIRECTION('center_axis',(0.987087457637498,0.,-0.160182243006963));
#24408=DIRECTION('ref_axis',(-0.160182243006963,0.,-0.987087457637497));
#24409=DIRECTION('center_axis',(0.948683298050514,0.,-0.316227766016838));
#24410=DIRECTION('ref_axis',(0.223606797749977,0.707106781186554,0.670820393249931));
#24411=DIRECTION('',(-0.948683298050514,0.,0.316227766016838));
#24412=DIRECTION('center_axis',(0.,0.,1.));
#24413=DIRECTION('ref_axis',(-0.707106781186548,0.707106781186548,0.));
#24414=DIRECTION('',(0.,0.,-1.));
#24415=DIRECTION('center_axis',(-0.707106781186548,0.,0.707106781186548));
#24416=DIRECTION('ref_axis',(-0.707106781186548,0.,-0.707106781186548));
#24417=DIRECTION('center_axis',(-1.,0.,0.));
#24418=DIRECTION('ref_axis',(0.,0.707106781186548,-0.707106781186548));
#24419=DIRECTION('',(1.,0.,0.));
#24420=DIRECTION('center_axis',(-0.988554494713124,0.,-0.150864213723736));
#24421=DIRECTION('ref_axis',(0.150864213723736,0.,-0.988554494713124));
#24422=DIRECTION('center_axis',(-0.95447997803503,0.,-0.298274993135947));
#24423=DIRECTION('ref_axis',(0.210912270304798,0.707106781186552,-0.674919264975352));
#24424=DIRECTION('',(0.95447997803503,0.,0.298274993135947));
#24425=DIRECTION('center_axis',(-0.855572029308614,0.,-0.517683786364553));
#24426=DIRECTION('ref_axis',(0.517683786364553,0.,-0.855572029308614));
#24427=DIRECTION('center_axis',(-0.707106781186548,0.,-0.707106781186548));
#24428=DIRECTION('ref_axis',(0.500000000000005,0.707106781186541,-0.500000000000005));
#24429=DIRECTION('',(0.707106781186547,0.,0.707106781186547));
#24430=DIRECTION('center_axis',(0.,1.,0.));
#24431=DIRECTION('ref_axis',(0.999898028249439,0.,-0.0142805147975766));
#24432=DIRECTION('center_axis',(0.,-1.,0.));
#24433=DIRECTION('ref_axis',(1.,0.,0.));
#24434=DIRECTION('center_axis',(0.,1.,0.));
#24435=DIRECTION('ref_axis',(1.,0.,0.));
#24436=DIRECTION('center_axis',(0.,1.,0.));
#24437=DIRECTION('ref_axis',(1.,0.,0.));
#24438=DIRECTION('center_axis',(0.,1.,0.));
#24439=DIRECTION('ref_axis',(1.,0.,0.));
#24440=DIRECTION('center_axis',(0.,1.,0.));
#24441=DIRECTION('ref_axis',(1.,0.,0.));
#24442=DIRECTION('center_axis',(0.,-1.,0.));
#24443=DIRECTION('ref_axis',(0.,0.,-1.));
#24444=DIRECTION('center_axis',(0.,1.,0.));
#24445=DIRECTION('ref_axis',(1.,0.,0.));
#24446=DIRECTION('center_axis',(-1.,0.,0.));
#24447=DIRECTION('ref_axis',(0.,0.,1.));
#24448=DIRECTION('center_axis',(0.,-1.,0.));
#24449=DIRECTION('ref_axis',(1.,0.,0.));
#24450=DIRECTION('center_axis',(0.,-1.,0.));
#24451=DIRECTION('ref_axis',(1.,0.,0.));
#24452=DIRECTION('center_axis',(0.,1.,0.));
#24453=DIRECTION('ref_axis',(1.,0.,0.));
#24454=DIRECTION('center_axis',(0.,-1.,0.));
#24455=DIRECTION('ref_axis',(1.,0.,0.));
#24456=DIRECTION('center_axis',(0.,-1.,0.));
#24457=DIRECTION('ref_axis',(1.,0.,0.));
#24458=DIRECTION('',(0.,1.,0.));
#24459=DIRECTION('center_axis',(0.,1.,0.));
#24460=DIRECTION('ref_axis',(1.,0.,0.));
#24461=DIRECTION('center_axis',(0.,1.,0.));
#24462=DIRECTION('ref_axis',(0.,0.,1.));
#24463=DIRECTION('center_axis',(-1.,0.,0.));
#24464=DIRECTION('ref_axis',(0.,0.,-1.));
#24465=DIRECTION('center_axis',(0.,1.,0.));
#24466=DIRECTION('ref_axis',(1.,0.,0.));
#24467=DIRECTION('center_axis',(0.,1.,0.));
#24468=DIRECTION('ref_axis',(1.,0.,0.));
#24469=DIRECTION('center_axis',(0.,1.,0.));
#24470=DIRECTION('ref_axis',(1.,0.,0.));
#24471=DIRECTION('',(0.,1.,0.));
#24472=DIRECTION('center_axis',(0.,-1.,0.));
#24473=DIRECTION('ref_axis',(1.,0.,0.));
#24474=DIRECTION('center_axis',(0.,-1.,0.));
#24475=DIRECTION('ref_axis',(1.,0.,0.));
#24476=DIRECTION('center_axis',(0.,-1.,0.));
#24477=DIRECTION('ref_axis',(0.,0.,-1.));
#24478=DIRECTION('center_axis',(-1.,0.,0.));
#24479=DIRECTION('ref_axis',(0.,0.,1.));
#24480=DIRECTION('center_axis',(0.,1.,0.));
#24481=DIRECTION('ref_axis',(0.,0.,1.));
#24482=DIRECTION('center_axis',(-1.,0.,0.));
#24483=DIRECTION('ref_axis',(0.,0.,-1.));
#24484=DIRECTION('center_axis',(0.,1.,0.));
#24485=DIRECTION('ref_axis',(1.,0.,0.));
#24486=DIRECTION('center_axis',(0.,1.,0.));
#24487=DIRECTION('ref_axis',(1.,0.,0.));
#24488=DIRECTION('center_axis',(0.,1.,0.));
#24489=DIRECTION('ref_axis',(1.,0.,0.));
#24490=DIRECTION('',(0.,1.,0.));
#24491=DIRECTION('center_axis',(0.,-1.,0.));
#24492=DIRECTION('ref_axis',(1.,0.,0.));
#24493=DIRECTION('center_axis',(0.,-1.,0.));
#24494=DIRECTION('ref_axis',(1.,0.,0.));
#24495=DIRECTION('center_axis',(0.,-1.,0.));
#24496=DIRECTION('ref_axis',(0.,0.,-1.));
#24497=DIRECTION('center_axis',(-1.,0.,0.));
#24498=DIRECTION('ref_axis',(0.,0.,1.));
#24499=DIRECTION('center_axis',(0.,-1.,0.));
#24500=DIRECTION('ref_axis',(0.,0.,-1.));
#24501=DIRECTION('center_axis',(-1.,0.,0.));
#24502=DIRECTION('ref_axis',(0.,0.,1.));
#24503=DIRECTION('center_axis',(0.,-1.,0.));
#24504=DIRECTION('ref_axis',(1.,0.,0.));
#24505=DIRECTION('center_axis',(0.,-1.,0.));
#24506=DIRECTION('ref_axis',(1.,0.,0.));
#24507=DIRECTION('center_axis',(0.,1.,0.));
#24508=DIRECTION('ref_axis',(1.,0.,0.));
#24509=DIRECTION('center_axis',(0.,1.,0.));
#24510=DIRECTION('ref_axis',(1.,0.,0.));
#24511=DIRECTION('center_axis',(0.,1.,0.));
#24512=DIRECTION('ref_axis',(1.,0.,0.));
#24513=DIRECTION('',(0.,1.,0.));
#24514=DIRECTION('center_axis',(0.,1.,0.));
#24515=DIRECTION('ref_axis',(0.,0.,1.));
#24516=DIRECTION('center_axis',(0.,-1.,0.));
#24517=DIRECTION('ref_axis',(1.,0.,0.));
#24518=DIRECTION('center_axis',(-1.,0.,0.));
#24519=DIRECTION('ref_axis',(0.,0.,-1.));
#24520=DIRECTION('center_axis',(0.,1.,0.));
#24521=DIRECTION('ref_axis',(1.,0.,0.));
#24522=DIRECTION('center_axis',(0.,-1.,0.));
#24523=DIRECTION('ref_axis',(1.,0.,0.));
#24524=DIRECTION('center_axis',(0.,-1.,0.));
#24525=DIRECTION('ref_axis',(0.,0.,-1.));
#24526=DIRECTION('center_axis',(-1.,0.,0.));
#24527=DIRECTION('ref_axis',(0.,0.,1.));
#24528=DIRECTION('center_axis',(0.,-1.,0.));
#24529=DIRECTION('ref_axis',(1.,0.,0.));
#24530=DIRECTION('center_axis',(0.,-1.,0.));
#24531=DIRECTION('ref_axis',(1.,0.,0.));
#24532=DIRECTION('center_axis',(0.,1.,0.));
#24533=DIRECTION('ref_axis',(1.,0.,0.));
#24534=DIRECTION('center_axis',(0.,1.,0.));
#24535=DIRECTION('ref_axis',(1.,0.,0.));
#24536=DIRECTION('center_axis',(0.,1.,0.));
#24537=DIRECTION('ref_axis',(1.,0.,0.));
#24538=DIRECTION('',(0.,1.,0.));
#24539=DIRECTION('center_axis',(0.,1.,0.));
#24540=DIRECTION('ref_axis',(0.,0.,1.));
#24541=DIRECTION('center_axis',(0.,-1.,0.));
#24542=DIRECTION('ref_axis',(1.,0.,0.));
#24543=DIRECTION('center_axis',(-1.,0.,0.));
#24544=DIRECTION('ref_axis',(0.,0.,-1.));
#24545=DIRECTION('center_axis',(0.,1.,0.));
#24546=DIRECTION('ref_axis',(1.,0.,0.));
#24547=DIRECTION('',(-1.,0.,0.));
#24548=DIRECTION('center_axis',(0.,-1.,0.));
#24549=DIRECTION('ref_axis',(1.,0.,0.));
#24550=DIRECTION('center_axis',(0.,-1.,0.));
#24551=DIRECTION('ref_axis',(0.,0.,-1.));
#24552=DIRECTION('center_axis',(-1.,0.,0.));
#24553=DIRECTION('ref_axis',(0.,0.,1.));
#24554=DIRECTION('center_axis',(0.,-1.,0.));
#24555=DIRECTION('ref_axis',(1.,0.,0.));
#24556=DIRECTION('center_axis',(0.,-1.,0.));
#24557=DIRECTION('ref_axis',(1.,0.,0.));
#24558=DIRECTION('center_axis',(0.,1.,0.));
#24559=DIRECTION('ref_axis',(1.,0.,0.));
#24560=DIRECTION('center_axis',(0.,1.,0.));
#24561=DIRECTION('ref_axis',(1.,0.,0.));
#24562=DIRECTION('center_axis',(0.,1.,0.));
#24563=DIRECTION('ref_axis',(1.,0.,0.));
#24564=DIRECTION('',(0.,1.,0.));
#24565=DIRECTION('center_axis',(0.,1.,0.));
#24566=DIRECTION('ref_axis',(0.,0.,1.));
#24567=DIRECTION('center_axis',(-1.,0.,0.));
#24568=DIRECTION('ref_axis',(0.,0.,-1.));
#24569=DIRECTION('center_axis',(0.,-1.,0.));
#24570=DIRECTION('ref_axis',(0.,0.,-1.));
#24571=DIRECTION('center_axis',(-1.,0.,0.));
#24572=DIRECTION('ref_axis',(0.,0.,1.));
#24573=DIRECTION('center_axis',(0.,-1.,0.));
#24574=DIRECTION('ref_axis',(1.,0.,0.));
#24575=DIRECTION('center_axis',(0.,-1.,0.));
#24576=DIRECTION('ref_axis',(1.,0.,0.));
#24577=DIRECTION('center_axis',(0.,1.,0.));
#24578=DIRECTION('ref_axis',(1.,0.,0.));
#24579=DIRECTION('center_axis',(0.,1.,0.));
#24580=DIRECTION('ref_axis',(1.,0.,0.));
#24581=DIRECTION('center_axis',(0.,1.,0.));
#24582=DIRECTION('ref_axis',(1.,0.,0.));
#24583=DIRECTION('',(0.,1.,0.));
#24584=DIRECTION('center_axis',(0.,1.,0.));
#24585=DIRECTION('ref_axis',(0.,0.,1.));
#24586=DIRECTION('center_axis',(-1.,0.,0.));
#24587=DIRECTION('ref_axis',(0.,0.,-1.));
#24588=DIRECTION('center_axis',(0.,-1.,0.));
#24589=DIRECTION('ref_axis',(0.,0.,-1.));
#24590=DIRECTION('center_axis',(0.,1.,0.));
#24591=DIRECTION('ref_axis',(1.,0.,0.));
#24592=DIRECTION('center_axis',(-1.,0.,0.));
#24593=DIRECTION('ref_axis',(0.,0.,1.));
#24594=DIRECTION('center_axis',(0.,-1.,0.));
#24595=DIRECTION('ref_axis',(1.,0.,0.));
#24596=DIRECTION('center_axis',(0.,-1.,0.));
#24597=DIRECTION('ref_axis',(1.,0.,0.));
#24598=DIRECTION('center_axis',(0.,1.,0.));
#24599=DIRECTION('ref_axis',(1.,0.,0.));
#24600=DIRECTION('center_axis',(0.,1.,0.));
#24601=DIRECTION('ref_axis',(1.,0.,0.));
#24602=DIRECTION('center_axis',(0.,1.,0.));
#24603=DIRECTION('ref_axis',(1.,0.,0.));
#24604=DIRECTION('',(0.,1.,0.));
#24605=DIRECTION('center_axis',(0.,1.,0.));
#24606=DIRECTION('ref_axis',(0.,0.,1.));
#24607=DIRECTION('',(0.707106781186547,0.,-0.707106781186548));
#24608=DIRECTION('',(1.,0.,0.));
#24609=DIRECTION('',(-1.,0.,0.));
#24610=DIRECTION('',(0.707106781186547,0.,0.707106781186548));
#24611=DIRECTION('',(1.,0.,0.));
#24612=DIRECTION('center_axis',(0.,1.,0.));
#24613=DIRECTION('ref_axis',(1.,0.,0.));
#24614=DIRECTION('',(0.,0.,1.));
#24615=DIRECTION('',(-1.,0.,0.));
#24616=DIRECTION('',(0.,0.,-1.));
#24617=DIRECTION('',(1.,0.,0.));
#24618=DIRECTION('',(0.,0.,1.));
#24619=DIRECTION('',(-1.,0.,0.));
#24620=DIRECTION('',(0.,0.,-1.));
#24621=DIRECTION('',(1.,0.,0.));
#24622=DIRECTION('center_axis',(-0.707106781186547,0.,0.707106781186548));
#24623=DIRECTION('ref_axis',(-0.500000000000001,0.707106781186546,-0.500000000000001));
#24624=DIRECTION('',(-0.707106781186547,0.,0.707106781186548));
#24625=DIRECTION('center_axis',(0.,0.171341174751248,0.985211754819675));
#24626=DIRECTION('ref_axis',(-0.985636596769451,-0.166382691564751,0.0289361202721306));
#24627=DIRECTION('center_axis',(-0.923879532511285,-5.12856164486977E-15,
0.382683432365094));
#24628=DIRECTION('ref_axis',(-0.382683432365094,-1.23814430785112E-14,-0.923879532511285));
#24629=DIRECTION('center_axis',(-1.,0.,0.));
#24630=DIRECTION('ref_axis',(0.,0.707106781186547,-0.707106781186548));
#24631=DIRECTION('center_axis',(-0.923879532511285,-5.12856164486977E-15,
-0.382683432365094));
#24632=DIRECTION('ref_axis',(0.382683432365094,-1.23814430785109E-14,-0.923879532511285));
#24633=DIRECTION('',(-1.,0.,0.));
#24634=DIRECTION('center_axis',(-0.707106781186547,0.,-0.707106781186548));
#24635=DIRECTION('ref_axis',(0.500000000000001,0.707106781186546,-0.500000000000001));
#24636=DIRECTION('',(-0.707106781186547,0.,-0.707106781186548));
#24637=DIRECTION('center_axis',(-0.707106781186548,0.,-0.707106781186547));
#24638=DIRECTION('ref_axis',(-0.707106781186547,0.,0.707106781186548));
#24639=DIRECTION('',(0.,1.,0.));
#24640=DIRECTION('',(0.707106781186547,0.,-0.707106781186548));
#24641=DIRECTION('center_axis',(0.,0.,-1.));
#24642=DIRECTION('ref_axis',(-1.,0.,0.));
#24643=DIRECTION('',(0.,1.,0.));
#24644=DIRECTION('',(1.,0.,0.));
#24645=DIRECTION('center_axis',(0.707106781186548,0.,-0.707106781186547));
#24646=DIRECTION('ref_axis',(-0.707106781186547,0.,-0.707106781186548));
#24647=DIRECTION('',(0.707106781186547,0.,0.707106781186548));
#24648=DIRECTION('center_axis',(1.,0.,0.));
#24649=DIRECTION('ref_axis',(0.,0.707106781186539,0.707106781186556));
#24650=DIRECTION('center_axis',(0.,1.,0.));
#24651=DIRECTION('ref_axis',(0.,0.,1.));
#24652=DIRECTION('center_axis',(0.,-1.,0.));
#24653=DIRECTION('ref_axis',(1.,0.,0.));
#24654=DIRECTION('center_axis',(-1.,0.,0.));
#24655=DIRECTION('ref_axis',(0.,0.,-1.));
#24656=DIRECTION('center_axis',(0.,1.,0.));
#24657=DIRECTION('ref_axis',(1.,0.,0.));
#24658=DIRECTION('',(-0.707106781186547,0.,0.707106781186548));
#24659=DIRECTION('',(-1.,0.,0.));
#24660=DIRECTION('',(-0.707106781186547,0.,-0.707106781186548));
#24661=DIRECTION('',(0.,0.,-1.));
#24662=DIRECTION('',(1.,0.,0.));
#24663=DIRECTION('',(0.,0.,1.));
#24664=DIRECTION('',(1.,0.,0.));
#24665=DIRECTION('',(0.,0.,-1.));
#24666=DIRECTION('',(1.,0.,0.));
#24667=DIRECTION('',(0.,0.,1.));
#24668=DIRECTION('',(1.,0.,0.));
#24669=DIRECTION('',(0.,0.,-1.));
#24670=DIRECTION('',(1.,0.,0.));
#24671=DIRECTION('',(0.,0.,1.));
#24672=DIRECTION('',(1.,0.,0.));
#24673=DIRECTION('',(0.,0.,-1.));
#24674=DIRECTION('',(1.,0.,0.));
#24675=DIRECTION('',(0.,0.,1.));
#24676=DIRECTION('',(1.,0.,0.));
#24677=DIRECTION('',(0.,0.,-1.));
#24678=DIRECTION('center_axis',(0.,-1.,0.));
#24679=DIRECTION('ref_axis',(1.,0.,0.));
#24680=DIRECTION('center_axis',(-1.,0.,0.));
#24681=DIRECTION('ref_axis',(0.,-0.707106781186539,-0.707106781186556));
#24682=DIRECTION('center_axis',(0.923879532511285,9.37720122241289E-15,
-0.382683432365094));
#24683=DIRECTION('ref_axis',(0.382683432365094,-2.26385663682504E-14,0.923879532511285));
#24684=DIRECTION('center_axis',(0.923879532511289,0.,0.382683432365086));
#24685=DIRECTION('ref_axis',(-0.382683432365086,0.,0.923879532511288));
#24686=DIRECTION('center_axis',(-0.707106781186547,0.,0.707106781186548));
#24687=DIRECTION('ref_axis',(-0.500000000000001,-0.707106781186546,-0.500000000000001));
#24688=DIRECTION('center_axis',(0.,0.,-1.));
#24689=DIRECTION('ref_axis',(0.707106781186548,-0.707106781186547,0.));
#24690=DIRECTION('center_axis',(0.382683432365094,0.,0.923879532511285));
#24691=DIRECTION('ref_axis',(-0.923879532511285,0.,0.382683432365094));
#24692=DIRECTION('center_axis',(-0.707106781186547,0.,-0.707106781186548));
#24693=DIRECTION('ref_axis',(0.500000000000001,-0.707106781186546,-0.500000000000001));
#24694=DIRECTION('center_axis',(0.,1.,0.));
#24695=DIRECTION('ref_axis',(0.,0.,1.));
#24696=DIRECTION('center_axis',(-1.,0.,0.));
#24697=DIRECTION('ref_axis',(0.,0.,-1.));
#24698=DIRECTION('center_axis',(0.,1.,0.));
#24699=DIRECTION('ref_axis',(1.,0.,0.));
#24700=DIRECTION('center_axis',(0.,1.,0.));
#24701=DIRECTION('ref_axis',(1.,0.,0.));
#24702=DIRECTION('center_axis',(0.,1.,0.));
#24703=DIRECTION('ref_axis',(1.,0.,0.));
#24704=DIRECTION('',(0.,1.,0.));
#24705=DIRECTION('center_axis',(0.,-1.,0.));
#24706=DIRECTION('ref_axis',(1.,0.,0.));
#24707=DIRECTION('center_axis',(0.,-1.,0.));
#24708=DIRECTION('ref_axis',(1.,0.,0.));
#24709=DIRECTION('center_axis',(0.,-1.,0.));
#24710=DIRECTION('ref_axis',(0.,0.,-1.));
#24711=DIRECTION('center_axis',(-1.,0.,0.));
#24712=DIRECTION('ref_axis',(0.,0.,1.));
#24713=DIRECTION('center_axis',(0.,0.,-1.));
#24714=DIRECTION('ref_axis',(0.707106781186548,0.707106781186547,0.));
#24715=DIRECTION('center_axis',(-0.707106781186548,0.,-0.707106781186548));
#24716=DIRECTION('ref_axis',(-0.707106781186548,0.,0.707106781186548));
#24717=DIRECTION('',(0.,0.,-1.));
#24718=DIRECTION('center_axis',(-0.707106781186548,0.,0.707106781186548));
#24719=DIRECTION('ref_axis',(0.707106781186548,0.,0.707106781186548));
#24720=DIRECTION('center_axis',(-1.,0.,0.));
#24721=DIRECTION('ref_axis',(0.,0.707106781186555,-0.70710678118654));
#24722=DIRECTION('',(-1.,0.,0.));
#24723=DIRECTION('center_axis',(0.707106781186548,0.,-0.707106781186548));
#24724=DIRECTION('ref_axis',(-0.707106781186548,0.,-0.707106781186548));
#24725=DIRECTION('center_axis',(1.,0.,0.));
#24726=DIRECTION('ref_axis',(0.,0.707106781186547,0.707106781186548));
#24727=DIRECTION('',(1.,0.,0.));
#24728=DIRECTION('center_axis',(-0.707106781186548,0.,-0.707106781186548));
#24729=DIRECTION('ref_axis',(-0.707106781186548,0.,0.707106781186548));
#24730=DIRECTION('center_axis',(0.,0.,1.));
#24731=DIRECTION('ref_axis',(-0.707106781186548,0.707106781186547,0.));
#24732=DIRECTION('',(0.,0.,1.));
#24733=DIRECTION('center_axis',(0.,0.,-1.));
#24734=DIRECTION('ref_axis',(-1.,0.,0.));
#24735=DIRECTION('',(0.,1.,0.));
#24736=DIRECTION('',(-1.,0.,0.));
#24737=DIRECTION('',(0.,1.,0.));
#24738=DIRECTION('center_axis',(-1.,0.,0.));
#24739=DIRECTION('ref_axis',(0.,0.,1.));
#24740=DIRECTION('',(0.,1.,0.));
#24741=DIRECTION('',(0.,0.,1.));
#24742=DIRECTION('center_axis',(0.,0.,1.));
#24743=DIRECTION('ref_axis',(0.707106781186548,-0.707106781186547,0.));
#24744=DIRECTION('center_axis',(0.,0.,1.));
#24745=DIRECTION('ref_axis',(0.707106781186548,-0.707106781186547,0.));
#24746=DIRECTION('center_axis',(-0.707106781186548,0.,0.707106781186548));
#24747=DIRECTION('ref_axis',(-0.707106781186548,0.,-0.707106781186548));
#24748=DIRECTION('center_axis',(-1.,0.,0.));
#24749=DIRECTION('ref_axis',(0.,-0.707106781186547,0.707106781186548));
#24750=DIRECTION('center_axis',(-0.707106781186548,0.,-0.707106781186548));
#24751=DIRECTION('ref_axis',(0.707106781186548,0.,-0.707106781186548));
#24752=DIRECTION('center_axis',(0.,0.,-1.));
#24753=DIRECTION('ref_axis',(-0.707106781186548,-0.707106781186547,0.));
#24754=DIRECTION('center_axis',(0.,0.,1.));
#24755=DIRECTION('ref_axis',(-0.707106781186548,-0.707106781186547,0.));
#24756=DIRECTION('',(0.,0.,-1.));
#24757=DIRECTION('center_axis',(1.,0.,0.));
#24758=DIRECTION('ref_axis',(0.,0.,-1.));
#24759=DIRECTION('',(0.,1.,0.));
#24760=DIRECTION('center_axis',(0.,0.,-1.));
#24761=DIRECTION('ref_axis',(0.707106781186548,0.707106781186547,0.));
#24762=DIRECTION('center_axis',(-0.707106781186548,0.,-0.707106781186548));
#24763=DIRECTION('ref_axis',(-0.707106781186548,0.,0.707106781186548));
#24764=DIRECTION('',(0.,0.,-1.));
#24765=DIRECTION('center_axis',(-0.707106781186548,0.,0.707106781186548));
#24766=DIRECTION('ref_axis',(0.707106781186548,0.,0.707106781186548));
#24767=DIRECTION('center_axis',(-1.,0.,0.));
#24768=DIRECTION('ref_axis',(0.,0.707106781186555,-0.70710678118654));
#24769=DIRECTION('',(-1.,0.,0.));
#24770=DIRECTION('center_axis',(0.707106781186548,0.,-0.707106781186548));
#24771=DIRECTION('ref_axis',(-0.707106781186548,0.,-0.707106781186548));
#24772=DIRECTION('center_axis',(1.,0.,0.));
#24773=DIRECTION('ref_axis',(0.,0.707106781186547,0.707106781186548));
#24774=DIRECTION('',(1.,0.,0.));
#24775=DIRECTION('center_axis',(-0.707106781186548,0.,-0.707106781186548));
#24776=DIRECTION('ref_axis',(-0.707106781186548,0.,0.707106781186548));
#24777=DIRECTION('center_axis',(0.,0.,1.));
#24778=DIRECTION('ref_axis',(-0.707106781186548,0.707106781186547,0.));
#24779=DIRECTION('',(0.,0.,1.));
#24780=DIRECTION('center_axis',(0.,0.,-1.));
#24781=DIRECTION('ref_axis',(-1.,0.,0.));
#24782=DIRECTION('',(0.,1.,0.));
#24783=DIRECTION('',(-1.,0.,0.));
#24784=DIRECTION('',(0.,1.,0.));
#24785=DIRECTION('center_axis',(-1.,0.,0.));
#24786=DIRECTION('ref_axis',(0.,0.,1.));
#24787=DIRECTION('',(0.,1.,0.));
#24788=DIRECTION('',(0.,0.,1.));
#24789=DIRECTION('center_axis',(0.,0.,1.));
#24790=DIRECTION('ref_axis',(0.707106781186548,-0.707106781186547,0.));
#24791=DIRECTION('center_axis',(0.,0.,1.));
#24792=DIRECTION('ref_axis',(0.707106781186548,-0.707106781186547,0.));
#24793=DIRECTION('center_axis',(-0.707106781186548,0.,0.707106781186548));
#24794=DIRECTION('ref_axis',(-0.707106781186548,0.,-0.707106781186548));
#24795=DIRECTION('center_axis',(-1.,0.,0.));
#24796=DIRECTION('ref_axis',(0.,-0.707106781186547,0.707106781186548));
#24797=DIRECTION('center_axis',(-0.707106781186548,0.,-0.707106781186548));
#24798=DIRECTION('ref_axis',(0.707106781186548,0.,-0.707106781186548));
#24799=DIRECTION('center_axis',(0.,0.,-1.));
#24800=DIRECTION('ref_axis',(-0.707106781186548,-0.707106781186547,0.));
#24801=DIRECTION('center_axis',(0.,0.,1.));
#24802=DIRECTION('ref_axis',(-0.707106781186548,-0.707106781186547,0.));
#24803=DIRECTION('',(0.,0.,-1.));
#24804=DIRECTION('center_axis',(1.,0.,0.));
#24805=DIRECTION('ref_axis',(0.,0.,-1.));
#24806=DIRECTION('',(0.,1.,0.));
#24807=DIRECTION('center_axis',(0.,0.,-1.));
#24808=DIRECTION('ref_axis',(-0.707106781186548,-0.707106781186547,0.));
#24809=DIRECTION('center_axis',(0.,0.,1.));
#24810=DIRECTION('ref_axis',(-0.707106781186548,-0.707106781186547,0.));
#24811=DIRECTION('',(0.,0.,1.));
#24812=DIRECTION('center_axis',(0.,0.,-1.));
#24813=DIRECTION('ref_axis',(-0.707106781186548,-0.707106781186547,0.));
#24814=DIRECTION('',(0.,0.,-1.));
#24815=DIRECTION('center_axis',(0.,0.,1.));
#24816=DIRECTION('ref_axis',(-0.707106781186548,-0.707106781186547,0.));
#24817=DIRECTION('',(0.,0.,-1.));
#24818=DIRECTION('center_axis',(0.,0.,-1.));
#24819=DIRECTION('ref_axis',(-0.707106781186548,0.707106781186547,0.));
#24820=DIRECTION('center_axis',(0.,0.,1.));
#24821=DIRECTION('ref_axis',(-0.707106781186548,0.707106781186547,0.));
#24822=DIRECTION('',(0.,0.,-1.));
#24823=DIRECTION('center_axis',(0.,0.,1.));
#24824=DIRECTION('ref_axis',(-0.707106781186548,0.707106781186547,0.));
#24825=DIRECTION('center_axis',(0.,0.,1.));
#24826=DIRECTION('ref_axis',(1.,0.,0.));
#24827=DIRECTION('',(0.,-1.,0.));
#24828=DIRECTION('center_axis',(0.,0.,1.));
#24829=DIRECTION('ref_axis',(0.707106781186548,-0.707106781186547,0.));
#24830=DIRECTION('center_axis',(0.,0.,1.));
#24831=DIRECTION('ref_axis',(0.707106781186548,0.707106781186547,0.));
#24832=DIRECTION('',(1.,0.,0.));
#24833=DIRECTION('',(0.,1.,0.));
#24834=DIRECTION('center_axis',(-1.,0.,0.));
#24835=DIRECTION('ref_axis',(0.,0.,-1.));
#24836=DIRECTION('',(0.,-1.,0.));
#24837=DIRECTION('center_axis',(0.,0.,-1.));
#24838=DIRECTION('ref_axis',(1.,0.,0.));
#24839=DIRECTION('',(1.,0.,0.));
#24840=DIRECTION('center_axis',(0.,0.,1.));
#24841=DIRECTION('ref_axis',(0.707106781186548,0.707106781186547,0.));
#24842=DIRECTION('center_axis',(0.,0.,1.));
#24843=DIRECTION('ref_axis',(0.707106781186548,-0.707106781186547,0.));
#24844=DIRECTION('',(1.,0.,0.));
#24845=DIRECTION('center_axis',(0.,0.,1.));
#24846=DIRECTION('ref_axis',(0.707106781186548,-0.707106781186547,0.));
#24847=DIRECTION('center_axis',(0.,0.,-1.));
#24848=DIRECTION('ref_axis',(0.707106781186548,-0.707106781186547,0.));
#24849=DIRECTION('',(0.,0.,-1.));
#24850=DIRECTION('',(0.,0.,1.));
#24851=DIRECTION('',(0.,0.,1.));
#24852=DIRECTION('center_axis',(0.,-1.,0.));
#24853=DIRECTION('ref_axis',(0.,0.,-1.));
#24854=DIRECTION('',(-1.,0.,0.));
#24855=DIRECTION('center_axis',(0.,0.,1.));
#24856=DIRECTION('ref_axis',(-1.,0.,0.));
#24857=DIRECTION('',(0.,-1.,0.));
#24858=DIRECTION('center_axis',(1.,0.,0.));
#24859=DIRECTION('ref_axis',(0.,0.,1.));
#24860=DIRECTION('center_axis',(0.,0.,1.));
#24861=DIRECTION('ref_axis',(0.707106781186548,0.707106781186547,0.));
#24862=DIRECTION('',(0.,0.,1.));
#24863=DIRECTION('center_axis',(0.,0.,-1.));
#24864=DIRECTION('ref_axis',(-0.707106781186548,-0.707106781186547,0.));
#24865=DIRECTION('center_axis',(0.,0.,1.));
#24866=DIRECTION('ref_axis',(-0.707106781186548,-0.707106781186547,0.));
#24867=DIRECTION('',(0.,0.,1.));
#24868=DIRECTION('center_axis',(0.,0.,-1.));
#24869=DIRECTION('ref_axis',(-0.707106781186548,-0.707106781186547,0.));
#24870=DIRECTION('',(0.,0.,-1.));
#24871=DIRECTION('center_axis',(0.,0.,1.));
#24872=DIRECTION('ref_axis',(-0.707106781186548,-0.707106781186547,0.));
#24873=DIRECTION('',(0.,0.,-1.));
#24874=DIRECTION('center_axis',(0.,0.,-1.));
#24875=DIRECTION('ref_axis',(-0.707106781186548,0.707106781186547,0.));
#24876=DIRECTION('center_axis',(0.,0.,1.));
#24877=DIRECTION('ref_axis',(-0.707106781186548,0.707106781186547,0.));
#24878=DIRECTION('',(0.,0.,-1.));
#24879=DIRECTION('center_axis',(0.,0.,1.));
#24880=DIRECTION('ref_axis',(-0.707106781186548,0.707106781186547,0.));
#24881=DIRECTION('center_axis',(0.,0.,1.));
#24882=DIRECTION('ref_axis',(1.,0.,0.));
#24883=DIRECTION('',(0.,-1.,0.));
#24884=DIRECTION('center_axis',(0.,0.,1.));
#24885=DIRECTION('ref_axis',(0.707106781186548,-0.707106781186547,0.));
#24886=DIRECTION('center_axis',(0.,0.,1.));
#24887=DIRECTION('ref_axis',(0.707106781186548,0.707106781186547,0.));
#24888=DIRECTION('',(1.,0.,0.));
#24889=DIRECTION('',(0.,1.,0.));
#24890=DIRECTION('center_axis',(-1.,0.,0.));
#24891=DIRECTION('ref_axis',(0.,0.,-1.));
#24892=DIRECTION('',(0.,-1.,0.));
#24893=DIRECTION('center_axis',(0.,0.,-1.));
#24894=DIRECTION('ref_axis',(1.,0.,0.));
#24895=DIRECTION('',(1.,0.,0.));
#24896=DIRECTION('center_axis',(0.,0.,1.));
#24897=DIRECTION('ref_axis',(0.707106781186548,0.707106781186547,0.));
#24898=DIRECTION('center_axis',(0.,0.,1.));
#24899=DIRECTION('ref_axis',(0.707106781186548,-0.707106781186547,0.));
#24900=DIRECTION('',(1.,0.,0.));
#24901=DIRECTION('center_axis',(0.,0.,1.));
#24902=DIRECTION('ref_axis',(0.707106781186548,-0.707106781186547,0.));
#24903=DIRECTION('center_axis',(0.,0.,-1.));
#24904=DIRECTION('ref_axis',(0.707106781186548,-0.707106781186547,0.));
#24905=DIRECTION('',(0.,0.,-1.));
#24906=DIRECTION('',(0.,0.,1.));
#24907=DIRECTION('',(0.,0.,1.));
#24908=DIRECTION('center_axis',(0.,-1.,0.));
#24909=DIRECTION('ref_axis',(0.,0.,-1.));
#24910=DIRECTION('',(-1.,0.,0.));
#24911=DIRECTION('center_axis',(0.,0.,1.));
#24912=DIRECTION('ref_axis',(-1.,0.,0.));
#24913=DIRECTION('',(0.,-1.,0.));
#24914=DIRECTION('center_axis',(1.,0.,0.));
#24915=DIRECTION('ref_axis',(0.,0.,1.));
#24916=DIRECTION('center_axis',(0.,0.,1.));
#24917=DIRECTION('ref_axis',(0.707106781186548,0.707106781186547,0.));
#24918=DIRECTION('',(0.,0.,1.));
#24919=DIRECTION('center_axis',(0.,1.,0.));
#24920=DIRECTION('ref_axis',(1.,0.,0.));
#24921=DIRECTION('center_axis',(0.,1.,0.));
#24922=DIRECTION('ref_axis',(1.,0.,0.));
#24923=DIRECTION('center_axis',(0.,0.,1.));
#24924=DIRECTION('ref_axis',(0.,1.,0.));
#24925=DIRECTION('center_axis',(0.,-0.171341174751248,-0.985211754819675));
#24926=DIRECTION('ref_axis',(0.,-0.985211754819675,0.171341174751248));
#24927=DIRECTION('center_axis',(0.,0.,-1.));
#24928=DIRECTION('ref_axis',(0.,1.,0.));
#24929=DIRECTION('axis',(0.,0.,1.));
#24930=DIRECTION('refdir',(1.,0.,0.));
#24931=DIRECTION('center_axis',(0.408248290463864,-0.816496580927723,0.408248290463868));
#24932=DIRECTION('ref_axis',(0.577350269189627,0.577350269189627,0.577350269189623));
#24933=DIRECTION('center_axis',(1.,0.,0.));
#24934=DIRECTION('ref_axis',(0.,0.,1.));
#24935=DIRECTION('center_axis',(0.,1.,0.));
#24936=DIRECTION('ref_axis',(1.,0.,0.));
#24937=DIRECTION('center_axis',(0.,0.,1.));
#24938=DIRECTION('ref_axis',(0.,1.,0.));
#24939=DIRECTION('center_axis',(0.408248290463864,-0.408248290463861,-0.816496580927727));
#24940=DIRECTION('ref_axis',(0.577350269189628,-0.577350269189626,0.577350269189624));
#24941=DIRECTION('center_axis',(0.,-1.,0.));
#24942=DIRECTION('ref_axis',(0.,0.,1.));
#24943=DIRECTION('center_axis',(1.,0.,0.));
#24944=DIRECTION('ref_axis',(0.,-1.,0.));
#24945=DIRECTION('center_axis',(0.,0.,1.));
#24946=DIRECTION('ref_axis',(1.,0.,0.));
#24947=DIRECTION('center_axis',(-1.,0.,0.));
#24948=DIRECTION('ref_axis',(0.,-0.707106781186547,0.707106781186548));
#24949=DIRECTION('center_axis',(1.,0.,1.38777878078144E-15));
#24950=DIRECTION('ref_axis',(-1.38777878078144E-15,0.,1.));
#24951=DIRECTION('',(1.,0.,0.));
#24952=DIRECTION('',(-1.,0.,0.));
#24953=DIRECTION('center_axis',(0.,0.,1.));
#24954=DIRECTION('ref_axis',(0.707106781186548,-0.707106781186547,0.));
#24955=DIRECTION('center_axis',(0.,0.,1.));
#24956=DIRECTION('ref_axis',(0.,-1.,0.));
#24957=DIRECTION('',(0.,0.,1.));
#24958=DIRECTION('',(0.,0.,-1.));
#24959=DIRECTION('center_axis',(0.,1.,0.));
#24960=DIRECTION('ref_axis',(0.707106781186548,0.,0.707106781186548));
#24961=DIRECTION('',(0.,-1.,0.));
#24962=DIRECTION('',(0.,1.,0.));
#24963=DIRECTION('center_axis',(0.408248290463864,-0.816496580927728,-0.408248290463859));
#24964=DIRECTION('ref_axis',(0.577350269189632,0.577350269189623,-0.577350269189623));
#24965=DIRECTION('center_axis',(0.,0.,-1.));
#24966=DIRECTION('ref_axis',(1.,0.,0.));
#24967=DIRECTION('center_axis',(0.,1.,0.));
#24968=DIRECTION('ref_axis',(0.,0.,-1.));
#24969=DIRECTION('center_axis',(1.,0.,0.));
#24970=DIRECTION('ref_axis',(0.,1.,0.));
#24971=DIRECTION('center_axis',(0.,1.,0.));
#24972=DIRECTION('ref_axis',(0.707106781186548,0.,-0.707106781186548));
#24973=DIRECTION('center_axis',(0.,1.,0.));
#24974=DIRECTION('ref_axis',(1.,0.,0.));
#24975=DIRECTION('',(0.,1.,0.));
#24976=DIRECTION('',(0.,-1.,0.));
#24977=DIRECTION('center_axis',(-1.,0.,0.));
#24978=DIRECTION('ref_axis',(0.,0.707106781186548,-0.707106781186548));
#24979=DIRECTION('',(1.,0.,0.));
#24980=DIRECTION('',(-1.,0.,0.));
#24981=DIRECTION('center_axis',(0.707106781186547,-0.707106781186549,0.));
#24982=DIRECTION('ref_axis',(0.707106781186548,0.707106781186546,0.));
#24983=DIRECTION('center_axis',(1.,0.,0.));
#24984=DIRECTION('ref_axis',(0.,0.707106781186548,0.707106781186548));
#24985=DIRECTION('',(1.,0.,0.));
#24986=DIRECTION('',(-1.,0.,0.));
#24987=DIRECTION('center_axis',(0.707106781186546,-0.707106781186549,-1.96261557335471E-15));
#24988=DIRECTION('ref_axis',(-0.707106781186549,-0.707106781186546,-1.9626155733547E-15));
#24989=DIRECTION('center_axis',(-0.408248290463864,-0.408248290463859,-0.816496580927728));
#24990=DIRECTION('ref_axis',(0.577350269189629,0.577350269189627,-0.577350269189622));
#24991=DIRECTION('center_axis',(0.,0.,-1.));
#24992=DIRECTION('ref_axis',(1.,0.,0.));
#24993=DIRECTION('center_axis',(0.,1.,0.));
#24994=DIRECTION('ref_axis',(0.,0.,-1.));
#24995=DIRECTION('center_axis',(1.,0.,-2.77555756156289E-15));
#24996=DIRECTION('ref_axis',(0.,1.,0.));
#24997=DIRECTION('center_axis',(0.,1.,0.));
#24998=DIRECTION('ref_axis',(0.707106781186548,0.,-0.707106781186548));
#24999=DIRECTION('',(0.,1.,0.));
#25000=DIRECTION('',(0.,-1.,0.));
#25001=DIRECTION('center_axis',(-1.,0.,0.));
#25002=DIRECTION('ref_axis',(0.,0.707106781186548,-0.707106781186548));
#25003=DIRECTION('center_axis',(1.,0.,-2.77555756156289E-15));
#25004=DIRECTION('ref_axis',(-2.77555756156289E-15,0.,-1.));
#25005=DIRECTION('',(1.,0.,0.));
#25006=DIRECTION('',(-1.,0.,0.));
#25007=DIRECTION('center_axis',(0.408248290463863,0.408248290463863,-0.816496580927726));
#25008=DIRECTION('ref_axis',(0.577350269189626,0.577350269189624,0.577350269189628));
#25009=DIRECTION('center_axis',(1.,-5.55111512312578E-15,0.));
#25010=DIRECTION('ref_axis',(0.,0.,1.));
#25011=DIRECTION('center_axis',(0.,1.,0.));
#25012=DIRECTION('ref_axis',(1.,0.,0.));
#25013=DIRECTION('center_axis',(0.,0.,1.));
#25014=DIRECTION('ref_axis',(0.,1.,0.));
#25015=DIRECTION('center_axis',(0.,1.,0.));
#25016=DIRECTION('ref_axis',(0.707106781186548,0.,0.707106781186548));
#25017=DIRECTION('',(0.,1.,0.));
#25018=DIRECTION('',(0.,-1.,0.));
#25019=DIRECTION('center_axis',(0.,0.,-1.));
#25020=DIRECTION('ref_axis',(0.707106781186548,0.707106781186548,0.));
#25021=DIRECTION('',(0.,0.,1.));
#25022=DIRECTION('',(0.,0.,-1.));
#25023=DIRECTION('center_axis',(-0.408248290463864,0.408248290463859,-0.816496580927728));
#25024=DIRECTION('ref_axis',(-0.577350269189629,0.577350269189627,0.577350269189622));
#25025=DIRECTION('center_axis',(0.,0.,1.));
#25026=DIRECTION('ref_axis',(-1.,0.,0.));
#25027=DIRECTION('center_axis',(0.,1.,0.));
#25028=DIRECTION('ref_axis',(0.,0.,1.));
#25029=DIRECTION('center_axis',(-1.,0.,2.77555756156289E-15));
#25030=DIRECTION('ref_axis',(0.,1.,0.));
#25031=DIRECTION('center_axis',(0.408248290463864,-0.816496580927728,-0.408248290463859));
#25032=DIRECTION('ref_axis',(-0.577350269189631,-0.577350269189624,0.577350269189622));
#25033=DIRECTION('center_axis',(0.,0.,1.));
#25034=DIRECTION('ref_axis',(0.,-1.,0.));
#25035=DIRECTION('center_axis',(-1.,0.,0.));
#25036=DIRECTION('ref_axis',(0.,0.,1.));
#25037=DIRECTION('center_axis',(0.,-1.,0.));
#25038=DIRECTION('ref_axis',(-1.,0.,0.));
#25039=DIRECTION('center_axis',(-1.,0.,0.));
#25040=DIRECTION('ref_axis',(0.,-0.707106781186547,0.707106781186548));
#25041=DIRECTION('center_axis',(-1.,0.,0.));
#25042=DIRECTION('ref_axis',(0.,-1.,0.));
#25043=DIRECTION('',(-1.,0.,0.));
#25044=DIRECTION('',(1.,0.,0.));
#25045=DIRECTION('center_axis',(-0.408248290463864,-0.816496580927728,0.408248290463859));
#25046=DIRECTION('ref_axis',(-0.577350269189632,0.577350269189623,0.577350269189623));
#25047=DIRECTION('center_axis',(0.,0.,1.));
#25048=DIRECTION('ref_axis',(-1.,0.,0.));
#25049=DIRECTION('center_axis',(0.,1.,0.));
#25050=DIRECTION('ref_axis',(0.,0.,1.));
#25051=DIRECTION('center_axis',(-1.,0.,0.));
#25052=DIRECTION('ref_axis',(0.,1.,0.));
#25053=DIRECTION('center_axis',(0.,1.,0.));
#25054=DIRECTION('ref_axis',(-0.707106781186548,0.,0.707106781186548));
#25055=DIRECTION('',(0.,-1.,0.));
#25056=DIRECTION('',(0.,1.,0.));
#25057=DIRECTION('center_axis',(1.,0.,0.));
#25058=DIRECTION('ref_axis',(0.,0.707106781186548,0.707106781186548));
#25059=DIRECTION('',(-1.,0.,0.));
#25060=DIRECTION('',(1.,0.,0.));
#25061=DIRECTION('center_axis',(-0.707106781186547,-0.707106781186549,0.));
#25062=DIRECTION('ref_axis',(-0.707106781186548,0.707106781186546,0.));
#25063=DIRECTION('center_axis',(-0.408248290463864,-0.816496580927723,-0.408248290463868));
#25064=DIRECTION('ref_axis',(-0.577350269189623,0.577350269189632,-0.577350269189623));
#25065=DIRECTION('center_axis',(0.,0.,-1.));
#25066=DIRECTION('ref_axis',(-1.,0.,0.));
#25067=DIRECTION('center_axis',(-1.,0.,0.));
#25068=DIRECTION('ref_axis',(0.,0.707106781186548,-0.707106781186548));
#25069=DIRECTION('center_axis',(0.,1.,0.));
#25070=DIRECTION('ref_axis',(-0.707106781186549,0.,-0.707106781186546));
#25071=DIRECTION('center_axis',(0.,0.,1.));
#25072=DIRECTION('ref_axis',(-0.707106781186548,0.707106781186548,0.));
#25073=DIRECTION('',(0.,0.,1.));
#25074=DIRECTION('',(0.,0.,-1.));
#25075=DIRECTION('center_axis',(0.,1.,0.));
#25076=DIRECTION('ref_axis',(-0.707106781186548,0.,0.707106781186548));
#25077=DIRECTION('',(0.,1.,0.));
#25078=DIRECTION('',(0.,-1.,0.));
#25079=DIRECTION('center_axis',(0.,0.,-1.));
#25080=DIRECTION('ref_axis',(-0.707106781186548,-0.707106781186547,0.));
#25081=DIRECTION('center_axis',(0.,0.,1.));
#25082=DIRECTION('ref_axis',(-1.,0.,0.));
#25083=DIRECTION('',(0.,0.,1.));
#25084=DIRECTION('',(0.,0.,-1.));
#25085=DIRECTION('center_axis',(0.408248290463864,-0.816496580927723,0.408248290463868));
#25086=DIRECTION('ref_axis',(-0.577350269189621,-0.577350269189627,-0.57735026918963));
#25087=DIRECTION('center_axis',(0.,-1.,0.));
#25088=DIRECTION('ref_axis',(-0.707106781186549,0.,-0.707106781186546));
#25089=DIRECTION('center_axis',(-1.,0.,0.));
#25090=DIRECTION('ref_axis',(0.,-0.707106781186546,-0.707106781186549));
#25091=DIRECTION('center_axis',(1.,0.,0.));
#25092=DIRECTION('ref_axis',(0.,0.707106781186548,0.707106781186548));
#25093=DIRECTION('',(-1.,0.,0.));
#25094=DIRECTION('',(1.,0.,0.));
#25095=DIRECTION('center_axis',(0.,0.,1.));
#25096=DIRECTION('ref_axis',(-0.707106781186548,0.707106781186548,0.));
#25097=DIRECTION('center_axis',(0.,0.,1.));
#25098=DIRECTION('ref_axis',(0.,1.,0.));
#25099=DIRECTION('',(0.,0.,1.));
#25100=DIRECTION('',(0.,0.,-1.));
#25101=DIRECTION('center_axis',(0.,0.,-1.));
#25102=DIRECTION('ref_axis',(0.707106781186548,0.707106781186548,0.));
#25103=DIRECTION('',(0.,0.,1.));
#25104=DIRECTION('',(0.,0.,-1.));
#25105=DIRECTION('center_axis',(0.408248290463864,-0.408248290463859,-0.816496580927728));
#25106=DIRECTION('ref_axis',(-0.57735026918963,0.577350269189624,-0.577350269189624));
#25107=DIRECTION('center_axis',(0.,1.,0.));
#25108=DIRECTION('ref_axis',(-0.707106781186549,0.,-0.707106781186546));
#25109=DIRECTION('center_axis',(0.,0.,-1.));
#25110=DIRECTION('ref_axis',(1.,0.,0.));
#25111=DIRECTION('center_axis',(0.,0.,-1.));
#25112=DIRECTION('ref_axis',(1.,0.,0.));
#25113=DIRECTION('center_axis',(-0.408248290463864,-0.816496580927727,0.40824829046386));
#25114=DIRECTION('ref_axis',(0.577350269189628,-0.577350269189625,-0.577350269189624));
#25115=DIRECTION('center_axis',(1.,0.,0.));
#25116=DIRECTION('ref_axis',(0.,-0.707106781186546,-0.707106781186549));
#25117=DIRECTION('center_axis',(1.,0.,0.));
#25118=DIRECTION('ref_axis',(0.,0.,-1.));
#25119=DIRECTION('',(0.,0.,1.));
#25120=DIRECTION('center_axis',(0.,1.,0.));
#25121=DIRECTION('ref_axis',(1.,0.,0.));
#25122=DIRECTION('',(-1.,0.,0.));
#25123=DIRECTION('center_axis',(0.,-1.,0.));
#25124=DIRECTION('ref_axis',(1.,0.,0.));
#25125=DIRECTION('center_axis',(0.,-1.,0.));
#25126=DIRECTION('ref_axis',(1.,0.,0.));
#25127=DIRECTION('center_axis',(-1.,0.,0.));
#25128=DIRECTION('ref_axis',(0.,0.,1.));
#25129=DIRECTION('',(0.,1.,0.));
#25130=DIRECTION('center_axis',(0.,1.,0.));
#25131=DIRECTION('ref_axis',(-0.707106781186548,0.,-0.707106781186548));
#25132=DIRECTION('',(0.,-1.,0.));
#25133=DIRECTION('center_axis',(1.,0.,0.));
#25134=DIRECTION('ref_axis',(0.,0.,-1.));
#25135=DIRECTION('center_axis',(0.,1.,0.));
#25136=DIRECTION('ref_axis',(0.,0.,1.));
#25137=DIRECTION('center_axis',(1.,0.,0.));
#25138=DIRECTION('ref_axis',(0.,-0.707106781186547,-0.707106781186548));
#25139=DIRECTION('',(1.,0.,0.));
#25140=DIRECTION('center_axis',(-1.,0.,0.));
#25141=DIRECTION('ref_axis',(0.,0.707106781186548,-0.707106781186548));
#25142=DIRECTION('',(1.,0.,0.));
#25143=DIRECTION('center_axis',(-0.707106781186546,-0.707106781186549,1.96261557335471E-15));
#25144=DIRECTION('ref_axis',(0.707106781186549,-0.707106781186546,1.9626155733547E-15));
#25145=DIRECTION('',(-1.,0.,0.));
#25146=DIRECTION('center_axis',(0.,1.,0.));
#25147=DIRECTION('ref_axis',(-0.707106781186548,0.,-0.707106781186548));
#25148=DIRECTION('',(0.,-1.,0.));
#25149=DIRECTION('',(0.,1.,0.));
#25150=DIRECTION('center_axis',(0.,1.,0.));
#25151=DIRECTION('ref_axis',(0.,0.,1.));
#25152=DIRECTION('',(0.,0.,-1.));
#25153=DIRECTION('center_axis',(0.,0.,1.));
#25154=DIRECTION('ref_axis',(1.,0.,0.));
#25155=DIRECTION('center_axis',(0.,0.,-1.));
#25156=DIRECTION('ref_axis',(1.,0.,0.));
#25157=DIRECTION('center_axis',(0.,-1.,0.));
#25158=DIRECTION('ref_axis',(-1.,0.,0.));
#25159=DIRECTION('center_axis',(0.,0.,1.));
#25160=DIRECTION('ref_axis',(1.,0.,0.));
#25161=DIRECTION('center_axis',(0.,0.,1.));
#25162=DIRECTION('ref_axis',(1.,0.,0.));
#25163=DIRECTION('center_axis',(0.,0.,1.));
#25164=DIRECTION('ref_axis',(1.,0.,0.));
#25165=DIRECTION('',(0.,0.,1.));
#25166=DIRECTION('center_axis',(0.,0.,1.));
#25167=DIRECTION('ref_axis',(1.,0.,0.));
#25168=DIRECTION('center_axis',(0.,0.,-1.));
#25169=DIRECTION('ref_axis',(1.,0.,0.));
#25170=DIRECTION('center_axis',(1.81408990951823E-16,-1.,0.));
#25171=DIRECTION('ref_axis',(-1.,-1.81408990951823E-16,0.));
#25172=DIRECTION('center_axis',(0.,0.,1.));
#25173=DIRECTION('ref_axis',(1.,0.,0.));
#25174=DIRECTION('center_axis',(0.,0.,1.));
#25175=DIRECTION('ref_axis',(1.,0.,0.));
#25176=DIRECTION('center_axis',(0.,0.,1.));
#25177=DIRECTION('ref_axis',(-1.,0.,0.));
#25178=DIRECTION('center_axis',(0.,0.,1.));
#25179=DIRECTION('ref_axis',(1.,0.,0.));
#25180=DIRECTION('',(0.,0.,-1.));
#25181=DIRECTION('center_axis',(0.,0.,-1.));
#25182=DIRECTION('ref_axis',(1.,0.,0.));
#25183=DIRECTION('center_axis',(0.,0.,-1.));
#25184=DIRECTION('ref_axis',(1.,0.,0.));
#25185=DIRECTION('center_axis',(0.,0.,-1.));
#25186=DIRECTION('ref_axis',(1.,0.,0.));
#25187=DIRECTION('center_axis',(0.,0.,-1.));
#25188=DIRECTION('ref_axis',(1.,0.,0.));
#25189=DIRECTION('center_axis',(0.,0.,-1.));
#25190=DIRECTION('ref_axis',(1.,0.,0.));
#25191=DIRECTION('center_axis',(0.,0.,-1.));
#25192=DIRECTION('ref_axis',(1.,0.,0.));
#25193=DIRECTION('center_axis',(0.,0.,1.));
#25194=DIRECTION('ref_axis',(-1.,0.,0.));
#25195=DIRECTION('center_axis',(0.,0.,-1.));
#25196=DIRECTION('ref_axis',(1.,0.,0.));
#25197=DIRECTION('center_axis',(-1.82088236683647E-16,1.,0.));
#25198=DIRECTION('ref_axis',(1.,1.82088236683647E-16,0.));
#25199=DIRECTION('center_axis',(0.,1.,0.));
#25200=DIRECTION('ref_axis',(0.,0.,1.));
#25201=DIRECTION('center_axis',(-1.,0.,0.));
#25202=DIRECTION('ref_axis',(0.,0.,-1.));
#25203=DIRECTION('center_axis',(0.,1.,0.));
#25204=DIRECTION('ref_axis',(1.,0.,0.));
#25205=DIRECTION('center_axis',(0.,1.,0.));
#25206=DIRECTION('ref_axis',(1.,0.,0.));
#25207=DIRECTION('center_axis',(0.,1.,0.));
#25208=DIRECTION('ref_axis',(1.,0.,0.));
#25209=DIRECTION('',(0.,1.,0.));
#25210=DIRECTION('center_axis',(0.,1.,0.));
#25211=DIRECTION('ref_axis',(1.,0.,0.));
#25212=DIRECTION('center_axis',(0.,1.,0.));
#25213=DIRECTION('ref_axis',(0.,0.,1.));
#25214=DIRECTION('center_axis',(-1.,0.,0.));
#25215=DIRECTION('ref_axis',(0.,0.,-1.));
#25216=DIRECTION('center_axis',(0.,1.,0.));
#25217=DIRECTION('ref_axis',(1.,0.,0.));
#25218=DIRECTION('center_axis',(0.,1.,0.));
#25219=DIRECTION('ref_axis',(1.,0.,0.));
#25220=DIRECTION('center_axis',(0.,1.,0.));
#25221=DIRECTION('ref_axis',(1.,0.,0.));
#25222=DIRECTION('',(0.,1.,0.));
#25223=DIRECTION('center_axis',(0.,1.,0.));
#25224=DIRECTION('ref_axis',(1.,0.,0.));
#25225=DIRECTION('center_axis',(0.,-1.,0.));
#25226=DIRECTION('ref_axis',(0.921659373087477,0.,0.387999999999999));
#25227=DIRECTION('',(0.,-1.,0.));
#25228=DIRECTION('center_axis',(-0.707106781186547,0.707106781186548,9.8130778667736E-16));
#25229=DIRECTION('ref_axis',(0.707106781186548,0.707106781186547,-9.81307786677362E-16));
#25230=DIRECTION('',(0.,1.,0.));
#25231=DIRECTION('center_axis',(-0.707106781186548,-0.707106781186547,5.88784672006415E-15));
#25232=DIRECTION('ref_axis',(-0.707106781186547,0.707106781186548,5.88784672006415E-15));
#25233=DIRECTION('center_axis',(1.,0.,0.));
#25234=DIRECTION('ref_axis',(0.,0.921659373087477,0.387999999999999));
#25235=DIRECTION('',(-1.,0.,0.));
#25236=DIRECTION('',(1.,0.,0.));
#25237=DIRECTION('center_axis',(-1.,0.,0.));
#25238=DIRECTION('ref_axis',(0.,-0.921659373087476,0.388));
#25239=DIRECTION('',(-1.,0.,0.));
#25240=DIRECTION('',(1.,0.,0.));
#25241=DIRECTION('center_axis',(1.08557947792634E-16,-4.02936130515309E-16,
-1.));
#25242=DIRECTION('ref_axis',(-0.97786928031163,-0.209216802917009,0.));
#25243=DIRECTION('center_axis',(0.,0.,1.));
#25244=DIRECTION('ref_axis',(1.,0.,0.));
#25245=DIRECTION('center_axis',(-2.11382759593089E-16,-7.1112105974302E-16,
1.));
#25246=DIRECTION('ref_axis',(0.965794610306648,-0.259308254212299,0.));
#25247=DIRECTION('center_axis',(0.,0.,1.));
#25248=DIRECTION('ref_axis',(1.,0.,0.));
#25249=DIRECTION('center_axis',(0.,0.,1.));
#25250=DIRECTION('ref_axis',(1.,0.,0.));
#25251=DIRECTION('',(-1.,0.,0.));
#25252=DIRECTION('',(0.,1.,0.));
#25253=DIRECTION('',(1.,0.,0.));
#25254=DIRECTION('center_axis',(1.,0.,0.));
#25255=DIRECTION('ref_axis',(0.,0.921659373087477,0.387999999999999));
#25256=DIRECTION('center_axis',(-0.707106781186548,-0.707106781186547,1.96261557335472E-15));
#25257=DIRECTION('ref_axis',(-0.707106781186547,0.707106781186548,-1.96261557335472E-15));
#25258=DIRECTION('',(-1.,0.,0.));
#25259=DIRECTION('center_axis',(-1.,0.,0.));
#25260=DIRECTION('ref_axis',(0.,-0.921659373087476,0.388));
#25261=DIRECTION('',(1.,0.,0.));
#25262=DIRECTION('center_axis',(-0.707106781186546,0.707106781186549,0.));
#25263=DIRECTION('ref_axis',(0.707106781186549,0.707106781186546,0.));
#25264=DIRECTION('center_axis',(0.,1.,0.));
#25265=DIRECTION('ref_axis',(-0.921659373087477,0.,0.387999999999999));
#25266=DIRECTION('',(0.,-1.,0.));
#25267=DIRECTION('center_axis',(0.,0.,1.));
#25268=DIRECTION('ref_axis',(-1.,0.,0.));
#25269=DIRECTION('center_axis',(0.,0.,-1.));
#25270=DIRECTION('ref_axis',(1.,0.,0.));
#25271=DIRECTION('center_axis',(0.,1.,0.));
#25272=DIRECTION('ref_axis',(1.,0.,0.));
#25273=DIRECTION('center_axis',(0.,0.,1.));
#25274=DIRECTION('ref_axis',(-1.,0.,0.));
#25275=DIRECTION('center_axis',(0.,0.,1.));
#25276=DIRECTION('ref_axis',(1.,0.,0.));
#25277=DIRECTION('center_axis',(0.,0.,1.));
#25278=DIRECTION('ref_axis',(-1.,0.,0.));
#25279=DIRECTION('center_axis',(0.,0.,1.));
#25280=DIRECTION('ref_axis',(-1.,0.,0.));
#25281=DIRECTION('center_axis',(0.,0.,-1.));
#25282=DIRECTION('ref_axis',(1.,0.,0.));
#25283=DIRECTION('center_axis',(0.,1.,0.));
#25284=DIRECTION('ref_axis',(1.,0.,0.));
#25285=DIRECTION('center_axis',(0.,0.,1.));
#25286=DIRECTION('ref_axis',(-1.,0.,0.));
#25287=DIRECTION('center_axis',(0.,0.,-1.));
#25288=DIRECTION('ref_axis',(1.,0.,0.));
#25289=DIRECTION('center_axis',(0.,1.,0.));
#25290=DIRECTION('ref_axis',(1.,0.,0.));
#25291=DIRECTION('center_axis',(0.,0.,1.));
#25292=DIRECTION('ref_axis',(-1.,0.,0.));
#25293=DIRECTION('center_axis',(0.,0.,1.));
#25294=DIRECTION('ref_axis',(1.,0.,0.));
#25295=DIRECTION('center_axis',(0.,0.,1.));
#25296=DIRECTION('ref_axis',(-1.,0.,0.));
#25297=DIRECTION('center_axis',(0.,0.,1.));
#25298=DIRECTION('ref_axis',(-1.,0.,0.));
#25299=DIRECTION('center_axis',(0.,0.,-1.));
#25300=DIRECTION('ref_axis',(1.,0.,0.));
#25301=DIRECTION('center_axis',(0.,1.,0.));
#25302=DIRECTION('ref_axis',(1.,0.,0.));
#25303=DIRECTION('center_axis',(0.,0.,-1.));
#25304=DIRECTION('ref_axis',(-1.,0.,0.));
#25305=DIRECTION('center_axis',(0.,0.,1.));
#25306=DIRECTION('ref_axis',(1.,0.,0.));
#25307=DIRECTION('center_axis',(0.,-1.,0.));
#25308=DIRECTION('ref_axis',(1.,0.,0.));
#25309=DIRECTION('center_axis',(0.,0.,-1.));
#25310=DIRECTION('ref_axis',(1.,0.,0.));
#25311=DIRECTION('center_axis',(0.,0.,1.));
#25312=DIRECTION('ref_axis',(1.,0.,0.));
#25313=DIRECTION('center_axis',(0.,0.,1.));
#25314=DIRECTION('ref_axis',(1.,0.,0.));
#25315=DIRECTION('center_axis',(0.,0.,1.));
#25316=DIRECTION('ref_axis',(1.,0.,0.));
#25317=DIRECTION('center_axis',(0.,0.,1.));
#25318=DIRECTION('ref_axis',(1.,0.,0.));
#25319=DIRECTION('center_axis',(0.,0.,1.));
#25320=DIRECTION('ref_axis',(1.,0.,0.));
#25321=DIRECTION('center_axis',(0.,1.,0.));
#25322=DIRECTION('ref_axis',(1.,0.,0.));
#25323=DIRECTION('center_axis',(0.,1.,0.));
#25324=DIRECTION('ref_axis',(1.,0.,0.));
#25325=DIRECTION('center_axis',(0.,0.,1.));
#25326=DIRECTION('ref_axis',(1.,0.,0.));
#25327=DIRECTION('center_axis',(0.,0.,1.));
#25328=DIRECTION('ref_axis',(1.,0.,0.));
#25329=DIRECTION('center_axis',(0.,0.,1.));
#25330=DIRECTION('ref_axis',(1.,0.,0.));
#25331=DIRECTION('center_axis',(0.,0.,-1.));
#25332=DIRECTION('ref_axis',(1.,0.,0.));
#25333=DIRECTION('center_axis',(0.,0.,1.));
#25334=DIRECTION('ref_axis',(1.,0.,0.));
#25335=DIRECTION('',(-0.707106781186547,8.65956056235493E-17,-0.707106781186548));
#25336=DIRECTION('center_axis',(0.,0.,-1.));
#25337=DIRECTION('ref_axis',(1.,0.,0.));
#25338=DIRECTION('center_axis',(0.,0.,1.));
#25339=DIRECTION('ref_axis',(1.,0.,0.));
#25340=DIRECTION('',(0.,0.,1.));
#25341=DIRECTION('center_axis',(0.,0.,-1.));
#25342=DIRECTION('ref_axis',(-1.,0.,0.));
#25343=DIRECTION('center_axis',(-1.,0.,0.));
#25344=DIRECTION('ref_axis',(0.,0.,1.));
#25345=DIRECTION('center_axis',(0.,1.,0.));
#25346=DIRECTION('ref_axis',(0.,0.,1.));
#25347=DIRECTION('axis',(0.,0.,1.));
#25348=DIRECTION('refdir',(1.,0.,0.));
#25349=DIRECTION('center_axis',(1.,0.,0.));
#25350=DIRECTION('ref_axis',(0.,-1.,0.));
#25351=DIRECTION('center_axis',(-1.,0.,0.));
#25352=DIRECTION('ref_axis',(0.,-1.,0.));
#25353=DIRECTION('',(-0.707106781186548,-0.707106781186547,-8.65956056235493E-17));
#25354=DIRECTION('center_axis',(1.,0.,0.));
#25355=DIRECTION('ref_axis',(0.,-1.,0.));
#25356=DIRECTION('center_axis',(-1.,0.,0.));
#25357=DIRECTION('ref_axis',(0.,-1.,0.));
#25358=DIRECTION('center_axis',(1.,0.,0.));
#25359=DIRECTION('ref_axis',(0.,1.,0.));
#25360=DIRECTION('center_axis',(1.,0.,0.));
#25361=DIRECTION('ref_axis',(0.,-1.,0.));
#25362=DIRECTION('center_axis',(1.,0.,0.));
#25363=DIRECTION('ref_axis',(0.,-1.,0.));
#25364=DIRECTION('',(-1.,0.,0.));
#25365=DIRECTION('center_axis',(-1.,0.,0.));
#25366=DIRECTION('ref_axis',(0.,0.,1.));
#25367=DIRECTION('center_axis',(1.,0.,0.));
#25368=DIRECTION('ref_axis',(0.,0.,-1.));
#25369=DIRECTION('center_axis',(-1.,0.,0.));
#25370=DIRECTION('ref_axis',(0.,-1.,0.));
#25371=DIRECTION('',(0.707106781186548,-0.707106781186547,8.65956056235493E-17));
#25372=DIRECTION('center_axis',(-1.,0.,0.));
#25373=DIRECTION('ref_axis',(0.,-1.,0.));
#25374=DIRECTION('center_axis',(1.,0.,0.));
#25375=DIRECTION('ref_axis',(0.,0.,-1.));
#25376=DIRECTION('center_axis',(-1.,0.,0.));
#25377=DIRECTION('ref_axis',(0.,0.,-1.));
#25378=DIRECTION('',(0.,-0.668692731746348,-0.743538856085952));
#25379=DIRECTION('',(0.,0.623489801858733,-0.78183148246803));
#25380=DIRECTION('',(0.,0.873694915787935,0.486474248163572));
#25381=DIRECTION('center_axis',(-1.,0.,0.));
#25382=DIRECTION('ref_axis',(0.,0.,-1.));
#25383=DIRECTION('',(0.,-0.925080752553848,-0.37977045863838));
#25384=DIRECTION('',(0.,0.222520933956314,-0.974927912181824));
#25385=DIRECTION('',(0.,0.998245184947169,0.0592161357215442));
#25386=DIRECTION('center_axis',(-1.,0.,0.));
#25387=DIRECTION('ref_axis',(0.,0.,-1.));
#25388=DIRECTION('',(0.,-0.998245184947169,0.0592161357215445));
#25389=DIRECTION('',(0.,-0.222520933956315,-0.974927912181824));
#25390=DIRECTION('',(0.,0.925080752553848,-0.37977045863838));
#25391=DIRECTION('center_axis',(-1.,0.,0.));
#25392=DIRECTION('ref_axis',(0.,0.,-1.));
#25393=DIRECTION('',(0.,-0.873694915787935,0.486474248163572));
#25394=DIRECTION('',(0.,-0.623489801858734,-0.78183148246803));
#25395=DIRECTION('',(0.,0.668692731746348,-0.743538856085952));
#25396=DIRECTION('center_axis',(-1.,0.,0.));
#25397=DIRECTION('ref_axis',(0.,0.,-1.));
#25398=DIRECTION('',(0.,-0.576098653391942,0.817380169541683));
#25399=DIRECTION('',(0.,-0.900968867902419,-0.433883739117558));
#25400=DIRECTION('',(0.,0.279861914438318,-0.96004026418006));
#25401=DIRECTION('center_axis',(-1.,0.,0.));
#25402=DIRECTION('ref_axis',(0.,0.,-1.));
#25403=DIRECTION('',(0.,-0.164398987305357,0.986393923832144));
#25404=DIRECTION('',(0.,-1.,1.22464679914735E-16));
#25405=DIRECTION('',(0.,-0.164398987305357,-0.986393923832144));
#25406=DIRECTION('center_axis',(-1.,0.,0.));
#25407=DIRECTION('ref_axis',(0.,0.,-1.));
#25408=DIRECTION('',(0.,0.279861914438319,0.96004026418006));
#25409=DIRECTION('',(0.,-0.900968867902419,0.433883739117558));
#25410=DIRECTION('',(0.,-0.576098653391942,-0.817380169541683));
#25411=DIRECTION('center_axis',(-1.,0.,0.));
#25412=DIRECTION('ref_axis',(0.,0.,-1.));
#25413=DIRECTION('',(0.,0.668692731746348,0.743538856085952));
#25414=DIRECTION('',(0.,-0.623489801858733,0.78183148246803));
#25415=DIRECTION('',(0.,-0.873694915787935,-0.486474248163572));
#25416=DIRECTION('center_axis',(-1.,0.,0.));
#25417=DIRECTION('ref_axis',(0.,0.,-1.));
#25418=DIRECTION('',(0.,0.925080752553848,0.37977045863838));
#25419=DIRECTION('',(0.,-0.222520933956314,0.974927912181824));
#25420=DIRECTION('',(0.,-0.998245184947169,-0.0592161357215443));
#25421=DIRECTION('center_axis',(-1.,0.,0.));
#25422=DIRECTION('ref_axis',(0.,0.,-1.));
#25423=DIRECTION('',(0.,0.998245184947169,-0.0592161357215444));
#25424=DIRECTION('',(0.,0.222520933956314,0.974927912181824));
#25425=DIRECTION('',(0.,-0.925080752553848,0.37977045863838));
#25426=DIRECTION('center_axis',(-1.,0.,0.));
#25427=DIRECTION('ref_axis',(0.,0.,-1.));
#25428=DIRECTION('',(0.,0.873694915787935,-0.486474248163572));
#25429=DIRECTION('',(0.,0.623489801858734,0.78183148246803));
#25430=DIRECTION('',(0.,-0.668692731746348,0.743538856085952));
#25431=DIRECTION('center_axis',(-1.,0.,0.));
#25432=DIRECTION('ref_axis',(0.,0.,-1.));
#25433=DIRECTION('',(0.,0.576098653391942,-0.817380169541683));
#25434=DIRECTION('',(0.,0.900968867902419,0.433883739117558));
#25435=DIRECTION('',(0.,-0.279861914438319,0.96004026418006));
#25436=DIRECTION('center_axis',(-1.,0.,0.));
#25437=DIRECTION('ref_axis',(0.,0.,-1.));
#25438=DIRECTION('',(0.,0.164398987305357,-0.986393923832144));
#25439=DIRECTION('',(0.,1.,0.));
#25440=DIRECTION('',(0.,0.164398987305357,0.986393923832144));
#25441=DIRECTION('center_axis',(-1.,0.,0.));
#25442=DIRECTION('ref_axis',(0.,0.,-1.));
#25443=DIRECTION('',(0.,-0.279861914438319,-0.96004026418006));
#25444=DIRECTION('',(0.,0.900968867902419,-0.433883739117558));
#25445=DIRECTION('',(0.,0.576098653391942,0.817380169541683));
#25446=DIRECTION('center_axis',(0.,-0.96004026418006,0.279861914438319));
#25447=DIRECTION('ref_axis',(0.,-0.279861914438319,-0.96004026418006));
#25448=DIRECTION('',(1.,0.,0.));
#25449=DIRECTION('',(0.,0.279861914438319,0.96004026418006));
#25450=DIRECTION('',(1.,0.,0.));
#25451=DIRECTION('center_axis',(0.,0.817380169541683,-0.576098653391942));
#25452=DIRECTION('ref_axis',(0.,0.576098653391942,0.817380169541683));
#25453=DIRECTION('',(-1.,0.,0.));
#25454=DIRECTION('',(1.,0.,0.));
#25455=DIRECTION('',(0.,-0.576098653391942,-0.817380169541683));
#25456=DIRECTION('center_axis',(0.,-0.433883739117558,-0.900968867902419));
#25457=DIRECTION('ref_axis',(0.,0.900968867902419,-0.433883739117558));
#25458=DIRECTION('',(0.,-0.900968867902419,0.433883739117558));
#25459=DIRECTION('center_axis',(1.,0.,0.));
#25460=DIRECTION('ref_axis',(0.,0.,-1.));
#25461=DIRECTION('center_axis',(1.,0.,0.));
#25462=DIRECTION('ref_axis',(0.,0.,-1.));
#25463=DIRECTION('',(1.,0.,0.));
#25464=DIRECTION('center_axis',(0.,-0.743538856085952,0.668692731746348));
#25465=DIRECTION('ref_axis',(0.,-0.668692731746348,-0.743538856085952));
#25466=DIRECTION('',(0.,0.668692731746348,0.743538856085952));
#25467=DIRECTION('',(1.,0.,0.));
#25468=DIRECTION('center_axis',(0.,0.486474248163572,-0.873694915787935));
#25469=DIRECTION('ref_axis',(0.,0.873694915787935,0.486474248163572));
#25470=DIRECTION('',(-1.,0.,0.));
#25471=DIRECTION('',(1.,0.,0.));
#25472=DIRECTION('',(0.,-0.873694915787935,-0.486474248163572));
#25473=DIRECTION('center_axis',(0.,-0.78183148246803,-0.623489801858733));
#25474=DIRECTION('ref_axis',(0.,0.623489801858733,-0.78183148246803));
#25475=DIRECTION('',(0.,-0.623489801858733,0.78183148246803));
#25476=DIRECTION('center_axis',(1.,0.,0.));
#25477=DIRECTION('ref_axis',(0.,0.,-1.));
#25478=DIRECTION('center_axis',(1.,0.,0.));
#25479=DIRECTION('ref_axis',(0.,0.,-1.));
#25480=DIRECTION('',(1.,0.,0.));
#25481=DIRECTION('center_axis',(0.,-0.37977045863838,0.925080752553848));
#25482=DIRECTION('ref_axis',(0.,-0.925080752553848,-0.37977045863838));
#25483=DIRECTION('',(0.,0.925080752553848,0.37977045863838));
#25484=DIRECTION('',(1.,0.,0.));
#25485=DIRECTION('center_axis',(0.,0.0592161357215442,-0.998245184947169));
#25486=DIRECTION('ref_axis',(0.,0.998245184947169,0.0592161357215442));
#25487=DIRECTION('',(-1.,0.,0.));
#25488=DIRECTION('',(1.,0.,0.));
#25489=DIRECTION('',(0.,-0.998245184947169,-0.0592161357215442));
#25490=DIRECTION('center_axis',(0.,-0.974927912181824,-0.222520933956314));
#25491=DIRECTION('ref_axis',(0.,0.222520933956314,-0.974927912181824));
#25492=DIRECTION('',(0.,-0.222520933956314,0.974927912181824));
#25493=DIRECTION('center_axis',(1.,0.,0.));
#25494=DIRECTION('ref_axis',(0.,0.,-1.));
#25495=DIRECTION('center_axis',(1.,0.,0.));
#25496=DIRECTION('ref_axis',(0.,0.,-1.));
#25497=DIRECTION('',(1.,0.,0.));
#25498=DIRECTION('center_axis',(0.,0.0592161357215445,0.998245184947169));
#25499=DIRECTION('ref_axis',(0.,-0.998245184947169,0.0592161357215445));
#25500=DIRECTION('',(0.,0.998245184947169,-0.0592161357215445));
#25501=DIRECTION('',(1.,0.,0.));
#25502=DIRECTION('center_axis',(0.,-0.37977045863838,-0.925080752553848));
#25503=DIRECTION('ref_axis',(0.,0.925080752553848,-0.37977045863838));
#25504=DIRECTION('',(-1.,0.,0.));
#25505=DIRECTION('',(1.,0.,0.));
#25506=DIRECTION('',(0.,-0.925080752553848,0.37977045863838));
#25507=DIRECTION('center_axis',(0.,-0.974927912181824,0.222520933956315));
#25508=DIRECTION('ref_axis',(0.,-0.222520933956315,-0.974927912181824));
#25509=DIRECTION('',(0.,0.222520933956315,0.974927912181824));
#25510=DIRECTION('center_axis',(1.,0.,0.));
#25511=DIRECTION('ref_axis',(0.,0.,-1.));
#25512=DIRECTION('center_axis',(1.,0.,0.));
#25513=DIRECTION('ref_axis',(0.,0.,-1.));
#25514=DIRECTION('',(1.,0.,0.));
#25515=DIRECTION('center_axis',(0.,0.486474248163572,0.873694915787935));
#25516=DIRECTION('ref_axis',(0.,-0.873694915787935,0.486474248163572));
#25517=DIRECTION('',(0.,0.873694915787935,-0.486474248163572));
#25518=DIRECTION('',(1.,0.,0.));
#25519=DIRECTION('center_axis',(0.,-0.743538856085952,-0.668692731746348));
#25520=DIRECTION('ref_axis',(0.,0.668692731746348,-0.743538856085952));
#25521=DIRECTION('',(-1.,0.,0.));
#25522=DIRECTION('',(1.,0.,0.));
#25523=DIRECTION('',(0.,-0.668692731746348,0.743538856085952));
#25524=DIRECTION('center_axis',(0.,-0.78183148246803,0.623489801858734));
#25525=DIRECTION('ref_axis',(0.,-0.623489801858734,-0.78183148246803));
#25526=DIRECTION('',(0.,0.623489801858734,0.78183148246803));
#25527=DIRECTION('center_axis',(1.,0.,0.));
#25528=DIRECTION('ref_axis',(0.,0.,-1.));
#25529=DIRECTION('center_axis',(1.,0.,0.));
#25530=DIRECTION('ref_axis',(0.,0.,-1.));
#25531=DIRECTION('',(1.,0.,0.));
#25532=DIRECTION('center_axis',(0.,0.817380169541683,0.576098653391942));
#25533=DIRECTION('ref_axis',(0.,-0.576098653391942,0.817380169541683));
#25534=DIRECTION('',(0.,0.576098653391942,-0.817380169541683));
#25535=DIRECTION('',(1.,0.,0.));
#25536=DIRECTION('center_axis',(0.,-0.96004026418006,-0.279861914438318));
#25537=DIRECTION('ref_axis',(0.,0.279861914438318,-0.96004026418006));
#25538=DIRECTION('',(-1.,0.,0.));
#25539=DIRECTION('',(1.,0.,0.));
#25540=DIRECTION('',(0.,-0.279861914438318,0.96004026418006));
#25541=DIRECTION('center_axis',(0.,-0.433883739117558,0.900968867902419));
#25542=DIRECTION('ref_axis',(0.,-0.900968867902419,-0.433883739117558));
#25543=DIRECTION('',(0.,0.900968867902419,0.433883739117558));
#25544=DIRECTION('center_axis',(1.,0.,0.));
#25545=DIRECTION('ref_axis',(0.,0.,-1.));
#25546=DIRECTION('center_axis',(1.,0.,0.));
#25547=DIRECTION('ref_axis',(0.,0.,-1.));
#25548=DIRECTION('',(1.,0.,0.));
#25549=DIRECTION('center_axis',(0.,0.986393923832144,0.164398987305357));
#25550=DIRECTION('ref_axis',(0.,-0.164398987305357,0.986393923832144));
#25551=DIRECTION('',(0.,0.164398987305357,-0.986393923832144));
#25552=DIRECTION('',(1.,0.,0.));
#25553=DIRECTION('center_axis',(0.,-0.986393923832144,0.164398987305357));
#25554=DIRECTION('ref_axis',(0.,-0.164398987305357,-0.986393923832144));
#25555=DIRECTION('',(-1.,0.,0.));
#25556=DIRECTION('',(1.,0.,0.));
#25557=DIRECTION('',(0.,0.164398987305357,0.986393923832144));
#25558=DIRECTION('center_axis',(0.,1.22464679914735E-16,1.));
#25559=DIRECTION('ref_axis',(0.,-1.,1.22464679914735E-16));
#25560=DIRECTION('',(0.,1.,-1.22464679914735E-16));
#25561=DIRECTION('center_axis',(1.,0.,0.));
#25562=DIRECTION('ref_axis',(0.,0.,-1.));
#25563=DIRECTION('center_axis',(1.,0.,0.));
#25564=DIRECTION('ref_axis',(0.,0.,-1.));
#25565=DIRECTION('',(1.,0.,0.));
#25566=DIRECTION('center_axis',(0.,0.96004026418006,-0.279861914438319));
#25567=DIRECTION('ref_axis',(0.,0.279861914438319,0.96004026418006));
#25568=DIRECTION('',(0.,-0.279861914438319,-0.96004026418006));
#25569=DIRECTION('',(1.,0.,0.));
#25570=DIRECTION('center_axis',(0.,-0.817380169541683,0.576098653391942));
#25571=DIRECTION('ref_axis',(0.,-0.576098653391942,-0.817380169541683));
#25572=DIRECTION('',(-1.,0.,0.));
#25573=DIRECTION('',(1.,0.,0.));
#25574=DIRECTION('',(0.,0.576098653391942,0.817380169541683));
#25575=DIRECTION('center_axis',(0.,0.433883739117558,0.900968867902419));
#25576=DIRECTION('ref_axis',(0.,-0.900968867902419,0.433883739117558));
#25577=DIRECTION('',(0.,0.900968867902419,-0.433883739117558));
#25578=DIRECTION('center_axis',(1.,0.,0.));
#25579=DIRECTION('ref_axis',(0.,0.,-1.));
#25580=DIRECTION('center_axis',(1.,0.,0.));
#25581=DIRECTION('ref_axis',(0.,0.,-1.));
#25582=DIRECTION('',(1.,0.,0.));
#25583=DIRECTION('center_axis',(0.,0.743538856085952,-0.668692731746348));
#25584=DIRECTION('ref_axis',(0.,0.668692731746348,0.743538856085952));
#25585=DIRECTION('',(0.,-0.668692731746348,-0.743538856085952));
#25586=DIRECTION('',(1.,0.,0.));
#25587=DIRECTION('center_axis',(0.,-0.486474248163572,0.873694915787935));
#25588=DIRECTION('ref_axis',(0.,-0.873694915787935,-0.486474248163572));
#25589=DIRECTION('',(-1.,0.,0.));
#25590=DIRECTION('',(1.,0.,0.));
#25591=DIRECTION('',(0.,0.873694915787935,0.486474248163572));
#25592=DIRECTION('center_axis',(0.,0.78183148246803,0.623489801858733));
#25593=DIRECTION('ref_axis',(0.,-0.623489801858733,0.78183148246803));
#25594=DIRECTION('',(0.,0.623489801858733,-0.78183148246803));
#25595=DIRECTION('center_axis',(1.,0.,0.));
#25596=DIRECTION('ref_axis',(0.,0.,-1.));
#25597=DIRECTION('center_axis',(1.,0.,0.));
#25598=DIRECTION('ref_axis',(0.,0.,-1.));
#25599=DIRECTION('',(1.,0.,0.));
#25600=DIRECTION('center_axis',(0.,0.37977045863838,-0.925080752553848));
#25601=DIRECTION('ref_axis',(0.,0.925080752553848,0.37977045863838));
#25602=DIRECTION('',(0.,-0.925080752553848,-0.37977045863838));
#25603=DIRECTION('',(1.,0.,0.));
#25604=DIRECTION('center_axis',(0.,-0.0592161357215443,0.998245184947169));
#25605=DIRECTION('ref_axis',(0.,-0.998245184947169,-0.0592161357215443));
#25606=DIRECTION('',(-1.,0.,0.));
#25607=DIRECTION('',(1.,0.,0.));
#25608=DIRECTION('',(0.,0.998245184947169,0.0592161357215443));
#25609=DIRECTION('center_axis',(0.,0.974927912181824,0.222520933956314));
#25610=DIRECTION('ref_axis',(0.,-0.222520933956314,0.974927912181824));
#25611=DIRECTION('',(0.,0.222520933956314,-0.974927912181824));
#25612=DIRECTION('center_axis',(1.,0.,0.));
#25613=DIRECTION('ref_axis',(0.,0.,-1.));
#25614=DIRECTION('center_axis',(1.,0.,0.));
#25615=DIRECTION('ref_axis',(0.,0.,-1.));
#25616=DIRECTION('',(1.,0.,0.));
#25617=DIRECTION('center_axis',(0.,-0.0592161357215444,-0.998245184947169));
#25618=DIRECTION('ref_axis',(0.,0.998245184947169,-0.0592161357215444));
#25619=DIRECTION('',(0.,-0.998245184947169,0.0592161357215444));
#25620=DIRECTION('',(1.,0.,0.));
#25621=DIRECTION('center_axis',(0.,0.37977045863838,0.925080752553848));
#25622=DIRECTION('ref_axis',(0.,-0.925080752553848,0.37977045863838));
#25623=DIRECTION('',(-1.,0.,0.));
#25624=DIRECTION('',(1.,0.,0.));
#25625=DIRECTION('',(0.,0.925080752553848,-0.37977045863838));
#25626=DIRECTION('center_axis',(0.,0.974927912181824,-0.222520933956314));
#25627=DIRECTION('ref_axis',(0.,0.222520933956314,0.974927912181824));
#25628=DIRECTION('',(0.,-0.222520933956314,-0.974927912181824));
#25629=DIRECTION('center_axis',(1.,0.,0.));
#25630=DIRECTION('ref_axis',(0.,0.,-1.));
#25631=DIRECTION('center_axis',(1.,0.,0.));
#25632=DIRECTION('ref_axis',(0.,0.,-1.));
#25633=DIRECTION('',(1.,0.,0.));
#25634=DIRECTION('center_axis',(0.,-0.486474248163572,-0.873694915787935));
#25635=DIRECTION('ref_axis',(0.,0.873694915787935,-0.486474248163572));
#25636=DIRECTION('',(0.,-0.873694915787935,0.486474248163572));
#25637=DIRECTION('',(1.,0.,0.));
#25638=DIRECTION('center_axis',(0.,0.743538856085952,0.668692731746348));
#25639=DIRECTION('ref_axis',(0.,-0.668692731746348,0.743538856085952));
#25640=DIRECTION('',(-1.,0.,0.));
#25641=DIRECTION('',(1.,0.,0.));
#25642=DIRECTION('',(0.,0.668692731746348,-0.743538856085952));
#25643=DIRECTION('center_axis',(0.,0.78183148246803,-0.623489801858734));
#25644=DIRECTION('ref_axis',(0.,0.623489801858734,0.78183148246803));
#25645=DIRECTION('',(0.,-0.623489801858734,-0.78183148246803));
#25646=DIRECTION('center_axis',(1.,0.,0.));
#25647=DIRECTION('ref_axis',(0.,0.,-1.));
#25648=DIRECTION('center_axis',(1.,0.,0.));
#25649=DIRECTION('ref_axis',(0.,0.,-1.));
#25650=DIRECTION('',(1.,0.,0.));
#25651=DIRECTION('center_axis',(0.,-0.817380169541683,-0.576098653391942));
#25652=DIRECTION('ref_axis',(0.,0.576098653391942,-0.817380169541683));
#25653=DIRECTION('',(0.,-0.576098653391942,0.817380169541683));
#25654=DIRECTION('',(1.,0.,0.));
#25655=DIRECTION('center_axis',(0.,0.96004026418006,0.279861914438319));
#25656=DIRECTION('ref_axis',(0.,-0.279861914438319,0.96004026418006));
#25657=DIRECTION('',(-1.,0.,0.));
#25658=DIRECTION('',(1.,0.,0.));
#25659=DIRECTION('',(0.,0.279861914438319,-0.96004026418006));
#25660=DIRECTION('center_axis',(0.,0.433883739117558,-0.900968867902419));
#25661=DIRECTION('ref_axis',(0.,0.900968867902419,0.433883739117558));
#25662=DIRECTION('',(0.,-0.900968867902419,-0.433883739117558));
#25663=DIRECTION('center_axis',(1.,0.,0.));
#25664=DIRECTION('ref_axis',(0.,0.,-1.));
#25665=DIRECTION('center_axis',(1.,0.,0.));
#25666=DIRECTION('ref_axis',(0.,0.,-1.));
#25667=DIRECTION('',(1.,0.,0.));
#25668=DIRECTION('center_axis',(0.,0.986393923832144,-0.164398987305357));
#25669=DIRECTION('ref_axis',(0.,0.164398987305357,0.986393923832144));
#25670=DIRECTION('',(-1.,0.,0.));
#25671=DIRECTION('',(1.,0.,0.));
#25672=DIRECTION('',(0.,-0.164398987305357,-0.986393923832144));
#25673=DIRECTION('center_axis',(0.,-0.986393923832144,-0.164398987305357));
#25674=DIRECTION('ref_axis',(0.,0.164398987305357,-0.986393923832144));
#25675=DIRECTION('',(0.,-0.164398987305357,0.986393923832144));
#25676=DIRECTION('',(1.,0.,0.));
#25677=DIRECTION('center_axis',(0.,0.,-1.));
#25678=DIRECTION('ref_axis',(0.,1.,0.));
#25679=DIRECTION('',(0.,-1.,0.));
#25680=DIRECTION('center_axis',(1.,0.,0.));
#25681=DIRECTION('ref_axis',(0.,0.,-1.));
#25682=DIRECTION('center_axis',(1.,0.,0.));
#25683=DIRECTION('ref_axis',(0.,0.,-1.));
#25684=DIRECTION('center_axis',(1.,0.,0.));
#25685=DIRECTION('ref_axis',(0.,1.,0.));
#25686=DIRECTION('center_axis',(1.,0.,0.));
#25687=DIRECTION('ref_axis',(0.,0.,-1.));
#25688=DIRECTION('center_axis',(1.,0.,0.));
#25689=DIRECTION('ref_axis',(0.,1.,0.));
#25690=DIRECTION('',(1.,0.,0.));
#25691=DIRECTION('axis',(0.,0.,1.));
#25692=DIRECTION('refdir',(1.,0.,0.));
#25693=DIRECTION('center_axis',(1.,0.,0.));
#25694=DIRECTION('ref_axis',(0.,-0.555251325848433,-0.831682610821915));
#25695=DIRECTION('',(-1.,0.,0.));
#25696=DIRECTION('center_axis',(-1.,0.,0.));
#25697=DIRECTION('ref_axis',(0.,1.,-3.76905526341366E-13));
#25698=DIRECTION('center_axis',(1.,0.,0.));
#25699=DIRECTION('ref_axis',(0.,-0.555251325848433,-0.831682610821915));
#25700=DIRECTION('',(-1.,0.,0.));
#25701=DIRECTION('center_axis',(1.,0.,0.));
#25702=DIRECTION('ref_axis',(0.,-0.555251325848433,-0.831682610821915));
#25703=DIRECTION('',(-1.,0.,0.));
#25704=DIRECTION('center_axis',(1.,0.,0.));
#25705=DIRECTION('ref_axis',(0.,-0.555251325848433,-0.831682610821915));
#25706=DIRECTION('',(-1.,0.,0.));
#25707=DIRECTION('center_axis',(1.,0.,0.));
#25708=DIRECTION('ref_axis',(0.,-0.555251325848433,-0.831682610821915));
#25709=DIRECTION('',(-1.,0.,0.));
#25710=DIRECTION('center_axis',(1.,0.,0.));
#25711=DIRECTION('ref_axis',(0.,-0.555251325848433,-0.831682610821915));
#25712=DIRECTION('',(-1.,0.,0.));
#25713=DIRECTION('center_axis',(1.,0.,0.));
#25714=DIRECTION('ref_axis',(0.,-0.555251325848433,-0.831682610821915));
#25715=DIRECTION('',(-1.,0.,0.));
#25716=DIRECTION('center_axis',(1.,0.,0.));
#25717=DIRECTION('ref_axis',(0.,-0.555251325848433,-0.831682610821915));
#25718=DIRECTION('',(-1.,0.,0.));
#25719=DIRECTION('center_axis',(1.,0.,0.));
#25720=DIRECTION('ref_axis',(0.,-0.555251325848433,-0.831682610821915));
#25721=DIRECTION('',(-1.,0.,0.));
#25722=DIRECTION('center_axis',(1.,0.,0.));
#25723=DIRECTION('ref_axis',(0.,-0.555251325848433,-0.831682610821915));
#25724=DIRECTION('',(-1.,0.,0.));
#25725=DIRECTION('center_axis',(1.,0.,0.));
#25726=DIRECTION('ref_axis',(0.,-0.555251325848433,-0.831682610821915));
#25727=DIRECTION('',(-1.,0.,0.));
#25728=DIRECTION('center_axis',(1.,0.,0.));
#25729=DIRECTION('ref_axis',(0.,-0.555251325848433,-0.831682610821915));
#25730=DIRECTION('',(-1.,0.,0.));
#25731=DIRECTION('center_axis',(1.,0.,0.));
#25732=DIRECTION('ref_axis',(0.,-0.555251325848433,-0.831682610821915));
#25733=DIRECTION('',(-1.,0.,0.));
#25734=DIRECTION('center_axis',(1.,0.,0.));
#25735=DIRECTION('ref_axis',(0.,-0.555251325848433,-0.831682610821915));
#25736=DIRECTION('',(-1.,0.,0.));
#25737=DIRECTION('center_axis',(1.,0.,0.));
#25738=DIRECTION('ref_axis',(0.,-0.555251325848433,-0.831682610821915));
#25739=DIRECTION('',(-1.,0.,0.));
#25740=DIRECTION('center_axis',(1.,0.,0.));
#25741=DIRECTION('ref_axis',(0.,-0.555251325848433,-0.831682610821915));
#25742=DIRECTION('',(-1.,0.,0.));
#25743=DIRECTION('center_axis',(1.,0.,0.));
#25744=DIRECTION('ref_axis',(0.,-0.555251325848433,-0.831682610821915));
#25745=DIRECTION('',(-1.,0.,0.));
#25746=DIRECTION('center_axis',(1.,0.,0.));
#25747=DIRECTION('ref_axis',(0.,-0.555251325848433,-0.831682610821915));
#25748=DIRECTION('',(-1.,0.,0.));
#25749=DIRECTION('center_axis',(1.,0.,0.));
#25750=DIRECTION('ref_axis',(0.,-0.555251325848433,-0.831682610821915));
#25751=DIRECTION('',(-1.,0.,0.));
#25752=DIRECTION('center_axis',(1.,0.,0.));
#25753=DIRECTION('ref_axis',(0.,-0.555251325848433,-0.831682610821915));
#25754=DIRECTION('',(-1.,0.,0.));
#25755=DIRECTION('center_axis',(1.,0.,0.));
#25756=DIRECTION('ref_axis',(0.,-0.555251325848433,-0.831682610821915));
#25757=DIRECTION('',(-1.,0.,0.));
#25758=DIRECTION('center_axis',(1.,0.,0.));
#25759=DIRECTION('ref_axis',(0.,-0.555251325848433,-0.831682610821915));
#25760=DIRECTION('',(-1.,0.,0.));
#25761=DIRECTION('center_axis',(1.,0.,0.));
#25762=DIRECTION('ref_axis',(0.,-0.555251325848433,-0.831682610821915));
#25763=DIRECTION('',(-1.,0.,0.));
#25764=DIRECTION('center_axis',(1.,0.,0.));
#25765=DIRECTION('ref_axis',(0.,-0.555251325848433,-0.831682610821915));
#25766=DIRECTION('',(-1.,0.,0.));
#25767=DIRECTION('center_axis',(1.,0.,0.));
#25768=DIRECTION('ref_axis',(0.,-0.555251325848433,-0.831682610821915));
#25769=DIRECTION('',(-1.,0.,0.));
#25770=DIRECTION('center_axis',(1.,0.,0.));
#25771=DIRECTION('ref_axis',(0.,-0.555251325848433,-0.831682610821915));
#25772=DIRECTION('',(-1.,0.,0.));
#25773=DIRECTION('center_axis',(1.,0.,0.));
#25774=DIRECTION('ref_axis',(0.,-0.555251325848433,-0.831682610821915));
#25775=DIRECTION('',(-1.,0.,0.));
#25776=DIRECTION('center_axis',(1.,0.,0.));
#25777=DIRECTION('ref_axis',(0.,-0.555251325848433,-0.831682610821915));
#25778=DIRECTION('',(-1.,0.,0.));
#25779=DIRECTION('center_axis',(1.,0.,0.));
#25780=DIRECTION('ref_axis',(0.,-0.555251325848433,-0.831682610821915));
#25781=DIRECTION('',(-1.,0.,0.));
#25782=DIRECTION('center_axis',(1.,0.,0.));
#25783=DIRECTION('ref_axis',(0.,-0.555251325848433,-0.831682610821915));
#25784=DIRECTION('',(-1.,0.,0.));
#25785=DIRECTION('center_axis',(1.,0.,0.));
#25786=DIRECTION('ref_axis',(0.,-0.555251325848433,-0.831682610821915));
#25787=DIRECTION('',(-1.,0.,0.));
#25788=DIRECTION('center_axis',(1.,0.,0.));
#25789=DIRECTION('ref_axis',(0.,-0.555251325848433,-0.831682610821915));
#25790=DIRECTION('',(-1.,0.,0.));
#25791=DIRECTION('center_axis',(1.,0.,0.));
#25792=DIRECTION('ref_axis',(0.,-0.555251325848433,-0.831682610821915));
#25793=DIRECTION('',(-1.,0.,0.));
#25794=DIRECTION('center_axis',(1.,0.,0.));
#25795=DIRECTION('ref_axis',(0.,-0.555251325848433,-0.831682610821915));
#25796=DIRECTION('',(-1.,0.,0.));
#25797=DIRECTION('center_axis',(1.,0.,0.));
#25798=DIRECTION('ref_axis',(0.,-0.555251325848433,-0.831682610821915));
#25799=DIRECTION('',(-1.,0.,0.));
#25800=DIRECTION('center_axis',(1.,0.,0.));
#25801=DIRECTION('ref_axis',(0.,-0.555251325848433,-0.831682610821915));
#25802=DIRECTION('',(-1.,0.,0.));
#25803=DIRECTION('center_axis',(1.,0.,0.));
#25804=DIRECTION('ref_axis',(0.,-0.555251325848433,-0.831682610821915));
#25805=DIRECTION('',(-1.,0.,0.));
#25806=DIRECTION('center_axis',(1.,0.,0.));
#25807=DIRECTION('ref_axis',(0.,-0.555251325848433,-0.831682610821915));
#25808=DIRECTION('',(-1.,0.,0.));
#25809=DIRECTION('center_axis',(1.,0.,0.));
#25810=DIRECTION('ref_axis',(0.,-0.555251325848433,-0.831682610821915));
#25811=DIRECTION('',(-1.,0.,0.));
#25812=DIRECTION('center_axis',(1.,0.,0.));
#25813=DIRECTION('ref_axis',(0.,1.,0.));
#25814=DIRECTION('center_axis',(1.,0.,0.));
#25815=DIRECTION('ref_axis',(0.,1.,0.));
#25816=DIRECTION('center_axis',(-1.,0.,0.));
#25817=DIRECTION('ref_axis',(0.,1.,0.));
#25818=DIRECTION('center_axis',(1.,0.,0.));
#25819=DIRECTION('ref_axis',(0.,-0.555251325848433,-0.831682610821915));
#25820=DIRECTION('center_axis',(1.,0.,0.));
#25821=DIRECTION('ref_axis',(0.,1.,-3.76905526341366E-13));
#25822=DIRECTION('center_axis',(1.,0.,0.));
#25823=DIRECTION('ref_axis',(0.,0.,-1.));
#25824=DIRECTION('center_axis',(1.,0.,0.));
#25825=DIRECTION('ref_axis',(0.,0.,-1.));
#25826=DIRECTION('',(1.,0.,0.));
#25827=DIRECTION('center_axis',(1.,0.,0.));
#25828=DIRECTION('ref_axis',(0.,0.,-1.));
#25829=DIRECTION('center_axis',(1.,0.,0.));
#25830=DIRECTION('ref_axis',(0.,0.,-1.));
#25831=DIRECTION('center_axis',(1.,0.,0.));
#25832=DIRECTION('ref_axis',(0.,0.,-1.));
#25833=DIRECTION('center_axis',(-1.,0.,0.));
#25834=DIRECTION('ref_axis',(0.,1.,0.));
#25835=DIRECTION('center_axis',(-1.,0.,0.));
#25836=DIRECTION('ref_axis',(0.,1.,0.));
#25837=DIRECTION('center_axis',(1.,0.,0.));
#25838=DIRECTION('ref_axis',(0.,0.,-1.));
#25839=DIRECTION('center_axis',(1.,0.,0.));
#25840=DIRECTION('ref_axis',(0.,1.,0.));
#25841=DIRECTION('center_axis',(1.,0.,0.));
#25842=DIRECTION('ref_axis',(0.,1.,0.));
#25843=DIRECTION('center_axis',(-1.,0.,0.));
#25844=DIRECTION('ref_axis',(0.,0.,1.));
#25845=DIRECTION('center_axis',(1.,0.,0.));
#25846=DIRECTION('ref_axis',(0.,0.,-1.));
#25847=DIRECTION('center_axis',(1.,0.,0.));
#25848=DIRECTION('ref_axis',(0.,1.,0.));
#25849=DIRECTION('',(-0.707106781186548,0.707106781186547,8.65956056235493E-17));
#25850=DIRECTION('center_axis',(-1.,0.,0.));
#25851=DIRECTION('ref_axis',(0.,1.,0.));
#25852=DIRECTION('',(0.707106781186546,0.707106781186549,-8.65956056235495E-17));
#25853=DIRECTION('center_axis',(1.,0.,0.));
#25854=DIRECTION('ref_axis',(0.,0.,-1.));
#25855=DIRECTION('center_axis',(1.,0.,0.));
#25856=DIRECTION('ref_axis',(0.,1.,0.));
#25857=DIRECTION('center_axis',(1.,0.,0.));
#25858=DIRECTION('ref_axis',(0.,0.,-1.));
#25859=DIRECTION('',(-1.,0.,0.));
#25860=DIRECTION('center_axis',(-1.,0.,0.));
#25861=DIRECTION('ref_axis',(0.,0.,1.));
#25862=DIRECTION('center_axis',(1.,0.,0.));
#25863=DIRECTION('ref_axis',(0.,0.,-1.));
#25864=DIRECTION('center_axis',(1.,0.,0.));
#25865=DIRECTION('ref_axis',(0.,1.,0.));
#25866=DIRECTION('center_axis',(1.,0.,0.));
#25867=DIRECTION('ref_axis',(0.,0.,-1.));
#25868=DIRECTION('',(-1.,0.,0.));
#25869=DIRECTION('center_axis',(1.,0.,0.));
#25870=DIRECTION('ref_axis',(0.,0.,-1.));
#25871=DIRECTION('center_axis',(1.,0.,0.));
#25872=DIRECTION('ref_axis',(0.,0.,-1.));
#25873=DIRECTION('center_axis',(1.,0.,0.));
#25874=DIRECTION('ref_axis',(0.,1.,0.));
#25875=DIRECTION('center_axis',(1.,0.,0.));
#25876=DIRECTION('ref_axis',(0.,0.,-1.));
#25877=DIRECTION('',(-1.,0.,0.));
#25878=DIRECTION('center_axis',(-1.,0.,0.));
#25879=DIRECTION('ref_axis',(0.,1.,0.));
#25880=DIRECTION('',(0.707106781186547,0.707106781186548,-8.65956056235494E-17));
#25881=DIRECTION('center_axis',(1.,0.,0.));
#25882=DIRECTION('ref_axis',(0.,0.,-1.));
#25883=DIRECTION('center_axis',(1.,0.,0.));
#25884=DIRECTION('ref_axis',(0.,0.,-1.));
#25885=DIRECTION('axis',(0.,0.,1.));
#25886=DIRECTION('refdir',(1.,0.,0.));
#25887=DIRECTION('center_axis',(0.,0.,1.));
#25888=DIRECTION('ref_axis',(1.,0.,0.));
#25889=DIRECTION('center_axis',(0.,0.,-1.));
#25890=DIRECTION('ref_axis',(6.12323399573677E-17,1.,0.));
#25891=DIRECTION('center_axis',(0.,0.,1.));
#25892=DIRECTION('ref_axis',(6.12323399573677E-17,1.,0.));
#25893=DIRECTION('center_axis',(0.,0.,1.));
#25894=DIRECTION('ref_axis',(1.,0.,0.));
#25895=DIRECTION('',(1.,0.,0.));
#25896=DIRECTION('center_axis',(0.,0.,1.));
#25897=DIRECTION('ref_axis',(1.,0.,0.));
#25898=DIRECTION('center_axis',(0.,0.,-1.));
#25899=DIRECTION('ref_axis',(0.936506715470107,0.350649642634058,0.));
#25900=DIRECTION('center_axis',(0.,0.,1.));
#25901=DIRECTION('ref_axis',(0.936506715470107,0.350649642634058,0.));
#25902=DIRECTION('center_axis',(0.,0.,1.));
#25903=DIRECTION('ref_axis',(1.,0.,0.));
#25904=DIRECTION('',(-1.,0.,0.));
#25905=DIRECTION('',(0.,1.,0.));
#25906=DIRECTION('center_axis',(0.,0.,1.));
#25907=DIRECTION('ref_axis',(1.,0.,0.));
#25908=DIRECTION('center_axis',(0.,0.,1.));
#25909=DIRECTION('ref_axis',(0.670584301865815,-0.741833333095203,0.));
#25910=DIRECTION('center_axis',(0.,0.,-1.));
#25911=DIRECTION('ref_axis',(0.670584301865815,-0.741833333095203,0.));
#25912=DIRECTION('center_axis',(-1.,0.,0.));
#25913=DIRECTION('ref_axis',(0.,-0.707106781186547,-0.707106781186547));
#25914=DIRECTION('',(1.,0.,0.));
#25915=DIRECTION('',(-1.,0.,0.));
#25916=DIRECTION('center_axis',(0.,0.,1.));
#25917=DIRECTION('ref_axis',(1.,0.,0.));
#25918=DIRECTION('center_axis',(0.,0.,-1.));
#25919=DIRECTION('ref_axis',(-0.670584301865815,-0.741833333095203,0.));
#25920=DIRECTION('center_axis',(0.,0.,1.));
#25921=DIRECTION('ref_axis',(-0.670584301865815,-0.741833333095203,0.));
#25922=DIRECTION('center_axis',(0.,0.,1.));
#25923=DIRECTION('ref_axis',(1.,0.,0.));
#25924=DIRECTION('',(1.,0.,0.));
#25925=DIRECTION('center_axis',(0.,0.,1.));
#25926=DIRECTION('ref_axis',(1.,0.,0.));
#25927=DIRECTION('center_axis',(0.,0.,-1.));
#25928=DIRECTION('ref_axis',(-0.936506715470107,0.350649642634058,0.));
#25929=DIRECTION('center_axis',(0.,0.,1.));
#25930=DIRECTION('ref_axis',(-0.936506715470107,0.350649642634058,0.));
#25931=DIRECTION('center_axis',(0.,0.,1.));
#25932=DIRECTION('ref_axis',(1.,0.,0.));
#25933=DIRECTION('',(0.,1.,0.));
#25934=DIRECTION('',(-1.,0.,0.));
#25935=DIRECTION('center_axis',(-1.,0.,0.));
#25936=DIRECTION('ref_axis',(0.,0.707106781186547,-0.707106781186547));
#25937=DIRECTION('center_axis',(1.,0.,0.));
#25938=DIRECTION('ref_axis',(0.,0.707106781186547,-0.707106781186547));
#25939=DIRECTION('',(-1.,0.,0.));
#25940=DIRECTION('center_axis',(-1.,0.,0.));
#25941=DIRECTION('ref_axis',(0.,0.707106781186547,-0.707106781186547));
#25942=DIRECTION('',(1.,0.,0.));
#25943=DIRECTION('center_axis',(0.,0.,-1.));
#25944=DIRECTION('ref_axis',(-1.,0.,0.));
#25945=DIRECTION('',(0.,1.,0.));
#25946=DIRECTION('',(1.,0.,0.));
#25947=DIRECTION('',(0.,-1.,0.));
#25948=DIRECTION('center_axis',(1.,0.,0.));
#25949=DIRECTION('ref_axis',(0.,-0.707106781186547,-0.707106781186547));
#25950=DIRECTION('center_axis',(0.707106781186549,0.,-0.707106781186546));
#25951=DIRECTION('ref_axis',(-0.707106781186546,0.,-0.707106781186549));
#25952=DIRECTION('',(-1.,0.,0.));
#25953=DIRECTION('center_axis',(-1.,0.,0.));
#25954=DIRECTION('ref_axis',(0.,-0.707106781186547,-0.707106781186547));
#25955=DIRECTION('center_axis',(0.,1.,0.));
#25956=DIRECTION('ref_axis',(1.,0.,0.));
#25957=DIRECTION('',(0.,0.,1.));
#25958=DIRECTION('center_axis',(0.,1.,0.));
#25959=DIRECTION('ref_axis',(0.707106781186547,0.,0.707106781186547));
#25960=DIRECTION('',(0.,0.,-1.));
#25961=DIRECTION('center_axis',(0.,1.,0.));
#25962=DIRECTION('ref_axis',(0.707106781186547,0.,-0.707106781186547));
#25963=DIRECTION('',(0.,0.,1.));
#25964=DIRECTION('center_axis',(0.,1.,0.));
#25965=DIRECTION('ref_axis',(-1.86143556795118E-16,0.,-1.));
#25966=DIRECTION('',(0.,0.,-1.));
#25967=DIRECTION('center_axis',(0.,1.,0.));
#25968=DIRECTION('ref_axis',(-0.707106781186547,0.,-0.707106781186547));
#25969=DIRECTION('',(0.,0.,1.));
#25970=DIRECTION('center_axis',(0.,1.,0.));
#25971=DIRECTION('ref_axis',(-0.707106781186547,0.,0.707106781186547));
#25972=DIRECTION('',(0.,0.,-1.));
#25973=DIRECTION('',(-1.,0.,0.));
#25974=DIRECTION('',(0.,0.,1.));
#25975=DIRECTION('',(1.,0.,0.));
#25976=DIRECTION('',(1.,0.,0.));
#25977=DIRECTION('',(0.,0.,1.));
#25978=DIRECTION('center_axis',(0.,0.,-1.));
#25979=DIRECTION('ref_axis',(0.707106781186547,-0.707106781186547,0.));
#25980=DIRECTION('center_axis',(0.,0.,-1.));
#25981=DIRECTION('ref_axis',(0.707106781186547,-0.707106781186547,0.));
#25982=DIRECTION('',(0.,0.,1.));
#25983=DIRECTION('center_axis',(-0.707106781186548,0.,-0.707106781186548));
#25984=DIRECTION('ref_axis',(-0.707106781186548,0.,0.707106781186548));
#25985=DIRECTION('center_axis',(1.,0.,0.));
#25986=DIRECTION('ref_axis',(0.,-0.707106781186547,-0.707106781186547));
#25987=DIRECTION('',(1.,0.,0.));
#25988=DIRECTION('center_axis',(1.,0.,0.));
#25989=DIRECTION('ref_axis',(0.,-0.707106781186547,-0.707106781186547));
#25990=DIRECTION('center_axis',(0.,0.568073288796263,-0.82297796966638));
#25991=DIRECTION('ref_axis',(0.70710678118655,-0.581933303118232,-0.40168847471878));
#25992=DIRECTION('',(0.,-0.568073288796263,0.82297796966638));
#25993=DIRECTION('center_axis',(0.,-0.464718576777245,-0.885458437419923));
#25994=DIRECTION('ref_axis',(-2.68719408286006E-17,-0.885458437419923,0.464718576777245));
#25995=DIRECTION('center_axis',(0.,-0.954719322541023,-0.297508008575921));
#25996=DIRECTION('ref_axis',(-1.72031375589252E-17,0.297508008575921,-0.954719322541023));
#25997=DIRECTION('',(0.,0.568073288796263,-0.82297796966638));
#25998=DIRECTION('',(0.,0.568073288796263,-0.82297796966638));
#25999=DIRECTION('center_axis',(0.,-0.464718576777247,-0.885458437419922));
#26000=DIRECTION('ref_axis',(-2.68719408286005E-17,-0.885458437419922,0.464718576777247));
#26001=DIRECTION('center_axis',(0.,-0.954719322541023,-0.297508008575921));
#26002=DIRECTION('ref_axis',(-1.72031375589252E-17,0.297508008575921,-0.954719322541023));
#26003=DIRECTION('',(0.,-0.568073288796263,0.82297796966638));
#26004=DIRECTION('center_axis',(0.,1.,0.));
#26005=DIRECTION('ref_axis',(9.85450070150229E-17,0.,-1.));
#26006=DIRECTION('',(0.,-0.568073288796263,0.82297796966638));
#26007=DIRECTION('center_axis',(0.,-1.,0.));
#26008=DIRECTION('ref_axis',(9.85450070150229E-17,0.,-1.));
#26009=DIRECTION('',(0.,-0.568073288796263,0.822977969666381));
#26010=DIRECTION('center_axis',(0.,0.82297796966638,-0.568073288796263));
#26011=DIRECTION('ref_axis',(1.08133826391977E-16,-0.568073288796263,-0.82297796966638));
#26012=DIRECTION('center_axis',(0.,0.82297796966638,0.568073288796263));
#26013=DIRECTION('ref_axis',(0.,0.568073288796263,-0.82297796966638));
#26014=DIRECTION('',(-1.,0.,0.));
#26015=DIRECTION('',(0.,0.568073288796263,-0.82297796966638));
#26016=DIRECTION('',(-1.,0.,0.));
#26017=DIRECTION('center_axis',(0.,0.82297796966638,0.568073288796263));
#26018=DIRECTION('ref_axis',(0.,0.568073288796263,-0.82297796966638));
#26019=DIRECTION('center_axis',(0.,0.82297796966638,0.568073288796263));
#26020=DIRECTION('ref_axis',(-3.78468392371919E-16,-0.568073288796263,0.82297796966638));
#26021=DIRECTION('',(0.,0.568073288796263,-0.82297796966638));
#26022=DIRECTION('',(-1.,0.,0.));
#26023=DIRECTION('center_axis',(1.,0.,0.));
#26024=DIRECTION('ref_axis',(0.,0.,-1.));
#26025=DIRECTION('',(0.,-0.568073288796263,-0.822977969666381));
#26026=DIRECTION('center_axis',(-1.,0.,0.));
#26027=DIRECTION('ref_axis',(0.,0.,-1.));
#26028=DIRECTION('',(0.,-0.568073288796263,-0.82297796966638));
#26029=DIRECTION('center_axis',(1.,0.,0.));
#26030=DIRECTION('ref_axis',(0.,0.,-1.));
#26031=DIRECTION('',(0.,0.,-1.));
#26032=DIRECTION('',(0.,1.,0.));
#26033=DIRECTION('',(0.,0.568073288796263,0.82297796966638));
#26034=DIRECTION('center_axis',(-1.,0.,0.));
#26035=DIRECTION('ref_axis',(0.,0.,-1.));
#26036=DIRECTION('',(0.,0.568073288796263,0.822977969666381));
#26037=DIRECTION('',(0.,0.,-1.));
#26038=DIRECTION('center_axis',(-1.,0.,0.));
#26039=DIRECTION('ref_axis',(0.,0.,-1.));
#26040=DIRECTION('',(0.,0.,-1.));
#26041=DIRECTION('center_axis',(1.,0.,0.));
#26042=DIRECTION('ref_axis',(0.,0.,-1.));
#26043=DIRECTION('',(0.,-1.,0.));
#26044=DIRECTION('',(0.,0.568073288796263,0.82297796966638));
#26045=DIRECTION('',(0.,0.,1.));
#26046=DIRECTION('',(0.,-1.,0.));
#26047=DIRECTION('',(0.,0.,-1.));
#26048=DIRECTION('center_axis',(0.,0.,1.));
#26049=DIRECTION('ref_axis',(0.707106781186545,-0.70710678118655,0.));
#26050=DIRECTION('',(0.,0.,1.));
#26051=DIRECTION('center_axis',(0.,0.,1.));
#26052=DIRECTION('ref_axis',(0.707106781186544,-0.707106781186551,0.));
#26053=DIRECTION('',(0.,0.,-1.));
#26054=DIRECTION('center_axis',(0.,0.,1.));
#26055=DIRECTION('ref_axis',(0.,-1.,0.));
#26056=DIRECTION('center_axis',(0.,-0.297508008575919,-0.954719322541024));
#26057=DIRECTION('ref_axis',(-5.52058007260196E-17,-0.954719322541023,0.297508008575919));
#26058=DIRECTION('center_axis',(-0.816496580927726,-0.408248290463864,0.408248290463863));
#26059=DIRECTION('ref_axis',(0.577350269189628,-0.577350269189625,0.577350269189625));
#26060=DIRECTION('center_axis',(0.,1.,0.));
#26061=DIRECTION('ref_axis',(0.,0.,1.));
#26062=DIRECTION('center_axis',(-1.,0.,0.));
#26063=DIRECTION('ref_axis',(0.,-1.,-1.85037170770859E-15));
#26064=DIRECTION('center_axis',(0.,1.,0.));
#26065=DIRECTION('ref_axis',(0.707106781186545,0.,0.70710678118655));
#26066=DIRECTION('center_axis',(0.,-0.885458437419923,0.464718576777245));
#26067=DIRECTION('ref_axis',(-2.04803405119211E-16,0.464718576777245,0.885458437419923));
#26068=DIRECTION('',(0.,1.,0.));
#26069=DIRECTION('center_axis',(0.,0.885458437419921,0.464718576777249));
#26070=DIRECTION('ref_axis',(-2.0480340511921E-16,-0.464718576777249,0.885458437419921));
#26071=DIRECTION('center_axis',(0.,1.,0.));
#26072=DIRECTION('ref_axis',(0.,0.,1.));
#26073=DIRECTION('',(0.,-1.,0.));
#26074=DIRECTION('center_axis',(0.,1.,0.));
#26075=DIRECTION('ref_axis',(-0.707106781186547,0.,0.707106781186547));
#26076=DIRECTION('center_axis',(0.,1.,0.));
#26077=DIRECTION('ref_axis',(-1.,0.,0.));
#26078=DIRECTION('',(0.,1.,0.));
#26079=DIRECTION('',(0.,-1.,0.));
#26080=DIRECTION('center_axis',(0.,0.,-1.));
#26081=DIRECTION('ref_axis',(-0.707106781186547,-0.707106781186547,0.));
#26082=DIRECTION('center_axis',(0.,0.,-1.));
#26083=DIRECTION('ref_axis',(0.,-1.,0.));
#26084=DIRECTION('',(0.,0.,-1.));
#26085=DIRECTION('center_axis',(0.,0.,1.));
#26086=DIRECTION('ref_axis',(-1.,0.,0.));
#26087=DIRECTION('',(0.,0.,1.));
#26088=DIRECTION('center_axis',(0.,1.,0.));
#26089=DIRECTION('ref_axis',(-0.707106781186547,0.,-0.707106781186547));
#26090=DIRECTION('',(0.,-1.,0.));
#26091=DIRECTION('center_axis',(0.,1.,0.));
#26092=DIRECTION('ref_axis',(0.,0.,-1.));
#26093=DIRECTION('',(0.,1.,0.));
#26094=DIRECTION('center_axis',(0.408248290463863,-0.816496580927727,0.408248290463863));
#26095=DIRECTION('ref_axis',(-0.577350269189626,-0.577350269189626,-0.577350269189626));
#26096=DIRECTION('center_axis',(-1.,0.,0.));
#26097=DIRECTION('ref_axis',(0.,-0.707106781186547,-0.707106781186547));
#26098=DIRECTION('center_axis',(0.408248290463863,-0.816496580927727,-0.408248290463863));
#26099=DIRECTION('ref_axis',(-0.577350269189626,-0.577350269189626,0.577350269189626));
#26100=DIRECTION('center_axis',(-1.,0.,0.));
#26101=DIRECTION('ref_axis',(0.,-0.707106781186547,0.707106781186547));
#26102=DIRECTION('center_axis',(0.,0.,1.));
#26103=DIRECTION('ref_axis',(1.,0.,0.));
#26104=DIRECTION('',(-1.,0.,0.));
#26105=DIRECTION('',(0.,1.,0.));
#26106=DIRECTION('',(1.,0.,0.));
#26107=DIRECTION('',(0.,1.,0.));
#26108=DIRECTION('center_axis',(1.,0.,0.));
#26109=DIRECTION('ref_axis',(0.,-0.707106781186547,0.707106781186547));
#26110=DIRECTION('',(1.,0.,0.));
#26111=DIRECTION('center_axis',(0.707106781186548,0.,0.707106781186548));
#26112=DIRECTION('ref_axis',(-0.707106781186548,0.,0.707106781186548));
#26113=DIRECTION('center_axis',(0.,1.,0.));
#26114=DIRECTION('ref_axis',(1.,0.,0.));
#26115=DIRECTION('',(-1.,0.,0.));
#26116=DIRECTION('',(1.,0.,0.));
#26117=DIRECTION('',(0.,0.,1.));
#26118=DIRECTION('',(1.,0.,0.));
#26119=DIRECTION('',(0.,0.,-1.));
#26120=DIRECTION('',(1.,0.,0.));
#26121=DIRECTION('',(0.,0.,1.));
#26122=DIRECTION('center_axis',(1.,0.,0.));
#26123=DIRECTION('ref_axis',(0.,-0.707106781186547,-0.707106781186547));
#26124=DIRECTION('',(1.,0.,0.));
#26125=DIRECTION('center_axis',(-1.,0.,0.));
#26126=DIRECTION('ref_axis',(0.,0.,-1.));
#26127=DIRECTION('center_axis',(0.,0.,-1.));
#26128=DIRECTION('ref_axis',(-1.,0.,0.));
#26129=DIRECTION('center_axis',(0.,0.,1.));
#26130=DIRECTION('ref_axis',(0.707106781186547,-0.707106781186547,0.));
#26131=DIRECTION('',(0.,-1.,0.));
#26132=DIRECTION('',(-1.,0.,0.));
#26133=DIRECTION('',(0.,1.,0.));
#26134=DIRECTION('center_axis',(0.,1.,0.));
#26135=DIRECTION('ref_axis',(1.22464679914735E-16,0.,-1.));
#26136=DIRECTION('center_axis',(0.,0.,-1.));
#26137=DIRECTION('ref_axis',(1.,0.,0.));
#26138=DIRECTION('center_axis',(3.70074341541718E-15,0.,-1.));
#26139=DIRECTION('ref_axis',(0.,-1.,0.));
#26140=DIRECTION('center_axis',(0.,-1.,0.));
#26141=DIRECTION('ref_axis',(-1.86143556795118E-16,0.,-1.));
#26142=DIRECTION('center_axis',(0.,0.,1.));
#26143=DIRECTION('ref_axis',(-0.707106781186547,-0.707106781186547,0.));
#26144=DIRECTION('center_axis',(0.,0.,1.));
#26145=DIRECTION('ref_axis',(-0.707106781186547,-0.707106781186547,0.));
#26146=DIRECTION('',(0.,0.,-1.));
#26147=DIRECTION('center_axis',(0.,0.,-1.));
#26148=DIRECTION('ref_axis',(0.707106781186547,-0.707106781186547,0.));
#26149=DIRECTION('',(0.,0.,1.));
#26150=DIRECTION('center_axis',(-1.,0.,0.));
#26151=DIRECTION('ref_axis',(0.,0.,1.));
#26152=DIRECTION('',(0.,1.,0.));
#26153=DIRECTION('center_axis',(1.,0.,0.));
#26154=DIRECTION('ref_axis',(0.,0.707106781186545,-0.70710678118655));
#26155=DIRECTION('',(0.,0.,1.));
#26156=DIRECTION('',(0.,1.,0.));
#26157=DIRECTION('center_axis',(0.,0.,1.));
#26158=DIRECTION('ref_axis',(-1.83697019872103E-16,1.,0.));
#26159=DIRECTION('center_axis',(0.,0.,-1.));
#26160=DIRECTION('ref_axis',(-1.83697019872103E-16,1.,0.));
#26161=DIRECTION('center_axis',(0.,0.,1.));
#26162=DIRECTION('ref_axis',(-1.83697019872103E-16,1.,0.));
#26163=DIRECTION('center_axis',(1.,0.,0.));
#26164=DIRECTION('ref_axis',(0.,-0.707106781186547,0.707106781186547));
#26165=DIRECTION('',(1.,0.,0.));
#26166=DIRECTION('',(-1.,0.,0.));
#26167=DIRECTION('center_axis',(0.,0.,1.));
#26168=DIRECTION('ref_axis',(6.12323399573677E-17,1.,0.));
#26169=DIRECTION('',(0.,0.,1.));
#26170=DIRECTION('center_axis',(0.,0.,-1.));
#26171=DIRECTION('ref_axis',(1.,0.,0.));
#26172=DIRECTION('',(0.,0.,-1.));
#26173=DIRECTION('center_axis',(0.,0.,1.));
#26174=DIRECTION('ref_axis',(1.,0.,0.));
#26175=DIRECTION('',(0.,0.,1.));
#26176=DIRECTION('',(0.,0.,-1.));
#26177=DIRECTION('center_axis',(0.,0.,1.));
#26178=DIRECTION('ref_axis',(1.,0.,0.));
#26179=DIRECTION('',(0.,0.,1.));
#26180=DIRECTION('center_axis',(0.,0.,-1.));
#26181=DIRECTION('ref_axis',(1.,0.,0.));
#26182=DIRECTION('',(0.,0.,-1.));
#26183=DIRECTION('center_axis',(0.,0.,1.));
#26184=DIRECTION('ref_axis',(1.,0.,0.));
#26185=DIRECTION('center_axis',(0.,0.,1.));
#26186=DIRECTION('ref_axis',(1.,0.,0.));
#26187=DIRECTION('center_axis',(0.,0.,-1.));
#26188=DIRECTION('ref_axis',(-1.,0.,0.));
#26189=DIRECTION('center_axis',(0.,-1.,0.));
#26190=DIRECTION('ref_axis',(1.,0.,0.));
#26191=DIRECTION('center_axis',(0.,0.,-1.));
#26192=DIRECTION('ref_axis',(1.,0.,0.));
#26193=DIRECTION('center_axis',(0.,0.,-1.));
#26194=DIRECTION('ref_axis',(1.,0.,0.));
#26195=DIRECTION('center_axis',(0.,0.,1.));
#26196=DIRECTION('ref_axis',(1.,0.,0.));
#26197=DIRECTION('',(0.,0.,1.));
#26198=DIRECTION('center_axis',(0.,1.,0.));
#26199=DIRECTION('ref_axis',(1.,0.,-2.47375896752486E-16));
#26200=DIRECTION('center_axis',(0.,1.,0.));
#26201=DIRECTION('ref_axis',(1.,0.,-2.47375896752486E-16));
#26202=DIRECTION('center_axis',(0.,1.,0.));
#26203=DIRECTION('ref_axis',(1.,0.,-2.47375896752486E-16));
#26204=DIRECTION('',(0.,1.,0.));
#26205=DIRECTION('center_axis',(0.,1.,0.));
#26206=DIRECTION('ref_axis',(-1.,0.,0.));
#26207=DIRECTION('center_axis',(0.,-1.,0.));
#26208=DIRECTION('ref_axis',(-1.,0.,0.));
#26209=DIRECTION('center_axis',(0.,0.,-1.));
#26210=DIRECTION('ref_axis',(1.,0.,0.));
#26211=DIRECTION('center_axis',(0.,1.,0.));
#26212=DIRECTION('ref_axis',(1.,0.,0.));
#26213=DIRECTION('center_axis',(0.,1.,0.));
#26214=DIRECTION('ref_axis',(1.,0.,0.));
#26215=DIRECTION('center_axis',(0.,0.,1.));
#26216=DIRECTION('ref_axis',(-0.707106781186547,-0.707106781186547,0.));
#26217=DIRECTION('',(0.,0.,-1.));
#26218=DIRECTION('center_axis',(0.,0.,-1.));
#26219=DIRECTION('ref_axis',(-0.707106781186547,-0.707106781186547,0.));
#26220=DIRECTION('center_axis',(0.,1.,0.));
#26221=DIRECTION('ref_axis',(-0.70710678118655,0.,0.707106781186545));
#26222=DIRECTION('center_axis',(0.,1.,0.));
#26223=DIRECTION('ref_axis',(-1.,0.,0.));
#26224=DIRECTION('',(0.,1.,0.));
#26225=DIRECTION('center_axis',(0.,-1.,0.));
#26226=DIRECTION('ref_axis',(0.,0.,1.));
#26227=DIRECTION('',(0.,-1.,0.));
#26228=DIRECTION('center_axis',(1.,0.,0.));
#26229=DIRECTION('ref_axis',(0.,0.707106781186545,0.70710678118655));
#26230=DIRECTION('center_axis',(1.,0.,0.));
#26231=DIRECTION('ref_axis',(0.,1.,0.));
#26232=DIRECTION('',(1.,0.,0.));
#26233=DIRECTION('center_axis',(-1.,0.,0.));
#26234=DIRECTION('ref_axis',(0.,0.,1.));
#26235=DIRECTION('',(-1.,0.,0.));
#26236=DIRECTION('center_axis',(-0.816496580927725,-0.408248290463866,-0.408248290463863));
#26237=DIRECTION('ref_axis',(-0.577350269189628,0.577350269189628,0.577350269189622));
#26238=DIRECTION('center_axis',(0.,0.,1.));
#26239=DIRECTION('ref_axis',(-0.707106781186551,0.707106781186544,0.));
#26240=DIRECTION('center_axis',(-0.816496580927725,0.408248290463866,0.408248290463863));
#26241=DIRECTION('ref_axis',(0.577350269189628,0.577350269189628,0.577350269189622));
#26242=DIRECTION('center_axis',(0.,0.,1.));
#26243=DIRECTION('ref_axis',(0.707106781186547,0.707106781186547,0.));
#26244=DIRECTION('center_axis',(-1.,0.,0.));
#26245=DIRECTION('ref_axis',(0.,-0.707106781186549,0.707106781186546));
#26246=DIRECTION('',(-1.,0.,0.));
#26247=DIRECTION('center_axis',(1.,0.,0.));
#26248=DIRECTION('ref_axis',(0.,0.,1.));
#26249=DIRECTION('center_axis',(-0.816496580927726,0.408248290463864,-0.408248290463863));
#26250=DIRECTION('ref_axis',(-0.577350269189628,-0.577350269189625,0.577350269189625));
#26251=DIRECTION('center_axis',(0.,0.,1.));
#26252=DIRECTION('ref_axis',(-0.70710678118655,-0.707106781186545,0.));
#26253=DIRECTION('center_axis',(0.,-0.568073288796263,-0.82297796966638));
#26254=DIRECTION('ref_axis',(0.707106781186551,-0.581933303118231,0.40168847471878));
#26255=DIRECTION('center_axis',(0.,-0.464718576777247,0.885458437419922));
#26256=DIRECTION('ref_axis',(-5.3743881657201E-17,-0.885458437419922,-0.464718576777247));
#26257=DIRECTION('',(0.,-0.568073288796263,-0.82297796966638));
#26258=DIRECTION('center_axis',(0.,1.,0.));
#26259=DIRECTION('ref_axis',(0.70710678118655,0.,-0.707106781186545));
#26260=DIRECTION('center_axis',(0.,-0.464718576777246,-0.885458437419922));
#26261=DIRECTION('ref_axis',(0.,0.885458437419922,-0.464718576777246));
#26262=DIRECTION('',(0.,1.,0.));
#26263=DIRECTION('center_axis',(0.,-0.568073288796263,0.822977969666381));
#26264=DIRECTION('ref_axis',(0.707106781186551,0.581933303118232,0.401688474718779));
#26265=DIRECTION('center_axis',(0.,0.82297796966638,-0.568073288796263));
#26266=DIRECTION('ref_axis',(-8.11003697939828E-16,0.568073288796263,0.82297796966638));
#26267=DIRECTION('',(0.,-0.568073288796263,0.822977969666381));
#26268=DIRECTION('center_axis',(0.,0.,1.));
#26269=DIRECTION('ref_axis',(1.,0.,0.));
#26270=DIRECTION('center_axis',(0.,0.,-1.));
#26271=DIRECTION('ref_axis',(0.707106781186547,0.707106781186547,0.));
#26272=DIRECTION('center_axis',(0.,-0.707106781186548,0.707106781186548));
#26273=DIRECTION('ref_axis',(0.,0.707106781186548,0.707106781186548));
#26274=DIRECTION('center_axis',(0.,0.,-1.));
#26275=DIRECTION('ref_axis',(0.707106781186547,0.707106781186547,0.));
#26276=DIRECTION('',(0.,0.,1.));
#26277=DIRECTION('center_axis',(1.,0.,0.));
#26278=DIRECTION('ref_axis',(0.,0.,-1.));
#26279=DIRECTION('center_axis',(1.,0.,0.));
#26280=DIRECTION('ref_axis',(0.,0.,-1.));
#26281=DIRECTION('',(1.,0.,0.));
#26282=DIRECTION('',(-1.,0.,0.));
#26283=DIRECTION('center_axis',(1.,0.,0.));
#26284=DIRECTION('ref_axis',(0.,0.,-1.));
#26285=DIRECTION('',(1.,0.,0.));
#26286=DIRECTION('',(-1.,0.,0.));
#26287=DIRECTION('center_axis',(1.,0.,0.));
#26288=DIRECTION('ref_axis',(0.,0.,-1.));
#26289=DIRECTION('',(1.,0.,0.));
#26290=DIRECTION('',(-1.,0.,0.));
#26291=DIRECTION('center_axis',(1.,0.,0.));
#26292=DIRECTION('ref_axis',(0.,0.,-1.));
#26293=DIRECTION('',(1.,0.,0.));
#26294=DIRECTION('center_axis',(1.41247214930022E-16,0.568073288796262,
0.822977969666381));
#26295=DIRECTION('ref_axis',(0.423270070760653,-0.745620968714058,0.514676420882269));
#26296=DIRECTION('center_axis',(0.,0.,-1.));
#26297=DIRECTION('ref_axis',(-5.71055681676799E-16,-1.,0.));
#26298=DIRECTION('',(0.,0.568073288796263,0.822977969666381));
#26299=DIRECTION('',(0.,-0.568073288796263,-0.822977969666381));
#26300=DIRECTION('',(0.,-0.568073288796263,-0.822977969666381));
#26301=DIRECTION('center_axis',(1.,0.,0.));
#26302=DIRECTION('ref_axis',(0.,0.,-1.));
#26303=DIRECTION('center_axis',(1.,0.,0.));
#26304=DIRECTION('ref_axis',(0.,0.,-1.));
#26305=DIRECTION('',(1.,0.,0.));
#26306=DIRECTION('center_axis',(-1.,0.,0.));
#26307=DIRECTION('ref_axis',(0.,-0.822977969666381,0.568073288796262));
#26308=DIRECTION('',(1.,0.,0.));
#26309=DIRECTION('',(-1.,0.,0.));
#26310=DIRECTION('center_axis',(-1.,0.,0.));
#26311=DIRECTION('ref_axis',(0.,-0.822977969666381,0.568073288796262));
#26312=DIRECTION('center_axis',(-1.,0.,0.));
#26313=DIRECTION('ref_axis',(0.,-0.707106781186549,0.707106781186546));
#26314=DIRECTION('center_axis',(-1.,0.,0.));
#26315=DIRECTION('ref_axis',(0.,-1.,0.));
#26316=DIRECTION('',(-1.,0.,0.));
#26317=DIRECTION('center_axis',(1.,0.,0.));
#26318=DIRECTION('ref_axis',(0.,0.,1.));
#26319=DIRECTION('center_axis',(0.,0.,1.));
#26320=DIRECTION('ref_axis',(0.707106781186547,-0.707106781186547,0.));
#26321=DIRECTION('center_axis',(1.85037170770859E-15,0.,-1.));
#26322=DIRECTION('ref_axis',(1.,0.,1.85037170770859E-15));
#26323=DIRECTION('center_axis',(0.707106781186548,0.,-0.707106781186548));
#26324=DIRECTION('ref_axis',(0.707106781186548,0.,0.707106781186548));
#26325=DIRECTION('',(0.,0.,1.));
#26326=DIRECTION('center_axis',(-0.408248290463863,-0.816496580927727,-0.408248290463863));
#26327=DIRECTION('ref_axis',(0.577350269189626,-0.577350269189626,0.577350269189626));
#26328=DIRECTION('center_axis',(0.,-1.,0.));
#26329=DIRECTION('ref_axis',(0.707106781186547,0.,0.707106781186547));
#26330=DIRECTION('center_axis',(0.,1.,0.));
#26331=DIRECTION('ref_axis',(-0.707106781186547,0.,0.707106781186547));
#26332=DIRECTION('center_axis',(0.,1.,0.));
#26333=DIRECTION('ref_axis',(-1.,0.,0.));
#26334=DIRECTION('',(0.,1.,0.));
#26335=DIRECTION('center_axis',(-0.707106781186548,0.707106781186548,0.));
#26336=DIRECTION('ref_axis',(-0.707106781186548,-0.707106781186548,0.));
#26337=DIRECTION('',(0.,-1.,0.));
#26338=DIRECTION('center_axis',(-0.816496580927726,0.408248290463864,-0.408248290463863));
#26339=DIRECTION('ref_axis',(-0.577350269189626,-0.577350269189626,0.577350269189626));
#26340=DIRECTION('center_axis',(0.,0.,1.));
#26341=DIRECTION('ref_axis',(-0.707106781186547,-0.707106781186547,0.));
#26342=DIRECTION('center_axis',(0.,0.,-1.));
#26343=DIRECTION('ref_axis',(-0.707106781186547,-0.707106781186547,0.));
#26344=DIRECTION('',(0.,0.,-1.));
#26345=DIRECTION('center_axis',(-1.,0.,0.));
#26346=DIRECTION('ref_axis',(0.,0.,1.));
#26347=DIRECTION('',(0.,1.,0.));
#26348=DIRECTION('center_axis',(1.,0.,0.));
#26349=DIRECTION('ref_axis',(0.,0.707106781186547,-0.707106781186547));
#26350=DIRECTION('',(0.,0.,-1.));
#26351=DIRECTION('',(0.,-1.,0.));
#26352=DIRECTION('',(0.,0.,1.));
#26353=DIRECTION('center_axis',(-1.,0.,0.));
#26354=DIRECTION('ref_axis',(0.,0.,-1.));
#26355=DIRECTION('center_axis',(-1.,0.,0.));
#26356=DIRECTION('ref_axis',(0.,0.,-1.));
#26357=DIRECTION('',(0.,0.,1.));
#26358=DIRECTION('center_axis',(-1.,0.,0.));
#26359=DIRECTION('ref_axis',(0.,0.,-1.));
#26360=DIRECTION('center_axis',(-1.,0.,0.));
#26361=DIRECTION('ref_axis',(0.,0.,1.));
#26362=DIRECTION('center_axis',(1.,0.,0.));
#26363=DIRECTION('ref_axis',(0.,0.,-1.));
#26364=DIRECTION('center_axis',(0.,-1.,0.));
#26365=DIRECTION('ref_axis',(0.,0.,-1.));
#26366=DIRECTION('center_axis',(-1.,0.,0.));
#26367=DIRECTION('ref_axis',(0.,0.,-1.));
#26368=DIRECTION('center_axis',(-1.,0.,0.));
#26369=DIRECTION('ref_axis',(0.,0.,-1.));
#26370=DIRECTION('center_axis',(1.,0.,0.));
#26371=DIRECTION('ref_axis',(0.,0.,-1.));
#26372=DIRECTION('center_axis',(0.,0.,-1.));
#26373=DIRECTION('ref_axis',(0.70710678118655,0.707106781186545,0.));
#26374=DIRECTION('',(0.,0.,-1.));
#26375=DIRECTION('center_axis',(-0.707106781186548,0.,0.707106781186548));
#26376=DIRECTION('ref_axis',(0.707106781186548,4.088782444489E-17,0.707106781186548));
#26377=DIRECTION('',(0.,0.,1.));
#26378=DIRECTION('center_axis',(0.,0.,1.));
#26379=DIRECTION('ref_axis',(0.707106781186551,0.707106781186544,0.));
#26380=DIRECTION('',(0.,0.,-1.));
#26381=DIRECTION('center_axis',(1.,0.,0.));
#26382=DIRECTION('ref_axis',(0.,0.,-1.));
#26383=DIRECTION('center_axis',(1.,0.,0.));
#26384=DIRECTION('ref_axis',(0.,0.,-1.));
#26385=DIRECTION('',(1.,0.,0.));
#26386=DIRECTION('center_axis',(-1.,0.,0.));
#26387=DIRECTION('ref_axis',(0.,0.,1.));
#26388=DIRECTION('center_axis',(1.,0.,0.));
#26389=DIRECTION('ref_axis',(0.,0.,-1.));
#26390=DIRECTION('center_axis',(0.,-1.,0.));
#26391=DIRECTION('ref_axis',(0.,0.,-1.));
#26392=DIRECTION('center_axis',(-1.,0.,0.));
#26393=DIRECTION('ref_axis',(0.,0.,-1.));
#26394=DIRECTION('center_axis',(-1.,0.,0.));
#26395=DIRECTION('ref_axis',(0.,0.,-1.));
#26396=DIRECTION('center_axis',(1.,0.,0.));
#26397=DIRECTION('ref_axis',(0.,0.,-1.));
#26398=DIRECTION('center_axis',(1.,0.,0.));
#26399=DIRECTION('ref_axis',(0.,0.,-1.));
#26400=DIRECTION('',(1.,0.,0.));
#26401=DIRECTION('center_axis',(1.,0.,0.));
#26402=DIRECTION('ref_axis',(0.,0.,-1.));
#26403=DIRECTION('',(0.,-1.,0.));
#26404=DIRECTION('',(0.,1.,0.));
#26405=DIRECTION('center_axis',(1.,0.,0.));
#26406=DIRECTION('ref_axis',(0.,0.,-1.));
#26407=DIRECTION('center_axis',(0.,-1.,0.));
#26408=DIRECTION('ref_axis',(0.,0.,1.));
#26409=DIRECTION('center_axis',(1.,0.,0.));
#26410=DIRECTION('ref_axis',(0.,0.,-1.));
#26411=DIRECTION('center_axis',(0.,-1.,0.));
#26412=DIRECTION('ref_axis',(0.,0.,1.));
#26413=DIRECTION('center_axis',(0.,0.,1.));
#26414=DIRECTION('ref_axis',(-0.70710678118655,0.707106781186545,0.));
#26415=DIRECTION('center_axis',(0.,0.,1.));
#26416=DIRECTION('ref_axis',(-0.707106781186551,0.707106781186544,0.));
#26417=DIRECTION('',(0.,0.,-1.));
#26418=DIRECTION('center_axis',(-0.707106781186548,0.,-0.707106781186548));
#26419=DIRECTION('ref_axis',(-0.707106781186548,4.088782444489E-17,0.707106781186548));
#26420=DIRECTION('center_axis',(-1.,0.,0.));
#26421=DIRECTION('ref_axis',(0.,0.707106781186547,-0.707106781186547));
#26422=DIRECTION('',(-1.,0.,0.));
#26423=DIRECTION('center_axis',(-1.,0.,0.));
#26424=DIRECTION('ref_axis',(0.,0.707106781186547,-0.707106781186547));
#26425=DIRECTION('',(1.,0.,0.));
#26426=DIRECTION('center_axis',(0.,0.,-1.));
#26427=DIRECTION('ref_axis',(-1.,0.,0.));
#26428=DIRECTION('',(0.,-1.,0.));
#26429=DIRECTION('center_axis',(-1.,0.,0.));
#26430=DIRECTION('ref_axis',(0.,-0.707106781186547,0.707106781186547));
#26431=DIRECTION('',(-1.,0.,0.));
#26432=DIRECTION('center_axis',(0.,0.,1.));
#26433=DIRECTION('ref_axis',(1.,0.,0.));
#26434=DIRECTION('',(0.,-1.,0.));
#26435=DIRECTION('',(1.,0.,0.));
#26436=DIRECTION('',(0.,1.,0.));
#26437=DIRECTION('',(1.,0.,0.));
#26438=DIRECTION('center_axis',(1.,0.,0.));
#26439=DIRECTION('ref_axis',(0.,0.707106781186547,0.707106781186547));
#26440=DIRECTION('center_axis',(0.707106781186548,0.707106781186548,0.));
#26441=DIRECTION('ref_axis',(-0.707106781186548,0.707106781186548,0.));
#26442=DIRECTION('',(-1.,0.,0.));
#26443=DIRECTION('center_axis',(0.,1.,0.));
#26444=DIRECTION('ref_axis',(0.,0.,1.));
#26445=DIRECTION('',(0.,0.,-1.));
#26446=DIRECTION('center_axis',(0.,1.,0.));
#26447=DIRECTION('ref_axis',(-0.707106781186547,0.,0.707106781186547));
#26448=DIRECTION('center_axis',(0.,-1.,0.));
#26449=DIRECTION('ref_axis',(0.,0.,1.));
#26450=DIRECTION('center_axis',(1.,0.,0.));
#26451=DIRECTION('ref_axis',(0.,0.707106781186545,0.70710678118655));
#26452=DIRECTION('center_axis',(1.,0.,0.));
#26453=DIRECTION('ref_axis',(0.,1.,0.));
#26454=DIRECTION('center_axis',(-1.,3.70074341541718E-15,0.));
#26455=DIRECTION('ref_axis',(0.,0.,1.));
#26456=DIRECTION('',(-1.,0.,0.));
#26457=DIRECTION('center_axis',(-0.816496580927725,-0.408248290463866,-0.408248290463863));
#26458=DIRECTION('ref_axis',(-0.577350269189628,0.577350269189628,0.577350269189622));
#26459=DIRECTION('center_axis',(0.,1.,0.));
#26460=DIRECTION('ref_axis',(0.707106781186547,0.,0.707106781186547));
#26461=DIRECTION('center_axis',(0.,-1.,0.));
#26462=DIRECTION('ref_axis',(1.,0.,0.));
#26463=DIRECTION('center_axis',(-0.816496580927725,0.408248290463866,0.408248290463863));
#26464=DIRECTION('ref_axis',(0.577350269189626,0.577350269189629,0.577350269189623));
#26465=DIRECTION('center_axis',(0.,1.,0.));
#26466=DIRECTION('ref_axis',(1.,0.,0.));
#26467=DIRECTION('',(1.,0.,0.));
#26468=DIRECTION('',(0.,0.,-1.));
#26469=DIRECTION('center_axis',(0.,1.,0.));
#26470=DIRECTION('ref_axis',(-0.708113264397705,0.,-0.706098863321579));
#26471=DIRECTION('center_axis',(0.,1.,0.));
#26472=DIRECTION('ref_axis',(-0.708113264397705,0.,-0.706098863321579));
#26473=DIRECTION('',(1.,0.,0.));
#26474=DIRECTION('',(0.,0.,-1.));
#26475=DIRECTION('',(1.,0.,0.));
#26476=DIRECTION('center_axis',(0.,-1.,0.));
#26477=DIRECTION('ref_axis',(0.70710678118655,0.,0.707106781186545));
#26478=DIRECTION('',(0.,0.,-1.));
#26479=DIRECTION('',(-1.,0.,0.));
#26480=DIRECTION('',(0.,0.,-1.));
#26481=DIRECTION('',(-1.,0.,0.));
#26482=DIRECTION('',(0.,0.,1.));
#26483=DIRECTION('',(-1.,0.,0.));
#26484=DIRECTION('',(0.,0.,-1.));
#26485=DIRECTION('',(1.,0.,0.));
#26486=DIRECTION('',(1.,0.,0.));
#26487=DIRECTION('',(0.,0.,1.));
#26488=DIRECTION('',(-1.,0.,0.));
#26489=DIRECTION('',(-1.,0.,0.));
#26490=DIRECTION('',(0.,0.,-1.));
#26491=DIRECTION('',(0.,0.,1.));
#26492=DIRECTION('',(-1.,0.,0.));
#26493=DIRECTION('',(0.,0.,-1.));
#26494=DIRECTION('',(1.,0.,0.));
#26495=DIRECTION('',(0.,0.,1.));
#26496=DIRECTION('',(-1.,0.,0.));
#26497=DIRECTION('center_axis',(0.,1.,0.));
#26498=DIRECTION('ref_axis',(1.,0.,0.));
#26499=DIRECTION('',(-1.,0.,0.));
#26500=DIRECTION('',(0.,0.,-1.));
#26501=DIRECTION('',(1.,0.,0.));
#26502=DIRECTION('center_axis',(0.,1.,0.));
#26503=DIRECTION('ref_axis',(1.,0.,0.));
#26504=DIRECTION('center_axis',(0.,1.,0.));
#26505=DIRECTION('ref_axis',(1.,0.,0.));
#26506=DIRECTION('center_axis',(1.,0.,0.));
#26507=DIRECTION('ref_axis',(0.,-0.707106781186547,0.707106781186547));
#26508=DIRECTION('center_axis',(0.707106781186548,0.,0.707106781186548));
#26509=DIRECTION('ref_axis',(-0.707106781186548,0.,0.707106781186548));
#26510=DIRECTION('',(-1.,0.,0.));
#26511=DIRECTION('center_axis',(0.,0.,-1.));
#26512=DIRECTION('ref_axis',(-0.70710678118655,-0.707106781186545,0.));
#26513=DIRECTION('',(0.,0.,-1.));
#26514=DIRECTION('center_axis',(1.,0.,0.));
#26515=DIRECTION('ref_axis',(0.,0.,-1.));
#26516=DIRECTION('center_axis',(-1.,0.,0.));
#26517=DIRECTION('ref_axis',(0.,0.,-1.));
#26518=DIRECTION('center_axis',(0.,-1.,0.));
#26519=DIRECTION('ref_axis',(0.,0.,1.));
#26520=DIRECTION('center_axis',(-1.,0.,0.));
#26521=DIRECTION('ref_axis',(0.,0.,-1.));
#26522=DIRECTION('center_axis',(0.,0.,1.));
#26523=DIRECTION('ref_axis',(-0.707106781186553,0.707106781186542,0.));
#26524=DIRECTION('center_axis',(-0.70710678118655,0.,-0.707106781186545));
#26525=DIRECTION('ref_axis',(-0.707106781186545,8.17756488897796E-17,0.70710678118655));
#26526=DIRECTION('',(0.,0.,1.));
#26527=DIRECTION('',(0.,0.,1.));
#26528=DIRECTION('center_axis',(0.,-0.822977969666381,-0.568073288796263));
#26529=DIRECTION('ref_axis',(0.,-0.568073288796263,0.822977969666381));
#26530=DIRECTION('',(-1.,0.,0.));
#26531=DIRECTION('',(0.,-0.568073288796263,0.822977969666381));
#26532=DIRECTION('',(-1.,0.,0.));
#26533=DIRECTION('center_axis',(0.,0.568073288796263,0.822977969666381));
#26534=DIRECTION('ref_axis',(0.707106781186551,0.581933303118231,-0.401688474718779));
#26535=DIRECTION('center_axis',(0.,0.,-1.));
#26536=DIRECTION('ref_axis',(9.51759469461333E-17,1.,0.));
#26537=DIRECTION('',(0.,0.568073288796263,0.822977969666381));
#26538=DIRECTION('center_axis',(0.,-0.822977969666381,0.568073288796263));
#26539=DIRECTION('ref_axis',(0.,0.568073288796263,0.822977969666381));
#26540=DIRECTION('',(-1.,0.,0.));
#26541=DIRECTION('',(0.,0.568073288796263,0.822977969666381));
#26542=DIRECTION('center_axis',(0.,-0.568073288796263,0.822977969666381));
#26543=DIRECTION('ref_axis',(0.707106781186551,0.581933303118231,0.401688474718779));
#26544=DIRECTION('center_axis',(0.,1.,0.));
#26545=DIRECTION('ref_axis',(0.,0.,1.));
#26546=DIRECTION('',(0.,-0.568073288796263,0.822977969666381));
#26547=DIRECTION('center_axis',(0.,-0.822977969666381,-0.568073288796263));
#26548=DIRECTION('ref_axis',(0.,-0.568073288796263,0.822977969666381));
#26549=DIRECTION('',(-1.,0.,0.));
#26550=DIRECTION('',(0.,-0.568073288796263,0.822977969666381));
#26551=DIRECTION('center_axis',(0.,-1.,0.));
#26552=DIRECTION('ref_axis',(0.70710678118655,0.,0.707106781186545));
#26553=DIRECTION('',(0.,-1.,0.));
#26554=DIRECTION('center_axis',(0.,-0.707106781186548,0.707106781186548));
#26555=DIRECTION('ref_axis',(0.,0.707106781186548,0.707106781186548));
#26556=DIRECTION('center_axis',(0.,0.885458437419924,0.464718576777243));
#26557=DIRECTION('ref_axis',(-3.07205107678817E-16,-0.464718576777243,0.885458437419924));
#26558=DIRECTION('center_axis',(0.,0.,-1.));
#26559=DIRECTION('ref_axis',(0.,-1.,0.));
#26560=DIRECTION('',(0.,-1.,0.));
#26561=DIRECTION('center_axis',(-0.408248290463865,0.408248290463858,-0.816496580927728));
#26562=DIRECTION('ref_axis',(0.577350269189634,-0.577350269189621,-0.577350269189622));
#26563=DIRECTION('center_axis',(0.,-1.,0.));
#26564=DIRECTION('ref_axis',(0.707106781186551,0.,-0.707106781186544));
#26565=DIRECTION('center_axis',(0.,0.,1.));
#26566=DIRECTION('ref_axis',(0.70710678118655,0.707106781186545,0.));
#26567=DIRECTION('center_axis',(0.,0.954719322541023,-0.297508008575921));
#26568=DIRECTION('ref_axis',(0.,0.297508008575921,0.954719322541023));
#26569=DIRECTION('',(0.,0.,1.));
#26570=DIRECTION('center_axis',(0.,-0.568073288796263,-0.822977969666381));
#26571=DIRECTION('ref_axis',(0.707106781186551,-0.581933303118231,0.401688474718779));
#26572=DIRECTION('center_axis',(0.,1.,0.));
#26573=DIRECTION('ref_axis',(0.70710678118655,0.,-0.707106781186545));
#26574=DIRECTION('center_axis',(0.,-1.,0.));
#26575=DIRECTION('ref_axis',(0.,0.,-1.));
#26576=DIRECTION('center_axis',(-1.,0.,0.));
#26577=DIRECTION('ref_axis',(0.,0.707106781186545,-0.70710678118655));
#26578=DIRECTION('center_axis',(-1.,0.,0.));
#26579=DIRECTION('ref_axis',(0.,1.,0.));
#26580=DIRECTION('center_axis',(-1.,0.,0.));
#26581=DIRECTION('ref_axis',(0.,0.707106781186545,-0.70710678118655));
#26582=DIRECTION('center_axis',(0.40824829046386,-0.816496580927726,-0.408248290463866));
#26583=DIRECTION('ref_axis',(0.577350269189622,0.577350269189628,-0.577350269189628));
#26584=DIRECTION('center_axis',(-1.,0.,0.));
#26585=DIRECTION('ref_axis',(0.,-0.707106781186547,0.707106781186547));
#26586=DIRECTION('',(-1.,0.,0.));
#26587=DIRECTION('center_axis',(-0.707106781186548,-0.707106781186548,0.));
#26588=DIRECTION('ref_axis',(0.707106781186548,-0.707106781186548,0.));
#26589=DIRECTION('center_axis',(0.,0.,1.));
#26590=DIRECTION('ref_axis',(1.,0.,0.));
#26591=DIRECTION('',(0.,-1.,0.));
#26592=DIRECTION('',(1.,0.,0.));
#26593=DIRECTION('',(0.,-1.,0.));
#26594=DIRECTION('',(1.,0.,0.));
#26595=DIRECTION('',(0.,1.,0.));
#26596=DIRECTION('',(-1.,0.,0.));
#26597=DIRECTION('center_axis',(1.,0.,0.));
#26598=DIRECTION('ref_axis',(0.,0.707106781186547,0.707106781186547));
#26599=DIRECTION('center_axis',(-0.707106781186548,0.707106781186548,0.));
#26600=DIRECTION('ref_axis',(0.707106781186548,0.707106781186548,0.));
#26601=DIRECTION('',(-1.,0.,0.));
#26602=DIRECTION('center_axis',(1.,0.,0.));
#26603=DIRECTION('ref_axis',(0.,0.,-1.));
#26604=DIRECTION('center_axis',(-1.,0.,0.));
#26605=DIRECTION('ref_axis',(0.,0.,-1.));
#26606=DIRECTION('center_axis',(0.,-1.,0.));
#26607=DIRECTION('ref_axis',(0.,0.,1.));
#26608=DIRECTION('center_axis',(1.,0.,0.));
#26609=DIRECTION('ref_axis',(0.,0.,-1.));
#26610=DIRECTION('center_axis',(-1.,0.,0.));
#26611=DIRECTION('ref_axis',(0.,0.,-1.));
#26612=DIRECTION('center_axis',(-1.,0.,0.));
#26613=DIRECTION('ref_axis',(0.,0.,-1.));
#26614=DIRECTION('center_axis',(-1.,0.,0.));
#26615=DIRECTION('ref_axis',(0.,0.,-1.));
#26616=DIRECTION('',(-1.,0.,0.));
#26617=DIRECTION('center_axis',(-1.,0.,0.));
#26618=DIRECTION('ref_axis',(0.,0.,1.));
#26619=DIRECTION('center_axis',(-1.,0.,0.));
#26620=DIRECTION('ref_axis',(0.,0.,-1.));
#26621=DIRECTION('',(0.,0.,1.));
#26622=DIRECTION('',(0.,1.,0.));
#26623=DIRECTION('',(0.,0.,-1.));
#26624=DIRECTION('',(0.,-1.,0.));
#26625=DIRECTION('',(0.,0.,1.));
#26626=DIRECTION('center_axis',(-1.,0.,0.));
#26627=DIRECTION('ref_axis',(0.,0.,-1.));
#26628=DIRECTION('center_axis',(1.,0.,0.));
#26629=DIRECTION('ref_axis',(0.,0.,-1.));
#26630=DIRECTION('center_axis',(0.,-1.,0.));
#26631=DIRECTION('ref_axis',(0.,0.,1.));
#26632=DIRECTION('center_axis',(1.,0.,0.));
#26633=DIRECTION('ref_axis',(0.,0.,-1.));
#26634=DIRECTION('center_axis',(0.,0.,1.));
#26635=DIRECTION('ref_axis',(-0.70710678118655,0.707106781186545,0.));
#26636=DIRECTION('center_axis',(0.,0.,-1.));
#26637=DIRECTION('ref_axis',(-1.,0.,0.));
#26638=DIRECTION('center_axis',(0.707106781186548,0.,0.707106781186548));
#26639=DIRECTION('ref_axis',(-0.707106781186548,4.088782444489E-17,0.707106781186548));
#26640=DIRECTION('center_axis',(-1.,0.,0.));
#26641=DIRECTION('ref_axis',(0.,0.,-1.));
#26642=DIRECTION('center_axis',(-1.,0.,0.));
#26643=DIRECTION('ref_axis',(0.,0.,-1.));
#26644=DIRECTION('center_axis',(-1.,0.,0.));
#26645=DIRECTION('ref_axis',(0.,0.,-1.));
#26646=DIRECTION('',(-1.,0.,0.));
#26647=DIRECTION('center_axis',(-1.,0.,0.));
#26648=DIRECTION('ref_axis',(0.,0.,1.));
#26649=DIRECTION('',(0.,1.,0.));
#26650=DIRECTION('center_axis',(-1.,0.,0.));
#26651=DIRECTION('ref_axis',(0.,0.,-1.));
#26652=DIRECTION('center_axis',(1.,0.,0.));
#26653=DIRECTION('ref_axis',(0.,0.707106781186545,0.70710678118655));
#26654=DIRECTION('',(1.,0.,0.));
#26655=DIRECTION('center_axis',(0.,0.,1.));
#26656=DIRECTION('ref_axis',(1.,0.,0.));
#26657=DIRECTION('center_axis',(1.,0.,0.));
#26658=DIRECTION('ref_axis',(0.,0.707106781186545,0.70710678118655));
#26659=DIRECTION('center_axis',(-0.707106781186548,0.,0.707106781186547));
#26660=DIRECTION('ref_axis',(0.707106781186547,-4.088782444489E-17,0.707106781186548));
#26661=DIRECTION('center_axis',(0.,0.,-1.));
#26662=DIRECTION('ref_axis',(0.70710678118655,0.707106781186545,0.));
#26663=DIRECTION('center_axis',(0.,0.,-1.));
#26664=DIRECTION('ref_axis',(0.70710678118655,0.707106781186545,0.));
#26665=DIRECTION('',(0.,0.,-1.));
#26666=DIRECTION('center_axis',(0.,0.,1.));
#26667=DIRECTION('ref_axis',(1.,0.,0.));
#26668=DIRECTION('',(0.,1.,0.));
#26669=DIRECTION('center_axis',(0.,0.,1.));
#26670=DIRECTION('ref_axis',(-0.70710678118655,0.707106781186545,0.));
#26671=DIRECTION('center_axis',(0.,0.,-1.));
#26672=DIRECTION('ref_axis',(-0.70710678118655,0.707106781186545,0.));
#26673=DIRECTION('center_axis',(-0.707106781186548,0.,-0.707106781186548));
#26674=DIRECTION('ref_axis',(-0.707106781186548,4.088782444489E-17,0.707106781186548));
#26675=DIRECTION('',(0.,0.,1.));
#26676=DIRECTION('center_axis',(-1.,0.,0.));
#26677=DIRECTION('ref_axis',(0.,0.,1.));
#26678=DIRECTION('',(0.,0.,1.));
#26679=DIRECTION('',(0.,1.,0.));
#26680=DIRECTION('',(0.,-1.,0.));
#26681=DIRECTION('center_axis',(1.,0.,0.));
#26682=DIRECTION('ref_axis',(0.,0.707106781186545,0.70710678118655));
#26683=DIRECTION('center_axis',(-0.707106781186548,0.,0.707106781186548));
#26684=DIRECTION('ref_axis',(0.707106781186548,4.088782444489E-17,0.707106781186548));
#26685=DIRECTION('',(1.,0.,0.));
#26686=DIRECTION('center_axis',(0.,0.,1.));
#26687=DIRECTION('ref_axis',(1.,0.,0.));
#26688=DIRECTION('',(0.,-1.,0.));
#26689=DIRECTION('',(-1.,0.,0.));
#26690=DIRECTION('',(0.,-1.,0.));
#26691=DIRECTION('center_axis',(1.,0.,0.));
#26692=DIRECTION('ref_axis',(0.,0.707106781186545,0.70710678118655));
#26693=DIRECTION('center_axis',(-1.,0.,0.));
#26694=DIRECTION('ref_axis',(0.,0.707106781186545,0.70710678118655));
#26695=DIRECTION('',(1.,0.,0.));
#26696=DIRECTION('center_axis',(0.,0.,1.));
#26697=DIRECTION('ref_axis',(1.,0.,0.));
#26698=DIRECTION('',(0.,-1.,0.));
#26699=DIRECTION('',(-1.,0.,0.));
#26700=DIRECTION('center_axis',(-1.,0.,0.));
#26701=DIRECTION('ref_axis',(0.,0.70710678118655,-0.707106781186545));
#26702=DIRECTION('center_axis',(0.707106781186548,0.,-0.707106781186548));
#26703=DIRECTION('ref_axis',(-0.707106781186548,0.,-0.707106781186548));
#26704=DIRECTION('',(-1.,0.,0.));
#26705=DIRECTION('center_axis',(-0.707106781186548,0.,-0.707106781186548));
#26706=DIRECTION('ref_axis',(0.707106781186548,0.,-0.707106781186548));
#26707=DIRECTION('center_axis',(0.,0.,1.));
#26708=DIRECTION('ref_axis',(-1.,0.,0.));
#26709=DIRECTION('',(0.,-1.,0.));
#26710=DIRECTION('',(-1.,0.,0.));
#26711=DIRECTION('center_axis',(0.,0.,1.));
#26712=DIRECTION('ref_axis',(1.,0.,0.));
#26713=DIRECTION('',(-1.,0.,0.));
#26714=DIRECTION('',(0.,-1.,0.));
#26715=DIRECTION('center_axis',(1.,0.,0.));
#26716=DIRECTION('ref_axis',(0.,0.70710678118655,0.707106781186545));
#26717=DIRECTION('center_axis',(-0.707106781186548,0.,0.707106781186548));
#26718=DIRECTION('ref_axis',(0.707106781186548,0.,0.707106781186548));
#26719=DIRECTION('',(1.,0.,0.));
#26720=DIRECTION('center_axis',(0.707106781186548,0.,0.707106781186548));
#26721=DIRECTION('ref_axis',(-0.707106781186548,0.,0.707106781186548));
#26722=DIRECTION('center_axis',(0.,0.,-1.));
#26723=DIRECTION('ref_axis',(1.,0.,0.));
#26724=DIRECTION('',(0.,-1.,0.));
#26725=DIRECTION('',(1.,0.,0.));
#26726=DIRECTION('center_axis',(0.,0.,-1.));
#26727=DIRECTION('ref_axis',(1.,0.,0.));
#26728=DIRECTION('',(1.,0.,0.));
#26729=DIRECTION('',(0.,-1.,0.));
#26730=DIRECTION('center_axis',(-1.,0.,0.));
#26731=DIRECTION('ref_axis',(0.,0.70710678118655,-0.707106781186545));
#26732=DIRECTION('center_axis',(0.707106781186548,0.,-0.707106781186548));
#26733=DIRECTION('ref_axis',(-0.707106781186548,0.,-0.707106781186548));
#26734=DIRECTION('',(-1.,0.,0.));
#26735=DIRECTION('center_axis',(-0.707106781186548,0.,-0.707106781186548));
#26736=DIRECTION('ref_axis',(0.707106781186548,0.,-0.707106781186548));
#26737=DIRECTION('center_axis',(0.,0.,1.));
#26738=DIRECTION('ref_axis',(-1.,0.,0.));
#26739=DIRECTION('',(0.,-1.,0.));
#26740=DIRECTION('',(-1.,0.,0.));
#26741=DIRECTION('center_axis',(0.,0.,1.));
#26742=DIRECTION('ref_axis',(1.,0.,0.));
#26743=DIRECTION('',(-1.,0.,0.));
#26744=DIRECTION('',(0.,-1.,0.));
#26745=DIRECTION('center_axis',(1.,0.,0.));
#26746=DIRECTION('ref_axis',(0.,0.70710678118655,0.707106781186545));
#26747=DIRECTION('center_axis',(-0.707106781186547,0.,0.707106781186548));
#26748=DIRECTION('ref_axis',(0.707106781186548,4.088782444489E-17,0.707106781186547));
#26749=DIRECTION('',(1.,0.,0.));
#26750=DIRECTION('center_axis',(0.707106781186547,0.,0.707106781186548));
#26751=DIRECTION('ref_axis',(-0.707106781186548,4.088782444489E-17,0.707106781186547));
#26752=DIRECTION('center_axis',(0.,0.,-1.));
#26753=DIRECTION('ref_axis',(1.,0.,0.));
#26754=DIRECTION('',(0.,-1.,0.));
#26755=DIRECTION('',(1.,0.,0.));
#26756=DIRECTION('center_axis',(0.,0.,-1.));
#26757=DIRECTION('ref_axis',(1.,0.,0.));
#26758=DIRECTION('',(1.,0.,0.));
#26759=DIRECTION('',(0.,-1.,0.));
#26760=DIRECTION('center_axis',(0.,-1.,0.));
#26761=DIRECTION('ref_axis',(0.,0.,-1.));
#26762=DIRECTION('center_axis',(-1.,0.,-1.22464679914735E-16));
#26763=DIRECTION('ref_axis',(-1.22464679914735E-16,0.,1.));
#26764=DIRECTION('center_axis',(0.,-1.,0.));
#26765=DIRECTION('ref_axis',(1.,0.,0.));
#26766=DIRECTION('center_axis',(0.,-1.,0.));
#26767=DIRECTION('ref_axis',(1.,0.,0.));
#26768=DIRECTION('center_axis',(0.,0.,-1.));
#26769=DIRECTION('ref_axis',(0.707106781186545,0.70710678118655,0.));
#26770=DIRECTION('',(0.,0.,-1.));
#26771=DIRECTION('center_axis',(-1.,0.,0.));
#26772=DIRECTION('ref_axis',(0.,0.,-1.));
#26773=DIRECTION('',(0.,0.,-1.));
#26774=DIRECTION('center_axis',(0.,0.,1.));
#26775=DIRECTION('ref_axis',(-0.707106781186545,0.70710678118655,0.));
#26776=DIRECTION('',(0.,0.,1.));
#26777=DIRECTION('center_axis',(1.,0.,0.));
#26778=DIRECTION('ref_axis',(0.,0.,1.));
#26779=DIRECTION('',(0.,0.,1.));
#26780=DIRECTION('center_axis',(0.,0.,-1.));
#26781=DIRECTION('ref_axis',(0.707106781186545,0.70710678118655,0.));
#26782=DIRECTION('',(0.,0.,-1.));
#26783=DIRECTION('center_axis',(-1.,0.,0.));
#26784=DIRECTION('ref_axis',(0.,0.,-1.));
#26785=DIRECTION('',(0.,0.,-1.));
#26786=DIRECTION('center_axis',(0.,0.,1.));
#26787=DIRECTION('ref_axis',(-0.707106781186545,0.70710678118655,0.));
#26788=DIRECTION('',(0.,0.,1.));
#26789=DIRECTION('center_axis',(1.,0.,0.));
#26790=DIRECTION('ref_axis',(0.,0.,1.));
#26791=DIRECTION('',(0.,0.,1.));
#26792=DIRECTION('center_axis',(0.,-1.,0.));
#26793=DIRECTION('ref_axis',(0.,0.,-1.));
#26794=DIRECTION('center_axis',(-1.,0.,0.));
#26795=DIRECTION('ref_axis',(0.,0.,1.));
#26796=DIRECTION('center_axis',(0.,-1.,0.));
#26797=DIRECTION('ref_axis',(1.,0.,0.));
#26798=DIRECTION('center_axis',(0.,-1.,0.));
#26799=DIRECTION('ref_axis',(1.,0.,0.));
#26800=DIRECTION('center_axis',(0.,-1.,0.));
#26801=DIRECTION('ref_axis',(1.,0.,0.));
#26802=DIRECTION('',(0.,-1.,0.));
#26803=DIRECTION('center_axis',(0.,-1.,0.));
#26804=DIRECTION('ref_axis',(1.,0.,0.));
#26805=DIRECTION('center_axis',(0.,-1.,0.));
#26806=DIRECTION('ref_axis',(0.,0.,-1.));
#26807=DIRECTION('center_axis',(-1.,0.,0.));
#26808=DIRECTION('ref_axis',(0.,0.,1.));
#26809=DIRECTION('center_axis',(0.,-1.,0.));
#26810=DIRECTION('ref_axis',(1.,0.,0.));
#26811=DIRECTION('center_axis',(0.,-1.,0.));
#26812=DIRECTION('ref_axis',(1.,0.,0.));
#26813=DIRECTION('center_axis',(0.,-1.,0.));
#26814=DIRECTION('ref_axis',(1.,0.,0.));
#26815=DIRECTION('',(0.,-1.,0.));
#26816=DIRECTION('center_axis',(0.,-1.,0.));
#26817=DIRECTION('ref_axis',(1.,0.,0.));
#26818=DIRECTION('center_axis',(0.,-1.,0.));
#26819=DIRECTION('ref_axis',(1.,0.,0.));
#26820=DIRECTION('',(0.,-1.,0.));
#26821=DIRECTION('center_axis',(0.,-1.,0.));
#26822=DIRECTION('ref_axis',(1.,0.,0.));
#26823=DIRECTION('center_axis',(0.,1.,0.));
#26824=DIRECTION('ref_axis',(-0.708113264397705,0.,-0.706098863321579));
#26825=DIRECTION('center_axis',(0.,-1.,0.));
#26826=DIRECTION('ref_axis',(1.,0.,0.));
#26827=DIRECTION('center_axis',(0.706098863321579,0.,-0.708113264397705));
#26828=DIRECTION('ref_axis',(0.708113264397705,0.,0.706098863321579));
#26829=DIRECTION('center_axis',(-1.,0.,0.));
#26830=DIRECTION('ref_axis',(0.,0.,1.));
#26831=DIRECTION('center_axis',(1.,0.,0.));
#26832=DIRECTION('ref_axis',(0.,0.,-1.));
#26833=DIRECTION('center_axis',(0.,-1.,0.));
#26834=DIRECTION('ref_axis',(0.,0.,-1.));
#26835=DIRECTION('center_axis',(1.,0.,0.));
#26836=DIRECTION('ref_axis',(0.,0.,-1.));
#26837=DIRECTION('center_axis',(0.,0.,-1.));
#26838=DIRECTION('ref_axis',(0.70710678118655,0.707106781186545,0.));
#26839=DIRECTION('',(0.,0.,-1.));
#26840=DIRECTION('center_axis',(0.,0.,1.));
#26841=DIRECTION('ref_axis',(0.707106781186551,0.707106781186544,0.));
#26842=DIRECTION('',(0.,0.,-1.));
#26843=DIRECTION('center_axis',(-1.,0.,0.));
#26844=DIRECTION('ref_axis',(0.,0.,1.));
#26845=DIRECTION('center_axis',(1.,0.,0.));
#26846=DIRECTION('ref_axis',(0.,0.,-1.));
#26847=DIRECTION('center_axis',(0.,-1.,0.));
#26848=DIRECTION('ref_axis',(0.,0.,-1.));
#26849=DIRECTION('center_axis',(1.,0.,0.));
#26850=DIRECTION('ref_axis',(0.,0.,-1.));
#26851=DIRECTION('',(0.,1.,0.));
#26852=DIRECTION('',(0.,0.,-1.));
#26853=DIRECTION('',(0.,1.,0.));
#26854=DIRECTION('',(0.,0.,1.));
#26855=DIRECTION('center_axis',(1.,0.,0.));
#26856=DIRECTION('ref_axis',(0.,0.707106781186545,0.70710678118655));
#26857=DIRECTION('center_axis',(1.,0.,0.));
#26858=DIRECTION('ref_axis',(0.,1.,0.));
#26859=DIRECTION('center_axis',(-1.,0.,0.));
#26860=DIRECTION('ref_axis',(0.,0.,1.));
#26861=DIRECTION('center_axis',(0.,1.,0.));
#26862=DIRECTION('ref_axis',(0.707106781186547,0.,0.707106781186547));
#26863=DIRECTION('center_axis',(0.,-1.,0.));
#26864=DIRECTION('ref_axis',(1.,0.,0.));
#26865=DIRECTION('center_axis',(-0.816496580927725,0.408248290463866,0.408248290463863));
#26866=DIRECTION('ref_axis',(0.577350269189628,0.577350269189628,0.577350269189622));
#26867=DIRECTION('center_axis',(-0.816496580927725,-0.408248290463866,-0.408248290463863));
#26868=DIRECTION('ref_axis',(-0.577350269189628,0.577350269189628,0.577350269189622));
#26869=DIRECTION('center_axis',(0.,1.,0.));
#26870=DIRECTION('ref_axis',(-0.707106781186547,0.,0.707106781186547));
#26871=DIRECTION('center_axis',(0.,1.,0.));
#26872=DIRECTION('ref_axis',(-0.707106781186547,0.,0.707106781186547));
#26873=DIRECTION('center_axis',(0.,1.,0.));
#26874=DIRECTION('ref_axis',(-1.,0.,0.));
#26875=DIRECTION('center_axis',(0.,0.,1.));
#26876=DIRECTION('ref_axis',(0.707106781186547,-0.707106781186547,0.));
#26877=DIRECTION('center_axis',(0.,0.,-1.));
#26878=DIRECTION('ref_axis',(1.,0.,0.));
#26879=DIRECTION('',(0.,0.,-1.));
#26880=DIRECTION('center_axis',(0.707106781186548,0.,-0.707106781186548));
#26881=DIRECTION('ref_axis',(0.707106781186548,0.,0.707106781186548));
#26882=DIRECTION('center_axis',(0.,1.,0.));
#26883=DIRECTION('ref_axis',(0.707106781186547,0.,0.707106781186547));
#26884=DIRECTION('center_axis',(0.,1.,0.));
#26885=DIRECTION('ref_axis',(0.,0.,1.));
#26886=DIRECTION('center_axis',(-0.816496580927726,-0.408248290463864,0.408248290463863));
#26887=DIRECTION('ref_axis',(0.577350269189625,-0.577350269189627,0.577350269189625));
#26888=DIRECTION('center_axis',(1.,0.,0.));
#26889=DIRECTION('ref_axis',(0.,-0.707106781186548,0.707106781186547));
#26890=DIRECTION('center_axis',(0.,1.,0.));
#26891=DIRECTION('ref_axis',(1.,0.,0.));
#26892=DIRECTION('',(1.,0.,0.));
#26893=DIRECTION('',(1.,0.,0.));
#26894=DIRECTION('',(0.,0.,1.));
#26895=DIRECTION('',(1.,0.,0.));
#26896=DIRECTION('',(0.,0.,1.));
#26897=DIRECTION('center_axis',(0.,1.,0.));
#26898=DIRECTION('ref_axis',(0.70710678118655,0.,0.707106781186545));
#26899=DIRECTION('',(-1.,0.,0.));
#26900=DIRECTION('',(0.,0.,1.));
#26901=DIRECTION('',(-1.,0.,0.));
#26902=DIRECTION('',(0.,0.,-1.));
#26903=DIRECTION('center_axis',(-1.,0.,0.));
#26904=DIRECTION('ref_axis',(0.,-0.707106781186549,0.707106781186546));
#26905=DIRECTION('center_axis',(-1.,0.,0.));
#26906=DIRECTION('ref_axis',(0.,-0.707106781186548,0.707106781186547));
#26907=DIRECTION('center_axis',(0.,1.,0.));
#26908=DIRECTION('ref_axis',(0.707106781186547,0.,-0.707106781186547));
#26909=DIRECTION('center_axis',(0.,1.,0.));
#26910=DIRECTION('ref_axis',(1.,0.,0.));
#26911=DIRECTION('',(0.,1.,0.));
#26912=DIRECTION('',(0.,-1.,0.));
#26913=DIRECTION('center_axis',(0.,0.,1.));
#26914=DIRECTION('ref_axis',(0.707106781186547,-0.707106781186547,0.));
#26915=DIRECTION('center_axis',(0.,0.,1.));
#26916=DIRECTION('ref_axis',(0.,-1.,0.));
#26917=DIRECTION('',(0.,0.,1.));
#26918=DIRECTION('center_axis',(0.,0.,-1.));
#26919=DIRECTION('ref_axis',(1.,0.,0.));
#26920=DIRECTION('center_axis',(0.,1.,0.));
#26921=DIRECTION('ref_axis',(0.707106781186547,0.,0.707106781186547));
#26922=DIRECTION('center_axis',(0.,1.,0.));
#26923=DIRECTION('ref_axis',(0.,0.,1.));
#26924=DIRECTION('',(0.,1.,0.));
#26925=DIRECTION('center_axis',(-0.408248290463863,-0.816496580927727,-0.408248290463863));
#26926=DIRECTION('ref_axis',(0.577350269189626,-0.577350269189626,0.577350269189626));
#26927=DIRECTION('center_axis',(1.,0.,0.));
#26928=DIRECTION('ref_axis',(0.,-0.707106781186547,0.707106781186547));
#26929=DIRECTION('center_axis',(-0.408248290463863,-0.816496580927727,0.408248290463863));
#26930=DIRECTION('ref_axis',(0.577350269189626,-0.577350269189626,-0.577350269189626));
#26931=DIRECTION('center_axis',(1.,0.,0.));
#26932=DIRECTION('ref_axis',(0.,-0.707106781186547,-0.707106781186547));
#26933=DIRECTION('center_axis',(0.,0.,-1.));
#26934=DIRECTION('ref_axis',(-1.,0.,0.));
#26935=DIRECTION('',(1.,0.,0.));
#26936=DIRECTION('',(0.,-1.,0.));
#26937=DIRECTION('',(-1.,0.,0.));
#26938=DIRECTION('center_axis',(1.,0.,0.));
#26939=DIRECTION('ref_axis',(0.,-0.707106781186547,-0.707106781186547));
#26940=DIRECTION('center_axis',(1.,0.,0.));
#26941=DIRECTION('ref_axis',(0.,-1.,0.));
#26942=DIRECTION('center_axis',(1.,0.,0.));
#26943=DIRECTION('ref_axis',(0.,-0.707106781186547,0.707106781186547));
#26944=DIRECTION('center_axis',(0.,0.,-1.));
#26945=DIRECTION('ref_axis',(-0.707106781186547,-0.707106781186547,0.));
#26946=DIRECTION('center_axis',(0.,-1.85037170770859E-15,-1.));
#26947=DIRECTION('ref_axis',(0.,-1.,1.85037170770859E-15));
#26948=DIRECTION('center_axis',(-0.707106781186548,0.,-0.707106781186548));
#26949=DIRECTION('ref_axis',(-0.707106781186548,0.,0.707106781186548));
#26950=DIRECTION('center_axis',(-0.816496580927726,0.408248290463864,-0.408248290463863));
#26951=DIRECTION('ref_axis',(-0.577350269189626,-0.577350269189629,0.577350269189623));
#26952=DIRECTION('center_axis',(-1.,0.,0.));
#26953=DIRECTION('ref_axis',(0.,0.,1.));
#26954=DIRECTION('center_axis',(1.,0.,0.));
#26955=DIRECTION('ref_axis',(0.,0.,-1.));
#26956=DIRECTION('center_axis',(0.,-1.,0.));
#26957=DIRECTION('ref_axis',(0.,0.,-1.));
#26958=DIRECTION('center_axis',(-1.,0.,0.));
#26959=DIRECTION('ref_axis',(0.,0.,-1.));
#26960=DIRECTION('center_axis',(-1.,0.,0.));
#26961=DIRECTION('ref_axis',(0.,0.,-1.));
#26962=DIRECTION('center_axis',(-1.,0.,0.));
#26963=DIRECTION('ref_axis',(0.,0.,-1.));
#26964=DIRECTION('',(-1.,0.,0.));
#26965=DIRECTION('center_axis',(1.,0.,0.));
#26966=DIRECTION('ref_axis',(0.,0.,-1.));
#26967=DIRECTION('',(1.,0.,0.));
#26968=DIRECTION('center_axis',(-1.,0.,0.));
#26969=DIRECTION('ref_axis',(0.,0.,-1.));
#26970=DIRECTION('',(-1.,0.,0.));
#26971=DIRECTION('center_axis',(1.,0.,0.));
#26972=DIRECTION('ref_axis',(0.,0.,-1.));
#26973=DIRECTION('',(1.,0.,0.));
#26974=DIRECTION('center_axis',(-1.,0.,0.));
#26975=DIRECTION('ref_axis',(0.,0.,-1.));
#26976=DIRECTION('',(-1.,0.,0.));
#26977=DIRECTION('',(1.,0.,0.));
#26978=DIRECTION('center_axis',(-1.,0.,0.));
#26979=DIRECTION('ref_axis',(0.,0.,-1.));
#26980=DIRECTION('',(-1.,0.,0.));
#26981=DIRECTION('center_axis',(1.,0.,0.));
#26982=DIRECTION('ref_axis',(0.,0.,-1.));
#26983=DIRECTION('',(0.,1.,0.));
#26984=DIRECTION('center_axis',(-1.,0.,0.));
#26985=DIRECTION('ref_axis',(0.,-0.707106781186547,0.707106781186547));
#26986=DIRECTION('center_axis',(1.,0.,0.));
#26987=DIRECTION('ref_axis',(0.,0.,-1.));
#26988=DIRECTION('center_axis',(1.,0.,0.));
#26989=DIRECTION('ref_axis',(0.,-0.707106781186547,0.707106781186547));
#26990=DIRECTION('center_axis',(1.,0.,0.));
#26991=DIRECTION('ref_axis',(0.,0.,-1.));
#26992=DIRECTION('center_axis',(0.,0.568073288796263,0.82297796966638));
#26993=DIRECTION('ref_axis',(-0.707106781186551,-0.581933303118232,0.40168847471878));
#26994=DIRECTION('center_axis',(0.,-0.954719322541023,0.29750800857592));
#26995=DIRECTION('ref_axis',(1.72031375589253E-17,0.29750800857592,0.954719322541023));
#26996=DIRECTION('',(0.,-0.568073288796263,-0.82297796966638));
#26997=DIRECTION('',(0.,0.568073288796263,0.82297796966638));
#26998=DIRECTION('center_axis',(0.,-0.464718576777245,0.885458437419923));
#26999=DIRECTION('ref_axis',(1.07487763314402E-16,-0.885458437419923,-0.464718576777245));
#27000=DIRECTION('center_axis',(0.,0.82297796966638,-0.568073288796263));
#27001=DIRECTION('ref_axis',(0.,0.568073288796263,0.82297796966638));
#27002=DIRECTION('',(0.,0.568073288796263,0.82297796966638));
#27003=DIRECTION('',(1.,0.,0.));
#27004=DIRECTION('center_axis',(-1.,0.,0.));
#27005=DIRECTION('ref_axis',(0.,0.,1.));
#27006=DIRECTION('',(0.,0.,1.));
#27007=DIRECTION('center_axis',(-1.,0.,0.));
#27008=DIRECTION('ref_axis',(0.,-1.,3.70074341541719E-15));
#27009=DIRECTION('',(0.,0.,1.));
#27010=DIRECTION('',(0.,-0.568073288796263,-0.822977969666381));
#27011=DIRECTION('center_axis',(-1.,0.,0.));
#27012=DIRECTION('ref_axis',(0.,0.,1.));
#27013=DIRECTION('',(0.,-1.,0.));
#27014=DIRECTION('',(0.,0.,-1.));
#27015=DIRECTION('',(0.,1.,0.));
#27016=DIRECTION('',(0.,0.,1.));
#27017=DIRECTION('center_axis',(0.,1.,0.));
#27018=DIRECTION('ref_axis',(-0.70710678118655,0.,0.707106781186545));
#27019=DIRECTION('center_axis',(0.,-0.707106781186548,0.707106781186548));
#27020=DIRECTION('ref_axis',(0.,0.707106781186548,0.707106781186548));
#27021=DIRECTION('',(0.,-1.,0.));
#27022=DIRECTION('center_axis',(0.,0.707106781186548,0.707106781186547));
#27023=DIRECTION('ref_axis',(0.,-0.707106781186547,0.707106781186548));
#27024=DIRECTION('center_axis',(0.,-0.464718576777245,0.885458437419923));
#27025=DIRECTION('ref_axis',(0.,0.885458437419923,0.464718576777245));
#27026=DIRECTION('',(0.,1.,0.));
#27027=DIRECTION('center_axis',(0.,0.464718576777246,0.885458437419923));
#27028=DIRECTION('ref_axis',(0.,-0.885458437419923,0.464718576777246));
#27029=DIRECTION('center_axis',(0.,0.,-1.));
#27030=DIRECTION('ref_axis',(-0.707106781186545,-0.70710678118655,0.));
#27031=DIRECTION('center_axis',(0.,0.954719322541023,-0.29750800857592));
#27032=DIRECTION('ref_axis',(-6.88125502357011E-17,-0.29750800857592,-0.954719322541023));
#27033=DIRECTION('',(0.,0.,-1.));
#27034=DIRECTION('center_axis',(0.,0.,-1.));
#27035=DIRECTION('ref_axis',(-0.707106781186544,-0.707106781186551,0.));
#27036=DIRECTION('center_axis',(0.,0.,-1.));
#27037=DIRECTION('ref_axis',(-0.707106781186545,-0.70710678118655,0.));
#27038=DIRECTION('center_axis',(0.,-0.707106781186548,0.707106781186548));
#27039=DIRECTION('ref_axis',(-4.088782444489E-17,-0.707106781186548,-0.707106781186548));
#27040=DIRECTION('center_axis',(0.,-0.954719322541023,-0.297508008575921));
#27041=DIRECTION('ref_axis',(1.72031375589253E-17,-0.297508008575921,0.954719322541023));
#27042=DIRECTION('',(0.,0.,-1.));
#27043=DIRECTION('center_axis',(0.,0.82297796966638,0.568073288796263));
#27044=DIRECTION('ref_axis',(-3.28483356716743E-17,-0.568073288796263,0.82297796966638));
#27045=DIRECTION('',(0.,0.,-1.));
#27046=DIRECTION('center_axis',(0.,0.822977969666381,-0.568073288796263));
#27047=DIRECTION('ref_axis',(3.28483356716743E-17,-0.568073288796263,-0.822977969666381));
#27048=DIRECTION('',(0.,0.,-1.));
#27049=DIRECTION('center_axis',(-1.,0.,0.));
#27050=DIRECTION('ref_axis',(0.,0.,1.));
#27051=DIRECTION('',(0.,0.,1.));
#27052=DIRECTION('',(0.,1.,0.));
#27053=DIRECTION('center_axis',(-1.,0.,0.));
#27054=DIRECTION('ref_axis',(0.,0.,1.));
#27055=DIRECTION('',(0.,-0.568073288796263,0.82297796966638));
#27056=DIRECTION('',(0.,-0.568073288796263,-0.82297796966638));
#27057=DIRECTION('',(0.,0.568073288796263,-0.822977969666381));
#27058=DIRECTION('',(0.,0.,1.));
#27059=DIRECTION('center_axis',(-1.,0.,0.));
#27060=DIRECTION('ref_axis',(0.,0.,1.));
#27061=DIRECTION('',(0.,-0.568073288796263,-0.822977969666381));
#27062=DIRECTION('',(0.,0.568073288796263,0.822977969666381));
#27063=DIRECTION('center_axis',(1.,0.,0.));
#27064=DIRECTION('ref_axis',(0.,0.,-1.));
#27065=DIRECTION('center_axis',(-1.,0.,0.));
#27066=DIRECTION('ref_axis',(0.,-0.822977969666383,0.568073288796259));
#27067=DIRECTION('center_axis',(0.,-0.568073288796263,-0.822977969666381));
#27068=DIRECTION('ref_axis',(-0.707106781186551,0.581933303118232,-0.40168847471878));
#27069=DIRECTION('center_axis',(0.,1.1421113633536E-15,-1.));
#27070=DIRECTION('ref_axis',(-1.90351893892266E-16,1.,1.1421113633536E-15));
#27071=DIRECTION('center_axis',(0.,1.,0.));
#27072=DIRECTION('ref_axis',(0.,0.,-1.));
#27073=DIRECTION('',(0.,-0.568073288796263,-0.822977969666381));
#27074=DIRECTION('',(0.,0.568073288796263,0.822977969666381));
#27075=DIRECTION('center_axis',(0.,0.82297796966638,0.568073288796263));
#27076=DIRECTION('ref_axis',(5.40669131959885E-16,0.568073288796263,-0.82297796966638));
#27077=DIRECTION('',(0.,0.568073288796263,0.822977969666381));
#27078=DIRECTION('center_axis',(0.,0.568073288796263,0.82297796966638));
#27079=DIRECTION('ref_axis',(-0.707106781186551,-0.581933303118232,0.40168847471878));
#27080=DIRECTION('center_axis',(0.,3.04563030227627E-15,-1.));
#27081=DIRECTION('ref_axis',(1.427639204192E-16,-1.,-3.04563030227627E-15));
#27082=DIRECTION('center_axis',(0.,-1.,0.));
#27083=DIRECTION('ref_axis',(1.31393342686697E-16,0.,1.));
#27084=DIRECTION('',(0.,0.568073288796263,0.82297796966638));
#27085=DIRECTION('',(0.,-0.568073288796263,-0.82297796966638));
#27086=DIRECTION('center_axis',(0.,-0.822977969666381,-0.568073288796263));
#27087=DIRECTION('ref_axis',(9.19137524331805E-16,-0.568073288796263,0.82297796966638));
#27088=DIRECTION('center_axis',(0.,0.568073288796263,-0.822977969666381));
#27089=DIRECTION('ref_axis',(-0.707106781186551,0.581933303118232,0.401688474718779));
#27090=DIRECTION('',(0.,-0.568073288796263,0.822977969666381));
#27091=DIRECTION('center_axis',(0.,0.464718576777247,0.885458437419922));
#27092=DIRECTION('ref_axis',(5.37438816572011E-17,0.885458437419922,-0.464718576777247));
#27093=DIRECTION('',(0.,0.568073288796263,-0.822977969666381));
#27094=DIRECTION('center_axis',(-1.,0.,0.));
#27095=DIRECTION('ref_axis',(0.,0.,1.));
#27096=DIRECTION('',(0.,-0.568073288796263,0.82297796966638));
#27097=DIRECTION('center_axis',(0.,0.82297796966638,0.568073288796263));
#27098=DIRECTION('ref_axis',(0.,-0.568073288796263,0.82297796966638));
#27099=DIRECTION('center_axis',(0.,0.82297796966638,0.568073288796263));
#27100=DIRECTION('ref_axis',(6.48802958351862E-16,-0.568073288796263,0.82297796966638));
#27101=DIRECTION('',(1.,0.,0.));
#27102=DIRECTION('',(0.,-0.568073288796263,0.82297796966638));
#27103=DIRECTION('',(1.,0.,0.));
#27104=DIRECTION('center_axis',(0.,0.82297796966638,0.568073288796263));
#27105=DIRECTION('ref_axis',(0.,0.568073288796263,-0.82297796966638));
#27106=DIRECTION('center_axis',(0.,0.568073288796263,0.822977969666381));
#27107=DIRECTION('ref_axis',(-0.707106781186549,-0.581933303118233,0.401688474718781));
#27108=DIRECTION('center_axis',(0.,0.568073288796261,0.822977969666382));
#27109=DIRECTION('ref_axis',(-1.,0.,0.));
#27110=DIRECTION('',(0.,0.568073288796263,0.822977969666381));
#27111=DIRECTION('center_axis',(0.,-0.822977969666381,-0.568073288796263));
#27112=DIRECTION('ref_axis',(0.,0.568073288796263,-0.822977969666381));
#27113=DIRECTION('center_axis',(0.,-0.822977969666381,-0.568073288796263));
#27114=DIRECTION('ref_axis',(-5.40669131959885E-16,0.568073288796263,-0.822977969666381));
#27115=DIRECTION('',(1.,0.,0.));
#27116=DIRECTION('',(0.,0.568073288796263,-0.822977969666381));
#27117=DIRECTION('',(1.,0.,0.));
#27118=DIRECTION('center_axis',(0.,-0.822977969666381,-0.568073288796263));
#27119=DIRECTION('ref_axis',(-3.28483356716743E-17,-0.568073288796263,0.822977969666381));
#27120=DIRECTION('center_axis',(0.,-0.822977969666381,-0.568073288796263));
#27121=DIRECTION('ref_axis',(0.,0.568073288796263,-0.822977969666381));
#27122=DIRECTION('center_axis',(0.,-0.568073288796263,-0.822977969666381));
#27123=DIRECTION('ref_axis',(-0.707106781186551,0.581933303118232,-0.40168847471878));
#27124=DIRECTION('',(0.,-0.568073288796263,-0.822977969666381));
#27125=DIRECTION('center_axis',(-1.,0.,0.));
#27126=DIRECTION('ref_axis',(0.,0.707106781186545,-0.70710678118655));
#27127=DIRECTION('center_axis',(1.,0.,0.));
#27128=DIRECTION('ref_axis',(0.,0.,-1.));
#27129=DIRECTION('center_axis',(0.,1.,0.));
#27130=DIRECTION('ref_axis',(-0.707106781186545,0.,-0.70710678118655));
#27131=DIRECTION('center_axis',(0.,1.,0.));
#27132=DIRECTION('ref_axis',(0.,0.,-1.));
#27133=DIRECTION('center_axis',(0.,-1.,0.));
#27134=DIRECTION('ref_axis',(-1.,0.,0.));
#27135=DIRECTION('center_axis',(-0.408248290463866,-0.816496580927725,-0.408248290463863));
#27136=DIRECTION('ref_axis',(-0.577350269189628,0.577350269189628,-0.577350269189622));
#27137=DIRECTION('center_axis',(0.,0.,-1.));
#27138=DIRECTION('ref_axis',(-0.707106781186547,0.707106781186547,0.));
#27139=DIRECTION('center_axis',(0.408248290463865,-0.816496580927726,0.408248290463862));
#27140=DIRECTION('ref_axis',(-0.577350269189628,-0.577350269189625,-0.577350269189625));
#27141=DIRECTION('center_axis',(0.,0.,1.));
#27142=DIRECTION('ref_axis',(-0.707106781186547,0.707106781186547,0.));
#27143=DIRECTION('center_axis',(0.,-0.707106781186548,-0.707106781186548));
#27144=DIRECTION('ref_axis',(0.,0.707106781186548,-0.707106781186548));
#27145=DIRECTION('center_axis',(0.,0.,-1.));
#27146=DIRECTION('ref_axis',(-0.707106781186547,0.707106781186547,0.));
#27147=DIRECTION('center_axis',(0.,-0.954719322541023,-0.297508008575921));
#27148=DIRECTION('ref_axis',(-3.44062751178505E-17,0.297508008575921,-0.954719322541023));
#27149=DIRECTION('',(0.,0.,1.));
#27150=DIRECTION('center_axis',(0.,1.,0.));
#27151=DIRECTION('ref_axis',(0.70710678118655,0.,0.707106781186545));
#27152=DIRECTION('',(0.,-1.,0.));
#27153=DIRECTION('center_axis',(0.,0.,1.));
#27154=DIRECTION('ref_axis',(1.,0.,0.));
#27155=DIRECTION('center_axis',(1.,0.,0.));
#27156=DIRECTION('ref_axis',(0.,0.,-1.));
#27157=DIRECTION('center_axis',(0.,-1.,0.));
#27158=DIRECTION('ref_axis',(0.,0.,1.));
#27159=DIRECTION('center_axis',(1.,0.,0.));
#27160=DIRECTION('ref_axis',(0.,-0.822977969666381,0.568073288796262));
#27161=DIRECTION('center_axis',(1.,0.,0.));
#27162=DIRECTION('ref_axis',(0.,-0.822977969666381,0.568073288796262));
#27163=DIRECTION('center_axis',(-1.,0.,0.));
#27164=DIRECTION('ref_axis',(0.,0.,1.));
#27165=DIRECTION('',(0.,-0.568073288796263,-0.822977969666381));
#27166=DIRECTION('',(0.,0.,1.));
#27167=DIRECTION('',(0.,-0.568073288796263,-0.822977969666381));
#27168=DIRECTION('center_axis',(0.,-1.,0.));
#27169=DIRECTION('ref_axis',(0.,0.,1.));
#27170=DIRECTION('',(-1.,0.,0.));
#27171=DIRECTION('center_axis',(0.,0.822977969666381,-0.568073288796263));
#27172=DIRECTION('ref_axis',(0.,-0.568073288796263,-0.822977969666381));
#27173=DIRECTION('center_axis',(0.,0.822977969666381,-0.568073288796263));
#27174=DIRECTION('ref_axis',(0.,-0.568073288796263,-0.822977969666381));
#27175=DIRECTION('center_axis',(0.,-1.85037170770859E-15,-1.));
#27176=DIRECTION('ref_axis',(0.,-1.,1.85037170770859E-15));
#27177=DIRECTION('center_axis',(0.,0.,1.));
#27178=DIRECTION('ref_axis',(-0.707106781186553,-0.707106781186542,0.));
#27179=DIRECTION('',(0.,0.,1.));
#27180=DIRECTION('center_axis',(0.,0.822977969666381,-0.568073288796263));
#27181=DIRECTION('ref_axis',(0.,0.568073288796263,0.822977969666381));
#27182=DIRECTION('center_axis',(0.,0.822977969666381,-0.568073288796263));
#27183=DIRECTION('ref_axis',(0.,0.568073288796263,0.822977969666381));
#27184=DIRECTION('',(1.,0.,0.));
#27185=DIRECTION('',(0.,0.568073288796263,0.822977969666381));
#27186=DIRECTION('',(1.,0.,0.));
#27187=DIRECTION('center_axis',(0.,0.,-1.));
#27188=DIRECTION('ref_axis',(-0.70710678118655,0.707106781186545,0.));
#27189=DIRECTION('',(0.,0.,-1.));
#27190=DIRECTION('center_axis',(0.,-0.822977969666381,-0.568073288796263));
#27191=DIRECTION('ref_axis',(0.,0.568073288796263,-0.822977969666381));
#27192=DIRECTION('',(1.,0.,0.));
#27193=DIRECTION('',(0.,0.568073288796263,-0.822977969666381));
#27194=DIRECTION('',(1.,0.,0.));
#27195=DIRECTION('center_axis',(0.,-1.,0.));
#27196=DIRECTION('ref_axis',(-0.70710678118655,0.,-0.707106781186545));
#27197=DIRECTION('',(0.,-1.,0.));
#27198=DIRECTION('center_axis',(0.,0.,1.));
#27199=DIRECTION('ref_axis',(0.,-1.,0.));
#27200=DIRECTION('',(0.,-1.,0.));
#27201=DIRECTION('center_axis',(0.,-0.568073288796263,0.82297796966638));
#27202=DIRECTION('ref_axis',(-0.707106781186551,-0.581933303118231,-0.40168847471878));
#27203=DIRECTION('',(0.,-0.568073288796263,0.82297796966638));
#27204=DIRECTION('center_axis',(0.,0.82297796966638,0.568073288796263));
#27205=DIRECTION('ref_axis',(0.,-0.568073288796263,0.82297796966638));
#27206=DIRECTION('',(1.,0.,0.));
#27207=DIRECTION('',(0.,-0.568073288796263,0.82297796966638));
#27208=DIRECTION('',(1.,0.,0.));
#27209=DIRECTION('center_axis',(0.,1.,0.));
#27210=DIRECTION('ref_axis',(0.,0.,1.));
#27211=DIRECTION('',(0.,0.,1.));
#27212=DIRECTION('center_axis',(-1.,0.,0.));
#27213=DIRECTION('ref_axis',(0.,0.,1.));
#27214=DIRECTION('center_axis',(0.,-1.,0.));
#27215=DIRECTION('ref_axis',(0.,0.,-1.));
#27216=DIRECTION('center_axis',(-1.,0.,0.));
#27217=DIRECTION('ref_axis',(0.,0.,-1.));
#27218=DIRECTION('center_axis',(-1.,0.,0.));
#27219=DIRECTION('ref_axis',(0.,0.,-1.));
#27220=DIRECTION('center_axis',(-1.,0.,0.));
#27221=DIRECTION('ref_axis',(0.,0.,-1.));
#27222=DIRECTION('',(-1.,0.,0.));
#27223=DIRECTION('center_axis',(1.,0.,0.));
#27224=DIRECTION('ref_axis',(0.,-0.822977969666381,0.568073288796262));
#27225=DIRECTION('',(-1.,0.,0.));
#27226=DIRECTION('center_axis',(1.,0.,0.));
#27227=DIRECTION('ref_axis',(0.,-0.822977969666381,0.568073288796262));
#27228=DIRECTION('center_axis',(0.,-1.,0.));
#27229=DIRECTION('ref_axis',(0.,0.,-1.));
#27230=DIRECTION('',(0.,0.,-1.));
#27231=DIRECTION('center_axis',(-1.,0.,0.));
#27232=DIRECTION('ref_axis',(0.,-0.822977969666381,0.568073288796262));
#27233=DIRECTION('center_axis',(-1.,0.,0.));
#27234=DIRECTION('ref_axis',(0.,-0.822977969666381,0.568073288796262));
#27235=DIRECTION('center_axis',(1.,0.,0.));
#27236=DIRECTION('ref_axis',(0.,0.,-1.));
#27237=DIRECTION('',(0.,0.568073288796263,0.822977969666381));
#27238=DIRECTION('center_axis',(0.,0.822977969666381,-0.568073288796263));
#27239=DIRECTION('ref_axis',(0.,0.568073288796263,0.822977969666381));
#27240=DIRECTION('center_axis',(1.,0.,0.));
#27241=DIRECTION('ref_axis',(0.,0.,-1.));
#27242=DIRECTION('',(0.,-0.568073288796263,-0.822977969666381));
#27243=DIRECTION('center_axis',(0.,-0.822977969666381,0.568073288796263));
#27244=DIRECTION('ref_axis',(0.,-0.568073288796263,-0.822977969666381));
#27245=DIRECTION('center_axis',(0.,1.,0.));
#27246=DIRECTION('ref_axis',(0.,0.,1.));
#27247=DIRECTION('',(0.,0.,1.));
#27248=DIRECTION('',(1.,0.,0.));
#27249=DIRECTION('center_axis',(0.,-0.822977969666381,0.568073288796263));
#27250=DIRECTION('ref_axis',(0.,-0.568073288796263,-0.822977969666381));
#27251=DIRECTION('',(0.,-0.568073288796263,-0.822977969666381));
#27252=DIRECTION('center_axis',(1.,0.,0.));
#27253=DIRECTION('ref_axis',(0.,0.,-1.));
#27254=DIRECTION('center_axis',(0.,0.82297796966638,-0.568073288796263));
#27255=DIRECTION('ref_axis',(0.,0.568073288796263,0.82297796966638));
#27256=DIRECTION('',(0.,0.568073288796263,0.82297796966638));
#27257=DIRECTION('center_axis',(1.,0.,0.));
#27258=DIRECTION('ref_axis',(0.,0.,-1.));
#27259=DIRECTION('center_axis',(0.,0.,-1.));
#27260=DIRECTION('ref_axis',(0.,1.,0.));
#27261=DIRECTION('',(1.,0.,0.));
#27262=DIRECTION('',(0.,1.,0.));
#27263=DIRECTION('center_axis',(0.,-0.822977969666381,0.568073288796263));
#27264=DIRECTION('ref_axis',(0.,-0.568073288796263,-0.822977969666381));
#27265=DIRECTION('',(0.,-0.568073288796263,-0.822977969666381));
#27266=DIRECTION('center_axis',(1.,0.,0.));
#27267=DIRECTION('ref_axis',(0.,0.,-1.));
#27268=DIRECTION('center_axis',(-1.,0.,0.));
#27269=DIRECTION('ref_axis',(0.,0.,1.));
#27270=DIRECTION('',(0.,0.,-1.));
#27271=DIRECTION('center_axis',(0.,1.,0.));
#27272=DIRECTION('ref_axis',(0.,0.,-1.));
#27273=DIRECTION('center_axis',(0.,-0.822977969666381,0.568073288796263));
#27274=DIRECTION('ref_axis',(0.,0.568073288796263,0.822977969666381));
#27275=DIRECTION('',(0.,0.568073288796263,0.822977969666381));
#27276=DIRECTION('',(-1.,0.,0.));
#27277=DIRECTION('center_axis',(0.,1.,0.));
#27278=DIRECTION('ref_axis',(0.,0.,-1.));
#27279=DIRECTION('',(0.,0.,-1.));
#27280=DIRECTION('center_axis',(-1.,0.,0.));
#27281=DIRECTION('ref_axis',(0.,0.,1.));
#27282=DIRECTION('center_axis',(0.,0.82297796966638,-0.568073288796263));
#27283=DIRECTION('ref_axis',(0.,-0.568073288796263,-0.82297796966638));
#27284=DIRECTION('',(-1.,0.,0.));
#27285=DIRECTION('',(0.,-0.568073288796263,-0.82297796966638));
#27286=DIRECTION('center_axis',(0.,0.,1.));
#27287=DIRECTION('ref_axis',(0.,1.,0.));
#27288=DIRECTION('',(0.,1.,0.));
#27289=DIRECTION('center_axis',(0.,0.82297796966638,-0.568073288796263));
#27290=DIRECTION('ref_axis',(0.,-0.568073288796263,-0.82297796966638));
#27291=DIRECTION('',(0.,-0.568073288796263,-0.82297796966638));
#27292=DIRECTION('center_axis',(-1.,0.,0.));
#27293=DIRECTION('ref_axis',(0.,0.,1.));
#27294=DIRECTION('center_axis',(-1.,0.,0.));
#27295=DIRECTION('ref_axis',(0.,0.,1.));
#27296=DIRECTION('center_axis',(0.,1.,0.));
#27297=DIRECTION('ref_axis',(1.,0.,0.));
#27298=DIRECTION('center_axis',(0.,1.,0.));
#27299=DIRECTION('ref_axis',(1.,0.,0.));
#27300=DIRECTION('center_axis',(0.,1.,0.));
#27301=DIRECTION('ref_axis',(1.,0.,0.));
#27302=DIRECTION('center_axis',(0.,1.,0.));
#27303=DIRECTION('ref_axis',(1.,0.,0.));
#27304=DIRECTION('center_axis',(0.,0.,1.));
#27305=DIRECTION('ref_axis',(1.,0.,0.));
#27306=DIRECTION('',(0.,0.,-1.));
#27307=DIRECTION('',(0.,0.,1.));
#27308=DIRECTION('center_axis',(0.,0.,1.));
#27309=DIRECTION('ref_axis',(1.,0.,0.));
#27310=DIRECTION('',(0.,0.,-1.));
#27311=DIRECTION('',(0.,0.,1.));
#27312=DIRECTION('center_axis',(0.,-1.,0.));
#27313=DIRECTION('ref_axis',(0.,0.,-1.));
#27314=DIRECTION('center_axis',(0.,-1.,0.));
#27315=DIRECTION('ref_axis',(0.,0.,-1.));
#27316=DIRECTION('center_axis',(0.,-1.,0.));
#27317=DIRECTION('ref_axis',(0.,0.,-1.));
#27318=DIRECTION('center_axis',(0.,-1.,0.));
#27319=DIRECTION('ref_axis',(0.,0.,-1.));
#27320=DIRECTION('center_axis',(0.,1.,0.));
#27321=DIRECTION('ref_axis',(0.,0.,1.));
#27322=DIRECTION('center_axis',(-1.,0.,0.));
#27323=DIRECTION('ref_axis',(0.,0.,1.));
#27324=DIRECTION('center_axis',(1.,0.,0.));
#27325=DIRECTION('ref_axis',(0.,0.,-1.));
#27326=DIRECTION('center_axis',(0.,1.,0.));
#27327=DIRECTION('ref_axis',(-1.,0.,0.));
#27328=DIRECTION('center_axis',(0.,0.,1.));
#27329=DIRECTION('ref_axis',(1.,0.,0.));
#27330=DIRECTION('center_axis',(1.,0.,0.));
#27331=DIRECTION('ref_axis',(0.,0.,-1.));
#27332=DIRECTION('axis',(0.,0.,1.));
#27333=DIRECTION('refdir',(1.,0.,0.));
#27334=DIRECTION('center_axis',(1.,0.,0.));
#27335=DIRECTION('ref_axis',(0.,0.,-1.));
#27336=DIRECTION('',(0.,-0.99999354730451,0.00359240161224881));
#27337=DIRECTION('center_axis',(0.027955631445268,-0.00359099757581823,
-0.999602714785683));
#27338=DIRECTION('ref_axis',(0.4350805171232,-0.900259809769442,0.0154019003274739));
#27339=DIRECTION('center_axis',(1.,0.,0.));
#27340=DIRECTION('ref_axis',(0.,0.,-1.));
#27341=DIRECTION('',(0.,0.999993547304682,0.00359240156428263));
#27342=DIRECTION('center_axis',(0.0279556313622445,-0.00359099752787914,
0.999602714788177));
#27343=DIRECTION('ref_axis',(-0.991456520419747,0.127356018817566,0.0281853257583967));
#27344=DIRECTION('axis',(0.,0.,1.));
#27345=DIRECTION('refdir',(1.,0.,0.));
#27346=DIRECTION('center_axis',(1.,0.,0.));
#27347=DIRECTION('ref_axis',(0.,0.,-1.));
#27348=DIRECTION('center_axis',(-1.,0.,0.));
#27349=DIRECTION('ref_axis',(0.,-1.,1.83697019872103E-16));
#27350=DIRECTION('center_axis',(0.,-1.,-1.22464679914735E-16));
#27351=DIRECTION('ref_axis',(0.,-1.22464679914735E-16,1.));
#27352=DIRECTION('center_axis',(1.,0.,0.));
#27353=DIRECTION('ref_axis',(0.,-1.,1.83697019872103E-16));
#27354=DIRECTION('center_axis',(1.,0.,0.));
#27355=DIRECTION('ref_axis',(0.,-1.,1.83697019872103E-16));
#27356=DIRECTION('center_axis',(1.,0.,0.));
#27357=DIRECTION('ref_axis',(0.,1.,0.));
#27358=DIRECTION('',(1.,0.,0.));
#27359=DIRECTION('center_axis',(-1.,0.,0.));
#27360=DIRECTION('ref_axis',(0.,-1.,1.83697019872103E-16));
#27361=DIRECTION('center_axis',(-1.,0.,0.));
#27362=DIRECTION('ref_axis',(0.,-1.,1.83697019872103E-16));
#27363=DIRECTION('center_axis',(-1.,0.,0.));
#27364=DIRECTION('ref_axis',(0.,0.,1.));
#27365=DIRECTION('center_axis',(1.,0.,0.));
#27366=DIRECTION('ref_axis',(0.,-1.,1.83697019872103E-16));
#27367=DIRECTION('center_axis',(1.,0.,0.));
#27368=DIRECTION('ref_axis',(0.,0.,-1.));
#27369=DIRECTION('center_axis',(0.,-1.,-1.22464679914735E-16));
#27370=DIRECTION('ref_axis',(0.,-1.22464679914735E-16,1.));
#27371=DIRECTION('center_axis',(1.,0.,0.));
#27372=DIRECTION('ref_axis',(0.,-1.,1.83697019872103E-16));
#27373=DIRECTION('center_axis',(1.,0.,0.));
#27374=DIRECTION('ref_axis',(0.,0.,-1.));
#27375=DIRECTION('center_axis',(1.,0.,0.));
#27376=DIRECTION('ref_axis',(0.,0.,-1.));
#27377=DIRECTION('center_axis',(1.,0.,0.));
#27378=DIRECTION('ref_axis',(0.,0.,-1.));
#27379=DIRECTION('center_axis',(-1.,0.,0.));
#27380=DIRECTION('ref_axis',(0.,-1.,1.83697019872103E-16));
#27381=DIRECTION('center_axis',(0.,-1.,-1.22464679914735E-16));
#27382=DIRECTION('ref_axis',(0.,-1.22464679914735E-16,1.));
#27383=DIRECTION('center_axis',(1.,0.,0.));
#27384=DIRECTION('ref_axis',(0.,-1.,1.83697019872103E-16));
#27385=DIRECTION('center_axis',(-1.,0.,0.));
#27386=DIRECTION('ref_axis',(0.,-1.,1.83697019872103E-16));
#27387=DIRECTION('center_axis',(1.,0.,0.));
#27388=DIRECTION('ref_axis',(0.,0.,-1.));
#27389=DIRECTION('center_axis',(-1.,0.,0.));
#27390=DIRECTION('ref_axis',(0.,-1.,1.83697019872103E-16));
#27391=DIRECTION('center_axis',(1.,0.,0.));
#27392=DIRECTION('ref_axis',(0.,1.,0.));
#27393=DIRECTION('',(1.,0.,0.));
#27394=DIRECTION('center_axis',(1.,0.,0.));
#27395=DIRECTION('ref_axis',(0.,0.,-1.));
#27396=DIRECTION('center_axis',(0.,-1.,-1.22464679914735E-16));
#27397=DIRECTION('ref_axis',(0.,-1.22464679914735E-16,1.));
#27398=DIRECTION('center_axis',(1.,0.,0.));
#27399=DIRECTION('ref_axis',(0.,-1.,1.83697019872103E-16));
#27400=DIRECTION('center_axis',(1.,0.,0.));
#27401=DIRECTION('ref_axis',(0.,-1.,1.83697019872103E-16));
#27402=DIRECTION('center_axis',(1.,0.,0.));
#27403=DIRECTION('ref_axis',(0.,1.,0.));
#27404=DIRECTION('',(-1.,0.,0.));
#27405=DIRECTION('center_axis',(1.,0.,0.));
#27406=DIRECTION('ref_axis',(0.,0.,-1.));
#27407=DIRECTION('center_axis',(1.,0.,0.));
#27408=DIRECTION('ref_axis',(0.,1.,0.));
#27409=DIRECTION('',(-1.,0.,0.));
#27410=DIRECTION('center_axis',(-1.,0.,0.));
#27411=DIRECTION('ref_axis',(0.,1.,0.));
#27412=DIRECTION('',(1.,0.,0.));
#27413=DIRECTION('center_axis',(1.,0.,0.));
#27414=DIRECTION('ref_axis',(0.,0.,-1.));
#27415=DIRECTION('center_axis',(-1.,0.,0.));
#27416=DIRECTION('ref_axis',(0.,-1.,1.83697019872103E-16));
#27417=DIRECTION('center_axis',(0.,-1.,-1.22464679914735E-16));
#27418=DIRECTION('ref_axis',(0.,-1.22464679914735E-16,1.));
#27419=DIRECTION('center_axis',(1.,0.,0.));
#27420=DIRECTION('ref_axis',(0.,-1.,1.83697019872103E-16));
#27421=DIRECTION('center_axis',(1.,0.,0.));
#27422=DIRECTION('ref_axis',(0.,-1.,1.83697019872103E-16));
#27423=DIRECTION('center_axis',(1.,0.,0.));
#27424=DIRECTION('ref_axis',(0.,1.,0.));
#27425=DIRECTION('',(-1.,0.,0.));
#27426=DIRECTION('center_axis',(-1.,0.,0.));
#27427=DIRECTION('ref_axis',(0.,-1.,1.83697019872103E-16));
#27428=DIRECTION('center_axis',(-1.,0.,0.));
#27429=DIRECTION('ref_axis',(0.,-1.,1.83697019872103E-16));
#27430=DIRECTION('center_axis',(1.,0.,0.));
#27431=DIRECTION('ref_axis',(0.,0.,-1.));
#27432=DIRECTION('center_axis',(1.,0.,0.));
#27433=DIRECTION('ref_axis',(0.,0.,-1.));
#27434=DIRECTION('center_axis',(0.,-1.,-1.22464679914735E-16));
#27435=DIRECTION('ref_axis',(0.,-1.22464679914735E-16,1.));
#27436=DIRECTION('center_axis',(-1.,0.,0.));
#27437=DIRECTION('ref_axis',(0.,-0.70710678118655,0.707106781186545));
#27438=DIRECTION('',(1.,0.,0.));
#27439=DIRECTION('center_axis',(-0.707106781186548,-0.707106781186548,0.));
#27440=DIRECTION('ref_axis',(0.707106781186547,-0.707106781186547,0.));
#27441=DIRECTION('',(-1.,0.,0.));
#27442=DIRECTION('center_axis',(0.707106781186548,-0.707106781186548,0.));
#27443=DIRECTION('ref_axis',(0.707106781186547,0.707106781186547,0.));
#27444=DIRECTION('center_axis',(0.,1.,0.));
#27445=DIRECTION('ref_axis',(0.707106781186545,0.,0.70710678118655));
#27446=DIRECTION('',(0.,-1.,0.));
#27447=DIRECTION('',(0.,1.,0.));
#27448=DIRECTION('center_axis',(0.707106781186548,-0.707106781186548,0.));
#27449=DIRECTION('ref_axis',(-0.707106781186547,-0.707106781186547,0.));
#27450=DIRECTION('center_axis',(0.,1.,0.));
#27451=DIRECTION('ref_axis',(-0.70710678118655,0.,0.707106781186545));
#27452=DIRECTION('',(0.,-1.,0.));
#27453=DIRECTION('',(0.,1.,0.));
#27454=DIRECTION('center_axis',(-0.707106781186548,-0.707106781186548,0.));
#27455=DIRECTION('ref_axis',(0.707106781186547,-0.707106781186547,0.));
#27456=DIRECTION('center_axis',(1.,0.,0.));
#27457=DIRECTION('ref_axis',(0.,0.70710678118655,0.707106781186545));
#27458=DIRECTION('',(-1.,0.,0.));
#27459=DIRECTION('',(1.,0.,0.));
#27460=DIRECTION('center_axis',(1.,0.,0.));
#27461=DIRECTION('ref_axis',(0.,0.,-1.));
#27462=DIRECTION('',(0.,0.,1.));
#27463=DIRECTION('',(0.,0.,-1.));
#27464=DIRECTION('center_axis',(0.,1.,0.));
#27465=DIRECTION('ref_axis',(1.,0.,0.));
#27466=DIRECTION('',(0.,0.,-1.));
#27467=DIRECTION('center_axis',(0.,0.,1.));
#27468=DIRECTION('ref_axis',(1.,0.,0.));
#27469=DIRECTION('',(-1.,0.,0.));
#27470=DIRECTION('',(0.,1.,0.));
#27471=DIRECTION('',(1.,0.,0.));
#27472=DIRECTION('',(0.,-1.,0.));
#27473=DIRECTION('center_axis',(0.,-1.,0.));
#27474=DIRECTION('ref_axis',(-1.,0.,0.));
#27475=DIRECTION('',(0.,0.,-1.));
#27476=DIRECTION('',(-1.,0.,0.));
#27477=DIRECTION('',(0.,0.,-1.));
#27478=DIRECTION('center_axis',(1.,0.,0.));
#27479=DIRECTION('ref_axis',(0.,-1.,0.));
#27480=DIRECTION('',(0.,0.,-1.));
#27481=DIRECTION('',(0.,-1.,0.));
#27482=DIRECTION('center_axis',(0.,1.,0.));
#27483=DIRECTION('ref_axis',(1.,0.,0.));
#27484=DIRECTION('',(0.,0.,-1.));
#27485=DIRECTION('',(1.,0.,0.));
#27486=DIRECTION('center_axis',(-1.,0.,0.));
#27487=DIRECTION('ref_axis',(0.,1.,0.));
#27488=DIRECTION('',(0.,1.,0.));
#27489=DIRECTION('center_axis',(0.,0.,-1.));
#27490=DIRECTION('ref_axis',(-1.,0.,0.));
#27491=DIRECTION('center_axis',(-1.,0.,0.));
#27492=DIRECTION('ref_axis',(0.,0.,1.));
#27493=DIRECTION('',(0.,0.,1.));
#27494=DIRECTION('center_axis',(0.,1.,0.));
#27495=DIRECTION('ref_axis',(0.,0.,1.));
#27496=DIRECTION('axis',(0.,0.,1.));
#27497=DIRECTION('refdir',(1.,0.,0.));
#27498=DIRECTION('center_axis',(0.,-1.,0.));
#27499=DIRECTION('ref_axis',(0.707106781186558,0.,0.707106781186537));
#27500=DIRECTION('center_axis',(0.,-1.,0.));
#27501=DIRECTION('ref_axis',(1.,0.,0.));
#27502=DIRECTION('',(0.,-1.,0.));
#27503=DIRECTION('center_axis',(0.,1.,0.));
#27504=DIRECTION('ref_axis',(0.,0.,1.));
#27505=DIRECTION('',(0.,1.,0.));
#27506=DIRECTION('center_axis',(1.,0.,0.));
#27507=DIRECTION('ref_axis',(0.,-0.707106781186534,0.707106781186561));
#27508=DIRECTION('center_axis',(1.,0.,0.));
#27509=DIRECTION('ref_axis',(0.,0.,1.));
#27510=DIRECTION('',(1.,0.,0.));
#27511=DIRECTION('center_axis',(-1.,0.,0.));
#27512=DIRECTION('ref_axis',(0.,-1.,0.));
#27513=DIRECTION('',(-1.,0.,0.));
#27514=DIRECTION('center_axis',(0.,1.,0.));
#27515=DIRECTION('ref_axis',(-0.707106781186558,0.,0.707106781186537));
#27516=DIRECTION('center_axis',(0.,1.,0.));
#27517=DIRECTION('ref_axis',(-1.,0.,0.));
#27518=DIRECTION('',(0.,1.,0.));
#27519=DIRECTION('center_axis',(0.,-1.,0.));
#27520=DIRECTION('ref_axis',(0.,0.,1.));
#27521=DIRECTION('',(0.,-1.,0.));
#27522=DIRECTION('center_axis',(-1.,0.,0.));
#27523=DIRECTION('ref_axis',(0.,0.707106781186555,0.70710678118654));
#27524=DIRECTION('center_axis',(-1.,0.,0.));
#27525=DIRECTION('ref_axis',(0.,0.,1.));
#27526=DIRECTION('',(-1.,0.,0.));
#27527=DIRECTION('center_axis',(1.,0.,0.));
#27528=DIRECTION('ref_axis',(0.,1.,0.));
#27529=DIRECTION('',(1.,0.,0.));
#27530=DIRECTION('center_axis',(-0.40824829046386,-0.816496580927729,0.40824829046386));
#27531=DIRECTION('ref_axis',(-0.57735026918963,0.577350269189623,0.577350269189624));
#27532=DIRECTION('center_axis',(0.,0.,1.));
#27533=DIRECTION('ref_axis',(-0.707106781186551,0.707106781186544,0.));
#27534=DIRECTION('center_axis',(-0.408248290463851,-0.408248290463851,-0.816496580927738));
#27535=DIRECTION('ref_axis',(-0.577350269189626,-0.577350269189631,0.57735026918962));
#27536=DIRECTION('center_axis',(0.,0.,1.));
#27537=DIRECTION('ref_axis',(-0.70710678118655,-0.707106781186544,0.));
#27538=DIRECTION('center_axis',(-0.408248290463842,-0.816496580927738,-0.40824829046386));
#27539=DIRECTION('ref_axis',(0.577350269189618,-0.577350269189612,0.577350269189648));
#27540=DIRECTION('center_axis',(0.,0.,1.));
#27541=DIRECTION('ref_axis',(0.70710678118655,-0.707106781186544,0.));
#27542=DIRECTION('center_axis',(0.40824829046386,-0.816496580927729,0.40824829046386));
#27543=DIRECTION('ref_axis',(0.57735026918963,0.577350269189623,0.577350269189624));
#27544=DIRECTION('center_axis',(0.,0.,1.));
#27545=DIRECTION('ref_axis',(0.707106781186551,0.707106781186544,0.));
#27546=DIRECTION('center_axis',(0.,0.,1.));
#27547=DIRECTION('ref_axis',(-0.70710678118655,-0.707106781186545,0.));
#27548=DIRECTION('',(0.,0.,-1.));
#27549=DIRECTION('center_axis',(0.,0.,1.));
#27550=DIRECTION('ref_axis',(-1.,0.,0.));
#27551=DIRECTION('',(0.,0.,1.));
#27552=DIRECTION('center_axis',(-1.,0.,0.));
#27553=DIRECTION('ref_axis',(0.,0.,1.));
#27554=DIRECTION('',(0.,0.,1.));
#27555=DIRECTION('',(0.,1.,0.));
#27556=DIRECTION('center_axis',(0.,0.,-1.));
#27557=DIRECTION('ref_axis',(-0.707106781186551,0.707106781186544,0.));
#27558=DIRECTION('',(0.,0.,-1.));
#27559=DIRECTION('center_axis',(0.,0.,1.));
#27560=DIRECTION('ref_axis',(1.48029736616688E-14,1.,0.));
#27561=DIRECTION('center_axis',(0.,1.,0.));
#27562=DIRECTION('ref_axis',(0.,0.,1.));
#27563=DIRECTION('',(0.,0.,1.));
#27564=DIRECTION('',(1.,0.,0.));
#27565=DIRECTION('center_axis',(0.,1.,0.));
#27566=DIRECTION('ref_axis',(1.,0.,0.));
#27567=DIRECTION('center_axis',(0.,1.,0.));
#27568=DIRECTION('ref_axis',(1.,0.,0.));
#27569=DIRECTION('center_axis',(0.,0.,1.));
#27570=DIRECTION('ref_axis',(0.,-1.,0.));
#27571=DIRECTION('center_axis',(0.,0.,1.));
#27572=DIRECTION('ref_axis',(0.707106781186551,0.707106781186544,0.));
#27573=DIRECTION('',(0.,0.,-1.));
#27574=DIRECTION('center_axis',(0.,0.,1.));
#27575=DIRECTION('ref_axis',(1.,0.,0.));
#27576=DIRECTION('center_axis',(0.,1.,0.));
#27577=DIRECTION('ref_axis',(0.99894638116538,0.,-0.0458925653738368));
#27578=DIRECTION('center_axis',(0.,-1.,0.));
#27579=DIRECTION('ref_axis',(0.995787744886652,0.,-0.091688424206963));
#27580=DIRECTION('',(0.,-1.,0.));
#27581=DIRECTION('center_axis',(0.,1.,0.));
#27582=DIRECTION('ref_axis',(1.,0.,0.));
#27583=DIRECTION('',(0.,1.,0.));
#27584=DIRECTION('center_axis',(0.,0.,1.));
#27585=DIRECTION('ref_axis',(1.,0.,0.));
#27586=DIRECTION('center_axis',(0.0916884242070712,0.,0.995787744886642));
#27587=DIRECTION('ref_axis',(2.70308839529112E-15,1.,-2.48890304916212E-16));
#27588=DIRECTION('center_axis',(0.,0.,-1.));
#27589=DIRECTION('ref_axis',(0.70710678118655,-0.707106781186545,0.));
#27590=DIRECTION('',(0.,0.,-1.));
#27591=DIRECTION('center_axis',(0.,0.,1.));
#27592=DIRECTION('ref_axis',(-1.48029736616688E-14,-1.,0.));
#27593=DIRECTION('',(0.,0.,1.));
#27594=DIRECTION('center_axis',(0.,0.,1.));
#27595=DIRECTION('ref_axis',(1.,0.,0.));
#27596=DIRECTION('center_axis',(0.0916884242070274,0.,0.995787744886646));
#27597=DIRECTION('ref_axis',(1.35154419764492E-14,-1.,-1.24445152457987E-15));
#27598=DIRECTION('center_axis',(-0.342464185150441,0.,-0.939530883946475));
#27599=DIRECTION('ref_axis',(0.,1.,0.));
#27600=DIRECTION('center_axis',(0.,1.,0.));
#27601=DIRECTION('ref_axis',(-0.991776726791891,0.,0.127980171096785));
#27602=DIRECTION('',(0.,1.,0.));
#27603=DIRECTION('center_axis',(-0.341922938227805,0.,-0.939727994854716));
#27604=DIRECTION('ref_axis',(0.939727994854716,0.,-0.341922938227805));
#27605=DIRECTION('center_axis',(0.,-1.,0.));
#27606=DIRECTION('ref_axis',(0.,0.,-1.));
#27607=DIRECTION('',(-1.,0.,0.));
#27608=DIRECTION('center_axis',(0.,-1.,0.));
#27609=DIRECTION('ref_axis',(1.,0.,0.));
#27610=DIRECTION('center_axis',(0.,-1.,0.));
#27611=DIRECTION('ref_axis',(1.,0.,0.));
#27612=DIRECTION('center_axis',(0.,1.,0.));
#27613=DIRECTION('ref_axis',(-0.9989463811658,0.,-0.0458925653646838));
#27614=DIRECTION('center_axis',(0.,-1.,4.03621661973593E-14));
#27615=DIRECTION('ref_axis',(-1.,0.,0.));
#27616=DIRECTION('',(0.,-1.,0.));
#27617=DIRECTION('center_axis',(0.,1.,7.06337908453787E-14));
#27618=DIRECTION('ref_axis',(-0.995787744888473,6.47630097698012E-15,-0.0916884241871869));
#27619=DIRECTION('center_axis',(0.,0.,1.));
#27620=DIRECTION('ref_axis',(1.,0.,0.));
#27621=DIRECTION('center_axis',(-0.0916884241872355,0.,0.995787744888469));
#27622=DIRECTION('ref_axis',(-2.70308839471129E-15,1.,-2.48890304808522E-16));
#27623=DIRECTION('center_axis',(0.,0.,1.));
#27624=DIRECTION('ref_axis',(1.,0.,0.));
#27625=DIRECTION('center_axis',(-0.0916884241872959,0.,0.995787744888463));
#27626=DIRECTION('ref_axis',(-1.54000185901395E-15,-1.,-1.4179763149657E-16));
#27627=DIRECTION('center_axis',(0.341922938227109,6.95538437848544E-15,
-0.939727994854969));
#27628=DIRECTION('ref_axis',(-9.06088119400516E-31,-1.,-7.40148683083437E-15));
#27629=DIRECTION('',(0.,1.,0.));
#27630=DIRECTION('center_axis',(0.,1.,0.));
#27631=DIRECTION('ref_axis',(0.99622596754828,0.,0.0867975897274464));
#27632=DIRECTION('center_axis',(-0.342464185149375,0.,0.939530883946863));
#27633=DIRECTION('ref_axis',(0.,1.,0.));
#27634=DIRECTION('center_axis',(-0.290611853669958,-0.507124729938608,0.811399567901786));
#27635=DIRECTION('ref_axis',(2.95685193295205E-17,0.847998304005092,0.529998940003174));
#27636=DIRECTION('center_axis',(-0.169633066553524,-0.522317820164791,0.835708512263665));
#27637=DIRECTION('ref_axis',(-4.86759141432297E-17,0.847998304005088,0.52999894000318));
#27638=DIRECTION('center_axis',(-0.157204875383854,3.6547284145087E-15,
0.987566011543303));
#27639=DIRECTION('ref_axis',(7.52525386954664E-31,1.,-3.7007434154172E-15));
#27640=DIRECTION('center_axis',(0.,0.,-1.));
#27641=DIRECTION('ref_axis',(-0.707106781186547,0.707106781186547,0.));
#27642=DIRECTION('',(0.,0.,-1.));
#27643=DIRECTION('center_axis',(0.,0.,1.));
#27644=DIRECTION('ref_axis',(0.,1.,0.));
#27645=DIRECTION('',(0.,0.,1.));
#27646=DIRECTION('center_axis',(0.,-1.,0.));
#27647=DIRECTION('ref_axis',(0.,0.,-1.));
#27648=DIRECTION('center_axis',(7.40148683083437E-15,0.,-1.));
#27649=DIRECTION('ref_axis',(0.,1.,0.));
#27650=DIRECTION('center_axis',(0.,1.,0.));
#27651=DIRECTION('ref_axis',(1.5559876576226E-16,0.,-1.));
#27652=DIRECTION('center_axis',(0.,-1.,0.));
#27653=DIRECTION('ref_axis',(1.5559876576226E-16,0.,-1.));
#27654=DIRECTION('center_axis',(0.,0.,1.));
#27655=DIRECTION('ref_axis',(0.707106781186547,0.707106781186547,0.));
#27656=DIRECTION('',(0.,0.,-1.));
#27657=DIRECTION('',(0.,0.,1.));
#27658=DIRECTION('center_axis',(0.15720487538553,0.,0.987566011543036));
#27659=DIRECTION('ref_axis',(0.987566011543036,0.,-0.15720487538553));
#27660=DIRECTION('center_axis',(-0.169633066555186,0.522317820164643,-0.835708512263421));
#27661=DIRECTION('ref_axis',(1.0172704914008E-16,0.847998304005086,0.529998940003184));
#27662=DIRECTION('center_axis',(-0.290611853669808,0.507124729938623,-0.81139956790183));
#27663=DIRECTION('ref_axis',(1.15214297628471E-16,0.847998304005098,0.529998940003164));
#27664=DIRECTION('center_axis',(-1.,0.,0.));
#27665=DIRECTION('ref_axis',(0.,0.,1.));
#27666=DIRECTION('',(0.,1.,0.));
#27667=DIRECTION('',(0.,0.,1.));
#27668=DIRECTION('center_axis',(1.,0.,0.));
#27669=DIRECTION('ref_axis',(0.,0.961248746164355,0.275682513042551));
#27670=DIRECTION('',(0.,-0.52999894000318,0.847998304005088));
#27671=DIRECTION('center_axis',(1.,0.,0.));
#27672=DIRECTION('ref_axis',(0.,-0.63620934106487,0.771516477038439));
#27673=DIRECTION('center_axis',(0.,1.,0.));
#27674=DIRECTION('ref_axis',(1.,0.,3.16411030729924E-16));
#27675=DIRECTION('',(0.,1.,0.));
#27676=DIRECTION('center_axis',(0.,1.,0.));
#27677=DIRECTION('ref_axis',(1.,0.,3.16411030729924E-16));
#27678=DIRECTION('center_axis',(1.,0.,0.));
#27679=DIRECTION('ref_axis',(0.,0.,-1.));
#27680=DIRECTION('center_axis',(-1.,0.,0.));
#27681=DIRECTION('ref_axis',(0.,0.6339690029848,-0.773358457155838));
#27682=DIRECTION('',(0.,0.52999894000318,-0.847998304005088));
#27683=DIRECTION('center_axis',(-1.,0.,0.));
#27684=DIRECTION('ref_axis',(0.,0.961248746164355,0.275682513042551));
#27685=DIRECTION('',(0.,0.,-1.));
#27686=DIRECTION('center_axis',(1.,0.,0.));
#27687=DIRECTION('ref_axis',(0.,0.,-1.));
#27688=DIRECTION('center_axis',(0.169039506365408,-0.52237187163154,0.835794994610462));
#27689=DIRECTION('ref_axis',(6.12619120378935E-17,-0.847998304005087,-0.529998940003181));
#27690=DIRECTION('center_axis',(-0.290495237999518,0.507143497604778,-0.81142959616765));
#27691=DIRECTION('ref_axis',(0.941484765039641,1.58293525692317E-16,-0.337055540227797));
#27692=DIRECTION('center_axis',(0.127825287380035,0.,0.991796700895003));
#27693=DIRECTION('ref_axis',(0.,-1.,0.));
#27694=DIRECTION('center_axis',(1.,0.,0.));
#27695=DIRECTION('ref_axis',(0.,-0.961248746164355,-0.275682513042551));
#27696=DIRECTION('',(1.,0.,0.));
#27697=DIRECTION('center_axis',(0.290495237999669,0.507143497604755,-0.811429596167611));
#27698=DIRECTION('ref_axis',(-9.8030109697363E-17,-0.847998304005089,-0.529998940003178));
#27699=DIRECTION('center_axis',(-0.169039506363714,-0.522371871631687,0.835794994610712));
#27700=DIRECTION('ref_axis',(-0.980154284762346,-2.33134209272865E-16,-0.198236167391356));
#27701=DIRECTION('center_axis',(-0.127825287380379,-3.67038511026951E-15,
0.991796700894958));
#27702=DIRECTION('ref_axis',(-0.991796700894958,2.7885015020519E-32,-0.127825287380379));
#27703=DIRECTION('center_axis',(1.,0.,0.));
#27704=DIRECTION('ref_axis',(0.,0.961248746164355,0.275682513042551));
#27705=DIRECTION('',(-1.,0.,0.));
#27706=DIRECTION('',(1.,0.,0.));
#27707=DIRECTION('center_axis',(0.,-1.,0.));
#27708=DIRECTION('ref_axis',(0.,0.,-1.));
#27709=DIRECTION('center_axis',(0.,-1.,0.));
#27710=DIRECTION('ref_axis',(1.,0.,0.));
#27711=DIRECTION('center_axis',(0.,-1.,0.));
#27712=DIRECTION('ref_axis',(1.,0.,0.));
#27713=DIRECTION('center_axis',(0.,1.,0.));
#27714=DIRECTION('ref_axis',(0.,0.,1.));
#27715=DIRECTION('center_axis',(-1.,0.,0.));
#27716=DIRECTION('ref_axis',(0.,0.,-1.));
#27717=DIRECTION('center_axis',(0.,1.,0.));
#27718=DIRECTION('ref_axis',(1.,0.,0.));
#27719=DIRECTION('center_axis',(0.,1.,0.));
#27720=DIRECTION('ref_axis',(1.,0.,0.));
#27721=DIRECTION('center_axis',(0.,1.,0.));
#27722=DIRECTION('ref_axis',(1.,0.,0.));
#27723=DIRECTION('',(0.,1.,0.));
#27724=DIRECTION('center_axis',(0.,-1.,0.));
#27725=DIRECTION('ref_axis',(1.,0.,0.));
#27726=DIRECTION('center_axis',(0.,-1.,0.));
#27727=DIRECTION('ref_axis',(1.,0.,0.));
#27728=DIRECTION('center_axis',(0.,-1.,0.));
#27729=DIRECTION('ref_axis',(0.,0.,-1.));
#27730=DIRECTION('center_axis',(-1.,0.,0.));
#27731=DIRECTION('ref_axis',(0.,0.,1.));
#27732=DIRECTION('center_axis',(0.,1.,0.));
#27733=DIRECTION('ref_axis',(0.,0.,1.));
#27734=DIRECTION('center_axis',(-1.,0.,1.22464679914735E-16));
#27735=DIRECTION('ref_axis',(-1.22464679914735E-16,0.,-1.));
#27736=DIRECTION('center_axis',(0.,1.,0.));
#27737=DIRECTION('ref_axis',(1.,0.,0.));
#27738=DIRECTION('center_axis',(0.,1.,0.));
#27739=DIRECTION('ref_axis',(1.,0.,0.));
#27740=DIRECTION('center_axis',(0.,1.,0.));
#27741=DIRECTION('ref_axis',(1.,0.,0.));
#27742=DIRECTION('',(0.,1.,0.));
#27743=DIRECTION('center_axis',(0.,-1.,0.));
#27744=DIRECTION('ref_axis',(1.,0.,0.));
#27745=DIRECTION('center_axis',(0.,-1.,0.));
#27746=DIRECTION('ref_axis',(1.,0.,0.));
#27747=DIRECTION('center_axis',(0.,-1.,0.));
#27748=DIRECTION('ref_axis',(0.,0.,-1.));
#27749=DIRECTION('center_axis',(0.,1.,0.));
#27750=DIRECTION('ref_axis',(1.,0.,0.));
#27751=DIRECTION('center_axis',(-1.,0.,-1.22464679914735E-16));
#27752=DIRECTION('ref_axis',(-1.22464679914735E-16,0.,1.));
#27753=DIRECTION('center_axis',(0.,1.,0.));
#27754=DIRECTION('ref_axis',(0.,0.,1.));
#27755=DIRECTION('',(-1.,0.,0.));
#27756=DIRECTION('center_axis',(0.,1.,0.));
#27757=DIRECTION('ref_axis',(1.,0.,0.));
#27758=DIRECTION('center_axis',(0.,1.,0.));
#27759=DIRECTION('ref_axis',(0.,0.,1.));
#27760=DIRECTION('center_axis',(-1.,0.,0.));
#27761=DIRECTION('ref_axis',(0.,0.,-1.));
#27762=DIRECTION('center_axis',(0.,1.,0.));
#27763=DIRECTION('ref_axis',(1.,0.,0.));
#27764=DIRECTION('center_axis',(0.,1.,0.));
#27765=DIRECTION('ref_axis',(1.,0.,0.));
#27766=DIRECTION('center_axis',(0.,1.,0.));
#27767=DIRECTION('ref_axis',(1.,0.,0.));
#27768=DIRECTION('',(0.,1.,0.));
#27769=DIRECTION('center_axis',(0.,-1.,0.));
#27770=DIRECTION('ref_axis',(1.,0.,0.));
#27771=DIRECTION('center_axis',(0.,-1.,0.));
#27772=DIRECTION('ref_axis',(1.,0.,0.));
#27773=DIRECTION('center_axis',(0.,-1.,0.));
#27774=DIRECTION('ref_axis',(0.,0.,-1.));
#27775=DIRECTION('center_axis',(-1.,0.,0.));
#27776=DIRECTION('ref_axis',(0.,0.,1.));
#27777=DIRECTION('center_axis',(0.,1.,0.));
#27778=DIRECTION('ref_axis',(0.,0.,1.));
#27779=DIRECTION('center_axis',(-1.,0.,1.22464679914735E-16));
#27780=DIRECTION('ref_axis',(-1.22464679914735E-16,0.,-1.));
#27781=DIRECTION('center_axis',(0.,1.,0.));
#27782=DIRECTION('ref_axis',(1.,0.,0.));
#27783=DIRECTION('center_axis',(0.,1.,0.));
#27784=DIRECTION('ref_axis',(1.,0.,0.));
#27785=DIRECTION('center_axis',(0.,1.,0.));
#27786=DIRECTION('ref_axis',(1.,0.,0.));
#27787=DIRECTION('',(0.,1.,0.));
#27788=DIRECTION('center_axis',(0.,-1.,0.));
#27789=DIRECTION('ref_axis',(1.,0.,0.));
#27790=DIRECTION('center_axis',(0.,-1.,0.));
#27791=DIRECTION('ref_axis',(1.,0.,0.));
#27792=DIRECTION('center_axis',(0.,-1.,0.));
#27793=DIRECTION('ref_axis',(0.,0.,-1.));
#27794=DIRECTION('center_axis',(-1.,0.,-1.22464679914735E-16));
#27795=DIRECTION('ref_axis',(-1.22464679914735E-16,0.,1.));
#27796=DIRECTION('center_axis',(0.,-0.847998304005088,-0.52999894000318));
#27797=DIRECTION('ref_axis',(0.,0.52999894000318,-0.847998304005088));
#27798=DIRECTION('center_axis',(1.,0.,0.));
#27799=DIRECTION('ref_axis',(0.,0.961248746164355,0.275682513042551));
#27800=DIRECTION('',(1.,0.,0.));
#27801=DIRECTION('center_axis',(1.,0.,0.));
#27802=DIRECTION('ref_axis',(0.,-0.961248746164355,-0.275682513042551));
#27803=DIRECTION('',(-1.,0.,0.));
#27804=DIRECTION('center_axis',(0.,0.847998304005088,0.52999894000318));
#27805=DIRECTION('ref_axis',(0.,-0.52999894000318,0.847998304005088));
#27806=DIRECTION('axis',(0.,0.,1.));
#27807=DIRECTION('refdir',(1.,0.,0.));
#27808=DIRECTION('center_axis',(-1.,0.,0.));
#27809=DIRECTION('ref_axis',(0.,0.,1.));
#27810=DIRECTION('center_axis',(1.,0.,0.));
#27811=DIRECTION('ref_axis',(0.,0.,-1.));
#27812=DIRECTION('center_axis',(1.,0.,0.));
#27813=DIRECTION('ref_axis',(0.,0.,-1.));
#27814=DIRECTION('center_axis',(1.,0.,0.));
#27815=DIRECTION('ref_axis',(0.,1.,0.));
#27816=DIRECTION('center_axis',(1.,0.,0.));
#27817=DIRECTION('ref_axis',(0.,1.,0.));
#27818=DIRECTION('',(-1.,0.,0.));
#27819=DIRECTION('center_axis',(1.,0.,0.));
#27820=DIRECTION('ref_axis',(0.,1.,0.));
#27821=DIRECTION('center_axis',(1.,0.,0.));
#27822=DIRECTION('ref_axis',(0.,1.,0.));
#27823=DIRECTION('',(1.,0.,0.));
#27824=DIRECTION('center_axis',(1.,0.,0.));
#27825=DIRECTION('ref_axis',(0.,0.,-1.));
#27826=DIRECTION('center_axis',(1.,0.,0.));
#27827=DIRECTION('ref_axis',(0.,0.,-1.));
#27828=DIRECTION('center_axis',(1.,0.,0.));
#27829=DIRECTION('ref_axis',(0.,0.,-1.));
#27830=DIRECTION('center_axis',(1.,0.,0.));
#27831=DIRECTION('ref_axis',(0.,1.,0.));
#27832=DIRECTION('',(-1.,0.,0.));
#27833=DIRECTION('center_axis',(-1.,0.,0.));
#27834=DIRECTION('ref_axis',(0.,1.,0.));
#27835=DIRECTION('center_axis',(-1.,0.,0.));
#27836=DIRECTION('ref_axis',(0.,0.,1.));
#27837=DIRECTION('center_axis',(1.,0.,0.));
#27838=DIRECTION('ref_axis',(0.,1.,0.));
#27839=DIRECTION('center_axis',(1.,0.,0.));
#27840=DIRECTION('ref_axis',(0.,0.,-1.));
#27841=DIRECTION('',(-1.,0.,0.));
#27842=DIRECTION('center_axis',(-1.,0.,0.));
#27843=DIRECTION('ref_axis',(0.,1.,0.));
#27844=DIRECTION('center_axis',(1.,0.,0.));
#27845=DIRECTION('ref_axis',(0.,0.,-1.));
#27846=DIRECTION('center_axis',(1.,0.,0.));
#27847=DIRECTION('ref_axis',(0.,0.,-1.));
#27848=DIRECTION('center_axis',(1.,0.,0.));
#27849=DIRECTION('ref_axis',(0.,1.,0.));
#27850=DIRECTION('center_axis',(1.,0.,0.));
#27851=DIRECTION('ref_axis',(0.,1.,0.));
#27852=DIRECTION('',(-1.,0.,0.));
#27853=DIRECTION('center_axis',(1.,0.,0.));
#27854=DIRECTION('ref_axis',(0.,0.,-1.));
#27855=DIRECTION('center_axis',(-1.,0.,0.));
#27856=DIRECTION('ref_axis',(0.,0.,1.));
#27857=DIRECTION('center_axis',(1.,0.,0.));
#27858=DIRECTION('ref_axis',(0.,0.,-1.));
#27859=DIRECTION('center_axis',(1.,0.,0.));
#27860=DIRECTION('ref_axis',(0.,1.,0.));
#27861=DIRECTION('',(1.,0.,0.));
#27862=DIRECTION('center_axis',(-1.,0.,0.));
#27863=DIRECTION('ref_axis',(0.,1.,0.));
#27864=DIRECTION('center_axis',(1.,0.,0.));
#27865=DIRECTION('ref_axis',(0.,0.,-1.));
#27866=DIRECTION('center_axis',(1.,0.,0.));
#27867=DIRECTION('ref_axis',(0.,0.,-1.));
#27868=DIRECTION('center_axis',(1.,0.,0.));
#27869=DIRECTION('ref_axis',(0.,0.,-1.));
#27870=DIRECTION('center_axis',(1.,0.,0.));
#27871=DIRECTION('ref_axis',(0.,1.,0.));
#27872=DIRECTION('center_axis',(1.,0.,0.));
#27873=DIRECTION('ref_axis',(0.,0.,-1.));
#27874=DIRECTION('center_axis',(1.,0.,0.));
#27875=DIRECTION('ref_axis',(0.,1.,0.));
#27876=DIRECTION('',(-1.,0.,0.));
#27877=DIRECTION('center_axis',(1.,0.,0.));
#27878=DIRECTION('ref_axis',(0.,0.,-1.));
#27879=DIRECTION('center_axis',(-1.,0.,0.));
#27880=DIRECTION('ref_axis',(0.,0.,1.));
#27881=DIRECTION('center_axis',(-1.,0.,0.));
#27882=DIRECTION('ref_axis',(0.,1.,0.));
#27883=DIRECTION('center_axis',(1.,0.,0.));
#27884=DIRECTION('ref_axis',(0.,1.,0.));
#27885=DIRECTION('',(-1.,0.,0.));
#27886=DIRECTION('center_axis',(1.,0.,0.));
#27887=DIRECTION('ref_axis',(0.,1.,0.));
#27888=DIRECTION('center_axis',(1.,0.,0.));
#27889=DIRECTION('ref_axis',(0.,0.,-1.));
#27890=DIRECTION('center_axis',(1.,0.,0.));
#27891=DIRECTION('ref_axis',(0.,0.,-1.));
#27892=DIRECTION('center_axis',(1.,0.,0.));
#27893=DIRECTION('ref_axis',(0.,1.,0.));
#27894=DIRECTION('',(-1.,0.,0.));
#27895=DIRECTION('center_axis',(1.,0.,0.));
#27896=DIRECTION('ref_axis',(0.,0.,-1.));
#27897=DIRECTION('center_axis',(-1.,0.,0.));
#27898=DIRECTION('ref_axis',(0.,0.,1.));
#27899=DIRECTION('center_axis',(-1.,0.,0.));
#27900=DIRECTION('ref_axis',(0.,1.,0.));
#27901=DIRECTION('center_axis',(1.,0.,0.));
#27902=DIRECTION('ref_axis',(0.,1.,0.));
#27903=DIRECTION('',(-1.,0.,0.));
#27904=DIRECTION('center_axis',(1.,0.,0.));
#27905=DIRECTION('ref_axis',(0.,0.,-1.));
#27906=DIRECTION('center_axis',(1.,0.,0.));
#27907=DIRECTION('ref_axis',(0.,1.,0.));
#27908=DIRECTION('',(-0.707106781186548,0.707106781186547,8.65956056235492E-17));
#27909=DIRECTION('center_axis',(1.,0.,0.));
#27910=DIRECTION('ref_axis',(0.,0.,-1.));
#27911=DIRECTION('center_axis',(1.,0.,0.));
#27912=DIRECTION('ref_axis',(0.,1.,0.));
#27913=DIRECTION('center_axis',(1.,0.,0.));
#27914=DIRECTION('ref_axis',(0.,0.,-1.));
#27915=DIRECTION('',(-1.,0.,0.));
#27916=DIRECTION('center_axis',(-1.,0.,0.));
#27917=DIRECTION('ref_axis',(0.,1.,0.));
#27918=DIRECTION('',(0.707106781186548,0.707106781186547,-8.65956056235492E-17));
#27919=DIRECTION('center_axis',(1.,0.,0.));
#27920=DIRECTION('ref_axis',(0.,0.,-1.));
#27921=DIRECTION('center_axis',(1.,0.,0.));
#27922=DIRECTION('ref_axis',(0.,1.,0.));
#27923=DIRECTION('',(1.,0.,0.));
#27924=DIRECTION('center_axis',(-1.,0.,0.));
#27925=DIRECTION('ref_axis',(0.,0.,1.));
#27926=DIRECTION('axis',(0.,0.,1.));
#27927=DIRECTION('refdir',(1.,0.,0.));
#27928=DIRECTION('center_axis',(1.,0.,0.));
#27929=DIRECTION('ref_axis',(0.,1.,0.));
#27930=DIRECTION('center_axis',(1.,0.,0.));
#27931=DIRECTION('ref_axis',(0.,0.,-1.));
#27932=DIRECTION('',(-0.707106781186548,0.707106781186547,8.65956056235492E-17));
#27933=DIRECTION('center_axis',(1.,0.,0.));
#27934=DIRECTION('ref_axis',(0.,0.,-1.));
#27935=DIRECTION('center_axis',(1.,0.,0.));
#27936=DIRECTION('ref_axis',(0.,1.,0.));
#27937=DIRECTION('center_axis',(1.,0.,0.));
#27938=DIRECTION('ref_axis',(0.,0.,-1.));
#27939=DIRECTION('',(-1.,0.,0.));
#27940=DIRECTION('center_axis',(-1.,0.,0.));
#27941=DIRECTION('ref_axis',(0.,1.,0.));
#27942=DIRECTION('',(0.707106781186548,0.707106781186547,-8.65956056235492E-17));
#27943=DIRECTION('center_axis',(1.,0.,0.));
#27944=DIRECTION('ref_axis',(0.,0.,-1.));
#27945=DIRECTION('center_axis',(1.,0.,0.));
#27946=DIRECTION('ref_axis',(0.,0.,-1.));
#27947=DIRECTION('center_axis',(1.,0.,0.));
#27948=DIRECTION('ref_axis',(0.,0.,-1.));
#27949=DIRECTION('center_axis',(1.,0.,0.));
#27950=DIRECTION('ref_axis',(0.,1.,0.));
#27951=DIRECTION('center_axis',(1.,0.,0.));
#27952=DIRECTION('ref_axis',(0.,0.,-1.));
#27953=DIRECTION('',(1.,0.,0.));
#27954=DIRECTION('center_axis',(-1.,0.,0.));
#27955=DIRECTION('ref_axis',(0.,0.,1.));
#27956=DIRECTION('axis',(0.,0.,1.));
#27957=DIRECTION('refdir',(1.,0.,0.));
#27958=DIRECTION('center_axis',(1.,0.,0.));
#27959=DIRECTION('ref_axis',(0.,1.,0.));
#27960=DIRECTION('center_axis',(1.,0.,0.));
#27961=DIRECTION('ref_axis',(0.,0.,-1.));
#27962=DIRECTION('',(-0.707106781186549,0.707106781186546,8.65956056235491E-17));
#27963=DIRECTION('center_axis',(1.,0.,0.));
#27964=DIRECTION('ref_axis',(0.,0.,-1.));
#27965=DIRECTION('center_axis',(1.,0.,0.));
#27966=DIRECTION('ref_axis',(0.,1.,0.));
#27967=DIRECTION('center_axis',(1.,0.,0.));
#27968=DIRECTION('ref_axis',(0.,0.,-1.));
#27969=DIRECTION('',(-1.,0.,0.));
#27970=DIRECTION('center_axis',(-1.,0.,0.));
#27971=DIRECTION('ref_axis',(0.,1.,0.));
#27972=DIRECTION('',(0.707106781186549,0.707106781186546,-8.65956056235491E-17));
#27973=DIRECTION('center_axis',(1.,0.,0.));
#27974=DIRECTION('ref_axis',(0.,0.,-1.));
#27975=DIRECTION('center_axis',(1.,0.,0.));
#27976=DIRECTION('ref_axis',(0.,0.,-1.));
#27977=DIRECTION('center_axis',(-1.,0.,0.));
#27978=DIRECTION('ref_axis',(0.,0.,1.));
#27979=DIRECTION('axis',(0.,0.,1.));
#27980=DIRECTION('refdir',(1.,0.,0.));
#27981=DIRECTION('center_axis',(1.,0.,0.));
#27982=DIRECTION('ref_axis',(0.,1.,0.));
#27983=DIRECTION('center_axis',(1.,0.,0.));
#27984=DIRECTION('ref_axis',(0.,0.,-1.));
#27985=DIRECTION('',(-0.707106781186548,0.707106781186547,8.65956056235492E-17));
#27986=DIRECTION('center_axis',(1.,0.,0.));
#27987=DIRECTION('ref_axis',(0.,0.,-1.));
#27988=DIRECTION('center_axis',(1.,0.,0.));
#27989=DIRECTION('ref_axis',(0.,1.,0.));
#27990=DIRECTION('center_axis',(1.,0.,0.));
#27991=DIRECTION('ref_axis',(0.,0.,-1.));
#27992=DIRECTION('',(-1.,0.,0.));
#27993=DIRECTION('center_axis',(-1.,0.,0.));
#27994=DIRECTION('ref_axis',(0.,1.,0.));
#27995=DIRECTION('',(0.707106781186548,0.707106781186547,-8.65956056235492E-17));
#27996=DIRECTION('center_axis',(1.,0.,0.));
#27997=DIRECTION('ref_axis',(0.,0.,-1.));
#27998=DIRECTION('center_axis',(1.,0.,0.));
#27999=DIRECTION('ref_axis',(0.,0.,-1.));
#28000=DIRECTION('center_axis',(-1.,0.,0.));
#28001=DIRECTION('ref_axis',(0.,0.,1.));
#28002=DIRECTION('axis',(0.,0.,1.));
#28003=DIRECTION('refdir',(1.,0.,0.));
#28004=DIRECTION('center_axis',(-1.,0.,0.));
#28005=DIRECTION('ref_axis',(0.,0.,1.));
#28006=DIRECTION('center_axis',(1.,0.,0.));
#28007=DIRECTION('ref_axis',(0.,0.,-1.));
#28008=DIRECTION('center_axis',(1.,0.,0.));
#28009=DIRECTION('ref_axis',(0.,1.,0.));
#28010=DIRECTION('center_axis',(1.,0.,0.));
#28011=DIRECTION('ref_axis',(0.,0.,-1.));
#28012=DIRECTION('',(-0.707106781186548,0.707106781186547,8.65956056235493E-17));
#28013=DIRECTION('center_axis',(1.,0.,0.));
#28014=DIRECTION('ref_axis',(0.,1.,0.));
#28015=DIRECTION('center_axis',(1.,0.,0.));
#28016=DIRECTION('ref_axis',(0.,0.,-1.));
#28017=DIRECTION('',(-1.,0.,0.));
#28018=DIRECTION('center_axis',(-1.,0.,0.));
#28019=DIRECTION('ref_axis',(0.,0.,1.));
#28020=DIRECTION('center_axis',(1.,0.,0.));
#28021=DIRECTION('ref_axis',(0.,0.,-1.));
#28022=DIRECTION('center_axis',(1.,0.,0.));
#28023=DIRECTION('ref_axis',(0.,1.,0.));
#28024=DIRECTION('center_axis',(1.,0.,0.));
#28025=DIRECTION('ref_axis',(0.,0.,-1.));
#28026=DIRECTION('',(-1.,0.,0.));
#28027=DIRECTION('center_axis',(-1.,0.,0.));
#28028=DIRECTION('ref_axis',(0.,1.,0.));
#28029=DIRECTION('',(0.707106781186548,0.707106781186547,-8.65956056235492E-17));
#28030=DIRECTION('center_axis',(1.,0.,0.));
#28031=DIRECTION('ref_axis',(0.,0.,-1.));
#28032=DIRECTION('center_axis',(1.,0.,0.));
#28033=DIRECTION('ref_axis',(0.,0.,-1.));
#28034=DIRECTION('center_axis',(1.,0.,0.));
#28035=DIRECTION('ref_axis',(0.,0.,-1.));
#28036=DIRECTION('center_axis',(1.,0.,0.));
#28037=DIRECTION('ref_axis',(0.,1.,0.));
#28038=DIRECTION('center_axis',(1.,0.,0.));
#28039=DIRECTION('ref_axis',(0.,0.,-1.));
#28040=DIRECTION('',(-1.,0.,0.));
#28041=DIRECTION('center_axis',(1.,0.,0.));
#28042=DIRECTION('ref_axis',(0.,0.,-1.));
#28043=DIRECTION('center_axis',(1.,0.,0.));
#28044=DIRECTION('ref_axis',(0.,0.,-1.));
#28045=DIRECTION('center_axis',(1.,0.,0.));
#28046=DIRECTION('ref_axis',(0.,1.,0.));
#28047=DIRECTION('center_axis',(1.,0.,0.));
#28048=DIRECTION('ref_axis',(0.,0.,-1.));
#28049=DIRECTION('',(-1.,0.,0.));
#28050=DIRECTION('center_axis',(-1.,0.,0.));
#28051=DIRECTION('ref_axis',(0.,0.,1.));
#28052=DIRECTION('center_axis',(1.,0.,0.));
#28053=DIRECTION('ref_axis',(0.,0.,-1.));
#28054=DIRECTION('center_axis',(1.,0.,0.));
#28055=DIRECTION('ref_axis',(0.,1.,0.));
#28056=DIRECTION('center_axis',(1.,0.,0.));
#28057=DIRECTION('ref_axis',(0.,0.,-1.));
#28058=DIRECTION('',(-1.,0.,0.));
#28059=DIRECTION('center_axis',(-1.,0.,0.));
#28060=DIRECTION('ref_axis',(0.,1.,0.));
#28061=DIRECTION('',(0.707106781186549,0.707106781186546,-8.65956056235491E-17));
#28062=DIRECTION('center_axis',(1.,0.,0.));
#28063=DIRECTION('ref_axis',(0.,0.,-1.));
#28064=DIRECTION('center_axis',(1.,0.,0.));
#28065=DIRECTION('ref_axis',(0.,0.,-1.));
#28066=DIRECTION('axis',(0.,0.,1.));
#28067=DIRECTION('refdir',(1.,0.,0.));
#28068=DIRECTION('center_axis',(1.,0.,0.));
#28069=DIRECTION('ref_axis',(0.,1.,0.));
#28070=DIRECTION('center_axis',(1.,0.,0.));
#28071=DIRECTION('ref_axis',(0.,0.,-1.));
#28072=DIRECTION('',(-0.707106781186548,0.707106781186547,8.65956056235493E-17));
#28073=DIRECTION('center_axis',(1.,0.,0.));
#28074=DIRECTION('ref_axis',(0.,0.,-1.));
#28075=DIRECTION('center_axis',(1.,0.,0.));
#28076=DIRECTION('ref_axis',(0.,1.,0.));
#28077=DIRECTION('center_axis',(1.,0.,0.));
#28078=DIRECTION('ref_axis',(0.,0.,-1.));
#28079=DIRECTION('',(-1.,0.,0.));
#28080=DIRECTION('center_axis',(-1.,0.,0.));
#28081=DIRECTION('ref_axis',(0.,1.,0.));
#28082=DIRECTION('',(0.707106781186548,0.707106781186547,-8.65956056235493E-17));
#28083=DIRECTION('center_axis',(1.,0.,0.));
#28084=DIRECTION('ref_axis',(0.,0.,-1.));
#28085=DIRECTION('center_axis',(1.,0.,0.));
#28086=DIRECTION('ref_axis',(0.,0.,-1.));
#28087=DIRECTION('center_axis',(-1.,0.,0.));
#28088=DIRECTION('ref_axis',(0.,0.,1.));
#28089=DIRECTION('axis',(0.,0.,1.));
#28090=DIRECTION('refdir',(1.,0.,0.));
#28091=DIRECTION('center_axis',(-1.18358034829556E-16,-1.16627939375949E-19,
1.));
#28092=DIRECTION('ref_axis',(-0.999999546524734,-0.000952339396609238,-5.91790461132479E-17));
#28093=DIRECTION('center_axis',(1.,0.,0.));
#28094=DIRECTION('ref_axis',(0.,0.,-1.));
#28095=DIRECTION('center_axis',(1.,0.,0.));
#28096=DIRECTION('ref_axis',(0.,0.,-1.));
#28097=DIRECTION('center_axis',(1.,0.,0.));
#28098=DIRECTION('ref_axis',(0.,0.,-1.));
#28099=DIRECTION('center_axis',(1.,0.,0.));
#28100=DIRECTION('ref_axis',(0.,1.,0.));
#28101=DIRECTION('center_axis',(1.,0.,0.));
#28102=DIRECTION('ref_axis',(0.,0.,-1.));
#28103=DIRECTION('',(-1.,0.,0.));
#28104=DIRECTION('center_axis',(-1.,0.,0.));
#28105=DIRECTION('ref_axis',(0.,0.,1.));
#28106=DIRECTION('center_axis',(1.,0.,0.));
#28107=DIRECTION('ref_axis',(0.,0.,-1.));
#28108=DIRECTION('center_axis',(1.,0.,0.));
#28109=DIRECTION('ref_axis',(0.,1.,0.));
#28110=DIRECTION('center_axis',(1.,0.,0.));
#28111=DIRECTION('ref_axis',(0.,0.,-1.));
#28112=DIRECTION('',(-1.,0.,0.));
#28113=DIRECTION('center_axis',(-1.,0.,0.));
#28114=DIRECTION('ref_axis',(0.,1.,0.));
#28115=DIRECTION('',(0.707106781186548,0.707106781186547,-8.65956056235493E-17));
#28116=DIRECTION('center_axis',(1.,0.,0.));
#28117=DIRECTION('ref_axis',(0.,0.,-1.));
#28118=DIRECTION('center_axis',(1.,0.,0.));
#28119=DIRECTION('ref_axis',(0.,0.,-1.));
#28120=DIRECTION('axis',(0.,0.,1.));
#28121=DIRECTION('refdir',(1.,0.,0.));
#28122=DIRECTION('center_axis',(-9.3953993621311E-17,-8.45359356200646E-19,
1.));
#28123=DIRECTION('ref_axis',(-0.999976174819374,-0.0069028829927877,-4.69787952835825E-17));
#28124=DIRECTION('center_axis',(1.,0.,0.));
#28125=DIRECTION('ref_axis',(0.,0.,-1.));
#28126=DIRECTION('center_axis',(1.,0.,0.));
#28127=DIRECTION('ref_axis',(0.,0.,-1.));
#28128=DIRECTION('center_axis',(1.,0.,0.));
#28129=DIRECTION('ref_axis',(0.,0.,-1.));
#28130=DIRECTION('center_axis',(1.,0.,0.));
#28131=DIRECTION('ref_axis',(0.,1.,0.));
#28132=DIRECTION('center_axis',(1.,0.,0.));
#28133=DIRECTION('ref_axis',(0.,0.,-1.));
#28134=DIRECTION('',(-1.,0.,0.));
#28135=DIRECTION('center_axis',(-1.,0.,0.));
#28136=DIRECTION('ref_axis',(0.,1.,0.));
#28137=DIRECTION('',(0.707106781186548,0.707106781186547,-8.65956056235492E-17));
#28138=DIRECTION('center_axis',(1.,0.,0.));
#28139=DIRECTION('ref_axis',(0.,0.,-1.));
#28140=DIRECTION('center_axis',(1.,0.,0.));
#28141=DIRECTION('ref_axis',(0.,0.,-1.));
#28142=DIRECTION('',(0.,0.,1.));
#28143=DIRECTION('',(1.,0.,0.));
#28144=DIRECTION('',(0.,0.,1.));
#28145=DIRECTION('',(1.,0.,0.));
#28146=DIRECTION('',(0.,0.,1.));
#28147=DIRECTION('',(1.,0.,0.));
#28148=DIRECTION('',(0.,0.,1.));
#28149=DIRECTION('',(1.,0.,0.));
#28150=DIRECTION('',(0.,1.,0.));
#28151=DIRECTION('',(0.,0.,1.));
#28152=DIRECTION('',(0.,1.,0.));
#28153=DIRECTION('',(0.,0.,1.));
#28154=DIRECTION('',(0.,0.,1.));
#28155=DIRECTION('',(1.,0.,0.));
#28156=DIRECTION('',(0.,1.,0.));
#28157=DIRECTION('',(0.,0.,1.));
#28158=DIRECTION('',(0.,1.,0.));
#28159=DIRECTION('',(0.,0.,1.));
#28160=DIRECTION('',(0.,0.,1.));
#28161=DIRECTION('',(1.,0.,0.));
#28162=DIRECTION('',(0.,0.,1.));
#28163=DIRECTION('',(1.,0.,0.));
#28164=DIRECTION('',(0.,0.,1.));
#28165=DIRECTION('',(1.,0.,0.));
#28166=DIRECTION('',(0.,0.,1.));
#28167=DIRECTION('',(1.,0.,0.));
#28168=DIRECTION('',(0.,0.,1.));
#28169=DIRECTION('',(0.,-1.,0.));
#28170=DIRECTION('',(0.,0.,1.));
#28171=DIRECTION('',(0.,-1.,0.));
#28172=DIRECTION('',(0.,0.,-1.));
#28173=DIRECTION('',(0.,1.,0.));
#28174=DIRECTION('',(0.,0.,-1.));
#28175=DIRECTION('',(0.,1.,0.));
#28176=DIRECTION('',(0.,0.,1.));
#28177=DIRECTION('',(1.,0.,0.));
#28178=DIRECTION('',(0.,0.,1.));
#28179=DIRECTION('',(1.,0.,0.));
#28180=DIRECTION('',(0.,0.,1.));
#28181=DIRECTION('',(1.,0.,0.));
#28182=DIRECTION('',(0.,0.,1.));
#28183=DIRECTION('',(1.,0.,0.));
#28184=DIRECTION('',(0.,0.,1.));
#28185=DIRECTION('',(1.,0.,0.));
#28186=DIRECTION('',(0.,0.,1.));
#28187=DIRECTION('',(0.,-1.,0.));
#28188=DIRECTION('',(0.,0.,1.));
#28189=DIRECTION('',(0.,-1.,0.));
#28190=DIRECTION('',(0.,0.,-1.));
#28191=DIRECTION('',(0.,1.,0.));
#28192=DIRECTION('',(0.,0.,-1.));
#28193=DIRECTION('',(0.,1.,0.));
#28194=CARTESIAN_POINT('',(0.,0.,0.));
#28195=CARTESIAN_POINT('',(0.,0.,0.));
#28196=CARTESIAN_POINT('Ctrl Pts',(38.2828091153483,1.11761889124797,-6.97607757441136));
#28197=CARTESIAN_POINT('Ctrl Pts',(37.8234650542136,1.10267068721089,-6.34100646753079));
#28198=CARTESIAN_POINT('Ctrl Pts',(37.4119152099722,1.08893748353005,-5.66458394800673));
#28199=CARTESIAN_POINT('Ctrl Pts',(36.1750430818529,1.05272528345341,-3.19923902056362));
#28200=CARTESIAN_POINT('Ctrl Pts',(35.6552816803935,1.04017275782615,-1.28742952530723));
#28201=CARTESIAN_POINT('Ctrl Pts',(35.4024624085441,1.03362032558888,2.58828262498384));
#28202=CARTESIAN_POINT('Ctrl Pts',(35.6533597239508,1.03853511081772,4.49488675691593));
#28203=CARTESIAN_POINT('Ctrl Pts',(36.9684333541811,1.07241301784844,8.4308675114562));
#28204=CARTESIAN_POINT('Ctrl Pts',(38.166980981151,1.10654958981212,10.3494011670926));
#28205=CARTESIAN_POINT('Ctrl Pts',(42.4575040433213,1.31384645443024,14.7529942978924));
#28206=CARTESIAN_POINT('Ctrl Pts',(49.7427089282406,1.83976032664608,17.7051751379966));
#28207=CARTESIAN_POINT('Ctrl Pts',(57.4412528288424,3.05949378929588,14.9345604704364));
#28208=CARTESIAN_POINT('Ctrl Pts',(60.2987018294292,3.48165017466642,12.2915412726567));
#28209=CARTESIAN_POINT('Ctrl Pts',(62.2074133981106,3.75719846747112,10.3606273747238));
#28210=CARTESIAN_POINT('Ctrl Pts',(63.3952259577481,3.96815686996487,8.42841971454959));
#28211=CARTESIAN_POINT('Ctrl Pts',(64.3744913950824,4.11561648662927,5.51345108116818));
#28212=CARTESIAN_POINT('Ctrl Pts',(64.8255995379143,4.15696630959856,3.66330292048651));
#28213=CARTESIAN_POINT('Ctrl Pts',(64.9117544346393,4.15341185643901,1.72453429192862));
#28214=CARTESIAN_POINT('Ctrl Pts',(64.8223415702672,4.18106939249892,0.39897045654781));
#28215=CARTESIAN_POINT('Ctrl Pts',(64.7753392842092,4.17529785000113,-0.106728049613198));
#28216=CARTESIAN_POINT('Ctrl Pts',(64.576120105023,4.10463228263791,-1.47947502913099));
#28217=CARTESIAN_POINT('Ctrl Pts',(64.1132581733554,3.92494468696414,-3.21690424520401));
#28218=CARTESIAN_POINT('Ctrl Pts',(63.4924556791943,3.96423510196274,-4.61414496951605));
#28219=CARTESIAN_POINT('Ctrl Pts',(62.8174909867282,4.12437261502235,-5.90593483351001));
#28220=CARTESIAN_POINT('Ctrl Pts',(62.1074018466296,4.41790060200681,-7.02319446864059));
#28221=CARTESIAN_POINT('Ctrl Pts',(60.874042949834,4.65644789261152,-8.48467747835397));
#28222=CARTESIAN_POINT('Ctrl Pts',(59.5348713215518,4.62838251566496,-9.75493905450226));
#28223=CARTESIAN_POINT('Ctrl Pts',(58.4404096210695,4.46707972840779,-10.538993216145));
#28224=CARTESIAN_POINT('Ctrl Pts',(57.7265849587516,4.3804810495509,-10.9717881911377));
#28225=CARTESIAN_POINT('Ctrl Pts',(57.427631809086,4.34556285696451,-11.1495376426103));
#28226=CARTESIAN_POINT('Ctrl Pts',(56.8142079310565,4.28689339090294,-11.4851678734925));
#28227=CARTESIAN_POINT('Ctrl Pts',(56.019812652493,4.23179766652216,-11.8577285498697));
#28228=CARTESIAN_POINT('Ctrl Pts',(55.0368711190457,4.16394895128873,-12.244451574114));
#28229=CARTESIAN_POINT('Ctrl Pts',(53.0324279581537,4.02139112324784,-12.8739714647708));
#28230=CARTESIAN_POINT('Ctrl Pts',(50.8522420828372,3.64495098639604,-13.1243776858381));
#28231=CARTESIAN_POINT('Ctrl Pts',(49.0742420084695,3.08805349273552,-13.0189954266342));
#28232=CARTESIAN_POINT('Ctrl Pts',(47.74311273162,2.65858895657289,-12.8839029021203));
#28233=CARTESIAN_POINT('Ctrl Pts',(46.0943092484674,2.06945988764268,-12.5441901629219));
#28234=CARTESIAN_POINT('Ctrl Pts',(43.9349361397835,1.53425192497824,-11.7148070258463));
#28235=CARTESIAN_POINT('Ctrl Pts',(42.7080397066157,1.37629460379916,-11.0306022357214));
#28236=CARTESIAN_POINT('Ctrl Pts',(41.8420335216443,1.28598589888282,-10.4618812091461));
#28237=CARTESIAN_POINT('Ctrl Pts',(41.2944047225801,1.23959147323119,-10.0745090823477));
#28238=CARTESIAN_POINT('Ctrl Pts',(39.9171313864447,1.1643772887167,-8.95351967626449));
#28239=CARTESIAN_POINT('Ctrl Pts',(38.9330416908621,1.13877908473415,-7.87506366436157));
#28240=CARTESIAN_POINT('Ctrl Pts',(38.2828091153483,1.11761889124797,-6.97607757441134));
#28241=CARTESIAN_POINT('Ctrl Pts',(38.2843482333976,0.970543869916695,-6.97820549874059));
#28242=CARTESIAN_POINT('Ctrl Pts',(37.824791924162,0.955556555693735,-6.34307994854715));
#28243=CARTESIAN_POINT('Ctrl Pts',(37.4129921013726,0.941740302951165,-5.66650842402892));
#28244=CARTESIAN_POINT('Ctrl Pts',(36.1752804401636,0.905197105915887,-3.20024374312772));
#28245=CARTESIAN_POINT('Ctrl Pts',(35.6553911302101,0.892454629920639,-1.28819029786402));
#28246=CARTESIAN_POINT('Ctrl Pts',(35.4023984837046,0.885821644900872,2.5885372043277));
#28247=CARTESIAN_POINT('Ctrl Pts',(35.6534560236685,0.890838387074693,4.4954292042868));
#28248=CARTESIAN_POINT('Ctrl Pts',(36.9690538044905,0.925251214315146,8.43257933875382));
#28249=CARTESIAN_POINT('Ctrl Pts',(38.1687976685799,0.959829053301754,10.3518678931255));
#28250=CARTESIAN_POINT('Ctrl Pts',(42.4632009249305,1.16789187702483,14.7578885142237));
#28251=CARTESIAN_POINT('Ctrl Pts',(49.7618317204618,1.6931399112023,17.7090114279978));
#28252=CARTESIAN_POINT('Ctrl Pts',(57.4610310499495,2.90441419567966,14.9231238711394));
#28253=CARTESIAN_POINT('Ctrl Pts',(60.3097400224713,3.32399961368451,12.2809040971181));
#28254=CARTESIAN_POINT('Ctrl Pts',(62.2158010395199,3.59788612667688,10.3487350385468));
#28255=CARTESIAN_POINT('Ctrl Pts',(63.4002833408593,3.80723506974322,8.41753794372203));
#28256=CARTESIAN_POINT('Ctrl Pts',(64.3756536499245,3.95482640879122,5.50797169852747));
#28257=CARTESIAN_POINT('Ctrl Pts',(64.8253779982732,3.99801213031397,3.66556685127137));
#28258=CARTESIAN_POINT('Ctrl Pts',(64.9117753274102,3.99589965313243,1.72084989994536));
#28259=CARTESIAN_POINT('Ctrl Pts',(64.8222143508002,4.02098591528982,0.397822582894523));
#28260=CARTESIAN_POINT('Ctrl Pts',(64.7759267056921,4.01433363661953,-0.100391348441605));
#28261=CARTESIAN_POINT('Ctrl Pts',(64.5786238367047,3.94076580473302,-1.46658139432066));
#28262=CARTESIAN_POINT('Ctrl Pts',(64.117831181995,3.75607887428162,-3.2065576872073));
#28263=CARTESIAN_POINT('Ctrl Pts',(63.4888906171941,3.78991406306379,-4.62291834378092));
#28264=CARTESIAN_POINT('Ctrl Pts',(62.802436085822,3.94505235147423,-5.93252337080619));
#28265=CARTESIAN_POINT('Ctrl Pts',(62.0853063832136,4.23159609271163,-7.05224389309994));
#28266=CARTESIAN_POINT('Ctrl Pts',(60.866372023969,4.46084159502816,-8.49116591110996));
#28267=CARTESIAN_POINT('Ctrl Pts',(59.5475053704118,4.43416211348493,-9.74333222473352));
#28268=CARTESIAN_POINT('Ctrl Pts',(58.4568923922613,4.27445806559024,-10.5279602375712));
#28269=CARTESIAN_POINT('Ctrl Pts',(57.7426864679962,4.18653414690636,-10.9621830331791));
#28270=CARTESIAN_POINT('Ctrl Pts',(57.4419997351774,4.14960693218127,-11.1414507351609));
#28271=CARTESIAN_POINT('Ctrl Pts',(56.8262448121692,4.08791202738523,-11.4791825193719));
#28272=CARTESIAN_POINT('Ctrl Pts',(56.0302740120864,4.02944743362823,-11.8531328935142));
#28273=CARTESIAN_POINT('Ctrl Pts',(55.0487268897378,3.95898137161517,-12.2403796446246));
#28274=CARTESIAN_POINT('Ctrl Pts',(53.0526650913507,3.81294159687107,-12.8684207467596));
#28275=CARTESIAN_POINT('Ctrl Pts',(50.8995528671741,3.44390300519801,-13.1207367571065));
#28276=CARTESIAN_POINT('Ctrl Pts',(49.1290190995407,2.90117687030285,-13.0231451906789));
#28277=CARTESIAN_POINT('Ctrl Pts',(47.7994031066733,2.4821543279567,-12.8933016449541));
#28278=CARTESIAN_POINT('Ctrl Pts',(46.1394375535869,1.90575400846461,-12.5586946873949));
#28279=CARTESIAN_POINT('Ctrl Pts',(43.9556751935569,1.38157721032517,-11.7254914115979));
#28280=CARTESIAN_POINT('Ctrl Pts',(42.7203926546672,1.22604125597042,-11.0380186679154));
#28281=CARTESIAN_POINT('Ctrl Pts',(41.8510060573403,1.13609818750472,-10.4681041752686));
#28282=CARTESIAN_POINT('Ctrl Pts',(41.300244194319,1.09125622040995,-10.0790642159954));
#28283=CARTESIAN_POINT('Ctrl Pts',(39.9191713337688,1.01731653755015,-8.95575210737738));
#28284=CARTESIAN_POINT('Ctrl Pts',(38.9348812604486,0.991759426515284,-7.87726865688117));
#28285=CARTESIAN_POINT('Ctrl Pts',(38.2843482333976,0.970543869916693,-6.97820549874057));
#28286=CARTESIAN_POINT('Ctrl Pts',(38.2338763919957,0.676840453798634,-7.02118403389358));
#28287=CARTESIAN_POINT('Ctrl Pts',(37.7717920326072,0.661775302774764,-6.38309719311575));
#28288=CARTESIAN_POINT('Ctrl Pts',(37.3575860906707,0.647794127754478,-5.70323225274495));
#28289=CARTESIAN_POINT('Ctrl Pts',(36.1123525330349,0.610593091434165,-3.22412755712282));
#28290=CARTESIAN_POINT('Ctrl Pts',(35.5896785478952,0.597473572198639,-1.30297380755022));
#28291=CARTESIAN_POINT('Ctrl Pts',(35.3351252218906,0.590680455223746,2.59338985996385));
#28292=CARTESIAN_POINT('Ctrl Pts',(35.5877124163472,0.59589966460025,4.50953805245734));
#28293=CARTESIAN_POINT('Ctrl Pts',(36.9108449328443,0.631375350576928,8.46662689486421));
#28294=CARTESIAN_POINT('Ctrl Pts',(38.1185183684278,0.666829439106687,10.3959359859494));
#28295=CARTESIAN_POINT('Ctrl Pts',(42.4406442978422,0.876416661809782,14.8257561155249));
#28296=CARTESIAN_POINT('Ctrl Pts',(49.7958477126675,1.40034557220048,17.7894082437089));
#28297=CARTESIAN_POINT('Ctrl Pts',(57.5366834538322,2.59483636795635,14.9687982987776));
#28298=CARTESIAN_POINT('Ctrl Pts',(60.3846991062462,3.00931729041542,12.3153796590069));
#28299=CARTESIAN_POINT('Ctrl Pts',(62.2964901059904,3.2799066287722,10.3717454931349));
#28300=CARTESIAN_POINT('Ctrl Pts',(63.4820778102999,3.48606190817418,8.43271076666013));
#28301=CARTESIAN_POINT('Ctrl Pts',(64.4545411897986,3.63390851895106,5.51796931146853));
#28302=CARTESIAN_POINT('Ctrl Pts',(64.9020137172839,3.68073403490991,3.6805130487955));
#28303=CARTESIAN_POINT('Ctrl Pts',(64.9879632943044,3.68148987723326,1.71407508637896));
#28304=CARTESIAN_POINT('Ctrl Pts',(64.9001507314642,3.70147455415994,0.388961732509691));
#28305=CARTESIAN_POINT('Ctrl Pts',(64.8559236706679,3.69307183338057,-0.0971210585065526));
#28306=CARTESIAN_POINT('Ctrl Pts',(64.6648905108266,3.61376880717593,-1.45821181459786));
#28307=CARTESIAN_POINT('Ctrl Pts',(64.2100297152053,3.41916239249666,-3.21445917834352));
#28308=CARTESIAN_POINT('Ctrl Pts',(63.5663200101209,3.44220843949932,-4.67995598826193));
#28309=CARTESIAN_POINT('Ctrl Pts',(62.8598470037644,3.5875286692031,-6.03733781860483));
#28310=CARTESIAN_POINT('Ctrl Pts',(62.1313319346664,3.8603129866682,-7.17486204206737));
#28311=CARTESIAN_POINT('Ctrl Pts',(60.9366508193253,4.07112216165055,-8.58492853258466));
#28312=CARTESIAN_POINT('Ctrl Pts',(59.6468918463728,4.04720779460478,-9.81081719124648));
#28313=CARTESIAN_POINT('Ctrl Pts',(58.554757623092,3.89068939024514,-10.6017315018052));
#28314=CARTESIAN_POINT('Ctrl Pts',(57.8348859259373,3.80015936073672,-11.043412961638));
#28315=CARTESIAN_POINT('Ctrl Pts',(57.5294671083027,3.75925621283239,-11.22905794043));
#28316=CARTESIAN_POINT('Ctrl Pts',(56.9057049465525,3.69159213430375,-11.5768172191285));
#28317=CARTESIAN_POINT('Ctrl Pts',(56.1015735095258,3.62649446962661,-11.9604026832035));
#28318=CARTESIAN_POINT('Ctrl Pts',(55.1154738556396,3.55087990661318,-12.355403877143));
#28319=CARTESIAN_POINT('Ctrl Pts',(53.1194939160782,3.39800079265719,-12.9908439077088));
#28320=CARTESIAN_POINT('Ctrl Pts',(50.9985372139996,3.04359005396801,-13.2449422202065));
#28321=CARTESIAN_POINT('Ctrl Pts',(49.2292301319419,2.52884635192557,-13.1480799473144));
#28322=CARTESIAN_POINT('Ctrl Pts',(47.8934345339389,2.13048353986497,-13.0161964109135));
#28323=CARTESIAN_POINT('Ctrl Pts',(46.2037204788327,1.57914981460136,-12.672375554347));
#28324=CARTESIAN_POINT('Ctrl Pts',(43.9658914820892,1.07677302966014,-11.8125313821532));
#28325=CARTESIAN_POINT('Ctrl Pts',(42.7096093696835,0.926038355842821,-11.1128523513539));
#28326=CARTESIAN_POINT('Ctrl Pts',(41.8297177896006,0.836813474807447,-10.5373478547873));
#28327=CARTESIAN_POINT('Ctrl Pts',(41.2711074075715,0.795053392302155,-10.1418327999497));
#28328=CARTESIAN_POINT('Ctrl Pts',(39.8770164559302,0.723645794097905,-9.00776748871939));
#28329=CARTESIAN_POINT('Ctrl Pts',(38.8879880449638,0.698166193651579,-7.92443909907391));
#28330=CARTESIAN_POINT('Ctrl Pts',(38.2338763919957,0.676840453798629,-7.02118403389356));
#28331=CARTESIAN_POINT('Ctrl Pts',(37.9755726500682,0.260078906144198,-7.21719833326774));
#28332=CARTESIAN_POINT('Ctrl Pts',(37.5026155044898,0.244950287093724,-6.56501278076528));
#28333=CARTESIAN_POINT('Ctrl Pts',(37.0783378702849,0.230836545601503,-5.86997432036658));
#28334=CARTESIAN_POINT('Ctrl Pts',(35.8021634986244,0.19311352273868,-3.33429548649416));
#28335=CARTESIAN_POINT('Ctrl Pts',(35.2667422286841,0.17970731942181,-1.37011705125621));
#28336=CARTESIAN_POINT('Ctrl Pts',(35.0057829672195,0.172789861916432,2.61538435750336));
#28337=CARTESIAN_POINT('Ctrl Pts',(35.2647213031546,0.178164003071174,4.57492439960631));
#28338=CARTESIAN_POINT('Ctrl Pts',(36.6209929910503,0.214460834622622,8.62171290521318));
#28339=CARTESIAN_POINT('Ctrl Pts',(37.8591948792036,0.250608489038568,10.5949420714734));
#28340=CARTESIAN_POINT('Ctrl Pts',(42.2901085418755,0.461561258183715,15.125001674628));
#28341=CARTESIAN_POINT('Ctrl Pts',(49.8305121070811,0.985076187029921,18.1566364375623));
#28342=CARTESIAN_POINT('Ctrl Pts',(57.7671470310111,2.16867740413173,15.2701980250863));
#28343=CARTESIAN_POINT('Ctrl Pts',(60.6718156147976,2.57897979706842,12.5568347354958));
#28344=CARTESIAN_POINT('Ctrl Pts',(62.6293284960575,2.84736891467804,10.566014989906));
#28345=CARTESIAN_POINT('Ctrl Pts',(63.8429017716634,3.05132886188749,8.58195565622854));
#28346=CARTESIAN_POINT('Ctrl Pts',(64.8285820743521,3.19878966350941,5.60448525990243));
#28347=CARTESIAN_POINT('Ctrl Pts',(65.275485562142,3.24760181738135,3.73737513244731));
#28348=CARTESIAN_POINT('Ctrl Pts',(65.3581463113578,3.25021437519247,1.7067892570071));
#28349=CARTESIAN_POINT('Ctrl Pts',(65.278918050488,3.26706734456811,0.353980649115699));
#28350=CARTESIAN_POINT('Ctrl Pts',(65.2393269706764,3.25764677656883,-0.125349094041277));
#28351=CARTESIAN_POINT('Ctrl Pts',(65.0640319535867,3.17608139024397,-1.5076834973838));
#28352=CARTESIAN_POINT('Ctrl Pts',(64.6212457938457,2.97538186506718,-3.3249923897941));
#28353=CARTESIAN_POINT('Ctrl Pts',(63.9611889154096,2.99381204921896,-4.89182750593231));
#28354=CARTESIAN_POINT('Ctrl Pts',(63.2368536880495,3.14024319198427,-6.35014365680316));
#28355=CARTESIAN_POINT('Ctrl Pts',(62.50227653091,3.41141589189322,-7.54919924147722));
#28356=CARTESIAN_POINT('Ctrl Pts',(61.3187069374386,3.61275670087874,-8.97794668849745));
#28357=CARTESIAN_POINT('Ctrl Pts',(60.0237974951738,3.59088824799297,-10.2076024056545));
#28358=CARTESIAN_POINT('Ctrl Pts',(58.8982776603944,3.43605957167923,-11.0244640574304));
#28359=CARTESIAN_POINT('Ctrl Pts',(58.1538979147083,3.34499063864486,-11.4908234586531));
#28360=CARTESIAN_POINT('Ctrl Pts',(57.8375768250259,3.30338878993206,-11.6947038585483));
#28361=CARTESIAN_POINT('Ctrl Pts',(57.191461854579,3.23515093659049,-12.0730719345562));
#28362=CARTESIAN_POINT('Ctrl Pts',(56.3590794249149,3.17002756060386,-12.4899209447339));
#28363=CARTESIAN_POINT('Ctrl Pts',(55.3412124627408,3.09523089727471,-12.9153793174091));
#28364=CARTESIAN_POINT('Ctrl Pts',(53.2858637202805,2.94410587092508,-13.5928076231749));
#28365=CARTESIAN_POINT('Ctrl Pts',(51.1252252958554,2.59665348818909,-13.8437949847423));
#28366=CARTESIAN_POINT('Ctrl Pts',(49.3161008082114,2.09001896696724,-13.7034803700494));
#28367=CARTESIAN_POINT('Ctrl Pts',(47.9461640300902,1.69674609843365,-13.5322820821945));
#28368=CARTESIAN_POINT('Ctrl Pts',(46.2002895057426,1.14928126906623,-13.1183870449433));
#28369=CARTESIAN_POINT('Ctrl Pts',(43.8718153675593,0.653583390728654,-12.1628380118467));
#28370=CARTESIAN_POINT('Ctrl Pts',(42.57085577801,0.505460781225472,-11.4270867861695));
#28371=CARTESIAN_POINT('Ctrl Pts',(41.6631348373488,0.416355188800432,-10.8327479115071));
#28372=CARTESIAN_POINT('Ctrl Pts',(41.0877064851766,0.376568431697981,-10.41767437804));
#28373=CARTESIAN_POINT('Ctrl Pts',(39.6561155818029,0.306894436867863,-9.24753265543428));
#28374=CARTESIAN_POINT('Ctrl Pts',(38.6450754670143,0.281494489279973,-8.1404110781305));
#28375=CARTESIAN_POINT('Ctrl Pts',(37.9755726500682,0.260078906144189,-7.21719833326772));
#28376=CARTESIAN_POINT('Ctrl Pts',(37.6827349553876,0.123820476106236,-7.43200930537173));
#28377=CARTESIAN_POINT('Ctrl Pts',(37.1981115312996,0.108758167919931,-6.76415338866424));
#28378=CARTESIAN_POINT('Ctrl Pts',(36.7631614809068,0.0947959133819992,
-6.0524004348351));
#28379=CARTESIAN_POINT('Ctrl Pts',(35.4544728346314,0.0576802462121595,
-3.45532498536105));
#28380=CARTESIAN_POINT('Ctrl Pts',(34.9052399965703,0.0446571520855538,
-1.44349856127014));
#28381=CARTESIAN_POINT('Ctrl Pts',(34.6375668077913,0.0378911336842094,
2.6394105962902));
#28382=CARTESIAN_POINT('Ctrl Pts',(34.9031853275286,0.0430667657461748,
4.64681425938547));
#28383=CARTESIAN_POINT('Ctrl Pts',(36.2948564127528,0.0783236368819047,
8.79157409478439));
#28384=CARTESIAN_POINT('Ctrl Pts',(37.5644599252781,0.113661228931385,10.8124043557161));
#28385=CARTESIAN_POINT('Ctrl Pts',(42.1078998944315,0.323523601766359,15.4501968176738));
#28386=CARTESIAN_POINT('Ctrl Pts',(49.8287231859174,0.849796931774696,18.5588719405612));
#28387=CARTESIAN_POINT('Ctrl Pts',(57.9754329065988,2.0540989824616,15.6254681029825));
#28388=CARTESIAN_POINT('Ctrl Pts',(60.9594784171162,2.46870777859652,12.8441351803459));
#28389=CARTESIAN_POINT('Ctrl Pts',(62.971560441687,2.74096720090711,10.8037036380583));
#28390=CARTESIAN_POINT('Ctrl Pts',(64.2214654517206,2.9484923882698,8.76815175703241));
#28391=CARTESIAN_POINT('Ctrl Pts',(65.2308459020326,3.09443853654356,5.7106058750305));
#28392=CARTESIAN_POINT('Ctrl Pts',(65.6823520855425,3.13806676670926,3.79439575576531));
#28393=CARTESIAN_POINT('Ctrl Pts',(65.762315057619,3.13733886966709,1.70709534462677));
#28394=CARTESIAN_POINT('Ctrl Pts',(65.6900530491722,3.16070120932451,0.318603327590335));
#28395=CARTESIAN_POINT('Ctrl Pts',(65.6529204214975,3.15356930340056,-0.170262844993036));
#28396=CARTESIAN_POINT('Ctrl Pts',(65.4862706901961,3.08217960117338,-1.59024642585578));
#28397=CARTESIAN_POINT('Ctrl Pts',(65.0461514716187,2.89386831665398,-3.46667020680638));
#28398=CARTESIAN_POINT('Ctrl Pts',(64.3809104358716,2.92998396789142,-5.09288798615411));
#28399=CARTESIAN_POINT('Ctrl Pts',(63.6556566613573,3.10360208747441,-6.60774501667949));
#28400=CARTESIAN_POINT('Ctrl Pts',(62.9225440804532,3.40530745932964,-7.85255781394852));
#28401=CARTESIAN_POINT('Ctrl Pts',(61.7086950342478,3.63132384902911,-9.34491776509278));
#28402=CARTESIAN_POINT('Ctrl Pts',(60.3613536516037,3.60718414391209,-10.6218630745699));
#28403=CARTESIAN_POINT('Ctrl Pts',(59.1952457990793,3.44841050071065,-11.4638466082202));
#28404=CARTESIAN_POINT('Ctrl Pts',(58.4263692487142,3.36258353011487,-11.9491687552984));
#28405=CARTESIAN_POINT('Ctrl Pts',(58.101489891242,3.32884046917442,-12.164519725722));
#28406=CARTESIAN_POINT('Ctrl Pts',(57.4362450214768,3.27343367240952,-12.5627748724467));
#28407=CARTESIAN_POINT('Ctrl Pts',(56.5774664878876,3.223674244555,-13.0020133628729));
#28408=CARTESIAN_POINT('Ctrl Pts',(55.5238152782093,3.16231592704423,-13.4494879741627));
#28409=CARTESIAN_POINT('Ctrl Pts',(53.3899462310028,3.029985365176,-14.1614509406894));
#28410=CARTESIAN_POINT('Ctrl Pts',(51.1305329459546,2.66262149151837,-14.4130141023804));
#28411=CARTESIAN_POINT('Ctrl Pts',(49.2708165592316,2.10607072348422,-14.2349085336049));
#28412=CARTESIAN_POINT('Ctrl Pts',(47.8677938844659,1.67422453698365,-14.0303104653549));
#28413=CARTESIAN_POINT('Ctrl Pts',(46.0951831056431,1.0718027650261,-13.5585223739087));
#28414=CARTESIAN_POINT('Ctrl Pts',(43.7219341720429,0.532922359928608,-12.5251822886396));
#28415=CARTESIAN_POINT('Ctrl Pts',(42.388913557605,0.377751766345516,-11.7591450726125));
#28416=CARTESIAN_POINT('Ctrl Pts',(41.457679963294,0.286900595795112,-11.1471711579781));
#28417=CARTESIAN_POINT('Ctrl Pts',(40.8697916597159,0.243253833273792,-10.7154469863502));
#28418=CARTESIAN_POINT('Ctrl Pts',(39.4040717113082,0.170652973788299,-9.51115933805032));
#28419=CARTESIAN_POINT('Ctrl Pts',(38.3687521783392,0.145142191730392,-8.37740451026479));
#28420=CARTESIAN_POINT('Ctrl Pts',(37.6827349553875,0.123820476106226,-7.43200930537172));
#28421=CARTESIAN_POINT('Ctrl Pts',(37.5039656670749,0.118112959038132,-7.56143810282447));
#28422=CARTESIAN_POINT('Ctrl Pts',(37.0123775719425,0.10313359302091,-6.88405610335296));
#28423=CARTESIAN_POINT('Ctrl Pts',(36.5711306628854,0.0893498876773675,
-6.16220244562775));
#28424=CARTESIAN_POINT('Ctrl Pts',(35.2433527822817,0.0529585045549561,
-3.52820338776542));
#28425=CARTESIAN_POINT('Ctrl Pts',(34.6859738142494,0.0403720985573172,
-1.48759930416187));
#28426=CARTESIAN_POINT('Ctrl Pts',(34.4143703467061,0.0337848714443707,
2.65385351185261));
#28427=CARTESIAN_POINT('Ctrl Pts',(34.6839009903238,0.0387342423626621,
4.69008938372649));
#28428=CARTESIAN_POINT('Ctrl Pts',(36.0963099966431,0.0727670904719236,
8.89387566280885));
#28429=CARTESIAN_POINT('Ctrl Pts',(37.3842658146977,0.107170593364541,10.9433341336584));
#28430=CARTESIAN_POINT('Ctrl Pts',(41.9934716582436,0.315543736904061,15.6460641572062));
#28431=CARTESIAN_POINT('Ctrl Pts',(49.8196297154773,0.84468878067967,18.8009942746542));
#28432=CARTESIAN_POINT('Ctrl Pts',(58.0877581529129,2.07108377161561,15.8397172942412));
#28433=CARTESIAN_POINT('Ctrl Pts',(61.1210009956106,2.49061701093176,13.0173740492313));
#28434=CARTESIAN_POINT('Ctrl Pts',(63.1652907725653,2.76697733959494,10.9477133500425));
#28435=CARTESIAN_POINT('Ctrl Pts',(64.4366398118809,2.97827221081983,8.88139359080468));
#28436=CARTESIAN_POINT('Ctrl Pts',(65.4622821937629,3.12300989375844,5.77488389114306));
#28437=CARTESIAN_POINT('Ctrl Pts',(65.9190548938414,3.16143432460456,3.82648857040399));
#28438=CARTESIAN_POINT('Ctrl Pts',(65.998639811114,3.15704672469335,1.70925454566402));
#28439=CARTESIAN_POINT('Ctrl Pts',(65.928095335385,3.18715779039101,0.298800350813972));
#28440=CARTESIAN_POINT('Ctrl Pts',(65.891116073978,3.18243009548258,-0.199734967314633));
#28441=CARTESIAN_POINT('Ctrl Pts',(65.724890489484,3.12052200322572,-1.64464387487764));
#28442=CARTESIAN_POINT('Ctrl Pts',(65.2803917641197,2.94481678182075,-3.55221350711536));
#28443=CARTESIAN_POINT('Ctrl Pts',(64.6112886712169,2.99710209211733,-5.19738775518303));
#28444=CARTESIAN_POINT('Ctrl Pts',(63.8845078135012,3.19262492584513,-6.72720317525355));
#28445=CARTESIAN_POINT('Ctrl Pts',(63.1478922725819,3.51893245868478,-7.98720386840469));
#28446=CARTESIAN_POINT('Ctrl Pts',(61.9033465036304,3.76669114727106,-9.51925813077716));
#28447=CARTESIAN_POINT('Ctrl Pts',(60.5179602038555,3.74004538058918,-10.8316209977219));
#28448=CARTESIAN_POINT('Ctrl Pts',(59.3303434129858,3.57752994005544,-11.6868660023985));
#28449=CARTESIAN_POINT('Ctrl Pts',(58.5488026525572,3.49573255165253,-12.1790390892533));
#28450=CARTESIAN_POINT('Ctrl Pts',(58.2193592315412,3.46833531514964,-12.3964860812939));
#28451=CARTESIAN_POINT('Ctrl Pts',(57.5441918319574,3.42281957210131,-12.7988621720065));
#28452=CARTESIAN_POINT('Ctrl Pts',(56.6717264715229,3.38439221421136,-13.2427196483312));
#28453=CARTESIAN_POINT('Ctrl Pts',(55.5988183637806,3.33268751766902,-13.6954762514658));
#28454=CARTESIAN_POINT('Ctrl Pts',(53.4217095394243,3.21319086988362,-14.4173723958613));
#28455=CARTESIAN_POINT('Ctrl Pts',(51.1016444796743,2.83048256335952,-14.6743846054424));
#28456=CARTESIAN_POINT('Ctrl Pts',(49.2134657180401,2.23435274398341,-14.4914393185008));
#28457=CARTESIAN_POINT('Ctrl Pts',(47.793446484243,1.77072158723543,-14.281705766681));
#28458=CARTESIAN_POINT('Ctrl Pts',(46.0121640592379,1.12290576810707,-13.7965877390655));
#28459=CARTESIAN_POINT('Ctrl Pts',(43.6223924642014,0.543466278467186,-12.7346019515179));
#28460=CARTESIAN_POINT('Ctrl Pts',(42.2733193663373,0.381005068405684,-11.9542639561288));
#28461=CARTESIAN_POINT('Ctrl Pts',(41.3294951498055,0.288584763006973,-11.332814913621));
#28462=CARTESIAN_POINT('Ctrl Pts',(40.734984113935,0.240755869996147,-10.8931568499415));
#28463=CARTESIAN_POINT('Ctrl Pts',(39.2498617813692,0.164868595658534,-9.67023765817002));
#28464=CARTESIAN_POINT('Ctrl Pts',(38.1998418527826,0.139317264414103,-8.52031812194351));
#28465=CARTESIAN_POINT('Ctrl Pts',(37.5039656670749,0.118112959038122,-7.56143810282446));
#28466=CARTESIAN_POINT('',(37.5042795392924,0.11812305820763,-7.56121085790808));
#28467=CARTESIAN_POINT('',(38.2828091153483,1.11761889124797,-6.97607757441136));
#28468=CARTESIAN_POINT('Ctrl Pts',(37.5042795392924,0.118123058207631,-7.56121085790808));
#28469=CARTESIAN_POINT('Ctrl Pts',(37.6829406508519,0.123916213079733,-7.43185841697136));
#28470=CARTESIAN_POINT('Ctrl Pts',(37.9756374600947,0.26018347422652,-7.21714915205247));
#28471=CARTESIAN_POINT('Ctrl Pts',(38.2338763919957,0.676840453798634,-7.02118403389358));
#28472=CARTESIAN_POINT('Ctrl Pts',(38.2843482333976,0.970543869916695,-6.97820549874059));
#28473=CARTESIAN_POINT('Ctrl Pts',(38.2828091153483,1.11761889124797,-6.97607757441136));
#28474=CARTESIAN_POINT('',(35.495997940798,1.03592643542494,1.63217755032596));
#28475=CARTESIAN_POINT('Ctrl Pts',(38.2828091153483,1.11761889124797,-6.97607757441136));
#28476=CARTESIAN_POINT('Ctrl Pts',(37.8234650542136,1.10267068721089,-6.34100646753079));
#28477=CARTESIAN_POINT('Ctrl Pts',(37.4119152099722,1.08893748353005,-5.66458394800673));
#28478=CARTESIAN_POINT('Ctrl Pts',(36.1750430818529,1.05272528345341,-3.19923902056362));
#28479=CARTESIAN_POINT('Ctrl Pts',(35.6552816803935,1.04017275782615,-1.28742952530723));
#28480=CARTESIAN_POINT('Ctrl Pts',(35.5063406075951,1.03631258419414,0.995832827675688));
#28481=CARTESIAN_POINT('Ctrl Pts',(35.495996386627,1.03600036720019,1.31426374489689));
#28482=CARTESIAN_POINT('Ctrl Pts',(35.495997940798,1.03592643542494,1.63217755032596));
#28483=CARTESIAN_POINT('Ctrl Pts',(35.495997940798,1.03592643542494,1.63217755032596));
#28484=CARTESIAN_POINT('Ctrl Pts',(35.4960057101111,1.03555684987327,3.22143127459461));
#28485=CARTESIAN_POINT('Ctrl Pts',(35.7545552599904,1.04114203174067,4.79776233220028));
#28486=CARTESIAN_POINT('Ctrl Pts',(36.9684333541811,1.07241301784844,8.4308675114562));
#28487=CARTESIAN_POINT('Ctrl Pts',(38.166980981151,1.10654958981212,10.3494011670926));
#28488=CARTESIAN_POINT('Ctrl Pts',(42.4575040433213,1.31384645443024,14.7529942978924));
#28489=CARTESIAN_POINT('Ctrl Pts',(49.7427089282406,1.83976032664608,17.7051751379966));
#28490=CARTESIAN_POINT('Ctrl Pts',(57.4412528288424,3.05949378929588,14.9345604704364));
#28491=CARTESIAN_POINT('Ctrl Pts',(60.2987018294292,3.48165017466642,12.2915412726567));
#28492=CARTESIAN_POINT('Ctrl Pts',(62.2074133981106,3.75719846747112,10.3606273747238));
#28493=CARTESIAN_POINT('Ctrl Pts',(63.3952259577481,3.96815686996487,8.42841971454959));
#28494=CARTESIAN_POINT('Ctrl Pts',(64.3744913950824,4.11561648662927,5.51345108116818));
#28495=CARTESIAN_POINT('Ctrl Pts',(64.8255995379143,4.15696630959856,3.66330292048651));
#28496=CARTESIAN_POINT('Ctrl Pts',(64.9117544346393,4.15341185643901,1.72453429192862));
#28497=CARTESIAN_POINT('Ctrl Pts',(64.8223415702672,4.18106939249892,0.39897045654781));
#28498=CARTESIAN_POINT('Ctrl Pts',(64.7753392842092,4.17529785000113,-0.106728049613198));
#28499=CARTESIAN_POINT('Ctrl Pts',(64.576120105023,4.10463228263791,-1.47947502913099));
#28500=CARTESIAN_POINT('Ctrl Pts',(64.1132581733554,3.92494468696414,-3.21690424520401));
#28501=CARTESIAN_POINT('Ctrl Pts',(63.4924556791943,3.96423510196274,-4.61414496951605));
#28502=CARTESIAN_POINT('Ctrl Pts',(62.8174909867282,4.12437261502235,-5.90593483351001));
#28503=CARTESIAN_POINT('Ctrl Pts',(62.1074018466296,4.41790060200681,-7.02319446864059));
#28504=CARTESIAN_POINT('Ctrl Pts',(60.874042949834,4.65644789261152,-8.48467747835397));
#28505=CARTESIAN_POINT('Ctrl Pts',(59.5348713215518,4.62838251566496,-9.75493905450226));
#28506=CARTESIAN_POINT('Ctrl Pts',(58.4404096210695,4.46707972840779,-10.538993216145));
#28507=CARTESIAN_POINT('Ctrl Pts',(57.7265849587516,4.3804810495509,-10.9717881911377));
#28508=CARTESIAN_POINT('Ctrl Pts',(57.427631809086,4.34556285696451,-11.1495376426103));
#28509=CARTESIAN_POINT('Ctrl Pts',(56.8142079310565,4.28689339090294,-11.4851678734925));
#28510=CARTESIAN_POINT('Ctrl Pts',(56.019812652493,4.23179766652216,-11.8577285498697));
#28511=CARTESIAN_POINT('Ctrl Pts',(55.0368711190457,4.16394895128873,-12.244451574114));
#28512=CARTESIAN_POINT('Ctrl Pts',(53.0324279581537,4.02139112324784,-12.8739714647708));
#28513=CARTESIAN_POINT('Ctrl Pts',(50.8522420828372,3.64495098639604,-13.1243776858381));
#28514=CARTESIAN_POINT('Ctrl Pts',(49.0742420084695,3.08805349273552,-13.0189954266342));
#28515=CARTESIAN_POINT('Ctrl Pts',(47.74311273162,2.65858895657289,-12.8839029021203));
#28516=CARTESIAN_POINT('Ctrl Pts',(46.0943092484674,2.06945988764268,-12.5441901629219));
#28517=CARTESIAN_POINT('Ctrl Pts',(43.9349361397835,1.53425192497824,-11.7148070258463));
#28518=CARTESIAN_POINT('Ctrl Pts',(42.7080397066157,1.37629460379916,-11.0306022357214));
#28519=CARTESIAN_POINT('Ctrl Pts',(41.8420335216443,1.28598589888282,-10.4618812091461));
#28520=CARTESIAN_POINT('Ctrl Pts',(41.2944047225801,1.23959147323119,-10.0745090823477));
#28521=CARTESIAN_POINT('Ctrl Pts',(39.9171313864447,1.1643772887167,-8.95351967626449));
#28522=CARTESIAN_POINT('Ctrl Pts',(38.9330416908621,1.13877908473415,-7.87506366436157));
#28523=CARTESIAN_POINT('Ctrl Pts',(38.2828091153483,1.11761889124797,-6.97607757441134));
#28524=CARTESIAN_POINT('',(41.6354952640144,0.318620154457148,-11.5338206587945));
#28525=CARTESIAN_POINT('Ctrl Pts',(37.5042795392924,0.118123058207621,-7.56121085790808));
#28526=CARTESIAN_POINT('Ctrl Pts',(38.2001384150095,0.139327569664645,-8.52006720115489));
#28527=CARTESIAN_POINT('Ctrl Pts',(39.2501325334149,0.164878829687915,-9.66995835627672));
#28528=CARTESIAN_POINT('Ctrl Pts',(40.7352207990105,0.240760335453449,-10.8928448336842));
#28529=CARTESIAN_POINT('Ctrl Pts',(41.3297202060976,0.28858188757864,-11.3324889652665));
#28530=CARTESIAN_POINT('Ctrl Pts',(41.6342353020102,0.318400150449319,-11.5329923830209));
#28531=CARTESIAN_POINT('',(58.6306321623861,3.50423391942768,-12.126881567578));
#28532=CARTESIAN_POINT('Ctrl Pts',(41.6354952640144,0.318620154457148,-11.5338206587945));
#28533=CARTESIAN_POINT('Ctrl Pts',(41.6362878084932,0.318697950647469,-11.5343425540537));
#28534=CARTESIAN_POINT('Ctrl Pts',(41.6370804004481,0.318775798580112,-11.5348645371535));
#28535=CARTESIAN_POINT('Ctrl Pts',(41.6378730398733,0.318853698316649,-11.535386607734));
#28536=CARTESIAN_POINT('Ctrl Pts',(41.6805430916827,0.323047264379738,-11.5634911632345));
#28537=CARTESIAN_POINT('Ctrl Pts',(41.7233594774993,0.327272758560646,-11.5905980399423));
#28538=CARTESIAN_POINT('Ctrl Pts',(41.7663216672521,0.331560773468719,-11.617196229109));
#28539=CARTESIAN_POINT('Ctrl Pts',(41.8237490958923,0.33729254998102,-11.6527499478352));
#28540=CARTESIAN_POINT('Ctrl Pts',(41.8814372382824,0.343135341510576,-11.6873965783807));
#28541=CARTESIAN_POINT('Ctrl Pts',(41.9393805747972,0.349184541000843,-11.7224062258384));
#28542=CARTESIAN_POINT('Ctrl Pts',(41.9484915860832,0.350135717238561,-11.7279111434405));
#28543=CARTESIAN_POINT('Ctrl Pts',(41.9576088967413,0.351092041842586,-11.7334251279012));
#28544=CARTESIAN_POINT('Ctrl Pts',(41.966732473864,0.352053933362217,-11.7389531680816));
#28545=CARTESIAN_POINT('Ctrl Pts',(42.0678457344272,0.36271422444658,-11.800218410832));
#28546=CARTESIAN_POINT('Ctrl Pts',(42.1697316625997,0.374060704226699,-11.8632120074282));
#28547=CARTESIAN_POINT('Ctrl Pts',(42.2723599254288,0.386135829849839,-11.9261906774715));
#28548=CARTESIAN_POINT('Ctrl Pts',(42.2821197317413,0.387284157649918,-11.9321798621707));
#28549=CARTESIAN_POINT('Ctrl Pts',(42.2918862233456,0.388439054026203,-11.9381689411694));
#28550=CARTESIAN_POINT('Ctrl Pts',(42.3016593559583,0.389600542077846,-11.9441564539643));
#28551=CARTESIAN_POINT('Ctrl Pts',(42.3936906818806,0.400538006007943,-12.0005394749798));
#28552=CARTESIAN_POINT('Ctrl Pts',(42.4863130122695,0.412061738656644,-12.0567865043064));
#28553=CARTESIAN_POINT('Ctrl Pts',(42.5794710623517,0.424232517306317,-12.1124724443935));
#28554=CARTESIAN_POINT('Ctrl Pts',(42.616739429467,0.429101501214791,-12.1347498971364));
#28555=CARTESIAN_POINT('Ctrl Pts',(42.6540932478344,0.434073788916218,-12.1569371588301));
#28556=CARTESIAN_POINT('Ctrl Pts',(42.6915278434756,0.439152057304701,-12.1790052390936));
#28557=CARTESIAN_POINT('Ctrl Pts',(42.7750031529593,0.450476075051076,-12.2282147950712));
#28558=CARTESIAN_POINT('Ctrl Pts',(42.8588810395273,0.462329209534337,-12.2768344282141));
#28559=CARTESIAN_POINT('Ctrl Pts',(42.9430983303904,0.474720322453312,-12.3245056174194));
#28560=CARTESIAN_POINT('Ctrl Pts',(42.9739518538696,0.479259883028827,-12.3419702513485));
#28561=CARTESIAN_POINT('Ctrl Pts',(43.0048507962696,0.483871351127161,-12.3593072142871));
#28562=CARTESIAN_POINT('Ctrl Pts',(43.0357916073031,0.48855404931147,-12.3764975648787));
#28563=CARTESIAN_POINT('Ctrl Pts',(43.0688709401821,0.49356039939852,-12.394876053048));
#28564=CARTESIAN_POINT('Ctrl Pts',(43.1019981319312,0.498648178118461,-12.413086934805));
#28565=CARTESIAN_POINT('Ctrl Pts',(43.1351685474621,0.503815669246779,-12.4311044326627));
#28566=CARTESIAN_POINT('Ctrl Pts',(43.2619434026418,0.523565435083243,-12.4999659662025));
#28567=CARTESIAN_POINT('Ctrl Pts',(43.3894520501079,0.544650665563608,-12.5675782480188));
#28568=CARTESIAN_POINT('Ctrl Pts',(43.517587224881,0.567178250965569,-12.6339106825963));
#28569=CARTESIAN_POINT('Ctrl Pts',(43.5580986076791,0.574300601540666,-12.6548824310164));
#28570=CARTESIAN_POINT('Ctrl Pts',(43.5986725234741,0.581566783988415,-12.6757260768497));
#28571=CARTESIAN_POINT('Ctrl Pts',(43.639305355365,0.588979215694766,-12.6964402253611));
#28572=CARTESIAN_POINT('Ctrl Pts',(43.770820391591,0.612970805230051,-12.7634850722274));
#28573=CARTESIAN_POINT('Ctrl Pts',(43.902951595011,0.63849760106563,-12.8291686268927));
#28574=CARTESIAN_POINT('Ctrl Pts',(44.0355913256016,0.665605135682187,-12.8934021229607));
#28575=CARTESIAN_POINT('Ctrl Pts',(44.170902783624,0.693258690284793,-12.9589294575546));
#28576=CARTESIAN_POINT('Ctrl Pts',(44.3067430280389,0.722557229868377,-13.0229470822634));
#28577=CARTESIAN_POINT('Ctrl Pts',(44.442994733047,0.753494258239274,-13.0853521869752));
#28578=CARTESIAN_POINT('Ctrl Pts',(44.5847248842449,0.785675211192184,-13.1502664933744));
#28579=CARTESIAN_POINT('Ctrl Pts',(44.7268998030087,0.819628907971195,-13.2134353747213));
#28580=CARTESIAN_POINT('Ctrl Pts',(44.869391068584,0.855290801050117,-13.2747439186379));
#28581=CARTESIAN_POINT('Ctrl Pts',(44.9602833090406,0.878038787375999,-13.313851374756));
#28582=CARTESIAN_POINT('Ctrl Pts',(45.0513043719664,0.901480660320446,-13.3522019415445));
#28583=CARTESIAN_POINT('Ctrl Pts',(45.1424228228309,0.925589006286844,-13.3897675411456));
#28584=CARTESIAN_POINT('Ctrl Pts',(45.2989388033037,0.967000393011594,-13.4542947208534));
#28585=CARTESIAN_POINT('Ctrl Pts',(45.4557410008675,1.01038049562556,-13.5165049785781));
#28586=CARTESIAN_POINT('Ctrl Pts',(45.6126867596284,1.05554311938658,-13.5762731041656));
#28587=CARTESIAN_POINT('Ctrl Pts',(45.634793280895,1.06190447958204,-13.5846917154731));
#28588=CARTESIAN_POINT('Ctrl Pts',(45.6569026820318,1.0683011314888,-13.5930619004269));
#28589=CARTESIAN_POINT('Ctrl Pts',(45.6790145959132,1.07473248690174,-13.6013833344557));
#28590=CARTESIAN_POINT('Ctrl Pts',(45.7022331439354,1.0814857121225,-13.6101212309873));
#28591=CARTESIAN_POINT('Ctrl Pts',(45.725454460823,1.08827720199514,-13.6188053740536));
#28592=CARTESIAN_POINT('Ctrl Pts',(45.7486783960119,1.09510594231381,-13.6274355210719));
#28593=CARTESIAN_POINT('Ctrl Pts',(45.8897873508652,1.1365974639485,-13.6798724149958));
#28594=CARTESIAN_POINT('Ctrl Pts',(46.0310824355953,1.17949718829418,-13.730358540107));
#28595=CARTESIAN_POINT('Ctrl Pts',(46.1724531782968,1.22353169119453,-13.7788017971356));
#28596=CARTESIAN_POINT('Ctrl Pts',(46.32153255783,1.26996729905082,-13.8298865588224));
#28597=CARTESIAN_POINT('Ctrl Pts',(46.470696032981,1.31766399879709,-13.8786996052067));
#28598=CARTESIAN_POINT('Ctrl Pts',(46.6198588270415,1.36626728785705,-13.925153963532));
#28599=CARTESIAN_POINT('Ctrl Pts',(46.7838432849947,1.41970007625068,-13.9762242912066));
#28600=CARTESIAN_POINT('Ctrl Pts',(46.9478267103645,1.4742275693381,-14.0244438551355));
#28601=CARTESIAN_POINT('Ctrl Pts',(47.111751758602,1.52935338987879,-14.0697223547562));
#28602=CARTESIAN_POINT('Ctrl Pts',(47.2839815191092,1.58727197505886,-14.1172947375594));
#28603=CARTESIAN_POINT('Ctrl Pts',(47.4561473004127,1.64584955469103,-14.1616207839425));
#28604=CARTESIAN_POINT('Ctrl Pts',(47.6282383345528,1.70450420101496,-14.202620250181));
#28605=CARTESIAN_POINT('Ctrl Pts',(47.8063777312818,1.76522034095631,-14.2450606958348));
#28606=CARTESIAN_POINT('Ctrl Pts',(47.9844378704465,1.8260174434581,-14.2839370275261));
#28607=CARTESIAN_POINT('Ctrl Pts',(48.1624546904282,1.88626804703706,-14.3191803292874));
#28608=CARTESIAN_POINT('Ctrl Pts',(48.2845509541258,1.92759208362686,-14.3433526264101));
#28609=CARTESIAN_POINT('Ctrl Pts',(48.4066278478853,1.96865945200782,-14.3658162976994));
#28610=CARTESIAN_POINT('Ctrl Pts',(48.5287060210717,2.00927801867859,-14.3865528070135));
#28611=CARTESIAN_POINT('Ctrl Pts',(48.5795058047287,2.02618042101204,-14.395181787604));
#28612=CARTESIAN_POINT('Ctrl Pts',(48.6303058803714,2.04300521698769,-14.4035117170511));
#28613=CARTESIAN_POINT('Ctrl Pts',(48.6811080503884,2.0597445246276,-14.411546778321));
#28614=CARTESIAN_POINT('Ctrl Pts',(48.7698851510948,2.08899656641255,-14.4255880966996));
#28615=CARTESIAN_POINT('Ctrl Pts',(48.8586361317935,2.11796377610708,-14.4387002156688));
#28616=CARTESIAN_POINT('Ctrl Pts',(48.9476431695491,2.14671805951331,-14.4509851041558));
#28617=CARTESIAN_POINT('Ctrl Pts',(49.1289020390981,2.20527487744969,-14.4760027326024));
#28618=CARTESIAN_POINT('Ctrl Pts',(49.3112299792474,2.26296695841828,-14.4976102350092));
#28619=CARTESIAN_POINT('Ctrl Pts',(49.494313376004,2.3190836575616,-14.5153939546957));
#28620=CARTESIAN_POINT('Ctrl Pts',(49.6708418613708,2.37319121771753,-14.5325409661456));
#28621=CARTESIAN_POINT('Ctrl Pts',(49.848074175385,2.42583287289,-14.5461339316348));
#28622=CARTESIAN_POINT('Ctrl Pts',(50.0257615281202,2.47639372396407,-14.5558261649752));
#28623=CARTESIAN_POINT('Ctrl Pts',(50.1942980989071,2.52435072441977,-14.5650192546652));
#28624=CARTESIAN_POINT('Ctrl Pts',(50.3630915255812,2.5704970187266,-14.5708751277587));
#28625=CARTESIAN_POINT('Ctrl Pts',(50.5321948117733,2.61460905768064,-14.5734097802231));
#28626=CARTESIAN_POINT('Ctrl Pts',(50.6971710074472,2.65764450976398,-14.5758825726232));
#28627=CARTESIAN_POINT('Ctrl Pts',(50.8624427189907,2.69874393343093,-14.5751944305834));
#28628=CARTESIAN_POINT('Ctrl Pts',(51.0280432903485,2.73774622267041,-14.57135806409));
#28629=CARTESIAN_POINT('Ctrl Pts',(51.1178357570973,2.75889416757757,-14.5692778972888));
#28630=CARTESIAN_POINT('Ctrl Pts',(51.2077245811264,2.77942633997864,-14.5662720832095));
#28631=CARTESIAN_POINT('Ctrl Pts',(51.2977121284949,2.7993227910621,-14.5623421493354));
#28632=CARTESIAN_POINT('Ctrl Pts',(51.476572612791,2.83886925032923,-14.5545309588261));
#28633=CARTESIAN_POINT('Ctrl Pts',(51.6558242884339,2.8759015177138,-14.5430693891014));
#28634=CARTESIAN_POINT('Ctrl Pts',(51.8353539157248,2.91049258394627,-14.5279826127422));
#28635=CARTESIAN_POINT('Ctrl Pts',(52.0277244870162,2.94755779303254,-14.5118167473585));
#28636=CARTESIAN_POINT('Ctrl Pts',(52.2204143047013,2.98182029930665,-14.4914887915954));
#28637=CARTESIAN_POINT('Ctrl Pts',(52.4132556251568,3.01342421633923,-14.4670192086256));
#28638=CARTESIAN_POINT('Ctrl Pts',(52.6151364581437,3.0465095793782,-14.4414026043567));
#28639=CARTESIAN_POINT('Ctrl Pts',(52.8171832798044,3.07668189726131,-14.4112472444537));
#28640=CARTESIAN_POINT('Ctrl Pts',(53.0191731687535,3.10415715631786,-14.3765615055575));
#28641=CARTESIAN_POINT('Ctrl Pts',(53.23945350474,3.13412033580066,-14.3387349279118));
#28642=CARTESIAN_POINT('Ctrl Pts',(53.4596662303745,3.16087663619287,-14.2955208513539));
#28643=CARTESIAN_POINT('Ctrl Pts',(53.6794860987647,3.18475461457528,-14.2469064357038));
#28644=CARTESIAN_POINT('Ctrl Pts',(53.8355717274022,3.20170944806556,-14.2123872101072));
#28645=CARTESIAN_POINT('Ctrl Pts',(53.9914584891298,3.2172141704109,-14.1751446872917));
#28646=CARTESIAN_POINT('Ctrl Pts',(54.1470201860804,3.23139546016389,-14.1351660195684));
#28647=CARTESIAN_POINT('Ctrl Pts',(54.237177508032,3.23961436707358,-14.1119959867918));
#28648=CARTESIAN_POINT('Ctrl Pts',(54.3272254441774,3.24738868938361,-14.0879067247933));
#28649=CARTESIAN_POINT('Ctrl Pts',(54.4171337810238,3.25474330129036,-14.0628870997708));
#28650=CARTESIAN_POINT('Ctrl Pts',(54.4848782213328,3.26028487935518,-14.0440352273712));
#28651=CARTESIAN_POINT('Ctrl Pts',(54.5525599073258,3.26558501280704,-14.0246434861282));
#28652=CARTESIAN_POINT('Ctrl Pts',(54.6201763752903,3.27066606446067,-14.00471935415));
#28653=CARTESIAN_POINT('Ctrl Pts',(54.8212606123777,3.28577657564425,-13.9454670891459));
#28654=CARTESIAN_POINT('Ctrl Pts',(55.0217685357112,3.29894547064154,-13.8815092378663));
#28655=CARTESIAN_POINT('Ctrl Pts',(55.2216267544097,3.31081104799838,-13.8129634769434));
#28656=CARTESIAN_POINT('Ctrl Pts',(55.406937860943,3.32181296367628,-13.7494069672962));
#28657=CARTESIAN_POINT('Ctrl Pts',(55.5916903573697,3.33169575577238,-13.6819049981657));
#28658=CARTESIAN_POINT('Ctrl Pts',(55.7758214214221,3.34100312231682,-13.6105321875762));
#28659=CARTESIAN_POINT('Ctrl Pts',(56.0257234664947,3.35363504809027,-13.5136652552054));
#28660=CARTESIAN_POINT('Ctrl Pts',(56.2744888438065,3.36519900722206,-13.4096494123916));
#28661=CARTESIAN_POINT('Ctrl Pts',(56.5208818625146,3.37649328426046,-13.298125861323));
#28662=CARTESIAN_POINT('Ctrl Pts',(56.5403976007538,3.37738785568719,-13.2892925573537));
#28663=CARTESIAN_POINT('Ctrl Pts',(56.5598984329187,3.37828073365513,-13.2804121394665));
#28664=CARTESIAN_POINT('Ctrl Pts',(56.5793837321424,3.37917231069026,-13.2714844240186));
#28665=CARTESIAN_POINT('Ctrl Pts',(56.7011413747803,3.38474350140081,-13.2156978756783));
#28666=CARTESIAN_POINT('Ctrl Pts',(56.8222678009723,3.39029559284719,-13.158134882614));
#28667=CARTESIAN_POINT('Ctrl Pts',(56.9427407283792,3.39596934234435,-13.0987731088611));
#28668=CARTESIAN_POINT('Ctrl Pts',(57.0022426840281,3.39877162496676,-13.069454143139));
#28669=CARTESIAN_POINT('Ctrl Pts',(57.0615852070991,3.40160350710119,-13.0396962421641));
#28670=CARTESIAN_POINT('Ctrl Pts',(57.1207634691196,3.40448790678842,-13.0095138025368));
#28671=CARTESIAN_POINT('Ctrl Pts',(57.2394457744615,3.41027258502532,-12.948982766418));
#28672=CARTESIAN_POINT('Ctrl Pts',(57.3574683316654,3.41626782467713,-12.8867410811329));
#28673=CARTESIAN_POINT('Ctrl Pts',(57.4747616997881,3.42264482405701,-12.8229308281502));
#28674=CARTESIAN_POINT('Ctrl Pts',(57.524842042396,3.42536758936647,-12.7956859857314));
#28675=CARTESIAN_POINT('Ctrl Pts',(57.5747892882394,3.42816006754099,-12.7681557937622));
#28676=CARTESIAN_POINT('Ctrl Pts',(57.6245972805189,3.43103602860081,-12.7403541019914));
#28677=CARTESIAN_POINT('Ctrl Pts',(57.6968840889615,3.43520993798171,-12.7000052448014));
#28678=CARTESIAN_POINT('Ctrl Pts',(57.768876811572,3.43957742139646,-12.6591218520253));
#28679=CARTESIAN_POINT('Ctrl Pts',(57.8405471761051,3.44417469677127,-12.6177486205741));
#28680=CARTESIAN_POINT('Ctrl Pts',(57.9103178844631,3.44865011923504,-12.5774720057666));
#28681=CARTESIAN_POINT('Ctrl Pts',(57.979782361742,3.45334489481511,-12.5367356281187));
#28682=CARTESIAN_POINT('Ctrl Pts',(58.0489530044697,3.45817075099943,-12.4952150159453));
#28683=CARTESIAN_POINT('Ctrl Pts',(58.1158780081092,3.46283993477397,-12.4550423789532));
#28684=CARTESIAN_POINT('Ctrl Pts',(58.1825279258874,3.46763181259156,-12.4141355213333));
#28685=CARTESIAN_POINT('Ctrl Pts',(58.2489206708859,3.47244908344074,-12.3721579743786));
#28686=CARTESIAN_POINT('Ctrl Pts',(58.2905482136799,3.47546946086947,-12.3458385002812));
#28687=CARTESIAN_POINT('Ctrl Pts',(58.3320756067246,3.47849784936122,-12.3190926740185));
#28688=CARTESIAN_POINT('Ctrl Pts',(58.3734322388319,3.4817278052044,-12.2924709828604));
#28689=CARTESIAN_POINT('Ctrl Pts',(58.3766957722737,3.48198268739313,-12.2903702126828));
#28690=CARTESIAN_POINT('Ctrl Pts',(58.3799582378835,3.48223883340623,-12.2882702406214));
#28691=CARTESIAN_POINT('Ctrl Pts',(58.3832195986403,3.48249634281616,-12.2861713501478));
#28692=CARTESIAN_POINT('Ctrl Pts',(58.4107742785886,3.48467199583441,-12.2684381830568));
#28693=CARTESIAN_POINT('Ctrl Pts',(58.4382726399568,3.48687721189157,-12.2505993231288));
#28694=CARTESIAN_POINT('Ctrl Pts',(58.4657016549427,3.48916124785644,-12.2327797434489));
#28695=CARTESIAN_POINT('Ctrl Pts',(58.492300617373,3.49137616468266,-12.2154994170984));
#28696=CARTESIAN_POINT('Ctrl Pts',(58.5188344931624,3.49366487702235,-12.1982362815353));
#28697=CARTESIAN_POINT('Ctrl Pts',(58.5452842975648,3.49609103963997,-12.1811518796883));
#28698=CARTESIAN_POINT('Ctrl Pts',(58.5688654567635,3.49825406988614,-12.165920387098));
#28699=CARTESIAN_POINT('Ctrl Pts',(58.5923797907988,3.5005263639239,-12.150830927202));
#28700=CARTESIAN_POINT('Ctrl Pts',(58.6158074637682,3.50296975356874,-12.1360415899455));
#28701=CARTESIAN_POINT('Ctrl Pts',(58.6186574373906,3.50326699162759,-12.1342424688323));
#28702=CARTESIAN_POINT('Ctrl Pts',(58.6215061199422,3.50356678411242,-12.1324478482872));
#28703=CARTESIAN_POINT('Ctrl Pts',(58.624353468298,3.5038692616587,-12.1306580639657));
#28704=CARTESIAN_POINT('Ctrl Pts',(58.6261974023257,3.50406514518629,-12.1294990051502));
#28705=CARTESIAN_POINT('Ctrl Pts',(58.6280412554071,3.50426063077623,-12.128338325465));
#28706=CARTESIAN_POINT('Ctrl Pts',(58.6298850303881,3.50445571262044,-12.1271760060145));
#28707=CARTESIAN_POINT('',(64.2981106326832,3.0811123562608,-5.85555843435015));
#28708=CARTESIAN_POINT('Ctrl Pts',(58.6309985074851,3.50412516642371,-12.1267371940558));
#28709=CARTESIAN_POINT('Ctrl Pts',(59.3307183820628,3.57738713031641,-11.6860335001487));
#28710=CARTESIAN_POINT('Ctrl Pts',(60.517944889496,3.73981722935225,-10.8310066664578));
#28711=CARTESIAN_POINT('Ctrl Pts',(61.9030047025891,3.76645360291022,-9.51895198440983));
#28712=CARTESIAN_POINT('Ctrl Pts',(63.1474965884414,3.51873308138032,-7.98696741401787));
#28713=CARTESIAN_POINT('Ctrl Pts',(63.8841059835174,3.19246873749153,-6.72699339972162));
#28714=CARTESIAN_POINT('Ctrl Pts',(64.2977768285069,3.08120206602316,-5.85626119470832));
#28715=CARTESIAN_POINT('',(65.9408742037128,3.18204282773931,0.563892468411459));
#28716=CARTESIAN_POINT('Ctrl Pts',(64.2990162441269,3.08086897348378,-5.8536518439966));
#28717=CARTESIAN_POINT('Ctrl Pts',(64.6116198958172,2.99692695046148,-5.19539506303037));
#28718=CARTESIAN_POINT('Ctrl Pts',(65.2801899672622,2.94481025351616,-3.5511642822986));
#28719=CARTESIAN_POINT('Ctrl Pts',(65.7244715160515,3.1204547806088,-1.64454837118901));
#28720=CARTESIAN_POINT('Ctrl Pts',(65.8904051975644,3.18227049415762,-0.202227005722761));
#28721=CARTESIAN_POINT('Ctrl Pts',(65.9273187549476,3.18706519524341,0.294007279412763));
#28722=CARTESIAN_POINT('Ctrl Pts',(65.9407606432144,3.18152655267827,0.560435122518436));
#28723=CARTESIAN_POINT('',(65.1820057808194,3.08346314704612,6.62245362259951));
#28724=CARTESIAN_POINT('Ctrl Pts',(65.9410186585186,3.18269955622032,0.568290390542557));
#28725=CARTESIAN_POINT('Ctrl Pts',(65.9482910538458,3.17968929367419,0.713809495459604));
#28726=CARTESIAN_POINT('Ctrl Pts',(65.9538461064654,3.17693067006538,0.860231473819412));
#28727=CARTESIAN_POINT('Ctrl Pts',(65.9576971484804,3.17445963453872,1.00728204069835));
#28728=CARTESIAN_POINT('Ctrl Pts',(65.9616531303433,3.17192126396582,1.15833969554288));
#28729=CARTESIAN_POINT('Ctrl Pts',(65.9638107706592,3.1696861756633,1.31006037972726));
#28730=CARTESIAN_POINT('Ctrl Pts',(65.9641614268585,3.1677446692947,1.46216354030635));
#28731=CARTESIAN_POINT('Ctrl Pts',(65.9645256747771,3.16572790856114,1.62016234302247));
#28732=CARTESIAN_POINT('Ctrl Pts',(65.9629399442982,3.16402755556653,1.77857356369251));
#28733=CARTESIAN_POINT('Ctrl Pts',(65.9593729998557,3.16258514975214,1.93710510064369));
#28734=CARTESIAN_POINT('Ctrl Pts',(65.9554990511008,3.16101859711898,2.10928133161282));
#28735=CARTESIAN_POINT('Ctrl Pts',(65.949288022404,3.15975582648078,2.28159897580233));
#28736=CARTESIAN_POINT('Ctrl Pts',(65.9406774857124,3.15867302061577,2.45371636122117));
#28737=CARTESIAN_POINT('Ctrl Pts',(65.9315288686373,3.15752254921307,2.63658952088078));
#28738=CARTESIAN_POINT('Ctrl Pts',(65.9196710752013,3.15657393498886,2.81923624761305));
#28739=CARTESIAN_POINT('Ctrl Pts',(65.9050093929959,3.15564006925673,3.00128898965019));
#28740=CARTESIAN_POINT('Ctrl Pts',(65.8893468159611,3.15464245221901,3.19576974954009));
#28741=CARTESIAN_POINT('Ctrl Pts',(65.8704837728399,3.15365958243021,3.38957235660907));
#28742=CARTESIAN_POINT('Ctrl Pts',(65.8482914544987,3.15244777519672,3.58230111020626));
#28743=CARTESIAN_POINT('Ctrl Pts',(65.8465233851039,3.15235123011075,3.59765587420649));
#28744=CARTESIAN_POINT('Ctrl Pts',(65.8447341805535,3.15225323446883,3.61300384904705));
#28745=CARTESIAN_POINT('Ctrl Pts',(65.8429237746156,3.15215366756841,3.6283448484288));
#28746=CARTESIAN_POINT('Ctrl Pts',(65.8267524394948,3.15126429260558,3.76537734312529));
#28747=CARTESIAN_POINT('Ctrl Pts',(65.8088894100432,3.150249141841,3.90185211718944));
#28748=CARTESIAN_POINT('Ctrl Pts',(65.7892859174208,3.14902631932301,4.03765352495476));
#28749=CARTESIAN_POINT('Ctrl Pts',(65.7625155923028,3.14735644564292,4.2231025113866));
#28750=CARTESIAN_POINT('Ctrl Pts',(65.7326172305382,3.14530962026868,4.4073328552257));
#28751=CARTESIAN_POINT('Ctrl Pts',(65.6994834206641,3.14270630129762,4.59044913856515));
#28752=CARTESIAN_POINT('Ctrl Pts',(65.6665345207502,3.14011751067718,4.77254350426792));
#28753=CARTESIAN_POINT('Ctrl Pts',(65.6303858121898,3.13697775158381,4.95353676926838));
#28754=CARTESIAN_POINT('Ctrl Pts',(65.5909440728671,3.1331492459991,5.13356289950103));
#28755=CARTESIAN_POINT('Ctrl Pts',(65.5796974902167,3.13205756989086,5.18489630385011));
#28756=CARTESIAN_POINT('Ctrl Pts',(65.5681832582793,3.13091016593668,5.23615126812696));
#28757=CARTESIAN_POINT('Ctrl Pts',(65.5563993018479,3.12970444792706,5.28733236991622));
#28758=CARTESIAN_POINT('Ctrl Pts',(65.5191527539497,3.12589343302229,5.449104807754));
#28759=CARTESIAN_POINT('Ctrl Pts',(65.4792102515102,3.12149696871513,5.61014156713253));
#28760=CARTESIAN_POINT('Ctrl Pts',(65.4365166245822,3.11646139895575,5.77056709721706));
#28761=CARTESIAN_POINT('Ctrl Pts',(65.4268592190441,3.1153223404409,5.80685575466259));
#28762=CARTESIAN_POINT('Ctrl Pts',(65.4170611155533,3.11415073489286,5.84311301303454));
#28763=CARTESIAN_POINT('Ctrl Pts',(65.4071218074921,3.11294623328413,5.87934008699024));
#28764=CARTESIAN_POINT('Ctrl Pts',(65.3803078629663,3.10969676771581,5.9770723179869));
#28765=CARTESIAN_POINT('Ctrl Pts',(65.3524660048671,3.10620755069197,6.07458048656183));
#28766=CARTESIAN_POINT('Ctrl Pts',(65.3235898025028,3.10247597339671,6.17180190452008));
#28767=CARTESIAN_POINT('Ctrl Pts',(65.3157399434555,3.10146156175691,6.19823108719857));
#28768=CARTESIAN_POINT('Ctrl Pts',(65.3078136652226,3.10042926681887,6.22463937508606));
#28769=CARTESIAN_POINT('Ctrl Pts',(65.2998108818847,3.09937909657588,6.25102616952741));
#28770=CARTESIAN_POINT('Ctrl Pts',(65.2810472815969,3.09691683140615,6.31289355277077));
#28771=CARTESIAN_POINT('Ctrl Pts',(65.2618630666386,3.09435625429473,6.37464772926933));
#28772=CARTESIAN_POINT('Ctrl Pts',(65.2422565977204,3.09169651310013,6.43643476558113));
#28773=CARTESIAN_POINT('Ctrl Pts',(65.2226501288021,3.08903677190554,6.49822180189292));
#28774=CARTESIAN_POINT('Ctrl Pts',(65.2026214010512,3.08627786254871,6.56004163681742));
#28775=CARTESIAN_POINT('Ctrl Pts',(65.1821694348226,3.08341966011011,6.62198291902686));
#28776=CARTESIAN_POINT('',(61.488060455579,2.54023853025181,12.6451667603895));
#28777=CARTESIAN_POINT('Ctrl Pts',(65.1820057808194,3.08346314704612,6.62245362259951));
#28778=CARTESIAN_POINT('Ctrl Pts',(64.4364313250544,2.978243913911,8.88068192566307));
#28779=CARTESIAN_POINT('Ctrl Pts',(63.1655278864518,2.76702770395235,10.9465222144682));
#28780=CARTESIAN_POINT('Ctrl Pts',(61.4888775365941,2.54034899309264,12.6443394503259));
#28781=CARTESIAN_POINT('',(39.0575084607384,0.182814626998845,12.6499766640859));
#28782=CARTESIAN_POINT('Ctrl Pts',(61.4877351764846,2.54019455511082,12.6454961116574));
#28783=CARTESIAN_POINT('Ctrl Pts',(61.1207173898856,2.49057863416769,13.0170698848163));
#28784=CARTESIAN_POINT('Ctrl Pts',(58.0875609241164,2.07105403856995,15.8393411259143));
#28785=CARTESIAN_POINT('Ctrl Pts',(49.8202147709309,0.844782240165095,18.8003653400802));
#28786=CARTESIAN_POINT('Ctrl Pts',(41.9948217404251,0.31563552772145,15.6461834941947));
#28787=CARTESIAN_POINT('Ctrl Pts',(39.0575084607384,0.182814626998845,12.6499766640859));
#28788=CARTESIAN_POINT('',(35.3362746312916,0.0544533848017485,6.63054475574935));
#28789=CARTESIAN_POINT('Ctrl Pts',(39.0562952757742,0.182759773910686,12.6487390081575));
#28790=CARTESIAN_POINT('Ctrl Pts',(37.384582188262,0.10718206711949,10.9431042532932));
#28791=CARTESIAN_POINT('Ctrl Pts',(36.0966585928923,0.0727769246540845,
8.89369604654459));
#28792=CARTESIAN_POINT('Ctrl Pts',(35.3362746312916,0.0544533848017485,
6.63054475574935));
#28793=CARTESIAN_POINT('',(34.5486968133484,0.0370407268214907,0.611571110133481));
#28794=CARTESIAN_POINT('Ctrl Pts',(35.3362641803865,0.0544531329586211,
6.63051365033307));
#28795=CARTESIAN_POINT('Ctrl Pts',(34.6842831176538,0.0387418751808522,
4.68999164416651));
#28796=CARTESIAN_POINT('Ctrl Pts',(34.4147629385807,0.0337921773623382,
2.65381724310736));
#28797=CARTESIAN_POINT('Ctrl Pts',(34.5486787314775,0.0370402882573318,
0.611846760577837));
#28798=CARTESIAN_POINT('',(36.1904970298096,0.0789173535423179,-5.40625271964083));
#28799=CARTESIAN_POINT('Ctrl Pts',(34.548710378627,0.0370410558386067,0.611364313220442));
#28800=CARTESIAN_POINT('Ctrl Pts',(34.6864441828166,0.0403816294309185,
-1.48783449464834));
#28801=CARTESIAN_POINT('Ctrl Pts',(35.2437959696896,0.0529688610259415,
-3.52821928318576));
#28802=CARTESIAN_POINT('Ctrl Pts',(36.1903620723292,0.0789136543077262,
-5.40598500767172));
#28803=CARTESIAN_POINT('Ctrl Pts',(36.1906166903305,0.0789206334815761,
-5.40649008739235));
#28804=CARTESIAN_POINT('Ctrl Pts',(36.5716643422744,0.089365667141814,-6.1623311541711));
#28805=CARTESIAN_POINT('Ctrl Pts',(37.0128131431011,0.103146882444921,-6.88399642848073));
#28806=CARTESIAN_POINT('Ctrl Pts',(37.5042795392924,0.118123058207631,-7.56121085790809));
#28807=CARTESIAN_POINT('Origin',(50.184,-32.64,1.632));
#28808=CARTESIAN_POINT('',(35.4961269461781,3.11629570184638,1.63325416304923));
#28809=CARTESIAN_POINT('',(35.496,-32.64,1.632));
#28810=CARTESIAN_POINT('',(45.4957186312967,4.13505468146236,-12.2876753485083));
#28811=CARTESIAN_POINT('Ctrl Pts',(45.4957186312967,4.13505468146236,-12.2876753485083));
#28812=CARTESIAN_POINT('Ctrl Pts',(46.5747881377784,4.51315986439798,-12.6511164012708));
#28813=CARTESIAN_POINT('Ctrl Pts',(48.7315111185874,5.55100447935154,-13.1127068857499));
#28814=CARTESIAN_POINT('Ctrl Pts',(52.2255324170519,6.61037667463491,-13.0603457351622));
#28815=CARTESIAN_POINT('Ctrl Pts',(55.7352401406832,6.78357937642121,-12.1273823391115));
#28816=CARTESIAN_POINT('Ctrl Pts',(57.8454449537772,6.76763575867449,-10.9565650346632));
#28817=CARTESIAN_POINT('Ctrl Pts',(58.9417818399741,6.90315486069136,-10.1604688849966));
#28818=CARTESIAN_POINT('Ctrl Pts',(59.1869377879013,6.93283823797164,-9.9764403477307));
#28819=CARTESIAN_POINT('Ctrl Pts',(59.6656000071998,6.98501272405032,-9.59287808094242));
#28820=CARTESIAN_POINT('Ctrl Pts',(60.4698386743377,7.03851518962114,-8.88527771072978));
#28821=CARTESIAN_POINT('Ctrl Pts',(61.935425590422,6.93159705832345,-7.32309238219473));
#28822=CARTESIAN_POINT('Ctrl Pts',(62.898870223949,6.33243798646893,-5.81981710521227));
#28823=CARTESIAN_POINT('Ctrl Pts',(63.6271064539284,6.1172012971021,-4.30394126827215));
#28824=CARTESIAN_POINT('Ctrl Pts',(63.9964631920437,6.08157109535702,-3.43096909542246));
#28825=CARTESIAN_POINT('Ctrl Pts',(64.4196909334568,6.16095583450854,-2.0750183342162));
#28826=CARTESIAN_POINT('Ctrl Pts',(64.7075353735302,6.25611577526355,-0.705188274299797));
#28827=CARTESIAN_POINT('Ctrl Pts',(64.8131179042321,6.27855936375402,0.234551382385882));
#28828=CARTESIAN_POINT('Ctrl Pts',(64.8578334301675,6.26126913644566,0.94307726867782));
#28829=CARTESIAN_POINT('Ctrl Pts',(64.8763131687878,6.25212971761612,1.41873044327074));
#28830=CARTESIAN_POINT('Ctrl Pts',(64.8669425474595,6.24148249015893,2.37159989960793));
#28831=CARTESIAN_POINT('Ctrl Pts',(64.7293383040315,6.23744524570034,4.02825143678288));
#28832=CARTESIAN_POINT('Ctrl Pts',(64.4090264396697,6.21556997011337,5.41180556034465));
#28833=CARTESIAN_POINT('Ctrl Pts',(63.392616944205,6.06901676370829,8.4362633730038));
#28834=CARTESIAN_POINT('Ctrl Pts',(62.2029128798603,5.85755777132363,10.3600282958658));
#28835=CARTESIAN_POINT('Ctrl Pts',(57.9137758164067,5.23547967962912,14.7285512014021));
#28836=CARTESIAN_POINT('Ctrl Pts',(50.2340493278717,3.97178337193033,17.9121952059345));
#28837=CARTESIAN_POINT('Ctrl Pts',(42.4627846177445,3.39626629188669,14.7465965189029));
#28838=CARTESIAN_POINT('Ctrl Pts',(38.1616839203783,3.18800029201627,10.3559731559896));
#28839=CARTESIAN_POINT('Ctrl Pts',(36.9711393616719,3.15313406811575,8.42495263430108));
#28840=CARTESIAN_POINT('Ctrl Pts',(35.7546310141604,3.1216063944377,4.80652569193013));
#28841=CARTESIAN_POINT('Ctrl Pts',(35.4967618613831,3.11596821566591,3.22213036278666));
#28842=CARTESIAN_POINT('Ctrl Pts',(35.4961269461781,3.11629570184638,1.63325416304923));
#28843=CARTESIAN_POINT('Ctrl Pts',(35.4961269461781,3.11629570184638,1.63325416304923));
#28844=CARTESIAN_POINT('Ctrl Pts',(35.4959999928206,3.11636118377183,1.31555320625316));
#28845=CARTESIAN_POINT('Ctrl Pts',(35.5061575990416,3.11666518074569,0.997673098419422));
#28846=CARTESIAN_POINT('Ctrl Pts',(35.6531385708734,3.12046556629585,-1.27776505111417));
#28847=CARTESIAN_POINT('Ctrl Pts',(36.175035699066,3.13335329444264,-3.19875344300605));
#28848=CARTESIAN_POINT('Ctrl Pts',(37.619750560802,3.17534463244499,-6.07811908458911));
#28849=CARTESIAN_POINT('Ctrl Pts',(39.0211463611516,3.22647042745986,-8.16085205297379));
#28850=CARTESIAN_POINT('Ctrl Pts',(40.9332506662835,3.2798490343456,-9.84541367809451));
#28851=CARTESIAN_POINT('Ctrl Pts',(42.2378053070641,3.41504440953276,-10.725652165237));
#28852=CARTESIAN_POINT('Ctrl Pts',(42.8038448826665,3.4807437957151,-11.0806258189848));
#28853=CARTESIAN_POINT('Ctrl Pts',(43.981345015687,3.67284868940879,-11.7113672365034));
#28854=CARTESIAN_POINT('Ctrl Pts',(44.8918845743013,3.92347165996875,-12.0842981943491));
#28855=CARTESIAN_POINT('Ctrl Pts',(45.4957186312967,4.13505468146236,-12.2876753485083));
#28856=CARTESIAN_POINT('Ctrl Pts',(-79.0674188627527,5.01522288740334,24.8190563538896));
#28857=CARTESIAN_POINT('Ctrl Pts',(-79.0681685301284,5.01561150558399,24.7698112319613));
#28858=CARTESIAN_POINT('Ctrl Pts',(-79.0689540583035,5.01601910927839,24.720540203059));
#28859=CARTESIAN_POINT('Ctrl Pts',(-79.0782218386017,5.02082390331305,24.1661600265106));
#28860=CARTESIAN_POINT('Ctrl Pts',(-79.0927115085079,5.02499992560426,23.175201774565));
#28861=CARTESIAN_POINT('Ctrl Pts',(-79.1310390764956,5.03563895843973,21.1518987112308));
#28862=CARTESIAN_POINT('Ctrl Pts',(-79.1918027806567,5.0685749771201,19.6199982936506));
#28863=CARTESIAN_POINT('Ctrl Pts',(-79.2833423745251,5.13810264877128,18.333204648019));
#28864=CARTESIAN_POINT('Ctrl Pts',(-79.3271997238556,5.16402211160836,17.8495119052833));
#28865=CARTESIAN_POINT('Ctrl Pts',(-79.4350333727236,5.21929371286925,16.8471015925371));
#28866=CARTESIAN_POINT('Ctrl Pts',(-79.6597754282508,5.33693138686091,15.0668568651258));
#28867=CARTESIAN_POINT('Ctrl Pts',(-79.8528862432256,5.52342881968698,13.4624410469408));
#28868=CARTESIAN_POINT('Ctrl Pts',(-79.9478677581679,5.77956933135521,12.0840553347989));
#28869=CARTESIAN_POINT('Ctrl Pts',(-79.987251247416,5.88971937931585,11.5496610322703));
#28870=CARTESIAN_POINT('Ctrl Pts',(-80.0644593134605,6.14288539486632,10.4849494061586));
#28871=CARTESIAN_POINT('Ctrl Pts',(-80.1868754301937,6.65297538854495,8.65255241882749));
#28872=CARTESIAN_POINT('Ctrl Pts',(-80.2380448998663,7.15195302098414,7.11347352122868));
#28873=CARTESIAN_POINT('Ctrl Pts',(-80.2204406795539,7.50474337783514,5.96584700843978));
#28874=CARTESIAN_POINT('Ctrl Pts',(-80.2096612212723,7.59336289588965,5.67864593273452));
#28875=CARTESIAN_POINT('Ctrl Pts',(-80.1847401855017,7.77374083996654,5.13331455388711));
#28876=CARTESIAN_POINT('Ctrl Pts',(-80.1261994373432,8.1062734462045,4.1910399007512));
#28877=CARTESIAN_POINT('Ctrl Pts',(-79.9741038356724,8.78915237629665,2.39877332558468));
#28878=CARTESIAN_POINT('Ctrl Pts',(-79.83947806308,9.27574137610065,0.998413592090816));
#28879=CARTESIAN_POINT('Ctrl Pts',(-79.7762751651938,9.47255640374571,0.106471325025258));
#28880=CARTESIAN_POINT('Ctrl Pts',(-79.7671955870895,9.49782362033992,-0.0121281782206109));
#28881=CARTESIAN_POINT('Ctrl Pts',(-79.7492052491573,9.54450055919095,-0.242617706451281));
#28882=CARTESIAN_POINT('Ctrl Pts',(-79.7157711688734,9.62061509733319,-0.650089358255339));
#28883=CARTESIAN_POINT('Ctrl Pts',(-79.6641805384973,9.71223607414345,-1.23187966460342));
#28884=CARTESIAN_POINT('Ctrl Pts',(-79.596965198778,9.79990417771364,-1.93470237003412));
#28885=CARTESIAN_POINT('Ctrl Pts',(-79.502992870302,9.89209711001119,-2.87653830176489));
#28886=CARTESIAN_POINT('Ctrl Pts',(-79.3825611224459,9.97162253608378,-4.06583643950883));
#28887=CARTESIAN_POINT('Ctrl Pts',(-79.2987282925754,10.0151797765619,-5.03298138339086));
#28888=CARTESIAN_POINT('Ctrl Pts',(-79.2557159682984,10.0403140537843,-5.64265285224522));
#28889=CARTESIAN_POINT('Ctrl Pts',(-79.2392565381024,10.0469385074052,-5.86265283336235));
#28890=CARTESIAN_POINT('Ctrl Pts',(-79.2076279337785,10.0536787811717,-6.32229182536503));
#28891=CARTESIAN_POINT('Ctrl Pts',(-79.1565003952743,10.0478001857035,-7.13344029341454));
#28892=CARTESIAN_POINT('Ctrl Pts',(-79.0957089826259,10.0015429336662,-8.33665236197077));
#28893=CARTESIAN_POINT('Ctrl Pts',(-79.0509111925855,9.93743960636052,-9.58843110743809));
#28894=CARTESIAN_POINT('Ctrl Pts',(-79.0268836059977,9.90337528247544,-10.4912277578721));
#28895=CARTESIAN_POINT('Ctrl Pts',(-79.0150770197293,9.89016083945574,-11.0141122843214));
#28896=CARTESIAN_POINT('Ctrl Pts',(-79.0097812960411,9.88618631938345,-11.2780557265188));
#28897=CARTESIAN_POINT('Ctrl Pts',(-79.006009248494,9.88440003313119,-11.477499488386));
#28898=CARTESIAN_POINT('Ctrl Pts',(-79.0036660448527,9.88335825035133,-11.6033946515416));
#28899=CARTESIAN_POINT('Ctrl Pts',(-78.9997418352511,9.88164895132235,-11.8592855042488));
#28900=CARTESIAN_POINT('Ctrl Pts',(-78.9947630668099,9.87966515108148,-12.3037147121711));
#28901=CARTESIAN_POINT('Ctrl Pts',(-78.9906403941104,9.87901424697721,-13.4432992984675));
#28902=CARTESIAN_POINT('Ctrl Pts',(-79.0055407029075,9.88809071261166,-14.6957989450663));
#28903=CARTESIAN_POINT('Ctrl Pts',(-79.0211143843459,9.89743215908292,-15.9454740463632));
#28904=CARTESIAN_POINT('Ctrl Pts',(-79.0275077450161,9.90133084380334,-16.5699512235593));
#28905=CARTESIAN_POINT('Ctrl Pts',(-79.0308484282295,9.90348313569322,-17.0700172931005));
#28906=CARTESIAN_POINT('Ctrl Pts',(-79.0317719310497,9.90415043469421,-17.3202164975421));
#28907=CARTESIAN_POINT('Ctrl Pts',(-79.0321242967022,9.9044653528448,-17.5072310514656));
#28908=CARTESIAN_POINT('Ctrl Pts',(-79.0323391539848,9.90466318448756,-17.6318736318689));
#28909=CARTESIAN_POINT('Ctrl Pts',(-79.0327007960053,9.90501350062777,-17.8806948619788));
#28910=CARTESIAN_POINT('Ctrl Pts',(-79.0329656912022,9.90529980852707,-18.1298687447505));
#28911=CARTESIAN_POINT('Ctrl Pts',(-79.0331441220501,9.90552904669751,-18.3791056565332));
#28912=CARTESIAN_POINT('Ctrl Pts',(-79.0332219147693,9.90564971859517,-18.5349686127661));
#28913=CARTESIAN_POINT('Ctrl Pts',(-79.0332651945694,9.90573358901976,-18.6596927977821));
#28914=CARTESIAN_POINT('Ctrl Pts',(-79.0332962921471,9.90580926151893,-18.784447455142));
#28915=CARTESIAN_POINT('Ctrl Pts',(-79.0333334879728,9.90598436409335,-19.1276271558624));
#28916=CARTESIAN_POINT('Ctrl Pts',(-79.033150149307,9.90610435638902,-19.6898219898101));
#28917=CARTESIAN_POINT('Ctrl Pts',(-79.0323557181868,9.90598203971701,-20.6911245536626));
#28918=CARTESIAN_POINT('Ctrl Pts',(-79.0309067855052,9.90546320762363,-21.9464416288123));
#28919=CARTESIAN_POINT('Ctrl Pts',(-79.0301647578065,9.90521322820462,-22.9549301708349));
#28920=CARTESIAN_POINT('Ctrl Pts',(-79.0301129783275,9.90528407108641,-23.5849311303309));
#28921=CARTESIAN_POINT('Ctrl Pts',(-79.0301033887371,9.90531333336311,-23.8340998786223));
#28922=CARTESIAN_POINT('Ctrl Pts',(-79.0301224332957,9.90537495702407,-24.3333441865812));
#28923=CARTESIAN_POINT('Ctrl Pts',(-79.0302414377352,9.90548775645281,-25.2087899694315));
#28924=CARTESIAN_POINT('Ctrl Pts',(-79.0305728693895,9.90564301980743,-26.4634885419102));
#28925=CARTESIAN_POINT('Ctrl Pts',(-79.0309607127377,9.90576143657678,-27.9717423759188));
#28926=CARTESIAN_POINT('Ctrl Pts',(-79.0310348337779,9.90575248186518,-28.9764101349217));
#28927=CARTESIAN_POINT('Ctrl Pts',(-79.030974280901,9.90571219648468,-29.5405779895657));
#28928=CARTESIAN_POINT('Ctrl Pts',(-79.0309568887622,9.90570176770536,-29.6659328550826));
#28929=CARTESIAN_POINT('Ctrl Pts',(-79.0309075280054,9.90567508984067,-29.9167097800688));
#28930=CARTESIAN_POINT('Ctrl Pts',(-79.0307858008553,9.90561395783502,-30.3557101965222));
#28931=CARTESIAN_POINT('Ctrl Pts',(-79.0304240360459,9.90544214485433,-31.2341706185155));
#28932=CARTESIAN_POINT('Ctrl Pts',(-79.0298462642804,9.9051666773888,-32.2385881451622));
#28933=CARTESIAN_POINT('Ctrl Pts',(-79.0293158017111,9.90488352664045,-33.2423420548747));
#28934=CARTESIAN_POINT('Ctrl Pts',(-79.0289945391947,9.90468490150068,-33.9945417552978));
#28935=CARTESIAN_POINT('Ctrl Pts',(-79.0288029824139,9.90451656743563,-34.7458244521028));
#28936=CARTESIAN_POINT('Ctrl Pts',(-79.0287969944716,9.9044364311933,-35.2458865326991));
#28937=CARTESIAN_POINT('Ctrl Pts',(-79.0288514758595,9.90439296894784,-35.621556386843));
#28938=CARTESIAN_POINT('Ctrl Pts',(-79.0289076082456,9.90434486162714,-35.8728434773854));
#28939=CARTESIAN_POINT('Ctrl Pts',(-79.0290895293272,9.9041887700443,-36.3750481796481));
#28940=CARTESIAN_POINT('Ctrl Pts',(-79.0295684482691,9.90379477628602,-37.2525756949588));
#28941=CARTESIAN_POINT('Ctrl Pts',(-79.030982819889,9.90286430485681,-39.0047230445932));
#28942=CARTESIAN_POINT('Ctrl Pts',(-79.0323534352322,9.90290751671525,-40.5079837793973));
#28943=CARTESIAN_POINT('Ctrl Pts',(-79.0328296458239,9.90448811011299,-41.641571295867));
#28944=CARTESIAN_POINT('Ctrl Pts',(-79.032917209571,9.90467855354968,-41.8894380420173));
#28945=CARTESIAN_POINT('Ctrl Pts',(-79.0330029087558,9.90459602900717,-42.2635358200489));
#28946=CARTESIAN_POINT('Ctrl Pts',(-79.0330513003446,9.90424331849555,-42.6380823834483));
#28947=CARTESIAN_POINT('Ctrl Pts',(-79.033076820358,9.90354620635817,-43.1388767357607));
#28948=CARTESIAN_POINT('Ctrl Pts',(-79.0330556176558,9.90250041232264,-43.7667436589721));
#28949=CARTESIAN_POINT('Ctrl Pts',(-79.0330088168266,9.90177277904131,-44.5229039800781));
#28950=CARTESIAN_POINT('Ctrl Pts',(-79.0330042982439,9.90228299286789,-45.1548080059856));
#28951=CARTESIAN_POINT('Ctrl Pts',(-79.0330513266589,9.90377740689026,-45.6611391413736));
#28952=CARTESIAN_POINT('Ctrl Pts',(-79.0331199231839,9.90554179418347,-46.0412449734119));
#28953=CARTESIAN_POINT('Ctrl Pts',(-79.0332294274041,9.90805317817079,-46.4216226721883));
#28954=CARTESIAN_POINT('Ctrl Pts',(-79.0334393286454,9.91254096860848,-46.9291402371028));
#28955=CARTESIAN_POINT('Ctrl Pts',(-79.0336816691687,9.91733189681885,-47.3099063411295));
#28956=CARTESIAN_POINT('Ctrl Pts',(-79.0339932833495,9.92331761422917,-47.6920768195153));
#28957=CARTESIAN_POINT('Ctrl Pts',(-79.0341735360946,9.92905486580875,-47.9610826353062));
#28958=CARTESIAN_POINT('Ctrl Pts',(-79.0345816125781,9.94535060407697,-48.4859414578514));
#28959=CARTESIAN_POINT('Ctrl Pts',(-79.0354059618012,9.98418172594247,-49.3951141832148));
#28960=CARTESIAN_POINT('Ctrl Pts',(-79.0371418804509,10.0534002757256,-50.6525346836543));
#28961=CARTESIAN_POINT('Ctrl Pts',(-79.0401273111891,10.1136514222037,-52.0997107598098));
#28962=CARTESIAN_POINT('Ctrl Pts',(-79.0422552206141,10.1120993389653,-53.0204920365356));
#28963=CARTESIAN_POINT('Ctrl Pts',(-79.0433045273899,10.0910469989791,-53.5823614484353));
#28964=CARTESIAN_POINT('Ctrl Pts',(-79.0434992845639,10.0797687358586,-53.7813889812428));
#28965=CARTESIAN_POINT('Ctrl Pts',(-79.0438680271245,10.0422770526706,-54.212352393059));
#28966=CARTESIAN_POINT('Ctrl Pts',(-79.0447540348028,9.94210946172304,-54.9970852215659));
#28967=CARTESIAN_POINT('Ctrl Pts',(-79.0490457006217,9.64640250166675,-56.7186062687235));
#28968=CARTESIAN_POINT('Ctrl Pts',(-79.0601766148963,9.39237875326479,-58.4313538319398));
#28969=CARTESIAN_POINT('Ctrl Pts',(-79.059766483128,9.47133330665219,-59.7671833797846));
#28970=CARTESIAN_POINT('Ctrl Pts',(-79.0598456780188,9.48084926379622,-59.9090085149049));
#28971=CARTESIAN_POINT('Ctrl Pts',(-79.0598234432279,9.50446791144338,-60.2030434562208));
#28972=CARTESIAN_POINT('Ctrl Pts',(-79.0596010942571,9.55558462025953,-60.7092328461816));
#28973=CARTESIAN_POINT('Ctrl Pts',(-79.0583387852863,9.69606554450088,-61.7148620605895));
#28974=CARTESIAN_POINT('Ctrl Pts',(-79.0556754227878,9.93263311243084,-62.8348748135968));
#28975=CARTESIAN_POINT('Ctrl Pts',(-79.0526696717474,10.2253808836434,-63.9269816046484));
#28976=CARTESIAN_POINT('Ctrl Pts',(-79.0509784410456,10.407659808702,-64.5298437089376));
#28977=CARTESIAN_POINT('Ctrl Pts',(-79.0499019636937,10.5350891047172,-64.9270005875748));
#28978=CARTESIAN_POINT('Ctrl Pts',(-79.0492009980767,10.6215251528287,-65.190447030245));
#28979=CARTESIAN_POINT('Ctrl Pts',(-79.0485251631571,10.7100790764068,-65.4520343939561));
#28980=CARTESIAN_POINT('Ctrl Pts',(-79.0479683208569,10.789141711712,-65.679125068285));
#28981=CARTESIAN_POINT('Ctrl Pts',(-79.0476607288907,10.8347393551293,-65.8083832714137));
#28982=CARTESIAN_POINT('Ctrl Pts',(-79.0472089442676,10.9035486536729,-66.0017870771877));
#28983=CARTESIAN_POINT('Ctrl Pts',(-79.0468583397703,10.96168030133,-66.1618627778113));
#28984=CARTESIAN_POINT('Ctrl Pts',(-79.0462811031981,11.0590539390145,-66.4261205989256));
#28985=CARTESIAN_POINT('Ctrl Pts',(-79.0439321978173,11.1763724490973,-66.7305525791315));
#28986=CARTESIAN_POINT('Ctrl Pts',(-79.0403369548941,11.4183562660455,-67.3072646266245));
#28987=CARTESIAN_POINT('Ctrl Pts',(-79.0340712069395,11.8774962769686,-68.2955742233012));
#28988=CARTESIAN_POINT('Ctrl Pts',(-79.0255132854485,12.8785149007951,-70.1534980895664));
#28989=CARTESIAN_POINT('Ctrl Pts',(-79.0268467610113,13.7541588492713,-71.6137842113818));
#28990=CARTESIAN_POINT('Ctrl Pts',(-79.0322812395531,14.3082343257534,-72.6661621417369));
#28991=CARTESIAN_POINT('Ctrl Pts',(-79.0318056712663,14.4438933775396,-72.9238448997369));
#28992=CARTESIAN_POINT('Ctrl Pts',(-79.031841873977,14.708725048567,-73.4254194790639));
#28993=CARTESIAN_POINT('Ctrl Pts',(-79.0315212396219,15.043288618854,-74.0571626127364));
#28994=CARTESIAN_POINT('Ctrl Pts',(-79.0314066683176,15.4439701285256,-74.8110570613112));
#28995=CARTESIAN_POINT('Ctrl Pts',(-79.0311527797013,16.2470909827666,-76.3186256623566));
#28996=CARTESIAN_POINT('Ctrl Pts',(-79.0311874647941,16.916487221391,-77.5711817650315));
#28997=CARTESIAN_POINT('Ctrl Pts',(-79.0314527933477,17.8844235621115,-79.3917431634465));
#28998=CARTESIAN_POINT('Ctrl Pts',(-79.0313374840439,18.3217664730177,-80.2144024929943));
#28999=CARTESIAN_POINT('Ctrl Pts',(-79.0313374840529,18.7582880604105,-81.0353801950843));
#29000=CARTESIAN_POINT('Ctrl Pts',(-78.1311770603316,4.8823848963277,24.8296314554803));
#29001=CARTESIAN_POINT('Ctrl Pts',(-78.1317596137954,4.88248902134106,24.7807222946484));
#29002=CARTESIAN_POINT('Ctrl Pts',(-78.132370290488,4.88259794481086,24.7317992370537));
#29003=CARTESIAN_POINT('Ctrl Pts',(-78.13957093287,4.88389587870922,24.1812167240996));
#29004=CARTESIAN_POINT('Ctrl Pts',(-78.1492429359712,4.88177210313678,23.1890789298898));
#29005=CARTESIAN_POINT('Ctrl Pts',(-78.1745369969141,4.87447718530254,21.1752495239669));
#29006=CARTESIAN_POINT('Ctrl Pts',(-78.2220508241846,4.88324527193882,19.6543634614215));
#29007=CARTESIAN_POINT('Ctrl Pts',(-78.3018347246677,4.91934124068949,18.3802224980497));
#29008=CARTESIAN_POINT('Ctrl Pts',(-78.3395077877287,4.93035417118105,17.9047186839576));
#29009=CARTESIAN_POINT('Ctrl Pts',(-78.4321792272901,4.94791278160678,16.9119065362627));
#29010=CARTESIAN_POINT('Ctrl Pts',(-78.62756606031,4.98365609259776,15.1385193686742));
#29011=CARTESIAN_POINT('Ctrl Pts',(-78.8098045608793,5.0898424320682,13.5202511675539));
#29012=CARTESIAN_POINT('Ctrl Pts',(-78.9141089484633,5.30595955448313,12.1229954701847));
#29013=CARTESIAN_POINT('Ctrl Pts',(-78.9585942274942,5.39913458638839,11.5903097961193));
#29014=CARTESIAN_POINT('Ctrl Pts',(-79.0492247135416,5.62075234576258,10.5216532651304));
#29015=CARTESIAN_POINT('Ctrl Pts',(-79.2018299524198,6.08316844415622,8.68166918251728));
#29016=CARTESIAN_POINT('Ctrl Pts',(-79.2830197421236,6.5635056595323,7.13011322696838));
#29017=CARTESIAN_POINT('Ctrl Pts',(-79.2878553005376,6.92316466988806,5.96944845900976));
#29018=CARTESIAN_POINT('Ctrl Pts',(-79.282984356692,7.0138990759062,5.68124408516632));
#29019=CARTESIAN_POINT('Ctrl Pts',(-79.2712479403953,7.2005591058413,5.13353015132918));
#29020=CARTESIAN_POINT('Ctrl Pts',(-79.2395729487823,7.54899370284812,4.18865635750972));
#29021=CARTESIAN_POINT('Ctrl Pts',(-79.1505290853445,8.27795044988715,2.39178151093953));
#29022=CARTESIAN_POINT('Ctrl Pts',(-79.070707980315,8.8246826800187,0.980147970971698));
#29023=CARTESIAN_POINT('Ctrl Pts',(-79.0228189077969,9.05591664951878,0.073019789545241));
#29024=CARTESIAN_POINT('Ctrl Pts',(-79.0149196694937,9.08588467337942,-0.0495288919925896));
#29025=CARTESIAN_POINT('Ctrl Pts',(-78.9990833022964,9.14173945834025,-0.286403911574409));
#29026=CARTESIAN_POINT('Ctrl Pts',(-78.9680083406107,9.23421776089135,-0.704916515177581));
#29027=CARTESIAN_POINT('Ctrl Pts',(-78.9167273956261,9.34909347519021,-1.29979756167584));
#29028=CARTESIAN_POINT('Ctrl Pts',(-78.8452758655552,9.46363978108595,-2.01421880695577));
#29029=CARTESIAN_POINT('Ctrl Pts',(-78.7408117788548,9.5901344998305,-2.96551425791824));
#29030=CARTESIAN_POINT('Ctrl Pts',(-78.5987783229652,9.70979958345411,-4.15435211288435));
#29031=CARTESIAN_POINT('Ctrl Pts',(-78.4950291376993,9.78175376820644,-5.10676453931961));
#29032=CARTESIAN_POINT('Ctrl Pts',(-78.4416371914842,9.82093148750338,-5.70314222326153));
#29033=CARTESIAN_POINT('Ctrl Pts',(-78.4207385059252,9.83260546240869,-5.92375435343461));
#29034=CARTESIAN_POINT('Ctrl Pts',(-78.3787166419865,9.84940723412515,-6.38078537772061));
#29035=CARTESIAN_POINT('Ctrl Pts',(-78.3063535050851,9.86034282260037,-7.18824112077948));
#29036=CARTESIAN_POINT('Ctrl Pts',(-78.2100675688258,9.83680828851061,-8.38360330684038));
#29037=CARTESIAN_POINT('Ctrl Pts',(-78.1312694080627,9.79254174665709,-9.62622235018801));
#29038=CARTESIAN_POINT('Ctrl Pts',(-78.0885083689964,9.7701710701754,-10.5210983780358));
#29039=CARTESIAN_POINT('Ctrl Pts',(-78.0681948463961,9.7628635691047,-11.0392011890184));
#29040=CARTESIAN_POINT('Ctrl Pts',(-78.0594913209939,9.76154320795425,-11.3006542720142));
#29041=CARTESIAN_POINT('Ctrl Pts',(-78.0535143369238,9.76161962452868,-11.4981602742583));
#29042=CARTESIAN_POINT('Ctrl Pts',(-78.0498065810985,9.76166029727339,-11.6217337400378));
#29043=CARTESIAN_POINT('Ctrl Pts',(-78.0435536653433,9.76183376963696,-11.8737775867398));
#29044=CARTESIAN_POINT('Ctrl Pts',(-78.0355242686166,9.76230016272006,-12.3116979655568));
#29045=CARTESIAN_POINT('Ctrl Pts',(-78.0282969034116,9.76406885016096,-13.437552775809));
#29046=CARTESIAN_POINT('Ctrl Pts',(-78.0502938289893,9.76693538421329,-14.6828676178628));
#29047=CARTESIAN_POINT('Ctrl Pts',(-78.0734333686552,9.76987668609478,-15.933933506998));
#29048=CARTESIAN_POINT('Ctrl Pts',(-78.0829759820323,9.77115854627909,-16.5611813088061));
#29049=CARTESIAN_POINT('Ctrl Pts',(-78.0879258747467,9.7719474833457,-17.0647077884012));
#29050=CARTESIAN_POINT('Ctrl Pts',(-78.0892801788362,9.77223811665514,-17.3170550822814));
#29051=CARTESIAN_POINT('Ctrl Pts',(-78.0897800630712,9.77240945302464,-17.5057890556041));
#29052=CARTESIAN_POINT('Ctrl Pts',(-78.0900870788457,9.77251532184126,-17.6302578973462));
#29053=CARTESIAN_POINT('Ctrl Pts',(-78.0906097519498,9.77270161694823,-17.8794826814823));
#29054=CARTESIAN_POINT('Ctrl Pts',(-78.0910083271607,9.77285036145401,-18.128758230635));
#29055=CARTESIAN_POINT('Ctrl Pts',(-78.0912885826298,9.77296663833634,-18.378228578358));
#29056=CARTESIAN_POINT('Ctrl Pts',(-78.091419685695,9.77302624849281,-18.5341964256989));
#29057=CARTESIAN_POINT('Ctrl Pts',(-78.0914988424284,9.77306672386026,-18.6590126744284));
#29058=CARTESIAN_POINT('Ctrl Pts',(-78.0915617440567,9.77310249825838,-18.7838528491809));
#29059=CARTESIAN_POINT('Ctrl Pts',(-78.0916723951705,9.77318196154698,-19.1272582738206));
#29060=CARTESIAN_POINT('Ctrl Pts',(-78.0915289923989,9.77321686059154,-19.689756310114));
#29061=CARTESIAN_POINT('Ctrl Pts',(-78.0906521378086,9.77309075816399,-20.6914139713249));
#29062=CARTESIAN_POINT('Ctrl Pts',(-78.0889259165822,9.77273700661441,-21.9468387332845));
#29063=CARTESIAN_POINT('Ctrl Pts',(-78.0880620482322,9.77256370885544,-22.9550493642093));
#29064=CARTESIAN_POINT('Ctrl Pts',(-78.0880383400088,9.77258901260607,-23.584773435821));
#29065=CARTESIAN_POINT('Ctrl Pts',(-78.0880395768243,9.7726007016267,-23.8339778576478));
#29066=CARTESIAN_POINT('Ctrl Pts',(-78.0880838000811,9.77262872959416,-24.3332133497713));
#29067=CARTESIAN_POINT('Ctrl Pts',(-78.088252906136,9.77268781310717,-25.2086881057995));
#29068=CARTESIAN_POINT('Ctrl Pts',(-78.0886628495693,9.77278573745366,-26.4634121522126));
#29069=CARTESIAN_POINT('Ctrl Pts',(-78.0891059208895,9.77287353184222,-27.971732488491));
#29070=CARTESIAN_POINT('Ctrl Pts',(-78.0891685459406,9.77287523721471,-28.9764534880619));
#29071=CARTESIAN_POINT('Ctrl Pts',(-78.0890765294099,9.772850268981,-29.5406571874715));
#29072=CARTESIAN_POINT('Ctrl Pts',(-78.0890507139456,9.77284358851919,-29.6660260140938));
#29073=CARTESIAN_POINT('Ctrl Pts',(-78.0889803736452,9.77282615857097,-29.916825941177));
#29074=CARTESIAN_POINT('Ctrl Pts',(-78.088811812522,9.77278558263809,-30.3558648188687));
#29075=CARTESIAN_POINT('Ctrl Pts',(-78.0883217064956,9.77267012835526,-31.2343865202128));
#29076=CARTESIAN_POINT('Ctrl Pts',(-78.0875465805831,9.77248607740738,-32.2388423203145));
#29077=CARTESIAN_POINT('Ctrl Pts',(-78.0868248669926,9.77230352837888,-33.2426016030373));
#29078=CARTESIAN_POINT('Ctrl Pts',(-78.0863774008031,9.77218073775463,-33.9947891081215));
#29079=CARTESIAN_POINT('Ctrl Pts',(-78.0860922922939,9.77208530274799,-34.7460433265988));
#29080=CARTESIAN_POINT('Ctrl Pts',(-78.0860550148545,9.77204885682753,-35.2460752767603));
#29081=CARTESIAN_POINT('Ctrl Pts',(-78.0861012732241,9.77203522768628,-35.6217188758795));
#29082=CARTESIAN_POINT('Ctrl Pts',(-78.086156285324,9.77200742994158,-35.8730071688202));
#29083=CARTESIAN_POINT('Ctrl Pts',(-78.0863516097015,9.77189278779233,-36.3752035941687));
#29084=CARTESIAN_POINT('Ctrl Pts',(-78.0868905139398,9.77157418955388,-37.252721497337));
#29085=CARTESIAN_POINT('Ctrl Pts',(-78.0885311437836,9.77079498681596,-39.0048450605797));
#29086=CARTESIAN_POINT('Ctrl Pts',(-78.0901452019584,9.77095530779979,-40.5080843164705));
#29087=CARTESIAN_POINT('Ctrl Pts',(-78.0906952190281,9.77259474634693,-41.641655016873));
#29088=CARTESIAN_POINT('Ctrl Pts',(-78.0907954655095,9.77279710383975,-41.8895200313038));
#29089=CARTESIAN_POINT('Ctrl Pts',(-78.0908911052138,9.77273076278161,-42.2636138212415));
#29090=CARTESIAN_POINT('Ctrl Pts',(-78.0909420739841,9.77239246210273,-42.6381563810303));
#29091=CARTESIAN_POINT('Ctrl Pts',(-78.0909635138741,9.77171257470949,-43.1389446717454));
#29092=CARTESIAN_POINT('Ctrl Pts',(-78.09092742472,9.77068485525827,-43.7668031474549));
#29093=CARTESIAN_POINT('Ctrl Pts',(-78.0908608932792,9.76997472163853,-44.5229517102528));
#29094=CARTESIAN_POINT('Ctrl Pts',(-78.0908498770293,9.77049710604355,-45.1548446000755));
#29095=CARTESIAN_POINT('Ctrl Pts',(-78.0909045527291,9.77200019178347,-45.6611661948043));
#29096=CARTESIAN_POINT('Ctrl Pts',(-78.0909870418411,9.77377081982469,-46.0412644517004));
#29097=CARTESIAN_POINT('Ctrl Pts',(-78.0911203204094,9.77628831072,-46.4216341649118));
#29098=CARTESIAN_POINT('Ctrl Pts',(-78.0913773835638,9.78078426220737,-46.9291405924077));
#29099=CARTESIAN_POINT('Ctrl Pts',(-78.0916751194715,9.78558159104817,-47.309897565456));
#29100=CARTESIAN_POINT('Ctrl Pts',(-78.092059060611,9.79157418755964,-47.6920585341438));
#29101=CARTESIAN_POINT('Ctrl Pts',(-78.0922909438206,9.79731541699787,-47.9610555557877));
#29102=CARTESIAN_POINT('Ctrl Pts',(-78.0928141854849,9.81361750367893,-48.4858996937119));
#29103=CARTESIAN_POINT('Ctrl Pts',(-78.0938702749711,9.85245636632907,-49.3950493909296));
#29104=CARTESIAN_POINT('Ctrl Pts',(-78.0960173981978,9.92168064086134,-50.6524469583706));
#29105=CARTESIAN_POINT('Ctrl Pts',(-78.0996054393462,9.98194546203058,-52.0996113003008));
#29106=CARTESIAN_POINT('Ctrl Pts',(-78.1021972194949,9.98041340611272,-53.0203965476282));
#29107=CARTESIAN_POINT('Ctrl Pts',(-78.103552984138,9.95937932560721,-53.5822721788142));
#29108=CARTESIAN_POINT('Ctrl Pts',(-78.1038796236689,9.9481109296527,-53.7812907141171));
#29109=CARTESIAN_POINT('Ctrl Pts',(-78.1045403781411,9.91063986083384,-54.2122458319189));
#29110=CARTESIAN_POINT('Ctrl Pts',(-78.1059994025237,9.81051140989646,-54.9969674720916));
#29111=CARTESIAN_POINT('Ctrl Pts',(-78.1115865709136,9.51488524279427,-56.7184898916356));
#29112=CARTESIAN_POINT('Ctrl Pts',(-78.1237638739996,9.26090797288462,-58.4312663199397));
#29113=CARTESIAN_POINT('Ctrl Pts',(-78.1237581974326,9.33988986088882,-59.7671397332803));
#29114=CARTESIAN_POINT('Ctrl Pts',(-78.1238844942955,9.34940969623997,-59.9089694744354));
#29115=CARTESIAN_POINT('Ctrl Pts',(-78.1239493445652,9.373035887766,-60.2030134747147));
#29116=CARTESIAN_POINT('Ctrl Pts',(-78.1238612804463,9.42416601746271,-60.7092172675734));
#29117=CARTESIAN_POINT('Ctrl Pts',(-78.1228017468007,9.5646735653548,-61.7148701901171));
#29118=CARTESIAN_POINT('Ctrl Pts',(-78.1202496321837,9.80126907269193,-62.8348983317338));
#29119=CARTESIAN_POINT('Ctrl Pts',(-78.1172942048821,10.0940392374588,-63.9270100056403));
#29120=CARTESIAN_POINT('Ctrl Pts',(-78.1156194824633,10.2763284006957,-64.5298711124851));
#29121=CARTESIAN_POINT('Ctrl Pts',(-78.1145537042295,10.4037633690798,-64.9270258410423));
#29122=CARTESIAN_POINT('Ctrl Pts',(-78.1138600882166,10.4902028980212,-65.1904704483085));
#29123=CARTESIAN_POINT('Ctrl Pts',(-78.1131924031274,10.5787598112662,-65.4520554048202));
#29124=CARTESIAN_POINT('Ctrl Pts',(-78.11264417627,10.6578246392337,-65.6791434485292));
#29125=CARTESIAN_POINT('Ctrl Pts',(-78.1123420474851,10.7034234087329,-65.8084000006324));
#29126=CARTESIAN_POINT('Ctrl Pts',(-78.1118990542037,10.7722342721755,-66.0018011861481));
#29127=CARTESIAN_POINT('Ctrl Pts',(-78.1115571420184,10.830366944376,-66.1618743867873));
#29128=CARTESIAN_POINT('Ctrl Pts',(-78.1109967335477,10.9277419669287,-66.4261277626537));
#29129=CARTESIAN_POINT('Ctrl Pts',(-78.1086634949448,11.0450638269318,-66.7305607142113));
#29130=CARTESIAN_POINT('Ctrl Pts',(-78.1050916349302,11.2870517329945,-67.3072716081194));
#29131=CARTESIAN_POINT('Ctrl Pts',(-78.0988486279178,11.7461964110975,-68.2955809227801));
#29132=CARTESIAN_POINT('Ctrl Pts',(-78.0902789114672,12.7472140896651,-70.153503416737));
#29133=CARTESIAN_POINT('Ctrl Pts',(-78.0915604899259,13.6228503189759,-71.6137900378666));
#29134=CARTESIAN_POINT('Ctrl Pts',(-78.0969926351875,14.1769257016773,-72.6661684679193));
#29135=CARTESIAN_POINT('Ctrl Pts',(-78.0965172414921,14.312584819131,-72.9238511155437));
#29136=CARTESIAN_POINT('Ctrl Pts',(-78.0965534003352,14.5774165362549,-73.4254256092325));
#29137=CARTESIAN_POINT('Ctrl Pts',(-78.0962328851151,14.9119801351456,-74.0571686215522));
#29138=CARTESIAN_POINT('Ctrl Pts',(-78.0961183673416,15.3126616085308,-74.8110629718493));
#29139=CARTESIAN_POINT('Ctrl Pts',(-78.0958646287455,16.1157823228879,-76.3186314304018));
#29140=CARTESIAN_POINT('Ctrl Pts',(-78.0958993832867,16.7851783804717,-77.5711876354937));
#29141=CARTESIAN_POINT('Ctrl Pts',(-78.0961645973801,17.7531148016156,-79.3917492952415));
#29142=CARTESIAN_POINT('Ctrl Pts',(-78.0960493444548,18.1904576864469,-80.2144085738812));
#29143=CARTESIAN_POINT('Ctrl Pts',(-78.0960493444647,18.626979273838,-81.0353862759772));
#29144=CARTESIAN_POINT('Ctrl Pts',(-76.2590042273726,4.61859600327472,24.8393189079396));
#29145=CARTESIAN_POINT('Ctrl Pts',(-76.2592681779219,4.61842447839424,24.7907142206875));
#29146=CARTESIAN_POINT('Ctrl Pts',(-76.2595448957426,4.61824498946315,24.7421095860943));
#29147=CARTESIAN_POINT('Ctrl Pts',(-76.2628180829915,4.61612282665744,24.1948927869701));
#29148=CARTESIAN_POINT('Ctrl Pts',(-76.2639562409209,4.60859831660333,23.1986363414545));
#29149=CARTESIAN_POINT('Ctrl Pts',(-76.2656140569439,4.58719755532069,21.1946693625333));
#29150=CARTESIAN_POINT('Ctrl Pts',(-76.2875114488552,4.57291627906073,19.688273194824));
#29151=CARTESIAN_POINT('Ctrl Pts',(-76.3407775511093,4.57211762926454,18.4315980029145));
#29152=CARTESIAN_POINT('Ctrl Pts',(-76.364795847461,4.56784519050253,17.9582353576507));
#29153=CARTESIAN_POINT('Ctrl Pts',(-76.4225713932389,4.54820072480068,16.9721940539584));
#29154=CARTESIAN_POINT('Ctrl Pts',(-76.5461514281704,4.50383717090078,15.2086150227548));
#29155=CARTESIAN_POINT('Ctrl Pts',(-76.6816334750586,4.51394771962339,13.6041032982031));
#29156=CARTESIAN_POINT('Ctrl Pts',(-76.7973140293964,4.6407009319777,12.217831420693));
#29157=CARTESIAN_POINT('Ctrl Pts',(-76.8482852102344,4.69590094579638,11.6963573236253));
#29158=CARTESIAN_POINT('Ctrl Pts',(-76.9619015909896,4.83491484815665,10.6384382958421));
#29159=CARTESIAN_POINT('Ctrl Pts',(-77.1773119360269,5.14739349753966,8.80323245732017));
#29160=CARTESIAN_POINT('Ctrl Pts',(-77.3359788946946,5.52637907226672,7.23241034151302));
#29161=CARTESIAN_POINT('Ctrl Pts',(-77.3978387797282,5.84607073042359,6.05183159679405));
#29162=CARTESIAN_POINT('Ctrl Pts',(-77.4104442325175,5.92294187553072,5.77136070217919));
#29163=CARTESIAN_POINT('Ctrl Pts',(-77.4347135540794,6.08613441821857,5.22885965815191));
#29164=CARTESIAN_POINT('Ctrl Pts',(-77.4719372792818,6.39735474942925,4.29054300823768));
#29165=CARTESIAN_POINT('Ctrl Pts',(-77.5145028871782,7.08180232375017,2.48801694228043));
#29166=CARTESIAN_POINT('Ctrl Pts',(-77.4910547207249,7.65143594580301,1.04581578691076));
#29167=CARTESIAN_POINT('Ctrl Pts',(-77.4563842398442,7.93937105777638,0.058709180579072));
#29168=CARTESIAN_POINT('Ctrl Pts',(-77.4493290402009,7.97629023793011,-0.0741410539284971));
#29169=CARTESIAN_POINT('Ctrl Pts',(-77.4352767501426,8.04762452283956,-0.330701773943114));
#29170=CARTESIAN_POINT('Ctrl Pts',(-77.4064452562596,8.1709111311268,-0.782749843811338));
#29171=CARTESIAN_POINT('Ctrl Pts',(-77.3563225287767,8.3397651769347,-1.42166221717552));
#29172=CARTESIAN_POINT('Ctrl Pts',(-77.2826938433032,8.53037197955925,-2.1802328912742));
#29173=CARTESIAN_POINT('Ctrl Pts',(-77.1698668107121,8.76522842254609,-3.17513515057689));
#29174=CARTESIAN_POINT('Ctrl Pts',(-77.0078569636857,9.01658055161386,-4.38307664684124));
#29175=CARTESIAN_POINT('Ctrl Pts',(-76.8810657628304,9.16472129690078,-5.30418238519797));
#29176=CARTESIAN_POINT('Ctrl Pts',(-76.8143618657502,9.23977927721158,-5.86669715931559));
#29177=CARTESIAN_POINT('Ctrl Pts',(-76.787607335228,9.26692705674221,-6.0982486037313));
#29178=CARTESIAN_POINT('Ctrl Pts',(-76.7305226862092,9.31381581727877,-6.56031291945888));
#29179=CARTESIAN_POINT('Ctrl Pts',(-76.6238236505912,9.37791596242654,-7.37656475134554));
#29180=CARTESIAN_POINT('Ctrl Pts',(-76.4588581176365,9.43436852869042,-8.55885890551735));
#29181=CARTESIAN_POINT('Ctrl Pts',(-76.3083560520247,9.47478587372195,-9.77012430061687));
#29182=CARTESIAN_POINT('Ctrl Pts',(-76.2268873631626,9.5027481596305,-10.6328071100525));
#29183=CARTESIAN_POINT('Ctrl Pts',(-76.1889655386322,9.51944302308452,-11.1295121211793));
#29184=CARTESIAN_POINT('Ctrl Pts',(-76.1732056728746,9.52823085883001,-11.3791648455793));
#29185=CARTESIAN_POINT('Ctrl Pts',(-76.1626504799191,9.5350719083413,-11.5673289815983));
#29186=CARTESIAN_POINT('Ctrl Pts',(-76.1561052967098,9.53898042037542,-11.6835151432893));
#29187=CARTESIAN_POINT('Ctrl Pts',(-76.144917308345,9.54587543167022,-11.9221807076453));
#29188=CARTESIAN_POINT('Ctrl Pts',(-76.13015184916,9.55494455746776,-12.3381370441309));
#29189=CARTESIAN_POINT('Ctrl Pts',(-76.1141485418874,9.5648471517035,-13.4170096797781));
#29190=CARTESIAN_POINT('Ctrl Pts',(-76.1462425759041,9.54491458592689,-14.6383048247315));
#29191=CARTESIAN_POINT('Ctrl Pts',(-76.1814626115458,9.52362292145339,-15.8942208802503));
#29192=CARTESIAN_POINT('Ctrl Pts',(-76.1958857385209,9.51493327790932,-16.5310031582579));
#29193=CARTESIAN_POINT('Ctrl Pts',(-76.2032145185471,9.51049482727055,-17.0463829734709));
#29194=CARTESIAN_POINT('Ctrl Pts',(-76.205081939314,9.50932336185469,-17.3060972556637));
#29195=CARTESIAN_POINT('Ctrl Pts',(-76.2056636418833,9.50892238711838,-17.5007252514251));
#29196=CARTESIAN_POINT('Ctrl Pts',(-76.2060215327765,9.50866985368353,-17.6246102520673));
#29197=CARTESIAN_POINT('Ctrl Pts',(-76.2066358525459,9.50821590728096,-17.8752338247666));
#29198=CARTESIAN_POINT('Ctrl Pts',(-76.2071030890251,9.50783307899538,-18.1248776552823));
#29199=CARTESIAN_POINT('Ctrl Pts',(-76.2074424999087,9.50751558146185,-18.3751638083415));
#29200=CARTESIAN_POINT('Ctrl Pts',(-76.2076034773988,9.50734240481563,-18.5315011597223));
#29201=CARTESIAN_POINT('Ctrl Pts',(-76.20770398336,9.50721831212379,-18.6566403311446));
#29202=CARTESIAN_POINT('Ctrl Pts',(-76.2077861285719,9.50710348714328,-18.781780869533));
#29203=CARTESIAN_POINT('Ctrl Pts',(-76.2079378679436,9.50682437559786,-19.1259787747093));
#29204=CARTESIAN_POINT('Ctrl Pts',(-76.2078153736874,9.50655555146275,-19.6895413001364));
#29205=CARTESIAN_POINT('Ctrl Pts',(-76.2068710997451,9.50646064275388,-20.6924449732618));
#29206=CARTESIAN_POINT('Ctrl Pts',(-76.2049542636278,9.50677431622997,-21.9482338168688));
#29207=CARTESIAN_POINT('Ctrl Pts',(-76.2039576717217,9.50690444115847,-22.9554522656082));
#29208=CARTESIAN_POINT('Ctrl Pts',(-76.2039275481492,9.50676784822903,-23.584208861743));
#29209=CARTESIAN_POINT('Ctrl Pts',(-76.2039300299676,9.50671629310398,-23.8335354558114));
#29210=CARTESIAN_POINT('Ctrl Pts',(-76.2039812982234,9.50662403516601,-24.3327382201223));
#29211=CARTESIAN_POINT('Ctrl Pts',(-76.2041739461635,9.50648909669583,-25.2083157606351));
#29212=CARTESIAN_POINT('Ctrl Pts',(-76.2046250598341,9.50636536455388,-26.4631392496011));
#29213=CARTESIAN_POINT('Ctrl Pts',(-76.2050816179087,9.50631559527858,-27.9716990325924));
#29214=CARTESIAN_POINT('Ctrl Pts',(-76.2050810711752,9.50634384078493,-28.9766011891009));
#29215=CARTESIAN_POINT('Ctrl Pts',(-76.2049293321848,9.50637549694148,-29.5409280424476));
#29216=CARTESIAN_POINT('Ctrl Pts',(-76.2048890852193,9.50638340512734,-29.6663460964825));
#29217=CARTESIAN_POINT('Ctrl Pts',(-76.2047833071876,9.50640205542425,-29.9172266777127));
#29218=CARTESIAN_POINT('Ctrl Pts',(-76.2045369353503,9.50644212052786,-30.3564002919477));
#29219=CARTESIAN_POINT('Ctrl Pts',(-76.2038391993363,9.50654997929938,-31.2351354934128));
#29220=CARTESIAN_POINT('Ctrl Pts',(-76.2027556621548,9.50672807600084,-32.2397232658103));
#29221=CARTESIAN_POINT('Ctrl Pts',(-76.2017504713315,9.50694345656999,-33.2434999211817));
#29222=CARTESIAN_POINT('Ctrl Pts',(-76.2011267950556,9.50711892763534,-33.9956442736657));
#29223=CARTESIAN_POINT('Ctrl Pts',(-76.2007236174732,9.50730363354043,-34.7467985689858));
#29224=CARTESIAN_POINT('Ctrl Pts',(-76.2006625756323,9.50742961952989,-35.2467251488447));
#29225=CARTESIAN_POINT('Ctrl Pts',(-76.2007175157305,9.50752450792639,-35.6222768028191));
#29226=CARTESIAN_POINT('Ctrl Pts',(-76.2007869898762,9.50756951397982,-35.8735693745529));
#29227=CARTESIAN_POINT('Ctrl Pts',(-76.2010421551002,9.50760093948215,-36.3757368169703));
#29228=CARTESIAN_POINT('Ctrl Pts',(-76.2017564177825,9.50753643027774,-37.2532219117906));
#29229=CARTESIAN_POINT('Ctrl Pts',(-76.2039537667349,9.50725174813394,-39.0052625360082));
#29230=CARTESIAN_POINT('Ctrl Pts',(-76.2061267775844,9.50776518387426,-40.5084306038123));
#29231=CARTESIAN_POINT('Ctrl Pts',(-76.2068678449123,9.50959628166372,-41.6419436757499));
#29232=CARTESIAN_POINT('Ctrl Pts',(-76.2070030478336,9.50983925074399,-41.8898029062589));
#29233=CARTESIAN_POINT('Ctrl Pts',(-76.2071324330694,9.50982923114487,-42.2638831022705));
#29234=CARTESIAN_POINT('Ctrl Pts',(-76.207201903782,9.50954278151185,-42.6384119642511));
#29235=CARTESIAN_POINT('Ctrl Pts',(-76.2072321498816,9.50892629007431,-43.1391794608419));
#29236=CARTESIAN_POINT('Ctrl Pts',(-76.2071857905377,9.50796757481491,-43.7670087702537));
#29237=CARTESIAN_POINT('Ctrl Pts',(-76.2070998926126,9.50732523819983,-44.5231165636665));
#29238=CARTESIAN_POINT('Ctrl Pts',(-76.2070893748377,9.50789273229008,-45.1549708187902));
#29239=CARTESIAN_POINT('Ctrl Pts',(-76.2071679695818,9.50942615111586,-45.661258620098));
#29240=CARTESIAN_POINT('Ctrl Pts',(-76.2072835240516,9.51121663437992,-46.0413300661524));
#29241=CARTESIAN_POINT('Ctrl Pts',(-76.2074683755412,9.5137512927683,-46.4216714909197));
#29242=CARTESIAN_POINT('Ctrl Pts',(-76.2078233899365,9.51826680586861,-46.9291382069745));
#29243=CARTESIAN_POINT('Ctrl Pts',(-76.2082324872451,9.52307518220736,-47.3098630957302));
#29244=CARTESIAN_POINT('Ctrl Pts',(-76.2087601881983,9.52907686736878,-47.6919901090945));
#29245=CARTESIAN_POINT('Ctrl Pts',(-76.2090940373854,9.53482117044283,-47.9609548438845));
#29246=CARTESIAN_POINT('Ctrl Pts',(-76.2098426948961,9.55112122915765,-48.4857456976199));
#29247=CARTESIAN_POINT('Ctrl Pts',(-76.2113481950911,9.58993737722253,-49.3948125759944));
#29248=CARTESIAN_POINT('Ctrl Pts',(-76.2142847700669,9.65909517046485,-50.6521313604828));
#29249=CARTESIAN_POINT('Ctrl Pts',(-76.2190279326259,9.71927703522356,-52.0992603167427));
#29250=CARTESIAN_POINT('Ctrl Pts',(-76.2225103933654,9.7177164037998,-53.0200657704971));
#29251=CARTESIAN_POINT('Ctrl Pts',(-76.2244565286584,9.69667881139509,-53.5819669884308));
#29252=CARTESIAN_POINT('Ctrl Pts',(-76.2250365305548,9.68541555942535,-53.7809570880999));
#29253=CARTESIAN_POINT('Ctrl Pts',(-76.2262583643598,9.64795122297238,-54.2118867929367));
#29254=CARTESIAN_POINT('Ctrl Pts',(-76.2288182517556,9.54783231147705,-54.9965727500687));
#29255=CARTESIAN_POINT('Ctrl Pts',(-76.2368998477477,9.25220215107105,-56.7180955616072));
#29256=CARTESIAN_POINT('Ctrl Pts',(-76.2511002172696,8.99816735527023,-58.4309623918978));
#29257=CARTESIAN_POINT('Ctrl Pts',(-76.25188003066,9.07715834511537,-59.7669855301454));
#29258=CARTESIAN_POINT('Ctrl Pts',(-76.2520979227219,9.08668132659362,-59.9088313263526));
#29259=CARTESIAN_POINT('Ctrl Pts',(-76.2523324143239,9.11031486210005,-60.2029067217604));
#29260=CARTESIAN_POINT('Ctrl Pts',(-76.252506727489,9.16146287136278,-60.7091604595888));
#29261=CARTESIAN_POINT('Ctrl Pts',(-76.2518467397678,9.30202067976079,-61.7148952707414));
#29262=CARTESIAN_POINT('Ctrl Pts',(-76.2495214391804,9.53869245490255,-62.8349751129574));
#29263=CARTESIAN_POINT('Ctrl Pts',(-76.2466756002566,9.83153216625402,-63.927101247565));
#29264=CARTESIAN_POINT('Ctrl Pts',(-76.2450394130943,10.0138543095137,-64.5299574543569));
#29265=CARTESIAN_POINT('Ctrl Pts',(-76.243998371472,10.1413072002774,-64.9271037524503));
#29266=CARTESIAN_POINT('Ctrl Pts',(-76.2433215730166,10.2277575008871,-65.1905413693236));
#29267=CARTESIAN_POINT('Ctrl Pts',(-76.2426720314166,10.3163233362897,-65.4521173384831));
#29268=CARTESIAN_POINT('Ctrl Pts',(-76.2421423804406,10.3953940639647,-65.6791957451958));
#29269=CARTESIAN_POINT('Ctrl Pts',(-76.2418518498307,10.4409956334978,-65.8084462860989));
#29270=CARTESIAN_POINT('Ctrl Pts',(-76.2414273462054,10.5098101142562,-66.0018379677946));
#29271=CARTESIAN_POINT('Ctrl Pts',(-76.2411033296708,10.5679445458857,-66.1619021679868));
#29272=CARTESIAN_POINT('Ctrl Pts',(-76.2405770538302,10.6653207752972,-66.4261396223808));
#29273=CARTESIAN_POINT('Ctrl Pts',(-76.238274380634,10.7826504114359,-66.7305752876175));
#29274=CARTESIAN_POINT('Ctrl Pts',(-76.2347483816778,11.0246467256038,-67.3072812057032));
#29275=CARTESIAN_POINT('Ctrl Pts',(-76.2285488107215,11.4838013522539,-68.2955882718413));
#29276=CARTESIAN_POINT('Ctrl Pts',(-76.2199525136906,12.484816163397,-70.153505038466));
#29277=CARTESIAN_POINT('Ctrl Pts',(-76.2211307523171,13.3604372158861,-71.6137934851493));
#29278=CARTESIAN_POINT('Ctrl Pts',(-76.2265609927081,13.914514542038,-72.6661742394984));
#29279=CARTESIAN_POINT('Ctrl Pts',(-76.2260858005073,14.0501737272878,-72.9238564325828));
#29280=CARTESIAN_POINT('Ctrl Pts',(-76.2261219886509,14.315005652721,-73.4254306124565));
#29281=CARTESIAN_POINT('Ctrl Pts',(-76.2258016137887,14.6495692888486,-74.0571731456247));
#29282=CARTESIAN_POINT('Ctrl Pts',(-76.2256871554553,15.0502506125563,-74.8110671326668));
#29283=CARTESIAN_POINT('Ctrl Pts',(-76.2254335074589,15.8533707573767,-76.3186350678062));
#29284=CARTESIAN_POINT('Ctrl Pts',(-76.2254681352656,16.5227663100739,-77.5711916489216));
#29285=CARTESIAN_POINT('Ctrl Pts',(-76.2257331671865,17.4907032123627,-79.3917542521962));
#29286=CARTESIAN_POINT('Ctrl Pts',(-76.2256179522378,17.9280460112828,-80.2144133326538));
#29287=CARTESIAN_POINT('Ctrl Pts',(-76.2256179522404,18.3645675986696,-81.0353910347614));
#29288=CARTESIAN_POINT('Ctrl Pts',(-73.4534503626178,4.22530732157714,24.8335657884132));
#29289=CARTESIAN_POINT('Ctrl Pts',(-73.4535264544043,4.22524571942005,24.7847806310169));
#29290=CARTESIAN_POINT('Ctrl Pts',(-73.4536065022151,4.22518103548679,24.7359973542828));
#29291=CARTESIAN_POINT('Ctrl Pts',(-73.4545515468872,4.22442734723246,24.1865265021468));
#29292=CARTESIAN_POINT('Ctrl Pts',(-73.4518396848519,4.22214509836896,23.1833993556362));
#29293=CARTESIAN_POINT('Ctrl Pts',(-73.4432875794321,4.21564386815076,21.1771447988208));
#29294=CARTESIAN_POINT('Ctrl Pts',(-73.4496482516278,4.21095932290573,19.6752901912072));
#29295=CARTESIAN_POINT('Ctrl Pts',(-73.480366066804,4.20940202828548,18.4259537128077));
#29296=CARTESIAN_POINT('Ctrl Pts',(-73.4934057763347,4.20716972644692,17.9326902717968));
#29297=CARTESIAN_POINT('Ctrl Pts',(-73.5231642093913,4.19898916407945,16.9350263710404));
#29298=CARTESIAN_POINT('Ctrl Pts',(-73.5876243829913,4.1820002035377,15.1776787075357));
#29299=CARTESIAN_POINT('Ctrl Pts',(-73.6730050953354,4.18371648075477,13.6462338534787));
#29300=CARTESIAN_POINT('Ctrl Pts',(-73.770746955575,4.21638770933198,12.3551078553633));
#29301=CARTESIAN_POINT('Ctrl Pts',(-73.8141207398876,4.22931004378227,11.8605695054897));
#29302=CARTESIAN_POINT('Ctrl Pts',(-73.914564301458,4.25858480531431,10.8516404283782));
#29303=CARTESIAN_POINT('Ctrl Pts',(-74.1168742425506,4.32647223867873,9.07410082103936));
#29304=CARTESIAN_POINT('Ctrl Pts',(-74.3029354570517,4.44250222456322,7.50899014168587));
#29305=CARTESIAN_POINT('Ctrl Pts',(-74.4141498819098,4.58646403629438,6.31642002121918));
#29306=CARTESIAN_POINT('Ctrl Pts',(-74.4407921161309,4.61616424599026,6.06973783334977));
#29307=CARTESIAN_POINT('Ctrl Pts',(-74.4971526282043,4.68062536381783,5.56172614019332));
#29308=CARTESIAN_POINT('Ctrl Pts',(-74.6016775943766,4.80347816750837,4.66722272176758));
#29309=CARTESIAN_POINT('Ctrl Pts',(-74.8082980429265,5.10837144424391,2.83336893354753));
#29310=CARTESIAN_POINT('Ctrl Pts',(-74.8896400752098,5.48503136133549,1.22545544900277));
#29311=CARTESIAN_POINT('Ctrl Pts',(-74.8560557702692,5.79782244142089,0.0737981143452186));
#29312=CARTESIAN_POINT('Ctrl Pts',(-74.8501359070869,5.83828255520455,-0.0741007103992069));
#29313=CARTESIAN_POINT('Ctrl Pts',(-74.8368000578546,5.9210901625713,-0.360514162164227));
#29314=CARTESIAN_POINT('Ctrl Pts',(-74.8077814370417,6.07422021650526,-0.857581343451014));
#29315=CARTESIAN_POINT('Ctrl Pts',(-74.7543904219924,6.30982751967589,-1.54628406476854));
#29316=CARTESIAN_POINT('Ctrl Pts',(-74.679453194965,6.60760255077807,-2.34684941248347));
#29317=CARTESIAN_POINT('Ctrl Pts',(-74.573252692236,7.00990006796143,-3.38247221632282));
#29318=CARTESIAN_POINT('Ctrl Pts',(-74.4409550234082,7.49588827955719,-4.62234798923736));
#29319=CARTESIAN_POINT('Ctrl Pts',(-74.3475267879606,7.80738658039865,-5.54684366132469));
#29320=CARTESIAN_POINT('Ctrl Pts',(-74.2938158486148,7.96133936928322,-6.09887709999131));
#29321=CARTESIAN_POINT('Ctrl Pts',(-74.2647795208492,8.03246017297698,-6.36322142372142));
#29322=CARTESIAN_POINT('Ctrl Pts',(-74.204142684526,8.16462655538642,-6.86450096167411));
#29323=CARTESIAN_POINT('Ctrl Pts',(-74.0823125138115,8.38762892071749,-7.74660662064083));
#29324=CARTESIAN_POINT('Ctrl Pts',(-73.8765358143582,8.67004701957717,-8.96897404996482));
#29325=CARTESIAN_POINT('Ctrl Pts',(-73.6612700003148,8.90659532438443,-10.1368517690802));
#29326=CARTESIAN_POINT('Ctrl Pts',(-73.536969782202,9.04056414474881,-10.9203308539594));
#29327=CARTESIAN_POINT('Ctrl Pts',(-73.4783977708949,9.10574841489709,-11.3597552080612));
#29328=CARTESIAN_POINT('Ctrl Pts',(-73.4540544265507,9.13408310685853,-11.5766197293273));
#29329=CARTESIAN_POINT('Ctrl Pts',(-73.4378784149944,9.15358518982697,-11.7387516496819));
#29330=CARTESIAN_POINT('Ctrl Pts',(-73.4277303903028,9.16489463380208,-11.8419689709694));
#29331=CARTESIAN_POINT('Ctrl Pts',(-73.4094360385693,9.18538739815458,-12.0534230548263));
#29332=CARTESIAN_POINT('Ctrl Pts',(-73.3828123696777,9.21382618350268,-12.4260876551212));
#29333=CARTESIAN_POINT('Ctrl Pts',(-73.3396234882099,9.25366459642119,-13.4097636359682));
#29334=CARTESIAN_POINT('Ctrl Pts',(-73.3513981969414,9.21041323300678,-14.5798442111602));
#29335=CARTESIAN_POINT('Ctrl Pts',(-73.3724414765133,9.15254517746251,-15.8391606330428));
#29336=CARTESIAN_POINT('Ctrl Pts',(-73.3809203128667,9.12816037948757,-16.4913836601658));
#29337=CARTESIAN_POINT('Ctrl Pts',(-73.3838080244589,9.11594801097321,-17.0271640927407));
#29338=CARTESIAN_POINT('Ctrl Pts',(-73.3834874083303,9.1132209118,-17.299854671422));
#29339=CARTESIAN_POINT('Ctrl Pts',(-73.382418156735,9.11276418517905,-17.5049038677841));
#29340=CARTESIAN_POINT('Ctrl Pts',(-73.3817366061404,9.11251885643354,-17.6264660402337));
#29341=CARTESIAN_POINT('Ctrl Pts',(-73.3805006647101,9.11203801180432,-17.8778403861542));
#29342=CARTESIAN_POINT('Ctrl Pts',(-73.3794378907323,9.11162404567047,-18.1262672036762));
#29343=CARTESIAN_POINT('Ctrl Pts',(-73.3785363964569,9.11125305690329,-18.3764169410916));
#29344=CARTESIAN_POINT('Ctrl Pts',(-73.3780354933547,9.1110426695193,-18.5324456069998));
#29345=CARTESIAN_POINT('Ctrl Pts',(-73.3776706912338,9.11088503822815,-18.6574338010098));
#29346=CARTESIAN_POINT('Ctrl Pts',(-73.3773289910963,9.11073495961537,-18.7824033715676));
#29347=CARTESIAN_POINT('Ctrl Pts',(-73.3764811288779,9.11035186572385,-19.1261708202472));
#29348=CARTESIAN_POINT('Ctrl Pts',(-73.3755667743369,9.10987842611151,-19.6891481817991));
#29349=CARTESIAN_POINT('Ctrl Pts',(-73.3749290409688,9.10936330232155,-20.6913688187418));
#29350=CARTESIAN_POINT('Ctrl Pts',(-73.3753285425777,9.10914109344479,-21.9470230877658));
#29351=CARTESIAN_POINT('Ctrl Pts',(-73.3754911264308,9.1089481309495,-22.9548469969399));
#29352=CARTESIAN_POINT('Ctrl Pts',(-73.3750955098072,9.10868038336673,-23.5842034053044));
#29353=CARTESIAN_POINT('Ctrl Pts',(-73.3749590412318,9.10857862176442,-23.8334635528237));
#29354=CARTESIAN_POINT('Ctrl Pts',(-73.3747576605167,9.10838989357654,-24.3327079378256));
#29355=CARTESIAN_POINT('Ctrl Pts',(-73.3745712186291,9.10809920532248,-25.2082707662882));
#29356=CARTESIAN_POINT('Ctrl Pts',(-73.3746578913938,9.10781325001986,-26.4631303759716));
#29357=CARTESIAN_POINT('Ctrl Pts',(-73.3749594298408,9.1076815981057,-27.9717572086069));
#29358=CARTESIAN_POINT('Ctrl Pts',(-73.3750307630492,9.10775043370461,-28.9767346163479));
#29359=CARTESIAN_POINT('Ctrl Pts',(-73.3749624986682,9.10782891690429,-29.5411160077894));
#29360=CARTESIAN_POINT('Ctrl Pts',(-73.3749426806809,9.10784793838067,-29.6665553412422));
#29361=CARTESIAN_POINT('Ctrl Pts',(-73.3748857815024,9.10789385649037,-29.917471271486));
#29362=CARTESIAN_POINT('Ctrl Pts',(-73.374745037268,9.10799489240151,-30.3567031022437));
#29363=CARTESIAN_POINT('Ctrl Pts',(-73.3743338055719,9.10826809090815,-31.2355308044657));
#29364=CARTESIAN_POINT('Ctrl Pts',(-73.373725112351,9.1087165407114,-32.2401731925551));
#29365=CARTESIAN_POINT('Ctrl Pts',(-73.3732937113373,9.1092241789564,-33.2439555370028));
#29366=CARTESIAN_POINT('Ctrl Pts',(-73.3731380822152,9.10961721873692,-33.9960806734612));
#29367=CARTESIAN_POINT('Ctrl Pts',(-73.373228976467,9.11001401755442,-34.7471878425551));
#29368=CARTESIAN_POINT('Ctrl Pts',(-73.3735069059235,9.11026772494588,-35.2470654367572));
#29369=CARTESIAN_POINT('Ctrl Pts',(-73.3738173886319,9.11044931268916,-35.6225752381303));
#29370=CARTESIAN_POINT('Ctrl Pts',(-73.3740685305789,9.11055357666728,-35.8738693081829));
#29371=CARTESIAN_POINT('Ctrl Pts',(-73.374722824881,9.11070510342909,-36.3760234464305));
#29372=CARTESIAN_POINT('Ctrl Pts',(-73.3762152519728,9.11086472772307,-37.2534889948367));
#29373=CARTESIAN_POINT('Ctrl Pts',(-73.3801684951591,9.11102366189834,-39.0054883315695));
#29374=CARTESIAN_POINT('Ctrl Pts',(-73.3837862952099,9.11189706598561,-40.5086064003644));
#29375=CARTESIAN_POINT('Ctrl Pts',(-73.3851750408898,9.11390494751553,-41.6420878899218));
#29376=CARTESIAN_POINT('Ctrl Pts',(-73.3854407772297,9.11418248909649,-41.8899452427818));
#29377=CARTESIAN_POINT('Ctrl Pts',(-73.385733110362,9.11421968779635,-42.2640193550185));
#29378=CARTESIAN_POINT('Ctrl Pts',(-73.3859371191632,9.11397489948023,-42.6385422942363));
#29379=CARTESIAN_POINT('Ctrl Pts',(-73.3861147834151,9.11340819415011,-43.1393000783977));
#29380=CARTESIAN_POINT('Ctrl Pts',(-73.3862039006377,9.11250144203186,-43.7671153050967));
#29381=CARTESIAN_POINT('Ctrl Pts',(-73.3862380108539,9.1119094287437,-44.5232019750015));
#29382=CARTESIAN_POINT('Ctrl Pts',(-73.3863216238271,9.11251236292798,-45.1550347080314));
#29383=CARTESIAN_POINT('Ctrl Pts',(-73.3864899830379,9.11407079904804,-45.6613051540447));
#29384=CARTESIAN_POINT('Ctrl Pts',(-73.3866844229875,9.11587953351574,-46.0413623597674));
#29385=CARTESIAN_POINT('Ctrl Pts',(-73.3869641726572,9.11843226101216,-46.4216884857227));
#29386=CARTESIAN_POINT('Ctrl Pts',(-73.3874731185593,9.12297234782612,-46.929134069437));
#29387=CARTESIAN_POINT('Ctrl Pts',(-73.3880347312395,9.12780023573987,-47.3098400721596));
#29388=CARTESIAN_POINT('Ctrl Pts',(-73.3887494498632,9.13382343347493,-47.6919484285281));
#29389=CARTESIAN_POINT('Ctrl Pts',(-73.3892094710157,9.13958046724949,-47.9608936712186));
#29390=CARTESIAN_POINT('Ctrl Pts',(-73.3902174338838,9.15590174806547,-48.4856540481513));
#29391=CARTESIAN_POINT('Ctrl Pts',(-73.3921986559709,9.19474692453655,-49.3946750318828));
#29392=CARTESIAN_POINT('Ctrl Pts',(-73.3959037699135,9.26393051387892,-50.6519564944643));
#29393=CARTESIAN_POINT('Ctrl Pts',(-73.4017847293707,9.32416468844298,-52.0990813594302));
#29394=CARTESIAN_POINT('Ctrl Pts',(-73.4062151490616,9.32266230323621,-53.0199070893121));
#29395=CARTESIAN_POINT('Ctrl Pts',(-73.4088284950924,9.30167781654893,-53.5818275823233));
#29396=CARTESIAN_POINT('Ctrl Pts',(-73.4096944558121,9.29044001726773,-53.7808119396728));
#29397=CARTESIAN_POINT('Ctrl Pts',(-73.4115556097283,9.25303083248528,-54.2117380381064));
#29398=CARTESIAN_POINT('Ctrl Pts',(-73.4153845540563,9.15301827167226,-54.9964148469323));
#29399=CARTESIAN_POINT('Ctrl Pts',(-73.4264161666536,8.85763669586025,-56.717925261362));
#29400=CARTESIAN_POINT('Ctrl Pts',(-73.4430808803201,8.60377450161111,-58.4308174042122));
#29401=CARTESIAN_POINT('Ctrl Pts',(-73.4448411697547,8.68284947729184,-59.7669033675985));
#29402=CARTESIAN_POINT('Ctrl Pts',(-73.4451747928894,8.69238433878198,-59.9087562831018));
#29403=CARTESIAN_POINT('Ctrl Pts',(-73.44562669213,8.71604056254549,-60.2028453790664));
#29404=CARTESIAN_POINT('Ctrl Pts',(-73.4461463667916,8.76722777315182,-60.709121236243));
#29405=CARTESIAN_POINT('Ctrl Pts',(-73.4460480073186,8.90786001593109,-61.7148920567937));
#29406=CARTESIAN_POINT('Ctrl Pts',(-73.4441197541151,9.1446054406115,-62.8349928689661));
#29407=CARTESIAN_POINT('Ctrl Pts',(-73.4415286901041,9.43750309762013,-63.9271205524142));
#29408=CARTESIAN_POINT('Ctrl Pts',(-73.4400020622522,9.61985202168433,-64.5299710521792));
#29409=CARTESIAN_POINT('Ctrl Pts',(-73.4390282344758,9.74732007330091,-64.9271112513151));
#29410=CARTESIAN_POINT('Ctrl Pts',(-73.4383952854194,9.83377984100711,-65.190544158916));
#29411=CARTESIAN_POINT('Ctrl Pts',(-73.437788842033,9.92235401522777,-65.452114631555));
#29412=CARTESIAN_POINT('Ctrl Pts',(-73.4372978605278,10.0014312044763,-65.6791874758265));
#29413=CARTESIAN_POINT('Ctrl Pts',(-73.4370298932181,10.0470362112387,-65.8084346445781));
#29414=CARTESIAN_POINT('Ctrl Pts',(-73.4366398093427,10.1158556040005,-66.0018210798071));
#29415=CARTESIAN_POINT('Ctrl Pts',(-73.4363458444488,10.1739935695649,-66.1618805005531));
#29416=CARTESIAN_POINT('Ctrl Pts',(-73.4358723151197,10.2713750523792,-66.4261097053089));
#29417=CARTESIAN_POINT('Ctrl Pts',(-73.4336120537652,10.3887106230506,-66.7305448161038));
#29418=CARTESIAN_POINT('Ctrl Pts',(-73.4301494517863,10.6307143027596,-67.3072459876494));
#29419=CARTESIAN_POINT('Ctrl Pts',(-73.424002389511,11.0898739110199,-68.2955486969726));
#29420=CARTESIAN_POINT('Ctrl Pts',(-73.4153433621308,12.0908752150646,-70.1534603463187));
#29421=CARTESIAN_POINT('Ctrl Pts',(-73.4163678681088,12.9664745957069,-71.6137496655871));
#29422=CARTESIAN_POINT('Ctrl Pts',(-73.4218155619401,13.5205584289329,-72.6661329169973));
#29423=CARTESIAN_POINT('Ctrl Pts',(-73.4213395272406,13.6562172198672,-72.9238147174108));
#29424=CARTESIAN_POINT('Ctrl Pts',(-73.4213765239796,13.9210493472121,-73.4253887032415));
#29425=CARTESIAN_POINT('Ctrl Pts',(-73.4210556809956,14.2556126777563,-74.0571308465917));
#29426=CARTESIAN_POINT('Ctrl Pts',(-73.4209409401286,14.6562937916129,-74.8110246011275));
#29427=CARTESIAN_POINT('Ctrl Pts',(-73.4206859365661,15.4594132840169,-76.318592205801));
#29428=CARTESIAN_POINT('Ctrl Pts',(-73.4207190966181,16.1288082739189,-77.571148953329));
#29429=CARTESIAN_POINT('Ctrl Pts',(-73.4209847269192,17.0967455638613,-79.3917120442865));
#29430=CARTESIAN_POINT('Ctrl Pts',(-73.420869138286,17.5340881419541,-80.2143709597686));
#29431=CARTESIAN_POINT('Ctrl Pts',(-73.4208691382803,17.9706097293417,-81.0353486618712));
#29432=CARTESIAN_POINT('Ctrl Pts',(-70.6494620665907,3.83081083471652,24.8276526399532));
#29433=CARTESIAN_POINT('Ctrl Pts',(-70.6496326998556,3.8309065566531,24.7786797052078));
#29434=CARTESIAN_POINT('Ctrl Pts',(-70.6498117133617,3.83100671102027,24.7297060068776));
#29435=CARTESIAN_POINT('Ctrl Pts',(-70.6519248484191,3.83219465222234,24.1780050135636));
#29436=CARTESIAN_POINT('Ctrl Pts',(-70.6530399902727,3.83471417259306,23.1723496464166));
#29437=CARTESIAN_POINT('Ctrl Pts',(-70.6553282802904,3.84151496701024,21.1618903863707));
#29438=CARTESIAN_POINT('Ctrl Pts',(-70.6694181592974,3.84933667283851,19.6579544149711));
#29439=CARTESIAN_POINT('Ctrl Pts',(-70.7017966351779,3.85799915528513,18.4074357876463));
#29440=CARTESIAN_POINT('Ctrl Pts',(-70.7166803709366,3.86261513924192,17.8992952787561));
#29441=CARTESIAN_POINT('Ctrl Pts',(-70.7528589610518,3.87486424445333,16.8915795958476));
#29442=CARTESIAN_POINT('Ctrl Pts',(-70.8302083467482,3.9004793077478,15.138016287893));
#29443=CARTESIAN_POINT('Ctrl Pts',(-70.9112744147464,3.91699381429674,13.6541787391245));
#29444=CARTESIAN_POINT('Ctrl Pts',(-70.9763140518782,3.91434651444167,12.4237745483885));
#29445=CARTESIAN_POINT('Ctrl Pts',(-71.0030618549083,3.91054737427746,11.9395233575876));
#29446=CARTESIAN_POINT('Ctrl Pts',(-71.0592521782506,3.894231013442,10.9566785715773));
#29447=CARTESIAN_POINT('Ctrl Pts',(-71.1632499017295,3.8509303468373,9.21600694973984));
#29448=CARTESIAN_POINT('Ctrl Pts',(-71.2580814374877,3.81527639561953,7.68018356218295));
#29449=CARTESIAN_POINT('Ctrl Pts',(-71.3272860059582,3.82213905637395,6.5082419323708));
#29450=CARTESIAN_POINT('Ctrl Pts',(-71.3427494575123,3.82225001371945,6.282526518141));
#29451=CARTESIAN_POINT('Ctrl Pts',(-71.3749139807024,3.81715308070013,5.80195460366119));
#29452=CARTESIAN_POINT('Ctrl Pts',(-71.4340129269757,3.79815273347038,4.94708162916697));
#29453=CARTESIAN_POINT('Ctrl Pts',(-71.5592342028308,3.74889431869233,3.13847244276675));
#29454=CARTESIAN_POINT('Ctrl Pts',(-71.6637008083176,3.81595423074781,1.43529809209986));
#29455=CARTESIAN_POINT('Ctrl Pts',(-71.6955799842735,4.05978002256819,0.17780386520389));
#29456=CARTESIAN_POINT('Ctrl Pts',(-71.6999728057474,4.08946262178212,0.0303556410748098));
#29457=CARTESIAN_POINT('Ctrl Pts',(-71.7086627700793,4.15430584581213,-0.263209799828586));
#29458=CARTESIAN_POINT('Ctrl Pts',(-71.7241795640316,4.2801082104513,-0.770234211702012));
#29459=CARTESIAN_POINT('Ctrl Pts',(-71.7446745302739,4.49143615920851,-1.47731101502265));
#29460=CARTESIAN_POINT('Ctrl Pts',(-71.7621594414976,4.78057190184174,-2.29733031108985));
#29461=CARTESIAN_POINT('Ctrl Pts',(-71.7719402743552,5.19615381873767,-3.35702259704706));
#29462=CARTESIAN_POINT('Ctrl Pts',(-71.7559940767548,5.73883787559449,-4.62551909003516));
#29463=CARTESIAN_POINT('Ctrl Pts',(-71.7136494335196,6.14233732235438,-5.60373018086587));
#29464=CARTESIAN_POINT('Ctrl Pts',(-71.6746530735446,6.36894140367775,-6.21041210479194));
#29465=CARTESIAN_POINT('Ctrl Pts',(-71.6454234832357,6.47958429679363,-6.50916202445099));
#29466=CARTESIAN_POINT('Ctrl Pts',(-71.5852869298051,6.69927064532406,-7.06348618753471));
#29467=CARTESIAN_POINT('Ctrl Pts',(-71.4592692103757,7.10401392951411,-8.02462301779982));
#29468=CARTESIAN_POINT('Ctrl Pts',(-71.2502864953223,7.68573763210261,-9.31372037528634));
#29469=CARTESIAN_POINT('Ctrl Pts',(-71.0413582371967,8.17269012460668,-10.4897486187166));
#29470=CARTESIAN_POINT('Ctrl Pts',(-70.9194484447363,8.41683088542299,-11.22389491883));
#29471=CARTESIAN_POINT('Ctrl Pts',(-70.8610061829472,8.52564011599825,-11.6150582453415));
#29472=CARTESIAN_POINT('Ctrl Pts',(-70.8363829293454,8.569358881547,-11.8004074281031));
#29473=CARTESIAN_POINT('Ctrl Pts',(-70.8199032162588,8.59828192577974,-11.9363061091416));
#29474=CARTESIAN_POINT('Ctrl Pts',(-70.8088878911491,8.61784484280418,-12.0351367520892));
#29475=CARTESIAN_POINT('Ctrl Pts',(-70.787732704196,8.65261205359186,-12.2300795541281));
#29476=CARTESIAN_POINT('Ctrl Pts',(-70.7529154929867,8.70419486900887,-12.5775059987084));
#29477=CARTESIAN_POINT('Ctrl Pts',(-70.674627889547,8.79351300847224,-13.4950550826304));
#29478=CARTESIAN_POINT('Ctrl Pts',(-70.6249383740797,8.77853835100137,-14.6202155928646));
#29479=CARTESIAN_POINT('Ctrl Pts',(-70.5943086444658,8.73281849448334,-15.8659974403439));
#29480=CARTESIAN_POINT('Ctrl Pts',(-70.5807074443851,8.71427141760064,-16.5189898372744));
#29481=CARTESIAN_POINT('Ctrl Pts',(-70.5696295443514,8.7084393082528,-17.0599664971091));
#29482=CARTESIAN_POINT('Ctrl Pts',(-70.5636960856804,8.710000548671,-17.3368382446092));
#29483=CARTESIAN_POINT('Ctrl Pts',(-70.5590378482671,8.71328878005061,-17.5453595325233));
#29484=CARTESIAN_POINT('Ctrl Pts',(-70.5561697720275,8.71501732932909,-17.66218208993));
#29485=CARTESIAN_POINT('Ctrl Pts',(-70.5510382949045,8.71822189311693,-17.9085187419594));
#29486=CARTESIAN_POINT('Ctrl Pts',(-70.5468139861943,8.72072632138071,-18.1508169083625));
#29487=CARTESIAN_POINT('Ctrl Pts',(-70.5434014822654,8.7226857771753,-18.3960892577941));
#29488=CARTESIAN_POINT('Ctrl Pts',(-70.5415889576892,8.72367630379317,-18.5490737482143));
#29489=CARTESIAN_POINT('Ctrl Pts',(-70.5403198577929,8.72434263374008,-18.6718055273237));
#29490=CARTESIAN_POINT('Ctrl Pts',(-70.539167663306,8.7249251220034,-18.7945738239458));
#29491=CARTESIAN_POINT('Ctrl Pts',(-70.5364628645629,8.72620000910083,-19.1326061304726));
#29492=CARTESIAN_POINT('Ctrl Pts',(-70.5344079682884,8.72660365685414,-19.6878742855126));
#29493=CARTESIAN_POINT('Ctrl Pts',(-70.5355608609243,8.72395856068241,-20.6811225067078));
#29494=CARTESIAN_POINT('Ctrl Pts',(-70.542387528159,8.7170164050489,-21.9344562421943));
#29495=CARTESIAN_POINT('Ctrl Pts',(-70.5458632611026,8.71339189514063,-22.9497488309881));
#29496=CARTESIAN_POINT('Ctrl Pts',(-70.5450374514181,8.7135098723975,-23.5865408257813));
#29497=CARTESIAN_POINT('Ctrl Pts',(-70.5447471842888,8.71355843775048,-23.8349075051346));
#29498=CARTESIAN_POINT('Ctrl Pts',(-70.5442924475687,8.71366924240936,-24.3345135506893));
#29499=CARTESIAN_POINT('Ctrl Pts',(-70.543800864288,8.71388643206869,-25.2095712506264));
#29500=CARTESIAN_POINT('Ctrl Pts',(-70.5437828030668,8.71422173656197,-26.4642473457495));
#29501=CARTESIAN_POINT('Ctrl Pts',(-70.5443151186548,8.714485394657,-27.972125838861));
#29502=CARTESIAN_POINT('Ctrl Pts',(-70.544657365899,8.71450179715225,-28.9765670388092));
#29503=CARTESIAN_POINT('Ctrl Pts',(-70.544753185945,8.71442826770179,-29.540599925421));
#29504=CARTESIAN_POINT('Ctrl Pts',(-70.5447725146452,8.71440819195271,-29.6659124473631));
#29505=CARTESIAN_POINT('Ctrl Pts',(-70.5448015365278,8.71435600444617,-29.9166176840538));
#29506=CARTESIAN_POINT('Ctrl Pts',(-70.5448305077078,8.71423710213987,-30.3554939541661));
#29507=CARTESIAN_POINT('Ctrl Pts',(-70.5448321347687,8.71389907695821,-31.2337491285771));
#29508=CARTESIAN_POINT('Ctrl Pts',(-70.5448349164206,8.71336869028112,-32.2380147384793));
#29509=CARTESIAN_POINT('Ctrl Pts',(-70.5451063262961,8.71283065278324,-33.2417295013175));
#29510=CARTESIAN_POINT('Ctrl Pts',(-70.5455105362915,8.71245869625278,-33.9939611185162));
#29511=CARTESIAN_POINT('Ctrl Pts',(-70.546176741767,8.71216609792829,-34.7453143056492));
#29512=CARTESIAN_POINT('Ctrl Pts',(-70.5468406439546,8.71204454454721,-35.2454583991906));
#29513=CARTESIAN_POINT('Ctrl Pts',(-70.5474393800059,8.71198876986363,-35.6212034339876));
#29514=CARTESIAN_POINT('Ctrl Pts',(-70.5478930911235,8.71193803468518,-35.8724848760286));
#29515=CARTESIAN_POINT('Ctrl Pts',(-70.5489856262303,8.71179501958184,-36.3747125556351));
#29516=CARTESIAN_POINT('Ctrl Pts',(-70.5513128995724,8.71147840408229,-37.252252911644));
#29517=CARTESIAN_POINT('Ctrl Pts',(-70.5571101664544,8.71082696437478,-39.0044582742178));
#29518=CARTESIAN_POINT('Ctrl Pts',(-70.5621980028138,8.71119560410614,-40.5077353732109));
#29519=CARTESIAN_POINT('Ctrl Pts',(-70.5642506312549,8.71287280584407,-41.6413572595022));
#29520=CARTESIAN_POINT('Ctrl Pts',(-70.5646509318823,8.71307821510131,-41.8892302310715));
#29521=CARTESIAN_POINT('Ctrl Pts',(-70.5651111355399,8.71300711616514,-42.2633393490989));
#29522=CARTESIAN_POINT('Ctrl Pts',(-70.5654537720773,8.7126560517315,-42.6378979443855));
#29523=CARTESIAN_POINT('Ctrl Pts',(-70.5657827919375,8.71195170856678,-43.1387093024551));
#29524=CARTESIAN_POINT('Ctrl Pts',(-70.5660093931435,8.7108842783085,-43.7665993987514));
#29525=CARTESIAN_POINT('Ctrl Pts',(-70.5661603846999,8.7101283917312,-44.5227897914755));
#29526=CARTESIAN_POINT('Ctrl Pts',(-70.5663301874602,8.71062807138128,-45.1547197983672));
#29527=CARTESIAN_POINT('Ctrl Pts',(-70.5665785295845,8.71212986471067,-45.6610761158928));
#29528=CARTESIAN_POINT('Ctrl Pts',(-70.5668426229271,8.71391030213836,-46.0412011432084));
#29529=CARTESIAN_POINT('Ctrl Pts',(-70.5672060860399,8.71645036476586,-46.4215986512285));
#29530=CARTESIAN_POINT('Ctrl Pts',(-70.5678510624984,8.72099633974999,-46.9291444376783));
#29531=CARTESIAN_POINT('Ctrl Pts',(-70.5685490049604,8.72585625964623,-47.3099306692449));
#29532=CARTESIAN_POINT('Ctrl Pts',(-70.5694315859434,8.73193307009486,-47.6921242948781));
#29533=CARTESIAN_POINT('Ctrl Pts',(-70.5700028112621,8.73773568313054,-47.9611506235088));
#29534=CARTESIAN_POINT('Ctrl Pts',(-70.5712340825493,8.75417753941003,-48.4860451568485));
#29535=CARTESIAN_POINT('Ctrl Pts',(-70.5736142010392,8.79330423740066,-49.3952751998665));
#29536=CARTESIAN_POINT('Ctrl Pts',(-70.5779570100187,8.86304416439338,-50.6527583617862));
#29537=CARTESIAN_POINT('Ctrl Pts',(-70.5848238355766,8.92405748189299,-52.0999793978263));
#29538=CARTESIAN_POINT('Ctrl Pts',(-70.5901323883384,8.92307983476999,-53.0207592136404));
#29539=CARTESIAN_POINT('Ctrl Pts',(-70.5933835869417,8.90240786789031,-53.5826175741996));
#29540=CARTESIAN_POINT('Ctrl Pts',(-70.5945272935145,8.89128748430115,-53.7816791081091));
#29541=CARTESIAN_POINT('Ctrl Pts',(-70.5970120911207,8.85415045768397,-54.2126751468643));
#29542=CARTESIAN_POINT('Ctrl Pts',(-70.6020877584862,8.75468433042563,-54.9974481723177));
#29543=CARTESIAN_POINT('Ctrl Pts',(-70.6160278517372,8.4606177040147,-56.7189510136224));
#29544=CARTESIAN_POINT('Ctrl Pts',(-70.6351143486718,8.20797974704676,-58.4315982466486));
#29545=CARTESIAN_POINT('Ctrl Pts',(-70.6378400431479,8.28745191915634,-59.7672962513482));
#29546=CARTESIAN_POINT('Ctrl Pts',(-70.6382882810371,8.29702776371256,-59.9091079122869));
#29547=CARTESIAN_POINT('Ctrl Pts',(-70.6389559396657,8.3207566747499,-60.203116134479));
#29548=CARTESIAN_POINT('Ctrl Pts',(-70.6398204929652,8.37204147372282,-60.7092633605087));
#29549=CARTESIAN_POINT('Ctrl Pts',(-70.6402897909106,8.51277007689702,-61.7148227459977));
#29550=CARTESIAN_POINT('Ctrl Pts',(-70.6387760021451,8.74946254134713,-62.8347878524703));
#29551=CARTESIAN_POINT('Ctrl Pts',(-70.63645635019,9.04226083934355,-63.9268742425419));
#29552=CARTESIAN_POINT('Ctrl Pts',(-70.6350467453139,9.22455565865073,-64.5297348535941));
#29553=CARTESIAN_POINT('Ctrl Pts',(-70.6341437471854,9.35199658562109,-64.9268950821234));
#29554=CARTESIAN_POINT('Ctrl Pts',(-70.6335566103036,9.43844111080219,-65.1903448912955));
#29555=CARTESIAN_POINT('Ctrl Pts',(-70.6329946828321,9.52700517591339,-65.451937409211));
#29556=CARTESIAN_POINT('Ctrl Pts',(-70.6325428578251,9.60607928875794,-65.6790341699771));
#29557=CARTESIAN_POINT('Ctrl Pts',(-70.6322975262368,9.65168438950241,-65.8082963195497));
#29558=CARTESIAN_POINT('Ctrl Pts',(-70.6319417515286,9.72050584533726,-66.0017064990561));
#29559=CARTESIAN_POINT('Ctrl Pts',(-70.6316773393184,9.77864984379035,-66.1617885164817));
#29560=CARTESIAN_POINT('Ctrl Pts',(-70.6312550527681,9.87604754909493,-66.4260578348278));
#29561=CARTESIAN_POINT('Ctrl Pts',(-70.6290388968904,9.99337956946595,-66.7304847584415));
#29562=CARTESIAN_POINT('Ctrl Pts',(-70.6256406643102,10.235385949348,-67.307196970974));
#29563=CARTESIAN_POINT('Ctrl Pts',(-70.6195478587563,10.6945412135849,-68.2955031148334));
#29564=CARTESIAN_POINT('Ctrl Pts',(-70.6108253052356,11.6955285102401,-70.1534276569231));
#29565=CARTESIAN_POINT('Ctrl Pts',(-70.6116939852769,12.5711088080986,-71.6137122958572));
#29566=CARTESIAN_POINT('Ctrl Pts',(-70.6171589562653,13.1251918432522,-72.6660905861456));
#29567=CARTESIAN_POINT('Ctrl Pts',(-70.6166820361121,13.2608502284483,-72.9237734197364));
#29568=CARTESIAN_POINT('Ctrl Pts',(-70.6167197576935,13.5256819745422,-73.4253481708406));
#29569=CARTESIAN_POINT('Ctrl Pts',(-70.6163984323959,13.8602451411829,-74.0570914180674));
#29570=CARTESIAN_POINT('Ctrl Pts',(-70.6162833700721,14.2609265969471,-74.8109860525134));
#29571=CARTESIAN_POINT('Ctrl Pts',(-70.6160270030381,15.0640473305046,-76.3185549282437));
#29572=CARTESIAN_POINT('Ctrl Pts',(-70.6160590352253,15.7334436640084,-77.5711107024718));
#29573=CARTESIAN_POINT('Ctrl Pts',(-70.6163255657832,16.7013800620162,-79.3916714201663));
#29574=CARTESIAN_POINT('Ctrl Pts',(-70.6162096418444,17.1387228581873,-80.2143307870197));
#29575=CARTESIAN_POINT('Ctrl Pts',(-70.6162096418429,17.5752444455778,-81.0353084891142));
#29576=CARTESIAN_POINT('Ctrl Pts',(-67.8429979490876,3.43540937587766,24.8291468061157));
#29577=CARTESIAN_POINT('Ctrl Pts',(-67.843255199307,3.43548039997282,24.7802219150478));
#29578=CARTESIAN_POINT('Ctrl Pts',(-67.8435249642338,3.43555466825619,24.7312970013852));
#29579=CARTESIAN_POINT('Ctrl Pts',(-67.8467076136049,3.43643894377634,24.1801610961006));
#29580=CARTESIAN_POINT('Ctrl Pts',(-67.8504237539074,3.43796780523234,23.1756926839324));
#29581=CARTESIAN_POINT('Ctrl Pts',(-67.8599419168608,3.44198305776693,21.1660006053159));
#29582=CARTESIAN_POINT('Ctrl Pts',(-67.8810374140118,3.44791190792428,19.6612635225141));
#29583=CARTESIAN_POINT('Ctrl Pts',(-67.9194104989257,3.45625007158521,18.4096589917386));
#29584=CARTESIAN_POINT('Ctrl Pts',(-67.9382125535026,3.46076834152602,17.9030504603971));
#29585=CARTESIAN_POINT('Ctrl Pts',(-67.9860602467786,3.47303181360074,16.8965429211016));
#29586=CARTESIAN_POINT('Ctrl Pts',(-68.0882538963617,3.49935505131162,15.1438911469587));
#29587=CARTESIAN_POINT('Ctrl Pts',(-68.1787023358157,3.51729839131463,13.6549281187412));
#29588=CARTESIAN_POINT('Ctrl Pts',(-68.2236661968178,3.51554813699857,12.416125634103));
#29589=CARTESIAN_POINT('Ctrl Pts',(-68.240294156464,3.5132479046786,11.9218528873524));
#29590=CARTESIAN_POINT('Ctrl Pts',(-68.2689151704927,3.50367771304502,10.9290940226273));
#29591=CARTESIAN_POINT('Ctrl Pts',(-68.3084503585006,3.47762876365091,9.18311221725741));
#29592=CARTESIAN_POINT('Ctrl Pts',(-68.3301235588637,3.45152683070009,7.6704450302173));
#29593=CARTESIAN_POINT('Ctrl Pts',(-68.3456628288656,3.44053057254519,6.52970039108954));
#29594=CARTESIAN_POINT('Ctrl Pts',(-68.3481621521419,3.43698218092217,6.2958605672267));
#29595=CARTESIAN_POINT('Ctrl Pts',(-68.3499178243137,3.42562356289472,5.81106989728593));
#29596=CARTESIAN_POINT('Ctrl Pts',(-68.3461693060382,3.39691433075224,4.95317410772437));
#29597=CARTESIAN_POINT('Ctrl Pts',(-68.3238707383516,3.3264308083201,3.17678700344086));
#29598=CARTESIAN_POINT('Ctrl Pts',(-68.3243575733678,3.30825572512503,1.5672747065012));
#29599=CARTESIAN_POINT('Ctrl Pts',(-68.3814826358144,3.39780225920189,0.387491389599531));
#29600=CARTESIAN_POINT('Ctrl Pts',(-68.3892510774313,3.40656307744178,0.265861555568177));
#29601=CARTESIAN_POINT('Ctrl Pts',(-68.4077487811753,3.42556704012703,0.0101690127921557));
#29602=CARTESIAN_POINT('Ctrl Pts',(-68.4474830193355,3.45999959830791,-0.435805451239607));
#29603=CARTESIAN_POINT('Ctrl Pts',(-68.5214053738539,3.51863065866942,-1.08807657225968));
#29604=CARTESIAN_POINT('Ctrl Pts',(-68.6244249906881,3.61485033990705,-1.88625004060008));
#29605=CARTESIAN_POINT('Ctrl Pts',(-68.762100742499,3.78900570837791,-2.97208690411789));
#29606=CARTESIAN_POINT('Ctrl Pts',(-68.8980921258,4.10565455346679,-4.35855017453348));
#29607=CARTESIAN_POINT('Ctrl Pts',(-68.9128972361772,4.46292517231313,-5.48743317652969));
#29608=CARTESIAN_POINT('Ctrl Pts',(-68.8835351541264,4.71911664935449,-6.20457641486434));
#29609=CARTESIAN_POINT('Ctrl Pts',(-68.8610406882809,4.84466478657557,-6.5358207313883));
#29610=CARTESIAN_POINT('Ctrl Pts',(-68.810269153138,5.111352077503,-7.14389354421227));
#29611=CARTESIAN_POINT('Ctrl Pts',(-68.7008986449468,5.6308280985943,-8.16490507596953));
#29612=CARTESIAN_POINT('Ctrl Pts',(-68.5263328009642,6.43604072547312,-9.48848437606004));
#29613=CARTESIAN_POINT('Ctrl Pts',(-68.3742509965807,7.15026503593484,-10.6834425942453));
#29614=CARTESIAN_POINT('Ctrl Pts',(-68.2960383802098,7.5095388116318,-11.4168829107783));
#29615=CARTESIAN_POINT('Ctrl Pts',(-68.2603561980416,7.66556287853389,-11.7970284531808));
#29616=CARTESIAN_POINT('Ctrl Pts',(-68.2455289714394,7.72624062966262,-11.97182504539));
#29617=CARTESIAN_POINT('Ctrl Pts',(-68.2353427298046,7.76560735334509,-12.097787494051));
#29618=CARTESIAN_POINT('Ctrl Pts',(-68.2257690214525,7.79765559041035,-12.2057348844777));
#29619=CARTESIAN_POINT('Ctrl Pts',(-68.2071477696638,7.8534301152825,-12.4091866131882));
#29620=CARTESIAN_POINT('Ctrl Pts',(-68.1716358694143,7.94179346169686,-12.7737393881953));
#29621=CARTESIAN_POINT('Ctrl Pts',(-68.0704929322039,8.1155169155222,-13.7174848416372));
#29622=CARTESIAN_POINT('Ctrl Pts',(-67.9379388540401,8.19410547769043,-14.8288865432328));
#29623=CARTESIAN_POINT('Ctrl Pts',(-67.827047180042,8.24470200634281,-16.0333715681186));
#29624=CARTESIAN_POINT('Ctrl Pts',(-67.7795672382218,8.26978736748521,-16.6593610065802));
#29625=CARTESIAN_POINT('Ctrl Pts',(-67.7480131276514,8.29424328490067,-17.1744632202735));
#29626=CARTESIAN_POINT('Ctrl Pts',(-67.73458059527,8.30876634793277,-17.4370136882304));
#29627=CARTESIAN_POINT('Ctrl Pts',(-67.7255258325098,8.32073410293769,-17.6343112047601));
#29628=CARTESIAN_POINT('Ctrl Pts',(-67.7200862703883,8.32680648549444,-17.7435073503106));
#29629=CARTESIAN_POINT('Ctrl Pts',(-67.7104146454208,8.33824536339626,-17.9755230869486));
#29630=CARTESIAN_POINT('Ctrl Pts',(-67.7026777620944,8.34715217005881,-18.2044889428511));
#29631=CARTESIAN_POINT('Ctrl Pts',(-67.6966341645092,8.3541764453997,-18.4375568529196));
#29632=CARTESIAN_POINT('Ctrl Pts',(-67.6935353376028,8.3577232053768,-18.5833563338914));
#29633=CARTESIAN_POINT('Ctrl Pts',(-67.6914358025922,8.36011433549464,-18.7006166844035));
#29634=CARTESIAN_POINT('Ctrl Pts',(-67.6895828416986,8.36220414098241,-18.8180952792904));
#29635=CARTESIAN_POINT('Ctrl Pts',(-67.6854660405954,8.36676764207297,-19.1423216763214));
#29636=CARTESIAN_POINT('Ctrl Pts',(-67.6837255962329,8.36814152476923,-19.6791089082259));
#29637=CARTESIAN_POINT('Ctrl Pts',(-67.6906843160803,8.35814000473539,-20.651093751224));
#29638=CARTESIAN_POINT('Ctrl Pts',(-67.710406632541,8.33191835568154,-21.899623813537));
#29639=CARTESIAN_POINT('Ctrl Pts',(-67.7210624318957,8.31774556571313,-22.9339497328628));
#29640=CARTESIAN_POINT('Ctrl Pts',(-67.7207994578438,8.31808112582329,-23.5892652088098));
#29641=CARTESIAN_POINT('Ctrl Pts',(-67.720733117923,8.31821360280331,-23.8355542489468));
#29642=CARTESIAN_POINT('Ctrl Pts',(-67.7207273213582,8.31850430364268,-24.3362847484307));
#29643=CARTESIAN_POINT('Ctrl Pts',(-67.7210039430532,8.31904808417056,-25.2105437686112));
#29644=CARTESIAN_POINT('Ctrl Pts',(-67.7219552216887,8.31985387668672,-26.4655180104148));
#29645=CARTESIAN_POINT('Ctrl Pts',(-67.7231943423994,8.32050740196497,-27.9726806839646));
#29646=CARTESIAN_POINT('Ctrl Pts',(-67.7235155311288,8.32051519025861,-28.9767684556765));
#29647=CARTESIAN_POINT('Ctrl Pts',(-67.7233971219608,8.32032151698294,-29.5405267267874));
#29648=CARTESIAN_POINT('Ctrl Pts',(-67.7233593675948,8.32027011766274,-29.6657703361541));
#29649=CARTESIAN_POINT('Ctrl Pts',(-67.723241014596,8.32013958929522,-29.9163521225107));
#29650=CARTESIAN_POINT('Ctrl Pts',(-67.7229297492033,8.31984426995699,-30.3550203608265));
#29651=CARTESIAN_POINT('Ctrl Pts',(-67.7219636671122,8.31901320679915,-31.2329310628976));
#29652=CARTESIAN_POINT('Ctrl Pts',(-67.720400340325,8.31768767781877,-32.2369480939191));
#29653=CARTESIAN_POINT('Ctrl Pts',(-67.7190338173315,8.31628904161721,-33.2405997552514));
#29654=CARTESIAN_POINT('Ctrl Pts',(-67.718271679738,8.31528342970505,-33.9928850424582));
#29655=CARTESIAN_POINT('Ctrl Pts',(-67.7179342080551,8.31441764247642,-34.7443623717059));
#29656=CARTESIAN_POINT('Ctrl Pts',(-67.7181023937929,8.31398381050784,-35.2446500331208));
#29657=CARTESIAN_POINT('Ctrl Pts',(-67.7184178356948,8.31372988048811,-35.6205257014851));
#29658=CARTESIAN_POINT('Ctrl Pts',(-67.7186970170676,8.31355042220773,-35.8717973937954));
#29659=CARTESIAN_POINT('Ctrl Pts',(-67.7194958221841,8.31316150286721,-36.3740651607934));
#29660=CARTESIAN_POINT('Ctrl Pts',(-67.7214436471302,8.31245406754501,-37.2516350499055));
#29661=CARTESIAN_POINT('Ctrl Pts',(-67.7268950573798,8.31112798346429,-39.0039525846174));
#29662=CARTESIAN_POINT('Ctrl Pts',(-67.7320219606896,8.31110091035574,-40.5072829288273));
#29663=CARTESIAN_POINT('Ctrl Pts',(-67.733879661603,8.31250535114878,-41.6409687968382));
#29664=CARTESIAN_POINT('Ctrl Pts',(-67.7342268248544,8.3126486066805,-41.8888478011433));
#29665=CARTESIAN_POINT('Ctrl Pts',(-67.734585193687,8.31248482742067,-42.2629729327167));
#29666=CARTESIAN_POINT('Ctrl Pts',(-67.7348093430965,8.31204199054457,-42.637548579422));
#29667=CARTESIAN_POINT('Ctrl Pts',(-67.7349662316575,8.31121885167147,-43.1383864958984));
#29668=CARTESIAN_POINT('Ctrl Pts',(-67.7349656602,8.31001211263342,-43.7663158642005));
#29669=CARTESIAN_POINT('Ctrl Pts',(-67.7348717584322,8.30911406018918,-44.5225635854086));
#29670=CARTESIAN_POINT('Ctrl Pts',(-67.7348996531857,8.30952467107504,-45.1545490110695));
#29671=CARTESIAN_POINT('Ctrl Pts',(-67.7350952479235,8.31097630696777,-45.6609588687116));
#29672=CARTESIAN_POINT('Ctrl Pts',(-67.7353560076653,8.3127316819013,-46.0411264962276));
#29673=CARTESIAN_POINT('Ctrl Pts',(-67.7357582008244,8.31526032504559,-46.421569382839));
#29674=CARTESIAN_POINT('Ctrl Pts',(-67.7365189774708,8.31981101030796,-46.9291804544779));
#29675=CARTESIAN_POINT('Ctrl Pts',(-67.7373839436146,8.32469869153759,-47.3100174825679));
#29676=CARTESIAN_POINT('Ctrl Pts',(-67.7385002254718,8.33082229499641,-47.6922674992038));
#29677=CARTESIAN_POINT('Ctrl Pts',(-67.739244988589,8.33666447214043,-47.9613494799267));
#29678=CARTESIAN_POINT('Ctrl Pts',(-67.7408837362312,8.35320967438326,-48.4863334714169));
#29679=CARTESIAN_POINT('Ctrl Pts',(-67.7441271193585,8.3925774158339,-49.3956976463571));
#29680=CARTESIAN_POINT('Ctrl Pts',(-67.75007447448,8.46278740267436,-50.6532900551304));
#29681=CARTESIAN_POINT('Ctrl Pts',(-67.759310281912,8.52447858594555,-52.1005349938358));
#29682=CARTESIAN_POINT('Ctrl Pts',(-67.7663979457576,8.52396820704625,-53.0212590273571));
#29683=CARTESIAN_POINT('Ctrl Pts',(-67.7707986217468,8.50358566761648,-53.5830646349072));
#29684=CARTESIAN_POINT('Ctrl Pts',(-67.7724421193683,8.49258175718754,-53.7821557918875));
#29685=CARTESIAN_POINT('Ctrl Pts',(-67.776029352105,8.45571054118338,-54.2131754916418));
#29686=CARTESIAN_POINT('Ctrl Pts',(-67.7832589050826,8.35677044352376,-54.9979892349162));
#29687=CARTESIAN_POINT('Ctrl Pts',(-67.8019983761006,8.06391832573667,-56.7195146620943));
#29688=CARTESIAN_POINT('Ctrl Pts',(-67.8248629176182,7.81231491994759,-58.4320640413801));
#29689=CARTESIAN_POINT('Ctrl Pts',(-67.8290231786131,7.89213968485429,-59.7675454191527));
#29690=CARTESIAN_POINT('Ctrl Pts',(-67.829637938248,7.90175378771661,-59.9093328492615));
#29691=CARTESIAN_POINT('Ctrl Pts',(-67.8306102124591,7.92555044535696,-60.2032942620685));
#29692=CARTESIAN_POINT('Ctrl Pts',(-67.8319358606205,7.97692831211166,-60.7093669674856));
#29693=CARTESIAN_POINT('Ctrl Pts',(-67.8330666988999,8.11775658317007,-61.7148057960873));
#29694=CARTESIAN_POINT('Ctrl Pts',(-67.8318365893804,8.3544189694753,-62.8347014563645));
#29695=CARTESIAN_POINT('Ctrl Pts',(-67.8295768244033,8.64714320487281,-63.9267786658913));
#29696=CARTESIAN_POINT('Ctrl Pts',(-67.8281626669886,8.82939642463849,-64.5296542650456));
#29697=CARTESIAN_POINT('Ctrl Pts',(-67.8272594889568,8.95681621745233,-64.9268322635415));
#29698=CARTESIAN_POINT('Ctrl Pts',(-67.8266742594514,9.04324888375184,-65.1902959131685));
#29699=CARTESIAN_POINT('Ctrl Pts',(-67.8261190407547,9.13180490501319,-65.4519052012751));
#29700=CARTESIAN_POINT('Ctrl Pts',(-67.8256806306326,9.21087657959977,-65.6790191260735));
#29701=CARTESIAN_POINT('Ctrl Pts',(-67.8254455665297,9.25648173733892,-65.8082917862273));
#29702=CARTESIAN_POINT('Ctrl Pts',(-67.8251080419102,9.32530480735155,-66.0017184022138));
#29703=CARTESIAN_POINT('Ctrl Pts',(-67.8248651643453,9.38345347502709,-66.1618155768751));
#29704=CARTESIAN_POINT('Ctrl Pts',(-67.8244897857844,9.48086408035106,-66.4261113164743));
#29705=CARTESIAN_POINT('Ctrl Pts',(-67.8223265957053,9.59820115895211,-66.7305377189812));
#29706=CARTESIAN_POINT('Ctrl Pts',(-67.8190059950224,9.8402199531971,-67.3072625970374));
#29707=CARTESIAN_POINT('Ctrl Pts',(-67.8129978099209,10.2993889138899,-68.2955787840444));
#29708=CARTESIAN_POINT('Ctrl Pts',(-67.8042650502226,11.300383254939,-70.1535168902183));
#29709=CARTESIAN_POINT('Ctrl Pts',(-67.8049715146091,12.1759405893878,-71.6137976724565));
#29710=CARTESIAN_POINT('Ctrl Pts',(-67.8104043429099,12.7300091438892,-72.6661690854145));
#29711=CARTESIAN_POINT('Ctrl Pts',(-67.8099292386307,12.865668301269,-72.9238530002178));
#29712=CARTESIAN_POINT('Ctrl Pts',(-67.8099657471829,13.1304995285569,-73.4254283169777));
#29713=CARTESIAN_POINT('Ctrl Pts',(-67.8096453736191,13.4650631962054,-74.0571725682281));
#29714=CARTESIAN_POINT('Ctrl Pts',(-67.8095307834107,13.8657451167143,-74.81106786658));
#29715=CARTESIAN_POINT('Ctrl Pts',(-67.8092764976037,14.6688673763839,-76.318637675562));
#29716=CARTESIAN_POINT('Ctrl Pts',(-67.8093100673287,15.3382645987951,-77.5711925792361));
#29717=CARTESIAN_POINT('Ctrl Pts',(-67.8095751893663,16.3061996227081,-79.3917515175623));
#29718=CARTESIAN_POINT('Ctrl Pts',(-67.8094597961512,16.743542771233,-80.2144112531435));
#29719=CARTESIAN_POINT('Ctrl Pts',(-67.8094597961536,17.1800643586234,-81.0353889552398));
#29720=CARTESIAN_POINT('Ctrl Pts',(-65.0350898325616,3.04280014736699,24.8318418817188));
#29721=CARTESIAN_POINT('Ctrl Pts',(-65.035302902329,3.04280068956435,24.7830007108261));
#29722=CARTESIAN_POINT('Ctrl Pts',(-65.0355263318473,3.0428012433223,24.7341611475317));
#29723=CARTESIAN_POINT('Ctrl Pts',(-65.0381652998135,3.04281055487639,24.1840050646084));
#29724=CARTESIAN_POINT('Ctrl Pts',(-65.0405012624098,3.04221819256434,23.1805167946382));
#29725=CARTESIAN_POINT('Ctrl Pts',(-65.046136422076,3.04039629670115,21.1726954882089));
#29726=CARTESIAN_POINT('Ctrl Pts',(-65.0636892145831,3.04050003718048,19.668687863039));
#29727=CARTESIAN_POINT('Ctrl Pts',(-65.0993528390164,3.04373154009752,18.4175940393545));
#29728=CARTESIAN_POINT('Ctrl Pts',(-65.1167624047629,3.04513799530223,17.916739559878));
#29729=CARTESIAN_POINT('Ctrl Pts',(-65.1610420261281,3.04848022156998,16.914221109985));
#29730=CARTESIAN_POINT('Ctrl Pts',(-65.2560901491897,3.05590136084768,15.1605997557044));
#29731=CARTESIAN_POINT('Ctrl Pts',(-65.3426276974946,3.06567624187454,13.6528135161078));
#29732=CARTESIAN_POINT('Ctrl Pts',(-65.3898854169488,3.07637962508634,12.3899242765431));
#29733=CARTESIAN_POINT('Ctrl Pts',(-65.4085188963124,3.08135345362665,11.8852540838332));
#29734=CARTESIAN_POINT('Ctrl Pts',(-65.4441924276268,3.09334441748007,10.8780247911361));
#29735=CARTESIAN_POINT('Ctrl Pts',(-65.5009212372911,3.11769138469222,9.11918270865987));
#29736=CARTESIAN_POINT('Ctrl Pts',(-65.5344759686303,3.13759494396961,7.61787678554747));
#29737=CARTESIAN_POINT('Ctrl Pts',(-65.5471823475504,3.14577486589797,6.4941358079782));
#29738=CARTESIAN_POINT('Ctrl Pts',(-65.5490064258502,3.14719343720313,6.24591568025131));
#29739=CARTESIAN_POINT('Ctrl Pts',(-65.5493650130214,3.14901199750275,5.7479323737717));
#29740=CARTESIAN_POINT('Ctrl Pts',(-65.5427232865531,3.15003714353534,4.87351085584839));
#29741=CARTESIAN_POINT('Ctrl Pts',(-65.5123332075237,3.1473687997001,3.11538441955382));
#29742=CARTESIAN_POINT('Ctrl Pts',(-65.4950406104052,3.15243776668915,1.59718257170604));
#29743=CARTESIAN_POINT('Ctrl Pts',(-65.5195969730143,3.16718209086072,0.529985838135656));
#29744=CARTESIAN_POINT('Ctrl Pts',(-65.5229264725584,3.168044097656,0.428401865576983));
#29745=CARTESIAN_POINT('Ctrl Pts',(-65.5308531279283,3.16715647935709,0.20693437589857));
#29746=CARTESIAN_POINT('Ctrl Pts',(-65.5479649445266,3.15891659841762,-0.182152293832136));
#29747=CARTESIAN_POINT('Ctrl Pts',(-65.5803536258395,3.1312880024813,-0.769064702460121));
#29748=CARTESIAN_POINT('Ctrl Pts',(-65.6288080052194,3.08514072014695,-1.51529846596412));
#29749=CARTESIAN_POINT('Ctrl Pts',(-65.7009443438072,3.02971820738691,-2.57286938657852));
#29750=CARTESIAN_POINT('Ctrl Pts',(-65.7958702426753,3.02141716607343,-4.01464059995897));
#29751=CARTESIAN_POINT('Ctrl Pts',(-65.8339671111026,3.21413230294904,-5.28558894656125));
#29752=CARTESIAN_POINT('Ctrl Pts',(-65.8290177318522,3.43646413138794,-6.09719401145983));
#29753=CARTESIAN_POINT('Ctrl Pts',(-65.8247331963601,3.54288486877194,-6.43980777047141));
#29754=CARTESIAN_POINT('Ctrl Pts',(-65.8126150415913,3.78785976564052,-7.07974275656304));
#29755=CARTESIAN_POINT('Ctrl Pts',(-65.7825405638733,4.28935048702146,-8.13424291300961));
#29756=CARTESIAN_POINT('Ctrl Pts',(-65.7262822211076,5.10673621212295,-9.47955334379582));
#29757=CARTESIAN_POINT('Ctrl Pts',(-65.6776040037731,5.87382394656201,-10.6881581647769));
#29758=CARTESIAN_POINT('Ctrl Pts',(-65.6530788862006,6.29690400402921,-11.4492892101479));
#29759=CARTESIAN_POINT('Ctrl Pts',(-65.6402560174144,6.4939315689468,-11.8545382815407));
#29760=CARTESIAN_POINT('Ctrl Pts',(-65.6338099852804,6.57563946285295,-12.0455045702372));
#29761=CARTESIAN_POINT('Ctrl Pts',(-65.6284734069914,6.63058551780554,-12.1854030496931));
#29762=CARTESIAN_POINT('Ctrl Pts',(-65.6190428236937,6.67764656971381,-12.3120037968729));
#29763=CARTESIAN_POINT('Ctrl Pts',(-65.6011861723993,6.76260038308683,-12.546849040613));
#29764=CARTESIAN_POINT('Ctrl Pts',(-65.5631649581857,6.90664395919742,-12.9665027856001));
#29765=CARTESIAN_POINT('Ctrl Pts',(-65.4439714345449,7.23556311786381,-14.0348885563294));
#29766=CARTESIAN_POINT('Ctrl Pts',(-65.2467963721198,7.50697144292392,-15.2036317173101));
#29767=CARTESIAN_POINT('Ctrl Pts',(-65.0613545935836,7.72730267070285,-16.3447670932083));
#29768=CARTESIAN_POINT('Ctrl Pts',(-64.9821956515023,7.82439148941587,-16.9129981157234));
#29769=CARTESIAN_POINT('Ctrl Pts',(-64.9318219661531,7.8931744738948,-17.3665625853196));
#29770=CARTESIAN_POINT('Ctrl Pts',(-64.9119293832766,7.92424621796352,-17.5936131468181));
#29771=CARTESIAN_POINT('Ctrl Pts',(-64.8993383270352,7.94603558521596,-17.7629146706841));
#29772=CARTESIAN_POINT('Ctrl Pts',(-64.8917663759709,7.95771535157678,-17.8627678181602));
#29773=CARTESIAN_POINT('Ctrl Pts',(-64.87829843768,7.97934358488809,-18.0718376780894));
#29774=CARTESIAN_POINT('Ctrl Pts',(-64.8675416986687,7.99634477320552,-18.2813039514666));
#29775=CARTESIAN_POINT('Ctrl Pts',(-64.8591829295582,8.00964496385992,-18.4954415917632));
#29776=CARTESIAN_POINT('Ctrl Pts',(-64.8549247713441,8.0163398028745,-18.6303160118129));
#29777=CARTESIAN_POINT('Ctrl Pts',(-64.8520602728037,8.02081409894711,-18.7391625487916));
#29778=CARTESIAN_POINT('Ctrl Pts',(-64.8495487097806,8.02469632094482,-18.8485295460239));
#29779=CARTESIAN_POINT('Ctrl Pts',(-64.8440461098093,8.03303268000617,-19.1515639158718));
#29780=CARTESIAN_POINT('Ctrl Pts',(-64.8422307342923,8.03444083547476,-19.660002172546));
#29781=CARTESIAN_POINT('Ctrl Pts',(-64.8535639039286,8.01101137755237,-20.5996246908767));
#29782=CARTESIAN_POINT('Ctrl Pts',(-64.8837685193248,7.95104762462188,-21.8412729116947));
#29783=CARTESIAN_POINT('Ctrl Pts',(-64.9003385408341,7.91656250618651,-22.9055157959435));
#29784=CARTESIAN_POINT('Ctrl Pts',(-64.9002603399163,7.91612971996068,-23.5899652055116));
#29785=CARTESIAN_POINT('Ctrl Pts',(-64.9002853704511,7.91597419274655,-23.8329246327572));
#29786=CARTESIAN_POINT('Ctrl Pts',(-64.9005209396592,7.91570372462549,-24.3354228327737));
#29787=CARTESIAN_POINT('Ctrl Pts',(-64.9013496705288,7.91533419006428,-25.2086189396213));
#29788=CARTESIAN_POINT('Ctrl Pts',(-64.9032377813096,7.91505426902946,-26.4649260715607));
#29789=CARTESIAN_POINT('Ctrl Pts',(-64.9051420818175,7.91497359547895,-27.9727284482595));
#29790=CARTESIAN_POINT('Ctrl Pts',(-64.9051740451273,7.91509119634508,-28.977928229516));
#29791=CARTESIAN_POINT('Ctrl Pts',(-64.9045909343935,7.91517658969557,-29.542350523228));
#29792=CARTESIAN_POINT('Ctrl Pts',(-64.9044396788063,7.9151974629864,-29.6678590219361));
#29793=CARTESIAN_POINT('Ctrl Pts',(-64.9040502584897,7.91524698093661,-29.9188765931247));
#29794=CARTESIAN_POINT('Ctrl Pts',(-64.9031570090159,7.91535731016294,-30.3582616791647));
#29795=CARTESIAN_POINT('Ctrl Pts',(-64.9006542075357,7.91565738205601,-31.2372934259634));
#29796=CARTESIAN_POINT('Ctrl Pts',(-64.896738035002,7.91617210820649,-32.241954517403));
#29797=CARTESIAN_POINT('Ctrl Pts',(-64.8929410178614,7.91678557699602,-33.2456522570364));
#29798=CARTESIAN_POINT('Ctrl Pts',(-64.8904447143674,7.91727679017316,-33.9976902843502));
#29799=CARTESIAN_POINT('Ctrl Pts',(-64.8885837756887,7.91779832763919,-34.7485988495637));
#29800=CARTESIAN_POINT('Ctrl Pts',(-64.8879625001898,7.91814877453707,-35.2483027153575));
#29801=CARTESIAN_POINT('Ctrl Pts',(-64.8878017993677,7.91840737253542,-35.6236749304173));
#29802=CARTESIAN_POINT('Ctrl Pts',(-64.8877802039006,7.91856704600513,-35.8749658786825));
#29803=CARTESIAN_POINT('Ctrl Pts',(-64.8880462852168,7.9188457091825,-36.3770736455709));
#29804=CARTESIAN_POINT('Ctrl Pts',(-64.8892204145641,7.91926455578023,-37.2544471887489));
#29805=CARTESIAN_POINT('Ctrl Pts',(-64.8936647430139,7.9200396565448,-39.0063061870146));
#29806=CARTESIAN_POINT('Ctrl Pts',(-64.8984157168729,7.92143147742256,-40.509206742286));
#29807=CARTESIAN_POINT('Ctrl Pts',(-64.8998413822583,7.92366309995064,-41.6425605863139));
#29808=CARTESIAN_POINT('Ctrl Pts',(-64.9000866589177,7.92398502833008,-41.8904057678773));
#29809=CARTESIAN_POINT('Ctrl Pts',(-64.9002737319323,7.92407597064351,-42.2644534304189));
#29810=CARTESIAN_POINT('Ctrl Pts',(-64.9003153064097,7.92387393480418,-42.6389519048891));
#29811=CARTESIAN_POINT('Ctrl Pts',(-64.9002215464106,7.92335187953369,-43.1396736261026));
#29812=CARTESIAN_POINT('Ctrl Pts',(-64.8999102341496,7.92248272763674,-43.7674421035051));
#29813=CARTESIAN_POINT('Ctrl Pts',(-64.899497759237,7.92192117742467,-44.5234680179482));
#29814=CARTESIAN_POINT('Ctrl Pts',(-64.899347390088,7.92254946999201,-45.1552451948918));
#29815=CARTESIAN_POINT('Ctrl Pts',(-64.8994781936819,7.92413700201671,-45.6614762962492));
#29816=CARTESIAN_POINT('Ctrl Pts',(-64.8997354762577,7.92597313553899,-46.0415025358713));
#29817=CARTESIAN_POINT('Ctrl Pts',(-64.9001857038644,7.92856083162908,-46.421796828405));
#29818=CARTESIAN_POINT('Ctrl Pts',(-64.9010872471559,7.93316033089061,-46.929200310135));
#29819=CARTESIAN_POINT('Ctrl Pts',(-64.9021548477992,7.9380492543922,-47.3098695287838));
#29820=CARTESIAN_POINT('Ctrl Pts',(-64.9035504526263,7.94414913770834,-47.6919428942751));
#29821=CARTESIAN_POINT('Ctrl Pts',(-64.9045064456491,7.94995809963907,-47.9608562576491));
#29822=CARTESIAN_POINT('Ctrl Pts',(-64.9066519832131,7.96638697291171,-48.4855609721244));
#29823=CARTESIAN_POINT('Ctrl Pts',(-64.9109876462315,8.00543160879661,-49.3944875787079));
#29824=CARTESIAN_POINT('Ctrl Pts',(-64.9189903444601,8.0749488016112,-50.6516519938867));
#29825=CARTESIAN_POINT('Ctrl Pts',(-64.9311863309774,8.13570078670839,-52.0986881422973));
#29826=CARTESIAN_POINT('Ctrl Pts',(-64.9404083729074,8.13464902825682,-53.0195058759792));
#29827=CARTESIAN_POINT('Ctrl Pts',(-64.9461372024873,8.11398242139807,-53.5814415216747));
#29828=CARTESIAN_POINT('Ctrl Pts',(-64.9483487490898,8.1028928551161,-53.7803715381629));
#29829=CARTESIAN_POINT('Ctrl Pts',(-64.9531816256131,8.06580685780084,-54.2112458480708));
#29830=CARTESIAN_POINT('Ctrl Pts',(-64.9628262208506,7.96642573989521,-54.9958597311264));
#29831=CARTESIAN_POINT('Ctrl Pts',(-64.9868870921632,7.672416767481,-56.7174028589548));
#29832=CARTESIAN_POINT('Ctrl Pts',(-65.0139477942561,7.41958191668347,-58.4304548950946));
#29833=CARTESIAN_POINT('Ctrl Pts',(-65.0196865912844,7.49908850817287,-59.7667398161207));
#29834=CARTESIAN_POINT('Ctrl Pts',(-65.020481436181,7.50867553992863,-59.9086131229831));
#29835=CARTESIAN_POINT('Ctrl Pts',(-65.0217813215993,7.53242952457539,-60.2027427012463));
#29836=CARTESIAN_POINT('Ctrl Pts',(-65.023594649291,7.58377340038694,-60.7090829018234));
#29837=CARTESIAN_POINT('Ctrl Pts',(-65.0253943628937,7.72466231531237,-61.7149615900748));
#29838=CARTESIAN_POINT('Ctrl Pts',(-65.0243823691169,7.96159119512331,-62.8351398823737));
#29839=CARTESIAN_POINT('Ctrl Pts',(-65.0220992216398,8.25460190105227,-63.9273046292012));
#29840=CARTESIAN_POINT('Ctrl Pts',(-65.0206361906803,8.43699629962348,-64.530160675701));
#29841=CARTESIAN_POINT('Ctrl Pts',(-65.0197085039787,8.56449059280231,-64.9272980267861));
#29842=CARTESIAN_POINT('Ctrl Pts',(-65.0191104802244,8.65096692107261,-65.1907272591478));
#29843=CARTESIAN_POINT('Ctrl Pts',(-65.018550261451,8.73955692474373,-65.4522913336752));
#29844=CARTESIAN_POINT('Ctrl Pts',(-65.018117988003,8.81864760344354,-65.6793561212113));
#29845=CARTESIAN_POINT('Ctrl Pts',(-65.0178900129609,8.86426034018339,-65.8085979580986));
#29846=CARTESIAN_POINT('Ctrl Pts',(-65.0175669761628,8.93309138951526,-66.0019756870505));
#29847=CARTESIAN_POINT('Ctrl Pts',(-65.0173448198335,8.99123936368044,-66.1620262154104));
#29848=CARTESIAN_POINT('Ctrl Pts',(-65.0170182798613,9.08863836597457,-66.4262390909692));
#29849=CARTESIAN_POINT('Ctrl Pts',(-65.0149069291614,9.20600383637598,-66.7306832709554));
#29850=CARTESIAN_POINT('Ctrl Pts',(-65.0116654762018,9.44804813625744,-67.3073862996916));
#29851=CARTESIAN_POINT('Ctrl Pts',(-65.0057472173816,9.90725703304797,-68.2956966704029));
#29852=CARTESIAN_POINT('Ctrl Pts',(-64.9970218138309,10.9082659234554,-70.1536088847422));
#29853=CARTESIAN_POINT('Ctrl Pts',(-64.9975725442118,11.7837973669017,-71.6138988712409));
#29854=CARTESIAN_POINT('Ctrl Pts',(-65.0029615035976,12.3378656929601,-72.6662798162345));
#29855=CARTESIAN_POINT('Ctrl Pts',(-65.0024890581818,12.4735259545828,-72.9239616761582));
#29856=CARTESIAN_POINT('Ctrl Pts',(-65.0025241219137,12.7383580418874,-73.4255354309714));
#29857=CARTESIAN_POINT('Ctrl Pts',(-65.0022053822186,13.0729224209133,-74.057277442144));
#29858=CARTESIAN_POINT('Ctrl Pts',(-65.0020916724498,13.4736037880218,-74.8111709421753));
#29859=CARTESIAN_POINT('Ctrl Pts',(-65.0018405734174,14.2767237520025,-76.3187381452471));
#29860=CARTESIAN_POINT('Ctrl Pts',(-65.0018764663666,14.9461187817725,-77.5712949176202));
#29861=CARTESIAN_POINT('Ctrl Pts',(-65.002139456689,15.914055900774,-79.3918586263518));
#29862=CARTESIAN_POINT('Ctrl Pts',(-65.0020250127354,16.3513988662646,-80.214517422021));
#29863=CARTESIAN_POINT('Ctrl Pts',(-65.0020250127364,16.7879204536536,-81.0354951241211));
#29864=CARTESIAN_POINT('Ctrl Pts',(-62.2324116460955,2.65110845064529,24.8313037818064));
#29865=CARTESIAN_POINT('Ctrl Pts',(-62.2325721397915,2.65111459129155,24.7824460238289));
#29866=CARTESIAN_POINT('Ctrl Pts',(-62.2327405043154,2.65112099191732,24.73358971044));
#29867=CARTESIAN_POINT('Ctrl Pts',(-62.2347287307477,2.6511997461256,24.1832352226466));
#29868=CARTESIAN_POINT('Ctrl Pts',(-62.2357093212771,2.65089278229138,23.1793101976511));
#29869=CARTESIAN_POINT('Ctrl Pts',(-62.2376383378861,2.64989439785791,21.1712233896418));
#29870=CARTESIAN_POINT('Ctrl Pts',(-62.2508930908442,2.65046521052102,19.6674111041318));
#29871=CARTESIAN_POINT('Ctrl Pts',(-62.2817163866741,2.65351012755467,18.4166246433661));
#29872=CARTESIAN_POINT('Ctrl Pts',(-62.2963498662037,2.65475210555508,17.9154924339037));
#29873=CARTESIAN_POINT('Ctrl Pts',(-62.3328704055141,2.65747355900587,16.9126547008369));
#29874=CARTESIAN_POINT('Ctrl Pts',(-62.4114012635184,2.66334020002405,15.1583826347409));
#29875=CARTESIAN_POINT('Ctrl Pts',(-62.4886607515688,2.67186631265648,13.6513035950692));
#29876=CARTESIAN_POINT('Ctrl Pts',(-62.5416546928848,2.68272729508388,12.3900260632852));
#29877=CARTESIAN_POINT('Ctrl Pts',(-62.5639055963637,2.68778477047206,11.8862901822519));
#29878=CARTESIAN_POINT('Ctrl Pts',(-62.6111307572197,2.70009687692735,10.8805271797224));
#29879=CARTESIAN_POINT('Ctrl Pts',(-62.6965536074913,2.72558808356462,9.12351965611986));
#29880=CARTESIAN_POINT('Ctrl Pts',(-62.7597622091768,2.74792172877984,7.62112790962481));
#29881=CARTESIAN_POINT('Ctrl Pts',(-62.7870470844756,2.75842119570929,6.49441772086995));
#29882=CARTESIAN_POINT('Ctrl Pts',(-62.7926887858624,2.76084923498194,6.24239217728173));
#29883=CARTESIAN_POINT('Ctrl Pts',(-62.8024673870572,2.76583093688162,5.73982653503197));
#29884=CARTESIAN_POINT('Ctrl Pts',(-62.8158649336197,2.77467005108555,4.85939849009647));
#29885=CARTESIAN_POINT('Ctrl Pts',(-62.8293424671233,2.79097056893532,3.10187317395191));
#29886=CARTESIAN_POINT('Ctrl Pts',(-62.8245365118151,2.79542564198213,1.60674978984311));
#29887=CARTESIAN_POINT('Ctrl Pts',(-62.8215989110629,2.79042377416418,0.562687943733352));
#29888=CARTESIAN_POINT('Ctrl Pts',(-62.8210181295631,2.78909536304729,0.458688210000553));
#29889=CARTESIAN_POINT('Ctrl Pts',(-62.819099431748,2.78353737887463,0.235639356286997));
#29890=CARTESIAN_POINT('Ctrl Pts',(-62.8139133497516,2.76682228410439,-0.156856655635209));
#29891=CARTESIAN_POINT('Ctrl Pts',(-62.8023804930994,2.7264976388699,-0.744805113266516));
#29892=CARTESIAN_POINT('Ctrl Pts',(-62.7849338452555,2.66393700041982,-1.4860279378941));
#29893=CARTESIAN_POINT('Ctrl Pts',(-62.7601070118959,2.58128821569208,-2.52537755151352));
#29894=CARTESIAN_POINT('Ctrl Pts',(-62.7319192302486,2.51604604164048,-3.91937798362081));
#29895=CARTESIAN_POINT('Ctrl Pts',(-62.7291090615613,2.61098576196056,-5.14442232357788));
#29896=CARTESIAN_POINT('Ctrl Pts',(-62.7362675602417,2.75758588449044,-5.93636656089618));
#29897=CARTESIAN_POINT('Ctrl Pts',(-62.7417753230037,2.82176011428813,-6.2451480087076));
#29898=CARTESIAN_POINT('Ctrl Pts',(-62.7599177726702,2.97657823602182,-6.85273841030402));
#29899=CARTESIAN_POINT('Ctrl Pts',(-62.8061257130493,3.30597747396704,-7.8806422937015));
#29900=CARTESIAN_POINT('Ctrl Pts',(-62.886404686147,3.89707297725855,-9.25228695764434));
#29901=CARTESIAN_POINT('Ctrl Pts',(-62.9397838682818,4.52675217606724,-10.5119105373165));
#29902=CARTESIAN_POINT('Ctrl Pts',(-62.9483184928025,4.9285398956449,-11.3479111829804));
#29903=CARTESIAN_POINT('Ctrl Pts',(-62.9426336815654,5.1384643004547,-11.8136597118286));
#29904=CARTESIAN_POINT('Ctrl Pts',(-62.9358884122851,5.23527166805804,-12.0423095827426));
#29905=CARTESIAN_POINT('Ctrl Pts',(-62.9289577891853,5.30491065956518,-12.2140201328765));
#29906=CARTESIAN_POINT('Ctrl Pts',(-62.9178577373982,5.36388019644879,-12.3629837700079));
#29907=CARTESIAN_POINT('Ctrl Pts',(-62.8961711642207,5.47660176938199,-12.638967148117));
#29908=CARTESIAN_POINT('Ctrl Pts',(-62.8501277346565,5.68011028976417,-13.1247575937463));
#29909=CARTESIAN_POINT('Ctrl Pts',(-62.7055635225399,6.20984207111696,-14.3304093147106));
#29910=CARTESIAN_POINT('Ctrl Pts',(-62.4912627490231,6.78243277690134,-15.5747311231459));
#29911=CARTESIAN_POINT('Ctrl Pts',(-62.2993265658437,7.20732218206552,-16.6805172535131));
#29912=CARTESIAN_POINT('Ctrl Pts',(-62.2163843982636,7.37604048928846,-17.1955856354033));
#29913=CARTESIAN_POINT('Ctrl Pts',(-62.1634884800495,7.48082183634278,-17.5834150637111));
#29914=CARTESIAN_POINT('Ctrl Pts',(-62.1425816155528,7.52290086798551,-17.7693030685432));
#29915=CARTESIAN_POINT('Ctrl Pts',(-62.1294522822413,7.55032238942497,-17.9052459033932));
#29916=CARTESIAN_POINT('Ctrl Pts',(-62.1211689409812,7.56758257430452,-17.9980979081998));
#29917=CARTESIAN_POINT('Ctrl Pts',(-62.1060500048589,7.5981531301875,-18.1847897844285));
#29918=CARTESIAN_POINT('Ctrl Pts',(-62.0930999650027,7.62314067975387,-18.3759185051838));
#29919=CARTESIAN_POINT('Ctrl Pts',(-62.0822251853017,7.64282104746964,-18.5711850893019));
#29920=CARTESIAN_POINT('Ctrl Pts',(-62.0762634979292,7.65299423254032,-18.6951881969995));
#29921=CARTESIAN_POINT('Ctrl Pts',(-62.0719773774967,7.65989572394792,-18.7955493623822));
#29922=CARTESIAN_POINT('Ctrl Pts',(-62.0680067906211,7.66598680920003,-18.8967172340001));
#29923=CARTESIAN_POINT('Ctrl Pts',(-62.0583511170679,7.6794882188253,-19.1781798294307));
#29924=CARTESIAN_POINT('Ctrl Pts',(-62.049173484007,7.68432097683299,-19.6572751966255));
#29925=CARTESIAN_POINT('Ctrl Pts',(-62.0471367134705,7.65430605731816,-20.5627028716984));
#29926=CARTESIAN_POINT('Ctrl Pts',(-62.0621562669111,7.56706421088203,-21.7946503974307));
#29927=CARTESIAN_POINT('Ctrl Pts',(-62.0707069159192,7.51367694952985,-22.8859623592707));
#29928=CARTESIAN_POINT('Ctrl Pts',(-62.0669229094418,7.51418611686719,-23.597568395228));
#29929=CARTESIAN_POINT('Ctrl Pts',(-62.065605431171,7.51428478253497,-23.8360696907441));
#29930=CARTESIAN_POINT('Ctrl Pts',(-62.0636147430115,7.51423124901991,-24.3384868425194));
#29931=CARTESIAN_POINT('Ctrl Pts',(-62.0616369095894,7.51353706611234,-25.2077394126351));
#29932=CARTESIAN_POINT('Ctrl Pts',(-62.0621090978214,7.51150180454813,-26.4627222976647));
#29933=CARTESIAN_POINT('Ctrl Pts',(-62.0648367787779,7.50912327519382,-27.9703278206264));
#29934=CARTESIAN_POINT('Ctrl Pts',(-62.0659098354568,7.50876672027581,-28.977760419241));
#29935=CARTESIAN_POINT('Ctrl Pts',(-62.0656790575361,7.50920693270786,-29.5438819590241));
#29936=CARTESIAN_POINT('Ctrl Pts',(-62.0656177966565,7.50931408197146,-29.6694987037349));
#29937=CARTESIAN_POINT('Ctrl Pts',(-62.0654621999351,7.5095788375689,-29.9208665818703));
#29938=CARTESIAN_POINT('Ctrl Pts',(-62.0651093215757,7.51016803327878,-30.3607331353584));
#29939=CARTESIAN_POINT('Ctrl Pts',(-62.0641551731755,7.51178083024612,-31.240593906287));
#29940=CARTESIAN_POINT('Ctrl Pts',(-62.0628134847873,7.51438388641435,-32.2457143097902));
#29941=CARTESIAN_POINT('Ctrl Pts',(-62.0618681293102,7.51721372304941,-33.2494668011189));
#29942=CARTESIAN_POINT('Ctrl Pts',(-62.0615205358396,7.51932631930793,-34.0013374152957));
#29943=CARTESIAN_POINT('Ctrl Pts',(-62.0616936586103,7.52133866738401,-34.7518363686095));
#29944=CARTESIAN_POINT('Ctrl Pts',(-62.0622663291613,7.52252721087467,-35.2511136693746));
#29945=CARTESIAN_POINT('Ctrl Pts',(-62.0629101197002,7.52333089608969,-35.6261195896978));
#29946=CARTESIAN_POINT('Ctrl Pts',(-62.0634331347508,7.52385463467722,-35.877425253617));
#29947=CARTESIAN_POINT('Ctrl Pts',(-62.0648031724192,7.52484270348859,-36.3794168797089));
#29948=CARTESIAN_POINT('Ctrl Pts',(-62.0679373960044,7.52647752632453,-37.256631961613));
#29949=CARTESIAN_POINT('Ctrl Pts',(-62.0762769369191,7.52947490759239,-39.0081317353124));
#29950=CARTESIAN_POINT('Ctrl Pts',(-62.0839209340646,7.53243636888415,-40.5106582147728));
#29951=CARTESIAN_POINT('Ctrl Pts',(-62.0868630236698,7.53555378748421,-41.643760836828));
#29952=CARTESIAN_POINT('Ctrl Pts',(-62.0874273668624,7.53606057387757,-41.8915881473257));
#29953=CARTESIAN_POINT('Ctrl Pts',(-62.0880498730019,7.53641673401846,-42.2655841484734));
#29954=CARTESIAN_POINT('Ctrl Pts',(-62.0884866387515,7.53646362757138,-42.6400314646002));
#29955=CARTESIAN_POINT('Ctrl Pts',(-62.0888701132174,7.53625336732302,-43.140671625036));
#29956=CARTESIAN_POINT('Ctrl Pts',(-62.0890699171536,7.53573296320779,-43.7683224820626));
#29957=CARTESIAN_POINT('Ctrl Pts',(-62.0891578668796,7.53552039690406,-44.524175919851));
#29958=CARTESIAN_POINT('Ctrl Pts',(-62.0893502736129,7.536377762892,-45.1557818376054));
#29959=CARTESIAN_POINT('Ctrl Pts',(-62.0897244006286,7.53810558976392,-45.6618674023183));
#29960=CARTESIAN_POINT('Ctrl Pts',(-62.0901508967091,7.54002629110324,-46.0417759029264));
#29961=CARTESIAN_POINT('Ctrl Pts',(-62.0907601063011,7.54267683770331,-46.4219444887662));
#29962=CARTESIAN_POINT('Ctrl Pts',(-62.0918650416074,7.54733023970297,-46.9291720541025));
#29963=CARTESIAN_POINT('Ctrl Pts',(-62.0930765605595,7.5522247703068,-47.3096923642799));
#29964=CARTESIAN_POINT('Ctrl Pts',(-62.0946204356517,7.55830553645758,-47.6916126248667));
#29965=CARTESIAN_POINT('Ctrl Pts',(-62.0956611667417,7.56408453136268,-47.9603797374788));
#29966=CARTESIAN_POINT('Ctrl Pts',(-62.0979298173075,7.58040451923821,-48.484847683365));
#29967=CARTESIAN_POINT('Ctrl Pts',(-62.1023740335685,7.61914468203589,-49.3934143881785));
#29968=CARTESIAN_POINT('Ctrl Pts',(-62.1103226825369,7.6879833924317,-50.6502627707064));
#29969=CARTESIAN_POINT('Ctrl Pts',(-62.1224187636886,7.74780400354067,-52.0972031986658));
#29970=CARTESIAN_POINT('Ctrl Pts',(-62.1317313561632,7.74616485099686,-53.0181336935282));
#29971=CARTESIAN_POINT('Ctrl Pts',(-62.1376297068955,7.72518476543617,-53.5801910295628));
#29972=CARTESIAN_POINT('Ctrl Pts',(-62.1399046696861,7.71398366576932,-53.7790286012338));
#29973=CARTESIAN_POINT('Ctrl Pts',(-62.1448964229361,7.67663304624389,-54.2098230859811));
#29974=CARTESIAN_POINT('Ctrl Pts',(-62.1548922339695,7.57671267544599,-54.9943108853671));
#29975=CARTESIAN_POINT('Ctrl Pts',(-62.1800038589513,7.2814270625882,-56.7158084727673));
#29976=CARTESIAN_POINT('Ctrl Pts',(-62.2081937086557,7.02731042184774,-58.429179473639));
#29977=CARTESIAN_POINT('Ctrl Pts',(-62.2144449752503,7.10646103808188,-59.766067468225));
#29978=CARTESIAN_POINT('Ctrl Pts',(-62.2153030164495,7.11601834418123,-59.9080059625841));
#29979=CARTESIAN_POINT('Ctrl Pts',(-62.2167297222136,7.13972355599113,-60.2022626238786));
#29980=CARTESIAN_POINT('Ctrl Pts',(-62.2187665552171,7.19102217448749,-60.7088053903155));
#29981=CARTESIAN_POINT('Ctrl Pts',(-62.2210163954321,7.33194976055543,-61.715014065663));
#29982=CARTESIAN_POINT('Ctrl Pts',(-62.2205026710733,7.56912629243654,-62.8353909891454));
#29983=CARTESIAN_POINT('Ctrl Pts',(-62.2186612717354,7.8624139680061,-63.9275925239715));
#29984=CARTESIAN_POINT('Ctrl Pts',(-62.2174192902535,8.04494851939812,-64.5304136453842));
#29985=CARTESIAN_POINT('Ctrl Pts',(-62.2166251202074,8.17251782148038,-64.9275067360983));
#29986=CARTESIAN_POINT('Ctrl Pts',(-62.216112444219,8.25903875171922,-65.1909008318996));
#29987=CARTESIAN_POINT('Ctrl Pts',(-62.2156312875442,8.34766383541202,-65.4524219722881));
#29988=CARTESIAN_POINT('Ctrl Pts',(-62.2152629695985,8.42677531857576,-65.6794422088368));
#29989=CARTESIAN_POINT('Ctrl Pts',(-62.2150699342168,8.47239682514454,-65.8086566631671));
#29990=CARTESIAN_POINT('Ctrl Pts',(-62.2147976898575,8.5412378240164,-66.0019914631938));
#29991=CARTESIAN_POINT('Ctrl Pts',(-62.2146142754426,8.5993869780191,-66.162002122305));
#29992=CARTESIAN_POINT('Ctrl Pts',(-62.2143468843432,8.69677781918142,-66.4261453563042));
#29993=CARTESIAN_POINT('Ctrl Pts',(-62.2122663839657,8.81415583938044,-66.7305933363832));
#29994=CARTESIAN_POINT('Ctrl Pts',(-62.2090735544206,9.05620581596369,-67.3072656757735));
#29995=CARTESIAN_POINT('Ctrl Pts',(-62.2031748317925,9.5154173411655,-68.2955530744696));
#29996=CARTESIAN_POINT('Ctrl Pts',(-62.1943357086957,10.5163936607581,-70.153431298556));
#29997=CARTESIAN_POINT('Ctrl Pts',(-62.1947416310962,11.3919028550599,-71.6137289819733));
#29998=CARTESIAN_POINT('Ctrl Pts',(-62.2001962725638,11.9460021900826,-72.6661254193472));
#29999=CARTESIAN_POINT('Ctrl Pts',(-62.1997204158704,12.0816609576166,-72.9238046059287));
#30000=CARTESIAN_POINT('Ctrl Pts',(-62.1997582965951,12.3464942952452,-73.4253768077921));
#30001=CARTESIAN_POINT('Ctrl Pts',(-62.1994376115016,12.6810575192846,-74.0571160945943));
#30002=CARTESIAN_POINT('Ctrl Pts',(-62.1993228596895,13.0817376901225,-74.8110077756463));
#30003=CARTESIAN_POINT('Ctrl Pts',(-62.1990669571479,13.8848537478945,-76.3185723843615));
#30004=CARTESIAN_POINT('Ctrl Pts',(-62.199097855418,14.5542456499623,-77.5711307629764));
#30005=CARTESIAN_POINT('Ctrl Pts',(-62.1993629968978,15.5221856398195,-79.3916987431088));
#30006=CARTESIAN_POINT('Ctrl Pts',(-62.1992471601886,15.9595275657022,-80.2143563979817));
#30007=CARTESIAN_POINT('Ctrl Pts',(-62.1992471601874,16.3960491530911,-81.0353341000812));
#30008=CARTESIAN_POINT('Ctrl Pts',(-59.4327183968758,2.25265122839169,24.8301364387822));
#30009=CARTESIAN_POINT('Ctrl Pts',(-59.4328841937094,2.25268691728004,24.7812415405472));
#30010=CARTESIAN_POINT('Ctrl Pts',(-59.4330580820664,2.25272429091666,24.7323473839837));
#30011=CARTESIAN_POINT('Ctrl Pts',(-59.4351118929449,2.25316729281828,24.181557485228));
#30012=CARTESIAN_POINT('Ctrl Pts',(-59.4365199278218,2.25376169001701,23.1771798534974));
#30013=CARTESIAN_POINT('Ctrl Pts',(-59.4396851090642,2.25528174738086,21.1682661339047));
#30014=CARTESIAN_POINT('Ctrl Pts',(-59.4533606108111,2.2582303591568,19.6641194136807));
#30015=CARTESIAN_POINT('Ctrl Pts',(-59.4831968696484,2.2632273018724,18.4131228363522));
#30016=CARTESIAN_POINT('Ctrl Pts',(-59.497368126688,2.26566892316074,17.9095299972916));
#30017=CARTESIAN_POINT('Ctrl Pts',(-59.5326978095034,2.27187083435169,16.9049738880677));
#30018=CARTESIAN_POINT('Ctrl Pts',(-59.6084620857887,2.28508910550582,15.1511096465538));
#30019=CARTESIAN_POINT('Ctrl Pts',(-59.6821606761099,2.29665137446202,13.6519191726693));
#30020=CARTESIAN_POINT('Ctrl Pts',(-59.7316230694136,2.30215371628457,12.400859407766));
#30021=CARTESIAN_POINT('Ctrl Pts',(-59.7521813816238,2.30419407380517,11.9013091163657));
#30022=CARTESIAN_POINT('Ctrl Pts',(-59.7951806640273,2.3076825131878,10.9016060004854));
#30023=CARTESIAN_POINT('Ctrl Pts',(-59.8719170049596,2.31235757963235,9.15030985240725));
#30024=CARTESIAN_POINT('Ctrl Pts',(-59.9284132374623,2.31423800236438,7.6443731963254));
#30025=CARTESIAN_POINT('Ctrl Pts',(-59.9544516997608,2.31509003621762,6.51126513178353));
#30026=CARTESIAN_POINT('Ctrl Pts',(-59.9599724708233,2.31518615800477,6.26176931787532));
#30027=CARTESIAN_POINT('Ctrl Pts',(-59.9701066362838,2.31511912260337,5.76118798583747));
#30028=CARTESIAN_POINT('Ctrl Pts',(-59.985437551415,2.31443601950404,4.8834987973579));
#30029=CARTESIAN_POINT('Ctrl Pts',(-60.0066383182567,2.31167052195812,3.1220569861816));
#30030=CARTESIAN_POINT('Ctrl Pts',(-60.0081640503809,2.31040451558357,1.61015252279124));
#30031=CARTESIAN_POINT('Ctrl Pts',(-60.0000054475934,2.31150617065875,0.547312270279649));
#30032=CARTESIAN_POINT('Ctrl Pts',(-59.9987719429314,2.3111616664216,0.432624314911944));
#30033=CARTESIAN_POINT('Ctrl Pts',(-59.9952824755793,2.30882437674471,0.194796398774891));
#30034=CARTESIAN_POINT('Ctrl Pts',(-59.9867324525885,2.30077823544184,-0.22188029869997));
#30035=CARTESIAN_POINT('Ctrl Pts',(-59.968749323234,2.280413820143,-0.830816811594355));
#30036=CARTESIAN_POINT('Ctrl Pts',(-59.9419776451423,2.24997017244242,-1.58054524315636));
#30037=CARTESIAN_POINT('Ctrl Pts',(-59.9045143667982,2.21331131315166,-2.60838361836337));
#30038=CARTESIAN_POINT('Ctrl Pts',(-59.8638638844383,2.1982498490195,-3.94729265834799));
#30039=CARTESIAN_POINT('Ctrl Pts',(-59.8547815312505,2.27162886589833,-5.07663826581443));
#30040=CARTESIAN_POINT('Ctrl Pts',(-59.8613065919288,2.36144504095905,-5.79808564937288));
#30041=CARTESIAN_POINT('Ctrl Pts',(-59.8668073479993,2.3953383972358,-6.05856085757831));
#30042=CARTESIAN_POINT('Ctrl Pts',(-59.8857885375052,2.47309818412149,-6.59755722116751));
#30043=CARTESIAN_POINT('Ctrl Pts',(-59.9370211914893,2.6300323610067,-7.53693441067443));
#30044=CARTESIAN_POINT('Ctrl Pts',(-60.0379558361062,2.9292811235094,-8.89353202373783));
#30045=CARTESIAN_POINT('Ctrl Pts',(-60.1099319053602,3.331710665947,-10.2468365016121));
#30046=CARTESIAN_POINT('Ctrl Pts',(-60.1185712193049,3.65741659751785,-11.1941046587181));
#30047=CARTESIAN_POINT('Ctrl Pts',(-60.1089528756095,3.85487089909554,-11.7360668264736));
#30048=CARTESIAN_POINT('Ctrl Pts',(-60.098819916929,3.95714002352826,-12.0071712114592));
#30049=CARTESIAN_POINT('Ctrl Pts',(-60.0888815169619,4.03583095585652,-12.2124781488849));
#30050=CARTESIAN_POINT('Ctrl Pts',(-60.0770949409152,4.10160480095275,-12.3804934812964));
#30051=CARTESIAN_POINT('Ctrl Pts',(-60.0533580255542,4.23333443500919,-12.6916634318784));
#30052=CARTESIAN_POINT('Ctrl Pts',(-60.0048392844905,4.48159518374812,-13.2286868483013));
#30053=CARTESIAN_POINT('Ctrl Pts',(-59.8591850430779,5.17319095150817,-14.520799126474));
#30054=CARTESIAN_POINT('Ctrl Pts',(-59.6737622709758,6.00239532719331,-15.7921178849206));
#30055=CARTESIAN_POINT('Ctrl Pts',(-59.5263695708326,6.61087952197628,-16.8978869745208));
#30056=CARTESIAN_POINT('Ctrl Pts',(-59.4652314700135,6.84135119363707,-17.3943244839072));
#30057=CARTESIAN_POINT('Ctrl Pts',(-59.4268061379572,6.97398181241572,-17.749766802165));
#30058=CARTESIAN_POINT('Ctrl Pts',(-59.4114107075389,7.02319302665999,-17.9115482795378));
#30059=CARTESIAN_POINT('Ctrl Pts',(-59.4014828487707,7.05388792561121,-18.0266474181241));
#30060=CARTESIAN_POINT('Ctrl Pts',(-59.3941817272012,7.07706386164247,-18.1188593896414));
#30061=CARTESIAN_POINT('Ctrl Pts',(-59.3804739949598,7.11648356283556,-18.29613591791));
#30062=CARTESIAN_POINT('Ctrl Pts',(-59.3672224174604,7.15029696899006,-18.4802941344704));
#30063=CARTESIAN_POINT('Ctrl Pts',(-59.3547804174123,7.17765498290196,-18.6669857253199));
#30064=CARTESIAN_POINT('Ctrl Pts',(-59.3472910192631,7.19246010955654,-18.7859857007086));
#30065=CARTESIAN_POINT('Ctrl Pts',(-59.3415001550889,7.20287995318006,-18.8822616582977));
#30066=CARTESIAN_POINT('Ctrl Pts',(-59.3358379461214,7.2124026048674,-18.9794207952203));
#30067=CARTESIAN_POINT('Ctrl Pts',(-59.3208037727125,7.23494416667871,-19.2500086791216));
#30068=CARTESIAN_POINT('Ctrl Pts',(-59.2992833716582,7.25249328063318,-19.7128242023755));
#30069=CARTESIAN_POINT('Ctrl Pts',(-59.2695945378286,7.23965402392194,-20.5959818589974));
#30070=CARTESIAN_POINT('Ctrl Pts',(-59.2466024375903,7.16395890440845,-21.8137011452256));
#30071=CARTESIAN_POINT('Ctrl Pts',(-59.2332940311674,7.11826912985185,-22.9079220046133));
#30072=CARTESIAN_POINT('Ctrl Pts',(-59.2225001191569,7.12827400914735,-23.6256217875921));
#30073=CARTESIAN_POINT('Ctrl Pts',(-59.2188039915616,7.13106784266876,-23.8586323041846));
#30074=CARTESIAN_POINT('Ctrl Pts',(-59.2130082602853,7.13573882821156,-24.3552887653573));
#30075=CARTESIAN_POINT('Ctrl Pts',(-59.2068812440707,7.14041873824705,-25.2138947714959));
#30076=CARTESIAN_POINT('Ctrl Pts',(-59.2070806050236,7.13979394289298,-26.4598831298544));
#30077=CARTESIAN_POINT('Ctrl Pts',(-59.2140897177481,7.1334418088711,-27.9631595619088));
#30078=CARTESIAN_POINT('Ctrl Pts',(-59.2182024954926,7.13023119006006,-28.9727175728279));
#30079=CARTESIAN_POINT('Ctrl Pts',(-59.2190175697542,7.12994002465576,-29.5412710567716));
#30080=CARTESIAN_POINT('Ctrl Pts',(-59.2192156653274,7.1298651627011,-29.6660415425381));
#30081=CARTESIAN_POINT('Ctrl Pts',(-59.2196582329829,7.12967351296968,-29.9165645862029));
#30082=CARTESIAN_POINT('Ctrl Pts',(-59.220554426431,7.12924881482313,-30.3546981134225));
#30083=CARTESIAN_POINT('Ctrl Pts',(-59.2228155884173,7.12806430740016,-31.231997036665));
#30084=CARTESIAN_POINT('Ctrl Pts',(-59.2263611472526,7.12624875019509,-32.235374646439));
#30085=CARTESIAN_POINT('Ctrl Pts',(-59.2306671790479,7.12438665706793,-33.2388778049522));
#30086=CARTESIAN_POINT('Ctrl Pts',(-59.2342226046425,7.1230697283121,-33.991252883038));
#30087=CARTESIAN_POINT('Ctrl Pts',(-59.2380309975618,7.12198989860983,-34.7429353412321));
#30088=CARTESIAN_POINT('Ctrl Pts',(-59.2407050015639,7.12147796415094,-35.2434716876348));
#30089=CARTESIAN_POINT('Ctrl Pts',(-59.2427536630326,7.12118948900547,-35.6195827369635));
#30090=CARTESIAN_POINT('Ctrl Pts',(-59.2442150573129,7.12099128564165,-35.8708339979703));
#30091=CARTESIAN_POINT('Ctrl Pts',(-59.2474467172818,7.12058821018909,-36.3731721058981));
#30092=CARTESIAN_POINT('Ctrl Pts',(-59.2537730541113,7.11993596026141,-37.2507570133435));
#30093=CARTESIAN_POINT('Ctrl Pts',(-59.2681644576381,7.11887801881393,-39.0032249173688));
#30094=CARTESIAN_POINT('Ctrl Pts',(-59.2800034741358,7.11923691355807,-40.5065455567628));
#30095=CARTESIAN_POINT('Ctrl Pts',(-59.2852313137663,7.12076542512632,-41.6403302586037));
#30096=CARTESIAN_POINT('Ctrl Pts',(-59.2862818754551,7.12092781263791,-41.888235467488));
#30097=CARTESIAN_POINT('Ctrl Pts',(-59.2875768563654,7.12078174250143,-42.2624016805809));
#30098=CARTESIAN_POINT('Ctrl Pts',(-59.2886310108195,7.12034618952707,-42.6370212228559));
#30099=CARTESIAN_POINT('Ctrl Pts',(-59.2897658837102,7.1195230928026,-43.1379181986253));
#30100=CARTESIAN_POINT('Ctrl Pts',(-59.2907736735576,7.11830360101143,-43.7659242265376));
#30101=CARTESIAN_POINT('Ctrl Pts',(-59.2916324835984,7.11738837896993,-44.5222636835069));
#30102=CARTESIAN_POINT('Ctrl Pts',(-59.2923109462295,7.11779890753617,-45.1543211423264));
#30103=CARTESIAN_POINT('Ctrl Pts',(-59.2929838888716,7.11926813498271,-45.6607996901971));
#30104=CARTESIAN_POINT('Ctrl Pts',(-59.2935916966502,7.12104796186459,-46.0410174981501));
#30105=CARTESIAN_POINT('Ctrl Pts',(-59.294340782817,7.12361458503253,-46.4215103632799));
#30106=CARTESIAN_POINT('Ctrl Pts',(-59.2955772293489,7.12823787347396,-46.9291911154372));
#30107=CARTESIAN_POINT('Ctrl Pts',(-59.2968324788671,7.13320605115335,-47.3100738833494));
#30108=CARTESIAN_POINT('Ctrl Pts',(-59.298380648924,7.13943526843574,-47.6923777956218));
#30109=CARTESIAN_POINT('Ctrl Pts',(-59.2993850683031,7.14535407475583,-47.9615186873962));
#30110=CARTESIAN_POINT('Ctrl Pts',(-59.3014603118004,7.16207268876626,-48.4866017625764));
#30111=CARTESIAN_POINT('Ctrl Pts',(-59.3052865602591,7.2017946763055,-49.396129784678));
#30112=CARTESIAN_POINT('Ctrl Pts',(-59.3118230764063,7.2726255534233,-50.6539095926112));
#30113=CARTESIAN_POINT('Ctrl Pts',(-59.322062828193,7.33518684047928,-52.1012995183051));
#30114=CARTESIAN_POINT('Ctrl Pts',(-59.3304629246601,7.33527504366464,-53.0220195395743));
#30115=CARTESIAN_POINT('Ctrl Pts',(-59.3360027967414,7.31527076853847,-53.5837864300138));
#30116=CARTESIAN_POINT('Ctrl Pts',(-59.3381330872285,7.30441091804775,-53.7829838756593));
#30117=CARTESIAN_POINT('Ctrl Pts',(-59.3428400672686,7.26786582493259,-54.214103866335));
#30118=CARTESIAN_POINT('Ctrl Pts',(-59.3523721996777,7.16957046701241,-54.9990388970232));
#30119=CARTESIAN_POINT('Ctrl Pts',(-59.3768268915765,6.87830936594744,-56.7204910521529));
#30120=CARTESIAN_POINT('Ctrl Pts',(-59.4048338955237,6.62818379471605,-58.4327351631704));
#30121=CARTESIAN_POINT('Ctrl Pts',(-59.4111517886009,6.70854270234599,-59.7678509567132));
#30122=CARTESIAN_POINT('Ctrl Pts',(-59.4120270987402,6.71821730117235,-59.9096006552835));
#30123=CARTESIAN_POINT('Ctrl Pts',(-59.4135033187453,6.74212534097523,-60.2034871715157));
#30124=CARTESIAN_POINT('Ctrl Pts',(-59.4156714996854,6.79367095362047,-60.7094406835807));
#30125=CARTESIAN_POINT('Ctrl Pts',(-59.418332233718,6.93474046783409,-61.714678385153));
#30126=CARTESIAN_POINT('Ctrl Pts',(-59.4185131411126,7.17151387462809,-62.8344252992925));
#30127=CARTESIAN_POINT('Ctrl Pts',(-59.4173708025752,7.46427674420058,-63.926424678659));
#30128=CARTESIAN_POINT('Ctrl Pts',(-59.4164873159989,7.64654168063073,-64.5292836353808));
#30129=CARTESIAN_POINT('Ctrl Pts',(-59.4159032525969,7.77397218102938,-64.9264627282968));
#30130=CARTESIAN_POINT('Ctrl Pts',(-59.4155220490055,7.86041325133793,-65.1899303784133));
#30131=CARTESIAN_POINT('Ctrl Pts',(-59.4151581240536,7.94898035286396,-65.4515487293264));
#30132=CARTESIAN_POINT('Ctrl Pts',(-59.4148775961833,8.02806528514184,-65.6786752745147));
#30133=CARTESIAN_POINT('Ctrl Pts',(-59.4147301846656,8.07367923751936,-65.8079565364368));
#30134=CARTESIAN_POINT('Ctrl Pts',(-59.4145216542839,8.14251677800326,-66.0013974175857));
#30135=CARTESIAN_POINT('Ctrl Pts',(-59.4143812193172,8.20068053593941,-66.1615094745568));
#30136=CARTESIAN_POINT('Ctrl Pts',(-59.4141694508199,8.29812039206658,-66.4258331073802));
#30137=CARTESIAN_POINT('Ctrl Pts',(-59.4121184531506,8.41545564797318,-66.7302393110289));
#30138=CARTESIAN_POINT('Ctrl Pts',(-59.4089645320295,8.65747843166566,-67.306955770546));
#30139=CARTESIAN_POINT('Ctrl Pts',(-59.4030611647312,9.11662704675057,-68.295250550469));
#30140=CARTESIAN_POINT('Ctrl Pts',(-59.3940478050956,10.1175438970205,-70.1531811722962));
#30141=CARTESIAN_POINT('Ctrl Pts',(-59.3943023247525,10.9930421956565,-71.6134584512388));
#30142=CARTESIAN_POINT('Ctrl Pts',(-59.3998704182841,11.5471501024684,-72.6658363506855));
#30143=CARTESIAN_POINT('Ctrl Pts',(-59.399388093542,11.6828060367678,-72.9235197213246));
#30144=CARTESIAN_POINT('Ctrl Pts',(-59.3994301178304,11.9476378029523,-73.4250952435116));
#30145=CARTESIAN_POINT('Ctrl Pts',(-59.3991056883216,12.282199468326,-74.056839118302));
#30146=CARTESIAN_POINT('Ctrl Pts',(-59.398988815121,12.6828808223937,-74.8107345944885));
#30147=CARTESIAN_POINT('Ctrl Pts',(-59.3987246047287,13.486001590597,-76.3183046987169));
#30148=CARTESIAN_POINT('Ctrl Pts',(-59.3987492158294,14.1553988360136,-77.5708588961577));
#30149=CARTESIAN_POINT('Ctrl Pts',(-59.3990199465909,15.1233351729319,-79.3914165419536));
#30150=CARTESIAN_POINT('Ctrl Pts',(-59.3989018465541,15.5606776339371,-80.2140760951489));
#30151=CARTESIAN_POINT('Ctrl Pts',(-59.3989018465536,15.9971992213268,-81.0350537972465));
#30152=CARTESIAN_POINT('Ctrl Pts',(-56.6218988576096,1.85135975369098,24.830305945651));
#30153=CARTESIAN_POINT('Ctrl Pts',(-56.6220771208639,1.8513926526504,24.7814164126151));
#30154=CARTESIAN_POINT('Ctrl Pts',(-56.6222640626647,1.85142711473754,24.7325276510878));
#30155=CARTESIAN_POINT('Ctrl Pts',(-56.6244716173778,1.85183533087296,24.1818026226272));
#30156=CARTESIAN_POINT('Ctrl Pts',(-56.6263912846077,1.85233538215404,23.1775909603722));
#30157=CARTESIAN_POINT('Ctrl Pts',(-56.6310064059174,1.85360104451151,21.1687551199745));
#30158=CARTESIAN_POINT('Ctrl Pts',(-56.6456879014065,1.85632152046014,19.6645215090319));
#30159=CARTESIAN_POINT('Ctrl Pts',(-56.6756899000187,1.86116117020704,18.4133896817507));
#30160=CARTESIAN_POINT('Ctrl Pts',(-56.6901377902638,1.86357831767313,17.9098159767833));
#30161=CARTESIAN_POINT('Ctrl Pts',(-56.7265081026977,1.86981384748473,16.9053246703197));
#30162=CARTESIAN_POINT('Ctrl Pts',(-56.8044350008068,1.88316004226665,15.1517241446086));
#30163=CARTESIAN_POINT('Ctrl Pts',(-56.8773927397668,1.89448873086831,13.6526002138188));
#30164=CARTESIAN_POINT('Ctrl Pts',(-56.9212630953127,1.8991353139138,12.4013088335406));
#30165=CARTESIAN_POINT('Ctrl Pts',(-56.9389604936624,1.90075751887008,11.9016148655307));
#30166=CARTESIAN_POINT('Ctrl Pts',(-56.9743053171184,1.90317356758234,10.9016120674607));
#30167=CARTESIAN_POINT('Ctrl Pts',(-57.0340146008934,1.90550527661059,9.14974790695198));
#30168=CARTESIAN_POINT('Ctrl Pts',(-57.0746626133434,1.90517739105699,7.64372859243564));
#30169=CARTESIAN_POINT('Ctrl Pts',(-57.0928894575461,1.90471487948243,6.51107083885909));
#30170=CARTESIAN_POINT('Ctrl Pts',(-57.0965664867556,1.9045157299458,6.26177103197025));
#30171=CARTESIAN_POINT('Ctrl Pts',(-57.1026094896939,1.90371984972078,5.76145104809821));
#30172=CARTESIAN_POINT('Ctrl Pts',(-57.1100269856796,1.90147186159325,4.88416698235186));
#30173=CARTESIAN_POINT('Ctrl Pts',(-57.114427530443,1.89495357174928,3.12305916100058));
#30174=CARTESIAN_POINT('Ctrl Pts',(-57.1081396707823,1.89053916476324,1.61151271554119));
#30175=CARTESIAN_POINT('Ctrl Pts',(-57.1069515118366,1.89320029256016,0.546521062953796));
#30176=CARTESIAN_POINT('Ctrl Pts',(-57.1067193922639,1.89325977797126,0.426774852984043));
#30177=CARTESIAN_POINT('Ctrl Pts',(-57.1059218532478,1.89254980474384,0.182314358857985));
#30178=CARTESIAN_POINT('Ctrl Pts',(-57.1037245963224,1.88931843331046,-0.245591088774696));
#30179=CARTESIAN_POINT('Ctrl Pts',(-57.0987044091975,1.88041735632271,-0.864386774086259));
#30180=CARTESIAN_POINT('Ctrl Pts',(-57.0909665484324,1.86725052592357,-1.61725556496489));
#30181=CARTESIAN_POINT('Ctrl Pts',(-57.0799859241427,1.85266601275522,-2.6357887229553));
#30182=CARTESIAN_POINT('Ctrl Pts',(-57.0681882866568,1.85141583259298,-3.93733134415447));
#30183=CARTESIAN_POINT('Ctrl Pts',(-57.0686338134797,1.8975336049876,-5.01284013637244));
#30184=CARTESIAN_POINT('Ctrl Pts',(-57.0741377233594,1.95117898364246,-5.69407277102527));
#30185=CARTESIAN_POINT('Ctrl Pts',(-57.0782624923922,1.968341193729,-5.92460777169142));
#30186=CARTESIAN_POINT('Ctrl Pts',(-57.0907813565385,2.00329563169115,-6.42030539819386));
#30187=CARTESIAN_POINT('Ctrl Pts',(-57.1223386706861,2.06395766073599,-7.29948928425403));
#30188=CARTESIAN_POINT('Ctrl Pts',(-57.1805994014943,2.17680783090116,-8.6327922182843));
#30189=CARTESIAN_POINT('Ctrl Pts',(-57.2188178486793,2.39767782185249,-10.0481485710067));
#30190=CARTESIAN_POINT('Ctrl Pts',(-57.2135095031993,2.65106102057314,-11.075169803635));
#30191=CARTESIAN_POINT('Ctrl Pts',(-57.1984185480159,2.82983507690918,-11.6693836511967));
#30192=CARTESIAN_POINT('Ctrl Pts',(-57.1864698978013,2.93142771294683,-11.968374134992));
#30193=CARTESIAN_POINT('Ctrl Pts',(-57.1755793884883,3.01319812834117,-12.1949580577661));
#30194=CARTESIAN_POINT('Ctrl Pts',(-57.1646573280793,3.08090027626859,-12.3737171427022));
#30195=CARTESIAN_POINT('Ctrl Pts',(-57.1424559875788,3.22031535553374,-12.7050150981405));
#30196=CARTESIAN_POINT('Ctrl Pts',(-57.0984492701348,3.48882118432202,-13.269768853707));
#30197=CARTESIAN_POINT('Ctrl Pts',(-56.971450424072,4.25779705956758,-14.6036767810547));
#30198=CARTESIAN_POINT('Ctrl Pts',(-56.821616693217,5.2117115170756,-15.8850776230598));
#30199=CARTESIAN_POINT('Ctrl Pts',(-56.7124849345261,5.92568874830589,-16.9994620802121));
#30200=CARTESIAN_POINT('Ctrl Pts',(-56.6705149547657,6.19751789378465,-17.4954244417774));
#30201=CARTESIAN_POINT('Ctrl Pts',(-56.6457436004024,6.35273777337066,-17.8450298557747));
#30202=CARTESIAN_POINT('Ctrl Pts',(-56.6361124070848,6.40938624849264,-18.0006668464923));
#30203=CARTESIAN_POINT('Ctrl Pts',(-56.6297990083521,6.44435211093092,-18.1098859771711));
#30204=CARTESIAN_POINT('Ctrl Pts',(-56.6238224116994,6.47364854166899,-18.2061271424651));
#30205=CARTESIAN_POINT('Ctrl Pts',(-56.6127470082692,6.52310520343213,-18.3863532881278));
#30206=CARTESIAN_POINT('Ctrl Pts',(-56.6010901193704,6.5673566044715,-18.5744851958529));
#30207=CARTESIAN_POINT('Ctrl Pts',(-56.5895322765753,6.60454437832707,-18.763467941586));
#30208=CARTESIAN_POINT('Ctrl Pts',(-56.58224180853,6.62550800540167,-18.8837829985038));
#30209=CARTESIAN_POINT('Ctrl Pts',(-56.5764278031212,6.6407926052895,-18.980842173998));
#30210=CARTESIAN_POINT('Ctrl Pts',(-56.5706154103516,6.65517482885583,-19.078680320108));
#30211=CARTESIAN_POINT('Ctrl Pts',(-56.5546691104267,6.69101365753071,-19.3505992028544));
#30212=CARTESIAN_POINT('Ctrl Pts',(-56.5290614864106,6.73029436785628,-19.8128903368675));
#30213=CARTESIAN_POINT('Ctrl Pts',(-56.4869367980868,6.7568518830943,-20.6888973291557));
#30214=CARTESIAN_POINT('Ctrl Pts',(-56.4440732140486,6.73201820804871,-21.8900996704012));
#30215=CARTESIAN_POINT('Ctrl Pts',(-56.4209020797944,6.72003372304772,-22.9645758384404));
#30216=CARTESIAN_POINT('Ctrl Pts',(-56.4084698223593,6.74461303690916,-23.6666494407614));
#30217=CARTESIAN_POINT('Ctrl Pts',(-56.4044520571116,6.75153694503519,-23.8933220995226));
#30218=CARTESIAN_POINT('Ctrl Pts',(-56.398617957031,6.76311230502334,-24.3786928060929));
#30219=CARTESIAN_POINT('Ctrl Pts',(-56.3939455464681,6.77486749362624,-25.2203664442027));
#30220=CARTESIAN_POINT('Ctrl Pts',(-56.3991641106537,6.77404460420982,-26.4506971606171));
#30221=CARTESIAN_POINT('Ctrl Pts',(-56.4128090599345,6.75952574652236,-27.9490394394889));
#30222=CARTESIAN_POINT('Ctrl Pts',(-56.4186020964461,6.75163853710771,-28.964769856858));
#30223=CARTESIAN_POINT('Ctrl Pts',(-56.4185413807569,6.75071680998041,-29.5392213230429));
#30224=CARTESIAN_POINT('Ctrl Pts',(-56.41850077081,6.75047701527422,-29.6630482265954));
#30225=CARTESIAN_POINT('Ctrl Pts',(-56.4183418667709,6.7498682969808,-29.9130092974894));
#30226=CARTESIAN_POINT('Ctrl Pts',(-56.4178679759819,6.74849085107283,-30.3496443283428));
#30227=CARTESIAN_POINT('Ctrl Pts',(-56.4162669443321,6.74460365616335,-31.2249500551174));
#30228=CARTESIAN_POINT('Ctrl Pts',(-56.4135345404153,6.7382792574658,-32.2268944758849));
#30229=CARTESIAN_POINT('Ctrl Pts',(-56.4110627833574,6.73139160220425,-33.2302213512026));
#30230=CARTESIAN_POINT('Ctrl Pts',(-56.4096388148828,6.72630365081552,-33.9829942708887));
#30231=CARTESIAN_POINT('Ctrl Pts',(-56.4089564710274,6.72171147475502,-34.7356406759868));
#30232=CARTESIAN_POINT('Ctrl Pts',(-56.4091943917731,6.71921902154299,-35.2372017854706));
#30233=CARTESIAN_POINT('Ctrl Pts',(-56.4097070974696,6.71764854985147,-35.6142149941863));
#30234=CARTESIAN_POINT('Ctrl Pts',(-56.4101658912545,6.71661412342689,-35.865417217711));
#30235=CARTESIAN_POINT('Ctrl Pts',(-56.4114906099971,6.71457458211718,-36.368036988799));
#30236=CARTESIAN_POINT('Ctrl Pts',(-56.4147583547514,6.71118598106391,-37.2459301139164));
#30237=CARTESIAN_POINT('Ctrl Pts',(-56.4239222246451,6.70512592455748,-38.9992306282585));
#30238=CARTESIAN_POINT('Ctrl Pts',(-56.4325797483113,6.70211084427062,-40.503204307213));
#30239=CARTESIAN_POINT('Ctrl Pts',(-56.4356597418105,6.70158386685987,-41.637518018572));
#30240=CARTESIAN_POINT('Ctrl Pts',(-56.436227148003,6.70129977242393,-41.8854637139816));
#30241=CARTESIAN_POINT('Ctrl Pts',(-56.4367999559624,6.70050414418084,-42.2597454053479));
#30242=CARTESIAN_POINT('Ctrl Pts',(-56.4371408314556,6.69944454592799,-42.6344827075468));
#30243=CARTESIAN_POINT('Ctrl Pts',(-56.4373510800416,6.69782878260777,-43.135565630316));
#30244=CARTESIAN_POINT('Ctrl Pts',(-56.4372757430818,6.69570282927745,-43.7638437316683));
#30245=CARTESIAN_POINT('Ctrl Pts',(-56.4370272452715,6.69386923707254,-44.520581936709));
#30246=CARTESIAN_POINT('Ctrl Pts',(-56.4370066578341,6.69368485012211,-45.153030469146));
#30247=CARTESIAN_POINT('Ctrl Pts',(-56.4372951630701,6.69479554136445,-45.6598675472249));
#30248=CARTESIAN_POINT('Ctrl Pts',(-56.4377102385364,6.69637061949979,-46.0403728670534));
#30249=CARTESIAN_POINT('Ctrl Pts',(-56.4383715762544,6.69880078721367,-46.4211725489629));
#30250=CARTESIAN_POINT('Ctrl Pts',(-56.4396469866395,6.70333891093526,-46.9292908559997));
#30251=CARTESIAN_POINT('Ctrl Pts',(-56.4411106225019,6.70835911318831,-47.3105250847255));
#30252=CARTESIAN_POINT('Ctrl Pts',(-56.4430182769622,6.71472635597951,-47.6932085369429));
#30253=CARTESIAN_POINT('Ctrl Pts',(-56.4443202971396,6.72078385397459,-47.9627015428219));
#30254=CARTESIAN_POINT('Ctrl Pts',(-56.4471805957533,6.73791561249716,-48.488363057411));
#30255=CARTESIAN_POINT('Ctrl Pts',(-56.452839064889,6.7786876824453,-49.3987692580904));
#30256=CARTESIAN_POINT('Ctrl Pts',(-56.4630087305302,6.8516965935292,-50.6573205793611));
#30257=CARTESIAN_POINT('Ctrl Pts',(-56.478554955567,6.91734142697298,-52.1049636847472));
#30258=CARTESIAN_POINT('Ctrl Pts',(-56.4906652637739,6.91946551340035,-53.0254034352169));
#30259=CARTESIAN_POINT('Ctrl Pts',(-56.4984723795404,6.90065827744901,-53.5868753803797));
#30260=CARTESIAN_POINT('Ctrl Pts',(-56.5016002918511,6.89025157491666,-53.7863134357493));
#30261=CARTESIAN_POINT('Ctrl Pts',(-56.5084824846647,6.85476627102659,-54.2176424541867));
#30262=CARTESIAN_POINT('Ctrl Pts',(-56.5222064261297,6.75859620610259,-55.002900407287));
#30263=CARTESIAN_POINT('Ctrl Pts',(-56.5557188725619,6.47235329506978,-56.7244566461801));
#30264=CARTESIAN_POINT('Ctrl Pts',(-56.5905103920183,6.22672792184383,-58.4359110328748));
#30265=CARTESIAN_POINT('Ctrl Pts',(-56.5993085295866,6.3084712124735,-59.7694917049779));
#30266=CARTESIAN_POINT('Ctrl Pts',(-56.6004698795833,6.31828583588924,-59.9110750466561));
#30267=CARTESIAN_POINT('Ctrl Pts',(-56.6024562371235,6.3424334183536,-60.2046373889052));
#30268=CARTESIAN_POINT('Ctrl Pts',(-56.6053617926738,6.39427272691221,-60.7100762799175));
#30269=CARTESIAN_POINT('Ctrl Pts',(-56.6089382009559,6.5355130961319,-61.7144784683024));
#30270=CARTESIAN_POINT('Ctrl Pts',(-56.6091698803726,6.77181605987139,-62.8337296048277));
#30271=CARTESIAN_POINT('Ctrl Pts',(-56.6076626515125,7.06395772219953,-63.9256374359719));
#30272=CARTESIAN_POINT('Ctrl Pts',(-56.6065228937132,7.24589964597599,-64.5285821372516));
#30273=CARTESIAN_POINT('Ctrl Pts',(-56.6057887546143,7.37315981700677,-64.9258717139614));
#30274=CARTESIAN_POINT('Ctrl Pts',(-56.6053161341454,7.45950133603607,-65.1894268522663));
#30275=CARTESIAN_POINT('Ctrl Pts',(-56.6048767227722,7.54799334393313,-65.451152914096));
#30276=CARTESIAN_POINT('Ctrl Pts',(-56.6045524245517,7.62703929608164,-65.678391165162));
#30277=CARTESIAN_POINT('Ctrl Pts',(-56.6043872291298,7.6726394260606,-65.8077411904003));
#30278=CARTESIAN_POINT('Ctrl Pts',(-56.6041598697884,7.74146499495084,-66.0012899423398));
#30279=CARTESIAN_POINT('Ctrl Pts',(-56.6040204700608,7.79963823627409,-66.1615022228199));
#30280=CARTESIAN_POINT('Ctrl Pts',(-56.6038401398609,7.89712205512293,-66.4260012968152));
#30281=CARTESIAN_POINT('Ctrl Pts',(-56.6018613301423,8.014442436703,-66.7303952892477));
#30282=CARTESIAN_POINT('Ctrl Pts',(-56.598807991678,8.256476084168,-67.307186300956));
#30283=CARTESIAN_POINT('Ctrl Pts',(-56.5930422710428,8.71563585450053,-68.2955341954575));
#30284=CARTESIAN_POINT('Ctrl Pts',(-56.5841020241658,9.71659757217878,-70.1535468005837));
#30285=CARTESIAN_POINT('Ctrl Pts',(-56.5841667701637,10.5920789188348,-71.6137998228524));
#30286=CARTESIAN_POINT('Ctrl Pts',(-56.589609187159,11.1461190431333,-72.6661384045627));
#30287=CARTESIAN_POINT('Ctrl Pts',(-56.589132916731,11.2817778728624,-72.9238283541102));
#30288=CARTESIAN_POINT('Ctrl Pts',(-56.5891691531417,11.5466066026176,-73.4254076537761));
#30289=CARTESIAN_POINT('Ctrl Pts',(-56.5888472189315,11.8811705517907,-74.0571578520545));
#30290=CARTESIAN_POINT('Ctrl Pts',(-56.5887317976132,12.2818546867643,-74.811057703383));
#30291=CARTESIAN_POINT('Ctrl Pts',(-56.5884758996885,13.0849847332041,-76.3186339768239));
#30292=CARTESIAN_POINT('Ctrl Pts',(-56.5885073839689,13.7543894226819,-77.5711826827783));
#30293=CARTESIAN_POINT('Ctrl Pts',(-56.5887725216993,14.7223187302815,-79.3917286320565));
#30294=CARTESIAN_POINT('Ctrl Pts',(-56.5886560510561,15.1596634720437,-80.2143905730094));
#30295=CARTESIAN_POINT('Ctrl Pts',(-56.5886560510566,15.5961850594335,-81.035368275107));
#30296=CARTESIAN_POINT('Ctrl Pts',(-53.7934016121151,1.46777263035546,24.8308339314903));
#30297=CARTESIAN_POINT('Ctrl Pts',(-53.7935673789398,1.46778911572206,24.7819610087646));
#30298=CARTESIAN_POINT('Ctrl Pts',(-53.7937412291651,1.46780639203802,24.7330891581798));
#30299=CARTESIAN_POINT('Ctrl Pts',(-53.7957940605583,1.4680113567613,24.182559255354));
#30300=CARTESIAN_POINT('Ctrl Pts',(-53.7974505746972,1.46806870936156,23.1785615709389));
#30301=CARTESIAN_POINT('Ctrl Pts',(-53.8013623765295,1.46812178194841,21.170090874394));
#30302=CARTESIAN_POINT('Ctrl Pts',(-53.8150194711945,1.46949731762704,19.6659938923605));
#30303=CARTESIAN_POINT('Ctrl Pts',(-53.8435681586524,1.47291723683062,18.4149444354279));
#30304=CARTESIAN_POINT('Ctrl Pts',(-53.8573208660153,1.47453448565679,17.9124519807325));
#30305=CARTESIAN_POINT('Ctrl Pts',(-53.8919646968564,1.47856781673371,16.9087225712457));
#30306=CARTESIAN_POINT('Ctrl Pts',(-53.9662720517638,1.48726824488107,15.154985516567));
#30307=CARTESIAN_POINT('Ctrl Pts',(-54.0360759968836,1.49596967969934,13.6523955194275));
#30308=CARTESIAN_POINT('Ctrl Pts',(-54.0783783253391,1.50214118899151,12.3965940749575));
#30309=CARTESIAN_POINT('Ctrl Pts',(-54.0955196430407,1.50475066335151,11.8950813235525));
#30310=CARTESIAN_POINT('Ctrl Pts',(-54.1299654040665,1.51034842817017,10.8924208756531));
#30311=CARTESIAN_POINT('Ctrl Pts',(-54.1885203186833,1.52060781579293,9.13802848610798));
#30312=CARTESIAN_POINT('Ctrl Pts',(-54.2283839579081,1.52835861779018,7.63360627521497));
#30313=CARTESIAN_POINT('Ctrl Pts',(-54.2457520045372,1.53183396510449,6.50373537823322));
#30314=CARTESIAN_POINT('Ctrl Pts',(-54.2492240717393,1.53257118037915,6.25319826017849));
#30315=CARTESIAN_POINT('Ctrl Pts',(-54.2548282374031,1.53394380346214,5.75188483012969));
#30316=CARTESIAN_POINT('Ctrl Pts',(-54.2614203310286,1.53607147592114,4.87331849088099));
#30317=CARTESIAN_POINT('Ctrl Pts',(-54.2642706333787,1.53913741979663,3.11388667514309));
#30318=CARTESIAN_POINT('Ctrl Pts',(-54.2573573900383,1.53962861673724,1.61024224287674));
#30319=CARTESIAN_POINT('Ctrl Pts',(-54.2557011205212,1.53829310187352,0.55436693754337));
#30320=CARTESIAN_POINT('Ctrl Pts',(-54.2554390849759,1.53794051723846,0.433325589773345));
#30321=CARTESIAN_POINT('Ctrl Pts',(-54.2546681386206,1.53649044292413,0.18795312726425));
#30322=CARTESIAN_POINT('Ctrl Pts',(-54.252728235578,1.53219001729857,-0.241485578503602));
#30323=CARTESIAN_POINT('Ctrl Pts',(-54.2485647358662,1.52204724154832,-0.859857757289458));
#30324=CARTESIAN_POINT('Ctrl Pts',(-54.2423653025322,1.50685522503959,-1.60940139514622));
#30325=CARTESIAN_POINT('Ctrl Pts',(-54.2337702553029,1.48741416699455,-2.61949206742553));
#30326=CARTESIAN_POINT('Ctrl Pts',(-54.2248290290242,1.47379740438393,-3.90374360005717));
#30327=CARTESIAN_POINT('Ctrl Pts',(-54.2237546998493,1.49469271641052,-4.95634090943278));
#30328=CARTESIAN_POINT('Ctrl Pts',(-54.2262898829685,1.52395867016253,-5.62053571048191));
#30329=CARTESIAN_POINT('Ctrl Pts',(-54.2285279466657,1.53131804401625,-5.83575830669255));
#30330=CARTESIAN_POINT('Ctrl Pts',(-54.2359652395121,1.54110790073169,-6.30995058400631));
#30331=CARTESIAN_POINT('Ctrl Pts',(-54.2558568768288,1.54636009588386,-7.15921369100389));
#30332=CARTESIAN_POINT('Ctrl Pts',(-54.2950429819351,1.55409167594932,-8.48036951587064));
#30333=CARTESIAN_POINT('Ctrl Pts',(-54.3205719897746,1.66848273124656,-9.9244522864012));
#30334=CARTESIAN_POINT('Ctrl Pts',(-54.312568655207,1.87351618397868,-10.9933412080439));
#30335=CARTESIAN_POINT('Ctrl Pts',(-54.2978584316208,2.03643173645517,-11.6154728873208));
#30336=CARTESIAN_POINT('Ctrl Pts',(-54.2867628586866,2.13458357810496,-11.9293880794604));
#30337=CARTESIAN_POINT('Ctrl Pts',(-54.2768008071091,2.2156141577047,-12.1672645885673));
#30338=CARTESIAN_POINT('Ctrl Pts',(-54.267494328204,2.28204721859384,-12.3507732600618));
#30339=CARTESIAN_POINT('Ctrl Pts',(-54.2483789945923,2.42117363210546,-12.6918139021029));
#30340=CARTESIAN_POINT('Ctrl Pts',(-54.2107920579036,2.69225073302814,-13.2700414996205));
#30341=CARTESIAN_POINT('Ctrl Pts',(-54.1030771678834,3.48048502493028,-14.6262372115562));
#30342=CARTESIAN_POINT('Ctrl Pts',(-53.9771754176793,4.47676316804508,-15.9132716989074));
#30343=CARTESIAN_POINT('Ctrl Pts',(-53.8897724903015,5.23569685768015,-17.0368058515114));
#30344=CARTESIAN_POINT('Ctrl Pts',(-53.8579894956111,5.52844808758236,-17.5377958305941));
#30345=CARTESIAN_POINT('Ctrl Pts',(-53.8404307262847,5.6977814388372,-17.8914023062076));
#30346=CARTESIAN_POINT('Ctrl Pts',(-53.8339744984258,5.76028275608763,-18.0485841585714));
#30347=CARTESIAN_POINT('Ctrl Pts',(-53.8297703239331,5.79916255628037,-18.1587919495587));
#30348=CARTESIAN_POINT('Ctrl Pts',(-53.8245910442156,5.83333739156381,-18.2602275211408));
#30349=CARTESIAN_POINT('Ctrl Pts',(-53.8152920655446,5.8914731828385,-18.4478752857952));
#30350=CARTESIAN_POINT('Ctrl Pts',(-53.805059196899,5.94520279417078,-18.6438764863963));
#30351=CARTESIAN_POINT('Ctrl Pts',(-53.794731083789,5.99190214459915,-18.8394772679612));
#30352=CARTESIAN_POINT('Ctrl Pts',(-53.7880865359489,6.01898670176359,-18.963714071526));
#30353=CARTESIAN_POINT('Ctrl Pts',(-53.7827277050717,6.0392157203007,-19.0636531415675));
#30354=CARTESIAN_POINT('Ctrl Pts',(-53.7773234858651,6.05859471368721,-19.1642367417344));
#30355=CARTESIAN_POINT('Ctrl Pts',(-53.7623277089261,6.10835396803088,-19.4430827885807));
#30356=CARTESIAN_POINT('Ctrl Pts',(-53.7372415696916,6.17142503101148,-19.9131603160178));
#30357=CARTESIAN_POINT('Ctrl Pts',(-53.6935132011328,6.24222084540794,-20.7924887338115));
#30358=CARTESIAN_POINT('Ctrl Pts',(-53.6442466092503,6.27298426820498,-21.9784669573157));
#30359=CARTESIAN_POINT('Ctrl Pts',(-53.6155684496993,6.29549036050109,-23.021350889866));
#30360=CARTESIAN_POINT('Ctrl Pts',(-53.6024693749055,6.33239130361649,-23.6991293794627));
#30361=CARTESIAN_POINT('Ctrl Pts',(-53.5985819342631,6.34261691041929,-23.9180512590553));
#30362=CARTESIAN_POINT('Ctrl Pts',(-53.5935358905347,6.35913189985168,-24.3889889387686));
#30363=CARTESIAN_POINT('Ctrl Pts',(-53.5918708358186,6.37391540030867,-25.2107698626316));
#30364=CARTESIAN_POINT('Ctrl Pts',(-53.6040498497994,6.36514225940184,-26.4264201050671));
#30365=CARTESIAN_POINT('Ctrl Pts',(-53.6242207361812,6.33345765269652,-27.9280588553213));
#30366=CARTESIAN_POINT('Ctrl Pts',(-53.6295728505492,6.31943683297756,-28.959629391164));
#30367=CARTESIAN_POINT('Ctrl Pts',(-53.6271869297582,6.31970805391784,-29.5468163864961));
#30368=CARTESIAN_POINT('Ctrl Pts',(-53.6265864783266,6.31978287904433,-29.671384628671));
#30369=CARTESIAN_POINT('Ctrl Pts',(-53.6250667987525,6.31996279399016,-29.923847888049));
#30370=CARTESIAN_POINT('Ctrl Pts',(-53.6216319863939,6.32038187020811,-30.3639241508376));
#30371=CARTESIAN_POINT('Ctrl Pts',(-53.6120885474211,6.32156814777126,-31.2451424338698));
#30372=CARTESIAN_POINT('Ctrl Pts',(-53.5969373333556,6.32371858918401,-32.2504383272288));
#30373=CARTESIAN_POINT('Ctrl Pts',(-53.5813612542214,6.32630002720943,-33.2541958950975));
#30374=CARTESIAN_POINT('Ctrl Pts',(-53.5704027525453,6.32832989098395,-34.0057459397616));
#30375=CARTESIAN_POINT('Ctrl Pts',(-53.5610483743253,6.33039553598111,-34.7556974144078));
#30376=CARTESIAN_POINT('Ctrl Pts',(-53.5565139258382,6.33167213419517,-35.2544308736739));
#30377=CARTESIAN_POINT('Ctrl Pts',(-53.5539829777077,6.33254473266672,-35.6289821016848));
#30378=CARTESIAN_POINT('Ctrl Pts',(-53.5524502113088,6.33310500932045,-35.8802919564392));
#30379=CARTESIAN_POINT('Ctrl Pts',(-53.5499879553691,6.3341905553782,-36.3821337994043));
#30380=CARTESIAN_POINT('Ctrl Pts',(-53.5470469584226,6.33605749177594,-37.2591689062186));
#30381=CARTESIAN_POINT('Ctrl Pts',(-53.545611343113,6.33963029040366,-39.0103239055287));
#30382=CARTESIAN_POINT('Ctrl Pts',(-53.5475157379776,6.34317576888129,-40.5124690600292));
#30383=CARTESIAN_POINT('Ctrl Pts',(-53.5463870493891,6.34658591977076,-41.6452248570771));
#30384=CARTESIAN_POINT('Ctrl Pts',(-53.5460466970974,6.34714783542476,-41.8929952917692));
#30385=CARTESIAN_POINT('Ctrl Pts',(-53.5452852331639,6.3475797869505,-42.2668944327146));
#30386=CARTESIAN_POINT('Ctrl Pts',(-53.5443403736996,6.34769293423752,-42.6412473608991));
#30387=CARTESIAN_POINT('Ctrl Pts',(-53.5429130930101,6.34756107786103,-43.1417584080132));
#30388=CARTESIAN_POINT('Ctrl Pts',(-53.5409700056762,6.34712133883608,-43.7692492442951));
#30389=CARTESIAN_POINT('Ctrl Pts',(-53.5388692960199,6.34698370328379,-44.5249144541569));
#30390=CARTESIAN_POINT('Ctrl Pts',(-53.5377154954766,6.347890329422,-45.1563683365974));
#30391=CARTESIAN_POINT('Ctrl Pts',(-53.5373957112746,6.34965487606607,-45.6623434458641));
#30392=CARTESIAN_POINT('Ctrl Pts',(-53.5375169831425,6.35160171309878,-46.0421706147613));
#30393=CARTESIAN_POINT('Ctrl Pts',(-53.538060660001,6.35427798974301,-46.4222597520264));
#30394=CARTESIAN_POINT('Ctrl Pts',(-53.5394265341858,6.35896795642496,-46.9293851512309));
#30395=CARTESIAN_POINT('Ctrl Pts',(-53.541272296068,6.36388958678053,-47.3098256250045));
#30396=CARTESIAN_POINT('Ctrl Pts',(-53.5437818261607,6.37000480373162,-47.6916677590655));
#30397=CARTESIAN_POINT('Ctrl Pts',(-53.5455924689859,6.37580304256165,-47.960337851122));
#30398=CARTESIAN_POINT('Ctrl Pts',(-53.5498248090328,6.39214339623986,-48.4846410143508));
#30399=CARTESIAN_POINT('Ctrl Pts',(-53.5587313083972,6.43088530243379,-49.3929125059758));
#30400=CARTESIAN_POINT('Ctrl Pts',(-53.5755060111104,6.49968058835098,-50.6493696743647));
#30401=CARTESIAN_POINT('Ctrl Pts',(-53.6004972349383,6.55960541879972,-52.0959799952106));
#30402=CARTESIAN_POINT('Ctrl Pts',(-53.6190623160665,6.558232531547,-53.0168836910162));
#30403=CARTESIAN_POINT('Ctrl Pts',(-53.6306238175058,6.53750837149187,-53.5789969700663));
#30404=CARTESIAN_POINT('Ctrl Pts',(-53.6353606964767,6.52646442318359,-53.7776352503713));
#30405=CARTESIAN_POINT('Ctrl Pts',(-53.645734295578,6.48945316580513,-54.2082374321146));
#30406=CARTESIAN_POINT('Ctrl Pts',(-53.6661324091788,6.39020190256059,-54.9924898053466));
#30407=CARTESIAN_POINT('Ctrl Pts',(-53.713710148044,6.09625529604762,-56.7140879374555));
#30408=CARTESIAN_POINT('Ctrl Pts',(-53.7589051895162,5.84293062820704,-58.4280636037592));
#30409=CARTESIAN_POINT('Ctrl Pts',(-53.7715828337572,5.92250213479751,-59.7656855936463));
#30410=CARTESIAN_POINT('Ctrl Pts',(-53.7731656932649,5.93211149096596,-59.9076936967855));
#30411=CARTESIAN_POINT('Ctrl Pts',(-53.77590163928,5.9559156563119,-60.202093386478));
#30412=CARTESIAN_POINT('Ctrl Pts',(-53.7798532617372,6.00737679110324,-60.708865386902));
#30413=CARTESIAN_POINT('Ctrl Pts',(-53.7845893375299,6.14858231987656,-61.7154729716548));
#30414=CARTESIAN_POINT('Ctrl Pts',(-53.7845303613166,6.38597608025257,-62.8361691722631));
#30415=CARTESIAN_POINT('Ctrl Pts',(-53.7821312316756,6.6794062497289,-63.9285641115212));
#30416=CARTESIAN_POINT('Ctrl Pts',(-53.7804431471772,6.86199977133404,-64.5314447099742));
#30417=CARTESIAN_POINT('Ctrl Pts',(-53.7794000606766,6.98960175420206,-64.9285561501802));
#30418=CARTESIAN_POINT('Ctrl Pts',(-53.778740463873,7.07614276013107,-65.1919565016734));
#30419=CARTESIAN_POINT('Ctrl Pts',(-53.7781525663691,7.16478614425998,-65.453475127933));
#30420=CARTESIAN_POINT('Ctrl Pts',(-53.7777420750812,7.2439118387775,-65.6804847015284));
#30421=CARTESIAN_POINT('Ctrl Pts',(-53.77754221375,7.28954106411927,-65.8096905892259));
#30422=CARTESIAN_POINT('Ctrl Pts',(-53.7772782956537,7.35839330495848,-66.0030101040648));
#30423=CARTESIAN_POINT('Ctrl Pts',(-53.7771430125486,7.41655114813598,-66.1630025048135));
#30424=CARTESIAN_POINT('Ctrl Pts',(-53.7770256834519,7.51395693356719,-66.4271098313235));
#30425=CARTESIAN_POINT('Ctrl Pts',(-53.7752148209481,7.63142091921661,-66.7316129850791));
#30426=CARTESIAN_POINT('Ctrl Pts',(-53.7724247277615,7.87358777963525,-67.3083279285345));
#30427=CARTESIAN_POINT('Ctrl Pts',(-53.7670988596911,8.33298698555509,-68.2966879559896));
#30428=CARTESIAN_POINT('Ctrl Pts',(-53.7586990304113,9.33415198459075,-70.1546042763352));
#30429=CARTESIAN_POINT('Ctrl Pts',(-53.7585430513173,10.2095760158847,-71.6149034133299));
#30430=CARTESIAN_POINT('Ctrl Pts',(-53.7635426717601,10.7635372970318,-72.6672677412076));
#30431=CARTESIAN_POINT('Ctrl Pts',(-53.7630975428578,10.8992077037409,-72.9249499844023));
#30432=CARTESIAN_POINT('Ctrl Pts',(-53.7631233115819,11.164039597928,-73.4265220770171));
#30433=CARTESIAN_POINT('Ctrl Pts',(-53.7628216263235,11.4986106864948,-74.0582634495331));
#30434=CARTESIAN_POINT('Ctrl Pts',(-53.7627152736492,11.8992935984681,-74.8121555077136));
#30435=CARTESIAN_POINT('Ctrl Pts',(-53.7624875317562,12.7024162513666,-76.3197207705758));
#30436=CARTESIAN_POINT('Ctrl Pts',(-53.7625345079358,13.3718089832052,-77.5722790747414));
#30437=CARTESIAN_POINT('Ctrl Pts',(-53.7627793283121,14.3397433529917,-79.3928470096629));
#30438=CARTESIAN_POINT('Ctrl Pts',(-53.7626727299908,14.7770883200868,-80.2155053720511));
#30439=CARTESIAN_POINT('Ctrl Pts',(-53.7626727299913,15.2136099074762,-81.0364830741499));
#30440=CARTESIAN_POINT('Ctrl Pts',(-50.9533304548877,1.12167625420265,24.8307786104982));
#30441=CARTESIAN_POINT('Ctrl Pts',(-50.9534791778414,1.12168955436835,24.7819039865689));
#30442=CARTESIAN_POINT('Ctrl Pts',(-50.9536351645509,1.12170348685097,24.7330304228356));
#30443=CARTESIAN_POINT('Ctrl Pts',(-50.9554771492024,1.12186904382061,24.1824800475833));
#30444=CARTESIAN_POINT('Ctrl Pts',(-50.9567903115075,1.12191614443668,23.1784269860304));
#30445=CARTESIAN_POINT('Ctrl Pts',(-50.9597831991283,1.12195817483025,21.1699338582703));
#30446=CARTESIAN_POINT('Ctrl Pts',(-50.9720463860967,1.12307056520977,19.6658727615868));
#30447=CARTESIAN_POINT('Ctrl Pts',(-50.9985453915116,1.1258322201535,18.4148737681668));
#30448=CARTESIAN_POINT('Ctrl Pts',(-51.0112286601023,1.12711396072438,17.9124017236622));
#30449=CARTESIAN_POINT('Ctrl Pts',(-51.0430398380213,1.13025729638921,16.9086671448333));
#30450=CARTESIAN_POINT('Ctrl Pts',(-51.1113070441228,1.13701225441876,15.1548226495192));
#30451=CARTESIAN_POINT('Ctrl Pts',(-51.1766279251767,1.14401741530908,13.6521351888613));
#30452=CARTESIAN_POINT('Ctrl Pts',(-51.2183692549294,1.14950702495355,12.3963110911906));
#30453=CARTESIAN_POINT('Ctrl Pts',(-51.235533688408,1.15187486393477,11.8947961481062));
#30454=CARTESIAN_POINT('Ctrl Pts',(-51.2708463731445,1.15709885931404,10.8921784782769));
#30455=CARTESIAN_POINT('Ctrl Pts',(-51.3326019245734,1.16696112254147,9.13794308818202));
#30456=CARTESIAN_POINT('Ctrl Pts',(-51.3765146408331,1.17472693684257,7.63358702269936));
#30457=CARTESIAN_POINT('Ctrl Pts',(-51.3959170056814,1.17829663045827,6.50362753793607));
#30458=CARTESIAN_POINT('Ctrl Pts',(-51.3999214168377,1.1790868432743,6.2529883040083));
#30459=CARTESIAN_POINT('Ctrl Pts',(-51.4068538864216,1.18062988460862,5.75153998446659));
#30460=CARTESIAN_POINT('Ctrl Pts',(-51.416308115296,1.18319700036463,4.87278314651673));
#30461=CARTESIAN_POINT('Ctrl Pts',(-51.4257086539026,1.18740562053211,3.11320814186707));
#30462=CARTESIAN_POINT('Ctrl Pts',(-51.4216042553005,1.18821623676665,1.61015579346892));
#30463=CARTESIAN_POINT('Ctrl Pts',(-51.4170601115308,1.18643334864416,0.554416805138194));
#30464=CARTESIAN_POINT('Ctrl Pts',(-51.4164071173122,1.18609291103861,0.431151137820113));
#30465=CARTESIAN_POINT('Ctrl Pts',(-51.4146833613188,1.18495731393319,0.182958129310269));
#30466=CARTESIAN_POINT('Ctrl Pts',(-51.410648398026,1.18187759185579,-0.251235209137858));
#30467=CARTESIAN_POINT('Ctrl Pts',(-51.4024023622892,1.17501101039931,-0.873530111729729));
#30468=CARTESIAN_POINT('Ctrl Pts',(-51.3899724528526,1.16476324658724,-1.62384337035073));
#30469=CARTESIAN_POINT('Ctrl Pts',(-51.3718328018968,1.15121190737502,-2.62909007476115));
#30470=CARTESIAN_POINT('Ctrl Pts',(-51.349775001512,1.13928759628803,-3.89638380984962));
#30471=CARTESIAN_POINT('Ctrl Pts',(-51.3405500283101,1.14653419606001,-4.92478128590191));
#30472=CARTESIAN_POINT('Ctrl Pts',(-51.3398462014328,1.15996094032754,-5.57072457193098));
#30473=CARTESIAN_POINT('Ctrl Pts',(-51.3403303336319,1.16146297983544,-5.77679497093547));
#30474=CARTESIAN_POINT('Ctrl Pts',(-51.3434925138929,1.15595023306681,-6.23609588440421));
#30475=CARTESIAN_POINT('Ctrl Pts',(-51.3541939270753,1.12720006963755,-7.0640227164336));
#30476=CARTESIAN_POINT('Ctrl Pts',(-51.3792213771192,1.06540256207554,-8.36907331474427));
#30477=CARTESIAN_POINT('Ctrl Pts',(-51.4015495864027,1.09674921786008,-9.81997961600263));
#30478=CARTESIAN_POINT('Ctrl Pts',(-51.4021396549063,1.25349998557423,-10.9088976947923));
#30479=CARTESIAN_POINT('Ctrl Pts',(-51.3955703314408,1.39477127206225,-11.5458179296493));
#30480=CARTESIAN_POINT('Ctrl Pts',(-51.389614833581,1.48450113854852,-11.8680356774828));
#30481=CARTESIAN_POINT('Ctrl Pts',(-51.3839415996276,1.56015129354294,-12.1121836484828));
#30482=CARTESIAN_POINT('Ctrl Pts',(-51.3787490189213,1.62065297830379,-12.2947777112652));
#30483=CARTESIAN_POINT('Ctrl Pts',(-51.3682634374915,1.74971620528955,-12.6374645040058));
#30484=CARTESIAN_POINT('Ctrl Pts',(-51.3479996635874,2.00356929358392,-13.2179149355049));
#30485=CARTESIAN_POINT('Ctrl Pts',(-51.2905740263312,2.7533922327797,-14.5828839916141));
#30486=CARTESIAN_POINT('Ctrl Pts',(-51.2256668031853,3.71761730434577,-15.8767255584963));
#30487=CARTESIAN_POINT('Ctrl Pts',(-51.1885763414454,4.47878004447763,-17.0163067639913));
#30488=CARTESIAN_POINT('Ctrl Pts',(-51.1770706210893,4.78354992039058,-17.5313964292859));
#30489=CARTESIAN_POINT('Ctrl Pts',(-51.1704850843513,4.96831779110436,-17.9033237884868));
#30490=CARTESIAN_POINT('Ctrl Pts',(-51.167229188462,5.03974550267696,-18.0726583338754));
#30491=CARTESIAN_POINT('Ctrl Pts',(-51.1643018164506,5.08537209352276,-18.1932669922235));
#30492=CARTESIAN_POINT('Ctrl Pts',(-51.1584545999822,5.12564206537231,-18.3047691678594));
#30493=CARTESIAN_POINT('Ctrl Pts',(-51.1471706920195,5.19551761151212,-18.5102585684698));
#30494=CARTESIAN_POINT('Ctrl Pts',(-51.1328002084724,5.26180800197633,-18.7239464425069));
#30495=CARTESIAN_POINT('Ctrl Pts',(-51.116724658712,5.32133053337001,-18.9355650130454));
#30496=CARTESIAN_POINT('Ctrl Pts',(-51.1057684698181,5.35663234480703,-19.0692789356967));
#30497=CARTESIAN_POINT('Ctrl Pts',(-51.0965781524275,5.38352508729994,-19.1763579639075));
#30498=CARTESIAN_POINT('Ctrl Pts',(-51.0870845657283,5.40964501617818,-19.2838035657413));
#30499=CARTESIAN_POINT('Ctrl Pts',(-51.0598271166654,5.4781846475641,-19.5803077367885));
#30500=CARTESIAN_POINT('Ctrl Pts',(-51.0094406856772,5.57381225777003,-20.0721143614749));
#30501=CARTESIAN_POINT('Ctrl Pts',(-50.910575715869,5.70783467344413,-20.9675428096839));
#30502=CARTESIAN_POINT('Ctrl Pts',(-50.7852287604282,5.82925232102871,-22.1337035918646));
#30503=CARTESIAN_POINT('Ctrl Pts',(-50.7156254993263,5.90750715406542,-23.1221787513864));
#30504=CARTESIAN_POINT('Ctrl Pts',(-50.6898345441324,5.9590716867468,-23.7523466442054));
#30505=CARTESIAN_POINT('Ctrl Pts',(-50.6811721509295,5.97338213884854,-23.9610904354294));
#30506=CARTESIAN_POINT('Ctrl Pts',(-50.6681064463434,5.9951799650087,-24.4095101062452));
#30507=CARTESIAN_POINT('Ctrl Pts',(-50.6558084367241,6.0109657081762,-25.2005643713538));
#30508=CARTESIAN_POINT('Ctrl Pts',(-50.6615509496638,5.98622743157021,-26.3899997669615));
#30509=CARTESIAN_POINT('Ctrl Pts',(-50.6846748525644,5.92620540135337,-27.8927626232332));
#30510=CARTESIAN_POINT('Ctrl Pts',(-50.6950725450099,5.90238162716418,-28.9466459296479));
#30511=CARTESIAN_POINT('Ctrl Pts',(-50.6946680449133,5.90477860278918,-29.5520802304263));
#30512=CARTESIAN_POINT('Ctrl Pts',(-50.6945508254151,5.90534173633429,-29.677033778452));
#30513=CARTESIAN_POINT('Ctrl Pts',(-50.6942580445904,5.9068311947904,-29.9321945236902));
#30514=CARTESIAN_POINT('Ctrl Pts',(-50.6935878682622,5.91026897368014,-30.3756626437439));
#30515=CARTESIAN_POINT('Ctrl Pts',(-50.6917551184676,5.92002859891122,-31.2632127989292));
#30516=CARTESIAN_POINT('Ctrl Pts',(-50.6890613925536,5.9359812317638,-32.2723858506756));
#30517=CARTESIAN_POINT('Ctrl Pts',(-50.6868947412653,5.95289748594645,-33.2770980839551));
#30518=CARTESIAN_POINT('Ctrl Pts',(-50.6858351741547,5.96521819887813,-34.0276841341326));
#30519=CARTESIAN_POINT('Ctrl Pts',(-50.6856401967328,5.97653066469745,-34.7751159223277));
#30520=CARTESIAN_POINT('Ctrl Pts',(-50.6862931357692,5.98283697053856,-35.271052122708));
#30521=CARTESIAN_POINT('Ctrl Pts',(-50.6871553890568,5.98690341449776,-35.6431453859886));
#30522=CARTESIAN_POINT('Ctrl Pts',(-50.6878761975856,5.98962265002083,-35.8946313720791));
#30523=CARTESIAN_POINT('Ctrl Pts',(-50.6898341097545,5.99483435716034,-36.395767705979));
#30524=CARTESIAN_POINT('Ctrl Pts',(-50.6944333194783,6.0036712000655,-37.2720147791089));
#30525=CARTESIAN_POINT('Ctrl Pts',(-50.7069709291633,6.01954031883897,-39.021050925013));
#30526=CARTESIAN_POINT('Ctrl Pts',(-50.7186526447881,6.03145574314737,-40.5212470340552));
#30527=CARTESIAN_POINT('Ctrl Pts',(-50.7231490087732,6.03971614409264,-41.6525612828924));
#30528=CARTESIAN_POINT('Ctrl Pts',(-50.7240138582823,6.04129354764351,-41.9002145372208));
#30529=CARTESIAN_POINT('Ctrl Pts',(-50.7249671509576,6.0432033393967,-42.2737976799135));
#30530=CARTESIAN_POINT('Ctrl Pts',(-50.7256383706633,6.04471914890834,-42.6478327578797));
#30531=CARTESIAN_POINT('Ctrl Pts',(-50.7262316131469,6.04636175646918,-43.1478435611945));
#30532=CARTESIAN_POINT('Ctrl Pts',(-50.7265560428689,6.04793140295822,-43.7746144533213));
#30533=CARTESIAN_POINT('Ctrl Pts',(-50.7267393027773,6.04981561867667,-44.5292312702339));
#30534=CARTESIAN_POINT('Ctrl Pts',(-50.7271050272879,6.0520335529836,-45.1596536767437));
#30535=CARTESIAN_POINT('Ctrl Pts',(-50.7277694704289,6.0545735137265,-45.6647365793174));
#30536=CARTESIAN_POINT('Ctrl Pts',(-50.7285051649595,6.05696506949741,-46.0438451965456));
#30537=CARTESIAN_POINT('Ctrl Pts',(-50.729536775059,6.05993891296549,-46.423168368104));
#30538=CARTESIAN_POINT('Ctrl Pts',(-50.7313883450178,6.06481877022237,-46.9292203912809));
#30539=CARTESIAN_POINT('Ctrl Pts',(-50.7333832907411,6.06963486277635,-47.3087618147421));
#30540=CARTESIAN_POINT('Ctrl Pts',(-50.7359198024195,6.07546295954423,-47.6896758652666));
#30541=CARTESIAN_POINT('Ctrl Pts',(-50.7376702893699,6.0809675711625,-47.9575267341525));
#30542=CARTESIAN_POINT('Ctrl Pts',(-50.7414914696128,6.09641726631753,-48.4804660928323));
#30543=CARTESIAN_POINT('Ctrl Pts',(-50.7489798664707,6.13288565255227,-49.3866459278097));
#30544=CARTESIAN_POINT('Ctrl Pts',(-50.7620693439921,6.19682865621681,-50.6411457416213));
#30545=CARTESIAN_POINT('Ctrl Pts',(-50.7813231122897,6.2499173146937,-52.086868455667));
#30546=CARTESIAN_POINT('Ctrl Pts',(-50.7960716411339,6.2439975724267,-53.0080978203009));
#30547=CARTESIAN_POINT('Ctrl Pts',(-50.8056264058366,6.22071433825672,-53.5706742298222));
#30548=CARTESIAN_POINT('Ctrl Pts',(-50.8094970551415,6.20873941564547,-53.7684937809378));
#30549=CARTESIAN_POINT('Ctrl Pts',(-50.8180425618644,6.16954749151094,-54.1982792283086));
#30550=CARTESIAN_POINT('Ctrl Pts',(-50.834994953766,6.06584658881332,-54.9813661150004));
#30551=CARTESIAN_POINT('Ctrl Pts',(-50.875570231979,5.76112726056181,-56.7026423623578));
#30552=CARTESIAN_POINT('Ctrl Pts',(-50.9151647960118,5.49674034592434,-58.4194361227807));
#30553=CARTESIAN_POINT('Ctrl Pts',(-50.9266859152298,5.57321472253499,-59.761822807359));
#30554=CARTESIAN_POINT('Ctrl Pts',(-50.928128630218,5.58252875863702,-59.9042858995927));
#30555=CARTESIAN_POINT('Ctrl Pts',(-50.9306713131631,5.60583319985075,-60.1996107149606));
#30556=CARTESIAN_POINT('Ctrl Pts',(-50.9344645029265,5.65671550344642,-60.7078459548891));
#30557=CARTESIAN_POINT('Ctrl Pts',(-50.9395525918382,5.79774460568798,-61.7168799795076));
#30558=CARTESIAN_POINT('Ctrl Pts',(-50.940989407537,6.0365126531914,-62.8391349080536));
#30559=CARTESIAN_POINT('Ctrl Pts',(-50.9404102811909,6.33164707325243,-63.9320080217962));
#30560=CARTESIAN_POINT('Ctrl Pts',(-50.9397345638824,6.51512947738313,-64.5347827398139));
#30561=CARTESIAN_POINT('Ctrl Pts',(-50.9393066330775,6.64320899975592,-64.9316825441917));
#30562=CARTESIAN_POINT('Ctrl Pts',(-50.9390387251047,6.73003396949343,-65.1949035881217));
#30563=CARTESIAN_POINT('Ctrl Pts',(-50.9388068656743,6.81889977404073,-65.4561906573326));
#30564=CARTESIAN_POINT('Ctrl Pts',(-50.9386705414863,6.89815450708725,-65.6829499251508));
#30565=CARTESIAN_POINT('Ctrl Pts',(-50.9386150345703,6.94383661586305,-65.811999693998));
#30566=CARTESIAN_POINT('Ctrl Pts',(-50.938555040127,7.01274676059864,-66.0050723994061));
#30567=CARTESIAN_POINT('Ctrl Pts',(-50.938560245344,7.07090482741248,-66.1648314188238));
#30568=CARTESIAN_POINT('Ctrl Pts',(-50.9386359168677,7.16824402500391,-66.428527890208));
#30569=CARTESIAN_POINT('Ctrl Pts',(-50.9371824527114,7.28588624149121,-66.7331492568909));
#30570=CARTESIAN_POINT('Ctrl Pts',(-50.9349525659208,7.52823531103306,-67.3097869512625));
#30571=CARTESIAN_POINT('Ctrl Pts',(-50.9304861349764,7.98794885641103,-68.2981607577382));
#30572=CARTESIAN_POINT('Ctrl Pts',(-50.9230496760407,8.98940213828054,-70.1559710706958));
#30573=CARTESIAN_POINT('Ctrl Pts',(-50.922523410447,9.86476328571874,-71.616315855169));
#30574=CARTESIAN_POINT('Ctrl Pts',(-50.9269629008514,10.4186203997032,-72.668691895132));
#30575=CARTESIAN_POINT('Ctrl Pts',(-50.9265763436931,10.5543070540633,-72.9263651780016));
#30576=CARTESIAN_POINT('Ctrl Pts',(-50.9266081693936,10.8191442348102,-73.4279271585352));
#30577=CARTESIAN_POINT('Ctrl Pts',(-50.9263470769324,11.1537252117817,-74.0596571749007));
#30578=CARTESIAN_POINT('Ctrl Pts',(-50.9262537917075,11.5544067101263,-74.8135397204989));
#30579=CARTESIAN_POINT('Ctrl Pts',(-50.9260447195237,12.3575189311881,-76.3210927366946));
#30580=CARTESIAN_POINT('Ctrl Pts',(-50.9260642885464,13.0268913326518,-77.5736623659616));
#30581=CARTESIAN_POINT('Ctrl Pts',(-50.9262764665433,13.9948297281972,-79.3942546484625));
#30582=CARTESIAN_POINT('Ctrl Pts',(-50.9261813181547,14.4321744477241,-80.2169082365069));
#30583=CARTESIAN_POINT('Ctrl Pts',(-50.9261813181544,14.8686960351134,-81.0378859386059));
#30584=CARTESIAN_POINT('Ctrl Pts',(-48.1081617547539,0.821656359931925,
24.830552683986));
#30585=CARTESIAN_POINT('Ctrl Pts',(-48.1083039636808,0.821672125848511,
24.7816707634521));
#30586=CARTESIAN_POINT('Ctrl Pts',(-48.1084531105878,0.821688653501879,
24.732789784926));
#30587=CARTESIAN_POINT('Ctrl Pts',(-48.1102144775847,0.821884019159318,
24.1821532281473));
#30588=CARTESIAN_POINT('Ctrl Pts',(-48.1115208354339,0.822073222653415,
23.1780001047735));
#30589=CARTESIAN_POINT('Ctrl Pts',(-48.1145318216691,0.822535351985165,
21.1693470838628));
#30590=CARTESIAN_POINT('Ctrl Pts',(-48.126255455966,0.823836447388182,19.6652171497628));
#30591=CARTESIAN_POINT('Ctrl Pts',(-48.1513382795527,0.826399378484051,
18.4141819950539));
#30592=CARTESIAN_POINT('Ctrl Pts',(-48.1633401608167,0.827635914492364,
17.9112439152697));
#30593=CARTESIAN_POINT('Ctrl Pts',(-48.1934269865468,0.830753452240787,
16.9071782974834));
#30594=CARTESIAN_POINT('Ctrl Pts',(-48.2579641279172,0.837425408361244,
15.1533914949236));
#30595=CARTESIAN_POINT('Ctrl Pts',(-48.3196332683591,0.843613068292844,
13.652156435697));
#30596=CARTESIAN_POINT('Ctrl Pts',(-48.3589776117825,0.847210384179055,
12.3982565477228));
#30597=CARTESIAN_POINT('Ctrl Pts',(-48.3751358823534,0.848646943941486,
11.897528758793));
#30598=CARTESIAN_POINT('Ctrl Pts',(-48.4083119188161,0.851471934511271,
10.8960549543969));
#30599=CARTESIAN_POINT('Ctrl Pts',(-48.4662308713391,0.85614738198588,9.14291198624129));
#30600=CARTESIAN_POINT('Ctrl Pts',(-48.5074038448447,0.8592283855912,7.63782893120229));
#30601=CARTESIAN_POINT('Ctrl Pts',(-48.5258475297395,0.860582296955385,
6.5066415629613));
#30602=CARTESIAN_POINT('Ctrl Pts',(-48.5296781633811,0.860845722172545,
6.25655649567007));
#30603=CARTESIAN_POINT('Ctrl Pts',(-48.5363908526945,0.861253424574854,
5.75555852726343));
#30604=CARTESIAN_POINT('Ctrl Pts',(-48.545759656092,0.861687853954917,4.87739075226462));
#30605=CARTESIAN_POINT('Ctrl Pts',(-48.5558977282952,0.861673437671844,
3.11698986917906));
#30606=CARTESIAN_POINT('Ctrl Pts',(-48.5528947975733,0.861079705323928,
1.61023685094202));
#30607=CARTESIAN_POINT('Ctrl Pts',(-48.5480633471258,0.861062762891678,
0.550176309058608));
#30608=CARTESIAN_POINT('Ctrl Pts',(-48.5473893780227,0.861027148752041,
0.424587748163117));
#30609=CARTESIAN_POINT('Ctrl Pts',(-48.5456685819528,0.860841602241671,
0.173139364999722));
#30610=CARTESIAN_POINT('Ctrl Pts',(-48.54174356037,0.860243995795441,-0.266434695632504));
#30611=CARTESIAN_POINT('Ctrl Pts',(-48.5338902708593,0.858800861815022,
-0.893677263874593));
#30612=CARTESIAN_POINT('Ctrl Pts',(-48.5220464083315,0.856663839146366,
-1.64617418074009));
#30613=CARTESIAN_POINT('Ctrl Pts',(-48.5045928368554,0.854088087482596,
-2.64919303917013));
#30614=CARTESIAN_POINT('Ctrl Pts',(-48.4825861334336,0.852765003354847,
-3.90421055258685));
#30615=CARTESIAN_POINT('Ctrl Pts',(-48.4708072113734,0.856709284057601,
-4.91207362175905));
#30616=CARTESIAN_POINT('Ctrl Pts',(-48.467174598008,0.861488882626109,-5.54220041312295));
#30617=CARTESIAN_POINT('Ctrl Pts',(-48.4656412820237,0.860176842610061,
-5.74937675803637));
#30618=CARTESIAN_POINT('Ctrl Pts',(-48.4623409990297,0.847828554841079,
-6.20559665179427));
#30619=CARTESIAN_POINT('Ctrl Pts',(-48.4566143171184,0.805000196574491,
-7.02775369438753));
#30620=CARTESIAN_POINT('Ctrl Pts',(-48.4512568492943,0.714582313920764,
-8.31564021221516));
#30621=CARTESIAN_POINT('Ctrl Pts',(-48.4548272637197,0.695021109452357,
-9.7389343685648));
#30622=CARTESIAN_POINT('Ctrl Pts',(-48.462384639111,0.797115569315175,-10.8079866159256));
#30623=CARTESIAN_POINT('Ctrl Pts',(-48.4674826334621,0.901596608971655,
-11.4354946003987));
#30624=CARTESIAN_POINT('Ctrl Pts',(-48.4701010695859,0.971232007744518,
-11.754049685775));
#30625=CARTESIAN_POINT('Ctrl Pts',(-48.4719964958873,1.03104359761252,-11.9955612518357));
#30626=CARTESIAN_POINT('Ctrl Pts',(-48.473529106806,1.07554150145775,-12.1651151016405));
#30627=CARTESIAN_POINT('Ctrl Pts',(-48.4781623142853,1.17300632768884,-12.4927722796286));
#30628=CARTESIAN_POINT('Ctrl Pts',(-48.489511688992,1.36611982186439,-13.052242725534));
#30629=CARTESIAN_POINT('Ctrl Pts',(-48.5308112607914,1.95530334230472,-14.4053170494689));
#30630=CARTESIAN_POINT('Ctrl Pts',(-48.5888559408709,2.7580852490192,-15.7095673420877));
#30631=CARTESIAN_POINT('Ctrl Pts',(-48.6283106335618,3.45801560557731,-16.8861968690548));
#30632=CARTESIAN_POINT('Ctrl Pts',(-48.6397409855395,3.765486400292,-17.4418615068456));
#30633=CARTESIAN_POINT('Ctrl Pts',(-48.6403024516574,3.97332766253734,-17.8666528805007));
#30634=CARTESIAN_POINT('Ctrl Pts',(-48.636912362217,4.06262286490203,-18.071547516743));
#30635=CARTESIAN_POINT('Ctrl Pts',(-48.632474912663,4.12340082888935,-18.2226153488267));
#30636=CARTESIAN_POINT('Ctrl Pts',(-48.6235145806418,4.17460316445271,-18.3555032689312));
#30637=CARTESIAN_POINT('Ctrl Pts',(-48.605596754408,4.268448050428,-18.6016985693474));
#30638=CARTESIAN_POINT('Ctrl Pts',(-48.5822050597156,4.3620306439826,-18.8545106578251));
#30639=CARTESIAN_POINT('Ctrl Pts',(-48.5555267249322,4.45148589084385,-19.1026422173759));
#30640=CARTESIAN_POINT('Ctrl Pts',(-48.5371827717206,4.50653850905639,-19.2581435796158));
#30641=CARTESIAN_POINT('Ctrl Pts',(-48.5216922566285,4.54977261479859,-19.381926994986));
#30642=CARTESIAN_POINT('Ctrl Pts',(-48.5056253886663,4.59257722741495,-19.5055887283884));
#30643=CARTESIAN_POINT('Ctrl Pts',(-48.4592200249797,4.70838941295987,-19.8446811813429));
#30644=CARTESIAN_POINT('Ctrl Pts',(-48.3717713410061,4.8876721721689,-20.3938681940595));
#30645=CARTESIAN_POINT('Ctrl Pts',(-48.1941620970936,5.1778872714237,-21.3486426272371));
#30646=CARTESIAN_POINT('Ctrl Pts',(-47.9526707384724,5.48953943497499,-22.4918864970005));
#30647=CARTESIAN_POINT('Ctrl Pts',(-47.8049933853911,5.67655780766664,-23.3546093073591));
#30648=CARTESIAN_POINT('Ctrl Pts',(-47.7509567118304,5.76175622151436,-23.8814288993932));
#30649=CARTESIAN_POINT('Ctrl Pts',(-47.73173689534,5.7886209866703,-24.0780477136886));
#30650=CARTESIAN_POINT('Ctrl Pts',(-47.6999262884633,5.8318768540918,-24.4891274562849));
#30651=CARTESIAN_POINT('Ctrl Pts',(-47.6611936995658,5.87571409871005,-25.2313155480994));
#30652=CARTESIAN_POINT('Ctrl Pts',(-47.6459111880626,5.86167981157645,-26.3718474704576));
#30653=CARTESIAN_POINT('Ctrl Pts',(-47.661058373748,5.77950696427442,-27.8554510831928));
#30654=CARTESIAN_POINT('Ctrl Pts',(-47.6739998276547,5.73644434286673,-28.9197758632713));
#30655=CARTESIAN_POINT('Ctrl Pts',(-47.6766918803409,5.73425012421519,-29.5379474946004));
#30656=CARTESIAN_POINT('Ctrl Pts',(-47.6774591617782,5.73378010778106,-29.6585572612093));
#30657=CARTESIAN_POINT('Ctrl Pts',(-47.6795712553516,5.73262182581156,-29.9093968540346));
#30658=CARTESIAN_POINT('Ctrl Pts',(-47.684742928468,5.73015329550106,-30.3440131851773));
#30659=CARTESIAN_POINT('Ctrl Pts',(-47.7003265643364,5.72372749685039,-31.2185001382784));
#30660=CARTESIAN_POINT('Ctrl Pts',(-47.7273744004624,5.71430071429274,-32.2189124389907));
#30661=CARTESIAN_POINT('Ctrl Pts',(-47.757903427418,5.70528168254876,-33.2224570918928));
#30662=CARTESIAN_POINT('Ctrl Pts',(-47.7810759779801,5.69915006762253,-33.9756302585514));
#30663=CARTESIAN_POINT('Ctrl Pts',(-47.8031029240017,5.69388154659206,-34.7292141379704));
#30664=CARTESIAN_POINT('Ctrl Pts',(-47.8160341705809,5.69115517646488,-35.2316463250507));
#30665=CARTESIAN_POINT('Ctrl Pts',(-47.8247247489547,5.68946889060385,-35.6094062744765));
#30666=CARTESIAN_POINT('Ctrl Pts',(-47.8306323129823,5.68830749268304,-35.8606118864872));
#30667=CARTESIAN_POINT('Ctrl Pts',(-47.8426811389759,5.68614016568386,-36.363486472667));
#30668=CARTESIAN_POINT('Ctrl Pts',(-47.8642643869878,5.68250296983621,-37.2416836110121));
#30669=CARTESIAN_POINT('Ctrl Pts',(-47.9075934048008,5.67667099570877,-38.9955257562694));
#30670=CARTESIAN_POINT('Ctrl Pts',(-47.9400147345898,5.67388707997918,-40.5001945577602));
#30671=CARTESIAN_POINT('Ctrl Pts',(-47.9565066550077,5.67372202887156,-41.635163653271));
#30672=CARTESIAN_POINT('Ctrl Pts',(-47.9599386496466,5.67356269835911,-41.8832164151772));
#30673=CARTESIAN_POINT('Ctrl Pts',(-47.9645610192146,5.67294174472812,-42.257684476039));
#30674=CARTESIAN_POINT('Ctrl Pts',(-47.9686903533609,5.67206761727831,-42.6326046825154));
#30675=CARTESIAN_POINT('Ctrl Pts',(-47.9736025573532,5.67069401156819,-43.1339401996902));
#30676=CARTESIAN_POINT('Ctrl Pts',(-47.9787312416865,5.66886933253452,-43.7625304581063));
#30677=CARTESIAN_POINT('Ctrl Pts',(-47.9836100894013,5.66737379968377,-44.519631153679));
#30678=CARTESIAN_POINT('Ctrl Pts',(-47.9868967370082,5.66743536136416,-45.1523662815642));
#30679=CARTESIAN_POINT('Ctrl Pts',(-47.9892190368056,5.66874051397247,-45.6593910470067));
#30680=CARTESIAN_POINT('Ctrl Pts',(-47.9908537750947,5.67044657197521,-46.0400313854599));
#30681=CARTESIAN_POINT('Ctrl Pts',(-47.9924228333032,5.67299423348329,-46.4209581938724));
#30682=CARTESIAN_POINT('Ctrl Pts',(-47.9944851694717,5.67766910053647,-46.929228720508));
#30683=CARTESIAN_POINT('Ctrl Pts',(-47.9960584325483,5.68276825329085,-47.3105867491211));
#30684=CARTESIAN_POINT('Ctrl Pts',(-47.9977427003301,5.68919643937715,-47.6933809474625));
#30685=CARTESIAN_POINT('Ctrl Pts',(-47.9986800935609,5.69530034202098,-47.9631886151501));
#30686=CARTESIAN_POINT('Ctrl Pts',(-48.0000606907457,5.71252845744749,-48.4892800747684));
#30687=CARTESIAN_POINT('Ctrl Pts',(-48.0013833800003,5.7534559225999,-49.4003811610625));
#30688=CARTESIAN_POINT('Ctrl Pts',(-48.0016186359631,5.82668280043133,-50.6595265053002));
#30689=CARTESIAN_POINT('Ctrl Pts',(-48.0031279455766,5.89225151943146,-52.1071552929537));
#30690=CARTESIAN_POINT('Ctrl Pts',(-48.0068413553413,5.89412700469785,-53.0269293633755));
#30691=CARTESIAN_POINT('Ctrl Pts',(-48.0104999550757,5.87504627401801,-53.5877251204438));
#30692=CARTESIAN_POINT('Ctrl Pts',(-48.0119186947241,5.8644984398709,-53.7870157793957));
#30693=CARTESIAN_POINT('Ctrl Pts',(-48.015236046728,5.82868565785535,-54.2180167794228));
#30694=CARTESIAN_POINT('Ctrl Pts',(-48.0223405541487,5.73182312345919,-55.0028496725892));
#30695=CARTESIAN_POINT('Ctrl Pts',(-48.0422819205056,5.44381604950419,-56.7239446729538));
#30696=CARTESIAN_POINT('Ctrl Pts',(-48.0652320306938,5.19648912835514,-58.4362411887274));
#30697=CARTESIAN_POINT('Ctrl Pts',(-48.072145366917,5.27833872248682,-59.7711023692122));
#30698=CARTESIAN_POINT('Ctrl Pts',(-48.0730810994228,5.28813022272174,-59.9127033359094));
#30699=CARTESIAN_POINT('Ctrl Pts',(-48.0748143844032,5.31227047765825,-60.2063755436483));
#30700=CARTESIAN_POINT('Ctrl Pts',(-48.0776908225279,5.36413329883143,-60.7119580011442));
#30701=CARTESIAN_POINT('Ctrl Pts',(-48.0827259548146,5.50557705051933,-61.7166455841316));
#30702=CARTESIAN_POINT('Ctrl Pts',(-48.0870712175635,5.74234063614827,-62.8361337598059));
#30703=CARTESIAN_POINT('Ctrl Pts',(-48.0902785989789,6.03499269362514,-63.9282626842282));
#30704=CARTESIAN_POINT('Ctrl Pts',(-48.09170694666,6.21721384595243,-64.5313341753743));
#30705=CARTESIAN_POINT('Ctrl Pts',(-48.0925230603127,6.34465176117515,-64.9287143411935));
#30706=CARTESIAN_POINT('Ctrl Pts',(-48.0930339900168,6.43110769486847,-65.1923324264293));
#30707=CARTESIAN_POINT('Ctrl Pts',(-48.0934898782398,6.519711978698,-65.4541244578588));
#30708=CARTESIAN_POINT('Ctrl Pts',(-48.0938525513821,6.59884897317687,-65.6814255430501));
#30709=CARTESIAN_POINT('Ctrl Pts',(-48.0940492907279,6.64449948092765,-65.8108129567606));
#30710=CARTESIAN_POINT('Ctrl Pts',(-48.0943334109498,6.71339881074584,-66.0044194815105));
#30711=CARTESIAN_POINT('Ctrl Pts',(-48.0945493743175,6.77163076478862,-66.1646832795354));
#30712=CARTESIAN_POINT('Ctrl Pts',(-48.0948612361393,6.8692076981214,-66.4292745880487));
#30713=CARTESIAN_POINT('Ctrl Pts',(-48.0938879421657,6.98676580433808,-66.7337926781003));
#30714=CARTESIAN_POINT('Ctrl Pts',(-48.0923778740631,7.22916551376678,-67.3107614717401));
#30715=CARTESIAN_POINT('Ctrl Pts',(-48.0889925647051,7.68892715311023,-68.299331484953));
#30716=CARTESIAN_POINT('Ctrl Pts',(-48.0826672547797,8.69063589248501,-70.1574981028561));
#30717=CARTESIAN_POINT('Ctrl Pts',(-48.0816700834379,9.5660147444683,-71.6177387695598));
#30718=CARTESIAN_POINT('Ctrl Pts',(-48.0855496326223,10.1195965515549,-72.669938484722));
#30719=CARTESIAN_POINT('Ctrl Pts',(-48.0852320074524,10.2552979808535,-72.9276394485621));
#30720=CARTESIAN_POINT('Ctrl Pts',(-48.0852797639747,10.5201259530456,-73.4292165411084));
#30721=CARTESIAN_POINT('Ctrl Pts',(-48.0850686567843,10.8547201758687,-74.0609738365155));
#30722=CARTESIAN_POINT('Ctrl Pts',(-48.0849890234844,11.2554147473501,-74.8148760797214));
#30723=CARTESIAN_POINT('Ctrl Pts',(-48.0847893538615,12.0585656117152,-76.3224589816106));
#30724=CARTESIAN_POINT('Ctrl Pts',(-48.0847638687617,12.727967876092,-77.5750096594133));
#30725=CARTESIAN_POINT('Ctrl Pts',(-48.0849471552217,13.6958775601037,-79.395550472923));
#30726=CARTESIAN_POINT('Ctrl Pts',(-48.0848645544605,14.1332336032719,-80.2182152143253));
#30727=CARTESIAN_POINT('Ctrl Pts',(-48.0848645544601,14.5697551906614,-81.0391929164233));
#30728=CARTESIAN_POINT('Ctrl Pts',(-45.2615345930742,0.568923653316842,
24.8305649181971));
#30729=CARTESIAN_POINT('Ctrl Pts',(-45.2616723458727,0.56893639381907,24.7816834208571));
#30730=CARTESIAN_POINT('Ctrl Pts',(-45.2618168168555,0.568949748036691,
24.7328028847575));
#30731=CARTESIAN_POINT('Ctrl Pts',(-45.2635227928271,0.569107674888664,
24.1821708638069));
#30732=CARTESIAN_POINT('Ctrl Pts',(-45.2648687934348,0.569263618641808,
23.1780301850203));
#30733=CARTESIAN_POINT('Ctrl Pts',(-45.2680271544534,0.56964532707125,21.1693806216249));
#30734=CARTESIAN_POINT('Ctrl Pts',(-45.2793788855699,0.57069704852392,19.6652250009272));
#30735=CARTESIAN_POINT('Ctrl Pts',(-45.3032612861431,0.572754317085861,
18.4141650801884));
#30736=CARTESIAN_POINT('Ctrl Pts',(-45.3147245804852,0.573757913519431,
17.9112021425638));
#30737=CARTESIAN_POINT('Ctrl Pts',(-45.343524261982,0.57630797389634,16.90712294505));
#30738=CARTESIAN_POINT('Ctrl Pts',(-45.4052807106741,0.581771843525628,
15.1533712283448));
#30739=CARTESIAN_POINT('Ctrl Pts',(-45.4637749100727,0.586723142739833,
13.652199025009));
#30740=CARTESIAN_POINT('Ctrl Pts',(-45.5001367390707,0.589383332340141,
12.3983651401701));
#30741=CARTESIAN_POINT('Ctrl Pts',(-45.5149616963227,0.590420663495616,
11.8976629685695));
#30742=CARTESIAN_POINT('Ctrl Pts',(-45.5450626839958,0.592375140886463,
10.8962020014157));
#30743=CARTESIAN_POINT('Ctrl Pts',(-45.5969183131899,0.595422785932535,
9.14302426569176));
#30744=CARTESIAN_POINT('Ctrl Pts',(-45.6331060963251,0.597204544866204,
7.63779283188048));
#30745=CARTESIAN_POINT('Ctrl Pts',(-45.6492210307351,0.597934723316499,
6.50656027802753));
#30746=CARTESIAN_POINT('Ctrl Pts',(-45.65252979313,0.598063469500555,6.25653232565011));
#30747=CARTESIAN_POINT('Ctrl Pts',(-45.6581926980207,0.598199683729433,
5.75559249943098));
#30748=CARTESIAN_POINT('Ctrl Pts',(-45.6657464934642,0.598162253780016,
4.87748364246271));
#30749=CARTESIAN_POINT('Ctrl Pts',(-45.6726272003006,0.597307704815268,
3.11705192901595));
#30750=CARTESIAN_POINT('Ctrl Pts',(-45.6685501368452,0.596356338009474,
1.60983415283903));
#30751=CARTESIAN_POINT('Ctrl Pts',(-45.6649011830657,0.596693744906996,
0.549181970152154));
#30752=CARTESIAN_POINT('Ctrl Pts',(-45.6644106870089,0.596736979590196,
0.422841734534823));
#30753=CARTESIAN_POINT('Ctrl Pts',(-45.6632187310025,0.596838489702751,
0.170391518020105));
#30754=CARTESIAN_POINT('Ctrl Pts',(-45.6606080667276,0.597052402569735,
-0.270865388521122));
#30755=CARTESIAN_POINT('Ctrl Pts',(-45.6555447983622,0.597453307539356,
-0.899661574341966));
#30756=CARTESIAN_POINT('Ctrl Pts',(-45.6478740955046,0.598048487429573,
-1.65267183829421));
#30757=CARTESIAN_POINT('Ctrl Pts',(-45.6362241180025,0.598951491118354,
-2.65459475895867));
#30758=CARTESIAN_POINT('Ctrl Pts',(-45.6203342687638,0.600156051117981,
-3.90475578181039));
#30759=CARTESIAN_POINT('Ctrl Pts',(-45.6091709952231,0.601137200513604,
-4.90501268537487));
#30760=CARTESIAN_POINT('Ctrl Pts',(-45.6035954437551,0.601759966525794,
-5.52991529103675));
#30761=CARTESIAN_POINT('Ctrl Pts',(-45.6006108814509,0.599729253591517,
-5.74989315896313));
#30762=CARTESIAN_POINT('Ctrl Pts',(-45.5922177925495,0.588103576083817,
-6.21834474534208));
#30763=CARTESIAN_POINT('Ctrl Pts',(-45.5727398228785,0.551803838808369,
-7.05489906573956));
#30764=CARTESIAN_POINT('Ctrl Pts',(-45.5400034086817,0.478480237096733,
-8.3289803346879));
#30765=CARTESIAN_POINT('Ctrl Pts',(-45.5231977388069,0.451676003483263,
-9.69594050140588));
#30766=CARTESIAN_POINT('Ctrl Pts',(-45.5312196791262,0.505876456142413,
-10.7037545406741));
#30767=CARTESIAN_POINT('Ctrl Pts',(-45.5428674671062,0.56588976699614,-11.2928459671084));
#30768=CARTESIAN_POINT('Ctrl Pts',(-45.5512155153025,0.607023081755394,
-11.5918143476826));
#30769=CARTESIAN_POINT('Ctrl Pts',(-45.5585084115334,0.642699657012322,
-11.8182084602322));
#30770=CARTESIAN_POINT('Ctrl Pts',(-45.564432885722,0.66595079654557,-11.96161215553));
#30771=CARTESIAN_POINT('Ctrl Pts',(-45.579301145316,0.717617991143493,-12.2518240391153));
#30772=CARTESIAN_POINT('Ctrl Pts',(-45.6125589798245,0.818560777400114,
-12.7533508080639));
#30773=CARTESIAN_POINT('Ctrl Pts',(-45.7295753087123,1.13208082807272,-14.026005831991));
#30774=CARTESIAN_POINT('Ctrl Pts',(-45.8977342546569,1.62991439444617,-15.3629814934345));
#30775=CARTESIAN_POINT('Ctrl Pts',(-45.9896689963964,2.1742378659247,-16.6449845617281));
#30776=CARTESIAN_POINT('Ctrl Pts',(-46.0127255866054,2.44684675915175,-17.2789902088887));
#30777=CARTESIAN_POINT('Ctrl Pts',(-46.0139719522059,2.66002778840069,-17.7842019315097));
#30778=CARTESIAN_POINT('Ctrl Pts',(-46.0086322280254,2.76387905082651,-18.0364848019655));
#30779=CARTESIAN_POINT('Ctrl Pts',(-46.0020276494765,2.84044587158191,-18.2258896669335));
#30780=CARTESIAN_POINT('Ctrl Pts',(-45.9916442991187,2.90255746472163,-18.3814126264322));
#30781=CARTESIAN_POINT('Ctrl Pts',(-45.9710572595573,3.02410551438022,-18.670089280978));
#30782=CARTESIAN_POINT('Ctrl Pts',(-45.9455273169221,3.1524972413311,-18.9598642552261));
#30783=CARTESIAN_POINT('Ctrl Pts',(-45.917597839482,3.2829544276836,-19.2407969343877));
#30784=CARTESIAN_POINT('Ctrl Pts',(-45.8989127160357,3.36586638758757,-19.4150986453484));
#30785=CARTESIAN_POINT('Ctrl Pts',(-45.8834412884027,3.43259720471774,-19.5530188450265));
#30786=CARTESIAN_POINT('Ctrl Pts',(-45.8676010038037,3.49963796574981,-19.6902312656681));
#30787=CARTESIAN_POINT('Ctrl Pts',(-45.8226911728824,3.68495541061571,-20.0642598939347));
#30788=CARTESIAN_POINT('Ctrl Pts',(-45.7429920353979,3.99094061991361,-20.6593839193205));
#30789=CARTESIAN_POINT('Ctrl Pts',(-45.5941611777489,4.5158905048341,-21.6696940569923));
#30790=CARTESIAN_POINT('Ctrl Pts',(-45.4103185036997,5.08397172095285,-22.8408731099591));
#30791=CARTESIAN_POINT('Ctrl Pts',(-45.2952033585105,5.35220520103119,-23.6349105739773));
#30792=CARTESIAN_POINT('Ctrl Pts',(-45.2470258602545,5.45367407042719,-24.0675321019981));
#30793=CARTESIAN_POINT('Ctrl Pts',(-45.2275642403591,5.49554360971262,-24.2646881816929));
#30794=CARTESIAN_POINT('Ctrl Pts',(-45.1897213634604,5.56191922129806,-24.6530653715348));
#30795=CARTESIAN_POINT('Ctrl Pts',(-45.126169787784,5.64579968547833,-25.3632536240763));
#30796=CARTESIAN_POINT('Ctrl Pts',(-45.0485809628158,5.68330120258022,-26.4538851411555));
#30797=CARTESIAN_POINT('Ctrl Pts',(-44.9827225203447,5.65136303060178,-27.9001949288379));
#30798=CARTESIAN_POINT('Ctrl Pts',(-44.9521248674338,5.6293916709228,-28.949492421806));
#30799=CARTESIAN_POINT('Ctrl Pts',(-44.9367599336799,5.63616027776272,-29.5612290563094));
#30800=CARTESIAN_POINT('Ctrl Pts',(-44.9335170536817,5.63713457503584,-29.6743255452956));
#30801=CARTESIAN_POINT('Ctrl Pts',(-44.9278388436267,5.63805208961385,-29.9142811768491));
#30802=CARTESIAN_POINT('Ctrl Pts',(-44.9198488782374,5.63668801870017,-30.3297606990247));
#30803=CARTESIAN_POINT('Ctrl Pts',(-44.9109910089194,5.62340525515849,-31.1739498277202));
#30804=CARTESIAN_POINT('Ctrl Pts',(-44.9136021605173,5.58905379630781,-32.1537761072688));
#30805=CARTESIAN_POINT('Ctrl Pts',(-44.9221536485736,5.54708312381198,-33.151610222345));
#30806=CARTESIAN_POINT('Ctrl Pts',(-44.9298865257232,5.51492405417621,-33.9076686728183));
#30807=CARTESIAN_POINT('Ctrl Pts',(-44.9372328903042,5.48530913853536,-34.6714518503932));
#30808=CARTESIAN_POINT('Ctrl Pts',(-44.9407885305601,5.46943186190011,-35.1856910262279));
#30809=CARTESIAN_POINT('Ctrl Pts',(-44.9425441216053,5.45980858080541,-35.5739854943983));
#30810=CARTESIAN_POINT('Ctrl Pts',(-44.9438779864364,5.45366779071273,-35.8236942203539));
#30811=CARTESIAN_POINT('Ctrl Pts',(-44.9471787513647,5.44144439102455,-36.3285083384014));
#30812=CARTESIAN_POINT('Ctrl Pts',(-44.9543182354928,5.42068637952117,-37.2078627950992));
#30813=CARTESIAN_POINT('Ctrl Pts',(-44.9725136640791,5.38222432218129,-38.9666810450322));
#30814=CARTESIAN_POINT('Ctrl Pts',(-44.988587990644,5.35608797243692,-40.4758943628781));
#30815=CARTESIAN_POINT('Ctrl Pts',(-44.9949719986201,5.34203825053049,-41.6149771521622));
#30816=CARTESIAN_POINT('Ctrl Pts',(-44.9962209741261,5.33888938097108,-41.8633286625312));
#30817=CARTESIAN_POINT('Ctrl Pts',(-44.9976487140526,5.33392929542106,-42.2386401419984));
#30818=CARTESIAN_POINT('Ctrl Pts',(-44.9987078765806,5.32890196674228,-42.6143871354106));
#30819=CARTESIAN_POINT('Ctrl Pts',(-44.9997164946637,5.32225541986517,-43.1170091303405));
#30820=CARTESIAN_POINT('Ctrl Pts',(-45.0004034480282,5.31439673661683,-43.7474301700452));
#30821=CARTESIAN_POINT('Ctrl Pts',(-45.000868285242,5.30671511110962,-44.5071548518077));
#30822=CARTESIAN_POINT('Ctrl Pts',(-45.0014224520297,5.30264469307216,-45.1424238784898));
#30823=CARTESIAN_POINT('Ctrl Pts',(-45.0022711041608,5.30134971650009,-45.6517276051057));
#30824=CARTESIAN_POINT('Ctrl Pts',(-45.0031683624121,5.30147692668183,-46.0341874242821));
#30825=CARTESIAN_POINT('Ctrl Pts',(-45.0043982702481,5.302839018119,-46.4170469581394));
#30826=CARTESIAN_POINT('Ctrl Pts',(-45.0065803989924,5.30648560360591,-46.9280543328961));
#30827=CARTESIAN_POINT('Ctrl Pts',(-45.0089112966019,5.31146635095098,-47.3116150666946));
#30828=CARTESIAN_POINT('Ctrl Pts',(-45.0118707869184,5.3182531796772,-47.6967600511927));
#30829=CARTESIAN_POINT('Ctrl Pts',(-45.013909593286,5.32485825500584,-47.9686672018424));
#30830=CARTESIAN_POINT('Ctrl Pts',(-45.0183049428734,5.34390019871555,-48.4982682740304));
#30831=CARTESIAN_POINT('Ctrl Pts',(-45.0267916828321,5.38990717621575,-49.4147594958146));
#30832=CARTESIAN_POINT('Ctrl Pts',(-45.0413469150811,5.47438659865881,-50.6789313209984));
#30833=CARTESIAN_POINT('Ctrl Pts',(-45.0626179306112,5.55591976262862,-52.1287880158482));
#30834=CARTESIAN_POINT('Ctrl Pts',(-45.0792744990489,5.56824779334821,-53.047472923302));
#30835=CARTESIAN_POINT('Ctrl Pts',(-45.0903088412658,5.55518331394269,-53.6068866561389));
#30836=CARTESIAN_POINT('Ctrl Pts',(-45.0949604559406,5.54685392911716,-53.8080038405276));
#30837=CARTESIAN_POINT('Ctrl Pts',(-45.1051935354558,5.51631442715935,-54.2407427058968));
#30838=CARTESIAN_POINT('Ctrl Pts',(-45.1253875800908,5.43020787584997,-55.0280992059488));
#30839=CARTESIAN_POINT('Ctrl Pts',(-45.1724343081567,5.16829959423166,-56.7498442628009));
#30840=CARTESIAN_POINT('Ctrl Pts',(-45.2150323715158,4.94541364590222,-58.4563942878425));
#30841=CARTESIAN_POINT('Ctrl Pts',(-45.229079940856,5.03428012136371,-59.7812103826349));
#30842=CARTESIAN_POINT('Ctrl Pts',(-45.2308059711601,5.0447516841388,-59.9217813236452));
#30843=CARTESIAN_POINT('Ctrl Pts',(-45.2339258062422,5.07004070521539,-60.2134142346763));
#30844=CARTESIAN_POINT('Ctrl Pts',(-45.2387137009182,5.12323156118997,-60.7157770799439));
#30845=CARTESIAN_POINT('Ctrl Pts',(-45.2457313086932,5.26509173462011,-61.7152178901686));
#30846=CARTESIAN_POINT('Ctrl Pts',(-45.2491207511983,5.49878674246531,-62.8315177848284));
#30847=CARTESIAN_POINT('Ctrl Pts',(-45.2501521594165,5.78765739615891,-63.9229299880029));
#30848=CARTESIAN_POINT('Ctrl Pts',(-45.2502525085497,5.96793885408008,-64.5264537867342));
#30849=CARTESIAN_POINT('Ctrl Pts',(-45.2502885274417,6.09435349669486,-64.9244694933693));
#30850=CARTESIAN_POINT('Ctrl Pts',(-45.2503156383113,6.18020953797663,-65.1885989491818));
#30851=CARTESIAN_POINT('Ctrl Pts',(-45.2503590074845,6.26835846071443,-65.4510299828515));
#30852=CARTESIAN_POINT('Ctrl Pts',(-45.2504452439476,6.34725184610613,-65.6790016185538));
#30853=CARTESIAN_POINT('Ctrl Pts',(-45.2505118720077,6.39281215966707,-65.8088036964063));
#30854=CARTESIAN_POINT('Ctrl Pts',(-45.2506305029969,6.46162677822535,-66.0030624735293));
#30855=CARTESIAN_POINT('Ctrl Pts',(-45.2507736039379,6.51990099608607,-66.1639364315662));
#30856=CARTESIAN_POINT('Ctrl Pts',(-45.2510741641748,6.6177086878099,-66.4295992762849));
#30857=CARTESIAN_POINT('Ctrl Pts',(-45.250321477465,6.73509315111427,-66.7340020498313));
#30858=CARTESIAN_POINT('Ctrl Pts',(-45.249119758346,6.97744203040324,-67.3113803339706));
#30859=CARTESIAN_POINT('Ctrl Pts',(-45.2463020674733,7.43710776352219,-68.3002085477061));
#30860=CARTESIAN_POINT('Ctrl Pts',(-45.240708715144,8.43898108975228,-70.1588293463694));
#30861=CARTESIAN_POINT('Ctrl Pts',(-45.2394128134625,9.31441095850817,-71.6189345572044));
#30862=CARTESIAN_POINT('Ctrl Pts',(-45.2425963587864,9.86768814163015,-72.6709320003031));
#30863=CARTESIAN_POINT('Ctrl Pts',(-45.242318918496,10.0033992160793,-72.928669941724));
#30864=CARTESIAN_POINT('Ctrl Pts',(-45.2423411399073,10.2682109987263,-73.4302705769965));
#30865=CARTESIAN_POINT('Ctrl Pts',(-45.2421524693102,10.6028146584613,-74.0620653647392));
#30866=CARTESIAN_POINT('Ctrl Pts',(-45.2420837499708,11.0035248370368,-74.8159945743116));
#30867=CARTESIAN_POINT('Ctrl Pts',(-45.2419300164671,11.8067277607913,-76.3236157009755));
#30868=CARTESIAN_POINT('Ctrl Pts',(-45.2419413548527,12.476175379063,-77.5761363944957));
#30869=CARTESIAN_POINT('Ctrl Pts',(-45.2420965906919,13.444046814902,-79.3966073326402));
#30870=CARTESIAN_POINT('Ctrl Pts',(-45.2420269735312,13.881415378809,-80.219287048203));
#30871=CARTESIAN_POINT('Ctrl Pts',(-45.2420269735315,14.3179369661985,-81.0402647503008));
#30872=CARTESIAN_POINT('Ctrl Pts',(-42.8889107614918,0.396069854539573,
24.8306499092207));
#30873=CARTESIAN_POINT('Ctrl Pts',(-42.8890409472221,0.396078250577575,
24.7817710962967));
#30874=CARTESIAN_POINT('Ctrl Pts',(-42.889177481851,0.396087052970513,24.7328933096333));
#30875=CARTESIAN_POINT('Ctrl Pts',(-42.8907898049868,0.396191175579392,
24.1822922709228));
#30876=CARTESIAN_POINT('Ctrl Pts',(-42.8920476582943,0.396261310671983,
23.1781820957105));
#30877=CARTESIAN_POINT('Ctrl Pts',(-42.8949896800306,0.396415381007176,
21.1695908064305));
#30878=CARTESIAN_POINT('Ctrl Pts',(-42.905718534153,0.397110116062497,19.6654456243867));
#30879=CARTESIAN_POINT('Ctrl Pts',(-42.9283626135728,0.398632648763516,
18.4143922632001));
#30880=CARTESIAN_POINT('Ctrl Pts',(-42.9392337126744,0.399361970835517,
17.9115967319916));
#30881=CARTESIAN_POINT('Ctrl Pts',(-42.9665506853066,0.401193597804371,
16.9076321680773));
#30882=CARTESIAN_POINT('Ctrl Pts',(-43.0251392083456,0.405128861753337,
15.1538536921797));
#30883=CARTESIAN_POINT('Ctrl Pts',(-43.0806351134471,0.40889600092376,13.652114312685));
#30884=CARTESIAN_POINT('Ctrl Pts',(-43.1151374652814,0.411298449155565,
12.39756559081));
#30885=CARTESIAN_POINT('Ctrl Pts',(-43.1292109879026,0.412286158686825,
11.8965753436264));
#30886=CARTESIAN_POINT('Ctrl Pts',(-43.157799097833,0.414317517348359,10.8946870573607));
#30887=CARTESIAN_POINT('Ctrl Pts',(-43.20706598892,0.417869362120652,9.14109869268271));
#30888=CARTESIAN_POINT('Ctrl Pts',(-43.2413947466429,0.420389756470078,
7.63604088896889));
#30889=CARTESIAN_POINT('Ctrl Pts',(-43.256602039586,0.421503566320526,6.50522218228596));
#30890=CARTESIAN_POINT('Ctrl Pts',(-43.2597224872715,0.421733781313164,
6.25498871804423));
#30891=CARTESIAN_POINT('Ctrl Pts',(-43.2650504875047,0.422134349062575,
5.75387948222069));
#30892=CARTESIAN_POINT('Ctrl Pts',(-43.2721220238125,0.422687100151175,
4.87552731214186));
#30893=CARTESIAN_POINT('Ctrl Pts',(-43.2784194879523,0.423255845091349,
3.11535973815131));
#30894=CARTESIAN_POINT('Ctrl Pts',(-43.274315924288,0.423057704554917,1.60922363435097));
#30895=CARTESIAN_POINT('Ctrl Pts',(-43.2706427662616,0.422748404666616,
0.550030671665346));
#30896=CARTESIAN_POINT('Ctrl Pts',(-43.2701595719556,0.422707204277705,
0.423860675108253));
#30897=CARTESIAN_POINT('Ctrl Pts',(-43.269016774996,0.422610273212511,0.171737684639995));
#30898=CARTESIAN_POINT('Ctrl Pts',(-43.2665760293404,0.42240324124909,-0.268981603410207));
#30899=CARTESIAN_POINT('Ctrl Pts',(-43.2619490022914,0.422015480510026,
-0.897168941895786));
#30900=CARTESIAN_POINT('Ctrl Pts',(-43.2549691537298,0.42142408674007,-1.64956521349317));
#30901=CARTESIAN_POINT('Ctrl Pts',(-43.2442733407787,0.420531584961871,
-2.65104169285572));
#30902=CARTESIAN_POINT('Ctrl Pts',(-43.2292854654237,0.419295148862323,
-3.90125771123846));
#30903=CARTESIAN_POINT('Ctrl Pts',(-43.2175701879556,0.418343911838244,
-4.90193027537972));
#30904=CARTESIAN_POINT('Ctrl Pts',(-43.2109790319918,0.417761881888926,
-5.52777685401367));
#30905=CARTESIAN_POINT('Ctrl Pts',(-43.2075375110887,0.416182369454823,
-5.76115929569839));
#30906=CARTESIAN_POINT('Ctrl Pts',(-43.1980371664098,0.408543968449964,
-6.24417082539291));
#30907=CARTESIAN_POINT('Ctrl Pts',(-43.1761218601326,0.385936981481704,
-7.09905037037054));
#30908=CARTESIAN_POINT('Ctrl Pts',(-43.1386135133381,0.34225609408002,-8.36515361030123));
#30909=CARTESIAN_POINT('Ctrl Pts',(-43.116395210378,0.325805827361278,-9.68282802245736));
#30910=CARTESIAN_POINT('Ctrl Pts',(-43.1211039919704,0.353517782545892,
-10.6331211566615));
#30911=CARTESIAN_POINT('Ctrl Pts',(-43.1312872417939,0.384608831349905,
-11.1834209787052));
#30912=CARTESIAN_POINT('Ctrl Pts',(-43.1391431884441,0.405967964406648,
-11.4612161011621));
#30913=CARTESIAN_POINT('Ctrl Pts',(-43.1462045688855,0.424475570505401,
-11.6708316967806));
#30914=CARTESIAN_POINT('Ctrl Pts',(-43.1516654022893,0.43559362531917,-11.7951174044754));
#30915=CARTESIAN_POINT('Ctrl Pts',(-43.1648351192485,0.459330218746731,
-12.0539176614948));
#30916=CARTESIAN_POINT('Ctrl Pts',(-43.1935325849912,0.502791872139162,
-12.5042798495235));
#30917=CARTESIAN_POINT('Ctrl Pts',(-43.2918349048567,0.629156086175763,
-13.6778160448311));
#30918=CARTESIAN_POINT('Ctrl Pts',(-43.4467642620028,0.841231802133456,
-15.019464871798));
#30919=CARTESIAN_POINT('Ctrl Pts',(-43.5583459167546,1.17536390238127,-16.3968425054621));
#30920=CARTESIAN_POINT('Ctrl Pts',(-43.5968156257216,1.37364721670612,-17.0927150275281));
#30921=CARTESIAN_POINT('Ctrl Pts',(-43.6139523508331,1.55240857647083,-17.6538909094906));
#30922=CARTESIAN_POINT('Ctrl Pts',(-43.6175451144521,1.6485074056122,-17.9356670485181));
#30923=CARTESIAN_POINT('Ctrl Pts',(-43.6181302561629,1.72310984528553,-18.1473356018224));
#30924=CARTESIAN_POINT('Ctrl Pts',(-43.615423729367,1.78144840511499,-18.3099380413222));
#30925=CARTESIAN_POINT('Ctrl Pts',(-43.6102834716429,1.90052337855645,-18.6147533670115));
#30926=CARTESIAN_POINT('Ctrl Pts',(-43.6028756356143,2.02979449666717,-18.916104536019));
#30927=CARTESIAN_POINT('Ctrl Pts',(-43.5946265935477,2.16472139261033,-19.2068666513642));
#30928=CARTESIAN_POINT('Ctrl Pts',(-43.5890067356035,2.25154884571202,-19.3861828601404));
#30929=CARTESIAN_POINT('Ctrl Pts',(-43.5843537026808,2.32209811486412,-19.5276752804076));
#30930=CARTESIAN_POINT('Ctrl Pts',(-43.5795884739498,2.39336597516418,-19.6681250028613));
#30931=CARTESIAN_POINT('Ctrl Pts',(-43.566082556781,2.59196363352519,-20.0498673569958));
#30932=CARTESIAN_POINT('Ctrl Pts',(-43.5426641158337,2.92794406976125,-20.6519833438532));
#30933=CARTESIAN_POINT('Ctrl Pts',(-43.502946975925,3.52412707502357,-21.6678184692176));
#30934=CARTESIAN_POINT('Ctrl Pts',(-43.4668549917711,4.21026357501831,-22.8465894487001));
#30935=CARTESIAN_POINT('Ctrl Pts',(-43.4611694703721,4.57462701073374,-23.6690582823401));
#30936=CARTESIAN_POINT('Ctrl Pts',(-43.4553982014206,4.71697932248017,-24.1238951932113));
#30937=CARTESIAN_POINT('Ctrl Pts',(-43.4462062290868,4.77898111591247,-24.343408087553));
#30938=CARTESIAN_POINT('Ctrl Pts',(-43.4250726566578,4.88081822070273,-24.7665431378758));
#30939=CARTESIAN_POINT('Ctrl Pts',(-43.37239277437,5.02244505804989,-25.5330343096657));
#30940=CARTESIAN_POINT('Ctrl Pts',(-43.2645514756731,5.13286377920033,-26.6650074898123));
#30941=CARTESIAN_POINT('Ctrl Pts',(-43.1112830283311,5.19738964776005,-28.1015600780752));
#30942=CARTESIAN_POINT('Ctrl Pts',(-43.0184092334532,5.23942265301599,-29.1106062811467));
#30943=CARTESIAN_POINT('Ctrl Pts',(-42.9752707928305,5.27425180200197,-29.6911654008103));
#30944=CARTESIAN_POINT('Ctrl Pts',(-42.966080271284,5.28009112339822,-29.8027089865303));
#30945=CARTESIAN_POINT('Ctrl Pts',(-42.9476684412197,5.29118639926699,-30.0366412065176));
#30946=CARTESIAN_POINT('Ctrl Pts',(-42.9160330273132,5.30655790883432,-30.443405350357));
#30947=CARTESIAN_POINT('Ctrl Pts',(-42.8548567708032,5.32453906176737,-31.2704688469183));
#30948=CARTESIAN_POINT('Ctrl Pts',(-42.7908746025857,5.32108460865568,-32.2357156564981));
#30949=CARTESIAN_POINT('Ctrl Pts',(-42.7334017987881,5.30747776413526,-33.2239132019661));
#30950=CARTESIAN_POINT('Ctrl Pts',(-42.6934997484444,5.29594667190586,-33.9755180951015));
#30951=CARTESIAN_POINT('Ctrl Pts',(-42.656735262742,5.28708252845668,-34.7375742637586));
#30952=CARTESIAN_POINT('Ctrl Pts',(-42.6342288122971,5.285790467693,-35.2525723965959));
#30953=CARTESIAN_POINT('Ctrl Pts',(-42.6180198871815,5.28767511879397,-35.6420443252481));
#30954=CARTESIAN_POINT('Ctrl Pts',(-42.6075403525927,5.28879993451498,-35.889267876483));
#30955=CARTESIAN_POINT('Ctrl Pts',(-42.5880311795273,5.29088059660548,-36.3910999468938));
#30956=CARTESIAN_POINT('Ctrl Pts',(-42.5574740714464,5.29404486631059,-37.2645796050843));
#30957=CARTESIAN_POINT('Ctrl Pts',(-42.5084906513819,5.29882509433162,-39.0133321957582));
#30958=CARTESIAN_POINT('Ctrl Pts',(-42.4805858811114,5.30240885701596,-40.5146262302045));
#30959=CARTESIAN_POINT('Ctrl Pts',(-42.4597594875166,5.30695522943146,-41.6480970175863));
#30960=CARTESIAN_POINT('Ctrl Pts',(-42.4550925408997,5.30776155485162,-41.895606773929));
#30961=CARTESIAN_POINT('Ctrl Pts',(-42.4480332237712,5.30857619507488,-42.2692941279595));
#30962=CARTESIAN_POINT('Ctrl Pts',(-42.4410083438519,5.30906868577314,-42.6433511919673));
#30963=CARTESIAN_POINT('Ctrl Pts',(-42.4318302536459,5.30942931340334,-43.143491020825));
#30964=CARTESIAN_POINT('Ctrl Pts',(-42.4209580775566,5.30954744650048,-43.7704874992468));
#30965=CARTESIAN_POINT('Ctrl Pts',(-42.4096873604175,5.30990040654643,-44.5255677386172));
#30966=CARTESIAN_POINT('Ctrl Pts',(-42.4024519124516,5.31099253303746,-45.156538694259));
#30967=CARTESIAN_POINT('Ctrl Pts',(-42.3983446705665,5.31272170388111,-45.6621639986098));
#30968=CARTESIAN_POINT('Ctrl Pts',(-42.3962160420237,5.31454333820731,-46.0417335671184));
#30969=CARTESIAN_POINT('Ctrl Pts',(-42.3951398730034,5.31698481800948,-46.4215727361831));
#30970=CARTESIAN_POINT('Ctrl Pts',(-42.3952426337664,5.32120622622578,-46.9283776251192));
#30971=CARTESIAN_POINT('Ctrl Pts',(-42.3972151547764,5.32558029912895,-47.3085737880552));
#30972=CARTESIAN_POINT('Ctrl Pts',(-42.4006589313626,5.33101012342549,-47.6901709112403));
#30973=CARTESIAN_POINT('Ctrl Pts',(-42.4034686953696,5.33625743612167,-47.9582779372634));
#30974=CARTESIAN_POINT('Ctrl Pts',(-42.4109197846148,5.35122933246416,-48.4817957617174));
#30975=CARTESIAN_POINT('Ctrl Pts',(-42.4284500089677,5.38698475992364,-49.3888319680093));
#30976=CARTESIAN_POINT('Ctrl Pts',(-42.4643923523527,5.45039872226269,-50.6443179207177));
#30977=CARTESIAN_POINT('Ctrl Pts',(-42.5189548253264,5.5040358902261,-52.0909303402843));
#30978=CARTESIAN_POINT('Ctrl Pts',(-42.5586526259613,5.49929556965035,-53.0127495907653));
#30979=CARTESIAN_POINT('Ctrl Pts',(-42.583009031644,5.47695283862441,-53.5757195163897));
#30980=CARTESIAN_POINT('Ctrl Pts',(-42.5934150689954,5.46535897339064,-53.7741421322066));
#30981=CARTESIAN_POINT('Ctrl Pts',(-42.6162874901187,5.42723297073372,-54.2046560451703));
#30982=CARTESIAN_POINT('Ctrl Pts',(-42.6608944871551,5.32608219999238,-54.988660204803));
#30983=CARTESIAN_POINT('Ctrl Pts',(-42.7601501828626,5.02862385309719,-56.7101234471156));
#30984=CARTESIAN_POINT('Ctrl Pts',(-42.8417295651558,4.77257551658811,-58.4251999633534));
#30985=CARTESIAN_POINT('Ctrl Pts',(-42.8686094143971,4.85145432001225,-59.7649620853934));
#30986=CARTESIAN_POINT('Ctrl Pts',(-42.8717657002582,4.86099496633503,-59.9072004863649));
#30987=CARTESIAN_POINT('Ctrl Pts',(-42.8773262490722,4.88469292687789,-60.2020612790792));
#30988=CARTESIAN_POINT('Ctrl Pts',(-42.8853093445454,4.93604879276198,-60.7095931176271));
#30989=CARTESIAN_POINT('Ctrl Pts',(-42.8949090270911,5.07731157743547,-61.7175466105396));
#30990=CARTESIAN_POINT('Ctrl Pts',(-42.8947467815965,5.31517540413371,-62.8393181260782));
#30991=CARTESIAN_POINT('Ctrl Pts',(-42.8900097131894,5.60915460119308,-63.932328552125));
#30992=CARTESIAN_POINT('Ctrl Pts',(-42.8867894283273,5.7920401895333,-64.5353932787128));
#30993=CARTESIAN_POINT('Ctrl Pts',(-42.8848858010747,5.91980672807307,-64.9325635567599));
#30994=CARTESIAN_POINT('Ctrl Pts',(-42.8837125739361,6.00644847706447,-65.1959859459554));
#30995=CARTESIAN_POINT('Ctrl Pts',(-42.882724377332,6.09517694280922,-65.4575020380078));
#30996=CARTESIAN_POINT('Ctrl Pts',(-42.8821069494855,6.17435955732801,-65.6844870530957));
#30997=CARTESIAN_POINT('Ctrl Pts',(-42.8818355425142,6.22001574696898,-65.8136725464171));
#30998=CARTESIAN_POINT('Ctrl Pts',(-42.8815148822881,6.28890287374054,-66.0069553415058));
#30999=CARTESIAN_POINT('Ctrl Pts',(-42.8814404622754,6.34707681703438,-66.1669031179569));
#31000=CARTESIAN_POINT('Ctrl Pts',(-42.8816188770637,6.44449486278725,-66.4309243422751));
#31001=CARTESIAN_POINT('Ctrl Pts',(-42.880851859429,6.56223130155641,-66.7356201814902));
#31002=CARTESIAN_POINT('Ctrl Pts',(-42.8796354188091,6.80477221912943,-67.3125008499134));
#31003=CARTESIAN_POINT('Ctrl Pts',(-42.8769453178782,7.26482353503976,-68.3011228654526));
#31004=CARTESIAN_POINT('Ctrl Pts',(-42.8717733301943,8.26679949765506,-70.1591795787803));
#31005=CARTESIAN_POINT('Ctrl Pts',(-42.870413129688,9.14210741751194,-71.6194843562164));
#31006=CARTESIAN_POINT('Ctrl Pts',(-42.8729356151749,9.69552819953706,-72.671723686886));
#31007=CARTESIAN_POINT('Ctrl Pts',(-42.8726762410367,9.83124532059666,-72.9294181564817));
#31008=CARTESIAN_POINT('Ctrl Pts',(-42.8726546748704,10.0960730243121,-73.4309906589323));
#31009=CARTESIAN_POINT('Ctrl Pts',(-42.8724705779236,10.4306758301375,-74.0627413153577));
#31010=CARTESIAN_POINT('Ctrl Pts',(-42.8724112796876,10.8313703210138,-74.8166367741079));
#31011=CARTESIAN_POINT('Ctrl Pts',(-42.8723200277616,11.6345193230121,-76.3242084294796));
#31012=CARTESIAN_POINT('Ctrl Pts',(-42.8724075953763,12.3039112027909,-77.576767132054));
#31013=CARTESIAN_POINT('Ctrl Pts',(-42.8725343781945,13.2718195563419,-79.3973298027057));
#31014=CARTESIAN_POINT('Ctrl Pts',(-42.8724765736113,13.7091763374169,-80.2199919219157));
#31015=CARTESIAN_POINT('Ctrl Pts',(-42.8724765736115,14.1456979248064,-81.0409696240142));
#31016=CARTESIAN_POINT('Ctrl Pts',(-40.9893941583173,0.280290173804462,
24.8306665397013));
#31017=CARTESIAN_POINT('Ctrl Pts',(-40.9895177486156,0.280296428295455,
24.7817882354976));
#31018=CARTESIAN_POINT('Ctrl Pts',(-40.989647367799,0.280302986842126,24.7329109790473));
#31019=CARTESIAN_POINT('Ctrl Pts',(-40.9911780305211,0.280380545189393,
24.1823155147162));
#31020=CARTESIAN_POINT('Ctrl Pts',(-40.9923510756847,0.280421693213243,
23.1782062681366));
#31021=CARTESIAN_POINT('Ctrl Pts',(-40.995081018544,0.280503669861664,21.1696270086331));
#31022=CARTESIAN_POINT('Ctrl Pts',(-41.0052679693907,0.281021736168168,
19.6654822805891));
#31023=CARTESIAN_POINT('Ctrl Pts',(-41.0268730592858,0.282211835134878,
18.4144323008035));
#31024=CARTESIAN_POINT('Ctrl Pts',(-41.0372378337411,0.28277635701125,17.9116777228209));
#31025=CARTESIAN_POINT('Ctrl Pts',(-41.0632709191315,0.284184273608307,
16.9077383763575));
#31026=CARTESIAN_POINT('Ctrl Pts',(-41.1191113931709,0.287209632289243,
15.1539432392821));
#31027=CARTESIAN_POINT('Ctrl Pts',(-41.1721280107876,0.290186683943603,
13.6520484506017));
#31028=CARTESIAN_POINT('Ctrl Pts',(-41.2052986276455,0.292230205805187,
12.397322192359));
#31029=CARTESIAN_POINT('Ctrl Pts',(-41.2188536880839,0.29308595464525,11.8962622431662));
#31030=CARTESIAN_POINT('Ctrl Pts',(-41.2464704555292,0.294896996873047,
10.8942718424413));
#31031=CARTESIAN_POINT('Ctrl Pts',(-41.2942284734365,0.298167507818841,
9.14059348098497));
#31032=CARTESIAN_POINT('Ctrl Pts',(-41.3276788341157,0.300601301858155,
7.63555392933036));
#31033=CARTESIAN_POINT('Ctrl Pts',(-41.3424956731047,0.301692855427609,
6.50481572178853));
#31034=CARTESIAN_POINT('Ctrl Pts',(-41.3455479496262,0.301926824087675,
6.25451208273883));
#31035=CARTESIAN_POINT('Ctrl Pts',(-41.3508061529118,0.302363239284339,
5.75333715203142));
#31036=CARTESIAN_POINT('Ctrl Pts',(-41.3579058294151,0.303039188454316,
4.87488423146479));
#31037=CARTESIAN_POINT('Ctrl Pts',(-41.3646446561493,0.303994073880602,
3.11477538310501));
#31038=CARTESIAN_POINT('Ctrl Pts',(-41.3609067466047,0.30398518686012,1.60893149366535));
#31039=CARTESIAN_POINT('Ctrl Pts',(-41.3568515310369,0.303452938888166,
0.550184452068615));
#31040=CARTESIAN_POINT('Ctrl Pts',(-41.3563184779633,0.303382434888984,
0.424092420441241));
#31041=CARTESIAN_POINT('Ctrl Pts',(-41.3550634218872,0.303215802556436,
0.172099832926385));
#31042=CARTESIAN_POINT('Ctrl Pts',(-41.3523931530852,0.302859818499856,
-0.268408450246914));
#31043=CARTESIAN_POINT('Ctrl Pts',(-41.3473577456846,0.30218733918811,-0.896407546601593));
#31044=CARTESIAN_POINT('Ctrl Pts',(-41.3397754482278,0.301179512381092,
-1.64862299843257));
#31045=CARTESIAN_POINT('Ctrl Pts',(-41.3281793044161,0.299652753592981,
-2.65005274693771));
#31046=CARTESIAN_POINT('Ctrl Pts',(-41.3119317130866,0.297544977724727,
-3.90045626766242));
#31047=CARTESIAN_POINT('Ctrl Pts',(-41.2993328034355,0.296007850935482,
-4.90158738099382));
#31048=CARTESIAN_POINT('Ctrl Pts',(-41.2922774157016,0.295203263328682,
-5.52814145730737));
#31049=CARTESIAN_POINT('Ctrl Pts',(-41.2888114147919,0.294151273016196,
-5.76976978184256));
#31050=CARTESIAN_POINT('Ctrl Pts',(-41.2797870177376,0.289634238603212,
-6.26180555436338));
#31051=CARTESIAN_POINT('Ctrl Pts',(-41.2597421505567,0.27681258848934,-7.12814873920402));
#31052=CARTESIAN_POINT('Ctrl Pts',(-41.2260511487051,0.252733800345328,
-8.38969650658993));
#31053=CARTESIAN_POINT('Ctrl Pts',(-41.2044973404892,0.24345916428999,-9.67758707980947));
#31054=CARTESIAN_POINT('Ctrl Pts',(-41.2056903628757,0.257265492438425,
-10.5928358962625));
#31055=CARTESIAN_POINT('Ctrl Pts',(-41.2124295969221,0.272938590382539,
-11.1192946726198));
#31056=CARTESIAN_POINT('Ctrl Pts',(-41.2180486738718,0.283730411189719,
-11.3838864658141));
#31057=CARTESIAN_POINT('Ctrl Pts',(-41.2232136440982,0.2930859116899,-11.5831004907457));
#31058=CARTESIAN_POINT('Ctrl Pts',(-41.2270561501629,0.298405308527004,
-11.7004395131457));
#31059=CARTESIAN_POINT('Ctrl Pts',(-41.2359452524065,0.308839615257286,
-11.946106685933));
#31060=CARTESIAN_POINT('Ctrl Pts',(-41.2546055704108,0.325559075605228,
-12.3752463137554));
#31061=CARTESIAN_POINT('Ctrl Pts',(-41.3164265455899,0.366930410177482,
-13.5036868298348));
#31062=CARTESIAN_POINT('Ctrl Pts',(-41.4165120412304,0.432307031414684,
-14.8218483401688));
#31063=CARTESIAN_POINT('Ctrl Pts',(-41.5127262532785,0.611950064184939,
-16.2117418031106));
#31064=CARTESIAN_POINT('Ctrl Pts',(-41.5561223426356,0.739176733282308,
-16.9227777590329));
#31065=CARTESIAN_POINT('Ctrl Pts',(-41.5858614479214,0.867942626871003,
-17.5004660887901));
#31066=CARTESIAN_POINT('Ctrl Pts',(-41.5986983768322,0.94206072424014,-17.7917806119061));
#31067=CARTESIAN_POINT('Ctrl Pts',(-41.6073703760708,1.00139682202911,-18.0106350515628));
#31068=CARTESIAN_POINT('Ctrl Pts',(-41.6123650780398,1.04574782279505,-18.1684664922214));
#31069=CARTESIAN_POINT('Ctrl Pts',(-41.6233648741053,1.13917584297077,-18.4708250805361));
#31070=CARTESIAN_POINT('Ctrl Pts',(-41.634803967744,1.24230920609741,-18.7691933000577));
#31071=CARTESIAN_POINT('Ctrl Pts',(-41.6467674858292,1.35219820309014,-19.0591948969288));
#31072=CARTESIAN_POINT('Ctrl Pts',(-41.6543663333302,1.42359984545195,-19.2381423937385));
#31073=CARTESIAN_POINT('Ctrl Pts',(-41.6605197218763,1.4820643382338,-19.3796077886087));
#31074=CARTESIAN_POINT('Ctrl Pts',(-41.6667092573891,1.54138879073417,-19.5200999449311));
#31075=CARTESIAN_POINT('Ctrl Pts',(-41.6838703240796,1.70782961601363,-19.9023775192806));
#31076=CARTESIAN_POINT('Ctrl Pts',(-41.7124555728774,1.99507960498138,-20.5066336265271));
#31077=CARTESIAN_POINT('Ctrl Pts',(-41.762410749083,2.51980468748958,-21.5288699023996));
#31078=CARTESIAN_POINT('Ctrl Pts',(-41.819893857012,3.15292972952515,-22.7211160695818));
#31079=CARTESIAN_POINT('Ctrl Pts',(-41.848746085566,3.53754515746703,-23.5902702058667));
#31080=CARTESIAN_POINT('Ctrl Pts',(-41.8531760227506,3.70920242886249,-24.1019496614625));
#31081=CARTESIAN_POINT('Ctrl Pts',(-41.8475597634427,3.78250620861328,-24.3425402779051));
#31082=CARTESIAN_POINT('Ctrl Pts',(-41.8332475454277,3.91348902157027,-24.805984915587));
#31083=CARTESIAN_POINT('Ctrl Pts',(-41.7917422112982,4.11801901399799,-25.6355828824697));
#31084=CARTESIAN_POINT('Ctrl Pts',(-41.6981795389215,4.34113924375327,-26.8317148586573));
#31085=CARTESIAN_POINT('Ctrl Pts',(-41.5528775003771,4.53997149540172,-28.2866430086673));
#31086=CARTESIAN_POINT('Ctrl Pts',(-41.458479131446,4.65222796034505,-29.2631070048381));
#31087=CARTESIAN_POINT('Ctrl Pts',(-41.4151931262802,4.71539802949842,-29.8137442335345));
#31088=CARTESIAN_POINT('Ctrl Pts',(-41.4060298351662,4.72790458771569,-29.9284510055469));
#31089=CARTESIAN_POINT('Ctrl Pts',(-41.3871249451852,4.75189565799189,-30.1629293166748));
#31090=CARTESIAN_POINT('Ctrl Pts',(-41.3535090630033,4.78947966529287,-30.572866073278));
#31091=CARTESIAN_POINT('Ctrl Pts',(-41.2839763646377,4.85023216494433,-31.401771891854));
#31092=CARTESIAN_POINT('Ctrl Pts',(-41.2021060952701,4.89366453810222,-32.3653918006517));
#31093=CARTESIAN_POINT('Ctrl Pts',(-41.1226823950886,4.92648406614013,-33.3475001279598));
#31094=CARTESIAN_POINT('Ctrl Pts',(-41.0655540894473,4.9494840992214,-34.0930378769679));
#31095=CARTESIAN_POINT('Ctrl Pts',(-41.011989975364,4.97464424292071,-34.8476229623568));
#31096=CARTESIAN_POINT('Ctrl Pts',(-40.9793866125484,4.99541429903991,-35.3568061789837));
#31097=CARTESIAN_POINT('Ctrl Pts',(-40.9562950743291,5.013520002653,-35.7416216108422));
#31098=CARTESIAN_POINT('Ctrl Pts',(-40.9413580508551,5.02474703743586,-35.9871460126007));
#31099=CARTESIAN_POINT('Ctrl Pts',(-40.9129411234468,5.04703973134136,-36.4848114727042));
#31100=CARTESIAN_POINT('Ctrl Pts',(-40.8670672335441,5.0841199248743,-37.3515626087591));
#31101=CARTESIAN_POINT('Ctrl Pts',(-40.7887382032561,5.15284178929198,-39.0869347384886));
#31102=CARTESIAN_POINT('Ctrl Pts',(-40.7383890275233,5.20209094587151,-40.5776698659022));
#31103=CARTESIAN_POINT('Ctrl Pts',(-40.7026003827779,5.23629387418686,-41.7033590423549));
#31104=CARTESIAN_POINT('Ctrl Pts',(-40.6947447559412,5.24353641556213,-41.9494496889739));
#31105=CARTESIAN_POINT('Ctrl Pts',(-40.6831450578572,5.25366097348401,-42.3207558307205));
#31106=CARTESIAN_POINT('Ctrl Pts',(-40.6718150888099,5.26309548536225,-42.692400344777));
#31107=CARTESIAN_POINT('Ctrl Pts',(-40.6571661791622,5.27485319002791,-43.1891777061944));
#31108=CARTESIAN_POINT('Ctrl Pts',(-40.6399177519583,5.2881969783719,-43.8117785949811));
#31109=CARTESIAN_POINT('Ctrl Pts',(-40.6215360973513,5.30262611370692,-44.5612594341765));
#31110=CARTESIAN_POINT('Ctrl Pts',(-40.6086618487947,5.31381997478719,-45.1873091829714));
#31111=CARTESIAN_POINT('Ctrl Pts',(-40.6001715928118,5.32264137343099,-45.6888585175579));
#31112=CARTESIAN_POINT('Ctrl Pts',(-40.594768069357,5.32923855463232,-46.0652951836812));
#31113=CARTESIAN_POINT('Ctrl Pts',(-40.5904073885478,5.33589999628747,-46.4419280754876));
#31114=CARTESIAN_POINT('Ctrl Pts',(-40.5860983180208,5.34497333867694,-46.9443661359885));
#31115=CARTESIAN_POINT('Ctrl Pts',(-40.5846293700653,5.35210128769182,-47.3211687659398));
#31116=CARTESIAN_POINT('Ctrl Pts',(-40.5845324546587,5.35963258663933,-47.6992852599114));
#31117=CARTESIAN_POINT('Ctrl Pts',(-40.5849097349468,5.36600268597118,-47.9641074827081));
#31118=CARTESIAN_POINT('Ctrl Pts',(-40.5873494265197,5.38199177152275,-48.4821214154056));
#31119=CARTESIAN_POINT('Ctrl Pts',(-40.5957227204869,5.41657899625576,-49.3804111342591));
#31120=CARTESIAN_POINT('Ctrl Pts',(-40.6178354563581,5.47168116794954,-50.6268280187354));
#31121=CARTESIAN_POINT('Ctrl Pts',(-40.6556343690552,5.50866564955266,-52.0671976655524));
#31122=CARTESIAN_POINT('Ctrl Pts',(-40.6853664855489,5.4917947350123,-52.9879942074645));
#31123=CARTESIAN_POINT('Ctrl Pts',(-40.7044696227113,5.46214712496547,-53.5512304200892));
#31124=CARTESIAN_POINT('Ctrl Pts',(-40.7128455580891,5.44787630494579,-53.7456026395922));
#31125=CARTESIAN_POINT('Ctrl Pts',(-40.7318083464858,5.40309378786118,-54.171519977409));
#31126=CARTESIAN_POINT('Ctrl Pts',(-40.7701270093372,5.28776865106253,-54.948811372113));
#31127=CARTESIAN_POINT('Ctrl Pts',(-40.8593317204784,4.95330030990605,-56.6664624097345));
#31128=CARTESIAN_POINT('Ctrl Pts',(-40.9364947249792,4.65832218134193,-58.3911740051108));
#31129=CARTESIAN_POINT('Ctrl Pts',(-40.9617903823933,4.72638396747244,-59.7488048668769));
#31130=CARTESIAN_POINT('Ctrl Pts',(-40.9647461461571,4.73485155802129,-59.8925661466653));
#31131=CARTESIAN_POINT('Ctrl Pts',(-40.9700258512831,4.75671650338397,-60.1906469541753));
#31132=CARTESIAN_POINT('Ctrl Pts',(-40.9777600062064,4.80587520115248,-60.7031893893145));
#31133=CARTESIAN_POINT('Ctrl Pts',(-40.987752912195,4.94604258228551,-61.7194421890793));
#31134=CARTESIAN_POINT('Ctrl Pts',(-40.9895154351334,5.18793826020981,-62.8463958974618));
#31135=CARTESIAN_POINT('Ctrl Pts',(-40.9871730813637,5.48701942402319,-63.940890731633));
#31136=CARTESIAN_POINT('Ctrl Pts',(-40.9852848038056,5.67251371052068,-64.5434949804964));
#31137=CARTESIAN_POINT('Ctrl Pts',(-40.9841884694266,5.80164006935051,-64.9398526733912));
#31138=CARTESIAN_POINT('Ctrl Pts',(-40.9835271184745,5.8890677405049,-65.2025993618358));
#31139=CARTESIAN_POINT('Ctrl Pts',(-40.9830027941993,5.97838745269654,-65.4632441843856));
#31140=CARTESIAN_POINT('Ctrl Pts',(-40.9827382954141,6.05786032431043,-65.6892951122439));
#31141=CARTESIAN_POINT('Ctrl Pts',(-40.9826514989447,6.10361269246761,-65.8178979997058));
#31142=CARTESIAN_POINT('Ctrl Pts',(-40.9825900249628,6.17257138556137,-66.0102599184474));
#31143=CARTESIAN_POINT('Ctrl Pts',(-40.9826914604614,6.23064889175667,-66.1693354930749));
#31144=CARTESIAN_POINT('Ctrl Pts',(-40.9831030283092,6.32767483575051,-66.4318170111501));
#31145=CARTESIAN_POINT('Ctrl Pts',(-40.9826595018947,6.44574019605698,-66.7368488770948));
#31146=CARTESIAN_POINT('Ctrl Pts',(-40.9819573406223,6.68846187245255,-67.3133359663928));
#31147=CARTESIAN_POINT('Ctrl Pts',(-40.9799958154659,7.14893613993861,-68.3018775822024));
#31148=CARTESIAN_POINT('Ctrl Pts',(-40.9755278485363,8.15121009323467,-70.1595076830405));
#31149=CARTESIAN_POINT('Ctrl Pts',(-40.973771100275,9.02663496104393,-71.619963856248));
#31150=CARTESIAN_POINT('Ctrl Pts',(-40.9759105947828,9.58019735042475,-72.6723092429353));
#31151=CARTESIAN_POINT('Ctrl Pts',(-40.975697760016,9.71592560132571,-72.9299653026806));
#31152=CARTESIAN_POINT('Ctrl Pts',(-40.9756869923594,9.9807728149155,-73.4315008472055));
#31153=CARTESIAN_POINT('Ctrl Pts',(-40.9755363779319,10.3153830864914,-74.0632051376608));
#31154=CARTESIAN_POINT('Ctrl Pts',(-40.9754873852925,10.7160627683641,-74.8170628142835));
#31155=CARTESIAN_POINT('Ctrl Pts',(-40.975405045408,11.5191559679699,-76.3245831081049));
#31156=CARTESIAN_POINT('Ctrl Pts',(-40.9754603446411,12.1885044744805,-77.577180313731));
#31157=CARTESIAN_POINT('Ctrl Pts',(-40.9755617664425,13.1564671972782,-79.3978378813868));
#31158=CARTESIAN_POINT('Ctrl Pts',(-40.9755123070535,13.5938177436188,-80.2204798316628));
#31159=CARTESIAN_POINT('Ctrl Pts',(-40.9755123070534,14.0303393310083,-81.0414575337613));
#31160=CARTESIAN_POINT('Ctrl Pts',(-39.0888001402497,0.180014935889884,
24.830657879308));
#31161=CARTESIAN_POINT('Ctrl Pts',(-39.088917316815,0.180019720217799,24.7817793004034));
#31162=CARTESIAN_POINT('Ctrl Pts',(-39.0890402101583,0.180024736696177,
24.7329017756012));
#31163=CARTESIAN_POINT('Ctrl Pts',(-39.0904914691558,0.1800840769936,24.1823027164344));
#31164=CARTESIAN_POINT('Ctrl Pts',(-39.0915869337663,0.180115913204324,
23.1781842967628));
#31165=CARTESIAN_POINT('Ctrl Pts',(-39.0941254999962,0.180179361754887,
21.1695999880857));
#31166=CARTESIAN_POINT('Ctrl Pts',(-39.1037841631934,0.180575900260667,
19.6654506338937));
#31167=CARTESIAN_POINT('Ctrl Pts',(-39.1243530113637,0.181485107226502,
18.4144014643961));
#31168=CARTESIAN_POINT('Ctrl Pts',(-39.1342130895912,0.181914718605493,
17.9116384563228));
#31169=CARTESIAN_POINT('Ctrl Pts',(-39.1589647024343,0.182983006233729,
16.9076901036643));
#31170=CARTESIAN_POINT('Ctrl Pts',(-39.2120609298036,0.185277316979706,
15.1538859030914));
#31171=CARTESIAN_POINT('Ctrl Pts',(-39.2625778615799,0.187551451732393,
13.6519981771989));
#31172=CARTESIAN_POINT('Ctrl Pts',(-39.2943891236822,0.189143259235937,
12.3973026245927));
#31173=CARTESIAN_POINT('Ctrl Pts',(-39.3074124097061,0.189812747891297,
11.8962578221136));
#31174=CARTESIAN_POINT('Ctrl Pts',(-39.3340182664446,0.191239244045362,
10.8942890475992));
#31175=CARTESIAN_POINT('Ctrl Pts',(-39.3801811561126,0.193834769361145,
9.14063943512921));
#31176=CARTESIAN_POINT('Ctrl Pts',(-39.4126589643153,0.195790079789512,
7.63554879952261));
#31177=CARTESIAN_POINT('Ctrl Pts',(-39.4270732637367,0.196673507474238,
6.50476253261587));
#31178=CARTESIAN_POINT('Ctrl Pts',(-39.4300591616367,0.196865202842096,
6.25445276686468));
#31179=CARTESIAN_POINT('Ctrl Pts',(-39.435258941596,0.197232346757206,5.75326596535956));
#31180=CARTESIAN_POINT('Ctrl Pts',(-39.4424218889848,0.197824694995779,
4.87478350553763));
#31181=CARTESIAN_POINT('Ctrl Pts',(-39.4497283637274,0.198728008388997,
3.11464478187555));
#31182=CARTESIAN_POINT('Ctrl Pts',(-39.4464205151028,0.198795280639079,
1.60867012703468));
#31183=CARTESIAN_POINT('Ctrl Pts',(-39.4418897974239,0.198252367947847,
0.549909941536338));
#31184=CARTESIAN_POINT('Ctrl Pts',(-39.4412945938795,0.19817944770704,0.423835971767908));
#31185=CARTESIAN_POINT('Ctrl Pts',(-39.4398911800345,0.198005968854597,
0.171865376680441));
#31186=CARTESIAN_POINT('Ctrl Pts',(-39.4369038750975,0.197632386715154,
-0.268604612588512));
#31187=CARTESIAN_POINT('Ctrl Pts',(-39.4312715773556,0.196928009174792,
-0.896605488280534));
#31188=CARTESIAN_POINT('Ctrl Pts',(-39.4228297437873,0.195872319618578,
-1.64880469502484));
#31189=CARTESIAN_POINT('Ctrl Pts',(-39.4099859739263,0.194306211522286,
-2.65032787018934));
#31190=CARTESIAN_POINT('Ctrl Pts',(-39.3922032627337,0.19221850645099,-3.90095990403691));
#31191=CARTESIAN_POINT('Ctrl Pts',(-39.378747393108,0.190844849193783,-4.90238820218311));
#31192=CARTESIAN_POINT('Ctrl Pts',(-39.3714091220386,0.190178367126032,
-5.52939258666469));
#31193=CARTESIAN_POINT('Ctrl Pts',(-39.3680546353478,0.18966453923232,-5.77732002007598));
#31194=CARTESIAN_POINT('Ctrl Pts',(-39.3599802837624,0.187845064398476,
-6.27624133314443));
#31195=CARTESIAN_POINT('Ctrl Pts',(-39.3430898444979,0.183072961379129,
-7.15137827865571));
#31196=CARTESIAN_POINT('Ctrl Pts',(-39.3157200332037,0.174613443335135,
-8.40956553707685));
#31197=CARTESIAN_POINT('Ctrl Pts',(-39.2965427974573,0.171291036054527,
-9.67486480366862));
#31198=CARTESIAN_POINT('Ctrl Pts',(-39.2939925399169,0.175456322303922,
-10.5634021553277));
#31199=CARTESIAN_POINT('Ctrl Pts',(-39.2965820046209,0.180257888939277,
-11.0715965941404));
#31200=CARTESIAN_POINT('Ctrl Pts',(-39.2993797017071,0.183568770539792,
-11.3259916623919));
#31201=CARTESIAN_POINT('Ctrl Pts',(-39.3021139832257,0.18643660005113,-11.5172312282543));
#31202=CARTESIAN_POINT('Ctrl Pts',(-39.3040028599904,0.18784577223247,-11.6321372911683));
#31203=CARTESIAN_POINT('Ctrl Pts',(-39.3079866743959,0.189457764488112,
-11.8713533836034));
#31204=CARTESIAN_POINT('Ctrl Pts',(-39.315572292305,0.189102148698272,-12.290150002075));
#31205=CARTESIAN_POINT('Ctrl Pts',(-39.3387249841932,0.176966665062875,
-13.3922597388429));
#31206=CARTESIAN_POINT('Ctrl Pts',(-39.3793104509326,0.152177319720917,
-14.684616780296));
#31207=CARTESIAN_POINT('Ctrl Pts',(-39.4444008963079,0.21143366494283,-16.0553046278289));
#31208=CARTESIAN_POINT('Ctrl Pts',(-39.4833859783724,0.272345394836458,
-16.7594975111963));
#31209=CARTESIAN_POINT('Ctrl Pts',(-39.5185388384933,0.345561837178436,
-17.3338623275751));
#31210=CARTESIAN_POINT('Ctrl Pts',(-39.5373323495522,0.391465068195811,
-17.6244284353275));
#31211=CARTESIAN_POINT('Ctrl Pts',(-39.5518079010771,0.429580386052769,
-17.8427249662891));
#31212=CARTESIAN_POINT('Ctrl Pts',(-39.5620866349126,0.456154357016654,
-17.9895464754391));
#31213=CARTESIAN_POINT('Ctrl Pts',(-39.5848759972109,0.514268268353239,
-18.2788335636466));
#31214=CARTESIAN_POINT('Ctrl Pts',(-39.6107202132686,0.579518601695886,
-18.5650135488669));
#31215=CARTESIAN_POINT('Ctrl Pts',(-39.6389605015963,0.651049904192671,
-18.8469815608269));
#31216=CARTESIAN_POINT('Ctrl Pts',(-39.6574562047748,0.698220492300876,
-19.0217040811562));
#31217=CARTESIAN_POINT('Ctrl Pts',(-39.6726828915373,0.737326663489326,
-19.1604954431962));
#31218=CARTESIAN_POINT('Ctrl Pts',(-39.6881655249372,0.77731466885754,-19.2986584821118));
#31219=CARTESIAN_POINT('Ctrl Pts',(-39.7316739135483,0.890776531212825,
-19.6760510166773));
#31220=CARTESIAN_POINT('Ctrl Pts',(-39.8066717585052,1.09398254141055,-20.279461655595));
#31221=CARTESIAN_POINT('Ctrl Pts',(-39.938277838171,1.48656520365138,-21.3150620832206));
#31222=CARTESIAN_POINT('Ctrl Pts',(-40.077341632778,2.00010489798032,-22.5472072770752));
#31223=CARTESIAN_POINT('Ctrl Pts',(-40.1321456942686,2.35388577460762,-23.4873219699195));
#31224=CARTESIAN_POINT('Ctrl Pts',(-40.1423069080736,2.53192731380775,-24.0633993869248));
#31225=CARTESIAN_POINT('Ctrl Pts',(-40.1399193224519,2.60832765495067,-24.3236021119375));
#31226=CARTESIAN_POINT('Ctrl Pts',(-40.1306249350369,2.75420279393139,-24.8247767992029));
#31227=CARTESIAN_POINT('Ctrl Pts',(-40.0971915732182,3.00295949420497,-25.7086237547162));
#31228=CARTESIAN_POINT('Ctrl Pts',(-40.0175805133852,3.3317714798528,-26.9556647229161));
#31229=CARTESIAN_POINT('Ctrl Pts',(-39.9025787170737,3.67809396319729,-28.4272529350418));
#31230=CARTESIAN_POINT('Ctrl Pts',(-39.8342238291159,3.86827373793614,-29.3797360671715));
#31231=CARTESIAN_POINT('Ctrl Pts',(-39.8047440456974,3.96216351133329,-29.9060423092907));
#31232=CARTESIAN_POINT('Ctrl Pts',(-39.7980205429724,3.98281121426406,-30.0247942372537));
#31233=CARTESIAN_POINT('Ctrl Pts',(-39.7842215053032,4.02234921237497,-30.2618607419045));
#31234=CARTESIAN_POINT('Ctrl Pts',(-39.759065878212,4.08747327702048,-30.6785565729723));
#31235=CARTESIAN_POINT('Ctrl Pts',(-39.7053748797711,4.20257737944751,-31.5169004102997));
#31236=CARTESIAN_POINT('Ctrl Pts',(-39.6384024007534,4.30612538685423,-32.4870338490126));
#31237=CARTESIAN_POINT('Ctrl Pts',(-39.5709404467581,4.39498269524525,-33.4687208426889));
#31238=CARTESIAN_POINT('Ctrl Pts',(-39.5215021532756,4.45768407502833,-34.2108591571771));
#31239=CARTESIAN_POINT('Ctrl Pts',(-39.4745696175246,4.51979157863402,-34.9587372020336));
#31240=CARTESIAN_POINT('Ctrl Pts',(-39.445985531223,4.56308844149943,-35.4612789463547));
#31241=CARTESIAN_POINT('Ctrl Pts',(-39.4259196026876,4.59716788322673,-35.8403775332147));
#31242=CARTESIAN_POINT('Ctrl Pts',(-39.4131817355006,4.61873093705687,-36.0854247647449));
#31243=CARTESIAN_POINT('Ctrl Pts',(-39.3886213104214,4.66107995131486,-36.5801668389091));
#31244=CARTESIAN_POINT('Ctrl Pts',(-39.3484506852508,4.73169399829863,-37.4426539206428));
#31245=CARTESIAN_POINT('Ctrl Pts',(-39.2770325138226,4.86037280466502,-39.1682155632337));
#31246=CARTESIAN_POINT('Ctrl Pts',(-39.2250551732578,4.9518917528671,-40.6505718461251));
#31247=CARTESIAN_POINT('Ctrl Pts',(-39.1846961695626,5.01278499443786,-41.7696323310482));
#31248=CARTESIAN_POINT('Ctrl Pts',(-39.1759032210977,5.02560217778097,-42.0139439899814));
#31249=CARTESIAN_POINT('Ctrl Pts',(-39.1629861359318,5.04379504566374,-42.3827593007497));
#31250=CARTESIAN_POINT('Ctrl Pts',(-39.1503600309008,5.06089925268883,-42.751882115462));
#31251=CARTESIAN_POINT('Ctrl Pts',(-39.1339231628734,5.08244887061201,-43.2453711960376));
#31252=CARTESIAN_POINT('Ctrl Pts',(-39.1141180502777,5.10720146264421,-43.8639216187556));
#31253=CARTESIAN_POINT('Ctrl Pts',(-39.0915763560939,5.13419137727256,-44.6086927863444));
#31254=CARTESIAN_POINT('Ctrl Pts',(-39.0738339354335,5.15507688085906,-45.2309580981883));
#31255=CARTESIAN_POINT('Ctrl Pts',(-39.0601599988728,5.1711967266364,-45.7295050929459));
#31256=CARTESIAN_POINT('Ctrl Pts',(-39.0502199963603,5.18311514449177,-46.1037425988828));
#31257=CARTESIAN_POINT('Ctrl Pts',(-39.040590911943,5.19496343795989,-46.4782291876173));
#31258=CARTESIAN_POINT('Ctrl Pts',(-39.0281251283629,5.21082106856711,-46.9778584393184));
#31259=CARTESIAN_POINT('Ctrl Pts',(-39.0193494459446,5.22292443950463,-47.3527036794028));
#31260=CARTESIAN_POINT('Ctrl Pts',(-39.010785432795,5.23546148056151,-47.7288783242806));
#31261=CARTESIAN_POINT('Ctrl Pts',(-39.0049867958231,5.24532767241946,-47.99209865349));
#31262=CARTESIAN_POINT('Ctrl Pts',(-38.9935183667642,5.26803527005199,-48.5071264413013));
#31263=CARTESIAN_POINT('Ctrl Pts',(-38.9740978249696,5.31410466326364,-49.4002542868204));
#31264=CARTESIAN_POINT('Ctrl Pts',(-38.950268636064,5.38418388501746,-50.6397406224838));
#31265=CARTESIAN_POINT('Ctrl Pts',(-38.932566017396,5.43631146552384,-52.0727982524135));
#31266=CARTESIAN_POINT('Ctrl Pts',(-38.9304335441673,5.42536496789242,-52.989488255695));
#31267=CARTESIAN_POINT('Ctrl Pts',(-38.9325212625522,5.39799805998086,-53.5500667727227));
#31268=CARTESIAN_POINT('Ctrl Pts',(-38.9336400312047,5.38485977924212,-53.7411047660093));
#31269=CARTESIAN_POINT('Ctrl Pts',(-38.9381602028544,5.34123153060828,-54.162852555021));
#31270=CARTESIAN_POINT('Ctrl Pts',(-38.9511573760908,5.22510906383587,-54.9346379848697));
#31271=CARTESIAN_POINT('Ctrl Pts',(-38.99249631887,4.87818796877245,-56.6484569514821));
#31272=CARTESIAN_POINT('Ctrl Pts',(-39.0347434104756,4.56039247618866,-58.3763175489968));
#31273=CARTESIAN_POINT('Ctrl Pts',(-39.047584331385,4.62341883253982,-59.7441081601773));
#31274=CARTESIAN_POINT('Ctrl Pts',(-39.0491546243172,4.63134886187758,-59.888231420937));
#31275=CARTESIAN_POINT('Ctrl Pts',(-39.0521002138274,4.65230957090921,-60.1874606307571));
#31276=CARTESIAN_POINT('Ctrl Pts',(-39.0568531914575,4.70032857345361,-60.7016038103045));
#31277=CARTESIAN_POINT('Ctrl Pts',(-39.0648358030033,4.83977848561367,-61.7205854703363));
#31278=CARTESIAN_POINT('Ctrl Pts',(-39.0710371837721,5.08321114489323,-62.8490547844155));
#31279=CARTESIAN_POINT('Ctrl Pts',(-39.0752893734243,5.38430626057982,-63.9439118204513));
#31280=CARTESIAN_POINT('Ctrl Pts',(-39.0771678446726,5.57084391741088,-64.5463225625434));
#31281=CARTESIAN_POINT('Ctrl Pts',(-39.0782980372909,5.7005156786258,-64.9424025034742));
#31282=CARTESIAN_POINT('Ctrl Pts',(-39.0790260694853,5.78826738637908,-65.2049249557145));
#31283=CARTESIAN_POINT('Ctrl Pts',(-39.0797243904785,5.87782236693452,-65.4652869654959));
#31284=CARTESIAN_POINT('Ctrl Pts',(-39.0803275770349,5.9574276594848,-65.6910396260822));
#31285=CARTESIAN_POINT('Ctrl Pts',(-39.0806724498338,6.00323009922179,-65.8194573134073));
#31286=CARTESIAN_POINT('Ctrl Pts',(-39.0811905813148,6.07223862779016,-66.0115272311747));
#31287=CARTESIAN_POINT('Ctrl Pts',(-39.0816290864477,6.1302936813055,-66.1703283551057));
#31288=CARTESIAN_POINT('Ctrl Pts',(-39.0823627216747,6.22720787006558,-66.4323252988748));
#31289=CARTESIAN_POINT('Ctrl Pts',(-39.0823776143426,6.34540720480139,-66.7374778327143));
#31290=CARTESIAN_POINT('Ctrl Pts',(-39.0823957104839,6.58823809941028,-67.313857165032));
#31291=CARTESIAN_POINT('Ctrl Pts',(-39.0814717921701,7.04891545187278,-68.3024021835632));
#31292=CARTESIAN_POINT('Ctrl Pts',(-39.0780496028852,8.05141164755579,-70.1599254084202));
#31293=CARTESIAN_POINT('Ctrl Pts',(-39.0759953206185,8.92684028983922,-71.6204368595171));
#31294=CARTESIAN_POINT('Ctrl Pts',(-39.0778599491261,9.48038853571346,-72.6727773216162));
#31295=CARTESIAN_POINT('Ctrl Pts',(-39.0777132912002,9.61612625611812,-72.9304182491998));
#31296=CARTESIAN_POINT('Ctrl Pts',(-39.0777424553879,9.88098000736009,-73.4319337176093));
#31297=CARTESIAN_POINT('Ctrl Pts',(-39.0776485013891,10.2155871994595,-74.0636178095387));
#31298=CARTESIAN_POINT('Ctrl Pts',(-39.0776133302215,10.6162558456429,-74.8174574888145));
#31299=CARTESIAN_POINT('Ctrl Pts',(-39.0775181921913,11.4193149429609,-76.324955350321));
#31300=CARTESIAN_POINT('Ctrl Pts',(-39.0775016266082,12.0886088877304,-77.5775761907898));
#31301=CARTESIAN_POINT('Ctrl Pts',(-39.0775880817214,13.0565775367831,-79.3982814865315));
#31302=CARTESIAN_POINT('Ctrl Pts',(-39.0775513690795,13.4939157183239,-80.220915054068));
#31303=CARTESIAN_POINT('Ctrl Pts',(-39.0775513690794,13.9304373057134,-81.0418927561665));
#31304=CARTESIAN_POINT('Ctrl Pts',(-36.711201720155,0.0846755602148468,
24.8306211994035));
#31305=CARTESIAN_POINT('Ctrl Pts',(-36.7113120028643,0.0846793100877247,
24.781741457617));
#31306=CARTESIAN_POINT('Ctrl Pts',(-36.7114276655895,0.0846832415760904,
24.7328627565529));
#31307=CARTESIAN_POINT('Ctrl Pts',(-36.7127935402306,0.0847297050999628,
24.1822497869885));
#31308=CARTESIAN_POINT('Ctrl Pts',(-36.7138292815451,0.0847707447900342,
23.1781129164513));
#31309=CARTESIAN_POINT('Ctrl Pts',(-36.7162322116714,0.0848690308091877,
21.1695035269936));
#31310=CARTESIAN_POINT('Ctrl Pts',(-36.7253229946257,0.0851785210529226,
19.6653423171276));
#31311=CARTESIAN_POINT('Ctrl Pts',(-36.7446583985594,0.08580782489809,18.4142882582294));
#31312=CARTESIAN_POINT('Ctrl Pts',(-36.7539257158908,0.0861108837197817,
17.9114529545179));
#31313=CARTESIAN_POINT('Ctrl Pts',(-36.7771865730825,0.0868740440157173,
16.907452295697));
#31314=CARTESIAN_POINT('Ctrl Pts',(-36.8270801555423,0.0885088814981871,
15.1536537250934));
#31315=CARTESIAN_POINT('Ctrl Pts',(-36.8745592957761,0.0900397746859907,
13.6519842643687));
#31316=CARTESIAN_POINT('Ctrl Pts',(-36.9044697043829,0.0909569223699599,
12.3975856133512));
#31317=CARTESIAN_POINT('Ctrl Pts',(-36.9167133201501,0.0913268259956495,
11.8966636497452));
#31318=CARTESIAN_POINT('Ctrl Pts',(-36.9417262912308,0.0920656429738596,
10.8948714710037));
#31319=CARTESIAN_POINT('Ctrl Pts',(-36.9851279506764,0.0933122188435441,
9.1413912793788));
#31320=CARTESIAN_POINT('Ctrl Pts',(-37.0156998270508,0.094154200871692,
7.63616215370004));
#31321=CARTESIAN_POINT('Ctrl Pts',(-37.0293041574709,0.0945217035687127,
6.50517410116762));
#31322=CARTESIAN_POINT('Ctrl Pts',(-37.0321344090801,0.0945957446429915,
6.25497355792918));
#31323=CARTESIAN_POINT('Ctrl Pts',(-37.0371099539078,0.0947172428471553,
5.75388043569213));
#31324=CARTESIAN_POINT('Ctrl Pts',(-37.0440813507022,0.0948653916598738,
4.87550989883566));
#31325=CARTESIAN_POINT('Ctrl Pts',(-37.0515656864022,0.0949446315277831,
3.11521636198001));
#31326=CARTESIAN_POINT('Ctrl Pts',(-37.0486042606475,0.0947837520977546,
1.60843751337755));
#31327=CARTESIAN_POINT('Ctrl Pts',(-37.0436575257864,0.0946981767982494,
0.548825679997348));
#31328=CARTESIAN_POINT('Ctrl Pts',(-37.043006429047,0.0946869608203108,
0.42262179116806));
#31329=CARTESIAN_POINT('Ctrl Pts',(-37.0414718052386,0.0946612696963625,
0.170422155403115));
#31330=CARTESIAN_POINT('Ctrl Pts',(-37.0382061177981,0.0946079689969842,
-0.270422265079373));
#31331=CARTESIAN_POINT('Ctrl Pts',(-37.0320655020198,0.0945099200478035,
-0.898877882758254));
#31332=CARTESIAN_POINT('Ctrl Pts',(-37.0228968170096,0.0943654510376819,
-1.65141723036078));
#31333=CARTESIAN_POINT('Ctrl Pts',(-37.0090454046044,0.0941451688310354,
-2.65321592415316));
#31334=CARTESIAN_POINT('Ctrl Pts',(-36.9900886001485,0.0938334943865793,
-3.90374987560333));
#31335=CARTESIAN_POINT('Ctrl Pts',(-36.9762392465201,0.0935908348151571,
-4.90470775986227));
#31336=CARTESIAN_POINT('Ctrl Pts',(-36.9689346734598,0.0934561646239056,
-5.53141437390056));
#31337=CARTESIAN_POINT('Ctrl Pts',(-36.965885586203,0.0934560411160533,
-5.78303893549836));
#31338=CARTESIAN_POINT('Ctrl Pts',(-36.9593883633974,0.0936321220515418,
-6.28587838196509));
#31339=CARTESIAN_POINT('Ctrl Pts',(-36.9472326785285,0.0942940185030665,
-7.16602952983162));
#31340=CARTESIAN_POINT('Ctrl Pts',(-36.9291349809246,0.0956253346127282,
-8.42199169718575));
#31341=CARTESIAN_POINT('Ctrl Pts',(-36.9140717168774,0.0958606590365747,
-9.67372572928418));
#31342=CARTESIAN_POINT('Ctrl Pts',(-36.9072337971097,0.0946254783342841,
-10.5462632941664));
#31343=CARTESIAN_POINT('Ctrl Pts',(-36.9046865248374,0.0934036409850022,
-11.0435648660092));
#31344=CARTESIAN_POINT('Ctrl Pts',(-36.9039172100298,0.0926004122272295,
-11.2918236171607));
#31345=CARTESIAN_POINT('Ctrl Pts',(-36.9035454721218,0.091917758319367,
-11.4784129535007));
#31346=CARTESIAN_POINT('Ctrl Pts',(-36.903145201881,0.0912228891846152,
-11.5969669025978));
#31347=CARTESIAN_POINT('Ctrl Pts',(-36.90181679827,0.0887691377984597,-11.8388638582651));
#31348=CARTESIAN_POINT('Ctrl Pts',(-36.8982881049238,0.0819826877349684,
-12.2623898158901));
#31349=CARTESIAN_POINT('Ctrl Pts',(-36.8849363606277,0.0544659407479422,
-13.3650568718358));
#31350=CARTESIAN_POINT('Ctrl Pts',(-36.8684847756465,0.00874815982371367,
-14.627968204471));
#31351=CARTESIAN_POINT('Ctrl Pts',(-36.8839622816576,-0.00132236754599921,
-15.9394295488705));
#31352=CARTESIAN_POINT('Ctrl Pts',(-36.9025953000082,0.00750601117003104,
-16.6076385810686));
#31353=CARTESIAN_POINT('Ctrl Pts',(-36.925786968904,0.0259046380924417,
-17.1501533085901));
#31354=CARTESIAN_POINT('Ctrl Pts',(-36.9404471432345,0.0394895220043137,
-17.4241536500862));
#31355=CARTESIAN_POINT('Ctrl Pts',(-36.9526487163045,0.0514713443528451,
-17.6296084885903));
#31356=CARTESIAN_POINT('Ctrl Pts',(-36.9613582831,0.0590767589393235,-17.7579478738763));
#31357=CARTESIAN_POINT('Ctrl Pts',(-36.9811360664443,0.0758277090006206,
-18.0191008493755));
#31358=CARTESIAN_POINT('Ctrl Pts',(-37.0042522483177,0.0943242665168838,
-18.2787705289901));
#31359=CARTESIAN_POINT('Ctrl Pts',(-37.0302501055141,0.114900987587735,
-18.5394145596037));
#31360=CARTESIAN_POINT('Ctrl Pts',(-37.0476045005527,0.128621094582331,
-18.7021796534871));
#31361=CARTESIAN_POINT('Ctrl Pts',(-37.0620917261753,0.140142097953813,
-18.8324923503967));
#31362=CARTESIAN_POINT('Ctrl Pts',(-37.0769615753961,0.152028238022326,
-18.962802336705));
#31363=CARTESIAN_POINT('Ctrl Pts',(-37.1193491862782,0.186251732259979,
-19.3212842178248));
#31364=CARTESIAN_POINT('Ctrl Pts',(-37.1959492565623,0.250921168216482,
-19.9083037268163));
#31365=CARTESIAN_POINT('Ctrl Pts',(-37.3417692430452,0.391973810946715,
-20.953189482416));
#31366=CARTESIAN_POINT('Ctrl Pts',(-37.5201245015063,0.618043471751103,
-22.2608038425323));
#31367=CARTESIAN_POINT('Ctrl Pts',(-37.6147314284528,0.841427703283629,
-23.309409082731));
#31368=CARTESIAN_POINT('Ctrl Pts',(-37.6482532597087,0.988116899634828,
-23.9659064207315));
#31369=CARTESIAN_POINT('Ctrl Pts',(-37.6592078803129,1.05206229864543,-24.2450313789672));
#31370=CARTESIAN_POINT('Ctrl Pts',(-37.6763853789569,1.18703243134129,-24.7843844548707));
#31371=CARTESIAN_POINT('Ctrl Pts',(-37.6941213656748,1.44305036514919,-25.7168694041114));
#31372=CARTESIAN_POINT('Ctrl Pts',(-37.6942808345933,1.83715730036241,-26.9990587814339));
#31373=CARTESIAN_POINT('Ctrl Pts',(-37.6819068176747,2.28970554590047,-28.4722406036395));
#31374=CARTESIAN_POINT('Ctrl Pts',(-37.6788534272093,2.54049055463771,-29.4066814895956));
#31375=CARTESIAN_POINT('Ctrl Pts',(-37.6805320778864,2.65829402513679,-29.9180192372393));
#31376=CARTESIAN_POINT('Ctrl Pts',(-37.6798971142878,2.68560134538136,-30.040367654817));
#31377=CARTESIAN_POINT('Ctrl Pts',(-37.6787749519767,2.73822820054902,-30.2806011843286));
#31378=CARTESIAN_POINT('Ctrl Pts',(-37.6756535886323,2.82773000309687,-30.704499948019));
#31379=CARTESIAN_POINT('Ctrl Pts',(-37.6665461775974,2.99523119806346,-31.554291765181));
#31380=CARTESIAN_POINT('Ctrl Pts',(-37.6512941902261,3.1648836902586,-32.5343411196971));
#31381=CARTESIAN_POINT('Ctrl Pts',(-37.6352765540523,3.3201650196893,-33.5196880727089));
#31382=CARTESIAN_POINT('Ctrl Pts',(-37.6236857795041,3.43146974877078,-34.261318219947));
#31383=CARTESIAN_POINT('Ctrl Pts',(-37.6133520513342,3.53951935406892,-35.0050084877505));
#31384=CARTESIAN_POINT('Ctrl Pts',(-37.6078242854473,3.61074952100345,-35.5020159286179));
#31385=CARTESIAN_POINT('Ctrl Pts',(-37.6043859413745,3.66452465859539,-35.8759848351879));
#31386=CARTESIAN_POINT('Ctrl Pts',(-37.6026077149196,3.69976408043587,-36.1223505688103));
#31387=CARTESIAN_POINT('Ctrl Pts',(-37.599521736483,3.76888157611279,-36.61706583695));
#31388=CARTESIAN_POINT('Ctrl Pts',(-37.5956363167035,3.88540317672125,-37.4809407775669));
#31389=CARTESIAN_POINT('Ctrl Pts',(-37.5910272717758,4.10181112895166,-39.2087099360799));
#31390=CARTESIAN_POINT('Ctrl Pts',(-37.5842203316147,4.2577499695969,-40.6943345599309));
#31391=CARTESIAN_POINT('Ctrl Pts',(-37.5695004329624,4.36034742096726,-41.8160021984482));
#31392=CARTESIAN_POINT('Ctrl Pts',(-37.5665328375025,4.38195344965808,-42.0583510628435));
#31393=CARTESIAN_POINT('Ctrl Pts',(-37.5619914612557,4.41277915320487,-42.426101932401));
#31394=CARTESIAN_POINT('Ctrl Pts',(-37.5574198149966,4.44190858472651,-42.7942788920664));
#31395=CARTESIAN_POINT('Ctrl Pts',(-37.5510699275548,4.47881121386559,-43.2875510134486));
#31396=CARTESIAN_POINT('Ctrl Pts',(-37.5424456046618,4.5216064260077,-43.9072300669672));
#31397=CARTESIAN_POINT('Ctrl Pts',(-37.5300912088607,4.56887774110081,-44.6558662586516));
#31398=CARTESIAN_POINT('Ctrl Pts',(-37.51734300484,4.60589289567608,-45.2834091457517));
#31399=CARTESIAN_POINT('Ctrl Pts',(-37.5051522081724,4.63477136604078,-45.7875099169756));
#31400=CARTESIAN_POINT('Ctrl Pts',(-37.4948762495891,4.65621548144282,-46.1665760379686));
#31401=CARTESIAN_POINT('Ctrl Pts',(-37.4833238302732,4.6776217492016,-46.5465778715606));
#31402=CARTESIAN_POINT('Ctrl Pts',(-37.4660098448967,4.70636683890851,-47.0545196654333));
#31403=CARTESIAN_POINT('Ctrl Pts',(-37.450643270566,4.72841232401127,-47.4366878571963));
#31404=CARTESIAN_POINT('Ctrl Pts',(-37.4332726036606,4.75130339337673,-47.8210731631867));
#31405=CARTESIAN_POINT('Ctrl Pts',(-37.4202177511839,4.7687530603907,-48.0908393827046));
#31406=CARTESIAN_POINT('Ctrl Pts',(-37.3907011252467,4.80681531263838,-48.6174288437083));
#31407=CARTESIAN_POINT('Ctrl Pts',(-37.330364145368,4.88087940265647,-49.5287521262629));
#31408=CARTESIAN_POINT('Ctrl Pts',(-37.2253304066405,4.99306825383668,-50.7857376411557));
#31409=CARTESIAN_POINT('Ctrl Pts',(-37.0880949687414,5.09629346708032,-52.2184190483748));
#31410=CARTESIAN_POINT('Ctrl Pts',(-37.0044748217046,5.11858167612536,-53.1159739539212));
#31411=CARTESIAN_POINT('Ctrl Pts',(-36.9601697039679,5.11062258468734,-53.6591378281997));
#31412=CARTESIAN_POINT('Ctrl Pts',(-36.9420090151494,5.10243329745112,-53.8510380841647));
#31413=CARTESIAN_POINT('Ctrl Pts',(-36.9054489373111,5.07227248968504,-54.268045146635));
#31414=CARTESIAN_POINT('Ctrl Pts',(-36.8424140357631,4.98413489528138,-55.0311205144958));
#31415=CARTESIAN_POINT('Ctrl Pts',(-36.7331692162939,4.7101346920984,-56.7253922598548));
#31416=CARTESIAN_POINT('Ctrl Pts',(-36.6715454224966,4.46365934886385,-58.4421024895548));
#31417=CARTESIAN_POINT('Ctrl Pts',(-36.6475119464927,4.55546795666475,-59.7851949896994));
#31418=CARTESIAN_POINT('Ctrl Pts',(-36.6449059782589,4.56606514697575,-59.9247754976334));
#31419=CARTESIAN_POINT('Ctrl Pts',(-36.6407132493246,4.59161748760519,-60.2162198707081));
#31420=CARTESIAN_POINT('Ctrl Pts',(-36.6359637670275,4.64494516710093,-60.7173390880193));
#31421=CARTESIAN_POINT('Ctrl Pts',(-36.6356179299687,4.78614159531689,-61.7151817385737));
#31422=CARTESIAN_POINT('Ctrl Pts',(-36.6505932905658,5.01770949926151,-62.8302806803964));
#31423=CARTESIAN_POINT('Ctrl Pts',(-36.6702551267837,5.30484735480991,-63.9217143924267));
#31424=CARTESIAN_POINT('Ctrl Pts',(-36.6811882701522,5.48443590993431,-64.5254920127128));
#31425=CARTESIAN_POINT('Ctrl Pts',(-36.6876545273568,5.61053871830678,-64.9237987567574));
#31426=CARTESIAN_POINT('Ctrl Pts',(-36.6917013086277,5.69622530650803,-65.1881525877755));
#31427=CARTESIAN_POINT('Ctrl Pts',(-36.6952656678883,5.78426189393477,-65.4508510728054));
#31428=CARTESIAN_POINT('Ctrl Pts',(-36.6978474820544,5.86310702128428,-65.6791061932655));
#31429=CARTESIAN_POINT('Ctrl Pts',(-36.6991500771139,5.90865362346796,-65.8090850134188));
#31430=CARTESIAN_POINT('Ctrl Pts',(-36.7009227045981,5.97746142112317,-66.0036242828082));
#31431=CARTESIAN_POINT('Ctrl Pts',(-36.7019998161728,6.03575793707553,-66.1647643785117));
#31432=CARTESIAN_POINT('Ctrl Pts',(-36.7031586109764,6.13363851366078,-66.430917607253));
#31433=CARTESIAN_POINT('Ctrl Pts',(-36.7038836856841,6.2510371660943,-66.7354556850828));
#31434=CARTESIAN_POINT('Ctrl Pts',(-36.7050109434939,6.49353163277098,-67.3132344553444));
#31435=CARTESIAN_POINT('Ctrl Pts',(-36.7057406882881,6.953561818789,-68.3024919286853));
#31436=CARTESIAN_POINT('Ctrl Pts',(-36.704221792431,7.95641216887806,-70.1615298613546));
#31437=CARTESIAN_POINT('Ctrl Pts',(-36.7020473445366,8.83230535659937,-71.6214506940054));
#31438=CARTESIAN_POINT('Ctrl Pts',(-36.7036840316439,9.38520851996215,-72.6730413981383));
#31439=CARTESIAN_POINT('Ctrl Pts',(-36.7036514060824,9.52095780102533,-72.9307926088001));
#31440=CARTESIAN_POINT('Ctrl Pts',(-36.7037729430077,9.78577010106223,-73.4323636649782));
#31441=CARTESIAN_POINT('Ctrl Pts',(-36.7037702968015,10.1203926230654,-74.0641471677288));
#31442=CARTESIAN_POINT('Ctrl Pts',(-36.7037495101504,10.5210994519818,-74.8180587766035));
#31443=CARTESIAN_POINT('Ctrl Pts',(-36.7035868948437,11.3242891788236,-76.3256640873389));
#31444=CARTESIAN_POINT('Ctrl Pts',(-36.7033606006525,11.9937021323769,-77.5781837508716));
#31445=CARTESIAN_POINT('Ctrl Pts',(-36.7034150745067,12.9615748789859,-79.3986762846247));
#31446=CARTESIAN_POINT('Ctrl Pts',(-36.7033839066019,13.3989424741646,-80.2213448491822));
#31447=CARTESIAN_POINT('Ctrl Pts',(-36.703383906602,13.835464061554,-81.0423225512805));
#31448=CARTESIAN_POINT('Ctrl Pts',(-34.1764447559102,0.0259685887429924,
24.8306203013275));
#31449=CARTESIAN_POINT('Ctrl Pts',(-34.1765480191343,0.0259706743427907,
24.781740533954));
#31450=CARTESIAN_POINT('Ctrl Pts',(-34.1766563187642,0.0259728602730872,
24.7328618093536));
#31451=CARTESIAN_POINT('Ctrl Pts',(-34.177935244816,0.0259987139595002,
24.1822484567547));
#31452=CARTESIAN_POINT('Ctrl Pts',(-34.1789192015653,0.0260245301400927,
23.1781109563667));
#31453=CARTESIAN_POINT('Ctrl Pts',(-34.1812111794164,0.0260877526726797,
21.1695007383349));
#31454=CARTESIAN_POINT('Ctrl Pts',(-34.1897227180841,0.0262600038941574,
19.6653375775111));
#31455=CARTESIAN_POINT('Ctrl Pts',(-34.2077555773017,0.0265955167688952,
18.4142816557505));
#31456=CARTESIAN_POINT('Ctrl Pts',(-34.2164043864526,0.026759174673617,
17.9114377995702));
#31457=CARTESIAN_POINT('Ctrl Pts',(-34.2381226623577,0.0271751853534956,
16.9074310683423));
#31458=CARTESIAN_POINT('Ctrl Pts',(-34.2847040215993,0.0280665516383967,
15.1536348084952));
#31459=CARTESIAN_POINT('Ctrl Pts',(-34.3289440787915,0.0288744170692373,
13.6519879457826));
#31460=CARTESIAN_POINT('Ctrl Pts',(-34.3566565846591,0.0293063872750294,
12.3976215172641));
#31461=CARTESIAN_POINT('Ctrl Pts',(-34.367982385136,0.0294745804022541,
11.8967125448909));
#31462=CARTESIAN_POINT('Ctrl Pts',(-34.3910627681017,0.0297910247937516,
10.8949354521761));
#31463=CARTESIAN_POINT('Ctrl Pts',(-34.4309925890151,0.0302831881620811,
9.14146337731071));
#31464=CARTESIAN_POINT('Ctrl Pts',(-34.4590006955027,0.0305702214085873,
7.63620452746495));
#31465=CARTESIAN_POINT('Ctrl Pts',(-34.4714526930686,0.0306863666185977,
6.50520016575504));
#31466=CARTESIAN_POINT('Ctrl Pts',(-34.4740409189562,0.0307019421184336,
6.25507309871996));
#31467=CARTESIAN_POINT('Ctrl Pts',(-34.4785821354951,0.030699029376128,
5.75405743334002));
#31468=CARTESIAN_POINT('Ctrl Pts',(-34.484920601066,0.03062048531772,4.87578204819422));
#31469=CARTESIAN_POINT('Ctrl Pts',(-34.4916138238924,0.0302903478700228,
3.11542709937152));
#31470=CARTESIAN_POINT('Ctrl Pts',(-34.4886869377477,0.0301425423443907,
1.60816029882331));
#31471=CARTESIAN_POINT('Ctrl Pts',(-34.4839896140949,0.0304955552585745,
0.548003023478769));
#31472=CARTESIAN_POINT('Ctrl Pts',(-34.4833725318882,0.0305416251743624,
0.421705744044932));
#31473=CARTESIAN_POINT('Ctrl Pts',(-34.4819234181444,0.0306499058822111,
0.169346943515288));
#31474=CARTESIAN_POINT('Ctrl Pts',(-34.4788505524739,0.0308785738956989,
-0.271757550688972));
#31475=CARTESIAN_POINT('Ctrl Pts',(-34.4730977900133,0.0313026784127056,
-0.900513330898582));
#31476=CARTESIAN_POINT('Ctrl Pts',(-34.4645288667361,0.0319138001759487,
-1.6532738974642));
#31477=CARTESIAN_POINT('Ctrl Pts',(-34.4516077232543,0.0328022853878508,
-2.65522365151925));
#31478=CARTESIAN_POINT('Ctrl Pts',(-34.4339496901778,0.0339207349723135,
-3.90560610978848));
#31479=CARTESIAN_POINT('Ctrl Pts',(-34.4210607531741,0.0345605068751547,
-4.9061316839446));
#31480=CARTESIAN_POINT('Ctrl Pts',(-34.4142586034067,0.0347905599414902,
-5.53243263620395));
#31481=CARTESIAN_POINT('Ctrl Pts',(-34.411552250874,0.0349353447619312,
-5.78405959293063));
#31482=CARTESIAN_POINT('Ctrl Pts',(-34.4062021269632,0.0353907288013687,
-6.28681327556158));
#31483=CARTESIAN_POINT('Ctrl Pts',(-34.3969869916172,0.0365103197768133,
-7.16686416697398));
#31484=CARTESIAN_POINT('Ctrl Pts',(-34.3841583516796,0.0383883562234742,
-8.42268589789923));
#31485=CARTESIAN_POINT('Ctrl Pts',(-34.3715179979297,0.0388972389018156,
-9.67421926002958));
#31486=CARTESIAN_POINT('Ctrl Pts',(-34.3626323059108,0.0376172677793105,
-10.5464996684573));
#31487=CARTESIAN_POINT('Ctrl Pts',(-34.3575249176696,0.0362881792757959,
-11.0436539495391));
#31488=CARTESIAN_POINT('Ctrl Pts',(-34.3549594447717,0.0354026940840104,
-11.2917817789517));
#31489=CARTESIAN_POINT('Ctrl Pts',(-34.353020902462,0.0346440961100884,
-11.4784125652706));
#31490=CARTESIAN_POINT('Ctrl Pts',(-34.3515853254475,0.0340253440693036,
-11.6018310614995));
#31491=CARTESIAN_POINT('Ctrl Pts',(-34.3482348486648,0.0323903181822838,
-11.8498926617208));
#31492=CARTESIAN_POINT('Ctrl Pts',(-34.3412463574436,0.0285811707377088,
-12.2836696573919));
#31493=CARTESIAN_POINT('Ctrl Pts',(-34.3188269874935,0.0148037986272326,
-13.4013716450607));
#31494=CARTESIAN_POINT('Ctrl Pts',(-34.2887178607569,-0.00644829959073418,
-14.6519870417332));
#31495=CARTESIAN_POINT('Ctrl Pts',(-34.2770936766063,-0.0173469197916623,
-15.9208591392115));
#31496=CARTESIAN_POINT('Ctrl Pts',(-34.2778715282682,-0.0189151721828352,
-16.5603275873268));
#31497=CARTESIAN_POINT('Ctrl Pts',(-34.2835910948713,-0.0170361134882322,
-17.0753241807094));
#31498=CARTESIAN_POINT('Ctrl Pts',(-34.2883451506099,-0.0149121363734472,
-17.3340551145771));
#31499=CARTESIAN_POINT('Ctrl Pts',(-34.2926726541808,-0.0128327334582615,
-17.527607743022));
#31500=CARTESIAN_POINT('Ctrl Pts',(-34.2957083466975,-0.0114556391860327,
-17.6501483562369));
#31501=CARTESIAN_POINT('Ctrl Pts',(-34.3024626660491,-0.00884695070967751,
-17.8989735893196));
#31502=CARTESIAN_POINT('Ctrl Pts',(-34.3102090859748,-0.00635436130592169,
-18.1473631261843));
#31503=CARTESIAN_POINT('Ctrl Pts',(-34.3188794786108,-0.00390516257062937,
-18.397159467746));
#31504=CARTESIAN_POINT('Ctrl Pts',(-34.3246725770309,-0.00236337394245413,
-18.553466654483));
#31505=CARTESIAN_POINT('Ctrl Pts',(-34.3295238385326,-0.00111268941660546,
-18.67876279445));
#31506=CARTESIAN_POINT('Ctrl Pts',(-34.3345179440761,0.000154153990505383,
-18.8041757961903));
#31507=CARTESIAN_POINT('Ctrl Pts',(-34.3488294337639,0.00374222852032763,
-19.1496292775457));
#31508=CARTESIAN_POINT('Ctrl Pts',(-34.3753237352747,0.010295460514461,
-19.7179520756166));
#31509=CARTESIAN_POINT('Ctrl Pts',(-34.4302004564404,0.0269303197528827,
-20.737473605222));
#31510=CARTESIAN_POINT('Ctrl Pts',(-34.5123332226738,0.0632200852246043,
-22.03016336335));
#31511=CARTESIAN_POINT('Ctrl Pts',(-34.588378884647,0.12643758942332,-23.0852752905503));
#31512=CARTESIAN_POINT('Ctrl Pts',(-34.6367374718653,0.18257139651334,-23.7495053415597));
#31513=CARTESIAN_POINT('Ctrl Pts',(-34.6568882840014,0.206942034622488,
-24.0174275813682));
#31514=CARTESIAN_POINT('Ctrl Pts',(-34.7002228691302,0.263440964308869,
-24.5469866326856));
#31515=CARTESIAN_POINT('Ctrl Pts',(-34.7824956712819,0.380990003104775,
-25.4672846369282));
#31516=CARTESIAN_POINT('Ctrl Pts',(-34.9084923498233,0.591534619965779,
-26.7554490787649));
#31517=CARTESIAN_POINT('Ctrl Pts',(-35.045972665964,0.87096394672074,-28.2560450148336));
#31518=CARTESIAN_POINT('Ctrl Pts',(-35.1159825518541,1.04214946371602,-29.2248771910313));
#31519=CARTESIAN_POINT('Ctrl Pts',(-35.147426229867,1.12467880819707,-29.7614661868142));
#31520=CARTESIAN_POINT('Ctrl Pts',(-35.1541715034908,1.14325309257035,-29.885785553879));
#31521=CARTESIAN_POINT('Ctrl Pts',(-35.1671738936228,1.1797785822778,-30.1318470076868));
#31522=CARTESIAN_POINT('Ctrl Pts',(-35.1885183811244,1.24269729319185,-30.5645356763689));
#31523=CARTESIAN_POINT('Ctrl Pts',(-35.2261496790866,1.36441854460525,-31.4312425399043));
#31524=CARTESIAN_POINT('Ctrl Pts',(-35.259457736917,1.49582490437396,-32.427062269871));
#31525=CARTESIAN_POINT('Ctrl Pts',(-35.2865720248284,1.623146359731,-33.4256684888729));
#31526=CARTESIAN_POINT('Ctrl Pts',(-35.3045754711524,1.71760899132426,-34.1758807071139));
#31527=CARTESIAN_POINT('Ctrl Pts',(-35.3209683482824,1.81196474024708,-34.9268708239082));
#31528=CARTESIAN_POINT('Ctrl Pts',(-35.3312868839817,1.87550180720795,-35.4278812620332));
#31529=CARTESIAN_POINT('Ctrl Pts',(-35.3389836740974,1.9237881832193,-35.8046197278162));
#31530=CARTESIAN_POINT('Ctrl Pts',(-35.3442435332927,1.95598856799882,-36.0547424865498));
#31531=CARTESIAN_POINT('Ctrl Pts',(-35.3547061858924,2.02038327537595,-36.5556382205856));
#31532=CARTESIAN_POINT('Ctrl Pts',(-35.3728056791848,2.13248774397748,-37.4302883273256));
#31533=CARTESIAN_POINT('Ctrl Pts',(-35.4062812466005,2.35380345787832,-39.1773607273832));
#31534=CARTESIAN_POINT('Ctrl Pts',(-35.4239022459999,2.53348259946413,-40.6774928642993));
#31535=CARTESIAN_POINT('Ctrl Pts',(-35.4241465093225,2.65916632645815,-41.8091242366946));
#31536=CARTESIAN_POINT('Ctrl Pts',(-35.4247462543187,2.68537536054886,-42.0492494691377));
#31537=CARTESIAN_POINT('Ctrl Pts',(-35.4251349689881,2.72277666504169,-42.4172280256115));
#31538=CARTESIAN_POINT('Ctrl Pts',(-35.4252853138477,2.75824759465529,-42.7860354981063));
#31539=CARTESIAN_POINT('Ctrl Pts',(-35.4248317572573,2.8037332042836,-43.2822379294712));
#31540=CARTESIAN_POINT('Ctrl Pts',(-35.4228770896236,2.85811465763686,-43.9084301033932));
#31541=CARTESIAN_POINT('Ctrl Pts',(-35.417311058886,2.92290442773719,-44.6698102121672));
#31542=CARTESIAN_POINT('Ctrl Pts',(-35.4091513232251,2.97943063806857,-45.311954153181));
#31543=CARTESIAN_POINT('Ctrl Pts',(-35.3999100222585,3.02803855823651,-45.830164972453));
#31544=CARTESIAN_POINT('Ctrl Pts',(-35.3914714749811,3.0666435275713,-46.2210682704118));
#31545=CARTESIAN_POINT('Ctrl Pts',(-35.3813564535755,3.10787646492832,-46.6141898897007));
#31546=CARTESIAN_POINT('Ctrl Pts',(-35.3653687619548,3.1670258645019,-47.1413517987742));
#31547=CARTESIAN_POINT('Ctrl Pts',(-35.3503107206238,3.21680331408655,-47.5400216957549));
#31548=CARTESIAN_POINT('Ctrl Pts',(-35.3326246137773,3.27145538187517,-47.9423865315486));
#31549=CARTESIAN_POINT('Ctrl Pts',(-35.3183119345572,3.31249728321088,-48.2260516348631));
#31550=CARTESIAN_POINT('Ctrl Pts',(-35.2865988651605,3.40282719589082,-48.7769682789169));
#31551=CARTESIAN_POINT('Ctrl Pts',(-35.2221127750781,3.58077321947741,-49.7262778060027));
#31552=CARTESIAN_POINT('Ctrl Pts',(-35.1137593741292,3.86342779255355,-51.0239732801702));
#31553=CARTESIAN_POINT('Ctrl Pts',(-34.9762521475711,4.16691945495112,-52.4854944337859));
#31554=CARTESIAN_POINT('Ctrl Pts',(-34.8885472983672,4.29756020423801,-53.3819511812763));
#31555=CARTESIAN_POINT('Ctrl Pts',(-34.8370493297166,4.34621727555356,-53.9147329162006));
#31556=CARTESIAN_POINT('Ctrl Pts',(-34.8157958118834,4.36068859569375,-54.1265981568054));
#31557=CARTESIAN_POINT('Ctrl Pts',(-34.768631396821,4.37775308482033,-54.5626870837952));
#31558=CARTESIAN_POINT('Ctrl Pts',(-34.6769728514841,4.3790834998756,-55.3502991729764));
#31559=CARTESIAN_POINT('Ctrl Pts',(-34.4703881875133,4.31550812532453,-57.0345848267836));
#31560=CARTESIAN_POINT('Ctrl Pts',(-34.3052078475783,4.29868794505819,-58.6813927067186));
#31561=CARTESIAN_POINT('Ctrl Pts',(-34.2389432707123,4.47416039380388,-59.926986696457));
#31562=CARTESIAN_POINT('Ctrl Pts',(-34.231463357557,4.49260480950002,-60.0560807286205));
#31563=CARTESIAN_POINT('Ctrl Pts',(-34.2178691418411,4.53282011579336,-60.3270192009488));
#31564=CARTESIAN_POINT('Ctrl Pts',(-34.1978085732581,4.60623812460767,-60.7953802851783));
#31565=CARTESIAN_POINT('Ctrl Pts',(-34.1709155858825,4.76983222090131,-61.7386111802352));
#31566=CARTESIAN_POINT('Ctrl Pts',(-34.1637778925812,4.99512102374594,-62.8160929526715));
#31567=CARTESIAN_POINT('Ctrl Pts',(-34.167090502353,5.2654214482681,-63.8931464258179));
#31568=CARTESIAN_POINT('Ctrl Pts',(-34.170474004141,5.43561574664774,-64.497241832218));
#31569=CARTESIAN_POINT('Ctrl Pts',(-34.1723711287775,5.55721115726879,-64.8991000042908));
#31570=CARTESIAN_POINT('Ctrl Pts',(-34.1734792843691,5.64047104498202,-65.1667042461347));
#31571=CARTESIAN_POINT('Ctrl Pts',(-34.1742466344374,5.72712066020137,-65.4339225707906));
#31572=CARTESIAN_POINT('Ctrl Pts',(-34.1744645507659,5.80596045959028,-65.6672469462392));
#31573=CARTESIAN_POINT('Ctrl Pts',(-34.174435438371,5.85189259297455,-65.8004333090785));
#31574=CARTESIAN_POINT('Ctrl Pts',(-34.1742272593377,5.92168347597517,-66.0000802553368));
#31575=CARTESIAN_POINT('Ctrl Pts',(-34.173683287128,5.98170708043398,-66.1661304146234));
#31576=CARTESIAN_POINT('Ctrl Pts',(-34.1721771518986,6.08376886778207,-66.440957951523));
#31577=CARTESIAN_POINT('Ctrl Pts',(-34.1707247734496,6.20051035645416,-66.7410825653339));
#31578=CARTESIAN_POINT('Ctrl Pts',(-34.168627217271,6.4438181995821,-67.3180377329392));
#31579=CARTESIAN_POINT('Ctrl Pts',(-34.1666336424948,6.90263474958834,-68.3028697099307));
#31580=CARTESIAN_POINT('Ctrl Pts',(-34.1674540085646,7.90114792029037,-70.1595842761014));
#31581=CARTESIAN_POINT('Ctrl Pts',(-34.1714825205131,8.77266649621883,-71.6191472444224));
#31582=CARTESIAN_POINT('Ctrl Pts',(-34.1722134259569,9.3266065933815,-72.6734520257454));
#31583=CARTESIAN_POINT('Ctrl Pts',(-34.1721742703938,9.46222766969651,-72.9311238226013));
#31584=CARTESIAN_POINT('Ctrl Pts',(-34.1722036357289,9.72703498910348,-73.4329215553792));
#31585=CARTESIAN_POINT('Ctrl Pts',(-34.1721788912052,10.0616140288131,-74.0647536923517));
#31586=CARTESIAN_POINT('Ctrl Pts',(-34.1721637242811,10.4623925547618,-74.8188030680971));
#31587=CARTESIAN_POINT('Ctrl Pts',(-34.1721036934396,11.2657757252011,-76.3265339173854));
#31588=CARTESIAN_POINT('Ctrl Pts',(-34.172046148687,11.9353594497907,-77.5788066455772));
#31589=CARTESIAN_POINT('Ctrl Pts',(-34.1720774576037,12.9030459298434,-79.3988899707441));
#31590=CARTESIAN_POINT('Ctrl Pts',(-34.1720596536215,13.340445430675,-80.2215858878274));
#31591=CARTESIAN_POINT('Ctrl Pts',(-34.1720596536215,13.7769670180645,-81.0425635899257));
#31592=CARTESIAN_POINT('Ctrl Pts',(-31.9633899561928,0.00119778082931517,
24.83063334628));
#31593=CARTESIAN_POINT('Ctrl Pts',(-31.963486415328,0.00119848231513045,
24.7817539900166));
#31594=CARTESIAN_POINT('Ctrl Pts',(-31.963587579573,0.00119921736695464,
24.7328756853541));
#31595=CARTESIAN_POINT('Ctrl Pts',(-31.9647822144503,0.00120792687973987,
24.1822671216868));
#31596=CARTESIAN_POINT('Ctrl Pts',(-31.9657019119787,0.00121427805477512,
23.1781340896351));
#31597=CARTESIAN_POINT('Ctrl Pts',(-31.9678452034461,0.00122829672387729,
21.1695331470275));
#31598=CARTESIAN_POINT('Ctrl Pts',(-31.9757952029295,0.00128662321772465,
19.6653742893852));
#31599=CARTESIAN_POINT('Ctrl Pts',(-31.9926356403998,0.00141196690703649,
18.4143207108312));
#31600=CARTESIAN_POINT('Ctrl Pts',(-32.0007139956558,0.00147248024287243,
17.9115005631452));
#31601=CARTESIAN_POINT('Ctrl Pts',(-32.0210021408705,0.00162548582569014,
16.9075098249226));
#31602=CARTESIAN_POINT('Ctrl Pts',(-32.064517452415,0.00195429177169138,
15.1537076950091));
#31603=CARTESIAN_POINT('Ctrl Pts',(-32.1058279763341,0.00226423029483334,
13.6519809000191));
#31604=CARTESIAN_POINT('Ctrl Pts',(-32.1316771815726,0.00245046653420001,
12.3975155713652));
#31605=CARTESIAN_POINT('Ctrl Pts',(-32.1422393341866,0.00252575916266231,
11.8965655658827));
#31606=CARTESIAN_POINT('Ctrl Pts',(-32.1637543912761,0.00267706382077597,
10.8947278493917));
#31607=CARTESIAN_POINT('Ctrl Pts',(-32.200957346963,0.002933521609905,9.14119507582939));
#31608=CARTESIAN_POINT('Ctrl Pts',(-32.2270184972505,0.0031079433499766,
7.63596847755042));
#31609=CARTESIAN_POINT('Ctrl Pts',(-32.2385906509075,0.00318140759757139,
6.50502566211766));
#31610=CARTESIAN_POINT('Ctrl Pts',(-32.240993356192,0.00319344205154197,
6.25484166364325));
#31611=CARTESIAN_POINT('Ctrl Pts',(-32.2451971504006,0.00320342667236139,
5.75377227711905));
#31612=CARTESIAN_POINT('Ctrl Pts',(-32.251033308732,0.00319090078006513,
4.87542789539196));
#31613=CARTESIAN_POINT('Ctrl Pts',(-32.2570919217592,0.00309167642484667,
3.11514117234228));
#31614=CARTESIAN_POINT('Ctrl Pts',(-32.2542667706258,0.00305980010968048,
1.608240603948));
#31615=CARTESIAN_POINT('Ctrl Pts',(-32.2499919488482,0.00321703737406999,
0.548503699734546));
#31616=CARTESIAN_POINT('Ctrl Pts',(-32.2494317489446,0.00323715527579488,
0.422276103173599));
#31617=CARTESIAN_POINT('Ctrl Pts',(-32.2481177291307,0.00328435765801334,
0.170036446586959));
#31618=CARTESIAN_POINT('Ctrl Pts',(-32.2453355398337,0.00338329837949874,
-0.270874468574266));
#31619=CARTESIAN_POINT('Ctrl Pts',(-32.2401289344388,0.00356642375268749,
-0.899419623093153));
#31620=CARTESIAN_POINT('Ctrl Pts',(-32.2323778555354,0.00382560313618471,
-1.65202044069393));
#31621=CARTESIAN_POINT('Ctrl Pts',(-32.2206654026539,0.00420060825483769,
-2.65388902201657));
#31622=CARTESIAN_POINT('Ctrl Pts',(-32.2046156275384,0.00466044519571738,
-3.90438805638575));
#31623=CARTESIAN_POINT('Ctrl Pts',(-32.1927725437737,0.00491225358191858,
-4.9052688291125));
#31624=CARTESIAN_POINT('Ctrl Pts',(-32.1864653645559,0.00499290243202669,
-5.53181917851233));
#31625=CARTESIAN_POINT('Ctrl Pts',(-32.1839612151424,0.00502739650865295,
-5.78278124881988));
#31626=CARTESIAN_POINT('Ctrl Pts',(-32.1790195663831,0.00510449628433056,
-6.28488274216901));
#31627=CARTESIAN_POINT('Ctrl Pts',(-32.1705210287039,0.00524909157024554,
-7.16411633179275));
#31628=CARTESIAN_POINT('Ctrl Pts',(-32.1586291276295,0.00542161434796207,
-8.4205372245363));
#31629=CARTESIAN_POINT('Ctrl Pts',(-32.146652015432,0.00537912234140981,
-9.6747258081599));
#31630=CARTESIAN_POINT('Ctrl Pts',(-32.1379970004511,0.00514992564405705,
-10.5500118621068));
#31631=CARTESIAN_POINT('Ctrl Pts',(-32.1329426296684,0.00495142736476526,
-11.0492147722401));
#31632=CARTESIAN_POINT('Ctrl Pts',(-32.1303718438646,0.00482809344718019,
-11.2984600882129));
#31633=CARTESIAN_POINT('Ctrl Pts',(-32.1284184632243,0.00472552966013362,
-11.4860294914805));
#31634=CARTESIAN_POINT('Ctrl Pts',(-32.1270425359593,0.00465137659907829,
-11.6119657079845));
#31635=CARTESIAN_POINT('Ctrl Pts',(-32.1240617896758,0.00447600785169626,
-11.8636240728352));
#31636=CARTESIAN_POINT('Ctrl Pts',(-32.1182999721354,0.00410789350910049,
-12.3033615968514));
#31637=CARTESIAN_POINT('Ctrl Pts',(-32.1012865417164,0.00290356550380467,
-13.4313439833862));
#31638=CARTESIAN_POINT('Ctrl Pts',(-32.0794453681356,0.00111694721556185,
-14.6793098499892));
#31639=CARTESIAN_POINT('Ctrl Pts',(-32.0657768239458,-0.000412029585329937,
-15.9311210824324));
#31640=CARTESIAN_POINT('Ctrl Pts',(-32.0618775272173,-0.00105043126173075,
-16.5587290362317));
#31641=CARTESIAN_POINT('Ctrl Pts',(-32.0611309886276,-0.00145536140317013,
-17.0623192438171));
#31642=CARTESIAN_POINT('Ctrl Pts',(-32.0616249769825,-0.00161050528413247,
-17.3146953342562));
#31643=CARTESIAN_POINT('Ctrl Pts',(-32.0623618610294,-0.00170653275002977,
-17.5034091618793));
#31644=CARTESIAN_POINT('Ctrl Pts',(-32.0628530949887,-0.00183129271206578,
-17.62715680891));
#31645=CARTESIAN_POINT('Ctrl Pts',(-32.0638781191395,-0.00217493216688328,
-17.8755151481028));
#31646=CARTESIAN_POINT('Ctrl Pts',(-32.0649763454848,-0.00266617360748607,
-18.1239882231087));
#31647=CARTESIAN_POINT('Ctrl Pts',(-32.0662428621126,-0.00324346823411917,
-18.3729472805465));
#31648=CARTESIAN_POINT('Ctrl Pts',(-32.0671071195084,-0.00363231595324318,
-18.5286660178601));
#31649=CARTESIAN_POINT('Ctrl Pts',(-32.0678541578989,-0.00395311658654445,
-18.6533413353119));
#31650=CARTESIAN_POINT('Ctrl Pts',(-32.0686393791069,-0.00427792217060808,
-18.7780730762426));
#31651=CARTESIAN_POINT('Ctrl Pts',(-32.0709513003664,-0.00519258990406764,
-19.1213246305473));
#31652=CARTESIAN_POINT('Ctrl Pts',(-32.0757287337685,-0.00665094281689207,
-19.6843236758518));
#31653=CARTESIAN_POINT('Ctrl Pts',(-32.0881606714366,-0.00840130287364682,
-20.6888453830507));
#31654=CARTESIAN_POINT('Ctrl Pts',(-32.1129225851262,-0.00756561865649902,
-21.9510487186381));
#31655=CARTESIAN_POINT('Ctrl Pts',(-32.1474366561549,-0.00189334990781983,
-22.9680105823071));
#31656=CARTESIAN_POINT('Ctrl Pts',(-32.1757176507403,0.00431896066786876,
-23.6045341315906));
#31657=CARTESIAN_POINT('Ctrl Pts',(-32.1879292627242,0.0068719456290228,
-23.8544532539764));
#31658=CARTESIAN_POINT('Ctrl Pts',(-32.2162312123548,0.0126773366715741,
-24.3563730776259));
#31659=CARTESIAN_POINT('Ctrl Pts',(-32.2748706455199,0.024969194001814,
-25.2364165939835));
#31660=CARTESIAN_POINT('Ctrl Pts',(-32.3786778435036,0.0513919839388159,
-26.4994086242991));
#31661=CARTESIAN_POINT('Ctrl Pts',(-32.5122749838379,0.101647104051024,
-28.0190052683457));
#31662=CARTESIAN_POINT('Ctrl Pts',(-32.5898304514288,0.144960956006053,
-29.0308522953232));
#31663=CARTESIAN_POINT('Ctrl Pts',(-32.6257479842602,0.169979253770006,
-29.5987031989526));
#31664=CARTESIAN_POINT('Ctrl Pts',(-32.6336861496392,0.175447346686321,
-29.7240888929289));
#31665=CARTESIAN_POINT('Ctrl Pts',(-32.6492514964225,0.186521785199724,
-29.9755083146498));
#31666=CARTESIAN_POINT('Ctrl Pts',(-32.6757338386092,0.206108161838533,
-30.4156921895497));
#31667=CARTESIAN_POINT('Ctrl Pts',(-32.7258571497013,0.246439084399044,
-31.2978925893485));
#31668=CARTESIAN_POINT('Ctrl Pts',(-32.7774103551025,0.296091287968215,
-32.3090426401619));
#31669=CARTESIAN_POINT('Ctrl Pts',(-32.8249726523566,0.351419932056421,
-33.3220680979162));
#31670=CARTESIAN_POINT('Ctrl Pts',(-32.8590641990171,0.396329061978688,
-34.0824306694152));
#31671=CARTESIAN_POINT('Ctrl Pts',(-32.8918831270656,0.445269987187108,
-34.8429797692874));
#31672=CARTESIAN_POINT('Ctrl Pts',(-32.9132036462384,0.480991058541578,
-35.34996569469));
#31673=CARTESIAN_POINT('Ctrl Pts',(-32.9291295102912,0.509166421897822,
-35.7311084598365));
#31674=CARTESIAN_POINT('Ctrl Pts',(-32.9398787407322,0.528403120565872,
-35.9852790675309));
#31675=CARTESIAN_POINT('Ctrl Pts',(-32.9614622283884,0.568373208158851,
-36.4933031905527));
#31676=CARTESIAN_POINT('Ctrl Pts',(-32.9991180244276,0.641977900674228,
-37.3798806011782));
#31677=CARTESIAN_POINT('Ctrl Pts',(-33.0712435325354,0.801360507046883,
-39.1472531161535));
#31678=CARTESIAN_POINT('Ctrl Pts',(-33.1186067375816,0.952013620523383,
-40.6594854156347));
#31679=CARTESIAN_POINT('Ctrl Pts',(-33.1377759168148,1.06467111808059,-41.797880604425));
#31680=CARTESIAN_POINT('Ctrl Pts',(-33.1424761583679,1.08750542024222,-42.0352953990767));
#31681=CARTESIAN_POINT('Ctrl Pts',(-33.1487725066544,1.12002822361257,-42.4026020567513));
#31682=CARTESIAN_POINT('Ctrl Pts',(-33.1546134098907,1.15073236623629,-42.7711097762434));
#31683=CARTESIAN_POINT('Ctrl Pts',(-33.1614844769426,1.19044675002746,-43.2688659578312));
#31684=CARTESIAN_POINT('Ctrl Pts',(-33.168217111019,1.23915922377811,-43.8996126182923));
#31685=CARTESIAN_POINT('Ctrl Pts',(-33.1724047691856,1.30155995660813,-44.6708248666733));
#31686=CARTESIAN_POINT('Ctrl Pts',(-33.171848709337,1.36144920188157,-45.3244573998258));
#31687=CARTESIAN_POINT('Ctrl Pts',(-33.1683254913266,1.41695997132591,-45.8536664211606));
#31688=CARTESIAN_POINT('Ctrl Pts',(-33.1640407718665,1.46315617965921,-46.2536671617113));
#31689=CARTESIAN_POINT('Ctrl Pts',(-33.157956831207,1.51466683832569,-46.6566748244397));
#31690=CARTESIAN_POINT('Ctrl Pts',(-33.1471917328883,1.59147860129533,-47.1979163208453));
#31691=CARTESIAN_POINT('Ctrl Pts',(-33.1360240660687,1.65939874991629,-47.6081090714609));
#31692=CARTESIAN_POINT('Ctrl Pts',(-33.1222528318697,1.73608488175619,-48.0222509129967));
#31693=CARTESIAN_POINT('Ctrl Pts',(-33.1110161789402,1.79348070878201,-48.3112911687026));
#31694=CARTESIAN_POINT('Ctrl Pts',(-33.0869896268488,1.92005463882968,-48.8720316258399));
#31695=CARTESIAN_POINT('Ctrl Pts',(-33.0400148518847,2.17032107029229,-49.8333463233307));
#31696=CARTESIAN_POINT('Ctrl Pts',(-32.9672074568071,2.5745685495611,-51.1406511782623));
#31697=CARTESIAN_POINT('Ctrl Pts',(-32.8831126446119,3.04088716857611,-52.6173629512002));
#31698=CARTESIAN_POINT('Ctrl Pts',(-32.8313136420262,3.28144591160892,-53.5347432801643));
#31699=CARTESIAN_POINT('Ctrl Pts',(-32.7982104275538,3.39474521054215,-54.0845057230478));
#31700=CARTESIAN_POINT('Ctrl Pts',(-32.7828042277012,3.43945308197284,-54.3169641369898));
#31701=CARTESIAN_POINT('Ctrl Pts',(-32.7480508776641,3.5183173872759,-54.7827999168957));
#31702=CARTESIAN_POINT('Ctrl Pts',(-32.6763054399274,3.63577804335648,-55.6164158521495));
#31703=CARTESIAN_POINT('Ctrl Pts',(-32.4972734098398,3.8175982572053,-57.3413344054663));
#31704=CARTESIAN_POINT('Ctrl Pts',(-32.3197492131095,4.0060677251506,-58.9245285098112));
#31705=CARTESIAN_POINT('Ctrl Pts',(-32.2367784110144,4.25684399776631,-60.0831956985914));
#31706=CARTESIAN_POINT('Ctrl Pts',(-32.2274934881362,4.28368004661584,-60.2080193295285));
#31707=CARTESIAN_POINT('Ctrl Pts',(-32.2091622758131,4.34003457150938,-60.4673425661025));
#31708=CARTESIAN_POINT('Ctrl Pts',(-32.1788227946222,4.43923363502762,-60.9181944078175));
#31709=CARTESIAN_POINT('Ctrl Pts',(-32.1240781685771,4.64620879476816,-61.8293188184246));
#31710=CARTESIAN_POINT('Ctrl Pts',(-32.0745304065476,4.90556161313208,-62.8804545977846));
#31711=CARTESIAN_POINT('Ctrl Pts',(-32.035229490394,5.20094248181456,-63.9402395323815));
#31712=CARTESIAN_POINT('Ctrl Pts',(-32.0164215840077,5.38318470466738,-64.5381662417493));
#31713=CARTESIAN_POINT('Ctrl Pts',(-32.0050248580873,5.51257267172476,-64.9372802738423));
#31714=CARTESIAN_POINT('Ctrl Pts',(-31.9977169116196,5.60101109084162,-65.2034253818815));
#31715=CARTESIAN_POINT('Ctrl Pts',(-31.990820420896,5.69286410115348,-65.4696998065714));
#31716=CARTESIAN_POINT('Ctrl Pts',(-31.9851064655405,5.7764135570505,-65.7026587699087));
#31717=CARTESIAN_POINT('Ctrl Pts',(-31.9819272561518,5.82509734658462,-65.8357626083149));
#31718=CARTESIAN_POINT('Ctrl Pts',(-31.9772414758308,5.89908237020845,-66.0354027013822));
#31719=CARTESIAN_POINT('Ctrl Pts',(-31.9735043246712,5.96276395488274,-66.2017138853978));
#31720=CARTESIAN_POINT('Ctrl Pts',(-31.967505526974,6.07113175039066,-66.4771126058172));
#31721=CARTESIAN_POINT('Ctrl Pts',(-31.9620408805721,6.1904845906763,-66.7691393250134));
#31722=CARTESIAN_POINT('Ctrl Pts',(-31.9538882168921,6.43821266169139,-67.3366326463683));
#31723=CARTESIAN_POINT('Ctrl Pts',(-31.9459533165198,6.89814538538485,-68.306149005519));
#31724=CARTESIAN_POINT('Ctrl Pts',(-31.9481839501384,7.88472205125732,-70.1482783297304));
#31725=CARTESIAN_POINT('Ctrl Pts',(-31.961892702002,8.74259077718073,-71.6099794297969));
#31726=CARTESIAN_POINT('Ctrl Pts',(-31.9613594031242,9.30272515454331,-72.6751607545568));
#31727=CARTESIAN_POINT('Ctrl Pts',(-31.9611909682197,9.4379959891971,-72.9319898102899));
#31728=CARTESIAN_POINT('Ctrl Pts',(-31.9609722373197,9.70305345665459,-73.4340042881566));
#31729=CARTESIAN_POINT('Ctrl Pts',(-31.9608149848749,10.037473067343,-74.0653454773225));
#31730=CARTESIAN_POINT('Ctrl Pts',(-31.9607946888063,10.4382175724794,-74.8193049140468));
#31731=CARTESIAN_POINT('Ctrl Pts',(-31.960975349681,11.2413208987991,-76.326711544533));
#31732=CARTESIAN_POINT('Ctrl Pts',(-31.9614077113351,11.9106302089475,-77.578887791324));
#31733=CARTESIAN_POINT('Ctrl Pts',(-31.961425949037,12.8784241477409,-79.3991342446787));
#31734=CARTESIAN_POINT('Ctrl Pts',(-31.9614229449857,13.3157470610903,-80.2216653571697));
#31735=CARTESIAN_POINT('Ctrl Pts',(-31.9614229449857,13.7522686484798,-81.0426430592681));
#31736=CARTESIAN_POINT('Ctrl Pts',(-30.071633215331,-0.00597951180148264,
24.830640601082));
#31737=CARTESIAN_POINT('Ctrl Pts',(-30.0717235578503,-0.00597957100751475,
24.7817614745945));
#31738=CARTESIAN_POINT('Ctrl Pts',(-30.071818306792,-0.00597963374140348,
24.7328834062058));
#31739=CARTESIAN_POINT('Ctrl Pts',(-30.0729372132796,-0.00598033382817053,
24.1822774716252));
#31740=CARTESIAN_POINT('Ctrl Pts',(-30.0737952229211,-0.00598426985520875,
23.1781457908663));
#31741=CARTESIAN_POINT('Ctrl Pts',(-30.075791952375,-0.00599635555943293,
21.1695503823648));
#31742=CARTESIAN_POINT('Ctrl Pts',(-30.0832387269141,-0.00600043596979835,
19.6653947528371));
#31743=CARTESIAN_POINT('Ctrl Pts',(-30.0990299640353,-0.00599207384416433,
18.414343595586));
#31744=CARTESIAN_POINT('Ctrl Pts',(-30.1066040175471,-0.00598923956017259,
17.91153802072));
#31745=CARTESIAN_POINT('Ctrl Pts',(-30.1256246862676,-0.00598378310477602,
16.9075565358832));
#31746=CARTESIAN_POINT('Ctrl Pts',(-30.1664223909486,-0.00597099758907751,
15.1537482643775));
#31747=CARTESIAN_POINT('Ctrl Pts',(-30.2051735404777,-0.00593914521947482,
13.6519695231452));
#31748=CARTESIAN_POINT('Ctrl Pts',(-30.2294490691694,-0.00588682107155954,
12.3974438775068));
#31749=CARTESIAN_POINT('Ctrl Pts',(-30.2393714334099,-0.00586177248898783,
11.8964689449408));
#31750=CARTESIAN_POINT('Ctrl Pts',(-30.2595955046103,-0.00579832815387727,
10.8945948339458));
#31751=CARTESIAN_POINT('Ctrl Pts',(-30.2945883665757,-0.00566357321014015,
9.14102577198835));
#31752=CARTESIAN_POINT('Ctrl Pts',(-30.3191303455414,-0.00554193805532452,
7.63581837867654));
#31753=CARTESIAN_POINT('Ctrl Pts',(-30.3300222173341,-0.00548627568986584,
6.50490508050203));
#31754=CARTESIAN_POINT('Ctrl Pts',(-30.3322859039162,-0.00546883603165987,
6.25461090169528));
#31755=CARTESIAN_POINT('Ctrl Pts',(-30.3362571088473,-0.00541696448505553,
5.75342693978769));
#31756=CARTESIAN_POINT('Ctrl Pts',(-30.3417982210222,-0.00529187093641845,
4.87493705883473));
#31757=CARTESIAN_POINT('Ctrl Pts',(-30.3476306312681,-0.00499582274034348,
3.11475253958408));
#31758=CARTESIAN_POINT('Ctrl Pts',(-30.3450141067293,-0.00495422222763471,
1.60853806549901));
#31759=CARTESIAN_POINT('Ctrl Pts',(-30.3408229503568,-0.00531572945932111,
0.54960980273059));
#31760=CARTESIAN_POINT('Ctrl Pts',(-30.3402731096133,-0.00536321355987347,
0.423522389547206));
#31761=CARTESIAN_POINT('Ctrl Pts',(-30.3389860512078,-0.00547324323998226,
0.171520488298055));
#31762=CARTESIAN_POINT('Ctrl Pts',(-30.3362646548094,-0.00570340570257375,
-0.269002060186466));
#31763=CARTESIAN_POINT('Ctrl Pts',(-30.3311870586109,-0.00612312604494034,
-0.897120357819737));
#31764=CARTESIAN_POINT('Ctrl Pts',(-30.323628029892,-0.00673069550680428,
-1.64939756698134));
#31765=CARTESIAN_POINT('Ctrl Pts',(-30.3122283222796,-0.00761099476841721,
-2.6510987622667));
#31766=CARTESIAN_POINT('Ctrl Pts',(-30.2966115981415,-0.00873495975655074,
-3.901868850698));
#31767=CARTESIAN_POINT('Ctrl Pts',(-30.2851276194664,-0.00940831283083989,
-4.90349257029006));
#31768=CARTESIAN_POINT('Ctrl Pts',(-30.2790097090084,-0.00968935407965794,
-5.53063466061613));
#31769=CARTESIAN_POINT('Ctrl Pts',(-30.2765467626583,-0.00981889465309108,
-5.78128773220245));
#31770=CARTESIAN_POINT('Ctrl Pts',(-30.2715829076617,-0.0101295382798206,
-6.28319987592385));
#31771=CARTESIAN_POINT('Ctrl Pts',(-30.2628332180127,-0.0107668890000689,
-7.16221259468513));
#31772=CARTESIAN_POINT('Ctrl Pts',(-30.250371375551,-0.0117035847530645,
-8.4192279934331));
#31773=CARTESIAN_POINT('Ctrl Pts',(-30.238509689104,-0.0120489224396454,
-9.67503048875515));
#31774=CARTESIAN_POINT('Ctrl Pts',(-30.2308111114464,-0.0116521148942716,
-10.5520356855271));
#31775=CARTESIAN_POINT('Ctrl Pts',(-30.2266269145913,-0.0111957267883302,
-11.0523825887198));
#31776=CARTESIAN_POINT('Ctrl Pts',(-30.2246146128345,-0.0108829124011361,
-11.302251951277));
#31777=CARTESIAN_POINT('Ctrl Pts',(-30.2231309221615,-0.0106128757297351,
-11.4903272187712));
#31778=CARTESIAN_POINT('Ctrl Pts',(-30.2221305481449,-0.0104027620643398,
-11.6171410305863));
#31779=CARTESIAN_POINT('Ctrl Pts',(-30.2201215864471,-0.00987262369023837,
-11.8701276993885));
#31780=CARTESIAN_POINT('Ctrl Pts',(-30.2165957861575,-0.00868010383560238,
-12.3120640957198));
#31781=CARTESIAN_POINT('Ctrl Pts',(-30.2075713677146,-0.00448774131343062,
-13.4440946831459));
#31782=CARTESIAN_POINT('Ctrl Pts',(-30.198231970908,0.00214994989502799,
-14.6923215132386));
#31783=CARTESIAN_POINT('Ctrl Pts',(-30.1911141964365,0.00666814874968618,
-15.9396992247391));
#31784=CARTESIAN_POINT('Ctrl Pts',(-30.1882525322469,0.00806802357273801,
-16.5639410441624));
#31785=CARTESIAN_POINT('Ctrl Pts',(-30.1864389162173,0.00844614510224558,
-17.0641007737644));
#31786=CARTESIAN_POINT('Ctrl Pts',(-30.1857067562827,0.00835852581970067,
-17.314498665145));
#31787=CARTESIAN_POINT('Ctrl Pts',(-30.1852277504504,0.00817254577115206,
-17.5017086410094));
#31788=CARTESIAN_POINT('Ctrl Pts',(-30.1848863847523,0.00808121126398812,
-17.6268680840601));
#31789=CARTESIAN_POINT('Ctrl Pts',(-30.1841191343115,0.00792206787407538,
-17.8763295177763));
#31790=CARTESIAN_POINT('Ctrl Pts',(-30.1832483101601,0.00781028158237286,
-18.1260366256064));
#31791=CARTESIAN_POINT('Ctrl Pts',(-30.1823129235598,0.0076824914715805,
-18.3755346530741));
#31792=CARTESIAN_POINT('Ctrl Pts',(-30.1817116725309,0.0075943715824794,
-18.5314870098462));
#31793=CARTESIAN_POINT('Ctrl Pts',(-30.1812257724091,0.00751113785243645,
-18.6562250235203));
#31794=CARTESIAN_POINT('Ctrl Pts',(-30.1807390870507,0.00741801411575103,
-18.7809607744239));
#31795=CARTESIAN_POINT('Ctrl Pts',(-30.1794008187061,0.00713188016881434,
-19.1239465463915));
#31796=CARTESIAN_POINT('Ctrl Pts',(-30.1773269821708,0.00634650351198699,
-19.6850783141798));
#31797=CARTESIAN_POINT('Ctrl Pts',(-30.1749159485127,0.00345073637503823,
-20.6824072644305));
#31798=CARTESIAN_POINT('Ctrl Pts',(-30.1765408003496,-0.00429941117768114,
-21.9292244997599));
#31799=CARTESIAN_POINT('Ctrl Pts',(-30.1863638355369,-0.0164890122786689,
-22.9271492452985));
#31800=CARTESIAN_POINT('Ctrl Pts',(-30.1960969485234,-0.0266514272288744,
-23.5490862532691));
#31801=CARTESIAN_POINT('Ctrl Pts',(-30.2003709868961,-0.0311728989940625,
-23.7916452788537));
#31802=CARTESIAN_POINT('Ctrl Pts',(-30.2102787176068,-0.0421759399504831,
-24.2814720313785));
#31803=CARTESIAN_POINT('Ctrl Pts',(-30.2308081746281,-0.0658145899230264,
-25.1435534007399));
#31804=CARTESIAN_POINT('Ctrl Pts',(-30.2665379126669,-0.10845369408875,
-26.3915697905687));
#31805=CARTESIAN_POINT('Ctrl Pts',(-30.3138158155059,-0.160647057996072,
-27.910620294727));
#31806=CARTESIAN_POINT('Ctrl Pts',(-30.3444695979264,-0.185350408131475,
-28.9361950965051));
#31807=CARTESIAN_POINT('Ctrl Pts',(-30.3603670215602,-0.19305099486998,
-29.5158505234813));
#31808=CARTESIAN_POINT('Ctrl Pts',(-30.3638764419697,-0.19467795492099,
-29.6412874995611));
#31809=CARTESIAN_POINT('Ctrl Pts',(-30.370841372724,-0.197795903543105,
-29.8942199006252));
#31810=CARTESIAN_POINT('Ctrl Pts',(-30.3828772641937,-0.202787979986712,
-30.3362471315004));
#31811=CARTESIAN_POINT('Ctrl Pts',(-30.4065867576155,-0.210771558043477,
-31.2223969914582));
#31812=CARTESIAN_POINT('Ctrl Pts',(-30.4336147741352,-0.214394541709777,
-32.2371582827311));
#31813=CARTESIAN_POINT('Ctrl Pts',(-30.4623143224833,-0.210608117314953,
-33.2535256868337));
#31814=CARTESIAN_POINT('Ctrl Pts',(-30.4850901250171,-0.203586469340701,
-34.0161657514148));
#31815=CARTESIAN_POINT('Ctrl Pts',(-30.509434012464,-0.191909535416984,
-34.7788584001386));
#31816=CARTESIAN_POINT('Ctrl Pts',(-30.527000089848,-0.180699245887847,
-35.2871635656252));
#31817=CARTESIAN_POINT('Ctrl Pts',(-30.5408206753329,-0.170838943841918,
-35.6692991188219));
#31818=CARTESIAN_POINT('Ctrl Pts',(-30.5504135271421,-0.163762007732125,
-35.9248598303208));
#31819=CARTESIAN_POINT('Ctrl Pts',(-30.5707746738688,-0.147753019969481,
-36.4352385447715));
#31820=CARTESIAN_POINT('Ctrl Pts',(-30.6089400303616,-0.115224998830483,
-37.3259440140739));
#31821=CARTESIAN_POINT('Ctrl Pts',(-30.6919117001604,-0.0327245065930569,
-39.1007929179948));
#31822=CARTESIAN_POINT('Ctrl Pts',(-30.7614648092647,0.0618686371559721,
-40.6170327393275));
#31823=CARTESIAN_POINT('Ctrl Pts',(-30.8002466391313,0.139773646463282,
-41.7574484740374));
#31824=CARTESIAN_POINT('Ctrl Pts',(-30.8088584930596,0.155056003248883,
-41.9933086116199));
#31825=CARTESIAN_POINT('Ctrl Pts',(-30.8212074427548,0.176328014535857,
-42.3598877698462));
#31826=CARTESIAN_POINT('Ctrl Pts',(-30.8331286126518,0.195988082731291,
-42.7278573057299));
#31827=CARTESIAN_POINT('Ctrl Pts',(-30.8483932090505,0.221309159407272,
-43.2258448569499));
#31828=CARTESIAN_POINT('Ctrl Pts',(-30.8663204058983,0.252903186846109,
-43.858221607421));
#31829=CARTESIAN_POINT('Ctrl Pts',(-30.8858735298339,0.296914557133909,
-44.6336920117819));
#31830=CARTESIAN_POINT('Ctrl Pts',(-30.900358069208,0.344014155448641,-45.2926442163476));
#31831=CARTESIAN_POINT('Ctrl Pts',(-30.9106122658943,0.391419190964656,
-45.8272055125904));
#31832=CARTESIAN_POINT('Ctrl Pts',(-30.9176059406292,0.432669988209861,
-46.2316555240505));
#31833=CARTESIAN_POINT('Ctrl Pts',(-30.9238322302709,0.480506653593239,
-46.6395184948446));
#31834=CARTESIAN_POINT('Ctrl Pts',(-30.930979550014,0.554279800503014,-47.1876716982823));
#31835=CARTESIAN_POINT('Ctrl Pts',(-30.9350040618108,0.622153380577239,
-47.603401841639));
#31836=CARTESIAN_POINT('Ctrl Pts',(-30.937853668355,0.700470061956545,-48.0229458365958));
#31837=CARTESIAN_POINT('Ctrl Pts',(-30.9398837417028,0.757623241431886,
-48.3078419742728));
#31838=CARTESIAN_POINT('Ctrl Pts',(-30.9447094693403,0.884257780076132,
-48.8663016682787));
#31839=CARTESIAN_POINT('Ctrl Pts',(-30.9540884552519,1.13479418413515,-49.8247060904745));
#31840=CARTESIAN_POINT('Ctrl Pts',(-30.9658562738545,1.54639350434677,-51.1377722660007));
#31841=CARTESIAN_POINT('Ctrl Pts',(-30.9672655462429,2.04700692304314,-52.6362661460573));
#31842=CARTESIAN_POINT('Ctrl Pts',(-30.9542947585683,2.33739849305094,-53.586533226448));
#31843=CARTESIAN_POINT('Ctrl Pts',(-30.9382889729449,2.49141968435564,-54.1662912690709));
#31844=CARTESIAN_POINT('Ctrl Pts',(-30.9291225129865,2.55517267883511,-54.4141505897421));
#31845=CARTESIAN_POINT('Ctrl Pts',(-30.9068388800674,2.67658080355494,-54.9058577640804));
#31846=CARTESIAN_POINT('Ctrl Pts',(-30.8560495734567,2.88053387167694,-55.7782833871445));
#31847=CARTESIAN_POINT('Ctrl Pts',(-30.718141123549,3.26645565618861,-57.5487625857468));
#31848=CARTESIAN_POINT('Ctrl Pts',(-30.5680043924138,3.6255385292795,-59.1042781383112));
#31849=CARTESIAN_POINT('Ctrl Pts',(-30.4891640217922,3.94202721780659,-60.2106447919612));
#31850=CARTESIAN_POINT('Ctrl Pts',(-30.4801173902694,3.97803208143601,-60.3371690260636));
#31851=CARTESIAN_POINT('Ctrl Pts',(-30.461387852414,4.05171834984927,-60.5951852873439));
#31852=CARTESIAN_POINT('Ctrl Pts',(-30.4280986510233,4.18090295995364,-61.0456191802627));
#31853=CARTESIAN_POINT('Ctrl Pts',(-30.3593934569128,4.44492181141008,-61.952351166067));
#31854=CARTESIAN_POINT('Ctrl Pts',(-30.2799851930437,4.76470369438984,-62.9948419468024));
#31855=CARTESIAN_POINT('Ctrl Pts',(-30.2076940068515,5.11416131601914,-64.0402606257236));
#31856=CARTESIAN_POINT('Ctrl Pts',(-30.1712404393034,5.32354239948677,-64.6282546742671));
#31857=CARTESIAN_POINT('Ctrl Pts',(-30.1492726927023,5.46923721772613,-65.0199525053915));
#31858=CARTESIAN_POINT('Ctrl Pts',(-30.1352898838634,5.56802668462955,-65.2809631375061));
#31859=CARTESIAN_POINT('Ctrl Pts',(-30.1223429458612,5.66942002501773,-65.5418067682793));
#31860=CARTESIAN_POINT('Ctrl Pts',(-30.1120234596837,5.76050010640036,-65.7697948671604));
#31861=CARTESIAN_POINT('Ctrl Pts',(-30.1064253922327,5.81324289372803,-65.8999984503125));
#31862=CARTESIAN_POINT('Ctrl Pts',(-30.0983336314726,5.89306380492265,-66.0952289388947));
#31863=CARTESIAN_POINT('Ctrl Pts',(-30.0922333964975,5.9610784662157,-66.2577492366815));
#31864=CARTESIAN_POINT('Ctrl Pts',(-30.0830549482081,6.07581543646423,-66.5266981578281));
#31865=CARTESIAN_POINT('Ctrl Pts',(-30.0746943339823,6.19979525758211,-66.8097215279348));
#31866=CARTESIAN_POINT('Ctrl Pts',(-30.0620885458429,6.45378746289753,-67.3629354741228));
#31867=CARTESIAN_POINT('Ctrl Pts',(-30.0494866581976,6.91657589646975,-68.3117542359668));
#31868=CARTESIAN_POINT('Ctrl Pts',(-30.0519299035184,7.88784277604413,-70.1317633075454));
#31869=CARTESIAN_POINT('Ctrl Pts',(-30.0724797044386,8.7274639830299,-71.5972679336727));
#31870=CARTESIAN_POINT('Ctrl Pts',(-30.0710020759233,9.29689859995957,-72.6777777073672));
#31871=CARTESIAN_POINT('Ctrl Pts',(-30.0707113821031,9.43171519037961,-72.9332896071135));
#31872=CARTESIAN_POINT('Ctrl Pts',(-30.070282603693,9.69719653373554,-73.4354404713998));
#31873=CARTESIAN_POINT('Ctrl Pts',(-30.0699952412353,10.0314082669893,-74.0659143981115));
#31874=CARTESIAN_POINT('Ctrl Pts',(-30.0699631027953,10.4320333495277,-74.8195879198025));
#31875=CARTESIAN_POINT('Ctrl Pts',(-30.0703311662541,11.2344964301764,-76.32633032144));
#31876=CARTESIAN_POINT('Ctrl Pts',(-30.0711438759096,11.9032275320862,-77.5785599567108));
#31877=CARTESIAN_POINT('Ctrl Pts',(-30.0711381425972,12.8714052347748,-79.3994559074687));
#31878=CARTESIAN_POINT('Ctrl Pts',(-30.0711343370146,13.3085843007755,-80.2216793738818));
#31879=CARTESIAN_POINT('Ctrl Pts',(-30.0711343370145,13.745105888165,-81.0426570759801));
#31880=CARTESIAN_POINT('Ctrl Pts',(-28.1863005461827,-0.00460604167494977,
24.8306401042851));
#31881=CARTESIAN_POINT('Ctrl Pts',(-28.1863847775742,-0.00460633545135409,
24.7817609620066));
#31882=CARTESIAN_POINT('Ctrl Pts',(-28.1864731178034,-0.00460664429642971,
24.7328828792526));
#31883=CARTESIAN_POINT('Ctrl Pts',(-28.1875163330769,-0.0046102481476268,
24.1822767102568));
#31884=CARTESIAN_POINT('Ctrl Pts',(-28.1883126217779,-0.00461560258461171,
23.1781432543363));
#31885=CARTESIAN_POINT('Ctrl Pts',(-28.1901636158954,-0.0046304985039466,
21.1695480668301));
#31886=CARTESIAN_POINT('Ctrl Pts',(-28.1971064762245,-0.00465391042639694,
19.6653941983213));
#31887=CARTESIAN_POINT('Ctrl Pts',(-28.2118477398425,-0.00469056804568364,
18.4143448435113));
#31888=CARTESIAN_POINT('Ctrl Pts',(-28.2189167353326,-0.00470939894775233,
17.9115392779163));
#31889=CARTESIAN_POINT('Ctrl Pts',(-28.2366663011845,-0.0047586054950456,
16.9075569728651));
#31890=CARTESIAN_POINT('Ctrl Pts',(-28.2747390509576,-0.00486360912988234,
15.1537447443413));
#31891=CARTESIAN_POINT('Ctrl Pts',(-28.3109227936906,-0.00494472184720988,
13.6519622575988));
#31892=CARTESIAN_POINT('Ctrl Pts',(-28.3336317464906,-0.0049640640775537,
12.3974379027123));
#31893=CARTESIAN_POINT('Ctrl Pts',(-28.3429188492018,-0.00496852004088664,
11.896463348646));
#31894=CARTESIAN_POINT('Ctrl Pts',(-28.3618627525136,-0.00496581361296356,
10.8945900324065));
#31895=CARTESIAN_POINT('Ctrl Pts',(-28.3946724405316,-0.00493736126333316,
9.14102108292138));
#31896=CARTESIAN_POINT('Ctrl Pts',(-28.4177082765907,-0.00489031242012178,
7.63581293756268));
#31897=CARTESIAN_POINT('Ctrl Pts',(-28.427936275759,-0.00486645967896916,
6.50489137702784));
#31898=CARTESIAN_POINT('Ctrl Pts',(-28.430076222178,-0.00484956678344242,
6.25451917695903));
#31899=CARTESIAN_POINT('Ctrl Pts',(-28.4338784345938,-0.00477752765288108,
5.75325079164063));
#31900=CARTESIAN_POINT('Ctrl Pts',(-28.4392992625228,-0.00457292789812331,
4.87465469053201));
#31901=CARTESIAN_POINT('Ctrl Pts',(-28.4453694619222,-0.00403931884329462,
3.11453429456818));
#31902=CARTESIAN_POINT('Ctrl Pts',(-28.4429563699568,-0.00398414553418337,
1.60880108702352));
#31903=CARTESIAN_POINT('Ctrl Pts',(-28.4381704350487,-0.00474055572035643,
0.550446199667754));
#31904=CARTESIAN_POINT('Ctrl Pts',(-28.4375445621273,-0.00483960300428552,
0.424461121558914));
#31905=CARTESIAN_POINT('Ctrl Pts',(-28.4360822446314,-0.0050688520581819,
0.17263186514994));
#31906=CARTESIAN_POINT('Ctrl Pts',(-28.432999126287,-0.00554756712592698,
-0.267607748437768));
#31907=CARTESIAN_POINT('Ctrl Pts',(-28.4272652661807,-0.00641984888925787,
-0.89541244968379));
#31908=CARTESIAN_POINT('Ctrl Pts',(-28.4187863090284,-0.0076797759635048,
-1.64744927029274));
#31909=CARTESIAN_POINT('Ctrl Pts',(-28.406065940695,-0.00950538541273805,
-2.64901595059585));
#31910=CARTESIAN_POINT('Ctrl Pts',(-28.3888401377251,-0.011829617360604,
-3.89997598939455));
#31911=CARTESIAN_POINT('Ctrl Pts',(-28.376493002255,-0.0131975675662079,
-4.90214870528169));
#31912=CARTESIAN_POINT('Ctrl Pts',(-28.3701063743469,-0.0137396685467702,
-5.52975857296791));
#31913=CARTESIAN_POINT('Ctrl Pts',(-28.3675242803865,-0.0139619450347725,
-5.78051104302905));
#31914=CARTESIAN_POINT('Ctrl Pts',(-28.3622872451714,-0.0144149998525911,
-6.2826421124058));
#31915=CARTESIAN_POINT('Ctrl Pts',(-28.3530121884009,-0.0152005766043735,
-7.16194751912559));
#31916=CARTESIAN_POINT('Ctrl Pts',(-28.3398977716336,-0.0161385482469937,
-8.41920740101793));
#31917=CARTESIAN_POINT('Ctrl Pts',(-28.3281935808401,-0.0163896778099333,
-9.67501169157448));
#31918=CARTESIAN_POINT('Ctrl Pts',(-28.3213834537875,-0.0159739830935321,
-10.5519002670555));
#31919=CARTESIAN_POINT('Ctrl Pts',(-28.3179797696801,-0.01553293702959,
-11.0521448672915));
#31920=CARTESIAN_POINT('Ctrl Pts',(-28.3164549382297,-0.0152391975934058,
-11.3019518748116));
#31921=CARTESIAN_POINT('Ctrl Pts',(-28.3153795119772,-0.0149880839074049,
-11.489973567269));
#31922=CARTESIAN_POINT('Ctrl Pts',(-28.314685095118,-0.014792879670191,
-11.6166790902712));
#31923=CARTESIAN_POINT('Ctrl Pts',(-28.3134047585379,-0.0143102633951334,
-11.8695121594015));
#31924=CARTESIAN_POINT('Ctrl Pts',(-28.3114336217475,-0.0132401939293641,
-12.311206357399));
#31925=CARTESIAN_POINT('Ctrl Pts',(-28.3076038610431,-0.00951646921472725,
-13.4428824026115));
#31926=CARTESIAN_POINT('Ctrl Pts',(-28.3061586258559,-0.00364668722937351,
-14.691316859968));
#31927=CARTESIAN_POINT('Ctrl Pts',(-28.3050443425316,0.000568090034001496,
-15.939616939592));
#31928=CARTESIAN_POINT('Ctrl Pts',(-28.3043418144241,0.00198931723314658,
-16.5645176054236));
#31929=CARTESIAN_POINT('Ctrl Pts',(-28.3035947968661,0.00254663777454252,
-17.0653489248785));
#31930=CARTESIAN_POINT('Ctrl Pts',(-28.3031304898045,0.00260742789917509,
-17.3161305034899));
#31931=CARTESIAN_POINT('Ctrl Pts',(-28.3027467966274,0.00256088562709459,
-17.5036502999823));
#31932=CARTESIAN_POINT('Ctrl Pts',(-28.3025155137543,0.00254198055265861,
-17.6290856683236));
#31933=CARTESIAN_POINT('Ctrl Pts',(-28.3021374514763,0.00259174819776393,
-17.8790380467737));
#31934=CARTESIAN_POINT('Ctrl Pts',(-28.3018630375286,0.00274320347158438,
-18.1292232356557));
#31935=CARTESIAN_POINT('Ctrl Pts',(-28.3016839981496,0.00296417225329587,
-18.3791633923168));
#31936=CARTESIAN_POINT('Ctrl Pts',(-28.3016017365269,0.00312302677002713,
-18.5353803170869));
#31937=CARTESIAN_POINT('Ctrl Pts',(-28.3015528172302,0.00325835718774737,
-18.6603210609758));
#31938=CARTESIAN_POINT('Ctrl Pts',(-28.301513346424,0.00339789381416274,
-18.785253407746));
#31939=CARTESIAN_POINT('Ctrl Pts',(-28.3014335207091,0.00378777524423548,
-19.1287568608658));
#31940=CARTESIAN_POINT('Ctrl Pts',(-28.3014303865288,0.00441569054555669,
-19.6905720048103));
#31941=CARTESIAN_POINT('Ctrl Pts',(-28.3012214735957,0.00463831851483729,
-20.6885682611972));
#31942=CARTESIAN_POINT('Ctrl Pts',(-28.2993755605549,0.00165391259089476,
-21.9346838395311));
#31943=CARTESIAN_POINT('Ctrl Pts',(-28.2941297489489,-0.00805261113508078,
-22.9304888622303));
#31944=CARTESIAN_POINT('Ctrl Pts',(-28.2891626298632,-0.0175098653397202,
-23.5509560293143));
#31945=CARTESIAN_POINT('Ctrl Pts',(-28.2868822650861,-0.0217358296645737,
-23.7941797621322));
#31946=CARTESIAN_POINT('Ctrl Pts',(-28.2813074727843,-0.032077390509107,
-24.2844080322069));
#31947=CARTESIAN_POINT('Ctrl Pts',(-28.2693454732741,-0.0544057891600798,
-25.147158667633));
#31948=CARTESIAN_POINT('Ctrl Pts',(-28.2486784083908,-0.0942889514449492,
-26.3948278722657));
#31949=CARTESIAN_POINT('Ctrl Pts',(-28.2257077673537,-0.14255782676672,
-27.9110090292924));
#31950=CARTESIAN_POINT('Ctrl Pts',(-28.216385187724,-0.167029701575379,
-28.9316551969023));
#31951=CARTESIAN_POINT('Ctrl Pts',(-28.2142667044121,-0.176558653404427,
-29.5076376535198));
#31952=CARTESIAN_POINT('Ctrl Pts',(-28.2138126885783,-0.178615435337877,
-29.633065948268));
#31953=CARTESIAN_POINT('Ctrl Pts',(-28.2129475846591,-0.182637689761345,
-29.8854739383231));
#31954=CARTESIAN_POINT('Ctrl Pts',(-28.2115838536727,-0.189353462795671,
-30.3266897748748));
#31955=CARTESIAN_POINT('Ctrl Pts',(-28.2096267231321,-0.201505456968724,
-31.2105582168276));
#31956=CARTESIAN_POINT('Ctrl Pts',(-28.2100031363158,-0.212082202476106,
-32.2217394016259));
#31957=CARTESIAN_POINT('Ctrl Pts',(-28.214681940452,-0.218758095344881,
-33.2334878724097));
#31958=CARTESIAN_POINT('Ctrl Pts',(-28.2207706234283,-0.221641983732676,
-33.9921974180832));
#31959=CARTESIAN_POINT('Ctrl Pts',(-28.2298770732745,-0.222163231633312,
-34.7504699343643));
#31960=CARTESIAN_POINT('Ctrl Pts',(-28.238249225568,-0.220820903106427,
-35.2555188277877));
#31961=CARTESIAN_POINT('Ctrl Pts',(-28.245520562333,-0.219135849961407,
-35.6351015437609));
#31962=CARTESIAN_POINT('Ctrl Pts',(-28.2508731165334,-0.217786895183696,
-35.889230843851));
#31963=CARTESIAN_POINT('Ctrl Pts',(-28.2633058084189,-0.214239235970583,
-36.3967042830002));
#31964=CARTESIAN_POINT('Ctrl Pts',(-28.2891464643115,-0.205729147312358,
-37.2826146212146));
#31965=CARTESIAN_POINT('Ctrl Pts',(-28.3534019588011,-0.180241286852696,
-39.0487948012157));
#31966=CARTESIAN_POINT('Ctrl Pts',(-28.4172498273522,-0.144300921438199,
-40.5588253834969));
#31967=CARTESIAN_POINT('Ctrl Pts',(-28.4564486934885,-0.111653453402085,
-41.6953858046599));
#31968=CARTESIAN_POINT('Ctrl Pts',(-28.4649228404561,-0.105861983781313,
-41.9313674162035));
#31969=CARTESIAN_POINT('Ctrl Pts',(-28.4772841445845,-0.0991681183657871,
-42.2973103574194));
#31970=CARTESIAN_POINT('Ctrl Pts',(-28.4893593522273,-0.0941570899006693,
-42.6645390481917));
#31971=CARTESIAN_POINT('Ctrl Pts',(-28.505203288971,-0.0887045924743431,
-43.1610624503874));
#31972=CARTESIAN_POINT('Ctrl Pts',(-28.5247366850926,-0.0826468713669569,
-43.7910003417678));
#31973=CARTESIAN_POINT('Ctrl Pts',(-28.5484404118947,-0.0709530661363236,
-44.5626348394999));
#31974=CARTESIAN_POINT('Ctrl Pts',(-28.5689764856386,-0.0525654338336199,
-45.2178320678155));
#31975=CARTESIAN_POINT('Ctrl Pts',(-28.5861701425892,-0.0294661635961474,
-45.7492950011563));
#31976=CARTESIAN_POINT('Ctrl Pts',(-28.5995201029825,-0.00712421863073947,
-46.1513607436204));
#31977=CARTESIAN_POINT('Ctrl Pts',(-28.613385212919,0.0210865954295373,
-46.5568519528627));
#31978=CARTESIAN_POINT('Ctrl Pts',(-28.6326148639367,0.0677117422033199,
-47.1019015008582));
#31979=CARTESIAN_POINT('Ctrl Pts',(-28.6479582923095,0.114099562474359,
-47.5154787240077));
#31980=CARTESIAN_POINT('Ctrl Pts',(-28.6639629462404,0.170110982033969,
-47.9327508282799));
#31981=CARTESIAN_POINT('Ctrl Pts',(-28.6760104425626,0.208815074499745,
-48.2040495811931));
#31982=CARTESIAN_POINT('Ctrl Pts',(-28.7034894331993,0.296045118550941,
-48.7479340590624));
#31983=CARTESIAN_POINT('Ctrl Pts',(-28.7587570263741,0.470865910892395,
-49.6895209659119));
#31984=CARTESIAN_POINT('Ctrl Pts',(-28.8456712155738,0.776483402567067,
-51.0114022234942));
#31985=CARTESIAN_POINT('Ctrl Pts',(-28.927339437998,1.19547757616793,-52.5558913273152));
#31986=CARTESIAN_POINT('Ctrl Pts',(-28.9490218947129,1.47956209353257,-53.5617487549242));
#31987=CARTESIAN_POINT('Ctrl Pts',(-28.9473547952781,1.65012798643743,-54.186254485831));
#31988=CARTESIAN_POINT('Ctrl Pts',(-28.9444871311617,1.72175364071754,-54.4480453615726));
#31989=CARTESIAN_POINT('Ctrl Pts',(-28.9341668134448,1.86520562706103,-54.9665377909226));
#31990=CARTESIAN_POINT('Ctrl Pts',(-28.9039504324693,2.12133746067361,-55.877091855804));
#31991=CARTESIAN_POINT('Ctrl Pts',(-28.8061314957623,2.6529879289795,-57.6947502180311));
#31992=CARTESIAN_POINT('Ctrl Pts',(-28.6903443350229,3.15423154962865,-59.2397974222075));
#31993=CARTESIAN_POINT('Ctrl Pts',(-28.6263471470519,3.53403403606696,-60.3184713489117));
#31994=CARTESIAN_POINT('Ctrl Pts',(-28.6183525944514,3.5803669285416,-60.4500322101376));
#31995=CARTESIAN_POINT('Ctrl Pts',(-28.6016837617537,3.67372926736117,-60.7128442372547));
#31996=CARTESIAN_POINT('Ctrl Pts',(-28.5708003187594,3.83905363322346,-61.1727900519157));
#31997=CARTESIAN_POINT('Ctrl Pts',(-28.503394716372,4.1776943041034,-62.0913978688054));
#31998=CARTESIAN_POINT('Ctrl Pts',(-28.4188521456682,4.5846543218748,-63.1356496646742));
#31999=CARTESIAN_POINT('Ctrl Pts',(-28.3388845614405,5.01183715274042,-64.1687182709692));
#32000=CARTESIAN_POINT('Ctrl Pts',(-28.2979803171294,5.25917876202764,-64.7449014612071));
#32001=CARTESIAN_POINT('Ctrl Pts',(-28.2733358642123,5.42676450286561,-65.1266980782478));
#32002=CARTESIAN_POINT('Ctrl Pts',(-28.2576679953265,5.53917211512882,-65.3805903841216));
#32003=CARTESIAN_POINT('Ctrl Pts',(-28.2432271711642,5.65260419490981,-65.6335437356018));
#32004=CARTESIAN_POINT('Ctrl Pts',(-28.2318222335131,5.75266344337316,-65.8539777388884));
#32005=CARTESIAN_POINT('Ctrl Pts',(-28.2256772991046,5.81006471456788,-65.9796823611048));
#32006=CARTESIAN_POINT('Ctrl Pts',(-28.2168428029436,5.89638926812434,-66.167985912538));
#32007=CARTESIAN_POINT('Ctrl Pts',(-28.2102987830632,5.96877716465577,-66.324358053145));
#32008=CARTESIAN_POINT('Ctrl Pts',(-28.2006623951268,6.08925573052596,-66.5826915117347));
#32009=CARTESIAN_POINT('Ctrl Pts',(-28.1918397593507,6.21898802956303,-66.8567837258073));
#32010=CARTESIAN_POINT('Ctrl Pts',(-28.1784070116348,6.48002646242587,-67.3934340007737));
#32011=CARTESIAN_POINT('Ctrl Pts',(-28.1646562164352,6.94658361661508,-68.3190168217354));
#32012=CARTESIAN_POINT('Ctrl Pts',(-28.1663770295904,7.90084850797895,-70.1119324976335));
#32013=CARTESIAN_POINT('Ctrl Pts',(-28.1881081132948,8.71948558422654,-71.582446078205));
#32014=CARTESIAN_POINT('Ctrl Pts',(-28.1863206363366,9.30013791883288,-72.680964220891));
#32015=CARTESIAN_POINT('Ctrl Pts',(-28.1859809829049,9.43444168834478,-72.9348507263182));
#32016=CARTESIAN_POINT('Ctrl Pts',(-28.1854737933729,9.70045760038316,-73.4370577568619));
#32017=CARTESIAN_POINT('Ctrl Pts',(-28.1851399583262,10.034413389861,-74.0664101829464));
#32018=CARTESIAN_POINT('Ctrl Pts',(-28.185104743579,10.4348437144677,-74.8196494289759));
#32019=CARTESIAN_POINT('Ctrl Pts',(-28.1855469585286,11.2363852336376,-76.3254833102637));
#32020=CARTESIAN_POINT('Ctrl Pts',(-28.1865222320035,11.9042541659904,-77.5779156822583));
#32021=CARTESIAN_POINT('Ctrl Pts',(-28.1865189209674,12.8729892730661,-79.399855078337));
#32022=CARTESIAN_POINT('Ctrl Pts',(-28.1865194110349,13.3099555663221,-80.221676071923));
#32023=CARTESIAN_POINT('Ctrl Pts',(-28.1865194110349,13.7464771537116,-81.0426537740213));
#32024=CARTESIAN_POINT('Ctrl Pts',(-26.3067668117876,-0.000538699954624175,
24.8306355267635));
#32025=CARTESIAN_POINT('Ctrl Pts',(-26.3068451876501,-0.000538876189496768,
24.781756239974));
#32026=CARTESIAN_POINT('Ctrl Pts',(-26.306927385946,-0.000539061754406431,
24.7328780109039));
#32027=CARTESIAN_POINT('Ctrl Pts',(-26.3078981083115,-0.000541218695861637,
24.1822701223404));
#32028=CARTESIAN_POINT('Ctrl Pts',(-26.308638797907,-0.000542921187126547,
23.1781339115758));
#32029=CARTESIAN_POINT('Ctrl Pts',(-26.3103596540731,-0.000547510562500565,
21.1695358988917));
#32030=CARTESIAN_POINT('Ctrl Pts',(-26.3168206355383,-0.000561494614877348,
19.6653821365272));
#32031=CARTESIAN_POINT('Ctrl Pts',(-26.3305400639719,-0.000590835905523418,
18.4143333475625));
#32032=CARTESIAN_POINT('Ctrl Pts',(-26.3371183800673,-0.000605254926751675,
17.9115190955673));
#32033=CARTESIAN_POINT('Ctrl Pts',(-26.3536351484472,-0.000641926725106596,
16.9075303164735));
#32034=CARTESIAN_POINT('Ctrl Pts',(-26.3890629920332,-0.000720784918182074,
15.1537172634109));
#32035=CARTESIAN_POINT('Ctrl Pts',(-26.4227431417796,-0.000791449315555003,
13.6519609598852));
#32036=CARTESIAN_POINT('Ctrl Pts',(-26.4438929028652,-0.000829734955752551,
12.3974737776712));
#32037=CARTESIAN_POINT('Ctrl Pts',(-26.4525430650074,-0.00084487329312605,
11.8965144636692));
#32038=CARTESIAN_POINT('Ctrl Pts',(-26.4701923515509,-0.000873398605924195,
10.8946630473504));
#32039=CARTESIAN_POINT('Ctrl Pts',(-26.5007676037454,-0.000918523372976478,
9.14111543813712));
#32040=CARTESIAN_POINT('Ctrl Pts',(-26.5222561422087,-0.000942796547773691,
7.63589175690357));
#32041=CARTESIAN_POINT('Ctrl Pts',(-26.5318021172031,-0.000952582193824432,
6.50494958170678));
#32042=CARTESIAN_POINT('Ctrl Pts',(-26.5338202972566,-0.000947585409883766,
6.25463586694622));
#32043=CARTESIAN_POINT('Ctrl Pts',(-26.5374815994599,-0.000913662062184531,
5.75342822449203));
#32044=CARTESIAN_POINT('Ctrl Pts',(-26.542884293761,-0.000804479291789807,
4.87490869188615));
#32045=CARTESIAN_POINT('Ctrl Pts',(-26.5494687884833,-0.000504712387683716,
3.11473294922618));
#32046=CARTESIAN_POINT('Ctrl Pts',(-26.5472854591206,-0.000478066320458629,
1.60861764398263));
#32047=CARTESIAN_POINT('Ctrl Pts',(-26.5414101923829,-0.000937735640324079,
0.549835984673704));
#32048=CARTESIAN_POINT('Ctrl Pts',(-26.5406416200034,-0.000998055376415954,
0.423780445023005));
#32049=CARTESIAN_POINT('Ctrl Pts',(-26.5388520301281,-0.0011376182369757,
0.171831141482077));
#32050=CARTESIAN_POINT('Ctrl Pts',(-26.5350910798596,-0.00142888191146685,
-0.268602127637444));
#32051=CARTESIAN_POINT('Ctrl Pts',(-26.5281424169917,-0.00195699496613554,
-0.896615216968427));
#32052=CARTESIAN_POINT('Ctrl Pts',(-26.5179253790002,-0.00271609093358323,
-1.64879887106375));
#32053=CARTESIAN_POINT('Ctrl Pts',(-26.5027296125362,-0.00380454918085976,
-2.65042863623411));
#32054=CARTESIAN_POINT('Ctrl Pts',(-26.4824144417945,-0.00516579915528091,
-3.90123622681562));
#32055=CARTESIAN_POINT('Ctrl Pts',(-26.4683792072888,-0.00593730752158881,
-4.90305082619869));
#32056=CARTESIAN_POINT('Ctrl Pts',(-26.4613995433984,-0.00622942189138888,
-5.53038586337433));
#32057=CARTESIAN_POINT('Ctrl Pts',(-26.4586055525338,-0.0063380563385362,
-5.78133473549539));
#32058=CARTESIAN_POINT('Ctrl Pts',(-26.4530433222871,-0.00652495285022699,
-6.28361018998542));
#32059=CARTESIAN_POINT('Ctrl Pts',(-26.4434403582543,-0.00677386241630181,
-7.16308898027664));
#32060=CARTESIAN_POINT('Ctrl Pts',(-26.4304432957718,-0.0069274983770433,
-8.42004337635663));
#32061=CARTESIAN_POINT('Ctrl Pts',(-26.419323612753,-0.00686441290470747,
-9.67491166013457));
#32062=CARTESIAN_POINT('Ctrl Pts',(-26.4130042716163,-0.0067357043217891,
-10.5507828150709));
#32063=CARTESIAN_POINT('Ctrl Pts',(-26.4098829159842,-0.00664094240293327,
-11.0503441710192));
#32064=CARTESIAN_POINT('Ctrl Pts',(-26.4084973739244,-0.0065873715842191,
-11.2997774800692));
#32065=CARTESIAN_POINT('Ctrl Pts',(-26.4075238006317,-0.00654481180717828,
-11.4874960340828));
#32066=CARTESIAN_POINT('Ctrl Pts',(-26.4068990555078,-0.0065126789462424,
-11.6137055904411));
#32067=CARTESIAN_POINT('Ctrl Pts',(-26.4057636148961,-0.00643259146762249,
-11.8657795877875));
#32068=CARTESIAN_POINT('Ctrl Pts',(-26.4040634719408,-0.00625453645064599,
-12.3062201720521));
#32069=CARTESIAN_POINT('Ctrl Pts',(-26.4010267927984,-0.00563307175450961,
-13.4355782116524));
#32070=CARTESIAN_POINT('Ctrl Pts',(-26.4007771402918,-0.00460249839055765,
-14.6839857455774));
#32071=CARTESIAN_POINT('Ctrl Pts',(-26.4011342734351,-0.00376334242939199,
-15.9348201084843));
#32072=CARTESIAN_POINT('Ctrl Pts',(-26.4012564354109,-0.00344118371370728,
-16.5615920969361));
#32073=CARTESIAN_POINT('Ctrl Pts',(-26.4011953559784,-0.00327847224339482,
-17.0642625997816));
#32074=CARTESIAN_POINT('Ctrl Pts',(-26.4010889745752,-0.00323185749929953,
-17.3160885549663));
#32075=CARTESIAN_POINT('Ctrl Pts',(-26.4009744528728,-0.00321370813660455,
-17.5043944183102));
#32076=CARTESIAN_POINT('Ctrl Pts',(-26.4009502260798,-0.00319047410131549,
-17.6291798260985));
#32077=CARTESIAN_POINT('Ctrl Pts',(-26.401090732026,-0.00313045400635487,
-17.8786393400492));
#32078=CARTESIAN_POINT('Ctrl Pts',(-26.4014814965549,-0.00304331594204274,
-18.1282409226063));
#32079=CARTESIAN_POINT('Ctrl Pts',(-26.4020734283397,-0.00294946836358305,
-18.3778951727794));
#32080=CARTESIAN_POINT('Ctrl Pts',(-26.4025133950277,-0.00288718042293722,
-18.5339729656228));
#32081=CARTESIAN_POINT('Ctrl Pts',(-26.4029014443056,-0.00283774620801123,
-18.6588550278531));
#32082=CARTESIAN_POINT('Ctrl Pts',(-26.4033113524095,-0.00278891479687412,
-18.7837532047067));
#32083=CARTESIAN_POINT('Ctrl Pts',(-26.4045102812651,-0.00265070793138668,
-19.1272863938833));
#32084=CARTESIAN_POINT('Ctrl Pts',(-26.4068039814181,-0.00246061209984525,
-19.6897931196873));
#32085=CARTESIAN_POINT('Ctrl Pts',(-26.4105766396482,-0.00235074624862679,
-20.6909483135089));
#32086=CARTESIAN_POINT('Ctrl Pts',(-26.4127186181016,-0.0030500036225254,
-21.944804180922));
#32087=CARTESIAN_POINT('Ctrl Pts',(-26.4066977217584,-0.00478894319038026,
-22.9508245281247));
#32088=CARTESIAN_POINT('Ctrl Pts',(-26.3990835556788,-0.0064034352788766,
-23.5787686036408));
#32089=CARTESIAN_POINT('Ctrl Pts',(-26.3955759960211,-0.00713908522416187,
-23.8270180069377));
#32090=CARTESIAN_POINT('Ctrl Pts',(-26.3867350909327,-0.0088416464694765,
-24.3247318868074));
#32091=CARTESIAN_POINT('Ctrl Pts',(-26.3671611553572,-0.0123384937718505,
-25.1980292444309));
#32092=CARTESIAN_POINT('Ctrl Pts',(-26.3309962257493,-0.0179683153941739,
-26.451199300417));
#32093=CARTESIAN_POINT('Ctrl Pts',(-26.286983275886,-0.0241164221772839,
-27.9603145633623));
#32094=CARTESIAN_POINT('Ctrl Pts',(-26.2648364528597,-0.0269527012872554,
-28.9674675109934));
#32095=CARTESIAN_POINT('Ctrl Pts',(-26.2565759171718,-0.0281304007585666,
-29.5336179009703));
#32096=CARTESIAN_POINT('Ctrl Pts',(-26.2547552462034,-0.0284027765599454,
-29.6589431501243));
#32097=CARTESIAN_POINT('Ctrl Pts',(-26.2511601601551,-0.0289274610454118,
-29.9099370325545));
#32098=CARTESIAN_POINT('Ctrl Pts',(-26.2450037793416,-0.0298100005573521,
-30.3491931563502));
#32099=CARTESIAN_POINT('Ctrl Pts',(-26.23347324007,-0.031427036391679,-31.2283707605503));
#32100=CARTESIAN_POINT('Ctrl Pts',(-26.2229714198081,-0.0329540249543629,
-32.2337271230666));
#32101=CARTESIAN_POINT('Ctrl Pts',(-26.2170313145426,-0.0341652924499194,
-33.2388001712352));
#32102=CARTESIAN_POINT('Ctrl Pts',(-26.2153206044666,-0.0349193705859608,
-33.9921653671943));
#32103=CARTESIAN_POINT('Ctrl Pts',(-26.2167440409269,-0.0354991514690913,
-34.744715353211));
#32104=CARTESIAN_POINT('Ctrl Pts',(-26.2201074284133,-0.0357706548368423,
-35.245701175117));
#32105=CARTESIAN_POINT('Ctrl Pts',(-26.2236621317938,-0.0359215423046611,
-35.6221289590457));
#32106=CARTESIAN_POINT('Ctrl Pts',(-26.226523386943,-0.036036968596862,
-35.874004709527));
#32107=CARTESIAN_POINT('Ctrl Pts',(-26.2339799499197,-0.0362914675196322,
-36.3772691388551));
#32108=CARTESIAN_POINT('Ctrl Pts',(-26.2510933692841,-0.0368106569182081,
-37.2561994063118));
#32109=CARTESIAN_POINT('Ctrl Pts',(-26.2977812793891,-0.0373645488137689,
-39.0104730415285));
#32110=CARTESIAN_POINT('Ctrl Pts',(-26.346463654717,-0.035831460880283,
-40.5130518138167));
#32111=CARTESIAN_POINT('Ctrl Pts',(-26.3743845800949,-0.0318724213306068,
-41.6455984565211));
#32112=CARTESIAN_POINT('Ctrl Pts',(-26.3803646184719,-0.0319919850056345,
-41.8821563107312));
#32113=CARTESIAN_POINT('Ctrl Pts',(-26.3888990724742,-0.0344735418328895,
-42.2477051044875));
#32114=CARTESIAN_POINT('Ctrl Pts',(-26.3970924896663,-0.0387561876770233,
-42.6143309685538));
#32115=CARTESIAN_POINT('Ctrl Pts',(-26.4077089334092,-0.0461283281546971,
-43.1092311587212));
#32116=CARTESIAN_POINT('Ctrl Pts',(-26.4206471327102,-0.0570574791966879,
-43.7359587822667));
#32117=CARTESIAN_POINT('Ctrl Pts',(-26.4365127811393,-0.0682199099401007,
-44.5016798704673));
#32118=CARTESIAN_POINT('Ctrl Pts',(-26.4507600954306,-0.0717721409268919,
-45.1502723734384));
#32119=CARTESIAN_POINT('Ctrl Pts',(-26.4631485089363,-0.0684515872827657,
-45.6756036567527));
#32120=CARTESIAN_POINT('Ctrl Pts',(-26.4730834273353,-0.0622375662230723,
-46.0726037171871));
#32121=CARTESIAN_POINT('Ctrl Pts',(-26.4837699828375,-0.0515935685134581,
-46.4726163317117));
#32122=CARTESIAN_POINT('Ctrl Pts',(-26.4991359060241,-0.0305036443217214,
-47.009862706898));
#32123=CARTESIAN_POINT('Ctrl Pts',(-26.5121828351866,-0.00591486366776645,
-47.4170859639793));
#32124=CARTESIAN_POINT('Ctrl Pts',(-26.526370740002,0.026204196782403,-47.8275722662938));
#32125=CARTESIAN_POINT('Ctrl Pts',(-26.5368999472404,0.0469741353359872,
-48.0837653863055));
#32126=CARTESIAN_POINT('Ctrl Pts',(-26.561505249712,0.0933214806286183,
-48.6082125153391));
#32127=CARTESIAN_POINT('Ctrl Pts',(-26.6122988327719,0.185167815068433,
-49.5236130485645));
#32128=CARTESIAN_POINT('Ctrl Pts',(-26.6981479760903,0.354523776728155,
-50.8430742403432));
#32129=CARTESIAN_POINT('Ctrl Pts',(-26.7897670019238,0.632358244960462,
-52.4342725278277));
#32130=CARTESIAN_POINT('Ctrl Pts',(-26.8215844026514,0.870582339384173,
-53.4999944261828));
#32131=CARTESIAN_POINT('Ctrl Pts',(-26.8260719038306,1.03697665514042,-54.1689646396975));
#32132=CARTESIAN_POINT('Ctrl Pts',(-26.8267141003341,1.10670827271461,-54.4412685219691));
#32133=CARTESIAN_POINT('Ctrl Pts',(-26.8239229838561,1.2530150747219,-54.9820638531088));
#32134=CARTESIAN_POINT('Ctrl Pts',(-26.8094090076117,1.52687003205735,-55.9232842367911));
#32135=CARTESIAN_POINT('Ctrl Pts',(-26.7502718252429,2.13524051873476,-57.7806701159655));
#32136=CARTESIAN_POINT('Ctrl Pts',(-26.6752243845139,2.7305383529955,-59.3268082550157));
#32137=CARTESIAN_POINT('Ctrl Pts',(-26.6326526327287,3.15991915978893,-60.3965741559011));
#32138=CARTESIAN_POINT('Ctrl Pts',(-26.626796545975,3.21513955923081,-60.5332834491796));
#32139=CARTESIAN_POINT('Ctrl Pts',(-26.6147773682979,3.32555826188788,-60.802125674637));
#32140=CARTESIAN_POINT('Ctrl Pts',(-26.5921560075181,3.52329843623239,-61.2727430817421));
#32141=CARTESIAN_POINT('Ctrl Pts',(-26.5424166539232,3.93163734514937,-62.2048352783439));
#32142=CARTESIAN_POINT('Ctrl Pts',(-26.4798588133065,4.42290831484138,-63.2519488087729));
#32143=CARTESIAN_POINT('Ctrl Pts',(-26.4209725251522,4.92351798754586,-64.275801140273));
#32144=CARTESIAN_POINT('Ctrl Pts',(-26.3908305504492,5.20574309869606,-64.842548605701));
#32145=CARTESIAN_POINT('Ctrl Pts',(-26.3726624707943,5.39290454963424,-65.2162099904711));
#32146=CARTESIAN_POINT('Ctrl Pts',(-26.3611127413162,5.51731893373302,-65.4641867626717));
#32147=CARTESIAN_POINT('Ctrl Pts',(-26.350457060261,5.64112088719479,-65.7104773833032));
#32148=CARTESIAN_POINT('Ctrl Pts',(-26.3420548604655,5.74863241414718,-65.924405367996));
#32149=CARTESIAN_POINT('Ctrl Pts',(-26.337532095308,5.8098084630586,-66.0461948795629));
#32150=CARTESIAN_POINT('Ctrl Pts',(-26.3310362843529,5.90130035682774,-66.2284296655541));
#32151=CARTESIAN_POINT('Ctrl Pts',(-26.3262335770603,5.97694150202082,-66.3793158252329));
#32152=CARTESIAN_POINT('Ctrl Pts',(-26.319205668863,6.10130572534613,-66.6280505446839));
#32153=CARTESIAN_POINT('Ctrl Pts',(-26.3127232182357,6.23599075482196,-66.8956533728625));
#32154=CARTESIAN_POINT('Ctrl Pts',(-26.3027625454309,6.50273866782855,-67.4190586948082));
#32155=CARTESIAN_POINT('Ctrl Pts',(-26.292289466235,6.97273749902019,-68.3260826013178));
#32156=CARTESIAN_POINT('Ctrl Pts',(-26.2927638675289,7.91373509191888,-70.0956972417704));
#32157=CARTESIAN_POINT('Ctrl Pts',(-26.3084135850719,8.71555338749269,-71.5704800074898));
#32158=CARTESIAN_POINT('Ctrl Pts',(-26.3069267097133,9.30581961794523,-72.6838758449878));
#32159=CARTESIAN_POINT('Ctrl Pts',(-26.3066448287013,9.43971394243508,-72.9363526706905));
#32160=CARTESIAN_POINT('Ctrl Pts',(-26.3062240590782,9.70620739982533,-73.4385206011396));
#32161=CARTESIAN_POINT('Ctrl Pts',(-26.305940355283,10.0399597181007,-74.0668450111416));
#32162=CARTESIAN_POINT('Ctrl Pts',(-26.3059074450485,10.4401946275587,-74.8196393294015));
#32163=CARTESIAN_POINT('Ctrl Pts',(-26.3062657564787,11.2408551638692,-76.3246049709325));
#32164=CARTESIAN_POINT('Ctrl Pts',(-26.3070482825158,11.9079288942245,-77.5772542386599));
#32165=CARTESIAN_POINT('Ctrl Pts',(-26.3070325410241,12.8772469790119,-79.4002400070955));
#32166=CARTESIAN_POINT('Ctrl Pts',(-26.3070253104064,13.3140222206688,-80.2216760094386));
#32167=CARTESIAN_POINT('Ctrl Pts',(-26.3070253104064,13.7505438080583,-81.0426537115369));
#32168=CARTESIAN_POINT('Ctrl Pts',(-24.4302598458315,0.00207241768738013,
24.8306321780374));
#32169=CARTESIAN_POINT('Ctrl Pts',(-24.4303326385072,0.00207243626309089,
24.7817527847082));
#32170=CARTESIAN_POINT('Ctrl Pts',(-24.4304089822103,0.00207245410495211,
24.7328744451339));
#32171=CARTESIAN_POINT('Ctrl Pts',(-24.431310518414,0.00207273452647534,
24.1822653742894));
#32172=CARTESIAN_POINT('Ctrl Pts',(-24.4319997949999,0.002074798633469,
23.1781282789352));
#32173=CARTESIAN_POINT('Ctrl Pts',(-24.4336029354561,0.00207958583484067,
21.169528032579));
#32174=CARTESIAN_POINT('Ctrl Pts',(-24.4396028097008,0.00208213590548975,
19.665375037048));
#32175=CARTESIAN_POINT('Ctrl Pts',(-24.4523362120325,0.00207846071060644,
18.4143265564543));
#32176=CARTESIAN_POINT('Ctrl Pts',(-24.4584422452079,0.00207700396147341,
17.9115055015473));
#32177=CARTESIAN_POINT('Ctrl Pts',(-24.4737736243947,0.00207419848106817,
16.9075122978479));
#32178=CARTESIAN_POINT('Ctrl Pts',(-24.5066586150648,0.00206743293100846,
15.1537005858998));
#32179=CARTESIAN_POINT('Ctrl Pts',(-24.5379117822613,0.00205552255842673,
13.6519696262246));
#32180=CARTESIAN_POINT('Ctrl Pts',(-24.5575252982735,0.00203417914685445,
12.3975128714527));
#32181=CARTESIAN_POINT('Ctrl Pts',(-24.5655458139266,0.0020235622723546,
11.896565806553));
#32182=CARTESIAN_POINT('Ctrl Pts',(-24.581904661484,0.00199730192436314,
10.8947319643132));
#32183=CARTESIAN_POINT('Ctrl Pts',(-24.6102349989673,0.00194086962837188,
9.14120368806769));
#32184=CARTESIAN_POINT('Ctrl Pts',(-24.6301298063699,0.00189647960059792,
7.63597166157432));
#32185=CARTESIAN_POINT('Ctrl Pts',(-24.6389709679162,0.00187539772952453,
6.50503228212297));
#32186=CARTESIAN_POINT('Ctrl Pts',(-24.6408586920625,0.00185852210705859,
6.25496417883429));
#32187=CARTESIAN_POINT('Ctrl Pts',(-24.6443450540568,0.00178646142423656,
5.75402051427475));
#32188=CARTESIAN_POINT('Ctrl Pts',(-24.6496310763466,0.00158564485051102,
4.87583468008954));
#32189=CARTESIAN_POINT('Ctrl Pts',(-24.6564832101539,0.001060595851991,
3.11545176947256));
#32190=CARTESIAN_POINT('Ctrl Pts',(-24.6544271176886,0.0010725556503662,
1.60780682331442));
#32191=CARTESIAN_POINT('Ctrl Pts',(-24.6477393559816,0.00187911894342457,
0.547228808229092));
#32192=CARTESIAN_POINT('Ctrl Pts',(-24.6468670454309,0.00198228716043408,
0.420859272548393));
#32193=CARTESIAN_POINT('Ctrl Pts',(-24.6448379805963,0.00222154099192133,
0.168378929386594));
#32194=CARTESIAN_POINT('Ctrl Pts',(-24.6405822662372,0.00271852968384454,
-0.27292074557853));
#32195=CARTESIAN_POINT('Ctrl Pts',(-24.6327330953819,0.00362879071700781,
-0.901883303165047));
#32196=CARTESIAN_POINT('Ctrl Pts',(-24.6212550923228,0.00492381701602845,
-1.65477326639694));
#32197=CARTESIAN_POINT('Ctrl Pts',(-24.6042511572935,0.00681216662778669,
-2.65675225674018));
#32198=CARTESIAN_POINT('Ctrl Pts',(-24.5817526291741,0.00920233268893764,
-3.90689693828391));
#32199=CARTESIAN_POINT('Ctrl Pts',(-24.5665854070869,0.0106595112999088,
-4.90704239014045));
#32200=CARTESIAN_POINT('Ctrl Pts',(-24.5592701464447,0.011252652744233,
-5.53300978139183));
#32201=CARTESIAN_POINT('Ctrl Pts',(-24.5563805916875,0.0114808742337481,
-5.78390798487287));
#32202=CARTESIAN_POINT('Ctrl Pts',(-24.5507648758424,0.0119110310305683,
-6.28579785044557));
#32203=CARTESIAN_POINT('Ctrl Pts',(-24.5413723315553,0.0125867636336026,
-7.16473631064441));
#32204=CARTESIAN_POINT('Ctrl Pts',(-24.5292461080297,0.013296537346102,
-8.42079248918329));
#32205=CARTESIAN_POINT('Ctrl Pts',(-24.5189813407149,0.0135655554008891,
-9.6747509929314));
#32206=CARTESIAN_POINT('Ctrl Pts',(-24.5128446667743,0.0134673077102899,
-10.5499339117164));
#32207=CARTESIAN_POINT('Ctrl Pts',(-24.5096481069911,0.0133233761694472,
-11.0490941768464));
#32208=CARTESIAN_POINT('Ctrl Pts',(-24.5081546115769,0.0132207732092439,
-11.298325141733));
#32209=CARTESIAN_POINT('Ctrl Pts',(-24.5070700376299,0.0131315030567913,
-11.4858819021457));
#32210=CARTESIAN_POINT('Ctrl Pts',(-24.5063550638443,0.0130605512375759,
-11.6116968164213));
#32211=CARTESIAN_POINT('Ctrl Pts',(-24.5049805016318,0.0128761532028387,
-11.8631927519117));
#32212=CARTESIAN_POINT('Ctrl Pts',(-24.5027188133538,0.0124505890990866,
-12.3026550313652));
#32213=CARTESIAN_POINT('Ctrl Pts',(-24.4976258539558,0.0109093890863102,
-13.4301717344791));
#32214=CARTESIAN_POINT('Ctrl Pts',(-24.4940183631344,0.00834978154633404,
-14.6783035848225));
#32215=CARTESIAN_POINT('Ctrl Pts',(-24.4922145413803,0.00639335755892261,
-15.9307710268368));
#32216=CARTESIAN_POINT('Ctrl Pts',(-24.4917335592822,0.00569212405988055,
-16.5588156965784));
#32217=CARTESIAN_POINT('Ctrl Pts',(-24.4915994843194,0.00536769089701191,
-17.0627887753014));
#32218=CARTESIAN_POINT('Ctrl Pts',(-24.4916099867796,0.00529831606360045,
-17.3153668936557));
#32219=CARTESIAN_POINT('Ctrl Pts',(-24.4916481807073,0.00528513131603834,
-17.5042432457089));
#32220=CARTESIAN_POINT('Ctrl Pts',(-24.4917240828623,0.0052615853092459,
-17.6284683291437));
#32221=CARTESIAN_POINT('Ctrl Pts',(-24.4920652428219,0.00517239651012107,
-17.8774695208318));
#32222=CARTESIAN_POINT('Ctrl Pts',(-24.4926623408773,0.0050290820999663,
-18.126553375236));
#32223=CARTESIAN_POINT('Ctrl Pts',(-24.493478719597,0.00485067977437561,
-18.375950292712));
#32224=CARTESIAN_POINT('Ctrl Pts',(-24.4940684557923,0.00472919091578594,
-18.531904423794));
#32225=CARTESIAN_POINT('Ctrl Pts',(-24.4945834813114,0.00462833140614637,
-18.6567339566448));
#32226=CARTESIAN_POINT('Ctrl Pts',(-24.4951251970626,0.00452598289165581,
-18.7816014343059));
#32227=CARTESIAN_POINT('Ctrl Pts',(-24.4967125631211,0.00424156214605843,
-19.1251545575784));
#32228=CARTESIAN_POINT('Ctrl Pts',(-24.4997778141386,0.00379928994353248,
-19.6882390161473));
#32229=CARTESIAN_POINT('Ctrl Pts',(-24.5055739239131,0.00349296678830271,
-20.691948680636));
#32230=CARTESIAN_POINT('Ctrl Pts',(-24.5116689861703,0.00477590510021411,
-21.9517128859598));
#32231=CARTESIAN_POINT('Ctrl Pts',(-24.5114599746138,0.00915274888702006,
-22.9653116795392));
#32232=CARTESIAN_POINT('Ctrl Pts',(-24.5085973031169,0.0134042955649363,
-23.5989907703078));
#32233=CARTESIAN_POINT('Ctrl Pts',(-24.5071839600544,0.0153250677326657,
-23.8507766410973));
#32234=CARTESIAN_POINT('Ctrl Pts',(-24.5033609516529,0.0199682168708636,
-24.3539080326969));
#32235=CARTESIAN_POINT('Ctrl Pts',(-24.494397425932,0.0299078898256353,
-25.2349883068055));
#32236=CARTESIAN_POINT('Ctrl Pts',(-24.4769679435678,0.0476718924133547,
-26.493080401859));
#32237=CARTESIAN_POINT('Ctrl Pts',(-24.4546824689337,0.0693532016334583,
-27.9987128880141));
#32238=CARTESIAN_POINT('Ctrl Pts',(-24.4428315205947,0.0806786400363348,
-28.9969020103129));
#32239=CARTESIAN_POINT('Ctrl Pts',(-24.4381971026002,0.0851810986839638,
-29.5562517451831));
#32240=CARTESIAN_POINT('Ctrl Pts',(-24.437158111982,0.0861796630639383,
-29.6816608219294));
#32241=CARTESIAN_POINT('Ctrl Pts',(-24.4350376262919,0.0881342235921294,
-29.9318858140557));
#32242=CARTESIAN_POINT('Ctrl Pts',(-24.431243098981,0.0914552866878719,
-30.3701639510382));
#32243=CARTESIAN_POINT('Ctrl Pts',(-24.4235320523414,0.0976282111301398,
-31.2466767067308));
#32244=CARTESIAN_POINT('Ctrl Pts',(-24.4153961523886,0.103398142960177,
-32.2483511659307));
#32245=CARTESIAN_POINT('Ctrl Pts',(-24.4098556239652,0.107400651713681,
-33.2487697414918));
#32246=CARTESIAN_POINT('Ctrl Pts',(-24.407476970373,0.109398407187711,-33.9982272445929));
#32247=CARTESIAN_POINT('Ctrl Pts',(-24.407340084132,0.110290937033988,-34.7464252744325));
#32248=CARTESIAN_POINT('Ctrl Pts',(-24.4090646693321,0.110065084728235,
-35.2442253444765));
#32249=CARTESIAN_POINT('Ctrl Pts',(-24.4111627264825,0.109555550582656,
-35.6181363661944));
#32250=CARTESIAN_POINT('Ctrl Pts',(-24.4129585191794,0.109054162214716,
-35.8680609341064));
#32251=CARTESIAN_POINT('Ctrl Pts',(-24.417942569389,0.107468332881441,-36.3678457663949));
#32252=CARTESIAN_POINT('Ctrl Pts',(-24.4298882542792,0.103316258927521,
-37.2412402280608));
#32253=CARTESIAN_POINT('Ctrl Pts',(-24.4630849505217,0.0905723985382749,
-38.9871180300605));
#32254=CARTESIAN_POINT('Ctrl Pts',(-24.4953445175915,0.0759084845649608,
-40.4869183501336));
#32255=CARTESIAN_POINT('Ctrl Pts',(-24.5091123507204,0.0669078016820844,
-41.6192789458791));
#32256=CARTESIAN_POINT('Ctrl Pts',(-24.5119517950053,0.0641038462103697,
-41.8564784811102));
#32257=CARTESIAN_POINT('Ctrl Pts',(-24.5156935975892,0.0575419311246697,
-42.222261181654));
#32258=CARTESIAN_POINT('Ctrl Pts',(-24.5189923423272,0.0491744390235501,
-42.5889094138677));
#32259=CARTESIAN_POINT('Ctrl Pts',(-24.5229053335981,0.0362327533694244,
-43.0832933189361));
#32260=CARTESIAN_POINT('Ctrl Pts',(-24.5270743109208,0.0179897766914957,
-43.7085230130832));
#32261=CARTESIAN_POINT('Ctrl Pts',(-24.5315455407593,-0.00303568299465702,
-44.4709890642209));
#32262=CARTESIAN_POINT('Ctrl Pts',(-24.5353508868689,-0.0161922105588385,
-45.1156507267256));
#32263=CARTESIAN_POINT('Ctrl Pts',(-24.5387295038189,-0.0217811995201414,
-45.6371377033781));
#32264=CARTESIAN_POINT('Ctrl Pts',(-24.5415198954755,-0.0229289638506116,
-46.0308811465701));
#32265=CARTESIAN_POINT('Ctrl Pts',(-24.5446424675927,-0.0204296702137602,
-46.4272764748594));
#32266=CARTESIAN_POINT('Ctrl Pts',(-24.5493386649675,-0.0113998295332617,
-46.9592228942674));
#32267=CARTESIAN_POINT('Ctrl Pts',(-24.5536095026516,0.00267333340698166,
-47.3619485254795));
#32268=CARTESIAN_POINT('Ctrl Pts',(-24.5584966620003,0.0229773607762555,
-47.7674954424624));
#32269=CARTESIAN_POINT('Ctrl Pts',(-24.5621553335303,0.0354725859022536,
-48.0152906571207));
#32270=CARTESIAN_POINT('Ctrl Pts',(-24.5707909193746,0.0622711721228399,
-48.5281809417318));
#32271=CARTESIAN_POINT('Ctrl Pts',(-24.5887105266626,0.113497280171948,
-49.4272609544128));
#32272=CARTESIAN_POINT('Ctrl Pts',(-24.6187359609351,0.210192496210709,
-50.740361535343));
#32273=CARTESIAN_POINT('Ctrl Pts',(-24.6503243045101,0.398680573907358,
-52.3517752767282));
#32274=CARTESIAN_POINT('Ctrl Pts',(-24.6607334085916,0.59837907497145,-53.449706273352));
#32275=CARTESIAN_POINT('Ctrl Pts',(-24.6613898700266,0.75495658257339,-54.1427419081582));
#32276=CARTESIAN_POINT('Ctrl Pts',(-24.6612844713376,0.820215401011333,
-54.4191314775285));
#32277=CARTESIAN_POINT('Ctrl Pts',(-24.6594955603515,0.960978655381601,
-54.9704129351631));
#32278=CARTESIAN_POINT('Ctrl Pts',(-24.6526704548069,1.23130756620562,-55.9263760818197));
#32279=CARTESIAN_POINT('Ctrl Pts',(-24.6268775428713,1.85499360305803,-57.8066070350233));
#32280=CARTESIAN_POINT('Ctrl Pts',(-24.5937661179274,2.48615112714016,-59.3601307886181));
#32281=CARTESIAN_POINT('Ctrl Pts',(-24.5743043395494,2.94126764369053,-60.4331272568145));
#32282=CARTESIAN_POINT('Ctrl Pts',(-24.5716009404588,3.00134291718464,-60.5731555051268));
#32283=CARTESIAN_POINT('Ctrl Pts',(-24.5661071223651,3.12119743169122,-60.8463917069801));
#32284=CARTESIAN_POINT('Ctrl Pts',(-24.5558500913542,3.33727209231942,-61.3242676932214));
#32285=CARTESIAN_POINT('Ctrl Pts',(-24.5336696574173,3.78612502179004,-62.2654638944784));
#32286=CARTESIAN_POINT('Ctrl Pts',(-24.5065252373297,4.32737664175834,-63.314694069021));
#32287=CARTESIAN_POINT('Ctrl Pts',(-24.4812937594002,4.87146583166284,-64.3341137358084));
#32288=CARTESIAN_POINT('Ctrl Pts',(-24.4684022046568,5.17422033520213,-64.8960125401331));
#32289=CARTESIAN_POINT('Ctrl Pts',(-24.4606128848326,5.3727638471553,-65.265377211583));
#32290=CARTESIAN_POINT('Ctrl Pts',(-24.455653438339,5.50412132243228,-65.5101940366358));
#32291=CARTESIAN_POINT('Ctrl Pts',(-24.4510643974821,5.63382037500812,-65.7528735627069));
#32292=CARTESIAN_POINT('Ctrl Pts',(-24.4474287044718,5.74548701822204,-65.9632044442411));
#32293=CARTESIAN_POINT('Ctrl Pts',(-24.4454660639254,5.80873343716068,-66.0828078307119));
#32294=CARTESIAN_POINT('Ctrl Pts',(-24.4426410572854,5.90302204618168,-66.2616316609985));
#32295=CARTESIAN_POINT('Ctrl Pts',(-24.4405393173356,5.98032222827673,-66.4093865925176));
#32296=CARTESIAN_POINT('Ctrl Pts',(-24.4374419315558,6.10651196484111,-66.6525651721026));
#32297=CARTESIAN_POINT('Ctrl Pts',(-24.4345549187866,6.2440967110459,-66.9170042846155));
#32298=CARTESIAN_POINT('Ctrl Pts',(-24.4300637962104,6.51409741201617,-67.4333801335246));
#32299=CARTESIAN_POINT('Ctrl Pts',(-24.425168552151,6.98636377680275,-68.3305700423672));
#32300=CARTESIAN_POINT('Ctrl Pts',(-24.4246416609853,7.92087819494418,-70.0871472467393));
#32301=CARTESIAN_POINT('Ctrl Pts',(-24.4309659146112,8.71389867548645,-71.5642871099131));
#32302=CARTESIAN_POINT('Ctrl Pts',(-24.4301357399251,9.30957432990654,-72.6856843844485));
#32303=CARTESIAN_POINT('Ctrl Pts',(-24.4299759003447,9.44326321325677,-72.9373360128412));
#32304=CARTESIAN_POINT('Ctrl Pts',(-24.4297382797287,9.71004184609948,-73.4393965823722));
#32305=CARTESIAN_POINT('Ctrl Pts',(-24.4295787141261,10.0436707306615,-74.0670696937808));
#32306=CARTESIAN_POINT('Ctrl Pts',(-24.4295603802771,10.4437552277089,-74.8195394237861));
#32307=CARTESIAN_POINT('Ctrl Pts',(-24.429763590671,11.2438033081569,-76.323923224447));
#32308=CARTESIAN_POINT('Ctrl Pts',(-24.4302109127262,11.9102911176329,-77.5767536096995));
#32309=CARTESIAN_POINT('Ctrl Pts',(-24.4302054054525,12.8800006302382,-79.4004972959445));
#32310=CARTESIAN_POINT('Ctrl Pts',(-24.4302025491906,13.3166339961519,-80.2216776786048));
#32311=CARTESIAN_POINT('Ctrl Pts',(-24.4302025491907,13.7531555835413,-81.0426553807033));
#32312=CARTESIAN_POINT('Ctrl Pts',(-21.9279465977811,0.00175951622296883,
24.8306324554501));
#32313=CARTESIAN_POINT('Ctrl Pts',(-21.9280121170153,0.00175964344790449,
24.781753071759));
#32314=CARTESIAN_POINT('Ctrl Pts',(-21.9280808293462,0.00175977781990619,
24.7328747382815));
#32315=CARTESIAN_POINT('Ctrl Pts',(-21.92889238123,0.00176131782851828,
24.1822659030951));
#32316=CARTESIAN_POINT('Ctrl Pts',(-21.9295158979077,0.00176336457478976,
23.1781303380483));
#32317=CARTESIAN_POINT('Ctrl Pts',(-21.9309656870421,0.00176950496491764,
21.1695302130375));
#32318=CARTESIAN_POINT('Ctrl Pts',(-21.9363681073529,0.00177920907406832,
19.6653789377107));
#32319=CARTESIAN_POINT('Ctrl Pts',(-21.9478185541189,0.00179538797735874,
18.4143308425655));
#32320=CARTESIAN_POINT('Ctrl Pts',(-21.9533099655257,0.00180374455169626,
17.9115099719552));
#32321=CARTESIAN_POINT('Ctrl Pts',(-21.9670999905151,0.00182548904108017,
16.9075176911551));
#32322=CARTESIAN_POINT('Ctrl Pts',(-21.9966773686041,0.00187213302403837,
15.1537079278605));
#32323=CARTESIAN_POINT('Ctrl Pts',(-22.0247784148631,0.00190770551231591,
13.651983107781));
#32324=CARTESIAN_POINT('Ctrl Pts',(-22.0423878964479,0.00191697506843397,
12.3975281756335));
#32325=CARTESIAN_POINT('Ctrl Pts',(-22.0495852477736,0.00191946799397687,
11.8965814801248));
#32326=CARTESIAN_POINT('Ctrl Pts',(-22.0642572378507,0.00191940508346344,
10.8947480143028));
#32327=CARTESIAN_POINT('Ctrl Pts',(-22.0896457188007,0.00190964450556511,
9.14122391316817));
#32328=CARTESIAN_POINT('Ctrl Pts',(-22.1074723723614,0.0018880970889791,
7.63599689309631));
#32329=CARTESIAN_POINT('Ctrl Pts',(-22.1153910834707,0.00187742024493833,
6.50508897037416));
#32330=CARTESIAN_POINT('Ctrl Pts',(-22.1170806542096,0.00183745708476382,
6.25535887539741));
#32331=CARTESIAN_POINT('Ctrl Pts',(-22.1202010397395,0.00163413418158526,
5.7547810784773));
#32332=CARTESIAN_POINT('Ctrl Pts',(-22.1249365315808,0.00102700920702048,
4.87705708893644));
#32333=CARTESIAN_POINT('Ctrl Pts',(-22.1310631764226,-0.000586504213302211,
3.11639638920408));
#32334=CARTESIAN_POINT('Ctrl Pts',(-22.1292472805707,-0.000624428257233562,
1.60666654112928));
#32335=CARTESIAN_POINT('Ctrl Pts',(-22.1232338886141,0.00196592706724001,
0.543614270522805));
#32336=CARTESIAN_POINT('Ctrl Pts',(-22.1224468642436,0.00230434065417858,
0.41680611961292));
#32337=CARTESIAN_POINT('Ctrl Pts',(-22.1206195413777,0.00308485495392856,
0.163585690488821));
#32338=CARTESIAN_POINT('Ctrl Pts',(-22.1167890626131,0.00470887143392074,
-0.278924031202465));
#32339=CARTESIAN_POINT('Ctrl Pts',(-22.1097491817296,0.00765941886444899,
-0.909217618427138));
#32340=CARTESIAN_POINT('Ctrl Pts',(-22.099434434,0.0119006843220359,-1.66311655997141));
#32341=CARTESIAN_POINT('Ctrl Pts',(-22.0841832508903,0.0180424043540248,
-2.66563404729465));
#32342=CARTESIAN_POINT('Ctrl Pts',(-22.0639466303909,0.0258459431950208,
-3.91493137792277));
#32343=CARTESIAN_POINT('Ctrl Pts',(-22.0502884904995,0.0304341271802674,
-4.91271788975723));
#32344=CARTESIAN_POINT('Ctrl Pts',(-22.0436783572246,0.0322449760248729,
-5.53670268338412));
#32345=CARTESIAN_POINT('Ctrl Pts',(-22.0410867838493,0.0329253083784759,
-5.78724516906531));
#32346=CARTESIAN_POINT('Ctrl Pts',(-22.0361114300666,0.0340915037912527,
-6.28827188597159));
#32347=CARTESIAN_POINT('Ctrl Pts',(-22.027930623879,0.0356660657653625,
-7.16603921623362));
#32348=CARTESIAN_POINT('Ctrl Pts',(-22.017585062098,0.0367750778497687,
-8.42096472119512));
#32349=CARTESIAN_POINT('Ctrl Pts',(-22.0085785512836,0.0369101653247734,
-9.67464069070803));
#32350=CARTESIAN_POINT('Ctrl Pts',(-22.0027354354742,0.0367827534589613,
-10.5500380438823));
#32351=CARTESIAN_POINT('Ctrl Pts',(-21.9994999796009,0.036687215795415,
-11.0494463898198));
#32352=CARTESIAN_POINT('Ctrl Pts',(-21.9979116395995,0.0366384598287954,
-11.2988436135343));
#32353=CARTESIAN_POINT('Ctrl Pts',(-21.9967239254123,0.0366042714378169,
-11.4865372190639));
#32354=CARTESIAN_POINT('Ctrl Pts',(-21.995920574385,0.0365690242444882,
-11.6122999921727));
#32355=CARTESIAN_POINT('Ctrl Pts',(-21.9942994172464,0.036453560970677,
-11.8637724354554));
#32356=CARTESIAN_POINT('Ctrl Pts',(-21.9914369892605,0.0361403869370173,
-12.3031537286525));
#32357=CARTESIAN_POINT('Ctrl Pts',(-21.9840608742727,0.0348460947202343,
-13.430502857113));
#32358=CARTESIAN_POINT('Ctrl Pts',(-21.9764939645097,0.0324567970781609,
-14.6784689813424));
#32359=CARTESIAN_POINT('Ctrl Pts',(-21.9715831482783,0.0305970299247923,
-15.9308156393427));
#32360=CARTESIAN_POINT('Ctrl Pts',(-21.9699662011677,0.0299202348326696,
-16.5588078732846));
#32361=CARTESIAN_POINT('Ctrl Pts',(-21.9692791158919,0.0296011100378451,
-17.0627381988692));
#32362=CARTESIAN_POINT('Ctrl Pts',(-21.969153381612,0.0295292129838952,
-17.3152951382543));
#32363=CARTESIAN_POINT('Ctrl Pts',(-21.9691483617438,0.0295116738601406,
-17.5041552476115));
#32364=CARTESIAN_POINT('Ctrl Pts',(-21.96916733847,0.0294900157658974,-17.6283858382307));
#32365=CARTESIAN_POINT('Ctrl Pts',(-21.9692943053054,0.0294045671680399,
-17.8773833116316));
#32366=CARTESIAN_POINT('Ctrl Pts',(-21.9695468595739,0.0292701391130193,
-18.1264625823667));
#32367=CARTESIAN_POINT('Ctrl Pts',(-21.9699270373279,0.0290973238702737,
-18.3758457729672));
#32368=CARTESIAN_POINT('Ctrl Pts',(-21.97021437127,0.0289788704117424,-18.5317897716106));
#32369=CARTESIAN_POINT('Ctrl Pts',(-21.9704745061476,0.0288790791668411,
-18.6566094709869));
#32370=CARTESIAN_POINT('Ctrl Pts',(-21.9707547161318,0.0287766287899759,
-18.7814662301224));
#32371=CARTESIAN_POINT('Ctrl Pts',(-21.9715975974669,0.0284937059708799,
-19.124987759595));
#32372=CARTESIAN_POINT('Ctrl Pts',(-21.9734082967844,0.0280234505304098,
-19.6880028128856));
#32373=CARTESIAN_POINT('Ctrl Pts',(-21.9776629528484,0.0275971656286527,
-20.6915562006487));
#32374=CARTESIAN_POINT('Ctrl Pts',(-21.9848932360202,0.0284341672262077,
-21.9510748950649));
#32375=CARTESIAN_POINT('Ctrl Pts',(-21.9920427959345,0.0322868659644219,
-22.9644653051218));
#32376=CARTESIAN_POINT('Ctrl Pts',(-21.9968786544342,0.0361029476538094,
-23.5980019232506));
#32377=CARTESIAN_POINT('Ctrl Pts',(-21.9989557767391,0.0378167863464522,
-23.849607605715));
#32378=CARTESIAN_POINT('Ctrl Pts',(-22.0036228945842,0.041998979988164,
-24.3525147490087));
#32379=CARTESIAN_POINT('Ctrl Pts',(-22.0129828236567,0.0510204938530624,
-25.2333101457441));
#32380=CARTESIAN_POINT('Ctrl Pts',(-22.0284157293752,0.0674214893682064,
-26.4913997422044));
#32381=CARTESIAN_POINT('Ctrl Pts',(-22.0470780687344,0.0877279468049168,
-27.9975063885432));
#32382=CARTESIAN_POINT('Ctrl Pts',(-22.0569039621362,0.098625472528748,
-28.9962578683356));
#32383=CARTESIAN_POINT('Ctrl Pts',(-22.061123162479,0.103028053224532,-29.5559979397897));
#32384=CARTESIAN_POINT('Ctrl Pts',(-22.0620360130022,0.104005175649616,
-29.6816094949658));
#32385=CARTESIAN_POINT('Ctrl Pts',(-22.063733901438,0.105945232381167,-29.9321457064587));
#32386=CARTESIAN_POINT('Ctrl Pts',(-22.0663793393813,0.109304486647811,
-30.3709342542632));
#32387=CARTESIAN_POINT('Ctrl Pts',(-22.0705750456291,0.115762611980201,
-31.2481658337376));
#32388=CARTESIAN_POINT('Ctrl Pts',(-22.0735587465917,0.122130800122623,
-32.2500012284327));
#32389=CARTESIAN_POINT('Ctrl Pts',(-22.0763008034624,0.126640527630062,
-33.2498713812575));
#32390=CARTESIAN_POINT('Ctrl Pts',(-22.0786225028573,0.128886482354336,
-33.9985658158203));
#32391=CARTESIAN_POINT('Ctrl Pts',(-22.0815007275582,0.129824944286313,
-34.7456311160509));
#32392=CARTESIAN_POINT('Ctrl Pts',(-22.0840662047962,0.129436579270529,
-35.2424402794722));
#32393=CARTESIAN_POINT('Ctrl Pts',(-22.0863382225049,0.128717640802482,
-35.6155133325656));
#32394=CARTESIAN_POINT('Ctrl Pts',(-22.0880810035669,0.128037969530672,
-35.8646198141343));
#32395=CARTESIAN_POINT('Ctrl Pts',(-22.0922926297467,0.125949254046027,
-36.3631591269725));
#32396=CARTESIAN_POINT('Ctrl Pts',(-22.1011590699198,0.120534929666342,
-37.2348392323456));
#32397=CARTESIAN_POINT('Ctrl Pts',(-22.1219758473207,0.10447665392804,-38.9797400897251));
#32398=CARTESIAN_POINT('Ctrl Pts',(-22.1351457038762,0.086800106356149,
-40.4823985574855));
#32399=CARTESIAN_POINT('Ctrl Pts',(-22.1325839123372,0.0773464135856958,
-41.6183954976229));
#32400=CARTESIAN_POINT('Ctrl Pts',(-22.1318279488977,0.074521697206918,
-41.856276485494));
#32401=CARTESIAN_POINT('Ctrl Pts',(-22.1301651456598,0.0680399957608525,
-42.222979159865));
#32402=CARTESIAN_POINT('Ctrl Pts',(-22.127982690836,0.0598733749880051,
-42.5903995515794));
#32403=CARTESIAN_POINT('Ctrl Pts',(-22.1244120000825,0.0473241374375181,
-43.0856421099198));
#32404=CARTESIAN_POINT('Ctrl Pts',(-22.1187339509867,0.0297859917647642,
-43.7116175102801));
#32405=CARTESIAN_POINT('Ctrl Pts',(-22.1101180735002,0.00980274759246461,
-44.4744759591554));
#32406=CARTESIAN_POINT('Ctrl Pts',(-22.1015488286281,-0.00245109850784833,
-45.1190547033691));
#32407=CARTESIAN_POINT('Ctrl Pts',(-22.0938461907087,-0.00732163858416031,
-45.6402470682028));
#32408=CARTESIAN_POINT('Ctrl Pts',(-22.0876997960238,-0.00798116879003842,
-46.0336530958471));
#32409=CARTESIAN_POINT('Ctrl Pts',(-22.0811966447842,-0.00506200183720292,
-46.42959582729));
#32410=CARTESIAN_POINT('Ctrl Pts',(-22.0720393034145,0.00442485698173024,
-46.9607970498843));
#32411=CARTESIAN_POINT('Ctrl Pts',(-22.0647624157281,0.0186330222264071,
-47.3627877957541));
#32412=CARTESIAN_POINT('Ctrl Pts',(-22.0571129555406,0.0389521252813495,
-47.7675399696603));
#32413=CARTESIAN_POINT('Ctrl Pts',(-22.0515225047895,0.0515088587977791,
-48.0159301973195));
#32414=CARTESIAN_POINT('Ctrl Pts',(-22.0387634523023,0.0785805657956414,
-48.5291621989758));
#32415=CARTESIAN_POINT('Ctrl Pts',(-22.0129658748973,0.130648390847141,
-49.4286561122732));
#32416=CARTESIAN_POINT('Ctrl Pts',(-21.9702800819051,0.229437488371507,
-50.7405595922032));
#32417=CARTESIAN_POINT('Ctrl Pts',(-21.9214343424393,0.419726202256797,
-52.3470454894489));
#32418=CARTESIAN_POINT('Ctrl Pts',(-21.898911774298,0.616568864009376,-53.4393474162767));
#32419=CARTESIAN_POINT('Ctrl Pts',(-21.8902388128371,0.768961070459955,
-54.128571033495));
#32420=CARTESIAN_POINT('Ctrl Pts',(-21.8869634548092,0.831824753648006,
-54.401827475866));
#32421=CARTESIAN_POINT('Ctrl Pts',(-21.8815941860788,0.966965310402138,
-54.9488620484349));
#32422=CARTESIAN_POINT('Ctrl Pts',(-21.8749151942011,1.22522399032231,-55.8993882470461));
#32423=CARTESIAN_POINT('Ctrl Pts',(-21.8703887781199,1.82095337687199,-57.7787441431066));
#32424=CARTESIAN_POINT('Ctrl Pts',(-21.8751637879929,2.43617689572333,-59.3440137893041));
#32425=CARTESIAN_POINT('Ctrl Pts',(-21.8779292841487,2.89418131546219,-60.4294964038471));
#32426=CARTESIAN_POINT('Ctrl Pts',(-21.8784919227777,2.95453939264026,-60.570781472954));
#32427=CARTESIAN_POINT('Ctrl Pts',(-21.8797312083696,3.07529745046665,-60.8464556959951));
#32428=CARTESIAN_POINT('Ctrl Pts',(-21.8824452933382,3.29355533259279,-61.3280540237837));
#32429=CARTESIAN_POINT('Ctrl Pts',(-21.8895449231649,3.74887633727324,-62.274937263336));
#32430=CARTESIAN_POINT('Ctrl Pts',(-21.9001371399266,4.3004097935474,-63.3272029625683));
#32431=CARTESIAN_POINT('Ctrl Pts',(-21.9107842226101,4.85424205636823,-64.3470411142037));
#32432=CARTESIAN_POINT('Ctrl Pts',(-21.916354209389,5.16169784818111,-64.9082123410851));
#32433=CARTESIAN_POINT('Ctrl Pts',(-21.9196919975189,5.36282079275618,-65.2766897005441));
#32434=CARTESIAN_POINT('Ctrl Pts',(-21.921808591829,5.49572942117165,-65.5208032178986));
#32435=CARTESIAN_POINT('Ctrl Pts',(-21.9237231005401,5.62672574373137,-65.7626107899648));
#32436=CARTESIAN_POINT('Ctrl Pts',(-21.9252038876219,5.73924436353136,-65.9720206725958));
#32437=CARTESIAN_POINT('Ctrl Pts',(-21.9259867036262,5.80289378805119,-66.0910507820888));
#32438=CARTESIAN_POINT('Ctrl Pts',(-21.9270959306165,5.89769989954532,-66.268968124062));
#32439=CARTESIAN_POINT('Ctrl Pts',(-21.92787046439,5.97524992867064,-66.4158616225611));
#32440=CARTESIAN_POINT('Ctrl Pts',(-21.928940083139,6.1015843192719,-66.657495581125));
#32441=CARTESIAN_POINT('Ctrl Pts',(-21.9298881234652,6.24001972444046,-66.9217149445331));
#32442=CARTESIAN_POINT('Ctrl Pts',(-21.9312815177686,6.51102410622419,-67.4369602737428));
#32443=CARTESIAN_POINT('Ctrl Pts',(-21.9324876222294,6.98469072279545,-68.3327696709343));
#32444=CARTESIAN_POINT('Ctrl Pts',(-21.9312406243433,7.92002328406678,-70.0871946567983));
#32445=CARTESIAN_POINT('Ctrl Pts',(-21.9276469013653,8.71290538373861,-71.5643646538029));
#32446=CARTESIAN_POINT('Ctrl Pts',(-21.9275638685428,9.30971569874061,-72.6865383203896));
#32447=CARTESIAN_POINT('Ctrl Pts',(-21.9275520227615,9.44341875895882,-72.9379611812549));
#32448=CARTESIAN_POINT('Ctrl Pts',(-21.9275331342995,9.71029529116342,-73.439824462405));
#32449=CARTESIAN_POINT('Ctrl Pts',(-21.9275143845236,10.0439103544011,-74.0672059355723));
#32450=CARTESIAN_POINT('Ctrl Pts',(-21.9275097575012,10.4438969252603,-74.8194571285693));
#32451=CARTESIAN_POINT('Ctrl Pts',(-21.9275180953303,11.2436125671748,-76.3235296670018));
#32452=CARTESIAN_POINT('Ctrl Pts',(-21.9275251403254,11.909792269642,-77.5764539148375));
#32453=CARTESIAN_POINT('Ctrl Pts',(-21.9275097517017,12.8797558916182,-79.4006430631371));
#32454=CARTESIAN_POINT('Ctrl Pts',(-21.9275018204326,13.3163203389153,-80.2216771291613));
#32455=CARTESIAN_POINT('Ctrl Pts',(-21.9275018204325,13.7528419263048,-81.0426548312598));
#32456=CARTESIAN_POINT('Ctrl Pts',(-19.4210619460671,-0.000916505951998524,
24.8306358879637));
#32457=CARTESIAN_POINT('Ctrl Pts',(-19.4211200360562,-0.000916505829417001,
24.7817566113921));
#32458=CARTESIAN_POINT('Ctrl Pts',(-19.4211809608811,-0.000916508832693608,
24.7328783890003));
#32459=CARTESIAN_POINT('Ctrl Pts',(-19.4219003643249,-0.000916399674711829,
24.1822707423388));
#32460=CARTESIAN_POINT('Ctrl Pts',(-19.4224514915254,-0.000916151011694828,
23.1781361925135));
#32461=CARTESIAN_POINT('Ctrl Pts',(-19.4237349522675,-0.000917980264369305,
21.1695382470795));
#32462=CARTESIAN_POINT('Ctrl Pts',(-19.4285220752422,-0.000915706084191834,
19.6653858677669));
#32463=CARTESIAN_POINT('Ctrl Pts',(-19.4386760515693,-0.000911420001045353,
18.4143371794428));
#32464=CARTESIAN_POINT('Ctrl Pts',(-19.4435460762392,-0.000909876636940407,
17.9115228552616));
#32465=CARTESIAN_POINT('Ctrl Pts',(-19.4557752214484,-0.000906076814717268,
16.9075348604225));
#32466=CARTESIAN_POINT('Ctrl Pts',(-19.482006160143,-0.000898354421432531,
15.1537241714337));
#32467=CARTESIAN_POINT('Ctrl Pts',(-19.5069222841565,-0.000883362688828362,
13.6519746322136));
#32468=CARTESIAN_POINT('Ctrl Pts',(-19.5225393837494,-0.000868771700885713,
12.397489885296));
#32469=CARTESIAN_POINT('Ctrl Pts',(-19.5289239036206,-0.000862754752594793,
11.8965312672799));
#32470=CARTESIAN_POINT('Ctrl Pts',(-19.5419385856058,-0.000847400333427081,
10.894680435061));
#32471=CARTESIAN_POINT('Ctrl Pts',(-19.5644638714673,-0.000817476897641216,
9.14113732412567));
#32472=CARTESIAN_POINT('Ctrl Pts',(-19.580257867826,-0.000779847760490609,
7.63591652937965));
#32473=CARTESIAN_POINT('Ctrl Pts',(-19.5872721615326,-0.00076358859827383,
6.50500747984503));
#32474=CARTESIAN_POINT('Ctrl Pts',(-19.5886972281251,-0.000782736056155837,
6.25506299062874));
#32475=CARTESIAN_POINT('Ctrl Pts',(-19.5910800027927,-0.000892230357137512,
5.7542530427598));
#32476=CARTESIAN_POINT('Ctrl Pts',(-19.5941198555159,-0.00122168871274602,
4.87623338232857));
#32477=CARTESIAN_POINT('Ctrl Pts',(-19.5964733422871,-0.0021199224373692,
3.1157476232137));
#32478=CARTESIAN_POINT('Ctrl Pts',(-19.5947716363984,-0.00205443966891327,
1.60737716484397));
#32479=CARTESIAN_POINT('Ctrl Pts',(-19.5943674949496,-0.000605263955023937,
0.545854015138203));
#32480=CARTESIAN_POINT('Ctrl Pts',(-19.5943137164219,-0.000421092946140771,
0.419298119551482));
#32481=CARTESIAN_POINT('Ctrl Pts',(-19.5941782922409,9.22222472031788E-6,
0.166505185772947));
#32482=CARTESIAN_POINT('Ctrl Pts',(-19.5938698855079,0.000905763389535935,
-0.275321494516036));
#32483=CARTESIAN_POINT('Ctrl Pts',(-19.5932146204517,0.00255021532002368,
-0.904904183802462));
#32484=CARTESIAN_POINT('Ctrl Pts',(-19.5921048641433,0.00486262550340788,
-1.65833181536422));
#32485=CARTESIAN_POINT('Ctrl Pts',(-19.590178420896,0.00818343368721628,
-2.66069903279666));
#32486=CARTESIAN_POINT('Ctrl Pts',(-19.587000103224,0.0122365579874156,
-3.91061817196258));
#32487=CARTESIAN_POINT('Ctrl Pts',(-19.5836302092038,0.0145300342991261,
-4.90966274692559));
#32488=CARTESIAN_POINT('Ctrl Pts',(-19.5812386079632,0.015367054816335,
-5.53462804813499));
#32489=CARTESIAN_POINT('Ctrl Pts',(-19.5802022899887,0.0156483145176531,
-5.78514459578171));
#32490=CARTESIAN_POINT('Ctrl Pts',(-19.5778668906237,0.0160679382836999,
-6.28637862974742));
#32491=CARTESIAN_POINT('Ctrl Pts',(-19.5731682577045,0.0164580977986604,
-7.16443891094301));
#32492=CARTESIAN_POINT('Ctrl Pts',(-19.5652302476183,0.0162972237888366,
-8.42002258121338));
#32493=CARTESIAN_POINT('Ctrl Pts',(-19.557064496691,0.0158192131697322,
-9.67455998065912));
#32494=CARTESIAN_POINT('Ctrl Pts',(-19.5519697806829,0.0156446112291823,
-10.5507139521068));
#32495=CARTESIAN_POINT('Ctrl Pts',(-19.549338791014,0.0156404148149878,
-11.050593627762));
#32496=CARTESIAN_POINT('Ctrl Pts',(-19.5481338881641,0.0156781632889342,
-11.3002387949875));
#32497=CARTESIAN_POINT('Ctrl Pts',(-19.5472749165968,0.0157242021426955,
-11.488131352607));
#32498=CARTESIAN_POINT('Ctrl Pts',(-19.546695715977,0.0157584682458296,
-11.6142688933052));
#32499=CARTESIAN_POINT('Ctrl Pts',(-19.5455310250035,0.0158376730394181,
-11.8663068121108));
#32500=CARTESIAN_POINT('Ctrl Pts',(-19.5434825830314,0.0160038830033236,
-12.3066351073796));
#32501=CARTESIAN_POINT('Ctrl Pts',(-19.5382292295015,0.0165498799783075,
-13.4357721193144));
#32502=CARTESIAN_POINT('Ctrl Pts',(-19.5328369824923,0.01736958990664,-14.6839651499632));
#32503=CARTESIAN_POINT('Ctrl Pts',(-19.5291128862856,0.0179736079118189,
-15.9347209983996));
#32504=CARTESIAN_POINT('Ctrl Pts',(-19.527763502,0.0181925712051342,-16.561478567343));
#32505=CARTESIAN_POINT('Ctrl Pts',(-19.5270563863637,0.0182932341679571,
-17.0641679158956));
#32506=CARTESIAN_POINT('Ctrl Pts',(-19.526835967203,0.0183163694167679,
-17.3160098089783));
#32507=CARTESIAN_POINT('Ctrl Pts',(-19.5267251826946,0.0183219158333973,
-17.504332176674));
#32508=CARTESIAN_POINT('Ctrl Pts',(-19.5266621148149,0.0183306924441913,
-17.6291328941662));
#32509=CARTESIAN_POINT('Ctrl Pts',(-19.5265769037342,0.0183696641094957,
-17.878620482306));
#32510=CARTESIAN_POINT('Ctrl Pts',(-19.5265537745837,0.0184355791817818,
-18.1282475743827));
#32511=CARTESIAN_POINT('Ctrl Pts',(-19.5265933327143,0.0185212039296075,
-18.3779283557147));
#32512=CARTESIAN_POINT('Ctrl Pts',(-19.5266445208543,0.0185809757856958,
-18.5340216452474));
#32513=CARTESIAN_POINT('Ctrl Pts',(-19.5267013915317,0.0186316683340416,
-18.6589159726346));
#32514=CARTESIAN_POINT('Ctrl Pts',(-19.5267686767785,0.018684079673204,
-18.7838261805894));
#32515=CARTESIAN_POINT('Ctrl Pts',(-19.5270008023804,0.018830814209969,
-19.1273876797336));
#32516=CARTESIAN_POINT('Ctrl Pts',(-19.5276179635945,0.0190852158251253,
-19.6899274884205));
#32517=CARTESIAN_POINT('Ctrl Pts',(-19.5294557494281,0.019370063550402,
-20.691048800915));
#32518=CARTESIAN_POINT('Ctrl Pts',(-19.5330639946868,0.0191287867613026,
-21.9446352642524));
#32519=CARTESIAN_POINT('Ctrl Pts',(-19.5375547434322,0.0174801796606266,
-22.9501448874616));
#32520=CARTESIAN_POINT('Ctrl Pts',(-19.5408112124324,0.0158055036722608,
-23.5777955722769));
#32521=CARTESIAN_POINT('Ctrl Pts',(-19.5422114714015,0.0150511106350368,
-23.8258589230651));
#32522=CARTESIAN_POINT('Ctrl Pts',(-19.5454469135472,0.013207219676755,
-24.3232982958536));
#32523=CARTESIAN_POINT('Ctrl Pts',(-19.5520791800536,0.00922621734496209,
-25.1962301250459));
#32524=CARTESIAN_POINT('Ctrl Pts',(-19.5636214428665,0.00206128376255883,
-26.4493421322969));
#32525=CARTESIAN_POINT('Ctrl Pts',(-19.5778196153715,-0.00664813705533941,
-27.9588536438995));
#32526=CARTESIAN_POINT('Ctrl Pts',(-19.5858724946287,-0.0111975382757344,
-28.9664156053144));
#32527=CARTESIAN_POINT('Ctrl Pts',(-19.5894199088021,-0.0130148584392199,
-29.5328122940666));
#32528=CARTESIAN_POINT('Ctrl Pts',(-19.5901963882779,-0.0134115298228288,
-29.6583647772461));
#32529=CARTESIAN_POINT('Ctrl Pts',(-19.5917246464236,-0.0141634489634931,
-29.9096808259213));
#32530=CARTESIAN_POINT('Ctrl Pts',(-19.5943400924366,-0.0153825265994865,
-30.3494739152574));
#32531=CARTESIAN_POINT('Ctrl Pts',(-19.59930001926,-0.017452777268995,-31.2293526898474));
#32532=CARTESIAN_POINT('Ctrl Pts',(-19.6043489049884,-0.0191261396280685,
-32.2347494206712));
#32533=CARTESIAN_POINT('Ctrl Pts',(-19.6086516849793,-0.0204363624778105,
-33.2389780365613));
#32534=CARTESIAN_POINT('Ctrl Pts',(-19.6114742352471,-0.0213296337544048,
-33.9912721629546));
#32535=CARTESIAN_POINT('Ctrl Pts',(-19.6139183172787,-0.0222359159331191,
-34.7423334052815));
#32536=CARTESIAN_POINT('Ctrl Pts',(-19.6152624456389,-0.0229101368754363,
-35.2420615653454));
#32537=CARTESIAN_POINT('Ctrl Pts',(-19.6161576020686,-0.0234681565954076,
-35.6174351663918));
#32538=CARTESIAN_POINT('Ctrl Pts',(-19.6167566587891,-0.0239017902451974,
-35.8683357370975));
#32539=CARTESIAN_POINT('Ctrl Pts',(-19.6179540719398,-0.0249342552168865,
-36.370103134513));
#32540=CARTESIAN_POINT('Ctrl Pts',(-19.6199848251125,-0.0270541396195468,
-37.2470687416748));
#32541=CARTESIAN_POINT('Ctrl Pts',(-19.623233273403,-0.0317230467432112,
-39.00028772146));
#32542=CARTESIAN_POINT('Ctrl Pts',(-19.6222297610433,-0.0331281923398602,
-40.5063468964214));
#32543=CARTESIAN_POINT('Ctrl Pts',(-19.617501610984,-0.029738409662969,
-41.6423833562812));
#32544=CARTESIAN_POINT('Ctrl Pts',(-19.6164284597141,-0.0299257028766041,
-41.8800353799142));
#32545=CARTESIAN_POINT('Ctrl Pts',(-19.6146902487838,-0.0323119462871963,
-42.246776723759));
#32546=CARTESIAN_POINT('Ctrl Pts',(-19.6128111946042,-0.0363403388279717,
-42.6144158763));
#32547=CARTESIAN_POINT('Ctrl Pts',(-19.6100854265847,-0.0431877514880426,
-43.1103019468172));
#32548=CARTESIAN_POINT('Ctrl Pts',(-19.6062259946451,-0.0532162990883177,
-43.7376670054504));
#32549=CARTESIAN_POINT('Ctrl Pts',(-19.6006968468197,-0.063196357447491,
-44.5031764047218));
#32550=CARTESIAN_POINT('Ctrl Pts',(-19.5951934401697,-0.0659653604278103,
-45.1507878703742));
#32551=CARTESIAN_POINT('Ctrl Pts',(-19.5902116566121,-0.0624520398921263,
-45.6748227179991));
#32552=CARTESIAN_POINT('Ctrl Pts',(-19.5861424054888,-0.0563207359842689,
-46.0706039170931));
#32553=CARTESIAN_POINT('Ctrl Pts',(-19.581721807771,-0.0460566055141686,
-46.469146416803));
#32554=CARTESIAN_POINT('Ctrl Pts',(-19.575351012063,-0.0260000737641728,
-47.0041046909466));
#32555=CARTESIAN_POINT('Ctrl Pts',(-19.5699477020232,-0.00276787019770777,
-47.4092388334075));
#32556=CARTESIAN_POINT('Ctrl Pts',(-19.5641458342478,0.0273068266469621,
-47.8174344977143));
#32557=CARTESIAN_POINT('Ctrl Pts',(-19.5599406370288,0.0468609417018277,
-48.0730561138821));
#32558=CARTESIAN_POINT('Ctrl Pts',(-19.5503695770238,0.0900955080363308,
-48.5957398962124));
#32559=CARTESIAN_POINT('Ctrl Pts',(-19.531042785612,0.174928325946335,-49.5082382959596));
#32560=CARTESIAN_POINT('Ctrl Pts',(-19.4985615237133,0.327996612663541,
-50.8231236678266));
#32561=CARTESIAN_POINT('Ctrl Pts',(-19.4604047596137,0.575748356626434,
-52.4111165545092));
#32562=CARTESIAN_POINT('Ctrl Pts',(-19.4406878844852,0.792935696991215,
-53.4767992959842));
#32563=CARTESIAN_POINT('Ctrl Pts',(-19.4317522726001,0.948041883886683,
-54.1457388948874));
#32564=CARTESIAN_POINT('Ctrl Pts',(-19.4282772934766,1.01183076778066,-54.4134605162196));
#32565=CARTESIAN_POINT('Ctrl Pts',(-19.4218630286443,1.14625404644578,-54.949384838544));
#32566=CARTESIAN_POINT('Ctrl Pts',(-19.4119486847664,1.39806011300074,-55.8843438780089));
#32567=CARTESIAN_POINT('Ctrl Pts',(-19.3970680007187,1.96484144832662,-57.7440060585629));
#32568=CARTESIAN_POINT('Ctrl Pts',(-19.3915395103084,2.54557848517724,-59.311537388298));
#32569=CARTESIAN_POINT('Ctrl Pts',(-19.3902776363852,2.99144062937233,-60.4060886231981));
#32570=CARTESIAN_POINT('Ctrl Pts',(-19.3902371034511,3.04914363192602,-60.5460390725025));
#32571=CARTESIAN_POINT('Ctrl Pts',(-19.3903364333557,3.165067562148,-60.820610591561));
#32572=CARTESIAN_POINT('Ctrl Pts',(-19.391050624363,3.37413960864631,-61.2999999169842));
#32573=CARTESIAN_POINT('Ctrl Pts',(-19.3942701404576,3.81025112716761,-62.244556982017));
#32574=CARTESIAN_POINT('Ctrl Pts',(-19.4008744605687,4.33894413365338,-63.2968001570556));
#32575=CARTESIAN_POINT('Ctrl Pts',(-19.408032994212,4.87295933801209,-64.3191518232226));
#32576=CARTESIAN_POINT('Ctrl Pts',(-19.4118534041911,5.17099277029054,-64.8826381760206));
#32577=CARTESIAN_POINT('Ctrl Pts',(-19.414138409824,5.36680743778216,-65.2530842010791));
#32578=CARTESIAN_POINT('Ctrl Pts',(-19.4155782054507,5.49646259973421,-65.4986251742135));
#32579=CARTESIAN_POINT('Ctrl Pts',(-19.4168834240223,5.62461885273898,-65.7420455204344));
#32580=CARTESIAN_POINT('Ctrl Pts',(-19.4178675237502,5.73509674141069,-65.9530362578082));
#32581=CARTESIAN_POINT('Ctrl Pts',(-19.4183812835749,5.7977079991849,-66.0730215724873));
#32582=CARTESIAN_POINT('Ctrl Pts',(-19.419100544842,5.89108965768411,-66.2524240198914));
#32583=CARTESIAN_POINT('Ctrl Pts',(-19.4195923407601,5.96772063530916,-66.4006740118791));
#32584=CARTESIAN_POINT('Ctrl Pts',(-19.4202302030272,6.09294374601363,-66.6447083575439));
#32585=CARTESIAN_POINT('Ctrl Pts',(-19.420811048886,6.23015025712785,-66.9109507681786));
#32586=CARTESIAN_POINT('Ctrl Pts',(-19.4216849945587,6.49984220861854,-67.4300688672473));
#32587=CARTESIAN_POINT('Ctrl Pts',(-19.4225561721023,6.9732157016267,-68.331546792137));
#32588=CARTESIAN_POINT('Ctrl Pts',(-19.4222665935473,7.91403700035587,-70.0931374115175));
#32589=CARTESIAN_POINT('Ctrl Pts',(-19.4206541084763,8.71289353145056,-71.5687521510131));
#32590=CARTESIAN_POINT('Ctrl Pts',(-19.4207401430524,9.30691320802472,-72.6860330122269));
#32591=CARTESIAN_POINT('Ctrl Pts',(-19.4207537005546,9.44077794422047,-72.9378075977793));
#32592=CARTESIAN_POINT('Ctrl Pts',(-19.4207750104813,9.70754452589275,-73.4395419598208));
#32593=CARTESIAN_POINT('Ctrl Pts',(-19.4207918757636,10.0412095495097,-74.0670948518826));
#32594=CARTESIAN_POINT('Ctrl Pts',(-19.4207949784166,10.4411892601614,-74.8193526804547));
#32595=CARTESIAN_POINT('Ctrl Pts',(-19.4207803986868,11.2409741801607,-76.3235224409878));
#32596=CARTESIAN_POINT('Ctrl Pts',(-19.4207534481394,11.9071720009682,-77.5764574158514));
#32597=CARTESIAN_POINT('Ctrl Pts',(-19.4207606707605,12.8770765807768,-79.4006016434487));
#32598=CARTESIAN_POINT('Ctrl Pts',(-19.4207643941571,13.3136450649744,-80.221677332283));
#32599=CARTESIAN_POINT('Ctrl Pts',(-19.4207643941571,13.7501666523639,-81.0426550343813));
#32600=CARTESIAN_POINT('Ctrl Pts',(-16.913660379476,-0.000827524452366188,
24.8306357980468));
#32601=CARTESIAN_POINT('Ctrl Pts',(-16.9137108968607,-0.000827562593606038,
24.7817565175913));
#32602=CARTESIAN_POINT('Ctrl Pts',(-16.9137638734474,-0.000827595928633068,
24.7328783162098));
#32603=CARTESIAN_POINT('Ctrl Pts',(-16.9143897036163,-0.000828290732081643,
24.1822697845243));
#32604=CARTESIAN_POINT('Ctrl Pts',(-16.9148697187099,-0.000831039143720871,
23.1781280489857));
#32605=CARTESIAN_POINT('Ctrl Pts',(-16.915983118499,-0.000833657719236496,
21.1695293293891));
#32606=CARTESIAN_POINT('Ctrl Pts',(-16.9201504841003,-0.000841378666284282,
19.6653597636092));
#32607=CARTESIAN_POINT('Ctrl Pts',(-16.9289876731134,-0.00084736231422761,
18.414303705657));
#32608=CARTESIAN_POINT('Ctrl Pts',(-16.9332251626503,-0.000849785270073788,
17.9114881806577));
#32609=CARTESIAN_POINT('Ctrl Pts',(-16.9438656945415,-0.000856758256674359,
16.907495137435));
#32610=CARTESIAN_POINT('Ctrl Pts',(-16.9666882842702,-0.000870140538567631,
15.1536788536165));
#32611=CARTESIAN_POINT('Ctrl Pts',(-16.9883804934798,-0.000888969966369119,
13.6518892300676));
#32612=CARTESIAN_POINT('Ctrl Pts',(-17.0019864152639,-0.000893597145185849,
12.3973860955814));
#32613=CARTESIAN_POINT('Ctrl Pts',(-17.0075488559807,-0.000893453937685075,
11.896422233197));
#32614=CARTESIAN_POINT('Ctrl Pts',(-17.0188932522792,-0.000893246999643471,
10.8945664248175));
#32615=CARTESIAN_POINT('Ctrl Pts',(-17.0385337832344,-0.000885605163967994,
9.14097928832284));
#32616=CARTESIAN_POINT('Ctrl Pts',(-17.0523343964969,-0.000904878685921128,
7.63574110810873));
#32617=CARTESIAN_POINT('Ctrl Pts',(-17.058462893848,-0.000910611061803188,
6.50455257652354));
#32618=CARTESIAN_POINT('Ctrl Pts',(-17.0594955260761,-0.000682540425813807,
6.25140352785833));
#32619=CARTESIAN_POINT('Ctrl Pts',(-17.060467662109,0.000515190728335706,
5.74711946451873));
#32620=CARTESIAN_POINT('Ctrl Pts',(-17.0598052676819,0.00408390829977201,
4.86471861541086));
#32621=CARTESIAN_POINT('Ctrl Pts',(-17.0530133395588,0.0136791305464913,
3.10686987562814));
#32622=CARTESIAN_POINT('Ctrl Pts',(-17.0516180191862,0.0134886283242293,
1.61853830947895));
#32623=CARTESIAN_POINT('Ctrl Pts',(-17.065678391724,-0.00182901029311958,
0.580426886332494));
#32624=CARTESIAN_POINT('Ctrl Pts',(-17.0675004108405,-0.00380065202265222,
0.457974728958677));
#32625=CARTESIAN_POINT('Ctrl Pts',(-17.071705724231,-0.00835573562866867,
0.212109502037044));
#32626=CARTESIAN_POINT('Ctrl Pts',(-17.0804338756127,-0.0177940242792748,
-0.218431181088192));
#32627=CARTESIAN_POINT('Ctrl Pts',(-17.0962659546607,-0.0348756595322693,
-0.835714085139599));
#32628=CARTESIAN_POINT('Ctrl Pts',(-17.1187683270229,-0.0589813267680445,
-1.58010214196588));
#32629=CARTESIAN_POINT('Ctrl Pts',(-17.1510521082473,-0.0934349918654345,
-2.57819276246352));
#32630=CARTESIAN_POINT('Ctrl Pts',(-17.1909713554602,-0.135908212143206,
-3.83709577057073));
#32631=CARTESIAN_POINT('Ctrl Pts',(-17.2128352459153,-0.16041053381123,
-4.85804507598944));
#32632=CARTESIAN_POINT('Ctrl Pts',(-17.2204011685386,-0.170144998815634,
-5.50097319703451));
#32633=CARTESIAN_POINT('Ctrl Pts',(-17.2230212629696,-0.173691798969035,
-5.75463993676661));
#32634=CARTESIAN_POINT('Ctrl Pts',(-17.226773868513,-0.179673592855956,
-6.26361243491258));
#32635=CARTESIAN_POINT('Ctrl Pts',(-17.2298530876921,-0.187463581975278,
-7.15218489059402));
#32636=CARTESIAN_POINT('Ctrl Pts',(-17.2265650894144,-0.192574991909092,
-8.41811165575204));
#32637=CARTESIAN_POINT('Ctrl Pts',(-17.2190399777856,-0.193630202867038,
-9.67560107069014));
#32638=CARTESIAN_POINT('Ctrl Pts',(-17.2146902681715,-0.194244578555661,
-10.5502480830811));
#32639=CARTESIAN_POINT('Ctrl Pts',(-17.2129238439725,-0.194853172807012,
-11.0481815051936));
#32640=CARTESIAN_POINT('Ctrl Pts',(-17.2123555665687,-0.195290853822891,
-11.2964895401434));
#32641=CARTESIAN_POINT('Ctrl Pts',(-17.2120742904713,-0.195688068967561,
-11.4832796278456));
#32642=CARTESIAN_POINT('Ctrl Pts',(-17.2118759660511,-0.195936161386144,
-11.6101075392821));
#32643=CARTESIAN_POINT('Ctrl Pts',(-17.2114470879894,-0.196355384094459,
-11.8626834939792));
#32644=CARTESIAN_POINT('Ctrl Pts',(-17.21061966665,-0.19690157283447,-12.3042683349485));
#32645=CARTESIAN_POINT('Ctrl Pts',(-17.2081713370828,-0.197446873889082,
-13.4358154650848));
#32646=CARTESIAN_POINT('Ctrl Pts',(-17.2049351929916,-0.196136768310324,
-14.6854741481397));
#32647=CARTESIAN_POINT('Ctrl Pts',(-17.2024782246753,-0.194764755203927,
-15.9361627357538));
#32648=CARTESIAN_POINT('Ctrl Pts',(-17.2015627415889,-0.194229737741456,
-16.5625565005464));
#32649=CARTESIAN_POINT('Ctrl Pts',(-17.2010751272355,-0.193977141073183,
-17.0647351725833));
#32650=CARTESIAN_POINT('Ctrl Pts',(-17.2009273546625,-0.193928109111946,
-17.3162519971077));
#32651=CARTESIAN_POINT('Ctrl Pts',(-17.2008550310802,-0.19392460053942,
-17.5043116056623));
#32652=CARTESIAN_POINT('Ctrl Pts',(-17.2008258624349,-0.193913976446662,
-17.6291696252631));
#32653=CARTESIAN_POINT('Ctrl Pts',(-17.2008354253315,-0.193863398359589,
-17.8786368721972));
#32654=CARTESIAN_POINT('Ctrl Pts',(-17.2009458402694,-0.193777953248453,
-18.1282934782865));
#32655=CARTESIAN_POINT('Ctrl Pts',(-17.2011338662123,-0.193661867242172,
-18.3779773053783));
#32656=CARTESIAN_POINT('Ctrl Pts',(-17.2012835071638,-0.193580598815288,
-18.5340783504585));
#32657=CARTESIAN_POINT('Ctrl Pts',(-17.2014194303729,-0.193510762286717,
-18.6589766827682));
#32658=CARTESIAN_POINT('Ctrl Pts',(-17.2015653324318,-0.193438044296604,
-18.7838916531124));
#32659=CARTESIAN_POINT('Ctrl Pts',(-17.2020178074861,-0.193235661709927,
-19.1274644447809));
#32660=CARTESIAN_POINT('Ctrl Pts',(-17.2029485625811,-0.192872842355594,
-19.6900253638797));
#32661=CARTESIAN_POINT('Ctrl Pts',(-17.2049585767724,-0.192422272388314,
-20.6911781623881));
#32662=CARTESIAN_POINT('Ctrl Pts',(-17.2073250106957,-0.192486080415645,
-21.9448455152447));
#32663=CARTESIAN_POINT('Ctrl Pts',(-17.2081516600097,-0.194217925765995,
-22.9504307734254));
#32664=CARTESIAN_POINT('Ctrl Pts',(-17.2077723489864,-0.195987817235101,
-23.5781458830157));
#32665=CARTESIAN_POINT('Ctrl Pts',(-17.207531945452,-0.196779858340764,
-23.8262844322728));
#32666=CARTESIAN_POINT('Ctrl Pts',(-17.2068115037894,-0.198739021591868,
-24.3238297132593));
#32667=CARTESIAN_POINT('Ctrl Pts',(-17.2049496914524,-0.203003236988368,
-25.1969032515018));
#32668=CARTESIAN_POINT('Ctrl Pts',(-17.2013628141071,-0.21087970254429,
-26.4501042965554));
#32669=CARTESIAN_POINT('Ctrl Pts',(-17.1966376310898,-0.220641929842346,
-27.9594600939016));
#32670=CARTESIAN_POINT('Ctrl Pts',(-17.1947174123027,-0.225915093926835,
-28.9669128292201));
#32671=CARTESIAN_POINT('Ctrl Pts',(-17.1941033398868,-0.228011167691387,
-29.5330458281712));
#32672=CARTESIAN_POINT('Ctrl Pts',(-17.1940103235576,-0.228509201821878,
-29.6568748700719));
#32673=CARTESIAN_POINT('Ctrl Pts',(-17.1940415331691,-0.22968414567057,
-29.9059782896191));
#32674=CARTESIAN_POINT('Ctrl Pts',(-17.1946196742512,-0.232137119393154,
-30.3421046429563));
#32675=CARTESIAN_POINT('Ctrl Pts',(-17.1973975961259,-0.238217812899528,
-31.2177721129568));
#32676=CARTESIAN_POINT('Ctrl Pts',(-17.2023621216832,-0.245855180371747,
-32.2244667020336));
#32677=CARTESIAN_POINT('Ctrl Pts',(-17.2051791592324,-0.250277943790212,
-33.2363333375358));
#32678=CARTESIAN_POINT('Ctrl Pts',(-17.2052435872608,-0.250996682862532,
-33.99745418694));
#32679=CARTESIAN_POINT('Ctrl Pts',(-17.2023928576229,-0.248121563635076,
-34.7605998167641));
#32680=CARTESIAN_POINT('Ctrl Pts',(-17.1978710785691,-0.243111695047323,
-35.2705175595103));
#32681=CARTESIAN_POINT('Ctrl Pts',(-17.1932447017443,-0.237922214682433,
-35.6544712301579));
#32682=CARTESIAN_POINT('Ctrl Pts',(-17.189572689603,-0.233756496190182,
-35.9138599889488));
#32683=CARTESIAN_POINT('Ctrl Pts',(-17.1801995897282,-0.223079963618858,
-36.4288669924271));
#32684=CARTESIAN_POINT('Ctrl Pts',(-17.1591257574078,-0.198762387458058,
-37.3248896233205));
#32685=CARTESIAN_POINT('Ctrl Pts',(-17.1043112841144,-0.134136510171068,
-39.0948524820125));
#32686=CARTESIAN_POINT('Ctrl Pts',(-17.055677831133,-0.0715788885984206,
-40.5774563651269));
#32687=CARTESIAN_POINT('Ctrl Pts',(-17.039939163976,-0.0473933387138723,
-41.676723963463));
#32688=CARTESIAN_POINT('Ctrl Pts',(-17.0368530908193,-0.0436179589478702,
-41.9105485570633));
#32689=CARTESIAN_POINT('Ctrl Pts',(-17.0331788357747,-0.0410479343042623,
-42.2702794698711));
#32690=CARTESIAN_POINT('Ctrl Pts',(-17.0303848046245,-0.041194751765132,
-42.6322830520466));
#32691=CARTESIAN_POINT('Ctrl Pts',(-17.0276749280209,-0.0441037814641113,
-43.1211740281135));
#32692=CARTESIAN_POINT('Ctrl Pts',(-17.0259722716986,-0.051378215425189,
-43.7416256933687));
#32693=CARTESIAN_POINT('Ctrl Pts',(-17.0257955214629,-0.0606767901658299,
-44.5013944238914));
#32694=CARTESIAN_POINT('Ctrl Pts',(-17.0265207254421,-0.0642878465005962,
-45.1464567264756));
#32695=CARTESIAN_POINT('Ctrl Pts',(-17.0273584080279,-0.061868937121287,
-45.6697526773922));
#32696=CARTESIAN_POINT('Ctrl Pts',(-17.0279500941828,-0.0565894168579634,
-46.0656376499745));
#32697=CARTESIAN_POINT('Ctrl Pts',(-17.0284130754296,-0.0470726749227195,
-46.4649407204044));
#32698=CARTESIAN_POINT('Ctrl Pts',(-17.0287785102378,-0.027711324519983,
-47.0017778071796));
#32699=CARTESIAN_POINT('Ctrl Pts',(-17.0284489638891,-0.00433057001500467,
-47.409310418673));
#32700=CARTESIAN_POINT('Ctrl Pts',(-17.0277061342787,0.026533196437943,
-47.820450921256));
#32701=CARTESIAN_POINT('Ctrl Pts',(-17.0272980415244,0.04630747610463,-48.0746939995828));
#32702=CARTESIAN_POINT('Ctrl Pts',(-17.0267681470394,0.0898860246021606,
-48.5966914106082));
#32703=CARTESIAN_POINT('Ctrl Pts',(-17.0264136197667,0.174680315576811,
-49.507451228005));
#32704=CARTESIAN_POINT('Ctrl Pts',(-17.0263194698604,0.326520770084301,
-50.8215873882974));
#32705=CARTESIAN_POINT('Ctrl Pts',(-17.0244732262949,0.571748883938012,
-52.4101266340064));
#32706=CARTESIAN_POINT('Ctrl Pts',(-17.019680884052,0.787993337413998,-53.4770518292365));
#32707=CARTESIAN_POINT('Ctrl Pts',(-17.0152049765085,0.943054767162755,
-54.1469480985672));
#32708=CARTESIAN_POINT('Ctrl Pts',(-17.0132158520225,1.00675878632521,-54.4147385821911));
#32709=CARTESIAN_POINT('Ctrl Pts',(-17.0084771905012,1.14111853808085,-54.9509279640968));
#32710=CARTESIAN_POINT('Ctrl Pts',(-16.9984395285394,1.39294874261741,-55.8861129023711));
#32711=CARTESIAN_POINT('Ctrl Pts',(-16.973683877416,1.96030674557442,-57.745888315172));
#32712=CARTESIAN_POINT('Ctrl Pts',(-16.9517208177551,2.54171784587128,-59.3129141111068));
#32713=CARTESIAN_POINT('Ctrl Pts',(-16.9425566585775,2.98804610390464,-60.4072064077515));
#32714=CARTESIAN_POINT('Ctrl Pts',(-16.9414412312354,3.04585547552463,-60.5471782172652));
#32715=CARTESIAN_POINT('Ctrl Pts',(-16.9393064923459,3.16197853912094,-60.8217554937349));
#32716=CARTESIAN_POINT('Ctrl Pts',(-16.9357919546893,3.37142078514763,-61.3011519121273));
#32717=CARTESIAN_POINT('Ctrl Pts',(-16.9295918848644,3.80832828880345,-62.2456574911334));
#32718=CARTESIAN_POINT('Ctrl Pts',(-16.9242940338859,4.33788660464919,-63.2977932858732));
#32719=CARTESIAN_POINT('Ctrl Pts',(-16.9201929569173,4.8726619443111,-64.3200099674657));
#32720=CARTESIAN_POINT('Ctrl Pts',(-16.9182376614387,5.17106378403726,-64.8834056112915));
#32721=CARTESIAN_POINT('Ctrl Pts',(-16.9170492480065,5.36707898374819,-65.2537774280137));
#32722=CARTESIAN_POINT('Ctrl Pts',(-16.9162791853453,5.4968614910262,-65.4992648282184));
#32723=CARTESIAN_POINT('Ctrl Pts',(-16.9155642280653,5.62511071424056,-65.7426262959858));
#32724=CARTESIAN_POINT('Ctrl Pts',(-16.9149560935067,5.73566048116463,-65.9535571297107));
#32725=CARTESIAN_POINT('Ctrl Pts',(-16.9146160876875,5.79830681867362,-66.0735058527206));
#32726=CARTESIAN_POINT('Ctrl Pts',(-16.9141117770561,5.89173625215646,-66.2528507981329));
#32727=CARTESIAN_POINT('Ctrl Pts',(-16.9137145858612,5.96838687667906,-66.4010494961629));
#32728=CARTESIAN_POINT('Ctrl Pts',(-16.9130609416537,6.09363292623985,-66.6449889221048));
#32729=CARTESIAN_POINT('Ctrl Pts',(-16.9124754105693,6.23087155580065,-66.9111670250714));
#32730=CARTESIAN_POINT('Ctrl Pts',(-16.9116001717781,6.50058807743624,-67.4301500253597));
#32731=CARTESIAN_POINT('Ctrl Pts',(-16.9108116823416,6.97391496129387,-68.3314415541294));
#32732=CARTESIAN_POINT('Ctrl Pts',(-16.9113899890333,7.91445730841173,-70.0927851753583));
#32733=CARTESIAN_POINT('Ctrl Pts',(-16.9134592054242,8.71297949991766,-71.5685144368547));
#32734=CARTESIAN_POINT('Ctrl Pts',(-16.9134782723112,9.30706797837199,-72.6860024639261));
#32735=CARTESIAN_POINT('Ctrl Pts',(-16.9134755702942,9.44092506181541,-72.9377664497756));
#32736=CARTESIAN_POINT('Ctrl Pts',(-16.913473633529,9.70769196988074,-73.4395108223667));
#32737=CARTESIAN_POINT('Ctrl Pts',(-16.9134806352122,10.0413473332645,-74.0670656031285));
#32738=CARTESIAN_POINT('Ctrl Pts',(-16.9134848785104,10.441325488255,-74.8193285939959));
#32739=CARTESIAN_POINT('Ctrl Pts',(-16.9134974165686,11.2411072259944,-76.3235025515291));
#32740=CARTESIAN_POINT('Ctrl Pts',(-16.9135408055664,11.9072850484377,-77.5764491734321));
#32741=CARTESIAN_POINT('Ctrl Pts',(-16.9135615147347,12.8771726655419,-79.4005966696148));
#32742=CARTESIAN_POINT('Ctrl Pts',(-16.9135721726838,13.3137342085495,-80.2216774052325));
#32743=CARTESIAN_POINT('Ctrl Pts',(-16.9135721726839,13.7502557959389,-81.0426551073307));
#32744=CARTESIAN_POINT('Ctrl Pts',(-15.0340696487865,-0.000210821217461291,
24.8306350086551));
#32745=CARTESIAN_POINT('Ctrl Pts',(-15.0341145257418,-0.000210843949456753,
24.7817557045308));
#32746=CARTESIAN_POINT('Ctrl Pts',(-15.0341615944517,-0.000210872430609927,
24.7328775245175));
#32747=CARTESIAN_POINT('Ctrl Pts',(-15.034717309544,-0.000210997311721509,
24.1822671849837));
#32748=CARTESIAN_POINT('Ctrl Pts',(-15.0351415677414,-0.000210036235135822,
23.1781123136946));
#32749=CARTESIAN_POINT('Ctrl Pts',(-15.0361299132171,-0.000210786122590035,
21.1695117270465));
#32750=CARTESIAN_POINT('Ctrl Pts',(-15.0398270933617,-0.000209397903320249,
19.6653103377228));
#32751=CARTESIAN_POINT('Ctrl Pts',(-15.0476763535126,-0.000211290125626849,
18.4142404576199));
#32752=CARTESIAN_POINT('Ctrl Pts',(-15.0514406999345,-0.000212723869813204,
17.9114214084088));
#32753=CARTESIAN_POINT('Ctrl Pts',(-15.0608925135565,-0.000216077529731644,
16.9074183611299));
#32754=CARTESIAN_POINT('Ctrl Pts',(-15.0811667598752,-0.000224215406749858,
15.1535926470682));
#32755=CARTESIAN_POINT('Ctrl Pts',(-15.1004296936536,-0.000224600233301203,
13.6517348544103));
#32756=CARTESIAN_POINT('Ctrl Pts',(-15.112515932568,-0.000224155863509205,
12.3972032802743));
#32757=CARTESIAN_POINT('Ctrl Pts',(-15.1174586204932,-0.000224715802731574,
11.8962330298534));
#32758=CARTESIAN_POINT('Ctrl Pts',(-15.1275381508422,-0.000223899547587101,
10.894368074858));
#32759=CARTESIAN_POINT('Ctrl Pts',(-15.1449930229432,-0.000222875154932196,
9.14071542262987));
#32760=CARTESIAN_POINT('Ctrl Pts',(-15.1572362388009,-0.000202554275669931,
7.63540656559452));
#32761=CARTESIAN_POINT('Ctrl Pts',(-15.1626756856597,-0.000193665754207598,
6.50379563471612));
#32762=CARTESIAN_POINT('Ctrl Pts',(-15.1633713553078,0.000401434165705328,
6.24603324501292));
#32763=CARTESIAN_POINT('Ctrl Pts',(-15.1630692903181,0.00352516011666141,
5.73674929179688));
#32764=CARTESIAN_POINT('Ctrl Pts',(-15.1589762101693,0.0128138667348422,
4.84803318861574));
#32765=CARTESIAN_POINT('Ctrl Pts',(-15.1436218457689,0.0375658550561563,
3.09396402820915));
#32766=CARTESIAN_POINT('Ctrl Pts',(-15.1422991151934,0.0370420676052799,
1.63422915566954));
#32767=CARTESIAN_POINT('Ctrl Pts',(-15.1698636910876,-0.000984415113118122,
0.629751746190038));
#32768=CARTESIAN_POINT('Ctrl Pts',(-15.1734444074368,-0.00581318203249671,
0.51323032427116));
#32769=CARTESIAN_POINT('Ctrl Pts',(-15.1817096352969,-0.0170453275908212,
0.277362288633637));
#32770=CARTESIAN_POINT('Ctrl Pts',(-15.1988795725625,-0.0403918395228711,
-0.136893473663548));
#32771=CARTESIAN_POINT('Ctrl Pts',(-15.2300183738483,-0.0828742763000551,
-0.736456418724525));
#32772=CARTESIAN_POINT('Ctrl Pts',(-15.274431671662,-0.14357994765381,-1.46782575099239));
#32773=CARTESIAN_POINT('Ctrl Pts',(-15.338283327315,-0.23092306394781,-2.45974486050588));
#32774=CARTESIAN_POINT('Ctrl Pts',(-15.4179285166044,-0.340180783742031,
-3.7316228060576));
#32775=CARTESIAN_POINT('Ctrl Pts',(-15.463058609532,-0.403833363193915,
-4.78418508811165));
#32776=CARTESIAN_POINT('Ctrl Pts',(-15.479901874256,-0.429108529628997,
-5.45306890189568));
#32777=CARTESIAN_POINT('Ctrl Pts',(-15.4858622096508,-0.438063691875341,
-5.71135488848376));
#32778=CARTESIAN_POINT('Ctrl Pts',(-15.4952017506763,-0.453072758781202,
-6.23156910938738));
#32779=CARTESIAN_POINT('Ctrl Pts',(-15.5053595039547,-0.472016689866684,
-7.13537326829117));
#32780=CARTESIAN_POINT('Ctrl Pts',(-15.506211843786,-0.483114774661327,
-8.41610862916057));
#32781=CARTESIAN_POINT('Ctrl Pts',(-15.4990448698447,-0.484040471410166,
-9.6776078698402));
#32782=CARTESIAN_POINT('Ctrl Pts',(-15.4950833952651,-0.484882331836825,
-10.5498451372121));
#32783=CARTESIAN_POINT('Ctrl Pts',(-15.4938652554776,-0.486172211228457,
-11.0448123107463));
#32784=CARTESIAN_POINT('Ctrl Pts',(-15.4937284111205,-0.487212411291013,
-11.2911040176186));
#32785=CARTESIAN_POINT('Ctrl Pts',(-15.4938501089971,-0.488192194439701,
-11.4762353961436));
#32786=CARTESIAN_POINT('Ctrl Pts',(-15.4939127005871,-0.488825135949953,
-11.6039934931571));
#32787=CARTESIAN_POINT('Ctrl Pts',(-15.4939510398894,-0.489929912388259,
-11.8572340996596));
#32788=CARTESIAN_POINT('Ctrl Pts',(-15.4938086869916,-0.49148328892933,
-12.3004477072361));
#32789=CARTESIAN_POINT('Ctrl Pts',(-15.4925012109195,-0.493701376635383,
-13.4350955010258));
#32790=CARTESIAN_POINT('Ctrl Pts',(-15.4891073643623,-0.49213447753875,
-14.6867391068569));
#32791=CARTESIAN_POINT('Ctrl Pts',(-15.486293576516,-0.490119048938007,
-15.9375432059456));
#32792=CARTESIAN_POINT('Ctrl Pts',(-15.4852325972702,-0.489277658623344,
-16.5635934600252));
#32793=CARTESIAN_POINT('Ctrl Pts',(-15.4847213819187,-0.488889211225351,
-17.065228188401));
#32794=CARTESIAN_POINT('Ctrl Pts',(-15.4845974520452,-0.488816016851646,
-17.316390296355));
#32795=CARTESIAN_POINT('Ctrl Pts',(-15.4845624417368,-0.488818430391284,
-17.5041561557632));
#32796=CARTESIAN_POINT('Ctrl Pts',(-15.4845605084085,-0.488813854935621,
-17.6289594914254));
#32797=CARTESIAN_POINT('Ctrl Pts',(-15.4846357561806,-0.488781645831683,
-17.8782617656739));
#32798=CARTESIAN_POINT('Ctrl Pts',(-15.4848197730921,-0.488717003757751,
-18.1278185570752));
#32799=CARTESIAN_POINT('Ctrl Pts',(-15.4850956191003,-0.488627896471198,
-18.3774196991142));
#32800=CARTESIAN_POINT('Ctrl Pts',(-15.4853021884926,-0.48856290194664,
-18.5334870841398));
#32801=CARTESIAN_POINT('Ctrl Pts',(-15.4854858266379,-0.48850631211949,
-18.6583654216715));
#32802=CARTESIAN_POINT('Ctrl Pts',(-15.4856808325107,-0.488446790050174,
-18.783266238916));
#32803=CARTESIAN_POINT('Ctrl Pts',(-15.4862618105197,-0.488272898475504,
-19.1268260250996));
#32804=CARTESIAN_POINT('Ctrl Pts',(-15.487416933585,-0.487940562173684,
-19.6894910265984));
#32805=CARTESIAN_POINT('Ctrl Pts',(-15.4896816665822,-0.487363835529118,
-20.6912070174202));
#32806=CARTESIAN_POINT('Ctrl Pts',(-15.4921467801256,-0.486910225703765,
-21.946226880138));
#32807=CARTESIAN_POINT('Ctrl Pts',(-15.4922291859508,-0.487421197561042,
-22.9536208320778));
#32808=CARTESIAN_POINT('Ctrl Pts',(-15.4911855039851,-0.488171590611569,
-23.582669839668));
#32809=CARTESIAN_POINT('Ctrl Pts',(-15.4906590900156,-0.488520922739212,
-23.8315946634435));
#32810=CARTESIAN_POINT('Ctrl Pts',(-15.4892167417865,-0.489406629375772,
-24.3303557486252));
#32811=CARTESIAN_POINT('Ctrl Pts',(-15.485795202301,-0.491377665390427,
-25.2051694330726));
#32812=CARTESIAN_POINT('Ctrl Pts',(-15.479157002439,-0.495019484766462,
-26.4594627009045));
#32813=CARTESIAN_POINT('Ctrl Pts',(-15.4707510145125,-0.499469758305157,
-27.9680031668306));
#32814=CARTESIAN_POINT('Ctrl Pts',(-15.4665564296506,-0.501764663321334,
-28.9735615475648));
#32815=CARTESIAN_POINT('Ctrl Pts',(-15.4650261259966,-0.502651525309478,
-29.5380529341808));
#32816=CARTESIAN_POINT('Ctrl Pts',(-15.4647905618725,-0.502970120966628,
-29.6594213057265));
#32817=CARTESIAN_POINT('Ctrl Pts',(-15.46471593299,-0.504074559115558,-29.9052068360382));
#32818=CARTESIAN_POINT('Ctrl Pts',(-15.4655271857808,-0.507104822699974,
-30.3358816568284));
#32819=CARTESIAN_POINT('Ctrl Pts',(-15.4701084649425,-0.516544753536145,
-31.2050201931821));
#32820=CARTESIAN_POINT('Ctrl Pts',(-15.4784576095206,-0.530407269101178,
-32.2128483187638));
#32821=CARTESIAN_POINT('Ctrl Pts',(-15.4825296956784,-0.537652201710911,
-33.2347909521993));
#32822=CARTESIAN_POINT('Ctrl Pts',(-15.4815887421991,-0.537269746738212,
-34.0078583156326));
#32823=CARTESIAN_POINT('Ctrl Pts',(-15.4747982556546,-0.528507549680347,
-34.7874935349868));
#32824=CARTESIAN_POINT('Ctrl Pts',(-15.4650828361564,-0.515241059459426,
-35.3114265018969));
#32825=CARTESIAN_POINT('Ctrl Pts',(-15.4553238411324,-0.501698729642147,
-35.7072440104675));
#32826=CARTESIAN_POINT('Ctrl Pts',(-15.4475606882035,-0.490722023148797,
-35.9784948813668));
#32827=CARTESIAN_POINT('Ctrl Pts',(-15.4279351556162,-0.462963031630886,
-36.5119195277882));
#32828=CARTESIAN_POINT('Ctrl Pts',(-15.3843101231493,-0.40092723253623,
-37.4342446096674));
#32829=CARTESIAN_POINT('Ctrl Pts',(-15.2718006860811,-0.239170262616976,
-39.2262614686388));
#32830=CARTESIAN_POINT('Ctrl Pts',(-15.1742119209602,-0.0943688510220052,
-40.6745248011419));
#32831=CARTESIAN_POINT('Ctrl Pts',(-15.1433506285053,-0.0457555244295182,
-41.7210473027235));
#32832=CARTESIAN_POINT('Ctrl Pts',(-15.1372456044953,-0.0370431808461871,
-41.9494258875079));
#32833=CARTESIAN_POINT('Ctrl Pts',(-15.1300553792688,-0.0285684953548626,
-42.2990803123208));
#32834=CARTESIAN_POINT('Ctrl Pts',(-15.1246437573577,-0.0242103880382995,
-42.6529450614386));
#32835=CARTESIAN_POINT('Ctrl Pts',(-15.1195490929288,-0.0228952361957256,
-43.1316637113185));
#32836=CARTESIAN_POINT('Ctrl Pts',(-15.1166812517057,-0.0279587687423588,
-43.7419250921212));
#32837=CARTESIAN_POINT('Ctrl Pts',(-15.117316613805,-0.0385683079696591,
-44.4929517663402));
#32838=CARTESIAN_POINT('Ctrl Pts',(-15.1199844499608,-0.0456198942806182,
-45.1337752418407));
#32839=CARTESIAN_POINT('Ctrl Pts',(-15.1226575630422,-0.0465603840325312,
-45.6554805491814));
#32840=CARTESIAN_POINT('Ctrl Pts',(-15.1247395447071,-0.0439822094079027,
-46.0510733259666));
#32841=CARTESIAN_POINT('Ctrl Pts',(-15.1267099246971,-0.0371484216702725,
-46.4509914011933));
#32842=CARTESIAN_POINT('Ctrl Pts',(-15.1289391518283,-0.0210245151836314,
-46.9898517547243));
#32843=CARTESIAN_POINT('Ctrl Pts',(-15.1298649672635,0.000485826508328478,
-47.4002758033805));
#32844=CARTESIAN_POINT('Ctrl Pts',(-15.1299281441084,0.030449471970366,
-47.8150612254708));
#32845=CARTESIAN_POINT('Ctrl Pts',(-15.1301783436448,0.0490313999239923,
-48.0659849956426));
#32846=CARTESIAN_POINT('Ctrl Pts',(-15.1314065155196,0.0897518029660117,
-48.5852232398212));
#32847=CARTESIAN_POINT('Ctrl Pts',(-15.1351320722241,0.167897705960403,
-49.4908701828698));
#32848=CARTESIAN_POINT('Ctrl Pts',(-15.1430849163375,0.307470878327013,
-50.8028655589996));
#32849=CARTESIAN_POINT('Ctrl Pts',(-15.1508412363502,0.539435350524335,
-52.3947240716309));
#32850=CARTESIAN_POINT('Ctrl Pts',(-15.1506480567004,0.751131888791374,
-53.4682817329514));
#32851=CARTESIAN_POINT('Ctrl Pts',(-15.1476109567481,0.905912498453314,
-54.1433711240342));
#32852=CARTESIAN_POINT('Ctrl Pts',(-15.1461202952764,0.969433044413928,
-54.4122310142868));
#32853=CARTESIAN_POINT('Ctrl Pts',(-15.142109011906,1.10399607711384,-54.9508340108951));
#32854=CARTESIAN_POINT('Ctrl Pts',(-15.1327556378678,1.35716166152049,-55.8892951044509));
#32855=CARTESIAN_POINT('Ctrl Pts',(-15.1073672179884,1.93029757933884,-57.753246710139));
#32856=CARTESIAN_POINT('Ctrl Pts',(-15.083216275239,2.51865994279119,-59.3197411843726));
#32857=CARTESIAN_POINT('Ctrl Pts',(-15.0731431840729,2.96744566208701,-60.4121663185723));
#32858=CARTESIAN_POINT('Ctrl Pts',(-15.0718837363928,3.02578692306643,-60.5524387601586));
#32859=CARTESIAN_POINT('Ctrl Pts',(-15.0694481839692,3.14288176895106,-60.8272805211502));
#32860=CARTESIAN_POINT('Ctrl Pts',(-15.065320652537,3.35419364121946,-61.3072037551322));
#32861=CARTESIAN_POINT('Ctrl Pts',(-15.0576778829909,3.79504838543236,-62.2523204944424));
#32862=CARTESIAN_POINT('Ctrl Pts',(-15.050338429514,4.32946696887476,-63.3045514635493));
#32863=CARTESIAN_POINT('Ctrl Pts',(-15.0443029598303,4.86848074759074,-64.3262573936111));
#32864=CARTESIAN_POINT('Ctrl Pts',(-15.0413660979999,5.16889192858953,-64.8891493786111));
#32865=CARTESIAN_POINT('Ctrl Pts',(-15.039590403758,5.36604126182675,-65.2590864213906));
#32866=CARTESIAN_POINT('Ctrl Pts',(-15.0384540513163,5.4965130215108,-65.5042581947861));
#32867=CARTESIAN_POINT('Ctrl Pts',(-15.0373902749899,5.62537760635623,-65.7472584806305));
#32868=CARTESIAN_POINT('Ctrl Pts',(-15.0365197826222,5.73636055026298,-65.9578371846317));
#32869=CARTESIAN_POINT('Ctrl Pts',(-15.0360397843803,5.79922704441969,-66.0775731162684));
#32870=CARTESIAN_POINT('Ctrl Pts',(-15.0353370564175,5.89295702670228,-66.2565875810318));
#32871=CARTESIAN_POINT('Ctrl Pts',(-15.0347884103062,5.96980765329387,-66.404481691943));
#32872=CARTESIAN_POINT('Ctrl Pts',(-15.0339269335575,6.09528802680313,-66.6478866046348));
#32873=CARTESIAN_POINT('Ctrl Pts',(-15.033147894299,6.23279681431226,-66.9136268045961));
#32874=CARTESIAN_POINT('Ctrl Pts',(-15.0319847166712,6.50279848479195,-67.431768557194));
#32875=CARTESIAN_POINT('Ctrl Pts',(-15.030883245086,6.97621744887788,-68.3318284641148));
#32876=CARTESIAN_POINT('Ctrl Pts',(-15.0315271538091,7.91561157226374,-70.091628231057));
#32877=CARTESIAN_POINT('Ctrl Pts',(-15.0340468472341,8.71293629115863,-71.5676334552757));
#32878=CARTESIAN_POINT('Ctrl Pts',(-15.034013342273,9.30764415560229,-72.6861482880389));
#32879=CARTESIAN_POINT('Ctrl Pts',(-15.0340065308162,9.44146712074772,-72.9378378628493));
#32880=CARTESIAN_POINT('Ctrl Pts',(-15.0339964645219,9.70825955523391,-73.4396095072806));
#32881=CARTESIAN_POINT('Ctrl Pts',(-15.0339906484446,10.0419117529944,-74.0671244842568));
#32882=CARTESIAN_POINT('Ctrl Pts',(-15.0339903349211,10.4418952801368,-74.8193852863724));
#32883=CARTESIAN_POINT('Ctrl Pts',(-15.034000079842,11.2416696930003,-76.3235367360246));
#32884=CARTESIAN_POINT('Ctrl Pts',(-15.0340231534456,11.9078687631932,-77.5764650361812));
#32885=CARTESIAN_POINT('Ctrl Pts',(-15.0340251082683,12.8777820837011,-79.4006095900798));
#32886=CARTESIAN_POINT('Ctrl Pts',(-15.0340261179702,13.3143507467422,-80.2216773228945));
#32887=CARTESIAN_POINT('Ctrl Pts',(-15.0340261179702,13.7508723341316,-81.0426550249928));
#32888=CARTESIAN_POINT('Ctrl Pts',(-13.1551501085346,0.000334283317693157,
24.8306343036982));
#32889=CARTESIAN_POINT('Ctrl Pts',(-13.1551893734422,0.000334288576141201,
24.7817549764308));
#32890=CARTESIAN_POINT('Ctrl Pts',(-13.1552305486304,0.000334309069330346,
24.732876823539));
#32891=CARTESIAN_POINT('Ctrl Pts',(-13.1557170169322,0.000333869307825757,
24.1822645064593));
#32892=CARTESIAN_POINT('Ctrl Pts',(-13.1560904963607,0.000329952799201668,
23.1780950644636));
#32893=CARTESIAN_POINT('Ctrl Pts',(-13.1569561071082,0.000330340267912158,
21.1694924498549));
#32894=CARTESIAN_POINT('Ctrl Pts',(-13.1601960309673,0.000320300549670185,
19.6652554863826));
#32895=CARTESIAN_POINT('Ctrl Pts',(-13.1670648392222,0.000315420358113045,
18.4141701152996));
#32896=CARTESIAN_POINT('Ctrl Pts',(-13.1703583133568,0.000314645245098799,
17.911347262654));
#32897=CARTESIAN_POINT('Ctrl Pts',(-13.1786284036948,0.000311635286896385,
16.9073331364927));
#32898=CARTESIAN_POINT('Ctrl Pts',(-13.1963663451238,0.000308308368792227,
15.1534970060382));
#32899=CARTESIAN_POINT('Ctrl Pts',(-13.2132280020023,0.000282947619664433,
13.6515624916615));
#32900=CARTESIAN_POINT('Ctrl Pts',(-13.2238045208785,0.000267953770380593,
12.3969987794564));
#32901=CARTESIAN_POINT('Ctrl Pts',(-13.2281281999324,0.000264653615848435,
11.8960199930155));
#32902=CARTESIAN_POINT('Ctrl Pts',(-13.2369467167224,0.000252238528283899,
10.8941480683364));
#32903=CARTESIAN_POINT('Ctrl Pts',(-13.2522139598646,0.000235521042924121,
9.1404079120666));
#32904=CARTESIAN_POINT('Ctrl Pts',(-13.2629486208776,0.000157953311529688,
7.63506274647202));
#32905=CARTESIAN_POINT('Ctrl Pts',(-13.2677164336163,0.000130044779467958,
6.5028757710561));
#32906=CARTESIAN_POINT('Ctrl Pts',(-13.2681176025061,0.00126267364318012,
6.23854702865849));
#32907=CARTESIAN_POINT('Ctrl Pts',(-13.2667638439163,0.00719521979917226,
5.72215032975373));
#32908=CARTESIAN_POINT('Ctrl Pts',(-13.2599284214127,0.0246871106678599,
4.82449852059114));
#32909=CARTESIAN_POINT('Ctrl Pts',(-13.2378016283123,0.0708993897733014,
3.07581123919757));
#32910=CARTESIAN_POINT('Ctrl Pts',(-13.2367589129128,0.0686478918711237,
1.6571204667629));
#32911=CARTESIAN_POINT('Ctrl Pts',(-13.2749785132875,0.000629895584349044,
0.70032287348691));
#32912=CARTESIAN_POINT('Ctrl Pts',(-13.2799367989849,-0.00777849232495627,
0.592200628888257));
#32913=CARTESIAN_POINT('Ctrl Pts',(-13.2913797621347,-0.0275861271661714,
0.370450620181562));
#32914=CARTESIAN_POINT('Ctrl Pts',(-13.3151282376604,-0.068962804676975,
-0.0208960537362408));
#32915=CARTESIAN_POINT('Ctrl Pts',(-13.3581349865091,-0.14539257342901,
-0.595770614284169));
#32916=CARTESIAN_POINT('Ctrl Pts',(-13.4192403351803,-0.256485334484831,
-1.30926981255708));
#32917=CARTESIAN_POINT('Ctrl Pts',(-13.5070022246835,-0.419351414251861,
-2.2930728602858));
#32918=CARTESIAN_POINT('Ctrl Pts',(-13.6164651099767,-0.628546828230703,
-3.58331904027932));
#32919=CARTESIAN_POINT('Ctrl Pts',(-13.6794191786112,-0.75494668425885,
-4.67998105132848));
#32920=CARTESIAN_POINT('Ctrl Pts',(-13.7034053121075,-0.805364352070461,
-5.38531907968524));
#32921=CARTESIAN_POINT('Ctrl Pts',(-13.711812253373,-0.82264389406825,-5.65011752865608));
#32922=CARTESIAN_POINT('Ctrl Pts',(-13.7253016587713,-0.851689010827571,
-6.18616764618947));
#32923=CARTESIAN_POINT('Ctrl Pts',(-13.7407257068587,-0.88773407989656,
-7.11147181124667));
#32924=CARTESIAN_POINT('Ctrl Pts',(-13.7449258328838,-0.907719595052291,
-8.41317522414356));
#32925=CARTESIAN_POINT('Ctrl Pts',(-13.7384418678751,-0.908107987950047,
-9.68045569583018));
#32926=CARTESIAN_POINT('Ctrl Pts',(-13.7348891547529,-0.90901605019472,
-10.5493544319712));
#32927=CARTESIAN_POINT('Ctrl Pts',(-13.7340705601867,-0.911173060866272,
-11.0401724781861));
#32928=CARTESIAN_POINT('Ctrl Pts',(-13.7342181547962,-0.913040175168312,
-11.2836385676462));
#32929=CARTESIAN_POINT('Ctrl Pts',(-13.734595811174,-0.914830641973323,
-11.4664445586127));
#32930=CARTESIAN_POINT('Ctrl Pts',(-13.7348265495321,-0.916019414652225,
-11.5955414439621));
#32931=CARTESIAN_POINT('Ctrl Pts',(-13.7351468223391,-0.918096161386488,
-11.8497587471897));
#32932=CARTESIAN_POINT('Ctrl Pts',(-13.7353808308897,-0.921076812804577,
-12.2953368249091));
#32933=CARTESIAN_POINT('Ctrl Pts',(-13.7344944584954,-0.925632694184054,
-13.4344907253095));
#32934=CARTESIAN_POINT('Ctrl Pts',(-13.7303643879806,-0.923608185100719,
-14.6889600179318));
#32935=CARTESIAN_POINT('Ctrl Pts',(-13.7267867092688,-0.920518695146856,
-15.9397629453685));
#32936=CARTESIAN_POINT('Ctrl Pts',(-13.7254524072941,-0.919219914483102,
-16.5652138437354));
#32937=CARTESIAN_POINT('Ctrl Pts',(-13.7248363073386,-0.918615753584493,
-17.0659631831709));
#32938=CARTESIAN_POINT('Ctrl Pts',(-13.7247119123663,-0.918511435023379,
-17.3165574963283));
#32939=CARTESIAN_POINT('Ctrl Pts',(-13.7246978826119,-0.918524245907937,
-17.5038581677432));
#32940=CARTESIAN_POINT('Ctrl Pts',(-13.7247086069979,-0.918530104126422,
-17.6286329123153));
#32941=CARTESIAN_POINT('Ctrl Pts',(-13.7248036965319,-0.918530711256441,
-17.8777412014854));
#32942=CARTESIAN_POINT('Ctrl Pts',(-13.7250049145367,-0.918518178892288,
-18.1271988002274));
#32943=CARTESIAN_POINT('Ctrl Pts',(-13.7252915898653,-0.918488106487544,
-18.3767028364522));
#32944=CARTESIAN_POINT('Ctrl Pts',(-13.7255046554761,-0.918463530061787,
-18.5327310273419));
#32945=CARTESIAN_POINT('Ctrl Pts',(-13.7256927785562,-0.918439784078445,
-18.6575838103995));
#32946=CARTESIAN_POINT('Ctrl Pts',(-13.7258919014263,-0.918413320075625,
-18.7824655906309));
#32947=CARTESIAN_POINT('Ctrl Pts',(-13.7264890957503,-0.918334197338507,
-19.1259957677016));
#32948=CARTESIAN_POINT('Ctrl Pts',(-13.7276729411882,-0.918147331683812,
-19.6887422443658));
#32949=CARTESIAN_POINT('Ctrl Pts',(-13.7300976648197,-0.917698555102597,
-20.6909608145285));
#32950=CARTESIAN_POINT('Ctrl Pts',(-13.7329660445855,-0.916847221647031,
-21.9472991675568));
#32951=CARTESIAN_POINT('Ctrl Pts',(-13.7339260928259,-0.915974400434199,
-22.9564516405322));
#32952=CARTESIAN_POINT('Ctrl Pts',(-13.7335909065193,-0.91532061521922,
-23.586839406153));
#32953=CARTESIAN_POINT('Ctrl Pts',(-13.7333720459406,-0.915033425050764,
-23.8365407161973));
#32954=CARTESIAN_POINT('Ctrl Pts',(-13.7326725951122,-0.914383629983113,
-24.336514511158));
#32955=CARTESIAN_POINT('Ctrl Pts',(-13.7308173358681,-0.913067424616607,
-25.2130517805888));
#32956=CARTESIAN_POINT('Ctrl Pts',(-13.727027503321,-0.910893971946881,
-26.4684878476616));
#32957=CARTESIAN_POINT('Ctrl Pts',(-13.7219681203734,-0.908224716400938,
-27.9762313767341));
#32958=CARTESIAN_POINT('Ctrl Pts',(-13.7195680699122,-0.906809058233843,
-28.9800397373653));
#32959=CARTESIAN_POINT('Ctrl Pts',(-13.7186976728711,-0.906178401053505,
-29.5428491015415));
#32960=CARTESIAN_POINT('Ctrl Pts',(-13.7186357852207,-0.906282813123428,
-29.660789949837));
#32961=CARTESIAN_POINT('Ctrl Pts',(-13.7190115634281,-0.907362158204569,
-29.9020317928129));
#32962=CARTESIAN_POINT('Ctrl Pts',(-13.7208604212975,-0.911336577467707,
-30.325235025951));
#32963=CARTESIAN_POINT('Ctrl Pts',(-13.7282606251036,-0.925829752687878,
-31.1855963678829));
#32964=CARTESIAN_POINT('Ctrl Pts',(-13.7403872876803,-0.948982661328658,
-32.1954921925686));
#32965=CARTESIAN_POINT('Ctrl Pts',(-13.7464168159969,-0.960613228500291,
-33.23190086473));
#32966=CARTESIAN_POINT('Ctrl Pts',(-13.7453894841776,-0.958641743033242,
-34.0218962636807));
#32967=CARTESIAN_POINT('Ctrl Pts',(-13.7362878221931,-0.940841001845677,
-34.8248369835493));
#32968=CARTESIAN_POINT('Ctrl Pts',(-13.7230148534269,-0.914724221017991,
-35.3684905729439));
#32969=CARTESIAN_POINT('Ctrl Pts',(-13.7096037677254,-0.888181576735158,
-35.7809178353369));
#32970=CARTESIAN_POINT('Ctrl Pts',(-13.6987970364002,-0.866293009330416,
-36.0686926579714));
#32971=CARTESIAN_POINT('Ctrl Pts',(-13.671569771722,-0.811851434411236,
-36.6277044534425));
#32972=CARTESIAN_POINT('Ctrl Pts',(-13.6108442528254,-0.691666448454139,
-37.5865862183716));
#32973=CARTESIAN_POINT('Ctrl Pts',(-13.4543351700341,-0.38735629443809,
-39.410125440965));
#32974=CARTESIAN_POINT('Ctrl Pts',(-13.3154256245931,-0.133535009111489,
-40.8132820690543));
#32975=CARTESIAN_POINT('Ctrl Pts',(-13.2698135895045,-0.0536258159889684,
-41.7861584105223));
#32976=CARTESIAN_POINT('Ctrl Pts',(-13.2607691869315,-0.0382086490022178,
-42.0069186031658));
#32977=CARTESIAN_POINT('Ctrl Pts',(-13.249920904955,-0.0216881580641046,
-42.3424365601118));
#32978=CARTESIAN_POINT('Ctrl Pts',(-13.2415653675482,-0.0109728837688096,
-42.6848694711389));
#32979=CARTESIAN_POINT('Ctrl Pts',(-13.2333766019918,-0.0034432187711669,
-43.1493156575476));
#32980=CARTESIAN_POINT('Ctrl Pts',(-13.2280268298175,-0.00466010038720499,
-43.7453358598114));
#32981=CARTESIAN_POINT('Ctrl Pts',(-13.2272319558763,-0.0158111723549196,
-44.4842770335761));
#32982=CARTESIAN_POINT('Ctrl Pts',(-13.2294437231869,-0.0263474888916997,
-45.1193836607821));
#32983=CARTESIAN_POINT('Ctrl Pts',(-13.2319498926359,-0.0310811416053446,
-45.6390704954399));
#32984=CARTESIAN_POINT('Ctrl Pts',(-13.2338868711412,-0.0315492607015707,
-46.0344362473196));
#32985=CARTESIAN_POINT('Ctrl Pts',(-13.2356169499968,-0.0276988033612878,
-46.4354227169262));
#32986=CARTESIAN_POINT('Ctrl Pts',(-13.2373207078135,-0.0151057061868057,
-46.9774255790535));
#32987=CARTESIAN_POINT('Ctrl Pts',(-13.23740813852,0.00481574300534024,
-47.3921808544604));
#32988=CARTESIAN_POINT('Ctrl Pts',(-13.2362799960084,0.0344572958470751,
-47.8123785321966));
#32989=CARTESIAN_POINT('Ctrl Pts',(-13.2357060059805,0.0521042990666052,
-48.0591893755926));
#32990=CARTESIAN_POINT('Ctrl Pts',(-13.2351927606908,0.0904170132760224,
-48.5752630537383));
#32991=CARTESIAN_POINT('Ctrl Pts',(-13.2356915822,0.162356093353207,-49.4747201946233));
#32992=CARTESIAN_POINT('Ctrl Pts',(-13.2387758395764,0.289567892495778,
-50.7837952574958));
#32993=CARTESIAN_POINT('Ctrl Pts',(-13.2419496016628,0.506524792408763,
-52.3789559389661));
#32994=CARTESIAN_POINT('Ctrl Pts',(-13.2402837800499,0.712955021961898,
-53.4596155677194));
#32995=CARTESIAN_POINT('Ctrl Pts',(-13.2372260073496,0.867360271403418,
-54.1403451215742));
#32996=CARTESIAN_POINT('Ctrl Pts',(-13.2358187991522,0.930601816612459,
-54.4102300948697));
#32997=CARTESIAN_POINT('Ctrl Pts',(-13.2322860209069,1.06528164613938,-54.9512789187452));
#32998=CARTESIAN_POINT('Ctrl Pts',(-13.2244696261721,1.31979280601954,-55.8929368737511));
#32999=CARTESIAN_POINT('Ctrl Pts',(-13.2043422333084,1.89931808336194,-57.760958976205));
#33000=CARTESIAN_POINT('Ctrl Pts',(-13.1860395153099,2.49496689438429,-59.3266437846506));
#33001=CARTESIAN_POINT('Ctrl Pts',(-13.1786973988809,2.94640801214391,-60.4171710430611));
#33002=CARTESIAN_POINT('Ctrl Pts',(-13.1778006140846,3.00533999312714,-60.5577447895152));
#33003=CARTESIAN_POINT('Ctrl Pts',(-13.1760857276374,3.12351075972109,-60.8328452449694));
#33004=CARTESIAN_POINT('Ctrl Pts',(-13.1732576712662,3.33685108478691,-61.3132715282016));
#33005=CARTESIAN_POINT('Ctrl Pts',(-13.1682631404326,3.78194623518818,-62.2589108855292));
#33006=CARTESIAN_POINT('Ctrl Pts',(-13.1639566703889,4.32129412642347,-63.311132796502));
#33007=CARTESIAN_POINT('Ctrl Pts',(-13.1606134591638,4.86461088337284,-64.3322721484445));
#33008=CARTESIAN_POINT('Ctrl Pts',(-13.1590189299969,5.16708564585913,-64.8946512637013));
#33009=CARTESIAN_POINT('Ctrl Pts',(-13.1580495871756,5.36539495771196,-65.2641506500079));
#33010=CARTESIAN_POINT('Ctrl Pts',(-13.1574229026006,5.49658427915357,-65.5090051569745));
#33011=CARTESIAN_POINT('Ctrl Pts',(-13.1568375735826,5.62605738444092,-65.7516476611018));
#33012=CARTESIAN_POINT('Ctrl Pts',(-13.156342424908,5.73748582541207,-65.9618743170868));
#33013=CARTESIAN_POINT('Ctrl Pts',(-13.156065649456,5.80057812624236,-66.0813973232228));
#33014=CARTESIAN_POINT('Ctrl Pts',(-13.1556555185828,5.8946184745073,-66.2600804080991));
#33015=CARTESIAN_POINT('Ctrl Pts',(-13.1553306040581,5.97165884095127,-66.4076735552761));
#33016=CARTESIAN_POINT('Ctrl Pts',(-13.1547985747114,6.09737128380689,-66.6505431582039));
#33017=CARTESIAN_POINT('Ctrl Pts',(-13.1543196231653,6.23514411689466,-66.9158510378909));
#33018=CARTESIAN_POINT('Ctrl Pts',(-13.153602518776,6.50542741523817,-67.4331524864784));
#33019=CARTESIAN_POINT('Ctrl Pts',(-13.1529416894374,6.97888521210212,-68.3319968438596));
#33020=CARTESIAN_POINT('Ctrl Pts',(-13.1533756026942,7.91707121646751,-70.0902548994053));
#33021=CARTESIAN_POINT('Ctrl Pts',(-13.1550149191262,8.71301264450386,-71.5666401701622));
#33022=CARTESIAN_POINT('Ctrl Pts',(-13.1550167477829,9.30829962930597,-72.6862300805453));
#33023=CARTESIAN_POINT('Ctrl Pts',(-13.1550132987847,9.44208731458616,-72.9378417548579));
#33024=CARTESIAN_POINT('Ctrl Pts',(-13.1550094243293,9.70890149614314,-73.439640119029));
#33025=CARTESIAN_POINT('Ctrl Pts',(-13.1550116726656,10.0425338980053,-74.0671190188514));
#33026=CARTESIAN_POINT('Ctrl Pts',(-13.1550139473927,10.4425138027341,-74.8193776474128));
#33027=CARTESIAN_POINT('Ctrl Pts',(-13.1550236387193,11.2422628255351,-76.3235076738163));
#33028=CARTESIAN_POINT('Ctrl Pts',(-13.1550542350392,11.9084264257806,-77.5764481272447));
#33029=CARTESIAN_POINT('Ctrl Pts',(-13.1550663076038,12.8783378734336,-79.4006160379139));
#33030=CARTESIAN_POINT('Ctrl Pts',(-13.1550725189431,13.3148957927065,-80.2216773986545));
#33031=CARTESIAN_POINT('Ctrl Pts',(-13.1550725189431,13.751417380096,-81.0426551007529));
#33032=CARTESIAN_POINT('Ctrl Pts',(-10.650042270715,0.000365604416696912,
24.8306342582036));
#33033=CARTESIAN_POINT('Ctrl Pts',(-10.6500740847871,0.000365622567542727,
24.7817549302156));
#33034=CARTESIAN_POINT('Ctrl Pts',(-10.6501074661384,0.00036562337306155,
24.7328768714934));
#33035=CARTESIAN_POINT('Ctrl Pts',(-10.6505009657446,0.000366460923403975,
24.1822613516484));
#33036=CARTESIAN_POINT('Ctrl Pts',(-10.6507985217012,0.000371994166762139,
23.1780652609194));
#33037=CARTESIAN_POINT('Ctrl Pts',(-10.6515005557346,0.000373666904444558,
21.1694597397613));
#33038=CARTESIAN_POINT('Ctrl Pts',(-10.6541120400923,0.00038789274538446,
19.665156351013));
#33039=CARTESIAN_POINT('Ctrl Pts',(-10.6596693248198,0.000395383454766491,
18.4140420097379));
#33040=CARTESIAN_POINT('Ctrl Pts',(-10.6623360336828,0.000397268296322463,
17.9112146130549));
#33041=CARTESIAN_POINT('Ctrl Pts',(-10.6690310413239,0.000403612342891138,
16.9071816012036));
#33042=CARTESIAN_POINT('Ctrl Pts',(-10.6833946406787,0.000413304763147904,
15.1533257466147));
#33043=CARTESIAN_POINT('Ctrl Pts',(-10.6970194022592,0.000446367192448972,
13.65123967164));
#33044=CARTESIAN_POINT('Ctrl Pts',(-10.7055652765539,0.000460391626742008,
12.396604516728));
#33045=CARTESIAN_POINT('Ctrl Pts',(-10.7090622322879,0.000462138910872274,
11.8956069838844));
#33046=CARTESIAN_POINT('Ctrl Pts',(-10.71618705933,0.000470076121078105,
10.8937100869054));
#33047=CARTESIAN_POINT('Ctrl Pts',(-10.7285262732713,0.00047519876483419,
9.13982057473998));
#33048=CARTESIAN_POINT('Ctrl Pts',(-10.7371199899901,0.000549749028605339,
7.63434823533288));
#33049=CARTESIAN_POINT('Ctrl Pts',(-10.7409414889771,0.000581970750385906,
6.50124583376022));
#33050=CARTESIAN_POINT('Ctrl Pts',(-10.741125057236,0.00259570504651152,
6.2267602931048));
#33051=CARTESIAN_POINT('Ctrl Pts',(-10.7392878601745,0.0130556637491886,
5.69935608672766));
#33052=CARTESIAN_POINT('Ctrl Pts',(-10.7315460602503,0.0436541037719018,
4.78794501792968));
#33053=CARTESIAN_POINT('Ctrl Pts',(-10.7076995794509,0.122780759576109,
3.04730104516099));
#33054=CARTESIAN_POINT('Ctrl Pts',(-10.7066809728001,0.117468289823324,
1.69232053262551));
#33055=CARTESIAN_POINT('Ctrl Pts',(-10.7467593103304,0.00918488066074162,
0.807560256124786));
#33056=CARTESIAN_POINT('Ctrl Pts',(-10.7519626603441,-0.00366202002174799,
0.712117710399012));
#33057=CARTESIAN_POINT('Ctrl Pts',(-10.7639074270763,-0.0346127647497942,
0.511455864381113));
#33058=CARTESIAN_POINT('Ctrl Pts',(-10.7885508414982,-0.100020448640092,
0.153839003233626));
#33059=CARTESIAN_POINT('Ctrl Pts',(-10.8325098601214,-0.224187245889308,
-0.385975306818793));
#33060=CARTESIAN_POINT('Ctrl Pts',(-10.8945063363775,-0.411994785650364,
-1.07465867196766));
#33061=CARTESIAN_POINT('Ctrl Pts',(-10.9836120542585,-0.696313194115999,
-2.04671364700164));
#33062=CARTESIAN_POINT('Ctrl Pts',(-11.0985387251657,-1.0796369475826,-3.35899297291827));
#33063=CARTESIAN_POINT('Ctrl Pts',(-11.171886523949,-1.32333560794751,-4.51856097352981));
#33064=CARTESIAN_POINT('Ctrl Pts',(-11.2013328963089,-1.42155056846409,
-5.2797800642824));
#33065=CARTESIAN_POINT('Ctrl Pts',(-11.2111143269299,-1.45404461826559,
-5.55455206726266));
#33066=CARTESIAN_POINT('Ctrl Pts',(-11.2273042145085,-1.50896260405546,
-6.1151264956646));
#33067=CARTESIAN_POINT('Ctrl Pts',(-11.2461025439228,-1.5759155046305,-7.07410960662139));
#33068=CARTESIAN_POINT('Ctrl Pts',(-11.2526452650533,-1.61081946830704,
-8.40897150999976));
#33069=CARTESIAN_POINT('Ctrl Pts',(-11.2470489340527,-1.60877605321405,
-9.68549243928046));
#33070=CARTESIAN_POINT('Ctrl Pts',(-11.2440734077914,-1.60906768347938,
-10.5492612995141));
#33071=CARTESIAN_POINT('Ctrl Pts',(-11.2435490792222,-1.61234277070398,
-11.0336093167728));
#33072=CARTESIAN_POINT('Ctrl Pts',(-11.2438342641925,-1.61546267429326,
-11.2726534396781));
#33073=CARTESIAN_POINT('Ctrl Pts',(-11.2443128285622,-1.61853239351233,
-11.4518215569661));
#33074=CARTESIAN_POINT('Ctrl Pts',(-11.244642200452,-1.6206336095023,-11.5831336298258));
#33075=CARTESIAN_POINT('Ctrl Pts',(-11.2451027763732,-1.62425012459985,
-11.8390401722566));
#33076=CARTESIAN_POINT('Ctrl Pts',(-11.245499325149,-1.62938835686632,-12.2885988051048));
#33077=CARTESIAN_POINT('Ctrl Pts',(-11.2445889024303,-1.63684237120518,
-13.4353109170186));
#33078=CARTESIAN_POINT('Ctrl Pts',(-11.2395266498228,-1.63217918211705,
-14.6942343328465));
#33079=CARTESIAN_POINT('Ctrl Pts',(-11.2351609777683,-1.62603694400866,
-15.9445922607557));
#33080=CARTESIAN_POINT('Ctrl Pts',(-11.2334936421301,-1.62345795467893,
-16.5687429713417));
#33081=CARTESIAN_POINT('Ctrl Pts',(-11.2327225455089,-1.62227723430756,
-17.067750318547));
#33082=CARTESIAN_POINT('Ctrl Pts',(-11.2325540866687,-1.6220597987632,-17.3172482783649));
#33083=CARTESIAN_POINT('Ctrl Pts',(-11.2325261615434,-1.62207425666605,
-17.5036664428382));
#33084=CARTESIAN_POINT('Ctrl Pts',(-11.2325208137062,-1.62208351508994,
-17.6286085458311));
#33085=CARTESIAN_POINT('Ctrl Pts',(-11.2325612882407,-1.62210073370477,
-17.8776147298047));
#33086=CARTESIAN_POINT('Ctrl Pts',(-11.232671136902,-1.62211043308421,-18.1271358360374));
#33087=CARTESIAN_POINT('Ctrl Pts',(-11.232848152788,-1.62211576375874,-18.3766187541966));
#33088=CARTESIAN_POINT('Ctrl Pts',(-11.2329838221442,-1.62211513012755,
-18.5326539574177));
#33089=CARTESIAN_POINT('Ctrl Pts',(-11.2331070956596,-1.6221125896366,-18.6575054790737));
#33090=CARTESIAN_POINT('Ctrl Pts',(-11.2332395984363,-1.62210818013834,
-18.782388318556));
#33091=CARTESIAN_POINT('Ctrl Pts',(-11.2336409056025,-1.62208945476857,
-19.1259219496441));
#33092=CARTESIAN_POINT('Ctrl Pts',(-11.2344837859616,-1.6220094344919,-19.6886807661217));
#33093=CARTESIAN_POINT('Ctrl Pts',(-11.2363723866999,-1.6217009240143,-20.6909416074719));
#33094=CARTESIAN_POINT('Ctrl Pts',(-11.2391462383464,-1.62084938520113,
-21.9473557243982));
#33095=CARTESIAN_POINT('Ctrl Pts',(-11.2412312975038,-1.61952792207212,
-22.9565995393526));
#33096=CARTESIAN_POINT('Ctrl Pts',(-11.242274432361,-1.61839941643641,-23.5870517203909));
#33097=CARTESIAN_POINT('Ctrl Pts',(-11.2426925129516,-1.61789843605843,
-23.8367914647876));
#33098=CARTESIAN_POINT('Ctrl Pts',(-11.2435586956675,-1.61672265215808,
-24.3368252655553));
#33099=CARTESIAN_POINT('Ctrl Pts',(-11.2451269298127,-1.61425020271206,
-25.2134378024879));
#33100=CARTESIAN_POINT('Ctrl Pts',(-11.2475055060001,-1.60997905946445,
-26.4689342912108));
#33101=CARTESIAN_POINT('Ctrl Pts',(-11.2502268402875,-1.60463449910935,
-27.9765152999299));
#33102=CARTESIAN_POINT('Ctrl Pts',(-11.2518846690841,-1.60184316346082,
-28.9803497799525));
#33103=CARTESIAN_POINT('Ctrl Pts',(-11.2526845529141,-1.6006395775289,-29.5426879338358));
#33104=CARTESIAN_POINT('Ctrl Pts',(-11.2530016388635,-1.60081773392649,
-29.6552622230315));
#33105=CARTESIAN_POINT('Ctrl Pts',(-11.2541316907256,-1.60272031221793,
-29.8896725175522));
#33106=CARTESIAN_POINT('Ctrl Pts',(-11.2573154165258,-1.60982261583138,
-30.301540866585));
#33107=CARTESIAN_POINT('Ctrl Pts',(-11.2674452022504,-1.63593292207713,
-31.14907078036));
#33108=CARTESIAN_POINT('Ctrl Pts',(-11.2829662937318,-1.67867594116351,
-32.1631522498279));
#33109=CARTESIAN_POINT('Ctrl Pts',(-11.2915281314437,-1.70059914198832,
-33.2233457754404));
#33110=CARTESIAN_POINT('Ctrl Pts',(-11.2913372530278,-1.69702533908146,
-34.040796301399));
#33111=CARTESIAN_POINT('Ctrl Pts',(-11.2813003503381,-1.66348397111689,
-34.8810679137723));
#33112=CARTESIAN_POINT('Ctrl Pts',(-11.2656754441518,-1.61374425816922,
-35.4558609216503));
#33113=CARTESIAN_POINT('Ctrl Pts',(-11.2496371955773,-1.56284553931442,
-35.8941482820626));
#33114=CARTESIAN_POINT('Ctrl Pts',(-11.2361268189636,-1.5200304380772,-36.2072998555992));
#33115=CARTESIAN_POINT('Ctrl Pts',(-11.2033119490395,-1.41487719118908,
-36.8046955101422));
#33116=CARTESIAN_POINT('Ctrl Pts',(-11.1324504370696,-1.18653719379417,
-37.8161641760809));
#33117=CARTESIAN_POINT('Ctrl Pts',(-10.9643210506542,-0.626215933228365,
-39.6790476430707));
#33118=CARTESIAN_POINT('Ctrl Pts',(-10.8244131060971,-0.212830624883642,
-41.0275041631862));
#33119=CARTESIAN_POINT('Ctrl Pts',(-10.7745159277284,-0.0923722011974562,
-41.8913882550613));
#33120=CARTESIAN_POINT('Ctrl Pts',(-10.7644262578356,-0.0667960726337613,
-42.100774923633));
#33121=CARTESIAN_POINT('Ctrl Pts',(-10.7521055535479,-0.0383479070046453,
-42.4150659459343));
#33122=CARTESIAN_POINT('Ctrl Pts',(-10.7423454245313,-0.0176547472067045,
-42.7402413431657));
#33123=CARTESIAN_POINT('Ctrl Pts',(-10.7324271418274,2.78979527989668E-5,
-43.183176332304));
#33124=CARTESIAN_POINT('Ctrl Pts',(-10.7251377519842,0.00629930368330282,
-43.7578870145591));
#33125=CARTESIAN_POINT('Ctrl Pts',(-10.722225468076,-0.00301713781191112,
-44.4792267442436));
#33126=CARTESIAN_POINT('Ctrl Pts',(-10.7226678608004,-0.0162766379087752,
-45.1065805339814));
#33127=CARTESIAN_POINT('Ctrl Pts',(-10.723545462882,-0.0242434157495022,
-45.6240842906144));
#33128=CARTESIAN_POINT('Ctrl Pts',(-10.7241700886567,-0.0273378354607701,
-46.0198535950271));
#33129=CARTESIAN_POINT('Ctrl Pts',(-10.7244611701676,-0.0258733857197475,
-46.4232938280841));
#33130=CARTESIAN_POINT('Ctrl Pts',(-10.7240076051067,-0.0154552381350729,
-46.9712845245771));
#33131=CARTESIAN_POINT('Ctrl Pts',(-10.7222645624063,0.00459948307228258,
-47.3936546235918));
#33132=CARTESIAN_POINT('Ctrl Pts',(-10.718999108387,0.0368370176291262,
-47.8231822015646));
#33133=CARTESIAN_POINT('Ctrl Pts',(-10.7168451494989,0.0551515656315621,
-48.0659853261855));
#33134=CARTESIAN_POINT('Ctrl Pts',(-10.7126438701732,0.0947533205243461,
-48.5802163021467));
#33135=CARTESIAN_POINT('Ctrl Pts',(-10.7055740500304,0.167328769646443,
-49.4743468728569));
#33136=CARTESIAN_POINT('Ctrl Pts',(-10.696191178236,0.292518409057621,-50.7801490138078));
#33137=CARTESIAN_POINT('Ctrl Pts',(-10.685966507583,0.505539967513752,-52.3744744198876));
#33138=CARTESIAN_POINT('Ctrl Pts',(-10.6796850250947,0.710589132746706,
-53.4575886581674));
#33139=CARTESIAN_POINT('Ctrl Pts',(-10.6758902888676,0.86539535947085,-54.1404651022306));
#33140=CARTESIAN_POINT('Ctrl Pts',(-10.6743290244131,0.928589158227978,
-54.4101838213268));
#33141=CARTESIAN_POINT('Ctrl Pts',(-10.6711673120377,1.06333532993672,-54.9514724741432));
#33142=CARTESIAN_POINT('Ctrl Pts',(-10.6655572848368,1.31795469515906,-55.8932151703261));
#33143=CARTESIAN_POINT('Ctrl Pts',(-10.6545603915192,1.8979592738655,-57.7615645354719));
#33144=CARTESIAN_POINT('Ctrl Pts',(-10.6471780206085,2.49412918412692,-59.3271216575852));
#33145=CARTESIAN_POINT('Ctrl Pts',(-10.6447300416341,2.9456620163703,-60.417473751051));
#33146=CARTESIAN_POINT('Ctrl Pts',(-10.6444864734455,3.00461178774495,-60.5580565408257));
#33147=CARTESIAN_POINT('Ctrl Pts',(-10.6440810657814,3.12281208563953,-60.8331584712121));
#33148=CARTESIAN_POINT('Ctrl Pts',(-10.6436200824622,3.33621174814075,-61.313592543236));
#33149=CARTESIAN_POINT('Ctrl Pts',(-10.643538445653,3.78141483002328,-62.2592373107269));
#33150=CARTESIAN_POINT('Ctrl Pts',(-10.6448782016157,4.32092352352002,-63.3114408017025));
#33151=CARTESIAN_POINT('Ctrl Pts',(-10.6466814092829,4.86435913111074,-64.3325544290971));
#33152=CARTESIAN_POINT('Ctrl Pts',(-10.6476978523703,5.16688179322271,-64.8949195301645));
#33153=CARTESIAN_POINT('Ctrl Pts',(-10.6483022010011,5.36521976706749,-65.2644093316576));
#33154=CARTESIAN_POINT('Ctrl Pts',(-10.6486804775451,5.49642366290479,-65.5092586775464));
#33155=CARTESIAN_POINT('Ctrl Pts',(-10.6490154796418,5.62591876808531,-65.7518925194187));
#33156=CARTESIAN_POINT('Ctrl Pts',(-10.6492563188143,5.73735950919451,-65.9621141841148));
#33157=CARTESIAN_POINT('Ctrl Pts',(-10.649377241876,5.80045868759503,-66.0816343708117));
#33158=CARTESIAN_POINT('Ctrl Pts',(-10.6495408928145,5.89450845196145,-66.2603135957034));
#33159=CARTESIAN_POINT('Ctrl Pts',(-10.6496390058144,5.97156070475074,-66.4079010048767));
#33160=CARTESIAN_POINT('Ctrl Pts',(-10.6497386183767,6.09728728657649,-66.6507639951798));
#33161=CARTESIAN_POINT('Ctrl Pts',(-10.6498293290638,6.23507055885311,-66.9160539783043));
#33162=CARTESIAN_POINT('Ctrl Pts',(-10.6499677310158,6.50536736913276,-67.4333300460254));
#33163=CARTESIAN_POINT('Ctrl Pts',(-10.6501114230242,6.97884573772282,-68.3321241661668));
#33164=CARTESIAN_POINT('Ctrl Pts',(-10.6500963227376,7.91702070557873,-70.0903209123917));
#33165=CARTESIAN_POINT('Ctrl Pts',(-10.6498795836695,8.71297626916867,-71.566667654021));
#33166=CARTESIAN_POINT('Ctrl Pts',(-10.6499011960763,9.30829482662004,-72.6862697910305));
#33167=CARTESIAN_POINT('Ctrl Pts',(-10.6499047637529,9.44208195132325,-72.9378791448345));
#33168=CARTESIAN_POINT('Ctrl Pts',(-10.649910300367,9.70889818600605,-73.4396768553508));
#33169=CARTESIAN_POINT('Ctrl Pts',(-10.6499144874314,10.0425345294427,-74.0671506210093));
#33170=CARTESIAN_POINT('Ctrl Pts',(-10.6499151827135,10.442516342387,-74.8194073811515));
#33171=CARTESIAN_POINT('Ctrl Pts',(-10.6499111240893,11.2422680992346,-76.3235337653213));
#33172=CARTESIAN_POINT('Ctrl Pts',(-10.6499030565891,11.9084448061482,-77.5764608335406));
#33173=CARTESIAN_POINT('Ctrl Pts',(-10.6499043672714,12.8783648733455,-79.4006205549652));
#33174=CARTESIAN_POINT('Ctrl Pts',(-10.6499050450884,13.3149270582603,-80.2216773804913));
#33175=CARTESIAN_POINT('Ctrl Pts',(-10.6499050450884,13.7514486456498,-81.0426550825896));
#33176=CARTESIAN_POINT('Ctrl Pts',(-8.14412189745736,-0.000152373436558693,
24.8306349266468));
#33177=CARTESIAN_POINT('Ctrl Pts',(-8.14414623195988,-0.000152375382121277,
24.7817556196536));
#33178=CARTESIAN_POINT('Ctrl Pts',(-8.1441717670015,-0.000152392198849738,
24.7328776300862));
#33179=CARTESIAN_POINT('Ctrl Pts',(-8.14447269564718,-0.000151918598724809,
24.1822607486252));
#33180=CARTESIAN_POINT('Ctrl Pts',(-8.14469979318938,-0.000147878987651978,
23.1780515264225));
#33181=CARTESIAN_POINT('Ctrl Pts',(-8.14523667747614,-0.000147765295944936,
21.1694450065643));
#33182=CARTESIAN_POINT('Ctrl Pts',(-8.14723298556225,-0.000137574708599251,
19.6651083293772));
#33183=CARTESIAN_POINT('Ctrl Pts',(-8.15148329064228,-0.000132911415445355,
18.4139794726141));
#33184=CARTESIAN_POINT('Ctrl Pts',(-8.15352302280712,-0.000132173521193853,
17.9111511130494));
#33185=CARTESIAN_POINT('Ctrl Pts',(-8.15864383708089,-0.000129196754508978,
16.9071094951091));
#33186=CARTESIAN_POINT('Ctrl Pts',(-8.16963053348841,-0.000125920397975024,
15.153243554802));
#33187=CARTESIAN_POINT('Ctrl Pts',(-8.18004947280553,-0.000101684712158349,
13.6510767010308));
#33188=CARTESIAN_POINT('Ctrl Pts',(-8.18658467464386,-8.88278457007875E-5,
12.3964004428332));
#33189=CARTESIAN_POINT('Ctrl Pts',(-8.18925923233085,-8.64346045489019E-5,
11.8953895179443));
#33190=CARTESIAN_POINT('Ctrl Pts',(-8.1947078772434,-7.69523185917187E-5,
10.8934820559683));
#33191=CARTESIAN_POINT('Ctrl Pts',(-8.20414480257374,-6.48462924612067E-5,
9.13949375918252));
#33192=CARTESIAN_POINT('Ctrl Pts',(-8.2107091480591,2.93700242304431E-6,
7.63402123554715));
#33193=CARTESIAN_POINT('Ctrl Pts',(-8.21362816021825,3.46121833831947E-5,
6.50030730567718));
#33194=CARTESIAN_POINT('Ctrl Pts',(-8.2139773816664,0.00271505638709518,
6.21868089666948));
#33195=CARTESIAN_POINT('Ctrl Pts',(-8.21366765236856,0.01653627011796,5.68352490005895));
#33196=CARTESIAN_POINT('Ctrl Pts',(-8.21103236130824,0.0566635365252091,
4.76263764161942));
#33197=CARTESIAN_POINT('Ctrl Pts',(-8.20152740606986,0.158430126564625,
3.0271363314686));
#33198=CARTESIAN_POINT('Ctrl Pts',(-8.20073061637961,0.149251458175202,
1.71872219634129));
#33199=CARTESIAN_POINT('Ctrl Pts',(-8.21717066237738,0.0181890322585064,
0.881529631657107));
#33200=CARTESIAN_POINT('Ctrl Pts',(-8.2193040340341,0.00329453289535601,
0.794356070514653));
#33201=CARTESIAN_POINT('Ctrl Pts',(-8.22416980127459,-0.033563900965499,
0.607050496827644));
#33202=CARTESIAN_POINT('Ctrl Pts',(-8.23413279979194,-0.112592668023086,
0.269906771666699));
#33203=CARTESIAN_POINT('Ctrl Pts',(-8.25161317521362,-0.267541466617309,
-0.25065980001266));
#33204=CARTESIAN_POINT('Ctrl Pts',(-8.2760674551824,-0.509570377892601,
-0.926107372523026));
#33205=CARTESIAN_POINT('Ctrl Pts',(-8.31129710119725,-0.885116143113864,
-1.89016358670453));
#33206=CARTESIAN_POINT('Ctrl Pts',(-8.35820655882308,-1.40718620794638,
-3.20511805596597));
#33207=CARTESIAN_POINT('Ctrl Pts',(-8.39167103174164,-1.75864819329131,
-4.39735605748105));
#33208=CARTESIAN_POINT('Ctrl Pts',(-8.4057490725845,-1.90357909164309,-5.19797714431349));
#33209=CARTESIAN_POINT('Ctrl Pts',(-8.41018696867969,-1.95004819727558,
-5.47978199297613));
#33210=CARTESIAN_POINT('Ctrl Pts',(-8.41764518232782,-2.0293328309496,-6.05846771470832));
#33211=CARTESIAN_POINT('Ctrl Pts',(-8.42608946693865,-2.12510790014958,
-7.04372337069025));
#33212=CARTESIAN_POINT('Ctrl Pts',(-8.42835688611333,-2.17335745278486,
-8.4058069611693));
#33213=CARTESIAN_POINT('Ctrl Pts',(-8.42483355820332,-2.16838683398674,
-9.69002623777674));
#33214=CARTESIAN_POINT('Ctrl Pts',(-8.4228693653896,-2.16758867316197,-10.549647857504));
#33215=CARTESIAN_POINT('Ctrl Pts',(-8.42227667941022,-2.1714754449322,-11.0287258129748));
#33216=CARTESIAN_POINT('Ctrl Pts',(-8.4222265668368,-2.17548571011368,-11.2641593891017));
#33217=CARTESIAN_POINT('Ctrl Pts',(-8.4223066588321,-2.17949860847749,-11.4403532700108));
#33218=CARTESIAN_POINT('Ctrl Pts',(-8.42237861265133,-2.18234534725527,
-11.5735122851675));
#33219=CARTESIAN_POINT('Ctrl Pts',(-8.42241335915678,-2.18714051116029,
-11.8308485666504));
#33220=CARTESIAN_POINT('Ctrl Pts',(-8.42226798867896,-2.19385085028673,
-12.2837525929814));
#33221=CARTESIAN_POINT('Ctrl Pts',(-8.42090827535907,-2.20284084437885,
-13.4368375872061));
#33222=CARTESIAN_POINT('Ctrl Pts',(-8.41742083334402,-2.19452611715802,
-14.699424889331));
#33223=CARTESIAN_POINT('Ctrl Pts',(-8.41459096562853,-2.18466983175675,
-15.9491420610126));
#33224=CARTESIAN_POINT('Ctrl Pts',(-8.41351488671319,-2.18063370066728,
-16.5720520403308));
#33225=CARTESIAN_POINT('Ctrl Pts',(-8.41300046580358,-2.17877051369586,
-17.0694513279955));
#33226=CARTESIAN_POINT('Ctrl Pts',(-8.41287266139027,-2.17841281520911,
-17.3179509620184));
#33227=CARTESIAN_POINT('Ctrl Pts',(-8.41283514635732,-2.17841198490692,
-17.5035714183381));
#33228=CARTESIAN_POINT('Ctrl Pts',(-8.4128192890245,-2.17840958154783,-17.6287745384218));
#33229=CARTESIAN_POINT('Ctrl Pts',(-8.41282274470808,-2.1783995227068,-17.8778185403976));
#33230=CARTESIAN_POINT('Ctrl Pts',(-8.41287433890386,-2.17837876830243,
-18.1275208893485));
#33231=CARTESIAN_POINT('Ctrl Pts',(-8.41297294837519,-2.17835392065712,
-18.3770615934934));
#33232=CARTESIAN_POINT('Ctrl Pts',(-8.41305237217696,-2.17833577105845,
-18.5331408135074));
#33233=CARTESIAN_POINT('Ctrl Pts',(-8.4131264249278,-2.17832044242199,-18.6580119473273));
#33234=CARTESIAN_POINT('Ctrl Pts',(-8.41320707340361,-2.17830426803329,
-18.7829114742903));
#33235=CARTESIAN_POINT('Ctrl Pts',(-8.41345624825908,-2.17825882731944,
-19.1264686399524));
#33236=CARTESIAN_POINT('Ctrl Pts',(-8.41400000345279,-2.17817104749403,
-19.6891521495847));
#33237=CARTESIAN_POINT('Ctrl Pts',(-8.41528017288101,-2.17804976165826,
-20.6909497614675));
#33238=CARTESIAN_POINT('Ctrl Pts',(-8.41726103341462,-2.1779744183845,-21.9461768404187));
#33239=CARTESIAN_POINT('Ctrl Pts',(-8.41893477480712,-2.17823712701764,
-22.953825983149));
#33240=CARTESIAN_POINT('Ctrl Pts',(-8.41986349686732,-2.17850502468349,
-23.5830767841885));
#33241=CARTESIAN_POINT('Ctrl Pts',(-8.42024378452539,-2.17862331222871,
-23.8321153579562));
#33242=CARTESIAN_POINT('Ctrl Pts',(-8.42106293419616,-2.17892596672298,
-24.3310626190291));
#33243=CARTESIAN_POINT('Ctrl Pts',(-8.42261468751758,-2.17958483043597,
-25.2061040655729));
#33244=CARTESIAN_POINT('Ctrl Pts',(-8.42511899294663,-2.18087935081873,
-26.4606390371043));
#33245=CARTESIAN_POINT('Ctrl Pts',(-8.42808089250611,-2.1824101925373,-27.9687820656938));
#33246=CARTESIAN_POINT('Ctrl Pts',(-8.42988072285208,-2.1833225916283,-28.9744904395833));
#33247=CARTESIAN_POINT('Ctrl Pts',(-8.43072515641183,-2.18365366003855,
-29.5378159164111));
#33248=CARTESIAN_POINT('Ctrl Pts',(-8.43096689351811,-2.18428588440253,
-29.6460087767788));
#33249=CARTESIAN_POINT('Ctrl Pts',(-8.43167406029457,-2.1876698352998,-29.8750129034852));
#33250=CARTESIAN_POINT('Ctrl Pts',(-8.43346090281294,-2.19874066252348,
-30.2778441726034));
#33251=CARTESIAN_POINT('Ctrl Pts',(-8.43877583514437,-2.2373949958194,-31.1153501423125));
#33252=CARTESIAN_POINT('Ctrl Pts',(-8.44693993544396,-2.30051991094785,
-32.1332707729797));
#33253=CARTESIAN_POINT('Ctrl Pts',(-8.45187694204408,-2.334473844321,-33.2140524330932));
#33254=CARTESIAN_POINT('Ctrl Pts',(-8.4522445888991,-2.33066489370667,-34.0552226771806));
#33255=CARTESIAN_POINT('Ctrl Pts',(-8.44752749223351,-2.28222892522994,
-34.9271681885516));
#33256=CARTESIAN_POINT('Ctrl Pts',(-8.43973025078375,-2.20888269376983,
-35.5269140529488));
#33257=CARTESIAN_POINT('Ctrl Pts',(-8.43168921619344,-2.133704304946,-35.984639162063));
#33258=CARTESIAN_POINT('Ctrl Pts',(-8.42470428825363,-2.06936251403802,
-36.3161971208814));
#33259=CARTESIAN_POINT('Ctrl Pts',(-8.40841115558265,-1.91462768039653,
-36.9382373792022));
#33260=CARTESIAN_POINT('Ctrl Pts',(-8.37476858189967,-1.58581660983551,
-37.9769230783518));
#33261=CARTESIAN_POINT('Ctrl Pts',(-8.30240748369846,-0.811573802930985,
-39.8436351201298));
#33262=CARTESIAN_POINT('Ctrl Pts',(-8.24766419492162,-0.281754963899915,
-41.1725199402397));
#33263=CARTESIAN_POINT('Ctrl Pts',(-8.22703915820806,-0.138584152464493,
-41.9674971713857));
#33264=CARTESIAN_POINT('Ctrl Pts',(-8.22279741361054,-0.106018153825827,
-42.1695350413675));
#33265=CARTESIAN_POINT('Ctrl Pts',(-8.21760452678912,-0.0696723394394581,
-42.4698336926041));
#33266=CARTESIAN_POINT('Ctrl Pts',(-8.21345399549118,-0.0419794705770708,
-42.783383071773));
#33267=CARTESIAN_POINT('Ctrl Pts',(-8.20920443802888,-0.0168922801706015,
-43.2117380270997));
#33268=CARTESIAN_POINT('Ctrl Pts',(-8.2060056324919,-0.00434463815486024,
-43.7719541949028));
#33269=CARTESIAN_POINT('Ctrl Pts',(-8.20454082076387,-0.0104625108048303,
-44.4815998892878));
#33270=CARTESIAN_POINT('Ctrl Pts',(-8.20440922525151,-0.0236201178969525,
-45.1041772238153));
#33271=CARTESIAN_POINT('Ctrl Pts',(-8.20441862179947,-0.0321411125244865,
-45.6207303121886));
#33272=CARTESIAN_POINT('Ctrl Pts',(-8.20434989009874,-0.0356782660657121,
-46.0172516471628));
#33273=CARTESIAN_POINT('Ctrl Pts',(-8.20406992251926,-0.0343648106023225,
-46.4229125033992));
#33274=CARTESIAN_POINT('Ctrl Pts',(-8.20323902185318,-0.0232669902564738,
-46.9758006019662));
#33275=CARTESIAN_POINT('Ctrl Pts',(-8.20188731183341,-0.00111372268798417,
-47.4040701896738));
#33276=CARTESIAN_POINT('Ctrl Pts',(-8.19979619418406,0.0351710604500778,
-47.8406800108478));
#33277=CARTESIAN_POINT('Ctrl Pts',(-8.19836170883178,0.0553133867555958,
-48.0821468140958));
#33278=CARTESIAN_POINT('Ctrl Pts',(-8.19535407046343,0.099077802122036,
-48.596971610594));
#33279=CARTESIAN_POINT('Ctrl Pts',(-8.18979813141032,0.178617138424551,
-49.4900316660884));
#33280=CARTESIAN_POINT('Ctrl Pts',(-8.18131347626536,0.313332652944236,
-50.7942648710663));
#33281=CARTESIAN_POINT('Ctrl Pts',(-8.17141615936791,0.535289599500542,
-52.3844504500429));
#33282=CARTESIAN_POINT('Ctrl Pts',(-8.16568083729471,0.743640919654865,
-53.4639249249685));
#33283=CARTESIAN_POINT('Ctrl Pts',(-8.16260421353783,0.899310397360863,
-54.1442403972218));
#33284=CARTESIAN_POINT('Ctrl Pts',(-8.16135401544335,0.962665926680855,
-54.41276557711));
#33285=CARTESIAN_POINT('Ctrl Pts',(-8.15887544372053,1.09733691858376,-54.9520352187707));
#33286=CARTESIAN_POINT('Ctrl Pts',(-8.15459691068634,1.3507946586784,-55.8907769762969));
#33287=CARTESIAN_POINT('Ctrl Pts',(-8.14657838814605,1.9255036615678,-57.7554882022754));
#33288=CARTESIAN_POINT('Ctrl Pts',(-8.14149181504208,2.51535089116785,-59.3213134096067));
#33289=CARTESIAN_POINT('Ctrl Pts',(-8.13972928395813,2.96457286522012,-60.4132064701784));
#33290=CARTESIAN_POINT('Ctrl Pts',(-8.13955344139843,3.02301727273934,-60.5535137041616));
#33291=CARTESIAN_POINT('Ctrl Pts',(-8.13926470646828,3.14029361968222,-60.8283650932639));
#33292=CARTESIAN_POINT('Ctrl Pts',(-8.13894720952011,3.35193263257086,-61.3083107938966));
#33293=CARTESIAN_POINT('Ctrl Pts',(-8.13894762339317,3.79342717132554,-62.2533982752636));
#33294=CARTESIAN_POINT('Ctrl Pts',(-8.1400365552858,4.32849389946224,-63.3055109143046));
#33295=CARTESIAN_POINT('Ctrl Pts',(-8.14146711027879,4.86804693212373,-64.3270786203418));
#33296=CARTESIAN_POINT('Ctrl Pts',(-8.14226817508642,5.16871692523809,-64.889895156736));
#33297=CARTESIAN_POINT('Ctrl Pts',(-8.14274451908316,5.36601178377058,-65.2597759526672));
#33298=CARTESIAN_POINT('Ctrl Pts',(-8.14304244247713,5.49657582154972,-65.5049110580499));
#33299=CARTESIAN_POINT('Ctrl Pts',(-8.14330765702863,5.62551558736444,-65.7478677462274));
#33300=CARTESIAN_POINT('Ctrl Pts',(-8.14349861608814,5.73655761778692,-65.9584086817351));
#33301=CARTESIAN_POINT('Ctrl Pts',(-8.14359486596038,5.79945465324739,-66.0781220853356));
#33302=CARTESIAN_POINT('Ctrl Pts',(-8.14372550172375,5.89322767828473,-66.2571021403003));
#33303=CARTESIAN_POINT('Ctrl Pts',(-8.1438054888816,5.97010448362115,-66.4049637463919));
#33304=CARTESIAN_POINT('Ctrl Pts',(-8.14388912480341,6.09562186726871,-66.6483134049626));
#33305=CARTESIAN_POINT('Ctrl Pts',(-8.14396545620633,6.2331613153188,-66.9139921069247));
#33306=CARTESIAN_POINT('Ctrl Pts',(-8.14408091872707,6.50319897559478,-67.4320256493946));
#33307=CARTESIAN_POINT('Ctrl Pts',(-8.14420049505799,6.97661293040496,-68.3319171006395));
#33308=CARTESIAN_POINT('Ctrl Pts',(-8.14417979226255,7.9158419811929,-70.0915028523489));
#33309=CARTESIAN_POINT('Ctrl Pts',(-8.14399378791187,8.71296190818585,-71.5675323137367));
#33310=CARTESIAN_POINT('Ctrl Pts',(-8.14401129173376,9.30773813911128,-72.6861798589276));
#33311=CARTESIAN_POINT('Ctrl Pts',(-8.14401378822158,9.44155634426351,-72.9378587433967));
#33312=CARTESIAN_POINT('Ctrl Pts',(-8.14401781863899,9.70835096815867,-73.4396327793342));
#33313=CARTESIAN_POINT('Ctrl Pts',(-8.14402139260452,10.0419982314087,-74.0671403835795));
#33314=CARTESIAN_POINT('Ctrl Pts',(-8.14402217907996,10.441980091082,-74.8193995595811));
#33315=CARTESIAN_POINT('Ctrl Pts',(-8.14401992121061,11.2417489323043,-76.3235460780868));
#33316=CARTESIAN_POINT('Ctrl Pts',(-8.14401659738412,11.9079355425531,-77.5764690921898));
#33317=CARTESIAN_POINT('Ctrl Pts',(-8.1440188815399,12.877844418806,-79.4006130100031));
#33318=CARTESIAN_POINT('Ctrl Pts',(-8.14402005669186,13.3144091843969,-80.2216773875901));
#33319=CARTESIAN_POINT('Ctrl Pts',(-8.14402005669182,13.7509307717864,-81.0426550896885));
#33320=CARTESIAN_POINT('Ctrl Pts',(-5.63798874401576,-0.000197003472309253,
24.8306349854119));
#33321=CARTESIAN_POINT('Ctrl Pts',(-5.63800558191124,-0.000197010017902819,
24.7817556802439));
#33322=CARTESIAN_POINT('Ctrl Pts',(-5.63802322829952,-0.000196997600998546,
24.732877683161));
#33323=CARTESIAN_POINT('Ctrl Pts',(-5.6382321992011,-0.000197727157601966,
24.1822611386521));
#33324=CARTESIAN_POINT('Ctrl Pts',(-5.63839540854526,-0.000203328251643161,
23.1780545711597));
#33325=CARTESIAN_POINT('Ctrl Pts',(-5.63876707035559,-0.000204428222765414,
21.1694483770277));
#33326=CARTESIAN_POINT('Ctrl Pts',(-5.64016391586993,-0.000218427565831332,
19.6651182773234));
#33327=CARTESIAN_POINT('Ctrl Pts',(-5.64311246961886,-0.000224802933236796,
18.4139922902723));
#33328=CARTESIAN_POINT('Ctrl Pts',(-5.64452522473937,-0.000225999139705922,
17.9111644969149));
#33329=CARTESIAN_POINT('Ctrl Pts',(-5.64807365157005,-0.000230617251699585,
16.9071248156262));
#33330=CARTESIAN_POINT('Ctrl Pts',(-5.6556821342335,-0.000236390082593806,
15.1532608344032));
#33331=CARTESIAN_POINT('Ctrl Pts',(-5.66292925317201,-0.000267962939935839,
13.6511084868801));
#33332=CARTESIAN_POINT('Ctrl Pts',(-5.66747180552725,-0.000282218227139333,
12.3964390741229));
#33333=CARTESIAN_POINT('Ctrl Pts',(-5.66932651967778,-0.000283883146473219,
11.895428735672));
#33334=CARTESIAN_POINT('Ctrl Pts',(-5.67311242407095,-0.000293045511818167,
10.8935268493743));
#33335=CARTESIAN_POINT('Ctrl Pts',(-5.67966191248225,-0.000299082491310505,
9.13954002036197));
#33336=CARTESIAN_POINT('Ctrl Pts',(-5.68431080553268,-0.000384941206993508,
7.63411967127975));
#33337=CARTESIAN_POINT('Ctrl Pts',(-5.686372275596,-0.000411482825566298,
6.50039814288972));
#33338=CARTESIAN_POINT('Ctrl Pts',(-5.68684776179194,0.00229630643279153,
6.21845427742025));
#33339=CARTESIAN_POINT('Ctrl Pts',(-5.68786142444616,0.0162632612901432,
5.68295491308527));
#33340=CARTESIAN_POINT('Ctrl Pts',(-5.68971236172501,0.0567615293401514,
4.76167563319915));
#33341=CARTESIAN_POINT('Ctrl Pts',(-5.69297084014264,0.159517117332154,
3.02639313928253));
#33342=CARTESIAN_POINT('Ctrl Pts',(-5.69264654080951,0.149618749208594,
1.72037399230591));
#33343=CARTESIAN_POINT('Ctrl Pts',(-5.68856841900556,0.0173647191069126,
0.885235947772052));
#33344=CARTESIAN_POINT('Ctrl Pts',(-5.68803099617261,0.00238318925849841,
0.798409810767109));
#33345=CARTESIAN_POINT('Ctrl Pts',(-5.68680608971042,-0.0347544439548622,
0.61164864292997));
#33346=CARTESIAN_POINT('Ctrl Pts',(-5.68428941420376,-0.114424015372209,
0.275299005848681));
#33347=CARTESIAN_POINT('Ctrl Pts',(-5.67990871577964,-0.270957526740268,
-0.244611018683231));
#33348=CARTESIAN_POINT('Ctrl Pts',(-5.67369396529163,-0.515273456664773,
-0.919737137559079));
#33349=CARTESIAN_POINT('Ctrl Pts',(-5.6646921537697,-0.894616695793402,
-1.88381123416328));
#33350=CARTESIAN_POINT('Ctrl Pts',(-5.65218739183062,-1.42140596824095,
-3.19924008823192));
#33351=CARTESIAN_POINT('Ctrl Pts',(-5.64245712789792,-1.77696374815495,
-4.3925641794195));
#33352=CARTESIAN_POINT('Ctrl Pts',(-5.63796441630677,-1.92370576951919,
-5.1946090699866));
#33353=CARTESIAN_POINT('Ctrl Pts',(-5.63650687495268,-1.9706510187358,-5.47668455904916));
#33354=CARTESIAN_POINT('Ctrl Pts',(-5.63387712655626,-2.05079010518533,
-6.0560630588307));
#33355=CARTESIAN_POINT('Ctrl Pts',(-5.63037973233777,-2.14756911677532,
-7.04237048376366));
#33356=CARTESIAN_POINT('Ctrl Pts',(-5.62771024023403,-2.19629179135161,
-8.40560259571312));
#33357=CARTESIAN_POINT('Ctrl Pts',(-5.62646453378276,-2.19120634551966,
-9.69018239553766));
#33358=CARTESIAN_POINT('Ctrl Pts',(-5.62553693460616,-2.19025626927096,
-10.5496403261192));
#33359=CARTESIAN_POINT('Ctrl Pts',(-5.62492773711517,-2.19409035070739,
-11.028506356485));
#33360=CARTESIAN_POINT('Ctrl Pts',(-5.62458342773447,-2.19809200746593,
-11.2637947462558));
#33361=CARTESIAN_POINT('Ctrl Pts',(-5.6243036959921,-2.20210252034327,-11.4398681067028));
#33362=CARTESIAN_POINT('Ctrl Pts',(-5.62410483522145,-2.20495370924458,
-11.5730994778588));
#33363=CARTESIAN_POINT('Ctrl Pts',(-5.62372750411003,-2.20974250570501,
-11.8304896121988));
#33364=CARTESIAN_POINT('Ctrl Pts',(-5.62310049238311,-2.21643113870861,
-12.283523795246));
#33365=CARTESIAN_POINT('Ctrl Pts',(-5.62168000244819,-2.22531034670341,
-13.4368678683667));
#33366=CARTESIAN_POINT('Ctrl Pts',(-5.62061026542929,-2.21676141606032,
-14.699629050403));
#33367=CARTESIAN_POINT('Ctrl Pts',(-5.61992998041975,-2.20662324725371,
-15.9492985747393));
#33368=CARTESIAN_POINT('Ctrl Pts',(-5.61970956077904,-2.20251357405667,
-16.5721572080187));
#33369=CARTESIAN_POINT('Ctrl Pts',(-5.61958734393837,-2.20060253110823,
-17.0694810153417));
#33370=CARTESIAN_POINT('Ctrl Pts',(-5.61954956517472,-2.2002384474806,-17.3179365617655));
#33371=CARTESIAN_POINT('Ctrl Pts',(-5.61952801743157,-2.20023584646593,
-17.5035209125398));
#33372=CARTESIAN_POINT('Ctrl Pts',(-5.61952113110232,-2.20023320019289,
-17.6287345805335));
#33373=CARTESIAN_POINT('Ctrl Pts',(-5.61953393535414,-2.20022439388902,
-17.8777776408766));
#33374=CARTESIAN_POINT('Ctrl Pts',(-5.61958764142248,-2.20021267485849,
-18.1274866656909));
#33375=CARTESIAN_POINT('Ctrl Pts',(-5.61967219934989,-2.20019766750374,
-18.377026362966));
#33376=CARTESIAN_POINT('Ctrl Pts',(-5.61973830896478,-2.20018791517279,
-18.5331054168968));
#33377=CARTESIAN_POINT('Ctrl Pts',(-5.61979786202761,-2.20017981841732,
-18.6579753380496));
#33378=CARTESIAN_POINT('Ctrl Pts',(-5.61986172050493,-2.20017160267944,
-18.7828733819617));
#33379=CARTESIAN_POINT('Ctrl Pts',(-5.62005763737625,-2.20015075591428,
-19.1264263327723));
#33380=CARTESIAN_POINT('Ctrl Pts',(-5.62046272300978,-2.2001199750147,-19.6890959425505));
#33381=CARTESIAN_POINT('Ctrl Pts',(-5.62134039297357,-2.20012734742513,
-20.690855324408));
#33382=CARTESIAN_POINT('Ctrl Pts',(-5.62247078887583,-2.20028948776679,
-21.9459931764134));
#33383=CARTESIAN_POINT('Ctrl Pts',(-5.62304153313537,-2.20076782870844,
-22.9535436359179));
#33384=CARTESIAN_POINT('Ctrl Pts',(-5.62311736659782,-2.20119855016699,
-23.5827128224497));
#33385=CARTESIAN_POINT('Ctrl Pts',(-5.62312505609341,-2.20138895511271,
-23.8316904452359));
#33386=CARTESIAN_POINT('Ctrl Pts',(-5.62307863861334,-2.20184988096975,
-24.3305490629185));
#33387=CARTESIAN_POINT('Ctrl Pts',(-5.62284832796686,-2.20283552305635,
-25.2054616107245));
#33388=CARTESIAN_POINT('Ctrl Pts',(-5.6222622772683,-2.20461588646114,-26.4599423345342));
#33389=CARTESIAN_POINT('Ctrl Pts',(-5.62144992063832,-2.20679856145,-27.9681630936482));
#33390=CARTESIAN_POINT('Ctrl Pts',(-5.6211590510458,-2.20797434227957,-28.9740718190661));
#33391=CARTESIAN_POINT('Ctrl Pts',(-5.62111618801636,-2.20844966017214,
-29.5375147504093));
#33392=CARTESIAN_POINT('Ctrl Pts',(-5.62109422172764,-2.20911507239076,
-29.6455549435117));
#33393=CARTESIAN_POINT('Ctrl Pts',(-5.62100876715226,-2.21258346457478,
-29.8743811766298));
#33394=CARTESIAN_POINT('Ctrl Pts',(-5.62075401832145,-2.22382403270066,
-30.2769177522939));
#33395=CARTESIAN_POINT('Ctrl Pts',(-5.61990887107815,-2.26295805170465,
-31.1141259057382));
#33396=CARTESIAN_POINT('Ctrl Pts',(-5.61848957316824,-2.32674809384181,
-32.1322815139189));
#33397=CARTESIAN_POINT('Ctrl Pts',(-5.61781000352031,-2.36116406208853,
-33.2138797468871));
#33398=CARTESIAN_POINT('Ctrl Pts',(-5.61809400321541,-2.35739190047119,
-34.0559545601601));
#33399=CARTESIAN_POINT('Ctrl Pts',(-5.61961452951742,-2.30835269989843,
-34.9291041558053));
#33400=CARTESIAN_POINT('Ctrl Pts',(-5.62177024593562,-2.23404940008006,
-35.529744944464));
#33401=CARTESIAN_POINT('Ctrl Pts',(-5.62393780073057,-2.15796077965923,
-35.9881178443849));
#33402=CARTESIAN_POINT('Ctrl Pts',(-5.62584009583325,-2.09278630793423,
-36.3202547621105));
#33403=CARTESIAN_POINT('Ctrl Pts',(-5.63013513192705,-1.9363345551221,-36.9430040876631));
#33404=CARTESIAN_POINT('Ctrl Pts',(-5.63860506790231,-1.60404305886794,
-37.9824489926659));
#33405=CARTESIAN_POINT('Ctrl Pts',(-5.65541457729167,-0.823249020271413,
-39.8498632334892));
#33406=CARTESIAN_POINT('Ctrl Pts',(-5.66661670520381,-0.28703789039762,
-41.1786802522904));
#33407=CARTESIAN_POINT('Ctrl Pts',(-5.67105654561514,-0.14240251435379,
-41.9710438412748));
#33408=CARTESIAN_POINT('Ctrl Pts',(-5.67202248528354,-0.109518971665621,
-42.1728083600125));
#33409=CARTESIAN_POINT('Ctrl Pts',(-5.67323543706194,-0.0727704952235973,
-42.4725554520429));
#33410=CARTESIAN_POINT('Ctrl Pts',(-5.67424842816243,-0.0447278973882266,
-42.7856337375846));
#33411=CARTESIAN_POINT('Ctrl Pts',(-5.67532096648076,-0.0192377484700357,
-43.2133842460989));
#33412=CARTESIAN_POINT('Ctrl Pts',(-5.67619447869966,-0.0063079848737366,
-43.7729890033109));
#33413=CARTESIAN_POINT('Ctrl Pts',(-5.67662753088596,-0.0121264093254704,
-44.482140388523));
#33414=CARTESIAN_POINT('Ctrl Pts',(-5.67660346780222,-0.0251049264471304,
-45.1045178144991));
#33415=CARTESIAN_POINT('Ctrl Pts',(-5.6764927226138,-0.0335587492382865,
-45.6210550178592));
#33416=CARTESIAN_POINT('Ctrl Pts',(-5.67635643262694,-0.0370325137349412,
-46.0176274785659));
#33417=CARTESIAN_POINT('Ctrl Pts',(-5.67619165632205,-0.035633795839697,
-46.4234041201591));
#33418=CARTESIAN_POINT('Ctrl Pts',(-5.6759795941213,-0.0243845393331214,
-46.9765347575413));
#33419=CARTESIAN_POINT('Ctrl Pts',(-5.67580300544141,-0.00199946540293369,
-47.4050759510626));
#33420=CARTESIAN_POINT('Ctrl Pts',(-5.67571775267112,0.0345851513673987,
-47.8420157886383));
#33421=CARTESIAN_POINT('Ctrl Pts',(-5.67564273379123,0.0548808751941392,
-48.0835009105947));
#33422=CARTESIAN_POINT('Ctrl Pts',(-5.67542062178334,0.098999274407724,
-48.5984489114891));
#33423=CARTESIAN_POINT('Ctrl Pts',(-5.67483381441346,0.17919214459599,-49.4916003161553));
#33424=CARTESIAN_POINT('Ctrl Pts',(-5.67337007871572,0.314922909631311,
-50.7957980320261));
#33425=CARTESIAN_POINT('Ctrl Pts',(-5.67081714031925,0.537881024433923,
-52.3856243686801));
#33426=CARTESIAN_POINT('Ctrl Pts',(-5.66846450176822,0.746623460845851,
-53.4646648158997));
#33427=CARTESIAN_POINT('Ctrl Pts',(-5.66683996713186,0.902366786944092,
-54.1446607528198));
#33428=CARTESIAN_POINT('Ctrl Pts',(-5.66613818814274,0.965739288299476,
-54.4130801179455));
#33429=CARTESIAN_POINT('Ctrl Pts',(-5.66453501303538,1.10040030864196,-54.9521509243576));
#33430=CARTESIAN_POINT('Ctrl Pts',(-5.66128069329804,1.35374995466334,-55.8906029672423));
#33431=CARTESIAN_POINT('Ctrl Pts',(-5.6536193010957,1.92793543307145,-57.7549412003636));
#33432=CARTESIAN_POINT('Ctrl Pts',(-5.64716225372688,2.51720283228602,-59.3207769290211));
#33433=CARTESIAN_POINT('Ctrl Pts',(-5.64455789154054,2.96622528244185,-60.4128272194335));
#33434=CARTESIAN_POINT('Ctrl Pts',(-5.64424507271109,3.02462206702412,-60.553109707374));
#33435=CARTESIAN_POINT('Ctrl Pts',(-5.64365588485913,3.14181292272085,-60.827939914503));
#33436=CARTESIAN_POINT('Ctrl Pts',(-5.64271282607086,3.35329136898542,-61.3078432002741));
#33437=CARTESIAN_POINT('Ctrl Pts',(-5.64114683715443,3.79445349188391,-62.252883979634));
#33438=CARTESIAN_POINT('Ctrl Pts',(-5.63999702692252,4.32913575921044,-63.3049907496339));
#33439=CARTESIAN_POINT('Ctrl Pts',(-5.63920737724254,4.86835251310299,-64.3266002920913));
#33440=CARTESIAN_POINT('Ctrl Pts',(-5.63885055859379,5.16886014394431,-64.8894571013804));
#33441=CARTESIAN_POINT('Ctrl Pts',(-5.6386317481306,5.36606332219433,-65.2593722248099));
#33442=CARTESIAN_POINT('Ctrl Pts',(-5.63848800035496,5.49657044970995,-65.5045323669089));
#33443=CARTESIAN_POINT('Ctrl Pts',(-5.63835259198041,5.62546168731041,-65.7475169610679));
#33444=CARTESIAN_POINT('Ctrl Pts',(-5.63823133523655,5.73646786926492,-65.9580854636632));
#33445=CARTESIAN_POINT('Ctrl Pts',(-5.63816171768633,5.79934662156983,-66.077815500769));
#33446=CARTESIAN_POINT('Ctrl Pts',(-5.63805635071558,5.89309438747521,-66.2568214244471));
#33447=CARTESIAN_POINT('Ctrl Pts',(-5.63796940294333,5.96995542512624,-66.4047063907607));
#33448=CARTESIAN_POINT('Ctrl Pts',(-5.63781800927207,6.0954529938488,-66.6480975667157));
#33449=CARTESIAN_POINT('Ctrl Pts',(-5.63768231546802,6.23297121546627,-66.9138116410786));
#33450=CARTESIAN_POINT('Ctrl Pts',(-5.637479034481,6.50298560865622,-67.4319127266579));
#33451=CARTESIAN_POINT('Ctrl Pts',(-5.63729628543975,6.97639589758447,-68.3319023920043));
#33452=CARTESIAN_POINT('Ctrl Pts',(-5.63743078458553,7.91572142956478,-70.0916119116528));
#33453=CARTESIAN_POINT('Ctrl Pts',(-5.63791663981526,8.71295327982952,-71.5676112934143));
#33454=CARTESIAN_POINT('Ctrl Pts',(-5.63792242673017,9.30768338133656,-72.6861728890823));
#33455=CARTESIAN_POINT('Ctrl Pts',(-5.63792178222381,9.44150440140497,-72.9378580825763));
#33456=CARTESIAN_POINT('Ctrl Pts',(-5.63792140995083,9.70829729496219,-73.4396300814865));
#33457=CARTESIAN_POINT('Ctrl Pts',(-5.63792335705853,10.0419462746335,-74.0671406986579));
#33458=CARTESIAN_POINT('Ctrl Pts',(-5.63792450110527,10.4419285249544,-74.8194001489715));
#33459=CARTESIAN_POINT('Ctrl Pts',(-5.63792772394606,11.2416996338346,-76.3235485176472));
#33460=CARTESIAN_POINT('Ctrl Pts',(-5.63793906758245,11.9078896183025,-77.5764705531983));
#33461=CARTESIAN_POINT('Ctrl Pts',(-5.63794461293377,12.8777987902702,-79.4006124326407));
#33462=CARTESIAN_POINT('Ctrl Pts',(-5.63794746754098,13.3143645759993,-80.22167739341));
#33463=CARTESIAN_POINT('Ctrl Pts',(-5.63794746754101,13.7508861633887,-81.0426550955084));
#33464=CARTESIAN_POINT('Ctrl Pts',(-3.75853532388587,-7.82717008495635E-5,
24.8306348326723));
#33465=CARTESIAN_POINT('Ctrl Pts',(-3.75854654435664,-7.82749362348716E-5,
24.7817555228025));
#33466=CARTESIAN_POINT('Ctrl Pts',(-3.75855831587281,-7.82802977327427E-5,
24.7328775181985));
#33467=CARTESIAN_POINT('Ctrl Pts',(-3.75869715731044,-7.82539305063524E-5,
24.1822610105156));
#33468=CARTESIAN_POINT('Ctrl Pts',(-3.75880238754123,-7.77773261011803E-5,
23.1780551437883));
#33469=CARTESIAN_POINT('Ctrl Pts',(-3.75904944284305,-7.7931664848751E-5,
21.1694489328841));
#33470=CARTESIAN_POINT('Ctrl Pts',(-3.75997170226701,-7.68106373729368E-5,
19.6651207230274));
#33471=CARTESIAN_POINT('Ctrl Pts',(-3.76193324311245,-7.65296069702623E-5,
18.4139955646262));
#33472=CARTESIAN_POINT('Ctrl Pts',(-3.76287426611526,-7.66096606190882E-5,
17.911167619251));
#33473=CARTESIAN_POINT('Ctrl Pts',(-3.76523680827642,-7.66850715270179E-5,
16.9071282930257));
#33474=CARTESIAN_POINT('Ctrl Pts',(-3.77030515875508,-7.72512599819896E-5,
15.1532648847908));
#33475=CARTESIAN_POINT('Ctrl Pts',(-3.77511624071878,-7.47472292143438E-5,
13.6511179057538));
#33476=CARTESIAN_POINT('Ctrl Pts',(-3.77813547303937,-7.31175951349916E-5,
12.3964515094638));
#33477=CARTESIAN_POINT('Ctrl Pts',(-3.77937083065646,-7.27403671319445E-5,
11.8954431352254));
#33478=CARTESIAN_POINT('Ctrl Pts',(-3.78188901434931,-7.14581327677145E-5,
10.8935397134728));
#33479=CARTESIAN_POINT('Ctrl Pts',(-3.78625108065095,-6.87239696068783E-5,
9.13956927306207));
#33480=CARTESIAN_POINT('Ctrl Pts',(-3.78929711946154,-6.07535379212773E-5,
7.63411764796906));
#33481=CARTESIAN_POINT('Ctrl Pts',(-3.79065166883889,-5.22034577220886E-5,
6.50050775733845));
#33482=CARTESIAN_POINT('Ctrl Pts',(-3.79107986193104,0.00252228322518703,
6.22000470746017));
#33483=CARTESIAN_POINT('Ctrl Pts',(-3.79234380964367,0.0158113917461691,
5.68607024174225));
#33484=CARTESIAN_POINT('Ctrl Pts',(-3.79531837082677,0.0544174247292424,
4.76668616845752));
#33485=CARTESIAN_POINT('Ctrl Pts',(-3.80220285402255,0.152587810395906,
3.03036886221659));
#33486=CARTESIAN_POINT('Ctrl Pts',(-3.80176228630631,0.143826217072127,
1.71474782041542));
#33487=CARTESIAN_POINT('Ctrl Pts',(-3.79140440831168,0.016248157303979,
0.870099283591018));
#33488=CARTESIAN_POINT('Ctrl Pts',(-3.79006590320266,0.00167268401214881,
0.781636720070122));
#33489=CARTESIAN_POINT('Ctrl Pts',(-3.78699184695418,-0.0342756137737318,
0.592244840357804));
#33490=CARTESIAN_POINT('Ctrl Pts',(-3.78066302350217,-0.111211123419434,
0.251903829461684));
#33491=CARTESIAN_POINT('Ctrl Pts',(-3.76939533703961,-0.261513074861836,
-0.271663801877638));
#33492=CARTESIAN_POINT('Ctrl Pts',(-3.75359988220739,-0.495283056373455,
-0.94914295080062));
#33493=CARTESIAN_POINT('Ctrl Pts',(-3.73072616249344,-0.857108261975899,
-1.9143557657));
#33494=CARTESIAN_POINT('Ctrl Pts',(-3.70064315115094,-1.35835307823454,
-3.22863941593501));
#33495=CARTESIAN_POINT('Ctrl Pts',(-3.67973778488251,-1.69407181273673,
-4.4157111301945));
#33496=CARTESIAN_POINT('Ctrl Pts',(-3.67085928169629,-1.83212785104798,
-5.210308046637));
#33497=CARTESIAN_POINT('Ctrl Pts',(-3.66793764503103,-1.87653006151095,
-5.4910274303086));
#33498=CARTESIAN_POINT('Ctrl Pts',(-3.66288142323918,-1.95219900130291,
-6.06694545421104));
#33499=CARTESIAN_POINT('Ctrl Pts',(-3.65650523893321,-2.04365923799453,
-7.04821528392791));
#33500=CARTESIAN_POINT('Ctrl Pts',(-3.65264711546065,-2.08974502003478,
-8.4062262755857));
#33501=CARTESIAN_POINT('Ctrl Pts',(-3.65203203181246,-2.08491430156149,
-9.68931684248278));
#33502=CARTESIAN_POINT('Ctrl Pts',(-3.65150826790285,-2.08404876723427,
-10.5495669923731));
#33503=CARTESIAN_POINT('Ctrl Pts',(-3.65096858012834,-2.08772800945087,
-11.0294381603198));
#33504=CARTESIAN_POINT('Ctrl Pts',(-3.65058185043361,-2.09155483800607,
-11.2654142598092));
#33505=CARTESIAN_POINT('Ctrl Pts',(-3.65023458911074,-2.09539087307951,
-11.4420542665395));
#33506=CARTESIAN_POINT('Ctrl Pts',(-3.64999169712714,-2.09810145524411,
-11.5749357706628));
#33507=CARTESIAN_POINT('Ctrl Pts',(-3.64955858697807,-2.10266722483507,
-11.8320568591363));
#33508=CARTESIAN_POINT('Ctrl Pts',(-3.64889746597844,-2.10904587316385,
-12.2844589281418));
#33509=CARTESIAN_POINT('Ctrl Pts',(-3.64768290265879,-2.11754588473787,
-13.4365947109693));
#33510=CARTESIAN_POINT('Ctrl Pts',(-3.64746698996492,-2.10947815317904,
-14.6986500552709));
#33511=CARTESIAN_POINT('Ctrl Pts',(-3.64758001480721,-2.09992789176325,
-15.948456137313));
#33512=CARTESIAN_POINT('Ctrl Pts',(-3.64764941892127,-2.09603249999465,
-16.5715515889072));
#33513=CARTESIAN_POINT('Ctrl Pts',(-3.64767599399056,-2.09422846040575,
-17.0691867471765));
#33514=CARTESIAN_POINT('Ctrl Pts',(-3.64767278213141,-2.09388242091375,
-17.3178339137197));
#33515=CARTESIAN_POINT('Ctrl Pts',(-3.64766195162746,-2.09388021807885,
-17.5035718635503));
#33516=CARTESIAN_POINT('Ctrl Pts',(-3.64766037907709,-2.09387863576372,
-17.628736956136));
#33517=CARTESIAN_POINT('Ctrl Pts',(-3.64767791885066,-2.0938758458656,-17.8777754411049));
#33518=CARTESIAN_POINT('Ctrl Pts',(-3.64772457263836,-2.09387183205052,
-18.127451726039));
#33519=CARTESIAN_POINT('Ctrl Pts',(-3.64779507913674,-2.09386947214827,
-18.3769832632093));
#33520=CARTESIAN_POINT('Ctrl Pts',(-3.6478483308591,-2.09386808188328,-18.5330555957456));
#33521=CARTESIAN_POINT('Ctrl Pts',(-3.64789576041336,-2.09386734399663,
-18.6579232856571));
#33522=CARTESIAN_POINT('Ctrl Pts',(-3.64794615788519,-2.09386665377775,
-18.7828197024514));
#33523=CARTESIAN_POINT('Ctrl Pts',(-3.64809782566923,-2.0938664352779,-19.1263719755194));
#33524=CARTESIAN_POINT('Ctrl Pts',(-3.64840051409532,-2.09386850931672,
-19.6890626879726));
#33525=CARTESIAN_POINT('Ctrl Pts',(-3.64901106867713,-2.09390750623519,
-20.6909211725876));
#33526=CARTESIAN_POINT('Ctrl Pts',(-3.64969208152518,-2.09399894836801,
-21.9463041772876));
#33527=CARTESIAN_POINT('Ctrl Pts',(-3.64979639834935,-2.09420105310877,
-22.9541717024532));
#33528=CARTESIAN_POINT('Ctrl Pts',(-3.64957735467363,-2.09434939667683,
-23.5835820407631));
#33529=CARTESIAN_POINT('Ctrl Pts',(-3.64946154252902,-2.09441198780494,
-23.8327092564764));
#33530=CARTESIAN_POINT('Ctrl Pts',(-3.64913803877753,-2.09456451664979,
-24.3317957111891));
#33531=CARTESIAN_POINT('Ctrl Pts',(-3.648352819248,-2.09488096347744,-25.207038469841));
#33532=CARTESIAN_POINT('Ctrl Pts',(-3.64683626660838,-2.09548696314257,
-26.4617048010875));
#33533=CARTESIAN_POINT('Ctrl Pts',(-3.64488331224232,-2.0961837752456,-27.9697879027271));
#33534=CARTESIAN_POINT('Ctrl Pts',(-3.64395769228688,-2.09662244536148,
-28.9752722261224));
#33535=CARTESIAN_POINT('Ctrl Pts',(-3.6436205019928,-2.09678630431028,-29.5384886302537));
#33536=CARTESIAN_POINT('Ctrl Pts',(-3.64351153512049,-2.0973662734663,-29.6473611136137));
#33537=CARTESIAN_POINT('Ctrl Pts',(-3.64317624760616,-2.10056409426989,
-29.8772090485191));
#33538=CARTESIAN_POINT('Ctrl Pts',(-3.64230927835962,-2.1111057457118,-30.2814499916388));
#33539=CARTESIAN_POINT('Ctrl Pts',(-3.63967466585405,-2.14803998985422,
-31.1205252839991));
#33540=CARTESIAN_POINT('Ctrl Pts',(-3.63572140605777,-2.20828479577518,
-32.1378836654998));
#33541=CARTESIAN_POINT('Ctrl Pts',(-3.63358924140075,-2.2405761068103,-33.2155342515335));
#33542=CARTESIAN_POINT('Ctrl Pts',(-3.63378778424351,-2.23686004340906,
-34.0530834789304));
#33543=CARTESIAN_POINT('Ctrl Pts',(-3.63675381955408,-2.190599093022,-34.9201817981066));
#33544=CARTESIAN_POINT('Ctrl Pts',(-3.64123191036651,-2.12068100214489,
-35.5160745326321));
#33545=CARTESIAN_POINT('Ctrl Pts',(-3.64576438011192,-2.04906134821434,
-35.9707720742832));
#33546=CARTESIAN_POINT('Ctrl Pts',(-3.64965298273566,-1.98788192349195,
-36.2994619330854));
#33547=CARTESIAN_POINT('Ctrl Pts',(-3.65880246984932,-1.84047979358516,
-36.9176012241994));
#33548=CARTESIAN_POINT('Ctrl Pts',(-3.67806204837734,-1.52651468642503,
-37.9518433469515));
#33549=CARTESIAN_POINT('Ctrl Pts',(-3.72086560389792,-0.784570381697561,
-39.8175211185846));
#33550=CARTESIAN_POINT('Ctrl Pts',(-3.75502335684506,-0.272190657553224,
-41.1494732605515));
#33551=CARTESIAN_POINT('Ctrl Pts',(-3.76762193450478,-0.13228232701847,
-41.9554888717754));
#33552=CARTESIAN_POINT('Ctrl Pts',(-3.77018890614804,-0.100794906990536,
-42.1587122714258));
#33553=CARTESIAN_POINT('Ctrl Pts',(-3.77337862406258,-0.0656523899136256,
-42.4612575185149));
#33554=CARTESIAN_POINT('Ctrl Pts',(-3.77595475717398,-0.0390350463462554,
-42.776673888403));
#33555=CARTESIAN_POINT('Ctrl Pts',(-3.7786365989841,-0.0150756310605251,
-43.2073666789962));
#33556=CARTESIAN_POINT('Ctrl Pts',(-3.78072522701561,-0.00346913651286049,
-43.7699070202859));
#33557=CARTESIAN_POINT('Ctrl Pts',(-3.78173732898778,-0.0100179160988367,
-44.4814310562548));
#33558=CARTESIAN_POINT('Ctrl Pts',(-3.78180044511189,-0.0231100159289182,
-45.1047807273984));
#33559=CARTESIAN_POINT('Ctrl Pts',(-3.78166099965021,-0.0314898532548608,
-45.6215024351169));
#33560=CARTESIAN_POINT('Ctrl Pts',(-3.78153156649938,-0.0349108490470552,
-46.0179165001026));
#33561=CARTESIAN_POINT('Ctrl Pts',(-3.78144717600605,-0.0335232889237656,
-46.4232364281124));
#33562=CARTESIAN_POINT('Ctrl Pts',(-3.78149126288203,-0.022464138604499,
-46.975363526501));
#33563=CARTESIAN_POINT('Ctrl Pts',(-3.78179709799868,-0.000576863581530635,
-47.4027053717721));
#33564=CARTESIAN_POINT('Ctrl Pts',(-3.78243277047768,0.0351297799016445,
-47.8382051253742));
#33565=CARTESIAN_POINT('Ctrl Pts',(-3.7828521655432,0.0550254679880845,
-48.0799370747199));
#33566=CARTESIAN_POINT('Ctrl Pts',(-3.78366605684173,0.0982302401516215,
-48.5947359044865));
#33567=CARTESIAN_POINT('Ctrl Pts',(-3.78499798423273,0.176872274547839,
-49.4880650124114));
#33568=CARTESIAN_POINT('Ctrl Pts',(-3.78647580599884,0.310424786308024,
-50.7925895120424));
#33569=CARTESIAN_POINT('Ctrl Pts',(-3.78717568337191,0.531337373178592,
-52.3833317731187));
#33570=CARTESIAN_POINT('Ctrl Pts',(-3.7865819860366,0.739296298888895,-53.4632179152833));
#33571=CARTESIAN_POINT('Ctrl Pts',(-3.78580490188227,0.894839020014008,
-54.1438065235354));
#33572=CARTESIAN_POINT('Ctrl Pts',(-3.78543262539753,0.958171122282076,
-54.4124863225216));
#33573=CARTESIAN_POINT('Ctrl Pts',(-3.78444370602454,1.09283917001359,-54.9520049683496));
#33574=CARTESIAN_POINT('Ctrl Pts',(-3.78216157813114,1.34642076525217,-55.8911232547336));
#33575=CARTESIAN_POINT('Ctrl Pts',(-3.77602584954904,1.92172700273483,-57.7562776592878));
#33576=CARTESIAN_POINT('Ctrl Pts',(-3.77022072522239,2.51236442779873,-59.3220758584305));
#33577=CARTESIAN_POINT('Ctrl Pts',(-3.76779455586239,2.96190521138445,-60.4137989092541));
#33578=CARTESIAN_POINT('Ctrl Pts',(-3.76749222284573,3.02041536309737,-60.5541442225808));
#33579=CARTESIAN_POINT('Ctrl Pts',(-3.76690761672463,3.13781401399604,-60.8290330399708));
#33580=CARTESIAN_POINT('Ctrl Pts',(-3.76591968324598,3.3496899726605,-61.309049494963));
#33581=CARTESIAN_POINT('Ctrl Pts',(-3.76409555893897,3.79169292000971,-62.2542211745589));
#33582=CARTESIAN_POINT('Ctrl Pts',(-3.76236115234085,4.32739169568999,-63.3063512843697));
#33583=CARTESIAN_POINT('Ctrl Pts',(-3.76093648081012,4.86749660007094,-64.3278585369242));
#33584=CARTESIAN_POINT('Ctrl Pts',(-3.76024239649334,5.1684273086147,-64.8906121976067));
#33585=CARTESIAN_POINT('Ctrl Pts',(-3.75982229879937,5.36586845324159,-65.2604378773822));
#33586=CARTESIAN_POINT('Ctrl Pts',(-3.75955278590453,5.49652119911916,-65.505532600228));
#33587=CARTESIAN_POINT('Ctrl Pts',(-3.75930152180481,5.62553933749147,-65.7484431426067));
#33588=CARTESIAN_POINT('Ctrl Pts',(-3.7590947164072,5.73663607593057,-65.9589384493982));
#33589=CARTESIAN_POINT('Ctrl Pts',(-3.75898058555973,5.79956068820915,-66.0786241831879));
#33590=CARTESIAN_POINT('Ctrl Pts',(-3.75881327243508,5.89337112016886,-66.2575611354474));
#33591=CARTESIAN_POINT('Ctrl Pts',(-3.75868316571257,5.97027208588428,-66.405383063182));
#33592=CARTESIAN_POINT('Ctrl Pts',(-3.758477673407,6.09581674659771,-66.648662549422));
#33593=CARTESIAN_POINT('Ctrl Pts',(-3.75829211778717,6.23339093492571,-66.9142887943685));
#33594=CARTESIAN_POINT('Ctrl Pts',(-3.75801448399417,6.50346468227751,-67.4322179601308));
#33595=CARTESIAN_POINT('Ctrl Pts',(-3.75775357067056,6.97689187339913,-68.331958489734));
#33596=CARTESIAN_POINT('Ctrl Pts',(-3.75790811579813,7.91598173799435,-70.0913522764039));
#33597=CARTESIAN_POINT('Ctrl Pts',(-3.75851702956022,8.7129544406287,-71.56741993476));
#33598=CARTESIAN_POINT('Ctrl Pts',(-3.75851139507746,9.30780849071006,-72.6861960657986));
#33599=CARTESIAN_POINT('Ctrl Pts',(-3.75850965202096,9.44162253911425,-72.9378654400856));
#33600=CARTESIAN_POINT('Ctrl Pts',(-3.7585072672047,9.70842045664312,-73.439642572339));
#33601=CARTESIAN_POINT('Ctrl Pts',(-3.75850659091144,10.042067263661,-74.0671451260673));
#33602=CARTESIAN_POINT('Ctrl Pts',(-3.7585068904606,10.4420495799701,-74.8194037887349));
#33603=CARTESIAN_POINT('Ctrl Pts',(-3.75851012699749,11.2418168738129,-76.3235472418929));
#33604=CARTESIAN_POINT('Ctrl Pts',(-3.75851897726527,11.9080053917647,-77.576469362933));
#33605=CARTESIAN_POINT('Ctrl Pts',(-3.75852120334172,12.877917815396,-79.4006144962138));
#33606=CARTESIAN_POINT('Ctrl Pts',(-3.75852234907699,13.3144832846348,-80.2216773890785));
#33607=CARTESIAN_POINT('Ctrl Pts',(-3.75852234907698,13.7510048720243,-81.0426550911768));
#33608=CARTESIAN_POINT('Ctrl Pts',(-1.87922647318657,7.43659936946723E-5,
24.8306346358243));
#33609=CARTESIAN_POINT('Ctrl Pts',(-1.8792320812944,7.43682799464241E-5,
24.781755319639));
#33610=CARTESIAN_POINT('Ctrl Pts',(-1.87923794877265,7.43856257991035E-5,
24.7328772901569));
#33611=CARTESIAN_POINT('Ctrl Pts',(-1.87930788335411,7.39106761634475E-5,
24.1822613292266));
#33612=CARTESIAN_POINT('Ctrl Pts',(-1.87936495452039,6.97862600438643E-5,
23.1780605579904));
#33613=CARTESIAN_POINT('Ctrl Pts',(-1.87948882589249,6.95445524143603E-5,
21.1694547708657));
#33614=CARTESIAN_POINT('Ctrl Pts',(-1.87996099259776,5.92851299646219E-5,
19.6651394211573));
#33615=CARTESIAN_POINT('Ctrl Pts',(-1.88094643808592,5.48594906311521E-5,
18.4140198688397));
#33616=CARTESIAN_POINT('Ctrl Pts',(-1.88141759062512,5.42365496829209E-5,
17.9111924083393));
#33617=CARTESIAN_POINT('Ctrl Pts',(-1.88260171332622,5.1515615193511E-5,
16.9071564758307));
#33618=CARTESIAN_POINT('Ctrl Pts',(-1.8851386273318,4.8840807487355E-5,
15.1532969718806));
#33619=CARTESIAN_POINT('Ctrl Pts',(-1.88756917454291,2.5212297710916E-5,
13.6511807365289));
#33620=CARTESIAN_POINT('Ctrl Pts',(-1.88909132532381,1.31179185919511E-5,
12.3965299246728));
#33621=CARTESIAN_POINT('Ctrl Pts',(-1.88971089815823,1.12234742488184E-5,
11.8955257512763));
#33622=CARTESIAN_POINT('Ctrl Pts',(-1.89097888630937,2.29670390858633E-6,
10.8936285883835));
#33623=CARTESIAN_POINT('Ctrl Pts',(-1.89316912932919,-6.67277562029711E-6,
9.13968656717126));
#33624=CARTESIAN_POINT('Ctrl Pts',(-1.89476488907268,-7.75933543378677E-5,
7.634263797525));
#33625=CARTESIAN_POINT('Ctrl Pts',(-1.89546999666034,-9.98435924221817E-5,
6.50081894633009));
#33626=CARTESIAN_POINT('Ctrl Pts',(-1.89572526873683,0.00230665268363747,
6.22211902701521));
#33627=CARTESIAN_POINT('Ctrl Pts',(-1.89656984995772,0.0147464668667423,
5.6901431042027));
#33628=CARTESIAN_POINT('Ctrl Pts',(-1.89870974110295,0.0509275694207369,
4.77316994900257));
#33629=CARTESIAN_POINT('Ctrl Pts',(-1.90384887013271,0.143249196984895,
3.03555484961679));
#33630=CARTESIAN_POINT('Ctrl Pts',(-1.90386759788697,0.135196680509002,
1.70833859041381));
#33631=CARTESIAN_POINT('Ctrl Pts',(-1.89609045310109,0.0134334976845784,
0.851658950433416));
#33632=CARTESIAN_POINT('Ctrl Pts',(-1.89507277414501,-0.000596206126116792,
0.761097201393625));
#33633=CARTESIAN_POINT('Ctrl Pts',(-1.89274386758357,-0.0350229766227751,
0.568310331140751));
#33634=CARTESIAN_POINT('Ctrl Pts',(-1.88794310623562,-0.108513562227805,
0.222760045781302));
#33635=CARTESIAN_POINT('Ctrl Pts',(-1.87945425802549,-0.251368970401314,
-0.305671681892107));
#33636=CARTESIAN_POINT('Ctrl Pts',(-1.86741465521342,-0.47234244992444,
-0.986225583648586));
#33637=CARTESIAN_POINT('Ctrl Pts',(-1.85007936140568,-0.813435797702823,
-1.95268467358928));
#33638=CARTESIAN_POINT('Ctrl Pts',(-1.82713104757049,-1.28439221945105,
-3.26444308371993));
#33639=CARTESIAN_POINT('Ctrl Pts',(-1.81144354971363,-1.5984732684984,-4.44282707602525));
#33640=CARTESIAN_POINT('Ctrl Pts',(-1.80476245096426,-1.72725980926203,
-5.22829718654077));
#33641=CARTESIAN_POINT('Ctrl Pts',(-1.80253991577537,-1.76890705186197,
-5.50734875644929));
#33642=CARTESIAN_POINT('Ctrl Pts',(-1.79872094345382,-1.83981142184769,
-6.07911225865069));
#33643=CARTESIAN_POINT('Ctrl Pts',(-1.79397191736841,-1.92574635832976,
-7.05450848993233));
#33644=CARTESIAN_POINT('Ctrl Pts',(-1.79134660398458,-1.96941694501554,
-8.40664655582761));
#33645=CARTESIAN_POINT('Ctrl Pts',(-1.7912688089539,-1.96525359414387,-9.68812119753314));
#33646=CARTESIAN_POINT('Ctrl Pts',(-1.79107002876421,-1.96460551414136,
-10.549293763825));
#33647=CARTESIAN_POINT('Ctrl Pts',(-1.79075743910556,-1.96817078064357,
-11.03032083609));
#33648=CARTESIAN_POINT('Ctrl Pts',(-1.79050564371391,-1.97182966370674,
-11.267085603225));
#33649=CARTESIAN_POINT('Ctrl Pts',(-1.79026848438622,-1.97548562812885,
-11.4443732616452));
#33650=CARTESIAN_POINT('Ctrl Pts',(-1.79010312595948,-1.97805319876885,
-11.5768525465978));
#33651=CARTESIAN_POINT('Ctrl Pts',(-1.78981400359038,-1.98239200926529,
-11.83366297907));
#33652=CARTESIAN_POINT('Ctrl Pts',(-1.78939243224564,-1.98847129358254,
-12.2853409495223));
#33653=CARTESIAN_POINT('Ctrl Pts',(-1.78872477134816,-1.99670111738816,
-13.4361160012765));
#33654=CARTESIAN_POINT('Ctrl Pts',(-1.78892194409522,-1.98938784146963,
-14.6974250005926));
#33655=CARTESIAN_POINT('Ctrl Pts',(-1.7892358485117,-1.9805396995022,-15.9474018586027));
#33656=CARTESIAN_POINT('Ctrl Pts',(-1.78938855573791,-1.97693589443852,
-16.5707912522935));
#33657=CARTESIAN_POINT('Ctrl Pts',(-1.78945400749427,-1.97526103685482,
-17.068792009475));
#33658=CARTESIAN_POINT('Ctrl Pts',(-1.78946777988097,-1.97494395888634,
-17.3176657243817));
#33659=CARTESIAN_POINT('Ctrl Pts',(-1.78946661540154,-1.97494499467903,
-17.5035835075773));
#33660=CARTESIAN_POINT('Ctrl Pts',(-1.7894691915749,-1.97494635491117,-17.6286867178594));
#33661=CARTESIAN_POINT('Ctrl Pts',(-1.78948555236713,-1.97495114467567,
-17.8777132092247));
#33662=CARTESIAN_POINT('Ctrl Pts',(-1.78952096602998,-1.97495958507703,
-18.1273468564737));
#33663=CARTESIAN_POINT('Ctrl Pts',(-1.78956735566838,-1.97496935158133,
-18.3768644877724));
#33664=CARTESIAN_POINT('Ctrl Pts',(-1.78960181669949,-1.9749762550401,-18.5329270333045));
#33665=CARTESIAN_POINT('Ctrl Pts',(-1.78963162475722,-1.97498194350401,
-18.6577906642006));
#33666=CARTESIAN_POINT('Ctrl Pts',(-1.78966291596671,-1.97498768563792,
-18.782683892236));
#33667=CARTESIAN_POINT('Ctrl Pts',(-1.78975753412344,-1.97500524550039,
-19.1262339458842));
#33668=CARTESIAN_POINT('Ctrl Pts',(-1.78993935028022,-1.97503357614361,
-19.6889521983325));
#33669=CARTESIAN_POINT('Ctrl Pts',(-1.79029584480078,-1.9750781273811,-20.6909515915249));
#33670=CARTESIAN_POINT('Ctrl Pts',(-1.79064055534606,-1.97505601143599,
-21.9466759565142));
#33671=CARTESIAN_POINT('Ctrl Pts',(-1.79060445085998,-1.97491323922974,
-22.9549969094165));
#33672=CARTESIAN_POINT('Ctrl Pts',(-1.79037559502688,-1.97474017900966,
-23.5847448392945));
#33673=CARTESIAN_POINT('Ctrl Pts',(-1.79026154891338,-1.97465962601369,
-23.8340744749038));
#33674=CARTESIAN_POINT('Ctrl Pts',(-1.78996266815782,-1.97446464689011,
-24.3334733094898));
#33675=CARTESIAN_POINT('Ctrl Pts',(-1.78927381304738,-1.97404218711815,
-25.209165972539));
#33676=CARTESIAN_POINT('Ctrl Pts',(-1.78798170886171,-1.97329878314502,
-26.4641179004378));
#33677=CARTESIAN_POINT('Ctrl Pts',(-1.78632982209942,-1.97235667129645,
-27.9720281857487));
#33678=CARTESIAN_POINT('Ctrl Pts',(-1.78549155115143,-1.97187672496451,
-28.9769975495061));
#33679=CARTESIAN_POINT('Ctrl Pts',(-1.78516656839224,-1.97167625059406,
-29.539906341611));
#33680=CARTESIAN_POINT('Ctrl Pts',(-1.7850666350457,-1.97215941396197,-29.6497164037394));
#33681=CARTESIAN_POINT('Ctrl Pts',(-1.78477169972964,-1.97505395985333,
-29.8807066150062));
#33682=CARTESIAN_POINT('Ctrl Pts',(-1.78402113263626,-1.98480013300052,
-30.2868589688187));
#33683=CARTESIAN_POINT('Ctrl Pts',(-1.78179302898577,-2.01927945684624,
-31.1279979786219));
#33684=CARTESIAN_POINT('Ctrl Pts',(-1.77843455939292,-2.07555131660762,
-32.1444463451454));
#33685=CARTESIAN_POINT('Ctrl Pts',(-1.7765632735973,-2.10549056347651,-33.2177245662806));
#33686=CARTESIAN_POINT('Ctrl Pts',(-1.77660523082701,-2.10175494826061,
-34.0502763097447));
#33687=CARTESIAN_POINT('Ctrl Pts',(-1.77880766198053,-2.05817849987701,
-34.9106733776414));
#33688=CARTESIAN_POINT('Ctrl Pts',(-1.7822325000575,-1.9926391339686,-35.5011482024419));
#33689=CARTESIAN_POINT('Ctrl Pts',(-1.78574196680919,-1.92562867740721,
-35.9515064265878));
#33690=CARTESIAN_POINT('Ctrl Pts',(-1.78873960982218,-1.86856136255701,
-36.2760710728659));
#33691=CARTESIAN_POINT('Ctrl Pts',(-1.79585687226293,-1.73081723039962,
-36.8883400341203));
#33692=CARTESIAN_POINT('Ctrl Pts',(-1.81071819779439,-1.43672452638524,
-37.9152325486312));
#33693=CARTESIAN_POINT('Ctrl Pts',(-1.84411300428762,-0.74008290519004,
-39.776554008902));
#33694=CARTESIAN_POINT('Ctrl Pts',(-1.86996309579029,-0.254721573964913,
-41.1127718926262));
#33695=CARTESIAN_POINT('Ctrl Pts',(-1.87944574652515,-0.120250328587189,
-41.9361856957747));
#33696=CARTESIAN_POINT('Ctrl Pts',(-1.88141687474336,-0.0904963193764836,
-42.1412581804935));
#33697=CARTESIAN_POINT('Ctrl Pts',(-1.88383775239668,-0.057328381547109,
-42.4473311457505));
#33698=CARTESIAN_POINT('Ctrl Pts',(-1.88579098865738,-0.032482726045188,
-42.7656755195937));
#33699=CARTESIAN_POINT('Ctrl Pts',(-1.88780408608839,-0.0104078350965731,
-43.2000369215372));
#33700=CARTESIAN_POINT('Ctrl Pts',(-1.88934964918851,-0.000417930478199928,
-43.766216661788));
#33701=CARTESIAN_POINT('Ctrl Pts',(-1.89005786507775,-0.00781083470753425,
-44.4806607424834));
#33702=CARTESIAN_POINT('Ctrl Pts',(-1.8900503045469,-0.0209520131984904,
-45.1051803940128));
#33703=CARTESIAN_POINT('Ctrl Pts',(-1.88995893058319,-0.029260011726896,
-45.6221161988452));
#33704=CARTESIAN_POINT('Ctrl Pts',(-1.88987679081064,-0.0326211432941866,
-46.0183182336727));
#33705=CARTESIAN_POINT('Ctrl Pts',(-1.88984019143788,-0.0312522604122497,
-46.4230535672428));
#33706=CARTESIAN_POINT('Ctrl Pts',(-1.88994150500147,-0.0204579713078959,
-46.9739112286859));
#33707=CARTESIAN_POINT('Ctrl Pts',(-1.89021927414918,0.000847090578713871,
-47.3997344095905));
#33708=CARTESIAN_POINT('Ctrl Pts',(-1.89079622330981,0.035450677665807,
-47.8334166079678));
#33709=CARTESIAN_POINT('Ctrl Pts',(-1.89118518624509,0.0548291878842356,
-48.0754222563547));
#33710=CARTESIAN_POINT('Ctrl Pts',(-1.8919684497567,0.096849072818417,-48.5899868840785));
#33711=CARTESIAN_POINT('Ctrl Pts',(-1.89331811174698,0.173463964332855,
-49.4834687046147));
#33712=CARTESIAN_POINT('Ctrl Pts',(-1.89500374569028,0.304184643793816,
-50.7883449345947));
#33713=CARTESIAN_POINT('Ctrl Pts',(-1.8963558861006,0.522336541724754,-52.3802914310615));
#33714=CARTESIAN_POINT('Ctrl Pts',(-1.8964105023605,0.729306886905037,-53.4613249704202));
#33715=CARTESIAN_POINT('Ctrl Pts',(-1.89613100861477,0.884610861304433,
-54.1427419720713));
#33716=CARTESIAN_POINT('Ctrl Pts',(-1.89598303975611,0.947891669923935,
-54.411771836144));
#33717=CARTESIAN_POINT('Ctrl Pts',(-1.89551625297565,1.0825818126608,-54.9518990099226));
#33718=CARTESIAN_POINT('Ctrl Pts',(-1.89430851430286,1.33651472026183,-55.8919087552172));
#33719=CARTESIAN_POINT('Ctrl Pts',(-1.89076753071172,1.91341936868272,-57.7581455372565));
#33720=CARTESIAN_POINT('Ctrl Pts',(-1.88722362432661,2.50596526061431,-59.3238337112826));
#33721=CARTESIAN_POINT('Ctrl Pts',(-1.88572660967207,2.95620938582178,-60.4150899796445));
#33722=CARTESIAN_POINT('Ctrl Pts',(-1.88553601853826,3.0148726044652,-60.5555183564978));
#33723=CARTESIAN_POINT('Ctrl Pts',(-1.88516359548367,3.13255149157178,-60.8304824737814));
#33724=CARTESIAN_POINT('Ctrl Pts',(-1.88452291602286,3.34496050530911,-61.3106450471766));
#33725=CARTESIAN_POINT('Ctrl Pts',(-1.88329441022756,3.78808659672977,-62.2559809772548));
#33726=CARTESIAN_POINT('Ctrl Pts',(-1.8820565125292,4.32512291249686,-63.3081334059565));
#33727=CARTESIAN_POINT('Ctrl Pts',(-1.88099241764672,4.86639785683072,-64.3295005770627));
#33728=CARTESIAN_POINT('Ctrl Pts',(-1.8804627043064,5.16788755886044,-64.8921173663213));
#33729=CARTESIAN_POINT('Ctrl Pts',(-1.88014234675638,5.36564326557466,-65.2618246643185));
#33730=CARTESIAN_POINT('Ctrl Pts',(-1.87993629780318,5.49648934849498,-65.5068329550256));
#33731=CARTESIAN_POINT('Ctrl Pts',(-1.87974758568304,5.62567418338341,-65.7496459357718));
#33732=CARTESIAN_POINT('Ctrl Pts',(-1.87959264777368,5.73689111164499,-65.9600447305898));
#33733=CARTESIAN_POINT('Ctrl Pts',(-1.87950787055948,5.79987661251178,-66.0796720507273));
#33734=CARTESIAN_POINT('Ctrl Pts',(-1.87938419873138,5.89377044043449,-66.2585180400154));
#33735=CARTESIAN_POINT('Ctrl Pts',(-1.8792911987843,5.97072364200638,-66.406257209168));
#33736=CARTESIAN_POINT('Ctrl Pts',(-1.87914620246728,6.09633077364163,-66.6493895977556));
#33737=CARTESIAN_POINT('Ctrl Pts',(-1.87901599600879,6.23397804167784,-66.9148991361219));
#33738=CARTESIAN_POINT('Ctrl Pts',(-1.87882043496205,6.5041293622886,-67.4326003206522));
#33739=CARTESIAN_POINT('Ctrl Pts',(-1.87864116952207,6.97757390129021,-68.3320115836156));
#33740=CARTESIAN_POINT('Ctrl Pts',(-1.87875637389118,7.91634431697053,-70.0909885233312));
#33741=CARTESIAN_POINT('Ctrl Pts',(-1.87920310482,8.71296113698193,-71.5671554587218));
#33742=CARTESIAN_POINT('Ctrl Pts',(-1.87920409650289,9.30797701881977,-72.6862204452462));
#33743=CARTESIAN_POINT('Ctrl Pts',(-1.87920288711204,9.4417816722211,-72.937868851734));
#33744=CARTESIAN_POINT('Ctrl Pts',(-1.87920154950468,9.70858596207869,-73.439653172257));
#33745=CARTESIAN_POINT('Ctrl Pts',(-1.87920244898022,10.0422290067306,-74.0671457930824));
#33746=CARTESIAN_POINT('Ctrl Pts',(-1.87920330165399,10.4422110758571,-74.8194038178528));
#33747=CARTESIAN_POINT('Ctrl Pts',(-1.8792068113137,11.2419727933141,-76.3235413741309));
#33748=CARTESIAN_POINT('Ctrl Pts',(-1.87921800986231,11.9081567732661,-77.5764657951134));
#33749=CARTESIAN_POINT('Ctrl Pts',(-1.87922251549513,12.8780717022048,-79.4006164692795));
#33750=CARTESIAN_POINT('Ctrl Pts',(-1.8792248343783,13.3146358968538,-80.2216773916581));
#33751=CARTESIAN_POINT('Ctrl Pts',(-1.87922483437827,13.7511574842433,-81.0426550937565));
#33752=CARTESIAN_POINT('Ctrl Pts',(-7.86816895413843E-6,0.000134138085496685,
24.8306345586402));
#33753=CARTESIAN_POINT('Ctrl Pts',(-7.86837039397705E-6,0.0001341424751082,
24.7817552401123));
#33754=CARTESIAN_POINT('Ctrl Pts',(-7.86758228674821E-6,0.000134149695995169,
24.7328772070671));
#33755=CARTESIAN_POINT('Ctrl Pts',(-7.90367859151917E-6,0.00013411567282899,
24.1822612582853));
#33756=CARTESIAN_POINT('Ctrl Pts',(-8.18809680975969E-6,0.000133513032849035,
23.1780607854083));
#33757=CARTESIAN_POINT('Ctrl Pts',(-8.23189606488739E-6,0.000133804106629631,
21.169454983822));
#33758=CARTESIAN_POINT('Ctrl Pts',(-8.93959770906373E-6,0.00013233366932893,
19.6651404452238));
#33759=CARTESIAN_POINT('Ctrl Pts',(-9.2601353069708E-6,0.000131836478995296,
18.4140212479634));
#33760=CARTESIAN_POINT('Ctrl Pts',(-9.31855293916846E-6,0.000131891105320219,
17.91119370092));
#33761=CARTESIAN_POINT('Ctrl Pts',(-9.53558031351182E-6,0.000131877154863405,
16.9071579078805));
#33762=CARTESIAN_POINT('Ctrl Pts',(-9.81102603618544E-6,0.000132380618664769,
15.1532986547908));
#33763=CARTESIAN_POINT('Ctrl Pts',(-1.13163675539412E-5,0.000128697056927304,
13.6511848101255));
#33764=CARTESIAN_POINT('Ctrl Pts',(-1.20215489539955E-5,0.00012598731728272,
12.3965353750791));
#33765=CARTESIAN_POINT('Ctrl Pts',(-1.21198252440109E-5,0.000125354011049059,
11.8955321306931));
#33766=CARTESIAN_POINT('Ctrl Pts',(-1.25719075545662E-5,0.000122663548405129,
10.893634209687));
#33767=CARTESIAN_POINT('Ctrl Pts',(-1.29806635370252E-5,0.000119128674288264,
9.13969986849073));
#33768=CARTESIAN_POINT('Ctrl Pts',(-1.68084968046005E-5,0.000102911589896075,
7.63426186513583));
#33769=CARTESIAN_POINT('Ctrl Pts',(-1.82403447152679E-5,0.00010109573980971,
6.50086936027134));
#33770=CARTESIAN_POINT('Ctrl Pts',(-1.64601354838555E-5,0.00244662050690851,
6.2228498478194));
#33771=CARTESIAN_POINT('Ctrl Pts',(-6.73044822835249E-6,0.014572420864447,
5.69161192423943));
#33772=CARTESIAN_POINT('Ctrl Pts',(2.07135641908368E-5,0.0498770565337277,
4.77553942507642));
#33773=CARTESIAN_POINT('Ctrl Pts',(9.95496872622605E-5,0.14000092241698,
3.03741192946093));
#33774=CARTESIAN_POINT('Ctrl Pts',(8.35363358727937E-5,0.132494558618385,
1.70571827028138));
#33775=CARTESIAN_POINT('Ctrl Pts',(-4.3165465129633E-5,0.0131276052745993,
0.844409225479565));
#33776=CARTESIAN_POINT('Ctrl Pts',(-5.87456527449067E-5,-0.000678586975984755,
0.753045172446035));
#33777=CARTESIAN_POINT('Ctrl Pts',(-9.40682916947416E-5,-0.0344900533728886,
0.558952015873453));
#33778=CARTESIAN_POINT('Ctrl Pts',(-0.000164093499659093,-0.106614488837571,
0.211381380066455));
#33779=CARTESIAN_POINT('Ctrl Pts',(-0.000283606969796099,-0.246519397169534,
-0.318981240870596));
#33780=CARTESIAN_POINT('Ctrl Pts',(-0.000438074335267664,-0.462725653626534,
-1.00076418485887));
#33781=CARTESIAN_POINT('Ctrl Pts',(-0.00067632928056198,-0.796092318982456,
-1.96767603702569));
#33782=CARTESIAN_POINT('Ctrl Pts',(-0.00104113729596573,-1.25617217791027,
-3.27826183066476));
#33783=CARTESIAN_POINT('Ctrl Pts',(-0.00144925043470265,-1.56238495854328,
-4.45318358255805));
#33784=CARTESIAN_POINT('Ctrl Pts',(-0.00164344066864579,-1.68786141248603,
-5.23520500674852));
#33785=CARTESIAN_POINT('Ctrl Pts',(-0.00169780486768979,-1.72854156947398,
-5.513626473583));
#33786=CARTESIAN_POINT('Ctrl Pts',(-0.00179701682113945,-1.79776427715872,
-6.08382750946227));
#33787=CARTESIAN_POINT('Ctrl Pts',(-0.00191717498362644,-1.88171648309701,
-7.05701935378413));
#33788=CARTESIAN_POINT('Ctrl Pts',(-0.00197726410329787,-1.92440052183823,
-8.40693623429189));
#33789=CARTESIAN_POINT('Ctrl Pts',(-0.00196970659771493,-1.92031956974289,
-9.68777019145027));
#33790=CARTESIAN_POINT('Ctrl Pts',(-0.00196543564596002,-1.91971220554664,
-10.5492737685884));
#33791=CARTESIAN_POINT('Ctrl Pts',(-0.00196716279840418,-1.9232243570222,
-11.0307243359037));
#33792=CARTESIAN_POINT('Ctrl Pts',(-0.0019700711110791,-1.9268200043073,
-11.2677791491987));
#33793=CARTESIAN_POINT('Ctrl Pts',(-0.00197308324111247,-1.93041253094738,
-11.4453057330445));
#33794=CARTESIAN_POINT('Ctrl Pts',(-0.00197588354150194,-1.93292971573111,
-11.5776350827829));
#33795=CARTESIAN_POINT('Ctrl Pts',(-0.00197997062913887,-1.93718924689335,
-11.8343290274479));
#33796=CARTESIAN_POINT('Ctrl Pts',(-0.00198541577020757,-1.94315917627825,
-12.2857350678419));
#33797=CARTESIAN_POINT('Ctrl Pts',(-0.00199021190869098,-1.95125874518291,
-13.435990027481));
#33798=CARTESIAN_POINT('Ctrl Pts',(-0.00197629221165083,-1.94412854859148,
-14.6969941891685));
#33799=CARTESIAN_POINT('Ctrl Pts',(-0.00196013412846356,-1.93551323635508,
-15.9470316019288));
#33800=CARTESIAN_POINT('Ctrl Pts',(-0.00195528042777413,-1.93199060585446,
-16.5705240611153));
#33801=CARTESIAN_POINT('Ctrl Pts',(-0.0019525135633656,-1.93035800022109,
-17.0686604800003));
#33802=CARTESIAN_POINT('Ctrl Pts',(-0.00195230352912211,-1.93004766012124,
-17.3176175926851));
#33803=CARTESIAN_POINT('Ctrl Pts',(-0.00195233573781056,-1.93004894171476,
-17.5036021570554));
#33804=CARTESIAN_POINT('Ctrl Pts',(-0.00195236553761999,-1.93005065707797,
-17.628681641473));
#33805=CARTESIAN_POINT('Ctrl Pts',(-0.00195222219453429,-1.93005739523279,
-17.877702982022));
#33806=CARTESIAN_POINT('Ctrl Pts',(-0.00195260067372203,-1.93006735831943,
-18.1273192668479));
#33807=CARTESIAN_POINT('Ctrl Pts',(-0.00195239498154048,-1.93008052775035,
-18.3768312531958));
#33808=CARTESIAN_POINT('Ctrl Pts',(-0.00195238244644089,-1.93008945422298,
-18.5328897673755));
#33809=CARTESIAN_POINT('Ctrl Pts',(-0.00195228565643687,-1.93009698291304,
-18.6577517412467));
#33810=CARTESIAN_POINT('Ctrl Pts',(-0.00195212946204278,-1.93010456739087,
-18.7826436765513));
#33811=CARTESIAN_POINT('Ctrl Pts',(-0.00195265544136155,-1.93012668860778,
-19.1261923033247));
#33812=CARTESIAN_POINT('Ctrl Pts',(-0.00195299924847534,-1.93016069924505,
-19.6889203191277));
#33813=CARTESIAN_POINT('Ctrl Pts',(-0.0019628499729974,-1.93020222093941,
-20.6909711259829));
#33814=CARTESIAN_POINT('Ctrl Pts',(-0.00197359275882038,-1.93013298869328,
-21.9468251921027));
#33815=CARTESIAN_POINT('Ctrl Pts',(-0.00200870222067299,-1.92987326196219,
-22.9553165950121));
#33816=CARTESIAN_POINT('Ctrl Pts',(-0.00202556675274397,-1.92958934005298,
-23.5851939129496));
#33817=CARTESIAN_POINT('Ctrl Pts',(-0.00203145635328623,-1.92945901432285,
-23.8346016612358));
#33818=CARTESIAN_POINT('Ctrl Pts',(-0.00204696141433901,-1.92914542303968,
-24.3341202973898));
#33819=CARTESIAN_POINT('Ctrl Pts',(-0.00207837479126103,-1.92846700729011,
-25.2099864486648));
#33820=CARTESIAN_POINT('Ctrl Pts',(-0.00215156754501358,-1.92728229243832,
-26.4650381951777));
#33821=CARTESIAN_POINT('Ctrl Pts',(-0.00222333586556621,-1.92577926784895,
-27.9728776779655));
#33822=CARTESIAN_POINT('Ctrl Pts',(-0.00228055085845308,-1.92502813324683,
-28.9776299813488));
#33823=CARTESIAN_POINT('Ctrl Pts',(-0.002298177987237,-1.92470980210758,
-29.5404151696509));
#33824=CARTESIAN_POINT('Ctrl Pts',(-0.00230130766395741,-1.92516042605284,
-29.6505728721337));
#33825=CARTESIAN_POINT('Ctrl Pts',(-0.00230978503821261,-1.92795253854498,
-29.8819857404979));
#33826=CARTESIAN_POINT('Ctrl Pts',(-0.00233059546001059,-1.93743770191964,
-30.288842694958));
#33827=CARTESIAN_POINT('Ctrl Pts',(-0.00239052663365571,-1.97110017924892,
-31.1307375695758));
#33828=CARTESIAN_POINT('Ctrl Pts',(-0.00248975575594169,-2.02609596226747,
-32.1468124521085));
#33829=CARTESIAN_POINT('Ctrl Pts',(-0.00255393362773429,-2.05528304965543,
-33.2184453682104));
#33830=CARTESIAN_POINT('Ctrl Pts',(-0.00255607068676999,-2.05156741016729,
-34.0491340814343));
#33831=CARTESIAN_POINT('Ctrl Pts',(-0.00248991705472534,-2.00898197987319,
-34.9070215761246));
#33832=CARTESIAN_POINT('Ctrl Pts',(-0.0023793876735871,-1.94501401488239,
-35.4954627611981));
#33833=CARTESIAN_POINT('Ctrl Pts',(-0.00226892854331357,-1.87962048862466,
-35.9441896793407));
#33834=CARTESIAN_POINT('Ctrl Pts',(-0.00216704516292421,-1.8240010896022,
-36.2672021766089));
#33835=CARTESIAN_POINT('Ctrl Pts',(-0.00195357476185786,-1.68961350158174,
-36.8772308283305));
#33836=CARTESIAN_POINT('Ctrl Pts',(-0.00155117525253687,-1.40258216824729,
-37.9012275834125));
#33837=CARTESIAN_POINT('Ctrl Pts',(-0.000952370227631846,-0.721863588740229,
-39.7604638106087));
#33838=CARTESIAN_POINT('Ctrl Pts',(-0.000618816224572059,-0.247226512287369,
-41.0986235843677));
#33839=CARTESIAN_POINT('Ctrl Pts',(-0.000457042263932061,-0.115183321968809,
-41.9287308981079));
#33840=CARTESIAN_POINT('Ctrl Pts',(-0.000425764461784592,-0.0860929365982914,
-42.1345110983509));
#33841=CARTESIAN_POINT('Ctrl Pts',(-0.000383611275539338,-0.0537133742847068,
-42.4419305296188));
#33842=CARTESIAN_POINT('Ctrl Pts',(-0.000348398037189352,-0.0295622812038002,
-42.7613877270058));
#33843=CARTESIAN_POINT('Ctrl Pts',(-0.000307974476746251,-0.00823942687768989,
-43.1971433320679));
#33844=CARTESIAN_POINT('Ctrl Pts',(-0.000271596152705288,0.00109993840456285,
-43.7647049359353));
#33845=CARTESIAN_POINT('Ctrl Pts',(-0.000241129946027054,-0.00666211470508639,
-44.4802635490114));
#33846=CARTESIAN_POINT('Ctrl Pts',(-0.000218092509743048,-0.0198790964273407,
-45.105238504849));
#33847=CARTESIAN_POINT('Ctrl Pts',(-0.000210848210031528,-0.0281666779737864,
-45.6222574130482));
#33848=CARTESIAN_POINT('Ctrl Pts',(-0.000203131619834829,-0.0315153753063813,
-46.0183819397791));
#33849=CARTESIAN_POINT('Ctrl Pts',(-0.000192990095033107,-0.0301650435608711,
-46.422899151946));
#33850=CARTESIAN_POINT('Ctrl Pts',(-0.000179976946274749,-0.0194765785343918,
-46.9732794940509));
#33851=CARTESIAN_POINT('Ctrl Pts',(-0.000152921065464157,0.00157914786618924,
-47.3985344890977));
#33852=CARTESIAN_POINT('Ctrl Pts',(-0.000130616097718489,0.0357606605654795,
-47.8315319828244));
#33853=CARTESIAN_POINT('Ctrl Pts',(-0.000115589656268732,0.0549381457458591,
-48.0736438273212));
#33854=CARTESIAN_POINT('Ctrl Pts',(-8.29538197244078E-5,0.0965018439824387,
-48.5881247084077));
#33855=CARTESIAN_POINT('Ctrl Pts',(-1.89201302580575E-5,0.172330139091039,
-49.4816721346524));
#33856=CARTESIAN_POINT('Ctrl Pts',(0.000104768315615061,0.301924242134264,
-50.786702156654));
#33857=CARTESIAN_POINT('Ctrl Pts',(0.000218759891771719,0.519013310827141,
-52.3791099138675));
#33858=CARTESIAN_POINT('Ctrl Pts',(0.000287059711293618,0.725574522676222,
-53.4605852128649));
#33859=CARTESIAN_POINT('Ctrl Pts',(0.000304880749959895,0.880778148203204,
-54.14231167573));
#33860=CARTESIAN_POINT('Ctrl Pts',(0.000309049917928886,0.944038711403875,
-54.4114723712317));
#33861=CARTESIAN_POINT('Ctrl Pts',(0.000313322841748133,1.07873450151376,
-54.9518265359057));
#33862=CARTESIAN_POINT('Ctrl Pts',(0.000314429842083324,1.3327900865459,
-55.8921728030728));
#33863=CARTESIAN_POINT('Ctrl Pts',(0.000284882742374926,1.91027806491778,
-57.7588207333756));
#33864=CARTESIAN_POINT('Ctrl Pts',(0.000237836621859263,2.50353264792865,
-59.3244902541145));
#33865=CARTESIAN_POINT('Ctrl Pts',(0.000214874912799959,2.95403965973707,
-60.4155795542004));
#33866=CARTESIAN_POINT('Ctrl Pts',(0.000211500358311257,3.01275985071423,
-60.5560389550589));
#33867=CARTESIAN_POINT('Ctrl Pts',(0.000204780571771536,3.13054311258116,
-60.8310316498565));
#33868=CARTESIAN_POINT('Ctrl Pts',(0.000191193440495367,3.34315184314077,
-61.3112496976771));
#33869=CARTESIAN_POINT('Ctrl Pts',(0.000162043330489063,3.78669936896942,
-62.2566494682892));
#33870=CARTESIAN_POINT('Ctrl Pts',(0.000118672692779613,4.32424582620751,
-63.3088124541968));
#33871=CARTESIAN_POINT('Ctrl Pts',(8.17628259240602E-5,4.86596465270228,
-64.3301283776222));
#33872=CARTESIAN_POINT('Ctrl Pts',(6.44246275231492E-5,5.16766507371822,
-64.8926939205394));
#33873=CARTESIAN_POINT('Ctrl Pts',(5.42269208335611E-5,5.36553930207075,
-65.262356915369));
#33874=CARTESIAN_POINT('Ctrl Pts',(4.83012049103832E-5,5.49645773933371,
-65.5073328453505));
#33875=CARTESIAN_POINT('Ctrl Pts',(4.1628878654448E-5,5.62570604049499,
-65.7501091651644));
#33876=CARTESIAN_POINT('Ctrl Pts',(3.72381543414075E-5,5.73696806356847,
-65.9604718020035));
#33877=CARTESIAN_POINT('Ctrl Pts',(3.48749553043657E-5,5.7999764236035,
-66.0800772441846));
#33878=CARTESIAN_POINT('Ctrl Pts',(3.15955711106227E-5,5.89390147861976,
-66.2588891870182));
#33879=CARTESIAN_POINT('Ctrl Pts',(2.84193281057929E-5,5.97087483489673,
-66.4065971904426));
#33880=CARTESIAN_POINT('Ctrl Pts',(2.44817438210786E-5,6.09650571081662,
-66.6496744393032));
#33881=CARTESIAN_POINT('Ctrl Pts',(2.04986805459089E-5,6.23418093562956,
-66.9151401191057));
#33882=CARTESIAN_POINT('Ctrl Pts',(1.48718372786516E-5,6.5043619711416,
-67.4327557777686));
#33883=CARTESIAN_POINT('Ctrl Pts',(6.62261016059817E-6,6.97781566951045,
-68.332042634089));
#33884=CARTESIAN_POINT('Ctrl Pts',(4.48053439701293E-6,7.91646970425133,
-70.0908617665458));
#33885=CARTESIAN_POINT('Ctrl Pts',(4.20848049135385E-6,8.71295983512131,
-71.5670614909078));
#33886=CARTESIAN_POINT('Ctrl Pts',(6.84354616859567E-7,9.30803814757989,
-72.6862328888755));
#33887=CARTESIAN_POINT('Ctrl Pts',(5.68114809718481E-7,9.44183934535038,
-72.9378734208353));
#33888=CARTESIAN_POINT('Ctrl Pts',(2.05586755580999E-7,9.70864620119544,
-73.4396602737137));
#33889=CARTESIAN_POINT('Ctrl Pts',(-7.21239062929604E-7,10.0422883693543,
-74.0671487882584));
#33890=CARTESIAN_POINT('Ctrl Pts',(-1.11438109418972E-6,10.442270567524,
-74.8194063862324));
#33891=CARTESIAN_POINT('Ctrl Pts',(-1.71035629119184E-6,11.2420305551737,
-76.3235414328312));
#33892=CARTESIAN_POINT('Ctrl Pts',(-4.32945481586382E-6,11.9082144683072,
-77.5764655497178));
#33893=CARTESIAN_POINT('Ctrl Pts',(-6.05635545269383E-6,12.8781314087794,
-79.4006176028791));
#33894=CARTESIAN_POINT('Ctrl Pts',(-6.94521695860565E-6,13.314695659481,
-80.2216773934557));
#33895=CARTESIAN_POINT('Ctrl Pts',(-6.94521697867286E-6,13.7512172468705,
-81.0426550955541));
#33896=CARTESIAN_POINT('Ctrl Pts',(1.87922065701991,7.61596117959377E-5,
24.8306346333771));
#33897=CARTESIAN_POINT('Ctrl Pts',(1.87922626560681,7.61620135603957E-5,
24.7817553171342));
#33898=CARTESIAN_POINT('Ctrl Pts',(1.87923216025948,7.61760040173549E-5,
24.7328772886127));
#33899=CARTESIAN_POINT('Ctrl Pts',(1.87930120315869,7.58194923152649E-5,
24.1822612927019));
#33900=CARTESIAN_POINT('Ctrl Pts',(1.87935079445246,7.26740057884463E-5,
23.1780602344503));
#33901=CARTESIAN_POINT('Ctrl Pts',(1.87947388483842,7.25425928646775E-5,
21.169454415134));
#33902=CARTESIAN_POINT('Ctrl Pts',(1.87992747111033,6.47238710413929E-5,
19.6651383523929));
#33903=CARTESIAN_POINT('Ctrl Pts',(1.88090486185821,6.13733892703204E-5,
18.4140184893336));
#33904=CARTESIAN_POINT('Ctrl Pts',(1.88137478720441,6.09217268373628E-5,
17.9111909771165));
#33905=CARTESIAN_POINT('Ctrl Pts',(1.88255374297555,5.89108913871656E-5,
16.9071548405334));
#33906=CARTESIAN_POINT('Ctrl Pts',(1.88508516688353,5.70155313945553E-5,
15.1532951221729));
#33907=CARTESIAN_POINT('Ctrl Pts',(1.88747375765592,3.89855064059539E-5,
13.651177276246));
#33908=CARTESIAN_POINT('Ctrl Pts',(1.8889753781808,2.96207864364287E-5,
12.3965256878489));
#33909=CARTESIAN_POINT('Ctrl Pts',(1.88959196096303,2.81242245297611E-5,
11.8955214044168));
#33910=CARTESIAN_POINT('Ctrl Pts',(1.8908457391163,2.10877770421448E-5,
10.893623706362));
#33911=CARTESIAN_POINT('Ctrl Pts',(1.89302201588768,1.3952629727407E-5,
9.13968114018261));
#33912=CARTESIAN_POINT('Ctrl Pts',(1.89449907752566,-4.11353129124917E-5,
7.63425381206281));
#33913=CARTESIAN_POINT('Ctrl Pts',(1.89515906367933,-5.7372725229025E-5,
6.50080706358199));
#33914=CARTESIAN_POINT('Ctrl Pts',(1.89540762219618,0.0023494898295555,
6.22210496316194));
#33915=CARTESIAN_POINT('Ctrl Pts',(1.89622309817872,0.0147904875425885,
5.69012664502278));
#33916=CARTESIAN_POINT('Ctrl Pts',(1.89824710817307,0.0509794365844755,
4.77314810156052));
#33917=CARTESIAN_POINT('Ctrl Pts',(1.90315893713563,0.143311521409256,3.0355352845081));
#33918=CARTESIAN_POINT('Ctrl Pts',(1.90277046926461,0.135314710798477,1.70830615109979));
#33919=CARTESIAN_POINT('Ctrl Pts',(1.89514572110263,0.0135512360379868,
0.851649839357737));
#33920=CARTESIAN_POINT('Ctrl Pts',(1.89416706532207,-0.000481487034814646,
0.761093637132466));
#33921=CARTESIAN_POINT('Ctrl Pts',(1.89191197327707,-0.0349124265759622,
0.568317371434498));
#33922=CARTESIAN_POINT('Ctrl Pts',(1.88726269607664,-0.108411282795717,
0.222787915872012));
#33923=CARTESIAN_POINT('Ctrl Pts',(1.87891203932446,-0.251263790050898,
-0.305614290368038));
#33924=CARTESIAN_POINT('Ctrl Pts',(1.8672190151571,-0.472266342518573,-0.986136213316851));
#33925=CARTESIAN_POINT('Ctrl Pts',(1.85019799115212,-0.813392882796135,
-1.95256231630457));
#33926=CARTESIAN_POINT('Ctrl Pts',(1.82794512867848,-1.28446993438294,-3.26430893703937));
#33927=CARTESIAN_POINT('Ctrl Pts',(1.81272281017777,-1.59859453901927,-4.44274312874163));
#33928=CARTESIAN_POINT('Ctrl Pts',(1.80638910274363,-1.7273997721369,-5.22825505005266));
#33929=CARTESIAN_POINT('Ctrl Pts',(1.80427869767207,-1.76905831655269,-5.50731245895802));
#33930=CARTESIAN_POINT('Ctrl Pts',(1.80065184481023,-1.83997895086455,-6.07909111574944));
#33931=CARTESIAN_POINT('Ctrl Pts',(1.79607620867608,-1.92592867677439,-7.05450472650263));
#33932=CARTESIAN_POINT('Ctrl Pts',(1.79334543307704,-1.96958741569615,-8.40665558072903));
#33933=CARTESIAN_POINT('Ctrl Pts',(1.79301141822182,-1.96539730646951,-9.68813059631163));
#33934=CARTESIAN_POINT('Ctrl Pts',(1.79274419096131,-1.96474439193333,-10.5492997925194));
#33935=CARTESIAN_POINT('Ctrl Pts',(1.79241023005762,-1.96830968052557,-11.0303231475472));
#33936=CARTESIAN_POINT('Ctrl Pts',(1.79215465822465,-1.97196962659183,-11.2670853827026));
#33937=CARTESIAN_POINT('Ctrl Pts',(1.79192032589268,-1.97562733286965,-11.4443710457125));
#33938=CARTESIAN_POINT('Ctrl Pts',(1.79175912918206,-1.9781959777931,-11.5768517128996));
#33939=CARTESIAN_POINT('Ctrl Pts',(1.79147608617423,-1.98253698716417,-11.8336633529133));
#33940=CARTESIAN_POINT('Ctrl Pts',(1.79105482303264,-1.98861872995816,-12.2853438149451));
#33941=CARTESIAN_POINT('Ctrl Pts',(1.79033442655468,-1.99684810126393,-13.4361224209512));
#33942=CARTESIAN_POINT('Ctrl Pts',(1.79037559992281,-1.98952102095365,-14.6974307834233));
#33943=CARTESIAN_POINT('Ctrl Pts',(1.79063171507148,-1.98067118531168,-15.9474082220266));
#33944=CARTESIAN_POINT('Ctrl Pts',(1.79073917055929,-1.97706320348729,-16.5707963211281));
#33945=CARTESIAN_POINT('Ctrl Pts',(1.79079316205804,-1.97538781040393,-17.0687964452538));
#33946=CARTESIAN_POINT('Ctrl Pts',(1.79079992984237,-1.97507008585841,-17.3176695608236));
#33947=CARTESIAN_POINT('Ctrl Pts',(1.79079700457479,-1.97507098594446,-17.5035869553218));
#33948=CARTESIAN_POINT('Ctrl Pts',(1.79079820480672,-1.97507223472088,-17.6286902970982));
#33949=CARTESIAN_POINT('Ctrl Pts',(1.79081303643941,-1.97507694677315,-17.8777168846834));
#33950=CARTESIAN_POINT('Ctrl Pts',(1.7908423737458,-1.97508492772897,-18.1273505684258));
#33951=CARTESIAN_POINT('Ctrl Pts',(1.7908870071724,-1.97509460752825,-18.3768683685547));
#33952=CARTESIAN_POINT('Ctrl Pts',(1.79091958228694,-1.97510139113122,-18.5329310092027));
#33953=CARTESIAN_POINT('Ctrl Pts',(1.7909485715885,-1.97510703421114,-18.6577947414661));
#33954=CARTESIAN_POINT('Ctrl Pts',(1.79097929787607,-1.97511272116633,-18.7826880802208));
#33955=CARTESIAN_POINT('Ctrl Pts',(1.79106851433894,-1.97513010281441,-19.1262383518251));
#33956=CARTESIAN_POINT('Ctrl Pts',(1.7912440182103,-1.97515778890431,-19.6889570515333));
#33957=CARTESIAN_POINT('Ctrl Pts',(1.79156652620716,-1.97520162435307,-20.6909569831857));
#33958=CARTESIAN_POINT('Ctrl Pts',(1.79190032472266,-1.97517555483402,-21.9466829676396));
#33959=CARTESIAN_POINT('Ctrl Pts',(1.79181893930524,-1.97502933168004,-22.9550048537654));
#33960=CARTESIAN_POINT('Ctrl Pts',(1.79160011312644,-1.97485112618095,-23.5847540984166));
#33961=CARTESIAN_POINT('Ctrl Pts',(1.79149584037637,-1.974767994845,-23.8340852761802));
#33962=CARTESIAN_POINT('Ctrl Pts',(1.79121783036047,-1.97456755508006,-24.3334861354704));
#33963=CARTESIAN_POINT('Ctrl Pts',(1.79057296578653,-1.97413291472412,-25.2091818472031));
#33964=CARTESIAN_POINT('Ctrl Pts',(1.78932843181765,-1.97337654638549,-26.4641335002892));
#33965=CARTESIAN_POINT('Ctrl Pts',(1.7877667392985,-1.97241463979719,-27.9720406937298));
#33966=CARTESIAN_POINT('Ctrl Pts',(1.78696631713144,-1.97193620457676,-28.9770024271066));
#33967=CARTESIAN_POINT('Ctrl Pts',(1.78666350274049,-1.97173369920145,-29.5399069473805));
#33968=CARTESIAN_POINT('Ctrl Pts',(1.78657098731778,-1.97221656613458,-29.6497131023628));
#33969=CARTESIAN_POINT('Ctrl Pts',(1.78629442080549,-1.9751112788456,-29.8806978494081));
#33970=CARTESIAN_POINT('Ctrl Pts',(1.7855939429116,-1.98486158926284,-30.2868406514868));
#33971=CARTESIAN_POINT('Ctrl Pts',(1.78349968794802,-2.01935510224964,-31.1279669106716));
#33972=CARTESIAN_POINT('Ctrl Pts',(1.78043296885725,-2.07565946440525,-32.1444103650944));
#33973=CARTESIAN_POINT('Ctrl Pts',(1.77875938834126,-2.10561496942114,-33.2176998689347));
#33974=CARTESIAN_POINT('Ctrl Pts',(1.77884649386387,-2.10188115948581,-34.0502677224308));
#33975=CARTESIAN_POINT('Ctrl Pts',(1.78097744958609,-2.05830577735026,-34.9106860529736));
#33976=CARTESIAN_POINT('Ctrl Pts',(1.78422692571106,-1.99276232309771,-35.5011821085368));
#33977=CARTESIAN_POINT('Ctrl Pts',(1.78750554178346,-1.92573953974817,-35.9515615389986));
#33978=CARTESIAN_POINT('Ctrl Pts',(1.79029021991389,-1.86866336738416,-36.276149755922));
#33979=CARTESIAN_POINT('Ctrl Pts',(1.79691647755597,-1.73088180147094,-36.8884573580224));
#33980=CARTESIAN_POINT('Ctrl Pts',(1.8111128882931,-1.43672381918429,-37.9153989559922));
#33981=CARTESIAN_POINT('Ctrl Pts',(1.84323794506374,-0.739869809114935,
-39.7767029410827));
#33982=CARTESIAN_POINT('Ctrl Pts',(1.86947535510397,-0.254607037277298,
-41.1128294039107));
#33983=CARTESIAN_POINT('Ctrl Pts',(1.87899508576981,-0.120158475357969,
-41.9361875204854));
#33984=CARTESIAN_POINT('Ctrl Pts',(1.88089764189098,-0.0904014568632321,
-42.1412540027529));
#33985=CARTESIAN_POINT('Ctrl Pts',(1.88326412278239,-0.057233445228627,
-42.4473182514808));
#33986=CARTESIAN_POINT('Ctrl Pts',(1.88516231205803,-0.032387317552159,
-42.7656567863243));
#33987=CARTESIAN_POINT('Ctrl Pts',(1.88713894608345,-0.0103148900108803,
-43.2000120944421));
#33988=CARTESIAN_POINT('Ctrl Pts',(1.88867239674863,-0.000330444911487711,
-43.7661869076419));
#33989=CARTESIAN_POINT('Ctrl Pts',(1.88943137570746,-0.00773447396790047,
-44.4806273744286));
#33990=CARTESIAN_POINT('Ctrl Pts',(1.88952521953819,-0.0208897500709426,
-45.1051458260789));
#33991=CARTESIAN_POINT('Ctrl Pts',(1.88943909368804,-0.0292027843404737,
-45.6220800031513));
#33992=CARTESIAN_POINT('Ctrl Pts',(1.88937202606144,-0.0325689471320249,
-46.0182813039979));
#33993=CARTESIAN_POINT('Ctrl Pts',(1.88935229353195,-0.0312056430228143,
-46.4230162698549));
#33994=CARTESIAN_POINT('Ctrl Pts',(1.88944668290529,-0.0204177420640209,
-46.9738736665184));
#33995=CARTESIAN_POINT('Ctrl Pts',(1.88977797873393,0.000877657567567272,
-47.3996979493288));
#33996=CARTESIAN_POINT('Ctrl Pts',(1.89033911609484,0.0354747851842442,
-47.8333811257174));
#33997=CARTESIAN_POINT('Ctrl Pts',(1.89071470667213,0.0548501897799582,
-48.0753819531635));
#33998=CARTESIAN_POINT('Ctrl Pts',(1.89146761287879,0.0968621047481274,
-48.5899412044517));
#33999=CARTESIAN_POINT('Ctrl Pts',(1.89277126953455,0.173459077297203,-49.4834146851367));
#34000=CARTESIAN_POINT('Ctrl Pts',(1.89449745127194,0.304140752206121,-50.7882896551614));
#34001=CARTESIAN_POINT('Ctrl Pts',(1.89579350141421,0.522243515316254,-52.3802470077318));
#34002=CARTESIAN_POINT('Ctrl Pts',(1.89593212526715,0.729188120289724,-53.461300559368));
#34003=CARTESIAN_POINT('Ctrl Pts',(1.89567407999173,0.884486289122258,-54.1427309942361));
#34004=CARTESIAN_POINT('Ctrl Pts',(1.8955253537994,0.947765356447221,-54.4117640933295));
#34005=CARTESIAN_POINT('Ctrl Pts',(1.89506593219007,1.0824539958618,-54.9518980607266));
#34006=CARTESIAN_POINT('Ctrl Pts',(1.8939009228576,1.33638837878062,-55.8919177460886));
#34007=CARTESIAN_POINT('Ctrl Pts',(1.89049136136924,1.91330971648247,-57.7581672374045));
#34008=CARTESIAN_POINT('Ctrl Pts',(1.88706535826581,2.50588183666261,-59.3238564112775));
#34009=CARTESIAN_POINT('Ctrl Pts',(1.88561817574945,2.95613587497698,-60.4151086469192));
#34010=CARTESIAN_POINT('Ctrl Pts',(1.88543527559833,3.01480092392394,-60.5555376788414));
#34011=CARTESIAN_POINT('Ctrl Pts',(1.88507824362982,3.13248322009135,-60.830502284115));
#34012=CARTESIAN_POINT('Ctrl Pts',(1.8844607487485,3.34489889769905,-61.310665724608));
#34013=CARTESIAN_POINT('Ctrl Pts',(1.88328108508382,3.78803882885241,-62.2560020211235));
#34014=CARTESIAN_POINT('Ctrl Pts',(1.88206459657106,4.32509239194982,-63.3081532507657));
#34015=CARTESIAN_POINT('Ctrl Pts',(1.88103553773681,4.86638112300206,-64.3295185491561));
#34016=CARTESIAN_POINT('Ctrl Pts',(1.88053102808851,5.1678768730388,-64.8921339858536));
#34017=CARTESIAN_POINT('Ctrl Pts',(1.88022675171844,5.3656359116224,-65.2618402500252));
#34018=CARTESIAN_POINT('Ctrl Pts',(1.88003357553327,5.49648391025698,-65.5068478162644));
#34019=CARTESIAN_POINT('Ctrl Pts',(1.87985097591106,5.62567062746725,-65.7496599480654));
#34020=CARTESIAN_POINT('Ctrl Pts',(1.87970493381329,5.73688874252341,-65.9600579521806));
#34021=CARTESIAN_POINT('Ctrl Pts',(1.87962492948782,5.79987484390888,-66.079684794079));
#34022=CARTESIAN_POINT('Ctrl Pts',(1.87950863690349,5.89376947121256,-66.2585300435357));
#34023=CARTESIAN_POINT('Ctrl Pts',(1.87941758530446,5.97072330512786,-66.4062684787644));
#34024=CARTESIAN_POINT('Ctrl Pts',(1.87927867663299,6.09633110207486,-66.64939961239));
#34025=CARTESIAN_POINT('Ctrl Pts',(1.87915208151063,6.23397919347889,-66.9149080623945));
#34026=CARTESIAN_POINT('Ctrl Pts',(1.87896352134001,6.50413138058693,-67.4326071669248));
#34027=CARTESIAN_POINT('Ctrl Pts',(1.87877816093101,6.97757667318536,-68.3320150970721));
#34028=CARTESIAN_POINT('Ctrl Pts',(1.8788680390831,7.91634487377019,-70.0909875251694));
#34029=CARTESIAN_POINT('Ctrl Pts',(1.87924656738061,8.71295995044206,-71.567154267523));
#34030=CARTESIAN_POINT('Ctrl Pts',(1.87923337319213,9.30797784656764,-72.6862215632396));
#34031=CARTESIAN_POINT('Ctrl Pts',(1.87923193113062,9.44178242559873,-72.9378697596276));
#34032=CARTESIAN_POINT('Ctrl Pts',(1.87922940657654,9.70858682183065,-73.4396541033119));
#34033=CARTESIAN_POINT('Ctrl Pts',(1.87922645837445,10.0422299603181,-74.0671465227276));
#34034=CARTESIAN_POINT('Ctrl Pts',(1.87922558503116,10.4422120792725,-74.8194044878806));
#34035=CARTESIAN_POINT('Ctrl Pts',(1.87922606073315,11.2419738247468,-76.3235419027106));
#34036=CARTESIAN_POINT('Ctrl Pts',(1.87922464770105,11.9081581569989,-77.5764660419606));
#34037=CARTESIAN_POINT('Ctrl Pts',(1.87922138294482,12.8780733791962,-79.4006165956265));
#34038=CARTESIAN_POINT('Ctrl Pts',(1.8792197023166,13.3146376913136,-80.2216773930927));
#34039=CARTESIAN_POINT('Ctrl Pts',(1.87921970231659,13.7511592787031,-81.042655095191));
#34040=CARTESIAN_POINT('Ctrl Pts',(4.38494444132642,-0.000133734827608889,
24.8306349039861));
#34041=CARTESIAN_POINT('Ctrl Pts',(4.38495753146493,-0.00013374032887973,
24.7817555964521));
#34042=CARTESIAN_POINT('Ctrl Pts',(4.38497125731604,-0.000133744552648744,
24.7328775966515));
#34043=CARTESIAN_POINT('Ctrl Pts',(4.38513347473583,-0.000133864397380097,
24.1822610347766));
#34044=CARTESIAN_POINT('Ctrl Pts',(4.3852582468995,-0.000134433697096954,
23.1780545188473));
#34045=CARTESIAN_POINT('Ctrl Pts',(4.38554667014594,-0.000134855584066727,
21.1694482846898));
#34046=CARTESIAN_POINT('Ctrl Pts',(4.38662762097494,-0.000136376740863039,
19.6651183959319));
#34047=CARTESIAN_POINT('Ctrl Pts',(4.38891822538359,-0.000137371987590711,
18.41399250541));
#34048=CARTESIAN_POINT('Ctrl Pts',(4.3900163968666,-0.000137730298437801,
17.9111645886437));
#34049=CARTESIAN_POINT('Ctrl Pts',(4.39277406888475,-0.000138809563126842,
16.907124878646));
#34050=CARTESIAN_POINT('Ctrl Pts',(4.3986885227367,-0.000140770907664884,
15.1532609539057));
#34051=CARTESIAN_POINT('Ctrl Pts',(4.40431300958534,-0.000144270691794568,
13.651109619525));
#34052=CARTESIAN_POINT('Ctrl Pts',(4.4078411305582,-0.00014522718386964,
12.39644086798));
#34053=CARTESIAN_POINT('Ctrl Pts',(4.4092832051397,-0.000145137964999622,
11.8954314878313));
#34054=CARTESIAN_POINT('Ctrl Pts',(4.41222508668909,-0.000145387654091127,
10.8935279540275));
#34055=CARTESIAN_POINT('Ctrl Pts',(4.41731809368509,-0.000143543800937141,
9.13954994961948));
#34056=CARTESIAN_POINT('Ctrl Pts',(4.42090548426581,-0.000150527145067114,
7.63410559711367));
#34057=CARTESIAN_POINT('Ctrl Pts',(4.42249863000223,-0.000147353245287479,
6.50044700529247));
#34058=CARTESIAN_POINT('Ctrl Pts',(4.42299616630408,0.00248284197451034,
6.21934256026946));
#34059=CARTESIAN_POINT('Ctrl Pts',(4.42445914823768,0.0160554202489226,
5.6847549980432));
#34060=CARTESIAN_POINT('Ctrl Pts',(4.42790007773388,0.0554580633367147,
4.76457601399349));
#34061=CARTESIAN_POINT('Ctrl Pts',(4.43584107924143,0.155572358940781,3.0286903083529));
#34062=CARTESIAN_POINT('Ctrl Pts',(4.43543312462318,0.146415497950293,1.71703744849467));
#34063=CARTESIAN_POINT('Ctrl Pts',(4.4235845204549,0.0168898128865376,0.876374772474017));
#34064=CARTESIAN_POINT('Ctrl Pts',(4.42204892079727,0.00214081928892977,
0.78860210460576));
#34065=CARTESIAN_POINT('Ctrl Pts',(4.4185311781697,-0.0343048651997382,
0.60032047710926));
#34066=CARTESIAN_POINT('Ctrl Pts',(4.41130252706129,-0.112371934479805,
0.261667363808621));
#34067=CARTESIAN_POINT('Ctrl Pts',(4.39851668321994,-0.265181268990898,
-0.260360024829797));
#34068=CARTESIAN_POINT('Ctrl Pts',(4.3805994085879,-0.503172644073552,-0.93691151551543));
#34069=CARTESIAN_POINT('Ctrl Pts',(4.35467542905104,-0.871862859368354,
-1.90182031569792));
#34070=CARTESIAN_POINT('Ctrl Pts',(4.32024185028443,-1.38292737347823,-3.21699911158908));
#34071=CARTESIAN_POINT('Ctrl Pts',(4.29559179121607,-1.72574738134475,-4.40684408194398));
#34072=CARTESIAN_POINT('Ctrl Pts',(4.28494920984687,-1.86685375632645,-5.20438075326181));
#34073=CARTESIAN_POINT('Ctrl Pts',(4.28149639120192,-1.91214565680086,-5.48564350309126));
#34074=CARTESIAN_POINT('Ctrl Pts',(4.27549161115425,-1.98936167253877,-6.06291218185832));
#34075=CARTESIAN_POINT('Ctrl Pts',(4.26796048132989,-2.08262140259452,-7.04610453435813));
#34076=CARTESIAN_POINT('Ctrl Pts',(4.26350476705694,-2.12952827711346,-8.40605252302899));
#34077=CARTESIAN_POINT('Ctrl Pts',(4.26290160138965,-2.12453036670742,-9.68968775091903));
#34078=CARTESIAN_POINT('Ctrl Pts',(4.26233004431676,-2.1235993642786,-10.5496387643383));
#34079=CARTESIAN_POINT('Ctrl Pts',(4.26172062194488,-2.12731348831879,-11.0291331838308));
#34080=CARTESIAN_POINT('Ctrl Pts',(4.26127901825024,-2.13119193174928,-11.2648521645087));
#34081=CARTESIAN_POINT('Ctrl Pts',(4.26088060468755,-2.1350823139462,-11.4412807325406));
#34082=CARTESIAN_POINT('Ctrl Pts',(4.26059750053618,-2.13783715675781,-11.5742931051035));
#34083=CARTESIAN_POINT('Ctrl Pts',(4.26009539343274,-2.14247157126928,-11.8315148074345));
#34084=CARTESIAN_POINT('Ctrl Pts',(4.25933127536179,-2.1489410967831,-12.2841524738275));
#34085=CARTESIAN_POINT('Ctrl Pts',(4.25794700299552,-2.15752446875554,-13.4367348500518));
#34086=CARTESIAN_POINT('Ctrl Pts',(4.25774924560805,-2.14923093736645,-14.6990441605346));
#34087=CARTESIAN_POINT('Ctrl Pts',(4.257898891459,-2.13944675254938,-15.9487908781029));
#34088=CARTESIAN_POINT('Ctrl Pts',(4.25798947493779,-2.1354625341751,-16.5717918598142));
#34089=CARTESIAN_POINT('Ctrl Pts',(4.25802180761526,-2.13361607940448,-17.069305966523));
#34090=CARTESIAN_POINT('Ctrl Pts',(4.25801831252641,-2.13326166550583,-17.3178788519545));
#34091=CARTESIAN_POINT('Ctrl Pts',(4.25800523628165,-2.13325861396676,-17.5035575132461));
#34092=CARTESIAN_POINT('Ctrl Pts',(4.25800303403809,-2.13325625333121,-17.6287430664321));
#34093=CARTESIAN_POINT('Ctrl Pts',(4.25802247592092,-2.1332510321176,-17.877785314546));
#34094=CARTESIAN_POINT('Ctrl Pts',(4.25807533223794,-2.13324369231377,-18.1274759620926));
#34095=CARTESIAN_POINT('Ctrl Pts',(4.25815578201396,-2.13323742070418,-18.3770116479716));
#34096=CARTESIAN_POINT('Ctrl Pts',(4.25821655397436,-2.13323347698379,-18.5330869888321));
#34097=CARTESIAN_POINT('Ctrl Pts',(4.2582707462992,-2.13323068283773,-18.6579557153899));
#34098=CARTESIAN_POINT('Ctrl Pts',(4.25832845323534,-2.13322798751371,-18.7828528356388));
#34099=CARTESIAN_POINT('Ctrl Pts',(4.25850066708906,-2.13322198399732,-19.1264052228547));
#34100=CARTESIAN_POINT('Ctrl Pts',(4.25884627993172,-2.13321684857528,-19.6890852084046));
#34101=CARTESIAN_POINT('Ctrl Pts',(4.25952647816828,-2.13325378494267,-20.6908951968342));
#34102=CARTESIAN_POINT('Ctrl Pts',(4.2602843313177,-2.13339493823762,-21.9461580058192));
#34103=CARTESIAN_POINT('Ctrl Pts',(4.26033098793204,-2.13372045578471,-22.9538712271591));
#34104=CARTESIAN_POINT('Ctrl Pts',(4.26004237114559,-2.133993612134,-23.5831634906123));
#34105=CARTESIAN_POINT('Ctrl Pts',(4.25989601774496,-2.13411302553283,-23.8322171555192));
#34106=CARTESIAN_POINT('Ctrl Pts',(4.2594892722799,-2.13440115952288,-24.3311913273362));
#34107=CARTESIAN_POINT('Ctrl Pts',(4.2585180312423,-2.13500677200017,-25.2062722948472));
#34108=CARTESIAN_POINT('Ctrl Pts',(4.25661156107835,-2.13611445719196,-26.4608432571924));
#34109=CARTESIAN_POINT('Ctrl Pts',(4.25421514420097,-2.13743125211775,-27.9689958353944));
#34110=CARTESIAN_POINT('Ctrl Pts',(4.25301855845424,-2.13818538230176,-28.9746783685956));
#34111=CARTESIAN_POINT('Ctrl Pts',(4.252594337193,-2.13848119146963,-29.5380129894862));
#34112=CARTESIAN_POINT('Ctrl Pts',(4.25246494386027,-2.13909508958004,-29.6465829713314));
#34113=CARTESIAN_POINT('Ctrl Pts',(4.25207003987882,-2.14239521561274,-29.8760648068341));
#34114=CARTESIAN_POINT('Ctrl Pts',(4.25104839864593,-2.15319445238582,-30.2796942725863));
#34115=CARTESIAN_POINT('Ctrl Pts',(4.24794966511473,-2.19091521088286,-31.1181176652429));
#34116=CARTESIAN_POINT('Ctrl Pts',(4.24321206419763,-2.25241329623747,-32.135797088019));
#34117=CARTESIAN_POINT('Ctrl Pts',(4.24060853356921,-2.28545836031402,-33.2148794748876));
#34118=CARTESIAN_POINT('Ctrl Pts',(4.24082448438597,-2.28175122961546,-34.0540552676246));
#34119=CARTESIAN_POINT('Ctrl Pts',(4.24437157033838,-2.23460163035187,-34.9233354941886));
#34120=CARTESIAN_POINT('Ctrl Pts',(4.24977549528951,-2.16323890794728,-35.5209805461277));
#34121=CARTESIAN_POINT('Ctrl Pts',(4.25525670096684,-2.09011394025412,-35.9770689509718));
#34122=CARTESIAN_POINT('Ctrl Pts',(4.26000233546485,-2.02758438872165,-36.3070700362323));
#34123=CARTESIAN_POINT('Ctrl Pts',(4.27103057364325,-1.87705461603904,-36.9270605674051));
#34124=CARTESIAN_POINT('Ctrl Pts',(4.29385848486922,-1.55664513660238,-37.9636207856555));
#34125=CARTESIAN_POINT('Ctrl Pts',(4.34311304510202,-0.800125491514468,
-39.8308322541445));
#34126=CARTESIAN_POINT('Ctrl Pts',(4.38119483574206,-0.278451825361257,
-41.1616575831691));
#34127=CARTESIAN_POINT('Ctrl Pts',(4.39548516377524,-0.136693188783896,
-41.9619869949894));
#34128=CARTESIAN_POINT('Ctrl Pts',(4.39842520476576,-0.104631661251257,
-42.1646065536608));
#34129=CARTESIAN_POINT('Ctrl Pts',(4.40208173363288,-0.0688288777778128,
-42.4659900876119));
#34130=CARTESIAN_POINT('Ctrl Pts',(4.40504729703054,-0.0416183495331478,
-42.7804374760604));
#34131=CARTESIAN_POINT('Ctrl Pts',(4.4081429290184,-0.0170206407560294,
-43.2099117875883));
#34132=CARTESIAN_POINT('Ctrl Pts',(4.41057027474141,-0.00485691508605945,
-43.77123943215));
#34133=CARTESIAN_POINT('Ctrl Pts',(4.4117742870394,-0.0110935056786064,
-44.4817888698965));
#34134=CARTESIAN_POINT('Ctrl Pts',(4.41188659105624,-0.024134170747513,
-45.1047465724255));
#34135=CARTESIAN_POINT('Ctrl Pts',(4.41175636241589,-0.0325221901227191,
-45.6214015911291));
#34136=CARTESIAN_POINT('Ctrl Pts',(4.41163173721691,-0.0359483457055346,
-46.0178897568402));
#34137=CARTESIAN_POINT('Ctrl Pts',(4.41156042456205,-0.0345379690853276,
-46.4234084111503));
#34138=CARTESIAN_POINT('Ctrl Pts',(4.41164198332398,-0.0233685406918769,
-46.975965217637));
#34139=CARTESIAN_POINT('Ctrl Pts',(4.41202937942913,-0.00125959827215216,
-47.4038163878187));
#34140=CARTESIAN_POINT('Ctrl Pts',(4.41278495644332,0.0348396358383206,
-47.8399267824656));
#34141=CARTESIAN_POINT('Ctrl Pts',(4.4132838759114,0.0549196106208449,-48.0815831819142));
#34142=CARTESIAN_POINT('Ctrl Pts',(4.41425913138979,0.0985496371173923,
-48.5964805029828));
#34143=CARTESIAN_POINT('Ctrl Pts',(4.41587201080464,0.177932520964587,-49.4897871839858));
#34144=CARTESIAN_POINT('Ctrl Pts',(4.41774428372684,0.312552417560597,-50.7942048465594));
#34145=CARTESIAN_POINT('Ctrl Pts',(4.41871611176856,0.534548942698696,-52.3845058858798));
#34146=CARTESIAN_POINT('Ctrl Pts',(4.41811880571771,0.742912336433342,-53.4639470870333));
#34147=CARTESIAN_POINT('Ctrl Pts',(4.41723188071979,0.898550865422039,-54.1442117798183));
#34148=CARTESIAN_POINT('Ctrl Pts',(4.41680184496303,0.961905712297198,-54.41276250448));
#34149=CARTESIAN_POINT('Ctrl Pts',(4.4156507935149,1.09657035164313,-54.9520528656041));
#34150=CARTESIAN_POINT('Ctrl Pts',(4.41298531917194,1.35002999176865,-55.8908387686135));
#34151=CARTESIAN_POINT('Ctrl Pts',(4.40577743472443,1.92474191344074,-57.755588741959));
#34152=CARTESIAN_POINT('Ctrl Pts',(4.39894561258167,2.51469589787006,-59.3214284512625));
#34153=CARTESIAN_POINT('Ctrl Pts',(4.39608239703651,2.96398234750693,-60.4133254990442));
#34154=CARTESIAN_POINT('Ctrl Pts',(4.39572420020829,3.02243441040618,-60.5536403951176));
#34155=CARTESIAN_POINT('Ctrl Pts',(4.39503159740573,3.13972743028378,-60.8285020826318));
#34156=CARTESIAN_POINT('Ctrl Pts',(4.39385789835129,3.35140393735138,-61.3084658780271));
#34157=CARTESIAN_POINT('Ctrl Pts',(4.39168537592052,3.79298878201076,-62.2535803239954));
#34158=CARTESIAN_POINT('Ctrl Pts',(4.38959734540799,4.3281999379598,-63.3057043206065));
#34159=CARTESIAN_POINT('Ctrl Pts',(4.38788098922377,4.86787702280524,-64.3272637172959));
#34160=CARTESIAN_POINT('Ctrl Pts',(4.38704573394525,5.16860177178643,-64.8900676807838));
#34161=CARTESIAN_POINT('Ctrl Pts',(4.38654071275671,5.36592715697807,-65.2599366680509));
#34162=CARTESIAN_POINT('Ctrl Pts',(4.38621762817815,5.49650820835829,-65.5050630813914));
#34163=CARTESIAN_POINT('Ctrl Pts',(4.38591471255685,5.62546575748379,-65.7480091109017));
#34164=CARTESIAN_POINT('Ctrl Pts',(4.38566703852788,5.73651809548135,-65.9585397229399));
#34165=CARTESIAN_POINT('Ctrl Pts',(4.38553044241807,5.79942023400714,-66.0782468295102));
#34166=CARTESIAN_POINT('Ctrl Pts',(4.38533047147116,5.89319979678333,-66.2572170941181));
#34167=CARTESIAN_POINT('Ctrl Pts',(4.38517400334211,5.97008206126848,-66.4050691863734));
#34168=CARTESIAN_POINT('Ctrl Pts',(4.38492849824558,6.09560395288787,-66.6484025458349));
#34169=CARTESIAN_POINT('Ctrl Pts',(4.38470615525269,6.23315175334774,-66.9140716153702));
#34170=CARTESIAN_POINT('Ctrl Pts',(4.38437396671341,6.50319749318971,-67.4320845675039));
#34171=CARTESIAN_POINT('Ctrl Pts',(4.38405715027776,6.97662108137445,-68.331945776566));
#34172=CARTESIAN_POINT('Ctrl Pts',(4.38423359111322,7.91583209385217,-70.0914928447299));
#34173=CARTESIAN_POINT('Ctrl Pts',(4.38494215631249,8.71294426216148,-71.5675208905616));
#34174=CARTESIAN_POINT('Ctrl Pts',(4.38493000258167,9.30774093474432,-72.6861891777452));
#34175=CARTESIAN_POINT('Ctrl Pts',(4.38492777760085,9.44155851431508,-72.9378663168809));
#34176=CARTESIAN_POINT('Ctrl Pts',(4.38492441286894,9.70835430006309,-73.4396407360582));
#34177=CARTESIAN_POINT('Ctrl Pts',(4.38492215877831,10.0420032022086,-74.0671467503144));
#34178=CARTESIAN_POINT('Ctrl Pts',(4.38492189125759,10.4419859347932,-74.8194055694887));
#34179=CARTESIAN_POINT('Ctrl Pts',(4.38492474424574,11.2417558570399,-76.3235510600817));
#34180=CARTESIAN_POINT('Ctrl Pts',(4.38493101488265,11.9079483102949,-77.5764715046922));
#34181=CARTESIAN_POINT('Ctrl Pts',(4.38493092127123,12.8778611632279,-79.4006140082112));
#34182=CARTESIAN_POINT('Ctrl Pts',(4.38493087314377,13.3144278324901,-80.2216773891645));
#34183=CARTESIAN_POINT('Ctrl Pts',(4.38493087314375,13.7509494198795,-81.0426550912629));
#34184=CARTESIAN_POINT('Ctrl Pts',(6.89104910298435,-0.00024498498954306,
24.8306350459706));
#34185=CARTESIAN_POINT('Ctrl Pts',(6.89106969042788,-0.000244992005475219,
24.7817557429577));
#34186=CARTESIAN_POINT('Ctrl Pts',(6.89109126507086,-0.000244999363845071,
24.7328777610462));
#34187=CARTESIAN_POINT('Ctrl Pts',(6.8913468151815,-0.000245085668324933,
24.1822608050565));
#34188=CARTESIAN_POINT('Ctrl Pts',(6.89154686940115,-0.000245309193916475,
23.1780506245846));
#34189=CARTESIAN_POINT('Ctrl Pts',(6.89200170238563,-0.000245943228249708,
21.1694440815797));
#34190=CARTESIAN_POINT('Ctrl Pts',(6.89371055321136,-0.000246501152717097,
19.6651049165689));
#34191=CARTESIAN_POINT('Ctrl Pts',(6.89731549185056,-0.000246902951521312,
18.4139749758576));
#34192=CARTESIAN_POINT('Ctrl Pts',(6.89904265364457,-0.000247155807051646,
17.9111466962113));
#34193=CARTESIAN_POINT('Ctrl Pts',(6.90338100601535,-0.000247888007577191,
16.9071045316924));
#34194=CARTESIAN_POINT('Ctrl Pts',(6.91268284218105,-0.000249412304973884,
15.1532378243496));
#34195=CARTESIAN_POINT('Ctrl Pts',(6.92154441509678,-0.000249921414807475,
13.6510643636072));
#34196=CARTESIAN_POINT('Ctrl Pts',(6.92709720790588,-0.000248609121187243,
12.3963845191955));
#34197=CARTESIAN_POINT('Ctrl Pts',(6.92936390855178,-0.000247823935322427,
11.8953717842346));
#34198=CARTESIAN_POINT('Ctrl Pts',(6.93399085127207,-0.000245912721741659,
10.8934648715124));
#34199=CARTESIAN_POINT('Ctrl Pts',(6.941993501733,-0.000240364403368093,
9.13946216763256));
#34200=CARTESIAN_POINT('Ctrl Pts',(6.94768031383367,-0.000237808466911361,
7.6340098511879));
#34201=CARTESIAN_POINT('Ctrl Pts',(6.95020094821363,-0.000230555480565149,
6.50020032101587));
#34202=CARTESIAN_POINT('Ctrl Pts',(6.95063684985277,0.00256165266826663,
6.21737010967138));
#34203=CARTESIAN_POINT('Ctrl Pts',(6.95110846856475,0.0169490906205031,
5.68090711620389));
#34204=CARTESIAN_POINT('Ctrl Pts',(6.95109368914234,0.0586645200695752,
4.75843655621655));
#34205=CARTESIAN_POINT('Ctrl Pts',(6.94892115892448,0.16424761237392,3.02377943901819));
#34206=CARTESIAN_POINT('Ctrl Pts',(6.94863380234148,0.154198492166273,1.72337900750542));
#34207=CARTESIAN_POINT('Ctrl Pts',(6.95342525135404,0.0192222826723204,
0.894091270258636));
#34208=CARTESIAN_POINT('Ctrl Pts',(6.95402987640926,0.00398319776505293,
0.808286238370748));
#34209=CARTESIAN_POINT('Ctrl Pts',(6.95541606875165,-0.0338837478143756,
0.623174343735704));
#34210=CARTESIAN_POINT('Ctrl Pts',(6.95824164768107,-0.115240968906443,
0.289354562987173));
#34211=CARTESIAN_POINT('Ctrl Pts',(6.96327163986587,-0.275499286305752,
-0.22816704014749));
#34212=CARTESIAN_POINT('Ctrl Pts',(6.97013009679123,-0.526548360153427,
-0.901612116200544));
#34213=CARTESIAN_POINT('Ctrl Pts',(6.98007564991511,-0.917055970967649,
-1.8645931081793));
#34214=CARTESIAN_POINT('Ctrl Pts',(6.9928688616949,-1.46101102771583,-3.18020351604593));
#34215=CARTESIAN_POINT('Ctrl Pts',(7.00181798897999,-1.8298425877256,-4.37745688997694));
#34216=CARTESIAN_POINT('Ctrl Pts',(7.00534376182817,-1.98247267596028,-5.1844399667158));
#34217=CARTESIAN_POINT('Ctrl Pts',(7.00641136561573,-2.0311953057056,-5.46739474082408));
#34218=CARTESIAN_POINT('Ctrl Pts',(7.00811865174563,-2.11444031578616,-6.04904983182828));
#34219=CARTESIAN_POINT('Ctrl Pts',(7.0097862660601,-2.21489225562981,-7.03866839639272));
#34220=CARTESIAN_POINT('Ctrl Pts',(7.00935572239978,-2.26528901955801,-8.4053192817156));
#34221=CARTESIAN_POINT('Ctrl Pts',(7.00725330740455,-2.25981898315895,-9.6908323666209));
#34222=CARTESIAN_POINT('Ctrl Pts',(7.00589690781737,-2.25878825103757,-10.5497523725835));
#34223=CARTESIAN_POINT('Ctrl Pts',(7.00529225341263,-2.26273389699714,-11.0279436565139));
#34224=CARTESIAN_POINT('Ctrl Pts',(7.00506881584601,-2.26686517166806,-11.2627708989377));
#34225=CARTESIAN_POINT('Ctrl Pts',(7.00493595031213,-2.27100964632756,-11.4384651606442));
#34226=CARTESIAN_POINT('Ctrl Pts',(7.00484836839363,-2.2739661211869,-11.5719308075916));
#34227=CARTESIAN_POINT('Ctrl Pts',(7.00463561274481,-2.27892706711406,-11.8295019931928));
#34228=CARTESIAN_POINT('Ctrl Pts',(7.00419443918313,-2.28585201946081,-12.2829590322349));
#34229=CARTESIAN_POINT('Ctrl Pts',(7.00275050857491,-2.29500391100284,-13.4371000127244));
#34230=CARTESIAN_POINT('Ctrl Pts',(7.00059379503007,-2.28604358714452,-14.7003011504045));
#34231=CARTESIAN_POINT('Ctrl Pts',(6.99890853765602,-2.275516690094,-15.949893638767));
#34232=CARTESIAN_POINT('Ctrl Pts',(6.99830005957763,-2.27123437456408,-16.5725928132207));
#34233=CARTESIAN_POINT('Ctrl Pts',(6.99799068376282,-2.26925031404122,-17.0697162473411));
#34234=CARTESIAN_POINT('Ctrl Pts',(6.99790913550761,-2.26886914319229,-17.3180464092085));
#34235=CARTESIAN_POINT('Ctrl Pts',(6.99787713820796,-2.26886529890116,-17.5035309910445));
#34236=CARTESIAN_POINT('Ctrl Pts',(6.9978639032166,-2.26886101581699,-17.6287753544509));
#34237=CARTESIAN_POINT('Ctrl Pts',(6.99786698761888,-2.26884742862941,-17.8778210848774));
#34238=CARTESIAN_POINT('Ctrl Pts',(6.99791421698644,-2.26882538596002,-18.1275501541622));
#34239=CARTESIAN_POINT('Ctrl Pts',(6.99799850102396,-2.26880018709046,-18.3770960467612));
#34240=CARTESIAN_POINT('Ctrl Pts',(6.9980664450061,-2.26878287323182,-18.5331800437488));
#34241=CARTESIAN_POINT('Ctrl Pts',(6.99812909445171,-2.26876872466669,-18.6580522536357));
#34242=CARTESIAN_POINT('Ctrl Pts',(6.9981972425833,-2.26875429147753,-18.7829523317202));
#34243=CARTESIAN_POINT('Ctrl Pts',(6.99840638378703,-2.26871451756231,-19.1265081948758));
#34244=CARTESIAN_POINT('Ctrl Pts',(6.99886006536309,-2.26864996988756,-19.6891706427572));
#34245=CARTESIAN_POINT('Ctrl Pts',(6.9998822485617,-2.26860388774605,-20.6908816494304));
#34246=CARTESIAN_POINT('Ctrl Pts',(7.00139967900657,-2.26874994953288,-21.945896967966));
#34247=CARTESIAN_POINT('Ctrl Pts',(7.00247309280133,-2.26933126992684,-22.9532794742794));
#34248=CARTESIAN_POINT('Ctrl Pts',(7.0029887564633,-2.26988649050958,-23.5823240349596));
#34249=CARTESIAN_POINT('Ctrl Pts',(7.00319420804157,-2.27013392172621,-23.8312307536037));
#34250=CARTESIAN_POINT('Ctrl Pts',(7.00360398344485,-2.27073812005696,-24.3299781180718));
#34251=CARTESIAN_POINT('Ctrl Pts',(7.00432709632794,-2.27203490661507,-25.2047311211729));
#34252=CARTESIAN_POINT('Ctrl Pts',(7.0053274540055,-2.27441233558042,-26.4591008069716));
#34253=CARTESIAN_POINT('Ctrl Pts',(7.00653584994815,-2.27733928484868,-27.9673691521971));
#34254=CARTESIAN_POINT('Ctrl Pts',(7.00726581201525,-2.27895576084736,-28.9734445269011));
#34255=CARTESIAN_POINT('Ctrl Pts',(7.00768741812352,-2.27959993181941,-29.5369717835662));
#34256=CARTESIAN_POINT('Ctrl Pts',(7.00780073972456,-2.28031670425964,-29.6444420501042));
#34257=CARTESIAN_POINT('Ctrl Pts',(7.00809766792642,-2.28396009662537,-29.8725594838599));
#34258=CARTESIAN_POINT('Ctrl Pts',(7.00877793961808,-2.29569033419828,-30.2739083653757));
#34259=CARTESIAN_POINT('Ctrl Pts',(7.0106802705156,-2.33639039519754,-31.1097812419148));
#34260=CARTESIAN_POINT('Ctrl Pts',(7.01341229050687,-2.4028184112436,-32.1283655105824));
#34261=CARTESIAN_POINT('Ctrl Pts',(7.01520429698212,-2.43879053088795,-33.2125950918116));
#34262=CARTESIAN_POINT('Ctrl Pts',(7.01557655242834,-2.43498485314343,-34.057735891391));
#34263=CARTESIAN_POINT('Ctrl Pts',(7.01439623030718,-2.38406503985142,-34.9349685769412));
#34264=CARTESIAN_POINT('Ctrl Pts',(7.0122274136511,-2.30676299171889,-35.5388148177783));
#34265=CARTESIAN_POINT('Ctrl Pts',(7.00998652770148,-2.22756133212805,-35.9996792004172));
#34266=CARTESIAN_POINT('Ctrl Pts',(7.00803909756502,-2.15962539500237,-36.3341747691404));
#34267=CARTESIAN_POINT('Ctrl Pts',(7.00347015250425,-1.99681681609787,-36.9600450235213));
#34268=CARTESIAN_POINT('Ctrl Pts',(6.9937431091387,-1.65190985969706,-38.002830542361));
#34269=CARTESIAN_POINT('Ctrl Pts',(6.97235829764089,-0.844341899209787,
-39.8703584526267));
#34270=CARTESIAN_POINT('Ctrl Pts',(6.95472791598771,-0.294406849577237,
-41.1965525582491));
#34271=CARTESIAN_POINT('Ctrl Pts',(6.94817137872906,-0.147220927628577,
-41.9802784413025));
#34272=CARTESIAN_POINT('Ctrl Pts',(6.94688299772939,-0.113472013097866,
-42.1811165076733));
#34273=CARTESIAN_POINT('Ctrl Pts',(6.94530724703268,-0.0757730453484783,
-42.4791089023079));
#34274=CARTESIAN_POINT('Ctrl Pts',(6.94407239284371,-0.0468827358548862,
-42.7907295132023));
#34275=CARTESIAN_POINT('Ctrl Pts',(6.9428166037123,-0.0205159884065598,
-43.2166553393947));
#34276=CARTESIAN_POINT('Ctrl Pts',(6.94188917056371,-0.00686498021950975,
-43.7744463599481));
#34277=CARTESIAN_POINT('Ctrl Pts',(6.94143803507245,-0.0123781368730491,
-44.4821346690289));
#34278=CARTESIAN_POINT('Ctrl Pts',(6.9412937478431,-0.0254512748617087,
-45.1039146783508));
#34279=CARTESIAN_POINT('Ctrl Pts',(6.9411669417653,-0.0340160506748517,
-45.6203215595853));
#34280=CARTESIAN_POINT('Ctrl Pts',(6.94100001408149,-0.0375857210191279,
-46.0169793624786));
#34281=CARTESIAN_POINT('Ctrl Pts',(6.94071683255022,-0.0362515468378396,
-46.4230240405838));
#34282=CARTESIAN_POINT('Ctrl Pts',(6.94012770127554,-0.0249707453746474,
-46.9767511611614));
#34283=CARTESIAN_POINT('Ctrl Pts',(6.93935359805737,-0.00240539020963474,
-47.4060205652198));
#34284=CARTESIAN_POINT('Ctrl Pts',(6.93828715749912,0.0346278594182365,
-47.843830926901));
#34285=CARTESIAN_POINT('Ctrl Pts',(6.93753780765541,0.0551177747709163,
-48.0851115474941));
#34286=CARTESIAN_POINT('Ctrl Pts',(6.9359028464867,0.0996744565208953,-48.6000854844173));
#34287=CARTESIAN_POINT('Ctrl Pts',(6.93271869400548,0.180558930246471,-49.4930326775486));
#34288=CARTESIAN_POINT('Ctrl Pts',(6.92746024155021,0.317107244885934,-50.7970279095856));
#34289=CARTESIAN_POINT('Ctrl Pts',(6.92077978587043,0.540751777371533,-52.3864353473554));
#34290=CARTESIAN_POINT('Ctrl Pts',(6.91657371441663,0.749687557481511,-53.4652019487692));
#34291=CARTESIAN_POINT('Ctrl Pts',(6.91418410317824,0.905493783202333,-54.1449974000241));
#34292=CARTESIAN_POINT('Ctrl Pts',(6.9131924896337,0.968874942190495,-54.4132984129917));
#34293=CARTESIAN_POINT('Ctrl Pts',(6.91113670604855,1.10352176270923,-54.9521794482773));
#34294=CARTESIAN_POINT('Ctrl Pts',(6.90738506736453,1.35675544402263,-55.8903497025829));
#34295=CARTESIAN_POINT('Ctrl Pts',(6.89968460661885,1.93045977921322,-57.7543508921274));
#34296=CARTESIAN_POINT('Ctrl Pts',(6.89408348717811,2.5191883577489,-59.3202380645919));
#34297=CARTESIAN_POINT('Ctrl Pts',(6.89195135839285,2.96800306623196,-60.4124402356466));
#34298=CARTESIAN_POINT('Ctrl Pts',(6.89171429919799,3.0263514212361,-60.5526931378033));
#34299=CARTESIAN_POINT('Ctrl Pts',(6.89128991775844,3.1434538716825,-60.8274949565257));
#34300=CARTESIAN_POINT('Ctrl Pts',(6.89068359683782,3.35476527656681,-61.3073433604132));
#34301=CARTESIAN_POINT('Ctrl Pts',(6.88995074751437,3.79557181295857,-62.252317471277));
#34302=CARTESIAN_POINT('Ctrl Pts',(6.88995917391789,4.32983562181616,-63.3044054893138));
#34303=CARTESIAN_POINT('Ctrl Pts',(6.89032196427239,4.86867416564934,-64.3260586974247));
#34304=CARTESIAN_POINT('Ctrl Pts',(6.89056898535275,5.16899624846297,-64.888961970895));
#34305=CARTESIAN_POINT('Ctrl Pts',(6.89071316539118,5.3660945447526,-65.2589185090952));
#34306=CARTESIAN_POINT('Ctrl Pts',(6.89080140524194,5.49653604670366,-65.5041091394283));
#34307=CARTESIAN_POINT('Ctrl Pts',(6.89087358680562,5.62537294269141,-65.7471279716458));
#34308=CARTESIAN_POINT('Ctrl Pts',(6.89091630878653,5.73633849640408,-65.9577307770876));
#34309=CARTESIAN_POINT('Ctrl Pts',(6.89093386030419,5.79919670625669,-66.0774815963281));
#34310=CARTESIAN_POINT('Ctrl Pts',(6.89095285967377,5.89291617543268,-66.2565199375178));
#34311=CARTESIAN_POINT('Ctrl Pts',(6.89095225893861,5.96976082905929,-66.4044339259934));
#34312=CARTESIAN_POINT('Ctrl Pts',(6.89092434227999,6.0952381855696,-66.6478771407354));
#34313=CARTESIAN_POINT('Ctrl Pts',(6.89089907668696,6.23273250392706,-66.9136308044214));
#34314=CARTESIAN_POINT('Ctrl Pts',(6.89086260692432,6.50272160355848,-67.4318102360639));
#34315=CARTESIAN_POINT('Ctrl Pts',(6.89083129094997,6.97613109832236,-68.3319099789933));
#34316=CARTESIAN_POINT('Ctrl Pts',(6.8908723959093,7.91557235664225,-70.09175669196));
#34317=CARTESIAN_POINT('Ctrl Pts',(6.89097650851583,8.71294015020471,-71.5677124890261));
#34318=CARTESIAN_POINT('Ctrl Pts',(6.89098028167908,9.30761950729522,-72.6861721206043));
#34319=CARTESIAN_POINT('Ctrl Pts',(6.89098108645138,9.44144384808963,-72.9378643900992));
#34320=CARTESIAN_POINT('Ctrl Pts',(6.89098226445106,9.70823498149448,-73.4396336082364));
#34321=CARTESIAN_POINT('Ctrl Pts',(6.89098289537523,10.0418864481601,-74.06714673629));
#34322=CARTESIAN_POINT('Ctrl Pts',(6.89098290635027,10.4418692957198,-74.8194059925143));
#34323=CARTESIAN_POINT('Ctrl Pts',(6.89098170197776,11.2416431420624,-76.3235556962517));
#34324=CARTESIAN_POINT('Ctrl Pts',(6.89097877132087,11.9078384197489,-77.5764742851218));
#34325=CARTESIAN_POINT('Ctrl Pts',(6.89097842229583,12.8777491700385,-79.4006126633289));
#34326=CARTESIAN_POINT('Ctrl Pts',(6.89097824243373,13.3143166100287,-80.2216774058681));
#34327=CARTESIAN_POINT('Ctrl Pts',(6.89097824243374,13.7508381974181,-81.0426551079665));
#34328=CARTESIAN_POINT('Ctrl Pts',(9.39709574952983,9.85060074434863E-5,
24.8306346021324));
#34329=CARTESIAN_POINT('Ctrl Pts',(9.39712382476148,9.85139203122644E-5,
24.7817552849976));
#34330=CARTESIAN_POINT('Ctrl Pts',(9.39715326797429,9.85273671940927E-5,
24.7328772539229));
#34331=CARTESIAN_POINT('Ctrl Pts',(9.3975010314311,9.84518919665791E-5,
24.1822613028827));
#34332=CARTESIAN_POINT('Ctrl Pts',(9.39776786851327,9.71467296369741E-5,
23.1780607007944));
#34333=CARTESIAN_POINT('Ctrl Pts',(9.39838786334986,9.73630010883039E-5,
21.1694549086907));
#34334=CARTESIAN_POINT('Ctrl Pts',(9.40070301825327,9.44172580033674E-5,
19.6651399776767));
#34335=CARTESIAN_POINT('Ctrl Pts',(9.40561179634645,9.38961761531635E-5,
18.4140206008922));
#34336=CARTESIAN_POINT('Ctrl Pts',(9.40796582390437,9.41854221663634E-5,
17.9111930870781));
#34337=CARTESIAN_POINT('Ctrl Pts',(9.41387706883776,9.4553365822232E-5,
16.9071572294501));
#34338=CARTESIAN_POINT('Ctrl Pts',(9.42655591655234,9.64268787003325E-5,
15.1532978757182));
#34339=CARTESIAN_POINT('Ctrl Pts',(9.43860374245195,9.06259428207321E-5,
13.651182963467));
#34340=CARTESIAN_POINT('Ctrl Pts',(9.44615688123903,8.73069875527575E-5,
12.396532862185));
#34341=CARTESIAN_POINT('Ctrl Pts',(9.4492444542645,8.69671991073794E-5,
11.895529349549));
#34342=CARTESIAN_POINT('Ctrl Pts',(9.4555398926741,8.41326905260385E-5,
10.8936312703422));
#34343=CARTESIAN_POINT('Ctrl Pts',(9.46643626337659,8.15860255114301E-5,
9.13969528076933));
#34344=CARTESIAN_POINT('Ctrl Pts',(9.47408873909819,5.54737107715689E-5,
7.6342584301987));
#34345=CARTESIAN_POINT('Ctrl Pts',(9.47748675819484,5.05234838685672E-5,
6.50085628110018));
#34346=CARTESIAN_POINT('Ctrl Pts',(9.47774676872149,0.00240407033145399,
6.22271251698896));
#34347=CARTESIAN_POINT('Ctrl Pts',(9.47663442596991,0.0145821795353661,
5.69133854372974));
#34348=CARTESIAN_POINT('Ctrl Pts',(9.4713534496034,0.0500243802638127,4.77508614954621));
#34349=CARTESIAN_POINT('Ctrl Pts',(9.45435632175483,0.140714471638447,3.03710695773964));
#34350=CARTESIAN_POINT('Ctrl Pts',(9.45372533458491,0.133068046649489,1.70611532398695));
#34351=CARTESIAN_POINT('Ctrl Pts',(9.48257740876507,0.0130386069436019,
0.845828636693778));
#34352=CARTESIAN_POINT('Ctrl Pts',(9.48630876393063,-0.000847748246050882,
0.754632089069898));
#34353=CARTESIAN_POINT('Ctrl Pts',(9.49486024241688,-0.0348148210482442,
0.560836824164949));
#34354=CARTESIAN_POINT('Ctrl Pts',(9.51244192469342,-0.107173781897646,
0.213757548909062));
#34355=CARTESIAN_POINT('Ctrl Pts',(9.54365652214872,-0.247172970664451,
-0.316122472084849));
#34356=CARTESIAN_POINT('Ctrl Pts',(9.58741988734466,-0.462822748651149,
-0.997961801831015));
#34357=CARTESIAN_POINT('Ctrl Pts',(9.65058012985507,-0.794350751155283,
-1.96586121105861));
#34358=CARTESIAN_POINT('Ctrl Pts',(9.73329874184328,-1.24970822682561,-3.27944088196305));
#34359=CARTESIAN_POINT('Ctrl Pts',(9.78933424622287,-1.54945484288796,-4.4560485225065));
#34360=CARTESIAN_POINT('Ctrl Pts',(9.81231789269538,-1.67175810583986,-5.23755586899791));
#34361=CARTESIAN_POINT('Ctrl Pts',(9.81975763370998,-1.71146137288016,-5.51594462977292));
#34362=CARTESIAN_POINT('Ctrl Pts',(9.83219696761995,-1.77894269056047,-6.08582494629925));
#34363=CARTESIAN_POINT('Ctrl Pts',(9.84658949085487,-1.86080320713964,-7.05828794318947));
#34364=CARTESIAN_POINT('Ctrl Pts',(9.85146478888084,-1.90278098250614,-8.40712935793198));
#34365=CARTESIAN_POINT('Ctrl Pts',(9.84696453471149,-1.89943818623475,-9.68764951150679));
#34366=CARTESIAN_POINT('Ctrl Pts',(9.84450263709722,-1.89922786536826,-10.549318186832));
#34367=CARTESIAN_POINT('Ctrl Pts',(9.84396945193637,-1.9028474624947,-11.030981263349));
#34368=CARTESIAN_POINT('Ctrl Pts',(9.84411071223977,-1.90644026244215,-11.2681837624333));
#34369=CARTESIAN_POINT('Ctrl Pts',(9.84441122490759,-1.91000441977411,-11.4458336189714));
#34370=CARTESIAN_POINT('Ctrl Pts',(9.84463107530365,-1.91249319772449,-11.5780920335527));
#34371=CARTESIAN_POINT('Ctrl Pts',(9.84490733911212,-1.91672407923323,-11.8347330068637));
#34372=CARTESIAN_POINT('Ctrl Pts',(9.84507523283692,-1.92268918027574,-12.2860098066065));
#34373=CARTESIAN_POINT('Ctrl Pts',(9.84400431113743,-1.93100390233827,-13.4360093674867));
#34374=CARTESIAN_POINT('Ctrl Pts',(9.83969839554375,-1.92457337722949,-14.6968539115163));
#34375=CARTESIAN_POINT('Ctrl Pts',(9.8360140155241,-1.91654013277157,-15.9468962665494));
#34376=CARTESIAN_POINT('Ctrl Pts',(9.83462020824012,-1.9132362729513,-16.5704247665775));
#34377=CARTESIAN_POINT('Ctrl Pts',(9.83396171319717,-1.91170774015949,-17.0686125869906));
#34378=CARTESIAN_POINT('Ctrl Pts',(9.83381192550018,-1.91142187832722,-17.317602341319));
#34379=CARTESIAN_POINT('Ctrl Pts',(9.83377912208015,-1.91142942347021,-17.5036135228565));
#34380=CARTESIAN_POINT('Ctrl Pts',(9.8337683516608,-1.91143332817741,-17.6286923495811));
#34381=CARTESIAN_POINT('Ctrl Pts',(9.83378925148769,-1.91143666779512,-17.877722086886));
#34382=CARTESIAN_POINT('Ctrl Pts',(9.8338690691644,-1.91143235734373,-18.1273414666358));
#34383=CARTESIAN_POINT('Ctrl Pts',(9.8340050059961,-1.91142124231706,-18.3768574556843));
#34384=CARTESIAN_POINT('Ctrl Pts',(9.83411137207806,-1.91141112487478,-18.5329174549527));
#34385=CARTESIAN_POINT('Ctrl Pts',(9.8342089902123,-1.91140120730261,-18.6577804903151));
#34386=CARTESIAN_POINT('Ctrl Pts',(9.83431464188427,-1.91138991853604,-18.7826732285614));
#34387=CARTESIAN_POINT('Ctrl Pts',(9.83463598146339,-1.91135465577494,-19.1262231260297));
#34388=CARTESIAN_POINT('Ctrl Pts',(9.83532550903627,-1.91126593733576,-19.6889483271403));
#34389=CARTESIAN_POINT('Ctrl Pts',(9.83689315628327,-1.91103332471521,-20.6909798403928));
#34390=CARTESIAN_POINT('Ctrl Pts',(9.83928212534762,-1.91055958819307,-21.9467826019539));
#34391=CARTESIAN_POINT('Ctrl Pts',(9.84116764454534,-1.91001418058634,-22.955204818448));
#34392=CARTESIAN_POINT('Ctrl Pts',(9.8421933054474,-1.90959220114503,-23.5850311524326));
#34393=CARTESIAN_POINT('Ctrl Pts',(9.84261393218004,-1.9094071339158,-23.8344089360016));
#34394=CARTESIAN_POINT('Ctrl Pts',(9.84350382388819,-1.90898251807467,-24.3338811135346));
#34395=CARTESIAN_POINT('Ctrl Pts',(9.8451725829466,-1.90810399481636,-25.2096813987555));
#34396=CARTESIAN_POINT('Ctrl Pts',(9.84775195150598,-1.90661928666474,-26.4646920808429));
#34397=CARTESIAN_POINT('Ctrl Pts',(9.85082969349042,-1.90472362092078,-27.9725650153342));
#34398=CARTESIAN_POINT('Ctrl Pts',(9.85260536859806,-1.90372500288613,-28.9773843873838));
#34399=CARTESIAN_POINT('Ctrl Pts',(9.85347022616558,-1.90327567303515,-29.5402360386186));
#34400=CARTESIAN_POINT('Ctrl Pts',(9.85376439664258,-1.90368429194054,-29.6505702179668));
#34401=CARTESIAN_POINT('Ctrl Pts',(9.85472331033051,-1.90634343794854,-29.8822173878728));
#34402=CARTESIAN_POINT('Ctrl Pts',(9.85729641826308,-1.91547380118253,-30.2894705601969));
#34403=CARTESIAN_POINT('Ctrl Pts',(9.86529427154334,-1.94801673142762,-31.1318876565905));
#34404=CARTESIAN_POINT('Ctrl Pts',(9.87755736457791,-2.00113995963799,-32.1479794298922));
#34405=CARTESIAN_POINT('Ctrl Pts',(9.88458332930815,-2.02914796194555,-33.2187160361868));
#34406=CARTESIAN_POINT('Ctrl Pts',(9.8846505448229,-2.02540533054684,-34.0482843286969));
#34407=CARTESIAN_POINT('Ctrl Pts',(9.87678603945088,-1.98416420939679,-34.9047570982295));
#34408=CARTESIAN_POINT('Ctrl Pts',(9.86434714101142,-1.92228483706194,-35.4923457190805));
#34409=CARTESIAN_POINT('Ctrl Pts',(9.85161255446927,-1.85892275316106,-35.9406210300452));
#34410=CARTESIAN_POINT('Ctrl Pts',(9.84072169333682,-1.80507065302535,-36.2632421397352));
#34411=CARTESIAN_POINT('Ctrl Pts',(9.81484982650837,-1.67442270398369,-36.8733766663579));
#34412=CARTESIAN_POINT('Ctrl Pts',(9.7600581790089,-1.39404280255062,-37.8990108669212));
#34413=CARTESIAN_POINT('Ctrl Pts',(9.63659735888789,-0.722613497645318,
-39.7639201836366));
#34414=CARTESIAN_POINT('Ctrl Pts',(9.53816382801678,-0.248912727847852,
-41.1021642167714));
#34415=CARTESIAN_POINT('Ctrl Pts',(9.50217064222597,-0.116651839270521,
-41.9305954513151));
#34416=CARTESIAN_POINT('Ctrl Pts',(9.49487857746734,-0.0874975350060252,
-42.1362059880072));
#34417=CARTESIAN_POINT('Ctrl Pts',(9.48594038761699,-0.0549897319655466,
-42.4433074274479));
#34418=CARTESIAN_POINT('Ctrl Pts',(9.47883283572487,-0.0307036412911002,
-42.7625139069713));
#34419=CARTESIAN_POINT('Ctrl Pts',(9.4715738737315,-0.00920915185482917,
-43.1979630713915));
#34420=CARTESIAN_POINT('Ctrl Pts',(9.46617075949442,0.00030125175059658,
-43.7652339495534));
#34421=CARTESIAN_POINT('Ctrl Pts',(9.46386173516898,-0.00733827689215994,
-44.4805653014695));
#34422=CARTESIAN_POINT('Ctrl Pts',(9.46394450808348,-0.0204975884789352,
-45.1054543111399));
#34423=CARTESIAN_POINT('Ctrl Pts',(9.46435067476216,-0.0287494965312834,
-45.6224691455761));
#34424=CARTESIAN_POINT('Ctrl Pts',(9.46459707476204,-0.0320676494958033,
-46.0186216064772));
#34425=CARTESIAN_POINT('Ctrl Pts',(9.46456526055404,-0.0306772902459179,
-46.4231979182499));
#34426=CARTESIAN_POINT('Ctrl Pts',(9.46386003704854,-0.0199159967342241,
-46.9736983984273));
#34427=CARTESIAN_POINT('Ctrl Pts',(9.46224277548488,0.00123271037981269,
-47.3990882005854));
#34428=CARTESIAN_POINT('Ctrl Pts',(9.45947300888553,0.0355427847841118,
-47.8322468349079));
#34429=CARTESIAN_POINT('Ctrl Pts',(9.45761404741026,0.0547904732236308,
-48.0743676862649));
#34430=CARTESIAN_POINT('Ctrl Pts',(9.45387130200266,0.0965200563031265,
-48.5889071297665));
#34431=CARTESIAN_POINT('Ctrl Pts',(9.44729751772116,0.172672927165151,-49.4824938544509));
#34432=CARTESIAN_POINT('Ctrl Pts',(9.43800296747507,0.302828721577757,-50.7874940600758));
#34433=CARTESIAN_POINT('Ctrl Pts',(9.42760104368089,0.520617671817749,-52.3796782186102));
#34434=CARTESIAN_POINT('Ctrl Pts',(9.42148449284729,0.727489544375616,-53.4608837581059));
#34435=CARTESIAN_POINT('Ctrl Pts',(9.41801653726967,0.882776450636743,-54.1424217070253));
#34436=CARTESIAN_POINT('Ctrl Pts',(9.41660018054459,0.946065112992808,-54.4115221367208));
#34437=CARTESIAN_POINT('Ctrl Pts',(9.41377399906611,1.0807879654595,-54.9517633279573));
#34438=CARTESIAN_POINT('Ctrl Pts',(9.40885840442797,1.33482818349171,-55.891951541443));
#34439=CARTESIAN_POINT('Ctrl Pts',(9.39951864609365,1.91208396809229,-57.7584288631972));
#34440=CARTESIAN_POINT('Ctrl Pts',(9.39355010701788,2.50502947097712,-59.3241279180903));
#34441=CARTESIAN_POINT('Ctrl Pts',(9.39156343535068,2.95537803265398,-60.415272793405));
#34442=CARTESIAN_POINT('Ctrl Pts',(9.39136735927576,3.0140632876918,-60.5557152480889));
#34443=CARTESIAN_POINT('Ctrl Pts',(9.3910492684304,3.1317814670137,-60.8306909163205));
#34444=CARTESIAN_POINT('Ctrl Pts',(9.39071295906558,3.34426521613766,-61.3108788866971));
#34445=CARTESIAN_POINT('Ctrl Pts',(9.39078821554258,3.7875443137992,-62.2562486506828));
#34446=CARTESIAN_POINT('Ctrl Pts',(9.39213953428988,4.3247693680003,-63.3084130369635));
#34447=CARTESIAN_POINT('Ctrl Pts',(9.39388778754442,4.86620950375434,-64.3297613140723));
#34448=CARTESIAN_POINT('Ctrl Pts',(9.39486435610099,5.16777800376065,-64.8923576658369));
#34449=CARTESIAN_POINT('Ctrl Pts',(9.39544586818117,5.36557938810239,-65.2620471351256));
#34450=CARTESIAN_POINT('Ctrl Pts',(9.39581056127253,5.49645330380412,-65.5070425816499));
#34451=CARTESIAN_POINT('Ctrl Pts',(9.39613415269145,5.62566425274362,-65.7498409109864));
#34452=CARTESIAN_POINT('Ctrl Pts',(9.39636931187523,5.73689993095036,-65.9602257093019));
#34453=CARTESIAN_POINT('Ctrl Pts',(9.39648826638796,5.79989522799455,-66.0798446515712));
#34454=CARTESIAN_POINT('Ctrl Pts',(9.39665040100374,5.8938026825324,-66.2586777183794));
#34455=CARTESIAN_POINT('Ctrl Pts',(9.39674981576714,5.97076589573635,-66.4064051929983));
#34456=CARTESIAN_POINT('Ctrl Pts',(9.39685726595448,6.09638583511326,-66.6495173501779));
#34457=CARTESIAN_POINT('Ctrl Pts',(9.39695467963757,6.2340448976683,-66.9150063715849));
#34458=CARTESIAN_POINT('Ctrl Pts',(9.39710259783481,6.50421003572679,-67.4326708346839));
#34459=CARTESIAN_POINT('Ctrl Pts',(9.39725124719125,6.97766078616841,-68.3320276092932));
#34460=CARTESIAN_POINT('Ctrl Pts',(9.39721704222952,7.91638427079446,-70.0909389565235));
#34461=CARTESIAN_POINT('Ctrl Pts',(9.39695920064004,8.71295332911861,-71.5671178811821));
#34462=CARTESIAN_POINT('Ctrl Pts',(9.39697619655444,9.30799708286968,-72.686226807902));
#34463=CARTESIAN_POINT('Ctrl Pts',(9.39697930001536,9.44180033126638,-72.9378719364681));
#34464=CARTESIAN_POINT('Ctrl Pts',(9.39698400304045,9.70860585557645,-73.4396573013827));
#34465=CARTESIAN_POINT('Ctrl Pts',(9.39698710758693,10.0422490477591,-74.067148102403));
#34466=CARTESIAN_POINT('Ctrl Pts',(9.39698746336443,10.4422314152469,-74.8194059221752));
#34467=CARTESIAN_POINT('Ctrl Pts',(9.39698343039283,11.2419928422341,-76.3235423766373));
#34468=CARTESIAN_POINT('Ctrl Pts',(9.39697452470082,11.9081784818574,-77.5764661824382));
#34469=CARTESIAN_POINT('Ctrl Pts',(9.39697457998603,12.8780952426034,-79.4006170546344));
#34470=CARTESIAN_POINT('Ctrl Pts',(9.39697460873377,13.3146600052307,-80.2216773745254));
#34471=CARTESIAN_POINT('Ctrl Pts',(9.39697460873379,13.7511815926202,-81.0426550766237));
#34472=CARTESIAN_POINT('Ctrl Pts',(11.5895003465238,0.000421249146080626,
24.8306341860236));
#34473=CARTESIAN_POINT('Ctrl Pts',(11.5895349558891,0.000421265971284107,
24.7817548555947));
#34474=CARTESIAN_POINT('Ctrl Pts',(11.5895712425403,0.000421288380151196,
24.732876758355));
#34475=CARTESIAN_POINT('Ctrl Pts',(11.590000249277,0.000421335496354015,
24.1822624226437));
#34476=CARTESIAN_POINT('Ctrl Pts',(11.5903315807401,0.000420438478241857,
23.1780764140684));
#34477=CARTESIAN_POINT('Ctrl Pts',(11.5910956631355,0.000421514181210609,
21.1694719372929));
#34478=CARTESIAN_POINT('Ctrl Pts',(11.59395600421,0.000419556677115865,
19.6651937504487));
#34479=CARTESIAN_POINT('Ctrl Pts',(11.6000108331372,0.000419595016915984,
18.4140903993403));
#34480=CARTESIAN_POINT('Ctrl Pts',(11.6029134738436,0.000420193598292942,
17.911264557871));
#34481=CARTESIAN_POINT('Ctrl Pts',(11.610202940336,0.000421505558988271,
16.9072385975303));
#34482=CARTESIAN_POINT('Ctrl Pts',(11.6258359918673,0.000425254069881499,
15.1533902639501));
#34483=CARTESIAN_POINT('Ctrl Pts',(11.6407048266074,0.000420578030577308,
13.6513622787079));
#34484=CARTESIAN_POINT('Ctrl Pts',(11.65002661683,0.000415634117589493,
12.3967550004797));
#34485=CARTESIAN_POINT('Ctrl Pts',(11.6538355348768,0.000414271683788634,
11.8957647331824));
#34486=CARTESIAN_POINT('Ctrl Pts',(11.6616052574914,0.00040872892343895,
10.89387820218));
#34487=CARTESIAN_POINT('Ctrl Pts',(11.6750512732423,0.000399384798179506,
9.14004403088222));
#34488=CARTESIAN_POINT('Ctrl Pts',(11.6845336306305,0.000369136692087825,
7.63462505162104));
#34489=CARTESIAN_POINT('Ctrl Pts',(11.6887426152279,0.000360629362696536,
6.50185638510926));
#34490=CARTESIAN_POINT('Ctrl Pts',(11.6889829938694,0.00204940874441417,
6.23104218068182));
#34491=CARTESIAN_POINT('Ctrl Pts',(11.6871933797293,0.0108499136959918,
5.70761822167393));
#34492=CARTESIAN_POINT('Ctrl Pts',(11.6794103159137,0.0366529171734025,
4.80116829281341));
#34493=CARTESIAN_POINT('Ctrl Pts',(11.6551428675138,0.103926667440031,3.05766827252427));
#34494=CARTESIAN_POINT('Ctrl Pts',(11.6544067577611,0.0997159897208348,
1.67957314750907));
#34495=CARTESIAN_POINT('Ctrl Pts',(11.6956884426168,0.00524533581804662,
0.76907608223799));
#34496=CARTESIAN_POINT('Ctrl Pts',(11.7010331324381,-0.00612686295736921,
0.669109293389778));
#34497=CARTESIAN_POINT('Ctrl Pts',(11.7133419918826,-0.033295340217515,
0.460962228982755));
#34498=CARTESIAN_POINT('Ctrl Pts',(11.7388026574533,-0.0904451889914446,
0.0914601360013011));
#34499=CARTESIAN_POINT('Ctrl Pts',(11.7846067217235,-0.197828873089581,
-0.460490590649874));
#34500=CARTESIAN_POINT('Ctrl Pts',(11.8492755833482,-0.35785312251849,-1.15772429267139));
#34501=CARTESIAN_POINT('Ctrl Pts',(11.9422531726328,-0.597449389264225,
-2.13404256300419));
#34502=CARTESIAN_POINT('Ctrl Pts',(12.0600747368333,-0.915142274293143,
-3.43977101294881));
#34503=CARTESIAN_POINT('Ctrl Pts',(12.1317881784433,-1.11347752640962,-4.57760409191073));
#34504=CARTESIAN_POINT('Ctrl Pts',(12.1598433026514,-1.19302471328253,-5.31855920096231));
#34505=CARTESIAN_POINT('Ctrl Pts',(12.169366898184,-1.21964202475537,-5.58971844115356));
#34506=CARTESIAN_POINT('Ctrl Pts',(12.1849416948029,-1.26453163793054,-6.14133750050855));
#34507=CARTESIAN_POINT('Ctrl Pts',(12.2030002467654,-1.31956548681415,-7.0879167372753));
#34508=CARTESIAN_POINT('Ctrl Pts',(12.2090841204405,-1.34885175444332,-8.41047338620064));
#34509=CARTESIAN_POINT('Ctrl Pts',(12.2033198192615,-1.34791613453023,-9.68356162650418));
#34510=CARTESIAN_POINT('Ctrl Pts',(12.2001610304695,-1.3485209109719,-10.5492284134047));
#34511=CARTESIAN_POINT('Ctrl Pts',(12.199565240339,-1.35141229690972,-11.0359749983344));
#34512=CARTESIAN_POINT('Ctrl Pts',(12.1998293163945,-1.35407559411239,-11.2766596539298));
#34513=CARTESIAN_POINT('Ctrl Pts',(12.2002966711747,-1.35667249736963,-11.4571774087692));
#34514=CARTESIAN_POINT('Ctrl Pts',(12.200602535717,-1.35843107697228,-11.5876611958586));
#34515=CARTESIAN_POINT('Ctrl Pts',(12.2010332957154,-1.36147606105468,-11.8429321527371));
#34516=CARTESIAN_POINT('Ctrl Pts',(12.2014008783385,-1.36582617024926,-12.2909985688009));
#34517=CARTESIAN_POINT('Ctrl Pts',(12.2005528795049,-1.37230550341324,-13.4348799242311));
#34518=CARTESIAN_POINT('Ctrl Pts',(12.1958185922034,-1.36885998545949,-14.692157276302));
#34519=CARTESIAN_POINT('Ctrl Pts',(12.1916526864696,-1.36400843945851,-15.9427077708804));
#34520=CARTESIAN_POINT('Ctrl Pts',(12.1900893000376,-1.36197258417533,-16.5673646493878));
#34521=CARTESIAN_POINT('Ctrl Pts',(12.1893597741114,-1.36103431008563,-17.0670389593229));
#34522=CARTESIAN_POINT('Ctrl Pts',(12.1892071133706,-1.36086730651945,-17.316956074871));
#34523=CARTESIAN_POINT('Ctrl Pts',(12.1891850913752,-1.36088367403509,-17.5037103865457));
#34524=CARTESIAN_POINT('Ctrl Pts',(12.1891860726778,-1.36089370079563,-17.6285722135397));
#34525=CARTESIAN_POINT('Ctrl Pts',(12.1892466645591,-1.36091024622022,-17.8775969971028));
#34526=CARTESIAN_POINT('Ctrl Pts',(12.1893903663723,-1.3609200070653,-18.1270748121356));
#34527=CARTESIAN_POINT('Ctrl Pts',(12.1896069748992,-1.3609210606696,-18.3765523507506));
#34528=CARTESIAN_POINT('Ctrl Pts',(12.1897706375991,-1.36091754738905,-18.5325779604253));
#34529=CARTESIAN_POINT('Ctrl Pts',(12.1899173027073,-1.36091196273073,-18.6574255762084));
#34530=CARTESIAN_POINT('Ctrl Pts',(12.1900741058559,-1.36090430584617,-18.7823042848857));
#34531=CARTESIAN_POINT('Ctrl Pts',(12.1905441675585,-1.36087613957535,-19.1258297086731));
#34532=CARTESIAN_POINT('Ctrl Pts',(12.1915123396548,-1.36077757925637,-19.6885889384576));
#34533=CARTESIAN_POINT('Ctrl Pts',(12.1935748924666,-1.36042389655417,-20.690890665205));
#34534=CARTESIAN_POINT('Ctrl Pts',(12.1964140789255,-1.35950880721579,-21.9474356554848));
#34535=CARTESIAN_POINT('Ctrl Pts',(12.1980823823026,-1.35811531701347,-22.9568678500849));
#34536=CARTESIAN_POINT('Ctrl Pts',(12.1986778233842,-1.35694704435592,-23.5874635626913));
#34537=CARTESIAN_POINT('Ctrl Pts',(12.1988951249704,-1.35642925560143,-23.8372801898254));
#34538=CARTESIAN_POINT('Ctrl Pts',(12.1992557838325,-1.35521683352075,-24.3374364321954));
#34539=CARTESIAN_POINT('Ctrl Pts',(12.1997222650968,-1.35268582991751,-25.2142287410768));
#34540=CARTESIAN_POINT('Ctrl Pts',(12.1999918287177,-1.3483298012673,-26.469843102847));
#34541=CARTESIAN_POINT('Ctrl Pts',(12.2001331733731,-1.3430080053085,-27.9774101168199));
#34542=CARTESIAN_POINT('Ctrl Pts',(12.2002979616086,-1.34021231189827,-28.9810214667866));
#34543=CARTESIAN_POINT('Ctrl Pts',(12.2005179979553,-1.33902294947022,-29.5433690165917));
#34544=CARTESIAN_POINT('Ctrl Pts',(12.2007155568601,-1.33913234315464,-29.6579343007927));
#34545=CARTESIAN_POINT('Ctrl Pts',(12.2016183131347,-1.34064013032727,-29.894857818671));
#34546=CARTESIAN_POINT('Ctrl Pts',(12.2044109963861,-1.34640703943498,-30.3109049420008));
#34547=CARTESIAN_POINT('Ctrl Pts',(12.2138037264528,-1.36780107507898,-31.1631350360708));
#34548=CARTESIAN_POINT('Ctrl Pts',(12.2282678471616,-1.40267735858772,-32.1756131064741));
#34549=CARTESIAN_POINT('Ctrl Pts',(12.2359281634714,-1.42035992478456,-33.2268804247612));
#34550=CARTESIAN_POINT('Ctrl Pts',(12.235382686702,-1.41727505453408,-34.0340411863746));
#34551=CARTESIAN_POINT('Ctrl Pts',(12.2254752043518,-1.38978026876474,-34.8603776714585));
#34552=CARTESIAN_POINT('Ctrl Pts',(12.2104691370127,-1.34925733430161,-35.4236498731343));
#34553=CARTESIAN_POINT('Ctrl Pts',(12.1951752297892,-1.30790111826445,-35.8524630983525));
#34554=CARTESIAN_POINT('Ctrl Pts',(12.1825211824852,-1.27333639386323,-36.1563718706145));
#34555=CARTESIAN_POINT('Ctrl Pts',(12.1512525619581,-1.1880725012926,-36.7400470871197));
#34556=CARTESIAN_POINT('Ctrl Pts',(12.0823704341283,-1.00177550927921,-37.7333136575194));
#34557=CARTESIAN_POINT('Ctrl Pts',(11.912067166079,-0.539417026971565,-39.5844202785541));
#34558=CARTESIAN_POINT('Ctrl Pts',(11.7643012553191,-0.183649155381337,
-40.9505201179462));
#34559=CARTESIAN_POINT('Ctrl Pts',(11.7132560199656,-0.0769147300689789,
-41.8530590205573));
#34560=CARTESIAN_POINT('Ctrl Pts',(11.7030577355911,-0.0549797254856127,
-42.0664949301454));
#34561=CARTESIAN_POINT('Ctrl Pts',(11.6906565557908,-0.0307525519755015,
-42.3883700308207));
#34562=CARTESIAN_POINT('Ctrl Pts',(11.6809257359326,-0.0136401693481867,
-42.7197339938335));
#34563=CARTESIAN_POINT('Ctrl Pts',(11.6711343612843,0.000378588213563514,
-43.170388084499));
#34564=CARTESIAN_POINT('Ctrl Pts',(11.6641582404438,0.003870671157017,-43.7527445567746));
#34565=CARTESIAN_POINT('Ctrl Pts',(11.6618085968409,-0.00627095441501176,
-44.4803624481653));
#34566=CARTESIAN_POINT('Ctrl Pts',(11.6628519722898,-0.0187202388324247,
-45.1104330869402));
#34567=CARTESIAN_POINT('Ctrl Pts',(11.6643176229784,-0.0256880940942903,
-45.6286559926594));
#34568=CARTESIAN_POINT('Ctrl Pts',(11.665417654692,-0.0279705948420053,
-46.0242224672143));
#34569=CARTESIAN_POINT('Ctrl Pts',(11.6662197469886,-0.0257940182038288,
-46.4267149613217));
#34570=CARTESIAN_POINT('Ctrl Pts',(11.6664945399492,-0.0148137185444308,
-46.9724562252043));
#34571=CARTESIAN_POINT('Ctrl Pts',(11.6653371442479,0.00499710263825592,
-47.3920033430256));
#34572=CARTESIAN_POINT('Ctrl Pts',(11.6626865579812,0.0360646717714845,
-47.8180888050839));
#34573=CARTESIAN_POINT('Ctrl Pts',(11.6609970542061,0.0540060645333786,
-48.0621584055523));
#34574=CARTESIAN_POINT('Ctrl Pts',(11.6579125669985,0.0928044846859556,
-48.5768198708537));
#34575=CARTESIAN_POINT('Ctrl Pts',(11.6531862216885,0.16443908310244,-49.4725388962503));
#34576=CARTESIAN_POINT('Ctrl Pts',(11.6477776932751,0.289023855935045,-50.7794141693277));
#34577=CARTESIAN_POINT('Ctrl Pts',(11.6417051597372,0.501721528728834,-52.3744925130066));
#34578=CARTESIAN_POINT('Ctrl Pts',(11.6368682309341,0.706544305032596,-53.4574473486582));
#34579=CARTESIAN_POINT('Ctrl Pts',(11.6332778401015,0.86106650825881,-54.1400827334346));
#34580=CARTESIAN_POINT('Ctrl Pts',(11.631747464244,0.924228189408537,-54.4100019188139));
#34581=CARTESIAN_POINT('Ctrl Pts',(11.6284383863139,1.05893209788025,-54.9514885117027));
#34582=CARTESIAN_POINT('Ctrl Pts',(11.6220936677995,1.31365760989207,-55.893593887579));
#34583=CARTESIAN_POINT('Ctrl Pts',(11.6081597107898,1.89428780354141,-57.7622977018779));
#34584=CARTESIAN_POINT('Ctrl Pts',(11.5972576739243,2.49130687345031,-59.3278233751766));
#34585=CARTESIAN_POINT('Ctrl Pts',(11.5932461563346,2.94318498687134,-60.4180302768753));
#34586=CARTESIAN_POINT('Ctrl Pts',(11.5927990424572,3.002203182863,-60.5586409281497));
#34587=CARTESIAN_POINT('Ctrl Pts',(11.5919848816902,3.12053101962373,-60.833766518273));
#34588=CARTESIAN_POINT('Ctrl Pts',(11.5907857315375,3.33417256712251,-61.3142431871049));
#34589=CARTESIAN_POINT('Ctrl Pts',(11.5891815844952,3.77988417078737,-62.2599187917617));
#34590=CARTESIAN_POINT('Ctrl Pts',(11.5887569117294,4.31997925913707,-63.3121003364946));
#34591=CARTESIAN_POINT('Ctrl Pts',(11.5889649652932,4.86391151043664,-64.3331503596558));
#34592=CARTESIAN_POINT('Ctrl Pts',(11.5891777174056,5.16666562729302,-64.8954629679139));
#34593=CARTESIAN_POINT('Ctrl Pts',(11.5892979571789,5.36513161334473,-65.264909254195));
#34594=CARTESIAN_POINT('Ctrl Pts',(11.5893689104412,5.49641360042041,-65.5097267921224));
#34595=CARTESIAN_POINT('Ctrl Pts',(11.589417857095,5.62597475449768,-65.7523254738009));
#34596=CARTESIAN_POINT('Ctrl Pts',(11.5894326263675,5.73746232256607,-65.9625116689282));
#34597=CARTESIAN_POINT('Ctrl Pts',(11.5894312284362,5.80058491029846,-66.082010275755));
#34598=CARTESIAN_POINT('Ctrl Pts',(11.5894186243491,5.89466641583682,-66.2606557110124));
#34599=CARTESIAN_POINT('Ctrl Pts',(11.5893837333011,5.97173763063546,-66.4082123733179));
#34600=CARTESIAN_POINT('Ctrl Pts',(11.5892865435401,6.09748576135826,-66.6510196056842));
#34601=CARTESIAN_POINT('Ctrl Pts',(11.5891983703341,6.23529702121285,-66.9162681907086));
#34602=CARTESIAN_POINT('Ctrl Pts',(11.5890696535673,6.50562214135505,-67.4334602383677));
#34603=CARTESIAN_POINT('Ctrl Pts',(11.588952931312,6.97910540105887,-68.3321328965063));
#34604=CARTESIAN_POINT('Ctrl Pts',(11.5890635559689,7.91715809051001,-70.0901682506227));
#34605=CARTESIAN_POINT('Ctrl Pts',(11.5893843546621,8.71297649813509,-71.5665593860804));
#34606=CARTESIAN_POINT('Ctrl Pts',(11.5893882636949,9.30835753260348,-72.6862749620062));
#34607=CARTESIAN_POINT('Ctrl Pts',(11.5893894963938,9.44214102812561,-72.9378761916324));
#34608=CARTESIAN_POINT('Ctrl Pts',(11.5893911749115,9.70895971908889,-73.4396767585204));
#34609=CARTESIAN_POINT('Ctrl Pts',(11.5893916578803,10.0425945061019,-74.0671471010587));
#34610=CARTESIAN_POINT('Ctrl Pts',(11.5893914474645,10.4425761394456,-74.8194037472044));
#34611=CARTESIAN_POINT('Ctrl Pts',(11.5893891715325,11.2423255426347,-76.3235281075312));
#34612=CARTESIAN_POINT('Ctrl Pts',(11.5893829173179,11.9085001528643,-77.5764577736852));
#34613=CARTESIAN_POINT('Ctrl Pts',(11.5893813335251,12.8784211622576,-79.4006208947267));
#34614=CARTESIAN_POINT('Ctrl Pts',(11.5893805197922,13.3149827504299,-80.2216774359031));
#34615=CARTESIAN_POINT('Ctrl Pts',(11.5893805197922,13.7515043378194,-81.0426551380014));
#34616=CARTESIAN_POINT('Ctrl Pts',(14.0944631116312,0.000239315415103097,
24.8306344290317));
#34617=CARTESIAN_POINT('Ctrl Pts',(14.0945051703635,0.000239310373125806,
24.7817551065899));
#34618=CARTESIAN_POINT('Ctrl Pts',(14.094549283557,0.000239308494718214,
24.7328769301283));
#34619=CARTESIAN_POINT('Ctrl Pts',(14.0950700886175,0.000239130724081029,
24.1822656284498));
#34620=CARTESIAN_POINT('Ctrl Pts',(14.0954676202415,0.000238294797979617,
23.1781042478625));
#34621=CARTESIAN_POINT('Ctrl Pts',(14.0963939340577,0.000238593416326289,
21.169502605));
#34622=CARTESIAN_POINT('Ctrl Pts',(14.0998586839277,0.000235783298849487,
19.6652856273898));
#34623=CARTESIAN_POINT('Ctrl Pts',(14.1072148356599,0.000232983959125036,
18.4142089765319));
#34624=CARTESIAN_POINT('Ctrl Pts',(14.1107427068927,0.00023202792923821,
17.9113877798041));
#34625=CARTESIAN_POINT('Ctrl Pts',(14.1196006764428,0.000229423541213125,
16.907379540741));
#34626=CARTESIAN_POINT('Ctrl Pts',(14.1386011789869,0.000224523189695424,
15.1535492780035));
#34627=CARTESIAN_POINT('Ctrl Pts',(14.1566536268648,0.000214244067486069,
13.6516594845658));
#34628=CARTESIAN_POINT('Ctrl Pts',(14.1679809427275,0.000207077916971663,
12.3971158810473));
#34629=CARTESIAN_POINT('Ctrl Pts',(14.1726133672633,0.000204695620792798,
11.8961428873256));
#34630=CARTESIAN_POINT('Ctrl Pts',(14.1820601727929,0.000198134753947263,
10.8942756519075));
#34631=CARTESIAN_POINT('Ctrl Pts',(14.1984197580504,0.000187296246933722,
9.14058768641498));
#34632=CARTESIAN_POINT('Ctrl Pts',(14.2098938545934,0.000163375509298961,
7.63525678927255));
#34633=CARTESIAN_POINT('Ctrl Pts',(14.2149923557477,0.000155107245014959,
6.50340589673276));
#34634=CARTESIAN_POINT('Ctrl Pts',(14.215505664609,0.000961838336879548,
6.24294842492752));
#34635=CARTESIAN_POINT('Ctrl Pts',(14.214494741344,0.00520287161040355,
5.73074485996725));
#34636=CARTESIAN_POINT('Ctrl Pts',(14.208472871761,0.0177970441974879,4.83834267556141));
#34637=CARTESIAN_POINT('Ctrl Pts',(14.1882723930367,0.0514117428276515,
3.08651160205499));
#34638=CARTESIAN_POINT('Ctrl Pts',(14.1870202056287,0.0504889425535852,
1.64352233320098));
#34639=CARTESIAN_POINT('Ctrl Pts',(14.2222965127537,-0.00105218817305978,
0.65884157414066));
#34640=CARTESIAN_POINT('Ctrl Pts',(14.2268798643112,-0.00758097557180187,
0.545811031676352));
#34641=CARTESIAN_POINT('Ctrl Pts',(14.2374646281445,-0.0227769719229255,
0.315844136561766));
#34642=CARTESIAN_POINT('Ctrl Pts',(14.2594646628206,-0.0543499942763772,
-0.0887617804289952));
#34643=CARTESIAN_POINT('Ctrl Pts',(14.29940595502,-0.111800663915594,-0.677724198690524));
#34644=CARTESIAN_POINT('Ctrl Pts',(14.3563852189701,-0.193695842118945,
-1.40127978883877));
#34645=CARTESIAN_POINT('Ctrl Pts',(14.438257220335,-0.311431996465603,-2.38958521327673));
#34646=CARTESIAN_POINT('Ctrl Pts',(14.5400067851163,-0.458336815684018,
-3.66964344286333));
#34647=CARTESIAN_POINT('Ctrl Pts',(14.5973641928648,-0.543987179230505,
-4.7410559036543));
#34648=CARTESIAN_POINT('Ctrl Pts',(14.6189747978427,-0.577967613166301,
-5.42511263803678));
#34649=CARTESIAN_POINT('Ctrl Pts',(14.6266712537219,-0.589946057792036,
-5.68610831669644));
#34650=CARTESIAN_POINT('Ctrl Pts',(14.6388917659254,-0.610003749620148,
-6.21288609120711));
#34651=CARTESIAN_POINT('Ctrl Pts',(14.6527014652724,-0.635210361922765,
-7.12556047241501));
#34652=CARTESIAN_POINT('Ctrl Pts',(14.6557197938956,-0.649738254045434,
-8.4149020244448));
#34653=CARTESIAN_POINT('Ctrl Pts',(14.6487675087243,-0.650689112584959,
-9.67872412606275));
#34654=CARTESIAN_POINT('Ctrl Pts',(14.6449804595606,-0.65169415946043,-10.5495371614848));
#34655=CARTESIAN_POINT('Ctrl Pts',(14.6440223013186,-0.653390173386025,
-11.0427651834159));
#34656=CARTESIAN_POINT('Ctrl Pts',(14.6440935479156,-0.654782110586744,
-11.2878771507872));
#34657=CARTESIAN_POINT('Ctrl Pts',(14.644410748038,-0.656098167934278,-11.4720377844606));
#34658=CARTESIAN_POINT('Ctrl Pts',(14.644596826737,-0.656954171553811,-11.6003216120659));
#34659=CARTESIAN_POINT('Ctrl Pts',(14.6448506490134,-0.65846059666502,-11.8539261484059));
#34660=CARTESIAN_POINT('Ctrl Pts',(14.6450078304074,-0.660620745336611,
-12.2980494275863));
#34661=CARTESIAN_POINT('Ctrl Pts',(14.6441144207941,-0.663938980749091,
-13.4344334651777));
#34662=CARTESIAN_POINT('Ctrl Pts',(14.6403828036926,-0.66250451342443,-14.6872309086493));
#34663=CARTESIAN_POINT('Ctrl Pts',(14.6371980784744,-0.660296369796018,
-15.9381573936582));
#34664=CARTESIAN_POINT('Ctrl Pts',(14.6360059921958,-0.65935859603253,-16.5640543178105));
#34665=CARTESIAN_POINT('Ctrl Pts',(14.635462637249,-0.658922651127044,-17.0654182024739));
#34666=CARTESIAN_POINT('Ctrl Pts',(14.635352481037,-0.658845427413407,-17.316400499451));
#34667=CARTESIAN_POINT('Ctrl Pts',(14.6353417591257,-0.658853429342191,
-17.5040152635562));
#34668=CARTESIAN_POINT('Ctrl Pts',(14.6353571064953,-0.658854724164119,
-17.6287585220641));
#34669=CARTESIAN_POINT('Ctrl Pts',(14.6354719377722,-0.658840559604473,
-17.8779376136121));
#34670=CARTESIAN_POINT('Ctrl Pts',(14.6357009996904,-0.658803757903174,
-18.1274062923526));
#34671=CARTESIAN_POINT('Ctrl Pts',(14.6360285153936,-0.658745667646573,
-18.3769412078243));
#34672=CARTESIAN_POINT('Ctrl Pts',(14.6362692312006,-0.658701461788393,
-18.5329793145762));
#34673=CARTESIAN_POINT('Ctrl Pts',(14.6364814865989,-0.658661504375778,
-18.6578404208514));
#34674=CARTESIAN_POINT('Ctrl Pts',(14.6367059358736,-0.658618534443917,
-18.7827285092989));
#34675=CARTESIAN_POINT('Ctrl Pts',(14.6373687437213,-0.658490720845063,
-19.1262718546939));
#34676=CARTESIAN_POINT('Ctrl Pts',(14.6386717472663,-0.658222632735348,
-19.6890094189946));
#34677=CARTESIAN_POINT('Ctrl Pts',(14.6411978702278,-0.657659795614467,
-20.6911364612033));
#34678=CARTESIAN_POINT('Ctrl Pts',(14.6439798247638,-0.656868696869042,
-21.9471940091887));
#34679=CARTESIAN_POINT('Ctrl Pts',(14.6441686157926,-0.656448414793447,
-22.9559680415154));
#34680=CARTESIAN_POINT('Ctrl Pts',(14.6431430916204,-0.656300061609959,
-23.5860567718861));
#34681=CARTESIAN_POINT('Ctrl Pts',(14.6426229433556,-0.656246471252463,
-23.8355925193941));
#34682=CARTESIAN_POINT('Ctrl Pts',(14.6411775215826,-0.65615890474012,-24.3353020723151));
#34683=CARTESIAN_POINT('Ctrl Pts',(14.6377218693294,-0.656040548619147,
-25.2114694865791));
#34684=CARTESIAN_POINT('Ctrl Pts',(14.630931002644,-0.655932213546865,-26.4666335432331));
#34685=CARTESIAN_POINT('Ctrl Pts',(14.6223146384926,-0.655668239594834,
-27.9745595516146));
#34686=CARTESIAN_POINT('Ctrl Pts',(14.6179171860164,-0.655445702698336,
-28.9786726424719));
#34687=CARTESIAN_POINT('Ctrl Pts',(14.6162837788159,-0.655294134551463,
-29.5419272467765));
#34688=CARTESIAN_POINT('Ctrl Pts',(14.6160526186354,-0.655431598986769,
-29.6618678131118));
#34689=CARTESIAN_POINT('Ctrl Pts',(14.616077382021,-0.656336226474451,-29.9056909605988));
#34690=CARTESIAN_POINT('Ctrl Pts',(14.617272582571,-0.659413701806968,-30.3331582640928));
#34691=CARTESIAN_POINT('Ctrl Pts',(14.6232727430873,-0.670210520658779,
-31.1983989008025));
#34692=CARTESIAN_POINT('Ctrl Pts',(14.6337803186591,-0.687008466127124,
-32.2067891285952));
#34693=CARTESIAN_POINT('Ctrl Pts',(14.6387619758346,-0.695431285875479,
-33.2344469506228));
#34694=CARTESIAN_POINT('Ctrl Pts',(14.6374425383742,-0.694208271454865,
-34.0143290999874));
#34695=CARTESIAN_POINT('Ctrl Pts',(14.6287348608639,-0.681999141243495,
-34.8034317094201));
#34696=CARTESIAN_POINT('Ctrl Pts',(14.6163979205044,-0.664066380160658,
-35.3354422613335));
#34697=CARTESIAN_POINT('Ctrl Pts',(14.6040256480247,-0.645869465357065,
-35.7381142952021));
#34698=CARTESIAN_POINT('Ctrl Pts',(14.5941965503113,-0.631098851807827,
-36.0162513416395));
#34699=CARTESIAN_POINT('Ctrl Pts',(14.5692778703312,-0.593921211685036,
-36.5604144990715));
#34700=CARTESIAN_POINT('Ctrl Pts',(14.5136952188433,-0.511016907625734,
-37.4982534980529));
#34701=CARTESIAN_POINT('Ctrl Pts',(14.3688154380279,-0.296013867944767,
-39.3038417030766));
#34702=CARTESIAN_POINT('Ctrl Pts',(14.2412748366334,-0.103913541802183,
-40.7308966430827));
#34703=CARTESIAN_POINT('Ctrl Pts',(14.2007198503395,-0.041093094070166,
-41.7462840081312));
#34704=CARTESIAN_POINT('Ctrl Pts',(14.1926845082915,-0.0295996644645384,
-41.9714637433589));
#34705=CARTESIAN_POINT('Ctrl Pts',(14.1831712501751,-0.0177873381933792,
-42.3151913299676));
#34706=CARTESIAN_POINT('Ctrl Pts',(14.175954585427,-0.0109313467580231,
-42.6642712761484));
#34707=CARTESIAN_POINT('Ctrl Pts',(14.1690727655943,-0.00731900968447937,
-43.1369985049661));
#34708=CARTESIAN_POINT('Ctrl Pts',(14.1649874111451,-0.0113324728833667,
-43.7412301831783));
#34709=CARTESIAN_POINT('Ctrl Pts',(14.1653540359968,-0.0230281051507635,
-44.4870156367657));
#34710=CARTESIAN_POINT('Ctrl Pts',(14.168437914655,-0.0323762303982092,
-45.1252156814221));
#34711=CARTESIAN_POINT('Ctrl Pts',(14.1715872552744,-0.0356362457752205,
-45.645851223175));
#34712=CARTESIAN_POINT('Ctrl Pts',(14.1740599557543,-0.0349179086061656,
-46.0411583115204));
#34713=CARTESIAN_POINT('Ctrl Pts',(14.1763997595407,-0.0299574615799581,
-46.4413118080271));
#34714=CARTESIAN_POINT('Ctrl Pts',(14.1790129891584,-0.0162060290324866,
-46.9811770540874));
#34715=CARTESIAN_POINT('Ctrl Pts',(14.1800566255083,0.00387885879804714,
-47.3931509835375));
#34716=CARTESIAN_POINT('Ctrl Pts',(14.1799839193984,0.0328654514553911,
-47.8099162855327));
#34717=CARTESIAN_POINT('Ctrl Pts',(14.1801699126152,0.050442263674094,-48.0585622102138));
#34718=CARTESIAN_POINT('Ctrl Pts',(14.1813949791877,0.0887586200856952,
-48.5757443673385));
#34719=CARTESIAN_POINT('Ctrl Pts',(14.1854212572758,0.161526430360534,-49.4778028225827));
#34720=CARTESIAN_POINT('Ctrl Pts',(14.1945592362753,0.291531467721919,-50.7883928435346));
#34721=CARTESIAN_POINT('Ctrl Pts',(14.2042550733362,0.513009107213242,-52.3831151560713));
#34722=CARTESIAN_POINT('Ctrl Pts',(14.2051663413128,0.721191364602573,-53.4616910628258));
#34723=CARTESIAN_POINT('Ctrl Pts',(14.2025787229755,0.875692912286117,-54.1407068771491));
#34724=CARTESIAN_POINT('Ctrl Pts',(14.2012739081521,0.939052912013921,-54.4104195310996));
#34725=CARTESIAN_POINT('Ctrl Pts',(14.1976254729671,1.07375873756196,-54.9508991578226));
#34726=CARTESIAN_POINT('Ctrl Pts',(14.1889001249657,1.3280120419816,-55.8918948767622));
#34727=CARTESIAN_POINT('Ctrl Pts',(14.1647212737922,1.90595529360788,-57.7590647206015));
#34728=CARTESIAN_POINT('Ctrl Pts',(14.1415184678372,2.49993288989735,-59.3250783966603));
#34729=CARTESIAN_POINT('Ctrl Pts',(14.131970141928,2.95077088735296,-60.4160582227018));
#34730=CARTESIAN_POINT('Ctrl Pts',(14.1307710836269,3.00955831636239,-60.5565771168024));
#34731=CARTESIAN_POINT('Ctrl Pts',(14.1284534374888,3.12746976575313,-60.831640867667));
#34732=CARTESIAN_POINT('Ctrl Pts',(14.1245188339413,3.3403348058412,-61.3119979220487));
#34733=CARTESIAN_POINT('Ctrl Pts',(14.1172208409135,3.7844632034876,-62.2576103132215));
#34734=CARTESIAN_POINT('Ctrl Pts',(14.1101772483488,4.32279535372546,-63.3099087432315));
#34735=CARTESIAN_POINT('Ctrl Pts',(14.1043800409819,4.86523831329963,-64.331189455735));
#34736=CARTESIAN_POINT('Ctrl Pts',(14.1015589331006,5.16728968206662,-64.8936695292806));
#34737=CARTESIAN_POINT('Ctrl Pts',(14.0998535271436,5.36536341095623,-65.2632505212294));
#34738=CARTESIAN_POINT('Ctrl Pts',(14.0987631670646,5.49640348952483,-65.5081634934525));
#34739=CARTESIAN_POINT('Ctrl Pts',(14.097740478461,5.62575958346341,-65.750870239036));
#34740=CARTESIAN_POINT('Ctrl Pts',(14.0969055959606,5.737097329896,-65.9611607932242));
#34741=CARTESIAN_POINT('Ctrl Pts',(14.0964453913745,5.80014387688518,-66.0807225592858));
#34742=CARTESIAN_POINT('Ctrl Pts',(14.0957720260039,5.894120752074,-66.2594662298233));
#34743=CARTESIAN_POINT('Ctrl Pts',(14.0952453994318,5.97112719209651,-66.4071136441018));
#34744=CARTESIAN_POINT('Ctrl Pts',(14.094420702844,6.09679499953658,-66.6500823173283));
#34745=CARTESIAN_POINT('Ctrl Pts',(14.0936733266644,6.2345195842633,-66.9154735311475));
#34746=CARTESIAN_POINT('Ctrl Pts',(14.0925563499899,6.50475175827377,-67.4329375581774));
#34747=CARTESIAN_POINT('Ctrl Pts',(14.0914884899755,6.97822414671521,-68.3320177551548));
#34748=CARTESIAN_POINT('Ctrl Pts',(14.0920786701469,7.91667658554508,-70.0905855126675));
#34749=CARTESIAN_POINT('Ctrl Pts',(14.0944616232842,8.71295349364137,-71.5668686173992));
#34750=CARTESIAN_POINT('Ctrl Pts',(14.0944203771024,9.30813886155358,-72.6862306066469));
#34751=CARTESIAN_POINT('Ctrl Pts',(14.0944129266693,9.44193414211487,-72.9378583214016));
#34752=CARTESIAN_POINT('Ctrl Pts',(14.094401644644,9.70874540476567,-73.4396508401897));
#34753=CARTESIAN_POINT('Ctrl Pts',(14.094393790156,10.0423867401557,-74.067135425168));
#34754=CARTESIAN_POINT('Ctrl Pts',(14.0943927400073,10.442369684355,-74.8193939097495));
#34755=CARTESIAN_POINT('Ctrl Pts',(14.094401938375,11.2421279686844,-76.3235272219561));
#34756=CARTESIAN_POINT('Ctrl Pts',(14.0944215158371,11.9083145311271,-77.576458354187));
#34757=CARTESIAN_POINT('Ctrl Pts',(14.0944204190697,12.8782355883391,-79.4006165662628));
#34758=CARTESIAN_POINT('Ctrl Pts',(14.0944198510847,13.3148007666061,-80.2216772868161));
#34759=CARTESIAN_POINT('Ctrl Pts',(14.0944198510847,13.7513223539956,-81.0426549889144));
#34760=CARTESIAN_POINT('Ctrl Pts',(16.9134010704912,-0.00101211290211373,
24.8306360281983));
#34761=CARTESIAN_POINT('Ctrl Pts',(16.9134515851132,-0.00101216298668399,
24.7817567553152));
#34762=CARTESIAN_POINT('Ctrl Pts',(16.9135045614701,-0.00101221733777369,
24.7328785600789));
#34763=CARTESIAN_POINT('Ctrl Pts',(16.9141302683925,-0.00101277382828913,
24.1822701699722));
#34764=CARTESIAN_POINT('Ctrl Pts',(16.9146093969652,-0.00101336582011031,
23.1781289778484));
#34765=CARTESIAN_POINT('Ctrl Pts',(16.9157222684248,-0.00101635417976157,
21.1695304690424));
#34766=CARTESIAN_POINT('Ctrl Pts',(16.919887647335,-0.00101909292100717,
19.6653620532305));
#34767=CARTESIAN_POINT('Ctrl Pts',(16.9287242477762,-0.00102394440616367,
18.4143064981284));
#34768=CARTESIAN_POINT('Ctrl Pts',(16.9329616521634,-0.00102672623135195,
17.9114915242589));
#34769=CARTESIAN_POINT('Ctrl Pts',(16.9436018359616,-0.00103395784223769,
16.9074991314347));
#34770=CARTESIAN_POINT('Ctrl Pts',(16.9664240149538,-0.00104977486294956,
15.1536831036689));
#34771=CARTESIAN_POINT('Ctrl Pts',(16.9881142952943,-0.00105774583357663,
13.6518945109012));
#34772=CARTESIAN_POINT('Ctrl Pts',(17.0017205179854,-0.00105612070077724,
12.3973905181308));
#34773=CARTESIAN_POINT('Ctrl Pts',(17.00728354403,-0.00105509932350135,
11.8964263867371));
#34774=CARTESIAN_POINT('Ctrl Pts',(17.0186292831805,-0.00104972614985391,
10.8945690573246));
#34775=CARTESIAN_POINT('Ctrl Pts',(17.038273396033,-0.00103592836115452,
9.14098616641578));
#34776=CARTESIAN_POINT('Ctrl Pts',(17.0520731254646,-0.00101141481218296,
7.63574208026637));
#34777=CARTESIAN_POINT('Ctrl Pts',(17.0582013852299,-0.00100031734776509,
6.50459176410634));
#34778=CARTESIAN_POINT('Ctrl Pts',(17.0592472161264,-0.000807859651648968,
6.25190653752823));
#34779=CARTESIAN_POINT('Ctrl Pts',(17.0602873551709,0.000198982466678631,
5.74812435408048));
#34780=CARTESIAN_POINT('Ctrl Pts',(17.0598280761885,0.00321326207857862,
4.86635425594689));
#34781=CARTESIAN_POINT('Ctrl Pts',(17.0535730927932,0.0112852006322439,
3.10810905803595));
#34782=CARTESIAN_POINT('Ctrl Pts',(17.0521709339728,0.0112998091967429,
1.61686178593503));
#34783=CARTESIAN_POINT('Ctrl Pts',(17.0653475382084,-0.0016525451973971,
0.575295319315679));
#34784=CARTESIAN_POINT('Ctrl Pts',(17.0670550137546,-0.00333319431329617,
0.452234021601371));
#34785=CARTESIAN_POINT('Ctrl Pts',(17.0709941824522,-0.00720646393610515,
0.205334822652025));
#34786=CARTESIAN_POINT('Ctrl Pts',(17.0791668908371,-0.015235953441166,
-0.226906573901212));
#34787=CARTESIAN_POINT('Ctrl Pts',(17.093976404849,-0.0297392650086584,
-0.846084503850126));
#34788=CARTESIAN_POINT('Ctrl Pts',(17.1150350693186,-0.0503005092990941,
-1.59187825505627));
#34789=CARTESIAN_POINT('Ctrl Pts',(17.1452781567032,-0.079676674057784,
-2.59060025215715));
#34790=CARTESIAN_POINT('Ctrl Pts',(17.1828830449709,-0.116026267737767,
-3.84795045468806));
#34791=CARTESIAN_POINT('Ctrl Pts',(17.20367526053,-0.13689468150225,-4.86553318329858));
#34792=CARTESIAN_POINT('Ctrl Pts',(17.2108571856803,-0.145209364453794,
-5.5058282838844));
#34793=CARTESIAN_POINT('Ctrl Pts',(17.2133370193797,-0.148277992537555,
-5.75901501432666));
#34794=CARTESIAN_POINT('Ctrl Pts',(17.2168625181439,-0.153461595669578,
-6.26684228454734));
#34795=CARTESIAN_POINT('Ctrl Pts',(17.2196570823651,-0.160268540870484,
-7.15387174200375));
#34796=CARTESIAN_POINT('Ctrl Pts',(17.2161957907094,-0.164846610753823,
-8.41831375137636));
#34797=CARTESIAN_POINT('Ctrl Pts',(17.2086652847334,-0.165894483071219,
-9.67542171650664));
#34798=CARTESIAN_POINT('Ctrl Pts',(17.204344428868,-0.166484237745355,-10.5503473101162));
#34799=CARTESIAN_POINT('Ctrl Pts',(17.202591260253,-0.167023235471124,-11.0486030835193));
#34800=CARTESIAN_POINT('Ctrl Pts',(17.2020271185242,-0.167400366556015,
-11.2971269343835));
#34801=CARTESIAN_POINT('Ctrl Pts',(17.2017475472665,-0.167740422767266,
-11.48409458387));
#34802=CARTESIAN_POINT('Ctrl Pts',(17.2015524547536,-0.16794943888993,-11.610846864052));
#34803=CARTESIAN_POINT('Ctrl Pts',(17.2011370054641,-0.168295419965447,
-11.8633836146047));
#34804=CARTESIAN_POINT('Ctrl Pts',(17.2003497396288,-0.168720501775088,
-12.3048501423687));
#34805=CARTESIAN_POINT('Ctrl Pts',(17.1980759356503,-0.168991746416044,
-13.4361686515847));
#34806=CARTESIAN_POINT('Ctrl Pts',(17.195166342771,-0.16748464734297,-14.6856322936344));
#34807=CARTESIAN_POINT('Ctrl Pts',(17.1929427647513,-0.166025264204655,
-15.936236513704));
#34808=CARTESIAN_POINT('Ctrl Pts',(17.192091582413,-0.165457473599947,-16.5626055131858));
#34809=CARTESIAN_POINT('Ctrl Pts',(17.1916233913902,-0.165193040786199,
-17.0647803125105));
#34810=CARTESIAN_POINT('Ctrl Pts',(17.1914677453772,-0.165139481591272,
-17.3162986549023));
#34811=CARTESIAN_POINT('Ctrl Pts',(17.1913850731145,-0.165134236199292,
-17.5043622594433));
#34812=CARTESIAN_POINT('Ctrl Pts',(17.191348644696,-0.16512106484283,-17.6292564913955));
#34813=CARTESIAN_POINT('Ctrl Pts',(17.1913446759282,-0.165061999303678,
-17.8787680895582));
#34814=CARTESIAN_POINT('Ctrl Pts',(17.1914332508204,-0.164961471165937,
-18.1284650671892));
#34815=CARTESIAN_POINT('Ctrl Pts',(17.1916038734292,-0.164828811201584,
-18.3781744105982));
#34816=CARTESIAN_POINT('Ctrl Pts',(17.1917401349492,-0.164736014496021,
-18.5342875656331));
#34817=CARTESIAN_POINT('Ctrl Pts',(17.1918657123936,-0.164656910754746,
-18.6591925189444));
#34818=CARTESIAN_POINT('Ctrl Pts',(17.1920016369369,-0.164574886043304,
-18.7841123853212));
#34819=CARTESIAN_POINT('Ctrl Pts',(17.1924117324506,-0.164345436637,-19.1276903432311));
#34820=CARTESIAN_POINT('Ctrl Pts',(17.1932699185797,-0.163941364873975,
-19.6902183631619));
#34821=CARTESIAN_POINT('Ctrl Pts',(17.1949883319485,-0.163455992169393,
-20.691191527286));
#34822=CARTESIAN_POINT('Ctrl Pts',(17.1969478648271,-0.163637135736605,
-21.9444203752336));
#34823=CARTESIAN_POINT('Ctrl Pts',(17.1969970314627,-0.165760114789861,
-22.9494207069731));
#34824=CARTESIAN_POINT('Ctrl Pts',(17.1961696538154,-0.167927488336689,
-23.576699079459));
#34825=CARTESIAN_POINT('Ctrl Pts',(17.1957545684123,-0.16889756834329,-23.824580657638));
#34826=CARTESIAN_POINT('Ctrl Pts',(17.1946012022147,-0.171294332463981,
-24.3217271026583));
#34827=CARTESIAN_POINT('Ctrl Pts',(17.1918508109013,-0.176506695480344,
-25.194230216388));
#34828=CARTESIAN_POINT('Ctrl Pts',(17.1864385424517,-0.186161713891325,
-26.4470593020611));
#34829=CARTESIAN_POINT('Ctrl Pts',(17.179693734892,-0.198235214341492,-27.9566636321236));
#34830=CARTESIAN_POINT('Ctrl Pts',(17.1764096119066,-0.204826586355265,
-28.9647261094821));
#34831=CARTESIAN_POINT('Ctrl Pts',(17.1753272541737,-0.207458681419564,
-29.5313529950025));
#34832=CARTESIAN_POINT('Ctrl Pts',(17.1751445967002,-0.208063086582707,
-29.6554266700394));
#34833=CARTESIAN_POINT('Ctrl Pts',(17.1749891798098,-0.209424878074251,
-29.9049026660955));
#34834=CARTESIAN_POINT('Ctrl Pts',(17.1752153459553,-0.212141967300124,
-30.3416243728318));
#34835=CARTESIAN_POINT('Ctrl Pts',(17.1772652557581,-0.21852268673992,-31.2180724911193));
#34836=CARTESIAN_POINT('Ctrl Pts',(17.1814166304052,-0.226246158720518,
-32.2247964553449));
#34837=CARTESIAN_POINT('Ctrl Pts',(17.1837242446055,-0.230889730583628,
-33.2358402786202));
#34838=CARTESIAN_POINT('Ctrl Pts',(17.1836212786991,-0.231969424975495,
-33.9959253124533));
#34839=CARTESIAN_POINT('Ctrl Pts',(17.180761376691,-0.229833784540344,-34.7575837027073));
#34840=CARTESIAN_POINT('Ctrl Pts',(17.1764123040643,-0.22565813026792,-35.2662106297554));
#34841=CARTESIAN_POINT('Ctrl Pts',(17.1719958652942,-0.221245152351467,
-35.6490605845432));
#34842=CARTESIAN_POINT('Ctrl Pts',(17.16849832909,-0.217712347575618,-35.9073148872236));
#34843=CARTESIAN_POINT('Ctrl Pts',(17.1596174202635,-0.208535106444459,
-36.420556897512));
#34844=CARTESIAN_POINT('Ctrl Pts',(17.1398262512644,-0.187586376473583,
-37.3140101396874));
#34845=CARTESIAN_POINT('Ctrl Pts',(17.0889808123628,-0.131047673218112,
-39.0817287769171));
#34846=CARTESIAN_POINT('Ctrl Pts',(17.0454414315167,-0.0761651363072375,
-40.5684528421309));
#34847=CARTESIAN_POINT('Ctrl Pts',(17.0318850438195,-0.0539912644416674,
-41.6732315274097));
#34848=CARTESIAN_POINT('Ctrl Pts',(17.0292214004439,-0.0505667957516916,
-41.907605347663));
#34849=CARTESIAN_POINT('Ctrl Pts',(17.0261376777833,-0.0483916202365658,
-42.2683784749758));
#34850=CARTESIAN_POINT('Ctrl Pts',(17.0238733039162,-0.0487778072880304,
-42.6312292904252));
#34851=CARTESIAN_POINT('Ctrl Pts',(17.0218305108725,-0.0518242957205186,
-43.1211998751754));
#34852=CARTESIAN_POINT('Ctrl Pts',(17.0208767056471,-0.0589310512847072,
-43.7427738125955));
#34853=CARTESIAN_POINT('Ctrl Pts',(17.0215749943808,-0.0675708651721102,
-44.5035932800172));
#34854=CARTESIAN_POINT('Ctrl Pts',(17.0230941742369,-0.0703394841680138,
-45.1492707441048));
#34855=CARTESIAN_POINT('Ctrl Pts',(17.0244855042361,-0.0670859480560476,
-45.6728939699293));
#34856=CARTESIAN_POINT('Ctrl Pts',(17.0255376111403,-0.0611357074905208,
-46.0689460167095));
#34857=CARTESIAN_POINT('Ctrl Pts',(17.0265051171325,-0.050916701376646,
-46.4683351154574));
#34858=CARTESIAN_POINT('Ctrl Pts',(17.0275494830201,-0.0305908520694293,
-47.0051754871332));
#34859=CARTESIAN_POINT('Ctrl Pts',(17.0279485298638,-0.00651356267870405,
-47.4125881784468));
#34860=CARTESIAN_POINT('Ctrl Pts',(17.027871025413,0.0250247472743915,-47.823537087381));
#34861=CARTESIAN_POINT('Ctrl Pts',(17.0279445204245,0.0453507766221093,
-48.0785047352768));
#34862=CARTESIAN_POINT('Ctrl Pts',(17.0284901041219,0.0901937661096688,
-48.6012889715114));
#34863=CARTESIAN_POINT('Ctrl Pts',(17.0302587584616,0.177593175442441,-49.5132589892957));
#34864=CARTESIAN_POINT('Ctrl Pts',(17.0337291862979,0.33360895778891,-50.8277687101996));
#34865=CARTESIAN_POINT('Ctrl Pts',(17.0351310915789,0.582883041778303,-52.4149695324514));
#34866=CARTESIAN_POINT('Ctrl Pts',(17.0318463451629,0.80031213472367,-53.4799784868388));
#34867=CARTESIAN_POINT('Ctrl Pts',(17.0277490187653,0.955439440182285,-54.1483596116179));
#34868=CARTESIAN_POINT('Ctrl Pts',(17.0258424488058,1.01918280988269,-54.4157872537986));
#34869=CARTESIAN_POINT('Ctrl Pts',(17.0211461857495,1.15344357491875,-54.951209548359));
#34870=CARTESIAN_POINT('Ctrl Pts',(17.0109087247023,1.40479153071745,-55.8853439606409));
#34871=CARTESIAN_POINT('Ctrl Pts',(16.984753882311,1.97014456173065,-57.7437500515642));
#34872=CARTESIAN_POINT('Ctrl Pts',(16.9606180598848,2.5494463143456,-59.3108745233488));
#34873=CARTESIAN_POINT('Ctrl Pts',(16.950361723684,2.9949772413804,-60.4057342821153));
#34874=CARTESIAN_POINT('Ctrl Pts',(16.9491073046583,3.05259874766688,-60.5455884776621));
#34875=CARTESIAN_POINT('Ctrl Pts',(16.9466853619297,3.16838014856612,-60.8200491397828));
#34876=CARTESIAN_POINT('Ctrl Pts',(16.942620918488,3.37717852163246,-61.299217702888));
#34877=CARTESIAN_POINT('Ctrl Pts',(16.9352294511537,3.81272231434839,-62.2434288889346));
#34878=CARTESIAN_POINT('Ctrl Pts',(16.9283406644973,4.34066707435569,-63.2954579139722));
#34879=CARTESIAN_POINT('Ctrl Pts',(16.9228040541019,4.87398964320674,-64.3178341147752));
#34880=CARTESIAN_POINT('Ctrl Pts',(16.920141194956,5.17167860343828,-64.8814124517947));
#34881=CARTESIAN_POINT('Ctrl Pts',(16.9185301080169,5.36729007332549,-65.2519469242985));
#34882=CARTESIAN_POINT('Ctrl Pts',(16.9175003525531,5.49682016376608,-65.4975540875435));
#34883=CARTESIAN_POINT('Ctrl Pts',(16.9165269998,5.62485777415317,-65.7410500677168));
#34884=CARTESIAN_POINT('Ctrl Pts',(16.9157288893456,5.73524940179998,-65.9521145711583));
#34885=CARTESIAN_POINT('Ctrl Pts',(16.9152866444826,5.79781536441384,-66.0721439981323));
#34886=CARTESIAN_POINT('Ctrl Pts',(16.9146373118575,5.89113377149035,-66.2516144809089));
#34887=CARTESIAN_POINT('Ctrl Pts',(16.9141213623647,5.96771782117635,-66.3999258533314));
#34888=CARTESIAN_POINT('Ctrl Pts',(16.9133049693211,6.09288052949987,-66.6440651452324));
#34889=CARTESIAN_POINT('Ctrl Pts',(16.9125662700127,6.23002422703788,-66.9103980955905));
#34890=CARTESIAN_POINT('Ctrl Pts',(16.9114683668413,6.49963646627558,-67.4296844202676));
#34891=CARTESIAN_POINT('Ctrl Pts',(16.9104262500859,6.97294614154424,-68.3314056845011));
#34892=CARTESIAN_POINT('Ctrl Pts',(16.9110520933701,7.91390854629592,-70.0932822293166));
#34893=CARTESIAN_POINT('Ctrl Pts',(16.9134073097484,8.71293266517356,-71.5688689618016));
#34894=CARTESIAN_POINT('Ctrl Pts',(16.9133674206332,9.30682319629896,-72.6859786116366));
#34895=CARTESIAN_POINT('Ctrl Pts',(16.9133622712192,9.44069244288629,-72.9377707805658));
#34896=CARTESIAN_POINT('Ctrl Pts',(16.9133536603917,9.70745196172853,-73.4395069259972));
#34897=CARTESIAN_POINT('Ctrl Pts',(16.9133456322856,10.0411163676074,-74.0670749356618));
#34898=CARTESIAN_POINT('Ctrl Pts',(16.9133436988121,10.4410973824441,-74.8193396278468));
#34899=CARTESIAN_POINT('Ctrl Pts',(16.9133478951202,11.2408916722415,-76.3235221726316));
#34900=CARTESIAN_POINT('Ctrl Pts',(16.913352509992,11.9070907868733,-77.5764604690554));
#34901=CARTESIAN_POINT('Ctrl Pts',(16.9133463396528,12.876981812635,-79.4005947887978));
#34902=CARTESIAN_POINT('Ctrl Pts',(16.9133431703429,13.3135497833338,-80.2216775335791));
#34903=CARTESIAN_POINT('Ctrl Pts',(16.9133431703429,13.7500713707233,-81.0426552356776));
#34904=CARTESIAN_POINT('Ctrl Pts',(19.7346230857497,-0.000642953111401741,
24.8306355395365));
#34905=CARTESIAN_POINT('Ctrl Pts',(19.7346821167419,-0.000642934736490794,
24.781756252557));
#34906=CARTESIAN_POINT('Ctrl Pts',(19.7347440260616,-0.000642913768523213,
24.7328780189341));
#34907=CARTESIAN_POINT('Ctrl Pts',(19.7354751641474,-0.000642741727641322,
24.1822702714333));
#34908=CARTESIAN_POINT('Ctrl Pts',(19.7360360872234,-0.000643517082627163,
23.1781357609119));
#34909=CARTESIAN_POINT('Ctrl Pts',(19.7373409930261,-0.000644592940470209,
21.169537608259));
#34910=CARTESIAN_POINT('Ctrl Pts',(19.7422073080115,-0.000644228994501214,
19.6653856082875));
#34911=CARTESIAN_POINT('Ctrl Pts',(19.7525254976372,-0.000639085395243651,
18.4143370820647));
#34912=CARTESIAN_POINT('Ctrl Pts',(19.7574741046864,-0.000636573362535956,
17.9115221213179));
#34913=CARTESIAN_POINT('Ctrl Pts',(19.7699008328156,-0.000630633018027315,
16.9075337937884));
#34914=CARTESIAN_POINT('Ctrl Pts',(19.79655504348,-0.000617266269918687,
15.1537233398426));
#34915=CARTESIAN_POINT('Ctrl Pts',(19.821875349484,-0.000605020852467982,
13.6519770448393));
#34916=CARTESIAN_POINT('Ctrl Pts',(19.8377436350961,-0.000592969546270982,
12.3974956126268));
#34917=CARTESIAN_POINT('Ctrl Pts',(19.8442301715107,-0.000587175138563672,
11.8965382478349));
#34918=CARTESIAN_POINT('Ctrl Pts',(19.8574528580582,-0.000574554883993074,
10.8946893215832));
#34919=CARTESIAN_POINT('Ctrl Pts',(19.8803358682593,-0.00054875605103042,
9.14114851187957));
#34920=CARTESIAN_POINT('Ctrl Pts',(19.8963889971374,-0.000536768765242916,
7.63592840905772));
#34921=CARTESIAN_POINT('Ctrl Pts',(19.9035179481799,-0.000530587930652473,
6.50502163852959));
#34922=CARTESIAN_POINT('Ctrl Pts',(19.9049801590683,-0.000553432928634556,
6.25511760243307));
#34923=CARTESIAN_POINT('Ctrl Pts',(19.9074770795704,-0.000679949177192419,
5.75435183526716));
#34924=CARTESIAN_POINT('Ctrl Pts',(19.9107964265407,-0.00106714628387842,
4.87638767184662));
#34925=CARTESIAN_POINT('Ctrl Pts',(19.9138001065816,-0.00209765951886981,
3.11587427664056));
#34926=CARTESIAN_POINT('Ctrl Pts',(19.9121023976492,-0.00212305173409241,
1.60724231122929));
#34927=CARTESIAN_POINT('Ctrl Pts',(19.9107191795177,-0.000458589584695931,
0.545455546299319));
#34928=CARTESIAN_POINT('Ctrl Pts',(19.910536721583,-0.000240879410105755,
0.418856935719241));
#34929=CARTESIAN_POINT('Ctrl Pts',(19.9101056334482,0.000263531734119996,
0.165994698487929));
#34930=CARTESIAN_POINT('Ctrl Pts',(19.9091827300556,0.00131805171169694,
-0.275935387072352));
#34931=CARTESIAN_POINT('Ctrl Pts',(19.9074245102459,0.00323972576446598,
-0.905606226749042));
#34932=CARTESIAN_POINT('Ctrl Pts',(19.9047108946236,0.00602030268412137,
-1.65908800201351));
#34933=CARTESIAN_POINT('Ctrl Pts',(19.9004523608938,0.01002517504186,-2.66149121249902));
#34934=CARTESIAN_POINT('Ctrl Pts',(19.8941653858529,0.0150642551577006,
-3.91142926653451));
#34935=CARTESIAN_POINT('Ctrl Pts',(19.8888148939253,0.0178887851550629,
-4.91030040063366));
#34936=CARTESIAN_POINT('Ctrl Pts',(19.8856001260017,0.0189503528382262,
-5.53506672615536));
#34937=CARTESIAN_POINT('Ctrl Pts',(19.8842625781479,0.019331232340815,-5.78557007654373));
#34938=CARTESIAN_POINT('Ctrl Pts',(19.881420005471,0.0199225557911846,-6.28673777410555));
#34939=CARTESIAN_POINT('Ctrl Pts',(19.8760732500074,0.020557544334544,-7.16470056012135));
#34940=CARTESIAN_POINT('Ctrl Pts',(19.86775437564,0.0205928311815489,-8.42014679737612));
#34941=CARTESIAN_POINT('Ctrl Pts',(19.8595226870973,0.0201745887778942,
-9.67457783212885));
#34942=CARTESIAN_POINT('Ctrl Pts',(19.8543205682205,0.0200185830632958,
-10.5506646481595));
#34943=CARTESIAN_POINT('Ctrl Pts',(19.8515839106785,0.0200193520216717,
-11.0505094359074));
#34944=CARTESIAN_POINT('Ctrl Pts',(19.8503064139383,0.020058521840743,-11.3001384889717));
#34945=CARTESIAN_POINT('Ctrl Pts',(19.8493831115964,0.02010609406382,-11.4880183077322));
#34946=CARTESIAN_POINT('Ctrl Pts',(19.848759579533,0.0201389662794458,-11.6141131856583));
#34947=CARTESIAN_POINT('Ctrl Pts',(19.8475035865337,0.0202088783303024,
-11.8660900631704));
#34948=CARTESIAN_POINT('Ctrl Pts',(19.8452901371666,0.0203402429399956,
-12.3063138185554));
#34949=CARTESIAN_POINT('Ctrl Pts',(19.8395963739657,0.0207155104692084,
-13.4352543682579));
#34950=CARTESIAN_POINT('Ctrl Pts',(19.8337233195694,0.0211892187478554,
-14.6834171900175));
#34951=CARTESIAN_POINT('Ctrl Pts',(19.8296973929213,0.021535321909794,-15.9343304218055));
#34952=CARTESIAN_POINT('Ctrl Pts',(19.828262623613,0.0216592588011182,-16.5612150515869));
#34953=CARTESIAN_POINT('Ctrl Pts',(19.827532909389,0.021717998410105,-17.0640315108058));
#34954=CARTESIAN_POINT('Ctrl Pts',(19.8273188497013,0.0217327140511073,
-17.3159473892265));
#34955=CARTESIAN_POINT('Ctrl Pts',(19.8272197499129,0.0217373640412579,
-17.5043252928702));
#34956=CARTESIAN_POINT('Ctrl Pts',(19.8271645940149,0.021743742715054,-17.6290672580878));
#34957=CARTESIAN_POINT('Ctrl Pts',(19.8270963895439,0.0217716370272419,
-17.8785042386958));
#34958=CARTESIAN_POINT('Ctrl Pts',(19.8270927400091,0.0218191141612584,
-18.1280752129324));
#34959=CARTESIAN_POINT('Ctrl Pts',(19.8271554676397,0.0218804577107381,
-18.3777251690563));
#34960=CARTESIAN_POINT('Ctrl Pts',(19.82722294071,0.0219235473964778,-18.5338030361248));
#34961=CARTESIAN_POINT('Ctrl Pts',(19.8272940849153,0.021960136806743,-18.658689553547));
#34962=CARTESIAN_POINT('Ctrl Pts',(19.8273765552953,0.021998026722338,-18.7835940973741));
#34963=CARTESIAN_POINT('Ctrl Pts',(19.8276539168662,0.0221052563178028,
-19.1271513721223));
#34964=CARTESIAN_POINT('Ctrl Pts',(19.8283688675522,0.0222941765936138,
-19.689739383064));
#34965=CARTESIAN_POINT('Ctrl Pts',(19.8304691154989,0.0225287937954849,
-20.6911098412784));
#34966=CARTESIAN_POINT('Ctrl Pts',(19.8346284038769,0.0224225988438274,
-21.9452964756393));
#34967=CARTESIAN_POINT('Ctrl Pts',(19.8398820955914,0.0213428595161395,
-22.9516036161008));
#34968=CARTESIAN_POINT('Ctrl Pts',(19.8437546466324,0.0202230855359422,
-23.5798476343222));
#34969=CARTESIAN_POINT('Ctrl Pts',(19.84542658254,0.0197138857317108,-23.8282650337369));
#34970=CARTESIAN_POINT('Ctrl Pts',(19.8492992870015,0.0184781981973547,
-24.3262507423293));
#34971=CARTESIAN_POINT('Ctrl Pts',(19.857267766854,0.015824936416586,-25.1999679111835));
#34972=CARTESIAN_POINT('Ctrl Pts',(19.8711374113828,0.0111859737214354,
-26.4535682981818));
#34973=CARTESIAN_POINT('Ctrl Pts',(19.8882621349692,0.00576243781980644,
-27.9627331221817));
#34974=CARTESIAN_POINT('Ctrl Pts',(19.8978645033397,0.00308643285001822,
-28.9694055740695));
#34975=CARTESIAN_POINT('Ctrl Pts',(19.9020476452313,0.00202842531119992,
-29.5351389851221));
#34976=CARTESIAN_POINT('Ctrl Pts',(19.9029598655213,0.00179395500155851,
-29.660711242041));
#34977=CARTESIAN_POINT('Ctrl Pts',(19.9047368949606,0.00136864071316774,
-29.9119673822201));
#34978=CARTESIAN_POINT('Ctrl Pts',(19.9077264104863,0.00071936380440862,
-30.3516893036152));
#34979=CARTESIAN_POINT('Ctrl Pts',(19.9132380639417,-0.000244003107841386,
-31.2313376651581));
#34980=CARTESIAN_POINT('Ctrl Pts',(19.9185788054482,-0.000796108407126999,
-32.2363666896278));
#34981=CARTESIAN_POINT('Ctrl Pts',(19.9231699515195,-0.00130293714163212,
-33.2400982545545));
#34982=CARTESIAN_POINT('Ctrl Pts',(19.926287582346,-0.00178506957046058,
-33.9919628075564));
#34983=CARTESIAN_POINT('Ctrl Pts',(19.9291537330895,-0.00247603470082823,
-34.7425267762971));
#34984=CARTESIAN_POINT('Ctrl Pts',(19.930921520269,-0.00316109123277813,
-35.2418837084394));
#34985=CARTESIAN_POINT('Ctrl Pts',(19.932212815312,-0.00379711533894955,
-35.6169656511168));
#34986=CARTESIAN_POINT('Ctrl Pts',(19.9331201298407,-0.00430080901852659,
-35.8676312652858));
#34987=CARTESIAN_POINT('Ctrl Pts',(19.9350542554739,-0.00559418401298511,
-36.3690027760414));
#34988=CARTESIAN_POINT('Ctrl Pts',(19.9385694048054,-0.00841243403087586,
-37.2453622153362));
#34989=CARTESIAN_POINT('Ctrl Pts',(19.9450600062419,-0.0153862358953072,
-38.9978150636203));
#34990=CARTESIAN_POINT('Ctrl Pts',(19.9457014876814,-0.0193132523885131,
-40.50342730423));
#34991=CARTESIAN_POINT('Ctrl Pts',(19.9405912460554,-0.0175424815871379,
-41.6396344433984));
#34992=CARTESIAN_POINT('Ctrl Pts',(19.939417941721,-0.0180609024665847,
-41.8773427901699));
#34993=CARTESIAN_POINT('Ctrl Pts',(19.9374487737961,-0.0209480616663699,
-42.2441269452064));
#34994=CARTESIAN_POINT('Ctrl Pts',(19.9352664823961,-0.0254730253434529,
-42.611783774443));
#34995=CARTESIAN_POINT('Ctrl Pts',(19.9320404046982,-0.0329960094720893,
-43.1076484405979));
#34996=CARTESIAN_POINT('Ctrl Pts',(19.9273834522402,-0.0438998692360093,
-43.7349078281428));
#34997=CARTESIAN_POINT('Ctrl Pts',(19.920645793495,-0.0550409518824901,
-44.5001571844784));
#34998=CARTESIAN_POINT('Ctrl Pts',(19.9139481025105,-0.058917689892779,
-45.1474411022027));
#34999=CARTESIAN_POINT('Ctrl Pts',(19.9079109430792,-0.0563763703496538,
-45.6711601971578));
#35000=CARTESIAN_POINT('Ctrl Pts',(19.9030063055532,-0.0510379740403673,
-46.0666739926564));
#35001=CARTESIAN_POINT('Ctrl Pts',(19.8977111471374,-0.041636222220782,
-46.4649218026843));
#35002=CARTESIAN_POINT('Ctrl Pts',(19.8901265591865,-0.0228219799811086,
-46.9994538907081));
#35003=CARTESIAN_POINT('Ctrl Pts',(19.8837762659454,-0.00066810850759029,
-47.4042332401222));
#35004=CARTESIAN_POINT('Ctrl Pts',(19.877004516628,0.0282497019994057,-47.8120475821032));
#35005=CARTESIAN_POINT('Ctrl Pts',(19.8720730452078,0.0469490572617378,
-48.0669242890347));
#35006=CARTESIAN_POINT('Ctrl Pts',(19.8608461763039,0.0882600632253731,
-48.5886303230491));
#35007=CARTESIAN_POINT('Ctrl Pts',(19.8381971947123,0.169269250258146,-49.4998005116595));
#35008=CARTESIAN_POINT('Ctrl Pts',(19.8005116026619,0.316415072387404,-50.8144923814608));
#35009=CARTESIAN_POINT('Ctrl Pts',(19.7571232499412,0.558733185701103,-52.4044613455247));
#35010=CARTESIAN_POINT('Ctrl Pts',(19.7354326536812,0.774332347196781,-53.4727165621296));
#35011=CARTESIAN_POINT('Ctrl Pts',(19.7259938964815,0.929292946652962,-54.1436236906726));
#35012=CARTESIAN_POINT('Ctrl Pts',(19.722378034875,0.993021295346837,-54.4118453951711));
#35013=CARTESIAN_POINT('Ctrl Pts',(19.7158892867674,1.1275509880106,-54.9488036427376));
#35014=CARTESIAN_POINT('Ctrl Pts',(19.7063490604149,1.37998863274845,-55.8852205667512));
#35015=CARTESIAN_POINT('Ctrl Pts',(19.6938101649099,1.94940883769124,-57.7468499435128));
#35016=CARTESIAN_POINT('Ctrl Pts',(19.6917179920513,2.53343609922751,-59.3144488274368));
#35017=CARTESIAN_POINT('Ctrl Pts',(19.6921472074124,2.98058714663305,-60.408320468436));
#35018=CARTESIAN_POINT('Ctrl Pts',(19.6923302411128,3.03855380157463,-60.5484454487465));
#35019=CARTESIAN_POINT('Ctrl Pts',(19.6928896930775,3.15496837800988,-60.8232006982505));
#35020=CARTESIAN_POINT('Ctrl Pts',(19.6944621969898,3.36498448187706,-61.3029405460856));
#35021=CARTESIAN_POINT('Ctrl Pts',(19.699547978084,3.80312264363572,-62.2479633131678));
#35022=CARTESIAN_POINT('Ctrl Pts',(19.708472488342,4.33433639755622,-63.3003758582488));
#35023=CARTESIAN_POINT('Ctrl Pts',(19.7178062533734,4.87058092910209,-64.3225010121906));
#35024=CARTESIAN_POINT('Ctrl Pts',(19.7227363601189,5.16968125139723,-64.8857202902664));
#35025=CARTESIAN_POINT('Ctrl Pts',(19.7256892775882,5.3660993240338,-65.2559282740194));
#35026=CARTESIAN_POINT('Ctrl Pts',(19.7275529269646,5.4961236312018,-65.5012946526292));
#35027=CARTESIAN_POINT('Ctrl Pts',(19.7292494930669,5.62460530306604,-65.7445154007033));
#35028=CARTESIAN_POINT('Ctrl Pts',(19.7305409820397,5.73531536293809,-65.9553101543504));
#35029=CARTESIAN_POINT('Ctrl Pts',(19.7312200009703,5.79804464979269,-66.0751771047758));
#35030=CARTESIAN_POINT('Ctrl Pts',(19.7321763080164,5.89158788007909,-66.2543957286631));
#35031=CARTESIAN_POINT('Ctrl Pts',(19.7328433165431,5.96832407956894,-66.402477667768));
#35032=CARTESIAN_POINT('Ctrl Pts',(19.7337361677523,6.09367212132328,-66.64621744546));
#35033=CARTESIAN_POINT('Ctrl Pts',(19.7345472830898,6.23102804903925,-66.9122358782964));
#35034=CARTESIAN_POINT('Ctrl Pts',(19.7357637525657,6.50088493107782,-67.4309132821684));
#35035=CARTESIAN_POINT('Ctrl Pts',(19.73696023581,6.97433195159225,-68.3317564250992));
#35036=CARTESIAN_POINT('Ctrl Pts',(19.7364841334505,7.91461052110222,-70.0925538466961));
#35037=CARTESIAN_POINT('Ctrl Pts',(19.7341525791219,8.71285882012307,-71.568314545697));
#35038=CARTESIAN_POINT('Ctrl Pts',(19.7342536478909,9.30719870643568,-72.6861159988526));
#35039=CARTESIAN_POINT('Ctrl Pts',(19.7342693216236,9.4410471924085,-72.9378486651355));
#35040=CARTESIAN_POINT('Ctrl Pts',(19.734294087738,9.70782792197631,-73.4395913415074));
#35041=CARTESIAN_POINT('Ctrl Pts',(19.73431380359,10.0414888140811,-74.0671184098798));
#35042=CARTESIAN_POINT('Ctrl Pts',(19.7343174844631,10.4414675358527,-74.8193699085516));
#35043=CARTESIAN_POINT('Ctrl Pts',(19.7343007359239,11.241238470148,-76.3235214394896));
#35044=CARTESIAN_POINT('Ctrl Pts',(19.7342702208829,11.9074313046534,-77.5764535976686));
#35045=CARTESIAN_POINT('Ctrl Pts',(19.7342790380661,12.8773505355511,-79.4006103950861));
#35046=CARTESIAN_POINT('Ctrl Pts',(19.7342835685967,13.3139183378821,-80.221677090073));
#35047=CARTESIAN_POINT('Ctrl Pts',(19.7342835685968,13.7504399252715,-81.0426547921714));
#35048=CARTESIAN_POINT('Ctrl Pts',(22.5540683561216,0.00218147413889375,
24.8306318837938));
#35049=CARTESIAN_POINT('Ctrl Pts',(22.554135708553,0.0021816069582444,24.781752480719));
#35050=CARTESIAN_POINT('Ctrl Pts',(22.5542063449766,0.00218174482895129,
24.7328741280427));
#35051=CARTESIAN_POINT('Ctrl Pts',(22.5550405516681,0.00218343279774944,
24.1822650476588));
#35052=CARTESIAN_POINT('Ctrl Pts',(22.5556808204131,0.00218653523452655,
23.1781290012419));
#35053=CARTESIAN_POINT('Ctrl Pts',(22.5571704372049,0.00219387923828822,
21.1695284782211));
#35054=CARTESIAN_POINT('Ctrl Pts',(22.5627227814794,0.00220569836013384,
19.6653768549175));
#35055=CARTESIAN_POINT('Ctrl Pts',(22.5744942562184,0.00222185508179394,
18.4143286693318));
#35056=CARTESIAN_POINT('Ctrl Pts',(22.5801396960068,0.00223007976877095,
17.9115066393623));
#35057=CARTESIAN_POINT('Ctrl Pts',(22.5943159820712,0.00225185213321563,
16.9075134210456));
#35058=CARTESIAN_POINT('Ctrl Pts',(22.6247225788558,0.00229799248967236,
15.153703473283));
#35059=CARTESIAN_POINT('Ctrl Pts',(22.6536089727913,0.00233443368688111,
13.6519813201694));
#35060=CARTESIAN_POINT('Ctrl Pts',(22.6717145277981,0.00234043481082431,
12.3975308629626));
#35061=CARTESIAN_POINT('Ctrl Pts',(22.679115594771,0.00234074687208769,
11.8965860813863));
#35062=CARTESIAN_POINT('Ctrl Pts',(22.6942029354826,0.00233563010780471,
10.8947553295711));
#35063=CARTESIAN_POINT('Ctrl Pts',(22.7203138747303,0.00231381924858082,
9.14123354533352));
#35064=CARTESIAN_POINT('Ctrl Pts',(22.7386363554764,0.00228962747677265,
7.63600350836706));
#35065=CARTESIAN_POINT('Ctrl Pts',(22.7467772039179,0.00227689513963197,
6.5050900642413));
#35066=CARTESIAN_POINT('Ctrl Pts',(22.7485221996124,0.00223748350450178,
6.25533927343516));
#35067=CARTESIAN_POINT('Ctrl Pts',(22.7517687074826,0.00204041652177819,
5.75473880201197));
#35068=CARTESIAN_POINT('Ctrl Pts',(22.756746021602,0.00145805657110865,
4.87698664852411));
#35069=CARTESIAN_POINT('Ctrl Pts',(22.7633409013492,-9.50353224288473E-5,
3.11633965161738));
#35070=CARTESIAN_POINT('Ctrl Pts',(22.7614298458992,-0.000101851369145884,
1.60673369886307));
#35071=CARTESIAN_POINT('Ctrl Pts',(22.754755687708,0.00237657533938654,
0.543821997324392));
#35072=CARTESIAN_POINT('Ctrl Pts',(22.7538849752791,0.00269824982403687,
0.417040370789071));
#35073=CARTESIAN_POINT('Ctrl Pts',(22.7518618090786,0.00344090667788074,
0.163862775610429));
#35074=CARTESIAN_POINT('Ctrl Pts',(22.7476225754754,0.00498369006181879,
-0.278579310015945));
#35075=CARTESIAN_POINT('Ctrl Pts',(22.7398195734886,0.00778723782990159,
-0.908804588765807));
#35076=CARTESIAN_POINT('Ctrl Pts',(22.7284275590651,0.0117866394648969,
-1.6626456912705));
#35077=CARTESIAN_POINT('Ctrl Pts',(22.7115977999302,0.0175719377185294,
-2.66510680565334));
#35078=CARTESIAN_POINT('Ctrl Pts',(22.6894237529051,0.0248789730569118,
-3.91437002671321));
#35079=CARTESIAN_POINT('Ctrl Pts',(22.6746279323472,0.0292114700920186,
-4.91228617641643));
#35080=CARTESIAN_POINT('Ctrl Pts',(22.6675562993878,0.0309313882324642,
-5.5364254127196));
#35081=CARTESIAN_POINT('Ctrl Pts',(22.6647896390813,0.0315766094374004,
-5.78702766260291));
#35082=CARTESIAN_POINT('Ctrl Pts',(22.6594992216835,0.0327005225668863,
-6.28815877217012));
#35083=CARTESIAN_POINT('Ctrl Pts',(22.6508460117802,0.0342590482256434,
-7.16606874547671));
#35084=CARTESIAN_POINT('Ctrl Pts',(22.6400133172493,0.0354626555877318,
-8.42107398284687));
#35085=CARTESIAN_POINT('Ctrl Pts',(22.6307092367043,0.0357005865857655,
-9.67465683280276));
#35086=CARTESIAN_POINT('Ctrl Pts',(22.6247301929899,0.0355672907810145,
-10.5498966593995));
#35087=CARTESIAN_POINT('Ctrl Pts',(22.6214297571352,0.0354360409498412,
-11.0491879677433));
#35088=CARTESIAN_POINT('Ctrl Pts',(22.6198116453495,0.0353568730948748,
-11.2985176495465));
#35089=CARTESIAN_POINT('Ctrl Pts',(22.6186028341508,0.0352940820780271,
-11.4861565312266));
#35090=CARTESIAN_POINT('Ctrl Pts',(22.6177874524816,0.0352378259324908,
-11.611867847455));
#35091=CARTESIAN_POINT('Ctrl Pts',(22.6161496709671,0.035072157733957,-11.8632532885014));
#35092=CARTESIAN_POINT('Ctrl Pts',(22.6132752194428,0.0346523606763489,
-12.3024953421541));
#35093=CARTESIAN_POINT('Ctrl Pts',(22.6059441579138,0.0330017977772016,
-13.4295791077051));
#35094=CARTESIAN_POINT('Ctrl Pts',(22.598602354385,0.030057379385193,-14.677520602664));
#35095=CARTESIAN_POINT('Ctrl Pts',(22.5939390070843,0.0277608272128385,
-15.9301343469425));
#35096=CARTESIAN_POINT('Ctrl Pts',(22.592426221169,0.0269196020107557,-16.5583233401281));
#35097=CARTESIAN_POINT('Ctrl Pts',(22.5918052172197,0.0265202899207708,
-17.0624557535612));
#35098=CARTESIAN_POINT('Ctrl Pts',(22.591704598448,0.026425712580917,-17.3151272795674));
#35099=CARTESIAN_POINT('Ctrl Pts',(22.5917144447763,0.0264002013132958,
-17.5040742508018));
#35100=CARTESIAN_POINT('Ctrl Pts',(22.5917487630321,0.0263702963468637,
-17.6282069779701));
#35101=CARTESIAN_POINT('Ctrl Pts',(22.5919252031847,0.0262575873912922,
-17.8771189025034));
#35102=CARTESIAN_POINT('Ctrl Pts',(22.5922557762722,0.0260765632870242,
-18.1261007585217));
#35103=CARTESIAN_POINT('Ctrl Pts',(22.5927310220947,0.0258508062393998,
-18.3754317061234));
#35104=CARTESIAN_POINT('Ctrl Pts',(22.5930852523955,0.0256949150880551,
-18.5313488908643));
#35105=CARTESIAN_POINT('Ctrl Pts',(22.5934018269883,0.0255643923002756,
-18.6561552304994));
#35106=CARTESIAN_POINT('Ctrl Pts',(22.5937398083511,0.0254310783739573,
-18.7810025555363));
#35107=CARTESIAN_POINT('Ctrl Pts',(22.5947569696741,0.0250516744836173,
-19.1245123719922));
#35108=CARTESIAN_POINT('Ctrl Pts',(22.5968697909726,0.0244272748524223,
-19.6876037237825));
#35109=CARTESIAN_POINT('Ctrl Pts',(22.6016928063477,0.023736309273104,-20.6915355013246));
#35110=CARTESIAN_POINT('Ctrl Pts',(22.6092220907402,0.0246838664602423,
-21.9520496006516));
#35111=CARTESIAN_POINT('Ctrl Pts',(22.6159651125159,0.0292734278575275,
-22.966722303222));
#35112=CARTESIAN_POINT('Ctrl Pts',(22.6200050894728,0.0340288155052018,
-23.6012568386363));
#35113=CARTESIAN_POINT('Ctrl Pts',(22.6216960539806,0.0361924278746453,
-23.8534746245936));
#35114=CARTESIAN_POINT('Ctrl Pts',(22.6254141445623,0.0414336069590376,
-24.3573247228981));
#35115=CARTESIAN_POINT('Ctrl Pts',(22.6326435229306,0.0527088136412557,
-25.2394652019242));
#35116=CARTESIAN_POINT('Ctrl Pts',(22.6443106503046,0.0727322552410105,
-26.4984118526265));
#35117=CARTESIAN_POINT('Ctrl Pts',(22.6577636488587,0.0972434087164042,
-28.0039143274124));
#35118=CARTESIAN_POINT('Ctrl Pts',(22.6648986224874,0.109910840772038,-29.0011715067303));
#35119=CARTESIAN_POINT('Ctrl Pts',(22.667906150243,0.115058735797627,-29.5597546137854));
#35120=CARTESIAN_POINT('Ctrl Pts',(22.6685373980379,0.116221209894467,-29.6853423185855));
#35121=CARTESIAN_POINT('Ctrl Pts',(22.6696760198942,0.118507809722523,-29.935698806095));
#35122=CARTESIAN_POINT('Ctrl Pts',(22.6713694335329,0.12242392958844,-30.3742436235447));
#35123=CARTESIAN_POINT('Ctrl Pts',(22.6737257579926,0.129834840657116,-31.2509365971211));
#35124=CARTESIAN_POINT('Ctrl Pts',(22.6749011413929,0.136936610672894,-32.2522134124557));
#35125=CARTESIAN_POINT('Ctrl Pts',(22.6761981716237,0.141970330127987,-33.2514988088751));
#35126=CARTESIAN_POINT('Ctrl Pts',(22.6776431338712,0.144534674572906,-33.9997484962132));
#35127=CARTESIAN_POINT('Ctrl Pts',(22.6800043956835,0.145645822770892,-34.7463847821545));
#35128=CARTESIAN_POINT('Ctrl Pts',(22.6824604269127,0.145311856209713,-35.2429076455261));
#35129=CARTESIAN_POINT('Ctrl Pts',(22.6847454964563,0.144612206113386,-35.6157555666383));
#35130=CARTESIAN_POINT('Ctrl Pts',(22.6865345137926,0.143935748993521,-35.8647138062475));
#35131=CARTESIAN_POINT('Ctrl Pts',(22.6909948954712,0.141825139239321,-36.3629355945598));
#35132=CARTESIAN_POINT('Ctrl Pts',(22.7007211017334,0.136319998449124,-37.2340753087831));
#35133=CARTESIAN_POINT('Ctrl Pts',(22.7247187730148,0.11964407152272,-38.9777466279288));
#35134=CARTESIAN_POINT('Ctrl Pts',(22.7420439175246,0.100879259671926,-40.4797501482002));
#35135=CARTESIAN_POINT('Ctrl Pts',(22.742174398847,0.0900117196293994,-41.6152353076556));
#35136=CARTESIAN_POINT('Ctrl Pts',(22.7419947456864,0.0868629477186161,
-41.8530396771713));
#35137=CARTESIAN_POINT('Ctrl Pts',(22.7411588868783,0.0798734920793458,
-42.2195939742537));
#35138=CARTESIAN_POINT('Ctrl Pts',(22.7397815779615,0.0711701094471297,
-42.586859208967));
#35139=CARTESIAN_POINT('Ctrl Pts',(22.737263822772,0.0578805058533532,-43.081875181358));
#35140=CARTESIAN_POINT('Ctrl Pts',(22.7329120829938,0.0393414645107835,
-43.7075346067066));
#35141=CARTESIAN_POINT('Ctrl Pts',(22.7259867352306,0.0180490019609267,
-44.4699595380308));
#35142=CARTESIAN_POINT('Ctrl Pts',(22.7189754097439,0.00461976903386266,
-45.1141309663419));
#35143=CARTESIAN_POINT('Ctrl Pts',(22.7127423271767,-0.00138856537622484,
-45.6349447941414));
#35144=CARTESIAN_POINT('Ctrl Pts',(22.7077745025803,-0.00293648720720613,
-46.0280483924158));
#35145=CARTESIAN_POINT('Ctrl Pts',(22.702539756329,-0.000952767527570727,
-46.4236679472298));
#35146=CARTESIAN_POINT('Ctrl Pts',(22.695248106512,0.00715860064351331,
-46.9544003416955));
#35147=CARTESIAN_POINT('Ctrl Pts',(22.6894368964206,0.0203671438046086,
-47.3560146155071));
#35148=CARTESIAN_POINT('Ctrl Pts',(22.6834694544482,0.039481350339373,-47.7603227791904));
#35149=CARTESIAN_POINT('Ctrl Pts',(22.6791422427141,0.0512307024465059,
-48.0075015017657));
#35150=CARTESIAN_POINT('Ctrl Pts',(22.6692324211024,0.0763142779141968,
-48.5191761118809));
#35151=CARTESIAN_POINT('Ctrl Pts',(22.6491107551827,0.124158552493288,-49.416497872572));
#35152=CARTESIAN_POINT('Ctrl Pts',(22.6148657729272,0.215268103806751,-50.7276117444274));
#35153=CARTESIAN_POINT('Ctrl Pts',(22.5746907034547,0.395225833157523,-52.3372310364046));
#35154=CARTESIAN_POINT('Ctrl Pts',(22.5555260121924,0.588228809792435,-53.4345630297578));
#35155=CARTESIAN_POINT('Ctrl Pts',(22.5480884581515,0.74030785136882,-54.1276488294856));
#35156=CARTESIAN_POINT('Ctrl Pts',(22.5452460751718,0.803140727604942,-54.4022021073488));
#35157=CARTESIAN_POINT('Ctrl Pts',(22.5404938550578,0.938793274403183,-54.9516189864557));
#35158=CARTESIAN_POINT('Ctrl Pts',(22.5341958029479,1.19920161828228,-55.9053975612708));
#35159=CARTESIAN_POINT('Ctrl Pts',(22.5281267758728,1.80275630578089,-57.7881154594452));
#35160=CARTESIAN_POINT('Ctrl Pts',(22.528583603618,2.42533038851665,-59.35130068497));
#35161=CARTESIAN_POINT('Ctrl Pts',(22.528532377079,2.88493160586583,-60.4337308314408));
#35162=CARTESIAN_POINT('Ctrl Pts',(22.5287259190148,2.94571920325708,-60.5750505472678));
#35163=CARTESIAN_POINT('Ctrl Pts',(22.5291677879915,3.06720147455161,-60.850552993609));
#35164=CARTESIAN_POINT('Ctrl Pts',(22.5303403340556,3.28675165509904,-61.3319382132006));
#35165=CARTESIAN_POINT('Ctrl Pts',(22.5338469167794,3.74449224051456,-62.2782340020111));
#35166=CARTESIAN_POINT('Ctrl Pts',(22.5397048431139,4.29830979361861,-63.3298919614451));
#35167=CARTESIAN_POINT('Ctrl Pts',(22.5457174570534,4.85400363670458,-64.3492239718143));
#35168=CARTESIAN_POINT('Ctrl Pts',(22.5488714298889,5.16234868040809,-64.9101497756193));
#35169=CARTESIAN_POINT('Ctrl Pts',(22.5507492352918,5.36397377145835,-65.2784630670283));
#35170=CARTESIAN_POINT('Ctrl Pts',(22.551931627265,5.49720250657446,-65.5224660380437));
#35171=CARTESIAN_POINT('Ctrl Pts',(22.5530001707,5.6284580866325,-65.7641630999649));
#35172=CARTESIAN_POINT('Ctrl Pts',(22.5538074203757,5.74118426524144,-65.9734681757563));
#35173=CARTESIAN_POINT('Ctrl Pts',(22.5542291325583,5.8049417377464,-66.0924361240013));
#35174=CARTESIAN_POINT('Ctrl Pts',(22.5548200729008,5.89990121284972,-66.2702572205141));
#35175=CARTESIAN_POINT('Ctrl Pts',(22.5552240851311,5.97754530004697,-66.4170687212062));
#35176=CARTESIAN_POINT('Ctrl Pts',(22.5557509286219,6.10401749845465,-66.6585493188342));
#35177=CARTESIAN_POINT('Ctrl Pts',(22.5562022351456,6.24252186488589,-66.922501445448));
#35178=CARTESIAN_POINT('Ctrl Pts',(22.5568282241031,6.51358133221557,-67.4373154524345));
#35179=CARTESIAN_POINT('Ctrl Pts',(22.5572574572638,6.98704795492337,-68.3324605421028));
#35180=CARTESIAN_POINT('Ctrl Pts',(22.5560808670878,7.92134723887345,-70.0860597307467));
#35181=CARTESIAN_POINT('Ctrl Pts',(22.5537908216693,8.71315752530691,-71.5635641333792));
#35182=CARTESIAN_POINT('Ctrl Pts',(22.5536221564192,9.3102139919392,-72.6864389144413));
#35183=CARTESIAN_POINT('Ctrl Pts',(22.5535880143634,9.44388849338344,-72.9378363622075));
#35184=CARTESIAN_POINT('Ctrl Pts',(22.5535378432735,9.71076529731538,-73.4397479822456));
#35185=CARTESIAN_POINT('Ctrl Pts',(22.5535059689553,10.0443610125397,-74.0671478108037));
#35186=CARTESIAN_POINT('Ctrl Pts',(22.5535030828491,10.444355436008,-74.8194294880936));
#35187=CARTESIAN_POINT('Ctrl Pts',(22.5535484575473,11.2440931997388,-76.3235325103929));
#35188=CARTESIAN_POINT('Ctrl Pts',(22.5536517783583,11.9102687075601,-77.5764681404427));
#35189=CARTESIAN_POINT('Ctrl Pts',(22.5536551658664,12.8801832338076,-79.4006231145849));
#35190=CARTESIAN_POINT('Ctrl Pts',(22.5536569200915,13.3167425765319,-80.2216775136107));
#35191=CARTESIAN_POINT('Ctrl Pts',(22.5536569200916,13.7532641639214,-81.0426552157089));
#35192=CARTESIAN_POINT('Ctrl Pts',(25.3681329014818,0.00175512325942154,
24.8306327114547));
#35193=CARTESIAN_POINT('Ctrl Pts',(25.3682084066264,0.00175506440139837,
24.7817533351788));
#35194=CARTESIAN_POINT('Ctrl Pts',(25.3682875944382,0.00175500320257746,
24.73287501414));
#35195=CARTESIAN_POINT('Ctrl Pts',(25.369222751594,0.00175425231120099,
24.1822661052121));
#35196=CARTESIAN_POINT('Ctrl Pts',(25.3699366350458,0.00175478425630212,
23.1781287518567));
#35197=CARTESIAN_POINT('Ctrl Pts',(25.3715957331742,0.00175722934477583,
21.1695289275335));
#35198=CARTESIAN_POINT('Ctrl Pts',(25.3778196824431,0.00175189404505957,
19.6653756524456));
#35199=CARTESIAN_POINT('Ctrl Pts',(25.3910342840048,0.00173499406283094,
18.4143272223797));
#35200=CARTESIAN_POINT('Ctrl Pts',(25.3973705443932,0.00172725455765711,
17.9115074792048));
#35201=CARTESIAN_POINT('Ctrl Pts',(25.4132791906795,0.00170817665878482,
16.9075149255972));
#35202=CARTESIAN_POINT('Ctrl Pts',(25.4474027842317,0.00166701913903138,
15.1537022583482));
#35203=CARTESIAN_POINT('Ctrl Pts',(25.4798405615858,0.00162111906728065,
13.6519650344697));
#35204=CARTESIAN_POINT('Ctrl Pts',(25.5002106904973,0.00158271977166255,
12.3975021657436));
#35205=CARTESIAN_POINT('Ctrl Pts',(25.5085421434162,0.00156602110601469,
11.8965526321469));
#35206=CARTESIAN_POINT('Ctrl Pts',(25.5255401762533,0.00152790014427616,
10.8947155709491));
#35207=CARTESIAN_POINT('Ctrl Pts',(25.5549874499801,0.00145470426919707,
9.14118230153193));
#35208=CARTESIAN_POINT('Ctrl Pts',(25.5756768333846,0.00139107439095266,
7.6359531409517));
#35209=CARTESIAN_POINT('Ctrl Pts',(25.5848715252591,0.00136281688660175,
6.50500245926613));
#35210=CARTESIAN_POINT('Ctrl Pts',(25.5868291161923,0.00135878771456196,
6.25475796638462));
#35211=CARTESIAN_POINT('Ctrl Pts',(25.5904255824825,0.00135700379304369,
5.75362379308219));
#35212=CARTESIAN_POINT('Ctrl Pts',(25.5958355797972,0.0013658411947461,
4.87519816783808));
#35213=CARTESIAN_POINT('Ctrl Pts',(25.6027324835524,0.00141374342985738,
3.11496398695253));
#35214=CARTESIAN_POINT('Ctrl Pts',(25.6006135930905,0.00139356100729972,
1.60842266632563));
#35215=CARTESIAN_POINT('Ctrl Pts',(25.5940653731096,0.00126840919376977,
0.549146222454319));
#35216=CARTESIAN_POINT('Ctrl Pts',(25.5932108642366,0.00125246996428166,
0.423005443203523));
#35217=CARTESIAN_POINT('Ctrl Pts',(25.5912223975216,0.0012154047501728,
0.170912548170089));
#35218=CARTESIAN_POINT('Ctrl Pts',(25.5870494140617,0.00113907015926919,
-0.269752289290245));
#35219=CARTESIAN_POINT('Ctrl Pts',(25.5793481002059,0.000999773781648224,
-0.898012224905597));
#35220=CARTESIAN_POINT('Ctrl Pts',(25.5680685042275,0.00081869072994828,
-1.65037512844969));
#35221=CARTESIAN_POINT('Ctrl Pts',(25.5513318271299,0.000564796045184066,
-2.65209276473023));
#35222=CARTESIAN_POINT('Ctrl Pts',(25.5290937037836,0.00028358619712762,
-3.90273938444517));
#35223=CARTESIAN_POINT('Ctrl Pts',(25.5139658455212,0.000143314572967394,
-4.90412568224005));
#35224=CARTESIAN_POINT('Ctrl Pts',(25.5066066317116,0.000113426011848074,
-5.53110188175309));
#35225=CARTESIAN_POINT('Ctrl Pts',(25.5036835254715,0.000114260159312473,
-5.78214345065753));
#35226=CARTESIAN_POINT('Ctrl Pts',(25.4979434853451,0.000157626732065502,
-6.2844308036127));
#35227=CARTESIAN_POINT('Ctrl Pts',(25.4882144756133,0.000320708389550938,
-7.16391082866169));
#35228=CARTESIAN_POINT('Ctrl Pts',(25.4754245271312,0.000690105851062742,
-8.42056581874819));
#35229=CARTESIAN_POINT('Ctrl Pts',(25.4646628399057,0.000930460627113542,
-9.67481228885));
#35230=CARTESIAN_POINT('Ctrl Pts',(25.4584799010143,0.000871282544065464,
-10.5500525215716));
#35231=CARTESIAN_POINT('Ctrl Pts',(25.4553746220341,0.000748308381848376,
-11.0492006290456));
#35232=CARTESIAN_POINT('Ctrl Pts',(25.4539712258333,0.00065353868288205,
-11.2984104554626));
#35233=CARTESIAN_POINT('Ctrl Pts',(25.4529730997057,0.000568068219536715,
-11.4859485564007));
#35234=CARTESIAN_POINT('Ctrl Pts',(25.452326132432,0.000502308203846308,
-11.6118537768369));
#35235=CARTESIAN_POINT('Ctrl Pts',(25.4511248493894,0.000339436248003312,
-11.8634638331684));
#35236=CARTESIAN_POINT('Ctrl Pts',(25.4492572720771,-2.13177763458417E-5,
-12.3031350879559));
#35237=CARTESIAN_POINT('Ctrl Pts',(25.4455733009429,-0.00127151211373016,
-13.4310595204373));
#35238=CARTESIAN_POINT('Ctrl Pts',(25.4442696957111,-0.00324028611677037,
-14.6793284460138));
#35239=CARTESIAN_POINT('Ctrl Pts',(25.4442188319478,-0.00469418068542391,
-15.9315714498161));
#35240=CARTESIAN_POINT('Ctrl Pts',(25.4443718553869,-0.00519040400416343,
-16.5594233238429));
#35241=CARTESIAN_POINT('Ctrl Pts',(25.444535750671,-0.00540381450733151,
-17.063191775564));
#35242=CARTESIAN_POINT('Ctrl Pts',(25.4446148166108,-0.0054358285895357,
-17.3156504373223));
#35243=CARTESIAN_POINT('Ctrl Pts',(25.4446703968559,-0.00543021020626045,
-17.5044367377568));
#35244=CARTESIAN_POINT('Ctrl Pts',(25.4447702572895,-0.00543876491614813,
-17.6287772188686));
#35245=CARTESIAN_POINT('Ctrl Pts',(25.4452033779121,-0.00548455064734357,
-17.8778862518301));
#35246=CARTESIAN_POINT('Ctrl Pts',(25.4459484732348,-0.00556518895829205,
-18.1270891705938));
#35247=CARTESIAN_POINT('Ctrl Pts',(25.4469513666631,-0.00566934587467172,
-18.3765573041242));
#35248=CARTESIAN_POINT('Ctrl Pts',(25.4476695073721,-0.00573957025722995,
-18.5325489822974));
#35249=CARTESIAN_POINT('Ctrl Pts',(25.4482921792919,-0.0057975462711501,
-18.6573999809797));
#35250=CARTESIAN_POINT('Ctrl Pts',(25.448943962461,-0.00585579423744788,
-18.7822849044884));
#35251=CARTESIAN_POINT('Ctrl Pts',(25.4508407251618,-0.00601388244252327,
-19.1258655044693));
#35252=CARTESIAN_POINT('Ctrl Pts',(25.4544128386284,-0.00623383029622586,
-19.6888923083069));
#35253=CARTESIAN_POINT('Ctrl Pts',(25.4607136401172,-0.00621497217796829,
-20.6921962973884));
#35254=CARTESIAN_POINT('Ctrl Pts',(25.4659070379412,-0.00488152850010207,
-21.950908820203));
#35255=CARTESIAN_POINT('Ctrl Pts',(25.4617334310053,-0.00136543214013412,
-22.9630575020273));
#35256=CARTESIAN_POINT('Ctrl Pts',(25.4548895692197,0.00193924301537645,
-23.5956290011506));
#35257=CARTESIAN_POINT('Ctrl Pts',(25.451682010114,0.00341722181846537,
-23.8468144058512));
#35258=CARTESIAN_POINT('Ctrl Pts',(25.4435054679934,0.00701771022553986,
-24.3489788833278));
#35259=CARTESIAN_POINT('Ctrl Pts',(25.4251966044907,0.0147766336876126,
-25.2286345451861));
#35260=CARTESIAN_POINT('Ctrl Pts',(25.3911009360267,0.0290385074477614,
-26.4856458523038));
#35261=CARTESIAN_POINT('Ctrl Pts',(25.3486156498219,0.0471068872725806,
-27.9915651436109));
#35262=CARTESIAN_POINT('Ctrl Pts',(25.3263690740992,0.0568900860452525,
-28.9911557795488));
#35263=CARTESIAN_POINT('Ctrl Pts',(25.3175812742222,0.0607584266492917,
-29.5516223804273));
#35264=CARTESIAN_POINT('Ctrl Pts',(25.3156293787246,0.061592916379088,-29.6769343510659));
#35265=CARTESIAN_POINT('Ctrl Pts',(25.3117385973929,0.0632320080383922,
-29.9271772256254));
#35266=CARTESIAN_POINT('Ctrl Pts',(25.3049829328802,0.0660034853406051,
-30.365428785787));
#35267=CARTESIAN_POINT('Ctrl Pts',(25.2919218208384,0.0711141872250324,
-31.2421328820492));
#35268=CARTESIAN_POINT('Ctrl Pts',(25.2789764183782,0.0758345991570889,
-32.244390638728));
#35269=CARTESIAN_POINT('Ctrl Pts',(25.2700163853228,0.0790603100313161,
-33.2458396436738));
#35270=CARTESIAN_POINT('Ctrl Pts',(25.2657798433522,0.0806436515990896,
-33.996278996021));
#35271=CARTESIAN_POINT('Ctrl Pts',(25.2644794704812,0.0813586561400045,
-34.745678118443));
#35272=CARTESIAN_POINT('Ctrl Pts',(25.2659042009034,0.081188793023538,-35.2444190767083));
#35273=CARTESIAN_POINT('Ctrl Pts',(25.2679651629538,0.080793461154485,-35.6190947913638));
#35274=CARTESIAN_POINT('Ctrl Pts',(25.2698038021904,0.0804011451233684,
-35.8696786868496));
#35275=CARTESIAN_POINT('Ctrl Pts',(25.2751350616424,0.0791410965171598,
-36.3705619577952));
#35276=CARTESIAN_POINT('Ctrl Pts',(25.2882912666579,0.0758383373910412,
-37.2456130265893));
#35277=CARTESIAN_POINT('Ctrl Pts',(25.3263009832524,0.0655881685321379,
-38.9934148472535));
#35278=CARTESIAN_POINT('Ctrl Pts',(25.3660237714869,0.0537048238599824,
-40.4924681546936));
#35279=CARTESIAN_POINT('Ctrl Pts',(25.3868173702797,0.0461422196979259,
-41.6233324791523));
#35280=CARTESIAN_POINT('Ctrl Pts',(25.3912373871007,0.0436140991761894,
-41.860221123796));
#35281=CARTESIAN_POINT('Ctrl Pts',(25.3973700983514,0.0374224242567952,
-42.2256358743637));
#35282=CARTESIAN_POINT('Ctrl Pts',(25.4031185807571,0.0293769893550175,
-42.5920052031964));
#35283=CARTESIAN_POINT('Ctrl Pts',(25.4103981796825,0.0168179227951479,
-43.0861397328003));
#35284=CARTESIAN_POINT('Ctrl Pts',(25.4190295780276,-0.00101099563237717,
-43.7112799075222));
#35285=CARTESIAN_POINT('Ctrl Pts',(25.4294620202946,-0.021554817131394,
-44.4739945711385));
#35286=CARTESIAN_POINT('Ctrl Pts',(25.4389209355737,-0.0342398653924662,
-45.1191659333761));
#35287=CARTESIAN_POINT('Ctrl Pts',(25.4473581299803,-0.0393363436383698,
-45.641235380365));
#35288=CARTESIAN_POINT('Ctrl Pts',(25.4542390415722,-0.0400471293213535,
-46.0355131625125));
#35289=CARTESIAN_POINT('Ctrl Pts',(25.4617820786829,-0.0370233890860234,
-46.4325422982045));
#35290=CARTESIAN_POINT('Ctrl Pts',(25.472856685772,-0.0271478199940004,
-46.9654673795409));
#35291=CARTESIAN_POINT('Ctrl Pts',(25.4825121168589,-0.0122484618405171,
-47.3690991664361));
#35292=CARTESIAN_POINT('Ctrl Pts',(25.493267506116,0.00907138186284126,
-47.7756692098869));
#35293=CARTESIAN_POINT('Ctrl Pts',(25.501211784735,0.0220973664887757,-48.0244308258799));
#35294=CARTESIAN_POINT('Ctrl Pts',(25.5199370045213,0.050323927401844,-48.5388691091687));
#35295=CARTESIAN_POINT('Ctrl Pts',(25.5588730890254,0.104697561159238,-49.440270598891));
#35296=CARTESIAN_POINT('Ctrl Pts',(25.6257355173962,0.208531107070698,-50.7555447682703));
#35297=CARTESIAN_POINT('Ctrl Pts',(25.7002509619933,0.409804400073271,-52.3671232960966));
#35298=CARTESIAN_POINT('Ctrl Pts',(25.728247498021,0.618019263522986,-53.4624325198976));
#35299=CARTESIAN_POINT('Ctrl Pts',(25.7334600658104,0.778437845763766,-54.1532441424037));
#35300=CARTESIAN_POINT('Ctrl Pts',(25.7349319083926,0.845541179631897,-54.4301320189739));
#35301=CARTESIAN_POINT('Ctrl Pts',(25.7347380859195,0.989797646729615,-54.9813031273514));
#35302=CARTESIAN_POINT('Ctrl Pts',(25.7272770131462,1.26607155773159,-55.9368281010095));
#35303=CARTESIAN_POINT('Ctrl Pts',(25.689298194883,1.89943737823761,-57.8135359681924));
#35304=CARTESIAN_POINT('Ctrl Pts',(25.6372206757203,2.53221269783963,-59.3618236532249));
#35305=CARTESIAN_POINT('Ctrl Pts',(25.6070393087952,2.98348633857783,-60.4301512945906));
#35306=CARTESIAN_POINT('Ctrl Pts',(25.6026691806258,3.0428503469781,-60.5693675812764));
#35307=CARTESIAN_POINT('Ctrl Pts',(25.5937983070444,3.16122724568963,-60.8412878946237));
#35308=CARTESIAN_POINT('Ctrl Pts',(25.5770435088133,3.37426564143506,-61.3171444820579));
#35309=CARTESIAN_POINT('Ctrl Pts',(25.5403294318885,3.81589521074941,-62.2556527357861));
#35310=CARTESIAN_POINT('Ctrl Pts',(25.4946976885163,4.34756025896486,-63.3039212552564));
#35311=CARTESIAN_POINT('Ctrl Pts',(25.4520398017056,4.88310998404356,-64.3237077519025));
#35312=CARTESIAN_POINT('Ctrl Pts',(25.4302032332109,5.18182040324868,-64.8863115932198));
#35313=CARTESIAN_POINT('Ctrl Pts',(25.4170265395301,5.37814378610955,-65.2563773576763));
#35314=CARTESIAN_POINT('Ctrl Pts',(25.4086409738142,5.50815980319325,-65.5017282449367));
#35315=CARTESIAN_POINT('Ctrl Pts',(25.4009045103152,5.63673168239466,-65.7450459230475));
#35316=CARTESIAN_POINT('Ctrl Pts',(25.394791660978,5.74763464779616,-65.9560398076997));
#35317=CARTESIAN_POINT('Ctrl Pts',(25.3914997534428,5.81051079104281,-66.0760542003117));
#35318=CARTESIAN_POINT('Ctrl Pts',(25.3867697623633,5.90431188593719,-66.2555271536956));
#35319=CARTESIAN_POINT('Ctrl Pts',(25.3832757638548,5.9813493352091,-66.4038965917702));
#35320=CARTESIAN_POINT('Ctrl Pts',(25.3781612478994,6.10730883680973,-66.6481876229862));
#35321=CARTESIAN_POINT('Ctrl Pts',(25.3734177864175,6.24427381811155,-66.9130325327389));
#35322=CARTESIAN_POINT('Ctrl Pts',(25.3660745822116,6.51358274593333,-67.4305557185275));
#35323=CARTESIAN_POINT('Ctrl Pts',(25.3582211469451,6.98514738255385,-68.3293237287385));
#35324=CARTESIAN_POINT('Ctrl Pts',(25.3580816655429,7.92020785558271,-70.0882057983418));
#35325=CARTESIAN_POINT('Ctrl Pts',(25.3693194658115,8.7143382475515,-71.5650278595612));
#35326=CARTESIAN_POINT('Ctrl Pts',(25.3681462159118,9.30898734236341,-72.685199163973));
#35327=CARTESIAN_POINT('Ctrl Pts',(25.367917096413,9.44269738110703,-72.9370229943887));
#35328=CARTESIAN_POINT('Ctrl Pts',(25.3675776648242,9.70941010015701,-73.4391576681312));
#35329=CARTESIAN_POINT('Ctrl Pts',(25.3673528745007,10.0430572274069,-74.0670009234832));
#35330=CARTESIAN_POINT('Ctrl Pts',(25.3673284253758,10.4431899420131,-74.819578242019));
#35331=CARTESIAN_POINT('Ctrl Pts',(25.367623027978,11.2434153013325,-76.324130100766));
#35332=CARTESIAN_POINT('Ctrl Pts',(25.3682779859034,11.9100659430314,-77.5769082849159));
#35333=CARTESIAN_POINT('Ctrl Pts',(25.368278431672,12.8796456096317,-79.4004200089946));
#35334=CARTESIAN_POINT('Ctrl Pts',(25.3682785991074,13.3163163216665,-80.2216769343914));
#35335=CARTESIAN_POINT('Ctrl Pts',(25.3682785991072,13.752837909056,-81.0426546364897));
#35336=CARTESIAN_POINT('Ctrl Pts',(27.7155278763841,-0.00393385284186832,
24.8306394904181));
#35337=CARTESIAN_POINT('Ctrl Pts',(27.7156106041345,-0.00393416938080131,
24.7817603293108));
#35338=CARTESIAN_POINT('Ctrl Pts',(27.7156973673394,-0.00393450211927658,
24.7328822274878));
#35339=CARTESIAN_POINT('Ctrl Pts',(27.716721963321,-0.00393838859547021,
24.182275835805));
#35340=CARTESIAN_POINT('Ctrl Pts',(27.717503441855,-0.00394355052081269,
23.1781418767792));
#35341=CARTESIAN_POINT('Ctrl Pts',(27.7193195511872,-0.00395770727941399,
21.1695464036031));
#35342=CARTESIAN_POINT('Ctrl Pts',(27.7261385733133,-0.00398305457749233,
19.6653929760623));
#35343=CARTESIAN_POINT('Ctrl Pts',(27.7406198960983,-0.00402582649965188,
18.414344021376));
#35344=CARTESIAN_POINT('Ctrl Pts',(27.7475639508972,-0.00404747964383108,
17.9115374502442));
#35345=CARTESIAN_POINT('Ctrl Pts',(27.7649993287739,-0.00410367701289973,
16.9075543253637));
#35346=CARTESIAN_POINT('Ctrl Pts',(27.8023983213515,-0.00422371392205734,
15.1537415029734));
#35347=CARTESIAN_POINT('Ctrl Pts',(27.8379460185578,-0.00432156848241613,
13.6519620075462));
#35348=CARTESIAN_POINT('Ctrl Pts',(27.8602632773443,-0.00435458583941141,
12.3974424140735));
#35349=CARTESIAN_POINT('Ctrl Pts',(27.8693910229039,-0.00436493508005512,
11.8964697298276));
#35350=CARTESIAN_POINT('Ctrl Pts',(27.8880124740053,-0.00437568075665919,
10.8945992424429));
#35351=CARTESIAN_POINT('Ctrl Pts',(27.9202693857805,-0.00437277336843283,
9.14103287468171));
#35352=CARTESIAN_POINT('Ctrl Pts',(27.942922372983,-0.00434869611805563,
7.63582414935623));
#35353=CARTESIAN_POINT('Ctrl Pts',(27.9529816133133,-0.0043349081756363,
6.50489909332326));
#35354=CARTESIAN_POINT('Ctrl Pts',(27.9550904561317,-0.00431925130350027,
6.25451764743701));
#35355=CARTESIAN_POINT('Ctrl Pts',(27.9588519820389,-0.00424701392688201,
5.75323897220658));
#35356=CARTESIAN_POINT('Ctrl Pts',(27.9642492028057,-0.00403750286507426,
4.87463059887487));
#35357=CARTESIAN_POINT('Ctrl Pts',(27.9703983457841,-0.00348262153394864,
3.11451716859049));
#35358=CARTESIAN_POINT('Ctrl Pts',(27.9680330925388,-0.00344023067093111,
1.60884636308336));
#35359=CARTESIAN_POINT('Ctrl Pts',(27.9630586530823,-0.00424528887266004,
0.550558997922009));
#35360=CARTESIAN_POINT('Ctrl Pts',(27.9624086450966,-0.0043499597142107,
0.424586029884561));
#35361=CARTESIAN_POINT('Ctrl Pts',(27.9608907300847,-0.00459286025227315,
0.172776845081321));
#35362=CARTESIAN_POINT('Ctrl Pts',(27.957692878994,-0.00510026698762377,
-0.267430351903845));
#35363=CARTESIAN_POINT('Ctrl Pts',(27.9517513083943,-0.00602934778227967,
-0.895200587868783));
#35364=CARTESIAN_POINT('Ctrl Pts',(27.9429819494069,-0.00736901072906046,
-1.64721018097085));
#35365=CARTESIAN_POINT('Ctrl Pts',(27.9298477572099,-0.00931740432985499,
-2.64876001923851));
#35366=CARTESIAN_POINT('Ctrl Pts',(27.9121217457491,-0.0117945338553188,
-3.89973019267382));
#35367=CARTESIAN_POINT('Ctrl Pts',(27.8995090785445,-0.0132557468094068,
-4.9019715887432));
#35368=CARTESIAN_POINT('Ctrl Pts',(27.8930349152043,-0.0138297519450205,
-5.52964563288159));
#35369=CARTESIAN_POINT('Ctrl Pts',(27.8904180812731,-0.0140601142080389,
-5.780437898808));
#35370=CARTESIAN_POINT('Ctrl Pts',(27.8851124581628,-0.0145173344259218,
-6.28262787103353));
#35371=CARTESIAN_POINT('Ctrl Pts',(27.875725454074,-0.0152837624433052,
-7.16201194286542));
#35372=CARTESIAN_POINT('Ctrl Pts',(27.8625139385489,-0.0161506201033615,
-8.41929816585113));
#35373=CARTESIAN_POINT('Ctrl Pts',(27.8508862565949,-0.0163576458403922,
-9.67501482097612));
#35374=CARTESIAN_POINT('Ctrl Pts',(27.8442716872927,-0.0159714395871801,
-10.5517788288946));
#35375=CARTESIAN_POINT('Ctrl Pts',(27.8410266987454,-0.0155721145169628,
-11.0519335897028));
#35376=CARTESIAN_POINT('Ctrl Pts',(27.8395988846676,-0.0153087597685989,
-11.3016901654378));
#35377=CARTESIAN_POINT('Ctrl Pts',(27.8386031475785,-0.0150845863514239,
-11.4896701473081));
#35378=CARTESIAN_POINT('Ctrl Pts',(27.837967769797,-0.014912003675546,-11.6163073222506));
#35379=CARTESIAN_POINT('Ctrl Pts',(27.8368262603536,-0.0144846864311702,
-11.8690358141286));
#35380=CARTESIAN_POINT('Ctrl Pts',(27.8351498853946,-0.0135375479306688,
-12.3105590020318));
#35381=CARTESIAN_POINT('Ctrl Pts',(27.8323064470357,-0.0102443343565817,
-13.4419288100555));
#35382=CARTESIAN_POINT('Ctrl Pts',(27.8324069463981,-0.00499426391876198,
-14.6904514807044));
#35383=CARTESIAN_POINT('Ctrl Pts',(27.8324832190777,-0.00107387732498213,
-15.9392029541057));
#35384=CARTESIAN_POINT('Ctrl Pts',(27.8322371672579,0.000304516178078215,
-16.5644082550696));
#35385=CARTESIAN_POINT('Ctrl Pts',(27.8317057618377,0.000906063691328227,
-17.0655127643589));
#35386=CARTESIAN_POINT('Ctrl Pts',(27.8312997053129,0.00101604259468865,
-17.3164424452256));
#35387=CARTESIAN_POINT('Ctrl Pts',(27.8309339665234,0.00101659999667262,
-17.5040710809957));
#35388=CARTESIAN_POINT('Ctrl Pts',(27.8307228356329,0.00104583334236606,
-17.6294604138463));
#35389=CARTESIAN_POINT('Ctrl Pts',(27.830410768655,0.00118037429640018,
-17.8793920992222));
#35390=CARTESIAN_POINT('Ctrl Pts',(27.8302444974371,0.00141827279767814,
-18.1295378971104));
#35391=CARTESIAN_POINT('Ctrl Pts',(27.8301871488947,0.00171258365097112,
-18.3794552586451));
#35392=CARTESIAN_POINT('Ctrl Pts',(27.8301887369512,0.00191364338468692,
-18.5356582031945));
#35393=CARTESIAN_POINT('Ctrl Pts',(27.8302079147249,0.0020789458745374,
-18.6605904464526));
#35394=CARTESIAN_POINT('Ctrl Pts',(27.8302373476539,0.00224571909714837,
-18.7855154584377));
#35395=CARTESIAN_POINT('Ctrl Pts',(27.8303558545768,0.00270723948490729,
-19.1290061737529));
#35396=CARTESIAN_POINT('Ctrl Pts',(27.8306773007071,0.00338746134337307,
-19.6908470469758));
#35397=CARTESIAN_POINT('Ctrl Pts',(27.8308588116303,0.00358852653968433,
-20.6890802452549));
#35398=CARTESIAN_POINT('Ctrl Pts',(27.8288808501303,0.000456470933084654,
-21.9360876156402));
#35399=CARTESIAN_POINT('Ctrl Pts',(27.821832683648,-0.00854233090364024,
-22.9332360638372));
#35400=CARTESIAN_POINT('Ctrl Pts',(27.8146537172427,-0.0170501805523391,
-23.5546173623963));
#35401=CARTESIAN_POINT('Ctrl Pts',(27.8113777751593,-0.0208561464693165,
-23.7986271585001));
#35402=CARTESIAN_POINT('Ctrl Pts',(27.8033019918199,-0.0300516119524009,
-24.2899600801057));
#35403=CARTESIAN_POINT('Ctrl Pts',(27.7857542022908,-0.0496849425336436,
-25.1542089073046));
#35404=CARTESIAN_POINT('Ctrl Pts',(27.7543748471676,-0.0845146120712593,
-26.4023025252781));
#35405=CARTESIAN_POINT('Ctrl Pts',(27.7174388846653,-0.126663579853726,
-27.9166945666629));
#35406=CARTESIAN_POINT('Ctrl Pts',(27.7004166352905,-0.148482904650703,
-28.9349257067696));
#35407=CARTESIAN_POINT('Ctrl Pts',(27.6948542233149,-0.157190087608495,
-29.5092422475926));
#35408=CARTESIAN_POINT('Ctrl Pts',(27.6936345431008,-0.159080801738769,
-29.6346285463885));
#35409=CARTESIAN_POINT('Ctrl Pts',(27.691264706659,-0.162783190872688,-29.8867589803176));
#35410=CARTESIAN_POINT('Ctrl Pts',(27.6873298225248,-0.16901547033627,-30.3275681171679));
#35411=CARTESIAN_POINT('Ctrl Pts',(27.680482994079,-0.180454499214935,-31.2104816765876));
#35412=CARTESIAN_POINT('Ctrl Pts',(27.6758378390379,-0.190954387007905,
-32.2204659203817));
#35413=CARTESIAN_POINT('Ctrl Pts',(27.6760328730208,-0.198361068611184,
-33.2308349292764));
#35414=CARTESIAN_POINT('Ctrl Pts',(27.6790154457573,-0.202235372088996,
-33.9884291090496));
#35415=CARTESIAN_POINT('Ctrl Pts',(27.6852693481341,-0.204317459123181,
-34.745514565451));
#35416=CARTESIAN_POINT('Ctrl Pts',(27.6919010382722,-0.204407326281904,
-35.249717218533));
#35417=CARTESIAN_POINT('Ctrl Pts',(27.6979241250912,-0.203944476816674,
-35.6286417414824));
#35418=CARTESIAN_POINT('Ctrl Pts',(27.7024562249202,-0.203472746778721,
-35.8823404494921));
#35419=CARTESIAN_POINT('Ctrl Pts',(27.7133274010445,-0.201882737834755,
-36.3889814167889));
#35420=CARTESIAN_POINT('Ctrl Pts',(27.7366196682698,-0.197448353427203,
-37.2735023505669));
#35421=CARTESIAN_POINT('Ctrl Pts',(27.7965248219601,-0.181978851313276,
-39.0372131646583));
#35422=CARTESIAN_POINT('Ctrl Pts',(27.8577782633427,-0.157797010592176,
-40.545514585732));
#35423=CARTESIAN_POINT('Ctrl Pts',(27.8956018334961,-0.134531942823141,
-41.6810303600698));
#35424=CARTESIAN_POINT('Ctrl Pts',(27.903761259723,-0.130667056236929,-41.9171031268057));
#35425=CARTESIAN_POINT('Ctrl Pts',(27.9156475993859,-0.126965301462498,
-42.2829138338868));
#35426=CARTESIAN_POINT('Ctrl Pts',(27.9272547782387,-0.124974790747706,
-42.6499725926779));
#35427=CARTESIAN_POINT('Ctrl Pts',(27.9425023899414,-0.123664606083567,
-43.1461020545497));
#35428=CARTESIAN_POINT('Ctrl Pts',(27.9613809979822,-0.123027792205116,
-43.7753169177318));
#35429=CARTESIAN_POINT('Ctrl Pts',(27.9845771199602,-0.118435365113253,
-44.545694783705));
#35430=CARTESIAN_POINT('Ctrl Pts',(28.0050528544863,-0.106634821138297,
-45.1995497251918));
#35431=CARTESIAN_POINT('Ctrl Pts',(28.0225406446347,-0.0893354422462611,
-45.729822479714));
#35432=CARTESIAN_POINT('Ctrl Pts',(28.0362989127611,-0.0716272099567747,
-46.1309291427025));
#35433=CARTESIAN_POINT('Ctrl Pts',(28.0507914761749,-0.0483595244083412,
-46.5354140463417));
#35434=CARTESIAN_POINT('Ctrl Pts',(28.0712128334668,-0.00879431783632524,
-47.0790793048288));
#35435=CARTESIAN_POINT('Ctrl Pts',(28.0878498794627,0.0318081545271698,
-47.4915893744711));
#35436=CARTESIAN_POINT('Ctrl Pts',(28.1055592638943,0.0815659363833794,
-47.9077561120951));
#35437=CARTESIAN_POINT('Ctrl Pts',(28.1188418354446,0.115297825002333,-48.1753761014028));
#35438=CARTESIAN_POINT('Ctrl Pts',(28.1493598687048,0.191566326899808,-48.7149396128666));
#35439=CARTESIAN_POINT('Ctrl Pts',(28.2113220874215,0.344705652707654,-49.6511595987853));
#35440=CARTESIAN_POINT('Ctrl Pts',(28.3112761493627,0.617893217392755,-50.9746068171927));
#35441=CARTESIAN_POINT('Ctrl Pts',(28.4097812738316,1.00886628162702,-52.5319378166776));
#35442=CARTESIAN_POINT('Ctrl Pts',(28.4390786440405,1.28767941036866,-53.552314578807));
#35443=CARTESIAN_POINT('Ctrl Pts',(28.4403749025846,1.46043255501218,-54.187964888863));
#35444=CARTESIAN_POINT('Ctrl Pts',(28.4389318054096,1.53300109764453,-54.4528958189231));
#35445=CARTESIAN_POINT('Ctrl Pts',(28.4312020513412,1.68004052263621,-54.9775443276195));
#35446=CARTESIAN_POINT('Ctrl Pts',(28.4053868143613,1.94588833285434,-55.8966092099976));
#35447=CARTESIAN_POINT('Ctrl Pts',(28.3162447976202,2.50764073843331,-57.7248393212858));
#35448=CARTESIAN_POINT('Ctrl Pts',(28.2091691509567,3.04002742409168,-59.2686626610434));
#35449=CARTESIAN_POINT('Ctrl Pts',(28.1493298592453,3.43444480648254,-60.3423774514013));
#35450=CARTESIAN_POINT('Ctrl Pts',(28.1416132495178,3.48323051822477,-60.4752311183287));
#35451=CARTESIAN_POINT('Ctrl Pts',(28.1255647390676,3.58128135589683,-60.7394082384028));
#35452=CARTESIAN_POINT('Ctrl Pts',(28.0955889856453,3.75532904521311,-61.2019343267608));
#35453=CARTESIAN_POINT('Ctrl Pts',(28.0296287411644,4.11229247223529,-62.1238604209113));
#35454=CARTESIAN_POINT('Ctrl Pts',(27.9461522198004,4.54104063594089,-63.1688325671928));
#35455=CARTESIAN_POINT('Ctrl Pts',(27.8669587469973,4.98745796642251,-64.1991496102626));
#35456=CARTESIAN_POINT('Ctrl Pts',(27.826380770832,5.24407774535702,-64.7725770283981));
#35457=CARTESIAN_POINT('Ctrl Pts',(27.8019337923344,5.41695386520446,-65.1520284576054));
#35458=CARTESIAN_POINT('Ctrl Pts',(27.7863902342801,5.53263278391158,-65.4042259418254));
#35459=CARTESIAN_POINT('Ctrl Pts',(27.7720769394183,5.64893176063813,-65.6552881250302));
#35460=CARTESIAN_POINT('Ctrl Pts',(27.7607817580091,5.75109744567071,-65.8738983477784));
#35461=CARTESIAN_POINT('Ctrl Pts',(27.7547015495567,5.80958162100798,-65.9985129337661));
#35462=CARTESIAN_POINT('Ctrl Pts',(27.7459661258242,5.89740668233722,-66.1851344259272));
#35463=CARTESIAN_POINT('Ctrl Pts',(27.7395146314148,5.97078045415491,-66.3400046904007));
#35464=CARTESIAN_POINT('Ctrl Pts',(27.7300438427688,6.09251013412725,-66.59573563328));
#35465=CARTESIAN_POINT('Ctrl Pts',(27.7213616823757,6.22361047539017,-66.8678269235341));
#35466=CARTESIAN_POINT('Ctrl Pts',(27.7081078774019,6.48628712014753,-67.4006280009251));
#35467=CARTESIAN_POINT('Ctrl Pts',(27.6944680391957,6.95376801043905,-68.3208241954038));
#35468=CARTESIAN_POINT('Ctrl Pts',(27.6959663569651,7.90413467785139,-70.1072879225436));
#35469=CARTESIAN_POINT('Ctrl Pts',(27.7174181757263,8.71791680473499,-71.5789932925461));
#35470=CARTESIAN_POINT('Ctrl Pts',(27.7156266075869,9.30124239502026,-72.6817383151479));
#35471=CARTESIAN_POINT('Ctrl Pts',(27.7152842047099,9.4354274875904,-72.9352364610077));
#35472=CARTESIAN_POINT('Ctrl Pts',(27.7147734692249,9.70157307813676,-73.4374478690909));
#35473=CARTESIAN_POINT('Ctrl Pts',(27.7144402769229,10.0354711469673,-74.0665268595069));
#35474=CARTESIAN_POINT('Ctrl Pts',(27.7144063687065,10.4358528450057,-74.8196553989177));
#35475=CARTESIAN_POINT('Ctrl Pts',(27.7148556365495,11.2371667797637,-76.325264132285));
#35476=CARTESIAN_POINT('Ctrl Pts',(27.7158522161718,11.9048293991325,-77.5777501015528));
#35477=CARTESIAN_POINT('Ctrl Pts',(27.7158562496574,12.8737109173691,-79.3999540031939));
#35478=CARTESIAN_POINT('Ctrl Pts',(27.7158606407362,13.3106272082791,-80.2216754077889));
#35479=CARTESIAN_POINT('Ctrl Pts',(27.7158606407362,13.7471487956685,-81.0426531098874));
#35480=CARTESIAN_POINT('Ctrl Pts',(29.6002100937378,-0.00570612383640002,
24.8306405759807));
#35481=CARTESIAN_POINT('Ctrl Pts',(29.6002989001342,-0.00570624884174762,
24.78176144937));
#35482=CARTESIAN_POINT('Ctrl Pts',(29.6003920380491,-0.00570637939760055,
24.7328833808383));
#35483=CARTESIAN_POINT('Ctrl Pts',(29.6014919216698,-0.00570793470053486,
24.1822774476937));
#35484=CARTESIAN_POINT('Ctrl Pts',(29.6023342893883,-0.00571269138779538,
23.1781454826973));
#35485=CARTESIAN_POINT('Ctrl Pts',(29.6042940170815,-0.00572583877534936,
21.1695502348416));
#35486=CARTESIAN_POINT('Ctrl Pts',(29.6116140134114,-0.00573620328390793,
19.6653954329726));
#35487=CARTESIAN_POINT('Ctrl Pts',(29.6271419186231,-0.00574044368796074,
18.414344917972));
#35488=CARTESIAN_POINT('Ctrl Pts',(29.6345892733583,-0.00574358245359698,
17.9115396664595));
#35489=CARTESIAN_POINT('Ctrl Pts',(29.6532908087813,-0.00575338624565161,
16.9075582711688));
#35490=CARTESIAN_POINT('Ctrl Pts',(29.6934046812983,-0.00577316241557398,
15.1537490041529));
#35491=CARTESIAN_POINT('Ctrl Pts',(29.7315107250221,-0.00577400371802316,
13.6519691858614));
#35492=CARTESIAN_POINT('Ctrl Pts',(29.7553945730525,-0.005741119949668,
12.3974430625798));
#35493=CARTESIAN_POINT('Ctrl Pts',(29.7651585260561,-0.00572368866968957,
11.896467784163));
#35494=CARTESIAN_POINT('Ctrl Pts',(29.7850637534519,-0.00567597881962372,
10.8945934236694));
#35495=CARTESIAN_POINT('Ctrl Pts',(29.8195144423163,-0.00556760762166768,
9.14102402407729));
#35496=CARTESIAN_POINT('Ctrl Pts',(29.8436795735494,-0.00546919741555448,
7.63581886876459));
#35497=CARTESIAN_POINT('Ctrl Pts',(29.8544057770259,-0.00542299840893521,
6.50490484182837));
#35498=CARTESIAN_POINT('Ctrl Pts',(29.8566388765318,-0.00540546234814099,
6.25458913080819));
#35499=CARTESIAN_POINT('Ctrl Pts',(29.8605682245575,-0.00534762537235711,
5.75338201666123));
#35500=CARTESIAN_POINT('Ctrl Pts',(29.8660787804742,-0.00520160560400977,
4.87486360767608));
#35501=CARTESIAN_POINT('Ctrl Pts',(29.8719697289,-0.00483948820640255,3.11469817291051));
#35502=CARTESIAN_POINT('Ctrl Pts',(29.869397961577,-0.0048114235087629,
1.60862425262526));
#35503=CARTESIAN_POINT('Ctrl Pts',(29.8650606763383,-0.00528875922251774,
0.549858267814596));
#35504=CARTESIAN_POINT('Ctrl Pts',(29.8644924991081,-0.00535056658702854,
0.423799297997487));
#35505=CARTESIAN_POINT('Ctrl Pts',(29.8631629038045,-0.00549418155172073,
0.171845739387263));
#35506=CARTESIAN_POINT('Ctrl Pts',(29.8603537126289,-0.00579390989457697,
-0.268597214816478));
#35507=CARTESIAN_POINT('Ctrl Pts',(29.8551149833809,-0.00634414333367143,
-0.896625607696168));
#35508=CARTESIAN_POINT('Ctrl Pts',(29.8473318446249,-0.00713040017255807,
-1.64883440985916));
#35509=CARTESIAN_POINT('Ctrl Pts',(29.835605595992,-0.00827613585702751,
-2.65049840535369));
#35510=CARTESIAN_POINT('Ctrl Pts',(29.8195877687245,-0.00972986558144148,
-3.90132680824059));
#35511=CARTESIAN_POINT('Ctrl Pts',(29.8078771861049,-0.0106079211921739,
-4.9031065281976));
#35512=CARTESIAN_POINT('Ctrl Pts',(29.8016893369936,-0.010963391753219,
-5.53037655675497));
#35513=CARTESIAN_POINT('Ctrl Pts',(29.7991956095894,-0.0111189600917785,
-5.78105177583071));
#35514=CARTESIAN_POINT('Ctrl Pts',(29.7941598437616,-0.0114712860324365,
-6.28301816895253));
#35515=CARTESIAN_POINT('Ctrl Pts',(29.7852703682728,-0.012158172617904,
-7.16210355326741));
#35516=CARTESIAN_POINT('Ctrl Pts',(29.7726228250825,-0.0131147854172198,
-8.41918825799379));
#35517=CARTESIAN_POINT('Ctrl Pts',(29.7607845675514,-0.0134483008526966,
-9.67500973180304));
#35518=CARTESIAN_POINT('Ctrl Pts',(29.7533079155556,-0.0130400411815235,
-10.5520040880199));
#35519=CARTESIAN_POINT('Ctrl Pts',(29.7493231299057,-0.01257931399796,-11.052338128805));
#35520=CARTESIAN_POINT('Ctrl Pts',(29.7474353170481,-0.0122651127567208,
-11.3021987660583));
#35521=CARTESIAN_POINT('Ctrl Pts',(29.7460566259942,-0.0119943543122567,
-11.4902662304204));
#35522=CARTESIAN_POINT('Ctrl Pts',(29.7451348168513,-0.0117821177244601,
-11.6170598970885));
#35523=CARTESIAN_POINT('Ctrl Pts',(29.7433122662121,-0.0112517730943604,
-11.8700207133685));
#35524=CARTESIAN_POINT('Ctrl Pts',(29.7401807944409,-0.0100653661808592,
-12.311918431288));
#35525=CARTESIAN_POINT('Ctrl Pts',(29.7324582218323,-0.00590550545204358,
-13.4439117837114));
#35526=CARTESIAN_POINT('Ctrl Pts',(29.7250466443676,0.000623289411662867,
-14.6921479165137));
#35527=CARTESIAN_POINT('Ctrl Pts',(29.7194556385609,0.00502339709455761,
-15.9396896263156));
#35528=CARTESIAN_POINT('Ctrl Pts',(29.7171528919325,0.00638833162455389,
-16.5640736481404));
#35529=CARTESIAN_POINT('Ctrl Pts',(29.7156637887129,0.00676695964046818,
-17.0644084781654));
#35530=CARTESIAN_POINT('Ctrl Pts',(29.7150340955089,0.00669424293120357,
-17.3149143689853));
#35531=CARTESIAN_POINT('Ctrl Pts',(29.7146138519149,0.00652709518728442,
-17.5022173432018));
#35532=CARTESIAN_POINT('Ctrl Pts',(29.7143264146382,0.00642164488428857,
-17.6274847142069));
#35533=CARTESIAN_POINT('Ctrl Pts',(29.7137256018092,0.00626720074023811,
-17.8771353260958));
#35534=CARTESIAN_POINT('Ctrl Pts',(29.7130842190378,0.00617674100949031,
-18.1270372465979));
#35535=CARTESIAN_POINT('Ctrl Pts',(29.7124460673569,0.00611433711372318,
-18.3767246179939));
#35536=CARTESIAN_POINT('Ctrl Pts',(29.712047395045,0.00608229662135253,
-18.5327935609526));
#35537=CARTESIAN_POINT('Ctrl Pts',(29.7117343091275,0.00605607845166938,
-18.6576230389906));
#35538=CARTESIAN_POINT('Ctrl Pts',(29.7114255053145,0.00602857561386291,
-18.782448723037));
#35539=CARTESIAN_POINT('Ctrl Pts',(29.7105856794882,0.00594243490906421,
-19.1256744595573));
#35540=CARTESIAN_POINT('Ctrl Pts',(29.7093569756374,0.00568593401260037,
-19.6871396016039));
#35541=CARTESIAN_POINT('Ctrl Pts',(29.7080087336263,0.00417192491291634,
-20.6847928678057));
#35542=CARTESIAN_POINT('Ctrl Pts',(29.7087982191887,-0.00112163915555453,
-21.9310851831672));
#35543=CARTESIAN_POINT('Ctrl Pts',(29.7139850254477,-0.0122670608579555,
-22.9276090155673));
#35544=CARTESIAN_POINT('Ctrl Pts',(29.7194119080898,-0.0224053888038508,
-23.548634519785));
#35545=CARTESIAN_POINT('Ctrl Pts',(29.7217664646152,-0.0269248482588539,
-23.7911111990818));
#35546=CARTESIAN_POINT('Ctrl Pts',(29.7272503068371,-0.0380593889693665,
-24.2806287192842));
#35547=CARTESIAN_POINT('Ctrl Pts',(29.7387592909759,-0.062226793790845,
-25.1423683057187));
#35548=CARTESIAN_POINT('Ctrl Pts',(29.7596607464096,-0.105749834326537,
-26.3902395876224));
#35549=CARTESIAN_POINT('Ctrl Pts',(29.7890543841874,-0.158476650180068,
-27.9092333040972));
#35550=CARTESIAN_POINT('Ctrl Pts',(29.8093101555645,-0.183628753409201,
-28.9340113861485));
#35551=CARTESIAN_POINT('Ctrl Pts',(29.8204946969917,-0.192072165295886,
-29.5129698492737));
#35552=CARTESIAN_POINT('Ctrl Pts',(29.8229722322911,-0.193866686645311,
-29.6384331626403));
#35553=CARTESIAN_POINT('Ctrl Pts',(29.8278919393808,-0.197330745845292,
-29.8913006822493));
#35554=CARTESIAN_POINT('Ctrl Pts',(29.8364146617225,-0.202940840499442,
-30.3332238844636));
#35555=CARTESIAN_POINT('Ctrl Pts',(29.8533485531302,-0.212312140634371,
-31.2189730912166));
#35556=CARTESIAN_POINT('Ctrl Pts',(29.873222181893,-0.217983824509602,-32.2329556173296));
#35557=CARTESIAN_POINT('Ctrl Pts',(29.8954103194336,-0.217222257306601,
-33.2482347387287));
#35558=CARTESIAN_POINT('Ctrl Pts',(29.9136435426566,-0.213057285220415,
-34.0099224273251));
#35559=CARTESIAN_POINT('Ctrl Pts',(29.9338055008375,-0.204823505354437,
-34.7715069329928));
#35560=CARTESIAN_POINT('Ctrl Pts',(29.9488407513319,-0.196378497002392,
-35.2789820981113));
#35561=CARTESIAN_POINT('Ctrl Pts',(29.9608608438713,-0.188819591402007,
-35.6604624402291));
#35562=CARTESIAN_POINT('Ctrl Pts',(29.9692936010343,-0.18335102815823,-35.915679061952));
#35563=CARTESIAN_POINT('Ctrl Pts',(29.9874908722616,-0.170850653216882,
-36.4253425766179));
#35564=CARTESIAN_POINT('Ctrl Pts',(30.0223072141217,-0.144947484904871,
-37.3148844095339));
#35565=CARTESIAN_POINT('Ctrl Pts',(30.100325464607,-0.0782827314807047,
-39.0876043893815));
#35566=CARTESIAN_POINT('Ctrl Pts',(30.1687343584942,0.000719127292588034,
-40.6023724685504));
#35567=CARTESIAN_POINT('Ctrl Pts',(30.2080583406784,0.0666362462407528,
-41.7418518157352));
#35568=CARTESIAN_POINT('Ctrl Pts',(30.2167140524775,0.0793717304027045,
-41.9777259748089));
#35569=CARTESIAN_POINT('Ctrl Pts',(30.2292099403697,0.0967553830352084,
-42.3441373781403));
#35570=CARTESIAN_POINT('Ctrl Pts',(30.2413254660434,0.112512992435887,-42.7119145187934));
#35571=CARTESIAN_POINT('Ctrl Pts',(30.2569693086651,0.132565735837706,-43.2095398905444));
#35572=CARTESIAN_POINT('Ctrl Pts',(30.2756372878933,0.157432667124367,-43.8413320000696));
#35573=CARTESIAN_POINT('Ctrl Pts',(30.2967247796072,0.193037461349602,-44.6159223094752));
#35574=CARTESIAN_POINT('Ctrl Pts',(30.3132192490903,0.232789029516669,-45.2740518150012));
#35575=CARTESIAN_POINT('Ctrl Pts',(30.3256359826119,0.274056483815724,-45.8079455044184));
#35576=CARTESIAN_POINT('Ctrl Pts',(30.3345612437144,0.310583052433669,-46.2118950495979));
#35577=CARTESIAN_POINT('Ctrl Pts',(30.3430579940097,0.353569674361366,-46.6192737502179));
#35578=CARTESIAN_POINT('Ctrl Pts',(30.353711866588,0.420723951037079,-47.1668036671869));
#35579=CARTESIAN_POINT('Ctrl Pts',(30.3609668156114,0.483431121928524,-47.5821347560762));
#35580=CARTESIAN_POINT('Ctrl Pts',(30.3674690616424,0.556484599912766,-48.0012328869044));
#35581=CARTESIAN_POINT('Ctrl Pts',(30.3723163449793,0.60922824910479,-48.2828209099944));
#35582=CARTESIAN_POINT('Ctrl Pts',(30.3833730441837,0.726570719937063,-48.8378186704525));
#35583=CARTESIAN_POINT('Ctrl Pts',(30.4050881001414,0.959498388023445,-49.7922951178013));
#35584=CARTESIAN_POINT('Ctrl Pts',(30.4360609436282,1.34705064834406,-51.1074078461644));
#35585=CARTESIAN_POINT('Ctrl Pts',(30.4569223855284,1.82982481176224,-52.6165998976898));
#35586=CARTESIAN_POINT('Ctrl Pts',(30.4525459065398,2.11955233242534,-53.5805979983041));
#35587=CARTESIAN_POINT('Ctrl Pts',(30.4403000101703,2.27815765531267,-54.1716093252403));
#35588=CARTESIAN_POINT('Ctrl Pts',(30.432735890706,2.34416941058513,-54.4230251518103));
#35589=CARTESIAN_POINT('Ctrl Pts',(30.4136112348139,2.47157031309743,-54.9216083177821));
#35590=CARTESIAN_POINT('Ctrl Pts',(30.3684069581331,2.68928140342694,-55.8039465899849));
#35591=CARTESIAN_POINT('Ctrl Pts',(30.2415291238702,3.11258624593874,-57.5867140656665));
#35592=CARTESIAN_POINT('Ctrl Pts',(30.1002208360485,3.50765107649709,-59.1391076348399));
#35593=CARTESIAN_POINT('Ctrl Pts',(30.0251249611869,3.84005238168457,-60.2381524787919));
#35594=CARTESIAN_POINT('Ctrl Pts',(30.0163721182157,3.87864932191528,-60.3659328037547));
#35595=CARTESIAN_POINT('Ctrl Pts',(29.9981933064438,3.95727247694841,-60.6251189253043));
#35596=CARTESIAN_POINT('Ctrl Pts',(29.9655464703264,4.09550572043887,-61.0778962302091));
#35597=CARTESIAN_POINT('Ctrl Pts',(29.8971217556328,4.37816350489105,-61.9875267268624));
#35598=CARTESIAN_POINT('Ctrl Pts',(29.8160872524673,4.71961990354699,-63.0303865845481));
#35599=CARTESIAN_POINT('Ctrl Pts',(29.7413689014789,5.08847429459405,-64.0726429042806));
#35600=CARTESIAN_POINT('Ctrl Pts',(29.7035172061765,5.30736914621276,-64.6576470039614));
#35601=CARTESIAN_POINT('Ctrl Pts',(29.680707169744,5.45856492187508,-65.0468473336499));
#35602=CARTESIAN_POINT('Ctrl Pts',(29.6661934302272,5.56078387914126,-65.3060644005528));
#35603=CARTESIAN_POINT('Ctrl Pts',(29.6527755459062,5.66520903499327,-65.5649233293135));
#35604=CARTESIAN_POINT('Ctrl Pts',(29.6421101614254,5.75856118215573,-65.7910134859799));
#35605=CARTESIAN_POINT('Ctrl Pts',(29.6363364245003,5.81248486888892,-65.9200874000455));
#35606=CARTESIAN_POINT('Ctrl Pts',(29.6280041870977,5.89395736346093,-66.113579136086));
#35607=CARTESIAN_POINT('Ctrl Pts',(29.6217565785856,5.96308461558392,-66.2745581212124));
#35608=CARTESIAN_POINT('Ctrl Pts',(29.612413901581,6.0792941599492,-66.5408461079343));
#35609=CARTESIAN_POINT('Ctrl Pts',(29.6038932231889,6.20472440432365,-66.8215903272585));
#35610=CARTESIAN_POINT('Ctrl Pts',(29.5910146048047,6.46050135730378,-67.3706075763046));
#35611=CARTESIAN_POINT('Ctrl Pts',(29.5780658698442,6.92422326566066,-68.3135400697311));
#35612=CARTESIAN_POINT('Ctrl Pts',(29.5803465546603,7.89115824189205,-70.1267298299807));
#35613=CARTESIAN_POINT('Ctrl Pts',(29.6013021167182,8.72542547986538,-71.5935063992352));
#35614=CARTESIAN_POINT('Ctrl Pts',(29.5997390704358,9.2976740218444,-72.6785697945003));
#35615=CARTESIAN_POINT('Ctrl Pts',(29.5994345993365,9.4323604289187,-72.9336723885517));
#35616=CARTESIAN_POINT('Ctrl Pts',(29.5989838213741,9.69797488227456,-73.435839448843));
#35617=CARTESIAN_POINT('Ctrl Pts',(29.5986845091741,10.0321181096191,-74.0660328586202));
#35618=CARTESIAN_POINT('Ctrl Pts',(29.5986520948479,10.4326930518429,-74.819598742444));
#35619=CARTESIAN_POINT('Ctrl Pts',(29.5990423700363,11.2349229683723,-76.3261145564624));
#35620=CARTESIAN_POINT('Ctrl Pts',(29.5999052687731,11.9034263089648,-77.5783970633848));
#35621=CARTESIAN_POINT('Ctrl Pts',(29.5999024700786,12.8717351076972,-79.3995546363377));
#35622=CARTESIAN_POINT('Ctrl Pts',(29.5999011496128,13.3088569590276,-80.2216783074562));
#35623=CARTESIAN_POINT('Ctrl Pts',(29.5999011496129,13.745378546417,-81.0426560095546));
#35624=CARTESIAN_POINT('Ctrl Pts',(31.0171866232326,-0.00299204424446314,
24.8306373191774));
#35625=CARTESIAN_POINT('Ctrl Pts',(31.0172800374408,-0.00299175195389374,
24.7817580900798));
#35626=CARTESIAN_POINT('Ctrl Pts',(31.0173780076597,-0.00299144622876444,
24.7328799158363));
#35627=CARTESIAN_POINT('Ctrl Pts',(31.0185349571666,-0.00298779232615199,
24.1822728181405));
#35628=CARTESIAN_POINT('Ctrl Pts',(31.0194242644657,-0.00298701896593174,
23.1781407180979));
#35629=CARTESIAN_POINT('Ctrl Pts',(31.0214952096736,-0.0029872921198035,
21.169542798472));
#35630=CARTESIAN_POINT('Ctrl Pts',(31.029194999137,-0.00296246222206313,
19.6653857519563));
#35631=CARTESIAN_POINT('Ctrl Pts',(31.0455122304153,-0.00289957867720278,
18.4143334371842));
#35632=CARTESIAN_POINT('Ctrl Pts',(31.0533392075379,-0.00286986433034777,
17.9115212109908));
#35633=CARTESIAN_POINT('Ctrl Pts',(31.0729958361359,-0.0027956849546429,
16.907535608882));
#35634=CARTESIAN_POINT('Ctrl Pts',(31.1151570483659,-0.00263552471530198,
15.1537304867153));
#35635=CARTESIAN_POINT('Ctrl Pts',(31.1551908943919,-0.00247432632475043,
13.6519762098179));
#35636=CARTESIAN_POINT('Ctrl Pts',(31.1802515164793,-0.00235944594013484,
12.3974782675912));
#35637=CARTESIAN_POINT('Ctrl Pts',(31.1904926330016,-0.00231080546792335,
11.8965147288727));
#35638=CARTESIAN_POINT('Ctrl Pts',(31.2113586077952,-0.00220612306289779,
10.8946572774833));
#35639=CARTESIAN_POINT('Ctrl Pts',(31.2474478081631,-0.00201365744969911,
9.14110480766528));
#35640=CARTESIAN_POINT('Ctrl Pts',(31.2727401436192,-0.00186903671229844,
7.63588960317416));
#35641=CARTESIAN_POINT('Ctrl Pts',(31.2839672924156,-0.00180566320929945,
6.50496387401208));
#35642=CARTESIAN_POINT('Ctrl Pts',(31.2862988414548,-0.00179111271627116,
6.25472622040602));
#35643=CARTESIAN_POINT('Ctrl Pts',(31.2903812975918,-0.00176082906178743,
5.75360134193579));
#35644=CARTESIAN_POINT('Ctrl Pts',(31.2960570243148,-0.00170698473366819,
4.87518683510538));
#35645=CARTESIAN_POINT('Ctrl Pts',(31.301972124276,-0.00161246329748242,
3.11495098143548));
#35646=CARTESIAN_POINT('Ctrl Pts',(31.2992403549997,-0.00161384079096441,
1.60838932949574));
#35647=CARTESIAN_POINT('Ctrl Pts',(31.2950393056685,-0.00170936156091001,
0.549047151704652));
#35648=CARTESIAN_POINT('Ctrl Pts',(31.2944887558957,-0.00172172143893924,
0.422887489995395));
#35649=CARTESIAN_POINT('Ctrl Pts',(31.2931984938341,-0.00175049760823538,
0.170763124126403));
#35650=CARTESIAN_POINT('Ctrl Pts',(31.2904683982893,-0.00181071082727286,
-0.269959669295347));
#35651=CARTESIAN_POINT('Ctrl Pts',(31.2853649746126,-0.00192254888288488,
-0.898298554812866));
#35652=CARTESIAN_POINT('Ctrl Pts',(31.2777684919425,-0.00208464034506392,
-1.65074301382481));
#35653=CARTESIAN_POINT('Ctrl Pts',(31.2662973694254,-0.0023259096128296,
-2.65253152566603));
#35654=CARTESIAN_POINT('Ctrl Pts',(31.2505760830858,-0.0026417561311629,
-3.90315870134114));
#35655=CARTESIAN_POINT('Ctrl Pts',(31.2389823001759,-0.00285192107937762,
-4.90440181540127));
#35656=CARTESIAN_POINT('Ctrl Pts',(31.2327966858658,-0.00295087232972535,
-5.53123792318891));
#35657=CARTESIAN_POINT('Ctrl Pts',(31.2303236229937,-0.00299944518517874,
-5.78202002293138));
#35658=CARTESIAN_POINT('Ctrl Pts',(31.225391374235,-0.00312588674535756,
-6.28399733300269));
#35659=CARTESIAN_POINT('Ctrl Pts',(31.2167989280666,-0.00340425233937084,
-7.16308358740321));
#35660=CARTESIAN_POINT('Ctrl Pts',(31.2046634006741,-0.00385283489059006,
-8.41981571843076));
#35661=CARTESIAN_POINT('Ctrl Pts',(31.192760038336,-0.00407574900706089,
-9.67490155539903));
#35662=CARTESIAN_POINT('Ctrl Pts',(31.184576129495,-0.003962792679451,-10.5511513249466));
#35663=CARTESIAN_POINT('Ctrl Pts',(31.1799452252549,-0.00379956597116409,
-11.0509969797361));
#35664=CARTESIAN_POINT('Ctrl Pts',(31.1776468697959,-0.00368176937487282,
-11.3005933523199));
#35665=CARTESIAN_POINT('Ctrl Pts',(31.1759217329085,-0.00357798355857695,
-11.4884477295729));
#35666=CARTESIAN_POINT('Ctrl Pts',(31.1747307640991,-0.00349601556723211,
-11.6148890942837));
#35667=CARTESIAN_POINT('Ctrl Pts',(31.1722364279941,-0.00327958682477642,
-11.8673074536642));
#35668=CARTESIAN_POINT('Ctrl Pts',(31.1676106338369,-0.00277616568156974,
-12.3083010607177));
#35669=CARTESIAN_POINT('Ctrl Pts',(31.1547118667396,-0.000960816288891971,
-13.4385717099228));
#35670=CARTESIAN_POINT('Ctrl Pts',(31.1393834657479,0.00201370407255788,
-14.6866895026391));
#35671=CARTESIAN_POINT('Ctrl Pts',(31.1288818117628,0.00396512956716421,
-15.9359205297263));
#35672=CARTESIAN_POINT('Ctrl Pts',(31.1253471619125,0.00449851534797558,
-16.5615504263016));
#35673=CARTESIAN_POINT('Ctrl Pts',(31.123813009011,0.00454494116123564,
-17.0631003642246));
#35674=CARTESIAN_POINT('Ctrl Pts',(31.1235321706078,0.00442294582556831,
-17.3142932229386));
#35675=CARTESIAN_POINT('Ctrl Pts',(31.1235178775408,0.00426874304661423,
-17.502099921976));
#35676=CARTESIAN_POINT('Ctrl Pts',(31.1234883913472,0.00418007425389375,
-17.6265784319385));
#35677=CARTESIAN_POINT('Ctrl Pts',(31.1233659176513,0.00395307306701036,
-17.8754407324593));
#35678=CARTESIAN_POINT('Ctrl Pts',(31.1231861318757,0.00367710873470516,
-18.1244853654518));
#35679=CARTESIAN_POINT('Ctrl Pts',(31.1229959777868,0.00332690480317081,
-18.3736241718446));
#35680=CARTESIAN_POINT('Ctrl Pts',(31.1228892610535,0.00308002734341012,
-18.5293970678065));
#35681=CARTESIAN_POINT('Ctrl Pts',(31.1228170511343,0.00286282586100117,
-18.6540461903583));
#35682=CARTESIAN_POINT('Ctrl Pts',(31.1227567187964,0.00263235993411028,
-18.7787192621887));
#35683=CARTESIAN_POINT('Ctrl Pts',(31.1226559341866,0.00195365178629543,
-19.1216563816462));
#35684=CARTESIAN_POINT('Ctrl Pts',(31.1229441836729,0.000533712239019911,
-19.68336488423));
#35685=CARTESIAN_POINT('Ctrl Pts',(31.1261109527912,-0.00285231282776662,
-20.6835784311914));
#35686=CARTESIAN_POINT('Ctrl Pts',(31.1377230351493,-0.00868577361617233,
-21.9374302792362));
#35687=CARTESIAN_POINT('Ctrl Pts',(31.1602385963435,-0.014065553654675,
-22.9445900629422));
#35688=CARTESIAN_POINT('Ctrl Pts',(31.1797508256719,-0.0172592242312334,
-23.5734793564911));
#35689=CARTESIAN_POINT('Ctrl Pts',(31.1882333981687,-0.0187590953521933,
-23.8193969122014));
#35690=CARTESIAN_POINT('Ctrl Pts',(31.2078655307222,-0.0224443650309819,
-24.314803704475));
#35691=CARTESIAN_POINT('Ctrl Pts',(31.2483979655463,-0.0301709904708716,
-25.1850798180763));
#35692=CARTESIAN_POINT('Ctrl Pts',(31.3192510621073,-0.0421576005802248,
-26.4397119259467));
#35693=CARTESIAN_POINT('Ctrl Pts',(31.4105442678541,-0.0490727090890887,
-27.958767976614));
#35694=CARTESIAN_POINT('Ctrl Pts',(31.4656991678369,-0.0437895376736689,
-28.9784359331697));
#35695=CARTESIAN_POINT('Ctrl Pts',(31.4920969623829,-0.036835621476926,
-29.5530483523592));
#35696=CARTESIAN_POINT('Ctrl Pts',(31.4979193479439,-0.0352906090957437,
-29.6784470123789));
#35697=CARTESIAN_POINT('Ctrl Pts',(31.5093943242123,-0.0320515077944978,
-29.9307145964565));
#35698=CARTESIAN_POINT('Ctrl Pts',(31.5290623113824,-0.026038521043076,
-30.3719366101199));
#35699=CARTESIAN_POINT('Ctrl Pts',(31.5668943942862,-0.0123207761499249,
-31.2564232518502));
#35700=CARTESIAN_POINT('Ctrl Pts',(31.6075126695474,0.00816049901412967,
-32.2698118697941));
#35701=CARTESIAN_POINT('Ctrl Pts',(31.6470161171525,0.0356857649896198,
-33.285012417737));
#35702=CARTESIAN_POINT('Ctrl Pts',(31.6764611302861,0.0604146604395156,
-34.0469117290958));
#35703=CARTESIAN_POINT('Ctrl Pts',(31.7061338079151,0.0897085824578493,
-34.8089853898741));
#35704=CARTESIAN_POINT('Ctrl Pts',(31.7263006112609,0.112683191082764,-35.316954376036));
#35705=CARTESIAN_POINT('Ctrl Pts',(31.7416977032748,0.131411147765765,-35.698841734656));
#35706=CARTESIAN_POINT('Ctrl Pts',(31.7522103743375,0.14440488890183,-35.9538749156084));
#35707=CARTESIAN_POINT('Ctrl Pts',(31.7738532824062,0.172180260359674,-36.4633985114814));
#35708=CARTESIAN_POINT('Ctrl Pts',(31.8129445351975,0.225103674084826,-37.3525870810542));
#35709=CARTESIAN_POINT('Ctrl Pts',(31.8926538715873,0.346789697405608,-39.1246789072447));
#35710=CARTESIAN_POINT('Ctrl Pts',(31.9522857829168,0.471316329837971,-40.6395337378253));
#35711=CARTESIAN_POINT('Ctrl Pts',(31.9818045876848,0.56827802006083,-41.7793140646381));
#35712=CARTESIAN_POINT('Ctrl Pts',(31.9885951174029,0.587669054701669,-42.0158666289406));
#35713=CARTESIAN_POINT('Ctrl Pts',(31.9980821327246,0.615086545272046,-42.3828188587321));
#35714=CARTESIAN_POINT('Ctrl Pts',(32.0071087518599,0.640791292565634,-42.7510825055653));
#35715=CARTESIAN_POINT('Ctrl Pts',(32.0183226475649,0.67403479725514,-43.249063143809));
#35716=CARTESIAN_POINT('Ctrl Pts',(32.0307682837515,0.715153783936835,-43.8808613990902));
#35717=CARTESIAN_POINT('Ctrl Pts',(32.042620373242,0.769682862548015,-44.6546381777675));
#35718=CARTESIAN_POINT('Ctrl Pts',(32.0494012967017,0.824467495919128,-45.3113909381642));
#35719=CARTESIAN_POINT('Ctrl Pts',(32.0526342092818,0.877055401355374,-45.843709339823));
#35720=CARTESIAN_POINT('Ctrl Pts',(32.0538325537096,0.921699636222757,-46.2462780366077));
#35721=CARTESIAN_POINT('Ctrl Pts',(32.0536974250961,0.972370016102763,-46.6520717026781));
#35722=CARTESIAN_POINT('Ctrl Pts',(32.051603455164,1.04907493013307,-47.197270800761));
#35723=CARTESIAN_POINT('Ctrl Pts',(32.0476327337414,1.11819982422158,-47.6105991423849));
#35724=CARTESIAN_POINT('Ctrl Pts',(32.0418554401568,1.19697063345933,-48.0278371428771));
#35725=CARTESIAN_POINT('Ctrl Pts',(32.0370093390979,1.2552571080079,-48.3153661676004));
#35726=CARTESIAN_POINT('Ctrl Pts',(32.0269492025836,1.38395180559172,-48.8756501702507));
#35727=CARTESIAN_POINT('Ctrl Pts',(32.0073796248885,1.63820497082836,-49.8362698327807));
#35728=CARTESIAN_POINT('Ctrl Pts',(31.9760030483103,2.05155110483119,-51.1465206922891));
#35729=CARTESIAN_POINT('Ctrl Pts',(31.9345223527777,2.54042952179378,-52.6333826654537));
#35730=CARTESIAN_POINT('Ctrl Pts',(31.9018911272374,2.80866824949851,-53.5658649239555));
#35731=CARTESIAN_POINT('Ctrl Pts',(31.8771846719511,2.94341900039249,-54.1295428104592));
#35732=CARTESIAN_POINT('Ctrl Pts',(31.8648175905742,2.99807320889389,-54.3697618998694));
#35733=CARTESIAN_POINT('Ctrl Pts',(31.8360856950958,3.09901795679906,-54.8483308358366));
#35734=CARTESIAN_POINT('Ctrl Pts',(31.7742711480597,3.26112727366891,-55.7010632445142));
#35735=CARTESIAN_POINT('Ctrl Pts',(31.6145810013345,3.54756645215416,-57.4480884546376));
#35736=CARTESIAN_POINT('Ctrl Pts',(31.4495654705191,3.82266725475589,-59.0165294959396));
#35737=CARTESIAN_POINT('Ctrl Pts',(31.367770953786,4.10638844852506,-60.1476588478776));
#35738=CARTESIAN_POINT('Ctrl Pts',(31.3585136584601,4.13772508255956,-60.2730723916295));
#35739=CARTESIAN_POINT('Ctrl Pts',(31.3397740472031,4.20257802447826,-60.5312989229257));
#35740=CARTESIAN_POINT('Ctrl Pts',(31.3075710473081,4.31634468200943,-60.9812009781816));
#35741=CARTESIAN_POINT('Ctrl Pts',(31.2449622958405,4.55065839947622,-61.8889297924662));
#35742=CARTESIAN_POINT('Ctrl Pts',(31.1794385244147,4.83839904044304,-62.9350100374388));
#35743=CARTESIAN_POINT('Ctrl Pts',(31.122726763293,5.15907701218947,-63.987551271028));
#35744=CARTESIAN_POINT('Ctrl Pts',(31.0946368142613,5.354039507125,-64.5807134970563));
#35745=CARTESIAN_POINT('Ctrl Pts',(31.0776806560438,5.49111596067101,-64.976348444816));
#35746=CARTESIAN_POINT('Ctrl Pts',(31.0668597264748,5.58444985936914,-65.2401034842792));
#35747=CARTESIAN_POINT('Ctrl Pts',(31.0567803435495,5.68084257221062,-65.5038761735702));
#35748=CARTESIAN_POINT('Ctrl Pts',(31.0486362195788,5.76800749574544,-65.734567400679));
#35749=CARTESIAN_POINT('Ctrl Pts',(31.0441788183548,5.81865115456034,-65.8663542619541));
#35750=CARTESIAN_POINT('Ctrl Pts',(31.0376906710409,5.89546615139976,-66.063997660731));
#35751=CARTESIAN_POINT('Ctrl Pts',(31.0327000962336,5.96127690314123,-66.2286057948698));
#35752=CARTESIAN_POINT('Ctrl Pts',(31.0250025050703,6.07281901289687,-66.5011152840611));
#35753=CARTESIAN_POINT('Ctrl Pts',(31.0179956380395,6.19437698960279,-66.7887030109143));
#35754=CARTESIAN_POINT('Ctrl Pts',(31.0074757471655,6.44513738098736,-67.3493144180915));
#35755=CARTESIAN_POINT('Ctrl Pts',(30.997085233629,6.906412501861,-68.3087923116582));
#35756=CARTESIAN_POINT('Ctrl Pts',(30.999493056306,7.8855409231497,-70.1403049410983));
#35757=CARTESIAN_POINT('Ctrl Pts',(31.0168899440058,8.73456822280869,-71.6038226179437));
#35758=CARTESIAN_POINT('Ctrl Pts',(31.0158700282441,9.29917548368328,-72.6764093602891));
#35759=CARTESIAN_POINT('Ctrl Pts',(31.0156385115126,9.43422564243663,-72.9326071116161));
#35760=CARTESIAN_POINT('Ctrl Pts',(31.0153112276913,9.69948548811709,-73.4346939262143));
#35761=CARTESIAN_POINT('Ctrl Pts',(31.0150889569634,10.0338049752592,-74.0656234388318));
#35762=CARTESIAN_POINT('Ctrl Pts',(31.0150636577838,10.4344948303806,-74.8194510270631));
#35763=CARTESIAN_POINT('Ctrl Pts',(31.0153438539892,11.2372986599713,-76.3265451457017));
#35764=CARTESIAN_POINT('Ctrl Pts',(31.0159819351073,11.9063383399868,-77.578742348905));
#35765=CARTESIAN_POINT('Ctrl Pts',(31.0159924606929,12.8743106021264,-79.3992882081553));
#35766=CARTESIAN_POINT('Ctrl Pts',(31.015991633413,13.3115662212557,-80.2216742641514));
#35767=CARTESIAN_POINT('Ctrl Pts',(31.0159916334131,13.7480878086451,-81.0426519662498));
#35768=CARTESIAN_POINT('Ctrl Pts',(32.4375725283096,0.00612073677650567,
24.8306303773195));
#35769=CARTESIAN_POINT('Ctrl Pts',(32.4376704492468,0.00612173323859073,
24.781750928448));
#35770=CARTESIAN_POINT('Ctrl Pts',(32.4377731465535,0.00612277784268754,
24.732872528879));
#35771=CARTESIAN_POINT('Ctrl Pts',(32.438985886721,0.0061351289779464,24.1822628969437));
#35772=CARTESIAN_POINT('Ctrl Pts',(32.4399193830562,0.00614560068208076,
23.1781289417908));
#35773=CARTESIAN_POINT('Ctrl Pts',(32.4420948130036,0.00617032469026516,
21.1695259205625));
#35774=CARTESIAN_POINT('Ctrl Pts',(32.4501651077224,0.00625264801595857,
19.6653663333986));
#35775=CARTESIAN_POINT('Ctrl Pts',(32.467261250398,0.00642226561136431,
18.4143123354664));
#35776=CARTESIAN_POINT('Ctrl Pts',(32.4754620024458,0.00650459012566578,
17.9114868513781));
#35777=CARTESIAN_POINT('Ctrl Pts',(32.4960567542474,0.00671318284351931,
16.9074925722283));
#35778=CARTESIAN_POINT('Ctrl Pts',(32.540229806681,0.0071610401825099,15.1536918206885));
#35779=CARTESIAN_POINT('Ctrl Pts',(32.5821659779686,0.0075747936488959,
13.6519837245366));
#35780=CARTESIAN_POINT('Ctrl Pts',(32.6084134956282,0.00781133248939808,
12.3975410538733));
#35781=CARTESIAN_POINT('Ctrl Pts',(32.6191392183056,0.00790562449951455,
11.8966003565388));
#35782=CARTESIAN_POINT('Ctrl Pts',(32.6409890710773,0.00808999154332186,
10.8947764919162));
#35783=CARTESIAN_POINT('Ctrl Pts',(32.6787755656417,0.00839256724841023,
9.14125760874515));
#35784=CARTESIAN_POINT('Ctrl Pts',(32.7052468202478,0.00858448180949316,
7.63602490847467));
#35785=CARTESIAN_POINT('Ctrl Pts',(32.7170051004007,0.00866427690422162,
6.50506873960121));
#35786=CARTESIAN_POINT('Ctrl Pts',(32.7194476626338,0.00867657290767804,
6.25489858217397));
#35787=CARTESIAN_POINT('Ctrl Pts',(32.723724156199,0.00868237884311895,
5.7538424239641));
#35788=CARTESIAN_POINT('Ctrl Pts',(32.7296680260123,0.008651717567273,4.87551538707216));
#35789=CARTESIAN_POINT('Ctrl Pts',(32.7358654941957,0.00849526231436584,
3.11521304601986));
#35790=CARTESIAN_POINT('Ctrl Pts',(32.7330050923788,0.00842882889151111,
1.60822825847469));
#35791=CARTESIAN_POINT('Ctrl Pts',(32.7286287931558,0.00863352408019025,
0.548390972029742));
#35792=CARTESIAN_POINT('Ctrl Pts',(32.7280556012293,0.00866031411611293,
0.422146457370445));
#35793=CARTESIAN_POINT('Ctrl Pts',(32.7267103229818,0.00872296322295062,
0.169878000266251));
#35794=CARTESIAN_POINT('Ctrl Pts',(32.7238611536692,0.00885483901651413,
-0.271079661633083));
#35795=CARTESIAN_POINT('Ctrl Pts',(32.7185257185815,0.00909719910768501,
-0.89967508832505));
#35796=CARTESIAN_POINT('Ctrl Pts',(32.7105872595901,0.00944673870218814,
-1.65231437353842));
#35797=CARTESIAN_POINT('Ctrl Pts',(32.698591518813,0.00995047629065278,
-2.65420250676402));
#35798=CARTESIAN_POINT('Ctrl Pts',(32.6821693413152,0.0105775487649706,
-3.9046733867623));
#35799=CARTESIAN_POINT('Ctrl Pts',(32.6700718046237,0.0109227635378567,
-4.90546860538031));
#35800=CARTESIAN_POINT('Ctrl Pts',(32.6636503115398,0.0110412576361191,
-5.53195733759867));
#35801=CARTESIAN_POINT('Ctrl Pts',(32.6611026206047,0.0111029208113027,
-5.78307151337921));
#35802=CARTESIAN_POINT('Ctrl Pts',(32.6560786904651,0.0112707827624278,
-6.28532116522749));
#35803=CARTESIAN_POINT('Ctrl Pts',(32.6474492938381,0.0116453384518062,
-7.16474040450405));
#35804=CARTESIAN_POINT('Ctrl Pts',(32.6353941325091,0.0122156502770102,
-8.42102129578186));
#35805=CARTESIAN_POINT('Ctrl Pts',(32.6232792542869,0.0123006655414279,
-9.67459864505452));
#35806=CARTESIAN_POINT('Ctrl Pts',(32.6145352572378,0.0118326570992625,
-10.5491928952008));
#35807=CARTESIAN_POINT('Ctrl Pts',(32.6094313904953,0.0113765141786167,
-11.0479256199958));
#35808=CARTESIAN_POINT('Ctrl Pts',(32.6068351489801,0.011080033509664,-11.2969138483581));
#35809=CARTESIAN_POINT('Ctrl Pts',(32.604862964816,0.0108284854691137,-11.4842693213742));
#35810=CARTESIAN_POINT('Ctrl Pts',(32.6034581502333,0.0106345574586929,
-11.6096889651575));
#35811=CARTESIAN_POINT('Ctrl Pts',(32.6003606096668,0.0101420129158296,
-11.860601970361));
#35812=CARTESIAN_POINT('Ctrl Pts',(32.5942538989981,0.00903576810677099,
-12.2991065557788));
#35813=CARTESIAN_POINT('Ctrl Pts',(32.5757932155024,0.00517063181383277,
-13.4249465396148));
#35814=CARTESIAN_POINT('Ctrl Pts',(32.5516633096074,-0.00076474121200517,
-14.6733009245517));
#35815=CARTESIAN_POINT('Ctrl Pts',(32.5380545352075,-0.00459324500449539,
-15.9284346040029));
#35816=CARTESIAN_POINT('Ctrl Pts',(32.5350003375435,-0.00565654912437246,
-16.5584041406639));
#35817=CARTESIAN_POINT('Ctrl Pts',(32.5355910795788,-0.00581636820274184,
-17.0643083481665));
#35818=CARTESIAN_POINT('Ctrl Pts',(32.5369915996141,-0.00562287815735871,
-17.3179877292813));
#35819=CARTESIAN_POINT('Ctrl Pts',(32.5385075377801,-0.00536457972547619,
-17.5076988195231));
#35820=CARTESIAN_POINT('Ctrl Pts',(32.5395516516621,-0.00526975227129406,
-17.6311265404471));
#35821=CARTESIAN_POINT('Ctrl Pts',(32.5418300401125,-0.00518431464235082,
-17.8795060413966));
#35822=CARTESIAN_POINT('Ctrl Pts',(32.5443808293887,-0.00525827931732753,
-18.1278998449213));
#35823=CARTESIAN_POINT('Ctrl Pts',(32.5472860436008,-0.00540480712456201,
-18.3770110834493));
#35824=CARTESIAN_POINT('Ctrl Pts',(32.5492427809058,-0.00551399113095648,
-18.5328476680375));
#35825=CARTESIAN_POINT('Ctrl Pts',(32.5509033290443,-0.00560164294745968,
-18.6576559792242));
#35826=CARTESIAN_POINT('Ctrl Pts',(32.5526266366226,-0.00568581122353676,
-18.7825370683472));
#35827=CARTESIAN_POINT('Ctrl Pts',(32.5576121159634,-0.00590691263338564,
-19.1262829157936));
#35828=CARTESIAN_POINT('Ctrl Pts',(32.5672340253502,-0.00599570887245065,
-19.6905177021123));
#35829=CARTESIAN_POINT('Ctrl Pts',(32.5890910784554,-0.00413567925224601,
-20.6984784042354));
#35830=CARTESIAN_POINT('Ctrl Pts',(32.6260269114473,0.00445448628603799,
-21.9672178731562));
#35831=CARTESIAN_POINT('Ctrl Pts',(32.6688510646589,0.0221318845874462,
-22.9920195822445));
#35832=CARTESIAN_POINT('Ctrl Pts',(32.7012102272047,0.0385324406427145,
-23.634396489595));
#35833=CARTESIAN_POINT('Ctrl Pts',(32.715031917855,0.0455217649744831,-23.8880348573153));
#35834=CARTESIAN_POINT('Ctrl Pts',(32.7465170742004,0.0616196840009675,
-24.3957111275666));
#35835=CARTESIAN_POINT('Ctrl Pts',(32.8105415409616,0.0952581051992893,
-25.2842461053142));
#35836=CARTESIAN_POINT('Ctrl Pts',(32.9210591618046,0.159762402551823,-26.5530608107758));
#35837=CARTESIAN_POINT('Ctrl Pts',(33.0589337037139,0.25910958635653,-28.0695863386293));
#35838=CARTESIAN_POINT('Ctrl Pts',(33.136796739872,0.330867870485165,-29.0725964140342));
#35839=CARTESIAN_POINT('Ctrl Pts',(33.1725279620985,0.368669790118915,-29.6338337416282));
#35840=CARTESIAN_POINT('Ctrl Pts',(33.1803870386095,0.377025613103238,-29.759044228272));
#35841=CARTESIAN_POINT('Ctrl Pts',(33.1957438638766,0.393733031112438,-30.0093990829174));
#35842=CARTESIAN_POINT('Ctrl Pts',(33.2217030508958,0.422957178392457,-30.4481178470327));
#35843=CARTESIAN_POINT('Ctrl Pts',(33.2702186084373,0.481524710545981,-31.3272291279453));
#35844=CARTESIAN_POINT('Ctrl Pts',(33.3188327155682,0.5498143672729,-32.3352499388375));
#35845=CARTESIAN_POINT('Ctrl Pts',(33.3627484758732,0.621597850833921,-33.3452623854794));
#35846=CARTESIAN_POINT('Ctrl Pts',(33.3938233587234,0.677804083201993,-34.1034748355415));
#35847=CARTESIAN_POINT('Ctrl Pts',(33.4234183964842,0.73715538275439,-34.8619437154264));
#35848=CARTESIAN_POINT('Ctrl Pts',(33.4424931158544,0.779237276920695,-35.3676000913595));
#35849=CARTESIAN_POINT('Ctrl Pts',(33.4567175399219,0.81197947781779,-35.7477541739545));
#35850=CARTESIAN_POINT('Ctrl Pts',(33.4663254823227,0.834162056159859,-36.0010457997609));
#35851=CARTESIAN_POINT('Ctrl Pts',(33.4855665553264,0.879653442348478,-36.5075046045366));
#35852=CARTESIAN_POINT('Ctrl Pts',(33.518976770033,0.962053734946922,-37.3914520772919));
#35853=CARTESIAN_POINT('Ctrl Pts',(33.5824998346805,1.13533938921436,-39.1543029953479));
#35854=CARTESIAN_POINT('Ctrl Pts',(33.6228063368028,1.29268351555625,-40.6638351678756));
#35855=CARTESIAN_POINT('Ctrl Pts',(33.637460801882,1.40823476310828,-41.8007123511776));
#35856=CARTESIAN_POINT('Ctrl Pts',(33.6411996738958,1.43179248615386,-42.0387259261224));
#35857=CARTESIAN_POINT('Ctrl Pts',(33.6461063511285,1.46536011018525,-42.4061764186738));
#35858=CARTESIAN_POINT('Ctrl Pts',(33.6506102473115,1.49707490134403,-42.7747444908318));
#35859=CARTESIAN_POINT('Ctrl Pts',(33.6557553728041,1.5380045112777,-43.2721482774162));
#35860=CARTESIAN_POINT('Ctrl Pts',(33.6604262132191,1.58789030168531,-43.9018736202697));
#35861=CARTESIAN_POINT('Ctrl Pts',(33.6622567248897,1.65073055016276,-44.6708978424729));
#35862=CARTESIAN_POINT('Ctrl Pts',(33.6598108879441,1.70982232506804,-45.3219908902517));
#35863=CARTESIAN_POINT('Ctrl Pts',(33.6548067440503,1.76380021439561,-45.8487647704021));
#35864=CARTESIAN_POINT('Ctrl Pts',(33.649419920791,1.80832894359961,-46.2467602469543));
#35865=CARTESIAN_POINT('Ctrl Pts',(33.6422362058874,1.85759769357008,-46.6475979770163));
#35866=CARTESIAN_POINT('Ctrl Pts',(33.6299889594092,1.93059838524708,-47.1857555957972));
#35867=CARTESIAN_POINT('Ctrl Pts',(33.61768960664,1.99458607735694,-47.5934589947759));
#35868=CARTESIAN_POINT('Ctrl Pts',(33.6027138623418,2.0665714935698,-48.0050566158937));
#35869=CARTESIAN_POINT('Ctrl Pts',(33.5905238784982,2.12049129158493,-48.2930096977021));
#35870=CARTESIAN_POINT('Ctrl Pts',(33.5641889649566,2.2394387576737,-48.8517379400952));
#35871=CARTESIAN_POINT('Ctrl Pts',(33.5121412511527,2.47469649448957,-49.8106673127384));
#35872=CARTESIAN_POINT('Ctrl Pts',(33.4296895252064,2.8540314627126,-51.116041684853));
#35873=CARTESIAN_POINT('Ctrl Pts',(33.3323497449342,3.28708577780795,-52.5895297498466));
#35874=CARTESIAN_POINT('Ctrl Pts',(33.2724679931295,3.50437584515634,-53.5024828340018));
#35875=CARTESIAN_POINT('Ctrl Pts',(33.2353734282258,3.603793727542,-54.048495646057));
#35876=CARTESIAN_POINT('Ctrl Pts',(33.2186887677575,3.64206286670646,-54.2765843642304));
#35877=CARTESIAN_POINT('Ctrl Pts',(33.1812690437434,3.70762601944653,-54.736104266661));
#35878=CARTESIAN_POINT('Ctrl Pts',(33.1052759700434,3.79981335244846,-55.5599817959337));
#35879=CARTESIAN_POINT('Ctrl Pts',(32.9199074710695,3.92750431317271,-57.275958678648));
#35880=CARTESIAN_POINT('Ctrl Pts',(32.7437274613203,4.07114128831046,-58.8721394454319));
#35881=CARTESIAN_POINT('Ctrl Pts',(32.6639824581932,4.30556649985029,-60.0493336085321));
#35882=CARTESIAN_POINT('Ctrl Pts',(32.6550523999368,4.33055841229675,-60.174987850211));
#35883=CARTESIAN_POINT('Ctrl Pts',(32.63768717107,4.38337873383551,-60.4366839407282));
#35884=CARTESIAN_POINT('Ctrl Pts',(32.6095138887291,4.47691107068816,-60.8910885081208));
#35885=CARTESIAN_POINT('Ctrl Pts',(32.5608295965856,4.67430312186353,-61.8088050207747));
#35886=CARTESIAN_POINT('Ctrl Pts',(32.5207812011383,4.92588842360142,-62.8654352013746));
#35887=CARTESIAN_POINT('Ctrl Pts',(32.4910556698706,5.21535938673554,-63.9289579808857));
#35888=CARTESIAN_POINT('Ctrl Pts',(32.4772375701882,5.39473052547573,-64.5283020847092));
#35889=CARTESIAN_POINT('Ctrl Pts',(32.4688275698169,5.52227196815787,-64.9280978430035));
#35890=CARTESIAN_POINT('Ctrl Pts',(32.4634077760578,5.60949149135347,-65.1946257634481));
#35891=CARTESIAN_POINT('Ctrl Pts',(32.4582349635776,5.70012474893571,-65.4611844737283));
#35892=CARTESIAN_POINT('Ctrl Pts',(32.4538496347377,5.78259031628741,-65.6943019960171));
#35893=CARTESIAN_POINT('Ctrl Pts',(32.4513753260859,5.83064584969686,-65.8274717215964));
#35894=CARTESIAN_POINT('Ctrl Pts',(32.4476902372352,5.90367903832255,-66.0271877027392));
#35895=CARTESIAN_POINT('Ctrl Pts',(32.4446685092354,5.96653900293033,-66.1935103058364));
#35896=CARTESIAN_POINT('Ctrl Pts',(32.4396698964425,6.07351165788405,-66.4689006508914));
#35897=CARTESIAN_POINT('Ctrl Pts',(32.4351018946248,6.19225514219894,-66.7627262695961));
#35898=CARTESIAN_POINT('Ctrl Pts',(32.4283028677017,6.43897617099595,-67.332382514625));
#35899=CARTESIAN_POINT('Ctrl Pts',(32.4217165914204,6.89862124151141,-68.3053596401035));
#35900=CARTESIAN_POINT('Ctrl Pts',(32.4236746454016,7.88786118882068,-70.1508134268032));
#35901=CARTESIAN_POINT('Ctrl Pts',(32.435278994445,8.74876384190553,-71.6120343198423));
#35902=CARTESIAN_POINT('Ctrl Pts',(32.435038763498,9.30747710662932,-72.6747612841359));
#35903=CARTESIAN_POINT('Ctrl Pts',(32.4349002184836,9.44282627201533,-72.9317827884244));
#35904=CARTESIAN_POINT('Ctrl Pts',(32.4347384980485,9.70782501925712,-73.4337510341519));
#35905=CARTESIAN_POINT('Ctrl Pts',(32.4346157241301,10.042276972751,-74.0652069607757));
#35906=CARTESIAN_POINT('Ctrl Pts',(32.4345986484725,10.4430286253234,-74.819189488878));
#35907=CARTESIAN_POINT('Ctrl Pts',(32.434728949116,11.2461960650344,-76.3266732241031));
#35908=CARTESIAN_POINT('Ctrl Pts',(32.4350650841433,11.9155592004831,-77.5788728671257));
#35909=CARTESIAN_POINT('Ctrl Pts',(32.435094458272,12.8833188081073,-79.3990793477341));
#35910=CARTESIAN_POINT('Ctrl Pts',(32.4350926663251,13.3206560018545,-80.2216501046058));
#35911=CARTESIAN_POINT('Ctrl Pts',(32.4350926663252,13.757177589244,-81.042627806704));
#35912=CARTESIAN_POINT('Ctrl Pts',(34.3348665008137,0.0296348787660989,
24.8306202558209));
#35913=CARTESIAN_POINT('Ctrl Pts',(34.3349702061934,0.029637068735487,24.7817404888869));
#35914=CARTESIAN_POINT('Ctrl Pts',(34.3350789693011,0.0296393640675755,
24.7328617643363));
#35915=CARTESIAN_POINT('Ctrl Pts',(34.3363633825367,0.0296665120963467,
24.1822484301607));
#35916=CARTESIAN_POINT('Ctrl Pts',(34.337350759526,0.0296933097880433,23.1781110319428));
#35917=CARTESIAN_POINT('Ctrl Pts',(34.3396499777359,0.0297587991764213,
21.1695008410527));
#35918=CARTESIAN_POINT('Ctrl Pts',(34.3481981529855,0.0299396228229842,
19.6653379702371));
#35919=CARTESIAN_POINT('Ctrl Pts',(34.3663127117265,0.0302934347281393,
18.4142822305806));
#35920=CARTESIAN_POINT('Ctrl Pts',(34.3750003475134,0.0304658073261087,
17.9114388071362));
#35921=CARTESIAN_POINT('Ctrl Pts',(34.3968154838019,0.0309034790139605,
16.907432448917));
#35922=CARTESIAN_POINT('Ctrl Pts',(34.4436049017858,0.0318414145430069,
15.1536361704964));
#35923=CARTESIAN_POINT('Ctrl Pts',(34.4880473484764,0.0326934662284305,
13.6519888957546));
#35924=CARTESIAN_POINT('Ctrl Pts',(34.5158961770517,0.0331547802921301,
12.397621207677));
#35925=CARTESIAN_POINT('Ctrl Pts',(34.5272788503318,0.0333352448613346,
11.8967116582713));
#35926=CARTESIAN_POINT('Ctrl Pts',(34.5504784914328,0.033677032523816,10.8949340302363));
#35927=CARTESIAN_POINT('Ctrl Pts',(34.5906219851948,0.0342144269964047,
9.14146183505485));
#35928=CARTESIAN_POINT('Ctrl Pts',(34.6187852923028,0.034531507353301,7.63620565117921));
#35929=CARTESIAN_POINT('Ctrl Pts',(34.6313071543681,0.0346614975994032,
6.50520241718005));
#35930=CARTESIAN_POINT('Ctrl Pts',(34.6339101122789,0.0346805129074275,
6.25507094287352));
#35931=CARTESIAN_POINT('Ctrl Pts',(34.6384775201399,0.0346848860572032,
5.75405063514034));
#35932=CARTESIAN_POINT('Ctrl Pts',(34.6448529888665,0.034618796147095,4.87576992215105));
#35933=CARTESIAN_POINT('Ctrl Pts',(34.6515912826497,0.0343121150855791,
3.11541901871874));
#35934=CARTESIAN_POINT('Ctrl Pts',(34.6486547883739,0.0341545534559291,
1.60818548078039));
#35935=CARTESIAN_POINT('Ctrl Pts',(34.6439423833365,0.0344775417838192,
0.548062255281211));
#35936=CARTESIAN_POINT('Ctrl Pts',(34.6433235709926,0.0345201216650427,
0.421770541410198));
#35937=CARTESIAN_POINT('Ctrl Pts',(34.6418698505304,0.0346199270201468,
0.169421305589011));
#35938=CARTESIAN_POINT('Ctrl Pts',(34.6387866018264,0.0348308422103272,
-0.271667565664166));
#35939=CARTESIAN_POINT('Ctrl Pts',(34.6330112099306,0.0352194887939851,
-0.900405073948883));
#35940=CARTESIAN_POINT('Ctrl Pts',(34.6244098621842,0.0357828305244157,
-1.65315227382485));
#35941=CARTESIAN_POINT('Ctrl Pts',(34.6114362072505,0.0365964720905593,
-2.65509310379257));
#35942=CARTESIAN_POINT('Ctrl Pts',(34.5937070812663,0.0376214045821537,
-3.90548388247732));
#35943=CARTESIAN_POINT('Ctrl Pts',(34.5807623271108,0.0381958727371875,
-4.90603699346939));
#35944=CARTESIAN_POINT('Ctrl Pts',(34.5739306797211,0.0384004064543149,
-5.53236276681657));
#35945=CARTESIAN_POINT('Ctrl Pts',(34.5712035777894,0.0385355389098031,
-5.78398927199619));
#35946=CARTESIAN_POINT('Ctrl Pts',(34.5657823899225,0.0389715066872898,
-6.28674790375234));
#35947=CARTESIAN_POINT('Ctrl Pts',(34.5563821271522,0.0400579145688246,
-7.16680494613018));
#35948=CARTESIAN_POINT('Ctrl Pts',(34.5432213468392,0.0418916352723083,
-8.42263682791367));
#35949=CARTESIAN_POINT('Ctrl Pts',(34.5304281853659,0.0423755989149951,
-9.67418519311426));
#35950=CARTESIAN_POINT('Ctrl Pts',(34.5216736231272,0.0410948990578466,
-10.5464833526537));
#35951=CARTESIAN_POINT('Ctrl Pts',(34.5167287269536,0.0397704858090913,
-11.0436474668148));
#35952=CARTESIAN_POINT('Ctrl Pts',(34.5142776957149,0.0388885449217639,
-11.2917836956804));
#35953=CARTESIAN_POINT('Ctrl Pts',(34.512438749955,0.0381334687157137,-11.4784120208249));
#35954=CARTESIAN_POINT('Ctrl Pts',(34.5110693944478,0.0375076169622718,
-11.6015276034163));
#35955=CARTESIAN_POINT('Ctrl Pts',(34.5078499703665,0.0358175810326835,
-11.849203928751));
#35956=CARTESIAN_POINT('Ctrl Pts',(34.5010910795936,0.03181512375827,-12.2823387512624));
#35957=CARTESIAN_POINT('Ctrl Pts',(34.4792962544431,0.0171493363518133,
-13.3990847781187));
#35958=CARTESIAN_POINT('Ctrl Pts',(34.4501747289077,-0.00563669577787649,
-14.6505064305469));
#35959=CARTESIAN_POINT('Ctrl Pts',(34.4402911621688,-0.0163880090013641,
-15.9220705631234));
#35960=CARTESIAN_POINT('Ctrl Pts',(34.4421816827344,-0.0172553614217765,
-16.5633264679564));
#35961=CARTESIAN_POINT('Ctrl Pts',(34.4489435583318,-0.0142978400379119,
-17.0800094717923));
#35962=CARTESIAN_POINT('Ctrl Pts',(34.4542793572371,-0.0114392291676308,
-17.3396666946536));
#35963=CARTESIAN_POINT('Ctrl Pts',(34.4590621679773,-0.00872845323497167,
-17.5339367992568));
#35964=CARTESIAN_POINT('Ctrl Pts',(34.4624250714993,-0.00693217023133912,
-17.6568219591938));
#35965=CARTESIAN_POINT('Ctrl Pts',(34.4699245154061,-0.00339418588522034,
-17.9063737364449));
#35966=CARTESIAN_POINT('Ctrl Pts',(34.4785499941884,0.000139553048910618,
-18.1554151286434));
#35967=CARTESIAN_POINT('Ctrl Pts',(34.4881981477845,0.00374441972305012,
-18.4058266429038));
#35968=CARTESIAN_POINT('Ctrl Pts',(34.4946424647782,0.00605320969936596,
-18.5624954125497));
#35969=CARTESIAN_POINT('Ctrl Pts',(34.5000341941741,0.00794431257695288,
-18.688069890545));
#35970=CARTESIAN_POINT('Ctrl Pts',(34.5055811412055,0.00986886720126,-18.8137530033974));
#35971=CARTESIAN_POINT('Ctrl Pts',(34.5214679358394,0.0153379856010082,
-19.1599197917746));
#35972=CARTESIAN_POINT('Ctrl Pts',(34.5507640173886,0.0253466481217635,
-19.7292428735243));
#35973=CARTESIAN_POINT('Ctrl Pts',(34.6108128715338,0.0490990947697404,
-20.7501383806793));
#35974=CARTESIAN_POINT('Ctrl Pts',(34.6988121604481,0.0959009703686677,
-22.0439214278242));
#35975=CARTESIAN_POINT('Ctrl Pts',(34.7768065662565,0.16854409880932,-23.0992880475148));
#35976=CARTESIAN_POINT('Ctrl Pts',(34.8247270237116,0.230398196361508,-23.7634141199022));
#35977=CARTESIAN_POINT('Ctrl Pts',(34.8445161595343,0.257282454815504,-24.0322039773686));
#35978=CARTESIAN_POINT('Ctrl Pts',(34.8866107950697,0.31890337558203,-24.5626599722539));
#35979=CARTESIAN_POINT('Ctrl Pts',(34.9654040907167,0.445760973026535,-25.4840804706916));
#35980=CARTESIAN_POINT('Ctrl Pts',(35.0836114628791,0.668955182248936,-26.7718438871875));
#35981=CARTESIAN_POINT('Ctrl Pts',(35.2107424432564,0.959877924312591,-28.2700879809425));
#35982=CARTESIAN_POINT('Ctrl Pts',(35.2756202929575,1.13589941731545,-29.2363892005653));
#35983=CARTESIAN_POINT('Ctrl Pts',(35.3049350040518,1.22055555336939,-29.7712659446889));
#35984=CARTESIAN_POINT('Ctrl Pts',(35.311152113083,1.23966678302167,-29.8954325847102));
#35985=CARTESIAN_POINT('Ctrl Pts',(35.3231424719885,1.27717133207363,-30.141072757404));
#35986=CARTESIAN_POINT('Ctrl Pts',(35.3427475768565,1.34168941918445,-30.5731204623188));
#35987=CARTESIAN_POINT('Ctrl Pts',(35.3770722102907,1.46610252274959,-31.4386112933145));
#35988=CARTESIAN_POINT('Ctrl Pts',(35.4070489402869,1.59963645464085,-32.4333294077523));
#35989=CARTESIAN_POINT('Ctrl Pts',(35.4312403420351,1.72847555459606,-33.4310363885322));
#35990=CARTESIAN_POINT('Ctrl Pts',(35.4472477001023,1.8238550384678,-34.1806796044288));
#35991=CARTESIAN_POINT('Ctrl Pts',(35.4619111545767,1.91895541470026,-34.9312137346278));
#35992=CARTESIAN_POINT('Ctrl Pts',(35.4712334901812,1.98293013095225,-35.4319905802502));
#35993=CARTESIAN_POINT('Ctrl Pts',(35.478233773719,2.03153925195565,-35.808572373394));
#35994=CARTESIAN_POINT('Ctrl Pts',(35.4830531735356,2.06392218397385,-36.0584646920786));
#35995=CARTESIAN_POINT('Ctrl Pts',(35.4926802077051,2.12861386739761,-36.5589901333385));
#35996=CARTESIAN_POINT('Ctrl Pts',(35.5094871138481,2.24105474199066,-37.4330062845498));
#35997=CARTESIAN_POINT('Ctrl Pts',(35.5408576479142,2.46234762716514,-39.1789748004921));
#35998=CARTESIAN_POINT('Ctrl Pts',(35.5572421876025,2.64112381329902,-40.6782951369843));
#35999=CARTESIAN_POINT('Ctrl Pts',(35.5567624571101,2.76578051166555,-41.8093748197993));
#36000=CARTESIAN_POINT('Ctrl Pts',(35.5571853301886,2.79177993029111,-42.0496317037747));
#36001=CARTESIAN_POINT('Ctrl Pts',(35.5573263029132,2.82889503479657,-42.4176035690288));
#36002=CARTESIAN_POINT('Ctrl Pts',(35.5572386302164,2.86409255204442,-42.7863815460673));
#36003=CARTESIAN_POINT('Ctrl Pts',(35.5564822691865,2.90921026862981,-43.2824239859168));
#36004=CARTESIAN_POINT('Ctrl Pts',(35.5541893094433,2.96307988572064,-43.9082524122556));
#36005=CARTESIAN_POINT('Ctrl Pts',(35.5482826496532,3.02703653127083,-44.6689075116179));
#36006=CARTESIAN_POINT('Ctrl Pts',(35.5398959644219,3.08256710346372,-45.3102081014407));
#36007=CARTESIAN_POINT('Ctrl Pts',(35.5305831733313,3.13009686860969,-45.8276045672095));
#36008=CARTESIAN_POINT('Ctrl Pts',(35.5221159032968,3.16774298696779,-46.2178189894755));
#36009=CARTESIAN_POINT('Ctrl Pts',(35.512004132919,3.20784441258354,-46.6101715258913));
#36010=CARTESIAN_POINT('Ctrl Pts',(35.4960988966223,3.26521600069479,-47.1362032751428));
#36011=CARTESIAN_POINT('Ctrl Pts',(35.4811021734307,3.31335286374751,-47.5338839460087));
#36012=CARTESIAN_POINT('Ctrl Pts',(35.4635967259766,3.36607212993744,-47.9351749220645));
#36013=CARTESIAN_POINT('Ctrl Pts',(35.4494898736546,3.4056746116725,-48.2179946905193));
#36014=CARTESIAN_POINT('Ctrl Pts',(35.4182032525292,3.49275120818139,-48.7674332494914));
#36015=CARTESIAN_POINT('Ctrl Pts',(35.3545447183938,3.6640815037813,-49.7144307196596));
#36016=CARTESIAN_POINT('Ctrl Pts',(35.2471415986055,3.93550743444783,-51.0097126548988));
#36017=CARTESIAN_POINT('Ctrl Pts',(35.1102158736415,4.22549151210901,-52.4694949292696));
#36018=CARTESIAN_POINT('Ctrl Pts',(35.0224921908637,4.34893489480374,-53.3657555146103));
#36019=CARTESIAN_POINT('Ctrl Pts',(34.9712095732623,4.39391473679624,-53.8990101827058));
#36020=CARTESIAN_POINT('Ctrl Pts',(34.9500808458707,4.40684644048079,-54.1095680986356));
#36021=CARTESIAN_POINT('Ctrl Pts',(34.9033724169422,4.42080872818289,-54.5443012692132));
#36022=CARTESIAN_POINT('Ctrl Pts',(34.8130378502953,4.41642697910621,-55.3300647584961));
#36023=CARTESIAN_POINT('Ctrl Pts',(34.6117438977039,4.34012314350154,-57.0146657734164));
#36024=CARTESIAN_POINT('Ctrl Pts',(34.4531051253727,4.30922070393653,-58.6662666751489));
#36025=CARTESIAN_POINT('Ctrl Pts',(34.3894975143158,4.47950355174856,-59.9180228144314));
#36026=CARTESIAN_POINT('Ctrl Pts',(34.3823210415351,4.49747234506587,-60.0477815322125));
#36027=CARTESIAN_POINT('Ctrl Pts',(34.3693125647404,4.53678421981033,-60.3200171731233));
#36028=CARTESIAN_POINT('Ctrl Pts',(34.35020497003,4.60894769444198,-60.7904494162606));
#36029=CARTESIAN_POINT('Ctrl Pts',(34.3249474995229,4.77107317620435,-61.7371283591797));
#36030=CARTESIAN_POINT('Ctrl Pts',(34.3191689863112,4.99662311074608,-62.8169964039174));
#36031=CARTESIAN_POINT('Ctrl Pts',(34.3234893783647,5.26791092913627,-63.8949689569154));
#36032=CARTESIAN_POINT('Ctrl Pts',(34.327336292537,5.43868107676422,-64.4990442638172));
#36033=CARTESIAN_POINT('Ctrl Pts',(34.3295138860271,5.56055800279895,-64.9006753433086));
#36034=CARTESIAN_POINT('Ctrl Pts',(34.330800849446,5.64397173868575,-65.1680715349568));
#36035=CARTESIAN_POINT('Ctrl Pts',(34.3317418024156,5.73071023424241,-65.4350013761785));
#36036=CARTESIAN_POINT('Ctrl Pts',(34.3321037329367,5.80955416821317,-65.6680022388863));
#36037=CARTESIAN_POINT('Ctrl Pts',(34.3321557140039,5.85546437902845,-65.8009841429503));
#36038=CARTESIAN_POINT('Ctrl Pts',(34.3320677894955,5.92519716045461,-66.0003057198109));
#36039=CARTESIAN_POINT('Ctrl Pts',(34.331624201174,5.98511440238383,-66.1660442121481));
#36040=CARTESIAN_POINT('Ctrl Pts',(34.3302806170565,6.08691727314271,-66.4403221129988));
#36041=CARTESIAN_POINT('Ctrl Pts',(34.3289626032204,6.20369935850024,-66.7407215332001));
#36042=CARTESIAN_POINT('Ctrl Pts',(34.3270621904633,6.44695750743629,-67.3177229835005));
#36043=CARTESIAN_POINT('Ctrl Pts',(34.3252412284561,6.90584758899664,-68.3028276387302));
#36044=CARTESIAN_POINT('Ctrl Pts',(34.3259284736756,7.90462355977505,-70.1596836659473));
#36045=CARTESIAN_POINT('Ctrl Pts',(34.3296133593729,8.77639942584956,-71.6192787849307));
#36046=CARTESIAN_POINT('Ctrl Pts',(34.3304097572867,9.33027438548443,-72.6734212274245));
#36047=CARTESIAN_POINT('Ctrl Pts',(34.3303710936354,9.46590328165915,-72.9310976231889));
#36048=CARTESIAN_POINT('Ctrl Pts',(34.3304069107005,9.73071077115545,-73.4328814476757));
#36049=CARTESIAN_POINT('Ctrl Pts',(34.3303857676624,10.0652916277749,-74.0647109462501));
#36050=CARTESIAN_POINT('Ctrl Pts',(34.3303712375336,10.466065257165,-74.8187519248144));
#36051=CARTESIAN_POINT('Ctrl Pts',(34.3303065315425,11.2694354886003,-76.3264752362663));
#36052=CARTESIAN_POINT('Ctrl Pts',(34.3302458442975,11.9390055802922,-77.5787656056257));
#36053=CARTESIAN_POINT('Ctrl Pts',(34.3302832165028,12.906702086019,-79.3988760800469));
#36054=CARTESIAN_POINT('Ctrl Pts',(34.330266902442,13.3440986555018,-80.2215709003871));
#36055=CARTESIAN_POINT('Ctrl Pts',(34.3302669024419,13.7806202428913,-81.0425486024853));
#36056=CARTESIAN_POINT('Ctrl Pts',(36.7112167699881,0.0846744253985972,
24.8306211802992));
#36057=CARTESIAN_POINT('Ctrl Pts',(36.7113270504777,0.0846781747077857,
24.7817414397337));
#36058=CARTESIAN_POINT('Ctrl Pts',(36.7114427105277,0.0846821056520928,
24.7328627397048));
#36059=CARTESIAN_POINT('Ctrl Pts',(36.7128085688682,0.0847285604531195,
24.1822497915495));
#36060=CARTESIAN_POINT('Ctrl Pts',(36.7138443146183,0.0847695523576969,
23.1781129933839));
#36061=CARTESIAN_POINT('Ctrl Pts',(36.7162470894082,0.0848677714251754,
21.1695036373261));
#36062=CARTESIAN_POINT('Ctrl Pts',(36.7253377401005,0.0851771162506037,
19.6653426120806));
#36063=CARTESIAN_POINT('Ctrl Pts',(36.7446729845777,0.0858063686810513,
18.4142886437229));
#36064=CARTESIAN_POINT('Ctrl Pts',(36.7539402129429,0.0861094140584334,
17.911453453911));
#36065=CARTESIAN_POINT('Ctrl Pts',(36.7772006719368,0.0868724352925051,
16.9074529235366));
#36066=CARTESIAN_POINT('Ctrl Pts',(36.8270936504073,0.0885071349433262,
15.1536543898094));
#36067=CARTESIAN_POINT('Ctrl Pts',(36.8745711220849,0.0900371434759867,
13.6519851701514));
#36068=CARTESIAN_POINT('Ctrl Pts',(36.9044813039543,0.0909542099707382,
12.3975863726652));
#36069=CARTESIAN_POINT('Ctrl Pts',(36.9167250679747,0.0913242311819742,
11.8966642822298));
#36070=CARTESIAN_POINT('Ctrl Pts',(36.9417383482741,0.092063240256459,10.8948719891067));
#36071=CARTESIAN_POINT('Ctrl Pts',(36.9851411517665,0.0933105117943699,
9.14139175481678));
#36072=CARTESIAN_POINT('Ctrl Pts',(37.0157109083655,0.0941508000170405,
7.63616346562538));
#36073=CARTESIAN_POINT('Ctrl Pts',(37.0293146481114,0.0945177922996605,
6.50517590311963));
#36074=CARTESIAN_POINT('Ctrl Pts',(37.0321450823204,0.0945919285604579,
6.2549752058218));
#36075=CARTESIAN_POINT('Ctrl Pts',(37.0371210043897,0.0947136005399027,
5.75388196216641));
#36076=CARTESIAN_POINT('Ctrl Pts',(37.0440927319416,0.0948615796641339,
4.87551145389234));
#36077=CARTESIAN_POINT('Ctrl Pts',(37.0515786051953,0.0949413242790322,
3.11521835137205));
#36078=CARTESIAN_POINT('Ctrl Pts',(37.0486124688515,0.0947750805650604,
1.60844265176952));
#36079=CARTESIAN_POINT('Ctrl Pts',(37.0436621926746,0.0946871777363435,
0.548832801105595));
#36080=CARTESIAN_POINT('Ctrl Pts',(37.0430108702942,0.0946759195152151,
0.422629163366355));
#36081=CARTESIAN_POINT('Ctrl Pts',(37.0414755532143,0.09464995393213,0.170430001263052));
#36082=CARTESIAN_POINT('Ctrl Pts',(37.0382084476048,0.0945961612704619,
-0.2704136055817));
#36083=CARTESIAN_POINT('Ctrl Pts',(37.032064141019,0.0944958624299077,-0.898867967521424));
#36084=CARTESIAN_POINT('Ctrl Pts',(37.0228917013655,0.0943506252441615,
-1.65140654519409));
#36085=CARTESIAN_POINT('Ctrl Pts',(37.0090325596193,0.0941270031994452,
-2.65320477270874));
#36086=CARTESIAN_POINT('Ctrl Pts',(36.9900665385056,0.0938128390382973,
-3.9037394793735));
#36087=CARTESIAN_POINT('Ctrl Pts',(36.9762063761215,0.0935646684807531,
-4.90469914381444));
#36088=CARTESIAN_POINT('Ctrl Pts',(36.9688985723988,0.0934289358944953,
-5.53140686327081));
#36089=CARTESIAN_POINT('Ctrl Pts',(36.965848701232,0.0934287654566223,-5.78303194814696));
#36090=CARTESIAN_POINT('Ctrl Pts',(36.9593500591013,0.0936049220407772,
-6.28587223138632));
#36091=CARTESIAN_POINT('Ctrl Pts',(36.9471928322836,0.0942670374755707,
-7.16602446820794));
#36092=CARTESIAN_POINT('Ctrl Pts',(36.9290905609926,0.0955974956355437,
-8.4219871970132));
#36093=CARTESIAN_POINT('Ctrl Pts',(36.9140217710994,0.0958307885018514,
-9.6737200225743));
#36094=CARTESIAN_POINT('Ctrl Pts',(36.9071799781076,0.0945953441252705,
-10.5462556420091));
#36095=CARTESIAN_POINT('Ctrl Pts',(36.9046304334507,0.0933734981130456,
-11.0435563604861));
#36096=CARTESIAN_POINT('Ctrl Pts',(36.9038594745276,0.0925705463853636,
-11.2918147610355));
#36097=CARTESIAN_POINT('Ctrl Pts',(36.9034865913886,0.0918882736245058,
-11.4784038866097));
#36098=CARTESIAN_POINT('Ctrl Pts',(36.9030853075895,0.0911945798563351,
-11.5969569379139));
#36099=CARTESIAN_POINT('Ctrl Pts',(36.9017538475644,0.0887426520100996,
-11.8388538451608));
#36100=CARTESIAN_POINT('Ctrl Pts',(36.898216268949,0.0819592352586638,-12.2623810155641));
#36101=CARTESIAN_POINT('Ctrl Pts',(36.8848261987535,0.0544563126445047,
-13.3650612644444));
#36102=CARTESIAN_POINT('Ctrl Pts',(36.8682840211302,0.00873084552395717,
-14.6279437361951));
#36103=CARTESIAN_POINT('Ctrl Pts',(36.883730091319,-0.00140900409272758,
-15.9393810040082));
#36104=CARTESIAN_POINT('Ctrl Pts',(36.9023667045802,0.00738003706140011,
-16.6075952081114));
#36105=CARTESIAN_POINT('Ctrl Pts',(36.9255929932009,0.0257459947431755,
-17.1501335700735));
#36106=CARTESIAN_POINT('Ctrl Pts',(36.9402796510903,0.0393172250515568,
-17.4241536848916));
#36107=CARTESIAN_POINT('Ctrl Pts',(36.9525070144203,0.0512901224359853,
-17.629627336922));
#36108=CARTESIAN_POINT('Ctrl Pts',(36.9612358256281,0.058874478576913,-17.7579791358429));
#36109=CARTESIAN_POINT('Ctrl Pts',(36.9810617739,0.0755937029143875,-18.0191630350841));
#36110=CARTESIAN_POINT('Ctrl Pts',(37.0042360390654,0.0940605022323197,
-18.278869703191));
#36111=CARTESIAN_POINT('Ctrl Pts',(37.0303076881267,0.114621356572637,-18.5395580253906));
#36112=CARTESIAN_POINT('Ctrl Pts',(37.0477123473,0.128337099242465,-18.7023527010502));
#36113=CARTESIAN_POINT('Ctrl Pts',(37.062242949944,0.139859105139886,-18.8326902634384));
#36114=CARTESIAN_POINT('Ctrl Pts',(37.0771577820906,0.151749504377015,-18.9630256422138));
#36115=CARTESIAN_POINT('Ctrl Pts',(37.1196737131603,0.185994854980597,-19.3215789081379));
#36116=CARTESIAN_POINT('Ctrl Pts',(37.1965049267673,0.250784832961701,-19.9087167246095));
#36117=CARTESIAN_POINT('Ctrl Pts',(37.3427176726399,0.392278988510994,-20.9537561882706));
#36118=CARTESIAN_POINT('Ctrl Pts',(37.5211894329389,0.619264465501433,-22.2612597859818));
#36119=CARTESIAN_POINT('Ctrl Pts',(37.6153479218006,0.84303517672332,-23.3094150400843));
#36120=CARTESIAN_POINT('Ctrl Pts',(37.6485511709952,0.98968170088537,-23.9656518899643));
#36121=CARTESIAN_POINT('Ctrl Pts',(37.6593603790078,1.05359960825901,-24.2446617278323));
#36122=CARTESIAN_POINT('Ctrl Pts',(37.6762771025471,1.18842239777695,-24.7838187391321));
#36123=CARTESIAN_POINT('Ctrl Pts',(37.6936520642177,1.44399158749902,-25.7160586081786));
#36124=CARTESIAN_POINT('Ctrl Pts',(37.6938852682224,1.8373117640372,-26.9982673915027));
#36125=CARTESIAN_POINT('Ctrl Pts',(37.6822568333526,2.28941532283948,-28.4718897646818));
#36126=CARTESIAN_POINT('Ctrl Pts',(37.679725915953,2.54033364704782,-29.4065852634538));
#36127=CARTESIAN_POINT('Ctrl Pts',(37.6816143028183,2.65819974592193,-29.9180122945906));
#36128=CARTESIAN_POINT('Ctrl Pts',(37.6810258951326,2.68551429704461,-30.0403811154778));
#36129=CARTESIAN_POINT('Ctrl Pts',(37.6799948340348,2.73816216919017,-30.2806536350076));
#36130=CARTESIAN_POINT('Ctrl Pts',(37.6770312359342,2.82771432743439,-30.7046151956739));
#36131=CARTESIAN_POINT('Ctrl Pts',(37.6682215238293,2.99534732000716,-31.5545149542589));
#36132=CARTESIAN_POINT('Ctrl Pts',(37.6532531101359,3.16522337037743,-32.5346457195609));
#36133=CARTESIAN_POINT('Ctrl Pts',(37.6374410450317,3.32069212311533,-33.5200421450193));
#36134=CARTESIAN_POINT('Ctrl Pts',(37.6259610794996,3.43210328958448,-34.2616953089193));
#36135=CARTESIAN_POINT('Ctrl Pts',(37.6157002543297,3.54025712278262,-35.0053877406598));
#36136=CARTESIAN_POINT('Ctrl Pts',(37.6101924543024,3.61153831044084,-35.5023857947915));
#36137=CARTESIAN_POINT('Ctrl Pts',(37.606760023377,3.66533539524376,-35.8763439464447));
#36138=CARTESIAN_POINT('Ctrl Pts',(37.6049850863926,3.70058659582321,-36.1227070445535));
#36139=CARTESIAN_POINT('Ctrl Pts',(37.601894064277,3.76970638580753,-36.6174113547226));
#36140=CARTESIAN_POINT('Ctrl Pts',(37.5979645128747,3.88624829952936,-37.4812630811199));
#36141=CARTESIAN_POINT('Ctrl Pts',(37.5931988424177,4.10248825673543,-39.208965058032));
#36142=CARTESIAN_POINT('Ctrl Pts',(37.5861294903716,4.25827904016071,-40.6945331880147));
#36143=CARTESIAN_POINT('Ctrl Pts',(37.5712416805247,4.36067583335185,-41.8161547039106));
#36144=CARTESIAN_POINT('Ctrl Pts',(37.5682415240926,4.38222806105262,-42.058508857134));
#36145=CARTESIAN_POINT('Ctrl Pts',(37.5636532761775,4.41297535307706,-42.4262547841356));
#36146=CARTESIAN_POINT('Ctrl Pts',(37.5590376997491,4.44202384408049,-42.7944249851715));
#36147=CARTESIAN_POINT('Ctrl Pts',(37.5526298265626,4.47881865486102,-43.2876809894668));
#36148=CARTESIAN_POINT('Ctrl Pts',(37.5439336707566,4.52147717949122,-43.9073297117841));
#36149=CARTESIAN_POINT('Ctrl Pts',(37.5314839039231,4.568582473753,-44.6559153643209));
#36150=CARTESIAN_POINT('Ctrl Pts',(37.5186404667206,4.60545971778606,-45.2834087418635));
#36151=CARTESIAN_POINT('Ctrl Pts',(37.506365694386,4.63423104404996,-45.7874623348475));
#36152=CARTESIAN_POINT('Ctrl Pts',(37.4960182599751,4.65559735298739,-46.1664926271542));
#36153=CARTESIAN_POINT('Ctrl Pts',(37.4843850602633,4.67692906601873,-46.5464584886975));
#36154=CARTESIAN_POINT('Ctrl Pts',(37.4669493900572,4.70558812969249,-47.0543505925715));
#36155=CARTESIAN_POINT('Ctrl Pts',(37.4514713193433,4.72756749779263,-47.4364875093737));
#36156=CARTESIAN_POINT('Ctrl Pts',(37.4339738194798,4.75041997909752,-47.8208376258834));
#36157=CARTESIAN_POINT('Ctrl Pts',(37.4208222272838,4.76784326333416,-48.0905868022626));
#36158=CARTESIAN_POINT('Ctrl Pts',(37.3910858757268,4.8058890086723,-48.6171456385995));
#36159=CARTESIAN_POINT('Ctrl Pts',(37.330309388502,4.88002773191839,-49.5284249880321));
#36160=CARTESIAN_POINT('Ctrl Pts',(37.2245928522151,4.99256283022992,-50.7853111888859));
#36161=CARTESIAN_POINT('Ctrl Pts',(37.086863900826,5.09644701465494,-52.2179456501514));
#36162=CARTESIAN_POINT('Ctrl Pts',(37.0032964705299,5.11897727890018,-53.1156669284226));
#36163=CARTESIAN_POINT('Ctrl Pts',(36.9591174381978,5.11110123786269,-53.6589488128304));
#36164=CARTESIAN_POINT('Ctrl Pts',(36.9409989107881,5.10299449829485,-53.8508893329867));
#36165=CARTESIAN_POINT('Ctrl Pts',(36.9045711625135,5.07293272516291,-54.268007339853));
#36166=CARTESIAN_POINT('Ctrl Pts',(36.8418253338402,4.98485325407387,-55.0312941587319));
#36167=CARTESIAN_POINT('Ctrl Pts',(36.7330788072467,4.71052689193802,-56.7257680108773));
#36168=CARTESIAN_POINT('Ctrl Pts',(36.6713543917833,4.46372288982941,-58.4421745126765));
#36169=CARTESIAN_POINT('Ctrl Pts',(36.6472973413736,4.55545974642122,-59.7852181242117));
#36170=CARTESIAN_POINT('Ctrl Pts',(36.6446924290674,4.56604719088446,-59.9247926927141));
#36171=CARTESIAN_POINT('Ctrl Pts',(36.6405006918235,4.59158900718835,-60.2162269454623));
#36172=CARTESIAN_POINT('Ctrl Pts',(36.6357573764282,4.64490957412634,-60.7173312098255));
#36173=CARTESIAN_POINT('Ctrl Pts',(36.6354347937168,4.78613690861304,-61.715152217054));
#36174=CARTESIAN_POINT('Ctrl Pts',(36.6504647026249,5.0177553381898,-62.8302318735079));
#36175=CARTESIAN_POINT('Ctrl Pts',(36.6701612909345,5.30491322392381,-63.9216539281145));
#36176=CARTESIAN_POINT('Ctrl Pts',(36.6811085561042,5.48450406800392,-64.5254323194787));
#36177=CARTESIAN_POINT('Ctrl Pts',(36.6875824323416,5.61060406842826,-64.9237425967269));
#36178=CARTESIAN_POINT('Ctrl Pts',(36.6916331850297,5.69628909573889,-65.1880995201401));
#36179=CARTESIAN_POINT('Ctrl Pts',(36.6952034565167,5.78432060322668,-65.4508024646126));
#36180=CARTESIAN_POINT('Ctrl Pts',(36.6977886480399,5.86316279414461,-65.6790619012919));
#36181=CARTESIAN_POINT('Ctrl Pts',(36.6990931550773,5.90870770418195,-65.8090432858565));
#36182=CARTESIAN_POINT('Ctrl Pts',(36.7008684362681,5.97751322044775,-66.0035864232181));
#36183=CARTESIAN_POINT('Ctrl Pts',(36.7019491948177,6.03580673631429,-66.1647301238399));
#36184=CARTESIAN_POINT('Ctrl Pts',(36.7031125057773,6.1336845974579,-66.4308883263072));
#36185=CARTESIAN_POINT('Ctrl Pts',(36.7038419183543,6.25108170444066,-66.7354276678796));
#36186=CARTESIAN_POINT('Ctrl Pts',(36.7049756302362,6.49357344121451,-67.31321041894));
#36187=CARTESIAN_POINT('Ctrl Pts',(36.7057176274359,6.95359681117788,-68.3024739392939));
#36188=CARTESIAN_POINT('Ctrl Pts',(36.7042062532507,7.95644289331439,-70.1615195305834));
#36189=CARTESIAN_POINT('Ctrl Pts',(36.7020394211586,8.83232363000405,-71.6214457270801));
#36190=CARTESIAN_POINT('Ctrl Pts',(36.7036824066944,9.38521971322024,-72.67303574198));
#36191=CARTESIAN_POINT('Ctrl Pts',(36.7036499997214,9.52096894610462,-72.9307872481302));
#36192=CARTESIAN_POINT('Ctrl Pts',(36.703772184435,9.78578067051566,-73.4323584766922));
#36193=CARTESIAN_POINT('Ctrl Pts',(36.7037713350486,10.1204017792823,-74.06414271824));
#36194=CARTESIAN_POINT('Ctrl Pts',(36.7037513271413,10.5211079906384,-74.8180546299337));
#36195=CARTESIAN_POINT('Ctrl Pts',(36.7035899613343,11.3242967756186,-76.3256604793899));
#36196=CARTESIAN_POINT('Ctrl Pts',(36.7033688472319,11.9937053006823,-77.578181963688));
#36197=CARTESIAN_POINT('Ctrl Pts',(36.703426617587,12.9615751163495,-79.3986755482907));
#36198=CARTESIAN_POINT('Ctrl Pts',(36.7033971809566,13.398941260589,-80.2213447601627));
#36199=CARTESIAN_POINT('Ctrl Pts',(36.7033971809565,13.8354628479784,-81.042322462261));
#36200=CARTESIAN_POINT('Ctrl Pts',(39.0888044266541,0.18001366521702,24.8306577616938));
#36201=CARTESIAN_POINT('Ctrl Pts',(39.088921603972,0.180018450330286,24.7817791815388));
#36202=CARTESIAN_POINT('Ctrl Pts',(39.0890444976507,0.180023467314007,24.7329016553144));
#36203=CARTESIAN_POINT('Ctrl Pts',(39.0904957807811,0.180082827660729,24.1823025865289));
#36204=CARTESIAN_POINT('Ctrl Pts',(39.091591381236,0.180114768840105,23.178184197145));
#36205=CARTESIAN_POINT('Ctrl Pts',(39.0941300425472,0.180178317661714,21.16959986221));
#36206=CARTESIAN_POINT('Ctrl Pts',(39.1037889658438,0.180575048338146,19.6654506295828));
#36207=CARTESIAN_POINT('Ctrl Pts',(39.1243579241454,0.1814843255736,18.4144015139445));
#36208=CARTESIAN_POINT('Ctrl Pts',(39.134218049248,0.181913975656292,17.9116384281828));
#36209=CARTESIAN_POINT('Ctrl Pts',(39.1589697243433,0.182982309247605,16.9076900689006));
#36210=CARTESIAN_POINT('Ctrl Pts',(39.2120662004859,0.185276856583134,15.1538859509933));
#36211=CARTESIAN_POINT('Ctrl Pts',(39.262582590445,0.187550367290034,13.6519990340237));
#36212=CARTESIAN_POINT('Ctrl Pts',(39.2943933523544,0.189141556091282,12.3973040853036));
#36213=CARTESIAN_POINT('Ctrl Pts',(39.3074164756704,0.189810834674528,11.8962594688207));
#36214=CARTESIAN_POINT('Ctrl Pts',(39.3340217961813,0.191236665964346,10.8942909995908));
#36215=CARTESIAN_POINT('Ctrl Pts',(39.3801836202682,0.193830901914628,9.14064171979857));
#36216=CARTESIAN_POINT('Ctrl Pts',(39.4126587791981,0.195783190608379,7.63555136734775));
#36217=CARTESIAN_POINT('Ctrl Pts',(39.4270720822274,0.196665431889854,6.50476503310077));
#36218=CARTESIAN_POINT('Ctrl Pts',(39.4300578896244,0.196857006372044,6.25445539718606));
#36219=CARTESIAN_POINT('Ctrl Pts',(39.4352574173322,0.197223852164122,5.75326871972413));
#36220=CARTESIAN_POINT('Ctrl Pts',(39.4424195833984,0.197815265041436,4.87478653411295));
#36221=CARTESIAN_POINT('Ctrl Pts',(39.4497248967473,0.198717316245392,3.11464776031493));
#36222=CARTESIAN_POINT('Ctrl Pts',(39.446414113801,0.198780500191082,1.60867348764858));
#36223=CARTESIAN_POINT('Ctrl Pts',(39.4418832112372,0.198236634498449,0.549912702370506));
#36224=CARTESIAN_POINT('Ctrl Pts',(39.4412881183038,0.198163774332367,0.4238385234358));
#36225=CARTESIAN_POINT('Ctrl Pts',(39.4398848802454,0.197990314496298,0.171867601864431));
#36226=CARTESIAN_POINT('Ctrl Pts',(39.4368979648691,0.197616824096262,-0.268602924693885));
#36227=CARTESIAN_POINT('Ctrl Pts',(39.431265864748,0.196911581478575,-0.896604365271294));
#36228=CARTESIAN_POINT('Ctrl Pts',(39.422825193491,0.195856232866555,-1.64880397032074));
#36229=CARTESIAN_POINT('Ctrl Pts',(39.4099826406263,0.194288855819704,-2.65032760331192));
#36230=CARTESIAN_POINT('Ctrl Pts',(39.3922023559894,0.192200604920921,-3.90095888032641));
#36231=CARTESIAN_POINT('Ctrl Pts',(39.3787476751708,0.190823568782034,-4.90238727422552));
#36232=CARTESIAN_POINT('Ctrl Pts',(39.3714100758577,0.1901561159036,-5.52939102985477));
#36233=CARTESIAN_POINT('Ctrl Pts',(39.3680558466428,0.189642076445195,-5.77731798908185));
#36234=CARTESIAN_POINT('Ctrl Pts',(39.359981910118,0.187821838661392,-6.27623871359611));
#36235=CARTESIAN_POINT('Ctrl Pts',(39.3430914959754,0.183047680568109,-7.15137509663719));
#36236=CARTESIAN_POINT('Ctrl Pts',(39.3157222785391,0.174582961782399,-8.40956360796454));
#36237=CARTESIAN_POINT('Ctrl Pts',(39.2965463492739,0.171255686152978,-9.67486595032553));
#36238=CARTESIAN_POINT('Ctrl Pts',(39.2939982741584,0.175420179906363,-10.563406034056));
#36239=CARTESIAN_POINT('Ctrl Pts',(39.296588702353,0.180221793186859,-11.0716016735842));
#36240=CARTESIAN_POINT('Ctrl Pts',(39.2993871951102,0.183532771774048,-11.325997245483));
#36241=CARTESIAN_POINT('Ctrl Pts',(39.302121938711,0.18640067801295,-11.5172370581218));
#36242=CARTESIAN_POINT('Ctrl Pts',(39.3040112231602,0.187809692523296,-11.6321437067357));
#36243=CARTESIAN_POINT('Ctrl Pts',(39.3079962810501,0.189421600017977,-11.8713598072385));
#36244=CARTESIAN_POINT('Ctrl Pts',(39.3155858132922,0.189066006906126,-12.2901555340803));
#36245=CARTESIAN_POINT('Ctrl Pts',(39.3387577077408,0.176925528543926,-13.3922563216631));
#36246=CARTESIAN_POINT('Ctrl Pts',(39.379396702992,0.152137055996183,-14.684633422449));
#36247=CARTESIAN_POINT('Ctrl Pts',(39.4445092732875,0.211426194910618,-16.0553377348217));
#36248=CARTESIAN_POINT('Ctrl Pts',(39.4835009488612,0.272356020893033,-16.7595291340688));
#36249=CARTESIAN_POINT('Ctrl Pts',(39.5186398233208,0.345587774340604,-17.3338818764406));
#36250=CARTESIAN_POINT('Ctrl Pts',(39.5374228354569,0.391497344347628,-17.6244377267164));
#36251=CARTESIAN_POINT('Ctrl Pts',(39.5518867733331,0.42961675462403,-17.8427244563372));
#36252=CARTESIAN_POINT('Ctrl Pts',(39.5621568573946,0.456200774441884,-17.9895396184138));
#36253=CARTESIAN_POINT('Ctrl Pts',(39.5849235986912,0.514329621361456,-18.2788108673388));
#36254=CARTESIAN_POINT('Ctrl Pts',(39.6107424637159,0.57959390861214,-18.5649718760519));
#36255=CARTESIAN_POINT('Ctrl Pts',(39.6389477430903,0.651132193211088,-18.8469173134216));
#36256=CARTESIAN_POINT('Ctrl Pts',(39.6574199768407,0.698304460318049,-19.0216247414068));
#36257=CARTESIAN_POINT('Ctrl Pts',(39.6726260334296,0.737409770914219,-19.1604034417413));
#36258=CARTESIAN_POINT('Ctrl Pts',(39.6880870527025,0.777395307511695,-19.2985535780004));
#36259=CARTESIAN_POINT('Ctrl Pts',(39.7315368481313,0.890845964556177,-19.6759094763723));
#36260=CARTESIAN_POINT('Ctrl Pts',(39.806426112475,1.09399290202479,-20.2792595435641));
#36261=CARTESIAN_POINT('Ctrl Pts',(39.9378740920715,1.48636765147355,-21.3147777341605));
#36262=CARTESIAN_POINT('Ctrl Pts',(40.0769022433718,1.99948303982382,-22.5469752458342));
#36263=CARTESIAN_POINT('Ctrl Pts',(40.1320094904387,2.35308133618794,-23.4873105317402));
#36264=CARTESIAN_POINT('Ctrl Pts',(40.142345779399,2.53113905762304,-24.0635136067293));
#36265=CARTESIAN_POINT('Ctrl Pts',(40.1400310526758,2.60755111479133,-24.3237713721114));
#36266=CARTESIAN_POINT('Ctrl Pts',(40.1308750507945,2.75349251735673,-24.8250400766174));
#36267=CARTESIAN_POINT('Ctrl Pts',(40.09763032855,3.00245212058905,-25.7090011208127));
#36268=CARTESIAN_POINT('Ctrl Pts',(40.0180962966849,3.33162945615507,-26.9560340181101));
#36269=CARTESIAN_POINT('Ctrl Pts',(39.902796621017,3.67815510636774,-28.4274121422462));
#36270=CARTESIAN_POINT('Ctrl Pts',(39.8343343846314,3.86829718954062,-29.379789457373));
#36271=CARTESIAN_POINT('Ctrl Pts',(39.804782197237,3.96216256771703,-29.9060565264981));
#36272=CARTESIAN_POINT('Ctrl Pts',(39.7980373400526,3.9828073368703,-30.0247988928929));
#36273=CARTESIAN_POINT('Ctrl Pts',(39.7841979689039,4.0223365292869,-30.2618473420464));
#36274=CARTESIAN_POINT('Ctrl Pts',(39.7589815634636,4.08744330929229,-30.678515203839));
#36275=CARTESIAN_POINT('Ctrl Pts',(39.7051855743335,4.20250038485936,-31.516812460355));
#36276=CARTESIAN_POINT('Ctrl Pts',(39.6381570765487,4.30598886780511,-32.4869174834327));
#36277=CARTESIAN_POINT('Ctrl Pts',(39.5706475585584,4.394788911564,-33.4685874803531));
#36278=CARTESIAN_POINT('Ctrl Pts',(39.5211677313474,4.45745183458457,-34.2107164143837));
#36279=CARTESIAN_POINT('Ctrl Pts',(39.4742297070753,4.51953514291641,-34.9585969492648));
#36280=CARTESIAN_POINT('Ctrl Pts',(39.4456483829112,4.56282399841279,-35.4611444533383));
#36281=CARTESIAN_POINT('Ctrl Pts',(39.4255847884175,4.59689962044293,-35.8402485675263));
#36282=CARTESIAN_POINT('Ctrl Pts',(39.4128475749602,4.61846189298307,-36.0852973690997));
#36283=CARTESIAN_POINT('Ctrl Pts',(39.3882931019907,4.66081433303966,-36.5800450924851));
#36284=CARTESIAN_POINT('Ctrl Pts',(39.3481419729083,4.73145168651063,-37.442542601468));
#36285=CARTESIAN_POINT('Ctrl Pts',(39.2768214004295,4.86023949916803,-39.1681386386344));
#36286=CARTESIAN_POINT('Ctrl Pts',(39.2248526929345,4.95191552713248,-40.6505048686668));
#36287=CARTESIAN_POINT('Ctrl Pts',(39.1845302849585,5.01293498501988,-41.7695811407451));
#36288=CARTESIAN_POINT('Ctrl Pts',(39.1757514004488,5.02577818599023,-42.0138900949182));
#36289=CARTESIAN_POINT('Ctrl Pts',(39.1628491891999,5.0440109556031,-42.3827068030056));
#36290=CARTESIAN_POINT('Ctrl Pts',(39.1502379767333,5.06115492093622,-42.751832091601));
#36291=CARTESIAN_POINT('Ctrl Pts',(39.1338144037273,5.08275736157524,-43.2453271230115));
#36292=CARTESIAN_POINT('Ctrl Pts',(39.1140240080415,5.10757619139148,-43.8638896754156));
#36293=CARTESIAN_POINT('Ctrl Pts',(39.091489653487,5.13464443295976,-44.6086804678692));
#36294=CARTESIAN_POINT('Ctrl Pts',(39.0737405500269,5.15559279761439,-45.2309635386264));
#36295=CARTESIAN_POINT('Ctrl Pts',(39.0600981040902,5.17176317841913,-45.7295320218957));
#36296=CARTESIAN_POINT('Ctrl Pts',(39.0501791060971,5.18371745533596,-46.1037852207575));
#36297=CARTESIAN_POINT('Ctrl Pts',(39.0405715239866,5.19559935655028,-46.4782873467315));
#36298=CARTESIAN_POINT('Ctrl Pts',(39.0281533890905,5.21149689504948,-46.9779392016722));
#36299=CARTESIAN_POINT('Ctrl Pts',(39.0193798005833,5.22362506194546,-47.3527953477327));
#36300=CARTESIAN_POINT('Ctrl Pts',(39.0108595472227,5.2361784215474,-47.728985458393));
#36301=CARTESIAN_POINT('Ctrl Pts',(39.005096807157,5.24605595530727,-47.9922131094468));
#36302=CARTESIAN_POINT('Ctrl Pts',(38.9937112535453,5.2687691243098,-48.5072542803165));
#36303=CARTESIAN_POINT('Ctrl Pts',(38.974450496436,5.31479689353639,-49.4003997772548));
#36304=CARTESIAN_POINT('Ctrl Pts',(38.9507961094573,5.38469715282765,-50.6399290110756));
#36305=CARTESIAN_POINT('Ctrl Pts',(38.9332314534559,5.4365038769883,-52.0730062175913));
#36306=CARTESIAN_POINT('Ctrl Pts',(38.9309692503806,5.42542938037497,-52.9896159479058));
#36307=CARTESIAN_POINT('Ctrl Pts',(38.9329698345153,5.39801919326263,-53.5501379417846));
#36308=CARTESIAN_POINT('Ctrl Pts',(38.9340646511458,5.384840725695,-53.7411566584974));
#36309=CARTESIAN_POINT('Ctrl Pts',(38.9385147088793,5.34116348643744,-54.1628515294699));
#36310=CARTESIAN_POINT('Ctrl Pts',(38.9513538843665,5.2250017558252,-54.9345356672974));
#36311=CARTESIAN_POINT('Ctrl Pts',(38.9924301618096,4.87821670055742,-56.6482573136251));
#36312=CARTESIAN_POINT('Ctrl Pts',(39.034695446014,4.56049109913903,-58.3762550348018));
#36313=CARTESIAN_POINT('Ctrl Pts',(39.0475405283856,4.62352423934888,-59.7440668955185));
#36314=CARTESIAN_POINT('Ctrl Pts',(39.0491105869675,4.63145905356436,-59.8881929790463));
#36315=CARTESIAN_POINT('Ctrl Pts',(39.0520556446838,4.65242359175444,-60.1874268764735));
#36316=CARTESIAN_POINT('Ctrl Pts',(39.0568083712244,4.70044200077084,-60.701577007053));
#36317=CARTESIAN_POINT('Ctrl Pts',(39.0647851026013,4.83986722574065,-61.7205682736498));
#36318=CARTESIAN_POINT('Ctrl Pts',(39.0709887180427,5.08325331232971,-62.8490477340757));
#36319=CARTESIAN_POINT('Ctrl Pts',(39.0752427482449,5.38432421645409,-63.9439111987074));
#36320=CARTESIAN_POINT('Ctrl Pts',(39.077120582972,5.57085697178719,-64.5463222893431));
#36321=CARTESIAN_POINT('Ctrl Pts',(39.0782501814497,5.70052797189769,-64.9424009107793));
#36322=CARTESIAN_POINT('Ctrl Pts',(39.0789768145255,5.78828008713039,-65.2049220123974));
#36323=CARTESIAN_POINT('Ctrl Pts',(39.0796760255791,5.87783519500164,-65.465282468161));
#36324=CARTESIAN_POINT('Ctrl Pts',(39.0802782205174,5.95744149860314,-65.6910332366747));
#36325=CARTESIAN_POINT('Ctrl Pts',(39.0806225187686,6.00324452874798,-65.8194497916867));
#36326=CARTESIAN_POINT('Ctrl Pts',(39.0811395675323,6.0722540117692,-66.0115179492368));
#36327=CARTESIAN_POINT('Ctrl Pts',(39.0815785188012,6.13030929947426,-66.1703178692351));
#36328=CARTESIAN_POINT('Ctrl Pts',(39.0823113015601,6.22722406914699,-66.4323128067553));
#36329=CARTESIAN_POINT('Ctrl Pts',(39.0823264257121,6.34542292308159,-66.7374653354443));
#36330=CARTESIAN_POINT('Ctrl Pts',(39.0823439741756,6.58825383385029,-67.3138435469778));
#36331=CARTESIAN_POINT('Ctrl Pts',(39.0814243175378,7.04892946372,-68.3023886475656));
#36332=CARTESIAN_POINT('Ctrl Pts',(39.0780104825526,8.05142233211918,-70.1599124261361));
#36333=CARTESIAN_POINT('Ctrl Pts',(39.0759796367523,8.92684404100238,-71.620429840862));
#36334=CARTESIAN_POINT('Ctrl Pts',(39.0778501765501,9.48039133128234,-72.6727733170531));
#36335=CARTESIAN_POINT('Ctrl Pts',(39.0777036163807,9.61612898152865,-72.930414174574));
#36336=CARTESIAN_POINT('Ctrl Pts',(39.0777332821649,9.88098261723943,-73.4319298126859));
#36337=CARTESIAN_POINT('Ctrl Pts',(39.0776408633731,10.2155893430233,-74.0636143082731));
#36338=CARTESIAN_POINT('Ctrl Pts',(39.0776063699703,10.6162577801302,-74.8174541772381));
#36339=CARTESIAN_POINT('Ctrl Pts',(39.0775123909014,11.4193164891573,-76.3249523442607));
#36340=CARTESIAN_POINT('Ctrl Pts',(39.0775007402611,12.088608941729,-77.5775747026988));
#36341=CARTESIAN_POINT('Ctrl Pts',(39.0775902789745,13.0565767107738,-79.3982809975936));
#36342=CARTESIAN_POINT('Ctrl Pts',(39.077555137614,13.4939144140808,-80.220915032169));
#36343=CARTESIAN_POINT('Ctrl Pts',(39.077555137614,13.9304360014702,-81.0418927342675));
#36344=CARTESIAN_POINT('Ctrl Pts',(40.9894004876467,0.280289965204604,24.8306664866128));
#36345=CARTESIAN_POINT('Ctrl Pts',(40.9895240781924,0.280296218581876,24.781788183931));
#36346=CARTESIAN_POINT('Ctrl Pts',(40.9896536969077,0.280302775699746,24.7329109288453));
#36347=CARTESIAN_POINT('Ctrl Pts',(40.9911843863448,0.280380328702297,24.1823154886843));
#36348=CARTESIAN_POINT('Ctrl Pts',(40.9923576072282,0.28042149746924,23.1782063197446));
#36349=CARTESIAN_POINT('Ctrl Pts',(40.9950876108615,0.280503393819463,21.1696270948689));
#36350=CARTESIAN_POINT('Ctrl Pts',(41.0052748446288,0.281021429451735,19.6654825420095));
#36351=CARTESIAN_POINT('Ctrl Pts',(41.0268800436286,0.282211470259995,18.4144326432552));
#36352=CARTESIAN_POINT('Ctrl Pts',(41.0372448640096,0.282775963518614,17.9116781675146));
#36353=CARTESIAN_POINT('Ctrl Pts',(41.0632779338851,0.284183692506976,16.907738953426));
#36354=CARTESIAN_POINT('Ctrl Pts',(41.1191186246586,0.287208855599439,15.1539438974559));
#36355=CARTESIAN_POINT('Ctrl Pts',(41.1721339589163,0.290184770111345,13.6520495013715));
#36356=CARTESIAN_POINT('Ctrl Pts',(41.2053038114973,0.292227955892151,12.3973231743278));
#36357=CARTESIAN_POINT('Ctrl Pts',(41.2188587008223,0.293083716779208,11.8962631232141));
#36358=CARTESIAN_POINT('Ctrl Pts',(41.2464748712986,0.294894702945755,10.8942726028637));
#36359=CARTESIAN_POINT('Ctrl Pts',(41.2942318035546,0.298165354622819,9.14059418922836));
#36360=CARTESIAN_POINT('Ctrl Pts',(41.3276780750111,0.300596870688662,7.6355550985603));
#36361=CARTESIAN_POINT('Ctrl Pts',(41.3424933819775,0.301687677932141,6.50481724059173));
#36362=CARTESIAN_POINT('Ctrl Pts',(41.3455455913616,0.301921698056121,6.25451349465145));
#36363=CARTESIAN_POINT('Ctrl Pts',(41.3508035537116,0.302358173568668,5.75333848629102));
#36364=CARTESIAN_POINT('Ctrl Pts',(41.3579025293381,0.303033911829633,4.87488551207728));
#36365=CARTESIAN_POINT('Ctrl Pts',(41.3646402494083,0.303988962607526,3.11477685097418));
#36366=CARTESIAN_POINT('Ctrl Pts',(41.3608998764056,0.303976963099249,1.60893402861812));
#36367=CARTESIAN_POINT('Ctrl Pts',(41.3568438589094,0.303443240710702,0.550188033900891));
#36368=CARTESIAN_POINT('Ctrl Pts',(41.3563108048481,0.303372710104812,0.424096199846747));
#36369=CARTESIAN_POINT('Ctrl Pts',(41.3550557054703,0.303205889073847,0.172103952862311));
#36370=CARTESIAN_POINT('Ctrl Pts',(41.3523853952267,0.30284952374001,-0.268403745043762));
#36371=CARTESIAN_POINT('Ctrl Pts',(41.3473498002463,0.302175450216627,-0.896402017998833));
#36372=CARTESIAN_POINT('Ctrl Pts',(41.3397676155733,0.301166611708825,-1.64861694312906));
#36373=CARTESIAN_POINT('Ctrl Pts',(41.32817131415,0.299636955694652,-2.65004641299644));
#36374=CARTESIAN_POINT('Ctrl Pts',(41.3119240978266,0.297526861549583,-3.90045072486229));
#36375=CARTESIAN_POINT('Ctrl Pts',(41.2993231966601,0.295985803859787,-4.90158298379786));
#36376=CARTESIAN_POINT('Ctrl Pts',(41.2922670659562,0.295180386852342,-5.52813800082197));
#36377=CARTESIAN_POINT('Ctrl Pts',(41.2888008321068,0.294128291656232,-5.76976692890284));
#36378=CARTESIAN_POINT('Ctrl Pts',(41.279775715755,0.289610906860302,-6.26180359560708));
#36379=CARTESIAN_POINT('Ctrl Pts',(41.2597292666415,0.276788673760391,-7.12814793049486));
#36380=CARTESIAN_POINT('Ctrl Pts',(41.2260339563164,0.252707693024928,-8.38969666255411));
#36381=CARTESIAN_POINT('Ctrl Pts',(41.2044754185102,0.243431514589407,-9.67758594137821));
#36382=CARTESIAN_POINT('Ctrl Pts',(41.2056667875271,0.257236423541392,-10.5928325387983));
#36383=CARTESIAN_POINT('Ctrl Pts',(41.2124055691996,0.272908132480897,-11.1192902137075));
#36384=CARTESIAN_POINT('Ctrl Pts',(41.2180245806747,0.283699034777166,-11.3838816397246));
#36385=CARTESIAN_POINT('Ctrl Pts',(41.2231896003388,0.293053885000704,-11.5830954853462));
#36386=CARTESIAN_POINT('Ctrl Pts',(41.2270321549076,0.298372571821632,-11.7004341390505));
#36387=CARTESIAN_POINT('Ctrl Pts',(41.2359213994023,0.308805474889505,-11.946101479798));
#36388=CARTESIAN_POINT('Ctrl Pts',(41.2545818424021,0.325521986599661,-12.3752423953399));
#36389=CARTESIAN_POINT('Ctrl Pts',(41.3164031698591,0.366888900265877,-13.503692810886));
#36390=CARTESIAN_POINT('Ctrl Pts',(41.4164791591404,0.432260449691268,-14.8218440732556));
#36391=CARTESIAN_POINT('Ctrl Pts',(41.5126853503333,0.611890804668134,-16.2117251793627));
#36392=CARTESIAN_POINT('Ctrl Pts',(41.5560798164476,0.739109737741911,-16.9227612255263));
#36393=CARTESIAN_POINT('Ctrl Pts',(41.5858226355929,0.867870462690142,-17.5004550174555));
#36394=CARTESIAN_POINT('Ctrl Pts',(41.5986631614551,0.941986198987689,-17.791774374434));
#36395=CARTESIAN_POINT('Ctrl Pts',(41.6073391088081,1.00132103356657,-18.01063350892));
#36396=CARTESIAN_POINT('Ctrl Pts',(41.612336789908,1.04566843983575,-18.168467840582));
#36397=CARTESIAN_POINT('Ctrl Pts',(41.6233445207234,1.13909153802182,-18.4708337039972));
#36398=CARTESIAN_POINT('Ctrl Pts',(41.6347930089352,1.24221991447412,-18.7692102602174));
#36399=CARTESIAN_POINT('Ctrl Pts',(41.6467691662253,1.35210739165747,-19.0592219699898));
#36400=CARTESIAN_POINT('Ctrl Pts',(41.6543765632466,1.42350899292141,-19.2381761479961));
#36401=CARTESIAN_POINT('Ctrl Pts',(41.6605374423642,1.48197440697328,-19.3796471871768));
#36402=CARTESIAN_POINT('Ctrl Pts',(41.6667347584479,1.54130043502988,-19.5201450978797));
#36403=CARTESIAN_POINT('Ctrl Pts',(41.683917789257,1.70774630290237,-19.9024388048089));
#36404=CARTESIAN_POINT('Ctrl Pts',(41.7125416786971,1.99501903901531,-20.5067211987056));
#36405=CARTESIAN_POINT('Ctrl Pts',(41.7625655220588,2.5198132595399,-21.5289948136643));
#36406=CARTESIAN_POINT('Ctrl Pts',(41.8200577472395,3.15307170736816,-22.7212180677817));
#36407=CARTESIAN_POINT('Ctrl Pts',(41.8488304236762,3.53774225526409,-23.5902816645653));
#36408=CARTESIAN_POINT('Ctrl Pts',(41.8532019455559,3.70939876819118,-24.1019133916231));
#36409=CARTESIAN_POINT('Ctrl Pts',(41.847559820479,3.78269989350591,-24.3424841016166));
#36410=CARTESIAN_POINT('Ctrl Pts',(41.8332034174373,3.91366476460714,-24.8058945510647));
#36411=CARTESIAN_POINT('Ctrl Pts',(41.7916431387842,4.11813149520393,-25.6354534315072));
#36412=CARTESIAN_POINT('Ctrl Pts',(41.6981196178867,4.34114005251492,-26.831589099475));
#36413=CARTESIAN_POINT('Ctrl Pts',(41.5529595890076,4.53989978629295,-28.2865892807906));
#36414=CARTESIAN_POINT('Ctrl Pts',(41.4586652482338,4.65218169883083,-29.2630855169144));
#36415=CARTESIAN_POINT('Ctrl Pts',(41.415417858304,4.71536033758119,-29.813734772255));
#36416=CARTESIAN_POINT('Ctrl Pts',(41.4062626735763,4.72786753785767,-29.928444759334));
#36417=CARTESIAN_POINT('Ctrl Pts',(41.3873736554326,4.75186071062575,-30.1629289810428));
#36418=CARTESIAN_POINT('Ctrl Pts',(41.3537867479734,4.78945139312945,-30.5728749307636));
#36419=CARTESIAN_POINT('Ctrl Pts',(41.2843093467636,4.85022130294728,-31.401795513503));
#36420=CARTESIAN_POINT('Ctrl Pts',(41.2025017262904,4.89369214843913,-32.3654256174241));
#36421=CARTESIAN_POINT('Ctrl Pts',(41.1231231912229,4.92654223259855,-33.3475404655346));
#36422=CARTESIAN_POINT('Ctrl Pts',(41.0660176057825,4.94955818888471,-34.0930821250591));
#36423=CARTESIAN_POINT('Ctrl Pts',(41.0124746989083,4.97473940354442,-34.8476683038026));
#36424=CARTESIAN_POINT('Ctrl Pts',(40.9798803467751,4.99552224079456,-35.3568512303255));
#36425=CARTESIAN_POINT('Ctrl Pts',(40.9567923276298,5.01363279690724,-35.7416656893073));
#36426=CARTESIAN_POINT('Ctrl Pts',(40.9418575375759,5.02486297072264,-35.9871898225954));
#36427=CARTESIAN_POINT('Ctrl Pts',(40.9134419266958,5.04715573300395,-36.4848538030037));
#36428=CARTESIAN_POINT('Ctrl Pts',(40.8675702390212,5.08425686877861,-37.3516034800416));
#36429=CARTESIAN_POINT('Ctrl Pts',(40.7892286304169,5.15295731690531,-39.0869665669963));
#36430=CARTESIAN_POINT('Ctrl Pts',(40.7388485386345,5.20226763694573,-40.5777014848992));
#36431=CARTESIAN_POINT('Ctrl Pts',(40.7030370031305,5.23646785505578,-41.7033865298728));
#36432=CARTESIAN_POINT('Ctrl Pts',(40.6951763053688,5.24370191326017,-41.9494781443332));
#36433=CARTESIAN_POINT('Ctrl Pts',(40.6835691587561,5.25381676112557,-42.3207839283218));
#36434=CARTESIAN_POINT('Ctrl Pts',(40.6722320093476,5.2632399079877,-42.6924276736823));
#36435=CARTESIAN_POINT('Ctrl Pts',(40.6575726542033,5.27498381439645,-43.1892030370711));
#36436=CARTESIAN_POINT('Ctrl Pts',(40.6403107816893,5.28830990789018,-43.8117997930508));
#36437=CARTESIAN_POINT('Ctrl Pts',(40.6219085941156,5.3027190798521,-44.561273695052));
#36438=CARTESIAN_POINT('Ctrl Pts',(40.6090109207754,5.31389855681178,-45.1873168583986));
#36439=CARTESIAN_POINT('Ctrl Pts',(40.6005058493631,5.32270348051234,-45.6888589250754));
#36440=CARTESIAN_POINT('Ctrl Pts',(40.5950885572115,5.32928921826061,-46.0652901742846));
#36441=CARTESIAN_POINT('Ctrl Pts',(40.5907117320026,5.33593953036712,-46.441917636326));
#36442=CARTESIAN_POINT('Ctrl Pts',(40.5863809911267,5.34499956462259,-46.9443480187945));
#36443=CARTESIAN_POINT('Ctrl Pts',(40.5848842655861,5.35211785123058,-47.3211462433141));
#36444=CARTESIAN_POINT('Ctrl Pts',(40.5847633692936,5.35964313775713,-47.6992573476703));
#36445=CARTESIAN_POINT('Ctrl Pts',(40.5851228662576,5.36600919820418,-47.9640771570023));
#36446=CARTESIAN_POINT('Ctrl Pts',(40.5875219759791,5.38199478861863,-48.4820864135602));
#36447=CARTESIAN_POINT('Ctrl Pts',(40.5958135821412,5.41659412432496,-49.3803699663312));
#36448=CARTESIAN_POINT('Ctrl Pts',(40.6177810554637,5.47173761809535,-50.6267686734295));
#36449=CARTESIAN_POINT('Ctrl Pts',(40.6554784269053,5.50882248832631,-52.0671302450754));
#36450=CARTESIAN_POINT('Ctrl Pts',(40.6851890519631,5.49197283852475,-52.9879476265502));
#36451=CARTESIAN_POINT('Ctrl Pts',(40.7043047716274,5.4623346564178,-53.5512015026042));
#36452=CARTESIAN_POINT('Ctrl Pts',(40.7126861506626,5.44807663353492,-53.7455801974626));
#36453=CARTESIAN_POINT('Ctrl Pts',(40.7316675370788,5.40330909356921,-54.1715151734727));
#36454=CARTESIAN_POINT('Ctrl Pts',(40.7700244549047,5.28798694743009,-54.9488391356619));
#36455=CARTESIAN_POINT('Ctrl Pts',(40.8592954416422,4.95345830992145,-56.6665193418863));
#36456=CARTESIAN_POINT('Ctrl Pts',(40.9364237216775,4.65839267261391,-58.3911774895459));
#36457=CARTESIAN_POINT('Ctrl Pts',(40.9617107797564,4.72643201987558,-59.7487986227702));
#36458=CARTESIAN_POINT('Ctrl Pts',(40.9646667376791,4.73489817031782,-59.8925588835541));
#36459=CARTESIAN_POINT('Ctrl Pts',(40.9699463811896,4.75676105502465,-60.1906378709165));
#36460=CARTESIAN_POINT('Ctrl Pts',(40.9776820611458,4.80591692343881,-60.7031777052071));
#36461=CARTESIAN_POINT('Ctrl Pts',(40.9876798094656,4.94608479796233,-61.719426669608));
#36462=CARTESIAN_POINT('Ctrl Pts',(40.9894597138152,5.18797722463457,-62.8463779555874));
#36463=CARTESIAN_POINT('Ctrl Pts',(40.9871287060037,5.4870542555106,-63.9408714139306));
#36464=CARTESIAN_POINT('Ctrl Pts',(40.9852447349333,5.67254707948159,-64.5434760398196));
#36465=CARTESIAN_POINT('Ctrl Pts',(40.9841506366498,5.80167198872239,-64.939834443487));
#36466=CARTESIAN_POINT('Ctrl Pts',(40.9834901228094,5.88909927246302,-65.2025816691557));
#36467=CARTESIAN_POINT('Ctrl Pts',(40.9829679493291,5.97841710390143,-65.4632274230487));
#36468=CARTESIAN_POINT('Ctrl Pts',(40.9827042111471,6.05788935343768,-65.6892791115769));
#36469=CARTESIAN_POINT('Ctrl Pts',(40.9826178379952,6.10364136767694,-65.8178824506503));
#36470=CARTESIAN_POINT('Ctrl Pts',(40.9825568597767,6.17259966365106,-66.0102450339768));
#36471=CARTESIAN_POINT('Ctrl Pts',(40.9826595793067,6.23067616599025,-66.1693213756176));
#36472=CARTESIAN_POINT('Ctrl Pts',(40.9830722826943,6.32770140186445,-66.4318038468455));
#36473=CARTESIAN_POINT('Ctrl Pts',(40.9826301895095,6.4457659668906,-66.7368360495315));
#36474=CARTESIAN_POINT('Ctrl Pts',(40.9819298733969,6.68848664498193,-67.3133239784796));
#36475=CARTESIAN_POINT('Ctrl Pts',(40.9799735479708,7.14895751891722,-68.3018674424394));
#36476=CARTESIAN_POINT('Ctrl Pts',(40.9755106159698,8.15122815727162,-70.1595000872727));
#36477=CARTESIAN_POINT('Ctrl Pts',(40.9737637925337,9.02664471902918,-71.6199599132457));
#36478=CARTESIAN_POINT('Ctrl Pts',(40.9759071636186,9.58020392439139,-72.6723061261848));
#36479=CARTESIAN_POINT('Ctrl Pts',(40.9756944292259,9.715932120259,-72.9299622522639));
#36480=CARTESIAN_POINT('Ctrl Pts',(40.9756840265696,9.9807790550013,-73.431497908536));
#36481=CARTESIAN_POINT('Ctrl Pts',(40.975534467898,10.3153885484625,-74.0632025611493));
#36482=CARTESIAN_POINT('Ctrl Pts',(40.9754859360213,10.7160678877822,-74.8170603952781));
#36483=CARTESIAN_POINT('Ctrl Pts',(40.9754043570265,11.519160529892,-76.3245809572268));
#36484=CARTESIAN_POINT('Ctrl Pts',(40.9754628439931,12.1885065742482,-77.577179230038));
#36485=CARTESIAN_POINT('Ctrl Pts',(40.9755662823054,13.1564677204213,-79.3978374532215));
#36486=CARTESIAN_POINT('Ctrl Pts',(40.9755178661405,13.5938174653931,-80.2204797593586));
#36487=CARTESIAN_POINT('Ctrl Pts',(40.9755178661405,14.0303390527825,-81.041457461457));
#36488=CARTESIAN_POINT('Ctrl Pts',(42.8889150787531,0.396068481711534,24.8306496888204));
#36489=CARTESIAN_POINT('Ctrl Pts',(42.8890452628421,0.396076880893202,24.7817708717695));
#36490=CARTESIAN_POINT('Ctrl Pts',(42.8891817953486,0.396085686243203,24.7328930807602));
#36491=CARTESIAN_POINT('Ctrl Pts',(42.890794111377,0.396189858653643,24.1822919985291));
#36492=CARTESIAN_POINT('Ctrl Pts',(42.8920520234772,0.396260174705627,23.1781818084037));
#36493=CARTESIAN_POINT('Ctrl Pts',(42.8949939595196,0.396414545731705,21.1695904333064));
#36494=CARTESIAN_POINT('Ctrl Pts',(42.9057228555591,0.397109674005268,19.6654453673117));
#36495=CARTESIAN_POINT('Ctrl Pts',(42.9283668323194,0.3986324421576,18.4143920639703));
#36496=CARTESIAN_POINT('Ctrl Pts',(42.9392378465306,0.399361893759621,17.9115963066885));
#36497=CARTESIAN_POINT('Ctrl Pts',(42.966554492716,0.401193810292415,16.9076316288254));
#36498=CARTESIAN_POINT('Ctrl Pts',(43.0251424311424,0.405129815060431,15.1538532275295));
#36499=CARTESIAN_POINT('Ctrl Pts',(43.0806374138684,0.408896580224321,13.6521151629944));
#36500=CARTESIAN_POINT('Ctrl Pts',(43.1151397951303,0.411298181410661,12.3975676992226));
#36501=CARTESIAN_POINT('Ctrl Pts',(43.1292134522289,0.412285537605512,11.8965778965405));
#36502=CARTESIAN_POINT('Ctrl Pts',(43.1578019090676,0.414315817551931,10.8946903077876));
#36503=CARTESIAN_POINT('Ctrl Pts',(43.2070698183594,0.417865337697373,9.14110268879431));
#36504=CARTESIAN_POINT('Ctrl Pts',(43.2413981262261,0.420381972370076,7.63604493878829));
#36505=CARTESIAN_POINT('Ctrl Pts',(43.2566055344275,0.421494236844582,6.5052257455832));
#36506=CARTESIAN_POINT('Ctrl Pts',(43.2597261675554,0.421724236178688,6.25499255122132));
#36507=CARTESIAN_POINT('Ctrl Pts',(43.265054561117,0.422124291502451,5.75388353416307));
#36508=CARTESIAN_POINT('Ctrl Pts',(43.2721266717543,0.422675761799587,4.87553172663561));
#36509=CARTESIAN_POINT('Ctrl Pts',(43.2784257741905,0.423242384308679,3.1153638161988));
#36510=CARTESIAN_POINT('Ctrl Pts',(43.2743206313889,0.423040356686762,1.60922688217153));
#36511=CARTESIAN_POINT('Ctrl Pts',(43.270646295444,0.422730846980912,0.550031961270142));
#36512=CARTESIAN_POINT('Ctrl Pts',(43.2701630446794,0.422689748586847,0.42386146716886));
#36513=CARTESIAN_POINT('Ctrl Pts',(43.2690200093843,0.422593013249137,0.171737673254688));
#36514=CARTESIAN_POINT('Ctrl Pts',(43.2665787031098,0.422386510342781,-0.26898297337776));
#36515=CARTESIAN_POINT('Ctrl Pts',(43.2619499985229,0.421999139749318,-0.897171771739731));
#36516=CARTESIAN_POINT('Ctrl Pts',(43.2549683112281,0.421409828411748,-1.64956913593561));
#36517=CARTESIAN_POINT('Ctrl Pts',(43.2442689204981,0.420519244475927,-2.65104599767104));
#36518=CARTESIAN_POINT('Ctrl Pts',(43.2292768897199,0.419285597860539,-3.90125975062038));
#36519=CARTESIAN_POINT('Ctrl Pts',(43.2175584682409,0.418332876173394,-4.90192971557075));
#36520=CARTESIAN_POINT('Ctrl Pts',(43.2109670967596,0.417750167584731,-5.52777393061073));
#36521=CARTESIAN_POINT('Ctrl Pts',(43.2075257487689,0.416170506748705,-5.76115476093335));
#36522=CARTESIAN_POINT('Ctrl Pts',(43.1980260184467,0.408531449786692,-6.24416404317574));
#36523=CARTESIAN_POINT('Ctrl Pts',(43.1761122863911,0.38592218775056,-7.09904072274838));
#36524=CARTESIAN_POINT('Ctrl Pts',(43.1386060796012,0.342232708468757,-8.36514300158209));
#36525=CARTESIAN_POINT('Ctrl Pts',(43.1163909787538,0.325771628148733,-9.68282259533749));
#36526=CARTESIAN_POINT('Ctrl Pts',(43.1211014388009,0.353483267386871,-10.6331225806478));
#36527=CARTESIAN_POINT('Ctrl Pts',(43.1312843977344,0.384576771432351,-11.1834256559264));
#36528=CARTESIAN_POINT('Ctrl Pts',(43.1391397568144,0.405937922333632,-11.4612218857337));
#36529=CARTESIAN_POINT('Ctrl Pts',(43.146200478672,0.424447290733482,-11.6708379761057));
#36530=CARTESIAN_POINT('Ctrl Pts',(43.1516607467815,0.435567740941252,-11.7951244626329));
#36531=CARTESIAN_POINT('Ctrl Pts',(43.1648288797801,0.459308919272857,-12.0539241755026));
#36532=CARTESIAN_POINT('Ctrl Pts',(43.1935227276973,0.502779393692827,-12.5042829261807));
#36533=CARTESIAN_POINT('Ctrl Pts',(43.2918119782271,0.629153848729037,-13.677793750993));
#36534=CARTESIAN_POINT('Ctrl Pts',(43.4467454125466,0.841220065238567,-15.019462467646));
#36535=CARTESIAN_POINT('Ctrl Pts',(43.5583435321655,1.17535730430707,-16.3968673604407));
#36536=CARTESIAN_POINT('Ctrl Pts',(43.5968235463072,1.37363963190595,-17.0927392942544));
#36537=CARTESIAN_POINT('Ctrl Pts',(43.6139629424047,1.55240211508456,-17.6539070332424));
#36538=CARTESIAN_POINT('Ctrl Pts',(43.6175553061863,1.64850035004579,-17.9356752158864));
#36539=CARTESIAN_POINT('Ctrl Pts',(43.6181384922512,1.72310238210498,-18.1473365030579));
#36540=CARTESIAN_POINT('Ctrl Pts',(43.6154303426995,1.7814430065369,-18.3099346755337));
#36541=CARTESIAN_POINT('Ctrl Pts',(43.6102846417711,1.90052004612951,-18.6147396344814));
#36542=CARTESIAN_POINT('Ctrl Pts',(43.602870007724,2.02979070845934,-18.9160782312125));
#36543=CARTESIAN_POINT('Ctrl Pts',(43.5946110817454,2.16471521744707,-19.2068265076608));
#36544=CARTESIAN_POINT('Ctrl Pts',(43.5889845057232,2.25153983815122,-19.3861334620883));
#36545=CARTESIAN_POINT('Ctrl Pts',(43.5843255425046,2.32208625553214,-19.5276182811613));
#36546=CARTESIAN_POINT('Ctrl Pts',(43.5795540667035,2.39335083839521,-19.6680602821549));
#36547=CARTESIAN_POINT('Ctrl Pts',(43.5660313407155,2.59193642338233,-20.0497805933487));
#36548=CARTESIAN_POINT('Ctrl Pts',(43.5425809194297,2.92788658122492,-20.65185956446));
#36549=CARTESIAN_POINT('Ctrl Pts',(43.502823575907,3.52399087311658,-21.6676436722937));
#36550=CARTESIAN_POINT('Ctrl Pts',(43.4667434267997,4.21004027159046,-22.8464385926046));
#36551=CARTESIAN_POINT('Ctrl Pts',(43.4612201547408,4.57433453371028,-23.6690393021299));
#36552=CARTESIAN_POINT('Ctrl Pts',(43.4555230860129,4.71666048256263,-24.1239260645268));
#36553=CARTESIAN_POINT('Ctrl Pts',(43.4463563974337,4.77865788443132,-24.3434559879189));
#36554=CARTESIAN_POINT('Ctrl Pts',(43.4252682870347,4.88049123337781,-24.7666198887204));
#36555=CARTESIAN_POINT('Ctrl Pts',(43.3726379146404,5.02212856520801,-25.533140126944));
#36556=CARTESIAN_POINT('Ctrl Pts',(43.2648052510907,5.13260362804228,-26.6650982276858));
#36557=CARTESIAN_POINT('Ctrl Pts',(43.1114452747013,5.19718538092319,-28.101595939478));
#36558=CARTESIAN_POINT('Ctrl Pts',(43.0185651733528,5.23924054246157,-29.1106253705117));
#36559=CARTESIAN_POINT('Ctrl Pts',(42.975411723984,5.27407710578951,-29.6911791890907));
#36560=CARTESIAN_POINT('Ctrl Pts',(42.9662152538132,5.27991788449142,-29.8027208427268));
#36561=CARTESIAN_POINT('Ctrl Pts',(42.9477927089147,5.29101628404784,-30.0366498359351));
#36562=CARTESIAN_POINT('Ctrl Pts',(42.91614290608,5.30639565662637,-30.443409397974));
#36563=CARTESIAN_POINT('Ctrl Pts',(42.8549443949215,5.3243938549592,-31.27046673341));
#36564=CARTESIAN_POINT('Ctrl Pts',(42.7909610327225,5.32097155220782,-32.2357129529905));
#36565=CARTESIAN_POINT('Ctrl Pts',(42.7334821383245,5.30738667036426,-33.2239095611256));
#36566=CARTESIAN_POINT('Ctrl Pts',(42.6935684398686,5.29586561496228,-33.9755125717022));
#36567=CARTESIAN_POINT('Ctrl Pts',(42.6568047178287,5.28701745361284,-34.7375684502777));
#36568=CARTESIAN_POINT('Ctrl Pts',(42.6342992001023,5.28573624978323,-35.2525662574588));
#36569=CARTESIAN_POINT('Ctrl Pts',(42.6180899591343,5.28762621774343,-35.6420378218769));
#36570=CARTESIAN_POINT('Ctrl Pts',(42.6076098316725,5.28875574807696,-35.8892618882715));
#36571=CARTESIAN_POINT('Ctrl Pts',(42.5880999328398,5.29084322749353,-36.3910947456908));
#36572=CARTESIAN_POINT('Ctrl Pts',(42.5575445668297,5.29403896822109,-37.2645761631907));
#36573=CARTESIAN_POINT('Ctrl Pts',(42.508580153775,5.29886526853191,-39.0133351135283));
#36574=CARTESIAN_POINT('Ctrl Pts',(42.4806557469868,5.30255980347641,-40.5146273530696));
#36575=CARTESIAN_POINT('Ctrl Pts',(42.4598279127556,5.3071617097167,-41.6480996481441));
#36576=CARTESIAN_POINT('Ctrl Pts',(42.4551630127186,5.30797458086478,-41.8956086156392));
#36577=CARTESIAN_POINT('Ctrl Pts',(42.4481045054802,5.3088012311728,-42.2692958029665));
#36578=CARTESIAN_POINT('Ctrl Pts',(42.4410806477194,5.3093045717839,-42.6433529512525));
#36579=CARTESIAN_POINT('Ctrl Pts',(42.4319011994612,5.3096803572806,-43.1434933004772));
#36580=CARTESIAN_POINT('Ctrl Pts',(42.4210267262244,5.30981707015305,-43.7704913693995));
#36581=CARTESIAN_POINT('Ctrl Pts',(42.4097481310677,5.31019237418895,-44.5255742396024));
#36582=CARTESIAN_POINT('Ctrl Pts',(42.4024993086791,5.3113033018907,-45.1565472183013));
#36583=CARTESIAN_POINT('Ctrl Pts',(42.398397320432,5.31304412980648,-45.6621764086441));
#36584=CARTESIAN_POINT('Ctrl Pts',(42.3962707885433,5.31487412266376,-46.0417486495161));
#36585=CARTESIAN_POINT('Ctrl Pts',(42.3951961796171,5.31732308733461,-46.421590372106));
#36586=CARTESIAN_POINT('Ctrl Pts',(42.3953084294671,5.32155303507846,-46.9283993184451));
#36587=CARTESIAN_POINT('Ctrl Pts',(42.3972711090846,5.32593157343998,-47.3085963361452));
#36588=CARTESIAN_POINT('Ctrl Pts',(42.4007224973633,5.33136402272493,-47.6901959858782));
#36589=CARTESIAN_POINT('Ctrl Pts',(42.4035392670192,5.33661313230962,-47.9583036263036));
#36590=CARTESIAN_POINT('Ctrl Pts',(42.4110068955218,5.35158369677478,-48.4818228843904));
#36591=CARTESIAN_POINT('Ctrl Pts',(42.4285681184022,5.38732529484062,-49.3888607634442));
#36592=CARTESIAN_POINT('Ctrl Pts',(42.4645238996338,5.45068060622925,-50.6443525671912));
#36593=CARTESIAN_POINT('Ctrl Pts',(42.5191045186815,5.50423224997189,-52.090968173697));
#36594=CARTESIAN_POINT('Ctrl Pts',(42.5587493674228,5.49944433627563,-53.0127660531225));
#36595=CARTESIAN_POINT('Ctrl Pts',(42.5830810557466,5.47708645406835,-53.5757228925217));
#36596=CARTESIAN_POINT('Ctrl Pts',(42.5934813918469,5.46548208533803,-53.7741404072612));
#36597=CARTESIAN_POINT('Ctrl Pts',(42.6163375594127,5.42734228091482,-54.2046414224714));
#36598=CARTESIAN_POINT('Ctrl Pts',(42.6609056441398,5.32617334286943,-54.9886206253845));
#36599=CARTESIAN_POINT('Ctrl Pts',(42.7600999447217,5.02873100100508,-56.7100594745335));
#36600=CARTESIAN_POINT('Ctrl Pts',(42.8416784052924,4.77265331680418,-58.4251679895872));
#36601=CARTESIAN_POINT('Ctrl Pts',(42.8685582931606,4.85151949519224,-59.7649378323137));
#36602=CARTESIAN_POINT('Ctrl Pts',(42.8717147900666,4.86106114166371,-59.9071771526114));
#36603=CARTESIAN_POINT('Ctrl Pts',(42.8772755002816,4.88475916132963,-60.2020395748597));
#36604=CARTESIAN_POINT('Ctrl Pts',(42.8852597130217,4.93611278948848,-60.7095740147467));
#36605=CARTESIAN_POINT('Ctrl Pts',(42.8948598975998,5.07736527871554,-61.717531467479));
#36606=CARTESIAN_POINT('Ctrl Pts',(42.8947058818154,5.31520926574883,-62.8393075875396));
#36607=CARTESIAN_POINT('Ctrl Pts',(42.8899738228548,5.60917737087592,-63.9323206739159));
#36608=CARTESIAN_POINT('Ctrl Pts',(42.8867547638397,5.79206068141782,-64.5353857364383));
#36609=CARTESIAN_POINT('Ctrl Pts',(42.8848516505248,5.91982637407483,-64.9325557510509));
#36610=CARTESIAN_POINT('Ctrl Pts',(42.8836781105316,6.00646819476968,-65.1959777609207));
#36611=CARTESIAN_POINT('Ctrl Pts',(42.8826910715564,6.09519584324768,-65.4574935630298));
#36612=CARTESIAN_POINT('Ctrl Pts',(42.882073521951,6.17437856538853,-65.6844780375945));
#36613=CARTESIAN_POINT('Ctrl Pts',(42.8818020470254,6.22003480886732,-65.8136632008719));
#36614=CARTESIAN_POINT('Ctrl Pts',(42.8814811499691,6.28892209624111,-66.0069454600372));
#36615=CARTESIAN_POINT('Ctrl Pts',(42.8814074477665,6.34709559252622,-66.1668929685478));
#36616=CARTESIAN_POINT('Ctrl Pts',(42.8815860469944,6.44451339963721,-66.4309135780944));
#36617=CARTESIAN_POINT('Ctrl Pts',(42.8808197276845,6.56224929149011,-66.7356096804903));
#36618=CARTESIAN_POINT('Ctrl Pts',(42.879603870637,6.80478971247199,-67.3124902879198));
#36619=CARTESIAN_POINT('Ctrl Pts',(42.8769176292393,7.26483872667389,-68.3011132441212));
#36620=CARTESIAN_POINT('Ctrl Pts',(42.8717509539682,8.26681183148849,-70.1591713034738));
#36621=CARTESIAN_POINT('Ctrl Pts',(42.8704039331454,9.14211299084993,-71.6194799934297));
#36622=CARTESIAN_POINT('Ctrl Pts',(42.8729303366428,9.69553181558638,-72.6717208012155));
#36623=CARTESIAN_POINT('Ctrl Pts',(42.872671040637,9.83124888405079,-72.9294152719817));
#36624=CARTESIAN_POINT('Ctrl Pts',(42.8726498197238,10.0960764052722,-73.4309878818336));
#36625=CARTESIAN_POINT('Ctrl Pts',(42.8724667652836,10.4306786414141,-74.0627388472059));
#36626=CARTESIAN_POINT('Ctrl Pts',(42.8724079265588,10.8313728766808,-74.8166344421457));
#36627=CARTESIAN_POINT('Ctrl Pts',(42.8723174539684,11.6345214397113,-76.3242063248351));
#36628=CARTESIAN_POINT('Ctrl Pts',(42.8724082948828,12.3039114944934,-77.5767660843792));
#36629=CARTESIAN_POINT('Ctrl Pts',(42.8725371303758,13.2718187211776,-79.3973294406647));
#36630=CARTESIAN_POINT('Ctrl Pts',(42.8724803799683,13.7091749119834,-80.2199918930716));
#36631=CARTESIAN_POINT('Ctrl Pts',(42.8724803799683,14.1456964993729,-81.0409695951699));
#36632=CARTESIAN_POINT('Ctrl Pts',(45.2615410902239,0.56892790035043,24.8305651889563));
#36633=CARTESIAN_POINT('Ctrl Pts',(45.2616788469112,0.568940634819196,24.7816836995172));
#36634=CARTESIAN_POINT('Ctrl Pts',(45.2618233193469,0.568953982664532,24.7328031712021));
#36635=CARTESIAN_POINT('Ctrl Pts',(45.2635294287772,0.569111836537056,24.182171251646));
#36636=CARTESIAN_POINT('Ctrl Pts',(45.2648761502202,0.569267594765854,23.1780307587285));
#36637=CARTESIAN_POINT('Ctrl Pts',(45.2680349536899,0.569648776159213,21.1693813670506));
#36638=CARTESIAN_POINT('Ctrl Pts',(45.2793879851866,0.570699976742199,19.6652259238777));
#36639=CARTESIAN_POINT('Ctrl Pts',(45.3032710496568,0.572756846002772,18.4141660720332));
#36640=CARTESIAN_POINT('Ctrl Pts',(45.3147346667214,0.573760233722913,17.9112035852143));
#36641=CARTESIAN_POINT('Ctrl Pts',(45.3435348065703,0.576309580397626,16.9071247576477));
#36642=CARTESIAN_POINT('Ctrl Pts',(45.4052930371425,0.581772246147764,15.153373130955));
#36643=CARTESIAN_POINT('Ctrl Pts',(45.4637836385732,0.586721616865389,13.6522000105154));
#36644=CARTESIAN_POINT('Ctrl Pts',(45.5001423649963,0.589381953653535,12.3983644658879));
#36645=CARTESIAN_POINT('Ctrl Pts',(45.5149663851462,0.590419644498185,11.8976615784835));
#36646=CARTESIAN_POINT('Ctrl Pts',(45.5450643958688,0.592375084156006,10.8961995239767));
#36647=CARTESIAN_POINT('Ctrl Pts',(45.5969137919438,0.595425285874441,9.14302073301941));
#36648=CARTESIAN_POINT('Ctrl Pts',(45.6330865439585,0.597206501163487,7.63778973696807));
#36649=CARTESIAN_POINT('Ctrl Pts',(45.649195554732,0.597936850330345,6.50655828026605));
#36650=CARTESIAN_POINT('Ctrl Pts',(45.6525038017218,0.598065911712743,6.2565298469245));
#36651=CARTESIAN_POINT('Ctrl Pts',(45.6581651586369,0.598202757340735,5.75558965548895));
#36652=CARTESIAN_POINT('Ctrl Pts',(45.6657159692505,0.598166373938152,4.87748020571371));
#36653=CARTESIAN_POINT('Ctrl Pts',(45.6725898914032,0.597314518635698,3.11704906257916));
#36654=CARTESIAN_POINT('Ctrl Pts',(45.6685138556414,0.596363463605718,1.60983243588655));
#36655=CARTESIAN_POINT('Ctrl Pts',(45.6648670787423,0.596698777805479,0.549183894455631));
#36656=CARTESIAN_POINT('Ctrl Pts',(45.6643767377126,0.596741852454767,0.422844585317528));
#36657=CARTESIAN_POINT('Ctrl Pts',(45.6631854073049,0.596842810294774,0.170395884188534));
#36658=CARTESIAN_POINT('Ctrl Pts',(45.6605762007441,0.597055391369542,-0.270858389192889));
#36659=CARTESIAN_POINT('Ctrl Pts',(45.6555185595092,0.59745299864442,-0.899651604736923));
#36660=CARTESIAN_POINT('Ctrl Pts',(45.6478526863677,0.598043494116904,-1.65265951815702));
#36661=CARTESIAN_POINT('Ctrl Pts',(45.6362144182659,0.598938873236841,-2.6545822356401));
#36662=CARTESIAN_POINT('Ctrl Pts',(45.6203390738768,0.6001363991942,-3.90474838480635));
#36663=CARTESIAN_POINT('Ctrl Pts',(45.6091854285172,0.601113517590204,-4.90501214468221));
#36664=CARTESIAN_POINT('Ctrl Pts',(45.6036109599966,0.601735734372738,-5.52991954576289));
#36665=CARTESIAN_POINT('Ctrl Pts',(45.6006260701382,0.599705001594043,-5.74990053211739));
#36666=CARTESIAN_POINT('Ctrl Pts',(45.5922312328804,0.588079076490982,-6.21835663472809));
#36667=CARTESIAN_POINT('Ctrl Pts',(45.5727483109654,0.551780036098233,-7.05491709802254));
#36668=CARTESIAN_POINT('Ctrl Pts',(45.5400013997707,0.478460081274117,-8.32900326154292));
#36669=CARTESIAN_POINT('Ctrl Pts',(45.5231832958852,0.451664466589343,-9.69595582677582));
#36670=CARTESIAN_POINT('Ctrl Pts',(45.5312025389088,0.50586094227689,-10.7037582186805));
#36671=CARTESIAN_POINT('Ctrl Pts',(45.5428511712477,0.565867706345419,-11.2928440346444));
#36672=CARTESIAN_POINT('Ctrl Pts',(45.5512011633854,0.606996131319551,-11.5918108244126));
#36673=CARTESIAN_POINT('Ctrl Pts',(45.5584957597952,0.642668846885867,-11.818204255642));
#36674=CARTESIAN_POINT('Ctrl Pts',(45.5644217032906,0.665914835001241,-11.9616068001552));
#36675=CARTESIAN_POINT('Ctrl Pts',(45.5792940450002,0.717572370742471,-12.2518202910108));
#36676=CARTESIAN_POINT('Ctrl Pts',(45.6125620818531,0.818496227435111,-12.7533551123664));
#36677=CARTESIAN_POINT('Ctrl Pts',(45.7296217181159,1.13198913807883,-14.026065678441));
#36678=CARTESIAN_POINT('Ctrl Pts',(45.8978143670819,1.62983274007774,-15.3630201137124));
#36679=CARTESIAN_POINT('Ctrl Pts',(45.9897284041635,2.17415695503713,-16.6449752515272));
#36680=CARTESIAN_POINT('Ctrl Pts',(46.0127724924086,2.44677387787828,-17.2789861198244));
#36681=CARTESIAN_POINT('Ctrl Pts',(46.014009774241,2.65995813440371,-17.7842112606934));
#36682=CARTESIAN_POINT('Ctrl Pts',(46.0086679235749,2.76381305873585,-18.0365081413938));
#36683=CARTESIAN_POINT('Ctrl Pts',(46.0020636910816,2.8403821505569,-18.2259250589348));
#36684=CARTESIAN_POINT('Ctrl Pts',(45.9916808054812,2.90249286496111,-18.3814549615846));
#36685=CARTESIAN_POINT('Ctrl Pts',(45.9710975209746,3.02404152226732,-18.6701480431207));
#36686=CARTESIAN_POINT('Ctrl Pts',(45.9455719114267,3.15243902328813,-18.9599438001704));
#36687=CARTESIAN_POINT('Ctrl Pts',(45.9176508537205,3.28290315146194,-19.2408978583454));
#36688=CARTESIAN_POINT('Ctrl Pts',(45.8989712480038,3.36582133959271,-19.4152139613651));
#36689=CARTESIAN_POINT('Ctrl Pts',(45.8835049784142,3.43255754172811,-19.5531457520749));
#36690=CARTESIAN_POINT('Ctrl Pts',(45.8676702465408,3.49960402086995,-19.6903699423378));
#36691=CARTESIAN_POINT('Ctrl Pts',(45.8227735189325,3.68494200445599,-20.064432073456));
#36692=CARTESIAN_POINT('Ctrl Pts',(45.7430985862396,3.99096854553774,-20.6596128083382));
#36693=CARTESIAN_POINT('Ctrl Pts',(45.5942885703309,4.51601048935695,-21.6699979055485));
#36694=CARTESIAN_POINT('Ctrl Pts',(45.4103878731843,5.08412976379374,-22.8411424812185));
#36695=CARTESIAN_POINT('Ctrl Pts',(45.2950650565968,5.35245248641301,-23.6349743610973));
#36696=CARTESIAN_POINT('Ctrl Pts',(45.2467980468575,5.45398333321623,-24.067533279953));
#36697=CARTESIAN_POINT('Ctrl Pts',(45.2273091162407,5.4958660759811,-24.2646722831934));
#36698=CARTESIAN_POINT('Ctrl Pts',(45.1894254535133,5.56227267487467,-24.6530195142001));
#36699=CARTESIAN_POINT('Ctrl Pts',(45.1258434031292,5.64619968427566,-25.3631834960375));
#36700=CARTESIAN_POINT('Ctrl Pts',(45.0483411872772,5.68371483506249,-26.4538242396258));
#36701=CARTESIAN_POINT('Ctrl Pts',(44.982611553414,5.65173052539128,-27.9001654232592));
#36702=CARTESIAN_POINT('Ctrl Pts',(44.9520931849871,5.6297158664385,-28.9494453654781));
#36703=CARTESIAN_POINT('Ctrl Pts',(44.9367550156712,5.63646385005425,-29.5611765185561));
#36704=CARTESIAN_POINT('Ctrl Pts',(44.9335181167507,5.63743428480618,-29.6742737992605));
#36705=CARTESIAN_POINT('Ctrl Pts',(44.9278510404227,5.638342727517,-29.9142297946347));
#36706=CARTESIAN_POINT('Ctrl Pts',(44.9198833000213,5.63695948677616,-30.329708561198));
#36707=CARTESIAN_POINT('Ctrl Pts',(44.9110674004613,5.62363210600333,-31.1738918958072));
#36708=CARTESIAN_POINT('Ctrl Pts',(44.9137412486688,5.58921702124126,-32.1537082145959));
#36709=CARTESIAN_POINT('Ctrl Pts',(44.9223411691491,5.54719748444965,-33.1515379207248));
#36710=CARTESIAN_POINT('Ctrl Pts',(44.9300993735876,5.51501168648089,-33.9075980489476));
#36711=CARTESIAN_POINT('Ctrl Pts',(44.9374788571034,5.48537115623183,-34.6713843255509));
#36712=CARTESIAN_POINT('Ctrl Pts',(44.9410536800944,5.46948092009931,-35.1856280500676));
#36713=CARTESIAN_POINT('Ctrl Pts',(44.9428188911152,5.45985012926995,-35.5739257705073));
#36714=CARTESIAN_POINT('Ctrl Pts',(44.9441592845655,5.45370335423039,-35.8236345693171));
#36715=CARTESIAN_POINT('Ctrl Pts',(44.9474689312597,5.44146970474214,-36.3284493873013));
#36716=CARTESIAN_POINT('Ctrl Pts',(44.954638159495,5.42069090277913,-37.207808874577));
#36717=CARTESIAN_POINT('Ctrl Pts',(44.9728639366942,5.38219060707259,-38.9666289774347));
#36718=CARTESIAN_POINT('Ctrl Pts',(44.9889923982044,5.35602496485368,-40.475866881289));
#36719=CARTESIAN_POINT('Ctrl Pts',(44.9953942460701,5.34195475745522,-41.6149580555204));
#36720=CARTESIAN_POINT('Ctrl Pts',(44.9966432669531,5.33880182227349,-41.8633103712195));
#36721=CARTESIAN_POINT('Ctrl Pts',(44.9980723578167,5.33383563704676,-42.2386233094709));
#36722=CARTESIAN_POINT('Ctrl Pts',(44.9991320563092,5.32880239446087,-42.6143713442757));
#36723=CARTESIAN_POINT('Ctrl Pts',(45.0001409655838,5.32214823876549,-43.1169950546398));
#36724=CARTESIAN_POINT('Ctrl Pts',(45.0008272884051,5.31428038683488,-43.7474178397165));
#36725=CARTESIAN_POINT('Ctrl Pts',(45.0012877427439,5.30658866273375,-44.5071452285576));
#36726=CARTESIAN_POINT('Ctrl Pts',(45.0018337011019,5.30251079913816,-45.1424179587062));
#36727=CARTESIAN_POINT('Ctrl Pts',(45.0026765863635,5.30120986027071,-45.6517210663674));
#36728=CARTESIAN_POINT('Ctrl Pts',(45.0035676018574,5.30133307305741,-46.0341809638089));
#36729=CARTESIAN_POINT('Ctrl Pts',(45.004789315115,5.30269163793039,-46.4170408268167));
#36730=CARTESIAN_POINT('Ctrl Pts',(45.0069605613675,5.30633439736445,-46.9280475789432));
#36731=CARTESIAN_POINT('Ctrl Pts',(45.0092740957863,5.31131329393198,-47.3116113548291));
#36732=CARTESIAN_POINT('Ctrl Pts',(45.0122199512957,5.31809960954172,-47.6967565980147));
#36733=CARTESIAN_POINT('Ctrl Pts',(45.0142487771965,5.32470451541727,-47.9686651663915));
#36734=CARTESIAN_POINT('Ctrl Pts',(45.0186202635373,5.34374882326917,-48.4982678866572));
#36735=CARTESIAN_POINT('Ctrl Pts',(45.0270592218719,5.38976720160193,-49.4147628842762));
#36736=CARTESIAN_POINT('Ctrl Pts',(45.0415152459114,5.4742819482128,-50.6789358291947));
#36737=CARTESIAN_POINT('Ctrl Pts',(45.0627150222664,5.55587055132917,-52.1287938500016));
#36738=CARTESIAN_POINT('Ctrl Pts',(45.0793287693003,5.56822594841936,-53.047487561374));
#36739=CARTESIAN_POINT('Ctrl Pts',(45.0903572481794,5.55517123050684,-53.6069076033485));
#36740=CARTESIAN_POINT('Ctrl Pts',(45.095008174112,5.54684870326733,-53.8080284349928));
#36741=CARTESIAN_POINT('Ctrl Pts',(45.1052426506285,5.5163187230399,-54.2407753067327));
#36742=CARTESIAN_POINT('Ctrl Pts',(45.1254358798707,5.4302233943472,-55.0281454420526));
#36743=CARTESIAN_POINT('Ctrl Pts',(45.1724795764375,5.16831036533154,-56.7499014534075));
#36744=CARTESIAN_POINT('Ctrl Pts',(45.2150148067347,4.94543213105456,-58.4564161559867));
#36745=CARTESIAN_POINT('Ctrl Pts',(45.2290442284572,5.03430264673683,-59.7812190912645));
#36746=CARTESIAN_POINT('Ctrl Pts',(45.2307700751369,5.04477387261886,-59.9217891402866));
#36747=CARTESIAN_POINT('Ctrl Pts',(45.2338887977571,5.07006301467846,-60.2134201034817));
#36748=CARTESIAN_POINT('Ctrl Pts',(45.238675751841,5.12325407856103,-60.7157796244941));
#36749=CARTESIAN_POINT('Ctrl Pts',(45.2456923316338,5.2651167467366,-61.7152143196181));
#36750=CARTESIAN_POINT('Ctrl Pts',(45.2490891950485,5.49881026242882,-62.8315081546936));
#36751=CARTESIAN_POINT('Ctrl Pts',(45.2501264528762,5.78767847262183,-63.9229172106332));
#36752=CARTESIAN_POINT('Ctrl Pts',(45.2502297313784,5.9679585610093,-64.5264409767567));
#36753=CARTESIAN_POINT('Ctrl Pts',(45.2502672432246,6.09437230432477,-64.9244570077799));
#36754=CARTESIAN_POINT('Ctrl Pts',(45.2502950068668,6.18022801163112,-65.1885868554451));
#36755=CARTESIAN_POINT('Ctrl Pts',(45.2503397288732,6.26837601445132,-65.4510184228235));
#36756=CARTESIAN_POINT('Ctrl Pts',(45.2504264703855,6.34726911685607,-65.6789906388552));
#36757=CARTESIAN_POINT('Ctrl Pts',(45.2504933615793,6.39282929282686,-65.8087930688745));
#36758=CARTESIAN_POINT('Ctrl Pts',(45.2506122890501,6.46164378698788,-66.0030523889319));
#36759=CARTESIAN_POINT('Ctrl Pts',(45.25075612524,6.51991763400415,-66.1639269551648));
#36760=CARTESIAN_POINT('Ctrl Pts',(45.2510572428287,6.61772521636265,-66.42959067944));
#36761=CARTESIAN_POINT('Ctrl Pts',(45.250305373501,6.73510925409277,-66.7339934534138));
#36762=CARTESIAN_POINT('Ctrl Pts',(45.2491046658658,6.97745770150096,-67.3113721716749));
#36763=CARTESIAN_POINT('Ctrl Pts',(45.2462900770827,7.43712178562395,-68.3002013325194));
#36764=CARTESIAN_POINT('Ctrl Pts',(45.2406999811744,8.43899343028371,-70.1588236954198));
#36765=CARTESIAN_POINT('Ctrl Pts',(45.2394106211059,9.31441939926999,-71.6189314434897));
#36766=CARTESIAN_POINT('Ctrl Pts',(45.2425965754305,9.86769517696103,-72.6709296364789));
#36767=CARTESIAN_POINT('Ctrl Pts',(45.2423191993804,10.0034062223631,-72.9286676159832));
#36768=CARTESIAN_POINT('Ctrl Pts',(45.2423416503406,10.2682178791503,-73.4302683407546));
#36769=CARTESIAN_POINT('Ctrl Pts',(45.2421536257646,10.6028211926649,-74.0620633849328));
#36770=CARTESIAN_POINT('Ctrl Pts',(45.242085184474,11.0035312252382,-74.8159927127367));
#36771=CARTESIAN_POINT('Ctrl Pts',(45.2419319021468,11.806733918079,-76.3236140381719));
#36772=CARTESIAN_POINT('Ctrl Pts',(45.241945137619,12.4761804875285,-77.5761354704948));
#36773=CARTESIAN_POINT('Ctrl Pts',(45.242101587135,13.4440512328765,-79.3966068480627));
#36774=CARTESIAN_POINT('Ctrl Pts',(45.2420325945625,13.8814194541,-80.219286814076));
#36775=CARTESIAN_POINT('Ctrl Pts',(45.2420325945625,14.3179410414895,-81.0402645161742));
#36776=CARTESIAN_POINT('Ctrl Pts',(48.1081629096089,0.821649737971831,24.8305516722305));
#36777=CARTESIAN_POINT('Ctrl Pts',(48.1083051106799,0.821665512614002,24.7816697400132));
#36778=CARTESIAN_POINT('Ctrl Pts',(48.1084542508962,0.821682047191606,24.7327887495063));
#36779=CARTESIAN_POINT('Ctrl Pts',(48.1102154710524,0.821877593257419,24.1821520591425));
#36780=CARTESIAN_POINT('Ctrl Pts',(48.1115212775643,0.822067622638418,23.1779988161717));
#36781=CARTESIAN_POINT('Ctrl Pts',(48.1145315886128,0.82253067075772,21.1693455405452));
#36782=CARTESIAN_POINT('Ctrl Pts',(48.1262541377065,0.823833454224577,19.6652159354718));
#36783=CARTESIAN_POINT('Ctrl Pts',(48.1513361492619,0.826397238176174,18.4141809690976));
#36784=CARTESIAN_POINT('Ctrl Pts',(48.1633375349177,0.827634154049395,17.9112422895808));
#36785=CARTESIAN_POINT('Ctrl Pts',(48.1934232679837,0.830752491267504,16.9071764083677));
#36786=CARTESIAN_POINT('Ctrl Pts',(48.2579574400696,0.837426380535316,15.1533897846288));
#36787=CARTESIAN_POINT('Ctrl Pts',(48.3196288164366,0.843613101712407,13.6521589092755));
#36788=CARTESIAN_POINT('Ctrl Pts',(48.3589766451503,0.84720841794872,12.3982627094592));
#36789=CARTESIAN_POINT('Ctrl Pts',(48.3751362078385,0.848644122282542,11.8975361584115));
#36790=CARTESIAN_POINT('Ctrl Pts',(48.408316262668,0.85146656541503,10.8960642754308));
#36791=CARTESIAN_POINT('Ctrl Pts',(48.4662441063241,0.856136247284531,9.14292354130284));
#36792=CARTESIAN_POINT('Ctrl Pts',(48.5074331513585,0.859208707164653,7.63783993867673));
#36793=CARTESIAN_POINT('Ctrl Pts',(48.5258835278248,0.860559046852656,6.50665095597728));
#36794=CARTESIAN_POINT('Ctrl Pts',(48.5297150707781,0.860822033143301,6.25656648324836));
#36795=CARTESIAN_POINT('Ctrl Pts',(48.5364301565456,0.861228582180177,5.75556890302458));
#36796=CARTESIAN_POINT('Ctrl Pts',(48.5458033902991,0.861660579302824,4.87740144016084));
#36797=CARTESIAN_POINT('Ctrl Pts',(48.5559513555871,0.861640785299128,3.11699919218724));
#36798=CARTESIAN_POINT('Ctrl Pts',(48.5529452741227,0.861041857828896,1.61024116156234));
#36799=CARTESIAN_POINT('Ctrl Pts',(48.5481105054958,0.861027202313047,0.550173774307906));
#36800=CARTESIAN_POINT('Ctrl Pts',(48.5474362951184,0.860991815439257,0.424583922210125));
#36801=CARTESIAN_POINT('Ctrl Pts',(48.5457145448333,0.860807080018294,0.173133236375915));
#36802=CARTESIAN_POINT('Ctrl Pts',(48.5417872384827,0.860211550198904,-0.266445020311065));
#36803=CARTESIAN_POINT('Ctrl Pts',(48.5339257686467,0.858773503319285,-0.893692784412118));
#36804=CARTESIAN_POINT('Ctrl Pts',(48.522073739976,0.856644410865061,-1.64619413650871));
#36805=CARTESIAN_POINT('Ctrl Pts',(48.5046013324232,0.854081092235267,-2.6492129028255));
#36806=CARTESIAN_POINT('Ctrl Pts',(48.4825692660466,0.85276775254009,-3.90422026265454));
#36807=CARTESIAN_POINT('Ctrl Pts',(48.4707732444907,0.856713137652613,-4.91207054954197));
#36808=CARTESIAN_POINT('Ctrl Pts',(48.4671393010514,0.86149262666492,-5.54219036151472));
#36809=CARTESIAN_POINT('Ctrl Pts',(48.4656067884327,0.860180392622072,-5.74936211818534));
#36810=CARTESIAN_POINT('Ctrl Pts',(48.4623097923741,0.847831923133697,-6.20557559939964));
#36811=CARTESIAN_POINT('Ctrl Pts',(48.4565916177326,0.805002100819759,-7.02772294470306));
#36812=CARTESIAN_POINT('Ctrl Pts',(48.4512469788016,0.714569697331715,-8.31560255293077));
#36813=CARTESIAN_POINT('Ctrl Pts',(48.4548341095276,0.694984707659641,-9.73891151249225));
#36814=CARTESIAN_POINT('Ctrl Pts',(48.4623957231446,0.797083729047604,-10.8079829560626));
#36815=CARTESIAN_POINT('Ctrl Pts',(48.4674917701297,0.901574142012729,-11.4354991653457));
#36816=CARTESIAN_POINT('Ctrl Pts',(48.470106832917,0.971216797118014,-11.75405631707));
#36817=CARTESIAN_POINT('Ctrl Pts',(48.4719992565174,1.03103416280663,-11.9955684581337));
#36818=CARTESIAN_POINT('Ctrl Pts',(48.4735291927885,1.07554025132908,-12.1651232691922));
#36819=CARTESIAN_POINT('Ctrl Pts',(48.4781552422806,1.1730200512042,-12.4927762950991));
#36820=CARTESIAN_POINT('Ctrl Pts',(48.4894872425771,1.36616230530559,-13.0522310028272));
#36821=CARTESIAN_POINT('Ctrl Pts',(48.5307186041763,1.95537885648209,-14.4052094810502));
#36822=CARTESIAN_POINT('Ctrl Pts',(48.5887220196266,2.75812147069433,-15.7094927741229));
#36823=CARTESIAN_POINT('Ctrl Pts',(48.6282107283581,3.45803842130641,-16.886201252276));
#36824=CARTESIAN_POINT('Ctrl Pts',(48.6396659611502,3.76548212629837,-17.4418553275266));
#36825=CARTESIAN_POINT('Ctrl Pts',(48.6402425297031,3.97331324839344,-17.8666263159455));
#36826=CARTESIAN_POINT('Ctrl Pts',(48.6368572480079,4.06259835365295,-18.0714978409077));
#36827=CARTESIAN_POINT('Ctrl Pts',(48.6324201979839,4.12337131538699,-18.2225466256693));
#36828=CARTESIAN_POINT('Ctrl Pts',(48.6234599825036,4.17457310433057,-18.3554234639945));
#36829=CARTESIAN_POINT('Ctrl Pts',(48.6055384286344,4.2684151651007,-18.6015930401312));
#36830=CARTESIAN_POINT('Ctrl Pts',(48.5821426501547,4.36198237974832,-18.8543700374838));
#36831=CARTESIAN_POINT('Ctrl Pts',(48.5554552185872,4.45142617483105,-19.102468133947));
#36832=CARTESIAN_POINT('Ctrl Pts',(48.5371054458672,4.50646811323497,-19.2579465929906));
#36833=CARTESIAN_POINT('Ctrl Pts',(48.5216094979501,4.5496941905776,-19.3817120668446));
#36834=CARTESIAN_POINT('Ctrl Pts',(48.5055367762919,4.59249085270137,-19.5053556776613));
#36835=CARTESIAN_POINT('Ctrl Pts',(48.4591184085395,4.70826835596746,-19.8443953493771));
#36836=CARTESIAN_POINT('Ctrl Pts',(48.3716444075612,4.88748874179812,-20.3934917640079));
#36837=CARTESIAN_POINT('Ctrl Pts',(48.1940359446113,5.177547094172,-21.3481529136738));
#36838=CARTESIAN_POINT('Ctrl Pts',(47.952649797924,5.48916359536832,-22.4914429176204));
#36839=CARTESIAN_POINT('Ctrl Pts',(47.8053384773659,5.67598473315981,-23.3545050106478));
#36840=CARTESIAN_POINT('Ctrl Pts',(47.7514393521066,5.76105663332847,-23.8814135650254));
#36841=CARTESIAN_POINT('Ctrl Pts',(47.7322571534499,5.78789453914611,-24.0780537403835));
#36842=CARTESIAN_POINT('Ctrl Pts',(47.7005023093246,5.83108303792997,-24.4891702584617));
#36843=CARTESIAN_POINT('Ctrl Pts',(47.6618055586385,5.87479485277564,-25.2313840795511));
#36844=CARTESIAN_POINT('Ctrl Pts',(47.6464171221041,5.86067949330697,-26.3718984732227));
#36845=CARTESIAN_POINT('Ctrl Pts',(47.661414214751,5.77854355816339,-27.855477204284));
#36846=CARTESIAN_POINT('Ctrl Pts',(47.6743009899302,5.73560298664759,-28.9198483764603));
#36847=CARTESIAN_POINT('Ctrl Pts',(47.6769703884333,5.73345395831467,-29.5380349652942));
#36848=CARTESIAN_POINT('Ctrl Pts',(47.677730957727,5.73299139472617,-29.6586445118241));
#36849=CARTESIAN_POINT('Ctrl Pts',(47.6798311884685,5.73185060628414,-29.9094857286936));
#36850=CARTESIAN_POINT('Ctrl Pts',(47.6849815494086,5.72942607414121,-30.3441072350726));
#36851=CARTESIAN_POINT('Ctrl Pts',(47.700527716251,5.72310267988212,-31.2186109898455));
#36852=CARTESIAN_POINT('Ctrl Pts',(47.7275269135778,5.71386386515405,-32.2190485708557));
#36853=CARTESIAN_POINT('Ctrl Pts',(47.7580119655262,5.70498183675231,-33.2226063845043));
#36854=CARTESIAN_POINT('Ctrl Pts',(47.781155007125,5.6989158027578,-33.9757793462538));
#36855=CARTESIAN_POINT('Ctrl Pts',(47.8031479086886,5.69373349890801,-34.7293605181625));
#36856=CARTESIAN_POINT('Ctrl Pts',(47.8160572371253,5.69105684482747,-35.2317860159007));
#36857=CARTESIAN_POINT('Ctrl Pts',(47.8247353087206,5.68939382962639,-35.609540706168));
#36858=CARTESIAN_POINT('Ctrl Pts',(47.8306340228238,5.68825044481764,-35.8607462274074));
#36859=CARTESIAN_POINT('Ctrl Pts',(47.8426692085815,5.68610487362212,-36.3636193365152));
#36860=CARTESIAN_POINT('Ctrl Pts',(47.8642093266045,5.6825643968688,-37.2418078118721));
#36861=CARTESIAN_POINT('Ctrl Pts',(47.9074925473444,5.67682038379547,-38.9956446854038));
#36862=CARTESIAN_POINT('Ctrl Pts',(47.9397934253085,5.67429448183844,-40.5002676053438));
#36863=CARTESIAN_POINT('Ctrl Pts',(47.9562383458176,5.67422694979235,-41.6352193462152));
#36864=CARTESIAN_POINT('Ctrl Pts',(47.9596673293312,5.67407137046705,-41.8832711523324));
#36865=CARTESIAN_POINT('Ctrl Pts',(47.9642819516124,5.67346258469438,-42.2577363877267));
#36866=CARTESIAN_POINT('Ctrl Pts',(47.9684051278346,5.6725968579029,-42.6326543517452));
#36867=CARTESIAN_POINT('Ctrl Pts',(47.9733073965259,5.67123657835768,-43.1339856927694));
#36868=CARTESIAN_POINT('Ctrl Pts',(47.9784245457529,5.66942716097581,-43.7625706582561));
#36869=CARTESIAN_POINT('Ctrl Pts',(47.9832885466205,5.66795036229496,-44.519662645377));
#36870=CARTESIAN_POINT('Ctrl Pts',(47.9865607651011,5.66802931005178,-45.1523870811576));
#36871=CARTESIAN_POINT('Ctrl Pts',(47.9888833465312,5.66933836408497,-45.6594096396806));
#36872=CARTESIAN_POINT('Ctrl Pts',(47.9905180716937,5.67104737260073,-46.0400472212068));
#36873=CARTESIAN_POINT('Ctrl Pts',(47.9920879918475,5.67359670763986,-46.4209707502011));
#36874=CARTESIAN_POINT('Ctrl Pts',(47.9941558677818,5.6782725369688,-46.9292389144956));
#36875=CARTESIAN_POINT('Ctrl Pts',(47.9957282263367,5.68336945103735,-47.310588569819));
#36876=CARTESIAN_POINT('Ctrl Pts',(47.997419450837,5.6897951869272,-47.6933797259154));
#36877=CARTESIAN_POINT('Ctrl Pts',(47.9983626666677,5.69589731397596,-47.9631838583766));
#36878=CARTESIAN_POINT('Ctrl Pts',(47.9997584629324,5.71311725397261,-48.4892701742966));
#36879=CARTESIAN_POINT('Ctrl Pts',(48.0011105924857,5.75402758165737,-49.4003616751971));
#36880=CARTESIAN_POINT('Ctrl Pts',(48.001392732923,5.82718212090007,-50.6594925731589));
#36881=CARTESIAN_POINT('Ctrl Pts',(48.0029449168854,5.89268556163609,-52.1071136716778));
#36882=CARTESIAN_POINT('Ctrl Pts',(48.0066715561608,5.89448880236947,-53.0268738746101));
#36883=CARTESIAN_POINT('Ctrl Pts',(48.0103335225241,5.87538737072239,-53.5876646128138));
#36884=CARTESIAN_POINT('Ctrl Pts',(48.011754185608,5.86483201236299,-53.7869517653904));
#36885=CARTESIAN_POINT('Ctrl Pts',(48.0150741130896,5.82900693060963,-54.2179462873563));
#36886=CARTESIAN_POINT('Ctrl Pts',(48.022185167171,5.73211236749528,-55.0027680394616));
#36887=CARTESIAN_POINT('Ctrl Pts',(48.0421436387735,5.44406860609416,-56.7238524205714));
#36888=CARTESIAN_POINT('Ctrl Pts',(48.0651576831185,5.19660981902691,-58.4361828195335));
#36889=CARTESIAN_POINT('Ctrl Pts',(48.0720910374252,5.27841745278614,-59.7710607470195));
#36890=CARTESIAN_POINT('Ctrl Pts',(48.0730274273232,5.28820917419853,-59.9126626681764));
#36891=CARTESIAN_POINT('Ctrl Pts',(48.074762526789,5.31234741047462,-60.2063371455483));
#36892=CARTESIAN_POINT('Ctrl Pts',(48.0776426768627,5.36420511218112,-60.7119239980234));
#36893=CARTESIAN_POINT('Ctrl Pts',(48.082684035864,5.5056353556155,-61.7166202365291));
#36894=CARTESIAN_POINT('Ctrl Pts',(48.0870397172443,5.74237823822888,-62.836120016294));
#36895=CARTESIAN_POINT('Ctrl Pts',(48.0902520185111,6.03501840008531,-63.9282554061026));
#36896=CARTESIAN_POINT('Ctrl Pts',(48.0916806212538,6.21723766416966,-64.5313278074762));
#36897=CARTESIAN_POINT('Ctrl Pts',(48.0924968060045,6.34467449486511,-64.9287081323857));
#36898=CARTESIAN_POINT('Ctrl Pts',(48.0930072141367,6.43113049693596,-65.1923259081768));
#36899=CARTESIAN_POINT('Ctrl Pts',(48.0934638368336,6.51973347346149,-65.4541179476157));
#36900=CARTESIAN_POINT('Ctrl Pts',(48.093826305083,6.59887034019588,-65.6814185423467));
#36901=CARTESIAN_POINT('Ctrl Pts',(48.0940229585271,6.64452074292956,-65.8108056498808));
#36902=CARTESIAN_POINT('Ctrl Pts',(48.0943068714726,6.7134200076301,-66.0044116477408));
#36903=CARTESIAN_POINT('Ctrl Pts',(48.0945234125043,6.77165114316365,-66.1646751482884));
#36904=CARTESIAN_POINT('Ctrl Pts',(48.0948355742627,6.8692273883312,-66.4292657126974));
#36905=CARTESIAN_POINT('Ctrl Pts',(48.0938628546097,6.98678481260344,-66.7337843123861));
#36906=CARTESIAN_POINT('Ctrl Pts',(48.0923533388769,7.22918372170347,-67.3107532529164));
#36907=CARTESIAN_POINT('Ctrl Pts',(48.0889709500158,7.68894236374983,-68.2993244133904));
#36908=CARTESIAN_POINT('Ctrl Pts',(48.0826493213745,8.69064771492824,-70.1574922702234));
#36909=CARTESIAN_POINT('Ctrl Pts',(48.0816614082155,9.56601796591246,-71.6177358852099));
#36910=CARTESIAN_POINT('Ctrl Pts',(48.085543824311,10.1195969025733,-72.6699364937867));
#36911=CARTESIAN_POINT('Ctrl Pts',(48.0852262519432,10.2552982719922,-72.9276374691411));
#36912=CARTESIAN_POINT('Ctrl Pts',(48.0852742552101,10.5201259865344,-73.4292146285592));
#36913=CARTESIAN_POINT('Ctrl Pts',(48.0850639260234,10.8547194339244,-74.0609721479818));
#36914=CARTESIAN_POINT('Ctrl Pts',(48.0849846417621,11.255413651863,-74.8148744822692));
#36915=CARTESIAN_POINT('Ctrl Pts',(48.0847855778271,12.0585639136749,-76.322457536711));
#36916=CARTESIAN_POINT('Ctrl Pts',(48.0847626220492,12.727963631217,-77.5750090039331));
#36917=CARTESIAN_POINT('Ctrl Pts',(48.0849474724551,13.6958717398979,-79.3955503463575));
#36918=CARTESIAN_POINT('Ctrl Pts',(48.0848656797528,14.1332269587404,-80.2182153328694));
#36919=CARTESIAN_POINT('Ctrl Pts',(48.0848656797527,14.5697485461299,-81.0391930349677));
#36920=CARTESIAN_POINT('Ctrl Pts',(50.9533414312497,1.12169071707122,24.8307796472817));
#36921=CARTESIAN_POINT('Ctrl Pts',(50.9534901764155,1.12170400700989,24.7819050388184));
#36922=CARTESIAN_POINT('Ctrl Pts',(50.953646180446,1.12171793023201,24.7330314904674));
#36923=CARTESIAN_POINT('Ctrl Pts',(50.9554886331472,1.12188331301799,24.1824813080586));
#36924=CARTESIAN_POINT('Ctrl Pts',(50.9568037911128,1.12192969540982,23.1784285843174));
#36925=CARTESIAN_POINT('Ctrl Pts',(50.9597987208206,1.12197063286745,21.1699357727456));
#36926=CARTESIAN_POINT('Ctrl Pts',(50.9720658618345,1.12308148654311,19.6658745886222));
#36927=CARTESIAN_POINT('Ctrl Pts',(50.9985674054642,1.1258424345923,18.4148754873179));
#36928=CARTESIAN_POINT('Ctrl Pts',(51.0112520755239,1.12712387007124,17.9124041050695));
#36929=CARTESIAN_POINT('Ctrl Pts',(51.0430661893009,1.13026647803661,16.908669997413));
#36930=CARTESIAN_POINT('Ctrl Pts',(51.1113415352745,1.13702052481593,15.1548258190807));
#36931=CARTESIAN_POINT('Ctrl Pts',(51.1766555159717,1.14402473626949,13.6521353545183));
#36932=CARTESIAN_POINT('Ctrl Pts',(51.2183870703309,1.14951437683359,12.3963078248059));
#36933=CARTESIAN_POINT('Ctrl Pts',(51.235547919752,1.15188249177447,11.8947916948912));
#36934=CARTESIAN_POINT('Ctrl Pts',(51.2708493229605,1.15710724391015,10.8921720267516));
#36935=CARTESIAN_POINT('Ctrl Pts',(51.3325796691209,1.16697185670893,9.13793432471975));
#36936=CARTESIAN_POINT('Ctrl Pts',(51.3764456484271,1.17473756336112,7.63357884883048));
#36937=CARTESIAN_POINT('Ctrl Pts',(51.3958297044449,1.17830805322875,6.50362118199104));
#36938=CARTESIAN_POINT('Ctrl Pts',(51.399831792773,1.17909826536064,6.25298174706968));
#36939=CARTESIAN_POINT('Ctrl Pts',(51.4067582655738,1.18064161126168,5.75153364143083));
#36940=CARTESIAN_POINT('Ctrl Pts',(51.4162015581993,1.18320978341969,4.87277716219866));
#36941=CARTESIAN_POINT('Ctrl Pts',(51.4255816469843,1.18742443036854,3.1132027445773));
#36942=CARTESIAN_POINT('Ctrl Pts',(51.4214908702378,1.18825181340388,1.61014543257973));
#36943=CARTESIAN_POINT('Ctrl Pts',(51.4169517383915,1.18646483593497,0.554414579386592));
#36944=CARTESIAN_POINT('Ctrl Pts',(51.4162990444907,1.18612419515353,0.431150301349283));
#36945=CARTESIAN_POINT('Ctrl Pts',(51.414576836636,1.18498720001586,0.182960482925087));
#36946=CARTESIAN_POINT('Ctrl Pts',(51.4105458029336,1.18190336825363,-0.25122582412197));
#36947=CARTESIAN_POINT('Ctrl Pts',(51.4023164143969,1.17502534226266,-0.873508478834048));
#36948=CARTESIAN_POINT('Ctrl Pts',(51.3899042130627,1.16476018757087,-1.62381014900014));
#36949=CARTESIAN_POINT('Ctrl Pts',(51.3718111002335,1.15118447847443,-2.62905519833519));
#36950=CARTESIAN_POINT('Ctrl Pts',(51.3498278423123,1.13925829229423,-3.8963786857563));
#36951=CARTESIAN_POINT('Ctrl Pts',(51.3406458821957,1.14652303269977,-4.92479211904332));
#36952=CARTESIAN_POINT('Ctrl Pts',(51.3399421908936,1.15995176317395,-5.57074037590767));
#36953=CARTESIAN_POINT('Ctrl Pts',(51.340422865111,1.16145463660532,-5.77681590727876));
#36954=CARTESIAN_POINT('Ctrl Pts',(51.3435729933499,1.15593856293644,-6.23612305337799));
#36955=CARTESIAN_POINT('Ctrl Pts',(51.3542468918493,1.12717613767436,-7.06406249501279));
#36956=CARTESIAN_POINT('Ctrl Pts',(51.3792368604421,1.06537306299732,-8.369130274419));
#36957=CARTESIAN_POINT('Ctrl Pts',(51.4015165176634,1.09673867444157,-9.82000774660129));
#36958=CARTESIAN_POINT('Ctrl Pts',(51.4020940342134,1.25347239491636,-10.9088988545458));
#36959=CARTESIAN_POINT('Ctrl Pts',(51.3955285966775,1.39472579842456,-11.545811398602));
#36960=CARTESIAN_POINT('Ctrl Pts',(51.3895806268922,1.4844434139763,-11.8680296924352));
#36961=CARTESIAN_POINT('Ctrl Pts',(51.383914084086,1.56008462901172,-12.112179992416));
#36962=CARTESIAN_POINT('Ctrl Pts',(51.3787279145381,1.6205720606341,-12.2947773166795));
#36963=CARTESIAN_POINT('Ctrl Pts',(51.368258303711,1.7496111927712,-12.6374803765801));
#36964=CARTESIAN_POINT('Ctrl Pts',(51.3480317930404,2.00341957948846,-13.217974870139));
#36965=CARTESIAN_POINT('Ctrl Pts',(51.2907428732227,2.75321150640632,-14.5831452083601));
#36966=CARTESIAN_POINT('Ctrl Pts',(51.225927360633,3.71750324084946,-15.8769039999603));
#36967=CARTESIAN_POINT('Ctrl Pts',(51.1888189023664,4.47867445749755,-17.016310178288));
#36968=CARTESIAN_POINT('Ctrl Pts',(51.1773022292006,4.78348110038424,-17.5314003101878));
#36969=CARTESIAN_POINT('Ctrl Pts',(51.1707092735231,4.96826566080369,-17.9033559813948));
#36970=CARTESIAN_POINT('Ctrl Pts',(51.167454142606,5.03970800806079,-18.0727299228598));
#36971=CARTESIAN_POINT('Ctrl Pts',(51.164531635878,5.08534082856387,-18.1933732667152));
#36972=CARTESIAN_POINT('Ctrl Pts',(51.158686915049,5.12560921907512,-18.3048956728737));
#36973=CARTESIAN_POINT('Ctrl Pts',(51.1474140167638,5.19548384510815,-18.5104348774773));
#36974=CARTESIAN_POINT('Ctrl Pts',(51.1330526263263,5.26178877509215,-18.7241888721022));
#36975=CARTESIAN_POINT('Ctrl Pts',(51.1169928924075,5.3213202709279,-18.9358738736356));
#36976=CARTESIAN_POINT('Ctrl Pts',(51.106045628326,5.35663218644509,-19.0696324172117));
#36977=CARTESIAN_POINT('Ctrl Pts',(51.0968633257256,5.38353229315555,-19.176746821762));
#36978=CARTESIAN_POINT('Ctrl Pts',(51.0873780885147,5.40965947712826,-19.284228081506));
#36979=CARTESIAN_POINT('Ctrl Pts',(51.0601357208132,5.4782355126452,-19.5808333938109));
#36980=CARTESIAN_POINT('Ctrl Pts',(51.0097682006336,5.57392886357255,-20.0728055332414));
#36981=CARTESIAN_POINT('Ctrl Pts',(50.9108460793228,5.70812600387179,-20.9684285024396));
#36982=CARTESIAN_POINT('Ctrl Pts',(50.7852015582486,5.82953407015952,-22.1344590978249));
#36983=CARTESIAN_POINT('Ctrl Pts',(50.714933507944,5.9081193598174,-23.1223234035987));
#36984=CARTESIAN_POINT('Ctrl Pts',(50.6888867590884,5.95993419098196,-23.7523420878989));
#36985=CARTESIAN_POINT('Ctrl Pts',(50.6801530113606,5.97429674512249,-23.9610482578587));
#36986=CARTESIAN_POINT('Ctrl Pts',(50.6669866029258,5.99623030389602,-24.4094074853637));
#36987=CARTESIAN_POINT('Ctrl Pts',(50.6546421899526,6.01225316678561,-25.2004327933986));
#36988=CARTESIAN_POINT('Ctrl Pts',(50.6606348920818,5.9876694949273,-26.3899162922315));
#36989=CARTESIAN_POINT('Ctrl Pts',(50.684070508213,5.92753779169261,-27.8927229744253));
#36990=CARTESIAN_POINT('Ctrl Pts',(50.6946061788475,5.90351872157916,-28.9465159456603));
#36991=CARTESIAN_POINT('Ctrl Pts',(50.6942533930777,5.90583493545004,-29.5519213155557));
#36992=CARTESIAN_POINT('Ctrl Pts',(50.6941500063852,5.90638391616636,-29.6768765989556));
#36993=CARTESIAN_POINT('Ctrl Pts',(50.6938822422483,5.90784051357585,-29.9320358454859));
#36994=CARTESIAN_POINT('Ctrl Pts',(50.6932605144441,5.9112054457662,-30.3754974172379));
#36995=CARTESIAN_POINT('Ctrl Pts',(50.6915185025583,5.92079918480938,-31.263020330328));
#36996=CARTESIAN_POINT('Ctrl Pts',(50.6889589583413,5.93649274814956,-32.2721514614383));
#36997=CARTESIAN_POINT('Ctrl Pts',(50.6869089393234,5.95321919885304,-33.2768405612288));
#36998=CARTESIAN_POINT('Ctrl Pts',(50.6859214788548,5.9654443733994,-34.0274257354587));
#36999=CARTESIAN_POINT('Ctrl Pts',(50.6858143945714,5.97664950657486,-34.7748619142795));
#37000=CARTESIAN_POINT('Ctrl Pts',(50.6865215248918,5.98289729769915,-35.270809249299));
#37001=CARTESIAN_POINT('Ctrl Pts',(50.6874148224352,5.98693541830552,-35.6429107206182));
#37002=CARTESIAN_POINT('Ctrl Pts',(50.6881567784551,5.98963164038767,-35.8943972430752));
#37003=CARTESIAN_POINT('Ctrl Pts',(50.690149158942,5.99481400010558,-36.3955360652468));
#37004=CARTESIAN_POINT('Ctrl Pts',(50.6948421222203,6.00354382030804,-37.2717999859299));
#37005=CARTESIAN_POINT('Ctrl Pts',(50.7075036636841,6.0193133879144,-39.0208470267752));
#37006=CARTESIAN_POINT('Ctrl Pts',(50.7193810329234,6.03097958496215,-40.5211261071569));
#37007=CARTESIAN_POINT('Ctrl Pts',(50.7239599109397,6.03914737439431,-41.6524715377103));
#37008=CARTESIAN_POINT('Ctrl Pts',(50.7248327254382,6.04072159743099,-41.9001262239914));
#37009=CARTESIAN_POINT('Ctrl Pts',(50.7258014357219,6.0426204028929,-42.2737142037943));
#37010=CARTESIAN_POINT('Ctrl Pts',(50.7264855424824,6.04412897403735,-42.6477530920575));
#37011=CARTESIAN_POINT('Ctrl Pts',(50.7270960595622,6.04576002792844,-43.1477711460489));
#37012=CARTESIAN_POINT('Ctrl Pts',(50.7274392596561,6.04731681597243,-43.7745513505533));
#37013=CARTESIAN_POINT('Ctrl Pts',(50.7276394978465,6.04918560965412,-44.5291835300691));
#37014=CARTESIAN_POINT('Ctrl Pts',(50.728013587656,6.05138931244001,-45.1596246848687));
#37015=CARTESIAN_POINT('Ctrl Pts',(50.7286772908058,6.05392767731241,-45.6647115464628));
#37016=CARTESIAN_POINT('Ctrl Pts',(50.7294097819383,6.05631812303614,-46.043824985108));
#37017=CARTESIAN_POINT('Ctrl Pts',(50.7304347944595,6.05929220166793,-46.4231538169804));
#37018=CARTESIAN_POINT('Ctrl Pts',(50.7322745208644,6.06417377448445,-46.9292097864943));
#37019=CARTESIAN_POINT('Ctrl Pts',(50.7342515600158,6.06899420874078,-47.3087654766622));
#37020=CARTESIAN_POINT('Ctrl Pts',(50.7367700662269,6.07482707758255,-47.6896844161141));
#37021=CARTESIAN_POINT('Ctrl Pts',(50.738506910136,6.08033525938134,-47.9575409942805));
#37022=CARTESIAN_POINT('Ctrl Pts',(50.7422933318491,6.09579700941191,-48.480488180462));
#37023=CARTESIAN_POINT('Ctrl Pts',(50.7497115606343,6.13228903674023,-49.3866831394771));
#37024=CARTESIAN_POINT('Ctrl Pts',(50.7626532705558,6.19631660090494,-50.6412054007193));
#37025=CARTESIAN_POINT('Ctrl Pts',(50.7817833437615,6.24948190302374,-52.0869414693963));
#37026=CARTESIAN_POINT('Ctrl Pts',(50.7964412108546,6.24364500559531,-53.0081849703579));
#37027=CARTESIAN_POINT('Ctrl Pts',(50.8059668372468,6.22038505455988,-53.5707667642567));
#37028=CARTESIAN_POINT('Ctrl Pts',(50.8098281664221,6.20841891443272,-53.7685903339318));
#37029=CARTESIAN_POINT('Ctrl Pts',(50.8183559178301,6.16924089319675,-54.1983830974968));
#37030=CARTESIAN_POINT('Ctrl Pts',(50.8352660608715,6.06557535448727,-54.9814807034273));
#37031=CARTESIAN_POINT('Ctrl Pts',(50.8757576452758,5.76089558294737,-56.7027655854137));
#37032=CARTESIAN_POINT('Ctrl Pts',(50.915202696598,5.496656556801,-58.4195020054296));
#37033=CARTESIAN_POINT('Ctrl Pts',(50.9266780699831,5.57317759167755,-59.76186377409));
#37034=CARTESIAN_POINT('Ctrl Pts',(50.9281192046078,5.58249120781337,-59.9043259989871));
#37035=CARTESIAN_POINT('Ctrl Pts',(50.9306575721336,5.60579772893743,-60.199648203657));
#37036=CARTESIAN_POINT('Ctrl Pts',(50.9344446796052,5.65668455670657,-60.7078780096647));
#37037=CARTESIAN_POINT('Ctrl Pts',(50.9395237932056,5.79772681030116,-61.7169001722879));
#37038=CARTESIAN_POINT('Ctrl Pts',(50.9409631986153,6.03650867779907,-62.8391384168951));
#37039=CARTESIAN_POINT('Ctrl Pts',(50.9403903714156,6.33165112392542,-63.9320017694799));
#37040=CARTESIAN_POINT('Ctrl Pts',(50.9397196268296,6.5151344126419,-64.5347751251295));
#37041=CARTESIAN_POINT('Ctrl Pts',(50.9392943502438,6.6432146121098,-64.9316744184796));
#37042=CARTESIAN_POINT('Ctrl Pts',(50.9390280538705,6.73003968502427,-65.1948956591214));
#37043=CARTESIAN_POINT('Ctrl Pts',(50.9387979083557,6.81890600506985,-65.4561826512923));
#37044=CARTESIAN_POINT('Ctrl Pts',(50.9386625642652,6.89816091629947,-65.6829423491466));
#37045=CARTESIAN_POINT('Ctrl Pts',(50.9386075263059,6.94384315526671,-65.8119923850296));
#37046=CARTESIAN_POINT('Ctrl Pts',(50.9385481095695,7.01275348645454,-66.0050655467178));
#37047=CARTESIAN_POINT('Ctrl Pts',(50.9385539169166,7.0709119129086,-66.1648250278806));
#37048=CARTESIAN_POINT('Ctrl Pts',(50.9386299432502,7.16825163935389,-66.4285222831356));
#37049=CARTESIAN_POINT('Ctrl Pts',(50.9371771379859,7.28589407409485,-66.7331431981932));
#37050=CARTESIAN_POINT('Ctrl Pts',(50.9349480821807,7.52824350147715,-67.3097807941499));
#37051=CARTESIAN_POINT('Ctrl Pts',(50.9304839220131,7.98795765327312,-68.2981545765869));
#37052=CARTESIAN_POINT('Ctrl Pts',(50.9230499483198,8.98941130983985,-70.1559656124676));
#37053=CARTESIAN_POINT('Ctrl Pts',(50.9225279560043,9.86477423134398,-71.6163124623247));
#37054=CARTESIAN_POINT('Ctrl Pts',(50.9269691274999,10.4186322923642,-72.6686895067181));
#37055=CARTESIAN_POINT('Ctrl Pts',(50.9265826329875,10.5543189518767,-72.9263627876053));
#37056=CARTESIAN_POINT('Ctrl Pts',(50.9266146411925,10.8191562096941,-73.4279248486359));
#37057=CARTESIAN_POINT('Ctrl Pts',(50.9263539659393,11.1537373969705,-74.0596550678505));
#37058=CARTESIAN_POINT('Ctrl Pts',(50.9262608462098,11.5544189999126,-74.8135377130594));
#37059=CARTESIAN_POINT('Ctrl Pts',(50.9260519983092,12.3575313978324,-76.3210909010518));
#37060=CARTESIAN_POINT('Ctrl Pts',(50.9260725792638,13.0269046053434,-77.5736611529628));
#37061=CARTESIAN_POINT('Ctrl Pts',(50.9262854692743,13.994843499425,-79.3942538055335));
#37062=CARTESIAN_POINT('Ctrl Pts',(50.9261906789385,14.432188480403,-80.2169075971474));
#37063=CARTESIAN_POINT('Ctrl Pts',(50.9261906789385,14.8687100677924,-81.0378852992458));
#37064=CARTESIAN_POINT('Ctrl Pts',(53.7933900457244,1.46776045816492,24.8308352754981));
#37065=CARTESIAN_POINT('Ctrl Pts',(53.7935558023369,1.46777693452164,24.7819623622908));
#37066=CARTESIAN_POINT('Ctrl Pts',(53.7937296500648,1.46779420749623,24.7330905217149));
#37067=CARTESIAN_POINT('Ctrl Pts',(53.7957820873193,1.46799885980126,24.1825607194227));
#37068=CARTESIAN_POINT('Ctrl Pts',(53.7974363241905,1.46805440166394,23.1785629963308));
#37069=CARTESIAN_POINT('Ctrl Pts',(53.8013468051514,1.4681064766261,21.1700925605004));
#37070=CARTESIAN_POINT('Ctrl Pts',(53.8149997112356,1.46947818305774,19.6659951252516));
#37071=CARTESIAN_POINT('Ctrl Pts',(53.8435465187149,1.47289619177137,18.4149454367022));
#37072=CARTESIAN_POINT('Ctrl Pts',(53.8572984478431,1.47451272292775,17.9124536811641));
#37073=CARTESIAN_POINT('Ctrl Pts',(53.8919413262604,1.47854467572399,16.9087243235041));
#37074=CARTESIAN_POINT('Ctrl Pts',(53.9662447392349,1.48724046780434,15.1549864169005));
#37075=CARTESIAN_POINT('Ctrl Pts',(54.0360578275002,1.49594448733498,13.6523890810428));
#37076=CARTESIAN_POINT('Ctrl Pts',(54.0783673965234,1.50212089892775,12.3965824151409));
#37077=CARTESIAN_POINT('Ctrl Pts',(54.0955109057738,1.50473227021855,11.8950679843877));
#37078=CARTESIAN_POINT('Ctrl Pts',(54.1299634716596,1.51033595700616,10.8924051910278));
#37079=CARTESIAN_POINT('Ctrl Pts',(54.1885336362757,1.52060807428504,9.1380099688249));
#37080=CARTESIAN_POINT('Ctrl Pts',(54.2284304999388,1.52838448388396,7.63358890128757));
#37081=CARTESIAN_POINT('Ctrl Pts',(54.2458099332916,1.53186915181062,6.50371998506009));
#37082=CARTESIAN_POINT('Ctrl Pts',(54.2492828248338,1.53260753050727,6.25318156712738));
#37083=CARTESIAN_POINT('Ctrl Pts',(54.2548893624485,1.53398291082753,5.75186684899312));
#37084=CARTESIAN_POINT('Ctrl Pts',(54.2614845506833,1.53611513211491,4.87329950549318));
#37085=CARTESIAN_POINT('Ctrl Pts',(54.2643379182555,1.53918683799225,3.11387145753909));
#37086=CARTESIAN_POINT('Ctrl Pts',(54.2573995536075,1.53965892925061,1.61025082422581));
#37087=CARTESIAN_POINT('Ctrl Pts',(54.2557401466238,1.53831993636108,0.554383333976408));
#37088=CARTESIAN_POINT('Ctrl Pts',(54.2554784051493,1.53796706602685,0.433343468268538));
#37089=CARTESIAN_POINT('Ctrl Pts',(54.2547074092181,1.53651660057094,0.187972714035989));
#37090=CARTESIAN_POINT('Ctrl Pts',(54.2527674583444,1.53221613334056,-0.241464717897606));
#37091=CARTESIAN_POINT('Ctrl Pts',(54.2485951736577,1.52207359627305,-0.859839813592334));
#37092=CARTESIAN_POINT('Ctrl Pts',(54.2423914644405,1.50688462047672,-1.60938817970641));
#37093=CARTESIAN_POINT('Ctrl Pts',(54.2337678506486,1.48744069579046,-2.61947890070179));
#37094=CARTESIAN_POINT('Ctrl Pts',(54.2247779796255,1.47379799843202,-3.9037136735069));
#37095=CARTESIAN_POINT('Ctrl Pts',(54.2236670013246,1.49465488165937,-4.95631565149324));
#37096=CARTESIAN_POINT('Ctrl Pts',(54.2262007246916,1.52391615578665,-5.62052064335219));
#37097=CARTESIAN_POINT('Ctrl Pts',(54.2284408836682,1.5312744986544,-5.83574805618841));
#37098=CARTESIAN_POINT('Ctrl Pts',(54.2358852067293,1.54106875243503,-6.30994821019978));
#37099=CARTESIAN_POINT('Ctrl Pts',(54.2557903425437,1.54633990549292,-7.15921814904195));
#37100=CARTESIAN_POINT('Ctrl Pts',(54.2949916301286,1.55411524466244,-8.48036615512007));
#37101=CARTESIAN_POINT('Ctrl Pts',(54.32054106886,1.6685408684751,-9.92444849402792));
#37102=CARTESIAN_POINT('Ctrl Pts',(54.3125401600623,1.87358765716265,-10.9933226813509));
#37103=CARTESIAN_POINT('Ctrl Pts',(54.2978284242317,2.03650352741588,-11.6154425790896));
#37104=CARTESIAN_POINT('Ctrl Pts',(54.2867299786695,2.1346535662497,-11.9293507756478));
#37105=CARTESIAN_POINT('Ctrl Pts',(54.2767660804809,2.21568134921396,-12.1672221744866));
#37106=CARTESIAN_POINT('Ctrl Pts',(54.2674574226275,2.2821125766626,-12.3507234833108));
#37107=CARTESIAN_POINT('Ctrl Pts',(54.2483381988399,2.42123276556235,-12.6917517760357));
#37108=CARTESIAN_POINT('Ctrl Pts',(54.2107430146763,2.69229588585007,-13.2699573998623));
#37109=CARTESIAN_POINT('Ctrl Pts',(54.1030026490132,3.48048290088805,-14.6261114160487));
#37110=CARTESIAN_POINT('Ctrl Pts',(53.9770524318318,4.47675841913185,-15.9131448940457));
#37111=CARTESIAN_POINT('Ctrl Pts',(53.8895858536794,5.23570734582795,-17.0367054326486));
#37112=CARTESIAN_POINT('Ctrl Pts',(53.8577495999718,5.52846547248409,-17.537705551924));
#37113=CARTESIAN_POINT('Ctrl Pts',(53.8401597088712,5.69780007321343,-17.8913214151969));
#37114=CARTESIAN_POINT('Ctrl Pts',(53.8336891383102,5.7603034739084,-18.0485034836148));
#37115=CARTESIAN_POINT('Ctrl Pts',(53.8294760043339,5.79918675991689,-18.158710746978));
#37116=CARTESIAN_POINT('Ctrl Pts',(53.8242922855261,5.83336507551644,-18.2601454739158));
#37117=CARTESIAN_POINT('Ctrl Pts',(53.8149854102744,5.89151040863206,-18.4477890497773));
#37118=CARTESIAN_POINT('Ctrl Pts',(53.804751226398,5.94525410329329,-18.643782080729));
#37119=CARTESIAN_POINT('Ctrl Pts',(53.7944218852403,5.99197085515748,-18.8393751415726));
#37120=CARTESIAN_POINT('Ctrl Pts',(53.7877788512421,6.01906761193404,-18.9636069738138));
#37121=CARTESIAN_POINT('Ctrl Pts',(53.782421418259,6.0393069256326,-19.0635424337132));
#37122=CARTESIAN_POINT('Ctrl Pts',(53.7770185795907,6.05869657425846,-19.1641225276032));
#37123=CARTESIAN_POINT('Ctrl Pts',(53.7620375678208,6.1084862383097,-19.4429606103963));
#37124=CARTESIAN_POINT('Ctrl Pts',(53.7369858902576,6.17161183200816,-19.913031472546));
#37125=CARTESIAN_POINT('Ctrl Pts',(53.6934032828376,6.24247369029086,-20.7923851127138));
#37126=CARTESIAN_POINT('Ctrl Pts',(53.6443264410865,6.27322765229458,-21.9784206991347));
#37127=CARTESIAN_POINT('Ctrl Pts',(53.6158452945417,6.29562851322709,-23.0213542879479));
#37128=CARTESIAN_POINT('Ctrl Pts',(53.6028045669425,6.3324843283351,-23.6991333497469));
#37129=CARTESIAN_POINT('Ctrl Pts',(53.5989325122426,6.3427047066574,-23.9180599088565));
#37130=CARTESIAN_POINT('Ctrl Pts',(53.593912842268,6.35920858361621,-24.3890009403331));
#37131=CARTESIAN_POINT('Ctrl Pts',(53.5922803110389,6.37398863179943,-25.2107803923371));
#37132=CARTESIAN_POINT('Ctrl Pts',(53.6044873488314,6.36525379676015,-26.4264350231629));
#37133=CARTESIAN_POINT('Ctrl Pts',(53.6246410636365,6.33362942494894,-27.9280681877689));
#37134=CARTESIAN_POINT('Ctrl Pts',(53.6299854794189,6.31962103324006,-28.9596498518069));
#37135=CARTESIAN_POINT('Ctrl Pts',(53.6275904114776,6.31989336884689,-29.5468372150394));
#37136=CARTESIAN_POINT('Ctrl Pts',(53.6269860187601,6.31996858519039,-29.6714025389371));
#37137=CARTESIAN_POINT('Ctrl Pts',(53.6254590818797,6.32014848759483,-29.9238618153255));
#37138=CARTESIAN_POINT('Ctrl Pts',(53.6220079088107,6.3205644028427,-30.3639320559427));
#37139=CARTESIAN_POINT('Ctrl Pts',(53.6124311150174,6.3217368740878,-31.2451434211193));
#37140=CARTESIAN_POINT('Ctrl Pts',(53.5972125571305,6.32385099937355,-32.2504375748529));
#37141=CARTESIAN_POINT('Ctrl Pts',(53.5815818658841,6.32639839639458,-33.2541968516878));
#37142=CARTESIAN_POINT('Ctrl Pts',(53.5705914377351,6.32840811557273,-34.0057485724029));
#37143=CARTESIAN_POINT('Ctrl Pts',(53.5611950937924,6.33045238168674,-34.7557043762172));
#37144=CARTESIAN_POINT('Ctrl Pts',(53.5566338912338,6.33171857726557,-35.2544416320367));
#37145=CARTESIAN_POINT('Ctrl Pts',(53.5540894921551,6.33258439456126,-35.62899651519));
#37146=CARTESIAN_POINT('Ctrl Pts',(53.5525471172708,6.33314112082372,-35.8803061566907));
#37147=CARTESIAN_POINT('Ctrl Pts',(53.5500721543656,6.33421910065837,-36.3821494728191));
#37148=CARTESIAN_POINT('Ctrl Pts',(53.5470779574238,6.33608019574568,-37.2591841034828));
#37149=CARTESIAN_POINT('Ctrl Pts',(53.5455939632914,6.33963405453553,-39.010344004449));
#37150=CARTESIAN_POINT('Ctrl Pts',(53.5473413277377,6.34321066214864,-40.5124796418315));
#37151=CARTESIAN_POINT('Ctrl Pts',(53.5461525409861,6.34663038394612,-41.6452339196233));
#37152=CARTESIAN_POINT('Ctrl Pts',(53.5458092971824,6.34719150048698,-41.8930044393535));
#37153=CARTESIAN_POINT('Ctrl Pts',(53.5450391848878,6.34762365510011,-42.2669036709439));
#37154=CARTESIAN_POINT('Ctrl Pts',(53.5440878423451,6.3477365541993,-42.641256929972));
#37155=CARTESIAN_POINT('Ctrl Pts',(53.5426497076838,6.34760526561751,-43.1417682640508));
#37156=CARTESIAN_POINT('Ctrl Pts',(53.5406937376445,6.34716654364843,-43.7692597722806));
#37157=CARTESIAN_POINT('Ctrl Pts',(53.5385753322947,6.3470316395596,-44.5249255638812));
#37158=CARTESIAN_POINT('Ctrl Pts',(53.5374029285173,6.3479421810165,-45.1563791848156));
#37159=CARTESIAN_POINT('Ctrl Pts',(53.537080678892,6.3497072495962,-45.6623565642534));
#37160=CARTESIAN_POINT('Ctrl Pts',(53.5371991985082,6.35165485412208,-46.0421851773418));
#37161=CARTESIAN_POINT('Ctrl Pts',(53.537740460393,6.35433187328488,-46.4222756890038));
#37162=CARTESIAN_POINT('Ctrl Pts',(53.5391068127767,6.35902267550402,-46.9294038353548));
#37163=CARTESIAN_POINT('Ctrl Pts',(53.5409466755713,6.36394510200445,-47.309844093545));
#37164=CARTESIAN_POINT('Ctrl Pts',(53.5434576323681,6.37006087923182,-47.6916881569233));
#37165=CARTESIAN_POINT('Ctrl Pts',(53.5452697516784,6.37585970371762,-47.9603598894965));
#37166=CARTESIAN_POINT('Ctrl Pts',(53.5495080101578,6.39220030227994,-48.4846658279806));
#37167=CARTESIAN_POINT('Ctrl Pts',(53.5584241102997,6.43094312194704,-49.392940886843));
#37168=CARTESIAN_POINT('Ctrl Pts',(53.5752247654874,6.49972793378469,-50.6493978653959));
#37169=CARTESIAN_POINT('Ctrl Pts',(53.6002412032182,6.55964718560622,-52.0960064010703));
#37170=CARTESIAN_POINT('Ctrl Pts',(53.6188318440274,6.55826208339829,-53.016900991182));
#37171=CARTESIAN_POINT('Ctrl Pts',(53.6304012698521,6.53753738298099,-53.5790092140046));
#37172=CARTESIAN_POINT('Ctrl Pts',(53.6351414755496,6.5264928871424,-53.7776482020704));
#37173=CARTESIAN_POINT('Ctrl Pts',(53.6455211434246,6.48948253197531,-54.2082493994463));
#37174=CARTESIAN_POINT('Ctrl Pts',(53.6659362726158,6.3902315350268,-54.9924992521234));
#37175=CARTESIAN_POINT('Ctrl Pts',(53.7135446693902,6.09630159129917,-56.7140924202626));
#37176=CARTESIAN_POINT('Ctrl Pts',(53.7588224207161,5.84296406092708,-58.4280717306404));
#37177=CARTESIAN_POINT('Ctrl Pts',(53.7715265525107,5.92253095411376,-59.7656862880565));
#37178=CARTESIAN_POINT('Ctrl Pts',(53.7731098754717,5.93214130941908,-59.9076934093206));
#37179=CARTESIAN_POINT('Ctrl Pts',(53.7758477299353,5.95594634872873,-60.2020912589034));
#37180=CARTESIAN_POINT('Ctrl Pts',(53.7798031476919,6.00740754199605,-60.7088605570528));
#37181=CARTESIAN_POINT('Ctrl Pts',(53.7845465584611,6.14860899244848,-61.7154641107162));
#37182=CARTESIAN_POINT('Ctrl Pts',(53.7844974228809,6.38599143747069,-62.8361597252832));
#37183=CARTESIAN_POINT('Ctrl Pts',(53.782103117691,6.67941249081592,-63.9285556400314));
#37184=CARTESIAN_POINT('Ctrl Pts',(53.7804151278263,6.86200279820823,-64.5314370204442));
#37185=CARTESIAN_POINT('Ctrl Pts',(53.7793721012228,6.98960307318282,-64.9285492426614));
#37186=CARTESIAN_POINT('Ctrl Pts',(53.7787120750193,7.07614332109049,-65.1919500989433));
#37187=CARTESIAN_POINT('Ctrl Pts',(53.7781246786664,7.16478566240634,-65.4534694683211));
#37188=CARTESIAN_POINT('Ctrl Pts',(53.7777139998342,7.24391099674154,-65.6804796823406));
#37189=CARTESIAN_POINT('Ctrl Pts',(53.7775140585173,7.28954006843651,-65.8096859661748));
#37190=CARTESIAN_POINT('Ctrl Pts',(53.7772499665168,7.35839217565976,-66.0030060923424));
#37191=CARTESIAN_POINT('Ctrl Pts',(53.7771150576058,7.41654978603355,-66.1629991209093));
#37192=CARTESIAN_POINT('Ctrl Pts',(53.7769979165408,7.51395562087826,-66.427107494371));
#37193=CARTESIAN_POINT('Ctrl Pts',(53.7751874557642,7.63141908140791,-66.7316106167228));
#37194=CARTESIAN_POINT('Ctrl Pts',(53.7723977403619,7.87358550472339,-67.3083260406967));
#37195=CARTESIAN_POINT('Ctrl Pts',(53.7670738293403,8.33298337809634,-68.2966866318741));
#37196=CARTESIAN_POINT('Ctrl Pts',(53.7586764378322,9.33414718261013,-70.1546037975584));
#37197=CARTESIAN_POINT('Ctrl Pts',(53.7585265782219,10.2095682818923,-71.614903576176));
#37198=CARTESIAN_POINT('Ctrl Pts',(53.7635280769974,10.7635283311995,-72.6672679359216));
#37199=CARTESIAN_POINT('Ctrl Pts',(53.7630829827452,10.8991987161,-72.9249502223087));
#37200=CARTESIAN_POINT('Ctrl Pts',(53.7631089119421,11.1640305013954,-73.4265223596093));
#37201=CARTESIAN_POINT('Ctrl Pts',(53.7628077454296,11.4986013205934,-74.058263832652));
#37202=CARTESIAN_POINT('Ctrl Pts',(53.7627016274684,11.8992841241948,-74.8121559447717));
#37203=CARTESIAN_POINT('Ctrl Pts',(53.762474296671,12.7024066212994,-76.3197212892488));
#37204=CARTESIAN_POINT('Ctrl Pts',(53.7625230103868,13.3717985159555,-77.5722797674868));
#37205=CARTESIAN_POINT('Ctrl Pts',(53.7627689020525,14.339732295039,-79.3928477645874));
#37206=CARTESIAN_POINT('Ctrl Pts',(53.7626628569048,14.7770769853391,-80.2155062080978));
#37207=CARTESIAN_POINT('Ctrl Pts',(53.7626628569049,15.2135985727285,-81.0364839101962));
#37208=CARTESIAN_POINT('Ctrl Pts',(56.6218989148777,1.85136045892844,24.8303065944882));
#37209=CARTESIAN_POINT('Ctrl Pts',(56.6220771833207,1.8513933644215,24.7814170542443));
#37210=CARTESIAN_POINT('Ctrl Pts',(56.622264131534,1.85142783688204,24.7325282854523));
#37211=CARTESIAN_POINT('Ctrl Pts',(56.6244717180094,1.85183601777454,24.1818031689162));
#37212=CARTESIAN_POINT('Ctrl Pts',(56.6263912820124,1.85233537909756,23.1775913604908));
#37213=CARTESIAN_POINT('Ctrl Pts',(56.6310067747904,1.85360135311401,21.1687553754193));
#37214=CARTESIAN_POINT('Ctrl Pts',(56.6456881661146,1.85632073692509,19.6645212396936));
#37215=CARTESIAN_POINT('Ctrl Pts',(56.6756903415303,1.86116033574717,18.4133891312005));
#37216=CARTESIAN_POINT('Ctrl Pts',(56.6901384311248,1.86357764549357,17.9098148785836));
#37217=CARTESIAN_POINT('Ctrl Pts',(56.7265093495165,1.86981416184756,16.9053229544563));
#37218=CARTESIAN_POINT('Ctrl Pts',(56.8044375131954,1.88316195303333,15.151722306397));
#37219=CARTESIAN_POINT('Ctrl Pts',(56.8773956848199,1.89449466324763,13.6525968306754));
#37220=CARTESIAN_POINT('Ctrl Pts',(56.921265128377,1.89914134215809,12.4013060922215));
#37221=CARTESIAN_POINT('Ctrl Pts',(56.9389620475575,1.90076308177012,11.901612767735));
#37222=CARTESIAN_POINT('Ctrl Pts',(56.9743051959492,1.90317797601583,10.9016108579509));
#37223=CARTESIAN_POINT('Ctrl Pts',(57.034010618561,1.90550671368578,9.14974706828727));
#37224=CARTESIAN_POINT('Ctrl Pts',(57.0746529435287,1.90518299224461,7.64372762768176));
#37225=CARTESIAN_POINT('Ctrl Pts',(57.0928779107252,1.90472166370263,6.51106889119965));
#37226=CARTESIAN_POINT('Ctrl Pts',(57.0965545657406,1.90452184313184,6.26176998816713));
#37227=CARTESIAN_POINT('Ctrl Pts',(57.1025967913818,1.90372493647001,5.76145095156286));
#37228=CARTESIAN_POINT('Ctrl Pts',(57.1100127971147,1.90147511564108,4.8841688074548));
#37229=CARTESIAN_POINT('Ctrl Pts',(57.1144126516609,1.89495506678394,3.12306096709394));
#37230=CARTESIAN_POINT('Ctrl Pts',(57.1081276593196,1.89054359979989,1.6115137914328));
#37231=CARTESIAN_POINT('Ctrl Pts',(57.1069369197323,1.89320424839432,0.546521002695334));
#37232=CARTESIAN_POINT('Ctrl Pts',(57.106704640349,1.89326396927256,0.42677368248937));
#37233=CARTESIAN_POINT('Ctrl Pts',(57.105906670196,1.89255411914581,0.182312017995565));
#37234=CARTESIAN_POINT('Ctrl Pts',(57.1037086906732,1.8893227496753,-0.245594539443753));
#37235=CARTESIAN_POINT('Ctrl Pts',(57.0986874322489,1.88041914765443,-0.864388880861254));
#37236=CARTESIAN_POINT('Ctrl Pts',(57.0909501720941,1.86725111695377,-1.61725535047182));
#37237=CARTESIAN_POINT('Ctrl Pts',(57.0799735255966,1.85266345272848,-2.63578860558777));
#37238=CARTESIAN_POINT('Ctrl Pts',(57.0681913152057,1.85142399966878,-3.93733882694326));
#37239=CARTESIAN_POINT('Ctrl Pts',(57.0686411870943,1.89755313172173,-5.01284603289817));
#37240=CARTESIAN_POINT('Ctrl Pts',(57.0741424054941,1.95119902184825,-5.69407227824501));
#37241=CARTESIAN_POINT('Ctrl Pts',(57.0782656048781,1.96836152596059,-5.92460398166542));
#37242=CARTESIAN_POINT('Ctrl Pts',(57.0907803209698,2.00331382182396,-6.42029618339497));
#37243=CARTESIAN_POINT('Ctrl Pts',(57.1223303131829,2.06396544800755,-7.29947588536513));
#37244=CARTESIAN_POINT('Ctrl Pts',(57.1805869280693,2.17680119997923,-8.63277978217996));
#37245=CARTESIAN_POINT('Ctrl Pts',(57.21879850434,2.39766107156909,-10.0481344865149));
#37246=CARTESIAN_POINT('Ctrl Pts',(57.2134878411633,2.65103974697223,-11.075163438603));
#37247=CARTESIAN_POINT('Ctrl Pts',(57.1983971901738,2.82981595871338,-11.6693844706438));
#37248=CARTESIAN_POINT('Ctrl Pts',(57.1864490593766,2.93141090109854,-11.9683787979901));
#37249=CARTESIAN_POINT('Ctrl Pts',(57.1755589950791,3.01318387312317,-12.1949656678289));
#37250=CARTESIAN_POINT('Ctrl Pts',(57.1646377021369,3.08088821895302,-12.3737291910729));
#37251=CARTESIAN_POINT('Ctrl Pts',(57.1424372935763,3.2203090751832,-12.7050339750465));
#37252=CARTESIAN_POINT('Ctrl Pts',(57.098431329832,3.48882736888547,-13.269798702969));
#37253=CARTESIAN_POINT('Ctrl Pts',(56.9714234943707,4.25784184103255,-14.6037208208315));
#37254=CARTESIAN_POINT('Ctrl Pts',(56.8215683084829,5.2117799632523,-15.8851297462418));
#37255=CARTESIAN_POINT('Ctrl Pts',(56.7124614258119,5.92576148056642,-16.9995115321707));
#37256=CARTESIAN_POINT('Ctrl Pts',(56.6705073804071,6.19760185968837,-17.49547298161));
#37257=CARTESIAN_POINT('Ctrl Pts',(56.6457536157039,6.35282413332364,-17.8450721535257));
#37258=CARTESIAN_POINT('Ctrl Pts',(56.6361291491391,6.40947553960446,-18.0007085032136));
#37259=CARTESIAN_POINT('Ctrl Pts',(56.6298206485322,6.44444041539305,-18.1099263859984));
#37260=CARTESIAN_POINT('Ctrl Pts',(56.6238465273791,6.47373614314704,-18.2061673528554));
#37261=CARTESIAN_POINT('Ctrl Pts',(56.6127753835527,6.52318789052139,-18.3863934508124));
#37262=CARTESIAN_POINT('Ctrl Pts',(56.6011197707429,6.56743761917295,-18.5745295664154));
#37263=CARTESIAN_POINT('Ctrl Pts',(56.5895622316385,6.60461514285489,-18.7635135846173));
#37264=CARTESIAN_POINT('Ctrl Pts',(56.5822709951931,6.62557263625537,-18.8838298576913));
#37265=CARTESIAN_POINT('Ctrl Pts',(56.5764559941441,6.64085081833095,-18.9808893137307));
#37266=CARTESIAN_POINT('Ctrl Pts',(56.5706422249478,6.65522596905915,-19.0787275580226));
#37267=CARTESIAN_POINT('Ctrl Pts',(56.5546912627251,6.69105086626354,-19.3506474291268));
#37268=CARTESIAN_POINT('Ctrl Pts',(56.5290686917994,6.73030576444265,-19.8129382656079));
#37269=CARTESIAN_POINT('Ctrl Pts',(56.4869033379652,6.75686122587932,-20.6889248100617));
#37270=CARTESIAN_POINT('Ctrl Pts',(56.4439828569392,6.73207638738493,-21.8901143268291));
#37271=CARTESIAN_POINT('Ctrl Pts',(56.4207878995836,6.72020579063288,-22.9645713483529));
#37272=CARTESIAN_POINT('Ctrl Pts',(56.4083502797615,6.74481557433032,-23.6666501706463));
#37273=CARTESIAN_POINT('Ctrl Pts',(56.4043291434562,6.75174230324922,-23.8933215011308));
#37274=CARTESIAN_POINT('Ctrl Pts',(56.398492185458,6.76332242913761,-24.3786922422349));
#37275=CARTESIAN_POINT('Ctrl Pts',(56.393815893827,6.77508570849919,-25.2203653565117));
#37276=CARTESIAN_POINT('Ctrl Pts',(56.3990629133695,6.77425355762422,-26.4506819756972));
#37277=CARTESIAN_POINT('Ctrl Pts',(56.4127399329853,6.7597315130406,-27.9490222417778));
#37278=CARTESIAN_POINT('Ctrl Pts',(56.4185729457465,6.75181328125929,-28.9647360897816));
#37279=CARTESIAN_POINT('Ctrl Pts',(56.4185239529943,6.7508906297659,-29.5391863786918));
#37280=CARTESIAN_POINT('Ctrl Pts',(56.418485093439,6.75065094731659,-29.6630149700534));
#37281=CARTESIAN_POINT('Ctrl Pts',(56.4183300862443,6.7500433467653,-29.9129783838157));
#37282=CARTESIAN_POINT('Ctrl Pts',(56.4178646736266,6.74866256221038,-30.3496161755409));
#37283=CARTESIAN_POINT('Ctrl Pts',(56.416282878756,6.74477104644997,-31.224923737901));
#37284=CARTESIAN_POINT('Ctrl Pts',(56.4135778544298,6.7384067889161,-32.2268641469045));
#37285=CARTESIAN_POINT('Ctrl Pts',(56.4111284320163,6.73150120937088,-33.2301868337395));
#37286=CARTESIAN_POINT('Ctrl Pts',(56.4097169184839,6.72641635934727,-33.9829585725888));
#37287=CARTESIAN_POINT('Ctrl Pts',(56.4090485548286,6.7218060372717,-34.735601000675));
#37288=CARTESIAN_POINT('Ctrl Pts',(56.4092942227924,6.7193015658958,-35.2371596816712));
#37289=CARTESIAN_POINT('Ctrl Pts',(56.4098113412844,6.71772837300494,-35.6141701797015));
#37290=CARTESIAN_POINT('Ctrl Pts',(56.4102730457911,6.71669168677539,-35.8653728421837));
#37291=CARTESIAN_POINT('Ctrl Pts',(56.4116026068534,6.71465379461935,-36.3679915774757));
#37292=CARTESIAN_POINT('Ctrl Pts',(56.4148812401533,6.71123663261034,-37.2458884360711));
#37293=CARTESIAN_POINT('Ctrl Pts',(56.4240612418311,6.70516318867893,-38.9991861724131));
#37294=CARTESIAN_POINT('Ctrl Pts',(56.4327316323619,6.7020467448753,-40.5031852469808));
#37295=CARTESIAN_POINT('Ctrl Pts',(56.4358176766823,6.70148464569061,-41.6375067241571));
#37296=CARTESIAN_POINT('Ctrl Pts',(56.4363859507804,6.70120093233901,-41.8854524324178));
#37297=CARTESIAN_POINT('Ctrl Pts',(56.4369600134697,6.70040278697019,-42.2597348467726));
#37298=CARTESIAN_POINT('Ctrl Pts',(56.4373019861491,6.69934223132865,-42.6344724404243));
#37299=CARTESIAN_POINT('Ctrl Pts',(56.4375131769031,6.69772413167307,-43.1355563860534));
#37300=CARTESIAN_POINT('Ctrl Pts',(56.43743857815,6.69559543263226,-43.7638356220231));
#37301=CARTESIAN_POINT('Ctrl Pts',(56.4371890772263,6.69375779937644,-44.520576384667));
#37302=CARTESIAN_POINT('Ctrl Pts',(56.4371652256954,6.69356873094274,-45.1530289938705));
#37303=CARTESIAN_POINT('Ctrl Pts',(56.4374532086234,6.69467889993727,-45.6598650883663));
#37304=CARTESIAN_POINT('Ctrl Pts',(56.4378670016389,6.69625334352035,-46.0403702892188));
#37305=CARTESIAN_POINT('Ctrl Pts',(56.438526314343,6.69868310825844,-46.4211700949389));
#37306=CARTESIAN_POINT('Ctrl Pts',(56.4397997988323,6.70322061635112,-46.9292871803912));
#37307=CARTESIAN_POINT('Ctrl Pts',(56.441257007958,6.70824138694336,-47.3105245310882));
#37308=CARTESIAN_POINT('Ctrl Pts',(56.4431613354401,6.71460849120052,-47.6932076238684));
#37309=CARTESIAN_POINT('Ctrl Pts',(56.444461059475,6.72066563953415,-47.9626999638013));
#37310=CARTESIAN_POINT('Ctrl Pts',(56.4473157330693,6.73779781636137,-48.4883604358934));
#37311=CARTESIAN_POINT('Ctrl Pts',(56.4529620758537,6.77856952444017,-49.3987669008521));
#37312=CARTESIAN_POINT('Ctrl Pts',(56.463100633075,6.85159433777694,-50.6573233141209));
#37313=CARTESIAN_POINT('Ctrl Pts',(56.4786218386434,6.91724554550676,-52.1049716210228));
#37314=CARTESIAN_POINT('Ctrl Pts',(56.4907106899684,6.91939000975858,-53.0254174522498));
#37315=CARTESIAN_POINT('Ctrl Pts',(56.4985114506127,6.90058592503779,-53.5868928127147));
#37316=CARTESIAN_POINT('Ctrl Pts',(56.5016375151978,6.8901798231696,-53.7863301337798));
#37317=CARTESIAN_POINT('Ctrl Pts',(56.5085164008023,6.85469462748162,-54.2176593433617));
#37318=CARTESIAN_POINT('Ctrl Pts',(56.5222326673793,6.75852920726253,-55.0029169699139));
#37319=CARTESIAN_POINT('Ctrl Pts',(56.5557322438817,6.47228382886766,-56.7244744790596));
#37320=CARTESIAN_POINT('Ctrl Pts',(56.590501809989,6.22669399758466,-58.4359143044246));
#37321=CARTESIAN_POINT('Ctrl Pts',(56.5992930633333,6.30844846728972,-59.7694961384221));
#37322=CARTESIAN_POINT('Ctrl Pts',(56.6004541754483,6.3182623376236,-59.9110802125503));
#37323=CARTESIAN_POINT('Ctrl Pts',(56.602439888185,6.34240962308779,-60.204643689476));
#37324=CARTESIAN_POINT('Ctrl Pts',(56.6053447885661,6.39424928086466,-60.7100838593593));
#37325=CARTESIAN_POINT('Ctrl Pts',(56.6089205249707,6.53549360265129,-61.7144870525455));
#37326=CARTESIAN_POINT('Ctrl Pts',(56.6091551083785,6.771803729698,-62.8337353857643));
#37327=CARTESIAN_POINT('Ctrl Pts',(56.6076504370481,7.06395119048437,-63.9256406327616));
#37328=CARTESIAN_POINT('Ctrl Pts',(56.6065119391543,7.24589488847553,-64.5285845829376));
#37329=CARTESIAN_POINT('Ctrl Pts',(56.6057784652313,7.37315606264269,-64.9258734582198));
#37330=CARTESIAN_POINT('Ctrl Pts',(56.6053061446002,7.45949804394918,-65.1894282456331));
#37331=CARTESIAN_POINT('Ctrl Pts',(56.6048672956263,7.54799056003658,-65.451153705338));
#37332=CARTESIAN_POINT('Ctrl Pts',(56.60454321205,7.62703670738344,-65.6783915114089));
#37333=CARTESIAN_POINT('Ctrl Pts',(56.6043781250423,7.67263691564513,-65.807741257995));
#37334=CARTESIAN_POINT('Ctrl Pts',(56.6041508853138,7.74146255176413,-66.0012895834968));
#37335=CARTESIAN_POINT('Ctrl Pts',(56.6040117583367,7.79963582982472,-66.1615014626742));
#37336=CARTESIAN_POINT('Ctrl Pts',(56.6038316081065,7.89711952784231,-66.4259998336907));
#37337=CARTESIAN_POINT('Ctrl Pts',(56.6018530730065,8.0144401400366,-66.7303939337344));
#37338=CARTESIAN_POINT('Ctrl Pts',(56.5988000638691,8.25647394535926,-67.3071847283582));
#37339=CARTESIAN_POINT('Ctrl Pts',(56.5930354521079,8.71563413707656,-68.2955326482492));
#37340=CARTESIAN_POINT('Ctrl Pts',(56.5840964631355,9.71659621429294,-70.1535453043583));
#37341=CARTESIAN_POINT('Ctrl Pts',(56.5841638540735,10.5920784606575,-71.6137990424342));
#37342=CARTESIAN_POINT('Ctrl Pts',(56.5896072067733,11.1461190268922,-72.6661379485151));
#37343=CARTESIAN_POINT('Ctrl Pts',(56.5891309607652,11.2817778639891,-72.9238278802343));
#37344=CARTESIAN_POINT('Ctrl Pts',(56.5891672866806,11.5466066329308,-73.4254071841434));
#37345=CARTESIAN_POINT('Ctrl Pts',(56.588845595627,11.8811706681873,-74.0571574235573));
#37346=CARTESIAN_POINT('Ctrl Pts',(56.5887302787201,12.2818548355253,-74.8110572860588));
#37347=CARTESIAN_POINT('Ctrl Pts',(56.5884745468439,13.0849849212197,-76.3186335874071));
#37348=CARTESIAN_POINT('Ctrl Pts',(56.5885067406493,13.7543899062702,-77.5711825092658));
#37349=CARTESIAN_POINT('Ctrl Pts',(56.5887723366122,14.7223194411704,-79.3917286253267));
#37350=CARTESIAN_POINT('Ctrl Pts',(56.5886561011866,15.1596642818603,-80.2143906195593));
#37351=CARTESIAN_POINT('Ctrl Pts',(56.5886561011865,15.5961858692498,-81.0353683216575));
#37352=CARTESIAN_POINT('Ctrl Pts',(59.4327147758635,2.25264759904533,24.8301370357426));
#37353=CARTESIAN_POINT('Ctrl Pts',(59.4328805699872,2.25268328427295,24.7812421415735));
#37354=CARTESIAN_POINT('Ctrl Pts',(59.4330544581857,2.25272065661361,24.7323479892438));
#37355=CARTESIAN_POINT('Ctrl Pts',(59.4351081479366,2.25316352958089,24.1815581347574));
#37356=CARTESIAN_POINT('Ctrl Pts',(59.4365154515769,2.25375717421373,23.1771805010386));
#37357=CARTESIAN_POINT('Ctrl Pts',(59.4396802483187,2.25527681160943,21.168266890462));
#37358=CARTESIAN_POINT('Ctrl Pts',(59.4533544085439,2.25822384829969,19.664119974994));
#37359=CARTESIAN_POINT('Ctrl Pts',(59.4831900958584,2.26322002674582,18.4131232939436));
#37360=CARTESIAN_POINT('Ctrl Pts',(59.4973611339143,2.26566136680147,17.909530731663));
#37361=CARTESIAN_POINT('Ctrl Pts',(59.5326905890348,2.27186275277079,16.9049746402285));
#37362=CARTESIAN_POINT('Ctrl Pts',(59.6084537998042,2.28507927696242,15.1511100840618));
#37363=CARTESIAN_POINT('Ctrl Pts',(59.682155229076,2.29664260171308,13.6519166082037));
#37364=CARTESIAN_POINT('Ctrl Pts',(59.7316197253229,2.30214680015721,12.4008547144836));
#37365=CARTESIAN_POINT('Ctrl Pts',(59.7521786564858,2.30418787278943,11.9013037511421));
#37366=CARTESIAN_POINT('Ctrl Pts',(59.7951798385236,2.30767854931378,10.9015996797567));
#37367=CARTESIAN_POINT('Ctrl Pts',(59.871920487792,2.31235844347836,9.15030235439126));
#37368=CARTESIAN_POINT('Ctrl Pts',(59.9284261569215,2.31424867536969,7.64436614155757));
#37369=CARTESIAN_POINT('Ctrl Pts',(59.9544677432662,2.31510430612518,6.51125887373394));
#37370=CARTESIAN_POINT('Ctrl Pts',(59.9599887072642,2.31520084670204,6.26176258734173));
#37371=CARTESIAN_POINT('Ctrl Pts',(59.9701234406006,2.31513483587211,5.76118080724149));
#37372=CARTESIAN_POINT('Ctrl Pts',(59.9854549317823,2.31445343676422,4.88349131580663));
#37373=CARTESIAN_POINT('Ctrl Pts',(60.0066557259146,2.3116903349232,3.122050961627));
#37374=CARTESIAN_POINT('Ctrl Pts',(60.0081729114145,2.31041786813838,1.61015526670906));
#37375=CARTESIAN_POINT('Ctrl Pts',(60.0000133827516,2.31151798348453,0.547318300038715));
#37376=CARTESIAN_POINT('Ctrl Pts',(59.9987799969336,2.31117336970775,0.43263093270387));
#37377=CARTESIAN_POINT('Ctrl Pts',(59.9952905821698,2.30883587110844,0.194803767687823));
#37378=CARTESIAN_POINT('Ctrl Pts',(59.9867407237385,2.30078952656156,-0.221872168562404));
#37379=CARTESIAN_POINT('Ctrl Pts',(59.9687552635737,2.28042457466313,-0.830809221312308));
#37380=CARTESIAN_POINT('Ctrl Pts',(59.9419828448459,2.24998125672055,-1.58053884969406));
#37381=CARTESIAN_POINT('Ctrl Pts',(59.9045114164938,2.21332006777769,-2.60837725670198));
#37382=CARTESIAN_POINT('Ctrl Pts',(59.8638467657641,2.19824901379055,-3.94728156666758));
#37383=CARTESIAN_POINT('Ctrl Pts',(59.8547531658741,2.27161453180319,-5.07662983961258));
#37384=CARTESIAN_POINT('Ctrl Pts',(59.8612777254522,2.36142900914507,-5.79808115446848));
#37385=CARTESIAN_POINT('Ctrl Pts',(59.8667790865954,2.39532201728264,-6.05855832069619));
#37386=CARTESIAN_POINT('Ctrl Pts',(59.8857622841587,2.47308322652155,-6.59755779715002));
#37387=CARTESIAN_POINT('Ctrl Pts',(59.9369986063271,2.63002365791845,-7.53693807282327));
#37388=CARTESIAN_POINT('Ctrl Pts',(60.0379370888202,2.92928801589726,-8.89353364220382));
#37389=CARTESIAN_POINT('Ctrl Pts',(60.1099184078909,3.33173088950953,-10.2468366988312));
#37390=CARTESIAN_POINT('Ctrl Pts',(60.1185581245289,3.65744077076127,-11.1940983723255));
#37391=CARTESIAN_POINT('Ctrl Pts',(60.1089394250062,3.85489440144113,-11.7360559881447));
#37392=CARTESIAN_POINT('Ctrl Pts',(60.0988057825633,3.95716232528036,-12.0071578997948));
#37393=CARTESIAN_POINT('Ctrl Pts',(60.088867015177,4.03585186488094,-12.2124631115407));
#37394=CARTESIAN_POINT('Ctrl Pts',(60.0770799382493,4.10162443878164,-12.3804759509473));
#37395=CARTESIAN_POINT('Ctrl Pts',(60.0533423220747,4.23335080955239,-12.6916421900252));
#37396=CARTESIAN_POINT('Ctrl Pts',(60.0048222621594,4.48160461407792,-13.2286596866252));
#37397=CARTESIAN_POINT('Ctrl Pts',(59.8591649769858,5.17318220046663,-14.520766291152));
#37398=CARTESIAN_POINT('Ctrl Pts',(59.6737288778186,6.00238966144673,-15.7920829004921));
#37399=CARTESIAN_POINT('Ctrl Pts',(59.5263120296862,6.61088078796949,-16.8978546252372));
#37400=CARTESIAN_POINT('Ctrl Pts',(59.4651538261524,6.84135783860763,-17.3942967990539));
#37401=CARTESIAN_POINT('Ctrl Pts',(59.4267168765041,6.97398996864091,-17.749743920164));
#37402=CARTESIAN_POINT('Ctrl Pts',(59.4113161943744,7.02320296959488,-17.9115274404766));
#37403=CARTESIAN_POINT('Ctrl Pts',(59.4013852878992,7.05389951784351,-18.0266279574196));
#37404=CARTESIAN_POINT('Ctrl Pts',(59.3940826480698,7.07707674929802,-18.1188405616837));
#37405=CARTESIAN_POINT('Ctrl Pts',(59.3803725278826,7.11649992658285,-18.2961177733231));
#37406=CARTESIAN_POINT('Ctrl Pts',(59.3671207098108,7.15031966048852,-18.480276260381));
#37407=CARTESIAN_POINT('Ctrl Pts',(59.3546789178648,7.17768441585883,-18.6669679798643));
#37408=CARTESIAN_POINT('Ctrl Pts',(59.3471904049831,7.19249453279696,-18.7859681713174));
#37409=CARTESIAN_POINT('Ctrl Pts',(59.3414003725508,7.20291843621819,-18.8822443641514));
#37410=CARTESIAN_POINT('Ctrl Pts',(59.3357390090068,7.21244523533041,-18.9794037813503));
#37411=CARTESIAN_POINT('Ctrl Pts',(59.3207106649973,7.23499990532823,-19.2499932907629));
#37412=CARTESIAN_POINT('Ctrl Pts',(59.2992033293261,7.2525723692102,-19.7128140108013));
#37413=CARTESIAN_POINT('Ctrl Pts',(59.2695633569605,7.23976893671297,-20.595989007654));
#37414=CARTESIAN_POINT('Ctrl Pts',(59.2466259148726,7.16407388584051,-21.8137241348146));
#37415=CARTESIAN_POINT('Ctrl Pts',(59.2333573088729,7.11836760292419,-22.9079330706097));
#37416=CARTESIAN_POINT('Ctrl Pts',(59.2225729318419,7.12836870657141,-23.6256260071911));
#37417=CARTESIAN_POINT('Ctrl Pts',(59.218879188711,7.13116315677762,-23.8586364848611));
#37418=CARTESIAN_POINT('Ctrl Pts',(59.2130886994703,7.13583646035015,-24.3552912337382));
#37419=CARTESIAN_POINT('Ctrl Pts',(59.2069711153891,7.14052696112994,-25.213894792417));
#37420=CARTESIAN_POINT('Ctrl Pts',(59.2071940926013,7.13992372229919,-26.4598845391602));
#37421=CARTESIAN_POINT('Ctrl Pts',(59.2142118004288,7.13359020698822,-27.9631595869271));
#37422=CARTESIAN_POINT('Ctrl Pts',(59.2183316401815,7.13037250268532,-28.9727155137208));
#37423=CARTESIAN_POINT('Ctrl Pts',(59.2191463856912,7.13007778108586,-29.5412674506224));
#37424=CARTESIAN_POINT('Ctrl Pts',(59.2193436844314,7.1300024132007,-29.6660369532951));
#37425=CARTESIAN_POINT('Ctrl Pts',(59.2197848025345,7.12980927296514,-29.9165584568622));
#37426=CARTESIAN_POINT('Ctrl Pts',(59.2206776267452,7.129379567084,-30.3546893553598));
#37427=CARTESIAN_POINT('Ctrl Pts',(59.2229317471094,7.12818122773045,-31.2319841001822));
#37428=CARTESIAN_POINT('Ctrl Pts',(59.2264614389033,7.12633563783124,-32.2353584891699));
#37429=CARTESIAN_POINT('Ctrl Pts',(59.2307545410767,7.12444933988321,-33.2388608029659));
#37430=CARTESIAN_POINT('Ctrl Pts',(59.2343020974957,7.1231198708239,-33.9912364403544));
#37431=CARTESIAN_POINT('Ctrl Pts',(59.2381004226901,7.1220247993843,-34.7429205634483));
#37432=CARTESIAN_POINT('Ctrl Pts',(59.2407678765008,7.1215048376743,-35.2434588351024));
#37433=CARTESIAN_POINT('Ctrl Pts',(59.2428133314656,7.12121201221069,-35.6195715682491));
#37434=CARTESIAN_POINT('Ctrl Pts',(59.2442723839178,7.12101105794536,-35.8708228135));
#37435=CARTESIAN_POINT('Ctrl Pts',(59.2475011339763,7.12060361293872,-36.3731615660546));
#37436=CARTESIAN_POINT('Ctrl Pts',(59.2538137491707,7.11994127909612,-37.2507475076407));
#37437=CARTESIAN_POINT('Ctrl Pts',(59.2681942977094,7.11886970086017,-39.0032177529718));
#37438=CARTESIAN_POINT('Ctrl Pts',(59.2799886515837,7.11921953999885,-40.5065411340942));
#37439=CARTESIAN_POINT('Ctrl Pts',(59.2851996153717,7.12074410872078,-41.6403275585497));
#37440=CARTESIAN_POINT('Ctrl Pts',(59.2862494874205,7.12090603734663,-41.8882328760425));
#37441=CARTESIAN_POINT('Ctrl Pts',(59.2875421020988,7.12075925363304,-42.2623994447051));
#37442=CARTESIAN_POINT('Ctrl Pts',(59.2885945057288,7.12032313164209,-42.6370193484372));
#37443=CARTESIAN_POINT('Ctrl Pts',(59.2897262224044,7.11949943860257,-43.1379169156182));
#37444=CARTESIAN_POINT('Ctrl Pts',(59.2907301525556,7.11827942067128,-43.7659238140434));
#37445=CARTESIAN_POINT('Ctrl Pts',(59.2915831244807,7.11736409262801,-44.5222645555723));
#37446=CARTESIAN_POINT('Ctrl Pts',(59.2922548730296,7.11777499065889,-45.1543232707919));
#37447=CARTESIAN_POINT('Ctrl Pts',(59.292926826433,7.1192442939905,-45.6608028819353));
#37448=CARTESIAN_POINT('Ctrl Pts',(59.2935333732457,7.12102430836641,-46.0410215359872));
#37449=CARTESIAN_POINT('Ctrl Pts',(59.2942811015061,7.12359120049604,-46.4215152867929));
#37450=CARTESIAN_POINT('Ctrl Pts',(59.2955170927399,7.12821485543452,-46.929197281356));
#37451=CARTESIAN_POINT('Ctrl Pts',(59.2967687246829,7.13318361907883,-47.310081014493));
#37452=CARTESIAN_POINT('Ctrl Pts',(59.2983163931068,7.13941329099905,-47.69238596202));
#37453=CARTESIAN_POINT('Ctrl Pts',(59.2993206163489,7.14533248224309,-47.9615277700545));
#37454=CARTESIAN_POINT('Ctrl Pts',(59.301396120705,7.16205185116678,-48.4866123228665));
#37455=CARTESIAN_POINT('Ctrl Pts',(59.3052220622473,7.20177535478386,-49.3961426670782));
#37456=CARTESIAN_POINT('Ctrl Pts',(59.3117584695497,7.27260781155126,-50.6539242057696));
#37457=CARTESIAN_POINT('Ctrl Pts',(59.3220001282436,7.33517126435499,-52.1013146689092));
#37458=CARTESIAN_POINT('Ctrl Pts',(59.3304026861646,7.33526075828364,-53.0220323256413));
#37459=CARTESIAN_POINT('Ctrl Pts',(59.335943439786,7.31525779761466,-53.5837977277501));
#37460=CARTESIAN_POINT('Ctrl Pts',(59.3380744041258,7.30439822250382,-53.7829956038034));
#37461=CARTESIAN_POINT('Ctrl Pts',(59.3427825664043,7.26785423620579,-54.2141155699194));
#37462=CARTESIAN_POINT('Ctrl Pts',(59.352318123001,7.16956134865011,-54.9990500754213));
#37463=CARTESIAN_POINT('Ctrl Pts',(59.3767789545431,6.87830922953412,-56.7205007536377));
#37464=CARTESIAN_POINT('Ctrl Pts',(59.4048060029405,6.62818987442243,-58.4327422573043));
#37465=CARTESIAN_POINT('Ctrl Pts',(59.411130482769,6.70855050145335,-59.767853832079));
#37466=CARTESIAN_POINT('Ctrl Pts',(59.4120059030465,6.71822542519762,-59.9096031455069));
#37467=CARTESIAN_POINT('Ctrl Pts',(59.4134825887939,6.74213391775351,-60.2034888696665));
#37468=CARTESIAN_POINT('Ctrl Pts',(59.4156518251278,6.7936798491486,-60.7094410989841));
#37469=CARTESIAN_POINT('Ctrl Pts',(59.4183146497419,6.93474877284089,-61.7146766129639));
#37470=CARTESIAN_POINT('Ctrl Pts',(59.4184992485081,7.1715190036146,-62.8344221591378));
#37471=CARTESIAN_POINT('Ctrl Pts',(59.4173589498161,7.46427912981003,-63.9264212002982));
#37472=CARTESIAN_POINT('Ctrl Pts',(59.4164757584546,7.6465429618124,-64.5292803407694));
#37473=CARTESIAN_POINT('Ctrl Pts',(59.4158918488738,7.77397289223777,-64.9264596667921));
#37474=CARTESIAN_POINT('Ctrl Pts',(59.4155105646797,7.86041369573992,-65.1899275045537));
#37475=CARTESIAN_POINT('Ctrl Pts',(59.4151469227141,7.94898045296805,-65.451546102566));
#37476=CARTESIAN_POINT('Ctrl Pts',(59.4148663751997,8.02806526429127,-65.6786728946603));
#37477=CARTESIAN_POINT('Ctrl Pts',(59.4147189579701,8.0736791676609,-65.8079543090621));
#37478=CARTESIAN_POINT('Ctrl Pts',(59.4145103915492,8.14251666840732,-66.0013954283672));
#37479=CARTESIAN_POINT('Ctrl Pts',(59.4143701375348,8.20068035980342,-66.1615077310751));
#37480=CARTESIAN_POINT('Ctrl Pts',(59.4141584642359,8.29812025686491,-66.4258317734694));
#37481=CARTESIAN_POINT('Ctrl Pts',(59.4121076614625,8.41545533517109,-66.7302379496878));
#37482=CARTESIAN_POINT('Ctrl Pts',(59.4089539368078,8.65747797861771,-67.3069545825026));
#37483=CARTESIAN_POINT('Ctrl Pts',(59.4030514710827,9.11662614725699,-68.2952495881172));
#37484=CARTESIAN_POINT('Ctrl Pts',(59.3940392140636,10.1175425980928,-70.1531805878224));
#37485=CARTESIAN_POINT('Ctrl Pts',(59.3942963770557,10.9930399610668,-71.6134582690787));
#37486=CARTESIAN_POINT('Ctrl Pts',(59.3998653033869,11.5471474796941,-72.6658362501666));
#37487=CARTESIAN_POINT('Ctrl Pts',(59.3993829957394,11.6828034066944,-72.9235196368838));
#37488=CARTESIAN_POINT('Ctrl Pts',(59.3994250933298,11.9476351383384,-73.4250951811133));
#37489=CARTESIAN_POINT('Ctrl Pts',(59.3991008911446,12.2821967199485,-74.0568391088504));
#37490=CARTESIAN_POINT('Ctrl Pts',(59.3989841193555,12.6828780415212,-74.8107346122541));
#37491=CARTESIAN_POINT('Ctrl Pts',(59.3987200829908,13.4859987647365,-76.3183047595498));
#37492=CARTESIAN_POINT('Ctrl Pts',(59.3987454302011,14.1553957607975,-77.570859071339));
#37493=CARTESIAN_POINT('Ctrl Pts',(59.3990166195318,15.1233319175322,-79.3914167710635));
#37494=CARTESIAN_POINT('Ctrl Pts',(59.3988987558118,15.5606742957496,-80.2140763701825));
#37495=CARTESIAN_POINT('Ctrl Pts',(59.3988987558118,15.997195883139,-81.0350540722808));
#37496=CARTESIAN_POINT('Ctrl Pts',(62.2324107530731,2.65110775638153,24.8313041334545));
#37497=CARTESIAN_POINT('Ctrl Pts',(62.2325712481792,2.65111389896304,24.7824463733246));
#37498=CARTESIAN_POINT('Ctrl Pts',(62.2327396152326,2.6511203034555,24.7335900578008));
#37499=CARTESIAN_POINT('Ctrl Pts',(62.2347278245421,2.65119902107034,24.1832355424136));
#37500=CARTESIAN_POINT('Ctrl Pts',(62.2357081947501,2.65089165244121,23.1793104561523));
#37501=CARTESIAN_POINT('Ctrl Pts',(62.2376372653672,2.64989331869101,21.1712236096822));
#37502=CARTESIAN_POINT('Ctrl Pts',(62.2508916536482,2.65046341990255,19.6674110821095));
#37503=CARTESIAN_POINT('Ctrl Pts',(62.2817148825578,2.65350817891073,18.4166244925075));
#37504=CARTESIAN_POINT('Ctrl Pts',(62.2963483870087,2.65475016941358,17.9154921162311));
#37505=CARTESIAN_POINT('Ctrl Pts',(62.3328691172103,2.6574719171568,16.9126541421275));
#37506=CARTESIAN_POINT('Ctrl Pts',(62.4114002121739,2.6633388598978,15.1583819672954));
#37507=CARTESIAN_POINT('Ctrl Pts',(62.4886606605266,2.67186677246271,13.6513017842059));
#37508=CARTESIAN_POINT('Ctrl Pts',(62.5416548070192,2.68272815015991,12.3900241288783));
#37509=CARTESIAN_POINT('Ctrl Pts',(62.5639056817367,2.68778557754191,11.8862883820249));
#37510=CARTESIAN_POINT('Ctrl Pts',(62.6111306817512,2.70009765356894,10.8805255622894));
#37511=CARTESIAN_POINT('Ctrl Pts',(62.6965531064208,2.72558859986316,9.12351798064619));
#37512=CARTESIAN_POINT('Ctrl Pts',(62.759762075258,2.74792577759869,7.62112627372732));
#37513=CARTESIAN_POINT('Ctrl Pts',(62.7870471025404,2.75842639956328,6.4944158415301));
#37514=CARTESIAN_POINT('Ctrl Pts',(62.7926887078876,2.76085425419954,6.24239056560327));
#37515=CARTESIAN_POINT('Ctrl Pts',(62.8024671671064,2.7658357454544,5.73982521057602));
#37516=CARTESIAN_POINT('Ctrl Pts',(62.8158643319916,2.77467446058688,4.85939786465086));
#37517=CARTESIAN_POINT('Ctrl Pts',(62.8293418335807,2.79097470902073,3.10187281411723));
#37518=CARTESIAN_POINT('Ctrl Pts',(62.8245351274415,2.79542965430205,1.60675084670123));
#37519=CARTESIAN_POINT('Ctrl Pts',(62.8215962252372,2.79042733884296,0.562689137332636));
#37520=CARTESIAN_POINT('Ctrl Pts',(62.8210154022939,2.78909900073173,0.458689070067316));
#37521=CARTESIAN_POINT('Ctrl Pts',(62.8190965256766,2.78354103411644,0.235639881228226));
#37522=CARTESIAN_POINT('Ctrl Pts',(62.8139101492631,2.76682592587925,-0.156856461533343));
#37523=CARTESIAN_POINT('Ctrl Pts',(62.8023761501897,2.72650026401499,-0.744804542152578));
#37524=CARTESIAN_POINT('Ctrl Pts',(62.7849294582608,2.66393931300271,-1.48602674337414));
#37525=CARTESIAN_POINT('Ctrl Pts',(62.7601020876933,2.58128900315883,-2.52537635631036));
#37526=CARTESIAN_POINT('Ctrl Pts',(62.7319170070745,2.51604925639296,-3.91937869392183));
#37527=CARTESIAN_POINT('Ctrl Pts',(62.7291057998474,2.61099085146794,-5.14442267966518));
#37528=CARTESIAN_POINT('Ctrl Pts',(62.7362630542708,2.75759085859505,-5.93636508459741));
#37529=CARTESIAN_POINT('Ctrl Pts',(62.741770321279,2.82176513592095,-6.24514557083446));
#37530=CARTESIAN_POINT('Ctrl Pts',(62.7599115715833,2.97658271776053,-6.85273437634613));
#37531=CARTESIAN_POINT('Ctrl Pts',(62.8061174584549,3.30597913808947,-7.8806370854957));
#37532=CARTESIAN_POINT('Ctrl Pts',(62.8863958085257,3.89707212753794,-9.25228156988392));
#37533=CARTESIAN_POINT('Ctrl Pts',(62.9397736056384,4.52674995443731,-10.5119043306548));
#37534=CARTESIAN_POINT('Ctrl Pts',(62.9483073836637,4.92853685878937,-11.3479068954967));
#37535=CARTESIAN_POINT('Ctrl Pts',(62.9426225817136,5.13846212177897,-11.8136574168422));
#37536=CARTESIAN_POINT('Ctrl Pts',(62.935877313132,5.23527026475624,-12.0423083109252));
#37537=CARTESIAN_POINT('Ctrl Pts',(62.9289467471649,5.30491005784014,-12.2140196746635));
#37538=CARTESIAN_POINT('Ctrl Pts',(62.9178468592772,5.36388030319758,-12.36298456468));
#37539=CARTESIAN_POINT('Ctrl Pts',(62.8961604147852,5.47660367245371,-12.638969827769));
#37540=CARTESIAN_POINT('Ctrl Pts',(62.8501167546216,5.68011606065942,-13.1247631815501));
#37541=CARTESIAN_POINT('Ctrl Pts',(62.7055471700459,6.20985984960202,-14.3304179005817));
#37542=CARTESIAN_POINT('Ctrl Pts',(62.4912338497451,6.78245990414777,-15.5747418743489));
#37543=CARTESIAN_POINT('Ctrl Pts',(62.2993029893369,7.20735187064418,-16.6805280552391));
#37544=CARTESIAN_POINT('Ctrl Pts',(62.2163632975749,7.37607495476045,-17.1955964358133));
#37545=CARTESIAN_POINT('Ctrl Pts',(62.1634721816956,7.48085730828298,-17.5834240481002));
#37546=CARTESIAN_POINT('Ctrl Pts',(62.1425670082912,7.52293760023202,-17.7693118352408));
#37547=CARTESIAN_POINT('Ctrl Pts',(62.1294390175357,7.55035896134082,-17.9052542089931));
#37548=CARTESIAN_POINT('Ctrl Pts',(62.1211563672464,7.56761908025001,-17.998106111389));
#37549=CARTESIAN_POINT('Ctrl Pts',(62.1060386122447,7.59818832727529,-18.1847977995392));
#37550=CARTESIAN_POINT('Ctrl Pts',(62.0930891012341,7.62317609429139,-18.3759276979325));
#37551=CARTESIAN_POINT('Ctrl Pts',(62.0822144223327,7.6428536058607,-18.5711944201463));
#37552=CARTESIAN_POINT('Ctrl Pts',(62.0762525917653,7.65302519565803,-18.6951977645338));
#37553=CARTESIAN_POINT('Ctrl Pts',(62.0719662087674,7.65992486605567,-18.7955588852272));
#37554=CARTESIAN_POINT('Ctrl Pts',(62.0679951985242,7.66601390368074,-18.8967266479224));
#37555=CARTESIAN_POINT('Ctrl Pts',(62.0583389004949,7.67951185973049,-19.1781893365365));
#37556=CARTESIAN_POINT('Ctrl Pts',(62.0491579848126,7.6843381603447,-19.6572844659895));
#37557=CARTESIAN_POINT('Ctrl Pts',(62.0471164144703,7.6543263621362,-20.5627064856723));
#37558=CARTESIAN_POINT('Ctrl Pts',(62.0621269100584,7.56710224252032,-21.7946524647982));
#37559=CARTESIAN_POINT('Ctrl Pts',(62.0706822093106,7.51375182233016,-22.8859597117177));
#37560=CARTESIAN_POINT('Ctrl Pts',(62.0668999269535,7.51427019692833,-23.5975676711049));
#37561=CARTESIAN_POINT('Ctrl Pts',(62.0655820576767,7.51436969700696,-23.8360686960198));
#37562=CARTESIAN_POINT('Ctrl Pts',(62.0635918991896,7.51431755456326,-24.3384860432659));
#37563=CARTESIAN_POINT('Ctrl Pts',(62.0616150444944,7.51362663741968,-25.2077384672639));
#37564=CARTESIAN_POINT('Ctrl Pts',(62.0621011031445,7.5115907307205,-26.4627170410167));
#37565=CARTESIAN_POINT('Ctrl Pts',(62.0648413323574,7.50921458405261,-27.970321999584));
#37566=CARTESIAN_POINT('Ctrl Pts',(62.0659292167856,7.50884682134933,-28.977749244481));
#37567=CARTESIAN_POINT('Ctrl Pts',(62.0657024475546,7.5092866457995,-29.5438704056461));
#37568=CARTESIAN_POINT('Ctrl Pts',(62.0656416363747,7.50939383567201,-29.6694876250792));
#37569=CARTESIAN_POINT('Ctrl Pts',(62.065487129712,7.50965895993831,-29.9208561665864));
#37570=CARTESIAN_POINT('Ctrl Pts',(62.0651364468902,7.51024656387718,-30.3607234336883));
#37571=CARTESIAN_POINT('Ctrl Pts',(62.0641874801837,7.51185658664952,-31.2405845311435));
#37572=CARTESIAN_POINT('Ctrl Pts',(62.0628511063028,7.51444177549677,-32.2457033193181));
#37573=CARTESIAN_POINT('Ctrl Pts',(62.0619103176685,7.51726239035914,-33.2494543277796));
#37574=CARTESIAN_POINT('Ctrl Pts',(62.0615653654591,7.51937480913954,-34.001324586973));
#37575=CARTESIAN_POINT('Ctrl Pts',(62.0617406922815,7.52137880169214,-34.7518222937873));
#37576=CARTESIAN_POINT('Ctrl Pts',(62.0623142980273,7.52256208676719,-35.2510989017198));
#37577=CARTESIAN_POINT('Ctrl Pts',(62.0629588222116,7.52336429710618,-35.6261040174291));
#37578=CARTESIAN_POINT('Ctrl Pts',(62.063482259618,7.52388694043014,-35.8774098318808));
#37579=CARTESIAN_POINT('Ctrl Pts',(62.0648533349532,7.5248751427224,-36.379401153661));
#37580=CARTESIAN_POINT('Ctrl Pts',(62.0679875202739,7.5264987578139,-37.2566176006549));
#37581=CARTESIAN_POINT('Ctrl Pts',(62.0763297936556,7.52948981660232,-39.0081166132972));
#37582=CARTESIAN_POINT('Ctrl Pts',(62.0839656121537,7.53241511387234,-40.5106520379719));
#37583=CARTESIAN_POINT('Ctrl Pts',(62.0869051196726,7.53551992569335,-41.6437574713479));
#37584=CARTESIAN_POINT('Ctrl Pts',(62.0874696162204,7.53602680982341,-41.8915847922602));
#37585=CARTESIAN_POINT('Ctrl Pts',(62.0880919637729,7.53638204364662,-42.2655810687143));
#37586=CARTESIAN_POINT('Ctrl Pts',(62.0885286959401,7.53642856982292,-42.6400285125531));
#37587=CARTESIAN_POINT('Ctrl Pts',(62.0889117416412,7.536217481607,-43.1406690708058));
#37588=CARTESIAN_POINT('Ctrl Pts',(62.089110888396,7.53569612756946,-43.7683203882214));
#37589=CARTESIAN_POINT('Ctrl Pts',(62.0891971286507,7.53548224296686,-44.5241748107218));
#37590=CARTESIAN_POINT('Ctrl Pts',(62.0893868535754,7.53633812587254,-45.1557822312303));
#37591=CARTESIAN_POINT('Ctrl Pts',(62.0897605897562,7.53806579301751,-45.6618675530432));
#37592=CARTESIAN_POINT('Ctrl Pts',(62.090186372261,7.53998630844427,-46.0417760871001));
#37593=CARTESIAN_POINT('Ctrl Pts',(62.0907946046371,7.54263675345113,-46.4219447920921));
#37594=CARTESIAN_POINT('Ctrl Pts',(62.0918987822575,7.54728997860321,-46.9291720506793));
#37595=CARTESIAN_POINT('Ctrl Pts',(62.0931073870063,7.55218477568363,-47.3096935045049));
#37596=CARTESIAN_POINT('Ctrl Pts',(62.0946500272994,7.55826552660255,-47.6916137330119));
#37597=CARTESIAN_POINT('Ctrl Pts',(62.0956899306758,7.56404442827066,-47.9603806883333));
#37598=CARTESIAN_POINT('Ctrl Pts',(62.0979567486044,7.58036458850267,-48.4848483930344));
#37599=CARTESIAN_POINT('Ctrl Pts',(62.1023967485155,7.61910468697639,-49.3934153829413));
#37600=CARTESIAN_POINT('Ctrl Pts',(62.1103353217924,7.68794869441984,-50.6502655802821));
#37601=CARTESIAN_POINT('Ctrl Pts',(62.1224233583074,7.74777139027884,-52.0972078070305));
#37602=CARTESIAN_POINT('Ctrl Pts',(62.1317299659118,7.74613906151579,-53.0181400026945));
#37603=CARTESIAN_POINT('Ctrl Pts',(62.1376265100412,7.72516009843336,-53.5801983221761));
#37604=CARTESIAN_POINT('Ctrl Pts',(62.1399009906046,7.71395919386377,-53.7790356598082));
#37605=CARTESIAN_POINT('Ctrl Pts',(62.144891893323,7.67660866103408,-54.2098301643304));
#37606=CARTESIAN_POINT('Ctrl Pts',(62.1548861078054,7.57668998629144,-54.9943176964645));
#37607=CARTESIAN_POINT('Ctrl Pts',(62.1799950971101,7.28140426678334,-56.7158154644147));
#37608=CARTESIAN_POINT('Ctrl Pts',(62.2081833873139,7.02729986390898,-58.4291811313585));
#37609=CARTESIAN_POINT('Ctrl Pts',(62.214434191419,7.10645430029738,-59.7660691188329));
#37610=CARTESIAN_POINT('Ctrl Pts',(62.2152921603056,7.11601138045444,-59.9080078322041));
#37611=CARTESIAN_POINT('Ctrl Pts',(62.2167187516735,7.13971652526845,-60.2022648135528));
#37612=CARTESIAN_POINT('Ctrl Pts',(62.2187556195035,7.19101526209245,-60.7088079055096));
#37613=CARTESIAN_POINT('Ctrl Pts',(62.2210058151301,7.33194406379086,-61.7150167266094));
#37614=CARTESIAN_POINT('Ctrl Pts',(62.220494103909,7.56912255440908,-62.8353925702497));
#37615=CARTESIAN_POINT('Ctrl Pts',(62.2186541786765,7.86241183339184,-63.9275931935359));
#37616=CARTESIAN_POINT('Ctrl Pts',(62.21741273019,8.04494685543862,-64.5304140788372));
#37617=CARTESIAN_POINT('Ctrl Pts',(62.2166188453856,8.17251642994582,-64.9275069514343));
#37618=CARTESIAN_POINT('Ctrl Pts',(62.2161062636506,8.25903749032414,-65.1909009442395));
#37619=CARTESIAN_POINT('Ctrl Pts',(62.2156253772436,8.34766269691667,-65.4524219022825));
#37620=CARTESIAN_POINT('Ctrl Pts',(62.215257134898,8.42677423198685,-65.6794420084634));
#37621=CARTESIAN_POINT('Ctrl Pts',(62.2150641387944,8.47239575868788,-65.8086563808691));
#37622=CARTESIAN_POINT('Ctrl Pts',(62.2147919316114,8.54123677518438,-66.00199105567));
#37623=CARTESIAN_POINT('Ctrl Pts',(62.214608655405,8.59938592525983,-66.1620016010331));
#37624=CARTESIAN_POINT('Ctrl Pts',(62.2143413509797,8.69677672156467,-66.4261446314036));
#37625=CARTESIAN_POINT('Ctrl Pts',(62.2122609913914,8.81415479402535,-66.7305926507935));
#37626=CARTESIAN_POINT('Ctrl Pts',(62.2090683229704,9.0562048004226,-67.3072649369297));
#37627=CARTESIAN_POINT('Ctrl Pts',(62.2031701902083,9.51541638792159,-68.2955523830468));
#37628=CARTESIAN_POINT('Ctrl Pts',(62.1943317515038,10.5163927506456,-70.1534306834209));
#37629=CARTESIAN_POINT('Ctrl Pts',(62.1947391875034,11.3919020579306,-71.6137286933384));
#37630=CARTESIAN_POINT('Ctrl Pts',(62.2001943443147,11.9460014704505,-72.6661252618744));
#37631=CARTESIAN_POINT('Ctrl Pts',(62.1997185000816,12.0816602390721,-72.9238044443063));
#37632=CARTESIAN_POINT('Ctrl Pts',(62.1997564287731,12.3464935835405,-73.4253766509266));
#37633=CARTESIAN_POINT('Ctrl Pts',(62.1994358797236,12.6810568195398,-74.0571159606845));
#37634=CARTESIAN_POINT('Ctrl Pts',(62.1993211872213,13.0817369941327,-74.8110076497966));
#37635=CARTESIAN_POINT('Ctrl Pts',(62.1990653816072,13.8848530540247,-76.3185722749635));
#37636=CARTESIAN_POINT('Ctrl Pts',(62.19909669396,14.5542450034784,-77.5711307503444));
#37637=CARTESIAN_POINT('Ctrl Pts',(62.1993620993693,15.522185035061,-79.3916988003171));
#37638=CARTESIAN_POINT('Ctrl Pts',(62.1992463983474,15.9595269771664,-80.2143564816684));
#37639=CARTESIAN_POINT('Ctrl Pts',(62.1992463983475,16.3960485645559,-81.0353341837667));
#37640=CARTESIAN_POINT('Ctrl Pts',(65.0350887199224,3.04279907572872,24.8318421095528));
#37641=CARTESIAN_POINT('Ctrl Pts',(65.0353017889815,3.04279961695075,24.7830009397453));
#37642=CARTESIAN_POINT('Ctrl Pts',(65.0355252186173,3.04280017067125,24.7341613775858));
#37643=CARTESIAN_POINT('Ctrl Pts',(65.0381641497023,3.04280943774363,24.1840053062511));
#37644=CARTESIAN_POINT('Ctrl Pts',(65.0404998815081,3.04221679745299,23.1805170310154));
#37645=CARTESIAN_POINT('Ctrl Pts',(65.0461349316008,3.04039477281519,21.1726957556785));
#37646=CARTESIAN_POINT('Ctrl Pts',(65.0636872999614,3.04049794599169,19.6686880458142));
#37647=CARTESIAN_POINT('Ctrl Pts',(65.0993507487901,3.04372919187809,18.4175941768535));
#37648=CARTESIAN_POINT('Ctrl Pts',(65.1167602515594,3.0451355595967,17.9167397691228));
#37649=CARTESIAN_POINT('Ctrl Pts',(65.1610398139268,3.0484776471246,16.9142213017312));
#37650=CARTESIAN_POINT('Ctrl Pts',(65.2560876381536,3.05589826579763,15.1605998381288));
#37651=CARTESIAN_POINT('Ctrl Pts',(65.342626033825,3.06567363951754,13.6528125363831));
#37652=CARTESIAN_POINT('Ctrl Pts',(65.3898843591986,3.07637763944379,12.3899226094541));
#37653=CARTESIAN_POINT('Ctrl Pts',(65.4085180142653,3.08135168757766,11.8852522165172));
#37654=CARTESIAN_POINT('Ctrl Pts',(65.4441920740314,3.0933433491944,10.8780226376535));
#37655=CARTESIAN_POINT('Ctrl Pts',(65.5009220975331,3.11769180542614,9.11918017470684));
#37656=CARTESIAN_POINT('Ctrl Pts',(65.5344794590062,3.13759875586273,7.6178743897185));
#37657=CARTESIAN_POINT('Ctrl Pts',(65.5471867022137,3.14577990885582,6.49413363918257));
#37658=CARTESIAN_POINT('Ctrl Pts',(65.5490108295873,3.14719859434244,6.24591338779225));
#37659=CARTESIAN_POINT('Ctrl Pts',(65.5493695640765,3.14901745638244,5.74792996731733));
#37660=CARTESIAN_POINT('Ctrl Pts',(65.5427279547781,3.15004309780587,4.87350841866235));
#37661=CARTESIAN_POINT('Ctrl Pts',(65.5123377950902,3.14737548357901,3.11538246504764));
#37662=CARTESIAN_POINT('Ctrl Pts',(65.4950425644462,3.15244240092772,1.59718349180721));
#37663=CARTESIAN_POINT('Ctrl Pts',(65.5195985678633,3.16718619113657,0.529987804286143));
#37664=CARTESIAN_POINT('Ctrl Pts',(65.5229281006724,3.16804817025962,0.428403986222372));
#37665=CARTESIAN_POINT('Ctrl Pts',(65.5308547631716,3.16716048655649,0.206936702530311));
#37666=CARTESIAN_POINT('Ctrl Pts',(65.547966618142,3.15892053708572,-0.18214975514755));
#37667=CARTESIAN_POINT('Ctrl Pts',(65.5803545845031,3.13129166108476,-0.769062301553117));
#37668=CARTESIAN_POINT('Ctrl Pts',(65.6288087636496,3.08514444170353,-1.51529637587801));
#37669=CARTESIAN_POINT('Ctrl Pts',(65.700942704077,3.02972102648233,-2.57286733842955));
#37670=CARTESIAN_POINT('Ctrl Pts',(65.7958646181749,3.02141719199554,-4.01463727808764));
#37671=CARTESIAN_POINT('Ctrl Pts',(65.833958114971,3.21412823865908,-5.28558652813274));
#37672=CARTESIAN_POINT('Ctrl Pts',(65.8290085163487,3.43645951471753,-6.09719268068851));
#37673=CARTESIAN_POINT('Ctrl Pts',(65.8247241295313,3.54288014629557,-6.43980697173696));
#37674=CARTESIAN_POINT('Ctrl Pts',(65.8126064943145,3.78785542812985,-7.07974279986513));
#37675=CARTESIAN_POINT('Ctrl Pts',(65.7825329713037,4.28934782841537,-8.13424384932138));
#37676=CARTESIAN_POINT('Ctrl Pts',(65.7262757152049,5.10673810755621,-9.47955367822884));
#37677=CARTESIAN_POINT('Ctrl Pts',(65.6775989537901,5.87382979784091,-10.6881579950518));
#37678=CARTESIAN_POINT('Ctrl Pts',(65.6530739245746,6.29691093481057,-11.4492871912878));
#37679=CARTESIAN_POINT('Ctrl Pts',(65.6402509604291,6.49393833534442,-11.8545350240845));
#37680=CARTESIAN_POINT('Ctrl Pts',(65.6338047380311,6.5756459006392,-12.0455006429786));
#37681=CARTESIAN_POINT('Ctrl Pts',(65.6284680607276,6.63059158179909,-12.1853986619525));
#37682=CARTESIAN_POINT('Ctrl Pts',(65.6190373441314,6.67765228874231,-12.311998747581));
#37683=CARTESIAN_POINT('Ctrl Pts',(65.6011805048907,6.76260522595195,-12.5468430177704));
#37684=CARTESIAN_POINT('Ctrl Pts',(65.5631589210313,6.90664693731635,-12.9664952301201));
#37685=CARTESIAN_POINT('Ctrl Pts',(65.4439643271269,7.2355614364749,-14.034879865786));
#37686=CARTESIAN_POINT('Ctrl Pts',(65.2467846105436,7.50697175850343,-15.2036231533799));
#37687=CARTESIAN_POINT('Ctrl Pts',(65.0613357293355,7.72730564767796,-16.3447594771015));
#37688=CARTESIAN_POINT('Ctrl Pts',(64.9821707265439,7.82439690662045,-16.9129922839534));
#37689=CARTESIAN_POINT('Ctrl Pts',(64.9317938132122,7.89318054939857,-17.3665581781212));
#37690=CARTESIAN_POINT('Ctrl Pts',(64.9118997134959,7.92425307371857,-17.593609467152));
#37691=CARTESIAN_POINT('Ctrl Pts',(64.8993078170653,7.94604297832826,-17.7629114259997));
#37692=CARTESIAN_POINT('Ctrl Pts',(64.8917354443301,7.9577231709319,-17.862764794746));
#37693=CARTESIAN_POINT('Ctrl Pts',(64.8782668624603,7.97935239629412,-18.071834896486));
#37694=CARTESIAN_POINT('Ctrl Pts',(64.8675100284545,7.99635574954936,-18.2813015057794));
#37695=CARTESIAN_POINT('Ctrl Pts',(64.8591513260664,8.00965782593826,-18.4954392521802));
#37696=CARTESIAN_POINT('Ctrl Pts',(64.8548934131429,8.01635413238409,-18.6303138116814));
#37697=CARTESIAN_POINT('Ctrl Pts',(64.8520291464493,8.02082955198509,-18.7391604425263));
#37698=CARTESIAN_POINT('Ctrl Pts',(64.8495178118383,8.02471289520919,-18.8485275415764));
#37699=CARTESIAN_POINT('Ctrl Pts',(64.8440168783019,8.03305322470471,-19.151562519944));
#37700=CARTESIAN_POINT('Ctrl Pts',(64.8422051716334,8.03446836901049,-19.6600026041905));
#37701=CARTESIAN_POINT('Ctrl Pts',(64.8535522086806,8.01105171857207,-20.5996300476593));
#37702=CARTESIAN_POINT('Ctrl Pts',(64.8837721490584,7.95109059523506,-21.8412831543704));
#37703=CARTESIAN_POINT('Ctrl Pts',(64.9003529795289,7.91660579442229,-22.9055204389761));
#37704=CARTESIAN_POINT('Ctrl Pts',(64.900277402366,7.91617325660034,-23.5899675786111));
#37705=CARTESIAN_POINT('Ctrl Pts',(64.9003030466406,7.91601809697143,-23.8329269136991));
#37706=CARTESIAN_POINT('Ctrl Pts',(64.9005401853198,7.91574867606951,-24.3354244521531));
#37707=CARTESIAN_POINT('Ctrl Pts',(64.9013716578895,7.91538329393073,-25.2086195369282));
#37708=CARTESIAN_POINT('Ctrl Pts',(64.9032688859418,7.91511031742878,-26.4649259761897));
#37709=CARTESIAN_POINT('Ctrl Pts',(64.9051772354161,7.91503595164712,-27.9727274470494));
#37710=CARTESIAN_POINT('Ctrl Pts',(64.9052137834096,7.91514938428072,-28.9779253703462));
#37711=CARTESIAN_POINT('Ctrl Pts',(64.9046311313933,7.91523345071605,-29.5423469924773));
#37712=CARTESIAN_POINT('Ctrl Pts',(64.9044796832551,7.91525415166103,-29.6678552241075));
#37713=CARTESIAN_POINT('Ctrl Pts',(64.9040899436161,7.91530319787013,-29.918872357726));
#37714=CARTESIAN_POINT('Ctrl Pts',(64.9031960134775,7.915411596412,-30.3582566268718));
#37715=CARTESIAN_POINT('Ctrl Pts',(64.9006918760774,7.91570657713133,-31.2372869259982));
#37716=CARTESIAN_POINT('Ctrl Pts',(64.89677233778,7.91620876660362,-32.2419466203269));
#37717=CARTESIAN_POINT('Ctrl Pts',(64.8929724427649,7.9168128149532,-33.2456438209988));
#37718=CARTESIAN_POINT('Ctrl Pts',(64.8904741843251,7.91729973895228,-33.99768199076));
#37719=CARTESIAN_POINT('Ctrl Pts',(64.8886108925044,7.91781497916351,-34.7485909478118));
#37720=CARTESIAN_POINT('Ctrl Pts',(64.8879880285033,7.91816196656921,-35.2482953845696));
#37721=CARTESIAN_POINT('Ctrl Pts',(64.8878265442141,7.9184188811029,-35.6236680650367));
#37722=CARTESIAN_POINT('Ctrl Pts',(64.8878043645194,7.9185774585649,-35.8749590326448));
#37723=CARTESIAN_POINT('Ctrl Pts',(64.8880697266912,7.91885465191016,-36.377066978034));
#37724=CARTESIAN_POINT('Ctrl Pts',(64.8892403338603,7.91926838647898,-37.2544411099771));
#37725=CARTESIAN_POINT('Ctrl Pts',(64.8936821150121,7.92003795010626,-39.0063008097556));
#37726=CARTESIAN_POINT('Ctrl Pts',(64.8984206741914,7.92142088740016,-40.5092037903869));
#37727=CARTESIAN_POINT('Ctrl Pts',(64.8998416479655,7.92364914218204,-41.6425587006194));
#37728=CARTESIAN_POINT('Ctrl Pts',(64.900086735534,7.92397092305037,-41.8904039225992));
#37729=CARTESIAN_POINT('Ctrl Pts',(64.9002731327335,7.92406146234017,-42.2644517559109));
#37730=CARTESIAN_POINT('Ctrl Pts',(64.9003142004051,7.92385916136743,-42.6389503791446));
#37731=CARTESIAN_POINT('Ctrl Pts',(64.9002194850142,7.92333674755533,-43.139672374497));
#37732=CARTESIAN_POINT('Ctrl Pts',(64.8999069802989,7.92246723541446,-43.7674412347485));
#37733=CARTESIAN_POINT('Ctrl Pts',(64.8994925944636,7.92190539145051,-44.5234677640342));
#37734=CARTESIAN_POINT('Ctrl Pts',(64.899339922121,7.92253352259311,-45.155245631552));
#37735=CARTESIAN_POINT('Ctrl Pts',(64.8994703796176,7.92412104846715,-45.661477068022));
#37736=CARTESIAN_POINT('Ctrl Pts',(64.8997271906668,7.92595720904262,-46.0415036119417));
#37737=CARTESIAN_POINT('Ctrl Pts',(64.900176872622,7.92854497560912,-46.4217982374827));
#37738=CARTESIAN_POINT('Ctrl Pts',(64.9010781824461,7.93314457097787,-46.9292021071505));
#37739=CARTESIAN_POINT('Ctrl Pts',(64.9021442437456,7.93803373319031,-47.3098718598978));
#37740=CARTESIAN_POINT('Ctrl Pts',(64.9035395227039,7.94413377331177,-47.6919455868718));
#37741=CARTESIAN_POINT('Ctrl Pts',(64.9044953458893,7.94994285497855,-47.9608592494408));
#37742=CARTESIAN_POINT('Ctrl Pts',(64.9066406887799,7.96637203100846,-48.4855644513516));
#37743=CARTESIAN_POINT('Ctrl Pts',(64.9109756826221,8.0054171998626,-49.3944919298558));
#37744=CARTESIAN_POINT('Ctrl Pts',(64.9189764880102,8.07493592398898,-50.6516573118312));
#37745=CARTESIAN_POINT('Ctrl Pts',(64.9311717897488,8.13568908426217,-52.0986939738742));
#37746=CARTESIAN_POINT('Ctrl Pts',(64.9403930891791,8.13463902398254,-53.0195112352081));
#37747=CARTESIAN_POINT('Ctrl Pts',(64.9461217879297,8.11397309546367,-53.5814465389996));
#37748=CARTESIAN_POINT('Ctrl Pts',(64.9483334556686,8.10288366697726,-53.7803766739668));
#37749=CARTESIAN_POINT('Ctrl Pts',(64.9531665353562,8.06579808845442,-54.2112509890253));
#37750=CARTESIAN_POINT('Ctrl Pts',(64.9628117033353,7.96641817521339,-54.9958646771246));
#37751=CARTESIAN_POINT('Ctrl Pts',(64.9868737195004,7.6724124170175,-56.7174073592783));
#37752=CARTESIAN_POINT('Ctrl Pts',(65.013938987719,7.4195820506246,-58.4304576933914));
#37753=CARTESIAN_POINT('Ctrl Pts',(65.0196793288631,7.49908996597736,-59.7667411537284));
#37754=CARTESIAN_POINT('Ctrl Pts',(65.020474205641,7.50867707433676,-59.9086143602503));
#37755=CARTESIAN_POINT('Ctrl Pts',(65.0217742074001,7.53243121116188,-60.2027437125628));
#37756=CARTESIAN_POINT('Ctrl Pts',(65.0235878298676,7.58377523464587,-60.7090835159779));
#37757=CARTESIAN_POINT('Ctrl Pts',(65.0253881213518,7.72466418199519,-61.7149614631889));
#37758=CARTESIAN_POINT('Ctrl Pts',(65.0243773613579,7.9615923705701,-62.8351390984063));
#37759=CARTESIAN_POINT('Ctrl Pts',(65.0220949239444,8.25460244180564,-63.9273035771588));
#37760=CARTESIAN_POINT('Ctrl Pts',(65.0206320327183,8.43699654685904,-64.5301596479062));
#37761=CARTESIAN_POINT('Ctrl Pts',(65.0197044168754,8.56449069371539,-64.9272970447687));
#37762=CARTESIAN_POINT('Ctrl Pts',(65.0191063773078,8.6509669508869,-65.1907263261488));
#37763=CARTESIAN_POINT('Ctrl Pts',(65.0185462704627,8.73955686405517,-65.4522904566082));
#37764=CARTESIAN_POINT('Ctrl Pts',(65.0181139983008,8.81864751039845,-65.6793553095181));
#37765=CARTESIAN_POINT('Ctrl Pts',(65.0178860252226,8.86426023414526,-65.8085971865833));
#37766=CARTESIAN_POINT('Ctrl Pts',(65.0175629808496,8.93309127293903,-66.0019749788851));
#37767=CARTESIAN_POINT('Ctrl Pts',(65.0173408944881,8.99123922852743,-66.1620255738922));
#37768=CARTESIAN_POINT('Ctrl Pts',(65.0170143927561,9.08863824119291,-66.4262385596083));
#37769=CARTESIAN_POINT('Ctrl Pts',(65.0149031169624,9.20600366322717,-66.7306827345292));
#37770=CARTESIAN_POINT('Ctrl Pts',(65.0116617417207,9.44804792453631,-67.3073858132993));
#37771=CARTESIAN_POINT('Ctrl Pts',(65.0057438245385,9.90725669751229,-68.2956962623178));
#37772=CARTESIAN_POINT('Ctrl Pts',(64.9970188351687,10.9082654800716,-70.1536086093708));
#37773=CARTESIAN_POINT('Ctrl Pts',(64.9975705399216,11.7837966760876,-71.6138987652382));
#37774=CARTESIAN_POINT('Ctrl Pts',(65.0029598100462,12.3378648994254,-72.6662797523441));
#37775=CARTESIAN_POINT('Ctrl Pts',(65.002487371209,12.4735251591182,-72.9239616170365));
#37776=CARTESIAN_POINT('Ctrl Pts',(65.0025224625631,12.7383572372994,-73.4255353796307));
#37777=CARTESIAN_POINT('Ctrl Pts',(65.0022038072545,13.0729215944058,-74.057277410925));
#37778=CARTESIAN_POINT('Ctrl Pts',(65.0020901349283,13.4736029531655,-74.8111709208594));
#37779=CARTESIAN_POINT('Ctrl Pts',(65.0018390996726,14.2767229057767,-76.3187381401072));
#37780=CARTESIAN_POINT('Ctrl Pts',(65.001875261823,14.9461178731812,-77.5712949614773));
#37781=CARTESIAN_POINT('Ctrl Pts',(65.0021384204276,15.9140549467347,-79.3918586961565));
#37782=CARTESIAN_POINT('Ctrl Pts',(65.002024063166,16.3513978914706,-80.2145175100176));
#37783=CARTESIAN_POINT('Ctrl Pts',(65.002024063166,16.7879194788601,-81.035495212116));
#37784=CARTESIAN_POINT('Ctrl Pts',(67.8429974293793,3.43540891085927,24.8291469487336));
#37785=CARTESIAN_POINT('Ctrl Pts',(67.8432546799249,3.43547993540378,24.7802220571657));
#37786=CARTESIAN_POINT('Ctrl Pts',(67.8435244457074,3.43555420488368,24.7312971430194));
#37787=CARTESIAN_POINT('Ctrl Pts',(67.8467070822611,3.43643846206893,24.1801612308648));
#37788=CARTESIAN_POINT('Ctrl Pts',(67.850423105421,3.4379671540823,23.1756927981266));
#37789=CARTESIAN_POINT('Ctrl Pts',(67.8599412644937,3.44198240237162,21.1660007123087));
#37790=CARTESIAN_POINT('Ctrl Pts',(67.8810365616718,3.44791094163207,19.6612635405338));
#37791=CARTESIAN_POINT('Ctrl Pts',(67.9194095919738,3.45624901551685,18.409658962508));
#37792=CARTESIAN_POINT('Ctrl Pts',(67.9382116424961,3.4607672753705,17.9030503904782));
#37793=CARTESIAN_POINT('Ctrl Pts',(67.9860593898693,3.47303081770967,16.8965427733973));
#37794=CARTESIAN_POINT('Ctrl Pts',(68.0882530593835,3.4993540656767,15.1438909478789));
#37795=CARTESIAN_POINT('Ctrl Pts',(68.1787020133392,3.51729805224381,13.654927397164));
#37796=CARTESIAN_POINT('Ctrl Pts',(68.2236660773134,3.51554802305279,12.4161247663745));
#37797=CARTESIAN_POINT('Ctrl Pts',(68.2402940648383,3.51324781151146,11.9218520300229));
#37798=CARTESIAN_POINT('Ctrl Pts',(68.2689151422823,3.50367772430015,10.9290931776768));
#37799=CARTESIAN_POINT('Ctrl Pts',(68.3084504452622,3.47762893596726,9.1831112953065));
#37800=CARTESIAN_POINT('Ctrl Pts',(68.330124390067,3.4515286669216,7.67044414590866));
#37801=CARTESIAN_POINT('Ctrl Pts',(68.3456639197554,3.44053297281301,6.52969946796556));
#37802=CARTESIAN_POINT('Ctrl Pts',(68.3481632218097,3.43698454189682,6.29585970801378));
#37803=CARTESIAN_POINT('Ctrl Pts',(68.3499188822826,3.42562590693248,5.8110691096698));
#37804=CARTESIAN_POINT('Ctrl Pts',(68.3461702772678,3.39691663158025,4.95317353448009));
#37805=CARTESIAN_POINT('Ctrl Pts',(68.3238717322638,3.32643314269278,3.17678659116776));
#37806=CARTESIAN_POINT('Ctrl Pts',(68.3243578395531,3.30825769820171,1.56727520685246));
#37807=CARTESIAN_POINT('Ctrl Pts',(68.3814824067012,3.39780401006464,0.387492102800521));
#37808=CARTESIAN_POINT('Ctrl Pts',(68.389250840906,3.40656484668491,0.26586218911445));
#37809=CARTESIAN_POINT('Ctrl Pts',(68.4077484859294,3.42556880479836,0.0101695747041382));
#37810=CARTESIAN_POINT('Ctrl Pts',(68.4474826307831,3.46000134869164,-0.435804959134103));
#37811=CARTESIAN_POINT('Ctrl Pts',(68.5214044436428,3.51863205261851,-1.08807597925497));
#37812=CARTESIAN_POINT('Ctrl Pts',(68.624423997359,3.6148516485158,-1.88624930375177));
#37813=CARTESIAN_POINT('Ctrl Pts',(68.7620990810596,3.78900640467524,-2.97208615448307));
#37814=CARTESIAN_POINT('Ctrl Pts',(68.8980905600522,4.10565556291278,-4.35854980325192));
#37815=CARTESIAN_POINT('Ctrl Pts',(68.9128946603297,4.46292612828363,-5.48743278551075));
#37816=CARTESIAN_POINT('Ctrl Pts',(68.8835321215552,4.7191174855521,-6.20457561297709));
#37817=CARTESIAN_POINT('Ctrl Pts',(68.8610375207658,4.84466562132032,-6.53581971169089));
#37818=CARTESIAN_POINT('Ctrl Pts',(68.8102656905332,5.11135281124297,-7.1438921545796));
#37819=CARTESIAN_POINT('Ctrl Pts',(68.7008946900405,5.63082823153305,-8.16490344646017));
#37820=CARTESIAN_POINT('Ctrl Pts',(68.5263288525118,6.43604086948472,-9.48848256415375));
#37821=CARTESIAN_POINT('Ctrl Pts',(68.3742468746776,7.15026545438326,-10.683440426365));
#37822=CARTESIAN_POINT('Ctrl Pts',(68.2960339802855,7.50953919485437,-11.4168810335362));
#37823=CARTESIAN_POINT('Ctrl Pts',(68.2603517774568,7.66556351915815,-11.7970269947054));
#37824=CARTESIAN_POINT('Ctrl Pts',(68.2455245078802,7.72624147090396,-11.9718237923998));
#37825=CARTESIAN_POINT('Ctrl Pts',(68.2353382633363,7.76560838945387,-12.0977864186943));
#37826=CARTESIAN_POINT('Ctrl Pts',(68.2257645812627,7.79765679592859,-12.2057340926592));
#37827=CARTESIAN_POINT('Ctrl Pts',(68.2071433316097,7.85343174661,-12.4091862488));
#37828=CARTESIAN_POINT('Ctrl Pts',(68.1716312700611,7.94179601760658,-12.7737396653198));
#37829=CARTESIAN_POINT('Ctrl Pts',(68.070486285267,8.11552251078656,-13.7174857085627));
#37830=CARTESIAN_POINT('Ctrl Pts',(67.9379271384842,8.19411424588751,-14.8288877330147));
#37831=CARTESIAN_POINT('Ctrl Pts',(67.8270359888485,8.24471186271882,-16.0333728136624));
#37832=CARTESIAN_POINT('Ctrl Pts',(67.7795558283908,8.2697989416524,-16.6593623509797));
#37833=CARTESIAN_POINT('Ctrl Pts',(67.7480027142475,8.29425523150742,-17.1744641828378));
#37834=CARTESIAN_POINT('Ctrl Pts',(67.7345704814989,8.30877875862203,-17.4370146473669));
#37835=CARTESIAN_POINT('Ctrl Pts',(67.7255160094835,8.3207465314588,-17.6343120719918));
#37836=CARTESIAN_POINT('Ctrl Pts',(67.7200766017121,8.32681894664132,-17.7435082074001));
#37837=CARTESIAN_POINT('Ctrl Pts',(67.7104052476175,8.33825756147983,-17.9755239104982));
#37838=CARTESIAN_POINT('Ctrl Pts',(67.702668557414,8.34716469625958,-18.2044901227104));
#37839=CARTESIAN_POINT('Ctrl Pts',(67.6966250109244,8.35418836361364,-18.437558078899));
#37840=CARTESIAN_POINT('Ctrl Pts',(67.6935261925001,8.35773483471823,-18.5833576386051));
#37841=CARTESIAN_POINT('Ctrl Pts',(67.6914266176471,8.36012556721365,-18.700617985052));
#37842=CARTESIAN_POINT('Ctrl Pts',(67.6895735618216,8.36221490888489,-18.8180965572433));
#37843=CARTESIAN_POINT('Ctrl Pts',(67.6854569006598,8.36677787513441,-19.1423230547089));
#37844=CARTESIAN_POINT('Ctrl Pts',(67.683716101415,8.36815072888433,-19.6791104208062));
#37845=CARTESIAN_POINT('Ctrl Pts',(67.6906761505665,8.35815154914856,-20.6510943341447));
#37846=CARTESIAN_POINT('Ctrl Pts',(67.7103986169785,8.33193530589776,-21.8996246348123));
#37847=CARTESIAN_POINT('Ctrl Pts',(67.7210587015029,8.31777296136097,-22.9339488548299));
#37848=CARTESIAN_POINT('Ctrl Pts',(67.7207969392067,8.3181111672581,-23.5892647051119));
#37849=CARTESIAN_POINT('Ctrl Pts',(67.7207306160019,8.31824392125545,-23.8355536683885));
#37850=CARTESIAN_POINT('Ctrl Pts',(67.7207252873965,8.31853514921489,-24.3362841907622));
#37851=CARTESIAN_POINT('Ctrl Pts',(67.7210028303336,8.31908037425217,-25.2105431345649));
#37852=CARTESIAN_POINT('Ctrl Pts',(67.7219597458375,8.31988698628591,-26.4655163566117));
#37853=CARTESIAN_POINT('Ctrl Pts',(67.7232034214329,8.3205421062546,-27.9726789655983));
#37854=CARTESIAN_POINT('Ctrl Pts',(67.7235294458012,8.32054619474664,-28.9767651545849));
#37855=CARTESIAN_POINT('Ctrl Pts',(67.7234122675956,8.32035226803725,-29.5405232802499));
#37856=CARTESIAN_POINT('Ctrl Pts',(67.7233746171398,8.32030086018687,-29.665766997083));
#37857=CARTESIAN_POINT('Ctrl Pts',(67.7232565399633,8.32017038515015,-29.9163489293805));
#37858=CARTESIAN_POINT('Ctrl Pts',(67.7229457623811,8.3198743612853,-30.3550172917412));
#37859=CARTESIAN_POINT('Ctrl Pts',(67.721980878253,8.31904185460349,-31.2329279534054));
#37860=CARTESIAN_POINT('Ctrl Pts',(67.7204180440811,8.31770949448862,-32.236944381495));
#37861=CARTESIAN_POINT('Ctrl Pts',(67.7190520692494,8.31630697009927,-33.240595565807));
#37862=CARTESIAN_POINT('Ctrl Pts',(67.7182903018882,8.31530078369864,-33.9928807647374));
#37863=CARTESIAN_POINT('Ctrl Pts',(67.7179528068233,8.31443177002382,-34.7443577769532));
#37864=CARTESIAN_POINT('Ctrl Pts',(67.7181208176444,8.31399598397217,-35.2446452982413));
#37865=CARTESIAN_POINT('Ctrl Pts',(67.7184362791062,8.3137414196746,-35.6205207851054));
#37866=CARTESIAN_POINT('Ctrl Pts',(67.7187154377707,8.31356151267366,-35.8717925217382));
#37867=CARTESIAN_POINT('Ctrl Pts',(67.7195144026143,8.31317245546242,-36.3740602203172));
#37868=CARTESIAN_POINT('Ctrl Pts',(67.7214612042378,8.31246119216897,-37.2516305553014));
#37869=CARTESIAN_POINT('Ctrl Pts',(67.7269127321384,8.31113260339281,-39.0039479458648));
#37870=CARTESIAN_POINT('Ctrl Pts',(67.7320337192982,8.31109429173692,-40.507281071242));
#37871=CARTESIAN_POINT('Ctrl Pts',(67.733889374357,8.31249478383146,-41.6409678438519));
#37872=CARTESIAN_POINT('Ctrl Pts',(67.7342365493349,8.31263805274339,-41.8888468551525));
#37873=CARTESIAN_POINT('Ctrl Pts',(67.7345947148907,8.31247397045901,-42.2629720819454));
#37874=CARTESIAN_POINT('Ctrl Pts',(67.7348187479955,8.31203100483415,-42.6375477798209));
#37875=CARTESIAN_POINT('Ctrl Pts',(67.7349753077395,8.31120760165609,-43.1383858366007));
#37876=CARTESIAN_POINT('Ctrl Pts',(67.7349742950132,8.31000056685548,-43.7663153738706));
#37877=CARTESIAN_POINT('Ctrl Pts',(67.7348795055068,8.3091021318316,-44.5225634357967));
#37878=CARTESIAN_POINT('Ctrl Pts',(67.7349061582348,8.30951233118236,-45.1545493559836));
#37879=CARTESIAN_POINT('Ctrl Pts',(67.7351015739539,8.31096392461986,-45.6609591786128));
#37880=CARTESIAN_POINT('Ctrl Pts',(67.735362038661,8.31271925403025,-46.0411268459948));
#37881=CARTESIAN_POINT('Ctrl Pts',(67.7357638526901,8.31524787949285,-46.4215697992487));
#37882=CARTESIAN_POINT('Ctrl Pts',(67.7365243631353,8.31979852684157,-46.9291808229217));
#37883=CARTESIAN_POINT('Ctrl Pts',(67.737388241482,8.32468631346973,-47.3100182253739));
#37884=CARTESIAN_POINT('Ctrl Pts',(67.7385041109757,8.33080992955567,-47.6922682683125));
#37885=CARTESIAN_POINT('Ctrl Pts',(67.739248602412,8.33665209329345,-47.9613502341259));
#37886=CARTESIAN_POINT('Ctrl Pts',(67.7408867984485,8.35319737208983,-48.4863342036919));
#37887=CARTESIAN_POINT('Ctrl Pts',(67.7441288417548,8.39256514828176,-49.3956985438844));
#37888=CARTESIAN_POINT('Ctrl Pts',(67.7500732418108,8.46277674166923,-50.6532915323841));
#37889=CARTESIAN_POINT('Ctrl Pts',(67.7593067036381,8.52446860885247,-52.1005370157973));
#37890=CARTESIAN_POINT('Ctrl Pts',(67.7663929158143,8.52396027275911,-53.0212614429966));
#37891=CARTESIAN_POINT('Ctrl Pts',(67.7707931388197,8.50357810494722,-53.5830672845635));
#37892=CARTESIAN_POINT('Ctrl Pts',(67.7724365295146,8.4925742604724,-53.7821583853968));
#37893=CARTESIAN_POINT('Ctrl Pts',(67.7760235766481,8.45570310541286,-54.2131780875111));
#37894=CARTESIAN_POINT('Ctrl Pts',(67.7832529202123,8.35676358196918,-54.9979917213648));
#37895=CARTESIAN_POINT('Ctrl Pts',(67.8019920467125,8.06391172112489,-56.7195171344691));
#37896=CARTESIAN_POINT('Ctrl Pts',(67.8248577335212,7.81231208452433,-58.4320647827162));
#37897=CARTESIAN_POINT('Ctrl Pts',(67.8290183714227,7.89213801775489,-59.7675459959514));
#37898=CARTESIAN_POINT('Ctrl Pts',(67.8296331107842,7.9017520647363,-59.9093334780841));
#37899=CARTESIAN_POINT('Ctrl Pts',(67.8306053782331,7.92554871689266,-60.2032949580968));
#37900=CARTESIAN_POINT('Ctrl Pts',(67.8319311069114,7.97692662403817,-60.7093677144899));
#37901=CARTESIAN_POINT('Ctrl Pts',(67.8330622134766,8.11775522230267,-61.7148065060258));
#37902=CARTESIAN_POINT('Ctrl Pts',(67.8318330009838,8.35441804035953,-62.8347017929115));
#37903=CARTESIAN_POINT('Ctrl Pts',(67.8295738539522,8.64714263134489,-63.9267787167824));
#37904=CARTESIAN_POINT('Ctrl Pts',(67.8281598888321,8.82939594565336,-64.529654252364));
#37905=CARTESIAN_POINT('Ctrl Pts',(67.8272568146161,8.95681579596969,-64.9268321940373));
#37906=CARTESIAN_POINT('Ctrl Pts',(67.8266716120575,9.04324849122267,-65.190295819569));
#37907=CARTESIAN_POINT('Ctrl Pts',(67.8261164977612,9.13180453280574,-65.4519050623698));
#37908=CARTESIAN_POINT('Ctrl Pts',(67.825678111527,9.21087621799224,-65.6790189570298));
#37909=CARTESIAN_POINT('Ctrl Pts',(67.8254430601022,9.25648137965921,-65.8082915981344));
#37910=CARTESIAN_POINT('Ctrl Pts',(67.8251055458828,9.32530445335825,-66.0017181851269));
#37911=CARTESIAN_POINT('Ctrl Pts',(67.8248627228961,9.38345311529571,-66.1618153350162));
#37912=CARTESIAN_POINT('Ctrl Pts',(67.8244873775853,9.48086370737567,-66.4261110285533));
#37913=CARTESIAN_POINT('Ctrl Pts',(67.8223242435178,9.59820079307097,-66.7305374425062));
#37914=CARTESIAN_POINT('Ctrl Pts',(67.8190037054621,9.84021958890711,-67.3072623116103));
#37915=CARTESIAN_POINT('Ctrl Pts',(67.8129957587451,10.2993885429522,-68.2955785243475));
#37916=CARTESIAN_POINT('Ctrl Pts',(67.8042632784492,11.3003828720975,-70.1535166719588));
#37917=CARTESIAN_POINT('Ctrl Pts',(67.8049703733839,12.1759401810533,-71.6137975769271));
#37918=CARTESIAN_POINT('Ctrl Pts',(67.8104034129806,12.7300087363492,-72.6661690355186));
#37919=CARTESIAN_POINT('Ctrl Pts',(67.8099283136533,12.8656678936038,-72.9238529497301));
#37920=CARTESIAN_POINT('Ctrl Pts',(67.8099648416568,13.130499120933,-73.4254282690125));
#37921=CARTESIAN_POINT('Ctrl Pts',(67.8096445242436,13.465062786893,-74.0571725299553));
#37922=CARTESIAN_POINT('Ctrl Pts',(67.8095299586602,13.8657447063598,-74.8110678320985));
#37923=CARTESIAN_POINT('Ctrl Pts',(67.8092757135153,14.6688669633785,-76.3186376482257));
#37924=CARTESIAN_POINT('Ctrl Pts',(67.8093094569773,15.338264183902,-77.5711925878768));
#37925=CARTESIAN_POINT('Ctrl Pts',(67.809574689212,16.3061992093518,-79.3917515508846));
#37926=CARTESIAN_POINT('Ctrl Pts',(67.8094593526752,16.7435423574498,-80.2144112969835));
#37927=CARTESIAN_POINT('Ctrl Pts',(67.809459352675,17.1800639448392,-81.0353889990819));
#37928=CARTESIAN_POINT('Ctrl Pts',(70.6494615867083,3.83081038259429,24.8276527484924));
#37929=CARTESIAN_POINT('Ctrl Pts',(70.6496322197946,3.83090610428414,24.7786798140215));
#37930=CARTESIAN_POINT('Ctrl Pts',(70.6498112335071,3.83100625888237,24.729706115986));
#37931=CARTESIAN_POINT('Ctrl Pts',(70.6519243534644,3.83219418091214,24.1780051253099));
#37932=CARTESIAN_POINT('Ctrl Pts',(70.6530393935946,3.83471357029684,23.1723497522651));
#37933=CARTESIAN_POINT('Ctrl Pts',(70.6553276454399,3.84151431914779,21.1618905015551));
#37934=CARTESIAN_POINT('Ctrl Pts',(70.6694173401099,3.84933576491011,19.6579544827044));
#37935=CARTESIAN_POINT('Ctrl Pts',(70.7017957450429,3.85799813994687,18.4074358300531));
#37936=CARTESIAN_POINT('Ctrl Pts',(70.716679458464,3.86261409154474,17.8992953377625));
#37937=CARTESIAN_POINT('Ctrl Pts',(70.7528580384059,3.8748631628684,16.8915796329347));
#37938=CARTESIAN_POINT('Ctrl Pts',(70.8302073256714,3.90047804800543,15.1380162766548));
#37939=CARTESIAN_POINT('Ctrl Pts',(70.9112737776838,3.91699285560921,13.6541782529586));
#37940=CARTESIAN_POINT('Ctrl Pts',(70.9763136585358,3.91434581461649,12.4237737939805));
#37941=CARTESIAN_POINT('Ctrl Pts',(71.0030615265596,3.91054675463754,11.9395225358356));
#37942=CARTESIAN_POINT('Ctrl Pts',(71.059252040738,3.89423065634749,10.9566776530166));
#37943=CARTESIAN_POINT('Ctrl Pts',(71.1632501986744,3.85093053759193,9.21600588337804));
#37944=CARTESIAN_POINT('Ctrl Pts',(71.258082759856,3.81527809606321,7.6801825507519));
#37945=CARTESIAN_POINT('Ctrl Pts',(71.3272876674223,3.82214129678024,6.50824099154105));
#37946=CARTESIAN_POINT('Ctrl Pts',(71.3427511315147,3.82225228568385,6.28252554743425));
#37947=CARTESIAN_POINT('Ctrl Pts',(71.3749157017795,3.81715545366023,5.80195360798077));
#37948=CARTESIAN_POINT('Ctrl Pts',(71.4340146686344,3.79815526889341,4.94708066621355));
#37949=CARTESIAN_POINT('Ctrl Pts',(71.5592359131306,3.74889711351366,3.13847167959589));
#37950=CARTESIAN_POINT('Ctrl Pts',(71.6637014711367,3.81595624082737,1.43529850844767));
#37951=CARTESIAN_POINT('Ctrl Pts',(71.695580427591,4.05978180199612,0.177804686666928));
#37952=CARTESIAN_POINT('Ctrl Pts',(71.6999732590441,4.08946439535741,0.0303564999101921));
#37953=CARTESIAN_POINT('Ctrl Pts',(71.7086632146237,4.15430759573429,-0.263208884210683));
#37954=CARTESIAN_POINT('Ctrl Pts',(71.7241800042281,4.28010993359288,-0.770233236761601));
#37955=CARTESIAN_POINT('Ctrl Pts',(71.7446746252156,4.49143771191879,-1.47731006830424));
#37956=CARTESIAN_POINT('Ctrl Pts',(71.762159457237,4.78057345871927,-2.29732944268844));
#37957=CARTESIAN_POINT('Ctrl Pts',(71.7719393440816,5.19615493718386,-3.35702174402344));
#37958=CARTESIAN_POINT('Ctrl Pts',(71.7559918046913,5.73883808961284,-4.62551787475727));
#37959=CARTESIAN_POINT('Ctrl Pts',(71.7136458140211,6.14233610559966,-5.60372928407037));
#37960=CARTESIAN_POINT('Ctrl Pts',(71.6746492911468,6.36893997037483,-6.21041150356981));
#37961=CARTESIAN_POINT('Ctrl Pts',(71.6454197256439,6.47958282642054,-6.50916156374574));
#37962=CARTESIAN_POINT('Ctrl Pts',(71.5852832929708,6.69926928674286,-7.06348594446982));
#37963=CARTESIAN_POINT('Ctrl Pts',(71.4592658050832,7.10401302870599,-8.02462303818132));
#37964=CARTESIAN_POINT('Ctrl Pts',(71.2502834631539,7.68573829926759,-9.31372015535913));
#37965=CARTESIAN_POINT('Ctrl Pts',(71.0413556697638,8.17269220545024,-10.4897481554329));
#37966=CARTESIAN_POINT('Ctrl Pts',(70.9194458564485,8.41683332486132,-11.2238938763871));
#37967=CARTESIAN_POINT('Ctrl Pts',(70.8610035588855,8.52564254806769,-11.615056859852));
#37968=CARTESIAN_POINT('Ctrl Pts',(70.8363802328729,8.56936123861665,-11.8004058535334));
#37969=CARTESIAN_POINT('Ctrl Pts',(70.8199004857342,8.59828419220826,-11.9363044116113));
#37970=CARTESIAN_POINT('Ctrl Pts',(70.8088851203888,8.61784702361031,-12.0351348832902));
#37971=CARTESIAN_POINT('Ctrl Pts',(70.7877298701005,8.65261401658615,-12.2300774357788));
#37972=CARTESIAN_POINT('Ctrl Pts',(70.7529125032501,8.70419637134419,-12.5775034833244));
#37973=CARTESIAN_POINT('Ctrl Pts',(70.6746241477646,8.79351350793665,-13.4950523222552));
#37974=CARTESIAN_POINT('Ctrl Pts',(70.6249320620081,8.77854019843266,-14.6202130090127));
#37975=CARTESIAN_POINT('Ctrl Pts',(70.5942999785663,8.73282150953588,-15.8659952169765));
#37976=CARTESIAN_POINT('Ctrl Pts',(70.5806966383333,8.71427565623005,-16.5189882853968));
#37977=CARTESIAN_POINT('Ctrl Pts',(70.5696178200984,8.70844385895726,-17.0599653686636));
#37978=CARTESIAN_POINT('Ctrl Pts',(70.5636838942566,8.71000547360416,-17.336837376577));
#37979=CARTESIAN_POINT('Ctrl Pts',(70.5590254237539,8.71329389796812,-17.5453587994702));
#37980=CARTESIAN_POINT('Ctrl Pts',(70.5561572316978,8.71502260422576,-17.6621814337956));
#37981=CARTESIAN_POINT('Ctrl Pts',(70.5510255856973,8.71822746059492,-17.9085181649483));
#37982=CARTESIAN_POINT('Ctrl Pts',(70.5468012755684,8.72073272086908,-18.150816531429));
#37983=CARTESIAN_POINT('Ctrl Pts',(70.5433888034654,8.72269270957472,-18.3960889291585));
#37984=CARTESIAN_POINT('Ctrl Pts',(70.5415763630612,8.72368369038835,-18.5490734867898));
#37985=CARTESIAN_POINT('Ctrl Pts',(70.5403073344523,8.72435033031262,-18.671805298334));
#37986=CARTESIAN_POINT('Ctrl Pts',(70.5391551996401,8.72493311342539,-18.7945736263313));
#37987=CARTESIAN_POINT('Ctrl Pts',(70.5364509944023,8.72620928357726,-19.1326061682313));
#37988=CARTESIAN_POINT('Ctrl Pts',(70.5343972821601,8.72661516653376,-19.687874997866));
#37989=CARTESIAN_POINT('Ctrl Pts',(70.5355551407817,8.72397510411148,-20.6811247268949));
#37990=CARTESIAN_POINT('Ctrl Pts',(70.5423870553301,8.71703505613488,-21.9344602149432));
#37991=CARTESIAN_POINT('Ctrl Pts',(70.5458672100272,8.71341297499298,-22.9497504021268));
#37992=CARTESIAN_POINT('Ctrl Pts',(70.5450425115542,8.71353162267228,-23.5865416628728));
#37993=CARTESIAN_POINT('Ctrl Pts',(70.5447524535521,8.71358037896091,-23.8349082908723));
#37994=CARTESIAN_POINT('Ctrl Pts',(70.5442983469629,8.7136916662106,-24.3345141000982));
#37995=CARTESIAN_POINT('Ctrl Pts',(70.5438078693597,8.7139106295647,-25.2095714068707));
#37996=CARTESIAN_POINT('Ctrl Pts',(70.5437941381743,8.71424852180923,-26.4642469765464));
#37997=CARTESIAN_POINT('Ctrl Pts',(70.5443287824551,8.71451471806677,-27.9721250967088));
#37998=CARTESIAN_POINT('Ctrl Pts',(70.5446736941038,8.71452884238773,-28.9765652628975));
#37999=CARTESIAN_POINT('Ctrl Pts',(70.5447699397357,8.71445478785512,-29.5405978731148));
#38000=CARTESIAN_POINT('Ctrl Pts',(70.5447892237904,8.71443464959818,-29.6659103240058));
#38001=CARTESIAN_POINT('Ctrl Pts',(70.5448181933689,8.71438230721395,-29.9166154371908));
#38002=CARTESIAN_POINT('Ctrl Pts',(70.54484704347,8.71426257513622,-30.3554914438346));
#38003=CARTESIAN_POINT('Ctrl Pts',(70.5448484874897,8.71392245129362,-31.2337460927015));
#38004=CARTESIAN_POINT('Ctrl Pts',(70.5448503146429,8.71338620005043,-32.2380110739719));
#38005=CARTESIAN_POINT('Ctrl Pts',(70.5451209127849,8.71284402078748,-33.2417255403863));
#38006=CARTESIAN_POINT('Ctrl Pts',(70.545524545668,8.71247043219124,-33.9939571890433));
#38007=CARTESIAN_POINT('Ctrl Pts',(70.5461899905228,8.71217492752451,-34.745310445793));
#38008=CARTESIAN_POINT('Ctrl Pts',(70.5468533445406,8.71205173577247,-35.2454547113171));
#38009=CARTESIAN_POINT('Ctrl Pts',(70.5474518280046,8.7119952320563,-35.6211998712757));
#38010=CARTESIAN_POINT('Ctrl Pts',(70.5479053429065,8.71194401385795,-35.8724813300518));
#38011=CARTESIAN_POINT('Ctrl Pts',(70.5489976699394,8.71180045174142,-36.3747090579339));
#38012=CARTESIAN_POINT('Ctrl Pts',(70.5513235945551,8.71148120053779,-37.25224972174));
#38013=CARTESIAN_POINT('Ctrl Pts',(70.5571200607568,8.71082727063191,-39.0044553013496));
#38014=CARTESIAN_POINT('Ctrl Pts',(70.5622026385591,8.71119028705882,-40.507733876685));
#38015=CARTESIAN_POINT('Ctrl Pts',(70.5642533127471,8.71286542617711,-41.6413563416797));
#38016=CARTESIAN_POINT('Ctrl Pts',(70.5646535512609,8.71307078591043,-41.8892293291521));
#38017=CARTESIAN_POINT('Ctrl Pts',(70.5651134875453,8.7129994767808,-42.2633385288916));
#38018=CARTESIAN_POINT('Ctrl Pts',(70.5654559292171,8.71264828930115,-42.6378971883292));
#38019=CARTESIAN_POINT('Ctrl Pts',(70.5657845586926,8.7119437590644,-43.1387086748049));
#38020=CARTESIAN_POINT('Ctrl Pts',(70.5660106650976,8.71087613352797,-43.7665989444598));
#38021=CARTESIAN_POINT('Ctrl Pts',(70.5661608227567,8.71012005394437,-44.5227896309756));
#38022=CARTESIAN_POINT('Ctrl Pts',(70.566329581619,8.71061958030634,-45.1547199927119));
#38023=CARTESIAN_POINT('Ctrl Pts',(70.5665777677508,8.71212136138571,-45.6610764214851));
#38024=CARTESIAN_POINT('Ctrl Pts',(70.5668416372251,8.71390179747749,-46.0412015657389));
#38025=CARTESIAN_POINT('Ctrl Pts',(70.5672048319196,8.71644188043345,-46.4215992068969));
#38026=CARTESIAN_POINT('Ctrl Pts',(70.5678496720794,8.72098788065634,-46.9291451205241));
#38027=CARTESIAN_POINT('Ctrl Pts',(70.5685468480872,8.72584790750339,-47.3099316252934));
#38028=CARTESIAN_POINT('Ctrl Pts',(70.5694292279528,8.73192477619373,-47.6921253853199));
#38029=CARTESIAN_POINT('Ctrl Pts',(70.5700003368078,8.73772742858547,-47.9611518169856));
#38030=CARTESIAN_POINT('Ctrl Pts',(70.5712314195025,8.75416940983707,-48.48604651909));
#38031=CARTESIAN_POINT('Ctrl Pts',(70.5736110193162,8.79329630484929,-49.3952769089704));
#38032=CARTESIAN_POINT('Ctrl Pts',(70.5779524846989,8.86303714057703,-50.6527605487821));
#38033=CARTESIAN_POINT('Ctrl Pts',(70.5848185478071,8.92405103147752,-52.0999818910618));
#38034=CARTESIAN_POINT('Ctrl Pts',(70.5901264532065,8.92307445153632,-53.020761634185));
#38035=CARTESIAN_POINT('Ctrl Pts',(70.5933774910263,8.90240281065996,-53.5826199270936));
#38036=CARTESIAN_POINT('Ctrl Pts',(70.5945212135569,8.89128249120398,-53.7816814909825));
#38037=CARTESIAN_POINT('Ctrl Pts',(70.5970060354552,8.85414562790396,-54.2126775327943));
#38038=CARTESIAN_POINT('Ctrl Pts',(70.602081823671,8.75468006093425,-54.9974504674917));
#38039=CARTESIAN_POINT('Ctrl Pts',(70.6160221912734,8.46061464007003,-56.7189531513493));
#38040=CARTESIAN_POINT('Ctrl Pts',(70.6351103426861,8.20797913919722,-58.4315994063654));
#38041=CARTESIAN_POINT('Ctrl Pts',(70.6378365999834,8.28745204929791,-59.7672968589652));
#38042=CARTESIAN_POINT('Ctrl Pts',(70.6382848453043,8.29702790860994,-59.9091084957715));
#38043=CARTESIAN_POINT('Ctrl Pts',(70.6389525410391,8.32075687283495,-60.2031166527417));
#38044=CARTESIAN_POINT('Ctrl Pts',(70.6398172088392,8.37204173475601,-60.709263749262));
#38045=CARTESIAN_POINT('Ctrl Pts',(70.6402867499701,8.51277042585894,-61.7148228641222));
#38046=CARTESIAN_POINT('Ctrl Pts',(70.638773558215,8.74946275086096,-62.8347876548578));
#38047=CARTESIAN_POINT('Ctrl Pts',(70.6364542699192,9.04226090895522,-63.9268738865825));
#38048=CARTESIAN_POINT('Ctrl Pts',(70.6350447518703,9.22455564675501,-64.5297344920004));
#38049=CARTESIAN_POINT('Ctrl Pts',(70.6341417987604,9.35199653545435,-64.9268947241361));
#38050=CARTESIAN_POINT('Ctrl Pts',(70.6335546618577,9.43844104194086,-65.190344545352));
#38051=CARTESIAN_POINT('Ctrl Pts',(70.6329927939914,9.52700508046247,-65.4519370729589));
#38052=CARTESIAN_POINT('Ctrl Pts',(70.6325409742643,9.60607918432695,-65.6790338502266));
#38053=CARTESIAN_POINT('Ctrl Pts',(70.6322956459119,9.65168428141731,-65.8082960098274));
#38054=CARTESIAN_POINT('Ctrl Pts',(70.6319398706883,9.72050573437257,-66.0017062053914));
#38055=CARTESIAN_POINT('Ctrl Pts',(70.6316754937635,9.77864972549694,-66.1617882408552));
#38056=CARTESIAN_POINT('Ctrl Pts',(70.6312532272026,9.87604743186078,-66.4260575880187));
#38057=CARTESIAN_POINT('Ctrl Pts',(70.6290371086404,9.99337943718072,-66.7304845122077));
#38058=CARTESIAN_POINT('Ctrl Pts',(70.6256389157257,10.2353858042967,-67.307196740313));
#38059=CARTESIAN_POINT('Ctrl Pts',(70.6195462770368,10.6945410254072,-68.2955029168157));
#38060=CARTESIAN_POINT('Ctrl Pts',(70.6108239238681,11.6955282837264,-70.1534275139502));
#38061=CARTESIAN_POINT('Ctrl Pts',(70.6116930692152,12.5711084944599,-71.6137122376235));
#38062=CARTESIAN_POINT('Ctrl Pts',(70.6171581906643,13.1251914954288,-72.6660905521361));
#38063=CARTESIAN_POINT('Ctrl Pts',(70.6166812737942,13.2608498799591,-72.9237733872693));
#38064=CARTESIAN_POINT('Ctrl Pts',(70.6167190088863,13.5256816230138,-73.4253481416168));
#38065=CARTESIAN_POINT('Ctrl Pts',(70.6163977241997,13.8602447820587,-74.057091397903));
#38066=CARTESIAN_POINT('Ctrl Pts',(70.6162826798284,14.2609262348746,-74.8109860365976));
#38067=CARTESIAN_POINT('Ctrl Pts',(70.616026343113,15.0640469642179,-76.3185549194688));
#38068=CARTESIAN_POINT('Ctrl Pts',(70.6160585036137,15.7334432769212,-77.5711107183318));
#38069=CARTESIAN_POINT('Ctrl Pts',(70.6163251147076,16.7013796602407,-79.3916714502491));
#38070=CARTESIAN_POINT('Ctrl Pts',(70.61620923224,17.1387224495204,-80.2143308256623));
#38071=CARTESIAN_POINT('Ctrl Pts',(70.6162092322401,17.5752440369097,-81.0353085277609));
#38072=CARTESIAN_POINT('Ctrl Pts',(73.4534500542343,4.22530703961414,24.8335658669903));
#38073=CARTESIAN_POINT('Ctrl Pts',(73.4535261461378,4.22524543761862,24.7847807094142));
#38074=CARTESIAN_POINT('Ctrl Pts',(73.4536061943624,4.22518075424666,24.7359974325107));
#38075=CARTESIAN_POINT('Ctrl Pts',(73.4545512309376,4.22442705508417,24.1865265777239));
#38076=CARTESIAN_POINT('Ctrl Pts',(73.4518393006747,4.22214471221797,23.1833994211906));
#38077=CARTESIAN_POINT('Ctrl Pts',(73.4432871874621,4.21564347341985,21.1771448625688));
#38078=CARTESIAN_POINT('Ctrl Pts',(73.4496477417741,4.21095875268741,19.675290208693));
#38079=CARTESIAN_POINT('Ctrl Pts',(73.4803655216321,4.20940140260513,18.4259537057235));
#38080=CARTESIAN_POINT('Ctrl Pts',(73.4934052258452,4.20716909151018,17.932690249231));
#38081=CARTESIAN_POINT('Ctrl Pts',(73.5231636817857,4.19898855516301,16.9350263109554));
#38082=CARTESIAN_POINT('Ctrl Pts',(73.5876238488452,4.18199957258835,15.1776786176254));
#38083=CARTESIAN_POINT('Ctrl Pts',(73.6730048552458,4.18371618038397,13.6462334631478));
#38084=CARTESIAN_POINT('Ctrl Pts',(73.7707468465167,4.21638754708557,12.3551073610112));
#38085=CARTESIAN_POINT('Ctrl Pts',(73.8141206538761,4.22930990269526,11.8605690057779));
#38086=CARTESIAN_POINT('Ctrl Pts',(73.9145642754093,4.25858474957933,10.8516399198657));
#38087=CARTESIAN_POINT('Ctrl Pts',(74.1168743384341,4.32647233590466,9.07410025684771));
#38088=CARTESIAN_POINT('Ctrl Pts',(74.3029360600045,4.4425032821772,7.50898960266336));
#38089=CARTESIAN_POINT('Ctrl Pts',(74.4141506591024,4.58646542369393,6.31641947569288));
#38090=CARTESIAN_POINT('Ctrl Pts',(74.4407928859277,4.61616562076266,6.06973731158189));
#38091=CARTESIAN_POINT('Ctrl Pts',(74.4971534009537,4.6806267462007,5.56172564630839));
#38092=CARTESIAN_POINT('Ctrl Pts',(74.601678333609,4.8034795552565,4.66722232741208));
#38093=CARTESIAN_POINT('Ctrl Pts',(74.8082987931951,5.10837288549013,2.83336863996513));
#38094=CARTESIAN_POINT('Ctrl Pts',(74.8896403398205,5.4850325276308,1.22545573439517));
#38095=CARTESIAN_POINT('Ctrl Pts',(74.8560557798504,5.79782347580794,0.0737985541994678));
#38096=CARTESIAN_POINT('Ctrl Pts',(74.85013591491,5.83828359682733,-0.0741003001395361));
#38097=CARTESIAN_POINT('Ctrl Pts',(74.8368000379755,5.92109119870578,-0.360513775030337));
#38098=CARTESIAN_POINT('Ctrl Pts',(74.8077813744316,6.07422124244255,-0.857580978294587));
#38099=CARTESIAN_POINT('Ctrl Pts',(74.7543900602967,6.30982836377159,-1.54628365855503));
#38100=CARTESIAN_POINT('Ctrl Pts',(74.6794527915681,6.60760335801143,-2.34684895453022));
#38101=CARTESIAN_POINT('Ctrl Pts',(74.5732518390376,7.00990054092547,-3.38247175253405));
#38102=CARTESIAN_POINT('Ctrl Pts',(74.4409539994718,7.4958887565096,-4.62234763704644));
#38103=CARTESIAN_POINT('Ctrl Pts',(74.3475250999459,7.80738682333361,-5.54684334097161));
#38104=CARTESIAN_POINT('Ctrl Pts',(74.2938139307462,7.96133952783586,-6.0988766407598));
#38105=CARTESIAN_POINT('Ctrl Pts',(74.2647775466287,8.03246032546773,-6.36322088900162));
#38106=CARTESIAN_POINT('Ctrl Pts',(74.2041405975534,8.16462668068318,-6.86450029538272));
#38107=CARTESIAN_POINT('Ctrl Pts',(74.082310243454,8.38762885031026,-7.74660588572107));
#38108=CARTESIAN_POINT('Ctrl Pts',(73.8765336055004,8.67004719556913,-8.96897319517573));
#38109=CARTESIAN_POINT('Ctrl Pts',(73.6612677870246,8.90659584048753,-10.136850718449));
#38110=CARTESIAN_POINT('Ctrl Pts',(73.5369674395633,9.04056470444529,-10.9203298436466));
#38111=CARTESIAN_POINT('Ctrl Pts',(73.4783954127976,9.10574908890705,-11.3597543307435));
#38112=CARTESIAN_POINT('Ctrl Pts',(73.4540520371645,9.1340838595355,-11.576618913669));
#38113=CARTESIAN_POINT('Ctrl Pts',(73.4378760186849,9.15358601547536,-11.738750893759));
#38114=CARTESIAN_POINT('Ctrl Pts',(73.4277279991916,9.16489552177659,-11.8419683144316));
#38115=CARTESIAN_POINT('Ctrl Pts',(73.4094336380798,9.18538844204145,-12.0534225491334));
#38116=CARTESIAN_POINT('Ctrl Pts',(73.3828098713282,9.21382756833954,-12.4260873709192));
#38117=CARTESIAN_POINT('Ctrl Pts',(73.3396199506344,9.25366717695632,-13.4097635557345));
#38118=CARTESIAN_POINT('Ctrl Pts',(73.3513919908944,9.21041740505572,-14.579844251102));
#38119=CARTESIAN_POINT('Ctrl Pts',(73.3724351517644,9.15254998529332,-15.8391607356278));
#38120=CARTESIAN_POINT('Ctrl Pts',(73.3809135708858,9.12816610581944,-16.4913838822319));
#38121=CARTESIAN_POINT('Ctrl Pts',(73.3838015871584,9.11595394197832,-17.0271642040383));
#38122=CARTESIAN_POINT('Ctrl Pts',(73.3834810356021,9.11322709619638,-17.2998548135131));
#38123=CARTESIAN_POINT('Ctrl Pts',(73.3824118783939,9.11277040383227,-17.5049039873859));
#38124=CARTESIAN_POINT('Ctrl Pts',(73.3817303794556,9.11252511086424,-17.6264661651878));
#38125=CARTESIAN_POINT('Ctrl Pts',(73.3804945331111,9.11204419200424,-17.8778405066787));
#38126=CARTESIAN_POINT('Ctrl Pts',(73.3794318496841,9.11163048321859,-18.1262675031507));
#38127=CARTESIAN_POINT('Ctrl Pts',(73.3785303839214,9.11125930326834,-18.376417266739));
#38128=CARTESIAN_POINT('Ctrl Pts',(73.3780294989107,9.11104885276049,-18.5324459754145));
#38129=CARTESIAN_POINT('Ctrl Pts',(73.3776646905098,9.11089109109327,-18.6574341720327));
#38130=CARTESIAN_POINT('Ctrl Pts',(73.3773229575204,9.11074085129781,-18.782403736847));
#38131=CARTESIAN_POINT('Ctrl Pts',(73.3764752540345,9.1103577006343,-19.126171262133));
#38132=CARTESIAN_POINT('Ctrl Pts',(73.375560929654,9.10988412298222,-19.6891487734336));
#38133=CARTESIAN_POINT('Ctrl Pts',(73.37492459789,9.10937069259306,-20.6913692318905));
#38134=CARTESIAN_POINT('Ctrl Pts',(73.3753250105335,9.1091511101525,-21.9470238577363));
#38135=CARTESIAN_POINT('Ctrl Pts',(73.3754902779273,9.10896297491011,-22.9548467423427));
#38136=CARTESIAN_POINT('Ctrl Pts',(73.3750953915219,9.10869646092465,-23.5842032232804));
#38137=CARTESIAN_POINT('Ctrl Pts',(73.3749589661061,9.10859484477579,-23.8334633318891));
#38138=CARTESIAN_POINT('Ctrl Pts',(73.374757891282,9.10840641206924,-24.3327077001457));
#38139=CARTESIAN_POINT('Ctrl Pts',(73.3745720422855,9.10811659521834,-25.2082704533436));
#38140=CARTESIAN_POINT('Ctrl Pts',(73.3746618262452,9.10783137522724,-26.4631295916326));
#38141=CARTESIAN_POINT('Ctrl Pts',(73.3749657200172,9.10770078254226,-27.9717563735793));
#38142=CARTESIAN_POINT('Ctrl Pts',(73.3750395148263,9.10776770662891,-28.9767329786706));
#38143=CARTESIAN_POINT('Ctrl Pts',(73.374971844802,9.10784600977214,-29.5411142749989));
#38144=CARTESIAN_POINT('Ctrl Pts',(73.3749520653695,9.10786501892074,-29.6665536455528));
#38145=CARTESIAN_POINT('Ctrl Pts',(73.3748952785016,9.10791093907323,-29.9174696229282));
#38146=CARTESIAN_POINT('Ctrl Pts',(73.374754720345,9.10801155353313,-30.356701473297));
#38147=CARTESIAN_POINT('Ctrl Pts',(73.374343963929,9.10828383298627,-31.235529090884));
#38148=CARTESIAN_POINT('Ctrl Pts',(73.3737352665426,9.10872849397928,-32.240171135434));
#38149=CARTESIAN_POINT('Ctrl Pts',(73.3733039339751,9.10923386491297,-33.2439532345848));
#38150=CARTESIAN_POINT('Ctrl Pts',(73.3731483647105,9.10962642968375,-33.9960783367514));
#38151=CARTESIAN_POINT('Ctrl Pts',(73.3732390933077,9.11002142319734,-34.7471853776243));
#38152=CARTESIAN_POINT('Ctrl Pts',(73.3735168372938,9.11027405601257,-35.2470629337144));
#38153=CARTESIAN_POINT('Ctrl Pts',(73.3738272805288,9.11045526780762,-35.6225726730903));
#38154=CARTESIAN_POINT('Ctrl Pts',(73.3740783756241,9.11055927079173,-35.8738667644384));
#38155=CARTESIAN_POINT('Ctrl Pts',(73.3747327033794,9.11071066242431,-36.3760208794514));
#38156=CARTESIAN_POINT('Ctrl Pts',(73.3762244220803,9.11086826910444,-37.2534866607658));
#38157=CARTESIAN_POINT('Ctrl Pts',(73.3801775570183,9.11102577369151,-39.005485963845));
#38158=CARTESIAN_POINT('Ctrl Pts',(73.3837917918894,9.11189357371564,-40.5086054277271));
#38159=CARTESIAN_POINT('Ctrl Pts',(73.3851792829503,9.11389947437443,-41.6420873839513));
#38160=CARTESIAN_POINT('Ctrl Pts',(73.3854450145328,9.11417701530638,-41.8899447419186));
#38161=CARTESIAN_POINT('Ctrl Pts',(73.3857372125606,9.1142140555757,-42.2640189060008));
#38162=CARTESIAN_POINT('Ctrl Pts',(73.3859411380443,9.11396919579392,-42.6385418757349));
#38163=CARTESIAN_POINT('Ctrl Pts',(73.3861185940242,9.1134023526539,-43.139299737331));
#38164=CARTESIAN_POINT('Ctrl Pts',(73.3862074374739,9.11249544850946,-43.7671150597367));
#38165=CARTESIAN_POINT('Ctrl Pts',(73.3862410262631,9.11190324748228,-44.5232019152918));
#38166=CARTESIAN_POINT('Ctrl Pts',(73.3863239318621,9.1125059872366,-45.1550349083222));
#38167=CARTESIAN_POINT('Ctrl Pts',(73.3864921887458,9.11406440388159,-45.6613053538075));
#38168=CARTESIAN_POINT('Ctrl Pts',(73.3866864657229,9.1158731191196,-46.0413625920448));
#38169=CARTESIAN_POINT('Ctrl Pts',(73.3869660099852,9.11842584219486,-46.4216887641487));
#38170=CARTESIAN_POINT('Ctrl Pts',(73.38747481916,9.12296591629808,-46.9291343438024));
#38171=CARTESIAN_POINT('Ctrl Pts',(73.3880358469146,9.12779386455806,-47.3098405435582));
#38172=CARTESIAN_POINT('Ctrl Pts',(73.3887503569359,9.13381707555844,-47.691948928767));
#38173=CARTESIAN_POINT('Ctrl Pts',(73.3892102426715,9.13957410884946,-47.9608941784767));
#38174=CARTESIAN_POINT('Ctrl Pts',(73.3902179406663,9.15589543877677,-48.4856545677139));
#38175=CARTESIAN_POINT('Ctrl Pts',(73.3921985051051,9.19474065609386,-49.3946756678471));
#38176=CARTESIAN_POINT('Ctrl Pts',(73.3959021785531,9.26392505198861,-50.6519574390876));
#38177=CARTESIAN_POINT('Ctrl Pts',(73.4017820248472,9.32415959397272,-52.0990825771574));
#38178=CARTESIAN_POINT('Ctrl Pts',(73.4062117762354,9.32265822262322,-53.0199084620258));
#38179=CARTESIAN_POINT('Ctrl Pts',(73.4088249153412,9.3016739371985,-53.5818290458706));
#38180=CARTESIAN_POINT('Ctrl Pts',(73.4096908343255,9.29043617440867,-53.7808133826808));
#38181=CARTESIAN_POINT('Ctrl Pts',(73.4115519159643,9.25302703661083,-54.2117394820634));
#38182=CARTESIAN_POINT('Ctrl Pts',(73.4153808109127,9.15301479350725,-54.9964162298912));
#38183=CARTESIAN_POINT('Ctrl Pts',(73.4264123496012,8.8576334816423,-56.7179266148824));
#38184=CARTESIAN_POINT('Ctrl Pts',(73.4430779286312,8.60377321678145,-58.4308178751789));
#38185=CARTESIAN_POINT('Ctrl Pts',(73.444838502715,8.68284878733253,-59.7669036929714));
#38186=CARTESIAN_POINT('Ctrl Pts',(73.4451721176443,8.69238362667795,-59.9087566277868));
#38187=CARTESIAN_POINT('Ctrl Pts',(73.4456240207106,8.71603985479539,-60.2028457441212));
#38188=CARTESIAN_POINT('Ctrl Pts',(73.446143750728,8.76722709000681,-60.709121606154));
#38189=CARTESIAN_POINT('Ctrl Pts',(73.4460455539418,8.90785948285092,-61.7148923746929));
#38190=CARTESIAN_POINT('Ctrl Pts',(73.4441177941321,9.14460506842151,-62.8349929840275));
#38191=CARTESIAN_POINT('Ctrl Pts',(73.4415270623419,9.43750285592813,-63.9271205232897));
#38192=CARTESIAN_POINT('Ctrl Pts',(73.4400005326718,9.6198518088817,-64.5299709949832));
#38193=CARTESIAN_POINT('Ctrl Pts',(73.4390267578198,9.74731987964292,-64.9271111701042));
#38194=CARTESIAN_POINT('Ctrl Pts',(73.4383938206596,9.83377965730146,-65.1905440689006));
#38195=CARTESIAN_POINT('Ctrl Pts',(73.4377874324485,9.9223538360786,-65.4521145233453));
#38196=CARTESIAN_POINT('Ctrl Pts',(73.4372964622778,10.0014310286135,-65.6791873567961));
#38197=CARTESIAN_POINT('Ctrl Pts',(73.4370285010553,10.0470360365303,-65.8084345186529));
#38198=CARTESIAN_POINT('Ctrl Pts',(73.4366384216936,10.1158554304746,-66.001820943482));
#38199=CARTESIAN_POINT('Ctrl Pts',(73.4363444861434,10.1739933922247,-66.1618803559984));
#38200=CARTESIAN_POINT('Ctrl Pts',(73.4358709744576,10.2713748692444,-66.4261095447157));
#38201=CARTESIAN_POINT('Ctrl Pts',(73.4336107433578,10.3887104406191,-66.73054466064));
#38202=CARTESIAN_POINT('Ctrl Pts',(73.430148174877,10.6307141189376,-67.3072458305105));
#38203=CARTESIAN_POINT('Ctrl Pts',(73.4240012424698,11.0898737170571,-68.2955485558258));
#38204=CARTESIAN_POINT('Ctrl Pts',(73.4153423680144,12.0908750091205,-70.1534602311583));
#38205=CARTESIAN_POINT('Ctrl Pts',(73.4163672214855,12.9664743628694,-71.6137496163334));
#38206=CARTESIAN_POINT('Ctrl Pts',(73.4218150309494,13.5205581904781,-72.6661328912094));
#38207=CARTESIAN_POINT('Ctrl Pts',(73.4213389989221,13.6562169812378,-72.9238146915836));
#38208=CARTESIAN_POINT('Ctrl Pts',(73.4213760062523,13.9210491080679,-73.4253886789845));
#38209=CARTESIAN_POINT('Ctrl Pts',(73.4210551940842,14.2556124364939,-74.0571308278724));
#38210=CARTESIAN_POINT('Ctrl Pts',(73.4209404667533,14.6562935493408,-74.8110245846817));
#38211=CARTESIAN_POINT('Ctrl Pts',(73.4206854856395,15.4594130397602,-76.3185921935163));
#38212=CARTESIAN_POINT('Ctrl Pts',(73.4207187415443,16.1288080248881,-77.5711489603293));
#38213=CARTESIAN_POINT('Ctrl Pts',(73.4209844325267,17.0967453127965,-79.3917120641317));
#38214=CARTESIAN_POINT('Ctrl Pts',(73.4208688751132,17.534087889402,-80.2143709854359));
#38215=CARTESIAN_POINT('Ctrl Pts',(73.4208688751139,17.9706094767917,-81.035348687534));
#38216=CARTESIAN_POINT('Ctrl Pts',(76.2590036766147,4.61859585860129,24.8393189247761));
#38217=CARTESIAN_POINT('Ctrl Pts',(76.2592676270511,4.61842433362789,24.7907142376174));
#38218=CARTESIAN_POINT('Ctrl Pts',(76.259544344814,4.61824484467112,24.7421096031221));
#38219=CARTESIAN_POINT('Ctrl Pts',(76.2628175286996,4.61612267835582,24.1948928050072));
#38220=CARTESIAN_POINT('Ctrl Pts',(76.2639556688969,4.60859814771707,23.1986363586193));
#38221=CARTESIAN_POINT('Ctrl Pts',(76.2656134729886,4.5871973764053,21.1946693826308));
#38222=CARTESIAN_POINT('Ctrl Pts',(76.2875108300358,4.57291605684706,19.6882732104818));
#38223=CARTESIAN_POINT('Ctrl Pts',(76.3407769139473,4.57211738482582,18.4315980169902));
#38224=CARTESIAN_POINT('Ctrl Pts',(76.3647952026638,4.56784493819628,17.9582353768577));
#38225=CARTESIAN_POINT('Ctrl Pts',(76.4225707356139,4.54820045830769,16.9721940721953));
#38226=CARTESIAN_POINT('Ctrl Pts',(76.5461507315241,4.50383685775637,15.2086150331147));
#38227=CARTESIAN_POINT('Ctrl Pts',(76.6816328251804,4.51394742999633,13.604103234509));
#38228=CARTESIAN_POINT('Ctrl Pts',(76.7973134235421,4.64070067877184,12.2178313104145));
#38229=CARTESIAN_POINT('Ctrl Pts',(76.8482846182611,4.6959007062244,11.6963571978168));
#38230=CARTESIAN_POINT('Ctrl Pts',(76.9619010427407,4.83491465463365,10.6384381496348));
#38231=CARTESIAN_POINT('Ctrl Pts',(77.1773114937794,5.14739340279784,8.80323228594006));
#38232=CARTESIAN_POINT('Ctrl Pts',(77.3359786624805,5.52637920512046,7.2324101828848));
#38233=CARTESIAN_POINT('Ctrl Pts',(77.3978386221007,5.84607093393154,6.05183145962771));
#38234=CARTESIAN_POINT('Ctrl Pts',(77.4104440826745,5.92294208370831,5.77136055629867));
#38235=CARTESIAN_POINT('Ctrl Pts',(77.4347134233158,6.08613463998106,5.22885950434643));
#38236=CARTESIAN_POINT('Ctrl Pts',(77.471937172593,6.39735498949603,4.29054285111247));
#38237=CARTESIAN_POINT('Ctrl Pts',(77.5145027935911,7.0818025705993,2.48801682144282));
#38238=CARTESIAN_POINT('Ctrl Pts',(77.4910544212567,7.65143597159282,1.04581588660632));
#38239=CARTESIAN_POINT('Ctrl Pts',(77.4563839266263,7.93937104286881,0.0587093473684586));
#38240=CARTESIAN_POINT('Ctrl Pts',(77.4493287306598,7.97629022026226,-0.0741408717249266));
#38241=CARTESIAN_POINT('Ctrl Pts',(77.4352764439675,8.04762450080056,-0.330701574080755));
#38242=CARTESIAN_POINT('Ctrl Pts',(77.4064449579892,8.17091110776995,-0.78274962825136));
#38243=CARTESIAN_POINT('Ctrl Pts',(77.3563221876615,8.33976514909286,-1.42166202765295));
#38244=CARTESIAN_POINT('Ctrl Pts',(77.2826934866484,8.53037197855714,-2.18023274413119));
#38245=CARTESIAN_POINT('Ctrl Pts',(77.1698662581585,8.76522838164144,-3.17513501720164));
#38246=CARTESIAN_POINT('Ctrl Pts',(77.0078560361427,9.0165802652799,-4.38307638235827));
#38247=CARTESIAN_POINT('Ctrl Pts',(76.8810645642699,9.16472063733229,-5.3041822170234));
#38248=CARTESIAN_POINT('Ctrl Pts',(76.8143606679954,9.23977858033352,-5.86669711176399));
#38249=CARTESIAN_POINT('Ctrl Pts',(76.7876061568717,9.266926356809,-6.09824862163579));
#38250=CARTESIAN_POINT('Ctrl Pts',(76.7305215689549,9.31381517204141,-6.56031303999017));
#38251=CARTESIAN_POINT('Ctrl Pts',(76.623822642093,9.3779155277621,-7.37656498058418));
#38252=CARTESIAN_POINT('Ctrl Pts',(76.4588572052781,9.43436856860635,-8.55885909257655));
#38253=CARTESIAN_POINT('Ctrl Pts',(76.3083552744269,9.47478631504437,-9.77012444616046));
#38254=CARTESIAN_POINT('Ctrl Pts',(76.2268866003434,9.50274871976792,-10.6328070530146));
#38255=CARTESIAN_POINT('Ctrl Pts',(76.1889647647772,9.51944356435535,-11.1295119194356));
#38256=CARTESIAN_POINT('Ctrl Pts',(76.1732048820239,9.5282313628706,-11.3791645664889));
#38257=CARTESIAN_POINT('Ctrl Pts',(76.1626496791194,9.5350723706033,-11.5673286472237));
#38258=CARTESIAN_POINT('Ctrl Pts',(76.1561044817567,9.5389808438474,-11.6835147323112));
#38259=CARTESIAN_POINT('Ctrl Pts',(76.1449164746475,9.54587575628024,-11.9221801824993));
#38260=CARTESIAN_POINT('Ctrl Pts',(76.1301509865121,9.55494466884804,-12.3381363417809));
#38261=CARTESIAN_POINT('Ctrl Pts',(76.1141476656422,9.5648467015866,-13.4170088493667));
#38262=CARTESIAN_POINT('Ctrl Pts',(76.1462414682578,9.54491422434753,-14.6383040341395));
#38263=CARTESIAN_POINT('Ctrl Pts',(76.1814607883465,9.52362279337754,-15.894220196008));
#38264=CARTESIAN_POINT('Ctrl Pts',(76.1958833316405,9.51493334637066,-16.5310026710859));
#38265=CARTESIAN_POINT('Ctrl Pts',(76.2032117585579,9.51049495165966,-17.046382647654));
#38266=CARTESIAN_POINT('Ctrl Pts',(76.2050790182465,9.5093235528455,-17.3060970096061));
#38267=CARTESIAN_POINT('Ctrl Pts',(76.2056606273789,9.50892263229608,-17.5007250548875));
#38268=CARTESIAN_POINT('Ctrl Pts',(76.2060184706633,9.50867014132164,-17.6246100787378));
#38269=CARTESIAN_POINT('Ctrl Pts',(76.2066327169784,9.50821630284198,-17.8752336778117));
#38270=CARTESIAN_POINT('Ctrl Pts',(76.2070999316946,9.50783368567201,-18.1248775363383));
#38271=CARTESIAN_POINT('Ctrl Pts',(76.2074393459038,9.50751639611427,-18.3751636995251));
#38272=CARTESIAN_POINT('Ctrl Pts',(76.2076003451942,9.50734337631093,-18.5315010636906));
#38273=CARTESIAN_POINT('Ctrl Pts',(76.2077008744814,9.50721940852223,-18.6566402448602));
#38274=CARTESIAN_POINT('Ctrl Pts',(76.2077830451556,9.50710470991487,-18.781780794401));
#38275=CARTESIAN_POINT('Ctrl Pts',(76.2079349339152,9.50682601690064,-19.1259787582423));
#38276=CARTESIAN_POINT('Ctrl Pts',(76.2078128004655,9.50655792868122,-19.6895414673316));
#38277=CARTESIAN_POINT('Ctrl Pts',(76.2068697612793,9.50646427618187,-20.6924456477076));
#38278=CARTESIAN_POINT('Ctrl Pts',(76.2049543558568,9.50677808697286,-21.9482349694304));
#38279=CARTESIAN_POINT('Ctrl Pts',(76.203958537714,9.50690801497891,-22.9554528492817));
#38280=CARTESIAN_POINT('Ctrl Pts',(76.2039285981864,9.50677138616243,-23.5842091939704));
#38281=CARTESIAN_POINT('Ctrl Pts',(76.2039311347776,9.50671986233443,-23.8335357791018));
#38282=CARTESIAN_POINT('Ctrl Pts',(76.2039825343625,9.50662769705605,-24.3327384697341));
#38283=CARTESIAN_POINT('Ctrl Pts',(76.2041753964794,9.50649314315013,-25.2083158964201));
#38284=CARTESIAN_POINT('Ctrl Pts',(76.2046272231609,9.50637007241075,-26.4631392982103));
#38285=CARTESIAN_POINT('Ctrl Pts',(76.2050840179851,9.5063208851935,-27.9716989624441));
#38286=CARTESIAN_POINT('Ctrl Pts',(76.2050838163052,9.50634879469455,-28.9766009445786));
#38287=CARTESIAN_POINT('Ctrl Pts',(76.2049320907037,9.50638032028333,-29.5409277274078));
#38288=CARTESIAN_POINT('Ctrl Pts',(76.2048918219022,9.50638821118415,-29.666345751297));
#38289=CARTESIAN_POINT('Ctrl Pts',(76.2047860045326,9.50640681192304,-29.9172262835149));
#38290=CARTESIAN_POINT('Ctrl Pts',(76.2045395599007,9.50644670041097,-30.3563998095175));
#38291=CARTESIAN_POINT('Ctrl Pts',(76.2038416766349,9.50655408259969,-31.2351348597051));
#38292=CARTESIAN_POINT('Ctrl Pts',(76.2027578708194,9.50673109815979,-32.2397225010295));
#38293=CARTESIAN_POINT('Ctrl Pts',(76.2017524308679,9.50694563130845,-33.2434991114049));
#38294=CARTESIAN_POINT('Ctrl Pts',(76.2011285677281,9.50712068230683,-33.9956434809428));
#38295=CARTESIAN_POINT('Ctrl Pts',(76.2007252022021,9.5073048364333,-34.7467978244661));
#38296=CARTESIAN_POINT('Ctrl Pts',(76.2006640374012,9.50743052225041,-35.2467244669251));
#38297=CARTESIAN_POINT('Ctrl Pts',(76.2007189105449,9.50752525625275,-35.622276173328));
#38298=CARTESIAN_POINT('Ctrl Pts',(76.2007883358698,9.50757016226445,-35.8735687461266));
#38299=CARTESIAN_POINT('Ctrl Pts',(76.2010434311644,9.50760144195324,-36.3757362086335));
#38300=CARTESIAN_POINT('Ctrl Pts',(76.2017574405851,9.50753650552576,-37.2532213547367));
#38301=CARTESIAN_POINT('Ctrl Pts',(76.2039545767969,9.5072513251119,-39.0052620549296));
#38302=CARTESIAN_POINT('Ctrl Pts',(76.206126750897,9.50776410084192,-40.5084303125359));
#38303=CARTESIAN_POINT('Ctrl Pts',(76.2068674914565,9.50959494160429,-41.6419434750376));
#38304=CARTESIAN_POINT('Ctrl Pts',(76.2070026761808,9.50983789499437,-41.8898027095891));
#38305=CARTESIAN_POINT('Ctrl Pts',(76.2071320080402,9.50982784025946,-42.2638829212183));
#38306=CARTESIAN_POINT('Ctrl Pts',(76.2072014362706,9.50954136566926,-42.6384117975113));
#38307=CARTESIAN_POINT('Ctrl Pts',(76.2072316055659,9.50892484198801,-43.1391793194606));
#38308=CARTESIAN_POINT('Ctrl Pts',(76.2071851505408,9.50796609456154,-43.76700866489));
#38309=CARTESIAN_POINT('Ctrl Pts',(76.2070991026037,9.50732373313355,-44.5231165146298));
#38310=CARTESIAN_POINT('Ctrl Pts',(76.2070884073366,9.50789121619783,-45.1549708306134));
#38311=CARTESIAN_POINT('Ctrl Pts',(76.2071669746945,9.50942463486588,-45.6612586675138));
#38312=CARTESIAN_POINT('Ctrl Pts',(76.2072824929622,9.5112151213506,-46.0413301443371));
#38313=CARTESIAN_POINT('Ctrl Pts',(76.2074673026926,9.5137497869097,-46.4216716023164));
#38314=CARTESIAN_POINT('Ctrl Pts',(76.2078223026706,9.5182653104936,-46.9291383597721));
#38315=CARTESIAN_POINT('Ctrl Pts',(76.2082312789042,9.52307370849484,-47.3098632961747));
#38316=CARTESIAN_POINT('Ctrl Pts',(76.2087589593374,9.5290754095034,-47.6919903466628));
#38317=CARTESIAN_POINT('Ctrl Pts',(76.2090927997495,9.53481972517867,-47.9609551129328));
#38318=CARTESIAN_POINT('Ctrl Pts',(76.2098414512392,9.55111981400484,-48.4857460181741));
#38319=CARTESIAN_POINT('Ctrl Pts',(76.2113469227438,9.58993601670354,-49.3948129839473));
#38320=CARTESIAN_POINT('Ctrl Pts',(76.2142833548468,9.65909393983966,-50.65213186042));
#38321=CARTESIAN_POINT('Ctrl Pts',(76.2190264986818,9.71927591471838,-52.0992608602766));
#38322=CARTESIAN_POINT('Ctrl Pts',(76.2225088710447,9.7177154226995,-53.020066261725));
#38323=CARTESIAN_POINT('Ctrl Pts',(76.2244549931009,9.6966778945239,-53.581967440294));
#38324=CARTESIAN_POINT('Ctrl Pts',(76.225035007649,9.68541465582122,-53.7809575537511));
#38325=CARTESIAN_POINT('Ctrl Pts',(76.2262568620834,9.64795036230627,-54.2118872595482));
#38326=CARTESIAN_POINT('Ctrl Pts',(76.2288167885687,9.54783156701677,-54.9965732007058));
#38327=CARTESIAN_POINT('Ctrl Pts',(76.236898472628,9.25220174007932,-56.7180959689487));
#38328=CARTESIAN_POINT('Ctrl Pts',(76.2510991373395,8.9981673470454,-58.4309626675799));
#38329=CARTESIAN_POINT('Ctrl Pts',(76.2518790547583,9.07715845498505,-59.766985659836));
#38330=CARTESIAN_POINT('Ctrl Pts',(76.2520969510277,9.08668144561503,-59.9088314444499));
#38331=CARTESIAN_POINT('Ctrl Pts',(76.2523314530188,9.11031499731494,-60.2029068149855));
#38332=CARTESIAN_POINT('Ctrl Pts',(76.2525057894986,9.16146302212859,-60.7091605105868));
#38333=CARTESIAN_POINT('Ctrl Pts',(76.2518458409884,9.30202082941623,-61.7148952460834));
#38334=CARTESIAN_POINT('Ctrl Pts',(76.249520620965,9.53869253043827,-62.8349750285185));
#38335=CARTESIAN_POINT('Ctrl Pts',(76.2466748244391,9.83153217266925,-63.9271011416989));
#38336=CARTESIAN_POINT('Ctrl Pts',(76.245038643789,10.0138542845839,-64.5299573523145));
#38337=CARTESIAN_POINT('Ctrl Pts',(76.2439976050462,10.1413071595377,-64.9271036563846));
#38338=CARTESIAN_POINT('Ctrl Pts',(76.2433208040966,10.2277574522173,-65.190541278871));
#38339=CARTESIAN_POINT('Ctrl Pts',(76.2426712695385,10.3163232784996,-65.4521172547543));
#38340=CARTESIAN_POINT('Ctrl Pts',(76.2421416178469,10.3953940026921,-65.6791956689038));
#38341=CARTESIAN_POINT('Ctrl Pts',(76.2418510869757,10.4409955708514,-65.808446214391));
#38342=CARTESIAN_POINT('Ctrl Pts',(76.2414265822491,10.5098100504663,-66.0018379033021));
#38343=CARTESIAN_POINT('Ctrl Pts',(76.2411025706284,10.5679444806704,-66.1619021108702));
#38344=CARTESIAN_POINT('Ctrl Pts',(76.2405762973677,10.6653207116708,-66.4261395776643));
#38345=CARTESIAN_POINT('Ctrl Pts',(76.2382736295417,10.782650343015,-66.7305752420116));
#38346=CARTESIAN_POINT('Ctrl Pts',(76.2347476360257,11.0246466535472,-67.3072811653499));
#38347=CARTESIAN_POINT('Ctrl Pts',(76.2285480902281,11.4838012691017,-68.2955882384519));
#38348=CARTESIAN_POINT('Ctrl Pts',(76.2199518240085,12.4848160711236,-70.1535050170501));
#38349=CARTESIAN_POINT('Ctrl Pts',(76.2211301356414,13.3604371029294,-71.6137934767777));
#38350=CARTESIAN_POINT('Ctrl Pts',(76.2265603989672,13.9145144198684,-72.6661742339041));
#38351=CARTESIAN_POINT('Ctrl Pts',(76.2260852072361,14.0501736049526,-72.923856427483));
#38352=CARTESIAN_POINT('Ctrl Pts',(76.2261213973963,14.3150055295701,-73.4254306080582));
#38353=CARTESIAN_POINT('Ctrl Pts',(76.2258010288081,14.6495691638506,-74.0571731429503));
#38354=CARTESIAN_POINT('Ctrl Pts',(76.2256865732654,15.0502504868885,-74.8110671308814));
#38355=CARTESIAN_POINT('Ctrl Pts',(76.2254329300688,15.8533706308797,-76.3186350674606));
#38356=CARTESIAN_POINT('Ctrl Pts',(76.2254675779746,16.5227661783838,-77.571191652404));
#38357=CARTESIAN_POINT('Ctrl Pts',(76.2257326223979,17.4907030767103,-79.3917542575282));
#38358=CARTESIAN_POINT('Ctrl Pts',(76.2256174138935,17.9280458738864,-80.2144133394732));
#38359=CARTESIAN_POINT('Ctrl Pts',(76.2256174138933,18.3645674612764,-81.0353910415709));
#38360=CARTESIAN_POINT('Ctrl Pts',(78.1311761235466,4.88238476433655,24.8296314603199));
#38361=CARTESIAN_POINT('Ctrl Pts',(78.1317586768894,4.88248888926511,24.7807222995813));
#38362=CARTESIAN_POINT('Ctrl Pts',(78.1323693534611,4.882597812653,24.7317992420864));
#38363=CARTESIAN_POINT('Ctrl Pts',(78.1395699941658,4.88389574527485,24.1812167300954));
#38364=CARTESIAN_POINT('Ctrl Pts',(78.1492419926987,4.88177196689673,23.1890789328558));
#38365=CARTESIAN_POINT('Ctrl Pts',(78.1745360446089,4.87447704577674,21.1752495305265));
#38366=CARTESIAN_POINT('Ctrl Pts',(78.2220498596193,4.88324512237042,19.6543634732364));
#38367=CARTESIAN_POINT('Ctrl Pts',(78.301833748746,4.91934107595181,18.3802225175682));
#38368=CARTESIAN_POINT('Ctrl Pts',(78.3395068064966,4.93035400094775,17.9047187002429));
#38369=CARTESIAN_POINT('Ctrl Pts',(78.4321782336654,4.94791260069687,16.9119065524815));
#38370=CARTESIAN_POINT('Ctrl Pts',(78.6275650402547,4.98365588797779,15.1385193904962));
#38371=CARTESIAN_POINT('Ctrl Pts',(78.8098035271563,5.08984219840305,13.5202512022143));
#38372=CARTESIAN_POINT('Ctrl Pts',(78.9141079171548,5.30595926923579,12.1229955240602));
#38373=CARTESIAN_POINT('Ctrl Pts',(78.9585931964819,5.39913427657366,11.5903098623216));
#38374=CARTESIAN_POINT('Ctrl Pts',(79.0492236844176,5.62075197894407,10.5216533462124));
#38375=CARTESIAN_POINT('Ctrl Pts',(79.2018289295449,6.08316796559141,8.68166927386263));
#38376=CARTESIAN_POINT('Ctrl Pts',(79.2830187397639,6.5635051146988,7.13011330676721));
#38377=CARTESIAN_POINT('Ctrl Pts',(79.2878543220827,6.92316409732294,5.96944852000437));
#38378=CARTESIAN_POINT('Ctrl Pts',(79.2829833844745,7.01389849089022,5.68124415713134));
#38379=CARTESIAN_POINT('Ctrl Pts',(79.271246982088,7.20055849904512,5.13353023311153));
#38380=CARTESIAN_POINT('Ctrl Pts',(79.2395720183877,7.54899306029872,4.18865645472214));
#38381=CARTESIAN_POINT('Ctrl Pts',(79.1505282295557,8.27794976463893,2.39178159898726));
#38382=CARTESIAN_POINT('Ctrl Pts',(79.0707071874785,8.82468205108704,0.980148004169901));
#38383=CARTESIAN_POINT('Ctrl Pts',(79.0228181033673,9.05591605411342,0.0730197621118544));
#38384=CARTESIAN_POINT('Ctrl Pts',(79.0149188641117,9.08588408324921,-0.0495289334430407));
#38385=CARTESIAN_POINT('Ctrl Pts',(78.9990824940997,9.14173887775737,-0.286403972854207));
#38386=CARTESIAN_POINT('Ctrl Pts',(78.9680075267001,9.23421719715553,-0.704916603339056));
#38387=CARTESIAN_POINT('Ctrl Pts',(78.9167265681545,9.34909292918604,-1.29979766176164));
#38388=CARTESIAN_POINT('Ctrl Pts',(78.8452750379769,9.46363926693925,-2.01421891223975));
#38389=CARTESIAN_POINT('Ctrl Pts',(78.7408109727822,9.5901340366282,-2.96551438085703));
#38390=CARTESIAN_POINT('Ctrl Pts',(78.5987776215388,9.70979928799303,-4.1543523026218));
#38391=CARTESIAN_POINT('Ctrl Pts',(78.4950284590842,9.78175363508764,-5.10676467868206));
#38392=CARTESIAN_POINT('Ctrl Pts',(78.4416364854941,9.82093138357967,-5.70314228973472));
#38393=CARTESIAN_POINT('Ctrl Pts',(78.4207377850043,9.83260536946596,-5.92375439756827));
#38394=CARTESIAN_POINT('Ctrl Pts',(78.3787158818719,9.84940713990351,-6.38078537880414));
#38395=CARTESIAN_POINT('Ctrl Pts',(78.3063526725102,9.86034267366957,-7.18824108477744));
#38396=CARTESIAN_POINT('Ctrl Pts',(78.2100666718561,9.83680804858785,-8.38360326993399));
#38397=CARTESIAN_POINT('Ctrl Pts',(78.1312684243954,9.79254145045081,-9.62622229216998));
#38398=CARTESIAN_POINT('Ctrl Pts',(78.0885073456006,9.77017076955802,-10.5210983738634));
#38399=CARTESIAN_POINT('Ctrl Pts',(78.0681938151062,9.76286330053317,-11.0392012330339));
#38400=CARTESIAN_POINT('Ctrl Pts',(78.0594902883523,9.76154296606314,-11.3006543404583));
#38401=CARTESIAN_POINT('Ctrl Pts',(78.053513304347,9.76161940798103,-11.4981603609995));
#38402=CARTESIAN_POINT('Ctrl Pts',(78.0498055521674,9.76166010227368,-11.6217338577917));
#38403=CARTESIAN_POINT('Ctrl Pts',(78.0435526389846,9.76183362725649,-11.8737777491659));
#38404=CARTESIAN_POINT('Ctrl Pts',(78.0355232386197,9.76230013096662,-12.3116981948741));
#38405=CARTESIAN_POINT('Ctrl Pts',(78.0282957738844,9.76406912607226,-13.4375530291881));
#38406=CARTESIAN_POINT('Ctrl Pts',(78.0502925386483,9.76693574462966,-14.6828678286821));
#38407=CARTESIAN_POINT('Ctrl Pts',(78.0734323284533,9.76987699356143,-15.933933680242));
#38408=CARTESIAN_POINT('Ctrl Pts',(78.0829751157319,9.77115884436228,-16.561181415999));
#38409=CARTESIAN_POINT('Ctrl Pts',(78.0879251613887,9.77194777263734,-17.064707833481));
#38410=CARTESIAN_POINT('Ctrl Pts',(78.0892795292674,9.77223839921884,-17.3170551029141));
#38411=CARTESIAN_POINT('Ctrl Pts',(78.0897794549923,9.77240971775399,-17.5057890593336));
#38412=CARTESIAN_POINT('Ctrl Pts',(78.0900864923832,9.77251557331494,-17.6302578920605));
#38413=CARTESIAN_POINT('Ctrl Pts',(78.0906091998735,9.77270182264529,-17.879482666526));
#38414=CARTESIAN_POINT('Ctrl Pts',(78.0910077930249,9.77285050784834,-18.1287582169543));
#38415=CARTESIAN_POINT('Ctrl Pts',(78.0912880502502,9.77296669339788,-18.3782285630347));
#38416=CARTESIAN_POINT('Ctrl Pts',(78.0914191479227,9.77302624074914,-18.5341964086388));
#38417=CARTESIAN_POINT('Ctrl Pts',(78.0914982961441,9.77306666014432,-18.6590126540799));
#38418=CARTESIAN_POINT('Ctrl Pts',(78.0915611860204,9.77310237578932,-18.7838528243454));
#38419=CARTESIAN_POINT('Ctrl Pts',(78.0916718013574,9.77318167950402,-19.1272582336073));
#38420=CARTESIAN_POINT('Ctrl Pts',(78.0915282776836,9.77321629682544,-19.6897562128712));
#38421=CARTESIAN_POINT('Ctrl Pts',(78.09065113725,9.77308984641989,-20.6914136827282));
#38422=CARTESIAN_POINT('Ctrl Pts',(78.0889245135217,9.77273623121217,-21.946838300024));
#38423=CARTESIAN_POINT('Ctrl Pts',(78.0880606587,9.77256333897646,-22.9550490867659));
#38424=CARTESIAN_POINT('Ctrl Pts',(78.08803696042,9.77258874259918,-23.5847732614642));
#38425=CARTESIAN_POINT('Ctrl Pts',(78.0880381835476,9.77260043014001,-23.8339776845296));
#38426=CARTESIAN_POINT('Ctrl Pts',(78.0880823882946,9.77262844554538,-24.3332132054465));
#38427=CARTESIAN_POINT('Ctrl Pts',(78.0882514781816,9.772687450661,-25.2086880038889));
#38428=CARTESIAN_POINT('Ctrl Pts',(78.0886614183903,9.77278519551231,-26.4634120692526));
#38429=CARTESIAN_POINT('Ctrl Pts',(78.0891046021519,9.77287286052947,-27.9717324597234));
#38430=CARTESIAN_POINT('Ctrl Pts',(78.0891672773944,9.77287455436938,-28.9764534780923));
#38431=CARTESIAN_POINT('Ctrl Pts',(78.0890753000005,9.77284962231787,-29.5406571996044));
#38432=CARTESIAN_POINT('Ctrl Pts',(78.0890494952249,9.77284294733562,-29.6660260402146));
#38433=CARTESIAN_POINT('Ctrl Pts',(78.0889791775516,9.77282553595872,-29.916825989271));
#38434=CARTESIAN_POINT('Ctrl Pts',(78.0888106525499,9.77278499385702,-30.3558649020516));
#38435=CARTESIAN_POINT('Ctrl Pts',(78.0883206261467,9.77266964692748,-31.2343866557592));
#38436=CARTESIAN_POINT('Ctrl Pts',(78.0875455572616,9.77248571113029,-32.2388424815497));
#38437=CARTESIAN_POINT('Ctrl Pts',(78.0868239127496,9.77230330533085,-33.2426017642358));
#38438=CARTESIAN_POINT('Ctrl Pts',(78.0863765096049,9.77218063491253,-33.994789260345));
#38439=CARTESIAN_POINT('Ctrl Pts',(78.0860914339031,9.7720852698536,-34.7460434515072));
#38440=CARTESIAN_POINT('Ctrl Pts',(78.0860541719157,9.77204885607964,-35.2460753752379));
#38441=CARTESIAN_POINT('Ctrl Pts',(78.0861004458006,9.7720352564668,-35.6217189501983));
#38442=CARTESIAN_POINT('Ctrl Pts',(78.0861554677218,9.77200747680218,-35.8730072441829));
#38443=CARTESIAN_POINT('Ctrl Pts',(78.0863508169533,9.77189287874838,-36.3752036603097));
#38444=CARTESIAN_POINT('Ctrl Pts',(78.0868897252747,9.77157429449981,-37.2527215600665));
#38445=CARTESIAN_POINT('Ctrl Pts',(78.0885304025336,9.77079517197216,-39.0048450922735));
#38446=CARTESIAN_POINT('Ctrl Pts',(78.0901443779921,9.77095535125212,-40.5080843724291));
#38447=CARTESIAN_POINT('Ctrl Pts',(78.0906943772335,9.77259474850997,-41.6416550706781));
#38448=CARTESIAN_POINT('Ctrl Pts',(78.090794629494,9.77279711194888,-41.8895200839283));
#38449=CARTESIAN_POINT('Ctrl Pts',(78.0908902742295,9.77273077332194,-42.2636138715192));
#38450=CARTESIAN_POINT('Ctrl Pts',(78.0909412497351,9.77239247733141,-42.6381564279869));
#38451=CARTESIAN_POINT('Ctrl Pts',(78.0909626971188,9.77171259311439,-43.1389447144232));
#38452=CARTESIAN_POINT('Ctrl Pts',(78.090926616524,9.77068487605055,-43.7668031830724));
#38453=CARTESIAN_POINT('Ctrl Pts',(78.0908600921664,9.7699747402942,-44.522951737293));
#38454=CARTESIAN_POINT('Ctrl Pts',(78.0908490780117,9.77049711716599,-45.1548446218977));
#38455=CARTESIAN_POINT('Ctrl Pts',(78.0909037548587,9.77200020186817,-45.6611662031078));
#38456=CARTESIAN_POINT('Ctrl Pts',(78.0909862434953,9.77377082767171,-46.0412644505658));
#38457=CARTESIAN_POINT('Ctrl Pts',(78.09111952065,9.7762883158246,-46.4216341543253));
#38458=CARTESIAN_POINT('Ctrl Pts',(78.0913765780375,9.78078426265377,-46.9291405658452));
#38459=CARTESIAN_POINT('Ctrl Pts',(78.091674312547,9.78558158784181,-47.3098975341711));
#38460=CARTESIAN_POINT('Ctrl Pts',(78.0920582451879,9.79157417936065,-47.6920584907085));
#38461=CARTESIAN_POINT('Ctrl Pts',(78.092290121104,9.79731540407121,-47.9610555008819));
#38462=CARTESIAN_POINT('Ctrl Pts',(78.0928133460247,9.81361748257627,-48.4858996199633));
#38463=CARTESIAN_POINT('Ctrl Pts',(78.0938693960702,9.85245632736365,-49.3950492918544));
#38464=CARTESIAN_POINT('Ctrl Pts',(78.0960164804529,9.92168060508791,-50.6524468435612));
#38465=CARTESIAN_POINT('Ctrl Pts',(78.0996044526606,9.98194540832576,-52.0996111866457));
#38466=CARTESIAN_POINT('Ctrl Pts',(78.1021962417671,9.98041336536394,-53.0203964617832));
#38467=CARTESIAN_POINT('Ctrl Pts',(78.1035520022358,9.95937927344506,-53.5822721134691));
#38468=CARTESIAN_POINT('Ctrl Pts',(78.1038786353797,9.94811087479182,-53.7812906420223));
#38469=CARTESIAN_POINT('Ctrl Pts',(78.1045393796479,9.91063979260362,-54.2122457592885));
#38470=CARTESIAN_POINT('Ctrl Pts',(78.1059983986141,9.8105113177491,-54.9969674004099));
#38471=CARTESIAN_POINT('Ctrl Pts',(78.1115855487694,9.51488504017041,-56.7184898330074));
#38472=CARTESIAN_POINT('Ctrl Pts',(78.1237628749783,9.26090774064384,-58.4312662472414));
#38473=CARTESIAN_POINT('Ctrl Pts',(78.1237572022669,9.33988962176433,-59.7671397048542));
#38474=CARTESIAN_POINT('Ctrl Pts',(78.1238834968223,9.34940945215823,-59.9089694517362));
#38475=CARTESIAN_POINT('Ctrl Pts',(78.123948344431,9.37303563774044,-60.2030134627939));
#38476=CARTESIAN_POINT('Ctrl Pts',(78.123860278138,9.42416576273053,-60.7092172719043));
#38477=CARTESIAN_POINT('Ctrl Pts',(78.1228007482891,9.56467332005635,-61.7148702192895));
#38478=CARTESIAN_POINT('Ctrl Pts',(78.1202486506339,9.80126886303687,-62.8348983695161));
#38479=CARTESIAN_POINT('Ctrl Pts',(78.1172932387441,10.0940390606951,-63.9270100415927));
#38480=CARTESIAN_POINT('Ctrl Pts',(78.1156185224597,10.2763282371946,-64.529871145115));
#38481=CARTESIAN_POINT('Ctrl Pts',(78.1145527478538,10.4037632125647,-64.9270258697791));
#38482=CARTESIAN_POINT('Ctrl Pts',(78.113859133745,10.4902027451492,-65.1904704743225));
#38483=CARTESIAN_POINT('Ctrl Pts',(78.113191450897,10.5787596618105,-65.4520554270822));
#38484=CARTESIAN_POINT('Ctrl Pts',(78.112643225262,10.6578244912705,-65.6791434672428));
#38485=CARTESIAN_POINT('Ctrl Pts',(78.1123410970943,10.7034232613404,-65.8084000171421));
#38486=CARTESIAN_POINT('Ctrl Pts',(78.1118981045971,10.7722341252842,-66.0018011992152));
#38487=CARTESIAN_POINT('Ctrl Pts',(78.1115561931355,10.8303667975822,-66.1618743965424));
#38488=CARTESIAN_POINT('Ctrl Pts',(78.1109957852442,10.9277418190334,-66.4261277666418));
#38489=CARTESIAN_POINT('Ctrl Pts',(78.1086625472797,11.0450636807174,-66.7305607189423));
#38490=CARTESIAN_POINT('Ctrl Pts',(78.105090688148,11.2870515878708,-67.3072716108154));
#38491=CARTESIAN_POINT('Ctrl Pts',(78.098847683009,11.7461962687019,-68.2955809242267));
#38492=CARTESIAN_POINT('Ctrl Pts',(78.0902779682787,12.747213949018,-70.1535034158577));
#38493=CARTESIAN_POINT('Ctrl Pts',(78.0915595497525,13.6228501821446,-71.6137900374506));
#38494=CARTESIAN_POINT('Ctrl Pts',(78.0969916965239,14.1769255672346,-72.6661684683484));
#38495=CARTESIAN_POINT('Ctrl Pts',(78.0965163028863,14.3125846847232,-72.9238511157893));
#38496=CARTESIAN_POINT('Ctrl Pts',(78.096552461901,14.5774164020563,-73.4254256093465));
#38497=CARTESIAN_POINT('Ctrl Pts',(78.0962319470329,14.9119800013117,-74.0571686214722));
#38498=CARTESIAN_POINT('Ctrl Pts',(78.0961174294113,15.3126614747988,-74.8110629716249));
#38499=CARTESIAN_POINT('Ctrl Pts',(78.0958636910111,16.1157821891972,-76.3186314299804));
#38500=CARTESIAN_POINT('Ctrl Pts',(78.0958984464845,16.7851782478249,-77.5711876351949));
#38501=CARTESIAN_POINT('Ctrl Pts',(78.0961636612281,17.7531146699538,-79.3917492952804));
#38502=CARTESIAN_POINT('Ctrl Pts',(78.0960484086298,18.1904575551487,-80.2144085738345));
#38503=CARTESIAN_POINT('Ctrl Pts',(78.0960484086287,18.6269791425379,-81.035386275933));
#38504=CARTESIAN_POINT('Ctrl Pts',(79.0674174572816,5.01522268798702,24.8190563697355));
#38505=CARTESIAN_POINT('Ctrl Pts',(79.0681671244069,5.01561130574058,24.7698112483116));
#38506=CARTESIAN_POINT('Ctrl Pts',(79.0689526523201,5.01601890898661,24.7205402199319));
#38507=CARTESIAN_POINT('Ctrl Pts',(79.0782204295203,5.02082369775688,24.1661600490855));
#38508=CARTESIAN_POINT('Ctrl Pts',(79.0927100922061,5.02499971059091,23.1752017953721));
#38509=CARTESIAN_POINT('Ctrl Pts',(79.13103764065,5.03563871650282,21.1518987462585));
#38510=CARTESIAN_POINT('Ctrl Pts',(79.1918013249263,5.06857469890096,19.6199983452087));
#38511=CARTESIAN_POINT('Ctrl Pts',(79.2833409011377,5.13810232036442,18.3332047185655));
#38512=CARTESIAN_POINT('Ctrl Pts',(79.3271982411792,5.16402176082393,17.84951198812));
#38513=CARTESIAN_POINT('Ctrl Pts',(79.4350318672687,5.21929330547081,16.8471016897774));
#38514=CARTESIAN_POINT('Ctrl Pts',(79.6597738786907,5.3369308565268,15.0668569726542));
#38515=CARTESIAN_POINT('Ctrl Pts',(79.8528846773185,5.52342816880157,13.4624411336813));
#38516=CARTESIAN_POINT('Ctrl Pts',(79.9478662062515,5.77956862039127,12.0840553932277));
#38517=CARTESIAN_POINT('Ctrl Pts',(79.9872497031577,5.88971864287113,11.549661093268));
#38518=CARTESIAN_POINT('Ctrl Pts',(80.0644577893544,6.14288461106471,10.4849494612428));
#38519=CARTESIAN_POINT('Ctrl Pts',(80.1868739514183,6.65297453317945,8.65255246253285));
#38520=CARTESIAN_POINT('Ctrl Pts',(80.2380434661674,7.1519521376352,7.11347354620467));
#38521=CARTESIAN_POINT('Ctrl Pts',(80.220439279543,7.50474250480026,5.96584701383932));
#38522=CARTESIAN_POINT('Ctrl Pts',(80.2096598301317,7.59336202603015,5.67864593662744));
#38523=CARTESIAN_POINT('Ctrl Pts',(80.1847388141545,7.77373997953912,5.13331455420261));
#38524=CARTESIAN_POINT('Ctrl Pts',(80.1261981063281,8.10627260965177,4.19103989716421));
#38525=CARTESIAN_POINT('Ctrl Pts',(79.9741025993112,8.78915160892049,2.3987733150821));
#38526=CARTESIAN_POINT('Ctrl Pts',(79.8394769089903,9.27574069900803,0.998413564670721));
#38527=CARTESIAN_POINT('Ctrl Pts',(79.776274034096,9.47255577832048,0.106471274813789));
#38528=CARTESIAN_POINT('Ctrl Pts',(79.767194457764,9.49782300197105,-0.0121282343591863));
#38529=CARTESIAN_POINT('Ctrl Pts',(79.7492041230658,9.54449995459902,-0.242617772173818));
#38530=CARTESIAN_POINT('Ctrl Pts',(79.7157700463245,9.62061451730498,-0.650089440549976));
#38531=CARTESIAN_POINT('Ctrl Pts',(79.6641794164148,9.71223552902357,-1.23187976654897));
#38532=CARTESIAN_POINT('Ctrl Pts',(79.5969640703358,9.79990367294021,-1.93470248939131));
#38533=CARTESIAN_POINT('Ctrl Pts',(79.5029917261061,9.89209665672663,-2.87653843532152));
#38534=CARTESIAN_POINT('Ctrl Pts',(79.3825599458077,9.97162214304041,-4.06583657236809));
#38535=CARTESIAN_POINT('Ctrl Pts',(79.2987270860321,10.0151794261321,-5.0329814941378));
#38536=CARTESIAN_POINT('Ctrl Pts',(79.2557147461728,10.0403137244337,-5.64265294304191));
#38537=CARTESIAN_POINT('Ctrl Pts',(79.2392553093125,10.0469381856339,-5.86265292508084));
#38538=CARTESIAN_POINT('Ctrl Pts',(79.2076266893868,10.0536784745051,-6.32229191317324));
#38539=CARTESIAN_POINT('Ctrl Pts',(79.1564991190038,10.0477999042845,-7.13344037568369));
#38540=CARTESIAN_POINT('Ctrl Pts',(79.095707653065,10.0015426863692,-8.3366524324552));
#38541=CARTESIAN_POINT('Ctrl Pts',(79.0509098119789,9.93743938884988,-9.58843116417154));
#38542=CARTESIAN_POINT('Ctrl Pts',(79.0268821972649,9.90337508252064,-10.4912278027067));
#38543=CARTESIAN_POINT('Ctrl Pts',(79.0150755982232,9.89016064836555,-11.0141123219708));
#38544=CARTESIAN_POINT('Ctrl Pts',(79.0097798694179,9.88618613227508,-11.2780557604261));
#38545=CARTESIAN_POINT('Ctrl Pts',(79.0060078185597,9.88439984881659,-11.4774995193815));
#38546=CARTESIAN_POINT('Ctrl Pts',(79.0036646128689,9.88335806765953,-11.603394679048));
#38547=CARTESIAN_POINT('Ctrl Pts',(78.9997403997698,9.8816487714516,-11.8592855259742));
#38548=CARTESIAN_POINT('Ctrl Pts',(78.994761626747,9.87966497487754,-12.3037147241161));
#38549=CARTESIAN_POINT('Ctrl Pts',(78.9906389493915,9.87901407437311,-13.4432992897924));
#38550=CARTESIAN_POINT('Ctrl Pts',(79.0055392688548,9.88809053067284,-14.6957989256028));
#38551=CARTESIAN_POINT('Ctrl Pts',(79.0211129616261,9.89743196753811,-15.9454740289875));
#38552=CARTESIAN_POINT('Ctrl Pts',(79.0275063270077,9.90133064832979,-16.5699512103482));
#38553=CARTESIAN_POINT('Ctrl Pts',(79.0308470126228,9.90348293817318,-17.0700172850903));
#38554=CARTESIAN_POINT('Ctrl Pts',(79.0317705160842,9.90415023660917,-17.3202164927592));
#38555=CARTESIAN_POINT('Ctrl Pts',(79.0321228819547,9.90446515454591,-17.5072310492657));
#38556=CARTESIAN_POINT('Ctrl Pts',(79.032337739374,9.90466298605188,-17.6318736294089));
#38557=CARTESIAN_POINT('Ctrl Pts',(79.0326993816342,9.90501330195036,-17.8806948601256));
#38558=CARTESIAN_POINT('Ctrl Pts',(79.0329642770318,9.90529960964907,-18.1298687430497));
#38559=CARTESIAN_POINT('Ctrl Pts',(79.0331427080346,9.90552884765909,-18.3791056551831));
#38560=CARTESIAN_POINT('Ctrl Pts',(79.0332205008359,9.9056495194714,-18.5349686115737));
#38561=CARTESIAN_POINT('Ctrl Pts',(79.033263780692,9.90573338983648,-18.6596927967284));
#38562=CARTESIAN_POINT('Ctrl Pts',(79.0332948783198,9.90580906228168,-18.7844474542172));
#38563=CARTESIAN_POINT('Ctrl Pts',(79.0333320742632,9.90598416472866,-19.1276271552783));
#38564=CARTESIAN_POINT('Ctrl Pts',(79.0331487356763,9.90610415692518,-19.6898219896876));
#38565=CARTESIAN_POINT('Ctrl Pts',(79.0323543044741,9.90598184028357,-20.691124554094));
#38566=CARTESIAN_POINT('Ctrl Pts',(79.0309053714312,9.90546300842679,-21.946441629422));
#38567=CARTESIAN_POINT('Ctrl Pts',(79.0301633435523,9.90521302908391,-22.9549301710126));
#38568=CARTESIAN_POINT('Ctrl Pts',(79.0301115641125,9.90528387188766,-23.5849311300825));
#38569=CARTESIAN_POINT('Ctrl Pts',(79.0301019745384,9.90531313413815,-23.8340998784275));
#38570=CARTESIAN_POINT('Ctrl Pts',(79.0301210191317,9.90537475774982,-24.33334418637));
#38571=CARTESIAN_POINT('Ctrl Pts',(79.0302400236347,9.90548755710516,-25.2087899692583));
#38572=CARTESIAN_POINT('Ctrl Pts',(79.0305714553795,9.90564282039012,-26.4634885417697));
#38573=CARTESIAN_POINT('Ctrl Pts',(79.030959298768,9.9057612371249,-27.9717423758669));
#38574=CARTESIAN_POINT('Ctrl Pts',(79.0310334197768,9.90575228243049,-28.9764101349445));
#38575=CARTESIAN_POINT('Ctrl Pts',(79.0309728668496,9.90571199706992,-29.5405779896386));
#38576=CARTESIAN_POINT('Ctrl Pts',(79.0309554746975,9.90570156829581,-29.6659328551748));
#38577=CARTESIAN_POINT('Ctrl Pts',(79.0309061139083,9.9056748904435,-29.9167097801928));
#38578=CARTESIAN_POINT('Ctrl Pts',(79.0307843866883,9.90561375846606,-30.3557101966999));
#38579=CARTESIAN_POINT('Ctrl Pts',(79.0304226216911,9.90544194556123,-31.2341706187796));
#38580=CARTESIAN_POINT('Ctrl Pts',(79.0298448496468,9.90516647822444,-32.2385881454819));
#38581=CARTESIAN_POINT('Ctrl Pts',(79.0293143868082,9.9048833276159,-33.2423420552038));
#38582=CARTESIAN_POINT('Ctrl Pts',(79.0289931241137,9.90468470258017,-33.9945417556105));
#38583=CARTESIAN_POINT('Ctrl Pts',(79.0288015672039,9.9045163686194,-34.7458244523766));
#38584=CARTESIAN_POINT('Ctrl Pts',(79.0287955792199,9.90443623244035,-35.2458865329308));
#38585=CARTESIAN_POINT('Ctrl Pts',(79.0288500605975,9.90439277023724,-35.621556387038));
#38586=CARTESIAN_POINT('Ctrl Pts',(79.0289061929832,9.90434466294553,-35.8728434775819));
#38587=CARTESIAN_POINT('Ctrl Pts',(79.0290881140862,9.90418857142105,-36.3750481798328));
#38588=CARTESIAN_POINT('Ctrl Pts',(79.0295670331225,9.90379457777519,-37.2525756951283));
#38589=CARTESIAN_POINT('Ctrl Pts',(79.030981405081,9.90286410656558,-39.004723044727));
#38590=CARTESIAN_POINT('Ctrl Pts',(79.0323520207929,9.90290731861339,-40.5079837794954));
#38591=CARTESIAN_POINT('Ctrl Pts',(79.032828231492,9.90448791210333,-41.6415712959431));
#38592=CARTESIAN_POINT('Ctrl Pts',(79.0329157952561,9.90467835555726,-41.889438042092));
#38593=CARTESIAN_POINT('Ctrl Pts',(79.0330014944524,9.90459583103868,-42.2635358201197));
#38594=CARTESIAN_POINT('Ctrl Pts',(79.033049886041,9.90424312054807,-42.6380823835159));
#38595=CARTESIAN_POINT('Ctrl Pts',(79.0330754060422,9.903546008436,-43.1388767358232));
#38596=CARTESIAN_POINT('Ctrl Pts',(79.0330542033092,9.90250021442703,-43.7667436590274));
#38597=CARTESIAN_POINT('Ctrl Pts',(79.0330074024399,9.90177258117173,-44.5229039801225));
#38598=CARTESIAN_POINT('Ctrl Pts',(79.0330028838391,9.90228279501689,-45.1548080060181));
#38599=CARTESIAN_POINT('Ctrl Pts',(79.0330499122594,9.90377720905201,-45.661139141396));
#38600=CARTESIAN_POINT('Ctrl Pts',(79.0331185088012,9.90554159635451,-46.0412449734253));
#38601=CARTESIAN_POINT('Ctrl Pts',(79.0332280130535,9.90805298035099,-46.4216226721918));
#38602=CARTESIAN_POINT('Ctrl Pts',(79.0334379143621,9.91254077080098,-46.9291402370918));
#38603=CARTESIAN_POINT('Ctrl Pts',(79.0336802549664,9.91733169902102,-47.3099063411047));
#38604=CARTESIAN_POINT('Ctrl Pts',(79.0339918692555,9.92331741644185,-47.6920768194761));
#38605=CARTESIAN_POINT('Ctrl Pts',(79.0341721220784,9.92905466802767,-47.9610826352538));
#38606=CARTESIAN_POINT('Ctrl Pts',(79.0345801987364,9.94535040630575,-48.4859414577754));
#38607=CARTESIAN_POINT('Ctrl Pts',(79.0354045483133,9.98418152818373,-49.3951141830985));
#38608=CARTESIAN_POINT('Ctrl Pts',(79.0371404675913,10.0534000779738,-50.6525346834891));
#38609=CARTESIAN_POINT('Ctrl Pts',(79.0401258992488,10.1136512244723,-52.0997107596071));
#38610=CARTESIAN_POINT('Ctrl Pts',(79.0422538093688,10.1120991412615,-53.0204920363285));
#38611=CARTESIAN_POINT('Ctrl Pts',(79.0433031166023,10.0910468013029,-53.5823614482346));
#38612=CARTESIAN_POINT('Ctrl Pts',(79.0434978739722,10.079768538197,-53.7813889810288));
#38613=CARTESIAN_POINT('Ctrl Pts',(79.0438666169688,10.0422768550406,-54.2123523928334));
#38614=CARTESIAN_POINT('Ctrl Pts',(79.0447526255036,9.94210926415323,-54.9970852213269));
#38615=CARTESIAN_POINT('Ctrl Pts',(79.0490442932728,9.64640230422955,-56.7186062684982));
#38616=CARTESIAN_POINT('Ctrl Pts',(79.0601752091258,9.39237855590308,-58.4313538317651));
#38617=CARTESIAN_POINT('Ctrl Pts',(79.059765077974,9.47133310933444,-59.7671833796691));
#38618=CARTESIAN_POINT('Ctrl Pts',(79.059844272936,9.48084906648494,-59.9090085147957));
#38619=CARTESIAN_POINT('Ctrl Pts',(79.0598220382771,9.50446771414443,-60.2030434561234));
#38620=CARTESIAN_POINT('Ctrl Pts',(79.0595996895095,9.55558442298195,-60.7092328461023));
#38621=CARTESIAN_POINT('Ctrl Pts',(79.0583373808453,9.69606534726421,-61.714862060537));
#38622=CARTESIAN_POINT('Ctrl Pts',(79.0556740185159,9.9326329152352,-62.8348748135544));
#38623=CARTESIAN_POINT('Ctrl Pts',(79.0526682675542,10.2253806864803,-63.9269816045994));
#38624=CARTESIAN_POINT('Ctrl Pts',(79.0509770368797,10.4076596115538,-64.5298437088795));
#38625=CARTESIAN_POINT('Ctrl Pts',(79.0499005595451,10.535088907577,-64.9270005875088));
#38626=CARTESIAN_POINT('Ctrl Pts',(79.0491995939402,10.6215249556936,-65.1904470301732));
#38627=CARTESIAN_POINT('Ctrl Pts',(79.0485237590337,10.7100788792758,-65.452034393878));
#38628=CARTESIAN_POINT('Ctrl Pts',(79.0479669167474,10.7891415145841,-65.6791250682007));
#38629=CARTESIAN_POINT('Ctrl Pts',(79.0476593247898,10.834739158003,-65.8083832713257));
#38630=CARTESIAN_POINT('Ctrl Pts',(79.0472075401805,10.9035484565487,-66.001787077094));
#38631=CARTESIAN_POINT('Ctrl Pts',(79.0468569356967,10.9616801042072,-66.1618627777127));
#38632=CARTESIAN_POINT('Ctrl Pts',(79.0462796991508,11.0590537418934,-66.4261205988185));
#38633=CARTESIAN_POINT('Ctrl Pts',(79.0439307937972,11.1763722519809,-66.7305525790236));
#38634=CARTESIAN_POINT('Ctrl Pts',(79.0403355509136,11.4183560689343,-67.3072646265125));
#38635=CARTESIAN_POINT('Ctrl Pts',(79.0340698029988,11.8774960798622,-68.2955742231883));
#38636=CARTESIAN_POINT('Ctrl Pts',(79.0255118814883,12.8785147036822,-70.1534980894638));
#38637=CARTESIAN_POINT('Ctrl Pts',(79.0268453569621,13.7541586521472,-71.6137842112993));
#38638=CARTESIAN_POINT('Ctrl Pts',(79.0322798354967,14.3082341286308,-72.6661621416571));
#38639=CARTESIAN_POINT('Ctrl Pts',(79.0318042672112,14.4438931804177,-72.923844899657));
#38640=CARTESIAN_POINT('Ctrl Pts',(79.0318404699244,14.7087248514462,-73.4254194789814));
#38641=CARTESIAN_POINT('Ctrl Pts',(79.0315198355751,15.043288421734,-74.0571626126466));
#38642=CARTESIAN_POINT('Ctrl Pts',(79.0314052642792,15.4439699314055,-74.8110570612082));
#38643=CARTESIAN_POINT('Ctrl Pts',(79.0311513756816,16.2470907856448,-76.3186256622214));
#38644=CARTESIAN_POINT('Ctrl Pts',(79.031186060788,16.9164870242636,-77.5711817648655));
#38645=CARTESIAN_POINT('Ctrl Pts',(79.0314513893355,17.8844233649719,-79.3917431632681));
#38646=CARTESIAN_POINT('Ctrl Pts',(79.0313360800254,18.3217662758759,-80.2144024928222));
#38647=CARTESIAN_POINT('Ctrl Pts',(79.0313360800244,18.7582878632648,-81.0353801949212));
#38648=CARTESIAN_POINT('',(6.0874749758614E-15,-1.93207323326078,-8.62957429809281));
#38649=CARTESIAN_POINT('',(-11.7470010949101,-1.24897189262896,-5.16040757324739));
#38650=CARTESIAN_POINT('Ctrl Pts',(6.41902973990636E-15,-1.93207323326078,
-8.62957429809281));
#38651=CARTESIAN_POINT('Ctrl Pts',(-0.658062683030888,-1.93165972294369,
-8.58745240866785));
#38652=CARTESIAN_POINT('Ctrl Pts',(-2.46516391286739,-1.98743098295203,
-8.49849688064982));
#38653=CARTESIAN_POINT('Ctrl Pts',(-4.39676963179061,-2.13852225314529,
-8.46329578588585));
#38654=CARTESIAN_POINT('Ctrl Pts',(-6.35409454450772,-2.18205385875907,
-8.11784826271868));
#38655=CARTESIAN_POINT('Ctrl Pts',(-8.15537660210863,-2.1050270665009,-7.52858105609529));
#38656=CARTESIAN_POINT('Ctrl Pts',(-10.2097165609597,-1.7375710793364,-6.40958181990177));
#38657=CARTESIAN_POINT('Ctrl Pts',(-11.2781006865412,-1.40420632664524,
-5.56975094644535));
#38658=CARTESIAN_POINT('Ctrl Pts',(-11.7470010949101,-1.24897189262896,
-5.16040757324739));
#38659=CARTESIAN_POINT('',(-16.6859947282585,-0.000213685071574765,0.653010349651234));
#38660=CARTESIAN_POINT('Ctrl Pts',(-11.7470010949101,-1.24897189262896,
-5.16040757324739));
#38661=CARTESIAN_POINT('Ctrl Pts',(-12.0051227941173,-1.16133413061408,
-4.91749318228553));
#38662=CARTESIAN_POINT('Ctrl Pts',(-12.7010876741305,-0.905923104279308,
-4.23327664549238));
#38663=CARTESIAN_POINT('Ctrl Pts',(-13.4034560583173,-0.630382964431516,
-3.47895409086386));
#38664=CARTESIAN_POINT('Ctrl Pts',(-14.2693062595799,-0.346358717812154,
-2.463047534852));
#38665=CARTESIAN_POINT('Ctrl Pts',(-14.9655514589865,-0.169147364522696,
-1.59527625944176));
#38666=CARTESIAN_POINT('Ctrl Pts',(-15.802459484106,-0.0396258388242596,
-0.512753421506671));
#38667=CARTESIAN_POINT('Ctrl Pts',(-16.3914046039635,-0.0079781652302746,
0.264045566458043));
#38668=CARTESIAN_POINT('Ctrl Pts',(-16.6859947282585,-0.000213685071574765,
0.653010349651234));
#38669=CARTESIAN_POINT('',(-21.1430614769936,0.000756295652328289,6.63001173744468));
#38670=CARTESIAN_POINT('Ctrl Pts',(-16.6863334278776,-0.000204653071346932,
0.653462911021818));
#38671=CARTESIAN_POINT('Ctrl Pts',(-16.8118521335206,0.00314150838095653,
0.821178522657258));
#38672=CARTESIAN_POINT('Ctrl Pts',(-16.937649788032,0.00537544180921331,
0.990238755444057));
#38673=CARTESIAN_POINT('Ctrl Pts',(-17.0633706860534,0.0068090556350368,
1.15985916130958));
#38674=CARTESIAN_POINT('Ctrl Pts',(-17.1804382136137,0.00814399380925252,
1.31780459322238));
#38675=CARTESIAN_POINT('Ctrl Pts',(-17.2974387804625,0.00878473931917982,
1.47623543730744));
#38676=CARTESIAN_POINT('Ctrl Pts',(-17.4141122266992,0.0089781522474648,
1.63455929336058));
#38677=CARTESIAN_POINT('Ctrl Pts',(-17.5138264956263,0.00914345145964242,
1.76986983804117));
#38678=CARTESIAN_POINT('Ctrl Pts',(-17.6133042468771,0.00898183853621348,
1.90510568704074));
#38679=CARTESIAN_POINT('Ctrl Pts',(-17.7124025646993,0.00864633652358228,
2.03992407930371));
#38680=CARTESIAN_POINT('Ctrl Pts',(-17.7724114264697,0.008443173701628,
2.1215631872443));
#38681=CARTESIAN_POINT('Ctrl Pts',(-17.8322823536763,0.00817623153716935,
2.20305085372838));
#38682=CARTESIAN_POINT('Ctrl Pts',(-17.8919878634841,0.00787965725593698,
2.28431647094987));
#38683=CARTESIAN_POINT('Ctrl Pts',(-17.9273873601848,0.00770381786818521,
2.33249899142373));
#38684=CARTESIAN_POINT('Ctrl Pts',(-17.962728014113,0.00751757003612775,
2.38060250534804));
#38685=CARTESIAN_POINT('Ctrl Pts',(-17.9980083677065,0.00732807539521961,
2.42861802646074));
#38686=CARTESIAN_POINT('Ctrl Pts',(-18.001488971058,0.00730938069363454,
2.43335502500778));
#38687=CARTESIAN_POINT('Ctrl Pts',(-18.0049689406119,0.00729065469608626,
2.43809110323027));
#38688=CARTESIAN_POINT('Ctrl Pts',(-18.0084482439713,0.00727190448674141,
2.4428262102729));
#38689=CARTESIAN_POINT('Ctrl Pts',(-18.0356067319927,0.00712554549378024,
2.47978715751235));
#38690=CARTESIAN_POINT('Ctrl Pts',(-18.0627246109005,0.00697771079836186,
2.51668890611163));
#38691=CARTESIAN_POINT('Ctrl Pts',(-18.0898011533159,0.0068289269468095,
2.5535288181166));
#38692=CARTESIAN_POINT('Ctrl Pts',(-18.1068160814727,0.00673543101567395,
2.57667905814547));
#38693=CARTESIAN_POINT('Ctrl Pts',(-18.1238146910947,0.00664156041842843,
2.59980488613449));
#38694=CARTESIAN_POINT('Ctrl Pts',(-18.1407968393983,0.00654744676484664,
2.62290570083462));
#38695=CARTESIAN_POINT('Ctrl Pts',(-18.1552563546868,0.00646731333363974,
2.64257497808765));
#38696=CARTESIAN_POINT('Ctrl Pts',(-18.1697062080985,0.00638699100024018,
2.6622292107353));
#38697=CARTESIAN_POINT('Ctrl Pts',(-18.1841315126729,0.0063066438702019,
2.68184790502516));
#38698=CARTESIAN_POINT('Ctrl Pts',(-18.2628094149958,0.0058684178614192,
2.78885137972402));
#38699=CARTESIAN_POINT('Ctrl Pts',(-18.3408481744454,0.00542899616870739,
2.89492157878975));
#38700=CARTESIAN_POINT('Ctrl Pts',(-18.4185857226721,0.00499942937006533,
3.00047974395752));
#38701=CARTESIAN_POINT('Ctrl Pts',(-18.4582257304868,0.00478038424137877,
3.05430606839922));
#38702=CARTESIAN_POINT('Ctrl Pts',(-18.4977862541486,0.00456389907576071,
3.10799768886104));
#38703=CARTESIAN_POINT('Ctrl Pts',(-18.5373111419189,0.00435140300386188,
3.16160920698918));
#38704=CARTESIAN_POINT('Ctrl Pts',(-18.5752980418245,0.0041471755545533,
3.21313459992012));
#38705=CARTESIAN_POINT('Ctrl Pts',(-18.6132539759574,0.00394662084038625,
3.26458865570651));
#38706=CARTESIAN_POINT('Ctrl Pts',(-18.651225173531,0.00375096160359643,
3.3160297059887));
#38707=CARTESIAN_POINT('Ctrl Pts',(-18.6968885985567,0.00351566560398003,
3.37789171437661));
#38708=CARTESIAN_POINT('Ctrl Pts',(-18.7425740592339,0.00328744702494928,
3.43973487390792));
#38709=CARTESIAN_POINT('Ctrl Pts',(-18.7883405339597,0.00306792151733238,
3.50163208321023));
#38710=CARTESIAN_POINT('Ctrl Pts',(-18.8311081784255,0.00286278033227939,
3.55947350221248));
#38711=CARTESIAN_POINT('Ctrl Pts',(-18.873948318386,0.00266521867923928,
3.61736450244666));
#38712=CARTESIAN_POINT('Ctrl Pts',(-18.9169244512462,0.00247653826503431,
3.67538501492457));
#38713=CARTESIAN_POINT('Ctrl Pts',(-18.9454700021879,0.00235121320628823,
3.713923324083));
#38714=CARTESIAN_POINT('Ctrl Pts',(-18.9740766062369,0.00222980450534266,
3.75252018088541));
#38715=CARTESIAN_POINT('Ctrl Pts',(-19.002750377202,0.00211276369809768,
3.79118206185684));
#38716=CARTESIAN_POINT('Ctrl Pts',(-19.0918166419762,0.0017492123695992,
3.91127332336012));
#38717=CARTESIAN_POINT('Ctrl Pts',(-19.1815578127268,0.00142743926558962,
4.03202941632129));
#38718=CARTESIAN_POINT('Ctrl Pts',(-19.2726875642447,0.00116042555726567,
4.15435173614995));
#38719=CARTESIAN_POINT('Ctrl Pts',(-19.2813816998375,0.00113495140259462,
4.16602176505818));
#38720=CARTESIAN_POINT('Ctrl Pts',(-19.2900885036145,0.00110997811710799,
4.17770607709459));
#38721=CARTESIAN_POINT('Ctrl Pts',(-19.2988086153749,0.0010855186267792,
4.18940547392399));
#38722=CARTESIAN_POINT('Ctrl Pts',(-19.3208152543193,0.0010237910724514,
4.21893082967267));
#38723=CARTESIAN_POINT('Ctrl Pts',(-19.3429066761686,0.000965335607998434,
4.24855229564063));
#38724=CARTESIAN_POINT('Ctrl Pts',(-19.3650764005361,0.000910020328793069,
4.27826132650726));
#38725=CARTESIAN_POINT('Ctrl Pts',(-19.3762575288259,0.00088212249736634,
4.2932448454712));
#38726=CARTESIAN_POINT('Ctrl Pts',(-19.3874585697425,0.000855023480585796,
4.30825063094925));
#38727=CARTESIAN_POINT('Ctrl Pts',(-19.3986786603822,0.000828706764082194,
4.32327754097334));
#38728=CARTESIAN_POINT('Ctrl Pts',(-19.4053571075269,0.00081304246993035,
4.33222189156429));
#38729=CARTESIAN_POINT('Ctrl Pts',(-19.4120423033525,0.000797655341410091,
4.34117372573289));
#38730=CARTESIAN_POINT('Ctrl Pts',(-19.4187340617144,0.000782541935546666,
4.35013279669144));
#38731=CARTESIAN_POINT('Ctrl Pts',(-19.4232484622159,0.00077234611505843,
4.35617677381085));
#38732=CARTESIAN_POINT('Ctrl Pts',(-19.4277598943644,0.000762288330701381,
4.36221607166435));
#38733=CARTESIAN_POINT('Ctrl Pts',(-19.4322675941183,0.000752368019598222,
4.36824967400285));
#38734=CARTESIAN_POINT('Ctrl Pts',(-19.4992389541811,0.000604980934588682,
4.45789152611113));
#38735=CARTESIAN_POINT('Ctrl Pts',(-19.5654385820019,0.00048765834225139,
4.54634670309566));
#38736=CARTESIAN_POINT('Ctrl Pts',(-19.6309044885807,0.000393902767859228,
4.63368322649588));
#38737=CARTESIAN_POINT('Ctrl Pts',(-19.6958323846366,0.00030091769353715,
4.72030200273454));
#38738=CARTESIAN_POINT('Ctrl Pts',(-19.760041586352,0.000231152537014414,
4.80582437353299));
#38739=CARTESIAN_POINT('Ctrl Pts',(-19.8235857619775,0.000179736863706651,
4.89033133041942));
#38740=CARTESIAN_POINT('Ctrl Pts',(-19.8670360901756,0.000144579780342639,
4.94811561946853));
#38741=CARTESIAN_POINT('Ctrl Pts',(-19.9101845732443,0.000118027126229189,
5.00543706756955));
#38742=CARTESIAN_POINT('Ctrl Pts',(-19.9530232955811,9.96610527972666E-5,
5.06228647275008));
#38743=CARTESIAN_POINT('Ctrl Pts',(-19.9690367114538,9.27956853033225E-5,
5.08353718046521));
#38744=CARTESIAN_POINT('Ctrl Pts',(-19.9850067567005,8.70756546104475E-5,
5.10472180088031));
#38745=CARTESIAN_POINT('Ctrl Pts',(-20.0009402615093,8.24965293587667E-5,
5.12584969761139));
#38746=CARTESIAN_POINT('Ctrl Pts',(-20.0882904962193,5.73929711453812E-5,
5.24167648905154));
#38747=CARTESIAN_POINT('Ctrl Pts',(-20.1744301620068,6.74023279539181E-5,
5.35564896659735));
#38748=CARTESIAN_POINT('Ctrl Pts',(-20.2594797574646,9.87670179380714E-5,
5.46798070174529));
#38749=CARTESIAN_POINT('Ctrl Pts',(-20.3187694951726,0.000120631957241371,
5.54628935303708));
#38750=CARTESIAN_POINT('Ctrl Pts',(-20.3775302368743,0.000152856878649054,
5.62380177343142));
#38751=CARTESIAN_POINT('Ctrl Pts',(-20.4358109975843,0.000190598969018732,
5.70060256600532));
#38752=CARTESIAN_POINT('Ctrl Pts',(-20.4813036494772,0.000220059596470905,
5.76055153851536));
#38753=CARTESIAN_POINT('Ctrl Pts',(-20.5265022303766,0.000253020880174828,
5.82006480704543));
#38754=CARTESIAN_POINT('Ctrl Pts',(-20.5714278548838,0.000287990739945883,
5.87918011463099));
#38755=CARTESIAN_POINT('Ctrl Pts',(-20.6679178821708,0.00036309804809229,
6.00614635504664));
#38756=CARTESIAN_POINT('Ctrl Pts',(-20.7631498007969,0.000447248524295111,
6.13127798052428));
#38757=CARTESIAN_POINT('Ctrl Pts',(-20.8573180070559,0.00052811713989227,
6.25493296623428));
#38758=CARTESIAN_POINT('Ctrl Pts',(-20.9389114498876,0.000598186954596536,
6.36207566766404));
#38759=CARTESIAN_POINT('Ctrl Pts',(-21.0197031680878,0.000665846435185652,
6.46810590314616));
#38760=CARTESIAN_POINT('Ctrl Pts',(-21.0998834016831,0.000725144819930417,
6.57334051556745));
#38761=CARTESIAN_POINT('Ctrl Pts',(-21.1142981099604,0.000735805413933246,
6.59225947066038));
#38762=CARTESIAN_POINT('Ctrl Pts',(-21.1286931164174,0.000746200536834672,
6.61115278824243));
#38763=CARTESIAN_POINT('Ctrl Pts',(-21.1430614769885,0.00075629653388815,
6.63001173743882));
#38764=CARTESIAN_POINT('',(-25.4512489408135,0.000583306484460569,12.6480025703979));
#38765=CARTESIAN_POINT('Ctrl Pts',(-21.1430614769933,0.000756296099460927,
6.63001173744467));
#38766=CARTESIAN_POINT('Ctrl Pts',(-21.5124085805419,0.00101581966494258,
7.11527647647093));
#38767=CARTESIAN_POINT('Ctrl Pts',(-21.9044241285154,0.00128152445976316,
7.62953628224353));
#38768=CARTESIAN_POINT('Ctrl Pts',(-22.6640844355056,0.00168268680946039,
8.64319916298904));
#38769=CARTESIAN_POINT('Ctrl Pts',(-23.0167102203234,0.00181865873821434,
9.12236041343943));
#38770=CARTESIAN_POINT('Ctrl Pts',(-23.7317035063752,0.00188587826873779,
10.1199883360218));
#38771=CARTESIAN_POINT('Ctrl Pts',(-24.0922922523239,0.00182192529464304,
10.6334016822487));
#38772=CARTESIAN_POINT('Ctrl Pts',(-24.7917978700544,0.0013940595563037,
11.6565878432607));
#38773=CARTESIAN_POINT('Ctrl Pts',(-25.1830186836289,0.000952760036780517,
12.2452305023429));
#38774=CARTESIAN_POINT('Ctrl Pts',(-25.4512489408144,0.000583307123841907,
12.6480025703979));
#38775=CARTESIAN_POINT('',(-30.3222847657765,-0.00413284663027091,18.6660068644689));
#38776=CARTESIAN_POINT('Ctrl Pts',(-25.4512489408144,0.000583307123841869,
12.6480025703979));
#38777=CARTESIAN_POINT('Ctrl Pts',(-26.2375266602302,-0.000499689987680418,
13.8286704081032));
#38778=CARTESIAN_POINT('Ctrl Pts',(-26.9256080520826,-0.00206137009404955,
14.8637894175972));
#38779=CARTESIAN_POINT('Ctrl Pts',(-28.5066600268001,-0.0048491048562661,
16.9014277594712));
#38780=CARTESIAN_POINT('Ctrl Pts',(-29.3327715286854,-0.00627370115692009,
17.789618484765));
#38781=CARTESIAN_POINT('Ctrl Pts',(-30.3222847382684,-0.00412017247110571,
18.6660068643839));
#38782=CARTESIAN_POINT('',(-44.3052665433893,0.50176463722647,24.6839663391592));
#38783=CARTESIAN_POINT('Ctrl Pts',(-30.3222847657765,-0.00413284663027091,
18.6660068644689));
#38784=CARTESIAN_POINT('Ctrl Pts',(-30.7285587386581,-0.00325138912786291,
19.0258393291216));
#38785=CARTESIAN_POINT('Ctrl Pts',(-31.3846390634535,-0.00108090020159251,
19.5676919050105));
#38786=CARTESIAN_POINT('Ctrl Pts',(-32.4133598840372,0.00689348995379523,
20.3244421620242));
#38787=CARTESIAN_POINT('Ctrl Pts',(-34.9086113550027,0.0335760566375183,
22.0306340145341));
#38788=CARTESIAN_POINT('Ctrl Pts',(-37.6978937468501,0.11693363945437,23.2888479293169));
#38789=CARTESIAN_POINT('Ctrl Pts',(-39.7806058664349,0.216865324193402,
23.8826917702588));
#38790=CARTESIAN_POINT('Ctrl Pts',(-40.597421702395,0.259993271724183,24.084560939485));
#38791=CARTESIAN_POINT('Ctrl Pts',(-41.4486629431555,0.307991395735675,
24.2719159198737));
#38792=CARTESIAN_POINT('Ctrl Pts',(-42.6707056826778,0.383592726711738,
24.4939878032503));
#38793=CARTESIAN_POINT('Ctrl Pts',(-43.7457382365382,0.459542695930701,
24.6297413546134));
#38794=CARTESIAN_POINT('Ctrl Pts',(-44.3052665433893,0.501764637226471,
24.6839663391592));
#38795=CARTESIAN_POINT('',(-49.3675963148847,0.956500242243167,24.6840252060176));
#38796=CARTESIAN_POINT('Ctrl Pts',(-44.3052665433893,0.501764637226471,
24.6839663391592));
#38797=CARTESIAN_POINT('Ctrl Pts',(-45.8824543200059,0.620779044324047,
24.8368171284471));
#38798=CARTESIAN_POINT('Ctrl Pts',(-47.6223636079185,0.774187094160568,
24.8731447167143));
#38799=CARTESIAN_POINT('Ctrl Pts',(-49.3675963149307,0.956500241803143,
24.6840252060176));
#38800=CARTESIAN_POINT('',(-61.5166608776679,2.54670163095537,18.6669577173835));
#38801=CARTESIAN_POINT('Ctrl Pts',(-49.3675963149307,0.956500241803143,
24.6840252060176));
#38802=CARTESIAN_POINT('Ctrl Pts',(-50.8584101085268,1.11223589479094,24.5224746204595));
#38803=CARTESIAN_POINT('Ctrl Pts',(-53.5751452720453,1.43410480188598,23.9491047084121));
#38804=CARTESIAN_POINT('Ctrl Pts',(-56.685826170517,1.86305916206279,22.9608139368193));
#38805=CARTESIAN_POINT('Ctrl Pts',(-58.1934501574325,2.0765014749507,22.2614053479118));
#38806=CARTESIAN_POINT('Ctrl Pts',(-59.4665491367357,2.25831996402558,21.3906391167669));
#38807=CARTESIAN_POINT('Ctrl Pts',(-60.5958520140507,2.41846826761656,20.1757428158229));
#38808=CARTESIAN_POINT('Ctrl Pts',(-61.2120138672132,2.50451285269251,19.2030902538488));
#38809=CARTESIAN_POINT('Ctrl Pts',(-61.5166608776679,2.54670163095537,18.6669577173835));
#38810=CARTESIAN_POINT('',(-64.4551411469067,2.94895124118343,12.643128511615));
#38811=CARTESIAN_POINT('Ctrl Pts',(-61.5166579557216,2.54672260023573,18.6669577083775));
#38812=CARTESIAN_POINT('Ctrl Pts',(-61.9449589659908,2.60609546337214,17.9143482600221));
#38813=CARTESIAN_POINT('Ctrl Pts',(-62.3851009475059,2.66495993045432,17.0249620269639));
#38814=CARTESIAN_POINT('Ctrl Pts',(-63.2835028538324,2.78486870373281,15.1472982754152));
#38815=CARTESIAN_POINT('Ctrl Pts',(-63.5467635706412,2.82032508158459,14.5938134505021));
#38816=CARTESIAN_POINT('Ctrl Pts',(-64.0017146934209,2.88329552572288,13.6289746707392));
#38817=CARTESIAN_POINT('Ctrl Pts',(-64.2299173026253,2.91581081465848,13.1396374113502));
#38818=CARTESIAN_POINT('Ctrl Pts',(-64.4551318427595,2.94901660708818,12.6431286647104));
#38819=CARTESIAN_POINT('',(-66.7632425918307,3.2720446654144,6.633020912074));
#38820=CARTESIAN_POINT('Ctrl Pts',(-64.4551411469067,2.94895124118343,12.643128511615));
#38821=CARTESIAN_POINT('Ctrl Pts',(-64.8619798876637,3.00903884605696,11.7454668071155));
#38822=CARTESIAN_POINT('Ctrl Pts',(-65.505440000895,3.11095649481449,10.2498012385406));
#38823=CARTESIAN_POINT('Ctrl Pts',(-66.2655539657919,3.21663700939875,8.09409501252873));
#38824=CARTESIAN_POINT('Ctrl Pts',(-66.6022993283403,3.25480527973138,7.07959750520892));
#38825=CARTESIAN_POINT('Ctrl Pts',(-66.7631910382533,3.27249821191336,6.63302022230481));
#38826=CARTESIAN_POINT('',(-73.6760374232779,5.16935883999202,0.190989875004182));
#38827=CARTESIAN_POINT('Ctrl Pts',(-66.7632425918307,3.2720446654144,6.633020912074));
#38828=CARTESIAN_POINT('Ctrl Pts',(-66.7778516238031,3.27363852677518,6.59368385722911));
#38829=CARTESIAN_POINT('Ctrl Pts',(-66.7926503366434,3.27521476311706,6.55407752441134));
#38830=CARTESIAN_POINT('Ctrl Pts',(-66.8076622570084,3.27677215677882,6.51414962524557));
#38831=CARTESIAN_POINT('Ctrl Pts',(-66.8227415209764,3.27833653692185,6.47404260918319));
#38832=CARTESIAN_POINT('Ctrl Pts',(-66.8380359055963,3.27988190475181,6.43361142106289));
#38833=CARTESIAN_POINT('Ctrl Pts',(-66.8535704549874,3.28140734584648,6.39274919904974));
#38834=CARTESIAN_POINT('Ctrl Pts',(-66.8691050043786,3.28293278694115,6.35188697703659));
#38835=CARTESIAN_POINT('Ctrl Pts',(-66.8848797161219,3.28443830178511,6.31059393057822));
#38836=CARTESIAN_POINT('Ctrl Pts',(-66.9009208783732,3.28592329229036,6.26870578557491));
#38837=CARTESIAN_POINT('Ctrl Pts',(-66.925751174839,3.28822192588786,6.20386665219223));
#38838=CARTESIAN_POINT('Ctrl Pts',(-66.9512195193938,3.29047109652991,6.13758563776401));
#38839=CARTESIAN_POINT('Ctrl Pts',(-66.9774293209226,3.2926746892832,6.07018552522113));
#38840=CARTESIAN_POINT('Ctrl Pts',(-66.9988272592458,3.29447372396008,6.0151594141083));
#38841=CARTESIAN_POINT('Ctrl Pts',(-67.0207195340082,3.29624244802965,5.95938828124706));
#38842=CARTESIAN_POINT('Ctrl Pts',(-67.0431661797375,3.29798514864501,5.90307322483236));
#38843=CARTESIAN_POINT('Ctrl Pts',(-67.081595026309,3.30096866677845,5.80666137387091));
#38844=CARTESIAN_POINT('Ctrl Pts',(-67.1216471810934,3.30387469587049,5.70866225403845));
#38845=CARTESIAN_POINT('Ctrl Pts',(-67.1636464856163,3.30674464355634,5.60964585544974));
#38846=CARTESIAN_POINT('Ctrl Pts',(-67.2071111346927,3.3097147229529,5.50717480107519));
#38847=CARTESIAN_POINT('Ctrl Pts',(-67.2527690423822,3.31264837414508,5.40305522896293));
#38848=CARTESIAN_POINT('Ctrl Pts',(-67.3008684292325,3.31559000642976,5.29763784637666));
#38849=CARTESIAN_POINT('Ctrl Pts',(-67.3207250789926,3.31680438702429,5.25411887073675));
#38850=CARTESIAN_POINT('Ctrl Pts',(-67.3409981849322,3.31802043944008,5.21037835697596));
#38851=CARTESIAN_POINT('Ctrl Pts',(-67.3617067668992,3.31924268717797,5.16643939842894));
#38852=CARTESIAN_POINT('Ctrl Pts',(-67.4131411385364,3.32227841142426,5.05730721705296));
#38853=CARTESIAN_POINT('Ctrl Pts',(-67.4672594232976,3.32534977695346,4.94695098046708));
#38854=CARTESIAN_POINT('Ctrl Pts',(-67.5243778514364,3.32854526909525,4.83578384025443));
#38855=CARTESIAN_POINT('Ctrl Pts',(-67.5797346638728,3.33164220759477,4.72804525692193));
#38856=CARTESIAN_POINT('Ctrl Pts',(-67.637909632063,3.33485546291609,4.61954493297593));
#38857=CARTESIAN_POINT('Ctrl Pts',(-67.6992220665778,3.33830219654704,4.51065257941795));
#38858=CARTESIAN_POINT('Ctrl Pts',(-67.7594871016904,3.34169004967889,4.40362043230804));
#38859=CARTESIAN_POINT('Ctrl Pts',(-67.8227834984399,3.34530314118978,4.29620941841597));
#38860=CARTESIAN_POINT('Ctrl Pts',(-67.8894425869409,3.34929320208703,4.18876581786222));
#38861=CARTESIAN_POINT('Ctrl Pts',(-67.9544129231919,3.35318217812895,4.08404421105687));
#38862=CARTESIAN_POINT('Ctrl Pts',(-68.022577948134,3.35742904100138,3.97929148951414));
#38863=CARTESIAN_POINT('Ctrl Pts',(-68.0942684114907,3.36221702676486,3.87482570228378));
#38864=CARTESIAN_POINT('Ctrl Pts',(-68.1439301056711,3.3655337787231,3.80245975938383));
#38865=CARTESIAN_POINT('Ctrl Pts',(-68.1952840339283,3.36911107463874,3.73023144553659));
#38866=CARTESIAN_POINT('Ctrl Pts',(-68.2484463317038,3.37302320707464,3.65824640771746));
#38867=CARTESIAN_POINT('Ctrl Pts',(-68.2963237263679,3.37654643154854,3.59341745543768));
#38868=CARTESIAN_POINT('Ctrl Pts',(-68.3456679353863,3.38034131488696,3.52878579007826));
#38869=CARTESIAN_POINT('Ctrl Pts',(-68.396566560834,3.38447437656862,3.46442745789461));
#38870=CARTESIAN_POINT('Ctrl Pts',(-68.4399174001416,3.38799454418091,3.40961285942435));
#38871=CARTESIAN_POINT('Ctrl Pts',(-68.4843962019402,3.39176007652746,3.35499649460645));
#38872=CARTESIAN_POINT('Ctrl Pts',(-68.5300478346321,3.39582059599171,3.30062598661843));
#38873=CARTESIAN_POINT('Ctrl Pts',(-68.605148574348,3.40250048885453,3.21118197053735));
#38874=CARTESIAN_POINT('Ctrl Pts',(-68.6832846494335,3.4099628769802,3.12244281424077));
#38875=CARTESIAN_POINT('Ctrl Pts',(-68.7644215211146,3.41843068019497,3.03458147483682));
#38876=CARTESIAN_POINT('Ctrl Pts',(-68.8437792250609,3.42671280158652,2.94864675716427));
#38877=CARTESIAN_POINT('Ctrl Pts',(-68.9260078649796,3.43595736036824,2.86355140090532));
#38878=CARTESIAN_POINT('Ctrl Pts',(-69.0110358708828,3.44639725953889,2.77947643571424));
#38879=CARTESIAN_POINT('Ctrl Pts',(-69.0953878948292,3.45675416036805,2.69606987570192));
#38880=CARTESIAN_POINT('Ctrl Pts',(-69.1824951022211,3.46828818269589,2.61366721682793));
#38881=CARTESIAN_POINT('Ctrl Pts',(-69.2722450959242,3.4812410257998,2.53246965132781));
#38882=CARTESIAN_POINT('Ctrl Pts',(-69.3615880501007,3.49413512439679,2.45164033787172));
#38883=CARTESIAN_POINT('Ctrl Pts',(-69.4535498120667,3.50843600124425,2.37200498389905));
#38884=CARTESIAN_POINT('Ctrl Pts',(-69.5479765076371,3.52438501326241,2.29379058216315));
#38885=CARTESIAN_POINT('Ctrl Pts',(-69.5835334743656,3.53039071415298,2.26433845675087));
#38886=CARTESIAN_POINT('Ctrl Pts',(-69.6194395246876,3.53663007920999,2.2350881216089));
#38887=CARTESIAN_POINT('Ctrl Pts',(-69.6556849168736,3.54311573774292,2.20605283237209));
#38888=CARTESIAN_POINT('Ctrl Pts',(-69.7514241999826,3.56024708219757,2.12935845527359));
#38889=CARTESIAN_POINT('Ctrl Pts',(-69.8495489942764,3.57910088692489,2.05416051893023));
#38890=CARTESIAN_POINT('Ctrl Pts',(-69.9497187807409,3.59988140484318,1.98056289443286));
#38891=CARTESIAN_POINT('Ctrl Pts',(-70.0493579133009,3.62055183704241,1.90735515662866));
#38892=CARTESIAN_POINT('Ctrl Pts',(-70.1510198437214,3.64312944268963,1.83573095377873));
#38893=CARTESIAN_POINT('Ctrl Pts',(-70.2543363411126,3.66778714917268,1.76581974058179));
#38894=CARTESIAN_POINT('Ctrl Pts',(-70.3568397508631,3.69225080265454,1.69645871970495));
#38895=CARTESIAN_POINT('Ctrl Pts',(-70.4609711070713,3.71876259431705,1.62878411238229));
#38896=CARTESIAN_POINT('Ctrl Pts',(-70.5663476422515,3.74745271803715,1.56294609407678));
#38897=CARTESIAN_POINT('Ctrl Pts',(-70.6704395356238,3.77579308142074,1.49791070484539));
#38898=CARTESIAN_POINT('Ctrl Pts',(-70.7757457442586,3.80625938925171,1.43466779231534));
#38899=CARTESIAN_POINT('Ctrl Pts',(-70.8818848613732,3.83893150095146,1.37338032282391));
#38900=CARTESIAN_POINT('Ctrl Pts',(-70.9359385471963,3.85557049427463,1.34216832755918));
#38901=CARTESIAN_POINT('Ctrl Pts',(-70.9902081180437,3.87278080606398,1.31146374997487));
#38902=CARTESIAN_POINT('Ctrl Pts',(-71.0446427957615,3.89056794250507,1.28128941908642));
#38903=CARTESIAN_POINT('Ctrl Pts',(-71.1348036965975,3.92002901974587,1.23131126234723));
#38904=CARTESIAN_POINT('Ctrl Pts',(-71.225431930372,3.95108245182755,1.18276232504616));
#38905=CARTESIAN_POINT('Ctrl Pts',(-71.316067797823,3.98366316485251,1.13570828437813));
#38906=CARTESIAN_POINT('Ctrl Pts',(-71.4049975632047,4.01563058842073,1.08953997469508));
#38907=CARTESIAN_POINT('Ctrl Pts',(-71.4939342726877,4.049068371674,1.04481112345883));
#38908=CARTESIAN_POINT('Ctrl Pts',(-71.5824508941236,4.08386513405905,1.00158432608665));
#38909=CARTESIAN_POINT('Ctrl Pts',(-71.6050814782526,4.09276144128134,0.990532755673197));
#38910=CARTESIAN_POINT('Ctrl Pts',(-71.6276846575919,4.10174631856564,0.979579355859735));
#38911=CARTESIAN_POINT('Ctrl Pts',(-71.6502534198816,4.11081736792181,0.968725141126268));
#38912=CARTESIAN_POINT('Ctrl Pts',(-71.7413595560693,4.14743560366732,0.924908579410377));
#38913=CARTESIAN_POINT('Ctrl Pts',(-71.8319031202047,4.18546188054524,0.882709644373667));
#38914=CARTESIAN_POINT('Ctrl Pts',(-71.9214481093997,4.22457715179907,0.842184297212655));
#38915=CARTESIAN_POINT('Ctrl Pts',(-72.0174138967299,4.26649717251995,0.79875309149031));
#38916=CARTESIAN_POINT('Ctrl Pts',(-72.1122322699238,4.30966740820752,0.757244478751865));
#38917=CARTESIAN_POINT('Ctrl Pts',(-72.2053958847573,4.35364318548031,0.717705234412282));
#38918=CARTESIAN_POINT('Ctrl Pts',(-72.2985594995909,4.3976189627531,0.678165990072699));
#38919=CARTESIAN_POINT('Ctrl Pts',(-72.390068306429,4.44239909257851,0.640596137078233));
#38920=CARTESIAN_POINT('Ctrl Pts',(-72.479447063832,4.48750315511749,0.605018247143105));
#38921=CARTESIAN_POINT('Ctrl Pts',(-72.5702985368102,4.53335040829074,0.568854131642064));
#38922=CARTESIAN_POINT('Ctrl Pts',(-72.659020807773,4.57956119168153,0.534719321379211));
#38923=CARTESIAN_POINT('Ctrl Pts',(-72.7457116179679,4.62594207736946,0.502385439090387));
#38924=CARTESIAN_POINT('Ctrl Pts',(-72.8366881117079,4.67461586813179,0.468453085326186));
#38925=CARTESIAN_POINT('Ctrl Pts',(-72.9254276354649,4.72347695076411,0.436503801608705));
#38926=CARTESIAN_POINT('Ctrl Pts',(-73.0120512426314,4.7723580160016,0.406259796438403));
#38927=CARTESIAN_POINT('Ctrl Pts',(-73.1013783849707,4.82276466627851,0.375071871539767));
#38928=CARTESIAN_POINT('Ctrl Pts',(-73.1884557723436,4.87319281725982,0.345696966659892));
#38929=CARTESIAN_POINT('Ctrl Pts',(-73.2734196953545,4.92351553196678,0.317821550706115));
#38930=CARTESIAN_POINT('Ctrl Pts',(-73.3629470980995,4.97654111961786,0.288448924038924));
#38931=CARTESIAN_POINT('Ctrl Pts',(-73.450128176113,5.02944981953762,0.260740832188493));
#38932=CARTESIAN_POINT('Ctrl Pts',(-73.5351217584104,5.08215181279788,0.234326404103092));
#38933=CARTESIAN_POINT('Ctrl Pts',(-73.582596736888,5.11158963537376,0.21957206182269));
#38934=CARTESIAN_POINT('Ctrl Pts',(-73.6293891746598,5.14096398116758,0.205221308463415));
#38935=CARTESIAN_POINT('Ctrl Pts',(-73.6755262547354,5.17026613426529,0.191209597395648));
#38936=CARTESIAN_POINT('',(-79.5980561166416,9.79488102647745,-1.92025417899612));
#38937=CARTESIAN_POINT('Ctrl Pts',(-73.6764877119598,5.1685596039116,0.190796321415114));
#38938=CARTESIAN_POINT('Ctrl Pts',(-74.7404219526711,5.85068157891375,-0.142609954538472));
#38939=CARTESIAN_POINT('Ctrl Pts',(-75.9741654535975,6.89428741101915,-0.412567402884934));
#38940=CARTESIAN_POINT('Ctrl Pts',(-77.4581499404949,8.19662250468364,-0.873282366765809));
#38941=CARTESIAN_POINT('Ctrl Pts',(-78.1080385927614,8.74315679055215,-1.12050093759123));
#38942=CARTESIAN_POINT('Ctrl Pts',(-78.8357086373011,9.31133939639374,-1.44888811728152));
#38943=CARTESIAN_POINT('Ctrl Pts',(-79.2776917908501,9.61051959968398,-1.69898330179011));
#38944=CARTESIAN_POINT('Ctrl Pts',(-79.5980561168787,9.79488102596951,-1.92025417907613));
#38945=CARTESIAN_POINT('',(-77.5413434256017,9.45934560247393,-5.67965754882122));
#38946=CARTESIAN_POINT('Ctrl Pts',(-79.5980561168786,9.7948810259695,-1.92025417907612));
#38947=CARTESIAN_POINT('Ctrl Pts',(-79.3926541200977,9.78652201900712,-2.47576181499884));
#38948=CARTESIAN_POINT('Ctrl Pts',(-78.8071962567564,9.7034726253451,-3.78882461998114));
#38949=CARTESIAN_POINT('Ctrl Pts',(-78.0251745283461,9.56134461172776,-5.02766395488251));
#38950=CARTESIAN_POINT('Ctrl Pts',(-77.5413122691002,9.45942207531784,-5.67964638243143));
#38951=CARTESIAN_POINT('',(-70.7282577522101,8.51486331985853,-11.892519184563));
#38952=CARTESIAN_POINT('Ctrl Pts',(-77.5413434256017,9.45934560247393,-5.67965754882122));
#38953=CARTESIAN_POINT('Ctrl Pts',(-77.5142821984464,9.45356384346927,-5.71556759801311));
#38954=CARTESIAN_POINT('Ctrl Pts',(-77.4869693706751,9.44763492792691,-5.75132849528266));
#38955=CARTESIAN_POINT('Ctrl Pts',(-77.459392567839,9.44158248309945,-5.78710530983847));
#38956=CARTESIAN_POINT('Ctrl Pts',(-77.4323651788443,9.43565062139332,-5.82216934136303));
#38957=CARTESIAN_POINT('Ctrl Pts',(-77.4050841899675,9.42960017534997,-5.85724885204878));
#38958=CARTESIAN_POINT('Ctrl Pts',(-77.3775393869878,9.42344934005853,-5.89245008383269));
#38959=CARTESIAN_POINT('Ctrl Pts',(-77.3507057470255,9.41745730955464,-5.926742475781));
#38960=CARTESIAN_POINT('Ctrl Pts',(-77.3236217027424,9.41137006917975,-5.96115047465854));
#38961=CARTESIAN_POINT('Ctrl Pts',(-77.2962797330602,9.40519958906143,-5.99572323319143));
#38962=CARTESIAN_POINT('Ctrl Pts',(-77.2823729183937,9.4020611274068,-6.01330780924863));
#38963=CARTESIAN_POINT('Ctrl Pts',(-77.2683994129127,9.39890104755503,-6.03093420635041));
#38964=CARTESIAN_POINT('Ctrl Pts',(-77.2543584747973,9.39572034184949,-6.04860371317784));
#38965=CARTESIAN_POINT('Ctrl Pts',(-77.2093734063961,9.38552983587676,-6.10521417372642));
#38966=CARTESIAN_POINT('Ctrl Pts',(-77.1636964406147,9.37512650810942,-6.16225985620397));
#38967=CARTESIAN_POINT('Ctrl Pts',(-77.1173124297829,9.36452720094655,-6.21966639031466));
#38968=CARTESIAN_POINT('Ctrl Pts',(-77.0724581614658,9.35427745843977,-6.27517965960673));
#38969=CARTESIAN_POINT('Ctrl Pts',(-77.0269427749634,9.34384437086552,-6.33103023795012));
#38970=CARTESIAN_POINT('Ctrl Pts',(-76.9807507843413,9.33325212543006,-6.38719925161227));
#38971=CARTESIAN_POINT('Ctrl Pts',(-76.9702354818589,9.33084087050855,-6.39998575768921));
#38972=CARTESIAN_POINT('Ctrl Pts',(-76.9596851070482,9.32842140837096,-6.41278897398065));
#38973=CARTESIAN_POINT('Ctrl Pts',(-76.9490994584738,9.32599409895416,-6.42560905396616));
#38974=CARTESIAN_POINT('Ctrl Pts',(-76.8689375031935,9.3076128096497,-6.52269169101637));
#38975=CARTESIAN_POINT('Ctrl Pts',(-76.7867518479299,9.28878025003937,-6.62074657320179));
#38976=CARTESIAN_POINT('Ctrl Pts',(-76.7024649817347,9.26965359217964,-6.71973310414691));
#38977=CARTESIAN_POINT('Ctrl Pts',(-76.625561125183,9.25220231158567,-6.81004902547595));
#38978=CARTESIAN_POINT('Ctrl Pts',(-76.5469082661047,9.23450749951946,-6.90114067648958));
#38979=CARTESIAN_POINT('Ctrl Pts',(-76.4664583841173,9.21669125658552,-6.99293229934345));
#38980=CARTESIAN_POINT('Ctrl Pts',(-76.4055809814877,9.20320948920882,-7.06239213501332));
#38981=CARTESIAN_POINT('Ctrl Pts',(-76.3436746896887,9.18965823967548,-7.13225188856446));
#38982=CARTESIAN_POINT('Ctrl Pts',(-76.2807215287226,9.17608787534858,-7.20245910972558));
#38983=CARTESIAN_POINT('Ctrl Pts',(-76.2175251915839,9.1624650912669,-7.27293752812414));
#38984=CARTESIAN_POINT('Ctrl Pts',(-76.1532738906648,9.14882286470201,-7.34376497718704));
#38985=CARTESIAN_POINT('Ctrl Pts',(-76.087955371975,9.13521006306119,-7.41489463717834));
#38986=CARTESIAN_POINT('Ctrl Pts',(-75.9758314377519,9.11184271018204,-7.53699381331019));
#38987=CARTESIAN_POINT('Ctrl Pts',(-75.8605011879027,9.08860063350606,-7.66039372555022));
#38988=CARTESIAN_POINT('Ctrl Pts',(-75.7413454478133,9.06564256808275,-7.78544462689756));
#38989=CARTESIAN_POINT('Ctrl Pts',(-75.6337419763672,9.04491031015393,-7.89837171779831));
#38990=CARTESIAN_POINT('Ctrl Pts',(-75.523018539085,9.0244100059248,-8.01264591774364));
#38991=CARTESIAN_POINT('Ctrl Pts',(-75.4087158498956,9.00428410594188,-8.12849174972041));
#38992=CARTESIAN_POINT('Ctrl Pts',(-75.3343282518198,8.99118627447822,-8.20388361712937));
#38993=CARTESIAN_POINT('Ctrl Pts',(-75.2584246377425,8.97824756940062,-8.27994043561488));
#38994=CARTESIAN_POINT('Ctrl Pts',(-75.1808786513554,8.96551237918548,-8.35671312887169));
#38995=CARTESIAN_POINT('Ctrl Pts',(-75.0861154632862,8.9499496494856,-8.45053133286425));
#38996=CARTESIAN_POINT('Ctrl Pts',(-74.9888998796607,8.93468501931142,-8.54536890727092));
#38997=CARTESIAN_POINT('Ctrl Pts',(-74.8895954521882,8.91990014338027,-8.64082848977418));
#38998=CARTESIAN_POINT('Ctrl Pts',(-74.8237602476036,8.91009831121166,-8.70411470272186));
#38999=CARTESIAN_POINT('Ctrl Pts',(-74.7570073460718,8.90050666601648,-8.7676736961274));
#39000=CARTESIAN_POINT('Ctrl Pts',(-74.6894475678803,8.89116756387664,-8.83138447768835));
#39001=CARTESIAN_POINT('Ctrl Pts',(-74.5927641137914,8.87780256065818,-8.92255970929652));
#39002=CARTESIAN_POINT('Ctrl Pts',(-74.4944270055992,8.86495684504577,-9.01404623510722));
#39003=CARTESIAN_POINT('Ctrl Pts',(-74.3947926712449,8.85270483437522,-9.10547037505296));
#39004=CARTESIAN_POINT('Ctrl Pts',(-74.29578008106,8.84052927943902,-9.19632400457842));
#39005=CARTESIAN_POINT('Ctrl Pts',(-74.195486619814,8.82894028441388,-9.28711544802413));
#39006=CARTESIAN_POINT('Ctrl Pts',(-74.0942825153974,8.81796417439208,-9.37747159674706));
#39007=CARTESIAN_POINT('Ctrl Pts',(-73.9934637520285,8.80702985660548,-9.46748370870173));
#39008=CARTESIAN_POINT('Ctrl Pts',(-73.891741598813,8.79670387124786,-9.55706325103888));
#39009=CARTESIAN_POINT('Ctrl Pts',(-73.7894983248483,8.78696310332303,-9.64584369468491));
#39010=CARTESIAN_POINT('Ctrl Pts',(-73.7744301881695,8.78552755439393,-9.65892774224506));
#39011=CARTESIAN_POINT('Ctrl Pts',(-73.7593507563086,8.78410462767017,-9.67199444704903));
#39012=CARTESIAN_POINT('Ctrl Pts',(-73.7442612753102,8.78269415742303,-9.68504265207626));
#39013=CARTESIAN_POINT('Ctrl Pts',(-73.6420318120065,8.77313838699025,-9.7734427101798));
#39014=CARTESIAN_POINT('Ctrl Pts',(-73.5393410808177,8.7641587418496,-9.8609932390083));
#39015=CARTESIAN_POINT('Ctrl Pts',(-73.4365784472836,8.75566920417689,-9.94734692942645));
#39016=CARTESIAN_POINT('Ctrl Pts',(-73.3285944434713,8.7467483130233,-10.0380882515845));
#39017=CARTESIAN_POINT('Ctrl Pts',(-73.2205317290125,8.73836812583255,-10.1275072089461));
#39018=CARTESIAN_POINT('Ctrl Pts',(-73.1128365659561,8.73037266133452,-10.2152131863157));
#39019=CARTESIAN_POINT('Ctrl Pts',(-73.071220190016,8.72728299373086,-10.2491051905879));
#39020=CARTESIAN_POINT('Ctrl Pts',(-73.0296585866431,8.72425024662359,-10.2827415972262));
#39021=CARTESIAN_POINT('Ctrl Pts',(-72.9881769722381,8.72126366625822,-10.3161007689154));
#39022=CARTESIAN_POINT('Ctrl Pts',(-72.927197056175,8.71687325323771,-10.3651403137527));
#39023=CARTESIAN_POINT('Ctrl Pts',(-72.8663948120556,8.71257989567172,-10.4135664782779));
#39024=CARTESIAN_POINT('Ctrl Pts',(-72.8057311638433,8.70833772590909,-10.4614014331091));
#39025=CARTESIAN_POINT('Ctrl Pts',(-72.6720088391437,8.69898661005723,-10.5668451634225));
#39026=CARTESIAN_POINT('Ctrl Pts',(-72.5389607681471,8.6898833035686,-10.6694195862342));
#39027=CARTESIAN_POINT('Ctrl Pts',(-72.4061666716076,8.68054726327208,-10.7693713198737));
#39028=CARTESIAN_POINT('Ctrl Pts',(-72.2844782862219,8.67199200592869,-10.8609639840058));
#39029=CARTESIAN_POINT('Ctrl Pts',(-72.1630026242835,8.66324239041884,-10.9503544622541));
#39030=CARTESIAN_POINT('Ctrl Pts',(-72.0414094827878,8.65392446659711,-11.0376910827571));
#39031=CARTESIAN_POINT('Ctrl Pts',(-71.9568362998022,8.6474434556887,-11.0984374036128));
#39032=CARTESIAN_POINT('Ctrl Pts',(-71.8722061531492,8.64068749379229,-11.1581892721519));
#39033=CARTESIAN_POINT('Ctrl Pts',(-71.7874075681809,8.63352479050082,-11.216982677569));
#39034=CARTESIAN_POINT('Ctrl Pts',(-71.6784906925915,8.62432488152153,-11.2924980181338));
#39035=CARTESIAN_POINT('Ctrl Pts',(-71.5692957068855,8.61445495735751,-11.3664337484946));
#39036=CARTESIAN_POINT('Ctrl Pts',(-71.4595925371217,8.60361780995115,-11.4388129550185));
#39037=CARTESIAN_POINT('Ctrl Pts',(-71.3942487439551,8.59716275199647,-11.4819250356525));
#39038=CARTESIAN_POINT('Ctrl Pts',(-71.3287247224875,8.59036411398718,-11.5244841417791));
#39039=CARTESIAN_POINT('Ctrl Pts',(-71.2629723517172,8.58315381021533,-11.5664879117912));
#39040=CARTESIAN_POINT('Ctrl Pts',(-71.1364990449913,8.56928494206896,-11.6472812828309));
#39041=CARTESIAN_POINT('Ctrl Pts',(-71.0091819466483,8.5538952244241,-11.7260192601636));
#39042=CARTESIAN_POINT('Ctrl Pts',(-70.8806724029974,8.53650122260619,-11.8027469173222));
#39043=CARTESIAN_POINT('Ctrl Pts',(-70.8660800072997,8.53452611515439,-11.8114594245991));
#39044=CARTESIAN_POINT('Ctrl Pts',(-70.85147221969,8.53252511247036,-11.8201459985682));
#39045=CARTESIAN_POINT('Ctrl Pts',(-70.8368485139656,8.53049746366489,-11.8288066959609));
#39046=CARTESIAN_POINT('Ctrl Pts',(-70.8017234668938,8.5256272029335,-11.8496090431446));
#39047=CARTESIAN_POINT('Ctrl Pts',(-70.7665066081501,8.52060323625991,-11.8702621150382));
#39048=CARTESIAN_POINT('Ctrl Pts',(-70.7311906833193,8.51541564895962,-11.8907668872392));
#39049=CARTESIAN_POINT('Ctrl Pts',(-70.7302019192612,8.51527040853634,-11.8913409733454));
#39050=CARTESIAN_POINT('Ctrl Pts',(-70.7292130176079,8.51512517529256,-11.8919155266462));
#39051=CARTESIAN_POINT('Ctrl Pts',(-70.7282239782404,8.51497994858646,-11.8924905441709));
#39052=CARTESIAN_POINT('',(-57.8135230789085,6.69056632342548,-18.0349157105246));
#39053=CARTESIAN_POINT('Ctrl Pts',(-70.7282577522101,8.51486331985853,-11.892519184563));
#39054=CARTESIAN_POINT('Ctrl Pts',(-70.1991067619348,8.44172633189886,-12.218539623772));
#39055=CARTESIAN_POINT('Ctrl Pts',(-68.595429397507,8.158930957405,-13.1757731414385));
#39056=CARTESIAN_POINT('Ctrl Pts',(-66.4080850486133,7.61830551402404,-14.5220628619485));
#39057=CARTESIAN_POINT('Ctrl Pts',(-63.7670026279933,7.28205441226018,-15.9847718406443));
#39058=CARTESIAN_POINT('Ctrl Pts',(-61.8892806965024,7.15471518367529,-16.8453028714865));
#39059=CARTESIAN_POINT('Ctrl Pts',(-59.9765401917668,7.00460230079879,-17.5365065043827));
#39060=CARTESIAN_POINT('Ctrl Pts',(-58.5497235666632,6.81245518627654,-17.8884040415039));
#39061=CARTESIAN_POINT('Ctrl Pts',(-57.8135230790975,6.69056632259502,-18.0349157107833));
#39062=CARTESIAN_POINT('',(-44.8643748761871,5.20597739865049,-23.9801519720622));
#39063=CARTESIAN_POINT('Ctrl Pts',(-57.8135230790975,6.69056632259502,-18.0349157107833));
#39064=CARTESIAN_POINT('Ctrl Pts',(-57.1239745403965,6.58412560248485,-18.1969381440623));
#39065=CARTESIAN_POINT('Ctrl Pts',(-55.0066008221098,6.23208146801642,-18.6635552175992));
#39066=CARTESIAN_POINT('Ctrl Pts',(-52.3438248091449,5.73435620824511,-19.2638310488358));
#39067=CARTESIAN_POINT('Ctrl Pts',(-50.0095424054025,5.30085549787886,-20.220604371564));
#39068=CARTESIAN_POINT('Ctrl Pts',(-48.2669654993335,5.10361702097977,-21.2264548583875));
#39069=CARTESIAN_POINT('Ctrl Pts',(-46.9594441235353,5.13430758608674,-22.1958151860038));
#39070=CARTESIAN_POINT('Ctrl Pts',(-45.8504881283735,5.21184561373662,-23.1088853518396));
#39071=CARTESIAN_POINT('Ctrl Pts',(-45.2012130342128,5.23387305606066,-23.6826188427425));
#39072=CARTESIAN_POINT('Ctrl Pts',(-44.8643748763769,5.20597739807172,-23.9801519722228));
#39073=CARTESIAN_POINT('',(-41.4215456143024,4.68791021227308,-29.7512571116587));
#39074=CARTESIAN_POINT('Ctrl Pts',(-44.8643748763769,5.20597739807172,-23.9801519722228));
#39075=CARTESIAN_POINT('Ctrl Pts',(-44.74295142856,5.19893273360771,-24.0982573983942));
#39076=CARTESIAN_POINT('Ctrl Pts',(-44.4866987396665,5.17768472779144,-24.3599634571171));
#39077=CARTESIAN_POINT('Ctrl Pts',(-43.7774989443756,5.08577719072335,-25.1469769549528));
#39078=CARTESIAN_POINT('Ctrl Pts',(-42.7956488003254,4.84372654876611,-26.5306371507459));
#39079=CARTESIAN_POINT('Ctrl Pts',(-41.9333999007591,4.68167633313014,-28.2389876838209));
#39080=CARTESIAN_POINT('Ctrl Pts',(-41.5686373679341,4.67844271843895,-29.2605708183325));
#39081=CARTESIAN_POINT('Ctrl Pts',(-41.4215456143024,4.68791021227308,-29.7512571116587));
#39082=CARTESIAN_POINT('',(-40.1355627918321,4.76730435132371,-35.6660886995316));
#39083=CARTESIAN_POINT('Ctrl Pts',(-41.4215456143025,4.68791021227309,-29.7512571116587));
#39084=CARTESIAN_POINT('Ctrl Pts',(-41.3092811227302,4.69284109397027,-30.1101403746882));
#39085=CARTESIAN_POINT('Ctrl Pts',(-41.1168122255416,4.70227545160565,-30.8154015426932));
#39086=CARTESIAN_POINT('Ctrl Pts',(-40.9411342639833,4.71057860533754,-31.5583878958659));
#39087=CARTESIAN_POINT('Ctrl Pts',(-40.72104027405,4.72052127144792,-32.5727429381947));
#39088=CARTESIAN_POINT('Ctrl Pts',(-40.5142429668683,4.72897579183149,-33.638548551572));
#39089=CARTESIAN_POINT('Ctrl Pts',(-40.3021090297733,4.74530128710119,-34.7695223916763));
#39090=CARTESIAN_POINT('Ctrl Pts',(-40.197670469322,4.75763956421394,-35.3320435682359));
#39091=CARTESIAN_POINT('Ctrl Pts',(-40.1355627919428,4.76730435097372,-35.6660886995623));
#39092=CARTESIAN_POINT('',(-38.8604541099244,4.82976572790842,-41.6539325852781));
#39093=CARTESIAN_POINT('Ctrl Pts',(-40.1355627919428,4.76730435097372,-35.6660886995623));
#39094=CARTESIAN_POINT('Ctrl Pts',(-40.0697893952873,4.77667332555081,-36.0099787209928));
#39095=CARTESIAN_POINT('Ctrl Pts',(-39.9548407119179,4.79179800913514,-36.603881143725));
#39096=CARTESIAN_POINT('Ctrl Pts',(-39.7443037262004,4.81133016772462,-37.6330866698068));
#39097=CARTESIAN_POINT('Ctrl Pts',(-39.5813565519597,4.82173156565819,-38.3962454196463));
#39098=CARTESIAN_POINT('Ctrl Pts',(-39.4305411403599,4.82773783061676,-39.0811836979273));
#39099=CARTESIAN_POINT('Ctrl Pts',(-39.2609912818215,4.83170251246378,-39.8388585382037));
#39100=CARTESIAN_POINT('Ctrl Pts',(-39.0664822089796,4.83206157401462,-40.699884114134));
#39101=CARTESIAN_POINT('Ctrl Pts',(-38.9270116850831,4.83045996119414,-41.3378025229821));
#39102=CARTESIAN_POINT('Ctrl Pts',(-38.8604541099244,4.82976572790842,-41.6539325852781));
#39103=CARTESIAN_POINT('',(-38.0224643186749,4.86842248838796,-47.6590907843941));
#39104=CARTESIAN_POINT('Ctrl Pts',(-38.8604525038006,4.82977022535046,-41.6539322549122));
#39105=CARTESIAN_POINT('Ctrl Pts',(-38.7895469391281,4.82895050845352,-41.9867860224295));
#39106=CARTESIAN_POINT('Ctrl Pts',(-38.7233060696144,4.82752930432473,-42.3153012863669));
#39107=CARTESIAN_POINT('Ctrl Pts',(-38.6000287997093,4.82483865752222,-42.9730936841352));
#39108=CARTESIAN_POINT('Ctrl Pts',(-38.5399565866358,4.8233804990704,-43.3171996550799));
#39109=CARTESIAN_POINT('Ctrl Pts',(-38.4516802292394,4.82286779338988,-43.8813591795731));
#39110=CARTESIAN_POINT('Ctrl Pts',(-38.4197926585925,4.82326787763993,-44.1037768924137));
#39111=CARTESIAN_POINT('Ctrl Pts',(-38.2254488332384,4.82915172129242,-45.5525914827238));
#39112=CARTESIAN_POINT('Ctrl Pts',(-38.1374175968506,4.85081367644718,-46.6695328022788));
#39113=CARTESIAN_POINT('Ctrl Pts',(-38.0216341588543,4.87047774970745,-47.6589526062877));
#39114=CARTESIAN_POINT('',(-36.1829138277439,4.79791400485576,-53.6562428681641));
#39115=CARTESIAN_POINT('Ctrl Pts',(-38.0224643186749,4.86842248838796,-47.6590907843941));
#39116=CARTESIAN_POINT('Ctrl Pts',(-37.9812657358155,4.87623123772776,-48.0222701187376));
#39117=CARTESIAN_POINT('Ctrl Pts',(-37.8390083119489,4.91385101443275,-49.095218604347));
#39118=CARTESIAN_POINT('Ctrl Pts',(-37.4172837879437,4.97200393690399,-51.0816259402684));
#39119=CARTESIAN_POINT('Ctrl Pts',(-36.8018062134426,4.93958207757202,-52.5177243515675));
#39120=CARTESIAN_POINT('Ctrl Pts',(-36.1829138277439,4.79791400485575,-53.6562428681641));
#39121=CARTESIAN_POINT('',(-33.2870419059708,4.35253527752949,-59.9326413363873));
#39122=CARTESIAN_POINT('Ctrl Pts',(-36.1829138277439,4.79791400485575,-53.6562428681641));
#39123=CARTESIAN_POINT('Ctrl Pts',(-35.8221894292354,4.71279832802143,-54.2735126527001));
#39124=CARTESIAN_POINT('Ctrl Pts',(-35.1345762789437,4.46191327643785,-55.4630423598499));
#39125=CARTESIAN_POINT('Ctrl Pts',(-34.1112888063175,4.18758073788383,-57.6561452037581));
#39126=CARTESIAN_POINT('Ctrl Pts',(-33.5340571648804,4.24789457701618,-59.2008344761412));
#39127=CARTESIAN_POINT('Ctrl Pts',(-33.2870419060249,4.35253527707242,-59.9326413364709));
#39128=CARTESIAN_POINT('',(-30.3753540341099,6.01695723880277,-66.3794227429406));
#39129=CARTESIAN_POINT('Ctrl Pts',(-33.2870419060249,4.35253527707242,-59.9326413364709));
#39130=CARTESIAN_POINT('Ctrl Pts',(-33.1236843979303,4.41327697339383,-60.3703598245789));
#39131=CARTESIAN_POINT('Ctrl Pts',(-32.6598069524929,4.6233160195265,-61.6572795724073));
#39132=CARTESIAN_POINT('Ctrl Pts',(-31.725539611122,5.1629429740609,-64.061279077029));
#39133=CARTESIAN_POINT('Ctrl Pts',(-30.929578969617,5.6097190919677,-65.4015789370632));
#39134=CARTESIAN_POINT('Ctrl Pts',(-30.3753540341099,6.01695723880277,-66.3794227429406));
#39135=CARTESIAN_POINT('',(-27.8032099026791,9.23603570625527,-72.5577783044281));
#39136=CARTESIAN_POINT('Ctrl Pts',(-30.3753540341099,6.01695723880277,-66.3794227429406));
#39137=CARTESIAN_POINT('Ctrl Pts',(-30.1088133612586,6.21732189962616,-66.8603832394881));
#39138=CARTESIAN_POINT('Ctrl Pts',(-29.7096580135423,6.55735136704459,-67.5873569901587));
#39139=CARTESIAN_POINT('Ctrl Pts',(-28.7821722057447,7.57574471691707,-69.5467552476757));
#39140=CARTESIAN_POINT('Ctrl Pts',(-28.2846186462697,8.42885715791647,-71.0332031632364));
#39141=CARTESIAN_POINT('Ctrl Pts',(-27.8032099026791,9.23603570625527,-72.5577783044281));
#39142=CARTESIAN_POINT('',(-25.9521939426092,12.4413262855032,-78.5797190178297));
#39143=CARTESIAN_POINT('Ctrl Pts',(-27.8032099155366,9.23604325175907,-72.5577743135822));
#39144=CARTESIAN_POINT('Ctrl Pts',(-27.7898641356696,9.25902028195003,-72.6011740541424));
#39145=CARTESIAN_POINT('Ctrl Pts',(-27.7716651061686,9.29043033079141,-72.6604932145904));
#39146=CARTESIAN_POINT('Ctrl Pts',(-27.7311843931623,9.36074589208966,-72.7932093170237));
#39147=CARTESIAN_POINT('Ctrl Pts',(-27.7131022311491,9.39228751256304,-72.8527202187813));
#39148=CARTESIAN_POINT('Ctrl Pts',(-27.6591706521313,9.48670680637636,-73.0308045499805));
#39149=CARTESIAN_POINT('Ctrl Pts',(-27.6233481930299,9.54988119753572,-73.1498763380756));
#39150=CARTESIAN_POINT('Ctrl Pts',(-27.5171321758154,9.73818724164291,-73.5045914452129));
#39151=CARTESIAN_POINT('Ctrl Pts',(-27.4454683323948,9.86657180310599,-73.7461526383459));
#39152=CARTESIAN_POINT('Ctrl Pts',(-27.2390203345148,10.2379066566848,-74.4442925145932));
#39153=CARTESIAN_POINT('Ctrl Pts',(-27.0994468304465,10.4909718054446,-74.9193670196221));
#39154=CARTESIAN_POINT('Ctrl Pts',(-26.7946207936278,11.0357645089441,-75.9416399738098));
#39155=CARTESIAN_POINT('Ctrl Pts',(-26.6360619980652,11.314717467905,-76.4648390599111));
#39156=CARTESIAN_POINT('Ctrl Pts',(-26.3050671814268,11.8772403762864,-77.5203681238995));
#39157=CARTESIAN_POINT('Ctrl Pts',(-26.1315729170005,12.1624636612076,-78.0558078244091));
#39158=CARTESIAN_POINT('Ctrl Pts',(-25.9521939426143,12.4413262860545,-78.5797190175208));
#39159=CARTESIAN_POINT('',(-25.701333505378,12.8213469096823,-79.2936899992609));
#39160=CARTESIAN_POINT('Ctrl Pts',(-25.9521939426076,12.4413262858927,-78.5797190176306));
#39161=CARTESIAN_POINT('Ctrl Pts',(-25.8694938500183,12.5699781302287,-78.8214229331902));
#39162=CARTESIAN_POINT('Ctrl Pts',(-25.7858492981987,12.6969136284318,-79.0599051073278));
#39163=CARTESIAN_POINT('Ctrl Pts',(-25.7013798878604,12.8212786209475,-79.2935616983239));
#39164=CARTESIAN_POINT('',(-20.8093218985896,12.6047452125772,-78.8857087163453));
#39165=CARTESIAN_POINT('Ctrl Pts',(-25.7013238054811,12.8213611907999,-79.2937168306377));
#39166=CARTESIAN_POINT('Ctrl Pts',(-25.677759723027,12.9497254061923,-79.5350654335173));
#39167=CARTESIAN_POINT('Ctrl Pts',(-25.6134596233024,13.054467242967,-79.731873404679));
#39168=CARTESIAN_POINT('Ctrl Pts',(-25.4062110463656,13.2656356021316,-80.128476351569));
#39169=CARTESIAN_POINT('Ctrl Pts',(-25.2498435162777,13.350811855551,-80.2882896491754));
#39170=CARTESIAN_POINT('Ctrl Pts',(-24.9061202849933,13.4995897428215,-80.5673656272477));
#39171=CARTESIAN_POINT('Ctrl Pts',(-24.6468918170405,13.5747625375941,-80.7082619530755));
#39172=CARTESIAN_POINT('Ctrl Pts',(-23.9892905759402,13.6953664711755,-80.9343907983184));
#39173=CARTESIAN_POINT('Ctrl Pts',(-23.4919735177951,13.7506233016025,-81.038109384192));
#39174=CARTESIAN_POINT('Ctrl Pts',(-22.5135030627148,13.7417998945799,-81.0220713233488));
#39175=CARTESIAN_POINT('Ctrl Pts',(-22.1753683303654,13.7101025139875,-80.9628345173954));
#39176=CARTESIAN_POINT('Ctrl Pts',(-21.6613306788478,13.620361236039,-80.7946514359959));
#39177=CARTESIAN_POINT('Ctrl Pts',(-21.4654769001396,13.5650100503355,-80.6908083589357));
#39178=CARTESIAN_POINT('Ctrl Pts',(-21.1272843829631,13.4213387174777,-80.4210520847113));
#39179=CARTESIAN_POINT('Ctrl Pts',(-21.0209737284345,13.3421252329789,-80.2722205693931));
#39180=CARTESIAN_POINT('Ctrl Pts',(-20.8884830981335,13.209475077092,-80.0229241692315));
#39181=CARTESIAN_POINT('Ctrl Pts',(-20.8159402909792,13.1168800297615,-79.8488783976986));
#39182=CARTESIAN_POINT('Ctrl Pts',(-20.7555355063041,12.8585107795136,-79.3630420047952));
#39183=CARTESIAN_POINT('Ctrl Pts',(-20.7713716558706,12.7296582669527,-79.1206857196503));
#39184=CARTESIAN_POINT('Ctrl Pts',(-20.8093218984874,12.6047452132069,-78.8857087160435));
#39185=CARTESIAN_POINT('',(-21.0431040492689,12.4421761536719,-78.5796470221002));
#39186=CARTESIAN_POINT('Ctrl Pts',(-20.8093218987925,12.6047452131661,-78.8857087159663));
#39187=CARTESIAN_POINT('Ctrl Pts',(-20.8889387478986,12.5521187796536,-78.7866255044787));
#39188=CARTESIAN_POINT('Ctrl Pts',(-20.9668291889875,12.4978886120539,-78.6845286315191));
#39189=CARTESIAN_POINT('Ctrl Pts',(-21.043057427238,12.4422102065963,-78.5797111314019));
#39190=CARTESIAN_POINT('',(-23.6734819284684,9.24326495192996,-72.5612011682817));
#39191=CARTESIAN_POINT('Ctrl Pts',(-21.0431231485117,12.4421622035058,-78.5796207589988));
#39192=CARTESIAN_POINT('Ctrl Pts',(-21.1180479364394,12.3874344879029,-78.4765929841646));
#39193=CARTESIAN_POINT('Ctrl Pts',(-21.1912719403466,12.3312721447608,-78.3708704737982));
#39194=CARTESIAN_POINT('Ctrl Pts',(-21.2629202654535,12.2738551841641,-78.2627919303907));
#39195=CARTESIAN_POINT('Ctrl Pts',(-21.3432015307692,12.2095200271257,-78.1416909527295));
#39196=CARTESIAN_POINT('Ctrl Pts',(-21.4215050496884,12.143609457215,-78.0176315203387));
#39197=CARTESIAN_POINT('Ctrl Pts',(-21.4979790544219,12.0763456889671,-77.8910318283258));
#39198=CARTESIAN_POINT('Ctrl Pts',(-21.565187494861,12.0172315759066,-77.7797709117582));
#39199=CARTESIAN_POINT('Ctrl Pts',(-21.630982480635,11.9570714261746,-77.6665463444693));
#39200=CARTESIAN_POINT('Ctrl Pts',(-21.6954456408304,11.8960034591588,-77.5516183175351));
#39201=CARTESIAN_POINT('Ctrl Pts',(-21.7623500478192,11.8326228227331,-77.4323379182326));
#39202=CARTESIAN_POINT('Ctrl Pts',(-21.82799276352,11.7680944969581,-77.310902619301));
#39203=CARTESIAN_POINT('Ctrl Pts',(-21.8921956945099,11.7028022397038,-77.1880352793384));
#39204=CARTESIAN_POINT('Ctrl Pts',(-21.9142041224075,11.680420396478,-77.1459169998324));
#39205=CARTESIAN_POINT('Ctrl Pts',(-21.9360435805853,11.6579489835836,-77.1036308166521));
#39206=CARTESIAN_POINT('Ctrl Pts',(-21.957707579971,11.6354040017278,-77.0612068658632));
#39207=CARTESIAN_POINT('Ctrl Pts',(-22.0297903066051,11.5603899779938,-76.9200494556811));
#39208=CARTESIAN_POINT('Ctrl Pts',(-22.099927047318,11.4845606008049,-76.7773651932802));
#39209=CARTESIAN_POINT('Ctrl Pts',(-22.1682847108296,11.4079311890524,-76.6331838251872));
#39210=CARTESIAN_POINT('Ctrl Pts',(-22.2206631919412,11.3492145508602,-76.5227060721842));
#39211=CARTESIAN_POINT('Ctrl Pts',(-22.2719983650367,11.2900282995873,-76.411349529747));
#39212=CARTESIAN_POINT('Ctrl Pts',(-22.3223795367015,11.2303864433944,-76.2991408990849));
#39213=CARTESIAN_POINT('Ctrl Pts',(-22.3765225385033,11.166291286005,-76.1785539438521));
#39214=CARTESIAN_POINT('Ctrl Pts',(-22.4294720817398,11.1017772920471,-76.0571848686692));
#39215=CARTESIAN_POINT('Ctrl Pts',(-22.4812879554131,11.0369702725863,-75.9352703929272));
#39216=CARTESIAN_POINT('Ctrl Pts',(-22.5008207932577,11.0125402106655,-75.8893127448791));
#39217=CARTESIAN_POINT('Ctrl Pts',(-22.5201926240654,10.9880687491465,-75.8432780440593));
#39218=CARTESIAN_POINT('Ctrl Pts',(-22.5394068429119,10.9635635598301,-75.7971807191217));
#39219=CARTESIAN_POINT('Ctrl Pts',(-22.5437545941372,10.9580185794316,-75.7867499177145));
#39220=CARTESIAN_POINT('Ctrl Pts',(-22.5480942753898,10.9524718743525,-75.7763159140468));
#39221=CARTESIAN_POINT('Ctrl Pts',(-22.5524259259098,10.9469235374562,-75.7658788827482));
#39222=CARTESIAN_POINT('Ctrl Pts',(-22.5561213420508,10.9421901422692,-75.7569748463429));
#39223=CARTESIAN_POINT('Ctrl Pts',(-22.5598105984477,10.9374559716686,-75.7480693818334));
#39224=CARTESIAN_POINT('Ctrl Pts',(-22.5634994289947,10.9327137217901,-75.7391487499829));
#39225=CARTESIAN_POINT('Ctrl Pts',(-22.5824755837965,10.9083185465013,-75.6932590598033));
#39226=CARTESIAN_POINT('Ctrl Pts',(-22.6014048462052,10.8837550175016,-75.6470534899443));
#39227=CARTESIAN_POINT('Ctrl Pts',(-22.6202838428499,10.8590326983467,-75.6005500503436));
#39228=CARTESIAN_POINT('Ctrl Pts',(-22.6320499157315,10.8436248557345,-75.5715674264319));
#39229=CARTESIAN_POINT('Ctrl Pts',(-22.6437961517736,10.8281557605298,-75.5424699027608));
#39230=CARTESIAN_POINT('Ctrl Pts',(-22.6555194494533,10.8126310685817,-75.5132681220383));
#39231=CARTESIAN_POINT('Ctrl Pts',(-22.6738690250963,10.7883314630426,-75.4675608220178));
#39232=CARTESIAN_POINT('Ctrl Pts',(-22.6921652750908,10.7638918850865,-75.4215910187751));
#39233=CARTESIAN_POINT('Ctrl Pts',(-22.7104142012248,10.7393109564447,-75.3753561336587));
#39234=CARTESIAN_POINT('Ctrl Pts',(-22.7539775345839,10.6806320412672,-75.2649854905671));
#39235=CARTESIAN_POINT('Ctrl Pts',(-22.7972711094583,10.6211470908519,-75.1531032527699));
#39236=CARTESIAN_POINT('Ctrl Pts',(-22.8402166930606,10.5610049408755,-75.0399873237489));
#39237=CARTESIAN_POINT('Ctrl Pts',(-22.867492931559,10.5228065630923,-74.9681434506626));
#39238=CARTESIAN_POINT('Ctrl Pts',(-22.8946288307021,10.484343222191,-74.89580218923));
#39239=CARTESIAN_POINT('Ctrl Pts',(-22.9216048537358,10.4456543240943,-74.8230371235709));
#39240=CARTESIAN_POINT('Ctrl Pts',(-22.9418060954355,10.4166817887221,-74.7685463382969));
#39241=CARTESIAN_POINT('Ctrl Pts',(-22.9619206816493,10.3875785173637,-74.7138099023665));
#39242=CARTESIAN_POINT('Ctrl Pts',(-22.981943766366,10.3583563871592,-74.6588499300766));
#39243=CARTESIAN_POINT('Ctrl Pts',(-23.0439255439702,10.2678988177548,-74.4887204606268));
#39244=CARTESIAN_POINT('Ctrl Pts',(-23.1050288911212,10.1763036291092,-74.3164514897427));
#39245=CARTESIAN_POINT('Ctrl Pts',(-23.1650997057093,10.0839475808336,-74.1427449174312));
#39246=CARTESIAN_POINT('Ctrl Pts',(-23.2188715201287,10.0012759486535,-73.9872531427013));
#39247=CARTESIAN_POINT('Ctrl Pts',(-23.2718178159678,9.91799184453354,-73.8306041553568));
#39248=CARTESIAN_POINT('Ctrl Pts',(-23.3238195434587,9.83438895875108,-73.6733455075521));
#39249=CARTESIAN_POINT('Ctrl Pts',(-23.3543891421507,9.78524238629715,-73.5808998526444));
#39250=CARTESIAN_POINT('Ctrl Pts',(-23.3846322346305,9.73598600952977,-73.4882441891714));
#39251=CARTESIAN_POINT('Ctrl Pts',(-23.4145252260723,9.68668036351007,-73.3954914020482));
#39252=CARTESIAN_POINT('Ctrl Pts',(-23.4370059800081,9.64960049821896,-73.3257375071183));
#39253=CARTESIAN_POINT('Ctrl Pts',(-23.4592874913637,9.61249489713648,-73.2559326884176));
#39254=CARTESIAN_POINT('Ctrl Pts',(-23.4813656216018,9.57537981682306,-73.186107108416));
#39255=CARTESIAN_POINT('Ctrl Pts',(-23.4978643016036,9.54764423293412,-73.1339274225477));
#39256=CARTESIAN_POINT('Ctrl Pts',(-23.5142498889896,9.51990254705391,-73.0817346219641));
#39257=CARTESIAN_POINT('Ctrl Pts',(-23.5305218647511,9.49215930247276,-73.0295370768705));
#39258=CARTESIAN_POINT('Ctrl Pts',(-23.5427177420063,9.47136568708553,-72.9904149160266));
#39259=CARTESIAN_POINT('Ctrl Pts',(-23.5548501855968,9.45057052225198,-72.9512888220383));
#39260=CARTESIAN_POINT('Ctrl Pts',(-23.5669176669966,9.42977789958617,-72.9121664177397));
#39261=CARTESIAN_POINT('Ctrl Pts',(-23.6031521881662,9.36734476203297,-72.7946952122912));
#39262=CARTESIAN_POINT('Ctrl Pts',(-23.6387828450897,9.30496036670618,-72.6773057886921));
#39263=CARTESIAN_POINT('Ctrl Pts',(-23.6734819284684,9.24326495192996,-72.5612011682817));
#39264=CARTESIAN_POINT('',(-24.8514914924163,6.0392731730085,-66.5176718854411));
#39265=CARTESIAN_POINT('Ctrl Pts',(-23.6734819284749,9.24326495191836,-72.5612011682599));
#39266=CARTESIAN_POINT('Ctrl Pts',(-23.7649042668809,9.0816244028814,-72.257009894464));
#39267=CARTESIAN_POINT('Ctrl Pts',(-24.026191926212,8.5949110125477,-71.3440354252429));
#39268=CARTESIAN_POINT('Ctrl Pts',(-24.3676733444401,7.85042242107576,-69.9555629639005));
#39269=CARTESIAN_POINT('Ctrl Pts',(-24.6786062061593,6.94797749971677,-68.2666525661597));
#39270=CARTESIAN_POINT('Ctrl Pts',(-24.8079585801581,6.32785027214234,-67.080190599109));
#39271=CARTESIAN_POINT('Ctrl Pts',(-24.8514914924163,6.0392731730085,-66.5176718854411));
#39272=CARTESIAN_POINT('',(-24.7799130650367,2.95812473554076,-60.3565443657526));
#39273=CARTESIAN_POINT('Ctrl Pts',(-24.8514914924163,6.0392731730085,-66.5176718854411));
#39274=CARTESIAN_POINT('Ctrl Pts',(-24.9519006567039,5.4000946661346,-65.2716949090004));
#39275=CARTESIAN_POINT('Ctrl Pts',(-24.9551931519226,4.48977772329943,-63.5721308413706));
#39276=CARTESIAN_POINT('Ctrl Pts',(-24.9193282160013,4.02246798717194,-62.6314379535427));
#39277=CARTESIAN_POINT('Ctrl Pts',(-24.9088241241943,3.89449030749864,-62.3747837256354));
#39278=CARTESIAN_POINT('Ctrl Pts',(-24.9003852832803,3.80179791434547,-62.1865158010774));
#39279=CARTESIAN_POINT('Ctrl Pts',(-24.8848681816847,3.64819007810987,-61.8717738157264));
#39280=CARTESIAN_POINT('Ctrl Pts',(-24.8483424703915,3.34834435316993,-61.2421934759334));
#39281=CARTESIAN_POINT('Ctrl Pts',(-24.8095511279375,3.11147085333639,-60.7161135136638));
#39282=CARTESIAN_POINT('Ctrl Pts',(-24.7799130650367,2.95812473554075,-60.3565443657526));
#39283=CARTESIAN_POINT('',(-23.8932421744747,0.740634811882228,-53.9986859556407));
#39284=CARTESIAN_POINT('Ctrl Pts',(-24.7799130650367,2.95812473554076,-60.3565443657526));
#39285=CARTESIAN_POINT('Ctrl Pts',(-24.7093254167293,2.61894304809241,-59.562121477931));
#39286=CARTESIAN_POINT('Ctrl Pts',(-24.5694830832048,2.04316650995158,-58.1763047923767));
#39287=CARTESIAN_POINT('Ctrl Pts',(-24.3518230181499,1.42202438632593,-56.4243962709067));
#39288=CARTESIAN_POINT('Ctrl Pts',(-24.1714172775178,1.07110956737089,-55.2893749713734));
#39289=CARTESIAN_POINT('Ctrl Pts',(-24.0036588764749,0.844289079598309,
-54.4481403827476));
#39290=CARTESIAN_POINT('Ctrl Pts',(-23.8932421744747,0.740634811882228,
-53.9986859556407));
#39291=CARTESIAN_POINT('',(-18.0841506639546,0.0170011460072001,-47.6824918097827));
#39292=CARTESIAN_POINT('Ctrl Pts',(-23.8932550579139,0.73992114273642,-53.9988467607157));
#39293=CARTESIAN_POINT('Ctrl Pts',(-23.865369025631,0.713604674760589,-53.8843295077257));
#39294=CARTESIAN_POINT('Ctrl Pts',(-23.8354617846255,0.68786774595474,-53.767717765413));
#39295=CARTESIAN_POINT('Ctrl Pts',(-23.8035406699943,0.662904079149062,
-53.6495820580012));
#39296=CARTESIAN_POINT('Ctrl Pts',(-23.7715750315953,0.637905592866783,
-53.5312815741754));
#39297=CARTESIAN_POINT('Ctrl Pts',(-23.7375902175562,0.613682667000672,
-53.4114530424051));
#39298=CARTESIAN_POINT('Ctrl Pts',(-23.7016079266509,0.590379285496312,
-53.2906700249736));
#39299=CARTESIAN_POINT('Ctrl Pts',(-23.6677194403066,0.568431924558008,
-53.1769153547216));
#39300=CARTESIAN_POINT('Ctrl Pts',(-23.6320595820234,0.547299755878345,
-53.0623142112197));
#39301=CARTESIAN_POINT('Ctrl Pts',(-23.5946537465948,0.527061396986049,
-52.9473439087602));
#39302=CARTESIAN_POINT('Ctrl Pts',(-23.5472816563339,0.501430814132001,
-52.8017413982689));
#39303=CARTESIAN_POINT('Ctrl Pts',(-23.4971096480315,0.477224946459548,
-52.6555051471916));
#39304=CARTESIAN_POINT('Ctrl Pts',(-23.4435698220804,0.454449330017018,
-52.5090750461682));
#39305=CARTESIAN_POINT('Ctrl Pts',(-23.425065721271,0.44657776347449,-52.4584667876851));
#39306=CARTESIAN_POINT('Ctrl Pts',(-23.4061595713412,0.438876645481701,
-52.4078353903899));
#39307=CARTESIAN_POINT('Ctrl Pts',(-23.3868286107285,0.431344925720856,
-52.3571990316685));
#39308=CARTESIAN_POINT('Ctrl Pts',(-23.3310171351507,0.409599684917134,
-52.2110040259085));
#39309=CARTESIAN_POINT('Ctrl Pts',(-23.2716636289628,0.389270140173637,
-52.064768000871));
#39310=CARTESIAN_POINT('Ctrl Pts',(-23.2082281614495,0.370301554837552,
-51.9188967633294));
#39311=CARTESIAN_POINT('Ctrl Pts',(-23.1457449149932,0.351617704320727,
-51.7752151788231));
#39312=CARTESIAN_POINT('Ctrl Pts',(-23.0793024602032,0.334254343966579,
-51.6318879227277));
#39313=CARTESIAN_POINT('Ctrl Pts',(-23.0083890530461,0.318110160841051,
-51.4892953868701));
#39314=CARTESIAN_POINT('Ctrl Pts',(-22.9415774480444,0.302899796125833,
-51.3549507465004));
#39315=CARTESIAN_POINT('Ctrl Pts',(-22.8707983153925,0.288771253646912,
-51.2212586648078));
#39316=CARTESIAN_POINT('Ctrl Pts',(-22.7956110574691,0.275598830743189,
-51.0885250594739));
#39317=CARTESIAN_POINT('Ctrl Pts',(-22.7475861174807,0.267185106969701,
-51.0037430949938));
#39318=CARTESIAN_POINT('Ctrl Pts',(-22.6977624520621,0.259160652050131,
-50.919351922552));
#39319=CARTESIAN_POINT('Ctrl Pts',(-22.6460187082459,0.251484345223507,
-50.8354272526696));
#39320=CARTESIAN_POINT('Ctrl Pts',(-22.6384330035932,0.250358987989642,
-50.8231237795952));
#39321=CARTESIAN_POINT('Ctrl Pts',(-22.6308060202752,0.249241101953243,
-50.8108303258452));
#39322=CARTESIAN_POINT('Ctrl Pts',(-22.6231373508233,0.248130568613676,
-50.7985471282056));
#39323=CARTESIAN_POINT('Ctrl Pts',(-22.6136841630144,0.246761611418079,
-50.7834056000817));
#39324=CARTESIAN_POINT('Ctrl Pts',(-22.60416746881,0.245403845777488,-50.7682798097095));
#39325=CARTESIAN_POINT('Ctrl Pts',(-22.5945866051412,0.244057158520407,
-50.75317136449));
#39326=CARTESIAN_POINT('Ctrl Pts',(-22.520830673283,0.233690016579786,-50.6368627001968));
#39327=CARTESIAN_POINT('Ctrl Pts',(-22.4432747299908,0.223981871840293,
-50.5215841488338));
#39328=CARTESIAN_POINT('Ctrl Pts',(-22.3615976638741,0.214866063520751,
-50.4080728596082));
#39329=CARTESIAN_POINT('Ctrl Pts',(-22.2778491054295,0.205519060229424,
-50.2916826990428));
#39330=CARTESIAN_POINT('Ctrl Pts',(-22.1897679291785,0.196793847772579,
-50.1771509867835));
#39331=CARTESIAN_POINT('Ctrl Pts',(-22.0969687417925,0.188595152285034,
-50.0652405302303));
#39332=CARTESIAN_POINT('Ctrl Pts',(-22.0208828689396,0.181873057835754,
-49.9734853650389));
#39333=CARTESIAN_POINT('Ctrl Pts',(-21.9416245491178,0.175504160748907,
-49.8834916975784));
#39334=CARTESIAN_POINT('Ctrl Pts',(-21.8589623507553,0.169432268974329,
-49.7956624028172));
#39335=CARTESIAN_POINT('Ctrl Pts',(-21.7652606973502,0.162549482043352,
-49.6961035923867));
#39336=CARTESIAN_POINT('Ctrl Pts',(-21.6671931181628,0.156046312566252,
-49.5993256138718));
#39337=CARTESIAN_POINT('Ctrl Pts',(-21.5655469854621,0.149823557003932,
-49.5057302780702));
#39338=CARTESIAN_POINT('Ctrl Pts',(-21.458001267195,0.143239630013606,-49.4067026284412));
#39339=CARTESIAN_POINT('Ctrl Pts',(-21.3464479140259,0.13696833417058,-49.3112370218204));
#39340=CARTESIAN_POINT('Ctrl Pts',(-21.2317882308461,0.130930860823799,
-49.2197844474539));
#39341=CARTESIAN_POINT('Ctrl Pts',(-21.2244571308433,0.130544837422701,
-49.2139371613844));
#39342=CARTESIAN_POINT('Ctrl Pts',(-21.2171133271496,0.130159785938529,
-49.2081062754909));
#39343=CARTESIAN_POINT('Ctrl Pts',(-21.2097570538576,0.129775692478805,
-49.2022919057832));
#39344=CARTESIAN_POINT('Ctrl Pts',(-21.0990434606392,0.123994998183015,
-49.1147843136807));
#39345=CARTESIAN_POINT('Ctrl Pts',(-20.9855047073545,0.118427639898545,
-49.0310147540628));
#39346=CARTESIAN_POINT('Ctrl Pts',(-20.8699414509509,0.113046831612799,
-48.951329823701));
#39347=CARTESIAN_POINT('Ctrl Pts',(-20.7287606166067,0.106473228316489,
-48.8539806722214));
#39348=CARTESIAN_POINT('Ctrl Pts',(-20.584559314947,0.100188172347876,-48.7628237679712));
#39349=CARTESIAN_POINT('Ctrl Pts',(-20.4343295065461,0.0940004548219974,
-48.6755849178391));
#39350=CARTESIAN_POINT('Ctrl Pts',(-20.2980308949655,0.088386540269303,
-48.59643595083));
#39351=CARTESIAN_POINT('Ctrl Pts',(-20.1567727277326,0.0828531018242971,
-48.5205157941745));
#39352=CARTESIAN_POINT('Ctrl Pts',(-20.0083008190481,0.0772774204330494,
-48.4461313374821));
#39353=CARTESIAN_POINT('Ctrl Pts',(-19.9067948782763,0.0734654886671241,
-48.3952768403435));
#39354=CARTESIAN_POINT('Ctrl Pts',(-19.8019169633049,0.0696340466546913,
-48.3451415621776));
#39355=CARTESIAN_POINT('Ctrl Pts',(-19.6929361743208,0.0657592881968911,
-48.2952882858672));
#39356=CARTESIAN_POINT('Ctrl Pts',(-19.5621032696068,0.0611075884906894,
-48.235438756331));
#39357=CARTESIAN_POINT('Ctrl Pts',(-19.4254042690855,0.0563375063641562,
-48.1752852783097));
#39358=CARTESIAN_POINT('Ctrl Pts',(-19.2809513108291,0.0515296105362735,
-48.115343315774));
#39359=CARTESIAN_POINT('Ctrl Pts',(-19.2430868439431,0.0502693496557501,
-48.099631138724));
#39360=CARTESIAN_POINT('Ctrl Pts',(-19.2046894662233,0.0490066581924538,
-48.0839333380788));
#39361=CARTESIAN_POINT('Ctrl Pts',(-19.1657248392323,0.0477433954684069,
-48.068258869099));
#39362=CARTESIAN_POINT('Ctrl Pts',(-19.0876721514813,0.0452128682040143,
-48.0368602769034));
#39363=CARTESIAN_POINT('Ctrl Pts',(-19.0073434524589,0.0426798135396984,
-48.0055549360527));
#39364=CARTESIAN_POINT('Ctrl Pts',(-18.9244607930308,0.0401473901296877,
-47.9742150154492));
#39365=CARTESIAN_POINT('Ctrl Pts',(-18.7868979753429,0.0359442515930639,
-47.922199216076));
#39366=CARTESIAN_POINT('Ctrl Pts',(-18.6422965332993,0.0317435187318599,
-47.8700852781068));
#39367=CARTESIAN_POINT('Ctrl Pts',(-18.4894608715532,0.0275580329317178,
-47.8173980644618));
#39368=CARTESIAN_POINT('Ctrl Pts',(-18.3604557424757,0.0240251589301201,
-47.7729259777816));
#39369=CARTESIAN_POINT('Ctrl Pts',(-18.2255837584678,0.0205033034188778,
-47.728047397392));
#39370=CARTESIAN_POINT('Ctrl Pts',(-18.0841506697213,0.0170011623984622,
-47.6824917993401));
#39371=CARTESIAN_POINT('',(-1.26595091974945E-14,-0.0251265935465125,-45.4192972571095));
#39372=CARTESIAN_POINT('Ctrl Pts',(-18.0841506673754,0.017001162336854,
-47.682491798537));
#39373=CARTESIAN_POINT('Ctrl Pts',(-18.0828067270674,0.0169658686183399,
-47.6820317354795));
#39374=CARTESIAN_POINT('Ctrl Pts',(-18.0814621764952,0.0169305690162963,
-47.6815715039635));
#39375=CARTESIAN_POINT('Ctrl Pts',(-18.0801170157235,0.016895263522413,
-47.6811111034811));
#39376=CARTESIAN_POINT('Ctrl Pts',(-17.9371307597341,0.0131424032754297,
-47.6321720156008));
#39377=CARTESIAN_POINT('Ctrl Pts',(-17.7872420326831,0.00952942749988126,
-47.5826598841899));
#39378=CARTESIAN_POINT('Ctrl Pts',(-17.6305393229821,0.00611053317163838,
-47.5326793306452));
#39379=CARTESIAN_POINT('Ctrl Pts',(-17.4856634580748,0.0029496735172275,
-47.4864709661751));
#39380=CARTESIAN_POINT('Ctrl Pts',(-17.3349630466611,-4.50415560202498E-5,
-47.4398622491996));
#39381=CARTESIAN_POINT('Ctrl Pts',(-17.1785524330135,-0.00283268066233115,
-47.3929444476255));
#39382=CARTESIAN_POINT('Ctrl Pts',(-17.1295044874326,-0.00370684110449546,
-47.3782317518262));
#39383=CARTESIAN_POINT('Ctrl Pts',(-17.0798953942529,-0.00456066835218952,
-47.363488727926));
#39384=CARTESIAN_POINT('Ctrl Pts',(-17.0297297511583,-0.00539300427001911,
-47.3487183767908));
#39385=CARTESIAN_POINT('Ctrl Pts',(-16.8246964071324,-0.00879486670131436,
-47.2883500789106));
#39386=CARTESIAN_POINT('Ctrl Pts',(-16.6103659378757,-0.0118351451518027,
-47.2275230092626));
#39387=CARTESIAN_POINT('Ctrl Pts',(-16.3868922470239,-0.0144668416866325,
-47.1664370632235));
#39388=CARTESIAN_POINT('Ctrl Pts',(-16.2677193435885,-0.0158702593140994,
-47.1338614632913));
#39389=CARTESIAN_POINT('Ctrl Pts',(-16.1459464731934,-0.01715800953983,
-47.1012127290439));
#39390=CARTESIAN_POINT('Ctrl Pts',(-16.0215982073155,-0.0183278502655368,
-47.0685249337755));
#39391=CARTESIAN_POINT('Ctrl Pts',(-15.8252153036707,-0.0201753767822469,
-47.0169011808969));
#39392=CARTESIAN_POINT('Ctrl Pts',(-15.6224066945634,-0.0217256335218394,
-46.9651818010465));
#39393=CARTESIAN_POINT('Ctrl Pts',(-15.4151351031891,-0.0229904625177885,
-46.9138752345334));
#39394=CARTESIAN_POINT('Ctrl Pts',(-15.3369804296771,-0.0234673841092691,
-46.894529370837));
#39395=CARTESIAN_POINT('Ctrl Pts',(-15.2581911495873,-0.0239042040029462,
-46.8752424356118));
#39396=CARTESIAN_POINT('Ctrl Pts',(-15.1788721220257,-0.0243032761764485,
-46.856042448883));
#39397=CARTESIAN_POINT('Ctrl Pts',(-15.1625141020367,-0.024385577117243,
-46.8520828218382));
#39398=CARTESIAN_POINT('Ctrl Pts',(-15.1461335503751,-0.0244662757029685,
-46.8481268939813));
#39399=CARTESIAN_POINT('Ctrl Pts',(-15.1297313855253,-0.0245453974024568,
-46.8441749113411));
#39400=CARTESIAN_POINT('Ctrl Pts',(-14.9052849331823,-0.0256280950168327,
-46.7900961667706));
#39401=CARTESIAN_POINT('Ctrl Pts',(-14.6767937755882,-0.0264119003889579,
-46.7367551086416));
#39402=CARTESIAN_POINT('Ctrl Pts',(-14.4465981274285,-0.0269614391779066,
-46.684780205967));
#39403=CARTESIAN_POINT('Ctrl Pts',(-14.201003504354,-0.0275477394525454,
-46.629328433817));
#39404=CARTESIAN_POINT('Ctrl Pts',(-13.9534691875118,-0.0278679797972098,
-46.5754330516193));
#39405=CARTESIAN_POINT('Ctrl Pts',(-13.706799907371,-0.0280476913177893,
-46.523860833991));
#39406=CARTESIAN_POINT('Ctrl Pts',(-13.6210212488823,-0.0281101855738291,
-46.5059267173433));
#39407=CARTESIAN_POINT('Ctrl Pts',(-13.5353468539472,-0.0281560242974536,
-46.4882734661745));
#39408=CARTESIAN_POINT('Ctrl Pts',(-13.4498935848609,-0.0281913248931165,
-46.4709329195597));
#39409=CARTESIAN_POINT('Ctrl Pts',(-13.3947418774956,-0.0282141079667501,
-46.4597412967852));
#39410=CARTESIAN_POINT('Ctrl Pts',(-13.3396835209908,-0.0282325237416178,
-46.4486794603052));
#39411=CARTESIAN_POINT('Ctrl Pts',(-13.2846698560428,-0.0282483363564616,
-46.4377360407384));
#39412=CARTESIAN_POINT('Ctrl Pts',(-13.2687094122857,-0.0282529238775821,
-46.434561159867));
#39413=CARTESIAN_POINT('Ctrl Pts',(-13.2527527303915,-0.0282572922185099,
-46.4313962462305));
#39414=CARTESIAN_POINT('Ctrl Pts',(-13.2367986226354,-0.0282614841788263,
-46.4282410231313));
#39415=CARTESIAN_POINT('Ctrl Pts',(-13.0892763365774,-0.0283002458305825,
-46.399065732871));
#39416=CARTESIAN_POINT('Ctrl Pts',(-12.9419741004642,-0.0283241198939822,
-46.3707185504486));
#39417=CARTESIAN_POINT('Ctrl Pts',(-12.7939331331414,-0.028343224990845,
-46.3429648529121));
#39418=CARTESIAN_POINT('Ctrl Pts',(-12.5746967900316,-0.0283715180481433,
-46.3018639383091));
#39419=CARTESIAN_POINT('Ctrl Pts',(-12.3538448271959,-0.0283892866023391,
-46.262067827578));
#39420=CARTESIAN_POINT('Ctrl Pts',(-12.1347763626038,-0.0284191143890332,
-46.2243744720574));
#39421=CARTESIAN_POINT('Ctrl Pts',(-11.8709361810454,-0.0284550381751039,
-46.1789776059104));
#39422=CARTESIAN_POINT('Ctrl Pts',(-11.6097640085207,-0.0285093107968806,
-46.1366172767541));
#39423=CARTESIAN_POINT('Ctrl Pts',(-11.3508600261442,-0.0286135301320314,
-46.0971144427993));
#39424=CARTESIAN_POINT('Ctrl Pts',(-11.1830270963695,-0.0286810896813166,
-46.0715069712718));
#39425=CARTESIAN_POINT('Ctrl Pts',(-11.0161473698877,-0.028769371570055,
-46.0471003452693));
#39426=CARTESIAN_POINT('Ctrl Pts',(-10.8501566632447,-0.0288779705235915,
-46.0238381222038));
#39427=CARTESIAN_POINT('Ctrl Pts',(-10.4732223772338,-0.0291245787213677,
-45.9710139031886));
#39428=CARTESIAN_POINT('Ctrl Pts',(-10.1008720497522,-0.0294794275624165,
-45.9240905189975));
#39429=CARTESIAN_POINT('Ctrl Pts',(-9.73236090663367,-0.0298927739575285,
-45.8824064986542));
#39430=CARTESIAN_POINT('Ctrl Pts',(-9.68205671591476,-0.0299491984545376,
-45.8767163561757));
#39431=CARTESIAN_POINT('Ctrl Pts',(-9.631824073381,-0.0300066355129424,
-45.8711238535276));
#39432=CARTESIAN_POINT('Ctrl Pts',(-9.58166109168264,-0.0300648897512124,
-45.8656273191521));
#39433=CARTESIAN_POINT('Ctrl Pts',(-9.24567084642815,-0.0304550750061715,
-45.828811685983));
#39434=CARTESIAN_POINT('Ctrl Pts',(-8.91274008570343,-0.0308847456751708,
-45.7963129911165));
#39435=CARTESIAN_POINT('Ctrl Pts',(-8.57742887241812,-0.03128402910407,
-45.7671425714244));
#39436=CARTESIAN_POINT('Ctrl Pts',(-8.49902646610787,-0.0313773894820865,
-45.7603219492492));
#39437=CARTESIAN_POINT('Ctrl Pts',(-8.42049382446556,-0.0314689376095564,
-45.7536834247549));
#39438=CARTESIAN_POINT('Ctrl Pts',(-8.34176123776652,-0.0315574694580133,
-45.7472145873094));
#39439=CARTESIAN_POINT('Ctrl Pts',(-8.08715481292663,-0.0318437648582421,
-45.7262955797686));
#39440=CARTESIAN_POINT('Ctrl Pts',(-7.83048096968442,-0.0320993774944369,
-45.7071512482778));
#39441=CARTESIAN_POINT('Ctrl Pts',(-7.57169189567683,-0.0322719886806445,
-45.6895230913565));
#39442=CARTESIAN_POINT('Ctrl Pts',(-7.20190019889642,-0.0325186381331987,
-45.6643336737429));
#39443=CARTESIAN_POINT('Ctrl Pts',(-6.82778698070184,-0.0325951368515084,
-45.6422400168539));
#39444=CARTESIAN_POINT('Ctrl Pts',(-6.44939824363277,-0.0325031565777305,
-45.6225053117476));
#39445=CARTESIAN_POINT('Ctrl Pts',(-6.44444500114691,-0.0325019525233935,
-45.6222469774733));
#39446=CARTESIAN_POINT('Ctrl Pts',(-6.43949102649156,-0.0325007193835964,
-45.6219890474588));
#39447=CARTESIAN_POINT('Ctrl Pts',(-6.43453631980744,-0.0324994571456015,
-45.6217315200549));
#39448=CARTESIAN_POINT('Ctrl Pts',(-6.21842329882119,-0.0324444011990702,
-45.6104987612247));
#39449=CARTESIAN_POINT('Ctrl Pts',(-6.00090618946411,-0.0323353474729835,
-45.6000308340222));
#39450=CARTESIAN_POINT('Ctrl Pts',(-5.77560994886962,-0.0321626830075255,
-45.5899650333598));
#39451=CARTESIAN_POINT('Ctrl Pts',(-5.74279596799418,-0.0321375347473838,
-45.5884989681048));
#39452=CARTESIAN_POINT('Ctrl Pts',(-5.70981670536415,-0.0321110076321296,
-45.5870414350255));
#39453=CARTESIAN_POINT('Ctrl Pts',(-5.6766789438265,-0.0320830654558977,
-45.5855923567214));
#39454=CARTESIAN_POINT('Ctrl Pts',(-5.34325440788587,-0.0318019177044804,
-45.5710120640674));
#39455=CARTESIAN_POINT('Ctrl Pts',(-4.99378241624136,-0.0313730561290432,
-45.5572877335279));
#39456=CARTESIAN_POINT('Ctrl Pts',(-4.63509797329108,-0.0308586817011578,
-45.5443778769458));
#39457=CARTESIAN_POINT('Ctrl Pts',(-4.35532338183212,-0.0304574686063414,
-45.5343081626829));
#39458=CARTESIAN_POINT('Ctrl Pts',(-4.0699446067672,-0.0300058174109945,
-45.5247339556168));
#39459=CARTESIAN_POINT('Ctrl Pts',(-3.78220667798257,-0.0295502499152284,
-45.5156356312772));
#39460=CARTESIAN_POINT('Ctrl Pts',(-3.46861138142814,-0.0290537431650103,
-45.5057196923827));
#39461=CARTESIAN_POINT('Ctrl Pts',(-3.1522146695807,-0.0285534430926371,
-45.4963690071689));
#39462=CARTESIAN_POINT('Ctrl Pts',(-2.83714271125343,-0.0280810467641607,
-45.4875460137214));
#39463=CARTESIAN_POINT('Ctrl Pts',(-2.51852111168483,-0.0276033283578366,
-45.478623619294));
#39464=CARTESIAN_POINT('Ctrl Pts',(-2.20128569847817,-0.0271549279698236,
-45.4702550907442));
#39465=CARTESIAN_POINT('Ctrl Pts',(-1.89031005001084,-0.0267655787251769,
-45.4624340903608));
#39466=CARTESIAN_POINT('Ctrl Pts',(-1.48085910226167,-0.0262529359571283,
-45.4521364479727));
#39467=CARTESIAN_POINT('Ctrl Pts',(-1.08225782611522,-0.0258445215130111,
-45.4427883875035));
#39468=CARTESIAN_POINT('Ctrl Pts',(-0.705597976452974,-0.0255659427647448,
-45.4344166975952));
#39469=CARTESIAN_POINT('Ctrl Pts',(-0.460130518267112,-0.0253843943005195,
-45.4289609065297));
#39470=CARTESIAN_POINT('Ctrl Pts',(-0.223981908421848,-0.0252572398727827,
-45.4239198757867));
#39471=CARTESIAN_POINT('Ctrl Pts',(-0.000229628303378027,-0.025181630927626,
-45.4193011387566));
#39472=CARTESIAN_POINT('Ctrl Pts',(-0.000153083802682067,-0.025181605062196,
-45.4192995587105));
#39473=CARTESIAN_POINT('Ctrl Pts',(-7.65407527787362E-5,-0.025181579202717,
-45.4192979787138));
#39474=CARTESIAN_POINT('Ctrl Pts',(8.46174760522986E-10,-0.0251815533491883,
-45.4192963987665));
#39475=CARTESIAN_POINT('',(18.0841508193839,0.0168309156012325,-47.6825044226343));
#39476=CARTESIAN_POINT('Ctrl Pts',(-1.26595091978188E-14,-0.0251265935465125,
-45.4192972571095));
#39477=CARTESIAN_POINT('Ctrl Pts',(1.86823193664136,-0.0257297519438969,
-45.4578611092371));
#39478=CARTESIAN_POINT('Ctrl Pts',(4.99154633771575,-0.0330411937754367,
-45.5347987761651));
#39479=CARTESIAN_POINT('Ctrl Pts',(7.59438888123013,-0.0326758765092276,
-45.6867097257879));
#39480=CARTESIAN_POINT('Ctrl Pts',(8.87729659300802,-0.0314509584309369,
-45.7887336658147));
#39481=CARTESIAN_POINT('Ctrl Pts',(10.1490597186576,-0.0297979816701636,
-45.9251950972821));
#39482=CARTESIAN_POINT('Ctrl Pts',(11.8978630897578,-0.0280707333736627,
-46.1680533783691));
#39483=CARTESIAN_POINT('Ctrl Pts',(13.9971210552705,-0.0295760205187906,
-46.5641348045042));
#39484=CARTESIAN_POINT('Ctrl Pts',(16.2942224646393,-0.020912204393549,
-47.1212890230629));
#39485=CARTESIAN_POINT('Ctrl Pts',(17.5354358574236,0.00240639897730605,
-47.4946669511334));
#39486=CARTESIAN_POINT('Ctrl Pts',(18.0841508193839,0.0168309156012325,
-47.6825044226343));
#39487=CARTESIAN_POINT('',(23.8932421744751,0.740634811882458,-53.9986859556419));
#39488=CARTESIAN_POINT('Ctrl Pts',(18.084150908273,0.0167426554045659,-47.6825109477353));
#39489=CARTESIAN_POINT('Ctrl Pts',(18.1987155194437,0.0195861254427249,
-47.7194117825297));
#39490=CARTESIAN_POINT('Ctrl Pts',(18.3103943645915,0.022475540768297,-47.7564347583435));
#39491=CARTESIAN_POINT('Ctrl Pts',(18.4193445590222,0.0254026786972833,
-47.7936289577478));
#39492=CARTESIAN_POINT('Ctrl Pts',(18.5282214999332,0.0283278485420727,
-47.8307981493399));
#39493=CARTESIAN_POINT('Ctrl Pts',(18.6343735286204,0.0312907237732249,
-47.8681382921366));
#39494=CARTESIAN_POINT('Ctrl Pts',(18.7379652732147,0.0342870063881137,
-47.9057497270012));
#39495=CARTESIAN_POINT('Ctrl Pts',(18.8428315995901,0.0373201549448468,
-47.9438239289503));
#39496=CARTESIAN_POINT('Ctrl Pts',(18.9450743118358,0.040387590032794,-47.982176137475));
#39497=CARTESIAN_POINT('Ctrl Pts',(19.0448712489869,0.0434882278119365,
-48.0209637155402));
#39498=CARTESIAN_POINT('Ctrl Pts',(19.0849372612699,0.044733057512033,-48.0365359728013));
#39499=CARTESIAN_POINT('Ctrl Pts',(19.1246091311894,0.0459832720316792,
-48.0521789977961));
#39500=CARTESIAN_POINT('Ctrl Pts',(19.1638986463213,0.0472389169849191,
-48.0679052958128));
#39501=CARTESIAN_POINT('Ctrl Pts',(19.2219450831028,0.0490940102624388,
-48.0911393713815));
#39502=CARTESIAN_POINT('Ctrl Pts',(19.2791569192096,0.0509609671828519,
-48.1145554898214));
#39503=CARTESIAN_POINT('Ctrl Pts',(19.3355727469523,0.0528341973035359,
-48.1381147405902));
#39504=CARTESIAN_POINT('Ctrl Pts',(19.4950924982023,0.0581308882294921,
-48.204730191832));
#39505=CARTESIAN_POINT('Ctrl Pts',(19.6482441434888,0.063505667847821,-48.2728646408851));
#39506=CARTESIAN_POINT('Ctrl Pts',(19.7949313158912,0.0688853311200943,
-48.3422730097862));
#39507=CARTESIAN_POINT('Ctrl Pts',(19.8168881712618,0.0696905855024445,
-48.3526623948463));
#39508=CARTESIAN_POINT('Ctrl Pts',(19.8387002488627,0.0704959647465784,
-48.3630802518836));
#39509=CARTESIAN_POINT('Ctrl Pts',(19.8603672871347,0.0713012414223432,
-48.3735256732479));
#39510=CARTESIAN_POINT('Ctrl Pts',(19.9107729332328,0.0731746165749647,
-48.3978256355237));
#39511=CARTESIAN_POINT('Ctrl Pts',(19.9603936428478,0.0750473763323183,
-48.4222748738969));
#39512=CARTESIAN_POINT('Ctrl Pts',(20.0092282211876,0.0769167885082638,
-48.4468652041084));
#39513=CARTESIAN_POINT('Ctrl Pts',(20.1312063825442,0.0815861737633733,
-48.5082865036942));
#39514=CARTESIAN_POINT('Ctrl Pts',(20.2482805495917,0.0862327145344832,
-48.5705874964604));
#39515=CARTESIAN_POINT('Ctrl Pts',(20.3604266550639,0.0908485352669065,
-48.6338442430478));
#39516=CARTESIAN_POINT('Ctrl Pts',(20.5132191095433,0.0971373187799356,
-48.7200278294754));
#39517=CARTESIAN_POINT('Ctrl Pts',(20.656840047702,0.10335686552353,-48.8078118787424));
#39518=CARTESIAN_POINT('Ctrl Pts',(20.7944734247409,0.10966857806978,-48.8991351066267));
#39519=CARTESIAN_POINT('Ctrl Pts',(20.9235524482946,0.115587997544541,-48.9847823045426));
#39520=CARTESIAN_POINT('Ctrl Pts',(21.0473616598833,0.12158880846096,-49.0735382248812));
#39521=CARTESIAN_POINT('Ctrl Pts',(21.16852043031,0.127827235660881,-49.1670105943016));
#39522=CARTESIAN_POINT('Ctrl Pts',(21.1762915499337,0.128227368180087,-49.1730059090586));
#39523=CARTESIAN_POINT('Ctrl Pts',(21.1840517734182,0.1286284868762,-49.1790206427108));
#39524=CARTESIAN_POINT('Ctrl Pts',(21.1918017959379,0.129030636814078,-49.1850552271197));
#39525=CARTESIAN_POINT('Ctrl Pts',(21.199328083761,0.129421177121913,-49.1909155996592));
#39526=CARTESIAN_POINT('Ctrl Pts',(21.2068449092765,0.129812697400302,-49.1967948066722));
#39527=CARTESIAN_POINT('Ctrl Pts',(21.2143527381798,0.130205290914701,-49.2026938820643));
#39528=CARTESIAN_POINT('Ctrl Pts',(21.3057065420645,0.134982292546271,-49.2744726856844));
#39529=CARTESIAN_POINT('Ctrl Pts',(21.3957264723332,0.139915989261395,-49.3491910673921));
#39530=CARTESIAN_POINT('Ctrl Pts',(21.4852627875948,0.145185702202063,-49.4286884617553));
#39531=CARTESIAN_POINT('Ctrl Pts',(21.562654034014,0.149740609912504,-49.4974025072112));
#39532=CARTESIAN_POINT('Ctrl Pts',(21.6396835855866,0.154546101638487,-49.5696869269092));
#39533=CARTESIAN_POINT('Ctrl Pts',(21.7169214420315,0.15974196995055,-49.6467493208211));
#39534=CARTESIAN_POINT('Ctrl Pts',(21.7881410900048,0.164532987323805,-49.7178071779264));
#39535=CARTESIAN_POINT('Ctrl Pts',(21.859537466347,0.169655261283032,-49.7929273233545));
#39536=CARTESIAN_POINT('Ctrl Pts',(21.9315818076129,0.17524815142689,-49.8730760608443));
#39537=CARTESIAN_POINT('Ctrl Pts',(21.937669704384,0.175720762283621,-49.8798487959628));
#39538=CARTESIAN_POINT('Ctrl Pts',(21.9437622455401,0.176196756270345,-49.886657451252));
#39539=CARTESIAN_POINT('Ctrl Pts',(21.949859725603,0.176676230825342,-49.893502617191));
#39540=CARTESIAN_POINT('Ctrl Pts',(22.024414003266,0.182538796793058,-49.9771988977529));
#39541=CARTESIAN_POINT('Ctrl Pts',(22.0996732772509,0.188916119582828,-50.0663301976786));
#39542=CARTESIAN_POINT('Ctrl Pts',(22.1749930865905,0.195943151743774,-50.1609225259217));
#39543=CARTESIAN_POINT('Ctrl Pts',(22.2476933313007,0.202725789168989,-50.2522250062555));
#39544=CARTESIAN_POINT('Ctrl Pts',(22.320450846829,0.210113748671374,-50.3486158005322));
#39545=CARTESIAN_POINT('Ctrl Pts',(22.392684004432,0.218275564232562,-50.4501150692848));
#39546=CARTESIAN_POINT('Ctrl Pts',(22.4611591436397,0.226012751353903,-50.5463337144049));
#39547=CARTESIAN_POINT('Ctrl Pts',(22.5291638692922,0.234445737880314,-50.6471434813298));
#39548=CARTESIAN_POINT('Ctrl Pts',(22.5961888185554,0.243758120959744,-50.7525521609327));
#39549=CARTESIAN_POINT('Ctrl Pts',(22.6130295110141,0.246097950847293,-50.7790371515992));
#39550=CARTESIAN_POINT('Ctrl Pts',(22.629808243826,0.248493487950718,-50.8058124139888));
#39551=CARTESIAN_POINT('Ctrl Pts',(22.646516690491,0.250948090769253,-50.8328781574941));
#39552=CARTESIAN_POINT('Ctrl Pts',(22.668560462742,0.254186495067567,-50.8685865089402));
#39553=CARTESIAN_POINT('Ctrl Pts',(22.6904819208903,0.257527697637064,-50.9048004771956));
#39554=CARTESIAN_POINT('Ctrl Pts',(22.7122612357526,0.260980254306303,-50.9415202972099));
#39555=CARTESIAN_POINT('Ctrl Pts',(22.7799397916474,0.271708968730789,-51.0556260166503));
#39556=CARTESIAN_POINT('Ctrl Pts',(22.8462191012757,0.283510533597232,-51.1745953303357));
#39557=CARTESIAN_POINT('Ctrl Pts',(22.9109154495669,0.296586488005412,-51.2978568518167));
#39558=CARTESIAN_POINT('Ctrl Pts',(22.9743577022108,0.309408973741241,-51.4187290307513));
#39559=CARTESIAN_POINT('Ctrl Pts',(23.0362779173961,0.323458065446983,-51.5437287398601));
#39560=CARTESIAN_POINT('Ctrl Pts',(23.0964575855699,0.338924255627626,-51.6722978795863));
#39561=CARTESIAN_POINT('Ctrl Pts',(23.1552286153321,0.354028425374639,-51.7978575738595));
#39562=CARTESIAN_POINT('Ctrl Pts',(23.2123393882499,0.370485159406622,-51.9268214888112));
#39563=CARTESIAN_POINT('Ctrl Pts',(23.267543575773,0.388456337883162,-52.0586509410712));
#39564=CARTESIAN_POINT('Ctrl Pts',(23.3069283752379,0.401277670687853,-52.1527031638061));
#39565=CARTESIAN_POINT('Ctrl Pts',(23.3453417948922,0.414869550872825,-52.2482135197643));
#39566=CARTESIAN_POINT('Ctrl Pts',(23.3826821376981,0.429281525652972,-52.3449808094157));
#39567=CARTESIAN_POINT('Ctrl Pts',(23.3842895172712,0.42990191400854,-52.3491463245943));
#39568=CARTESIAN_POINT('Ctrl Pts',(23.3858949397253,0.430523824532476,-52.3533141957799));
#39569=CARTESIAN_POINT('Ctrl Pts',(23.3874984084789,0.431147263946951,-52.3574844276811));
#39570=CARTESIAN_POINT('Ctrl Pts',(23.45025399397,0.455547056824136,-52.5206964291624));
#39571=CARTESIAN_POINT('Ctrl Pts',(23.5100190844356,0.48228532595743,-52.6875245048839));
#39572=CARTESIAN_POINT('Ctrl Pts',(23.5669861146598,0.511784370525597,-52.8582128818545));
#39573=CARTESIAN_POINT('Ctrl Pts',(23.6214149651037,0.539969078043565,-53.0212961969944));
#39574=CARTESIAN_POINT('Ctrl Pts',(23.6732893711278,0.570673497582892,-53.1879034344015));
#39575=CARTESIAN_POINT('Ctrl Pts',(23.7227566502917,0.604307975088757,-53.3582474117429));
#39576=CARTESIAN_POINT('Ctrl Pts',(23.7694381353582,0.636048296892312,-53.5189983155489));
#39577=CARTESIAN_POINT('Ctrl Pts',(23.8139759842495,0.670397707363726,-53.683076977716));
#39578=CARTESIAN_POINT('Ctrl Pts',(23.856476319499,0.707744562605335,-53.8506620217186));
#39579=CARTESIAN_POINT('Ctrl Pts',(23.8689008425278,0.718662520317364,-53.8996537349901));
#39580=CARTESIAN_POINT('Ctrl Pts',(23.8811511121812,0.729836956328725,-53.9489451074243));
#39581=CARTESIAN_POINT('Ctrl Pts',(23.8932294586005,0.741278376047805,-53.998540585514));
#39582=CARTESIAN_POINT('',(24.779917851313,2.95805914746005,-60.3565719312425));
#39583=CARTESIAN_POINT('Ctrl Pts',(23.8932421744751,0.740634811882458,-53.9986859556419));
#39584=CARTESIAN_POINT('Ctrl Pts',(24.1789074622363,1.00880462386192,-55.1614948960392));
#39585=CARTESIAN_POINT('Ctrl Pts',(24.4015168304308,1.52786212045763,-56.7701588656369));
#39586=CARTESIAN_POINT('Ctrl Pts',(24.6106655417996,2.23012064092564,-58.6108222610336));
#39587=CARTESIAN_POINT('Ctrl Pts',(24.6996147992407,2.59058304170841,-59.488342199932));
#39588=CARTESIAN_POINT('Ctrl Pts',(24.7614059735443,2.86919605364059,-60.1482578252368));
#39589=CARTESIAN_POINT('Ctrl Pts',(24.7799130650375,2.95812473554106,-60.3565443657544));
#39590=CARTESIAN_POINT('',(24.8514916543763,6.03923858554143,-66.5176896450865));
#39591=CARTESIAN_POINT('Ctrl Pts',(24.779917851313,2.95805914746005,-60.3565719312425));
#39592=CARTESIAN_POINT('Ctrl Pts',(24.7799895645231,2.95843001198034,-60.3574418978072));
#39593=CARTESIAN_POINT('Ctrl Pts',(24.7800612610776,2.95880082135715,-60.3583117041383));
#39594=CARTESIAN_POINT('Ctrl Pts',(24.7801329409828,2.95917157559642,-60.3591813503334));
#39595=CARTESIAN_POINT('Ctrl Pts',(24.782850114062,2.97322577160842,-60.3921470639848));
#39596=CARTESIAN_POINT('Ctrl Pts',(24.7854889932182,2.98775170779073,-60.4260593448895));
#39597=CARTESIAN_POINT('Ctrl Pts',(24.7880733411611,3.00245300125521,-60.4602186160377));
#39598=CARTESIAN_POINT('Ctrl Pts',(24.790657689104,3.01715429471969,-60.4943778871858));
#39599=CARTESIAN_POINT('Ctrl Pts',(24.7931875024825,3.03203104417362,-60.5287843802129));
#39600=CARTESIAN_POINT('Ctrl Pts',(24.7956852978824,3.04680849773651,-60.5627893873063));
#39601=CARTESIAN_POINT('Ctrl Pts',(24.7997592646229,3.07091089392493,-60.6182524039801));
#39602=CARTESIAN_POINT('Ctrl Pts',(24.8037477026985,3.09475532602969,-60.6726623536342));
#39603=CARTESIAN_POINT('Ctrl Pts',(24.807640058142,3.1185033429446,-60.7264536078775));
#39604=CARTESIAN_POINT('Ctrl Pts',(24.8086370145993,3.1245859680175,-60.7402312648892));
#39605=CARTESIAN_POINT('Ctrl Pts',(24.8096276727509,3.13066217248865,-60.753968082751));
#39606=CARTESIAN_POINT('Ctrl Pts',(24.8106118655328,3.13673447852751,-60.7676708548502));
#39607=CARTESIAN_POINT('Ctrl Pts',(24.8175901251703,3.17978918175043,-60.8648281427549));
#39608=CARTESIAN_POINT('Ctrl Pts',(24.8242436151014,3.22264459863511,-60.9602694931683));
#39609=CARTESIAN_POINT('Ctrl Pts',(24.8305948353243,3.2651730442168,-61.0539224311071));
#39610=CARTESIAN_POINT('Ctrl Pts',(24.8333537358119,3.28364693508087,-61.0946042413853));
#39611=CARTESIAN_POINT('Ctrl Pts',(24.8360555624196,3.30205957960063,-61.1349491214377));
#39612=CARTESIAN_POINT('Ctrl Pts',(24.8387019930301,3.32040245695602,-61.1749533980223));
#39613=CARTESIAN_POINT('Ctrl Pts',(24.8473299426402,3.38020429755557,-61.3053761951255));
#39614=CARTESIAN_POINT('Ctrl Pts',(24.8553694766898,3.43926203519713,-61.4321825541305));
#39615=CARTESIAN_POINT('Ctrl Pts',(24.8628528986356,3.49756785052833,-61.5558365171184));
#39616=CARTESIAN_POINT('Ctrl Pts',(24.8707807160366,3.55933609782335,-61.6868335458274));
#39617=CARTESIAN_POINT('Ctrl Pts',(24.878084408929,3.62026073480025,-61.8142924947148));
#39618=CARTESIAN_POINT('Ctrl Pts',(24.8847959620516,3.68037730644259,-61.9387294841922));
#39619=CARTESIAN_POINT('Ctrl Pts',(24.8855286870584,3.68694045428096,-61.9523147292617));
#39620=CARTESIAN_POINT('Ctrl Pts',(24.8862543485207,3.69349401005971,-61.9658639243795));
#39621=CARTESIAN_POINT('Ctrl Pts',(24.8869729838308,3.70003804787625,-61.9793777186503));
#39622=CARTESIAN_POINT('Ctrl Pts',(24.8941500846434,3.76539417284185,-62.1143416739154));
#39623=CARTESIAN_POINT('Ctrl Pts',(24.9006269211175,3.82979673956721,-62.2457759883461));
#39624=CARTESIAN_POINT('Ctrl Pts',(24.9064352343685,3.89331878396889,-62.3742333816749));
#39625=CARTESIAN_POINT('Ctrl Pts',(24.9127907163239,3.96282488488277,-62.5147920275426));
#39626=CARTESIAN_POINT('Ctrl Pts',(24.9183457611226,4.03127715580299,-62.6517867408018));
#39627=CARTESIAN_POINT('Ctrl Pts',(24.9231341915356,4.09882908674397,-62.7859194402446));
#39628=CARTESIAN_POINT('Ctrl Pts',(24.92841190277,4.17328345990476,-62.9337577909514));
#39629=CARTESIAN_POINT('Ctrl Pts',(24.9327582355061,4.24664478696968,-63.0781198376651));
#39630=CARTESIAN_POINT('Ctrl Pts',(24.9362103791751,4.31917689646916,-63.2199133595421));
#39631=CARTESIAN_POINT('Ctrl Pts',(24.938917382834,4.37605305940895,-63.3311009633458));
#39632=CARTESIAN_POINT('Ctrl Pts',(24.9410743459718,4.432420760898,-63.4407085438744));
#39633=CARTESIAN_POINT('Ctrl Pts',(24.9426970276412,4.48842376217373,-63.5491593895862));
#39634=CARTESIAN_POINT('Ctrl Pts',(24.9449724583695,4.56695484586879,-63.7012362827417));
#39635=CARTESIAN_POINT('Ctrl Pts',(24.9461971222277,4.6447690876326,-63.8510408186009));
#39636=CARTESIAN_POINT('Ctrl Pts',(24.946407595751,4.72229821683466,-63.9997135117098));
#39637=CARTESIAN_POINT('Ctrl Pts',(24.946506062956,4.75856917642749,-64.0692680301186));
#39638=CARTESIAN_POINT('Ctrl Pts',(24.9463825550078,4.79477795245802,-64.1385740912501));
#39639=CARTESIAN_POINT('Ctrl Pts',(24.9460409903019,4.83096908536384,-64.2077445975581));
#39640=CARTESIAN_POINT('Ctrl Pts',(24.9458654050398,4.84957355311802,-64.2433024911862));
#39641=CARTESIAN_POINT('Ctrl Pts',(24.9456382269762,4.86812945857314,-64.2787402545597));
#39642=CARTESIAN_POINT('Ctrl Pts',(24.9453594450881,4.886636828798,-64.3140620599136));
#39643=CARTESIAN_POINT('Ctrl Pts',(24.9437597620407,4.9928342815915,-64.5167427061147));
#39644=CARTESIAN_POINT('Ctrl Pts',(24.9404617573982,5.09743126890092,-64.715608986053));
#39645=CARTESIAN_POINT('Ctrl Pts',(24.9354637963307,5.20042818855995,-64.9113531224432));
#39646=CARTESIAN_POINT('Ctrl Pts',(24.9341520994142,5.22745935989115,-64.9627254674158));
#39647=CARTESIAN_POINT('Ctrl Pts',(24.9327232621582,5.25438044388104,-65.0138825151559));
#39648=CARTESIAN_POINT('Ctrl Pts',(24.9311771504824,5.28119160080954,-65.0648362277982));
#39649=CARTESIAN_POINT('Ctrl Pts',(24.9292934777797,5.31385641100498,-65.1269146139212));
#39650=CARTESIAN_POINT('Ctrl Pts',(24.9272357335071,5.34635806319471,-65.1886912006868));
#39651=CARTESIAN_POINT('Ctrl Pts',(24.9250033985565,5.37869693430714,-65.2501871378648));
#39652=CARTESIAN_POINT('Ctrl Pts',(24.9227624877507,5.41116004012454,-65.3119193210633));
#39653=CARTESIAN_POINT('Ctrl Pts',(24.920345643013,5.4434591252389,-65.373368702813));
#39654=CARTESIAN_POINT('Ctrl Pts',(24.9177526911727,5.47559663338616,-65.4345600259899));
#39655=CARTESIAN_POINT('Ctrl Pts',(24.9125444975047,5.5401479157627,-65.5574686959243));
#39656=CARTESIAN_POINT('Ctrl Pts',(24.9066258928006,5.60404780990366,-65.679336808958));
#39657=CARTESIAN_POINT('Ctrl Pts',(24.8999923148938,5.66728147743902,-65.8003020279644));
#39658=CARTESIAN_POINT('Ctrl Pts',(24.8966662667709,5.69898657296373,-65.8609534811103));
#39659=CARTESIAN_POINT('Ctrl Pts',(24.893160454361,5.73052406852277,-65.9213778014053));
#39660=CARTESIAN_POINT('Ctrl Pts',(24.8894744854003,5.76189345915637,-65.9815949128062));
#39661=CARTESIAN_POINT('Ctrl Pts',(24.8876301593938,5.77758957151306,-66.0117253848127));
#39662=CARTESIAN_POINT('Ctrl Pts',(24.8857407271724,5.79324358507265,-66.0418039679763));
#39663=CARTESIAN_POINT('Ctrl Pts',(24.8838061082895,5.80885572606948,-66.0718338287028));
#39664=CARTESIAN_POINT('Ctrl Pts',(24.8818710463165,5.82447144274909,-66.101870567234));
#39665=CARTESIAN_POINT('Ctrl Pts',(24.8798907769973,5.8400452681505,-66.1318585611686));
#39666=CARTESIAN_POINT('Ctrl Pts',(24.8778652734126,5.85557623163462,-66.1617986107554));
#39667=CARTESIAN_POINT('Ctrl Pts',(24.8697941592722,5.91746315197329,-66.2811020567788));
#39668=CARTESIAN_POINT('Ctrl Pts',(24.8610049424217,5.97867070779074,-66.3996450476185));
#39669=CARTESIAN_POINT('Ctrl Pts',(24.8514916543763,6.03923858554143,-66.5176896450865));
#39670=CARTESIAN_POINT('',(23.6735115908442,9.24321250611622,-72.561102470647));
#39671=CARTESIAN_POINT('Ctrl Pts',(24.8513977161428,6.03989465182049,-66.5188833083044));
#39672=CARTESIAN_POINT('Ctrl Pts',(24.8455563449766,6.07859700744056,-66.5943232191673));
#39673=CARTESIAN_POINT('Ctrl Pts',(24.8392456975847,6.11853992684884,-66.6719944461383));
#39674=CARTESIAN_POINT('Ctrl Pts',(24.8325458971074,6.15890669998349,-66.7502957817005));
#39675=CARTESIAN_POINT('Ctrl Pts',(24.8288926950955,6.18091750125012,-66.792991172046));
#39676=CARTESIAN_POINT('Ctrl Pts',(24.8251244574647,6.20305492610137,-66.835875661678));
#39677=CARTESIAN_POINT('Ctrl Pts',(24.8212608534789,6.22518355641302,-66.8786879369743));
#39678=CARTESIAN_POINT('Ctrl Pts',(24.8195825881908,6.2347957506915,-66.8972846554272));
#39679=CARTESIAN_POINT('Ctrl Pts',(24.8178866452593,6.24440485662598,-66.9158650238878));
#39680=CARTESIAN_POINT('Ctrl Pts',(24.8161739568127,6.25400514818417,-66.9344181693235));
#39681=CARTESIAN_POINT('Ctrl Pts',(24.8089951973117,6.29424491530175,-67.0121839587378));
#39682=CARTESIAN_POINT('Ctrl Pts',(24.801517394167,6.33436121211685,-67.0895325794895));
#39683=CARTESIAN_POINT('Ctrl Pts',(24.7937073724979,6.3744931447567,-67.1667457514888));
#39684=CARTESIAN_POINT('Ctrl Pts',(24.7891659179578,6.39782948816398,-67.2116444886992));
#39685=CARTESIAN_POINT('Ctrl Pts',(24.7845119935623,6.42117111645289,-67.2564973368654));
#39686=CARTESIAN_POINT('Ctrl Pts',(24.7797378488086,6.44454552107585,-67.3013593087938));
#39687=CARTESIAN_POINT('Ctrl Pts',(24.7596506163026,6.54289341888224,-67.4901162290998));
#39688=CARTESIAN_POINT('Ctrl Pts',(24.7374303353443,6.64182229051228,-67.6790337218885));
#39689=CARTESIAN_POINT('Ctrl Pts',(24.7128946885005,6.74137185376332,-67.8683499375534));
#39690=CARTESIAN_POINT('Ctrl Pts',(24.701588943133,6.78724315362051,-67.9555846838746));
#39691=CARTESIAN_POINT('Ctrl Pts',(24.689792372908,6.83324531621845,-68.0429026099102));
#39692=CARTESIAN_POINT('Ctrl Pts',(24.6774900108944,6.87938288129889,-68.1303294426426));
#39693=CARTESIAN_POINT('Ctrl Pts',(24.6464496443559,6.99579361036991,-68.3509180524012));
#39694=CARTESIAN_POINT('Ctrl Pts',(24.6121838247661,7.11308591791533,-68.5722375519615));
#39695=CARTESIAN_POINT('Ctrl Pts',(24.5743909110932,7.23163931920386,-68.7952844661815));
#39696=CARTESIAN_POINT('Ctrl Pts',(24.5598155341771,7.27736113158979,-68.8813056942052));
#39697=CARTESIAN_POINT('Ctrl Pts',(24.544723680255,7.32324646567535,-68.9675386393311));
#39698=CARTESIAN_POINT('Ctrl Pts',(24.5290841934132,7.36936421298444,-69.0541220985275));
#39699=CARTESIAN_POINT('Ctrl Pts',(24.5054539641581,7.43904507608807,-69.1849439733877));
#39700=CARTESIAN_POINT('Ctrl Pts',(24.480574481159,7.50925615086605,-69.3165654178659));
#39701=CARTESIAN_POINT('Ctrl Pts',(24.454478968152,7.58001729247573,-69.4490443969127));
#39702=CARTESIAN_POINT('Ctrl Pts',(24.4490308268951,7.5947905868306,-69.4767029522832));
#39703=CARTESIAN_POINT('Ctrl Pts',(24.4435290302948,7.60958954672013,-69.5044018522722));
#39704=CARTESIAN_POINT('Ctrl Pts',(24.4379734711635,7.62441430239803,-69.5321434571217));
#39705=CARTESIAN_POINT('Ctrl Pts',(24.4345989630252,7.63341902316507,-69.5489940151158));
#39706=CARTESIAN_POINT('Ctrl Pts',(24.4312055161453,7.64243086407736,-69.565855843189));
#39707=CARTESIAN_POINT('Ctrl Pts',(24.4277933102453,7.65144951807085,-69.582728481914));
#39708=CARTESIAN_POINT('Ctrl Pts',(24.3862613384946,7.76122087825921,-69.7880953253642));
#39709=CARTESIAN_POINT('Ctrl Pts',(24.3419502429364,7.87199934178849,-69.9950599001169));
#39710=CARTESIAN_POINT('Ctrl Pts',(24.2951968906539,7.98321493822236,-70.2027569600603));
#39711=CARTESIAN_POINT('Ctrl Pts',(24.2446138727013,8.10354043867051,-70.4274669241358));
#39712=CARTESIAN_POINT('Ctrl Pts',(24.1911719768325,8.2243777484948,-70.6530368414904));
#39713=CARTESIAN_POINT('Ctrl Pts',(24.1352980932057,8.34503713068008,-70.8784046499643));
#39714=CARTESIAN_POINT('Ctrl Pts',(24.0817771124609,8.46061543044053,-71.0942820036554));
#39715=CARTESIAN_POINT('Ctrl Pts',(24.0260241432573,8.57603160210702,-71.3099765369464));
#39716=CARTESIAN_POINT('Ctrl Pts',(23.9684197384083,8.69069685263161,-71.5245442088329));
#39717=CARTESIAN_POINT('Ctrl Pts',(23.9153048804812,8.79642537298955,-71.7223889993114));
#39718=CARTESIAN_POINT('Ctrl Pts',(23.8606155216188,8.90151629720597,-71.9192768214147));
#39719=CARTESIAN_POINT('Ctrl Pts',(23.8046611444706,9.00550935262722,-72.1144338489968));
#39720=CARTESIAN_POINT('Ctrl Pts',(23.761660871844,9.08542677754184,-72.2644097010878));
#39721=CARTESIAN_POINT('Ctrl Pts',(23.7179136506019,9.16470432536132,-72.4133583231326));
#39722=CARTESIAN_POINT('Ctrl Pts',(23.673567339905,9.24311393663887,-72.5609169730204));
#39723=CARTESIAN_POINT('',(21.0430574415837,12.442190173977,-78.5797217830346));
#39724=CARTESIAN_POINT('Ctrl Pts',(23.6734819284753,9.2432649519181,-72.5612011682563));
#39725=CARTESIAN_POINT('Ctrl Pts',(23.5615106118548,9.44235138733137,-72.9358619934788));
#39726=CARTESIAN_POINT('Ctrl Pts',(23.2106747185919,10.0332017364569,-74.0473320232884));
#39727=CARTESIAN_POINT('Ctrl Pts',(22.4162563803382,11.1958361188247,-76.2337986537702));
#39728=CARTESIAN_POINT('Ctrl Pts',(21.6377011779931,12.0078686581778,-77.7620529729162));
#39729=CARTESIAN_POINT('Ctrl Pts',(21.0430574415837,12.442190173977,-78.5797217830346));
#39730=CARTESIAN_POINT('',(20.8093219137291,12.6047243941762,-78.8857197857179));
#39731=CARTESIAN_POINT('Ctrl Pts',(21.0430574363752,12.4421970963867,-78.5797181023401));
#39732=CARTESIAN_POINT('Ctrl Pts',(20.966393338375,12.4981910797977,-78.6851364132037));
#39733=CARTESIAN_POINT('Ctrl Pts',(20.8885043059515,12.5523874433895,-78.7871760259047));
#39734=CARTESIAN_POINT('Ctrl Pts',(20.8093219137031,12.6047243946578,-78.8857197854716));
#39735=CARTESIAN_POINT('',(25.7013491764599,12.8213346415145,-79.293640964296));
#39736=CARTESIAN_POINT('Ctrl Pts',(20.8093219137031,12.6047243946579,-78.8857197854716));
#39737=CARTESIAN_POINT('Ctrl Pts',(20.7840585047214,12.6878774354483,-79.0421442877749));
#39738=CARTESIAN_POINT('Ctrl Pts',(20.7688933687643,12.7738276928524,-79.2038152925502));
#39739=CARTESIAN_POINT('Ctrl Pts',(20.7703883247029,12.8593245421261,-79.3646100531889));
#39740=CARTESIAN_POINT('Ctrl Pts',(20.7718832806414,12.9448213913999,-79.5254048138275));
#39741=CARTESIAN_POINT('Ctrl Pts',(20.7900383284828,13.0298648236847,-79.6853233350397));
#39742=CARTESIAN_POINT('Ctrl Pts',(20.8316864377639,13.1115279871602,-79.8388510633934));
#39743=CARTESIAN_POINT('Ctrl Pts',(20.8733345470451,13.1931911506358,-79.9923787917472));
#39744=CARTESIAN_POINT('Ctrl Pts',(20.9384757176957,13.2714741339522,-80.1395156801066));
#39745=CARTESIAN_POINT('Ctrl Pts',(21.0312181697793,13.3423337920754,-80.2726523540952));
#39746=CARTESIAN_POINT('Ctrl Pts',(21.1239606218628,13.4131934501986,-80.4057890280839));
#39747=CARTESIAN_POINT('Ctrl Pts',(21.2443043552774,13.4766299304238,-80.5249254093838));
#39748=CARTESIAN_POINT('Ctrl Pts',(21.3835931186265,13.5285264211225,-80.6223375406638));
#39749=CARTESIAN_POINT('Ctrl Pts',(21.4184153094637,13.5415005437972,-80.6466905734838));
#39750=CARTESIAN_POINT('Ctrl Pts',(21.4544215646831,13.5537534008702,-80.6696858493211));
#39751=CARTESIAN_POINT('Ctrl Pts',(21.4915342779707,13.5654172411284,-80.6915723859151));
#39752=CARTESIAN_POINT('Ctrl Pts',(21.5286469912584,13.5770810813866,-80.7134589225092));
#39753=CARTESIAN_POINT('Ctrl Pts',(21.5668661626148,13.5881559038188,-80.7342367203975));
#39754=CARTESIAN_POINT('Ctrl Pts',(21.6059140724305,13.5985438937157,-80.7537224018477));
#39755=CARTESIAN_POINT('Ctrl Pts',(21.6840098920621,13.6193198735095,-80.7926937647481));
#39756=CARTESIAN_POINT('Ctrl Pts',(21.7654206655389,13.6373485207903,-80.826496663157));
#39757=CARTESIAN_POINT('Ctrl Pts',(21.8485678910789,13.6530496506021,-80.8559244908226));
#39758=CARTESIAN_POINT('Ctrl Pts',(22.014862342159,13.6844519102255,-80.9147801461538));
#39759=CARTESIAN_POINT('Ctrl Pts',(22.1881026013518,13.7065442425174,-80.9561354427192));
#39760=CARTESIAN_POINT('Ctrl Pts',(22.3667510409472,13.7214448954529,-80.9839923851256));
#39761=CARTESIAN_POINT('Ctrl Pts',(22.4282524899153,13.7265745889906,-80.9935824063185));
#39762=CARTESIAN_POINT('Ctrl Pts',(22.490395192073,13.7308519682516,-81.0015727254715));
#39763=CARTESIAN_POINT('Ctrl Pts',(22.5528649735285,13.7343255298831,-81.0080555375436));
#39764=CARTESIAN_POINT('Ctrl Pts',(22.6718564286154,13.7409419153296,-81.0204038957984));
#39765=CARTESIAN_POINT('Ctrl Pts',(22.7920344808733,13.7446418002757,-81.0272827150941));
#39766=CARTESIAN_POINT('Ctrl Pts',(22.9112327926434,13.7457620573825,-81.0293291152419));
#39767=CARTESIAN_POINT('Ctrl Pts',(23.0930094843542,13.7474704425745,-81.0324498628704));
#39768=CARTESIAN_POINT('Ctrl Pts',(23.2725062469405,13.7431799593285,-81.024331855367));
#39769=CARTESIAN_POINT('Ctrl Pts',(23.453334415982,13.7329853385207,-81.0051586905715));
#39770=CARTESIAN_POINT('Ctrl Pts',(23.7245766695442,13.717693407309,-80.9763989433782));
#39771=CARTESIAN_POINT('Ctrl Pts',(23.9988145883369,13.6891140752413,-80.9227667359737));
#39772=CARTESIAN_POINT('Ctrl Pts',(24.2566884728839,13.645897639705,-80.8417199326631));
#39773=CARTESIAN_POINT('Ctrl Pts',(24.5145623574308,13.6026812041686,-80.7606731293525));
#39774=CARTESIAN_POINT('Ctrl Pts',(24.7560722095976,13.544828389164,-80.6522113451778));
#39775=CARTESIAN_POINT('Ctrl Pts',(24.9680647929619,13.4679875742907,-80.5080837891733));
#39776=CARTESIAN_POINT('Ctrl Pts',(25.1093931818714,13.4167603643751,-80.4119987518369));
#39777=CARTESIAN_POINT('Ctrl Pts',(25.2376027841621,13.3570942619928,-80.3000621441297));
#39778=CARTESIAN_POINT('Ctrl Pts',(25.3433331128627,13.289655597635,-80.1734804456779));
#39779=CARTESIAN_POINT('Ctrl Pts',(25.3519347957313,13.2841691302135,-80.1631824012054));
#39780=CARTESIAN_POINT('Ctrl Pts',(25.3603876963185,13.2786312235604,-80.1527874266039));
#39781=CARTESIAN_POINT('Ctrl Pts',(25.3686909709012,13.2730439238718,-80.1422993517087));
#39782=CARTESIAN_POINT('Ctrl Pts',(25.4624500443877,13.2099531472293,-80.0238699085973));
#39783=CARTESIAN_POINT('Ctrl Pts',(25.5371310844642,13.1405649390909,-79.8935692943807));
#39784=CARTESIAN_POINT('Ctrl Pts',(25.5915191111769,13.0678252000338,-79.7569144572679));
#39785=CARTESIAN_POINT('Ctrl Pts',(25.6507237247329,12.9886436521574,-79.6081575099976));
#39786=CARTESIAN_POINT('Ctrl Pts',(25.6858818958191,12.9054906353473,-79.4518710147319));
#39787=CARTESIAN_POINT('Ctrl Pts',(25.7013238222668,12.8213719704933,-79.2937110989762));
#39788=CARTESIAN_POINT('',(25.9521939529868,12.4413326875396,-78.5797156137649));
#39789=CARTESIAN_POINT('Ctrl Pts',(25.7013815084256,12.8212870391611,-79.293551527726));
#39790=CARTESIAN_POINT('Ctrl Pts',(25.7859000295341,12.6968486583446,-79.0597595468301));
#39791=CARTESIAN_POINT('Ctrl Pts',(25.8695209159813,12.5699441739082,-78.8213395443483));
#39792=CARTESIAN_POINT('Ctrl Pts',(25.952193952974,12.4413326879221,-78.5797156136114));
#39793=CARTESIAN_POINT('',(27.8032099026773,9.23603570625547,-72.5577783044314));
#39794=CARTESIAN_POINT('Ctrl Pts',(25.9521939530147,12.4413326882658,-78.5797156132792));
#39795=CARTESIAN_POINT('Ctrl Pts',(26.1287870546047,12.1667972870379,-78.0639430465837));
#39796=CARTESIAN_POINT('Ctrl Pts',(26.2992662638511,11.8864855960595,-77.5377185702874));
#39797=CARTESIAN_POINT('Ctrl Pts',(26.6249152504807,11.3331555384472,-76.4994184116619));
#39798=CARTESIAN_POINT('Ctrl Pts',(26.7835000842749,11.0543284251978,-75.9764391079278));
#39799=CARTESIAN_POINT('Ctrl Pts',(27.0855446094684,10.5155281999478,-74.9654367676289));
#39800=CARTESIAN_POINT('Ctrl Pts',(27.2314148704176,10.2516696780351,-74.470116440961));
#39801=CARTESIAN_POINT('Ctrl Pts',(27.4390175574596,9.87838321168263,-73.7683380431596));
#39802=CARTESIAN_POINT('Ctrl Pts',(27.5122084373452,9.74719436950816,-73.5215103039169));
#39803=CARTESIAN_POINT('Ctrl Pts',(27.620165889337,9.55564988556187,-73.1607059454969));
#39804=CARTESIAN_POINT('Ctrl Pts',(27.6566443739694,9.49125974573235,-73.0393458765082));
#39805=CARTESIAN_POINT('Ctrl Pts',(27.7114876925037,9.39517048279879,-72.858114884868));
#39806=CARTESIAN_POINT('Ctrl Pts',(27.7298944275117,9.36304055589236,-72.797494717765));
#39807=CARTESIAN_POINT('Ctrl Pts',(27.7708537404106,9.29185801117427,-72.6631426458087));
#39808=CARTESIAN_POINT('Ctrl Pts',(27.789295348826,9.26001909606324,-72.6030135173959));
#39809=CARTESIAN_POINT('Ctrl Pts',(27.8032099492931,9.23606309930771,-72.5577638163968));
#39810=CARTESIAN_POINT('',(30.3753540341101,6.01695723880264,-66.3794227429407));
#39811=CARTESIAN_POINT('Ctrl Pts',(27.8032099026773,9.23603570625547,-72.5577783044314));
#39812=CARTESIAN_POINT('Ctrl Pts',(28.1510242423018,8.65285503600956,-71.4562837782078));
#39813=CARTESIAN_POINT('Ctrl Pts',(28.8443112604251,7.45365732155485,-69.2995688107867));
#39814=CARTESIAN_POINT('Ctrl Pts',(29.7346820906896,6.49856484963839,-67.5354860661677));
#39815=CARTESIAN_POINT('Ctrl Pts',(30.3753540341101,6.01695723880264,-66.3794227429407));
#39816=CARTESIAN_POINT('',(33.2873624690393,4.35252899916091,-59.9316190686982));
#39817=CARTESIAN_POINT('Ctrl Pts',(30.3753540341101,6.01695723880265,-66.3794227429407));
#39818=CARTESIAN_POINT('Ctrl Pts',(30.7734090781721,5.72447094290213,-65.6771164512212));
#39819=CARTESIAN_POINT('Ctrl Pts',(31.4978217512257,5.28838679537279,-64.4647865749015));
#39820=CARTESIAN_POINT('Ctrl Pts',(32.3856289559011,4.77997444759906,-62.3963211915439));
#39821=CARTESIAN_POINT('Ctrl Pts',(32.8375602373923,4.5442896682234,-61.1512919674956));
#39822=CARTESIAN_POINT('Ctrl Pts',(33.0921495677964,4.42939107495768,-60.4613459843507));
#39823=CARTESIAN_POINT('Ctrl Pts',(33.2133445958773,4.37993836178462,-60.1301142016715));
#39824=CARTESIAN_POINT('Ctrl Pts',(33.2870419060244,4.35253527707261,-59.9326413364725));
#39825=CARTESIAN_POINT('',(36.1829914186425,4.79767940081217,-53.6562556717971));
#39826=CARTESIAN_POINT('Ctrl Pts',(33.2879498115781,4.35251749663435,-59.9297460474139));
#39827=CARTESIAN_POINT('Ctrl Pts',(33.3193429188025,4.33924707865741,-59.836759691682));
#39828=CARTESIAN_POINT('Ctrl Pts',(33.3527820526142,4.32635858806945,-59.7387076557157));
#39829=CARTESIAN_POINT('Ctrl Pts',(33.3885290935015,4.31421583300761,-59.635464898597));
#39830=CARTESIAN_POINT('Ctrl Pts',(33.4236835691159,4.30227436383656,-59.5339335578932));
#39831=CARTESIAN_POINT('Ctrl Pts',(33.4610701996642,4.29105457425154,-59.4273816074148));
#39832=CARTESIAN_POINT('Ctrl Pts',(33.5009269768532,4.28094099462918,-59.3157162971264));
#39833=CARTESIAN_POINT('Ctrl Pts',(33.5397082187402,4.27110032999598,-59.2070642757114));
#39834=CARTESIAN_POINT('Ctrl Pts',(33.5808284261384,4.2623077625252,-59.0935703856562));
#39835=CARTESIAN_POINT('Ctrl Pts',(33.6244906665991,4.25496188680782,-58.9751811881067));
#39836=CARTESIAN_POINT('Ctrl Pts',(33.6651578575728,4.24811990784578,-58.8649130008777));
#39837=CARTESIAN_POINT('Ctrl Pts',(33.7080229607883,4.24258396476386,-58.7503927918472));
#39838=CARTESIAN_POINT('Ctrl Pts',(33.7532493913408,4.2385859318034,-58.6316247260045));
#39839=CARTESIAN_POINT('Ctrl Pts',(33.7781485708435,4.23638483525158,-58.5662375761791));
#39840=CARTESIAN_POINT('Ctrl Pts',(33.8037624161283,4.23464993176182,-58.4995656615771));
#39841=CARTESIAN_POINT('Ctrl Pts',(33.830116374127,4.23342993811555,-58.431608832582));
#39842=CARTESIAN_POINT('Ctrl Pts',(33.8772223557387,4.23124927901796,-58.3101404316232));
#39843=CARTESIAN_POINT('Ctrl Pts',(33.9266919107457,4.23071374517117,-58.1845694789117));
#39844=CARTESIAN_POINT('Ctrl Pts',(33.9787951067483,4.23218950266131,-58.0550320213901));
#39845=CARTESIAN_POINT('Ctrl Pts',(34.0170138421718,4.23327200026974,-57.9600137078069));
#39846=CARTESIAN_POINT('Ctrl Pts',(34.0566502834616,4.23543688539143,-57.8628598169221));
#39847=CARTESIAN_POINT('Ctrl Pts',(34.0977995205523,4.23882699399173,-57.7636506686872));
#39848=CARTESIAN_POINT('Ctrl Pts',(34.1105235373635,4.23987527099202,-57.732973578194));
#39849=CARTESIAN_POINT('Ctrl Pts',(34.1233921062565,4.24104067164571,-57.7021001731857));
#39850=CARTESIAN_POINT('Ctrl Pts',(34.1364078860249,4.24232734701405,-57.6710331046924));
#39851=CARTESIAN_POINT('Ctrl Pts',(34.1493998562702,4.24361166869114,-57.6400228666078));
#39852=CARTESIAN_POINT('Ctrl Pts',(34.1625348460402,4.24501644543468,-57.6088283708759));
#39853=CARTESIAN_POINT('Ctrl Pts',(34.1758182484859,4.24654595697531,-57.5774455065173));
#39854=CARTESIAN_POINT('Ctrl Pts',(34.1922641067537,4.24843960810267,-57.5385911436089));
#39855=CARTESIAN_POINT('Ctrl Pts',(34.2089380837605,4.25052449795675,-57.49944651308));
#39856=CARTESIAN_POINT('Ctrl Pts',(34.2258536530513,4.25280960171236,-57.4599968745805));
#39857=CARTESIAN_POINT('Ctrl Pts',(34.2390115898942,4.25458709145444,-57.4293105971679));
#39858=CARTESIAN_POINT('Ctrl Pts',(34.2523157279084,4.25648573961938,-57.3984397369432));
#39859=CARTESIAN_POINT('Ctrl Pts',(34.26575497327,4.25850063205734,-57.3674086665775));
#39860=CARTESIAN_POINT('Ctrl Pts',(34.2781317989214,4.26035624014695,-57.3388307116878));
#39861=CARTESIAN_POINT('Ctrl Pts',(34.2906222853231,4.26231024523409,-57.3101189316576));
#39862=CARTESIAN_POINT('Ctrl Pts',(34.3032320058153,4.2643614058939,-57.281260241763));
#39863=CARTESIAN_POINT('Ctrl Pts',(34.3353173948163,4.26958057690682,-57.2078294078357));
#39864=CARTESIAN_POINT('Ctrl Pts',(34.3681640087544,4.2754259772561,-57.1334699365933));
#39865=CARTESIAN_POINT('Ctrl Pts',(34.4017682786756,4.28187637012116,-57.0582108210068));
#39866=CARTESIAN_POINT('Ctrl Pts',(34.4086934361437,4.28320566507165,-57.0427014459315));
#39867=CARTESIAN_POINT('Ctrl Pts',(34.415650780798,4.28456071279837,-57.027153953167));
#39868=CARTESIAN_POINT('Ctrl Pts',(34.4226403295208,4.28594142333925,-57.0115686651073));
#39869=CARTESIAN_POINT('Ctrl Pts',(34.4258994958212,4.28658523675896,-57.0043013796729));
#39870=CARTESIAN_POINT('Ctrl Pts',(34.429167321032,4.28723496733483,-56.9970222000307));
#39871=CARTESIAN_POINT('Ctrl Pts',(34.4324324617172,4.28788832163034,-56.9897563806894));
#39872=CARTESIAN_POINT('Ctrl Pts',(34.4652349505291,4.29445209606898,-56.9167619891382));
#39873=CARTESIAN_POINT('Ctrl Pts',(34.4979753191527,4.30142033433672,-56.8446463818856));
#39874=CARTESIAN_POINT('Ctrl Pts',(34.5306719667931,4.30874438156103,-56.7733274368403));
#39875=CARTESIAN_POINT('Ctrl Pts',(34.5600103523251,4.31531617826277,-56.7093336375833));
#39876=CARTESIAN_POINT('Ctrl Pts',(34.5893154621551,4.32217536766797,-56.6459775876097));
#39877=CARTESIAN_POINT('Ctrl Pts',(34.6186155012557,4.32930500506736,-56.5831926500093));
#39878=CARTESIAN_POINT('Ctrl Pts',(34.6267458294818,4.33128337417434,-56.5657707568646));
#39879=CARTESIAN_POINT('Ctrl Pts',(34.6348759116403,4.33328266952345,-56.548392652979));
#39880=CARTESIAN_POINT('Ctrl Pts',(34.6430101831854,4.33530366538436,-56.5310491039294));
#39881=CARTESIAN_POINT('Ctrl Pts',(34.6641901616557,4.34056592502068,-56.4858900514644));
#39882=CARTESIAN_POINT('Ctrl Pts',(34.685388439502,4.34597281030537,-56.4409868113198));
#39883=CARTESIAN_POINT('Ctrl Pts',(34.7065762247373,4.35151265306868,-56.3964075588278));
#39884=CARTESIAN_POINT('Ctrl Pts',(34.7269322203096,4.35683501279193,-56.353578397768));
#39885=CARTESIAN_POINT('Ctrl Pts',(34.7472784056529,4.3622800874029,-56.3110485760468));
#39886=CARTESIAN_POINT('Ctrl Pts',(34.7676538333411,4.36784902616682,-56.268736385199));
#39887=CARTESIAN_POINT('Ctrl Pts',(34.7779097223884,4.3706521289506,-56.2474387152152));
#39888=CARTESIAN_POINT('Ctrl Pts',(34.7881730263819,4.37348662257477,-56.2261961965177));
#39889=CARTESIAN_POINT('Ctrl Pts',(34.7984487796813,4.3763527052992,-56.2049984515675));
#39890=CARTESIAN_POINT('Ctrl Pts',(34.8084407611364,4.37913963921997,-56.1843860966128));
#39891=CARTESIAN_POINT('Ctrl Pts',(34.8184407814739,4.38195540987727,-56.1638238008178));
#39892=CARTESIAN_POINT('Ctrl Pts',(34.8284479955918,4.38479857514819,-56.1433131111396));
#39893=CARTESIAN_POINT('Ctrl Pts',(34.8744185960652,4.39785935442295,-56.0490922111449));
#39894=CARTESIAN_POINT('Ctrl Pts',(34.920552158193,4.41150287932467,-55.9559411034495));
#39895=CARTESIAN_POINT('Ctrl Pts',(34.966934193085,4.42562295944024,-55.8636347575493));
#39896=CARTESIAN_POINT('Ctrl Pts',(35.0057045413381,4.43742581424635,-55.7864766685424));
#39897=CARTESIAN_POINT('Ctrl Pts',(35.0446482571423,4.44956094597523,-55.7099084471863));
#39898=CARTESIAN_POINT('Ctrl Pts',(35.0838003791657,4.4619543730562,-55.6338032881274));
#39899=CARTESIAN_POINT('Ctrl Pts',(35.1033921354031,4.46815605484938,-55.5957201997113));
#39900=CARTESIAN_POINT('Ctrl Pts',(35.1230360065799,4.47442231987154,-55.5577528539355));
#39901=CARTESIAN_POINT('Ctrl Pts',(35.1427351931354,4.48074331663663,-55.5198857676554));
#39902=CARTESIAN_POINT('Ctrl Pts',(35.1515556497795,4.48357358974243,-55.5029304993841));
#39903=CARTESIAN_POINT('Ctrl Pts',(35.1603865099301,4.48641461662677,-55.4859966435756));
#39904=CARTESIAN_POINT('Ctrl Pts',(35.16922544088,4.48926466526989,-55.469087709146));
#39905=CARTESIAN_POINT('Ctrl Pts',(35.1800953274311,4.49276958069363,-55.4482935429746));
#39906=CARTESIAN_POINT('Ctrl Pts',(35.1909797949457,4.49628889993367,-55.4275324894031));
#39907=CARTESIAN_POINT('Ctrl Pts',(35.2018857234225,4.49982305678331,-55.4067896722193));
#39908=CARTESIAN_POINT('Ctrl Pts',(35.2251618051249,4.50736586469342,-55.3625191171226));
#39909=CARTESIAN_POINT('Ctrl Pts',(35.2485353596057,4.5149761197521,-55.3183319108149));
#39910=CARTESIAN_POINT('Ctrl Pts',(35.2719897294641,4.52263364313067,-55.274239624144));
#39911=CARTESIAN_POINT('Ctrl Pts',(35.2874168173186,4.52767037132342,-55.2452379675536));
#39912=CARTESIAN_POINT('Ctrl Pts',(35.3028783324909,4.53272739361122,-55.2162784591772));
#39913=CARTESIAN_POINT('Ctrl Pts',(35.3183720972909,4.53779994429228,-55.1873604599376));
#39914=CARTESIAN_POINT('Ctrl Pts',(35.3567990507267,4.55038066120243,-55.1156393111672));
#39915=CARTESIAN_POINT('Ctrl Pts',(35.3954510211321,4.56306580132258,-55.0441217312217));
#39916=CARTESIAN_POINT('Ctrl Pts',(35.4343467852101,4.57579980706008,-54.972723810768));
#39917=CARTESIAN_POINT('Ctrl Pts',(35.4580836639989,4.58357097592261,-54.9291518737267));
#39918=CARTESIAN_POINT('Ctrl Pts',(35.4819130032678,4.59136089096042,-54.8856219885748));
#39919=CARTESIAN_POINT('Ctrl Pts',(35.5058437810806,4.59915739223225,-54.8421114637831));
#39920=CARTESIAN_POINT('Ctrl Pts',(35.5166852243627,4.60268946824744,-54.8223997398101));
#39921=CARTESIAN_POINT('Ctrl Pts',(35.5275474313267,4.6062228600002,-54.8026921414144));
#39922=CARTESIAN_POINT('Ctrl Pts',(35.5384308800317,4.60975620962218,-54.7829874465923));
#39923=CARTESIAN_POINT('Ctrl Pts',(35.5428940276423,4.6112051860772,-54.7749068313391));
#39924=CARTESIAN_POINT('Ctrl Pts',(35.5473607443006,4.61265415344328,-54.7668267117997));
#39925=CARTESIAN_POINT('Ctrl Pts',(35.5518310486815,4.61410300911227,-54.7587470363111));
#39926=CARTESIAN_POINT('Ctrl Pts',(35.5559724443439,4.61544526325692,-54.7512618339241));
#39927=CARTESIAN_POINT('Ctrl Pts',(35.56011966303,4.61678830788818,-54.7437720684435));
#39928=CARTESIAN_POINT('Ctrl Pts',(35.5642570127954,4.61812698146163,-54.7363060240264));
#39929=CARTESIAN_POINT('Ctrl Pts',(35.604680894705,4.63120646120528,-54.663359206628));
#39930=CARTESIAN_POINT('Ctrl Pts',(35.6444001071669,4.64394591788954,-54.5922440303002));
#39931=CARTESIAN_POINT('Ctrl Pts',(35.6834479721225,4.65628937713368,-54.5228259069607));
#39932=CARTESIAN_POINT('Ctrl Pts',(35.695230871715,4.66001408118762,-54.5018786214141));
#39933=CARTESIAN_POINT('Ctrl Pts',(35.7069525999216,4.66370269122389,-54.4810861717907));
#39934=CARTESIAN_POINT('Ctrl Pts',(35.718613806074,4.66735348114836,-54.460445910469));
#39935=CARTESIAN_POINT('Ctrl Pts',(35.7417218506995,4.67458794861172,-54.4195448172657));
#39936=CARTESIAN_POINT('Ctrl Pts',(35.7645949778937,4.68167474578746,-54.3792365323959));
#39937=CARTESIAN_POINT('Ctrl Pts',(35.7872336535589,4.68860586750444,-54.3394930764735));
#39938=CARTESIAN_POINT('Ctrl Pts',(35.8109318354677,4.69586137068449,-54.2978895983346));
#39939=CARTESIAN_POINT('Ctrl Pts',(35.8343776374465,4.70294759661248,-54.2568972277437));
#39940=CARTESIAN_POINT('Ctrl Pts',(35.8575430046428,4.70984679047995,-54.2165339087682));
#39941=CARTESIAN_POINT('Ctrl Pts',(35.8863332239078,4.71842119823762,-54.1663698516339));
#39942=CARTESIAN_POINT('Ctrl Pts',(35.9146885521825,4.72670608754568,-54.1171804254787));
#39943=CARTESIAN_POINT('Ctrl Pts',(35.9425539712792,4.73466916979316,-54.0690003817303));
#39944=CARTESIAN_POINT('Ctrl Pts',(35.9557139144567,4.73842987798603,-54.0462464932703));
#39945=CARTESIAN_POINT('Ctrl Pts',(35.9687646274413,4.74211885856277,-54.0237176519991));
#39946=CARTESIAN_POINT('Ctrl Pts',(35.981699463113,4.7457327148002,-54.001418937057));
#39947=CARTESIAN_POINT('Ctrl Pts',(35.9904281226407,4.7481714099239,-53.9863713635451));
#39948=CARTESIAN_POINT('Ctrl Pts',(35.9991021184289,4.75057538140656,-53.9714318441434));
#39949=CARTESIAN_POINT('Ctrl Pts',(36.0077274345209,4.75294583366281,-53.9565881348688));
#39950=CARTESIAN_POINT('Ctrl Pts',(36.0300298181379,4.75907508562308,-53.9182069213559));
#39951=CARTESIAN_POINT('Ctrl Pts',(36.0520201758314,4.76498481343368,-53.880442836908));
#39952=CARTESIAN_POINT('Ctrl Pts',(36.0739039034926,4.77071695984771,-53.8429123359909));
#39953=CARTESIAN_POINT('Ctrl Pts',(36.082315379934,4.77292023230962,-53.8284866892645));
#39954=CARTESIAN_POINT('Ctrl Pts',(36.0907111626026,4.77509715849289,-53.8140954911172));
#39955=CARTESIAN_POINT('Ctrl Pts',(36.0991010506208,4.77724914208039,-53.7997202332773));
#39956=CARTESIAN_POINT('Ctrl Pts',(36.1184352358726,4.78220830831117,-53.7665929856289));
#39957=CARTESIAN_POINT('Ctrl Pts',(36.1377220120453,4.78702974102347,-53.7335782690287));
#39958=CARTESIAN_POINT('Ctrl Pts',(36.1567145307872,4.79164136430998,-53.7010756726801));
#39959=CARTESIAN_POINT('Ctrl Pts',(36.165518137879,4.79377899123678,-53.6860097358443));
#39960=CARTESIAN_POINT('Ctrl Pts',(36.1742588505742,4.79587179689088,-53.6710532217596));
#39961=CARTESIAN_POINT('Ctrl Pts',(36.1829138277446,4.79791400485598,-53.6562428681622));
#39962=CARTESIAN_POINT('',(38.0216852001562,4.87035269640389,-47.6589608371561));
#39963=CARTESIAN_POINT('Ctrl Pts',(36.1830969697801,4.79736025611348,-53.6562730892812));
#39964=CARTESIAN_POINT('Ctrl Pts',(36.183936161047,4.79755340016328,-53.6547287540334));
#39965=CARTESIAN_POINT('Ctrl Pts',(36.1847749166295,4.79774608622482,-53.6531833391776));
#39966=CARTESIAN_POINT('Ctrl Pts',(36.1856132372291,4.79793831318313,-53.6516368116431));
#39967=CARTESIAN_POINT('Ctrl Pts',(36.2353363294914,4.80933982089724,-53.5599080251673));
#39968=CARTESIAN_POINT('Ctrl Pts',(36.2838250944541,4.81981537446271,-53.4691803615298));
#39969=CARTESIAN_POINT('Ctrl Pts',(36.3311210963185,4.82950527468665,-53.379305289989));
#39970=CARTESIAN_POINT('Ctrl Pts',(36.382327292743,4.8399962869211,-53.2819998014581));
#39971=CARTESIAN_POINT('Ctrl Pts',(36.4321352795488,4.84956616905091,-53.185693829071));
#39972=CARTESIAN_POINT('Ctrl Pts',(36.4806030253521,4.85834600565935,-53.0901555874634));
#39973=CARTESIAN_POINT('Ctrl Pts',(36.5307167410359,4.86742400646695,-52.9913728568557));
#39974=CARTESIAN_POINT('Ctrl Pts',(36.5793976635715,4.87565684395552,-52.8934106499926));
#39975=CARTESIAN_POINT('Ctrl Pts',(36.6267155733464,4.88314763835947,-52.7959696942444));
#39976=CARTESIAN_POINT('Ctrl Pts',(36.6772824731675,4.89115277324405,-52.6918381493133));
#39977=CARTESIAN_POINT('Ctrl Pts',(36.7262928124926,4.89831011493297,-52.5883018726186));
#39978=CARTESIAN_POINT('Ctrl Pts',(36.7738376014596,4.904705500865,-52.4849490338879));
#39979=CARTESIAN_POINT('Ctrl Pts',(36.81088898026,4.9096893880983,-52.4044067649851));
#39980=CARTESIAN_POINT('Ctrl Pts',(36.8470504776515,4.91420964272209,-52.3239748839792));
#39981=CARTESIAN_POINT('Ctrl Pts',(36.8823668850021,4.91829385211365,-52.2434412285763));
#39982=CARTESIAN_POINT('Ctrl Pts',(36.9169119340263,4.92228885682225,-52.1646665376408));
#39983=CARTESIAN_POINT('Ctrl Pts',(36.9506484477767,4.9258665600734,-52.0857943442769));
#39984=CARTESIAN_POINT('Ctrl Pts',(36.9836202495651,4.92905006187823,-52.0066157573371));
#39985=CARTESIAN_POINT('Ctrl Pts',(37.0244261353492,4.9329899621565,-51.9086243768252));
#39986=CARTESIAN_POINT('Ctrl Pts',(37.0640788100562,4.93634183787733,-51.8102526024379));
#39987=CARTESIAN_POINT('Ctrl Pts',(37.1025879776156,4.93913229986728,-51.7112748626131));
#39988=CARTESIAN_POINT('Ctrl Pts',(37.1555435239945,4.9429695793696,-51.5751664857263));
#39989=CARTESIAN_POINT('Ctrl Pts',(37.2063364481489,4.94574534134144,-51.4379137453509));
#39990=CARTESIAN_POINT('Ctrl Pts',(37.2550159356616,4.94752183743243,-51.2988780651826));
#39991=CARTESIAN_POINT('Ctrl Pts',(37.3058849186964,4.94937823638262,-51.153588868088));
#39992=CARTESIAN_POINT('Ctrl Pts',(37.3544465987836,4.95014231523103,-51.0063527325029));
#39993=CARTESIAN_POINT('Ctrl Pts',(37.4007617379197,4.9498744481247,-50.856386642756));
#39994=CARTESIAN_POINT('Ctrl Pts',(37.410231376825,4.94981967975265,-50.8257244285334));
#39995=CARTESIAN_POINT('Ctrl Pts',(37.4196070999113,4.94972177133796,-50.7949479162553));
#39996=CARTESIAN_POINT('Ctrl Pts',(37.4288894174247,4.94958125584787,-50.7640501489819));
#39997=CARTESIAN_POINT('Ctrl Pts',(37.4743950672278,4.94889239246057,-50.6125768800247));
#39998=CARTESIAN_POINT('Ctrl Pts',(37.517656483668,4.94717786909833,-50.4581937142545));
#39999=CARTESIAN_POINT('Ctrl Pts',(37.5587354913008,4.94452707813926,-50.3000098640844));
#40000=CARTESIAN_POINT('Ctrl Pts',(37.5893664918137,4.94255048756646,-50.1820583877729));
#40001=CARTESIAN_POINT('Ctrl Pts',(37.618784061382,4.94006319661273,-50.0620609190039));
#40002=CARTESIAN_POINT('Ctrl Pts',(37.6468085603049,4.93721482921126,-49.9412776473568));
#40003=CARTESIAN_POINT('Ctrl Pts',(37.6746737760593,4.93438265110852,-49.8211808729869));
#40004=CARTESIAN_POINT('Ctrl Pts',(37.7011616853365,4.931194526339,-49.7003073206902));
#40005=CARTESIAN_POINT('Ctrl Pts',(37.7261170122967,4.92779364152766,-49.579942038672));
#40006=CARTESIAN_POINT('Ctrl Pts',(37.7408671357427,4.92578351074985,-49.5087988005482));
#40007=CARTESIAN_POINT('Ctrl Pts',(37.7550822582431,4.923698898499,-49.4378340007195));
#40008=CARTESIAN_POINT('Ctrl Pts',(37.7687338082478,4.92156650463797,-49.3673203123641));
#40009=CARTESIAN_POINT('Ctrl Pts',(37.7773608907145,4.9202189406116,-49.3227592622079));
#40010=CARTESIAN_POINT('Ctrl Pts',(37.7857562022919,4.9188575258676,-49.2784542891617));
#40011=CARTESIAN_POINT('Ctrl Pts',(37.7939305095075,4.91748741564007,-49.2344038995284));
#40012=CARTESIAN_POINT('Ctrl Pts',(37.8199143669757,4.91313221489596,-49.0943799176225));
#40013=CARTESIAN_POINT('Ctrl Pts',(37.843666168356,4.90869138538402,-48.9569322895143));
#40014=CARTESIAN_POINT('Ctrl Pts',(37.865517087473,4.9043315399468,-48.8221395022688));
#40015=CARTESIAN_POINT('Ctrl Pts',(37.8859210597262,4.90026039928434,-48.69627256385));
#40016=CARTESIAN_POINT('Ctrl Pts',(37.9046673858781,4.89625931178411,-48.5727196058065));
#40017=CARTESIAN_POINT('Ctrl Pts',(37.9220149739313,4.89244366591783,-48.4515107005609));
#40018=CARTESIAN_POINT('Ctrl Pts',(37.9342485601373,4.88975285769171,-48.3660337116726));
#40019=CARTESIAN_POINT('Ctrl Pts',(37.9457864755788,4.88715352624105,-48.2817167006948));
#40020=CARTESIAN_POINT('Ctrl Pts',(37.9567236321371,4.88466346217324,-48.1982533436109));
#40021=CARTESIAN_POINT('Ctrl Pts',(37.962989829765,4.88323683602303,-48.1504348921342));
#40022=CARTESIAN_POINT('Ctrl Pts',(37.9690587532084,4.88184608572439,-48.1028976671077));
#40023=CARTESIAN_POINT('Ctrl Pts',(37.9749476898649,4.88049461981221,-48.055591658421));
#40024=CARTESIAN_POINT('Ctrl Pts',(37.9814496169309,4.87900247729043,-48.0033614789831));
#40025=CARTESIAN_POINT('Ctrl Pts',(37.9877319798698,4.87755856000559,-47.9514181081798));
#40026=CARTESIAN_POINT('Ctrl Pts',(37.9938059210639,4.8761962760931,-47.9001933518132));
#40027=CARTESIAN_POINT('Ctrl Pts',(38.0000321368439,4.8747998395255,-47.847684383381));
#40028=CARTESIAN_POINT('Ctrl Pts',(38.0060393577986,4.87348916692692,-47.7959304224487));
#40029=CARTESIAN_POINT('Ctrl Pts',(38.0118410068565,4.87229617339883,-47.7453415826759));
#40030=CARTESIAN_POINT('Ctrl Pts',(38.0151649334287,4.87161267413012,-47.7163578252825));
#40031=CARTESIAN_POINT('Ctrl Pts',(38.0184214069431,4.8709677295453,-47.687755518355));
#40032=CARTESIAN_POINT('Ctrl Pts',(38.0216131392841,4.87036678928707,-47.65960415993));
#40033=CARTESIAN_POINT('Ctrl Pts',(38.0216374408772,4.87036221377633,-47.6593898177534));
#40034=CARTESIAN_POINT('Ctrl Pts',(38.0216617394702,4.87035763848295,-47.6591754855729));
#40035=CARTESIAN_POINT('Ctrl Pts',(38.0216860350653,4.87035306340718,-47.6589611633871));
#40036=CARTESIAN_POINT('',(38.8604541099242,4.82976572790836,-41.6539325852788));
#40037=CARTESIAN_POINT('Ctrl Pts',(38.0216847782692,4.87035252387637,-47.6589606733005));
#40038=CARTESIAN_POINT('Ctrl Pts',(38.0531429489832,4.8650107124254,-47.3901353023222));
#40039=CARTESIAN_POINT('Ctrl Pts',(38.0789292235204,4.86042782994193,-47.1515865306677));
#40040=CARTESIAN_POINT('Ctrl Pts',(38.1330392026837,4.85049018544439,-46.6247656528001));
#40041=CARTESIAN_POINT('Ctrl Pts',(38.1596864519082,4.8456555010739,-46.3559543002791));
#40042=CARTESIAN_POINT('Ctrl Pts',(38.2427598130137,4.83283230623519,-45.5385385890846));
#40043=CARTESIAN_POINT('Ctrl Pts',(38.2941022354012,4.82771455234146,-45.0623082156166));
#40044=CARTESIAN_POINT('Ctrl Pts',(38.4970335348424,4.81981565007625,-43.495441392056));
#40045=CARTESIAN_POINT('Ctrl Pts',(38.6580818054566,4.82748306299288,-42.6038309561148));
#40046=CARTESIAN_POINT('Ctrl Pts',(38.8604349389735,4.8298193957887,-41.6539286669107));
#40047=CARTESIAN_POINT('',(40.1355627916624,4.76730435185959,-35.666088699485));
#40048=CARTESIAN_POINT('Ctrl Pts',(38.8604541099242,4.82976572790836,-41.6539325852788));
#40049=CARTESIAN_POINT('Ctrl Pts',(39.0048197292983,4.83127154325761,-40.9682358462176));
#40050=CARTESIAN_POINT('Ctrl Pts',(39.2693233059464,4.83474737532154,-39.8104175938772));
#40051=CARTESIAN_POINT('Ctrl Pts',(39.6452981730948,4.8199494242592,-38.1129891991618));
#40052=CARTESIAN_POINT('Ctrl Pts',(39.8853277117453,4.79858865457864,-36.9461294764195));
#40053=CARTESIAN_POINT('Ctrl Pts',(40.0280907705529,4.78204396051868,-36.2245904908727));
#40054=CARTESIAN_POINT('Ctrl Pts',(40.1031985714104,4.7719144148413,-35.8353019842399));
#40055=CARTESIAN_POINT('Ctrl Pts',(40.1355627919427,4.76730435097364,-35.6660886995628));
#40056=CARTESIAN_POINT('',(41.4215456143027,4.68791021227265,-29.7512571116574));
#40057=CARTESIAN_POINT('Ctrl Pts',(40.1355627919427,4.76730435097364,-35.6660886995628));
#40058=CARTESIAN_POINT('Ctrl Pts',(40.302285441518,4.74136007283982,-34.7693736439926));
#40059=CARTESIAN_POINT('Ctrl Pts',(40.511283714206,4.72982184735761,-33.6344138386462));
#40060=CARTESIAN_POINT('Ctrl Pts',(40.7814488661554,4.71765074492916,-32.2936083574543));
#40061=CARTESIAN_POINT('Ctrl Pts',(40.942076978619,4.71061953663584,-31.5521512150188));
#40062=CARTESIAN_POINT('Ctrl Pts',(41.140790301564,4.70106929600114,-30.7187864537994));
#40063=CARTESIAN_POINT('Ctrl Pts',(41.3201726461196,4.69236271641177,-30.0753227275525));
#40064=CARTESIAN_POINT('Ctrl Pts',(41.4215456143027,4.68791021227266,-29.7512571116574));
#40065=CARTESIAN_POINT('',(44.8643748761838,5.20597739866059,-23.980151972059));
#40066=CARTESIAN_POINT('Ctrl Pts',(41.4215456143027,4.68791021227266,-29.7512571116574));
#40067=CARTESIAN_POINT('Ctrl Pts',(41.4802706020203,4.68413040514277,-29.5553552623875));
#40068=CARTESIAN_POINT('Ctrl Pts',(41.6778820652349,4.68063495532933,-28.9529142456678));
#40069=CARTESIAN_POINT('Ctrl Pts',(42.0667678924717,4.70419304693246,-27.964824273678));
#40070=CARTESIAN_POINT('Ctrl Pts',(42.6729216974824,4.823611553925,-26.7992794766923));
#40071=CARTESIAN_POINT('Ctrl Pts',(43.1602150679141,4.93691815783542,-26.0485095188922));
#40072=CARTESIAN_POINT('Ctrl Pts',(43.3508405942975,4.97964296442833,-25.7696090237298));
#40073=CARTESIAN_POINT('Ctrl Pts',(43.6185109451061,5.03817773651984,-25.3933166689187));
#40074=CARTESIAN_POINT('Ctrl Pts',(44.1126562896923,5.13439651094732,-24.7624182520843));
#40075=CARTESIAN_POINT('Ctrl Pts',(44.5974177071842,5.19048925540186,-24.2398142598933));
#40076=CARTESIAN_POINT('Ctrl Pts',(44.864374876377,5.20597739807143,-23.9801519722225));
#40077=CARTESIAN_POINT('',(57.8135230789767,6.69056632316042,-18.0349157106052));
#40078=CARTESIAN_POINT('Ctrl Pts',(44.864374876377,5.20597739807143,-23.9801519722225));
#40079=CARTESIAN_POINT('Ctrl Pts',(45.1224142763232,5.22734724195968,-23.7522227177446));
#40080=CARTESIAN_POINT('Ctrl Pts',(45.9649684987856,5.22804284539893,-23.0069752550256));
#40081=CARTESIAN_POINT('Ctrl Pts',(47.4758616466553,5.06915938849053,-21.7520512140078));
#40082=CARTESIAN_POINT('Ctrl Pts',(49.1569256056527,5.20366478491719,-20.7106555371184));
#40083=CARTESIAN_POINT('Ctrl Pts',(50.0106311017377,5.31735504507218,-20.255161743136));
#40084=CARTESIAN_POINT('Ctrl Pts',(50.9536821648416,5.47540829520537,-19.8330327894735));
#40085=CARTESIAN_POINT('Ctrl Pts',(52.3106429243915,5.72884656211269,-19.3291250816917));
#40086=CARTESIAN_POINT('Ctrl Pts',(54.584459674483,6.15313027810468,-18.7389663173459));
#40087=CARTESIAN_POINT('Ctrl Pts',(56.7527899477957,6.52682846803759,-18.2841549642181));
#40088=CARTESIAN_POINT('Ctrl Pts',(57.8135230791049,6.69056632259679,-18.0349157107808));
#40089=CARTESIAN_POINT('',(70.7282577520135,8.51486332053725,-11.8925191843911));
#40090=CARTESIAN_POINT('Ctrl Pts',(57.8135230791049,6.6905663225968,-18.0349157107808));
#40091=CARTESIAN_POINT('Ctrl Pts',(58.3834371192583,6.78492400902022,-17.921496800064));
#40092=CARTESIAN_POINT('Ctrl Pts',(60.069006328368,7.0315326697423,-17.5237672087188));
#40093=CARTESIAN_POINT('Ctrl Pts',(62.2034160825709,7.1647901104433,-16.747451663188));
#40094=CARTESIAN_POINT('Ctrl Pts',(64.7264374328703,7.37946418630416,-15.4764719489058));
#40095=CARTESIAN_POINT('Ctrl Pts',(66.8940351574184,7.74903378142021,-14.2111203469359));
#40096=CARTESIAN_POINT('Ctrl Pts',(68.5152601688859,8.12096232366399,-13.2306538995856));
#40097=CARTESIAN_POINT('Ctrl Pts',(69.7958454230149,8.37193054851245,-12.4618050355517));
#40098=CARTESIAN_POINT('Ctrl Pts',(70.4319511017933,8.47390908124125,-12.0750795994181));
#40099=CARTESIAN_POINT('Ctrl Pts',(70.7282577522084,8.51486331986406,-11.8925191845565));
#40100=CARTESIAN_POINT('',(77.5413122691233,9.45942207531685,-5.67964638243729));
#40101=CARTESIAN_POINT('Ctrl Pts',(70.7282577522084,8.51486331986405,-11.8925191845565));
#40102=CARTESIAN_POINT('Ctrl Pts',(71.1586139886749,8.57802101438411,-11.6423301611079));
#40103=CARTESIAN_POINT('Ctrl Pts',(71.9827018728919,8.65468599963629,-11.0972577103214));
#40104=CARTESIAN_POINT('Ctrl Pts',(73.1303575054126,8.72650011278445,-10.21988802762));
#40105=CARTESIAN_POINT('Ctrl Pts',(74.1065736572356,8.81331425878696,-9.37805983947955));
#40106=CARTESIAN_POINT('Ctrl Pts',(75.1777989853639,8.95359154800345,-8.37681652932542));
#40107=CARTESIAN_POINT('Ctrl Pts',(76.3760621018627,9.18465108771821,-7.13733271471052));
#40108=CARTESIAN_POINT('Ctrl Pts',(77.1569389883271,9.37730603443782,-6.18970317121555));
#40109=CARTESIAN_POINT('Ctrl Pts',(77.5413122691233,9.45942207531684,-5.67964638243731));
#40110=CARTESIAN_POINT('',(79.5980561166602,9.79488102651321,-1.92025417898536));
#40111=CARTESIAN_POINT('Ctrl Pts',(77.5413122691233,9.45942207531684,-5.67964638243731));
#40112=CARTESIAN_POINT('Ctrl Pts',(78.375913647818,9.63522559747283,-4.55505891458532));
#40113=CARTESIAN_POINT('Ctrl Pts',(79.119383339007,9.77540103482857,-3.21481989604027));
#40114=CARTESIAN_POINT('Ctrl Pts',(79.5980561168973,9.79488102600527,-1.92025417906537));
#40115=CARTESIAN_POINT('',(73.6764401502847,5.16864402629879,0.190816765641456));
#40116=CARTESIAN_POINT('Ctrl Pts',(79.5980561168973,9.79488102600527,-1.92025417906537));
#40117=CARTESIAN_POINT('Ctrl Pts',(79.1741566879662,9.55093781207194,-1.62747314540123));
#40118=CARTESIAN_POINT('Ctrl Pts',(78.5111339416338,9.08098342033927,-1.27556034622203));
#40119=CARTESIAN_POINT('Ctrl Pts',(77.4831763160976,8.21812193305731,-0.881741433435836));
#40120=CARTESIAN_POINT('Ctrl Pts',(76.6699028312841,7.50475073429994,-0.627389809719394));
#40121=CARTESIAN_POINT('Ctrl Pts',(75.80573025497,6.75707546613834,-0.393749096424453));
#40122=CARTESIAN_POINT('Ctrl Pts',(75.0458066034774,6.13922536294966,-0.198996877529824));
#40123=CARTESIAN_POINT('Ctrl Pts',(74.3631359901759,5.6296023451996,-0.0144922142290973));
#40124=CARTESIAN_POINT('Ctrl Pts',(73.9161602099363,5.32222124600158,0.115689882622076));
#40125=CARTESIAN_POINT('Ctrl Pts',(73.6764877132773,5.1685596047474,0.19079632099573));
#40126=CARTESIAN_POINT('',(66.7632138022084,3.27206535817644,6.63309335729773));
#40127=CARTESIAN_POINT('Ctrl Pts',(73.6755257075894,5.17026710901218,0.191209832939039));
#40128=CARTESIAN_POINT('Ctrl Pts',(73.5820796918697,5.11091856903798,0.219589144636978));
#40129=CARTESIAN_POINT('Ctrl Pts',(73.4858752309367,5.0511962114572,0.249512021491082));
#40130=CARTESIAN_POINT('Ctrl Pts',(73.3869816798903,4.9913985445888,0.281309980862911));
#40131=CARTESIAN_POINT('Ctrl Pts',(73.2902869491031,4.93293043177097,0.312400937639211));
#40132=CARTESIAN_POINT('Ctrl Pts',(73.191021158279,4.87439026430786,0.345284932597864));
#40133=CARTESIAN_POINT('Ctrl Pts',(73.089263706746,4.81610240265113,0.380260242493337));
#40134=CARTESIAN_POINT('Ctrl Pts',(72.9903546154458,4.75944611514159,0.414256535320878));
#40135=CARTESIAN_POINT('Ctrl Pts',(72.8890911547841,4.70302833913953,0.450229099490815));
#40136=CARTESIAN_POINT('Ctrl Pts',(72.7855635481439,4.64718964924717,0.488434895496889));
#40137=CARTESIAN_POINT('Ctrl Pts',(72.7308024362584,4.61765367479579,0.508643919327953));
#40138=CARTESIAN_POINT('Ctrl Pts',(72.6754081532722,4.58828044060218,0.529477456516567));
#40139=CARTESIAN_POINT('Ctrl Pts',(72.6193965038322,4.55912510610204,0.550970931020803));
#40140=CARTESIAN_POINT('Ctrl Pts',(72.5261115336594,4.51056816238732,0.586767379582583));
#40141=CARTESIAN_POINT('Ctrl Pts',(72.4310749804319,4.46259978603407,0.624408249719697));
#40142=CARTESIAN_POINT('Ctrl Pts',(72.3347504347956,4.4156675454695,0.663888051858643));
#40143=CARTESIAN_POINT('Ctrl Pts',(72.2418625645885,4.37040975742295,0.701959290219107));
#40144=CARTESIAN_POINT('Ctrl Pts',(72.1477772313745,4.32611625075105,0.741740417083424));
#40145=CARTESIAN_POINT('Ctrl Pts',(72.0529368199214,4.28315485360461,0.783206316147256));
#40146=CARTESIAN_POINT('Ctrl Pts',(71.962539835658,4.242206267635,0.822729470546409));
#40147=CARTESIAN_POINT('Ctrl Pts',(71.8714571976677,4.20246836735063,0.863782979464733));
#40148=CARTESIAN_POINT('Ctrl Pts',(71.7800923301779,4.16422001174982,0.9063294470121));
#40149=CARTESIAN_POINT('Ctrl Pts',(71.7368716737269,4.14612641535269,0.926456289064087));
#40150=CARTESIAN_POINT('Ctrl Pts',(71.6935881326869,4.12836551900764,0.946917017120839));
#40151=CARTESIAN_POINT('Ctrl Pts',(71.6502857816389,4.11096308649717,0.967706624656799));
#40152=CARTESIAN_POINT('Ctrl Pts',(71.5726520176656,4.0797634794231,1.00497886150965));
#40153=CARTESIAN_POINT('Ctrl Pts',(71.4949576430323,4.04971750824251,1.04330805975467));
#40154=CARTESIAN_POINT('Ctrl Pts',(71.4174691269399,4.02087317004293,1.08266200151297));
#40155=CARTESIAN_POINT('Ctrl Pts',(71.3536327008094,3.9971106880957,1.11508248292992));
#40156=CARTESIAN_POINT('Ctrl Pts',(71.2899407935869,3.97416790693136,1.14820120033015));
#40157=CARTESIAN_POINT('Ctrl Pts',(71.2269259559942,3.95219042132279,1.18171128723549));
#40158=CARTESIAN_POINT('Ctrl Pts',(71.1894170622134,3.93910856306922,1.20165780044306));
#40159=CARTESIAN_POINT('Ctrl Pts',(71.1521481315531,3.92636766968791,1.22174306636928));
#40160=CARTESIAN_POINT('Ctrl Pts',(71.1152315400551,3.91398981467949,1.24190348951963));
#40161=CARTESIAN_POINT('Ctrl Pts',(71.0354159426054,3.88722824616644,1.28549137651809));
#40162=CARTESIAN_POINT('Ctrl Pts',(70.9572542145306,3.86215910818005,1.32942580059498));
#40163=CARTESIAN_POINT('Ctrl Pts',(70.8804278798133,3.83851758671466,1.37384802610265));
#40164=CARTESIAN_POINT('Ctrl Pts',(70.8620232274237,3.83285398209086,1.38448989287729));
#40165=CARTESIAN_POINT('Ctrl Pts',(70.8436951679833,3.82727254040222,1.39515976751782));
#40166=CARTESIAN_POINT('Ctrl Pts',(70.8254392477934,3.82177004629204,1.40585961048212));
#40167=CARTESIAN_POINT('Ctrl Pts',(70.714142899413,3.78822435289081,1.47109069375712));
#40168=CARTESIAN_POINT('Ctrl Pts',(70.6055211244504,3.75761012028982,1.53744133052309));
#40169=CARTESIAN_POINT('Ctrl Pts',(70.4997817703001,3.7295890075074,1.60467058390328));
#40170=CARTESIAN_POINT('Ctrl Pts',(70.4260311776581,3.71004497216883,1.6515613306788));
#40171=CARTESIAN_POINT('Ctrl Pts',(70.3536820295784,3.69176235831917,1.69888024428319));
#40172=CARTESIAN_POINT('Ctrl Pts',(70.2827935127124,3.67462778803868,1.74655537625686));
#40173=CARTESIAN_POINT('Ctrl Pts',(70.1816200961733,3.65017300900184,1.8145982159011));
#40174=CARTESIAN_POINT('Ctrl Pts',(70.0834250059408,3.62805484101416,1.88336363179219));
#40175=CARTESIAN_POINT('Ctrl Pts',(69.9881855044465,3.60792581144506,1.95274040185771));
#40176=CARTESIAN_POINT('Ctrl Pts',(69.9210193305481,3.59373012709947,2.00166728754712));
#40177=CARTESIAN_POINT('Ctrl Pts',(69.8553223782819,3.58052444170591,2.05089878906696));
#40178=CARTESIAN_POINT('Ctrl Pts',(69.791076817367,3.56819685019557,2.10040256093751));
#40179=CARTESIAN_POINT('Ctrl Pts',(69.7134049543905,3.55329298781217,2.16025183504746));
#40180=CARTESIAN_POINT('Ctrl Pts',(69.6378589189134,3.53967072030751,2.22049587198181));
#40181=CARTESIAN_POINT('Ctrl Pts',(69.5640380577044,3.52709664497903,2.28126322686332));
#40182=CARTESIAN_POINT('Ctrl Pts',(69.5271276270999,3.52080960731478,2.31164690430409));
#40183=CARTESIAN_POINT('Ctrl Pts',(69.4906482126204,3.51478661703879,2.34216143218193));
#40184=CARTESIAN_POINT('Ctrl Pts',(69.4550109833168,3.50906985735859,2.3725916283862));
#40185=CARTESIAN_POINT('Ctrl Pts',(69.4193737540132,3.5033530976784,2.40302182459044));
#40186=CARTESIAN_POINT('Ctrl Pts',(69.3845790920987,3.49793934079213,2.43336770489355));
#40187=CARTESIAN_POINT('Ctrl Pts',(69.3498330799623,3.4926920257565,2.46398464800622));
#40188=CARTESIAN_POINT('Ctrl Pts',(69.2896247814923,3.48359941655028,2.5170380471109));
#40189=CARTESIAN_POINT('Ctrl Pts',(69.2296102593908,3.47501734135315,2.57085342398526));
#40190=CARTESIAN_POINT('Ctrl Pts',(69.1694253615057,3.46685718341993,2.62639316269928));
#40191=CARTESIAN_POINT('Ctrl Pts',(69.1069888381267,3.45839173927236,2.68401074313119));
#40192=CARTESIAN_POINT('Ctrl Pts',(69.0443685754615,3.45038104759951,2.74348439598306));
#40193=CARTESIAN_POINT('Ctrl Pts',(68.9811856468568,3.44276220137922,2.80585531536981));
#40194=CARTESIAN_POINT('Ctrl Pts',(68.9168073375991,3.43499921145475,2.86940625271379));
#40195=CARTESIAN_POINT('Ctrl Pts',(68.8518446835568,3.4276440543443,2.93596529709815));
#40196=CARTESIAN_POINT('Ctrl Pts',(68.7859294095244,3.42065385850673,3.00659652686413));
#40197=CARTESIAN_POINT('Ctrl Pts',(68.718344605385,3.41348661201471,3.07901673447066));
#40198=CARTESIAN_POINT('Ctrl Pts',(68.6497584139789,3.40670451572753,3.15571813494658));
#40199=CARTESIAN_POINT('Ctrl Pts',(68.5798088336028,3.40026713156069,3.23780643100444));
#40200=CARTESIAN_POINT('Ctrl Pts',(68.5515071958064,3.39766256246869,3.27101939968653));
#40201=CARTESIAN_POINT('Ctrl Pts',(68.5229827499876,3.39511436007263,3.30511374067851));
#40202=CARTESIAN_POINT('Ctrl Pts',(68.4942129036598,3.39261916495141,3.34016082576519));
#40203=CARTESIAN_POINT('Ctrl Pts',(68.4619893586378,3.38982443218114,3.37941516558042));
#40204=CARTESIAN_POINT('Ctrl Pts',(68.4294149535231,3.38709221292072,3.41988751388573));
#40205=CARTESIAN_POINT('Ctrl Pts',(68.3965806450077,3.38442708502318,3.46156378462874));
#40206=CARTESIAN_POINT('Ctrl Pts',(68.347076532678,3.38040888586572,3.52439887638567));
#40207=CARTESIAN_POINT('Ctrl Pts',(68.2969825696369,3.37654398048543,3.58997028569425));
#40208=CARTESIAN_POINT('Ctrl Pts',(68.2465830018763,3.37283705789084,3.65823607603959));
#40209=CARTESIAN_POINT('Ctrl Pts',(68.1859376180816,3.3683765485366,3.74037973796942));
#40210=CARTESIAN_POINT('Ctrl Pts',(68.1248508938036,3.36414515624265,3.82642422986708));
#40211=CARTESIAN_POINT('Ctrl Pts',(68.0637806680368,3.36012805833028,3.91630856639725));
#40212=CARTESIAN_POINT('Ctrl Pts',(68.0020010445552,3.35606429741571,4.00723700817083));
#40213=CARTESIAN_POINT('Ctrl Pts',(67.9402384693474,3.35221938996863,4.10209499325176));
#40214=CARTESIAN_POINT('Ctrl Pts',(67.8789232542081,3.34855084749676,4.2008365426439));
#40215=CARTESIAN_POINT('Ctrl Pts',(67.8157330182447,3.34477012090365,4.30259761110501));
#40216=CARTESIAN_POINT('Ctrl Pts',(67.7530181004581,3.34117618230318,4.40848346717966));
#40217=CARTESIAN_POINT('Ctrl Pts',(67.6912005113719,3.33770132789118,4.51846170635032));
#40218=CARTESIAN_POINT('Ctrl Pts',(67.647034253233,3.33521867984191,4.5970368719735));
#40219=CARTESIAN_POINT('Ctrl Pts',(67.6033249805881,3.33279635196203,4.67770142782428));
#40220=CARTESIAN_POINT('Ctrl Pts',(67.560211592247,3.33040570470243,4.7604482025443));
#40221=CARTESIAN_POINT('Ctrl Pts',(67.5030340789018,3.32723519848964,4.87018800722854));
#40222=CARTESIAN_POINT('Ctrl Pts',(67.4469958924026,3.32412842972577,4.9836052813711));
#40223=CARTESIAN_POINT('Ctrl Pts',(67.3922782031099,3.32097851832306,5.09928652163564));
#40224=CARTESIAN_POINT('Ctrl Pts',(67.3817314770598,3.32037137914968,5.12158385118265));
#40225=CARTESIAN_POINT('Ctrl Pts',(67.3712337501578,3.31976269008265,5.14396542535823));
#40226=CARTESIAN_POINT('Ctrl Pts',(67.3607862519462,3.31915177658107,5.16642130746712));
#40227=CARTESIAN_POINT('Ctrl Pts',(67.3039017197311,3.3158254751013,5.28868908137495));
#40228=CARTESIAN_POINT('Ctrl Pts',(67.2485058467987,3.31242967257486,5.41315817519173));
#40229=CARTESIAN_POINT('Ctrl Pts',(67.1947972253839,3.30887182807225,5.5383406212005));
#40230=CARTESIAN_POINT('Ctrl Pts',(67.1753348086868,3.30758257039947,5.58370303906188));
#40231=CARTESIAN_POINT('Ctrl Pts',(67.1560940283144,3.30627247758143,5.629159280694));
#40232=CARTESIAN_POINT('Ctrl Pts',(67.137084892584,3.30493882395428,5.67463873313827));
#40233=CARTESIAN_POINT('Ctrl Pts',(67.1054532744659,3.30271959511434,5.7503175379157));
#40234=CARTESIAN_POINT('Ctrl Pts',(67.0744664739271,3.30044219646204,5.8265021274338));
#40235=CARTESIAN_POINT('Ctrl Pts',(67.0439283533832,3.2980713592277,5.90308348319905));
#40236=CARTESIAN_POINT('Ctrl Pts',(67.0104544275529,3.29547259976495,5.98702704544908));
#40237=CARTESIAN_POINT('Ctrl Pts',(66.977519486075,3.29276151625854,6.07144315063479));
#40238=CARTESIAN_POINT('Ctrl Pts',(66.9448701424927,3.28989842821305,6.15588714158495));
#40239=CARTESIAN_POINT('Ctrl Pts',(66.9303273345756,3.28862313949581,6.19350053914223));
#40240=CARTESIAN_POINT('Ctrl Pts',(66.9158412634233,3.28731774542639,6.23112011639764));
#40241=CARTESIAN_POINT('Ctrl Pts',(66.901389897882,3.28597900649281,6.26870995157757));
#40242=CARTESIAN_POINT('Ctrl Pts',(66.8814989574804,3.284136358733,6.32044881107371));
#40243=CARTESIAN_POINT('Ctrl Pts',(66.8616737379568,3.28223055848634,6.37213594417084));
#40244=CARTESIAN_POINT('Ctrl Pts',(66.8418573733355,3.28025518624225,6.42417246121676));
#40245=CARTESIAN_POINT('Ctrl Pts',(66.822565995373,3.27833214670874,6.47483039658318));
#40246=CARTESIAN_POINT('Ctrl Pts',(66.8032830102522,3.27634316919812,6.52581955560616));
#40247=CARTESIAN_POINT('Ctrl Pts',(66.7839566804709,3.27428245778291,6.57746051724003));
#40248=CARTESIAN_POINT('Ctrl Pts',(66.7770581476665,3.27354688690841,6.5958937568626));
#40249=CARTESIAN_POINT('Ctrl Pts',(66.770154099003,3.27280217762856,6.61440956897775));
#40250=CARTESIAN_POINT('Ctrl Pts',(66.7632422045598,3.27204807172044,6.63302090600835));
#40251=CARTESIAN_POINT('',(64.4551540394283,2.94901890714283,12.6430799879059));
#40252=CARTESIAN_POINT('Ctrl Pts',(66.7626079618727,3.27243408934811,6.63463878967692));
#40253=CARTESIAN_POINT('Ctrl Pts',(66.7582438740882,3.27195413689024,6.64675428470166));
#40254=CARTESIAN_POINT('Ctrl Pts',(66.7538841597794,3.27147418576871,6.65888415304361));
#40255=CARTESIAN_POINT('Ctrl Pts',(66.7495284430053,3.27099416305559,6.67102845311044));
#40256=CARTESIAN_POINT('Ctrl Pts',(66.744846305267,3.27047816704921,6.68408285691971));
#40257=CARTESIAN_POINT('Ctrl Pts',(66.7401657718722,3.26996175625489,6.69716233557186));
#40258=CARTESIAN_POINT('Ctrl Pts',(66.7354845820625,3.26944463942253,6.71027211865419));
#40259=CARTESIAN_POINT('Ctrl Pts',(66.6809666044278,3.26342220387788,6.8629510079821));
#40260=CARTESIAN_POINT('Ctrl Pts',(66.6264369335311,3.25731251986083,7.01953283719209));
#40261=CARTESIAN_POINT('Ctrl Pts',(66.571060967788,3.25095694222195,7.18059086773355));
#40262=CARTESIAN_POINT('Ctrl Pts',(66.5446749256618,3.24792857897688,7.2573332580759));
#40263=CARTESIAN_POINT('Ctrl Pts',(66.5180964371422,3.24484435668027,7.3350913428522));
#40264=CARTESIAN_POINT('Ctrl Pts',(66.4912348586684,3.2416871768498,7.41392273497785));
#40265=CARTESIAN_POINT('Ctrl Pts',(66.4405666300019,3.23573187866256,7.56262013957055));
#40266=CARTESIAN_POINT('Ctrl Pts',(66.3888905563711,3.22951681633887,7.71513726506168));
#40267=CARTESIAN_POINT('Ctrl Pts',(66.3355831927921,3.22293399710941,7.87189817464005));
#40268=CARTESIAN_POINT('Ctrl Pts',(66.308765753888,3.2196223654576,7.95076018980873));
#40269=CARTESIAN_POINT('Ctrl Pts',(66.2815357166608,3.21621771829495,8.03069556540575));
#40270=CARTESIAN_POINT('Ctrl Pts',(66.2538159346678,3.21270677850378,8.11175363983937));
#40271=CARTESIAN_POINT('Ctrl Pts',(66.1991717354852,3.20578563845603,8.2715439861641));
#40272=CARTESIAN_POINT('Ctrl Pts',(66.1426207789929,3.19846053540797,8.4357013913799));
#40273=CARTESIAN_POINT('Ctrl Pts',(66.0835682271523,3.19060269005156,8.60465395408236));
#40274=CARTESIAN_POINT('Ctrl Pts',(66.0617317921506,3.18769701834,8.66712918231278));
#40275=CARTESIAN_POINT('Ctrl Pts',(66.0395535824283,3.18471855611422,8.73025968650451));
#40276=CARTESIAN_POINT('Ctrl Pts',(66.0170046138161,3.18166100123051,8.79406563030403));
#40277=CARTESIAN_POINT('Ctrl Pts',(65.9943401000079,3.17858777885512,8.85819852787281));
#40278=CARTESIAN_POINT('Ctrl Pts',(65.9713403757572,3.17544058934947,8.92290296450967));
#40279=CARTESIAN_POINT('Ctrl Pts',(65.9479113350192,3.17220436938723,8.98838307743012));
#40280=CARTESIAN_POINT('Ctrl Pts',(65.9119955708399,3.1672433761355,9.08876142071671));
#40281=CARTESIAN_POINT('Ctrl Pts',(65.8750725641278,3.16207354628284,9.19096145543401));
#40282=CARTESIAN_POINT('Ctrl Pts',(65.8371161191711,3.15668978690338,9.29487750489127));
#40283=CARTESIAN_POINT('Ctrl Pts',(65.8192619842666,3.1541573483053,9.34375803540111));
#40284=CARTESIAN_POINT('Ctrl Pts',(65.8011786230049,3.15157745031492,9.39301896048947));
#40285=CARTESIAN_POINT('Ctrl Pts',(65.7828612214198,3.14894903800416,9.44264976966276));
#40286=CARTESIAN_POINT('Ctrl Pts',(65.7719027971886,3.14737658478136,9.47234150619706));
#40287=CARTESIAN_POINT('Ctrl Pts',(65.7608572760255,3.14578636360764,9.50217457066608));
#40288=CARTESIAN_POINT('Ctrl Pts',(65.7497218072676,3.14417797450116,9.53215067526452));
#40289=CARTESIAN_POINT('Ctrl Pts',(65.7369478785919,3.14233292889279,9.56653742901881));
#40290=CARTESIAN_POINT('Ctrl Pts',(65.7241525267092,3.14047797905138,9.60085143804542));
#40291=CARTESIAN_POINT('Ctrl Pts',(65.7113335685273,3.13861315887182,9.63509460891077));
#40292=CARTESIAN_POINT('Ctrl Pts',(65.675285029997,3.13336904767802,9.73139075457402));
#40293=CARTESIAN_POINT('Ctrl Pts',(65.6389780277389,3.12803839930249,9.82731896967742));
#40294=CARTESIAN_POINT('Ctrl Pts',(65.6024906864775,3.1226370759973,9.92255311418928));
#40295=CARTESIAN_POINT('Ctrl Pts',(65.556412456212,3.11581598653473,10.0428200530305));
#40296=CARTESIAN_POINT('Ctrl Pts',(65.5100459047643,3.1088821443127,10.1619850432727));
#40297=CARTESIAN_POINT('Ctrl Pts',(65.463212531056,3.10183216685072,10.2806741465391));
#40298=CARTESIAN_POINT('Ctrl Pts',(65.3879225999276,3.0904985328299,10.4714802683934));
#40299=CARTESIAN_POINT('Ctrl Pts',(65.3116519243754,3.07889057491832,10.6604749294055));
#40300=CARTESIAN_POINT('Ctrl Pts',(65.234506165267,3.06710243124938,10.8480506983372));
#40301=CARTESIAN_POINT('Ctrl Pts',(65.2117989721025,3.063632692168,10.9032620186656));
#40302=CARTESIAN_POINT('Ctrl Pts',(65.1890159374527,3.06014733840129,10.9583503403728));
#40303=CARTESIAN_POINT('Ctrl Pts',(65.1661480826901,3.05664663471501,11.0133411959318));
#40304=CARTESIAN_POINT('Ctrl Pts',(65.1491066523579,3.05403786364302,11.054321114846));
#40305=CARTESIAN_POINT('Ctrl Pts',(65.1320205196827,3.05142106746363,11.0952410669356));
#40306=CARTESIAN_POINT('Ctrl Pts',(65.1148886686486,3.04879690068722,11.1361052727008));
#40307=CARTESIAN_POINT('Ctrl Pts',(65.0917641754397,3.04525481252177,11.1912635884499));
#40308=CARTESIAN_POINT('Ctrl Pts',(65.0685599925776,3.04170057085351,11.2463115263669));
#40309=CARTESIAN_POINT('Ctrl Pts',(65.0452684027928,3.03813443698347,11.3012725404979));
#40310=CARTESIAN_POINT('Ctrl Pts',(64.9618817011173,3.02536724745703,11.4980396024053));
#40311=CARTESIAN_POINT('Ctrl Pts',(64.8773749226518,3.01244768631303,11.6936927880249));
#40312=CARTESIAN_POINT('Ctrl Pts',(64.7918465919002,2.99946266463069,11.8887146066709));
#40313=CARTESIAN_POINT('Ctrl Pts',(64.6957882909471,2.98487896926703,12.1077468780047));
#40314=CARTESIAN_POINT('Ctrl Pts',(64.5984198280383,2.9702283213973,12.3260248599227));
#40315=CARTESIAN_POINT('Ctrl Pts',(64.4999193330072,2.95563529360733,12.5441356757672));
#40316=CARTESIAN_POINT('Ctrl Pts',(64.4850232036326,2.95342840490227,12.5771203519336));
#40317=CARTESIAN_POINT('Ctrl Pts',(64.4701012223787,2.95122280440128,12.6101011343138));
#40318=CARTESIAN_POINT('Ctrl Pts',(64.4551540394283,2.94901890714283,12.6430799879059));
#40319=CARTESIAN_POINT('',(61.5166583930919,2.54671945820444,18.6669577091217));
#40320=CARTESIAN_POINT('Ctrl Pts',(64.455131965346,2.94901573117602,12.6431286671725));
#40321=CARTESIAN_POINT('Ctrl Pts',(64.3756406866424,2.93729544625666,12.8183754180639));
#40322=CARTESIAN_POINT('Ctrl Pts',(64.2949735702456,2.92553927651984,12.9941893144439));
#40323=CARTESIAN_POINT('Ctrl Pts',(64.1453393500078,2.90398855251153,13.3183226136813));
#40324=CARTESIAN_POINT('Ctrl Pts',(64.0517379200529,2.89064511331178,13.520320295579));
#40325=CARTESIAN_POINT('Ctrl Pts',(63.8113439371817,2.85680317093103,14.0344315980323));
#40326=CARTESIAN_POINT('Ctrl Pts',(63.6411847868847,2.8333580159102,14.392662513831));
#40327=CARTESIAN_POINT('Ctrl Pts',(63.367659946999,2.7962459604253,14.9686646720361));
#40328=CARTESIAN_POINT('Ctrl Pts',(63.2444061328582,2.77968504765282,15.2284282557368));
#40329=CARTESIAN_POINT('Ctrl Pts',(62.886939604599,2.73188620171305,15.9801214605262));
#40330=CARTESIAN_POINT('Ctrl Pts',(62.6232915029037,2.69700497899866,16.53067421596));
#40331=CARTESIAN_POINT('Ctrl Pts',(62.1036482761331,2.6273101994606,17.5771759416381));
#40332=CARTESIAN_POINT('Ctrl Pts',(61.8045070651265,2.58662238128951,18.1611507203481));
#40333=CARTESIAN_POINT('Ctrl Pts',(61.5166583935928,2.54671945895772,18.6669577094661));
#40334=CARTESIAN_POINT('',(49.3675957670801,0.956505486201908,24.6840252059531));
#40335=CARTESIAN_POINT('Ctrl Pts',(61.5166583915077,2.5467194586667,18.6669577089628));
#40336=CARTESIAN_POINT('Ctrl Pts',(61.5166207736063,2.54671424394586,18.6670239120275));
#40337=CARTESIAN_POINT('Ctrl Pts',(61.5165831563685,2.54670902930684,18.6670901132125));
#40338=CARTESIAN_POINT('Ctrl Pts',(61.5165455397943,2.54670381474961,18.6671563125178));
#40339=CARTESIAN_POINT('Ctrl Pts',(61.440598562313,2.53617574652035,18.8008111509416));
#40340=CARTESIAN_POINT('Ctrl Pts',(61.3673089566769,2.52599500692197,18.926675616836));
#40341=CARTESIAN_POINT('Ctrl Pts',(61.2953855126163,2.51598545816718,19.0465923056338));
#40342=CARTESIAN_POINT('Ctrl Pts',(61.2181583162547,2.50523778892978,19.1753518470292));
#40343=CARTESIAN_POINT('Ctrl Pts',(61.1425070165007,2.49468764125461,19.2972541878678));
#40344=CARTESIAN_POINT('Ctrl Pts',(61.0668941562081,2.48412302983043,19.4145920223673));
#40345=CARTESIAN_POINT('Ctrl Pts',(60.9832401113652,2.47243490595301,19.5444083582525));
#40346=CARTESIAN_POINT('Ctrl Pts',(60.899633716831,2.46072921556197,19.6686377804292));
#40347=CARTESIAN_POINT('Ctrl Pts',(60.8140534103825,2.44872366676954,19.7903973547229));
#40348=CARTESIAN_POINT('Ctrl Pts',(60.8085305719405,2.44794890083169,19.7982549855902));
#40349=CARTESIAN_POINT('Ctrl Pts',(60.8029995299401,2.44717288716868,19.8061023341489));
#40350=CARTESIAN_POINT('Ctrl Pts',(60.7974597477827,2.44639555031116,19.8139402396247));
#40351=CARTESIAN_POINT('Ctrl Pts',(60.6275577239221,2.42255506316564,20.0543244217698));
#40352=CARTESIAN_POINT('Ctrl Pts',(60.4492882397345,2.39744916755369,20.285799444722));
#40353=CARTESIAN_POINT('Ctrl Pts',(60.2598484860335,2.37067877124953,20.5074382120966));
#40354=CARTESIAN_POINT('Ctrl Pts',(60.0546114750151,2.34167600908422,20.747559291506));
#40355=CARTESIAN_POINT('Ctrl Pts',(59.8362641090708,2.31071933158198,20.9761348857896));
#40356=CARTESIAN_POINT('Ctrl Pts',(59.6012986958576,2.27731469479028,21.1920080513495));
#40357=CARTESIAN_POINT('Ctrl Pts',(59.5483682209496,2.2697896583803,21.2406376305575));
#40358=CARTESIAN_POINT('Ctrl Pts',(59.4945946258952,2.26214045636031,21.2886227035624));
#40359=CARTESIAN_POINT('Ctrl Pts',(59.4399380897665,2.25436154671837,21.3359502099995));
#40360=CARTESIAN_POINT('Ctrl Pts',(59.3251199132003,2.23802022170907,21.4353721341723));
#40361=CARTESIAN_POINT('Ctrl Pts',(59.2064051575535,2.22110625075009,21.5318921728796));
#40362=CARTESIAN_POINT('Ctrl Pts',(59.0834292363997,2.20357785323861,21.6253876201116));
#40363=CARTESIAN_POINT('Ctrl Pts',(59.0632484738035,2.20070138420669,21.6407305377064));
#40364=CARTESIAN_POINT('Ctrl Pts',(59.0429527992837,2.19780835258924,21.6559919699139));
#40365=CARTESIAN_POINT('Ctrl Pts',(59.0225450240649,2.19489921098158,21.6711714773165));
#40366=CARTESIAN_POINT('Ctrl Pts',(58.8001707963232,2.16319962043547,21.8365756529287));
#40367=CARTESIAN_POINT('Ctrl Pts',(58.5644828709371,2.12958414079278,21.9922525289487));
#40368=CARTESIAN_POINT('Ctrl Pts',(58.3191411311679,2.09465967824874,22.1376328116747));
#40369=CARTESIAN_POINT('Ctrl Pts',(58.2069674438234,2.07869172373037,22.2041027176757));
#40370=CARTESIAN_POINT('Ctrl Pts',(58.0927762566005,2.06245063882631,22.2684201738044));
#40371=CARTESIAN_POINT('Ctrl Pts',(57.9769203136681,2.04599642011994,22.3305308335531));
#40372=CARTESIAN_POINT('Ctrl Pts',(57.7755910457054,2.01740301590426,22.438463955872));
#40373=CARTESIAN_POINT('Ctrl Pts',(57.5692249334683,1.98816219670544,22.5397333935213));
#40374=CARTESIAN_POINT('Ctrl Pts',(57.3531349720908,1.95767600444684,22.6371193347432));
#40375=CARTESIAN_POINT('Ctrl Pts',(57.1479418687527,1.92872715204006,22.7295943547462));
#40376=CARTESIAN_POINT('Ctrl Pts',(56.9339817287562,1.89865408522091,22.8185679023946));
#40377=CARTESIAN_POINT('Ctrl Pts',(56.7072181447654,1.86698155708814,22.9064219236721));
#40378=CARTESIAN_POINT('Ctrl Pts',(56.6795557795455,1.86311789862399,22.9171390325652));
#40379=CARTESIAN_POINT('Ctrl Pts',(56.6517031245348,1.85923055057753,22.9278394762033));
#40380=CARTESIAN_POINT('Ctrl Pts',(56.6238148783573,1.85534126944944,22.9384756468297));
#40381=CARTESIAN_POINT('Ctrl Pts',(56.5343603223993,1.8428659809679,22.9725923106896));
#40382=CARTESIAN_POINT('Ctrl Pts',(56.4445386642837,1.83037181694639,23.0060476860461));
#40383=CARTESIAN_POINT('Ctrl Pts',(56.3594657709293,1.81856838050457,23.037270574256));
#40384=CARTESIAN_POINT('Ctrl Pts',(56.2881077385875,1.80866781210787,23.0634599252799));
#40385=CARTESIAN_POINT('Ctrl Pts',(56.2200877909376,1.79924885481185,23.0880785380807));
#40386=CARTESIAN_POINT('Ctrl Pts',(56.1411095920773,1.78834134685333,23.1157628475816));
#40387=CARTESIAN_POINT('Ctrl Pts',(56.0965756774391,1.78219086437399,23.1313733666099));
#40388=CARTESIAN_POINT('Ctrl Pts',(56.0485570767083,1.77556757273511,23.1479586453918));
#40389=CARTESIAN_POINT('Ctrl Pts',(55.9944861447575,1.76812431597734,23.1663498795247));
#40390=CARTESIAN_POINT('Ctrl Pts',(55.9834762727519,1.76660872707862,23.1700946852183));
#40391=CARTESIAN_POINT('Ctrl Pts',(55.9722155459999,1.76505917553994,23.173914352136));
#40392=CARTESIAN_POINT('Ctrl Pts',(55.9607053836033,1.7634759418204,23.1778074609361));
#40393=CARTESIAN_POINT('Ctrl Pts',(55.8442429111033,1.74745641862258,23.2171988318781));
#40394=CARTESIAN_POINT('Ctrl Pts',(55.7022443876334,1.7279845356483,23.264109262772));
#40395=CARTESIAN_POINT('Ctrl Pts',(55.5361736098594,1.70537682788494,23.3170673603437));
#40396=CARTESIAN_POINT('Ctrl Pts',(55.378986512611,1.68397848191223,23.3671925524134));
#40397=CARTESIAN_POINT('Ctrl Pts',(55.2002330785305,1.65977062163439,23.4227357204199));
#40398=CARTESIAN_POINT('Ctrl Pts',(55.0011514813534,1.63306739719635,23.4824469066612));
#40399=CARTESIAN_POINT('Ctrl Pts',(54.8650711105551,1.61481465694027,23.5232619316547));
#40400=CARTESIAN_POINT('Ctrl Pts',(54.7194928057945,1.59539694607339,23.566024319518));
#40401=CARTESIAN_POINT('Ctrl Pts',(54.5648131060747,1.57492870704247,23.6103341755122));
#40402=CARTESIAN_POINT('Ctrl Pts',(54.3281046519902,1.54360588169681,23.6781421524613));
#40403=CARTESIAN_POINT('Ctrl Pts',(54.0700905768493,1.50982335770047,23.7495805755989));
#40404=CARTESIAN_POINT('Ctrl Pts',(53.7943690560697,1.47432005250733,23.8225022067969));
#40405=CARTESIAN_POINT('Ctrl Pts',(53.4973758221844,1.43607769335773,23.9010496883589));
#40406=CARTESIAN_POINT('Ctrl Pts',(53.1798365176838,1.39584378645511,23.9813174692087));
#40407=CARTESIAN_POINT('Ctrl Pts',(52.8462862359951,1.35449227659147,24.0606355793502));
#40408=CARTESIAN_POINT('Ctrl Pts',(52.647437516317,1.32984023687047,24.1079217173474));
#40409=CARTESIAN_POINT('Ctrl Pts',(52.4428992466314,1.30479073854547,24.1548704602671));
#40410=CARTESIAN_POINT('Ctrl Pts',(52.2336396985611,1.27952382229616,24.2009170329423));
#40411=CARTESIAN_POINT('Ctrl Pts',(51.8629974700757,1.23477085292413,24.2824751002697));
#40412=CARTESIAN_POINT('Ctrl Pts',(51.4775197598703,1.18933379101783,24.3611984471246));
#40413=CARTESIAN_POINT('Ctrl Pts',(51.0806283298492,1.1439453075006,24.4331895149969));
#40414=CARTESIAN_POINT('Ctrl Pts',(51.0384353196498,1.13912011702501,24.4408427915135));
#40415=CARTESIAN_POINT('Ctrl Pts',(50.9961133574418,1.13429544845148,24.4484199862611));
#40416=CARTESIAN_POINT('Ctrl Pts',(50.953666582741,1.12947216046453,24.4559164186186));
#40417=CARTESIAN_POINT('Ctrl Pts',(50.6003160043242,1.08932042662669,24.5183208940646));
#40418=CARTESIAN_POINT('Ctrl Pts',(50.2383145786455,1.04926822505876,24.5751286405623));
#40419=CARTESIAN_POINT('Ctrl Pts',(49.8700363839702,1.00972402104231,24.6236399656901));
#40420=CARTESIAN_POINT('Ctrl Pts',(49.7037634610372,0.991870315658882,24.6455422122553));
#40421=CARTESIAN_POINT('Ctrl Pts',(49.5362113339751,0.974119523575312,24.6657533142736));
#40422=CARTESIAN_POINT('Ctrl Pts',(49.3675995744407,0.956505883929035,24.6840247933719));
#40423=CARTESIAN_POINT('Ctrl Pts',(49.3675983053205,0.956505751353318,24.684024930899));
#40424=CARTESIAN_POINT('Ctrl Pts',(49.3675970362003,0.956505618777609,24.6840250684261));
#40425=CARTESIAN_POINT('Ctrl Pts',(49.3675957670801,0.956505486201908,24.6840252059531));
#40426=CARTESIAN_POINT('',(44.3052665433902,0.501764637226403,24.6839663391593));
#40427=CARTESIAN_POINT('Ctrl Pts',(49.367596314931,0.956500241803234,24.6840252060176));
#40428=CARTESIAN_POINT('Ctrl Pts',(48.9249563174813,0.91026051062961,24.7319912218939));
#40429=CARTESIAN_POINT('Ctrl Pts',(48.2454451876077,0.842024097628023,24.7841312821754));
#40430=CARTESIAN_POINT('Ctrl Pts',(46.6888479202391,0.694486082024801,24.8361224907741));
#40431=CARTESIAN_POINT('Ctrl Pts',(45.4053646426555,0.584777912483909,24.7905806974873));
#40432=CARTESIAN_POINT('Ctrl Pts',(44.3052665433902,0.501764637226404,24.6839663391593));
#40433=CARTESIAN_POINT('',(30.3222847657761,-0.00413284663037694,18.6660068644684));
#40434=CARTESIAN_POINT('Ctrl Pts',(44.3052665433902,0.501764637226404,24.6839663391593));
#40435=CARTESIAN_POINT('Ctrl Pts',(43.5184633083404,0.442392556145283,24.6077156960038));
#40436=CARTESIAN_POINT('Ctrl Pts',(42.2816666702738,0.357564010552012,24.4340698272278));
#40437=CARTESIAN_POINT('Ctrl Pts',(39.7590447329804,0.209255798855571,23.9283169242352));
#40438=CARTESIAN_POINT('Ctrl Pts',(36.2988021098604,0.0624334299665293,
22.7904348263529));
#40439=CARTESIAN_POINT('Ctrl Pts',(33.2830669754168,0.0134785075079505,
20.9642163836828));
#40440=CARTESIAN_POINT('Ctrl Pts',(31.3601866444384,-0.00140202227099839,
19.5546871871865));
#40441=CARTESIAN_POINT('Ctrl Pts',(30.6635153578141,-0.00339250812609648,
18.9682311100362));
#40442=CARTESIAN_POINT('Ctrl Pts',(30.3222847657761,-0.00413284663037694,
18.6660068644684));
#40443=CARTESIAN_POINT('',(25.4512489032773,0.000555756585220059,12.648002570409));
#40444=CARTESIAN_POINT('Ctrl Pts',(30.3222847579815,-0.00412925426626926,
18.6660068644463));
#40445=CARTESIAN_POINT('Ctrl Pts',(29.3243355961853,-0.00630000276266593,
17.7821469838973));
#40446=CARTESIAN_POINT('Ctrl Pts',(28.4882783945593,-0.00480235629088497,
16.8802696648002));
#40447=CARTESIAN_POINT('Ctrl Pts',(27.2613257884266,-0.00266691039312472,
15.2953825351106));
#40448=CARTESIAN_POINT('Ctrl Pts',(26.8875894678604,-0.00191427135626064,
14.7718457182022));
#40449=CARTESIAN_POINT('Ctrl Pts',(26.340767674565,-0.000872705426741305,
13.9769047302795));
#40450=CARTESIAN_POINT('Ctrl Pts',(26.1604061374871,-0.000538421769267547,
13.7098371610195));
#40451=CARTESIAN_POINT('Ctrl Pts',(25.8945556885661,-8.20109892347277E-5,
13.3131630236195));
#40452=CARTESIAN_POINT('Ctrl Pts',(25.8053019634277,6.50220491256103E-5,
13.1794702756233));
#40453=CARTESIAN_POINT('Ctrl Pts',(25.6290023245359,0.000339467860826898,
12.9149907782377));
#40454=CARTESIAN_POINT('Ctrl Pts',(25.5412899884507,0.000468171758386591,
12.783207411861));
#40455=CARTESIAN_POINT('Ctrl Pts',(25.4512489498233,0.000589988472317472,
12.6480025702534));
#40456=CARTESIAN_POINT('',(21.143061504949,0.000717013383189543,6.63001173766479));
#40457=CARTESIAN_POINT('Ctrl Pts',(25.4512489060474,0.000557793871117651,
12.6480025703997));
#40458=CARTESIAN_POINT('Ctrl Pts',(25.2761532109731,0.000795927984841995,
12.3850804994989));
#40459=CARTESIAN_POINT('Ctrl Pts',(25.0385405727546,0.00107944402204348,
12.0284981506081));
#40460=CARTESIAN_POINT('Ctrl Pts',(24.5346770904967,0.00153952329737014,
11.2801401659155));
#40461=CARTESIAN_POINT('Ctrl Pts',(23.7748717062593,0.00195060306715209,
10.1720733370841));
#40462=CARTESIAN_POINT('Ctrl Pts',(22.5874547933106,0.00176250665503241,
8.52818644438044));
#40463=CARTESIAN_POINT('Ctrl Pts',(21.7214346225638,0.00113305483753488,
7.38990420970681));
#40464=CARTESIAN_POINT('Ctrl Pts',(21.143061504949,0.000717013383189635,
6.63001173766479));
#40465=CARTESIAN_POINT('',(16.6859947282585,-0.000213685071588365,0.653010349651272));
#40466=CARTESIAN_POINT('Ctrl Pts',(21.143061504949,0.000717013383189635,
6.63001173766479));
#40467=CARTESIAN_POINT('Ctrl Pts',(21.0596090213757,0.000656984091852039,
6.5204775896832));
#40468=CARTESIAN_POINT('Ctrl Pts',(20.9749493812227,0.000581686629534018,
6.40937966448351));
#40469=CARTESIAN_POINT('Ctrl Pts',(20.8887163398544,0.000503337030319878,
6.29615377755028));
#40470=CARTESIAN_POINT('Ctrl Pts',(20.8782653958811,0.000493841513766926,
6.28243145740597));
#40471=CARTESIAN_POINT('Ctrl Pts',(20.8677913737256,0.000484599446368201,
6.26867792435866));
#40472=CARTESIAN_POINT('Ctrl Pts',(20.8572936227993,0.000475319602753722,
6.25489217579666));
#40473=CARTESIAN_POINT('Ctrl Pts',(20.7639844529272,0.000392835791668964,
6.13235766688846));
#40474=CARTESIAN_POINT('Ctrl Pts',(20.6688013656666,0.00030697584799982,
6.00727901155367));
#40475=CARTESIAN_POINT('Ctrl Pts',(20.5713613914627,0.000230367938072254,
5.87904920835524));
#40476=CARTESIAN_POINT('Ctrl Pts',(20.4390491065871,0.000126343201973351,
5.70492787479612));
#40477=CARTESIAN_POINT('Ctrl Pts',(20.302572845078,4.62809998690632E-5,
5.52499310762258));
#40478=CARTESIAN_POINT('Ctrl Pts',(20.1609437810453,2.88128682006106E-5,
5.33768334477713));
#40479=CARTESIAN_POINT('Ctrl Pts',(20.1049955882517,2.19123749649575E-5,
5.26368975599391));
#40480=CARTESIAN_POINT('Ctrl Pts',(20.0482435177667,2.45223961111146E-5,
5.18854554072461));
#40481=CARTESIAN_POINT('Ctrl Pts',(19.9906274051637,3.89817441291494E-5,
5.11215529601011));
#40482=CARTESIAN_POINT('Ctrl Pts',(19.9637371164834,4.57301348963764E-5,
5.0765028432512));
#40483=CARTESIAN_POINT('Ctrl Pts',(19.9366587691311,5.50600375822944E-5,
5.04057917079713));
#40484=CARTESIAN_POINT('Ctrl Pts',(19.9093864780487,6.75721501229822E-5,
5.00437426454754));
#40485=CARTESIAN_POINT('Ctrl Pts',(19.8219754132208,0.000107675017795418,
4.88833306369241));
#40486=CARTESIAN_POINT('Ctrl Pts',(19.7325741562302,0.000181835093669053,
4.76940538345263));
#40487=CARTESIAN_POINT('Ctrl Pts',(19.640991672691,0.00030893622753794,
4.64726735002378));
#40488=CARTESIAN_POINT('Ctrl Pts',(19.6046361822504,0.00035939155347774,
4.5987822256294));
#40489=CARTESIAN_POINT('Ctrl Pts',(19.5679372662935,0.000418182392978269,
4.54979164217064));
#40490=CARTESIAN_POINT('Ctrl Pts',(19.5308843034958,0.000486453624597445,
4.50027729897209));
#40491=CARTESIAN_POINT('Ctrl Pts',(19.4649269930547,0.000607982012022067,
4.41213771014967));
#40492=CARTESIAN_POINT('Ctrl Pts',(19.3979604575256,0.000755754893077826,
4.32248935160143));
#40493=CARTESIAN_POINT('Ctrl Pts',(19.32967497191,0.000939646903500107,
4.23089537491404));
#40494=CARTESIAN_POINT('Ctrl Pts',(19.3260653667936,0.000949367527666284,
4.22605367123578));
#40495=CARTESIAN_POINT('Ctrl Pts',(19.3224520692927,0.000959189247964836,
4.22120652086859));
#40496=CARTESIAN_POINT('Ctrl Pts',(19.3188350312757,0.000969113583970318,
4.21635385578221));
#40497=CARTESIAN_POINT('Ctrl Pts',(19.2777054431015,0.00108196389156541,
4.16117386718128));
#40498=CARTESIAN_POINT('Ctrl Pts',(19.2360924231322,0.00120807388850654,
4.10528115905047));
#40499=CARTESIAN_POINT('Ctrl Pts',(19.1941052786264,0.00134680194697621,
4.04882712612678));
#40500=CARTESIAN_POINT('Ctrl Pts',(19.1255959475606,0.00157316090988453,
3.95671254969881));
#40501=CARTESIAN_POINT('Ctrl Pts',(19.0558951897339,0.00183348354698827,
3.86284161002992));
#40502=CARTESIAN_POINT('Ctrl Pts',(18.9849352541343,0.00212458137739411,
3.76713326639925));
#40503=CARTESIAN_POINT('Ctrl Pts',(18.9473688786483,0.00227868933011117,
3.71646501897776));
#40504=CARTESIAN_POINT('Ctrl Pts',(18.9100686735636,0.00243890737907993,
3.66611665801017));
#40505=CARTESIAN_POINT('Ctrl Pts',(18.8730284743227,0.00260445671863931,
3.61608395584742));
#40506=CARTESIAN_POINT('Ctrl Pts',(18.7755646591026,0.00304006642299761,
3.48443298910044));
#40507=CARTESIAN_POINT('Ctrl Pts',(18.679648004789,0.00351385896967246,
3.35462748521827));
#40508=CARTESIAN_POINT('Ctrl Pts',(18.5857625174182,0.00401352288344629,
3.22736737383541));
#40509=CARTESIAN_POINT('Ctrl Pts',(18.535886146263,0.00427896777289746,
3.15976083818942));
#40510=CARTESIAN_POINT('Ctrl Pts',(18.4865835643325,0.0045518186419106,
3.0928728969965));
#40511=CARTESIAN_POINT('Ctrl Pts',(18.4376106715998,0.00482723791978553,
3.02638559791964));
#40512=CARTESIAN_POINT('Ctrl Pts',(18.3555927639463,0.00528849947976878,
2.9150352395573));
#40513=CARTESIAN_POINT('Ctrl Pts',(18.2748688846044,0.00575567155003901,
2.80530938048468));
#40514=CARTESIAN_POINT('Ctrl Pts',(18.1953681077857,0.0061993131329244,
2.69717844492762));
#40515=CARTESIAN_POINT('Ctrl Pts',(18.131947821558,0.00655322006685646,
2.61091897480016));
#40516=CARTESIAN_POINT('Ctrl Pts',(18.0693048287704,0.00689210898023805,
2.5256731902104));
#40517=CARTESIAN_POINT('Ctrl Pts',(18.0073887079404,0.00720102569903335,
2.44140765258671));
#40518=CARTESIAN_POINT('Ctrl Pts',(17.9720494218701,0.00737734320974101,
2.39331219860742));
#40519=CARTESIAN_POINT('Ctrl Pts',(17.9369644798575,0.00754381435446798,
2.3455599795844));
#40520=CARTESIAN_POINT('Ctrl Pts',(17.9021016613117,0.0076978459350133,
2.2981136802392));
#40521=CARTESIAN_POINT('Ctrl Pts',(17.7975276756785,0.00815987674499643,
2.15579447505053));
#40522=CARTESIAN_POINT('Ctrl Pts',(17.694951671179,0.00850987289057204,
2.01622713361538));
#40523=CARTESIAN_POINT('Ctrl Pts',(17.5943127853703,0.00864476446222271,
1.87944134538212));
#40524=CARTESIAN_POINT('Ctrl Pts',(17.4946689503696,0.00877832231513908,
1.74400800464469));
#40525=CARTESIAN_POINT('Ctrl Pts',(17.3968684248807,0.00870150263032668,
1.61122539970131));
#40526=CARTESIAN_POINT('Ctrl Pts',(17.3007553288245,0.00831336603052086,
1.48099171860255));
#40527=CARTESIAN_POINT('Ctrl Pts',(17.2909959501874,0.00827395441861914,
1.46776771628336));
#40528=CARTESIAN_POINT('Ctrl Pts',(17.2812539945132,0.00823132892112186,
1.45457003148099));
#40529=CARTESIAN_POINT('Ctrl Pts',(17.2715293155224,0.00818538078796312,
1.44139858314228));
#40530=CARTESIAN_POINT('Ctrl Pts',(17.2513591319137,0.00809007869283378,
1.41407937480295));
#40531=CARTESIAN_POINT('Ctrl Pts',(17.2312632696569,0.00798048367228278,
1.38687303087359));
#40532=CARTESIAN_POINT('Ctrl Pts',(17.211237278093,0.0078553703108523,1.3597745396171));
#40533=CARTESIAN_POINT('Ctrl Pts',(17.1601159789753,0.00753598749512902,
1.29059893486631));
#40534=CARTESIAN_POINT('Ctrl Pts',(17.1094635746198,0.00711965377695296,
1.22214448899761));
#40535=CARTESIAN_POINT('Ctrl Pts',(17.0592536261995,0.00658289176926766,
1.15439218065909));
#40536=CARTESIAN_POINT('Ctrl Pts',(16.9522296725837,0.00543876806429331,
1.00997618078031));
#40537=CARTESIAN_POINT('Ctrl Pts',(16.8472142918112,0.00375032947837653,
0.868748571791631));
#40538=CARTESIAN_POINT('Ctrl Pts',(16.7439590026656,0.00130420671304145,
0.730530474948701));
#40539=CARTESIAN_POINT('Ctrl Pts',(16.7246782284289,0.00084744424417522,
0.704721124718759));
#40540=CARTESIAN_POINT('Ctrl Pts',(16.7054587525926,0.000364295203661793,
0.679016585636762));
#40541=CARTESIAN_POINT('Ctrl Pts',(16.6862988702478,-0.00014658020414501,
0.653415534774706));
#40542=CARTESIAN_POINT('',(11.7470010947906,-1.24897189209217,-5.16040757331412));
#40543=CARTESIAN_POINT('Ctrl Pts',(16.6859947282585,-0.000213685071588365,
0.653010349651272));
#40544=CARTESIAN_POINT('Ctrl Pts',(16.4192854137287,-0.0072433137319682,
0.300858250357417));
#40545=CARTESIAN_POINT('Ctrl Pts',(15.9095207379221,-0.0351396207084642,
-0.370166803666931));
#40546=CARTESIAN_POINT('Ctrl Pts',(15.1895782981127,-0.127632624932323,
-1.30811589893802));
#40547=CARTESIAN_POINT('Ctrl Pts',(14.4478451522131,-0.294302251982803,
-2.24397964816492));
#40548=CARTESIAN_POINT('Ctrl Pts',(13.3092516261401,-0.649917867944524,
-3.60699541669691));
#40549=CARTESIAN_POINT('Ctrl Pts',(12.4232261256394,-1.01937922958051,-4.52402251923096));
#40550=CARTESIAN_POINT('Ctrl Pts',(11.7470010949101,-1.24897189262897,-5.16040757324743));
#40551=CARTESIAN_POINT('Ctrl Pts',(11.7470010949101,-1.24897189262897,-5.16040757324743));
#40552=CARTESIAN_POINT('Ctrl Pts',(10.7125397951466,-1.59144123476306,-6.0634775436082));
#40553=CARTESIAN_POINT('Ctrl Pts',(9.24118021009056,-1.93913982160653,-6.97487125430323));
#40554=CARTESIAN_POINT('Ctrl Pts',(7.87873760695008,-2.09354224390961,-7.58570787305198));
#40555=CARTESIAN_POINT('Ctrl Pts',(7.28211573159564,-2.13599647613335,-7.80368259116433));
#40556=CARTESIAN_POINT('Ctrl Pts',(6.7745203245172,-2.15695778989224,-7.96476246664597));
#40557=CARTESIAN_POINT('Ctrl Pts',(6.29786588949097,-2.16773371799523,-8.09674109067091));
#40558=CARTESIAN_POINT('Ctrl Pts',(5.00815621212858,-2.16216752644387,-8.38292053232245));
#40559=CARTESIAN_POINT('Ctrl Pts',(3.22852047111695,-2.04767166606362,-8.49451211875645));
#40560=CARTESIAN_POINT('Ctrl Pts',(1.19527622155365,-1.93132215124059,-8.55306594389669));
#40561=CARTESIAN_POINT('Ctrl Pts',(6.41902973990636E-15,-1.93207323326078,
-8.62957429809281));
#40562=CARTESIAN_POINT('',(-36.1915542569364,0.0787940302150566,-5.40804187715572));
#40563=CARTESIAN_POINT('',(-35.11517701784,0.0508510909662735,-2.65562493453964));
#40564=CARTESIAN_POINT('Ctrl Pts',(-36.190739898305,0.0787719633382659,
-5.40642988539957));
#40565=CARTESIAN_POINT('Ctrl Pts',(-35.7431048645438,0.0666427433527001,
-4.52019980252406));
#40566=CARTESIAN_POINT('Ctrl Pts',(-35.3838115012789,0.0575373937785139,
-3.5969362359802));
#40567=CARTESIAN_POINT('Ctrl Pts',(-35.11517701784,0.0508510909662703,-2.65562493453964));
#40568=CARTESIAN_POINT('',(-41.6364777727387,0.319028652933056,-11.5323619171013));
#40569=CARTESIAN_POINT('Ctrl Pts',(-41.6333832694247,0.318726115297504,
-11.530271378588));
#40570=CARTESIAN_POINT('Ctrl Pts',(-40.469472385245,0.204977053081564,-10.7437628031316));
#40571=CARTESIAN_POINT('Ctrl Pts',(-38.3559078896116,0.147573716864128,
-8.89963534126349));
#40572=CARTESIAN_POINT('Ctrl Pts',(-36.8151557983613,0.095692551513825,
-6.64222332188911));
#40573=CARTESIAN_POINT('Ctrl Pts',(-36.1917138133952,0.0787983537557951,
-5.4083577130619));
#40574=CARTESIAN_POINT('',(-58.6294249853169,3.50507048772823,-12.1300984569962));
#40575=CARTESIAN_POINT('Ctrl Pts',(-58.6294249853169,3.50507048772823,-12.1300984569962));
#40576=CARTESIAN_POINT('Ctrl Pts',(-57.9716624173195,3.44148099145208,-12.5594172014826));
#40577=CARTESIAN_POINT('Ctrl Pts',(-56.9350672575427,3.39429553816601,-13.1429311762582));
#40578=CARTESIAN_POINT('Ctrl Pts',(-54.8001566067438,3.30035269345341,-14.0186136905654));
#40579=CARTESIAN_POINT('Ctrl Pts',(-52.5620566289039,3.10483667886162,-14.5433464527275));
#40580=CARTESIAN_POINT('Ctrl Pts',(-49.295584910841,2.34465836914774,-14.632672959566));
#40581=CARTESIAN_POINT('Ctrl Pts',(-46.4621628306032,1.23462273661855,-14.0012119190018));
#40582=CARTESIAN_POINT('Ctrl Pts',(-43.6129610195816,0.540799292570524,
-12.7246728134981));
#40583=CARTESIAN_POINT('Ctrl Pts',(-42.2733694331884,0.381318100537509,
-11.9625083064448));
#40584=CARTESIAN_POINT('Ctrl Pts',(-41.6364777727387,0.319028652933056,
-11.5323619171013));
#40585=CARTESIAN_POINT('',(-64.2985865890396,3.08034664292734,-5.85430278968146));
#40586=CARTESIAN_POINT('Ctrl Pts',(-64.2984271691748,3.08038932251095,-5.85463968857846));
#40587=CARTESIAN_POINT('Ctrl Pts',(-64.2149763686856,3.10273760294942,-6.03098199576973));
#40588=CARTESIAN_POINT('Ctrl Pts',(-63.5361674281905,3.32898348528657,-7.40198206074098));
#40589=CARTESIAN_POINT('Ctrl Pts',(-62.3504191551611,3.80834832178581,-9.12254403970273));
#40590=CARTESIAN_POINT('Ctrl Pts',(-60.6939165981419,3.73345458801685,-10.6556781858428));
#40591=CARTESIAN_POINT('Ctrl Pts',(-59.5525626426981,3.61048189569459,-11.5252172226885));
#40592=CARTESIAN_POINT('Ctrl Pts',(-58.9445304645418,3.53557780820992,-11.9244241512045));
#40593=CARTESIAN_POINT('Ctrl Pts',(-58.6320070381566,3.50532029143236,-12.1284131364863));
#40594=CARTESIAN_POINT('',(-65.940882311202,3.18169312325483,0.560736956423784));
#40595=CARTESIAN_POINT('Ctrl Pts',(-65.9408665795194,3.18169905920862,0.560433515178698));
#40596=CARTESIAN_POINT('Ctrl Pts',(-65.9143728994958,3.19163129587113,0.0501692994464946));
#40597=CARTESIAN_POINT('Ctrl Pts',(-65.7949103863174,3.14832895362465,-1.25211448306953));
#40598=CARTESIAN_POINT('Ctrl Pts',(-65.3271399010989,2.96188037443542,-3.39681624176221));
#40599=CARTESIAN_POINT('Ctrl Pts',(-64.6778756435701,2.97883584484194,-5.05270118071992));
#40600=CARTESIAN_POINT('Ctrl Pts',(-64.2988876471629,3.08026604421803,-5.85366656941012));
#40601=CARTESIAN_POINT('',(-65.1818229259373,3.08339058983654,6.62273332431001));
#40602=CARTESIAN_POINT('Ctrl Pts',(-65.1820138144051,3.08344362593875,6.62193263425266));
#40603=CARTESIAN_POINT('Ctrl Pts',(-65.2023991572908,3.0862917576968,6.56019789543742));
#40604=CARTESIAN_POINT('Ctrl Pts',(-65.2223744107905,3.08902484343314,6.49853102562792));
#40605=CARTESIAN_POINT('Ctrl Pts',(-65.2419378771287,3.09164815398979,6.43685530311948));
#40606=CARTESIAN_POINT('Ctrl Pts',(-65.2615689182929,3.09428052581152,6.37496654442693));
#40607=CARTESIAN_POINT('Ctrl Pts',(-65.2807853319273,3.09680238556488,6.31306895097167));
#40608=CARTESIAN_POINT('Ctrl Pts',(-65.2995864378602,3.0992186946728,6.25102614942384));
#40609=CARTESIAN_POINT('Ctrl Pts',(-65.328858256588,3.10298069476203,6.15443046793842));
#40610=CARTESIAN_POINT('Ctrl Pts',(-65.3571231565645,3.10648660394772,6.05746651472737));
#40611=CARTESIAN_POINT('Ctrl Pts',(-65.3843787248702,3.10975354311192,5.96022145009967));
#40612=CARTESIAN_POINT('Ctrl Pts',(-65.3919295545984,3.1106586095954,5.93328086619102));
#40613=CARTESIAN_POINT('Ctrl Pts',(-65.3994029474697,3.11154534378614,5.9063190073824));
#40614=CARTESIAN_POINT('Ctrl Pts',(-65.4067965504853,3.11241384365897,5.87933776802483));
#40615=CARTESIAN_POINT('Ctrl Pts',(-65.4502767239497,3.11752130277536,5.72066695961275));
#40616=CARTESIAN_POINT('Ctrl Pts',(-65.4910054802836,3.12199916303113,5.56133319312213));
#40617=CARTESIAN_POINT('Ctrl Pts',(-65.5290825875995,3.12593851324299,5.401417880817));
#40618=CARTESIAN_POINT('Ctrl Pts',(-65.5641348605888,3.12956492262019,5.25420619439375));
#40619=CARTESIAN_POINT('Ctrl Pts',(-65.5969413278409,3.13273509500721,5.10649720222318));
#40620=CARTESIAN_POINT('Ctrl Pts',(-65.6275443166768,3.13551583469991,4.95832938162754));
#40621=CARTESIAN_POINT('Ctrl Pts',(-65.6663255026627,3.13903968603937,4.77056589753007));
#40622=CARTESIAN_POINT('Ctrl Pts',(-65.7015662727776,3.14193797149757,4.58207020571463));
#40623=CARTESIAN_POINT('Ctrl Pts',(-65.7333517374092,3.14434707116289,4.39298046147203));
#40624=CARTESIAN_POINT('Ctrl Pts',(-65.7540687165909,3.14591726270142,4.26973644599696));
#40625=CARTESIAN_POINT('Ctrl Pts',(-65.7733177100259,3.14727965268877,4.14624240801174));
#40626=CARTESIAN_POINT('Ctrl Pts',(-65.7911247600377,3.1484722064521,4.02254559511262));
#40627=CARTESIAN_POINT('Ctrl Pts',(-65.7969314450796,3.14886108524418,3.9822094118193));
#40628=CARTESIAN_POINT('Ctrl Pts',(-65.8025848056586,3.14923190422925,3.9418518235844));
#40629=CARTESIAN_POINT('Ctrl Pts',(-65.8080857829282,3.14958597965166,3.90147479140268));
#40630=CARTESIAN_POINT('Ctrl Pts',(-65.8122533101222,3.14985422634299,3.87088524860251));
#40631=CARTESIAN_POINT('Ctrl Pts',(-65.8163333772144,3.15011286303388,3.84028454606075));
#40632=CARTESIAN_POINT('Ctrl Pts',(-65.8203264104579,3.1503624622411,3.80967353994764));
#40633=CARTESIAN_POINT('Ctrl Pts',(-65.8234339407524,3.1505567098345,3.78585089108904));
#40634=CARTESIAN_POINT('Ctrl Pts',(-65.8264893985082,3.1507455242109,3.76201719191869));
#40635=CARTESIAN_POINT('Ctrl Pts',(-65.8294939234993,3.15092922842115,3.73816463867714));
#40636=CARTESIAN_POINT('Ctrl Pts',(-65.8331602401737,3.15115339623844,3.70905820290531));
#40637=CARTESIAN_POINT('Ctrl Pts',(-65.8367502423687,3.15136992509179,3.67992730670294));
#40638=CARTESIAN_POINT('Ctrl Pts',(-65.8402641068065,3.15157928490807,3.65077229499262));
#40639=CARTESIAN_POINT('Ctrl Pts',(-65.8615591734033,3.15284806784186,3.47408422776829));
#40640=CARTESIAN_POINT('Ctrl Pts',(-65.8800565538659,3.15385321994246,3.29650470733162));
#40641=CARTESIAN_POINT('Ctrl Pts',(-65.8957954274969,3.15479469408719,3.11815426760985));
#40642=CARTESIAN_POINT('Ctrl Pts',(-65.9104251056954,3.15566981794246,2.95237305601382));
#40643=CARTESIAN_POINT('Ctrl Pts',(-65.9226716782155,3.15649018549394,2.78592275316682));
#40644=CARTESIAN_POINT('Ctrl Pts',(-65.9325836358646,3.15741782690276,2.61893372892488));
#40645=CARTESIAN_POINT('Ctrl Pts',(-65.9378901130687,3.15791445008898,2.52953429020231));
#40646=CARTESIAN_POINT('Ctrl Pts',(-65.9425278145653,3.15844183471541,2.43997962823197));
#40647=CARTESIAN_POINT('Ctrl Pts',(-65.9465061693714,3.15902460511505,2.35030054189828));
#40648=CARTESIAN_POINT('Ctrl Pts',(-65.9499589751705,3.15953039032363,2.27246825080328));
#40649=CARTESIAN_POINT('Ctrl Pts',(-65.9529154178099,3.16007791310227,2.19453831713516));
#40650=CARTESIAN_POINT('Ctrl Pts',(-65.9553831634599,3.16068322693473,2.11651288325481));
#40651=CARTESIAN_POINT('Ctrl Pts',(-65.9570020166317,3.16108031575857,2.06532781840632));
#40652=CARTESIAN_POINT('Ctrl Pts',(-65.9584105277869,3.16150225489745,2.01410341967322));
#40653=CARTESIAN_POINT('Ctrl Pts',(-65.9596098983724,3.1619500963955,1.96285658232393));
#40654=CARTESIAN_POINT('Ctrl Pts',(-65.9620404632496,3.1628576622711,1.85900314084093));
#40655=CARTESIAN_POINT('Ctrl Pts',(-65.9636135459671,3.16387181256393,1.7550240340113));
#40656=CARTESIAN_POINT('Ctrl Pts',(-65.9643350584048,3.16500289072531,1.6509649698538));
#40657=CARTESIAN_POINT('Ctrl Pts',(-65.9645966980952,3.16541304989168,1.61323037248798));
#40658=CARTESIAN_POINT('Ctrl Pts',(-65.9647462801353,3.16583859524181,1.57548525747449));
#40659=CARTESIAN_POINT('Ctrl Pts',(-65.9647838219684,3.16628005752532,1.53773183134651));
#40660=CARTESIAN_POINT('Ctrl Pts',(-65.964814152205,3.16663671713484,1.50723064761264));
#40661=CARTESIAN_POINT('Ctrl Pts',(-65.9647713681457,3.16700374895558,1.47672527941099));
#40662=CARTESIAN_POINT('Ctrl Pts',(-65.9646553256625,3.16738159960587,1.44620476843088));
#40663=CARTESIAN_POINT('Ctrl Pts',(-65.9645189092163,3.16782579074596,1.4103256702788));
#40664=CARTESIAN_POINT('Ctrl Pts',(-65.964281214949,3.1682848589196,1.37443237344843));
#40665=CARTESIAN_POINT('Ctrl Pts',(-65.9639422079975,3.16875903076749,1.33854708614654));
#40666=CARTESIAN_POINT('Ctrl Pts',(-65.9630174029551,3.17005256328616,1.24065264919655));
#40667=CARTESIAN_POINT('Ctrl Pts',(-65.9613372844884,3.17145872738211,1.14281766425937));
#40668=CARTESIAN_POINT('Ctrl Pts',(-65.9589158777346,3.17299774944126,1.04494380771358));
#40669=CARTESIAN_POINT('Ctrl Pts',(-65.9587830004562,3.17308220491834,1.03957287543947));
#40670=CARTESIAN_POINT('Ctrl Pts',(-65.9586478955613,3.17316705961954,1.03420182780611));
#40671=CARTESIAN_POINT('Ctrl Pts',(-65.958510566995,3.17325231657106,1.02883064941742));
#40672=CARTESIAN_POINT('Ctrl Pts',(-65.9583795817216,3.1733336354503,1.02370756914105));
#40673=CARTESIAN_POINT('Ctrl Pts',(-65.9582468049946,3.17341517649201,1.01859342997896));
#40674=CARTESIAN_POINT('Ctrl Pts',(-65.9581122745334,3.17349693078692,1.01348869045227));
#40675=CARTESIAN_POINT('Ctrl Pts',(-65.9566984971929,3.17435608468119,0.959843107075385));
#40676=CARTESIAN_POINT('Ctrl Pts',(-65.955093127377,3.17523907659001,0.907177309217897));
#40677=CARTESIAN_POINT('Ctrl Pts',(-65.9532671389238,3.17617002788351,0.854114316309088));
#40678=CARTESIAN_POINT('Ctrl Pts',(-65.9521293961761,3.17675008800426,0.821051656330386));
#40679=CARTESIAN_POINT('Ctrl Pts',(-65.9509051456926,3.17734891470678,0.787834642983174));
#40680=CARTESIAN_POINT('Ctrl Pts',(-65.9495788904456,3.17797408345389,0.754124291378267));
#40681=CARTESIAN_POINT('Ctrl Pts',(-65.9486209022187,3.17842565889602,0.729774438637609));
#40682=CARTESIAN_POINT('Ctrl Pts',(-65.9476094927885,3.17889112211251,0.705163238122186));
#40683=CARTESIAN_POINT('Ctrl Pts',(-65.9465425041965,3.17936386644549,0.680489633390043));
#40684=CARTESIAN_POINT('Ctrl Pts',(-65.9456241685326,3.17977074800368,0.659253557060112));
#40685=CARTESIAN_POINT('Ctrl Pts',(-65.9446646284688,3.18018304018358,0.637970848329328));
#40686=CARTESIAN_POINT('Ctrl Pts',(-65.9436620707991,3.1805956413506,0.616805703615335));
#40687=CARTESIAN_POINT('Ctrl Pts',(-65.9428109180125,3.18094593205576,0.598836890002149));
#40688=CARTESIAN_POINT('Ctrl Pts',(-65.9419287464167,3.1812964441945,0.58095295893464));
#40689=CARTESIAN_POINT('Ctrl Pts',(-65.9410143684102,3.18164329479668,0.563284147647862));
#40690=CARTESIAN_POINT('',(-61.4911136899846,2.54023943605001,12.6453526575845));
#40691=CARTESIAN_POINT('Ctrl Pts',(-61.492579746848,2.54044123593051,12.6438559805174));
#40692=CARTESIAN_POINT('Ctrl Pts',(-61.6274523636194,2.55900663594459,12.5061409518654));
#40693=CARTESIAN_POINT('Ctrl Pts',(-61.7598465090111,2.57732079123508,12.3659924353731));
#40694=CARTESIAN_POINT('Ctrl Pts',(-61.8897040632185,2.59541821568171,12.2235148275418));
#40695=CARTESIAN_POINT('Ctrl Pts',(-61.9897936428061,2.60936706613971,12.1136981599209));
#40696=CARTESIAN_POINT('Ctrl Pts',(-62.0883755887928,2.62318675732009,12.0024985721511));
#40697=CARTESIAN_POINT('Ctrl Pts',(-62.1854109821693,2.6368833832955,11.889978089556));
#40698=CARTESIAN_POINT('Ctrl Pts',(-62.3238252998524,2.65642067863669,11.7294753566682));
#40699=CARTESIAN_POINT('Ctrl Pts',(-62.4590940743637,2.67570916811489,11.566288083022));
#40700=CARTESIAN_POINT('Ctrl Pts',(-62.5910712856209,2.69473476474226,11.4005537560769));
#40701=CARTESIAN_POINT('Ctrl Pts',(-62.6611812893503,2.70484169636926,11.3125110237785));
#40702=CARTESIAN_POINT('Ctrl Pts',(-62.7303615707873,2.71487377663084,11.2237492830725));
#40703=CARTESIAN_POINT('Ctrl Pts',(-62.7985844799531,2.72482496592381,11.134287123968));
#40704=CARTESIAN_POINT('Ctrl Pts',(-62.9431636119667,2.74591369298148,10.9446974176723));
#40705=CARTESIAN_POINT('Ctrl Pts',(-63.0834410426147,2.76664159563338,10.751962951605));
#40706=CARTESIAN_POINT('Ctrl Pts',(-63.2191716943302,2.78691893809744,10.5562648470109));
#40707=CARTESIAN_POINT('Ctrl Pts',(-63.3535448424178,2.8069934776897,10.3625240076594));
#40708=CARTESIAN_POINT('Ctrl Pts',(-63.4834608710437,2.82662525100169,10.1658788201834));
#40709=CARTESIAN_POINT('Ctrl Pts',(-63.6087184396249,2.84569774795751,9.96648572222226));
#40710=CARTESIAN_POINT('Ctrl Pts',(-63.67949054989,2.85647394992979,9.85382610033401));
#40711=CARTESIAN_POINT('Ctrl Pts',(-63.7487762439001,2.86707116758227,9.74028885547898));
#40712=CARTESIAN_POINT('Ctrl Pts',(-63.8165455959749,2.87746643979862,9.62589900736996));
#40713=CARTESIAN_POINT('Ctrl Pts',(-63.9248200021698,2.89407486074408,9.4431395076914));
#40714=CARTESIAN_POINT('Ctrl Pts',(-64.0292220240533,2.91016730101018,9.25820452933871));
#40715=CARTESIAN_POINT('Ctrl Pts',(-64.1296563228998,2.92565150500005,9.07117745884888));
#40716=CARTESIAN_POINT('Ctrl Pts',(-64.2384680726629,2.94242728129537,8.86855003946347));
#40717=CARTESIAN_POINT('Ctrl Pts',(-64.3426275897165,2.95848842946922,8.66351672570398));
#40718=CARTESIAN_POINT('Ctrl Pts',(-64.4421008134935,2.97373763848325,8.4562287198291));
#40719=CARTESIAN_POINT('Ctrl Pts',(-64.5422735745952,2.98909408631466,8.24748297797682));
#40720=CARTESIAN_POINT('Ctrl Pts',(-64.6376943180403,3.003626370476,8.03645036383814));
#40721=CARTESIAN_POINT('Ctrl Pts',(-64.7283703588063,3.01726328798042,7.82326802272764));
#40722=CARTESIAN_POINT('Ctrl Pts',(-64.8217603485428,3.0313083606922,7.60370509871675));
#40723=CARTESIAN_POINT('Ctrl Pts',(-64.9101179346527,3.04440303516322,7.38186138031529));
#40724=CARTESIAN_POINT('Ctrl Pts',(-64.993488227946,3.0565104069069,7.15787463734448));
#40725=CARTESIAN_POINT('Ctrl Pts',(-65.0593066522129,3.06606882512404,6.98104361160777));
#40726=CARTESIAN_POINT('Ctrl Pts',(-65.1220175846494,3.07501276033487,6.80287657192886));
#40727=CARTESIAN_POINT('Ctrl Pts',(-65.181654605396,3.08334382396569,6.62343935220894));
#40728=CARTESIAN_POINT('',(-39.0604050365398,0.183119270849635,12.6471138640382));
#40729=CARTESIAN_POINT('Ctrl Pts',(-39.0604050365398,0.183119270849635,
12.6471138640382));
#40730=CARTESIAN_POINT('Ctrl Pts',(-39.0606668888501,0.183131142235521,
12.6473775711718));
#40731=CARTESIAN_POINT('Ctrl Pts',(-39.0609287502018,0.183143014646322,
12.6476412700229));
#40732=CARTESIAN_POINT('Ctrl Pts',(-39.0611906205948,0.183154888082176,
12.6479049605897));
#40733=CARTESIAN_POINT('Ctrl Pts',(-39.2840366840252,0.193258926222401,
12.8722999526221));
#40734=CARTESIAN_POINT('Ctrl Pts',(-39.5128971796941,0.204080431476651,
13.0905291572134));
#40735=CARTESIAN_POINT('Ctrl Pts',(-39.7477834050656,0.215700609772212,
13.3015853068891));
#40736=CARTESIAN_POINT('Ctrl Pts',(-39.902683352274,0.223363745410276,13.4407700819481));
#40737=CARTESIAN_POINT('Ctrl Pts',(-40.0602034639206,0.231374318042895,
13.5768350566888));
#40738=CARTESIAN_POINT('Ctrl Pts',(-40.2203420197422,0.239753276541817,
13.7094884715307));
#40739=CARTESIAN_POINT('Ctrl Pts',(-40.4916274961205,0.253947795383785,
13.9342122718297));
#40740=CARTESIAN_POINT('Ctrl Pts',(-40.7702788233318,0.269192848806674,
14.1490879279519));
#40741=CARTESIAN_POINT('Ctrl Pts',(-41.0556719421123,0.285548471670355,
14.3539554115054));
#40742=CARTESIAN_POINT('Ctrl Pts',(-41.085318076012,0.287247464930951,14.3752366844214));
#40743=CARTESIAN_POINT('Ctrl Pts',(-41.1150369180175,0.288958427338304,
14.3964099463438));
#40744=CARTESIAN_POINT('Ctrl Pts',(-41.1448277413998,0.290681415935031,
14.4174750072174));
#40745=CARTESIAN_POINT('Ctrl Pts',(-41.4545942194746,0.308597137918321,
14.6365105683868));
#40746=CARTESIAN_POINT('Ctrl Pts',(-41.7721472637896,0.327815031465181,
14.8438489703323));
#40747=CARTESIAN_POINT('Ctrl Pts',(-42.0966485620468,0.348385513803167,
15.0392663439725));
#40748=CARTESIAN_POINT('Ctrl Pts',(-42.2446048226632,0.357764618485189,
15.1283668314546));
#40749=CARTESIAN_POINT('Ctrl Pts',(-42.3940049066234,0.367424596614065,
15.2149888136249));
#40750=CARTESIAN_POINT('Ctrl Pts',(-42.5447664170058,0.377368657537596,
15.2991099938131));
#40751=CARTESIAN_POINT('Ctrl Pts',(-42.7671859547678,0.392039201952269,
15.423214574392));
#40752=CARTESIAN_POINT('Ctrl Pts',(-42.9925689275241,0.407328091485488,
15.5418760411507));
#40753=CARTESIAN_POINT('Ctrl Pts',(-43.2206488887303,0.423241653007795,
15.6550241882715));
#40754=CARTESIAN_POINT('Ctrl Pts',(-43.6176817449801,0.450943371084633,
15.8519881468463));
#40755=CARTESIAN_POINT('Ctrl Pts',(-44.0228896448743,0.480539226963428,
16.032246467644));
#40756=CARTESIAN_POINT('Ctrl Pts',(-44.4348255327009,0.512045625941868,
16.1954177560798));
#40757=CARTESIAN_POINT('Ctrl Pts',(-44.7387179971087,0.535288459385418,
16.3157921309005));
#40758=CARTESIAN_POINT('Ctrl Pts',(-45.0462708019942,0.559570753892732,
16.426866915952));
#40759=CARTESIAN_POINT('Ctrl Pts',(-45.3568885891016,0.5848900031984,16.5284829339606));
#40760=CARTESIAN_POINT('Ctrl Pts',(-45.7630705890824,0.617998935615831,
16.6613619870541));
#40761=CARTESIAN_POINT('Ctrl Pts',(-46.1744954614692,0.65288278895461,16.77806697134));
#40762=CARTESIAN_POINT('Ctrl Pts',(-46.5898247303867,0.689544215461607,
16.8782249009176));
#40763=CARTESIAN_POINT('Ctrl Pts',(-47.0240057882049,0.727869703533806,
16.9829289973234));
#40764=CARTESIAN_POINT('Ctrl Pts',(-47.4624513529612,0.768138554332072,
17.0695489583781));
#40765=CARTESIAN_POINT('Ctrl Pts',(-47.9036097711811,0.810306044668031,
17.1376550430375));
#40766=CARTESIAN_POINT('Ctrl Pts',(-47.9500332036625,0.814743361422456,
17.1448218976008));
#40767=CARTESIAN_POINT('Ctrl Pts',(-47.99648667759,0.819201655130773,17.1517837424007));
#40768=CARTESIAN_POINT('Ctrl Pts',(-48.0429683888055,0.823680839660802,
17.1585400804775));
#40769=CARTESIAN_POINT('Ctrl Pts',(-48.0905363285643,0.828264698006835,
17.1654543070458));
#40770=CARTESIAN_POINT('Ctrl Pts',(-48.1381338407373,0.832870435007399,
17.1721533097098));
#40771=CARTESIAN_POINT('Ctrl Pts',(-48.1857589944567,0.837497951118463,
17.1786365573383));
#40772=CARTESIAN_POINT('Ctrl Pts',(-48.5894375001487,0.876721526118069,
17.2335896128204));
#40773=CARTESIAN_POINT('Ctrl Pts',(-48.9950997343204,0.917513509102992,
17.273040738628));
#40774=CARTESIAN_POINT('Ctrl Pts',(-49.4015504710882,0.959821260145756,
17.2966290468743));
#40775=CARTESIAN_POINT('Ctrl Pts',(-49.70885328167,0.991808631870625,17.3144633199245));
#40776=CARTESIAN_POINT('Ctrl Pts',(-50.0166070974792,1.02466130307784,17.3232301877965));
#40777=CARTESIAN_POINT('Ctrl Pts',(-50.3243092135675,1.0583429324575,17.3227777244192));
#40778=CARTESIAN_POINT('Ctrl Pts',(-50.5598248881171,1.08412290356764,17.3224314082519));
#40779=CARTESIAN_POINT('Ctrl Pts',(-50.7953336343792,1.11039082495756,17.3167118478853));
#40780=CARTESIAN_POINT('Ctrl Pts',(-51.0305863517201,1.13712426615352,17.3056788143251));
#40781=CARTESIAN_POINT('Ctrl Pts',(-51.4761245154068,1.18775393978326,17.2847836783712));
#40782=CARTESIAN_POINT('Ctrl Pts',(-51.9207412909683,1.24005387209177,17.2448303381155));
#40783=CARTESIAN_POINT('Ctrl Pts',(-52.3625858524104,1.2936972330631,17.1862403088709));
#40784=CARTESIAN_POINT('Ctrl Pts',(-52.4264742939416,1.30145378600056,17.1777684932499));
#40785=CARTESIAN_POINT('Ctrl Pts',(-52.4903048604507,1.30923840713047,17.1689070336471));
#40786=CARTESIAN_POINT('Ctrl Pts',(-52.5540720323581,1.31705009289058,17.1596572113284));
#40787=CARTESIAN_POINT('Ctrl Pts',(-53.003553927648,1.37211308558476,17.0944570849539));
#40788=CARTESIAN_POINT('Ctrl Pts',(-53.4498856007116,1.42852058127125,17.0099600355678));
#40789=CARTESIAN_POINT('Ctrl Pts',(-53.8911418598714,1.48592156034486,16.9066194449686));
#40790=CARTESIAN_POINT('Ctrl Pts',(-53.9875034657967,1.49845679448691,16.8840519117934));
#40791=CARTESIAN_POINT('Ctrl Pts',(-54.0836230056315,1.51103942881208,16.8605857879481));
#40792=CARTESIAN_POINT('Ctrl Pts',(-54.1794803052346,1.52366130162109,16.8362272941616));
#40793=CARTESIAN_POINT('Ctrl Pts',(-54.5812987873487,1.57657017548416,16.7341203806515));
#40794=CARTESIAN_POINT('Ctrl Pts',(-54.9787920780597,1.63020748646383,16.6159478440198));
#40795=CARTESIAN_POINT('Ctrl Pts',(-55.3707700094445,1.68400548366404,16.4823550595151));
#40796=CARTESIAN_POINT('Ctrl Pts',(-55.7254062830265,1.73267843110742,16.361488950786));
#40797=CARTESIAN_POINT('Ctrl Pts',(-56.0755280958839,1.78148331561148,16.2280022066449));
#40798=CARTESIAN_POINT('Ctrl Pts',(-56.4202194358333,1.82997079988972,16.0823687023087));
#40799=CARTESIAN_POINT('Ctrl Pts',(-56.5357517080917,1.84622264200326,16.0335558436062));
#40800=CARTESIAN_POINT('Ctrl Pts',(-56.6506736005584,1.86243855447853,15.9833782377977));
#40801=CARTESIAN_POINT('Ctrl Pts',(-56.7649497587316,1.87860083920917,15.9318530432299));
#40802=CARTESIAN_POINT('Ctrl Pts',(-56.9620517553632,1.90647733279682,15.8429830734261));
#40803=CARTESIAN_POINT('Ctrl Pts',(-57.1572326127867,1.9341941425919,15.7501044856584));
#40804=CARTESIAN_POINT('Ctrl Pts',(-57.3503735845836,1.96167081317485,15.6532998685256));
#40805=CARTESIAN_POINT('Ctrl Pts',(-57.62978046508,2.00141986663867,15.513257722941));
#40806=CARTESIAN_POINT('Ctrl Pts',(-57.9049183209555,2.04066520647406,15.3650015932308));
#40807=CARTESIAN_POINT('Ctrl Pts',(-58.1754298370156,2.07917259253651,15.2087506681607));
#40808=CARTESIAN_POINT('Ctrl Pts',(-58.4302797952656,2.11545055169057,15.0615460599776));
#40809=CARTESIAN_POINT('Ctrl Pts',(-58.6810244436519,2.15107239926173,14.9072461379215));
#40810=CARTESIAN_POINT('Ctrl Pts',(-58.9273599534012,2.18586651354731,14.7459925951525));
#40811=CARTESIAN_POINT('Ctrl Pts',(-59.1409340208908,2.21603317738004,14.6061850007812));
#40812=CARTESIAN_POINT('Ctrl Pts',(-59.3511944237414,2.24557728638283,14.461150039835));
#40813=CARTESIAN_POINT('Ctrl Pts',(-59.5579291538172,2.27441462267184,14.3109480361353));
#40814=CARTESIAN_POINT('Ctrl Pts',(-59.5896414679669,2.27883815938143,14.2879076252402));
#40815=CARTESIAN_POINT('Ctrl Pts',(-59.6212707800306,2.28324513082026,14.2647455684019));
#40816=CARTESIAN_POINT('Ctrl Pts',(-59.6528162738773,2.28763530890052,14.241462012894));
#40817=CARTESIAN_POINT('Ctrl Pts',(-59.8518978018344,2.31534143277572,14.094521032058));
#40818=CARTESIAN_POINT('Ctrl Pts',(-60.047644383031,2.34237709488712,13.9427405811155));
#40819=CARTESIAN_POINT('Ctrl Pts',(-60.2398413018096,2.36880093753368,13.7861505347015));
#40820=CARTESIAN_POINT('Ctrl Pts',(-60.4212087887707,2.39373591550897,13.6383836330169));
#40821=CARTESIAN_POINT('Ctrl Pts',(-60.5994160124284,2.41812677579402,13.4863335428754));
#40822=CARTESIAN_POINT('Ctrl Pts',(-60.7742400315841,2.44203497255451,13.3300325388928));
#40823=CARTESIAN_POINT('Ctrl Pts',(-60.9362372604305,2.46418903147968,13.1851992966795));
#40824=CARTESIAN_POINT('Ctrl Pts',(-61.0953297847282,2.48592927582932,13.0367159414217));
#40825=CARTESIAN_POINT('Ctrl Pts',(-61.251296640164,2.50730614462313,12.8846171702282));
#40826=CARTESIAN_POINT('Ctrl Pts',(-61.3318896415521,2.51835224805042,12.8060229301655));
#40827=CARTESIAN_POINT('Ctrl Pts',(-61.4116472956318,2.52930129871605,12.7264634937059));
#40828=CARTESIAN_POINT('Ctrl Pts',(-61.4905336880022,2.54015959990334,12.6459447735438));
#40829=CARTESIAN_POINT('',(-35.3373097934181,0.0544178896829728,6.63137155234305));
#40830=CARTESIAN_POINT('Ctrl Pts',(-35.3376973936001,0.0544271591152199,
6.63251752009926));
#40831=CARTESIAN_POINT('Ctrl Pts',(-35.8138531895274,0.0658148084159087,
8.03995386779416));
#40832=CARTESIAN_POINT('Ctrl Pts',(-36.9028760126082,0.0948092812359606,
10.1871843261409));
#40833=CARTESIAN_POINT('Ctrl Pts',(-38.4270467968691,0.154379143867951,
12.0091830811851));
#40834=CARTESIAN_POINT('Ctrl Pts',(-39.059611759677,0.183132402525965,12.6463171581384));
#40835=CARTESIAN_POINT('',(-34.5485284593044,0.0369496769146498,0.611350965839471));
#40836=CARTESIAN_POINT('Ctrl Pts',(-34.5485283758344,0.03694967497705,0.611352241800955));
#40837=CARTESIAN_POINT('Ctrl Pts',(-34.4156250594086,0.0338645726825741,
2.642977068212));
#40838=CARTESIAN_POINT('Ctrl Pts',(-34.6822137461999,0.0387518832851432,
4.69404824512284));
#40839=CARTESIAN_POINT('Ctrl Pts',(-35.3369428780847,0.0544091149274879,
6.63028674082642));
#40840=CARTESIAN_POINT('Origin',(-42.8058228112322,0.246536164900552,0.301815738582165));
#40841=CARTESIAN_POINT('',(-2.90417482900993,-2.04618953971544,-29.4756275701078));
#40842=CARTESIAN_POINT('',(1.92208295535431,-2.10378908788117,-32.4806927333858));
#40843=CARTESIAN_POINT('Ctrl Pts',(-2.90469444443151,-2.04568606478228,
-29.4775763495009));
#40844=CARTESIAN_POINT('Ctrl Pts',(-3.02250615524581,-2.05288116339367,
-29.9513503562729));
#40845=CARTESIAN_POINT('Ctrl Pts',(-3.00491991129501,-2.09425330667714,
-30.9658956033376));
#40846=CARTESIAN_POINT('Ctrl Pts',(-2.22452399291722,-2.12061194796893,
-32.362721059084));
#40847=CARTESIAN_POINT('Ctrl Pts',(-0.907169341450753,-2.06911023237464,
-33.2201637931267));
#40848=CARTESIAN_POINT('Ctrl Pts',(0.615978874200203,-2.06181054642213,
-33.3001206932397));
#40849=CARTESIAN_POINT('Ctrl Pts',(1.5420796957956,-2.09550075658161,-32.818473935249));
#40850=CARTESIAN_POINT('Ctrl Pts',(1.92209690915283,-2.10352759449249,-32.4807021153953));
#40851=CARTESIAN_POINT('',(2.90362501667649,-2.04722624614018,-29.4766633543452));
#40852=CARTESIAN_POINT('Ctrl Pts',(2.90308452694824,-2.04719239277948,-29.474406698116));
#40853=CARTESIAN_POINT('Ctrl Pts',(2.88735153351078,-2.04620772726132,-29.4089081520382));
#40854=CARTESIAN_POINT('Ctrl Pts',(2.86940368652239,-2.04508734517392,-29.3434470545767));
#40855=CARTESIAN_POINT('Ctrl Pts',(2.84929693172628,-2.04383765038075,-29.2786192026188));
#40856=CARTESIAN_POINT('Ctrl Pts',(2.82919017693018,-2.04258795558759,-29.2137913506608));
#40857=CARTESIAN_POINT('Ctrl Pts',(2.80692451694612,-2.04120892472319,-29.1495967442315));
#40858=CARTESIAN_POINT('Ctrl Pts',(2.7825317098188,-2.03970656265669,-29.0861967026844));
#40859=CARTESIAN_POINT('Ctrl Pts',(2.73374609556417,-2.03670183852368,-28.9593966195901));
#40860=CARTESIAN_POINT('Ctrl Pts',(2.67645197152196,-2.03320240315436,-28.8357747958726));
#40861=CARTESIAN_POINT('Ctrl Pts',(2.61179122164448,-2.02932718705402,-28.7171887138959));
#40862=CARTESIAN_POINT('Ctrl Pts',(2.54713047176699,-2.02545197095368,-28.5986026319191));
#40863=CARTESIAN_POINT('Ctrl Pts',(2.47510323222483,-2.02119934730129,-28.4850522930688));
#40864=CARTESIAN_POINT('Ctrl Pts',(2.3955719043754,-2.01664372796269,-28.3761609709903));
#40865=CARTESIAN_POINT('Ctrl Pts',(2.31604057652597,-2.01208810862409,-28.2672696489119));
#40866=CARTESIAN_POINT('Ctrl Pts',(2.2290050097441,-2.00723040475461,-28.1630373398676));
#40867=CARTESIAN_POINT('Ctrl Pts',(2.13573747909507,-2.00226792456411,-28.0654780193846));
#40868=CARTESIAN_POINT('Ctrl Pts',(2.10510252136045,-2.00063793211297,-28.0334333663438));
#40869=CARTESIAN_POINT('Ctrl Pts',(2.07379026957427,-1.99899664908459,-28.0021082308194));
#40870=CARTESIAN_POINT('Ctrl Pts',(2.04183842704365,-1.99735154115993,-27.9715221607636));
#40871=CARTESIAN_POINT('Ctrl Pts',(1.96415372391943,-1.99335178056358,-27.8971580683097));
#40872=CARTESIAN_POINT('Ctrl Pts',(1.88268977963344,-1.98932850068838,-27.8271627986765));
#40873=CARTESIAN_POINT('Ctrl Pts',(1.79797339964551,-1.98539854586267,-27.7618102269358));
#40874=CARTESIAN_POINT('Ctrl Pts',(1.68751703571273,-1.9802745247403,-27.6766011156733));
#40875=CARTESIAN_POINT('Ctrl Pts',(1.57153248611584,-1.97531224434771,-27.5992844729345));
#40876=CARTESIAN_POINT('Ctrl Pts',(1.45116736980479,-1.97070354368304,-27.5304674892138));
#40877=CARTESIAN_POINT('Ctrl Pts',(1.3307473501235,-1.96609274080465,-27.4616191152993));
#40878=CARTESIAN_POINT('Ctrl Pts',(1.20594261715742,-1.96183640196311,-27.4012780911951));
#40879=CARTESIAN_POINT('Ctrl Pts',(1.07785376018322,-1.95810634097014,-27.3500520637452));
#40880=CARTESIAN_POINT('Ctrl Pts',(0.980716380361522,-1.95527761441273,
-27.3112043278632));
#40881=CARTESIAN_POINT('Ctrl Pts',(0.881689174663142,-1.95275119975537,
-27.2775986958651));
#40882=CARTESIAN_POINT('Ctrl Pts',(0.781235294330189,-1.95059127976565,
-27.2495003578474));
#40883=CARTESIAN_POINT('Ctrl Pts',(0.65354375093492,-1.94784570621304,-27.213783269205));
#40884=CARTESIAN_POINT('Ctrl Pts',(0.523559123780202,-1.94569474885112,
-27.1869677858605));
#40885=CARTESIAN_POINT('Ctrl Pts',(0.392452217526058,-1.94424311303873,
-27.1690991815742));
#40886=CARTESIAN_POINT('Ctrl Pts',(0.261961270808454,-1.94279829722498,
-27.1513145266199));
#40887=CARTESIAN_POINT('Ctrl Pts',(0.130357497803029,-1.94204670075839,
-27.1423928625267));
#40888=CARTESIAN_POINT('Ctrl Pts',(-0.0012244446283809,-1.94204416881763,
-27.1423803600789));
#40889=CARTESIAN_POINT('Ctrl Pts',(-0.132937227564624,-1.94204163435919,
-27.1423678451991));
#40890=CARTESIAN_POINT('Ctrl Pts',(-0.264629521271901,-1.94278968028664,
-27.1512822184035));
#40891=CARTESIAN_POINT('Ctrl Pts',(-0.395211802238616,-1.94423427599342,
-27.1691724987033));
#40892=CARTESIAN_POINT('Ctrl Pts',(-0.525191584400474,-1.94567220642233,
-27.1869802343238));
#40893=CARTESIAN_POINT('Ctrl Pts',(-0.654073098514614,-1.94779976552174,
-27.2136812604207));
#40894=CARTESIAN_POINT('Ctrl Pts',(-0.780761159825137,-1.95051665312194,
-27.2493254261413));
#40895=CARTESIAN_POINT('Ctrl Pts',(-0.905730503191791,-1.95319668197301,
-27.284486024061));
#40896=CARTESIAN_POINT('Ctrl Pts',(-1.02847993168707,-1.95644703883071,
-27.3283458553242));
#40897=CARTESIAN_POINT('Ctrl Pts',(-1.14812360802916,-1.9601403266743,-27.380250679094));
#40898=CARTESIAN_POINT('Ctrl Pts',(-1.26522460546488,-1.96375512440974,
-27.4310524165615));
#40899=CARTESIAN_POINT('Ctrl Pts',(-1.37935085255374,-1.96779375243808,
-27.4895608744682));
#40900=CARTESIAN_POINT('Ctrl Pts',(-1.48962667553174,-1.97211585340783,
-27.5551628282496));
#40901=CARTESIAN_POINT('Ctrl Pts',(-1.5966495103396,-1.97631045822345,-27.6188296127996));
#40902=CARTESIAN_POINT('Ctrl Pts',(-1.70004567430087,-1.98077163288984,
-27.6891776063067));
#40903=CARTESIAN_POINT('Ctrl Pts',(-1.79896953891725,-1.98535773050927,
-27.7656458759941));
#40904=CARTESIAN_POINT('Ctrl Pts',(-1.88227805225432,-1.98921990245508,
-27.8300434598311));
#40905=CARTESIAN_POINT('Ctrl Pts',(-1.96241327293777,-1.99316904229066,
-27.8987816629645));
#40906=CARTESIAN_POINT('Ctrl Pts',(-2.03883360446083,-1.99709174802028,
-27.9715254605583));
#40907=CARTESIAN_POINT('Ctrl Pts',(-2.07163284680243,-1.99877535463775,
-28.0027467520468));
#40908=CARTESIAN_POINT('Ctrl Pts',(-2.1037475964743,-2.00045425090691,-28.0347059052958));
#40909=CARTESIAN_POINT('Ctrl Pts',(-2.13513427484619,-2.00212021210337,
-28.0673759138912));
#40910=CARTESIAN_POINT('Ctrl Pts',(-2.23341005555917,-2.00733655373979,
-28.1696699687946));
#40911=CARTESIAN_POINT('Ctrl Pts',(-2.32464409832483,-2.01242717098687,
-28.2789336743929));
#40912=CARTESIAN_POINT('Ctrl Pts',(-2.40797105482908,-2.01720078911666,
-28.3945871456283));
#40913=CARTESIAN_POINT('Ctrl Pts',(-2.48245612953968,-2.02146787527885,
-28.4979685459206));
#40914=CARTESIAN_POINT('Ctrl Pts',(-2.5506222869504,-2.02548272140289,-28.6064554636897));
#40915=CARTESIAN_POINT('Ctrl Pts',(-2.61184466862664,-2.0291407687602,-28.7196209343883));
#40916=CARTESIAN_POINT('Ctrl Pts',(-2.68434196982149,-2.03347249440997,
-28.8536273384104));
#40917=CARTESIAN_POINT('Ctrl Pts',(-2.74710988830725,-2.037304020544,-28.9942033551653));
#40918=CARTESIAN_POINT('Ctrl Pts',(-2.79941817523428,-2.04052343290909,
-29.1362172253607));
#40919=CARTESIAN_POINT('Ctrl Pts',(-2.84069994926609,-2.04306419770141,
-29.2482947725946));
#40920=CARTESIAN_POINT('Ctrl Pts',(-2.87546707541627,-2.0452247984993,-29.3612672939009));
#40921=CARTESIAN_POINT('Ctrl Pts',(-2.90337385306132,-2.04696563544976,
-29.4726235687673));
#40922=CARTESIAN_POINT('Ctrl Pts',(1.92207267078475,-2.1039818201281,-32.4806858184279));
#40923=CARTESIAN_POINT('Ctrl Pts',(1.94570149082075,-2.10449565912181,-32.4596820712235));
#40924=CARTESIAN_POINT('Ctrl Pts',(1.96901911603971,-2.1049796930935,-32.4382919517595));
#40925=CARTESIAN_POINT('Ctrl Pts',(1.99201749223354,-2.10543071793912,-32.4165308998389));
#40926=CARTESIAN_POINT('Ctrl Pts',(2.06732876952195,-2.10690765948167,-32.3452714073658));
#40927=CARTESIAN_POINT('Ctrl Pts',(2.13921799697769,-2.10802702932969,-32.2700343379296));
#40928=CARTESIAN_POINT('Ctrl Pts',(2.20739068358619,-2.10870039618712,-32.191359200355));
#40929=CARTESIAN_POINT('Ctrl Pts',(2.27504610063264,-2.10936865378164,-32.1132810211224));
#40930=CARTESIAN_POINT('Ctrl Pts',(2.33904087107875,-2.10959750519711,-32.0318171289645));
#40931=CARTESIAN_POINT('Ctrl Pts',(2.39907206939851,-2.10934954213335,-31.9474917835656));
#40932=CARTESIAN_POINT('Ctrl Pts',(2.45953044016332,-2.10909981460393,-31.8625663924407));
#40933=CARTESIAN_POINT('Ctrl Pts',(2.51596829845644,-2.10836641745561,-31.7747390657846));
#40934=CARTESIAN_POINT('Ctrl Pts',(2.56806548722448,-2.10716268647844,-31.6845364347016));
#40935=CARTESIAN_POINT('Ctrl Pts',(2.62076318314301,-2.10594508049043,-31.5932940675744));
#40936=CARTESIAN_POINT('Ctrl Pts',(2.66901916924568,-2.10424639435496,-31.4996217130001));
#40937=CARTESIAN_POINT('Ctrl Pts',(2.71249669614725,-2.10213221353835,-31.4040494206905));
#40938=CARTESIAN_POINT('Ctrl Pts',(2.75731514920407,-2.09995282753284,-31.3055295047323));
#40939=CARTESIAN_POINT('Ctrl Pts',(2.79705536527492,-2.09733221388986,-31.2049911191522));
#40940=CARTESIAN_POINT('Ctrl Pts',(2.83134952205391,-2.09439377260728,-31.1029922953511));
#40941=CARTESIAN_POINT('Ctrl Pts',(2.8551918307538,-2.09235088160964,-31.0320797063708));
#40942=CARTESIAN_POINT('Ctrl Pts',(2.87640183846363,-2.09015549991434,-30.960460741654));
#40943=CARTESIAN_POINT('Ctrl Pts',(2.89485812731065,-2.08786139532915,-30.8883150573738));
#40944=CARTESIAN_POINT('Ctrl Pts',(2.90485621446488,-2.08661863966067,-30.8492325069643));
#40945=CARTESIAN_POINT('Ctrl Pts',(2.91404624218871,-2.08534708334318,-30.8099952396228));
#40946=CARTESIAN_POINT('Ctrl Pts',(2.92240935668647,-2.0840546461131,-30.7706352155149));
#40947=CARTESIAN_POINT('Ctrl Pts',(2.94423157437584,-2.08068223663669,-30.6679314901779));
#40948=CARTESIAN_POINT('Ctrl Pts',(2.96042458860711,-2.07716776638078,-30.5643979173112));
#40949=CARTESIAN_POINT('Ctrl Pts',(2.97105097182711,-2.07369775772111,-30.460872438973));
#40950=CARTESIAN_POINT('Ctrl Pts',(2.98105660782707,-2.07043045191757,-30.3633944700792));
#40951=CARTESIAN_POINT('Ctrl Pts',(2.98612711938388,-2.06720357050776,-30.265923986485));
#40952=CARTESIAN_POINT('Ctrl Pts',(2.98633045828053,-2.06416780224706,-30.1691214121975));
#40953=CARTESIAN_POINT('Ctrl Pts',(2.98636573781319,-2.06364109295896,-30.1523260541168));
#40954=CARTESIAN_POINT('Ctrl Pts',(2.98625453975004,-2.06312010372482,-30.1355506971481));
#40955=CARTESIAN_POINT('Ctrl Pts',(2.98599726747777,-2.06260556427644,-30.1187951986278));
#40956=CARTESIAN_POINT('Ctrl Pts',(2.98514166557009,-2.06089437740919,-30.0630719900135));
#40957=CARTESIAN_POINT('Ctrl Pts',(2.9826718792187,-2.05922215959374,-30.0064291308722));
#40958=CARTESIAN_POINT('Ctrl Pts',(2.97858161858244,-2.05764921751408,-29.949628457099));
#40959=CARTESIAN_POINT('Ctrl Pts',(2.97549374305047,-2.05646175055467,-29.9067477151756));
#40960=CARTESIAN_POINT('Ctrl Pts',(2.97148236537055,-2.05533058902833,-29.8637753993326));
#40961=CARTESIAN_POINT('Ctrl Pts',(2.96654581446586,-2.05427308936306,-29.8210264932436));
#40962=CARTESIAN_POINT('Ctrl Pts',(2.96231247261508,-2.05336622996333,-29.7843671461173));
#40963=CARTESIAN_POINT('Ctrl Pts',(2.95739877849598,-2.05251344145991,-29.7478747275606));
#40964=CARTESIAN_POINT('Ctrl Pts',(2.95180427171811,-2.05171931701828,-29.7121213665861));
#40965=CARTESIAN_POINT('Ctrl Pts',(2.94850476819136,-2.05125096180845,-29.69103490708));
#40966=CARTESIAN_POINT('Ctrl Pts',(2.94496846414992,-2.05080291548886,-29.6702049581298));
#40967=CARTESIAN_POINT('Ctrl Pts',(2.94119535400504,-2.05037525312523,-29.64973985319));
#40968=CARTESIAN_POINT('Ctrl Pts',(2.93747306284587,-2.04995335082869,-29.6295503871357));
#40969=CARTESIAN_POINT('Ctrl Pts',(2.93352030186384,-2.04955128589555,-29.609711353304));
#40970=CARTESIAN_POINT('Ctrl Pts',(2.92933714208969,-2.04916851502035,-29.5898408349141));
#40971=CARTESIAN_POINT('Ctrl Pts',(2.92545273819812,-2.048813081148,-29.5713894433516));
#40972=CARTESIAN_POINT('Ctrl Pts',(2.92136967055431,-2.04847427759482,-29.5529106469571));
#40973=CARTESIAN_POINT('Ctrl Pts',(2.91708804313664,-2.04815118292927,-29.5341422151136));
#40974=CARTESIAN_POINT('Ctrl Pts',(2.91287958321207,-2.04783360953504,-29.5156945115759));
#40975=CARTESIAN_POINT('Ctrl Pts',(2.9084792919759,-2.04753121099856,-29.4969665520236));
#40976=CARTESIAN_POINT('Ctrl Pts',(2.90388731009679,-2.04724267478498,-29.4777584835398));
#40977=CARTESIAN_POINT('',(-3.07785474838095,-2.05544258673707,-11.3802428859977));
#40978=CARTESIAN_POINT('',(-2.61114764827022,-2.0293363270777,-11.4114346363442));
#40979=CARTESIAN_POINT('Ctrl Pts',(-3.07785472543547,-2.0554425853949,-11.3802428874211));
#40980=CARTESIAN_POINT('Ctrl Pts',(-2.92178819655231,-2.04631362593077,
-11.3899240379752));
#40981=CARTESIAN_POINT('Ctrl Pts',(-2.76624123292387,-2.03739189066906,
-11.4002647340113));
#40982=CARTESIAN_POINT('Ctrl Pts',(-2.61113444695314,-2.02883635882995,
-11.4108058436411));
#40983=CARTESIAN_POINT('',(2.61122247994174,-2.02926323098797,-11.4125016806131));
#40984=CARTESIAN_POINT('Ctrl Pts',(2.61122237625547,-2.02965625320091,-11.4128346487702));
#40985=CARTESIAN_POINT('Ctrl Pts',(2.39875792985278,-2.01772426094543,-11.4270868286368));
#40986=CARTESIAN_POINT('Ctrl Pts',(2.1871564334896,-2.00643541293128,-11.4410322220247));
#40987=CARTESIAN_POINT('Ctrl Pts',(1.97613297653908,-1.99640438922013,-11.4539962913991));
#40988=CARTESIAN_POINT('Ctrl Pts',(1.91789246634328,-1.99363592003114,-11.4575742538943));
#40989=CARTESIAN_POINT('Ctrl Pts',(1.859695749177,-1.99096338945399,-11.4610776073231));
#40990=CARTESIAN_POINT('Ctrl Pts',(1.80153632549014,-1.98839997822234,-11.4644926311939));
#40991=CARTESIAN_POINT('Ctrl Pts',(1.59873281478295,-1.97946129272292,-11.4764009133992));
#40992=CARTESIAN_POINT('Ctrl Pts',(1.39638417062112,-1.9718500439803,-11.4872313448092));
#40993=CARTESIAN_POINT('Ctrl Pts',(1.19437115603402,-1.96568856683472,-11.4964386378558));
#40994=CARTESIAN_POINT('Ctrl Pts',(0.980675451148058,-1.9591707629969,-11.5061784013147));
#40995=CARTESIAN_POINT('Ctrl Pts',(0.767354975171277,-1.95427561618771,
-11.5141021933605));
#40996=CARTESIAN_POINT('Ctrl Pts',(0.554249877638709,-1.95113788380568,
-11.5196211009003));
#40997=CARTESIAN_POINT('Ctrl Pts',(0.369028086300903,-1.94841070168162,
-11.5244178981266));
#40998=CARTESIAN_POINT('Ctrl Pts',(0.183968471591849,-1.94701109754869,
-11.5273997130952));
#40999=CARTESIAN_POINT('Ctrl Pts',(-0.00104078931658883,-1.94701860388953,
-11.5282019238506));
#41000=CARTESIAN_POINT('Ctrl Pts',(-0.20445415490362,-1.94702685693614,
-11.5290839358583));
#41001=CARTESIAN_POINT('Ctrl Pts',(-0.407807096520058,-1.94873642445981,
-11.5273306514672));
#41002=CARTESIAN_POINT('Ctrl Pts',(-0.611415636147186,-1.95203148158355,
-11.5224797887525));
#41003=CARTESIAN_POINT('Ctrl Pts',(-0.809364164139178,-1.95523494106756,
-11.5177637727365));
#41004=CARTESIAN_POINT('Ctrl Pts',(-1.00739173111074,-1.95993310178898,
-11.5100789145489));
#41005=CARTESIAN_POINT('Ctrl Pts',(-1.20576775842101,-1.96602432643602,
-11.5003732163943));
#41006=CARTESIAN_POINT('Ctrl Pts',(-1.40414378573127,-1.97211555108305,
-11.4906675182397));
#41007=CARTESIAN_POINT('Ctrl Pts',(-1.60286886520362,-1.97959958284084,
-11.4789414813465));
#41008=CARTESIAN_POINT('Ctrl Pts',(-1.80218974550519,-1.98836758664635,
-11.4661962804132));
#41009=CARTESIAN_POINT('Ctrl Pts',(-1.99103922808684,-1.99667496006071,
-11.4541206534241));
#41010=CARTESIAN_POINT('Ctrl Pts',(-2.18042304860645,-2.00613336719599,
-11.4411345888113));
#41011=CARTESIAN_POINT('Ctrl Pts',(-2.37035555543366,-2.01629257404216,
-11.4281032174532));
#41012=CARTESIAN_POINT('Ctrl Pts',(-2.45052349742492,-2.02058063783243,
-11.4226028518731));
#41013=CARTESIAN_POINT('Ctrl Pts',(-2.53078895766986,-2.02499373517506,
-11.4170941227293));
#41014=CARTESIAN_POINT('Ctrl Pts',(-2.61115194137134,-2.02949891799445,
-11.411639121294));
#41015=CARTESIAN_POINT('',(3.07783214882012,-2.05593621639069,-11.3803366865443));
#41016=CARTESIAN_POINT('Ctrl Pts',(2.61122263327693,-2.02868201487814,-11.4120092747117));
#41017=CARTESIAN_POINT('Ctrl Pts',(2.76631582482945,-2.03712920349075,-11.4015963148637));
#41018=CARTESIAN_POINT('Ctrl Pts',(2.92183777297706,-2.04606748664476,-11.3909675841183));
#41019=CARTESIAN_POINT('Ctrl Pts',(3.07786335075085,-2.05541632542898,-11.3803478078873));
#41020=CARTESIAN_POINT('',(3.2359026159775,-2.06532548171789,-11.3703777985423));
#41021=CARTESIAN_POINT('Ctrl Pts',(3.07779520430534,-2.05655179109612,-11.3803235183648));
#41022=CARTESIAN_POINT('Ctrl Pts',(3.13041748499745,-2.0596409038771,-11.3767435349223));
#41023=CARTESIAN_POINT('Ctrl Pts',(3.18311592723968,-2.06275417483888,-11.3736233513253));
#41024=CARTESIAN_POINT('Ctrl Pts',(3.23586984059878,-2.06586860583926,-11.3703662673297));
#41025=CARTESIAN_POINT('',(3.23664856024641,-2.06541997225008,-17.2991999978929));
#41026=CARTESIAN_POINT('Ctrl Pts',(3.23664856024641,-2.06541997225008,-17.2991999978929));
#41027=CARTESIAN_POINT('Ctrl Pts',(3.23681728092954,-2.06558188082221,-17.1465460270592));
#41028=CARTESIAN_POINT('Ctrl Pts',(3.2378092903911,-2.06653538159817,-16.7935834100567));
#41029=CARTESIAN_POINT('Ctrl Pts',(3.24099557149147,-2.06963003990913,-16.2391544763694));
#41030=CARTESIAN_POINT('Ctrl Pts',(3.24554996678201,-2.07412283442935,-15.6358291186907));
#41031=CARTESIAN_POINT('Ctrl Pts',(3.25030484001515,-2.07889552730337,-15.0311078760445));
#41032=CARTESIAN_POINT('Ctrl Pts',(3.25441336551011,-2.08309603063915,-14.42527398279));
#41033=CARTESIAN_POINT('Ctrl Pts',(3.25707692954116,-2.08586417392827,-13.8179806012891));
#41034=CARTESIAN_POINT('Ctrl Pts',(3.25752083357516,-2.08636008311531,-13.2096246578577));
#41035=CARTESIAN_POINT('Ctrl Pts',(3.25495835163609,-2.0836979792605,-12.5981980422748));
#41036=CARTESIAN_POINT('Ctrl Pts',(3.24852404096208,-2.07718177263222,-11.9897144106618));
#41037=CARTESIAN_POINT('Ctrl Pts',(3.24098309020377,-2.06950210825037,-11.5754888699177));
#41038=CARTESIAN_POINT('Ctrl Pts',(3.23609357785739,-2.06492021774181,-11.3768457644699));
#41039=CARTESIAN_POINT('Ctrl Pts',(3.23601450783738,-2.06484630648251,-11.373619320441));
#41040=CARTESIAN_POINT('Ctrl Pts',(3.23593596564798,-2.06477284094976,-11.3703895318054));
#41041=CARTESIAN_POINT('',(3.23657188269419,-2.06534153551088,-17.9847374128284));
#41042=CARTESIAN_POINT('Ctrl Pts',(3.23664856024641,-2.06541997225008,-17.2991999978929));
#41043=CARTESIAN_POINT('Ctrl Pts',(3.23659586671488,-2.06536940622408,-17.3468756987971));
#41044=CARTESIAN_POINT('Ctrl Pts',(3.23656856170872,-2.06534326877989,-17.3945522866107));
#41045=CARTESIAN_POINT('Ctrl Pts',(3.23656896082705,-2.06534377018181,-17.6221221200761));
#41046=CARTESIAN_POINT('Ctrl Pts',(3.23657012615242,-2.06534337879792,-17.8038210873795));
#41047=CARTESIAN_POINT('Ctrl Pts',(3.23657188269388,-2.06534153551086,-17.9847374128284));
#41048=CARTESIAN_POINT('',(-2.61111949366609,-2.02928657753388,-17.9437023142098));
#41049=CARTESIAN_POINT('Ctrl Pts',(-2.6111194931606,-2.02928657750628,-17.9437023141764));
#41050=CARTESIAN_POINT('Ctrl Pts',(-1.57600593216534,-1.97277420562122,
-17.8752896129969));
#41051=CARTESIAN_POINT('Ctrl Pts',(0.353906469946108,-1.90148014402363,
-17.7529935172544));
#41052=CARTESIAN_POINT('Ctrl Pts',(2.29676905143962,-2.00870599133178,-17.924480085149));
#41053=CARTESIAN_POINT('Ctrl Pts',(3.2365718826948,-2.06534153551092,-17.9847374128284));
#41054=CARTESIAN_POINT('',(-3.2365718826939,-2.06534153551084,-17.9847374128283));
#41055=CARTESIAN_POINT('Ctrl Pts',(-2.61111949366609,-2.02928657753388,
-17.9437023142098));
#41056=CARTESIAN_POINT('Ctrl Pts',(-2.81875234052328,-2.0406223624171,-17.9574251794512));
#41057=CARTESIAN_POINT('Ctrl Pts',(-3.02717407631301,-2.05272254957051,
-17.9713114560054));
#41058=CARTESIAN_POINT('Ctrl Pts',(-3.23657188269391,-2.06534153551084,
-17.9847374128283));
#41059=CARTESIAN_POINT('',(-3.23593596335375,-2.06477283939947,-11.3703894654623));
#41060=CARTESIAN_POINT('Ctrl Pts',(-3.23593596401738,-2.06477283942456,
-11.3703894647525));
#41061=CARTESIAN_POINT('Ctrl Pts',(-3.23601450622251,-2.06484630497268,
-11.3736192543818));
#41062=CARTESIAN_POINT('Ctrl Pts',(-3.2360940577226,-2.06491840819467,-11.3767602403348));
#41063=CARTESIAN_POINT('Ctrl Pts',(-3.28422590292882,-2.11198472512398,
-13.4234076931397));
#41064=CARTESIAN_POINT('Ctrl Pts',(-3.23652783128775,-2.06535065050216,
-15.4352998782646));
#41065=CARTESIAN_POINT('Ctrl Pts',(-3.23657277689822,-2.06534385547269,
-17.6226933437992));
#41066=CARTESIAN_POINT('Ctrl Pts',(-3.23657012621139,-2.06534337873604,
-17.8038271587737));
#41067=CARTESIAN_POINT('Ctrl Pts',(-3.2365718826939,-2.06534153551084,-17.9847374128284));
#41068=CARTESIAN_POINT('Ctrl Pts',(-3.23593596401738,-2.06477283942457,
-11.3703894647526));
#41069=CARTESIAN_POINT('Ctrl Pts',(-3.18318064607444,-2.06164678027482,
-11.3736469970726));
#41070=CARTESIAN_POINT('Ctrl Pts',(-3.13048329082671,-2.05852104088958,
-11.3769782285977));
#41071=CARTESIAN_POINT('Ctrl Pts',(-3.07785477132643,-2.05544258807925,
-11.3802428845744));
#41072=CARTESIAN_POINT('',(-2.63912633614846,-2.0305825038593,-23.4602042419168));
#41073=CARTESIAN_POINT('',(1.94660615461814,-1.99343809749213,-24.3399007166515));
#41074=CARTESIAN_POINT('Ctrl Pts',(-2.63891815890426,-2.03090937194728,
-23.4605640099381));
#41075=CARTESIAN_POINT('Ctrl Pts',(-2.57069092949632,-2.02697783307983,
-23.5905899220032));
#41076=CARTESIAN_POINT('Ctrl Pts',(-2.49280814932383,-2.02253779605632,
-23.7152970983048));
#41077=CARTESIAN_POINT('Ctrl Pts',(-2.40655502964787,-2.01775533738805,
-23.8336815307012));
#41078=CARTESIAN_POINT('Ctrl Pts',(-2.32446314413585,-2.01320360579925,
-23.9463545714816));
#41079=CARTESIAN_POINT('Ctrl Pts',(-2.23479011295999,-2.00834158165483,
-24.0532985809489));
#41080=CARTESIAN_POINT('Ctrl Pts',(-2.13862719628931,-2.00335509341864,
-24.1536460659598));
#41081=CARTESIAN_POINT('Ctrl Pts',(-2.12093352671768,-2.00243759550751,
-24.1721096827427));
#41082=CARTESIAN_POINT('Ctrl Pts',(-2.10302007685531,-2.00151600931177,
-24.190349985842));
#41083=CARTESIAN_POINT('Ctrl Pts',(-2.08489354548269,-2.00059166263827,
-24.2083615856434));
#41084=CARTESIAN_POINT('Ctrl Pts',(-1.99543563554869,-1.99602983446685,
-24.2972522862234));
#41085=CARTESIAN_POINT('Ctrl Pts',(-1.90078990820332,-1.99139836734861,
-24.3805725948069));
#41086=CARTESIAN_POINT('Ctrl Pts',(-1.80174732651187,-1.98687547582441,
-24.4576762292758));
#41087=CARTESIAN_POINT('Ctrl Pts',(-1.69898972684165,-1.982182933802,-24.5376719671551));
#41088=CARTESIAN_POINT('Ctrl Pts',(-1.59150114951611,-1.97761033049424,
-24.6109757740146));
#41089=CARTESIAN_POINT('Ctrl Pts',(-1.48009773821805,-1.97331306608969,
-24.6768689330204));
#41090=CARTESIAN_POINT('Ctrl Pts',(-1.36905360466076,-1.96902966042993,
-24.7425495855596));
#41091=CARTESIAN_POINT('Ctrl Pts',(-1.25411981359012,-1.96502024562575,
-24.8008672655674));
#41092=CARTESIAN_POINT('Ctrl Pts',(-1.13605319549524,-1.96142991286828,
-24.8511135069562));
#41093=CARTESIAN_POINT('Ctrl Pts',(-1.11041960758882,-1.96065041133061,
-24.8620225298993));
#41094=CARTESIAN_POINT('Ctrl Pts',(-1.08463815715074,-1.95989061731232,
-24.8725511010247));
#41095=CARTESIAN_POINT('Ctrl Pts',(-1.05871627923612,-1.95915192999953,
-24.8826919936357));
#41096=CARTESIAN_POINT('Ctrl Pts',(-0.985241244461081,-1.95705813586262,
-24.9114361471148));
#41097=CARTESIAN_POINT('Ctrl Pts',(-0.910681653336464,-1.95513549044351,
-24.9370675670189));
#41098=CARTESIAN_POINT('Ctrl Pts',(-0.835278052412186,-1.95341456979757,
-24.9595801877773));
#41099=CARTESIAN_POINT('Ctrl Pts',(-0.712322279460726,-1.95060837585437,
-24.9962900617433));
#41100=CARTESIAN_POINT('Ctrl Pts',(-0.587123850541278,-1.94834073444966,
-25.0247068773822));
#41101=CARTESIAN_POINT('Ctrl Pts',(-0.460692338166107,-1.9467150574206,
-25.0448084797718));
#41102=CARTESIAN_POINT('Ctrl Pts',(-0.331909263579163,-1.94505914362068,
-25.0652839618033));
#41103=CARTESIAN_POINT('Ctrl Pts',(-0.201845369292106,-1.94406993971383,
-25.0771320454022));
#41104=CARTESIAN_POINT('Ctrl Pts',(-0.0715420642523354,-1.94381084899931,
-25.0803345004781));
#41105=CARTESIAN_POINT('Ctrl Pts',(-0.0480902413338543,-1.94376421818243,
-25.0809108742648));
#41106=CARTESIAN_POINT('Ctrl Pts',(-0.0246306324117139,-1.94374110538926,
-25.0812072091216));
#41107=CARTESIAN_POINT('Ctrl Pts',(-0.00116928290565843,-1.94374170274464,
-25.0812234161527));
#41108=CARTESIAN_POINT('Ctrl Pts',(0.128803537399696,-1.94374501201559,
-25.0813132009939));
#41109=CARTESIAN_POINT('Ctrl Pts',(0.258830619866978,-1.94448011545841,
-25.0728054144191));
#41110=CARTESIAN_POINT('Ctrl Pts',(0.387837616754974,-1.94589346353832,
-25.055688816754));
#41111=CARTESIAN_POINT('Ctrl Pts',(0.51707907690444,-1.94730938030216,-25.0385411105954));
#41112=CARTESIAN_POINT('Ctrl Pts',(0.645297809325559,-1.94940553453171,
-25.012753246554));
#41113=CARTESIAN_POINT('Ctrl Pts',(0.771393514954707,-1.95208063276428,
-24.9783191341716));
#41114=CARTESIAN_POINT('Ctrl Pts',(0.793305539292303,-1.95254549250938,
-24.9723354164486));
#41115=CARTESIAN_POINT('Ctrl Pts',(0.815153383398775,-1.95302772984231,
-24.9660906209875));
#41116=CARTESIAN_POINT('Ctrl Pts',(0.836931176722144,-1.95352668545461,
-24.9595847330815));
#41117=CARTESIAN_POINT('Ctrl Pts',(0.901500092336839,-1.95500603748753,
-24.9402954450915));
#41118=CARTESIAN_POINT('Ctrl Pts',(0.965453424995386,-1.95663253784695,
-24.9187109635716));
#41119=CARTESIAN_POINT('Ctrl Pts',(1.02863637449105,-1.9583872698216,-24.8948311706605));
#41120=CARTESIAN_POINT('Ctrl Pts',(1.15265648240947,-1.96183158590056,-24.847958169043));
#41121=CARTESIAN_POINT('Ctrl Pts',(1.27374678785909,-1.9657722892421,-24.7922297062563));
#41122=CARTESIAN_POINT('Ctrl Pts',(1.3908276584165,-1.97004779084986,-24.7285336236751));
#41123=CARTESIAN_POINT('Ctrl Pts',(1.50924541800924,-1.97437211231343,-24.6641102267684));
#41124=CARTESIAN_POINT('Ctrl Pts',(1.62356190778831,-1.9790382618604,-24.591536283455));
#41125=CARTESIAN_POINT('Ctrl Pts',(1.73261065266286,-1.98385876331907,-24.5117343231421));
#41126=CARTESIAN_POINT('Ctrl Pts',(1.75557148880081,-1.98487374743671,-24.4949315645562));
#41127=CARTESIAN_POINT('Ctrl Pts',(1.77829860862472,-1.98589552411659,-24.4778083726114));
#41128=CARTESIAN_POINT('Ctrl Pts',(1.80078084202138,-1.98692227374157,-24.4603733756465));
#41129=CARTESIAN_POINT('Ctrl Pts',(1.8506274960014,-1.98919873944575,-24.4217172401318));
#41130=CARTESIAN_POINT('Ctrl Pts',(1.89927055199605,-1.99149949877641,-24.3815283365078));
#41131=CARTESIAN_POINT('Ctrl Pts',(1.94658876137122,-1.99379905023128,-24.3399008862741));
#41132=CARTESIAN_POINT('',(2.6385842279831,-2.03021101218547,-23.4598822017706));
#41133=CARTESIAN_POINT('Ctrl Pts',(2.63870147030063,-2.03006717564156,-23.4598499951656));
#41134=CARTESIAN_POINT('Ctrl Pts',(3.02841473772455,-2.05254216577806,-22.7219672093624));
#41135=CARTESIAN_POINT('Ctrl Pts',(3.12535689549827,-2.05736702644637,-21.3572451381931));
#41136=CARTESIAN_POINT('Ctrl Pts',(2.24443363996642,-2.0075727180072,-19.8991125414343));
#41137=CARTESIAN_POINT('Ctrl Pts',(0.875888921590289,-1.93951562021359,
-18.8989839842624));
#41138=CARTESIAN_POINT('Ctrl Pts',(-0.876166156177594,-1.94068888543705,
-18.9034203539545));
#41139=CARTESIAN_POINT('Ctrl Pts',(-2.24514248919297,-2.008276670812,-19.8989668914236));
#41140=CARTESIAN_POINT('Ctrl Pts',(-2.79206912005562,-2.03859979060451,
-20.8121851494891));
#41141=CARTESIAN_POINT('Ctrl Pts',(-3.08399217684054,-2.05645735956288,
-22.0442240090313));
#41142=CARTESIAN_POINT('Ctrl Pts',(-2.93065240429659,-2.0466350002413,-22.9044061081406));
#41143=CARTESIAN_POINT('Ctrl Pts',(-2.63925053477479,-2.03038749422856,
-23.4599896041728));
#41144=CARTESIAN_POINT('Ctrl Pts',(1.94658876137122,-1.99379905023128,-24.3399008862741));
#41145=CARTESIAN_POINT('Ctrl Pts',(1.99464098969257,-1.99613427324596,-24.2976276944209));
#41146=CARTESIAN_POINT('Ctrl Pts',(2.04142781673245,-1.9984731378491,-24.2537468856496));
#41147=CARTESIAN_POINT('Ctrl Pts',(2.08685895123224,-2.00079368617497,-24.2083598616942));
#41148=CARTESIAN_POINT('Ctrl Pts',(2.18080318813562,-2.00559220472556,-24.1145068382608));
#41149=CARTESIAN_POINT('Ctrl Pts',(2.26895279483658,-2.01030987186438,-24.0142130776004));
#41150=CARTESIAN_POINT('Ctrl Pts',(2.35047939148303,-2.0147823881411,-23.9083777871828));
#41151=CARTESIAN_POINT('Ctrl Pts',(2.3694324676969,-2.01582214627338,-23.8837734935178));
#41152=CARTESIAN_POINT('Ctrl Pts',(2.38802744952198,-2.01684882264998,-23.8588697164727));
#41153=CARTESIAN_POINT('Ctrl Pts',(2.40625367999039,-2.01786065239614,-23.8336777755453));
#41154=CARTESIAN_POINT('Ctrl Pts',(2.4920251890086,-2.02262226036265,-23.7151260655696));
#41155=CARTESIAN_POINT('Ctrl Pts',(2.56963226957361,-2.02705128970956,-23.5901943757206));
#41156=CARTESIAN_POINT('Ctrl Pts',(2.63794735430056,-2.03099234874833,-23.4600571517336));
#41157=CARTESIAN_POINT('Ctrl Pts',(45.4957186312967,4.13505468146236,-12.2876753485083));
#41158=CARTESIAN_POINT('Ctrl Pts',(46.5747881377784,4.51315986439798,-12.6511164012708));
#41159=CARTESIAN_POINT('Ctrl Pts',(48.7315111185874,5.55100447935154,-13.1127068857499));
#41160=CARTESIAN_POINT('Ctrl Pts',(52.2255324170519,6.61037667463491,-13.0603457351622));
#41161=CARTESIAN_POINT('Ctrl Pts',(55.7352401406832,6.78357937642121,-12.1273823391115));
#41162=CARTESIAN_POINT('Ctrl Pts',(57.8454449537772,6.76763575867449,-10.9565650346632));
#41163=CARTESIAN_POINT('Ctrl Pts',(58.9417818399741,6.90315486069136,-10.1604688849966));
#41164=CARTESIAN_POINT('Ctrl Pts',(59.1869377879013,6.93283823797164,-9.9764403477307));
#41165=CARTESIAN_POINT('Ctrl Pts',(59.6656000071998,6.98501272405032,-9.59287808094242));
#41166=CARTESIAN_POINT('Ctrl Pts',(60.4698386743377,7.03851518962114,-8.88527771072978));
#41167=CARTESIAN_POINT('Ctrl Pts',(61.935425590422,6.93159705832345,-7.32309238219473));
#41168=CARTESIAN_POINT('Ctrl Pts',(62.898870223949,6.33243798646893,-5.81981710521227));
#41169=CARTESIAN_POINT('Ctrl Pts',(63.6271064539284,6.1172012971021,-4.30394126827215));
#41170=CARTESIAN_POINT('Ctrl Pts',(63.9964631920437,6.08157109535702,-3.43096909542246));
#41171=CARTESIAN_POINT('Ctrl Pts',(64.4196909334568,6.16095583450854,-2.0750183342162));
#41172=CARTESIAN_POINT('Ctrl Pts',(64.7075353735302,6.25611577526355,-0.705188274299797));
#41173=CARTESIAN_POINT('Ctrl Pts',(64.8131179042321,6.27855936375402,0.234551382385882));
#41174=CARTESIAN_POINT('Ctrl Pts',(64.8578334301675,6.26126913644566,0.94307726867782));
#41175=CARTESIAN_POINT('Ctrl Pts',(64.8763131687878,6.25212971761612,1.41873044327074));
#41176=CARTESIAN_POINT('Ctrl Pts',(64.8669425474595,6.24148249015893,2.37159989960793));
#41177=CARTESIAN_POINT('Ctrl Pts',(64.7293383040315,6.23744524570034,4.02825143678288));
#41178=CARTESIAN_POINT('Ctrl Pts',(64.4090264396697,6.21556997011337,5.41180556034465));
#41179=CARTESIAN_POINT('Ctrl Pts',(63.392616944205,6.06901676370829,8.4362633730038));
#41180=CARTESIAN_POINT('Ctrl Pts',(62.2029128798603,5.85755777132363,10.3600282958658));
#41181=CARTESIAN_POINT('Ctrl Pts',(57.9137758164067,5.23547967962912,14.7285512014021));
#41182=CARTESIAN_POINT('Ctrl Pts',(50.2340493278717,3.97178337193033,17.9121952059345));
#41183=CARTESIAN_POINT('Ctrl Pts',(42.4627846177445,3.39626629188669,14.7465965189029));
#41184=CARTESIAN_POINT('Ctrl Pts',(38.1616839203783,3.18800029201627,10.3559731559896));
#41185=CARTESIAN_POINT('Ctrl Pts',(36.9711393616719,3.15313406811575,8.42495263430108));
#41186=CARTESIAN_POINT('Ctrl Pts',(35.6532723602024,3.11897952995874,4.50504080276018));
#41187=CARTESIAN_POINT('Ctrl Pts',(35.4035953598297,3.11401329970943,2.5854570740989));
#41188=CARTESIAN_POINT('Ctrl Pts',(35.6531385708734,3.12046556629585,-1.27776505111417));
#41189=CARTESIAN_POINT('Ctrl Pts',(36.175035699066,3.13335329444264,-3.19875344300605));
#41190=CARTESIAN_POINT('Ctrl Pts',(37.619750560802,3.17534463244499,-6.07811908458911));
#41191=CARTESIAN_POINT('Ctrl Pts',(39.0211463611516,3.22647042745986,-8.16085205297379));
#41192=CARTESIAN_POINT('Ctrl Pts',(40.9332506662835,3.2798490343456,-9.84541367809451));
#41193=CARTESIAN_POINT('Ctrl Pts',(42.2378053070641,3.41504440953276,-10.725652165237));
#41194=CARTESIAN_POINT('Ctrl Pts',(42.8038448826665,3.4807437957151,-11.0806258189848));
#41195=CARTESIAN_POINT('Ctrl Pts',(43.981345015687,3.67284868940879,-11.7113672365034));
#41196=CARTESIAN_POINT('Ctrl Pts',(44.8918845743013,3.92347165996875,-12.0842981943491));
#41197=CARTESIAN_POINT('Ctrl Pts',(45.4957186312967,4.13505468146236,-12.2876753485083));
#41198=CARTESIAN_POINT('Ctrl Pts',(45.4226909351084,4.3829089607378,-12.2630789136873));
#41199=CARTESIAN_POINT('Ctrl Pts',(46.4885376077135,4.73594338198905,-12.6289760053212));
#41200=CARTESIAN_POINT('Ctrl Pts',(48.6563981762571,5.73344573284324,-13.1089448312689));
#41201=CARTESIAN_POINT('Ctrl Pts',(52.2019430219846,6.78342595894654,-13.0678581912781));
#41202=CARTESIAN_POINT('Ctrl Pts',(55.7389585640039,6.9553202878816,-12.1264740028574));
#41203=CARTESIAN_POINT('Ctrl Pts',(57.8403370940749,6.95575633967418,-10.9585779856605));
#41204=CARTESIAN_POINT('Ctrl Pts',(58.9264187763328,7.10412715681792,-10.1717777373723));
#41205=CARTESIAN_POINT('Ctrl Pts',(59.1736262174514,7.13246285828779,-9.98671186741939));
#41206=CARTESIAN_POINT('Ctrl Pts',(59.6556436943423,7.18385453217346,-9.60140532586356));
#41207=CARTESIAN_POINT('Ctrl Pts',(60.4705001186037,7.23456742927621,-8.88509390469854));
#41208=CARTESIAN_POINT('Ctrl Pts',(61.9608263373809,7.1262553463295,-7.29673934126728));
#41209=CARTESIAN_POINT('Ctrl Pts',(62.9304716293567,6.54211572529945,-5.76158733043494));
#41210=CARTESIAN_POINT('Ctrl Pts',(63.6321908187021,6.36074410415715,-4.29220747239235));
#41211=CARTESIAN_POINT('Ctrl Pts',(63.9940798094662,6.33427373390901,-3.43607273910697));
#41212=CARTESIAN_POINT('Ctrl Pts',(64.4146420733654,6.42472104796742,-2.09374987503663));
#41213=CARTESIAN_POINT('Ctrl Pts',(64.7054278241187,6.52953208474263,-0.71990867105941));
#41214=CARTESIAN_POINT('Ctrl Pts',(64.8128653718556,6.55685484276445,0.231003469905035));
#41215=CARTESIAN_POINT('Ctrl Pts',(64.8580472393094,6.5414965438589,0.95160233440216));
#41216=CARTESIAN_POINT('Ctrl Pts',(64.876095206118,6.5340459390533,1.42254718097353));
#41217=CARTESIAN_POINT('Ctrl Pts',(64.8666543146928,6.5242433141999,2.37413725116621));
#41218=CARTESIAN_POINT('Ctrl Pts',(64.7292489158462,6.51789648322309,4.02837788027091));
#41219=CARTESIAN_POINT('Ctrl Pts',(64.4075066260974,6.49250579105984,5.41929417877616));
#41220=CARTESIAN_POINT('Ctrl Pts',(63.3835505344909,6.34444534627468,8.45633506936137));
#41221=CARTESIAN_POINT('Ctrl Pts',(62.1894742836605,6.13520939625073,10.3796948486764));
#41222=CARTESIAN_POINT('Ctrl Pts',(57.8817168152093,5.51782830014487,14.7492052945439));
#41223=CARTESIAN_POINT('Ctrl Pts',(50.1889367119781,4.27174239122586,17.9080324411693));
#41224=CARTESIAN_POINT('Ctrl Pts',(42.4513123201647,3.7027604475385,14.7350414399812));
#41225=CARTESIAN_POINT('Ctrl Pts',(38.1580401199668,3.49283715598917,10.3507391715678));
#41226=CARTESIAN_POINT('Ctrl Pts',(36.9697716264182,3.45725996326839,8.42121430282625));
#41227=CARTESIAN_POINT('Ctrl Pts',(35.6532386126616,3.42202646347052,4.50394140790714));
#41228=CARTESIAN_POINT('Ctrl Pts',(35.4037695650286,3.41684585962461,2.58491200481547));
#41229=CARTESIAN_POINT('Ctrl Pts',(35.6530418433231,3.42350542454771,-1.27617009765779));
#41230=CARTESIAN_POINT('Ctrl Pts',(36.1745351298173,3.4366362204548,-3.19650288315925));
#41231=CARTESIAN_POINT('Ctrl Pts',(37.6174484445499,3.47973090050457,-6.07366716564505));
#41232=CARTESIAN_POINT('Ctrl Pts',(39.0177744495317,3.53068548887777,-8.15722126293493));
#41233=CARTESIAN_POINT('Ctrl Pts',(40.9267557148107,3.58453856247977,-9.83812324731517));
#41234=CARTESIAN_POINT('Ctrl Pts',(42.2154596021336,3.71009055098709,-10.7107480567621));
#41235=CARTESIAN_POINT('Ctrl Pts',(42.7766214516271,3.77492500412091,-11.0639711667881));
#41236=CARTESIAN_POINT('Ctrl Pts',(43.9336311230074,3.9542166984862,-11.687940244315));
#41237=CARTESIAN_POINT('Ctrl Pts',(44.8262562137227,4.1853552298959,-12.0583273903082));
#41238=CARTESIAN_POINT('Ctrl Pts',(45.4226909351084,4.3829089607378,-12.2630789136873));
#41239=CARTESIAN_POINT('Ctrl Pts',(45.2362559210283,4.81395978114001,-12.3967533670572));
#41240=CARTESIAN_POINT('Ctrl Pts',(46.3031207984177,5.12499660732279,-12.7410768028134));
#41241=CARTESIAN_POINT('Ctrl Pts',(48.51867911769,6.05214572917268,-13.2054239348972));
#41242=CARTESIAN_POINT('Ctrl Pts',(52.1723223958436,7.08619467178563,-13.1602949061944));
#41243=CARTESIAN_POINT('Ctrl Pts',(55.774901305395,7.25546503413852,-12.199711943089));
#41244=CARTESIAN_POINT('Ctrl Pts',(57.8793869234972,7.28458661649953,-11.04383767945));
#41245=CARTESIAN_POINT('Ctrl Pts',(58.9653776144854,7.45501929857546,-10.2803849930773));
#41246=CARTESIAN_POINT('Ctrl Pts',(59.2169323719478,7.4810504105106,-10.0906577031871));
#41247=CARTESIAN_POINT('Ctrl Pts',(59.7076295156488,7.53110130805176,-9.69852527008054));
#41248=CARTESIAN_POINT('Ctrl Pts',(60.5438525648364,7.5771049587259,-8.95863731260499));
#41249=CARTESIAN_POINT('Ctrl Pts',(62.0884747892352,7.46627421307784,-7.31479565231356));
#41250=CARTESIAN_POINT('Ctrl Pts',(63.0932644635168,6.90857606179419,-5.72668888160001));
#41251=CARTESIAN_POINT('Ctrl Pts',(63.7895723587306,6.78515334133648,-4.33844754181989));
#41252=CARTESIAN_POINT('Ctrl Pts',(64.1548219109931,6.77419647605495,-3.50652508171551));
#41253=CARTESIAN_POINT('Ctrl Pts',(64.5933355322215,6.88323321345314,-2.17605782839782));
#41254=CARTESIAN_POINT('Ctrl Pts',(64.9078972715697,7.00416841028133,-0.779117188900245));
#41255=CARTESIAN_POINT('Ctrl Pts',(65.0272679117268,7.03970770065191,0.203945258498023));
#41256=CARTESIAN_POINT('Ctrl Pts',(65.0775628156496,7.02755258341766,0.955800165700155));
#41257=CARTESIAN_POINT('Ctrl Pts',(65.097818958486,7.02290128163086,1.4257561538819));
#41258=CARTESIAN_POINT('Ctrl Pts',(65.0895377707789,7.01451194446682,2.38992058125223));
#41259=CARTESIAN_POINT('Ctrl Pts',(64.9461830318912,7.00445388751589,4.06526506532641));
#41260=CARTESIAN_POINT('Ctrl Pts',(64.6115433183857,6.97329492674332,5.48770512704195));
#41261=CARTESIAN_POINT('Ctrl Pts',(63.5587315973221,6.82268765355066,8.58954807570769));
#41262=CARTESIAN_POINT('Ctrl Pts',(62.3429488193778,6.61708776059798,10.5421828944442));
#41263=CARTESIAN_POINT('Ctrl Pts',(57.9482932775536,6.0075841917312,14.9849327447503));
#41264=CARTESIAN_POINT('Ctrl Pts',(50.120992280796,4.7907537093198,18.1842129862357));
#41265=CARTESIAN_POINT('Ctrl Pts',(42.2914692710772,4.23252014330705,14.9529853278185));
#41266=CARTESIAN_POINT('Ctrl Pts',(37.937704741533,4.02000608144395,10.4970477594956));
#41267=CARTESIAN_POINT('Ctrl Pts',(36.7331397611778,3.98325676303847,8.53535003460254));
#41268=CARTESIAN_POINT('Ctrl Pts',(35.3975369817611,3.94626884381358,4.55234212195737));
#41269=CARTESIAN_POINT('Ctrl Pts',(35.1444459825535,3.94073405856047,2.60094188977881));
#41270=CARTESIAN_POINT('Ctrl Pts',(35.3972682786971,3.947715411657,-1.3248018941845));
#41271=CARTESIAN_POINT('Ctrl Pts',(35.926694176603,3.96126168526223,-3.2774721598599));
#41272=CARTESIAN_POINT('Ctrl Pts',(37.3901262851908,4.00601018812854,-6.20291896929763));
#41273=CARTESIAN_POINT('Ctrl Pts',(38.8134827657176,4.05684134261308,-8.32453245845042));
#41274=CARTESIAN_POINT('Ctrl Pts',(40.7511286928979,4.11081645998679,-10.0306407741865));
#41275=CARTESIAN_POINT('Ctrl Pts',(42.0428239458654,4.22042746992371,-10.8926234608938));
#41276=CARTESIAN_POINT('Ctrl Pts',(42.6054806472463,4.28363615455033,-11.2484717789448));
#41277=CARTESIAN_POINT('Ctrl Pts',(43.7559350871281,4.44202305995758,-11.8552481254079));
#41278=CARTESIAN_POINT('Ctrl Pts',(44.6392514247374,4.63990738924053,-12.2040741968255));
#41279=CARTESIAN_POINT('Ctrl Pts',(45.2362559210283,4.81395978114001,-12.3967533670572));
#41280=CARTESIAN_POINT('Ctrl Pts',(45.0393082808176,5.03095193627101,-12.7701404172511));
#41281=CARTESIAN_POINT('Ctrl Pts',(46.1334687087117,5.35176317337511,-13.0718012479004));
#41282=CARTESIAN_POINT('Ctrl Pts',(48.4047643981397,6.28128470705804,-13.4535437106496));
#41283=CARTESIAN_POINT('Ctrl Pts',(52.1693689098252,7.31892628045186,-13.3716165012657));
#41284=CARTESIAN_POINT('Ctrl Pts',(55.8543152135557,7.48812989610121,-12.3862535247233));
#41285=CARTESIAN_POINT('Ctrl Pts',(57.9923320772498,7.52622499658178,-11.2496579661572));
#41286=CARTESIAN_POINT('Ctrl Pts',(59.1068119148139,7.6978190428995,-10.5096866568958));
#41287=CARTESIAN_POINT('Ctrl Pts',(59.3629402571142,7.72383493669142,-10.3124417661215));
#41288=CARTESIAN_POINT('Ctrl Pts',(59.8647407600303,7.77395345886841,-9.90933860675373));
#41289=CARTESIAN_POINT('Ctrl Pts',(60.7218337050463,7.82050499147147,-9.14015892556009));
#41290=CARTESIAN_POINT('Ctrl Pts',(62.3247704239217,7.7061385428919,-7.43738447894348));
#41291=CARTESIAN_POINT('Ctrl Pts',(63.3886024430437,7.14841447789296,-5.82205137164671));
#41292=CARTESIAN_POINT('Ctrl Pts',(64.1366259862645,7.02254302921227,-4.47918514639915));
#41293=CARTESIAN_POINT('Ctrl Pts',(64.5266343691297,7.00658243194664,-3.64991069569223));
#41294=CARTESIAN_POINT('Ctrl Pts',(65.0054037197404,7.10634554942755,-2.30157654706013));
#41295=CARTESIAN_POINT('Ctrl Pts',(65.3561087229281,7.21883370016228,-0.863559409343484));
#41296=CARTESIAN_POINT('Ctrl Pts',(65.4922044619082,7.24991771370432,0.156636010686802));
#41297=CARTESIAN_POINT('Ctrl Pts',(65.5502525107814,7.23511124126408,0.939802923614275));
#41298=CARTESIAN_POINT('Ctrl Pts',(65.5750930683425,7.22873886389136,1.42145069534216));
#41299=CARTESIAN_POINT('Ctrl Pts',(65.5687887080707,7.21933156229316,2.41592252691496));
#41300=CARTESIAN_POINT('Ctrl Pts',(65.414725807752,7.21198235972297,4.14322185797141));
#41301=CARTESIAN_POINT('Ctrl Pts',(65.0596681727028,7.18443986743527,5.61298191689179));
#41302=CARTESIAN_POINT('Ctrl Pts',(63.9672133193117,7.03419770034737,8.81868578869884));
#41303=CARTESIAN_POINT('Ctrl Pts',(62.7161166820525,6.82577914982853,10.8349003538464));
#41304=CARTESIAN_POINT('Ctrl Pts',(58.1850006970887,6.20879216622989,15.4282146019174));
#41305=CARTESIAN_POINT('Ctrl Pts',(50.1104914220837,4.9684119737969,18.7709296527553));
#41306=CARTESIAN_POINT('Ctrl Pts',(41.9978933461976,4.40390858006523,15.4335469013269));
#41307=CARTESIAN_POINT('Ctrl Pts',(37.493584849084,4.19415487226654,10.8143287573227));
#41308=CARTESIAN_POINT('Ctrl Pts',(36.2484614816851,4.15867987120878,8.78180343114533));
#41309=CARTESIAN_POINT('Ctrl Pts',(34.8683368651209,4.12336748697614,4.65611205748337));
#41310=CARTESIAN_POINT('Ctrl Pts',(34.6069082029005,4.11816980101638,2.63537705212125));
#41311=CARTESIAN_POINT('Ctrl Pts',(34.8681508421745,4.12485500101605,-1.42986135097754));
#41312=CARTESIAN_POINT('Ctrl Pts',(35.4155051923742,4.13797466334024,-3.45205726244952));
#41313=CARTESIAN_POINT('Ctrl Pts',(36.9285012394375,4.18123249165731,-6.48311952745601));
#41314=CARTESIAN_POINT('Ctrl Pts',(38.4015645590874,4.23156809046291,-8.68099638738615));
#41315=CARTESIAN_POINT('Ctrl Pts',(40.4097975334022,4.28659532550123,-10.4483512133793));
#41316=CARTESIAN_POINT('Ctrl Pts',(41.7493555547286,4.40717619984816,-11.317445711143));
#41317=CARTESIAN_POINT('Ctrl Pts',(42.3294549111165,4.47074736329829,-11.6836732045952));
#41318=CARTESIAN_POINT('Ctrl Pts',(43.5186765626443,4.64093291483995,-12.282897501734));
#41319=CARTESIAN_POINT('Ctrl Pts',(44.4270295293464,4.85142990393974,-12.6013347174204));
#41320=CARTESIAN_POINT('Ctrl Pts',(45.0393082808176,5.03095193627101,-12.7701404172511));
#41321=CARTESIAN_POINT('Ctrl Pts',(44.9671960021647,5.06936132425713,-12.9468323394379));
#41322=CARTESIAN_POINT('Ctrl Pts',(46.0737017506393,5.40581314007301,-13.2335334133338));
#41323=CARTESIAN_POINT('Ctrl Pts',(48.3643075999864,6.35380835363947,-13.5778554041427));
#41324=CARTESIAN_POINT('Ctrl Pts',(52.1729677903268,7.39852199644268,-13.4768906188369));
#41325=CARTESIAN_POINT('Ctrl Pts',(55.8938002527975,7.56810054532598,-12.4809580618348));
#41326=CARTESIAN_POINT('Ctrl Pts',(58.0500408302575,7.60482227579029,-11.352167081635));
#41327=CARTESIAN_POINT('Ctrl Pts',(59.1799059046439,7.77152332437818,-10.6198965981888));
#41328=CARTESIAN_POINT('Ctrl Pts',(59.4379281617953,7.7981238809332,-10.4193877736077));
#41329=CARTESIAN_POINT('Ctrl Pts',(59.9445192777259,7.84863591825408,-10.0113807547288));
#41330=CARTESIAN_POINT('Ctrl Pts',(60.809824883128,7.8967925806761,-9.23021697908096));
#41331=CARTESIAN_POINT('Ctrl Pts',(62.4360688307817,7.7807213081155,-7.50363616006776));
#41332=CARTESIAN_POINT('Ctrl Pts',(63.5247667463043,7.21631726880368,-5.882214856638));
#41333=CARTESIAN_POINT('Ctrl Pts',(64.2978125074662,7.07524290401267,-4.54781307837155));
#41334=CARTESIAN_POINT('Ctrl Pts',(64.6990534903062,7.0525690841578,-3.71481086803514));
#41335=CARTESIAN_POINT('Ctrl Pts',(65.1937668335651,7.14243217860219,-2.35375057630837));
#41336=CARTESIAN_POINT('Ctrl Pts',(65.5570967288631,7.2462698730418,-0.89745620523494));
#41337=CARTESIAN_POINT('Ctrl Pts',(65.6986423579354,7.27296271621864,0.136607376960506));
#41338=CARTESIAN_POINT('Ctrl Pts',(65.7592354870047,7.25589970503656,0.930580036746943));
#41339=CARTESIAN_POINT('Ctrl Pts',(65.7856454558346,7.24790516504022,1.41859891137044));
#41340=CARTESIAN_POINT('Ctrl Pts',(65.7799206851199,7.23760363176885,2.42672092669585));
#41341=CARTESIAN_POINT('Ctrl Pts',(65.6219675454031,7.23269723783848,4.17753766607333));
#41342=CARTESIAN_POINT('Ctrl Pts',(65.2593810692705,7.20859173918288,5.66675087052868));
#41343=CARTESIAN_POINT('Ctrl Pts',(64.1513986946448,7.05911518128976,8.91567711964445));
#41344=CARTESIAN_POINT('Ctrl Pts',(62.8850361125523,6.84822040784708,10.9598101495106));
#41345=CARTESIAN_POINT('Ctrl Pts',(58.2964793934186,6.2251056267945,15.6180768610311));
#41346=CARTESIAN_POINT('Ctrl Pts',(50.1158709003265,4.96503903391737,19.021940331474));
#41347=CARTESIAN_POINT('Ctrl Pts',(41.8772269224742,4.39494460937913,15.639166517446));
#41348=CARTESIAN_POINT('Ctrl Pts',(37.3065111143528,4.18729150714763,10.9500795882153));
#41349=CARTESIAN_POINT('Ctrl Pts',(36.0433455999976,4.1527741837325,8.88726750897097));
#41350=CARTESIAN_POINT('Ctrl Pts',(34.643523589437,4.11877042040954,4.70052993027424));
#41351=CARTESIAN_POINT('Ctrl Pts',(34.3784008811423,4.11383558693573,2.65012644089586));
#41352=CARTESIAN_POINT('Ctrl Pts',(34.6433770295448,4.12027840323245,-1.47489204003542));
#41353=CARTESIAN_POINT('Ctrl Pts',(35.1985818678004,4.13308125156768,-3.52683212118584));
#41354=CARTESIAN_POINT('Ctrl Pts',(36.7334877998714,4.17508278517857,-6.60303135134555));
#41355=CARTESIAN_POINT('Ctrl Pts',(38.2279573123907,4.22527365145291,-8.83301677026279));
#41356=CARTESIAN_POINT('Ctrl Pts',(40.2667716354802,4.28049099639363,-10.6271201515531));
#41357=CARTESIAN_POINT('Ctrl Pts',(41.6289539539425,4.41064411427425,-11.5039959467974));
#41358=CARTESIAN_POINT('Ctrl Pts',(42.2177215221571,4.474688119656,-11.8752322978503));
#41359=CARTESIAN_POINT('Ctrl Pts',(43.4267198452443,4.65618460624521,-12.4764006835622));
#41360=CARTESIAN_POINT('Ctrl Pts',(44.3480089607584,4.88108701596907,-12.786397935949));
#41361=CARTESIAN_POINT('Ctrl Pts',(44.9671960021647,5.06936132425713,-12.9468323394379));
#41362=CARTESIAN_POINT('',(44.9671960021647,5.06936132425713,-12.9468323394379));
#41363=CARTESIAN_POINT('Ctrl Pts',(44.9671960021647,5.06936132425713,-12.9468323394379));
#41364=CARTESIAN_POINT('Ctrl Pts',(45.0393082808176,5.03095193627101,-12.7701404172511));
#41365=CARTESIAN_POINT('Ctrl Pts',(45.2362559210283,4.81395978114001,-12.3967533670572));
#41366=CARTESIAN_POINT('Ctrl Pts',(45.4226909351084,4.3829089607378,-12.2630789136873));
#41367=CARTESIAN_POINT('Ctrl Pts',(45.4957186312967,4.13505468146236,-12.2876753485083));
#41368=CARTESIAN_POINT('',(41.3411273923048,4.38314300528299,-11.3187137406582));
#41369=CARTESIAN_POINT('Ctrl Pts',(44.9671960021647,5.06936132425713,-12.9468323394379));
#41370=CARTESIAN_POINT('Ctrl Pts',(44.3480089607584,4.88108701596907,-12.786397935949));
#41371=CARTESIAN_POINT('Ctrl Pts',(43.4267198452443,4.65618460624521,-12.4764006835622));
#41372=CARTESIAN_POINT('Ctrl Pts',(42.2177215221571,4.474688119656,-11.8752322978503));
#41373=CARTESIAN_POINT('Ctrl Pts',(41.6289539539425,4.41064411427425,-11.5039959467974));
#41374=CARTESIAN_POINT('Ctrl Pts',(41.3411273923048,4.38314300528299,-11.3187137406582));
#41375=CARTESIAN_POINT('',(36.135527542684,4.15872006235187,-5.40462207903584));
#41376=CARTESIAN_POINT('Ctrl Pts',(41.3386675640102,4.38290809676367,-11.3171298578528));
#41377=CARTESIAN_POINT('Ctrl Pts',(40.2652156414254,4.28044885388744,-10.6257507841702));
#41378=CARTESIAN_POINT('Ctrl Pts',(38.2281132730671,4.22527416890354,-8.83280500219181));
#41379=CARTESIAN_POINT('Ctrl Pts',(36.7345527005594,4.17511854755004,-6.60462019357029));
#41380=CARTESIAN_POINT('Ctrl Pts',(36.1359227536501,4.15873087918382,-5.4054139657304));
#41381=CARTESIAN_POINT('',(34.5091948905088,4.11701580411013,0.61399232466525));
#41382=CARTESIAN_POINT('Ctrl Pts',(36.1346424692247,4.15869583809775,-5.40284865178772));
#41383=CARTESIAN_POINT('Ctrl Pts',(35.1990480848672,4.13309400924318,-3.52776649543769));
#41384=CARTESIAN_POINT('Ctrl Pts',(34.6439301778968,4.1202911596584,-1.47693598688928));
#41385=CARTESIAN_POINT('Ctrl Pts',(34.5092829751989,4.11701794563615,0.612623215338439));
#41386=CARTESIAN_POINT('',(35.2891842733433,4.13445448140289,6.63164062429908));
#41387=CARTESIAN_POINT('Ctrl Pts',(34.509081999843,4.11701305949813,0.615746995805597));
#41388=CARTESIAN_POINT('Ctrl Pts',(34.3784661277573,4.11383717338778,2.64911071365206));
#41389=CARTESIAN_POINT('Ctrl Pts',(34.6432589465792,4.11876549469344,4.69848247877565));
#41390=CARTESIAN_POINT('Ctrl Pts',(35.2886534294729,4.13444158703147,6.63005240363038));
#41391=CARTESIAN_POINT('',(38.9650172416945,4.26263943020926,12.6515372403238));
#41392=CARTESIAN_POINT('Ctrl Pts',(35.2896208971195,4.13446508713737,6.63294694983923));
#41393=CARTESIAN_POINT('Ctrl Pts',(36.0433455999976,4.1527741837325,8.88726750897097));
#41394=CARTESIAN_POINT('Ctrl Pts',(37.3065111143528,4.18729150714763,10.9500795882153));
#41395=CARTESIAN_POINT('Ctrl Pts',(38.9648272977679,4.26263080069001,12.6513423808761));
#41396=CARTESIAN_POINT('',(61.2178517606911,6.62182084999648,12.6523225981111));
#41397=CARTESIAN_POINT('Ctrl Pts',(38.9650172416945,4.26263943020926,12.6515372403238));
#41398=CARTESIAN_POINT('Ctrl Pts',(41.8774060263554,4.39495700302059,15.6392400564092));
#41399=CARTESIAN_POINT('Ctrl Pts',(50.1159598214397,4.9650527305176,19.0219033323523));
#41400=CARTESIAN_POINT('Ctrl Pts',(58.2964793934186,6.2251056267945,15.6180768610311));
#41401=CARTESIAN_POINT('Ctrl Pts',(61.2178517606911,6.62182084999648,12.6523225981111));
#41402=CARTESIAN_POINT('',(64.9287215031429,7.16301726873607,6.63668503037258));
#41403=CARTESIAN_POINT('Ctrl Pts',(61.2181484097314,6.62066005626491,12.6521825294247));
#41404=CARTESIAN_POINT('Ctrl Pts',(61.2184817862553,6.62070599214976,12.6518439895148));
#41405=CARTESIAN_POINT('Ctrl Pts',(61.2188151436046,6.62075192600279,12.6515054358842));
#41406=CARTESIAN_POINT('Ctrl Pts',(61.2191484817782,6.62079785782461,12.6511668685336));
#41407=CARTESIAN_POINT('Ctrl Pts',(61.3585198686239,6.64000232408162,12.5096091205001));
#41408=CARTESIAN_POINT('Ctrl Pts',(61.4948662035403,6.65890301905649,12.3657092611848));
#41409=CARTESIAN_POINT('Ctrl Pts',(61.6281869302241,6.67754009064395,12.2194998303496));
#41410=CARTESIAN_POINT('Ctrl Pts',(61.7230124842131,6.69079587376165,12.1155070707672));
#41411=CARTESIAN_POINT('Ctrl Pts',(61.8163080541546,6.70391793770475,12.0103450216132));
#41412=CARTESIAN_POINT('Ctrl Pts',(61.9080811679174,6.71691444214465,11.9040128177346));
#41413=CARTESIAN_POINT('Ctrl Pts',(61.9456900876825,6.72224045182945,11.8604375356053));
#41414=CARTESIAN_POINT('Ctrl Pts',(61.9830433964093,6.72754531096285,11.8166655938875));
#41415=CARTESIAN_POINT('Ctrl Pts',(62.0201418786322,6.73282929205629,11.7726977909551));
#41416=CARTESIAN_POINT('Ctrl Pts',(62.1561084355408,6.75219517100867,11.6115550589251));
#41417=CARTESIAN_POINT('Ctrl Pts',(62.2886541368923,6.7712840398024,11.4477805493039));
#41418=CARTESIAN_POINT('Ctrl Pts',(62.4178458249931,6.79009941384757,11.2814180648038));
#41419=CARTESIAN_POINT('Ctrl Pts',(62.4499480296618,6.79477475323972,11.2400794724755));
#41420=CARTESIAN_POINT('Ctrl Pts',(62.4818430174384,6.79943299647369,11.1985811492951));
#41421=CARTESIAN_POINT('Ctrl Pts',(62.5135315437829,6.80407378816793,11.1569239057277));
#41422=CARTESIAN_POINT('Ctrl Pts',(62.6418377521643,6.82286426077312,10.9882545610051));
#41423=CARTESIAN_POINT('Ctrl Pts',(62.7667618614452,6.84137151992753,10.8169790114194));
#41424=CARTESIAN_POINT('Ctrl Pts',(62.888333557696,6.85954888471648,10.6431486339496));
#41425=CARTESIAN_POINT('Ctrl Pts',(63.0088431539118,6.87756744461603,10.4708369097163));
#41426=CARTESIAN_POINT('Ctrl Pts',(63.1260591461416,6.89526116929565,10.2960145222447));
#41427=CARTESIAN_POINT('Ctrl Pts',(63.2399722491003,6.91255371978634,10.1187451005626));
#41428=CARTESIAN_POINT('Ctrl Pts',(63.3333417291813,6.92672765067446,9.97344527721647));
#41429=CARTESIAN_POINT('Ctrl Pts',(63.4244916019108,6.94063128924984,9.82650167738523));
#41430=CARTESIAN_POINT('Ctrl Pts',(63.5133942469259,6.95421218942382,9.67795776882544));
#41431=CARTESIAN_POINT('Ctrl Pts',(63.5173580953864,6.95481771280547,9.67133473142122));
#41432=CARTESIAN_POINT('Ctrl Pts',(63.5213174728839,6.95542259352705,9.66470851402652));
#41433=CARTESIAN_POINT('Ctrl Pts',(63.5252723753743,6.95602682667384,9.65807912151982));
#41434=CARTESIAN_POINT('Ctrl Pts',(63.6435744367229,6.9741011096611,9.45977567385646));
#41435=CARTESIAN_POINT('Ctrl Pts',(63.7578761830907,6.9915949103269,9.25862943060299));
#41436=CARTESIAN_POINT('Ctrl Pts',(63.8680452798276,7.00838069986764,9.05478280687235));
#41437=CARTESIAN_POINT('Ctrl Pts',(63.9757163373921,7.02478587850157,8.85555832189317));
#41438=CARTESIAN_POINT('Ctrl Pts',(64.0794401717447,7.04051441179248,8.65375513836877));
#41439=CARTESIAN_POINT('Ctrl Pts',(64.1790492592415,7.05546338414968,8.44952127121358));
#41440=CARTESIAN_POINT('Ctrl Pts',(64.2136493607692,7.06065604251341,8.3785788229234));
#41441=CARTESIAN_POINT('Ctrl Pts',(64.2477525747637,7.06575480881764,8.3073431861715));
#41442=CARTESIAN_POINT('Ctrl Pts',(64.2813505141886,7.07075593400366,8.23582079704894));
#41443=CARTESIAN_POINT('Ctrl Pts',(64.2946901741793,7.07274157094135,8.20742368791221));
#41444=CARTESIAN_POINT('Ctrl Pts',(64.3079501755489,7.07471181916513,8.17898137608073));
#41445=CARTESIAN_POINT('Ctrl Pts',(64.3211299659384,7.07666644901065,8.15049424887497));
#41446=CARTESIAN_POINT('Ctrl Pts',(64.4110197913255,7.08999756660192,7.95620414147232));
#41447=CARTESIAN_POINT('Ctrl Pts',(64.4971824252759,7.1026000785673,7.75982946344119));
#41448=CARTESIAN_POINT('Ctrl Pts',(64.5794112867232,7.11441613487273,7.56149561010692));
#41449=CARTESIAN_POINT('Ctrl Pts',(64.6655794624388,7.12679825956799,7.35366023425911));
#41450=CARTESIAN_POINT('Ctrl Pts',(64.7474272412586,7.13831620850769,7.14367380505442));
#41451=CARTESIAN_POINT('Ctrl Pts',(64.8246711519124,7.14893800982192,6.93167689573328));
#41452=CARTESIAN_POINT('Ctrl Pts',(64.8603292248536,7.15384134735136,6.8338128545176));
#41453=CARTESIAN_POINT('Ctrl Pts',(64.8950056468963,7.15855423653779,6.73552029375412));
#41454=CARTESIAN_POINT('Ctrl Pts',(64.9286699552961,7.16307609763269,6.63681248550691));
#41455=CARTESIAN_POINT('',(65.7391367015185,7.26119855263812,0.666704654999593));
#41456=CARTESIAN_POINT('Ctrl Pts',(64.9288018797564,7.16309381772388,6.63642564979216));
#41457=CARTESIAN_POINT('Ctrl Pts',(64.9288458571943,7.16309972467879,6.63629669110962));
#41458=CARTESIAN_POINT('Ctrl Pts',(64.9288898326923,7.16310563127935,6.63616773234612));
#41459=CARTESIAN_POINT('Ctrl Pts',(64.9289338062505,7.16311153752559,6.63603877350158));
#41460=CARTESIAN_POINT('Ctrl Pts',(64.9503545652844,7.16598863646083,6.57321928728059));
#41461=CARTESIAN_POINT('Ctrl Pts',(64.971388959141,7.16876609138983,6.51005745533909));
#41462=CARTESIAN_POINT('Ctrl Pts',(64.9920390165022,7.17144233608347,6.44669889230024));
#41463=CARTESIAN_POINT('Ctrl Pts',(65.0126890738633,7.17411858077712,6.3833403292614));
#41464=CARTESIAN_POINT('Ctrl Pts',(65.0329547982903,7.17669360798898,6.31978511582696));
#41465=CARTESIAN_POINT('Ctrl Pts',(65.0528373460216,7.17916647493196,6.25624184522514));
#41466=CARTESIAN_POINT('Ctrl Pts',(65.0561770622229,7.17958184794677,6.24556833933532));
#41467=CARTESIAN_POINT('Ctrl Pts',(65.0595059651528,7.17999434009969,6.23489531721834));
#41468=CARTESIAN_POINT('Ctrl Pts',(65.0628240555067,7.18040395591848,6.224222671335));
#41469=CARTESIAN_POINT('Ctrl Pts',(65.0931664635859,7.18414970392527,6.12662624021454));
#41470=CARTESIAN_POINT('Ctrl Pts',(65.1226050606912,7.18765453668743,6.02906556129779));
#41471=CARTESIAN_POINT('Ctrl Pts',(65.1511379065764,7.19092499995632,5.93142984372355));
#41472=CARTESIAN_POINT('Ctrl Pts',(65.1565797849785,7.19154875348933,5.9128084378924));
#41473=CARTESIAN_POINT('Ctrl Pts',(65.161988703818,7.19216399537294,5.89418415118355));
#41474=CARTESIAN_POINT('Ctrl Pts',(65.1673646324934,7.19277079005854,5.87555600259647));
#41475=CARTESIAN_POINT('Ctrl Pts',(65.2154331838497,7.19819640919683,5.70899350315027));
#41476=CARTESIAN_POINT('Ctrl Pts',(65.2608667358397,7.20294399273001,5.54211906858637));
#41477=CARTESIAN_POINT('Ctrl Pts',(65.3036270097848,7.20706869339074,5.37495061458637));
#41478=CARTESIAN_POINT('Ctrl Pts',(65.3257800655607,7.20920560027571,5.28834471280473));
#41479=CARTESIAN_POINT('Ctrl Pts',(65.3472150985877,7.21117586345505,5.20166043892277));
#41480=CARTESIAN_POINT('Ctrl Pts',(65.3679238187994,7.21299045865816,5.11490335790102));
#41481=CARTESIAN_POINT('Ctrl Pts',(65.4115654921534,7.21681454678692,4.9320709977942));
#41482=CARTESIAN_POINT('Ctrl Pts',(65.4519830723729,7.21994485461651,4.74891823145015));
#41483=CARTESIAN_POINT('Ctrl Pts',(65.489077587359,7.22252585471296,4.56541184608723));
#41484=CARTESIAN_POINT('Ctrl Pts',(65.5282164754697,7.22524910029323,4.37179195681246));
#41485=CARTESIAN_POINT('Ctrl Pts',(65.5636555909094,7.22736125746581,4.17777881063003));
#41486=CARTESIAN_POINT('Ctrl Pts',(65.5952517618632,7.22907154405549,3.9832989377398));
#41487=CARTESIAN_POINT('Ctrl Pts',(65.6118700002137,7.22997108185823,3.88101081913205));
#41488=CARTESIAN_POINT('Ctrl Pts',(65.6274247555755,7.23076005347637,3.7785929856992));
#41489=CARTESIAN_POINT('Ctrl Pts',(65.6418928693717,7.23147220065846,3.67603076236863));
#41490=CARTESIAN_POINT('Ctrl Pts',(65.6452225762008,7.23163609495518,3.65242698510805));
#41491=CARTESIAN_POINT('Ctrl Pts',(65.6484956836855,7.23179605039584,3.62882003309272));
#41492=CARTESIAN_POINT('Ctrl Pts',(65.6517118944198,7.23195248664629,3.60520988238758));
#41493=CARTESIAN_POINT('Ctrl Pts',(65.6809645779071,7.23337533499121,3.39046640855726));
#41494=CARTESIAN_POINT('Ctrl Pts',(65.7055108831295,7.23450635373548,3.17546255458444));
#41495=CARTESIAN_POINT('Ctrl Pts',(65.7251244766241,7.23564865272918,2.96012537847259));
#41496=CARTESIAN_POINT('Ctrl Pts',(65.7443070624322,7.2367658497625,2.74952022549235));
#41497=CARTESIAN_POINT('Ctrl Pts',(65.7587707928361,7.23789538119044,2.53859610056453));
#41498=CARTESIAN_POINT('Ctrl Pts',(65.7683035228476,7.23931496822057,2.32723654627968));
#41499=CARTESIAN_POINT('Ctrl Pts',(65.7706053312466,7.23965774697809,2.27620088318106));
#41500=CARTESIAN_POINT('Ctrl Pts',(65.7726196584985,7.24001735093067,2.22513961330637));
#41501=CARTESIAN_POINT('Ctrl Pts',(65.7743435705949,7.24039748436144,2.17405067881274));
#41502=CARTESIAN_POINT('Ctrl Pts',(65.7789289220895,7.24140858312839,2.03816166067096));
#41503=CARTESIAN_POINT('Ctrl Pts',(65.7814658400794,7.24256751566722,1.90208027562438));
#41504=CARTESIAN_POINT('Ctrl Pts',(65.7818938839385,7.24392674011077,1.76655218109663));
#41505=CARTESIAN_POINT('Ctrl Pts',(65.7822577194509,7.24508207527429,1.65135386046897));
#41506=CARTESIAN_POINT('Ctrl Pts',(65.7810981991626,7.24638198058078,1.53655483801955));
#41507=CARTESIAN_POINT('Ctrl Pts',(65.778398635131,7.24784312512079,1.42259784523347));
#41508=CARTESIAN_POINT('Ctrl Pts',(65.7759936138484,7.24914484779693,1.32107441784296));
#41509=CARTESIAN_POINT('Ctrl Pts',(65.7723418318705,7.25057459162317,1.21984766497745));
#41510=CARTESIAN_POINT('Ctrl Pts',(65.7674933210383,7.25218497646143,1.11758555148493));
#41511=CARTESIAN_POINT('Ctrl Pts',(65.7629022371217,7.25370985950005,1.02075294436282));
#41512=CARTESIAN_POINT('Ctrl Pts',(65.757238274101,7.25539653525347,0.922992088228064));
#41513=CARTESIAN_POINT('Ctrl Pts',(65.7505069779292,7.25730958972767,0.823191555098794));
#41514=CARTESIAN_POINT('Ctrl Pts',(65.7471237017694,7.25827112691603,0.773029928591891));
#41515=CARTESIAN_POINT('Ctrl Pts',(65.7434701828239,7.25929018905904,0.722353333373553));
#41516=CARTESIAN_POINT('Ctrl Pts',(65.7395430551969,7.26037728034992,0.67102260240682));
#41517=CARTESIAN_POINT('',(64.0813578732502,7.1147451735158,-4.9214479327892));
#41518=CARTESIAN_POINT('Ctrl Pts',(65.7389291876497,7.26161795425529,0.664499595664831));
#41519=CARTESIAN_POINT('Ctrl Pts',(65.6986423579354,7.27296271621864,0.136607376960506));
#41520=CARTESIAN_POINT('Ctrl Pts',(65.5570967288631,7.2462698730418,-0.89745620523494));
#41521=CARTESIAN_POINT('Ctrl Pts',(65.1937668335651,7.14243217860219,-2.35375057630837));
#41522=CARTESIAN_POINT('Ctrl Pts',(64.6990534903062,7.0525690841578,-3.71481086803514));
#41523=CARTESIAN_POINT('Ctrl Pts',(64.2978125074662,7.07524290401267,-4.54781307837155));
#41524=CARTESIAN_POINT('Ctrl Pts',(64.0834287546126,7.11436614001603,-4.91787404424419));
#41525=CARTESIAN_POINT('',(59.0519282969413,7.75264142256226,-10.7028394440091));
#41526=CARTESIAN_POINT('Ctrl Pts',(64.0813578732502,7.1147451735158,-4.9214479327892));
#41527=CARTESIAN_POINT('Ctrl Pts',(63.522973579707,7.21724646178511,-5.88488505418209));
#41528=CARTESIAN_POINT('Ctrl Pts',(62.4349210154288,7.7808032321029,-7.50485479394792));
#41529=CARTESIAN_POINT('Ctrl Pts',(60.809824883128,7.8967925806761,-9.23021697908096));
#41530=CARTESIAN_POINT('Ctrl Pts',(59.9445192777259,7.84863591825408,-10.0113807547288));
#41531=CARTESIAN_POINT('Ctrl Pts',(59.4379281617953,7.7981238809332,-10.4193877736077));
#41532=CARTESIAN_POINT('Ctrl Pts',(59.1799059046439,7.77152332437818,-10.6198965981888));
#41533=CARTESIAN_POINT('Ctrl Pts',(59.0519282969413,7.75264142256226,-10.7028394440091));
#41534=CARTESIAN_POINT('Ctrl Pts',(59.0488631773053,7.75218963151952,-10.7048255423251));
#41535=CARTESIAN_POINT('Ctrl Pts',(58.0478420217809,7.60478481070341,-11.3533179919244));
#41536=CARTESIAN_POINT('Ctrl Pts',(55.8925355385909,7.56804290542898,-12.4812965801815));
#41537=CARTESIAN_POINT('Ctrl Pts',(52.1729677903268,7.39852199644268,-13.4768906188369));
#41538=CARTESIAN_POINT('Ctrl Pts',(48.3643075999864,6.35380835363947,-13.5778554041427));
#41539=CARTESIAN_POINT('Ctrl Pts',(46.0737017506393,5.40581314007301,-13.2335334133338));
#41540=CARTESIAN_POINT('Ctrl Pts',(44.9671960021647,5.06936132425713,-12.9468323394379));
#41541=CARTESIAN_POINT('Ctrl Pts',(-78.4945771627079,9.05474218205592,24.842213566055));
#41542=CARTESIAN_POINT('Ctrl Pts',(-78.4942430393453,9.0549729145804,24.7937000767725));
#41543=CARTESIAN_POINT('Ctrl Pts',(-78.493893310809,9.05521430182308,24.7452145480178));
#41544=CARTESIAN_POINT('Ctrl Pts',(-78.4897721700274,9.05806595339949,24.1983805187352));
#41545=CARTESIAN_POINT('Ctrl Pts',(-78.4800323908824,9.0588894037684,23.1810818557846));
#41546=CARTESIAN_POINT('Ctrl Pts',(-78.453292839765,9.059173840812,21.18718883834));
#41547=CARTESIAN_POINT('Ctrl Pts',(-78.4267803867925,9.07675855169213,19.7108117288188));
#41548=CARTESIAN_POINT('Ctrl Pts',(-78.4038531589849,9.1189183801019,18.4955202792461));
#41549=CARTESIAN_POINT('Ctrl Pts',(-78.3943810292591,9.13428496488478,17.9735826164074));
#41550=CARTESIAN_POINT('Ctrl Pts',(-78.3757398731157,9.158365928414,16.9680205844024));
#41551=CARTESIAN_POINT('Ctrl Pts',(-78.3430924629631,9.20103363542677,15.2406507036223));
#41552=CARTESIAN_POINT('Ctrl Pts',(-78.3160481524978,9.29112547810365,13.8416236115423));
#41553=CARTESIAN_POINT('Ctrl Pts',(-78.2931666472542,9.45650110611498,12.7110809531426));
#41554=CARTESIAN_POINT('Ctrl Pts',(-78.2830149502941,9.53239101935469,12.2435591992148));
#41555=CARTESIAN_POINT('Ctrl Pts',(-78.2621377476868,9.7127340787664,11.3046239100435));
#41556=CARTESIAN_POINT('Ctrl Pts',(-78.233855153337,9.98806838959211,10.1083484386801));
#41557=CARTESIAN_POINT('Ctrl Pts',(-78.1944828593662,10.3777342049461,8.64934200022291));
#41558=CARTESIAN_POINT('Ctrl Pts',(-78.1618184396354,10.6635084371553,7.66205018358527));
#41559=CARTESIAN_POINT('Ctrl Pts',(-78.1387930513469,10.8452663063005,7.04333861977662));
#41560=CARTESIAN_POINT('Ctrl Pts',(-78.133402700815,10.912869808309,6.83011671310147));
#41561=CARTESIAN_POINT('Ctrl Pts',(-78.1149695289094,11.064995924835,6.37324722091285));
#41562=CARTESIAN_POINT('Ctrl Pts',(-78.0725840850058,11.3579840167717,5.55881334907034));
#41563=CARTESIAN_POINT('Ctrl Pts',(-77.9532365531557,12.0288854151737,3.83067012142867));
#41564=CARTESIAN_POINT('Ctrl Pts',(-77.8411159275384,12.6322932422376,2.21795993639161));
#41565=CARTESIAN_POINT('Ctrl Pts',(-77.8221287620908,12.9420213178242,0.991067409735633));
#41566=CARTESIAN_POINT('Ctrl Pts',(-77.8217435561929,12.9760180772211,0.857310714534967));
#41567=CARTESIAN_POINT('Ctrl Pts',(-77.8220736569469,13.0435990014378,0.583493345690348));
#41568=CARTESIAN_POINT('Ctrl Pts',(-77.8278046968341,13.1564804673548,0.109426405530356));
#41569=CARTESIAN_POINT('Ctrl Pts',(-77.8482438214774,13.304977041924,-0.565538588983384));
#41570=CARTESIAN_POINT('Ctrl Pts',(-77.8892172593172,13.4622340620191,-1.36766559761172));
#41571=CARTESIAN_POINT('Ctrl Pts',(-77.959952732425,13.6450724388,-2.42940282804239));
#41572=CARTESIAN_POINT('Ctrl Pts',(-78.0675394978228,13.824152611481,-3.74125436564201));
#41573=CARTESIAN_POINT('Ctrl Pts',(-78.1459494468364,13.9210022962567,-4.77639531899031));
#41574=CARTESIAN_POINT('Ctrl Pts',(-78.1832005730778,13.9704832935621,-5.42026978261095));
#41575=CARTESIAN_POINT('Ctrl Pts',(-78.1979784088637,13.9887758338138,-5.70207633600367));
#41576=CARTESIAN_POINT('Ctrl Pts',(-78.2284833960188,14.0140574631234,-6.2466200716614));
#41577=CARTESIAN_POINT('Ctrl Pts',(-78.2828487750725,14.034352423442,-7.19391985365614));
#41578=CARTESIAN_POINT('Ctrl Pts',(-78.3592784126476,14.0116276257462,-8.50392380560081));
#41579=CARTESIAN_POINT('Ctrl Pts',(-78.4241139961074,13.9655621504964,-9.76132886787205));
#41580=CARTESIAN_POINT('Ctrl Pts',(-78.4590782716348,13.9419667305869,-10.6099301044122));
#41581=CARTESIAN_POINT('Ctrl Pts',(-78.4754805876884,13.9336604987353,-11.0859876724879));
#41582=CARTESIAN_POINT('Ctrl Pts',(-78.4823943700663,13.9316620148722,-11.320827749481));
#41583=CARTESIAN_POINT('Ctrl Pts',(-78.4870806277781,13.9311209038135,-11.4967547220627));
#41584=CARTESIAN_POINT('Ctrl Pts',(-78.4900109429774,13.9307491749155,-11.6230481807716));
#41585=CARTESIAN_POINT('Ctrl Pts',(-78.4950039243602,13.9302052683135,-11.8709752846205));
#41586=CARTESIAN_POINT('Ctrl Pts',(-78.50158798223,13.9296731190014,-12.306866865955));
#41587=CARTESIAN_POINT('Ctrl Pts',(-78.5070362894155,13.9302180558575,-13.1764566391381));
#41588=CARTESIAN_POINT('Ctrl Pts',(-78.497971327531,13.9345131198473,-14.4200831305645));
#41589=CARTESIAN_POINT('Ctrl Pts',(-78.482140644731,13.939588022815,-15.5449301391067));
#41590=CARTESIAN_POINT('Ctrl Pts',(-78.4736152025284,13.9422773104388,-16.299632681148));
#41591=CARTESIAN_POINT('Ctrl Pts',(-78.4688194777899,13.9438174524136,-16.8040925592002));
#41592=CARTESIAN_POINT('Ctrl Pts',(-78.4666111678699,13.9446078703403,-17.1842824856503));
#41593=CARTESIAN_POINT('Ctrl Pts',(-78.4659788038903,13.944970277296,-17.5013553829099));
#41594=CARTESIAN_POINT('Ctrl Pts',(-78.4657361371791,13.9451041184716,-17.6259545333056));
#41595=CARTESIAN_POINT('Ctrl Pts',(-78.4652797768498,13.9453411302425,-17.8757845538622));
#41596=CARTESIAN_POINT('Ctrl Pts',(-78.4648652232822,13.9455334668203,-18.1255165553471));
#41597=CARTESIAN_POINT('Ctrl Pts',(-78.4644893805365,13.9456854776639,-18.3754472022896));
#41598=CARTESIAN_POINT('Ctrl Pts',(-78.4642698390973,13.9457647728761,-18.5316752423212));
#41599=CARTESIAN_POINT('Ctrl Pts',(-78.4641030424882,13.9458192895378,-18.6566913664842));
#41600=CARTESIAN_POINT('Ctrl Pts',(-78.463982245853,13.9458558892278,-18.7504648090307));
#41601=CARTESIAN_POINT('Ctrl Pts',(-78.4638850796552,13.9458829377025,-18.8286218460667));
#41602=CARTESIAN_POINT('Ctrl Pts',(-78.4638093983772,13.9459025641903,-18.8911536255898));
#41603=CARTESIAN_POINT('Ctrl Pts',(-78.4631775351181,13.9460583154654,-19.422716488597));
#41604=CARTESIAN_POINT('Ctrl Pts',(-78.4623252407263,13.9460139894593,-20.4402842043313));
#41605=CARTESIAN_POINT('Ctrl Pts',(-78.461663196691,13.9455458166235,-21.9471797599321));
#41606=CARTESIAN_POINT('Ctrl Pts',(-78.46133516632,13.9453589828729,-22.954942534609));
#41607=CARTESIAN_POINT('Ctrl Pts',(-78.4610782904957,13.9454019364029,-23.5841024904954));
#41608=CARTESIAN_POINT('Ctrl Pts',(-78.4609887806561,13.9454201016436,-23.8333894280329));
#41609=CARTESIAN_POINT('Ctrl Pts',(-78.4608536657511,13.9454604662962,-24.3326208461672));
#41610=CARTESIAN_POINT('Ctrl Pts',(-78.46072122286,13.9455386704867,-25.2081915803845));
#41611=CARTESIAN_POINT('Ctrl Pts',(-78.4607646129605,13.9456564764122,-26.4630707118391));
#41612=CARTESIAN_POINT('Ctrl Pts',(-78.4609833447558,13.9457527260614,-27.9715986022803));
#41613=CARTESIAN_POINT('Ctrl Pts',(-78.4611025507938,13.9457535017472,-28.976520387269));
#41614=CARTESIAN_POINT('Ctrl Pts',(-78.4611236704402,13.9457254084153,-29.5408216774617));
#41615=CARTESIAN_POINT('Ctrl Pts',(-78.4611270417918,13.9457179309976,-29.6662231218047));
#41616=CARTESIAN_POINT('Ctrl Pts',(-78.4611289989437,13.9456985609124,-29.9170775247896));
#41617=CARTESIAN_POINT('Ctrl Pts',(-78.4611213062099,13.9456539467802,-30.356213341546));
#41618=CARTESIAN_POINT('Ctrl Pts',(-78.4610732406616,13.9455273503159,-31.2348958611842));
#41619=CARTESIAN_POINT('Ctrl Pts',(-78.4609779260847,13.9452750970535,-32.4906412748349));
#41620=CARTESIAN_POINT('Ctrl Pts',(-78.4610256022749,13.9450184448771,-33.7450945614149));
#41621=CARTESIAN_POINT('Ctrl Pts',(-78.461256827609,13.9448645106084,-34.7467138664715));
#41622=CARTESIAN_POINT('Ctrl Pts',(-78.461454504277,13.944814809868,-35.2466998259681));
#41623=CARTESIAN_POINT('Ctrl Pts',(-78.4616408300557,13.9447904868293,-35.6223062979808));
#41624=CARTESIAN_POINT('Ctrl Pts',(-78.4617840518671,13.9447551008324,-35.8741696983526));
#41625=CARTESIAN_POINT('Ctrl Pts',(-78.4621352014927,13.9446227499953,-36.3769681150403));
#41626=CARTESIAN_POINT('Ctrl Pts',(-78.4628959419818,13.9442741979241,-37.2553128798882));
#41627=CARTESIAN_POINT('Ctrl Pts',(-78.4648207036372,13.9434162779456,-39.0069967221859));
#41628=CARTESIAN_POINT('Ctrl Pts',(-78.4665267377335,13.9435422548098,-40.5068899792746));
#41629=CARTESIAN_POINT('Ctrl Pts',(-78.4672797289669,13.9453373815765,-41.761281264071));
#41630=CARTESIAN_POINT('Ctrl Pts',(-78.46744861403,13.9454019902603,-42.1397854152623));
#41631=CARTESIAN_POINT('Ctrl Pts',(-78.4675940368839,13.9449412810732,-42.6420714244579));
#41632=CARTESIAN_POINT('Ctrl Pts',(-78.4676956880371,13.9442556435418,-43.1445884596069));
#41633=CARTESIAN_POINT('Ctrl Pts',(-78.4677599030067,13.9432273462217,-43.7718110326914));
#41634=CARTESIAN_POINT('Ctrl Pts',(-78.4677971292163,13.9425265168204,-44.5229801602098));
#41635=CARTESIAN_POINT('Ctrl Pts',(-78.4678464599873,13.9430529812452,-45.1471072402556));
#41636=CARTESIAN_POINT('Ctrl Pts',(-78.4679291472011,13.9445307104614,-45.6451047526845));
#41637=CARTESIAN_POINT('Ctrl Pts',(-78.468020348216,13.9462682631092,-46.0178540945607));
#41638=CARTESIAN_POINT('Ctrl Pts',(-78.468148706838,13.9487332459747,-46.3898211447335));
#41639=CARTESIAN_POINT('Ctrl Pts',(-78.4683807861075,13.9531152796023,-46.8845673874527));
#41640=CARTESIAN_POINT('Ctrl Pts',(-78.4686337170895,13.9577929720615,-47.2543487105996));
#41641=CARTESIAN_POINT('Ctrl Pts',(-78.4689592301306,13.9635854610414,-47.6235305242231));
#41642=CARTESIAN_POINT('Ctrl Pts',(-78.4692251198566,13.9686209787161,-47.8578271164692));
#41643=CARTESIAN_POINT('Ctrl Pts',(-78.4697866257101,13.9835436409415,-48.3393103705291));
#41644=CARTESIAN_POINT('Ctrl Pts',(-78.470862112878,14.0198646528519,-49.1904283836821));
#41645=CARTESIAN_POINT('Ctrl Pts',(-78.4724213367011,14.0887986766884,-50.4447004208244));
#41646=CARTESIAN_POINT('Ctrl Pts',(-78.4743226796318,14.1545233458233,-52.0044960456846));
#41647=CARTESIAN_POINT('Ctrl Pts',(-78.4760762905936,14.1541375255512,-53.0821713269056));
#41648=CARTESIAN_POINT('Ctrl Pts',(-78.4776544781521,14.1284631318028,-53.7698156147898));
#41649=CARTESIAN_POINT('Ctrl Pts',(-78.4785936774332,14.1115115093101,-54.0753552476011));
#41650=CARTESIAN_POINT('Ctrl Pts',(-78.4807458995816,14.0605153672445,-54.6538882081308));
#41651=CARTESIAN_POINT('Ctrl Pts',(-78.4848308816969,13.9360332161937,-55.6360647071896));
#41652=CARTESIAN_POINT('Ctrl Pts',(-78.491877924565,13.6174829420838,-57.4442356893185));
#41653=CARTESIAN_POINT('Ctrl Pts',(-78.4899803670269,13.4538371774993,-58.73175430535));
#41654=CARTESIAN_POINT('Ctrl Pts',(-78.4939878848484,13.5005570278821,-59.4963920718888));
#41655=CARTESIAN_POINT('Ctrl Pts',(-78.494330086782,13.5081132678948,-59.6097203027396));
#41656=CARTESIAN_POINT('Ctrl Pts',(-78.4951351392656,13.52569399078,-59.8258300441764));
#41657=CARTESIAN_POINT('Ctrl Pts',(-78.4965765226948,13.5647737988659,-60.2118618597667));
#41658=CARTESIAN_POINT('Ctrl Pts',(-78.4997259099805,13.6737008935838,-60.9876947457136));
#41659=CARTESIAN_POINT('Ctrl Pts',(-78.5035267773202,13.8644901121535,-61.8929344593412));
#41660=CARTESIAN_POINT('Ctrl Pts',(-78.5071315715766,14.110557833353,-62.8075866929281));
#41661=CARTESIAN_POINT('Ctrl Pts',(-78.5090479495058,14.2673734772625,-63.3251314989186));
#41662=CARTESIAN_POINT('Ctrl Pts',(-78.5102654963792,14.3786007391778,-63.670806276571));
#41663=CARTESIAN_POINT('Ctrl Pts',(-78.5110606059872,14.4544665900404,-63.9014452479474));
#41664=CARTESIAN_POINT('Ctrl Pts',(-78.5118344655014,14.5327699112622,-64.1321796205846));
#41665=CARTESIAN_POINT('Ctrl Pts',(-78.5124870725892,14.6032711905195,-64.3342200226466));
#41666=CARTESIAN_POINT('Ctrl Pts',(-78.5128531780397,14.6440966265582,-64.4496929118452));
#41667=CARTESIAN_POINT('Ctrl Pts',(-78.5133969953046,14.7058497796128,-64.6228914162233));
#41668=CARTESIAN_POINT('Ctrl Pts',(-78.5138341200789,14.7583905987037,-64.7672726597123));
#41669=CARTESIAN_POINT('Ctrl Pts',(-78.5145728733114,14.8464089436773,-65.0056542132996));
#41670=CARTESIAN_POINT('Ctrl Pts',(-78.5170679509954,14.9292431087916,-65.2185839665801));
#41671=CARTESIAN_POINT('Ctrl Pts',(-78.5208802770348,15.1184939346135,-65.6685774085504));
#41672=CARTESIAN_POINT('Ctrl Pts',(-78.5273486236522,15.4869686409682,-66.4580791550208));
#41673=CARTESIAN_POINT('Ctrl Pts',(-78.5357663537906,16.3671014409282,-68.0970395735812));
#41674=CARTESIAN_POINT('Ctrl Pts',(-78.5339375754532,17.265256936789,-69.5915577692196));
#41675=CARTESIAN_POINT('Ctrl Pts',(-78.5285044735435,17.8967482249873,-70.7930139720104));
#41676=CARTESIAN_POINT('Ctrl Pts',(-78.5289803247857,18.0256326228804,-71.037566404661));
#41677=CARTESIAN_POINT('Ctrl Pts',(-78.5289445405091,18.2909799306739,-71.5400815342296));
#41678=CARTESIAN_POINT('Ctrl Pts',(-78.5292654390903,18.6209759850393,-72.1628107133783));
#41679=CARTESIAN_POINT('Ctrl Pts',(-78.5293800439328,19.0200253462203,-72.9134949573155));
#41680=CARTESIAN_POINT('Ctrl Pts',(-78.5296335577199,19.8195296036977,-74.4139812794394));
#41681=CARTESIAN_POINT('Ctrl Pts',(-78.5295981985945,20.4894190367254,-75.6668216819808));
#41682=CARTESIAN_POINT('Ctrl Pts',(-78.5293329625961,21.4611343311253,-77.4942136478313));
#41683=CARTESIAN_POINT('Ctrl Pts',(-78.5294483398302,21.8968341110043,-78.3135083159309));
#41684=CARTESIAN_POINT('Ctrl Pts',(-78.5294483398211,22.3333556983922,-79.1344860180165));
#41685=CARTESIAN_POINT('Ctrl Pts',(-77.5605622313936,8.92234122508525,24.8316381486366));
#41686=CARTESIAN_POINT('Ctrl Pts',(-77.5604387774315,8.92234787215812,24.7827885464113));
#41687=CARTESIAN_POINT('Ctrl Pts',(-77.5603096057366,8.92235475347985,24.7339548758836));
#41688=CARTESIAN_POINT('Ctrl Pts',(-77.5587942555384,8.92244266640463,24.1833219152387));
#41689=CARTESIAN_POINT('Ctrl Pts',(-77.554258549875,8.91820891771524,23.1672059573088));
#41690=CARTESIAN_POINT('Ctrl Pts',(-77.541451457475,8.90545403671313,21.1638359878524));
#41691=CARTESIAN_POINT('Ctrl Pts',(-77.5317639126002,8.90605198121365,19.6764549410896));
#41692=CARTESIAN_POINT('Ctrl Pts',(-77.5283075185792,8.92708953511933,18.4485053088963));
#41693=CARTESIAN_POINT('Ctrl Pts',(-77.5287626473163,8.93213707683049,17.9183678770559));
#41694=CARTESIAN_POINT('Ctrl Pts',(-77.5347537825327,8.9333601545357,16.903190119934));
#41695=CARTESIAN_POINT('Ctrl Pts',(-77.5518195499198,8.93282314541542,15.168894290023));
#41696=CARTESIAN_POINT('Ctrl Pts',(-77.5546312711207,8.9885250482066,13.7837693440693));
#41697=CARTESIAN_POINT('Ctrl Pts',(-77.53359507326,9.12199597784422,12.672244322638));
#41698=CARTESIAN_POINT('Ctrl Pts',(-77.5229667840858,9.18515494747207,12.2030199939226));
#41699=CARTESIAN_POINT('Ctrl Pts',(-77.4981187857294,9.3358461525626,11.2681351002097));
#41700=CARTESIAN_POINT('Ctrl Pts',(-77.4600782135362,9.5697676915878,10.0771246130041));
#41701=CARTESIAN_POINT('Ctrl Pts',(-77.403506324231,9.91002280123826,8.62883552518502));
#41702=CARTESIAN_POINT('Ctrl Pts',(-77.3557053914638,10.1680431025947,7.65099599076623));
#41703=CARTESIAN_POINT('Ctrl Pts',(-77.3215767830405,10.3355620495419,7.03954778271346));
#41704=CARTESIAN_POINT('Ctrl Pts',(-77.3107744956535,10.3973824621495,6.82725579207872));
#41705=CARTESIAN_POINT('Ctrl Pts',(-77.2797725803335,10.5379845248233,6.37265413598938));
#41706=CARTESIAN_POINT('Ctrl Pts',(-77.2107099444863,10.8112098277032,5.56059953382364));
#41707=CARTESIAN_POINT('Ctrl Pts',(-77.0244810600929,11.4499454185789,3.83707431163502));
#41708=CARTESIAN_POINT('Ctrl Pts',(-76.8477432926891,12.0395828792395,2.23630315428687));
#41709=CARTESIAN_POINT('Ctrl Pts',(-76.8046079877836,12.364444511154,1.0247750956615));
#41710=CARTESIAN_POINT('Ctrl Pts',(-76.8019223014061,12.3999715081068,0.895013675434835));
#41711=CARTESIAN_POINT('Ctrl Pts',(-76.7976649249607,12.4720640570219,0.62764000810655));
#41712=CARTESIAN_POINT('Ctrl Pts',(-76.7962844213738,12.5955669638363,0.164676117981452));
#41713=CARTESIAN_POINT('Ctrl Pts',(-76.8083097193984,12.7670560255125,-0.497218249202318));
#41714=CARTESIAN_POINT('Ctrl Pts',(-76.8424049921976,12.9615331517708,-1.2878859532549));
#41715=CARTESIAN_POINT('Ctrl Pts',(-76.9076048367717,13.2025207156588,-2.34038669747703));
#41716=CARTESIAN_POINT('Ctrl Pts',(-77.0165986235876,13.4605791888376,-3.65307361606854));
#41717=CARTESIAN_POINT('Ctrl Pts',(-77.1017170835597,13.609227067021,-4.7029565071481));
#41718=CARTESIAN_POINT('Ctrl Pts',(-77.1431811253545,13.6838611873837,-5.36001763704743));
#41719=CARTESIAN_POINT('Ctrl Pts',(-77.1600451514562,13.7125934766704,-5.6412449157383));
#41720=CARTESIAN_POINT('Ctrl Pts',(-77.1965197113903,13.7579444542025,-6.18838193223148));
#41721=CARTESIAN_POINT('Ctrl Pts',(-77.2651383971875,13.8118043448065,-7.13931324784504));
#41722=CARTESIAN_POINT('Ctrl Pts',(-77.3690417908761,13.830839847122,-8.45694301051994));
#41723=CARTESIAN_POINT('Ctrl Pts',(-77.4621505355479,13.8168121760837,-9.72343570812446));
#41724=CARTESIAN_POINT('Ctrl Pts',(-77.5129001275405,13.8093477664188,-10.5800393080932));
#41725=CARTESIAN_POINT('Ctrl Pts',(-77.5363598234594,13.8083967802335,-11.0609170898356));
#41726=CARTESIAN_POINT('Ctrl Pts',(-77.5460246624927,13.8094608419419,-11.2982581903072));
#41727=CARTESIAN_POINT('Ctrl Pts',(-77.5524436116671,13.8110046780333,-11.4761248034273));
#41728=CARTESIAN_POINT('Ctrl Pts',(-77.5564449255508,13.8120124718556,-11.6047405441445));
#41729=CARTESIAN_POINT('Ctrl Pts',(-77.5632774692677,13.8137480384397,-11.8565145078029));
#41730=CARTESIAN_POINT('Ctrl Pts',(-77.5722937764428,13.8161794316539,-12.2989111630824));
#41731=CARTESIAN_POINT('Ctrl Pts',(-77.5797445566846,13.818941441053,-13.1791401492147));
#41732=CARTESIAN_POINT('Ctrl Pts',(-77.5674968670907,13.8186385187503,-14.4318739954401));
#41733=CARTESIAN_POINT('Ctrl Pts',(-77.5461666858491,13.81583301518,-15.5574007012155));
#41734=CARTESIAN_POINT('Ctrl Pts',(-77.534708353667,13.8142366747743,-16.3094388277202));
#41735=CARTESIAN_POINT('Ctrl Pts',(-77.528288033385,13.8133710490608,-16.8112944245664));
#41736=CARTESIAN_POINT('Ctrl Pts',(-77.5253230418953,13.813039309252,-17.1885873651413));
#41737=CARTESIAN_POINT('Ctrl Pts',(-77.5245053831638,13.8130914149489,-17.5028070181097));
#41738=CARTESIAN_POINT('Ctrl Pts',(-77.5241930537433,13.813110936165,-17.6275815282398));
#41739=CARTESIAN_POINT('Ctrl Pts',(-77.5236099127463,13.8131423047389,-17.8770136375089));
#41740=CARTESIAN_POINT('Ctrl Pts',(-77.5230795711236,13.8131600529192,-18.1266467012188));
#41741=CARTESIAN_POINT('Ctrl Pts',(-77.5226080070204,13.8131705608945,-18.3763473173682));
#41742=CARTESIAN_POINT('Ctrl Pts',(-77.5223335142488,13.8131728699296,-18.5324722230117));
#41743=CARTESIAN_POINT('Ctrl Pts',(-77.522126959027,13.8131730148287,-18.6573974883988));
#41744=CARTESIAN_POINT('Ctrl Pts',(-77.5219778740186,13.8131720644925,-18.7511081445821));
#41745=CARTESIAN_POINT('Ctrl Pts',(-77.5218584026611,13.8131704404636,-18.8292132885579));
#41746=CARTESIAN_POINT('Ctrl Pts',(-77.5217657900787,13.8131687381478,-18.8917050333239));
#41747=CARTESIAN_POINT('Ctrl Pts',(-77.5209932738126,13.8131511529393,-19.4229325698188));
#41748=CARTESIAN_POINT('Ctrl Pts',(-77.5199706551422,13.8130279794193,-20.4400524685141));
#41749=CARTESIAN_POINT('Ctrl Pts',(-77.5192704733705,13.8127761979766,-21.9468150252231));
#41750=CARTESIAN_POINT('Ctrl Pts',(-77.5188911458241,13.8126627894026,-22.9548469725142));
#41751=CARTESIAN_POINT('Ctrl Pts',(-77.518568691947,13.8126460353685,-23.5842755507642));
#41752=CARTESIAN_POINT('Ctrl Pts',(-77.5184561260384,13.8126414861031,-23.833527095969));
#41753=CARTESIAN_POINT('Ctrl Pts',(-77.5182802283595,13.8126387384901,-24.332765842506));
#41754=CARTESIAN_POINT('Ctrl Pts',(-77.5180898702341,13.8126484042317,-25.208305279854));
#41755=CARTESIAN_POINT('Ctrl Pts',(-77.5180804863412,13.8126898608283,-26.4631542351967));
#41756=CARTESIAN_POINT('Ctrl Pts',(-77.5182771608326,13.812743634875,-27.9716121803736));
#41757=CARTESIAN_POINT('Ctrl Pts',(-77.5183897450772,13.8127538497128,-28.9764797182323));
#41758=CARTESIAN_POINT('Ctrl Pts',(-77.518409404043,13.8127449387252,-29.5407448559064));
#41759=CARTESIAN_POINT('Ctrl Pts',(-77.5184126615536,13.8127424447381,-29.6661318629424));
#41760=CARTESIAN_POINT('Ctrl Pts',(-77.5184139821417,13.8127352953142,-29.9169626055781));
#41761=CARTESIAN_POINT('Ctrl Pts',(-77.5184042983497,13.8127176675713,-30.3560588133006));
#41762=CARTESIAN_POINT('Ctrl Pts',(-77.5183512122079,13.8126652565372,-31.2346783702434));
#41763=CARTESIAN_POINT('Ctrl Pts',(-77.518256016693,13.8125623200684,-32.4903746976785));
#41764=CARTESIAN_POINT('Ctrl Pts',(-77.5183410107469,13.8124753380149,-33.7448350377107));
#41765=CARTESIAN_POINT('Ctrl Pts',(-77.5186420139193,13.8124473588727,-34.7464932442673));
#41766=CARTESIAN_POINT('Ctrl Pts',(-77.5188895728758,13.8124531071784,-35.2465100432844));
#41767=CARTESIAN_POINT('Ctrl Pts',(-77.5191205277262,13.8124664844248,-35.6221434557117));
#41768=CARTESIAN_POINT('Ctrl Pts',(-77.5192975405256,13.8124566477443,-35.8740055899186));
#41769=CARTESIAN_POINT('Ctrl Pts',(-77.5197301121733,13.8123761438697,-36.3768125041924));
#41770=CARTESIAN_POINT('Ctrl Pts',(-77.5206639247282,13.8121190691633,-37.255166775776));
#41771=CARTESIAN_POINT('Ctrl Pts',(-77.5230204521266,13.8114433402877,-39.0068749104896));
#41772=CARTESIAN_POINT('Ctrl Pts',(-77.5251060267396,13.8117025312366,-40.5067885445302));
#41773=CARTESIAN_POINT('Ctrl Pts',(-77.5260313793896,13.81357505,-41.7611984172332));
#41774=CARTESIAN_POINT('Ctrl Pts',(-77.5262400106917,13.8136607899694,-42.1397051347198));
#41775=CARTESIAN_POINT('Ctrl Pts',(-77.5264214202809,13.8132243812615,-42.641997009049));
#41776=CARTESIAN_POINT('Ctrl Pts',(-77.5265497432783,13.812560662035,-43.1445200214958));
#41777=CARTESIAN_POINT('Ctrl Pts',(-77.5266338491028,13.8115556437239,-43.7717512237256));
#41778=CARTESIAN_POINT('Ctrl Pts',(-77.5266860831431,13.8108773220283,-44.5229321628846));
#41779=CARTESIAN_POINT('Ctrl Pts',(-77.5267510857491,13.8114189789815,-45.1470704258221));
#41780=CARTESIAN_POINT('Ctrl Pts',(-77.5268546649749,13.8129073872144,-45.6450777096892));
#41781=CARTESIAN_POINT('Ctrl Pts',(-77.5269672404777,13.8146523264497,-46.0178347862417));
#41782=CARTESIAN_POINT('Ctrl Pts',(-77.5271242715448,13.8171242298824,-46.3898099774271));
#41783=CARTESIAN_POINT('Ctrl Pts',(-77.5274064571625,13.8215150706867,-46.8845676431613));
#41784=CARTESIAN_POINT('Ctrl Pts',(-77.5277125964672,13.8261991156127,-47.2543581434956));
#41785=CARTESIAN_POINT('Ctrl Pts',(-77.5281051874555,13.8319981148867,-47.6235496848856));
#41786=CARTESIAN_POINT('Ctrl Pts',(-77.528417512923,13.8370375676126,-47.8578552969448));
#41787=CARTESIAN_POINT('Ctrl Pts',(-77.5290784121588,13.8519659591563,-48.3393536095675));
#41788=CARTESIAN_POINT('Ctrl Pts',(-77.5303452532985,13.8882920897764,-49.1904951739617));
#41789=CARTESIAN_POINT('Ctrl Pts',(-77.5322298106515,13.9572226845556,-50.4447903896764));
#41790=CARTESIAN_POINT('Ctrl Pts',(-77.5346109148192,14.0229378429031,-52.004597757606));
#41791=CARTESIAN_POINT('Ctrl Pts',(-77.5367463120574,14.0225525269654,-53.0822685809883));
#41792=CARTESIAN_POINT('Ctrl Pts',(-77.5385840020939,13.9968841947445,-53.7699063146854));
#41793=CARTESIAN_POINT('Ctrl Pts',(-77.5396350492413,13.9799334558601,-54.0754551446048));
#41794=CARTESIAN_POINT('Ctrl Pts',(-77.5420353655896,13.9289417295368,-54.6539965423128));
#41795=CARTESIAN_POINT('Ctrl Pts',(-77.5466086990039,13.8044720837318,-55.6361844457582));
#41796=CARTESIAN_POINT('Ctrl Pts',(-77.5547711897704,13.4859675619227,-57.4443539913586));
#41797=CARTESIAN_POINT('Ctrl Pts',(-77.5537829988704,13.3223909757157,-58.73184362296));
#41798=CARTESIAN_POINT('Ctrl Pts',(-77.5581488466774,13.3691402428739,-59.4964364928422));
#41799=CARTESIAN_POINT('Ctrl Pts',(-77.5585332519993,13.3766995350279,-59.6097599795229));
#41800=CARTESIAN_POINT('Ctrl Pts',(-77.5594169699108,13.3942864670697,-59.8258604061041));
#41801=CARTESIAN_POINT('Ctrl Pts',(-77.5609817760681,13.433376654244,-60.2118774312076));
#41802=CARTESIAN_POINT('Ctrl Pts',(-77.5643257108139,13.5423234571866,-60.9876860163811));
#41803=CARTESIAN_POINT('Ctrl Pts',(-77.5682512471025,13.733133786666,-61.8929101105795));
#41804=CARTESIAN_POINT('Ctrl Pts',(-77.5719270540266,13.9792222036695,-62.8075574722455));
#41805=CARTESIAN_POINT('Ctrl Pts',(-77.5738716287693,14.1360492148047,-63.3251033426239));
#41806=CARTESIAN_POINT('Ctrl Pts',(-77.5751065662629,14.2472839188875,-63.6707803575806));
#41807=CARTESIAN_POINT('Ctrl Pts',(-77.5759131347471,14.3231546834061,-63.9014212267432));
#41808=CARTESIAN_POINT('Ctrl Pts',(-77.5766985861895,14.4014628472646,-64.1321580938732));
#41809=CARTESIAN_POINT('Ctrl Pts',(-77.5773620846279,14.4719682833765,-64.3342012106559));
#41810=CARTESIAN_POINT('Ctrl Pts',(-77.5777347139773,14.5127960706364,-64.449675803314));
#41811=CARTESIAN_POINT('Ctrl Pts',(-77.5782886620031,14.5745527225633,-64.6228770100818));
#41812=CARTESIAN_POINT('Ctrl Pts',(-77.5787350351066,14.6270964076299,-64.7672608325005));
#41813=CARTESIAN_POINT('Ctrl Pts',(-77.5794906598248,14.7151193616744,-65.0056469690786));
#41814=CARTESIAN_POINT('Ctrl Pts',(-77.5820005722859,14.797955593113,-65.218575733287));
#41815=CARTESIAN_POINT('Ctrl Pts',(-77.5858348074542,14.9872106092925,-65.668570377743));
#41816=CARTESIAN_POINT('Ctrl Pts',(-77.5923226968906,15.3556889863614,-66.4580724359124));
#41817=CARTESIAN_POINT('Ctrl Pts',(-77.6007229792136,16.2358205060688,-68.0970342827442));
#41818=CARTESIAN_POINT('Ctrl Pts',(-77.5988428319072,17.1339682870552,-69.5915519625025));
#41819=CARTESIAN_POINT('Ctrl Pts',(-77.5934123976625,17.7654604108893,-70.7930076399653));
#41820=CARTESIAN_POINT('Ctrl Pts',(-77.5938881334521,17.8943448958101,-71.0375601872648));
#41821=CARTESIAN_POINT('Ctrl Pts',(-77.5938524835593,18.1596923809589,-71.5400754049442));
#41822=CARTESIAN_POINT('Ctrl Pts',(-77.5941733219395,18.4896885503407,-72.1628047092907));
#41823=CARTESIAN_POINT('Ctrl Pts',(-77.594287879392,18.8887379623775,-72.9134890543831));
#41824=CARTESIAN_POINT('Ctrl Pts',(-77.5945411639157,19.6882421618109,-74.4139755229999));
#41825=CARTESIAN_POINT('Ctrl Pts',(-77.5945055628805,20.3581313177361,-75.6668158185921));
#41826=CARTESIAN_POINT('Ctrl Pts',(-77.5942404436912,21.329846512682,-77.4942075142949));
#41827=CARTESIAN_POINT('Ctrl Pts',(-77.5943557645253,21.7655463117544,-78.3135022346463));
#41828=CARTESIAN_POINT('Ctrl Pts',(-77.5943557645153,22.2020678991426,-79.1344799367424));
#41829=CARTESIAN_POINT('Ctrl Pts',(-75.6921159965246,8.65897413900046,24.8219423290036));
#41830=CARTESIAN_POINT('Ctrl Pts',(-75.6923447613647,8.65879522040642,24.7727884167587));
#41831=CARTESIAN_POINT('Ctrl Pts',(-75.6925847365169,8.65860782647033,24.7236365407136));
#41832=CARTESIAN_POINT('Ctrl Pts',(-75.6954155315407,8.65639934571804,24.1696381817257));
#41833=CARTESIAN_POINT('Ctrl Pts',(-75.6994921847873,8.64926564283647,23.1576310625885));
#41834=CARTESIAN_POINT('Ctrl Pts',(-75.7102951838337,8.62911964770645,21.1444014910015));
#41835=CARTESIAN_POINT('Ctrl Pts',(-75.7290344711282,8.61493829029717,19.6425156660459));
#41836=CARTESIAN_POINT('Ctrl Pts',(-75.759278305029,8.61193125725722,18.3971139448735));
#41837=CARTESIAN_POINT('Ctrl Pts',(-75.7765502794134,8.60616141273255,17.8648515751132));
#41838=CARTESIAN_POINT('Ctrl Pts',(-75.8248824601033,8.58551179224008,16.8429356054507));
#41839=CARTESIAN_POINT('Ctrl Pts',(-75.929640513178,8.54295467644432,15.098977383154));
#41840=CARTESIAN_POINT('Ctrl Pts',(-75.997603174384,8.55594794995412,13.7000298821579));
#41841=CARTESIAN_POINT('Ctrl Pts',(-75.9829940661346,8.64280327427609,12.5772729490234));
#41842=CARTESIAN_POINT('Ctrl Pts',(-75.9733493918736,8.6841735069898,12.0967648569456));
#41843=CARTESIAN_POINT('Ctrl Pts',(-75.9416242162755,8.78166381994826,11.1511668134419));
#41844=CARTESIAN_POINT('Ctrl Pts',(-75.8808356906706,8.93169360542806,9.95649943037897));
#41845=CARTESIAN_POINT('Ctrl Pts',(-75.7828579358023,9.15097965676827,8.52048566943689));
#41846=CARTESIAN_POINT('Ctrl Pts',(-75.7043210034514,9.32436933204821,7.55803023860428));
#41847=CARTESIAN_POINT('Ctrl Pts',(-75.6511581152083,9.44176191124195,6.9578249226186));
#41848=CARTESIAN_POINT('Ctrl Pts',(-75.628363393581,9.48735617559372,6.73793790452049));
#41849=CARTESIAN_POINT('Ctrl Pts',(-75.5741769251662,9.58680749797722,6.27838908714747));
#41850=CARTESIAN_POINT('Ctrl Pts',(-75.4623493303006,9.77638255963925,5.46024348137765));
#41851=CARTESIAN_POINT('Ctrl Pts',(-75.2050639128527,10.2138340247438,3.74232314061025));
#41852=CARTESIAN_POINT('Ctrl Pts',(-75.0098015096056,10.663415287569,2.17056181264629));
#41853=CARTESIAN_POINT('Ctrl Pts',(-74.9456166558476,10.9820988934014,1.03851406443687));
#41854=CARTESIAN_POINT('Ctrl Pts',(-74.9408920572205,11.0178662505396,0.918945979694379));
#41855=CARTESIAN_POINT('Ctrl Pts',(-74.9313758811006,11.0933095500304,0.671107632293839));
#41856=CARTESIAN_POINT('Ctrl Pts',(-74.9190173258224,11.2300190033541,0.241491523103302));
#41857=CARTESIAN_POINT('Ctrl Pts',(-74.9108524012778,11.4382770412393,-0.376413458452138));
#41858=CARTESIAN_POINT('Ctrl Pts',(-74.9166341377895,11.6992118543583,-1.12272086716767));
#41859=CARTESIAN_POINT('Ctrl Pts',(-74.9432675005682,12.0514832952064,-2.13113802139702));
#41860=CARTESIAN_POINT('Ctrl Pts',(-75.0080517507911,12.4809013027542,-3.42363524866221));
#41861=CARTESIAN_POINT('Ctrl Pts',(-75.0748004827117,12.7669916964717,-4.50470312477017));
#41862=CARTESIAN_POINT('Ctrl Pts',(-75.1114900539174,12.9121996468757,-5.19585586668643));
#41863=CARTESIAN_POINT('Ctrl Pts',(-75.1270219536629,12.9687856032635,-5.4660722503953));
#41864=CARTESIAN_POINT('Ctrl Pts',(-75.1647137181936,13.0729691030591,-6.00823556293463));
#41865=CARTESIAN_POINT('Ctrl Pts',(-75.2447328180899,13.2331229490125,-6.95057580271206));
#41866=CARTESIAN_POINT('Ctrl Pts',(-75.3885826331589,13.3990097777801,-8.28181093903442));
#41867=CARTESIAN_POINT('Ctrl Pts',(-75.5306746339452,13.4951208489467,-9.57980856854873));
#41868=CARTESIAN_POINT('Ctrl Pts',(-75.6076564304303,13.5418799491235,-10.4683980241704));
#41869=CARTESIAN_POINT('Ctrl Pts',(-75.6426977577952,13.5653647317475,-10.9705730285057));
#41870=CARTESIAN_POINT('Ctrl Pts',(-75.6567932523914,13.5763949616513,-11.21968403738));
#41871=CARTESIAN_POINT('Ctrl Pts',(-75.665967802336,13.5845892879007,-11.4068849713555));
#41872=CARTESIAN_POINT('Ctrl Pts',(-75.6716767264812,13.5900584416014,-11.5428852548299));
#41873=CARTESIAN_POINT('Ctrl Pts',(-75.6815252715505,13.5991851699896,-11.8080322118912));
#41874=CARTESIAN_POINT('Ctrl Pts',(-75.6947836859738,13.6113211144299,-12.2724048014959));
#41875=CARTESIAN_POINT('Ctrl Pts',(-75.7071707703566,13.6215936347519,-13.1892081062607));
#41876=CARTESIAN_POINT('Ctrl Pts',(-75.6937744661824,13.6061651387076,-14.4733910901186));
#41877=CARTESIAN_POINT('Ctrl Pts',(-75.6670757378233,13.5780267593918,-15.6009938779762));
#41878=CARTESIAN_POINT('Ctrl Pts',(-75.6527894765495,13.562799510879,-16.3435925262125));
#41879=CARTESIAN_POINT('Ctrl Pts',(-75.6448300448953,13.5542712485532,-16.8363372080636));
#41880=CARTESIAN_POINT('Ctrl Pts',(-75.641343095406,13.5504597280976,-17.2035568900481));
#41881=CARTESIAN_POINT('Ctrl Pts',(-75.6405970526558,13.5495515514651,-17.5079024946932));
#41882=CARTESIAN_POINT('Ctrl Pts',(-75.6403086742588,13.5492098226299,-17.6332552488187));
#41883=CARTESIAN_POINT('Ctrl Pts',(-75.6397615638604,13.5485941867171,-17.881274919397));
#41884=CARTESIAN_POINT('Ctrl Pts',(-75.6392583532568,13.5480779667676,-18.1305314212828));
#41885=CARTESIAN_POINT('Ctrl Pts',(-75.6387937274463,13.5476482161608,-18.379407794415));
#41886=CARTESIAN_POINT('Ctrl Pts',(-75.6385194129121,13.5474146201461,-18.5351594934329));
#41887=CARTESIAN_POINT('Ctrl Pts',(-75.6383088963852,13.5472471341751,-18.659758006526));
#41888=CARTESIAN_POINT('Ctrl Pts',(-75.6381554906238,13.5471310613474,-18.7532425003298));
#41889=CARTESIAN_POINT('Ctrl Pts',(-75.638031303301,13.5470420138082,-18.8311610906567));
#41890=CARTESIAN_POINT('Ctrl Pts',(-75.6379340475833,13.5469752106932,-18.8935087206951));
#41891=CARTESIAN_POINT('Ctrl Pts',(-75.6371195986504,13.5464324576899,-19.4235310655964));
#41892=CARTESIAN_POINT('Ctrl Pts',(-75.6359439274737,13.5461618762464,-20.4390743303277));
#41893=CARTESIAN_POINT('Ctrl Pts',(-75.634864971159,13.5467473242472,-21.9453895012519));
#41894=CARTESIAN_POINT('Ctrl Pts',(-75.6343245502054,13.5469551304571,-22.9544210717622));
#41895=CARTESIAN_POINT('Ctrl Pts',(-75.6339553824512,13.5467702978225,-23.584833399548));
#41896=CARTESIAN_POINT('Ctrl Pts',(-75.6338241245163,13.5467000977553,-23.8339615872695));
#41897=CARTESIAN_POINT('Ctrl Pts',(-75.6336169104993,13.5465709414473,-24.3332354712502));
#41898=CARTESIAN_POINT('Ctrl Pts',(-75.633385180036,13.5463734807082,-25.2086755739493));
#41899=CARTESIAN_POINT('Ctrl Pts',(-75.6333480779871,13.5461804995033,-26.4634304778581));
#41900=CARTESIAN_POINT('Ctrl Pts',(-75.6335152876745,13.5460910742537,-27.9716539612101));
#41901=CARTESIAN_POINT('Ctrl Pts',(-75.6335968855616,13.5461354282596,-28.9763368670655));
#41902=CARTESIAN_POINT('Ctrl Pts',(-75.6335855550659,13.5461879021644,-29.5404783410885));
#41903=CARTESIAN_POINT('Ctrl Pts',(-75.6335806332078,13.5462007412436,-29.6658174535336));
#41904=CARTESIAN_POINT('Ctrl Pts',(-75.633562342921,13.5462316844819,-29.916569276828));
#41905=CARTESIAN_POINT('Ctrl Pts',(-75.6335106440104,13.546299471024,-30.3555335376507));
#41906=CARTESIAN_POINT('Ctrl Pts',(-75.6333487173523,13.5464831048139,-31.2339430110599));
#41907=CARTESIAN_POINT('Ctrl Pts',(-75.6330652885746,13.5468592114955,-32.4894754032597));
#41908=CARTESIAN_POINT('Ctrl Pts',(-75.6330206994714,13.5473116404508,-33.743958832858));
#41909=CARTESIAN_POINT('Ctrl Pts',(-75.633313476897,13.5476727368069,-34.745746801062));
#41910=CARTESIAN_POINT('Ctrl Pts',(-75.6336001558874,13.5478488490821,-35.245866546638));
#41911=CARTESIAN_POINT('Ctrl Pts',(-75.6338801375847,13.5479750387175,-35.6215898145587));
#41912=CARTESIAN_POINT('Ctrl Pts',(-75.6340982843881,13.5480410686006,-35.8734477474361));
#41913=CARTESIAN_POINT('Ctrl Pts',(-75.6346422595824,13.5481116777071,-36.3762829408899));
#41914=CARTESIAN_POINT('Ctrl Pts',(-75.6358387140055,13.5481207949868,-37.2546696620858));
#41915=CARTESIAN_POINT('Ctrl Pts',(-75.6389085318736,13.5479548706782,-39.0064589406112));
#41916=CARTESIAN_POINT('Ctrl Pts',(-75.6416606556734,13.5485909875611,-40.5064448190074));
#41917=CARTESIAN_POINT('Ctrl Pts',(-75.6428684946547,13.5506879531502,-41.7609185403146));
#41918=CARTESIAN_POINT('Ctrl Pts',(-75.6431384271574,13.5508353275622,-42.1394337958565));
#41919=CARTESIAN_POINT('Ctrl Pts',(-75.6433691289682,13.5504705830997,-42.6417451415882));
#41920=CARTESIAN_POINT('Ctrl Pts',(-75.6435296071986,13.5498727505972,-43.1442881511953));
#41921=CARTESIAN_POINT('Ctrl Pts',(-75.6436299000572,13.5489391994608,-43.7715483625547));
#41922=CARTESIAN_POINT('Ctrl Pts',(-75.6436894358512,13.5483311083971,-44.5227694286739));
#41923=CARTESIAN_POINT('Ctrl Pts',(-75.6437723235048,13.5489197957315,-45.146946138206));
#41924=CARTESIAN_POINT('Ctrl Pts',(-75.6439101440714,13.5504390634564,-45.6449865082951));
#41925=CARTESIAN_POINT('Ctrl Pts',(-75.6440617719633,13.5522043159601,-46.0177699219705));
#41926=CARTESIAN_POINT('Ctrl Pts',(-75.6442744865655,13.5546938354661,-46.389772918041));
#41927=CARTESIAN_POINT('Ctrl Pts',(-75.6446573797619,13.559104895256,-46.8845694663249));
#41928=CARTESIAN_POINT('Ctrl Pts',(-75.6450739944625,13.5638006721358,-47.2543918244836));
#41929=CARTESIAN_POINT('Ctrl Pts',(-75.6456069604917,13.5696097310337,-47.6236166737643));
#41930=CARTESIAN_POINT('Ctrl Pts',(-75.6460176039176,13.5746544762556,-47.8579539210514));
#41931=CARTESIAN_POINT('Ctrl Pts',(-75.6468926688973,13.5895854830564,-48.3395044348218));
#41932=CARTESIAN_POINT('Ctrl Pts',(-75.6485797019952,13.6258983739338,-49.1907272539963));
#41933=CARTESIAN_POINT('Ctrl Pts',(-75.6511923920832,13.6947642150988,-50.4451004143629));
#41934=CARTESIAN_POINT('Ctrl Pts',(-75.6546407320632,13.7603715617149,-52.0049430108417));
#41935=CARTESIAN_POINT('Ctrl Pts',(-75.6576093036443,13.7599216629611,-53.0825950363202));
#41936=CARTESIAN_POINT('Ctrl Pts',(-75.6600038773525,13.7342295213886,-53.7702081331066));
#41937=CARTESIAN_POINT('Ctrl Pts',(-75.6612950918065,13.7172632093226,-54.075784837558));
#41938=CARTESIAN_POINT('Ctrl Pts',(-75.6642262716333,13.6662448593001,-54.6543512556725));
#41939=CARTESIAN_POINT('Ctrl Pts',(-75.6698408369108,13.5417335232503,-55.6365742588973));
#41940=CARTESIAN_POINT('Ctrl Pts',(-75.6803639426854,13.2231870482516,-57.4447436616881));
#41941=CARTESIAN_POINT('Ctrl Pts',(-75.681282064688,13.059670403835,-58.7321430875395));
#41942=CARTESIAN_POINT('Ctrl Pts',(-75.6863956938303,13.1064525118599,-59.4965891093409));
#41943=CARTESIAN_POINT('Ctrl Pts',(-75.6868679897915,13.1140146369142,-59.6098969334171));
#41944=CARTESIAN_POINT('Ctrl Pts',(-75.6879149993631,13.1316083652691,-59.8259666891569));
#41945=CARTESIAN_POINT('Ctrl Pts',(-75.6897345617221,13.1707110281061,-60.2119348572073));
#41946=CARTESIAN_POINT('Ctrl Pts',(-75.6934742771951,13.2796876085821,-60.9876632047891));
#41947=CARTESIAN_POINT('Ctrl Pts',(-75.6976408619348,13.4705431429276,-61.8928361581727));
#41948=CARTESIAN_POINT('Ctrl Pts',(-75.701444272716,13.7166853950894,-62.8074689649149));
#41949=CARTESIAN_POINT('Ctrl Pts',(-75.7034366519234,13.873544319781,-63.3250195269508));
#41950=CARTESIAN_POINT('Ctrl Pts',(-75.7047012154514,13.9848001926648,-63.6707047148809));
#41951=CARTESIAN_POINT('Ctrl Pts',(-75.7055274561093,14.0606850141304,-63.9013523952973));
#41952=CARTESIAN_POINT('Ctrl Pts',(-75.7063332430143,14.1390069406578,-64.1320979910642));
#41953=CARTESIAN_POINT('Ctrl Pts',(-75.707016474211,14.2095241235918,-64.3341505038452));
#41954=CARTESIAN_POINT('Ctrl Pts',(-75.7074011288797,14.2503585013626,-64.4496309575972));
#41955=CARTESIAN_POINT('Ctrl Pts',(-75.7079739620691,14.3121249045545,-64.6228414340704));
#41956=CARTESIAN_POINT('Ctrl Pts',(-75.708438040624,14.3646763995539,-64.7672340258762));
#41957=CARTESIAN_POINT('Ctrl Pts',(-75.7092266721553,14.4527116415818,-65.005635688223));
#41958=CARTESIAN_POINT('Ctrl Pts',(-75.7117667830696,14.5355526360062,-65.2185617805244));
#41959=CARTESIAN_POINT('Ctrl Pts',(-75.7156454045534,14.724818485127,-65.668561251195));
#41960=CARTESIAN_POINT('Ctrl Pts',(-75.7221741072873,15.0933070411488,-66.4580654331261));
#41961=CARTESIAN_POINT('Ctrl Pts',(-75.7305427718633,15.9734396090043,-68.0970327921023));
#41962=CARTESIAN_POINT('Ctrl Pts',(-75.7285600851967,16.8715705729392,-69.5915485739548));
#41963=CARTESIAN_POINT('Ctrl Pts',(-75.7231320655152,17.5030633452021,-70.793001962088));
#41964=CARTESIAN_POINT('Ctrl Pts',(-75.7236077231866,17.6319482655893,-71.0375549507293));
#41965=CARTESIAN_POINT('Ctrl Pts',(-75.7235722165254,17.8972962896899,-71.540070471556));
#41966=CARTESIAN_POINT('Ctrl Pts',(-75.7238930232004,18.2272929043099,-72.1628002331602));
#41967=CARTESIAN_POINT('Ctrl Pts',(-75.7240075301994,18.6263425104643,-72.9134849283308));
#41968=CARTESIAN_POINT('Ctrl Pts',(-75.7242605650699,19.4258466085276,-74.4139719006252));
#41969=CARTESIAN_POINT('Ctrl Pts',(-75.7242247109526,20.0957347727082,-75.6668117968037));
#41970=CARTESIAN_POINT('Ctrl Pts',(-75.7239597457827,21.0674494694115,-77.4942025512152));
#41971=CARTESIAN_POINT('Ctrl Pts',(-75.7240750175091,21.5031493372222,-78.3134974540841));
#41972=CARTESIAN_POINT('Ctrl Pts',(-75.7240750175066,21.939670924612,-79.1344751561986));
#41973=CARTESIAN_POINT('Ctrl Pts',(-72.8865680674535,8.26575232185009,24.8276912522435));
#41974=CARTESIAN_POINT('Ctrl Pts',(-72.8869414421383,8.26573286341148,24.7787178932437));
#41975=CARTESIAN_POINT('Ctrl Pts',(-72.8873327680767,8.26571236274712,24.729744826743));
#41976=CARTESIAN_POINT('Ctrl Pts',(-72.8919550651354,8.26547621202624,24.1779986734955));
#41977=CARTESIAN_POINT('Ctrl Pts',(-72.8989341377874,8.26453602047102,23.1728399881855));
#41978=CARTESIAN_POINT('Ctrl Pts',(-72.9174048097993,8.26169786168248,21.1618965904426));
#41979=CARTESIAN_POINT('Ctrl Pts',(-72.9481006229035,8.25999530162877,19.6554113963992));
#41980=CARTESIAN_POINT('Ctrl Pts',(-72.9959818140564,8.26039309449099,18.4026337347238));
#41981=CARTESIAN_POINT('Ctrl Pts',(-73.0210030137968,8.25960530135002,17.8902665411261));
#41982=CARTESIAN_POINT('Ctrl Pts',(-73.0875426278879,8.25565539996311,16.8799446059181));
#41983=CARTESIAN_POINT('Ctrl Pts',(-73.229943398351,8.24611163285477,15.1296376299366));
#41984=CARTESIAN_POINT('Ctrl Pts',(-73.3374512605349,8.24874818684716,13.6575521217196));
#41985=CARTESIAN_POINT('Ctrl Pts',(-73.3533279432813,8.27501923579358,12.439741783186));
#41986=CARTESIAN_POINT('Ctrl Pts',(-73.3567837062602,8.28502742178981,11.9323235896795));
#41987=CARTESIAN_POINT('Ctrl Pts',(-73.3521445253704,8.3043377425253,10.9376815727366));
#41988=CARTESIAN_POINT('Ctrl Pts',(-73.3246186828076,8.3312814040697,9.70190084284496));
#41989=CARTESIAN_POINT('Ctrl Pts',(-73.2567457688751,8.37994614453916,8.2446764166352));
#41990=CARTESIAN_POINT('Ctrl Pts',(-73.1890088003569,8.43111706791072,7.28737224708644));
#41991=CARTESIAN_POINT('Ctrl Pts',(-73.1399135755569,8.47187327739597,6.69378252491712));
#41992=CARTESIAN_POINT('Ctrl Pts',(-73.1173392770425,8.48995716105188,6.43996597869799));
#41993=CARTESIAN_POINT('Ctrl Pts',(-73.0652853571013,8.52137581014927,5.94571821208205));
#41994=CARTESIAN_POINT('Ctrl Pts',(-72.9585437937225,8.5706759054832,5.08330708674856));
#41995=CARTESIAN_POINT('Ctrl Pts',(-72.710409440949,8.65655741011438,3.39659394490956));
#41996=CARTESIAN_POINT('Ctrl Pts',(-72.5373531107517,8.79271546662842,1.99110235750803));
#41997=CARTESIAN_POINT('Ctrl Pts',(-72.486130774036,9.02060243584483,1.02407232192719));
#41998=CARTESIAN_POINT('Ctrl Pts',(-72.4814597395665,9.0467585181321,0.919658573672963));
#41999=CARTESIAN_POINT('Ctrl Pts',(-72.4717982353608,9.10540038958677,0.7018507216913));
#42000=CARTESIAN_POINT('Ctrl Pts',(-72.4561006574169,9.22010108007979,0.317554629446909));
#42001=CARTESIAN_POINT('Ctrl Pts',(-72.434475200519,9.41780924635723,-0.250230368461771));
#42002=CARTESIAN_POINT('Ctrl Pts',(-72.4071883371743,9.69723158663515,-0.954375802733552));
#42003=CARTESIAN_POINT('Ctrl Pts',(-72.3679637323457,10.1098687883021,-1.92235452420412));
#42004=CARTESIAN_POINT('Ctrl Pts',(-72.315204166524,10.6685800030012,-3.18449761246109));
#42005=CARTESIAN_POINT('Ctrl Pts',(-72.2846125510446,11.095248182418,-4.26272411289597));
#42006=CARTESIAN_POINT('Ctrl Pts',(-72.277107189919,11.3322228678791,-4.96422958465152));
#42007=CARTESIAN_POINT('Ctrl Pts',(-72.2820261073132,11.4180006409522,-5.20171825302269));
#42008=CARTESIAN_POINT('Ctrl Pts',(-72.2959241019649,11.5997573778334,-5.70456172189619));
#42009=CARTESIAN_POINT('Ctrl Pts',(-72.3402000381889,11.9221019350025,-6.58073860490952));
#42010=CARTESIAN_POINT('Ctrl Pts',(-72.4485572929506,12.3824063008201,-7.87143171517512));
#42011=CARTESIAN_POINT('Ctrl Pts',(-72.5868739232216,12.7734181938476,-9.21275087736498));
#42012=CARTESIAN_POINT('Ctrl Pts',(-72.6695584917179,12.9827799224197,-10.180743840257));
#42013=CARTESIAN_POINT('Ctrl Pts',(-72.7080669955866,13.0813270808735,-10.7403067660567));
#42014=CARTESIAN_POINT('Ctrl Pts',(-72.7236469770478,13.1231949475135,-11.022237072098));
#42015=CARTESIAN_POINT('Ctrl Pts',(-72.7337116967939,13.1518582962864,-11.2354778521101));
#42016=CARTESIAN_POINT('Ctrl Pts',(-72.7400437346278,13.1708727140572,-11.3844506421277));
#42017=CARTESIAN_POINT('Ctrl Pts',(-72.75183445656,13.203182773435,-11.6768142474498));
#42018=CARTESIAN_POINT('Ctrl Pts',(-72.7698806280746,13.2475047047871,-12.1844701611177));
#42019=CARTESIAN_POINT('Ctrl Pts',(-72.7963087796921,13.2920790566331,-13.175224571561));
#42020=CARTESIAN_POINT('Ctrl Pts',(-72.810913539449,13.266201707407,-14.5238487361184));
#42021=CARTESIAN_POINT('Ctrl Pts',(-72.8100289523327,13.2060455556474,-15.6607798739506));
#42022=CARTESIAN_POINT('Ctrl Pts',(-72.8095164431849,13.1755895645277,-16.3891086797765));
#42023=CARTESIAN_POINT('Ctrl Pts',(-72.8096395484204,13.1592459050039,-16.8669798526424));
#42024=CARTESIAN_POINT('Ctrl Pts',(-72.8107379701226,13.1531058507421,-17.2167843215973));
#42025=CARTESIAN_POINT('Ctrl Pts',(-72.8127847793528,13.1530562057521,-17.5037849767314));
#42026=CARTESIAN_POINT('Ctrl Pts',(-72.8135450880309,13.1529895968429,-17.631465345179));
#42027=CARTESIAN_POINT('Ctrl Pts',(-72.8148441009318,13.1528746224633,-17.8787508000146));
#42028=CARTESIAN_POINT('Ctrl Pts',(-72.815834791024,13.1527349638102,-18.1292304775296));
#42029=CARTESIAN_POINT('Ctrl Pts',(-72.8165477639545,13.152592856749,-18.3782516548426));
#42030=CARTESIAN_POINT('Ctrl Pts',(-72.8168850950152,13.1524983325586,-18.5343165379471));
#42031=CARTESIAN_POINT('Ctrl Pts',(-72.8170938851606,13.1524214947919,-18.6590680081469));
#42032=CARTESIAN_POINT('Ctrl Pts',(-72.8172210419957,13.1523626742158,-18.7526857093762));
#42033=CARTESIAN_POINT('Ctrl Pts',(-72.8173033240809,13.1523128478981,-18.8307023222607));
#42034=CARTESIAN_POINT('Ctrl Pts',(-72.8173554323772,13.1522726266496,-18.8931289934987));
#42035=CARTESIAN_POINT('Ctrl Pts',(-72.8177222997263,13.151927576941,-19.4238049830459));
#42036=CARTESIAN_POINT('Ctrl Pts',(-72.8160783882301,13.1511531583128,-20.4402734819812));
#42037=CARTESIAN_POINT('Ctrl Pts',(-72.8111063553451,13.1500545858526,-21.9467249018876));
#42038=CARTESIAN_POINT('Ctrl Pts',(-72.8089203623372,13.1494766711097,-22.9551277264119));
#42039=CARTESIAN_POINT('Ctrl Pts',(-72.8087826744896,13.1492380882382,-23.5849128827914));
#42040=CARTESIAN_POINT('Ctrl Pts',(-72.8087463021177,13.1491493109577,-23.8341081872102));
#42041=CARTESIAN_POINT('Ctrl Pts',(-72.8087378441687,13.148986603098,-24.333334836021));
#42042=CARTESIAN_POINT('Ctrl Pts',(-72.8088675228599,13.1487395044348,-25.2087791315747));
#42043=CARTESIAN_POINT('Ctrl Pts',(-72.809320336019,13.1484986769883,-26.4634752931833));
#42044=CARTESIAN_POINT('Ctrl Pts',(-72.8098331928483,13.1483899012864,-27.9716152992162));
#42045=CARTESIAN_POINT('Ctrl Pts',(-72.8098480232188,13.1484405227099,-28.976217642425));
#42046=CARTESIAN_POINT('Ctrl Pts',(-72.8096797178121,13.1485023055856,-29.5403032171419));
#42047=CARTESIAN_POINT('Ctrl Pts',(-72.8096343913625,13.1485177135259,-29.6656190121026));
#42048=CARTESIAN_POINT('Ctrl Pts',(-72.8095143066656,13.1485545150383,-29.9163326943316));
#42049=CARTESIAN_POINT('Ctrl Pts',(-72.8092326749967,13.1486349098195,-30.3552337608238));
#42050=CARTESIAN_POINT('Ctrl Pts',(-72.8084334077922,13.1488518912644,-31.2335434893697));
#42051=CARTESIAN_POINT('Ctrl Pts',(-72.8068941888047,13.1492995404523,-32.489001190465));
#42052=CARTESIAN_POINT('Ctrl Pts',(-72.8055717125501,13.1498467714524,-33.7435017093954));
#42053=CARTESIAN_POINT('Ctrl Pts',(-72.8050922656081,13.1502919622503,-34.7453540357136));
#42054=CARTESIAN_POINT('Ctrl Pts',(-72.8051181249078,13.1505133837545,-35.2455261813069));
#42055=CARTESIAN_POINT('Ctrl Pts',(-72.8052663797821,13.1506736703081,-35.6212940420671));
#42056=CARTESIAN_POINT('Ctrl Pts',(-72.8054103276837,13.1507642395526,-35.8731501737671));
#42057=CARTESIAN_POINT('Ctrl Pts',(-72.8058573239597,13.1508887209446,-36.3759995572946));
#42058=CARTESIAN_POINT('Ctrl Pts',(-72.8070018602344,13.1510064726944,-37.2544049579662));
#42059=CARTESIAN_POINT('Ctrl Pts',(-72.8103329337767,13.151083984824,-39.0062374472486));
#42060=CARTESIAN_POINT('Ctrl Pts',(-72.8135288102678,13.1519316475286,-40.5062668572796));
#42061=CARTESIAN_POINT('Ctrl Pts',(-72.8147940400713,13.1541324879213,-41.7607748435403));
#42062=CARTESIAN_POINT('Ctrl Pts',(-72.8150508433956,13.1543051922145,-42.139293505977));
#42063=CARTESIAN_POINT('Ctrl Pts',(-72.8152250149216,13.1539653770489,-42.6416139194372));
#42064=CARTESIAN_POINT('Ctrl Pts',(-72.8153098594775,13.1533881732182,-43.1441664804877));
#42065=CARTESIAN_POINT('Ctrl Pts',(-72.8152935731392,13.1524735165275,-43.7714412043856));
#42066=CARTESIAN_POINT('Ctrl Pts',(-72.8152214340072,13.1518824373665,-44.5226834273021));
#42067=CARTESIAN_POINT('Ctrl Pts',(-72.8152377100189,13.1524849569531,-45.146881417179));
#42068=CARTESIAN_POINT('Ctrl Pts',(-72.8153700975781,13.1540170297017,-45.6449400484013));
#42069=CARTESIAN_POINT('Ctrl Pts',(-72.8155469327632,13.1557937148195,-46.0177382696206));
#42070=CARTESIAN_POINT('Ctrl Pts',(-72.8158196149017,13.1582970756863,-46.3897570995508));
#42071=CARTESIAN_POINT('Ctrl Pts',(-72.8163359950318,13.1627306891508,-46.8845758998427));
#42072=CARTESIAN_POINT('Ctrl Pts',(-72.8169213641905,13.1674489540909,-47.2544170165257));
#42073=CARTESIAN_POINT('Ctrl Pts',(-72.8176800146892,13.1732856641719,-47.6236613330653));
#42074=CARTESIAN_POINT('Ctrl Pts',(-72.8182543664395,13.1783499070941,-47.8580189203204));
#42075=CARTESIAN_POINT('Ctrl Pts',(-72.8195030698015,13.1933212767559,-48.3396013453518));
#42076=CARTESIAN_POINT('Ctrl Pts',(-72.8219596249252,13.229709474452,-49.1908719162654));
#42077=CARTESIAN_POINT('Ctrl Pts',(-72.8259700723709,13.2986915340731,-50.4452830186504));
#42078=CARTESIAN_POINT('Ctrl Pts',(-72.8314710092657,13.3644612971796,-52.0051294364399));
#42079=CARTESIAN_POINT('Ctrl Pts',(-72.8359995992376,13.364139636692,-53.0827593739283));
#42080=CARTESIAN_POINT('Ctrl Pts',(-72.8394107859471,13.3385396684649,-53.7703518384481));
#42081=CARTESIAN_POINT('Ctrl Pts',(-72.8411415506986,13.3216111243518,-54.0759351268447));
#42082=CARTESIAN_POINT('Ctrl Pts',(-72.8450429256167,13.2706795792392,-54.6545057657787));
#42083=CARTESIAN_POINT('Ctrl Pts',(-72.852555674139,13.1463416430414,-55.6367389748052));
#42084=CARTESIAN_POINT('Ctrl Pts',(-72.8673335059477,12.8281990268769,-57.4449208146386));
#42085=CARTESIAN_POINT('Ctrl Pts',(-72.8716432703236,12.6650429159702,-58.7322956460207));
#42086=CARTESIAN_POINT('Ctrl Pts',(-72.8780587972058,12.7119721350998,-59.4966749041411));
#42087=CARTESIAN_POINT('Ctrl Pts',(-72.8786824357828,12.719550818378,-59.6099750270973));
#42088=CARTESIAN_POINT('Ctrl Pts',(-72.8800079592648,12.7371757831492,-59.8260300265551));
#42089=CARTESIAN_POINT('Ctrl Pts',(-72.8822536109264,12.7763270405229,-60.2119744961277));
#42090=CARTESIAN_POINT('Ctrl Pts',(-72.8866228266663,12.8853804043739,-60.9876644881528));
#42091=CARTESIAN_POINT('Ctrl Pts',(-72.8911029626343,13.0762882899736,-61.8928156844469));
#42092=CARTESIAN_POINT('Ctrl Pts',(-72.8950199421075,13.3224683876046,-62.8074470955451));
#42093=CARTESIAN_POINT('Ctrl Pts',(-72.8970393317336,13.4793462452144,-63.3250036462584));
#42094=CARTESIAN_POINT('Ctrl Pts',(-72.8983224238168,13.5906149021888,-63.6706953025752));
#42095=CARTESIAN_POINT('Ctrl Pts',(-72.8991621720125,13.6665083868823,-63.9013479527401));
#42096=CARTESIAN_POINT('Ctrl Pts',(-72.8999848651695,13.7448392040268,-64.1320994034226));
#42097=CARTESIAN_POINT('Ctrl Pts',(-72.9006885231233,13.8153646331157,-64.3341578281979));
#42098=CARTESIAN_POINT('Ctrl Pts',(-72.9010868611603,13.8562038708251,-64.4496418724454));
#42099=CARTESIAN_POINT('Ctrl Pts',(-72.901682426375,13.9179777271408,-64.6228579385507));
#42100=CARTESIAN_POINT('Ctrl Pts',(-72.902170464986,13.9705357796231,-64.7672556263047));
#42101=CARTESIAN_POINT('Ctrl Pts',(-72.9030076305139,14.0585824816158,-65.0056661064065));
#42102=CARTESIAN_POINT('Ctrl Pts',(-72.9055969738179,14.1414324975294,-65.2185926643699));
#42103=CARTESIAN_POINT('Ctrl Pts',(-72.9095482917182,14.3307137143814,-65.6685970674762));
#42104=CARTESIAN_POINT('Ctrl Pts',(-72.9161514089217,14.6992194686521,-66.4581056413799));
#42105=CARTESIAN_POINT('Ctrl Pts',(-72.9244946737035,15.579356371815,-68.097078216371));
#42106=CARTESIAN_POINT('Ctrl Pts',(-72.9223549274365,16.4774628368235,-69.5915927640089));
#42107=CARTESIAN_POINT('Ctrl Pts',(-72.9169103750747,17.1089503039591,-70.7930434498888));
#42108=CARTESIAN_POINT('Ctrl Pts',(-72.9173870473759,17.237835907039,-71.0375968471999));
#42109=CARTESIAN_POINT('Ctrl Pts',(-72.9173509939031,17.5031841378782,-71.5401125637486));
#42110=CARTESIAN_POINT('Ctrl Pts',(-72.917672410201,17.8331812855221,-72.1628427052565));
#42111=CARTESIAN_POINT('Ctrl Pts',(-72.9177872026895,18.2322311103456,-72.9135276335728));
#42112=CARTESIAN_POINT('Ctrl Pts',(-72.9180413274558,19.0317354550891,-74.4140149336155));
#42113=CARTESIAN_POINT('Ctrl Pts',(-72.9180063208637,19.70162313999,-75.6668545626666));
#42114=CARTESIAN_POINT('Ctrl Pts',(-72.917740703414,20.6733372941337,-77.4942447409276));
#42115=CARTESIAN_POINT('Ctrl Pts',(-72.917856315526,21.1090373153559,-78.3135397879966));
#42116=CARTESIAN_POINT('Ctrl Pts',(-72.9178563155317,21.5455589027462,-79.1345174901012));
#42117=CARTESIAN_POINT('Ctrl Pts',(-70.0797300922936,7.87083409769097,24.8336095804827));
#42118=CARTESIAN_POINT('Ctrl Pts',(-70.0799646667605,7.87093845762237,24.7848236666139));
#42119=CARTESIAN_POINT('Ctrl Pts',(-70.0802106206726,7.87104776413738,24.7360406870304));
#42120=CARTESIAN_POINT('Ctrl Pts',(-70.0831162832123,7.87233944489162,24.1865206508717));
#42121=CARTESIAN_POINT('Ctrl Pts',(-70.0856956491753,7.87502546693778,23.1838837033978));
#42122=CARTESIAN_POINT('Ctrl Pts',(-70.0918978853719,7.88239184231991,21.1771390793342));
#42123=CARTESIAN_POINT('Ctrl Pts',(-70.1112127705556,7.89097251402827,19.672722175038));
#42124=CARTESIAN_POINT('Ctrl Pts',(-70.1504440078457,7.90066506163222,18.4211235716628));
#42125=CARTESIAN_POINT('Ctrl Pts',(-70.1697003096978,7.90590967768963,17.9236165225639));
#42126=CARTESIAN_POINT('Ctrl Pts',(-70.2188717945085,7.92010557264673,16.9233332269309));
#42127=CARTESIAN_POINT('Ctrl Pts',(-70.3245072267018,7.95020258260261,15.1692690929129));
#42128=CARTESIAN_POINT('Ctrl Pts',(-70.4196449338281,7.96904497304481,13.6495592012489));
#42129=CARTESIAN_POINT('Ctrl Pts',(-70.4695606398365,7.96298537878605,12.3710022159992));
#42130=CARTESIAN_POINT('Ctrl Pts',(-70.490216149405,7.95733326394079,11.8533220878073));
#42131=CARTESIAN_POINT('Ctrl Pts',(-70.53210178241,7.93718721593872,10.8325501005278));
#42132=CARTESIAN_POINT('Ctrl Pts',(-70.5812230449941,7.90165812831565,9.57061253256148));
#42133=CARTESIAN_POINT('Ctrl Pts',(-70.6213518385245,7.86263523571733,8.08298723669083));
#42134=CARTESIAN_POINT('Ctrl Pts',(-70.6263413494506,7.85051196817903,7.10760374122982));
#42135=CARTESIAN_POINT('Ctrl Pts',(-70.6199133696501,7.85046321124629,6.50252850665239));
#42136=CARTESIAN_POINT('Ctrl Pts',(-70.6171502217435,7.84849425242508,6.22778268160475));
#42137=CARTESIAN_POINT('Ctrl Pts',(-70.6099046660388,7.83921247672353,5.7061450396773));
#42138=CARTESIAN_POINT('Ctrl Pts',(-70.5921107527037,7.81304674889243,4.80420574951403));
#42139=CARTESIAN_POINT('Ctrl Pts',(-70.5320835521922,7.75566715378061,3.09229665864847));
#42140=CARTESIAN_POINT('Ctrl Pts',(-70.425694019437,7.78731605055769,1.78224082503292));
#42141=CARTESIAN_POINT('Ctrl Pts',(-70.3395780432339,7.91047947804615,0.920418189731267));
#42142=CARTESIAN_POINT('Ctrl Pts',(-70.3281862757546,7.9265152414774,0.81546603095744));
#42143=CARTESIAN_POINT('Ctrl Pts',(-70.3034672863993,7.96089874100147,0.604597509478728));
#42144=CARTESIAN_POINT('Ctrl Pts',(-70.254815071026,8.02834317441377,0.229801605440034));
#42145=CARTESIAN_POINT('Ctrl Pts',(-70.1738770417327,8.14462932123709,-0.32043261565958));
#42146=CARTESIAN_POINT('Ctrl Pts',(-70.0675190259357,8.31623264682582,-1.005864139264));
#42147=CARTESIAN_POINT('Ctrl Pts',(-69.9234752204677,8.58551139528495,-1.94994725910126));
#42148=CARTESIAN_POINT('Ctrl Pts',(-69.7537363853315,8.99303427045749,-3.18139531531514));
#42149=CARTESIAN_POINT('Ctrl Pts',(-69.6555765300377,9.37167205002254,-4.2050076167861));
#42150=CARTESIAN_POINT('Ctrl Pts',(-69.6175750115734,9.61674332323064,-4.8518866619604));
#42151=CARTESIAN_POINT('Ctrl Pts',(-69.614996384641,9.70391730270588,-5.05492488932629));
#42152=CARTESIAN_POINT('Ctrl Pts',(-69.6082938426236,9.91073799703179,-5.50489344233537));
#42153=CARTESIAN_POINT('Ctrl Pts',(-69.6106257681355,10.318486485829,-6.30250377295544));
#42154=CARTESIAN_POINT('Ctrl Pts',(-69.634414507676,11.0005103287512,-7.52679652658411));
#42155=CARTESIAN_POINT('Ctrl Pts',(-69.6766863625143,11.6866796254722,-8.85991637902529));
#42156=CARTESIAN_POINT('Ctrl Pts',(-69.7071716493671,12.0968998297548,-9.87706752674961));
#42157=CARTESIAN_POINT('Ctrl Pts',(-69.722762042575,12.2973318855679,-10.4847897843783));
#42158=CARTESIAN_POINT('Ctrl Pts',(-69.7294646151064,12.3838364503264,-10.7982059734627));
#42159=CARTESIAN_POINT('Ctrl Pts',(-69.7339098166316,12.4427321913131,-11.0376746143682));
#42160=CARTESIAN_POINT('Ctrl Pts',(-69.7373366428525,12.4792362201273,-11.191032336319));
#42161=CARTESIAN_POINT('Ctrl Pts',(-69.7451836481932,12.5453552435596,-11.4998982538861));
#42162=CARTESIAN_POINT('Ctrl Pts',(-69.7614512775317,12.641968099703,-12.0328224750319));
#42163=CARTESIAN_POINT('Ctrl Pts',(-69.8018292172795,12.767713728289,-13.0749517757829));
#42164=CARTESIAN_POINT('Ctrl Pts',(-69.8692804996059,12.8027391307006,-14.4766171192183));
#42165=CARTESIAN_POINT('Ctrl Pts',(-69.9236037530677,12.7681274810262,-15.6326832106271));
#42166=CARTESIAN_POINT('Ctrl Pts',(-69.9528293609611,12.7525926142196,-16.3621025680776));
#42167=CARTESIAN_POINT('Ctrl Pts',(-69.9702257048737,12.7458542468064,-16.8377075153323));
#42168=CARTESIAN_POINT('Ctrl Pts',(-69.9806833299977,12.7469682670916,-17.1822224171611));
#42169=CARTESIAN_POINT('Ctrl Pts',(-69.9876533243847,12.7532730120962,-17.4633727546574));
#42170=CARTESIAN_POINT('Ctrl Pts',(-69.9901878041358,12.7559302447579,-17.5957832338958));
#42171=CARTESIAN_POINT('Ctrl Pts',(-69.9946058127628,12.7604059255415,-17.8480854166894));
#42172=CARTESIAN_POINT('Ctrl Pts',(-69.9980492085591,12.7640263564037,-18.1046796823426));
#42173=CARTESIAN_POINT('Ctrl Pts',(-70.0006278395402,12.7667954845501,-18.3585667860185));
#42174=CARTESIAN_POINT('Ctrl Pts',(-70.0018985491503,12.7682120625135,-18.5176708497133));
#42175=CARTESIAN_POINT('Ctrl Pts',(-70.0027234975775,12.7691626491919,-18.6446737562696));
#42176=CARTESIAN_POINT('Ctrl Pts',(-70.0032495291657,12.7697890061634,-18.7399419573746));
#42177=CARTESIAN_POINT('Ctrl Pts',(-70.0036134451858,12.7702402913664,-18.8192804051432));
#42178=CARTESIAN_POINT('Ctrl Pts',(-70.0038613073673,12.7705610527564,-18.8827386925231));
#42179=CARTESIAN_POINT('Ctrl Pts',(-70.0057291557627,12.7730591465881,-19.4220221149389));
#42180=CARTESIAN_POINT('Ctrl Pts',(-70.0018986583592,12.770776648951,-20.4500653832152));
#42181=CARTESIAN_POINT('Ctrl Pts',(-69.9879997992902,12.7594571042562,-21.9592664440623));
#42182=CARTESIAN_POINT('Ctrl Pts',(-69.981963518983,12.7544602708346,-22.960197688122));
#42183=CARTESIAN_POINT('Ctrl Pts',(-69.9818921980815,12.7546653219054,-23.5825699741119));
#42184=CARTESIAN_POINT('Ctrl Pts',(-69.981894991941,12.7547519566139,-23.8326565024476));
#42185=CARTESIAN_POINT('Ctrl Pts',(-69.9820122597349,12.7549340746958,-24.3315249118144));
#42186=CARTESIAN_POINT('Ctrl Pts',(-69.9824658818906,12.7552624643131,-25.2074809115996));
#42187=CARTESIAN_POINT('Ctrl Pts',(-69.9835672729193,12.7557137255404,-26.4623716600327));
#42188=CARTESIAN_POINT('Ctrl Pts',(-69.9847896256528,12.7560536229567,-27.971270691958));
#42189=CARTESIAN_POINT('Ctrl Pts',(-69.9849923393715,12.7560277680565,-28.9763997254712));
#42190=CARTESIAN_POINT('Ctrl Pts',(-69.9847790976071,12.7559071214205,-29.5408320492003));
#42191=CARTESIAN_POINT('Ctrl Pts',(-69.9847190327587,12.7558758616894,-29.6662774310689));
#42192=CARTESIAN_POINT('Ctrl Pts',(-69.984552223832,12.7557959781981,-29.9172053601299));
#42193=CARTESIAN_POINT('Ctrl Pts',(-69.9841465990849,12.755614662297,-30.3564674006169));
#42194=CARTESIAN_POINT('Ctrl Pts',(-69.9829532444279,12.755104651033,-31.2353562879841));
#42195=CARTESIAN_POINT('Ctrl Pts',(-69.9805687035159,12.7540941885417,-32.4912820588143));
#42196=CARTESIAN_POINT('Ctrl Pts',(-69.9783817358907,12.753042894257,-33.7457473070251));
#42197=CARTESIAN_POINT('Ctrl Pts',(-69.9774127622085,12.7523768445192,-34.7472551726568));
#42198=CARTESIAN_POINT('Ctrl Pts',(-69.9772980945349,12.7521433192641,-35.247158075241));
#42199=CARTESIAN_POINT('Ctrl Pts',(-69.9773927097792,12.7520138717686,-35.622686066461));
#42200=CARTESIAN_POINT('Ctrl Pts',(-69.9775133714002,12.7519146402004,-35.8745548934899));
#42201=CARTESIAN_POINT('Ctrl Pts',(-69.9779586307213,12.7516764180863,-36.3773291823379));
#42202=CARTESIAN_POINT('Ctrl Pts',(-69.9792060003252,12.7512071226226,-37.2556581271203));
#42203=CARTESIAN_POINT('Ctrl Pts',(-69.9830484660371,12.7502671745843,-39.0072803971456));
#42204=CARTESIAN_POINT('Ctrl Pts',(-69.9868358117171,12.7504863846341,-40.5071496610249));
#42205=CARTESIAN_POINT('Ctrl Pts',(-69.9882537365034,12.7522335185554,-41.7614999300598));
#42206=CARTESIAN_POINT('Ctrl Pts',(-69.988523924384,12.7522689106951,-42.1399969035111));
#42207=CARTESIAN_POINT('Ctrl Pts',(-69.9886722200598,12.7517528417585,-42.6422651008279));
#42208=CARTESIAN_POINT('Ctrl Pts',(-69.9887094014331,12.7510060141183,-43.1447647900567));
#42209=CARTESIAN_POINT('Ctrl Pts',(-69.9886054825973,12.7498953589051,-43.7719630105579));
#42210=CARTESIAN_POINT('Ctrl Pts',(-69.988425173086,12.749106300016,-44.5231007995684));
#42211=CARTESIAN_POINT('Ctrl Pts',(-69.988383644029,12.7495845265692,-45.1472004354468));
#42212=CARTESIAN_POINT('Ctrl Pts',(-69.9885096857935,12.7510464325718,-45.6451717793566));
#42213=CARTESIAN_POINT('Ctrl Pts',(-69.9887071266115,12.7527869079614,-46.017901097045));
#42214=CARTESIAN_POINT('Ctrl Pts',(-69.9890309693273,12.7552717791395,-46.3898474617455));
#42215=CARTESIAN_POINT('Ctrl Pts',(-69.9896632214316,12.7597063096198,-46.8845642943284));
#42216=CARTESIAN_POINT('Ctrl Pts',(-69.9903971337144,12.7644558765816,-47.254324379301));
#42217=CARTESIAN_POINT('Ctrl Pts',(-69.9913561982648,12.7703474655071,-47.6234819913124));
#42218=CARTESIAN_POINT('Ctrl Pts',(-69.9920745336061,12.7754555967541,-47.8577571348398));
#42219=CARTESIAN_POINT('Ctrl Pts',(-69.9936461974301,12.7905471997396,-48.3392030878483));
#42220=CARTESIAN_POINT('Ctrl Pts',(-69.9967581941422,12.8272250940851,-49.1902610781344));
#42221=CARTESIAN_POINT('Ctrl Pts',(-70.0019464278965,12.8968161905817,-50.4444677902403));
#42222=CARTESIAN_POINT('Ctrl Pts',(-70.0092115061526,12.9635283622005,-52.0042169411895));
#42223=CARTESIAN_POINT('Ctrl Pts',(-70.0151328854528,12.9638783345927,-53.0818951197487));
#42224=CARTESIAN_POINT('Ctrl Pts',(-70.0194805733487,12.9386820326978,-53.7695514912596));
#42225=CARTESIAN_POINT('Ctrl Pts',(-70.021616000932,12.9219428845158,-54.0750564285113));
#42226=CARTESIAN_POINT('Ctrl Pts',(-70.026421203681,12.8714101731903,-54.6535562856163));
#42227=CARTESIAN_POINT('Ctrl Pts',(-70.0357215940866,12.7478235203842,-55.6356921285918));
#42228=CARTESIAN_POINT('Ctrl Pts',(-70.0545706652888,12.4312446036475,-57.443882033324));
#42229=CARTESIAN_POINT('Ctrl Pts',(-70.0621906425967,12.2690752169479,-58.7315035512416));
#42230=CARTESIAN_POINT('Ctrl Pts',(-70.0698682848343,12.3163671846014,-59.4962771807332));
#42231=CARTESIAN_POINT('Ctrl Pts',(-70.0706383028307,12.3239921932981,-59.609619365006));
#42232=CARTESIAN_POINT('Ctrl Pts',(-70.0722338644273,12.3416983613519,-59.8257567538662));
#42233=CARTESIAN_POINT('Ctrl Pts',(-70.0748935291213,12.3809699258908,-60.2118321945912));
#42234=CARTESIAN_POINT('Ctrl Pts',(-70.0798793331697,12.490177829677,-60.9877372918059));
#42235=CARTESIAN_POINT('Ctrl Pts',(-70.084679822235,12.6810981003491,-61.8930259126653));
#42236=CARTESIAN_POINT('Ctrl Pts',(-70.0887291925924,12.9272005920432,-62.8076987730538));
#42237=CARTESIAN_POINT('Ctrl Pts',(-70.0907884488415,13.0840177628279,-63.3252448496941));
#42238=CARTESIAN_POINT('Ctrl Pts',(-70.0920985582379,13.1952454731271,-63.6709159868783));
#42239=CARTESIAN_POINT('Ctrl Pts',(-70.0929574092067,13.2711121021537,-63.9015513719062));
#42240=CARTESIAN_POINT('Ctrl Pts',(-70.0938023132969,13.3494172624026,-64.1322802790929));
#42241=CARTESIAN_POINT('Ctrl Pts',(-70.094530689255,13.4199226892588,-64.3343142963286));
#42242=CARTESIAN_POINT('Ctrl Pts',(-70.0949450256968,13.46075135641,-64.4497830538115));
#42243=CARTESIAN_POINT('Ctrl Pts',(-70.0955666466438,13.5225103365915,-64.6229748956723));
#42244=CARTESIAN_POINT('Ctrl Pts',(-70.0960810583999,13.5750580934916,-64.7673495223908));
#42245=CARTESIAN_POINT('Ctrl Pts',(-70.0969701168715,13.6630921096615,-65.0057190804797));
#42246=CARTESIAN_POINT('Ctrl Pts',(-70.0996087278747,13.7459487610903,-65.2186539217629));
#42247=CARTESIAN_POINT('Ctrl Pts',(-70.1036343446273,13.9352298848311,-65.6686469867403));
#42248=CARTESIAN_POINT('Ctrl Pts',(-70.1103127543902,14.3037368141752,-66.4581519152683));
#42249=CARTESIAN_POINT('Ctrl Pts',(-70.1186303204434,15.1838581762324,-68.0971112119206));
#42250=CARTESIAN_POINT('Ctrl Pts',(-70.1163303848665,16.0819463876766,-69.5916304392682));
#42251=CARTESIAN_POINT('Ctrl Pts',(-70.1108693306998,16.7134282989604,-70.7930862089204));
#42252=CARTESIAN_POINT('Ctrl Pts',(-70.1113470826655,16.8423130561934,-71.0376385468314));
#42253=CARTESIAN_POINT('Ctrl Pts',(-70.1113105709919,17.1076598182307,-71.5401534806291));
#42254=CARTESIAN_POINT('Ctrl Pts',(-70.1116326619803,17.4376558910464,-72.1628824859081));
#42255=CARTESIAN_POINT('Ctrl Pts',(-70.111747802197,17.8367052278182,-72.9135665131352));
#42256=CARTESIAN_POINT('Ctrl Pts',(-70.1120030741606,18.6362099071052,-74.4140525108728));
#42257=CARTESIAN_POINT('Ctrl Pts',(-70.1119687058294,19.3060997676304,-75.6668931110029));
#42258=CARTESIAN_POINT('Ctrl Pts',(-70.1117021926187,20.2778148148096,-77.4942856965309));
#42259=CARTESIAN_POINT('Ctrl Pts',(-70.1118181513274,20.7135146017487,-78.3135802751711));
#42260=CARTESIAN_POINT('Ctrl Pts',(-70.1118181513289,21.1500361891381,-79.1345579772626));
#42261=CARTESIAN_POINT('Ctrl Pts',(-67.2754322320213,7.4757630221787,24.8321255810971));
#42262=CARTESIAN_POINT('Ctrl Pts',(-67.2755705809386,7.47581763243593,24.7832923099026));
#42263=CARTESIAN_POINT('Ctrl Pts',(-67.2757157318436,7.47587475234481,24.7344612301898));
#42264=CARTESIAN_POINT('Ctrl Pts',(-67.2774319088059,7.47655431889977,24.1843846336179));
#42265=CARTESIAN_POINT('Ctrl Pts',(-67.2774494651673,7.47755687413155,23.1805744464059));
#42266=CARTESIAN_POINT('Ctrl Pts',(-67.2766235035466,7.48011201430047,21.1730765472028));
#42267=CARTESIAN_POINT('Ctrl Pts',(-67.2881197826209,7.4845991280751,19.6694790344265));
#42268=CARTESIAN_POINT('Ctrl Pts',(-67.3189731485589,7.49180979772324,18.4189751922483));
#42269=CARTESIAN_POINT('Ctrl Pts',(-67.3332328314049,7.4956322349772,17.9199743333444));
#42270=CARTESIAN_POINT('Ctrl Pts',(-67.3681259975055,7.50594132134161,16.9185156642757));
#42271=CARTESIAN_POINT('Ctrl Pts',(-67.4432905113739,7.52812635253163,15.1635432795567));
#42272=CARTESIAN_POINT('Ctrl Pts',(-67.522772202602,7.54446416298015,13.648896070725));
#42273=CARTESIAN_POINT('Ctrl Pts',(-67.5872153009134,7.54582825987786,12.3786335598512));
#42274=CARTESIAN_POINT('Ctrl Pts',(-67.6154204776456,7.54540033180308,11.8709509904796));
#42275=CARTESIAN_POINT('Ctrl Pts',(-67.6787468185927,7.5412077711249,10.8599911652357));
#42276=CARTESIAN_POINT('Ctrl Pts',(-67.7651833140421,7.53071460451453,9.60191254014628));
#42277=CARTESIAN_POINT('Ctrl Pts',(-67.8630876090932,7.51397052777016,8.10026383947153));
#42278=CARTESIAN_POINT('Ctrl Pts',(-67.9126109843987,7.50342730317955,7.10301976831543));
#42279=CARTESIAN_POINT('Ctrl Pts',(-67.9350070138697,7.4984053138877,6.48056930618348));
#42280=CARTESIAN_POINT('Ctrl Pts',(-67.9444957931639,7.49500156432598,6.21395100057163));
#42281=CARTESIAN_POINT('Ctrl Pts',(-67.9652928589601,7.48429166055158,5.69653581018919));
#42282=CARTESIAN_POINT('Ctrl Pts',(-68.0044466838936,7.45799259920056,4.79761339447914));
#42283=CARTESIAN_POINT('Ctrl Pts',(-68.0793245519533,7.39327191476882,3.05333199869326));
#42284=CARTESIAN_POINT('Ctrl Pts',(-68.0845307050997,7.39164300891083,1.64861862663291));
#42285=CARTESIAN_POINT('Ctrl Pts',(-68.0031627403797,7.4622667172992,0.710098961592749));
#42286=CARTESIAN_POINT('Ctrl Pts',(-67.9923709016977,7.47255008470439,0.579449910835283));
#42287=CARTESIAN_POINT('Ctrl Pts',(-67.9672546452685,7.49147815214768,0.331053566575222));
#42288=CARTESIAN_POINT('Ctrl Pts',(-67.9144380698456,7.5238364670556,-0.103990457920467));
#42289=CARTESIAN_POINT('Ctrl Pts',(-67.8174273409239,7.56603084566458,-0.707454744008557));
#42290=CARTESIAN_POINT('Ctrl Pts',(-67.6796650820582,7.61274839096469,-1.41320481599388));
#42291=CARTESIAN_POINT('Ctrl Pts',(-67.4859137058936,7.67763165669604,-2.33059832461395));
#42292=CARTESIAN_POINT('Ctrl Pts',(-67.2607353653355,7.78643519277926,-3.44759918903815));
#42293=CARTESIAN_POINT('Ctrl Pts',(-67.1478083966393,7.97895549501847,-4.3222442690895));
#42294=CARTESIAN_POINT('Ctrl Pts',(-67.1058926808869,8.15325576339432,-4.85873369997395));
#42295=CARTESIAN_POINT('Ctrl Pts',(-67.0971683145861,8.21760514823808,-5.02933657075882));
#42296=CARTESIAN_POINT('Ctrl Pts',(-67.0760798163985,8.39201841664085,-5.42526239502765));
#42297=CARTESIAN_POINT('Ctrl Pts',(-67.03904188196,8.78206000803595,-6.16219966869188));
#42298=CARTESIAN_POINT('Ctrl Pts',(-66.9674979596952,9.53618905798644,-7.35158730514667));
#42299=CARTESIAN_POINT('Ctrl Pts',(-66.8802894966432,10.372303287372,-8.66590951801085));
#42300=CARTESIAN_POINT('Ctrl Pts',(-66.8243846116526,10.9059313183747,-9.68399100585595));
#42301=CARTESIAN_POINT('Ctrl Pts',(-66.7972919426213,11.1783971007118,-10.3028728735934));
#42302=CARTESIAN_POINT('Ctrl Pts',(-66.7860516655838,11.3002413050387,-10.626878444251));
#42303=CARTESIAN_POINT('Ctrl Pts',(-66.77887046776,11.3847166946218,-10.8762865151733));
#42304=CARTESIAN_POINT('Ctrl Pts',(-66.7772989784454,11.4332747003404,-11.0205302214951));
#42305=CARTESIAN_POINT('Ctrl Pts',(-66.7756940985764,11.5284492720659,-11.320889056081));
#42306=CARTESIAN_POINT('Ctrl Pts',(-66.7809843984739,11.6784361246504,-11.8366659747363));
#42307=CARTESIAN_POINT('Ctrl Pts',(-66.8177655934338,11.924917887323,-12.8582347187859));
#42308=CARTESIAN_POINT('Ctrl Pts',(-66.9274108154291,12.1408200082236,-14.2621470942844));
#42309=CARTESIAN_POINT('Ctrl Pts',(-67.041480430644,12.2352182624232,-15.4502559001017));
#42310=CARTESIAN_POINT('Ctrl Pts',(-67.1033752206594,12.2839359550366,-16.2104420116553));
#42311=CARTESIAN_POINT('Ctrl Pts',(-67.1396331269749,12.3143823159889,-16.7094247054265));
#42312=CARTESIAN_POINT('Ctrl Pts',(-67.1597751406538,12.3367540398636,-17.0744826446256));
#42313=CARTESIAN_POINT('Ctrl Pts',(-67.1710420796526,12.3572346069264,-17.3744609695137));
#42314=CARTESIAN_POINT('Ctrl Pts',(-67.1750081532322,12.3661954177773,-17.5145108019458));
#42315=CARTESIAN_POINT('Ctrl Pts',(-67.1819313592866,12.3810343842226,-17.7811673358964));
#42316=CARTESIAN_POINT('Ctrl Pts',(-67.1872045835245,12.3930034573781,-18.0511067663896));
#42317=CARTESIAN_POINT('Ctrl Pts',(-67.1910471326289,12.4020167829618,-18.3172149975864));
#42318=CARTESIAN_POINT('Ctrl Pts',(-67.1928746823619,12.4065925190783,-18.4835108802885));
#42319=CARTESIAN_POINT('Ctrl Pts',(-67.1940169378708,12.409629318995,-18.6159908563114));
#42320=CARTESIAN_POINT('Ctrl Pts',(-67.1947179035365,12.4116154912796,-18.7152308292935));
#42321=CARTESIAN_POINT('Ctrl Pts',(-67.1951772825936,12.4130321638294,-18.7977648718811));
#42322=CARTESIAN_POINT('Ctrl Pts',(-67.1954721588069,12.4140298350441,-18.8637109791609));
#42323=CARTESIAN_POINT('Ctrl Pts',(-67.1975777453642,12.4217425034244,-19.4237549404876));
#42324=CARTESIAN_POINT('Ctrl Pts',(-67.1891546020952,12.4130338676924,-20.4793867008131));
#42325=CARTESIAN_POINT('Ctrl Pts',(-67.1629544371965,12.3746171685172,-21.9943111510365));
#42326=CARTESIAN_POINT('Ctrl Pts',(-67.1512169371865,12.35790654959,-22.9761797143203));
#42327=CARTESIAN_POINT('Ctrl Pts',(-67.1503428753901,12.3581065561651,-23.5799735642095));
#42328=CARTESIAN_POINT('Ctrl Pts',(-67.1500443571836,12.3582079065643,-23.832139615935));
#42329=CARTESIAN_POINT('Ctrl Pts',(-67.1496270629664,12.3584370651098,-24.3298720223066));
#42330=CARTESIAN_POINT('Ctrl Pts',(-67.1493180411603,12.3589006541,-25.2066041979464));
#42331=CARTESIAN_POINT('Ctrl Pts',(-67.1497943090567,12.359625042183,-26.4611455773589));
#42332=CARTESIAN_POINT('Ctrl Pts',(-67.1509133188839,12.3602460538217,-27.9707230001521));
#42333=CARTESIAN_POINT('Ctrl Pts',(-67.1514200620566,12.3602526285253,-28.9761938345696));
#42334=CARTESIAN_POINT('Ctrl Pts',(-67.1514670086208,12.3600746705999,-29.5408978499594));
#42335=CARTESIAN_POINT('Ctrl Pts',(-67.1514707984293,12.3600288621789,-29.6664071507096));
#42336=CARTESIAN_POINT('Ctrl Pts',(-67.15145485088,12.3599117051442,-29.9174517359273));
#42337=CARTESIAN_POINT('Ctrl Pts',(-67.1513709046654,12.3596452911758,-30.3569094723028));
#42338=CARTESIAN_POINT('Ctrl Pts',(-67.1510286339558,12.3588955981039,-31.2361249633699));
#42339=CARTESIAN_POINT('Ctrl Pts',(-67.1503177795842,12.3574019954836,-32.492341994905));
#42340=CARTESIAN_POINT('Ctrl Pts',(-67.1500578075652,12.3558315772813,-33.7468367107806));
#42341=CARTESIAN_POINT('Ctrl Pts',(-67.1505685996278,12.3548177890257,-34.7481724761365));
#42342=CARTESIAN_POINT('Ctrl Pts',(-67.1511366027792,12.3544470739449,-35.2479443558075));
#42343=CARTESIAN_POINT('Ctrl Pts',(-67.151710177535,12.3542337839783,-35.6233483768898));
#42344=CARTESIAN_POINT('Ctrl Pts',(-67.1521595997931,12.3540805990332,-35.8752264773858));
#42345=CARTESIAN_POINT('Ctrl Pts',(-67.1532881011523,12.3537436882837,-36.37796293713));
#42346=CARTESIAN_POINT('Ctrl Pts',(-67.1557824192001,12.3531236898836,-37.2562620752088));
#42347=CARTESIAN_POINT('Ctrl Pts',(-67.1622143470569,12.3519562497411,-39.0077775913824));
#42348=CARTESIAN_POINT('Ctrl Pts',(-67.1679797364291,12.3520581762157,-40.5075856924395));
#42349=CARTESIAN_POINT('Ctrl Pts',(-67.1704705762212,12.3536956253068,-41.7618662070699));
#42350=CARTESIAN_POINT('Ctrl Pts',(-67.1710199552577,12.3536945457625,-42.1403574085443));
#42351=CARTESIAN_POINT('Ctrl Pts',(-67.1714736601701,12.3531280238148,-42.6426012862483));
#42352=CARTESIAN_POINT('Ctrl Pts',(-67.1717766222623,12.3523303716963,-43.1450763086216));
#42353=CARTESIAN_POINT('Ctrl Pts',(-67.1719403089611,12.35115790606,-43.7722363024753));
#42354=CARTESIAN_POINT('Ctrl Pts',(-67.1720084137478,12.3503043777855,-44.5233188378637));
#42355=CARTESIAN_POINT('Ctrl Pts',(-67.1721388745049,12.3507428083146,-45.147364066605));
#42356=CARTESIAN_POINT('Ctrl Pts',(-67.1723970297961,12.3521845659274,-45.6452843848084));
#42357=CARTESIAN_POINT('Ctrl Pts',(-67.1726945719965,12.3539166793565,-46.0179728583073));
#42358=CARTESIAN_POINT('Ctrl Pts',(-67.1731233944469,12.3564007832012,-46.3898756442327));
#42359=CARTESIAN_POINT('Ctrl Pts',(-67.173907190769,12.3608454915033,-46.8845301952318));
#42360=CARTESIAN_POINT('Ctrl Pts',(-67.1747736668019,12.3656167149972,-47.2542405740443));
#42361=CARTESIAN_POINT('Ctrl Pts',(-67.1758857581577,12.3715408530953,-47.6233441990874));
#42362=CARTESIAN_POINT('Ctrl Pts',(-67.1767001397065,12.376672274449,-47.8575659949926));
#42363=CARTESIAN_POINT('Ctrl Pts',(-67.1784460180514,12.3918218385907,-48.3389264315629));
#42364=CARTESIAN_POINT('Ctrl Pts',(-67.1818261944169,12.4286292243439,-49.1898560942608));
#42365=CARTESIAN_POINT('Ctrl Pts',(-67.1873609124508,12.4984868596341,-50.4439578574161));
#42366=CARTESIAN_POINT('Ctrl Pts',(-67.1951733397397,12.565626926741,-52.0036846004141));
#42367=CARTESIAN_POINT('Ctrl Pts',(-67.2016690783125,12.5663061222207,-53.0814149816948));
#42368=CARTESIAN_POINT('Ctrl Pts',(-67.2064789926283,12.5413177612883,-53.7691211085328));
#42369=CARTESIAN_POINT('Ctrl Pts',(-67.2088116313674,12.5246755553911,-54.0745985103634));
#42370=CARTESIAN_POINT('Ctrl Pts',(-67.2140688628474,12.4743493841427,-54.6530762516019));
#42371=CARTESIAN_POINT('Ctrl Pts',(-67.2242908291814,12.3511593671177,-55.6351736922375));
#42372=CARTESIAN_POINT('Ctrl Pts',(-67.2453866476106,12.0354472455036,-57.4433406611621));
#42373=CARTESIAN_POINT('Ctrl Pts',(-67.2549899284182,11.87386411116,-58.7310581353012));
#42374=CARTESIAN_POINT('Ctrl Pts',(-67.2634764260892,11.9213680452202,-59.4960375627948));
#42375=CARTESIAN_POINT('Ctrl Pts',(-67.2643428975657,11.929020325518,-59.6094025664119));
#42376=CARTESIAN_POINT('Ctrl Pts',(-67.2661229085829,11.9467751815193,-59.8255841341478));
#42377=CARTESIAN_POINT('Ctrl Pts',(-67.2690844957648,11.9861214596594,-60.2117300472603));
#42378=CARTESIAN_POINT('Ctrl Pts',(-67.2745957471064,12.0954359936569,-60.9877494117348));
#42379=CARTESIAN_POINT('Ctrl Pts',(-67.2798403939225,12.2863932650726,-61.8931045719696));
#42380=CARTESIAN_POINT('Ctrl Pts',(-67.2842233506651,12.532479666206,-62.8077863856855));
#42381=CARTESIAN_POINT('Ctrl Pts',(-67.2864382164809,12.6892759716219,-63.3253180861268));
#42382=CARTESIAN_POINT('Ctrl Pts',(-67.2878428582821,12.8004882189023,-63.6709723005203));
#42383=CARTESIAN_POINT('Ctrl Pts',(-67.2887625715289,12.876344402861,-63.9015944753022));
#42384=CARTESIAN_POINT('Ctrl Pts',(-67.2896655043126,12.9546392534038,-64.1323074621358));
#42385=CARTESIAN_POINT('Ctrl Pts',(-67.2904429757562,13.0251364600611,-64.334325166348));
#42386=CARTESIAN_POINT('Ctrl Pts',(-67.2908849974231,13.0659607520918,-64.4497839441229));
#42387=CARTESIAN_POINT('Ctrl Pts',(-67.2915478237582,13.1277135490983,-64.6229601846799));
#42388=CARTESIAN_POINT('Ctrl Pts',(-67.292096048499,13.1802570070354,-64.7673204410586));
#42389=CARTESIAN_POINT('Ctrl Pts',(-67.2930408018807,13.2682857663681,-65.0056649728891));
#42390=CARTESIAN_POINT('Ctrl Pts',(-67.2957192466897,13.3511433890363,-65.2186001383609));
#42391=CARTESIAN_POINT('Ctrl Pts',(-67.2998050326217,13.5404202332849,-65.6685810191878));
#42392=CARTESIAN_POINT('Ctrl Pts',(-67.3065272003076,13.9089172400581,-66.4580761268423));
#42393=CARTESIAN_POINT('Ctrl Pts',(-67.3147653261941,14.7890086193988,-68.0970223218478));
#42394=CARTESIAN_POINT('Ctrl Pts',(-67.3123125064053,15.6870807723725,-69.5915449895342));
#42395=CARTESIAN_POINT('Ctrl Pts',(-67.3068846662169,16.3185728591383,-70.7930072900375));
#42396=CARTESIAN_POINT('Ctrl Pts',(-67.3073607613388,16.4474560716216,-71.0375585891527));
#42397=CARTESIAN_POINT('Ctrl Pts',(-67.307325727314,16.7128021838016,-71.5400729754856));
#42398=CARTESIAN_POINT('Ctrl Pts',(-67.3076469814166,17.0427969476755,-72.1628009962699));
#42399=CARTESIAN_POINT('Ctrl Pts',(-67.3077616390266,17.4418457255338,-72.9134843805435));
#42400=CARTESIAN_POINT('Ctrl Pts',(-67.3080145306994,18.2413498671255,-74.4139694720434));
#42401=CARTESIAN_POINT('Ctrl Pts',(-67.3079779188089,18.9112408709397,-75.6668108364885));
#42402=CARTESIAN_POINT('Ctrl Pts',(-67.3077127272134,19.8829571287319,-77.4942050732508));
#42403=CARTESIAN_POINT('Ctrl Pts',(-67.3078280944553,20.318656508363,-78.3134992775899));
#42404=CARTESIAN_POINT('Ctrl Pts',(-67.3078280944529,20.7551780957521,-79.134476979685));
#42405=CARTESIAN_POINT('Ctrl Pts',(-65.1729327667129,7.18175574164057,24.8300916319504));
#42406=CARTESIAN_POINT('Ctrl Pts',(-65.1731006306621,7.18176547068664,24.781194303211));
#42407=CARTESIAN_POINT('Ctrl Pts',(-65.1732766972058,7.18177566391607,24.7322978687525));
#42408=CARTESIAN_POINT('Ctrl Pts',(-65.1753571165701,7.18189796096853,24.181473259413));
#42409=CARTESIAN_POINT('Ctrl Pts',(-65.176438647727,7.18157806354087,23.1769240129338));
#42410=CARTESIAN_POINT('Ctrl Pts',(-65.1785990533414,7.18054693828407,21.1679996176307));
#42411=CARTESIAN_POINT('Ctrl Pts',(-65.192484643868,7.18138468374927,19.6638715508315));
#42412=CARTESIAN_POINT('Ctrl Pts',(-65.2244936611386,7.18522550993877,18.4129862938216));
#42413=CARTESIAN_POINT('Ctrl Pts',(-65.2395231838244,7.18700742344305,17.9096005950179));
#42414=CARTESIAN_POINT('Ctrl Pts',(-65.2767049565944,7.19137325174919,16.9050968056351));
#42415=CARTESIAN_POINT('Ctrl Pts',(-65.3564962710775,7.20089393748341,15.1508281818811));
#42416=CARTESIAN_POINT('Ctrl Pts',(-65.4366562425691,7.21131561767836,13.6505216649638));
#42417=CARTESIAN_POINT('Ctrl Pts',(-65.4947464921632,7.22052378517439,12.3986048174561));
#42418=CARTESIAN_POINT('Ctrl Pts',(-65.5194228726211,7.22461698459507,11.8988115580567));
#42419=CARTESIAN_POINT('Ctrl Pts',(-65.5726798734756,7.23405319214692,10.898840753164));
#42420=CARTESIAN_POINT('Ctrl Pts',(-65.6430001132168,7.2471190074519,9.64780942493501));
#42421=CARTESIAN_POINT('Ctrl Pts',(-65.7210118147592,7.2622821734432,8.14323182215361));
#42422=CARTESIAN_POINT('Ctrl Pts',(-65.7607837886347,7.26991612109166,7.13698809994421));
#42423=CARTESIAN_POINT('Ctrl Pts',(-65.7791343148924,7.27337759048613,6.50737055322745));
#42424=CARTESIAN_POINT('Ctrl Pts',(-65.7866816659716,7.2744078822174,6.25153810606456));
#42425=CARTESIAN_POINT('Ctrl Pts',(-65.8021713561666,7.27501414102468,5.74396397630533));
#42426=CARTESIAN_POINT('Ctrl Pts',(-65.8293878736281,7.27299490306546,4.85742889524331));
#42427=CARTESIAN_POINT('Ctrl Pts',(-65.8752994724579,7.26213375344673,3.09979743749822));
#42428=CARTESIAN_POINT('Ctrl Pts',(-65.8735048151651,7.25912195022732,1.62896241126073));
#42429=CARTESIAN_POINT('Ctrl Pts',(-65.8322698068349,7.28148808984448,0.604410369730052));
#42430=CARTESIAN_POINT('Ctrl Pts',(-65.8269365106498,7.28382509893192,0.458530192554338));
#42431=CARTESIAN_POINT('Ctrl Pts',(-65.8150539209303,7.28525649887588,0.183890613738274));
#42432=CARTESIAN_POINT('Ctrl Pts',(-65.7909935752901,7.28121908724863,-0.295181368341263));
#42433=CARTESIAN_POINT('Ctrl Pts',(-65.7479654170422,7.2620589119011,-0.950370087138988));
#42434=CARTESIAN_POINT('Ctrl Pts',(-65.6840197828005,7.23415949011369,-1.69777034578746));
#42435=CARTESIAN_POINT('Ctrl Pts',(-65.5854876409769,7.20742295195961,-2.63740705266532));
#42436=CARTESIAN_POINT('Ctrl Pts',(-65.4443779860654,7.22096622634433,-3.70705755910344));
#42437=CARTESIAN_POINT('Ctrl Pts',(-65.345245023354,7.33247226156198,-4.47217890661716));
#42438=CARTESIAN_POINT('Ctrl Pts',(-65.2979157678212,7.45312012683586,-4.93759588484351));
#42439=CARTESIAN_POINT('Ctrl Pts',(-65.2804785126524,7.50112655480425,-5.0995647485744));
#42440=CARTESIAN_POINT('Ctrl Pts',(-65.2395481259881,7.63544794831347,-5.47205399305951));
#42441=CARTESIAN_POINT('Ctrl Pts',(-65.1562506133512,7.95410912208094,-6.18518406530892));
#42442=CARTESIAN_POINT('Ctrl Pts',(-65.0052479173948,8.61964836548844,-7.35890192235289));
#42443=CARTESIAN_POINT('Ctrl Pts',(-64.8395199160683,9.40141111790384,-8.66272049186451));
#42444=CARTESIAN_POINT('Ctrl Pts',(-64.7377773979986,9.91756603305767,-9.65968667108287));
#42445=CARTESIAN_POINT('Ctrl Pts',(-64.6888422500041,10.1892383163194,-10.259520915547));
#42446=CARTESIAN_POINT('Ctrl Pts',(-64.6685015126593,10.3146673064093,-10.571342686021));
#42447=CARTESIAN_POINT('Ctrl Pts',(-64.6554064435216,10.40373887505,-10.8102983290437));
#42448=CARTESIAN_POINT('Ctrl Pts',(-64.6520444913612,10.4533044253585,-10.9405423567448));
#42449=CARTESIAN_POINT('Ctrl Pts',(-64.6458528877893,10.5562636271704,-11.2173755632169));
#42450=CARTESIAN_POINT('Ctrl Pts',(-64.6443003259781,10.729009873209,-11.6917518645855));
#42451=CARTESIAN_POINT('Ctrl Pts',(-64.6692140356061,11.0572039967835,-12.6414406117879));
#42452=CARTESIAN_POINT('Ctrl Pts',(-64.7748437077602,11.4627448290961,-13.9868601108971));
#42453=CARTESIAN_POINT('Ctrl Pts',(-64.9023929031954,11.7353176655387,-15.1977465931819));
#42454=CARTESIAN_POINT('Ctrl Pts',(-64.9730859398394,11.8780561006582,-16.003632893284));
#42455=CARTESIAN_POINT('Ctrl Pts',(-65.0144064204024,11.9637472321134,-16.5408015357675));
#42456=CARTESIAN_POINT('Ctrl Pts',(-65.036810908705,12.0176256541411,-16.9430078212279));
#42457=CARTESIAN_POINT('Ctrl Pts',(-65.0483918994916,12.0576678349292,-17.2778640553446));
#42458=CARTESIAN_POINT('Ctrl Pts',(-65.0524394558381,12.0742199515051,-17.4248988623711));
#42459=CARTESIAN_POINT('Ctrl Pts',(-65.059593815533,12.1019222700238,-17.7087034577803));
#42460=CARTESIAN_POINT('Ctrl Pts',(-65.065115123067,12.1239068138689,-17.9932360279406));
#42461=CARTESIAN_POINT('Ctrl Pts',(-65.0692116335719,12.1403445332771,-18.2735090635166));
#42462=CARTESIAN_POINT('Ctrl Pts',(-65.0711917791365,12.1485863813074,-18.4479829553626));
#42463=CARTESIAN_POINT('Ctrl Pts',(-65.0724518363108,12.1540079468313,-18.5867619236669));
#42464=CARTESIAN_POINT('Ctrl Pts',(-65.0732381579507,12.1575226457074,-18.6905548579323));
#42465=CARTESIAN_POINT('Ctrl Pts',(-65.0737661119046,12.1600040267476,-18.776760678138));
#42466=CARTESIAN_POINT('Ctrl Pts',(-65.0741139960963,12.161734611473,-18.8455631933068));
#42467=CARTESIAN_POINT('Ctrl Pts',(-65.0766615262646,12.1750053272291,-19.4294573932671));
#42468=CARTESIAN_POINT('Ctrl Pts',(-65.0687114676951,12.1567208841226,-20.5166934694074));
#42469=CARTESIAN_POINT('Ctrl Pts',(-65.0420209941393,12.0860740690322,-22.0377659033389));
#42470=CARTESIAN_POINT('Ctrl Pts',(-65.0297090483665,12.0563534656099,-22.9972621820203));
#42471=CARTESIAN_POINT('Ctrl Pts',(-65.0288044687836,12.0559985325857,-23.5792914978727));
#42472=CARTESIAN_POINT('Ctrl Pts',(-65.0284706314498,12.0558629287408,-23.8339510858948));
#42473=CARTESIAN_POINT('Ctrl Pts',(-65.0278976338286,12.0556160776309,-24.3303747538134));
#42474=CARTESIAN_POINT('Ctrl Pts',(-65.0271282891604,12.0552335060199,-25.2079354084859));
#42475=CARTESIAN_POINT('Ctrl Pts',(-65.026601121765,12.0548554597604,-26.4615383680323));
#42476=CARTESIAN_POINT('Ctrl Pts',(-65.0265849159444,12.0546807638577,-27.9706860922064));
#42477=CARTESIAN_POINT('Ctrl Pts',(-65.0267830893282,12.0547572443005,-28.975322605205));
#42478=CARTESIAN_POINT('Ctrl Pts',(-65.0268966462046,12.0548512731844,-29.539530536201));
#42479=CARTESIAN_POINT('Ctrl Pts',(-65.0269197971744,12.0548744982796,-29.6648497847285));
#42480=CARTESIAN_POINT('Ctrl Pts',(-65.0269599296714,12.0549296743612,-29.9155791753429));
#42481=CARTESIAN_POINT('Ctrl Pts',(-65.0270172921303,12.055050139514,-30.3545185075444));
#42482=CARTESIAN_POINT('Ctrl Pts',(-65.027114817731,12.0553729207471,-31.2329193484625));
#42483=CARTESIAN_POINT('Ctrl Pts',(-65.0273850542116,12.0560432368111,-32.4885410674878));
#42484=CARTESIAN_POINT('Ctrl Pts',(-65.0283289325803,12.0568680050243,-33.7431920138229));
#42485=CARTESIAN_POINT('Ctrl Pts',(-65.0297895448079,12.0575451092745,-34.7450603784708));
#42486=CARTESIAN_POINT('Ctrl Pts',(-65.0308017464864,12.0578906286939,-35.2452602875554));
#42487=CARTESIAN_POINT('Ctrl Pts',(-65.0316892610028,12.0581422004777,-35.6210283418864));
#42488=CARTESIAN_POINT('Ctrl Pts',(-65.032356599898,12.0582981071551,-35.8728926831772));
#42489=CARTESIAN_POINT('Ctrl Pts',(-65.0339471095556,12.0585643755601,-36.3757447541211));
#42490=CARTESIAN_POINT('Ctrl Pts',(-65.0373045889605,12.0589701842811,-37.2541885309612));
#42491=CARTESIAN_POINT('Ctrl Pts',(-65.0455921016347,12.0596801196328,-39.0060372985966));
#42492=CARTESIAN_POINT('Ctrl Pts',(-65.0528329561677,12.0610847527648,-40.506167908724));
#42493=CARTESIAN_POINT('Ctrl Pts',(-65.0561230687881,12.0635538952629,-41.7607219271154));
#42494=CARTESIAN_POINT('Ctrl Pts',(-65.0568807869497,12.0637897616258,-42.1392522960393));
#42495=CARTESIAN_POINT('Ctrl Pts',(-65.0575648769863,12.0635101890673,-42.6415769457643));
#42496=CARTESIAN_POINT('Ctrl Pts',(-65.0580703731843,12.0629819805719,-43.1441349944183));
#42497=CARTESIAN_POINT('Ctrl Pts',(-65.0584428191974,12.0621103910298,-43.7714134904261));
#42498=CARTESIAN_POINT('Ctrl Pts',(-65.0587147492222,12.0615562535142,-44.5226577243393));
#42499=CARTESIAN_POINT('Ctrl Pts',(-65.058996497838,12.0621888968184,-45.1468563514877));
#42500=CARTESIAN_POINT('Ctrl Pts',(-65.0593768292321,12.0637490456156,-45.6449060383322));
#42501=CARTESIAN_POINT('Ctrl Pts',(-65.05976957428,12.065551588587,-46.0176971655781));
#42502=CARTESIAN_POINT('Ctrl Pts',(-65.0603002313248,12.0680870066288,-46.3897078745373));
#42503=CARTESIAN_POINT('Ctrl Pts',(-65.0612326202001,12.0725740901228,-46.8845125519888));
#42504=CARTESIAN_POINT('Ctrl Pts',(-65.0622297353678,12.0773464433905,-47.2543460356923));
#42505=CARTESIAN_POINT('Ctrl Pts',(-65.0634913888751,12.0832508706114,-47.6235775922098));
#42506=CARTESIAN_POINT('Ctrl Pts',(-65.0644034048839,12.0883602483909,-47.8579214938423));
#42507=CARTESIAN_POINT('Ctrl Pts',(-65.0663413372696,12.1034236213073,-48.3394840139549));
#42508=CARTESIAN_POINT('Ctrl Pts',(-65.070052685802,12.1399819433414,-49.190730687232));
#42509=CARTESIAN_POINT('Ctrl Pts',(-65.0760796661541,12.2092354674003,-50.4451446520436));
#42510=CARTESIAN_POINT('Ctrl Pts',(-65.0845863352261,12.275437662191,-52.0050245066472));
#42511=CARTESIAN_POINT('Ctrl Pts',(-65.0916544734623,12.275475630366,-53.0826911850069));
#42512=CARTESIAN_POINT('Ctrl Pts',(-65.09686685345,12.2501386925666,-53.7703051293251));
#42513=CARTESIAN_POINT('Ctrl Pts',(-65.0993710942821,12.2333246964283,-54.0758996019516));
#42514=CARTESIAN_POINT('Ctrl Pts',(-65.1050038878201,12.1826499594705,-54.6544835605439));
#42515=CARTESIAN_POINT('Ctrl Pts',(-65.1159591757095,12.0588208329425,-55.6367269241876));
#42516=CARTESIAN_POINT('Ctrl Pts',(-65.1387536951772,11.7418820496672,-57.4448818104869));
#42517=CARTESIAN_POINT('Ctrl Pts',(-65.1497661458798,11.5796938358338,-58.7322284200674));
#42518=CARTESIAN_POINT('Ctrl Pts',(-65.1588520219563,11.6269959572717,-59.4966254801638));
#42519=CARTESIAN_POINT('Ctrl Pts',(-65.1597913711798,11.6346205198146,-59.6099285989042));
#42520=CARTESIAN_POINT('Ctrl Pts',(-65.1617104418904,11.6523304276544,-59.8259887953581));
#42521=CARTESIAN_POINT('Ctrl Pts',(-65.1649009270484,11.691615509919,-60.2119414469383));
#42522=CARTESIAN_POINT('Ctrl Pts',(-65.1708131027259,11.8008814112987,-60.9876425042924));
#42523=CARTESIAN_POINT('Ctrl Pts',(-65.1763985760326,11.9919267773979,-61.8927913471379));
#42524=CARTESIAN_POINT('Ctrl Pts',(-65.1810324756269,12.2381836869314,-62.8074081928519));
#42525=CARTESIAN_POINT('Ctrl Pts',(-65.1833616050184,12.3950912618894,-63.3249534797546));
#42526=CARTESIAN_POINT('Ctrl Pts',(-65.1848342053435,12.5063773919337,-63.6706366796427));
#42527=CARTESIAN_POINT('Ctrl Pts',(-65.1857972679305,12.5822823477447,-63.9012835400789));
#42528=CARTESIAN_POINT('Ctrl Pts',(-65.1867409286383,12.660624217389,-64.1320289060336));
#42529=CARTESIAN_POINT('Ctrl Pts',(-65.1875523445398,12.731160099571,-64.3340819354547));
#42530=CARTESIAN_POINT('Ctrl Pts',(-65.1880133661692,12.7720055701951,-64.4495628783271));
#42531=CARTESIAN_POINT('Ctrl Pts',(-65.1887043345812,12.8337891082829,-64.6227742878501));
#42532=CARTESIAN_POINT('Ctrl Pts',(-65.1892753734552,12.886355873928,-64.7671680924818));
#42533=CARTESIAN_POINT('Ctrl Pts',(-65.1902574334737,12.9744186327503,-65.0055722577058));
#42534=CARTESIAN_POINT('Ctrl Pts',(-65.1929639939196,13.0572795677294,-65.2184944200882));
#42535=CARTESIAN_POINT('Ctrl Pts',(-65.1970899407941,13.2465759472662,-65.6684907956169));
#42536=CARTESIAN_POINT('Ctrl Pts',(-65.2038379111266,13.6150876757719,-66.4579896989852));
#42537=CARTESIAN_POINT('Ctrl Pts',(-65.2120073023104,14.495184046943,-68.0969542174842));
#42538=CARTESIAN_POINT('Ctrl Pts',(-65.2094453005085,15.3932338570684,-69.5914701280964));
#42539=CARTESIAN_POINT('Ctrl Pts',(-65.2040506590276,16.0247361035807,-70.7929256923783));
#42540=CARTESIAN_POINT('Ctrl Pts',(-65.2045249298405,16.1536203661614,-71.0374784533412));
#42541=CARTESIAN_POINT('Ctrl Pts',(-65.2044911734284,16.4189686424828,-71.5399939605228));
#42542=CARTESIAN_POINT('Ctrl Pts',(-65.2048113970372,16.748964735239,-72.1627235728458));
#42543=CARTESIAN_POINT('Ctrl Pts',(-65.2049254398224,17.1480141148444,-72.9134082444139));
#42544=CARTESIAN_POINT('Ctrl Pts',(-65.2051758444602,17.94751750513,-74.4138952011896));
#42545=CARTESIAN_POINT('Ctrl Pts',(-65.2051372831542,18.6174048008469,-75.666735182131));
#42546=CARTESIAN_POINT('Ctrl Pts',(-65.2048737521369,19.589119601252,-77.4941259620686));
#42547=CARTESIAN_POINT('Ctrl Pts',(-65.2049884661457,20.0248191246354,-78.3134208257811));
#42548=CARTESIAN_POINT('Ctrl Pts',(-65.2049884661443,20.4613407120248,-79.1343985278809));
#42549=CARTESIAN_POINT('Ctrl Pts',(-63.7696894174353,6.98565352544322,24.8297715781906));
#42550=CARTESIAN_POINT('Ctrl Pts',(-63.7698754022371,6.98565901678319,24.7808654437697));
#42551=CARTESIAN_POINT('Ctrl Pts',(-63.7700704419802,6.98566484175051,24.7319599955762));
#42552=CARTESIAN_POINT('Ctrl Pts',(-63.7723747362441,6.98573226498455,24.1810332173695));
#42553=CARTESIAN_POINT('Ctrl Pts',(-63.7740759382634,6.98531388885199,23.1764572572281));
#42554=CARTESIAN_POINT('Ctrl Pts',(-63.7779798012375,6.98405340995919,21.1672988065382));
#42555=CARTESIAN_POINT('Ctrl Pts',(-63.7933215085387,6.98451453063052,19.662989697282));
#42556=CARTESIAN_POINT('Ctrl Pts',(-63.8261929975327,6.98782796082582,18.4119278795435));
#42557=CARTESIAN_POINT('Ctrl Pts',(-63.8418447324602,6.98925763853974,17.9076482542059));
#42558=CARTESIAN_POINT('Ctrl Pts',(-63.880926988907,6.99260755998853,16.9025804656894));
#42559=CARTESIAN_POINT('Ctrl Pts',(-63.9647088951749,6.99992394929679,15.1487433991109));
#42560=CARTESIAN_POINT('Ctrl Pts',(-64.0455470805801,7.00949894400017,13.6515218526789));
#42561=CARTESIAN_POINT('Ctrl Pts',(-64.098696702948,7.01997981272938,12.4032514948202));
#42562=CARTESIAN_POINT('Ctrl Pts',(-64.1207157044886,7.02480995950052,11.9049960438307));
#42563=CARTESIAN_POINT('Ctrl Pts',(-64.1665352750066,7.03635887512195,10.9070850335965));
#42564=CARTESIAN_POINT('Ctrl Pts',(-64.2244318158956,7.05318465097466,9.65722545946371));
#42565=CARTESIAN_POINT('Ctrl Pts',(-64.2866992888549,7.0730305690719,8.15210701155296));
#42566=CARTESIAN_POINT('Ctrl Pts',(-64.3177633310595,7.08346918516099,7.14421141822163));
#42567=CARTESIAN_POINT('Ctrl Pts',(-64.3322248208874,7.08827621830881,6.51340849004068));
#42568=CARTESIAN_POINT('Ctrl Pts',(-64.3379036734705,7.09000405968928,6.26145462276259));
#42569=CARTESIAN_POINT('Ctrl Pts',(-64.3488488955487,7.0928476106599,5.75783761392703));
#42570=CARTESIAN_POINT('Ctrl Pts',(-64.3665313656493,7.09644101342747,4.87630620818669));
#42571=CARTESIAN_POINT('Ctrl Pts',(-64.3931775759778,7.09983365583526,3.11473296932821));
#42572=CARTESIAN_POINT('Ctrl Pts',(-64.390706566645,7.10323420609789,1.61707447161998));
#42573=CARTESIAN_POINT('Ctrl Pts',(-64.3656735433867,7.11125149590393,0.566093556418151));
#42574=CARTESIAN_POINT('Ctrl Pts',(-64.3626063731248,7.11154332115744,0.417459700651948));
#42575=CARTESIAN_POINT('Ctrl Pts',(-64.3562519135411,7.10849507332251,0.137579049188044));
#42576=CARTESIAN_POINT('Ctrl Pts',(-64.3444164021131,7.09530783242205,-0.349523687108764));
#42577=CARTESIAN_POINT('Ctrl Pts',(-64.3252031381455,7.05979166709545,-1.01361669019925));
#42578=CARTESIAN_POINT('Ctrl Pts',(-64.2970831645417,7.00916298099789,-1.76931776303998));
#42579=CARTESIAN_POINT('Ctrl Pts',(-64.252057415312,6.95081827755828,-2.71870875872315));
#42580=CARTESIAN_POINT('Ctrl Pts',(-64.1790545778391,6.93153335347633,-3.79916535074235));
#42581=CARTESIAN_POINT('Ctrl Pts',(-64.1044018915843,7.02167392362584,-4.55546854069931));
#42582=CARTESIAN_POINT('Ctrl Pts',(-64.055960785065,7.12358918683067,-5.00983827241397));
#42583=CARTESIAN_POINT('Ctrl Pts',(-64.0352080829805,7.16701362915479,-5.1804555944748));
#42584=CARTESIAN_POINT('Ctrl Pts',(-63.9845619585847,7.2837517387543,-5.55675071672487));
#42585=CARTESIAN_POINT('Ctrl Pts',(-63.8768951076057,7.55749257169478,-6.2706362403536));
#42586=CARTESIAN_POINT('Ctrl Pts',(-63.6860409931831,8.12647345543323,-7.43121625720289));
#42587=CARTESIAN_POINT('Ctrl Pts',(-63.4897568246847,8.81062253157607,-8.71673413747512));
#42588=CARTESIAN_POINT('Ctrl Pts',(-63.3751676902504,9.27810483645933,-9.68542634044361));
#42589=CARTESIAN_POINT('Ctrl Pts',(-63.3215359864303,9.53122238448528,-10.2618406454498));
#42590=CARTESIAN_POINT('Ctrl Pts',(-63.299654584813,9.65124363494989,-10.5588933561495));
#42591=CARTESIAN_POINT('Ctrl Pts',(-63.2856764206741,9.73803276839272,-10.7852775908397));
#42592=CARTESIAN_POINT('Ctrl Pts',(-63.2822813596893,9.78582617521137,-10.9050332690881));
#42593=CARTESIAN_POINT('Ctrl Pts',(-63.275435806406,9.88868110167001,-11.1631131951564));
#42594=CARTESIAN_POINT('Ctrl Pts',(-63.2722147714165,10.0681138616425,-11.6064577992792));
#42595=CARTESIAN_POINT('Ctrl Pts',(-63.2908788132213,10.4351120140857,-12.5043246842074));
#42596=CARTESIAN_POINT('Ctrl Pts',(-63.3792311558901,10.9515206937253,-13.804208650469));
#42597=CARTESIAN_POINT('Ctrl Pts',(-63.4895117642943,11.3514805234501,-15.0210988949459));
#42598=CARTESIAN_POINT('Ctrl Pts',(-63.5517362811958,11.5696710320611,-15.855747929383));
#42599=CARTESIAN_POINT('Ctrl Pts',(-63.5881689262417,11.7012922018101,-16.4186870190564));
#42600=CARTESIAN_POINT('Ctrl Pts',(-63.6079221058119,11.7828702143422,-16.8479091406712));
#42601=CARTESIAN_POINT('Ctrl Pts',(-63.6177306458527,11.8399814853698,-17.209139536956));
#42602=CARTESIAN_POINT('Ctrl Pts',(-63.6212262162933,11.8623333559051,-17.3601464543715));
#42603=CARTESIAN_POINT('Ctrl Pts',(-63.6275625825483,11.9004279682416,-17.6553308721399));
#42604=CARTESIAN_POINT('Ctrl Pts',(-63.6327263352227,11.9305108061342,-17.9493048631528));
#42605=CARTESIAN_POINT('Ctrl Pts',(-63.636814929413,11.9532190071079,-18.2390800966978));
#42606=CARTESIAN_POINT('Ctrl Pts',(-63.6389297014477,11.9646334412043,-18.419027608437));
#42607=CARTESIAN_POINT('Ctrl Pts',(-63.6403699837502,11.9721946874457,-18.5620587376317));
#42608=CARTESIAN_POINT('Ctrl Pts',(-63.6413268066055,11.9771192867651,-18.6689280061842));
#42609=CARTESIAN_POINT('Ctrl Pts',(-63.6420245297228,11.9806217858325,-18.7576224800683));
#42610=CARTESIAN_POINT('Ctrl Pts',(-63.6425237893563,11.9830812331201,-18.8283632041732));
#42611=CARTESIAN_POINT('Ctrl Pts',(-63.6464473787105,12.0020513115575,-19.4284651472464));
#42612=CARTESIAN_POINT('Ctrl Pts',(-63.6437138971256,11.9798821969473,-20.5374478886419));
#42613=CARTESIAN_POINT('Ctrl Pts',(-63.6262506952142,11.8912747104092,-22.0636299507839));
#42614=CARTESIAN_POINT('Ctrl Pts',(-63.6179169859225,11.8553060677419,-23.0089801859288));
#42615=CARTESIAN_POINT('Ctrl Pts',(-63.618118343459,11.8553665692817,-23.5769319212298));
#42616=CARTESIAN_POINT('Ctrl Pts',(-63.6181784988178,11.8553617093484,-23.833611292254));
#42617=CARTESIAN_POINT('Ctrl Pts',(-63.6182267748102,11.855244353337,-24.3297026902985));
#42618=CARTESIAN_POINT('Ctrl Pts',(-63.6181442093241,11.8547963251245,-25.2086594719894));
#42619=CARTESIAN_POINT('Ctrl Pts',(-63.6176784819112,11.8537177944518,-26.4623719266191));
#42620=CARTESIAN_POINT('Ctrl Pts',(-63.6169388654805,11.8525376530228,-27.9714101984933));
#42621=CARTESIAN_POINT('Ctrl Pts',(-63.6166024463615,11.8523626942919,-28.9751301649085));
#42622=CARTESIAN_POINT('Ctrl Pts',(-63.616525609042,11.8525915130598,-29.538673180489));
#42623=CARTESIAN_POINT('Ctrl Pts',(-63.6165016390556,11.8526496677232,-29.663897709431));
#42624=CARTESIAN_POINT('Ctrl Pts',(-63.6164302295526,11.8527912434887,-29.9144197942482));
#42625=CARTESIAN_POINT('Ctrl Pts',(-63.6162516972046,11.8531027923439,-30.3530468480679));
#42626=CARTESIAN_POINT('Ctrl Pts',(-63.6157311073167,11.8539546247715,-31.2309389380913));
#42627=CARTESIAN_POINT('Ctrl Pts',(-63.6148431265873,11.8556795568147,-32.4861989169135));
#42628=CARTESIAN_POINT('Ctrl Pts',(-63.6145935192643,11.8576843350789,-33.7409476810005));
#42629=CARTESIAN_POINT('Ctrl Pts',(-63.6152713142585,11.8592171607395,-34.7431466351753));
#42630=CARTESIAN_POINT('Ctrl Pts',(-63.6159933336223,11.859920622453,-35.2436139868135));
#42631=CARTESIAN_POINT('Ctrl Pts',(-63.6167079047789,11.8604100846371,-35.6196094130991));
#42632=CARTESIAN_POINT('Ctrl Pts',(-63.6172684324702,11.8607237861603,-35.8714646383254));
#42633=CARTESIAN_POINT('Ctrl Pts',(-63.6186752536478,11.861303074395,-36.3743891623664));
#42634=CARTESIAN_POINT('Ctrl Pts',(-63.6217993206522,11.8622275208018,-37.252922343994));
#42635=CARTESIAN_POINT('Ctrl Pts',(-63.6298477047311,11.8639233401363,-39.0049862482332));
#42636=CARTESIAN_POINT('Ctrl Pts',(-63.6371263912388,11.8659636564327,-40.5053058386373));
#42637=CARTESIAN_POINT('Ctrl Pts',(-63.640311572706,11.868849022841,-41.7600215564704));
#42638=CARTESIAN_POINT('Ctrl Pts',(-63.6410215578774,11.8692071894829,-42.1385714134598));
#42639=CARTESIAN_POINT('Ctrl Pts',(-63.6416247968917,11.8690788609008,-42.6409437357382));
#42640=CARTESIAN_POINT('Ctrl Pts',(-63.6420442113358,11.8686913607439,-43.1435505796875));
#42641=CARTESIAN_POINT('Ctrl Pts',(-63.6423057211347,11.8679765546826,-43.7709009231348));
#42642=CARTESIAN_POINT('Ctrl Pts',(-63.642464081799,11.8675775925606,-44.5222452391161));
#42643=CARTESIAN_POINT('Ctrl Pts',(-63.6426880223968,11.8683102916394,-45.1465401450018));
#42644=CARTESIAN_POINT('Ctrl Pts',(-63.6430543735511,11.8699350545023,-45.6446752421376));
#42645=CARTESIAN_POINT('Ctrl Pts',(-63.6434567293027,11.8717768159626,-46.0175343101423));
#42646=CARTESIAN_POINT('Ctrl Pts',(-63.6440198836177,11.8743423734263,-46.3896168324758));
#42647=CARTESIAN_POINT('Ctrl Pts',(-63.6450304489903,11.8788571094554,-46.8845230715641));
#42648=CARTESIAN_POINT('Ctrl Pts',(-63.6461291598736,11.8836364224796,-47.2544375579395));
#42649=CARTESIAN_POINT('Ctrl Pts',(-63.647528478827,11.8895375926054,-47.6237561523055));
#42650=CARTESIAN_POINT('Ctrl Pts',(-63.6485428951208,11.8946411569445,-47.8581835740059));
#42651=CARTESIAN_POINT('Ctrl Pts',(-63.6507219838377,11.9096733665,-48.3398826218171));
#42652=CARTESIAN_POINT('Ctrl Pts',(-63.6549464333906,11.9461278115514,-49.191338394477));
#42653=CARTESIAN_POINT('Ctrl Pts',(-63.6619157754883,12.0151208620817,-50.4459409503195));
#42654=CARTESIAN_POINT('Ctrl Pts',(-63.6717891625091,12.0808794384306,-52.005892033572));
#42655=CARTESIAN_POINT('Ctrl Pts',(-63.6798303075965,12.0806248037229,-53.083496984492));
#42656=CARTESIAN_POINT('Ctrl Pts',(-63.6856537767969,12.0551219416618,-53.7710411485962));
#42657=CARTESIAN_POINT('Ctrl Pts',(-63.6884233195104,12.0382215980599,-54.0767002566206));
#42658=CARTESIAN_POINT('Ctrl Pts',(-63.6946323725045,11.9873734678641,-54.6553408493773));
#42659=CARTESIAN_POINT('Ctrl Pts',(-63.7066933073477,11.8632328948125,-55.6376679014349));
#42660=CARTESIAN_POINT('Ctrl Pts',(-63.7319072425593,11.5456916330798,-57.4458331464746));
#42661=CARTESIAN_POINT('Ctrl Pts',(-63.7447621529028,11.3832837960144,-58.7329792961044));
#42662=CARTESIAN_POINT('Ctrl Pts',(-63.7545613485058,11.4305221025594,-59.4970096797001));
#42663=CARTESIAN_POINT('Ctrl Pts',(-63.7555848923888,11.4381341868878,-59.6102728268609));
#42664=CARTESIAN_POINT('Ctrl Pts',(-63.7576573519843,11.4558255574764,-59.8262552169067));
#42665=CARTESIAN_POINT('Ctrl Pts',(-63.7610798780398,11.4950864058057,-60.2120843422442));
#42666=CARTESIAN_POINT('Ctrl Pts',(-63.7673238661899,11.604340302306,-60.9875841261972));
#42667=CARTESIAN_POINT('Ctrl Pts',(-63.7730478757242,11.7954457433543,-61.8926106059757));
#42668=CARTESIAN_POINT('Ctrl Pts',(-63.7777058427018,12.0418075447461,-62.8071988471768));
#42669=CARTESIAN_POINT('Ctrl Pts',(-63.7800290846894,12.1987823712394,-63.3247601796953));
#42670=CARTESIAN_POINT('Ctrl Pts',(-63.7814988872406,12.3101139836278,-63.6704669069245));
#42671=CARTESIAN_POINT('Ctrl Pts',(-63.7824611602337,12.3860489760023,-63.9011327444094));
#42672=CARTESIAN_POINT('Ctrl Pts',(-63.7834061546104,12.4644205718716,-64.1319021146194));
#42673=CARTESIAN_POINT('Ctrl Pts',(-63.7842226387807,12.534981143384,-64.3339803821948));
#42674=CARTESIAN_POINT('Ctrl Pts',(-63.7846878529151,12.5758403042838,-64.4494769739131));
#42675=CARTESIAN_POINT('Ctrl Pts',(-63.7853865526954,12.6376438717188,-64.6227130283474));
#42676=CARTESIAN_POINT('Ctrl Pts',(-63.7859671043656,12.6902263580769,-64.7671299996233));
#42677=CARTESIAN_POINT('Ctrl Pts',(-63.7869707071906,12.7783127131793,-65.0055749183316));
#42678=CARTESIAN_POINT('Ctrl Pts',(-63.7897023542802,12.8611805287705,-65.2184920273913));
#42679=CARTESIAN_POINT('Ctrl Pts',(-63.7938642659111,13.0504967665102,-65.6685032220532));
#42680=CARTESIAN_POINT('Ctrl Pts',(-63.8006501111802,13.419030367146,-66.4580109154324));
#42681=CARTESIAN_POINT('Ctrl Pts',(-63.8088093151091,14.2991451022795,-68.0969920796353));
#42682=CARTESIAN_POINT('Ctrl Pts',(-63.8061682095631,15.197178338022,-69.5915031348636));
#42683=CARTESIAN_POINT('Ctrl Pts',(-63.8007614617662,15.8286774377953,-70.7929513875053));
#42684=CARTESIAN_POINT('Ctrl Pts',(-63.8012363421957,15.9575632529478,-71.0375054692253));
#42685=CARTESIAN_POINT('Ctrl Pts',(-63.8012020563296,16.2229128823079,-71.5400218089304));
#42686=CARTESIAN_POINT('Ctrl Pts',(-63.8015224371708,16.5529105451709,-72.1627527612785));
#42687=CARTESIAN_POINT('Ctrl Pts',(-63.8016365427922,16.9519606071174,-72.9134384000559));
#42688=CARTESIAN_POINT('Ctrl Pts',(-63.801887531904,17.7514641555769,-74.4139267390471));
#42689=CARTESIAN_POINT('Ctrl Pts',(-63.8018491238696,18.4213494921883,-75.6667656774867));
#42690=CARTESIAN_POINT('Ctrl Pts',(-63.8015849222615,19.3930630603169,-77.4941539578504));
#42691=CARTESIAN_POINT('Ctrl Pts',(-63.8016996598983,19.8287630444859,-78.3134493621658));
#42692=CARTESIAN_POINT('Ctrl Pts',(-63.8016996598979,20.2652846318753,-79.1344270642664));
#42693=CARTESIAN_POINT('Ctrl Pts',(-62.8338151407029,6.8546477540195,24.8297302613622));
#42694=CARTESIAN_POINT('Ctrl Pts',(-62.8340115792225,6.85465323508077,24.7808221078273));
#42695=CARTESIAN_POINT('Ctrl Pts',(-62.8342175601913,6.85465899790165,24.7319145444119));
#42696=CARTESIAN_POINT('Ctrl Pts',(-62.8366511414996,6.85472789486385,24.180965761181));
#42697=CARTESIAN_POINT('Ctrl Pts',(-62.8387162951856,6.85434969833623,23.1764292239802));
#42698=CARTESIAN_POINT('Ctrl Pts',(-62.8436351601958,6.8531811917745,21.1672018319798));
#42699=CARTESIAN_POINT('Ctrl Pts',(-62.8598283586026,6.85366027580704,19.662794087716));
#42700=CARTESIAN_POINT('Ctrl Pts',(-62.8931842631358,6.85683026604056,18.4116172696421));
#42701=CARTESIAN_POINT('Ctrl Pts',(-62.9091943230322,6.85816151222857,17.9069947365679));
#42702=CARTESIAN_POINT('Ctrl Pts',(-62.9493960520515,6.86118423799795,16.9017134160942));
#42703=CARTESIAN_POINT('Ctrl Pts',(-63.0355303640731,6.86776884027254,15.1480772929341));
#42704=CARTESIAN_POINT('Ctrl Pts',(-63.1167830427203,6.87677402886358,13.6519841949253));
#42705=CARTESIAN_POINT('Ctrl Pts',(-63.1668769608044,6.88742580172407,12.4050174992644));
#42706=CARTESIAN_POINT('Ctrl Pts',(-63.1872702187809,6.89236509125422,11.9072337591036));
#42707=CARTESIAN_POINT('Ctrl Pts',(-63.2285708140232,6.90433015335502,10.9099577545617));
#42708=CARTESIAN_POINT('Ctrl Pts',(-63.2791532115687,6.92188623197643,9.66042858869122));
#42709=CARTESIAN_POINT('Ctrl Pts',(-63.3319835707986,6.94309248454624,8.1550995458438));
#42710=CARTESIAN_POINT('Ctrl Pts',(-63.3577200966173,6.95446308247782,7.14685283004719));
#42711=CARTESIAN_POINT('Ctrl Pts',(-63.3695412050602,6.95984072374416,6.5158568507044));
#42712=CARTESIAN_POINT('Ctrl Pts',(-63.3740112364851,6.96194049935772,6.26579931908071));
#42713=CARTESIAN_POINT('Ctrl Pts',(-63.3819402533974,6.96596381357759,5.76417995360215));
#42714=CARTESIAN_POINT('Ctrl Pts',(-63.3931890708294,6.97246277513824,4.88524930960752));
#42715=CARTESIAN_POINT('Ctrl Pts',(-63.4049800456724,6.98320362282675,3.12260412316239));
#42716=CARTESIAN_POINT('Ctrl Pts',(-63.397064949177,6.98692004233924,1.61454048227347));
#42717=CARTESIAN_POINT('Ctrl Pts',(-63.3837705927333,6.98698504325039,0.549557566522543));
#42718=CARTESIAN_POINT('Ctrl Pts',(-63.3823088516265,6.98602192500681,0.400247124524424));
#42719=CARTESIAN_POINT('Ctrl Pts',(-63.379865221235,6.9805549762376,0.11840182408989));
#42720=CARTESIAN_POINT('Ctrl Pts',(-63.376586020454,6.96292688560398,-0.371955668368111));
#42721=CARTESIAN_POINT('Ctrl Pts',(-63.3735372952247,6.92107897807562,-1.04112212290876));
#42722=CARTESIAN_POINT('Ctrl Pts',(-63.3684057548297,6.86309953998232,-1.80275589269775));
#42723=CARTESIAN_POINT('Ctrl Pts',(-63.3552431104083,6.7953694544763,-2.75947712877428));
#42724=CARTESIAN_POINT('Ctrl Pts',(-63.3187759597658,6.76383147787105,-3.8469482611788));
#42725=CARTESIAN_POINT('Ctrl Pts',(-63.2579283717942,6.84104022493431,-4.60512667349721));
#42726=CARTESIAN_POINT('Ctrl Pts',(-63.209633432285,6.93174634857654,-5.05880999706912));
#42727=CARTESIAN_POINT('Ctrl Pts',(-63.1874589389198,6.97222160551015,-5.23775199780588));
#42728=CARTESIAN_POINT('Ctrl Pts',(-63.1324664682631,7.07740834543431,-5.62111870290018));
#42729=CARTESIAN_POINT('Ctrl Pts',(-63.0132710022083,7.32070934558602,-6.34142159100564));
#42730=CARTESIAN_POINT('Ctrl Pts',(-62.8029714049297,7.82089116164816,-7.49528858757482));
#42731=CARTESIAN_POINT('Ctrl Pts',(-62.5937142138828,8.43184828164372,-8.76555145163734));
#42732=CARTESIAN_POINT('Ctrl Pts',(-62.4750153791188,8.86099477492063,-9.71158643825483));
#42733=CARTESIAN_POINT('Ctrl Pts',(-62.4202266875157,9.09858812391573,-10.2697765285665));
#42734=CARTESIAN_POINT('Ctrl Pts',(-62.3980883968512,9.21353757691983,-10.5555636968051));
#42735=CARTESIAN_POINT('Ctrl Pts',(-62.3840055420638,9.29775731001258,-10.772483691087));
#42736=CARTESIAN_POINT('Ctrl Pts',(-62.3807561244255,9.34383584914166,-10.8851100172883));
#42737=CARTESIAN_POINT('Ctrl Pts',(-62.3737895087591,9.44543509673677,-11.1302410859108));
#42738=CARTESIAN_POINT('Ctrl Pts',(-62.3697124507635,9.62728392490675,-11.552595682906));
#42739=CARTESIAN_POINT('Ctrl Pts',(-62.3836776826827,10.0163651883242,-12.4161722919694));
#42740=CARTESIAN_POINT('Ctrl Pts',(-62.4572892794437,10.6025342688307,-13.6872799140626));
#42741=CARTESIAN_POINT('Ctrl Pts',(-62.551144293846,11.0857746927166,-14.9067694176834));
#42742=CARTESIAN_POINT('Ctrl Pts',(-62.6046657741735,11.3546649960417,-15.7588413683948));
#42743=CARTESIAN_POINT('Ctrl Pts',(-62.6360151165037,11.5174995819471,-16.3378357915975));
#42744=CARTESIAN_POINT('Ctrl Pts',(-62.6529197325506,11.6183684103482,-16.7844771132674));
#42745=CARTESIAN_POINT('Ctrl Pts',(-62.661007271049,11.6874564495597,-17.1630785787601));
#42746=CARTESIAN_POINT('Ctrl Pts',(-62.6639773063431,11.7137391607947,-17.3164072826276));
#42747=CARTESIAN_POINT('Ctrl Pts',(-62.6694917572641,11.7590410886046,-17.6187296259618));
#42748=CARTESIAN_POINT('Ctrl Pts',(-62.6742326758448,11.7948232448022,-17.9185801404599));
#42749=CARTESIAN_POINT('Ctrl Pts',(-62.6782132969468,11.8220628977155,-18.214357897131));
#42750=CARTESIAN_POINT('Ctrl Pts',(-62.6803854927335,11.8358204920855,-18.3977662585142));
#42751=CARTESIAN_POINT('Ctrl Pts',(-62.681938094352,11.8449976740084,-18.5434958556949));
#42752=CARTESIAN_POINT('Ctrl Pts',(-62.6830112083581,11.8510066622983,-18.6523195445154));
#42753=CARTESIAN_POINT('Ctrl Pts',(-62.6838310955826,11.8553124749393,-18.7425981540404));
#42754=CARTESIAN_POINT('Ctrl Pts',(-62.6844423537282,11.8583569043954,-18.8145734035056));
#42755=CARTESIAN_POINT('Ctrl Pts',(-62.689399559392,11.8819763640981,-19.4250116413265));
#42756=CARTESIAN_POINT('Ctrl Pts',(-62.6910339248514,11.8589163836346,-20.5480768373031));
#42757=CARTESIAN_POINT('Ctrl Pts',(-62.6815934174645,11.7609615658011,-22.0780145591206));
#42758=CARTESIAN_POINT('Ctrl Pts',(-62.6769185361321,11.721960099837,-23.0149122259586));
#42759=CARTESIAN_POINT('Ctrl Pts',(-62.678123904909,11.7226307795498,-23.5742749277269));
#42760=CARTESIAN_POINT('Ctrl Pts',(-62.6785373306137,11.7228653133253,-23.8323956434533));
#42761=CARTESIAN_POINT('Ctrl Pts',(-62.6791628363596,11.723061351535,-24.328550779212));
#42762=CARTESIAN_POINT('Ctrl Pts',(-62.6797649486642,11.7228301746731,-25.208812019077));
#42763=CARTESIAN_POINT('Ctrl Pts',(-62.6795180509527,11.721354647077,-26.4629723137077));
#42764=CARTESIAN_POINT('Ctrl Pts',(-62.6783663162937,11.719331824033,-27.9721402328826));
#42765=CARTESIAN_POINT('Ctrl Pts',(-62.6776431536264,11.7188561776346,-28.9752162355559));
#42766=CARTESIAN_POINT('Ctrl Pts',(-62.6774118773276,11.7191185710211,-29.5382640782203));
#42767=CARTESIAN_POINT('Ctrl Pts',(-62.6773491361315,11.7191843518876,-29.6634734726559));
#42768=CARTESIAN_POINT('Ctrl Pts',(-62.6771832973685,11.7193464575595,-29.9139158292759));
#42769=CARTESIAN_POINT('Ctrl Pts',(-62.6767974667868,11.7197081187366,-30.3524427022208));
#42770=CARTESIAN_POINT('Ctrl Pts',(-62.6757161266157,11.7207035080354,-31.2301571714372));
#42771=CARTESIAN_POINT('Ctrl Pts',(-62.6737284539109,11.7227420343164,-32.4853003188504));
#42772=CARTESIAN_POINT('Ctrl Pts',(-62.6723076625688,11.7250992605578,-33.7400848304719));
#42773=CARTESIAN_POINT('Ctrl Pts',(-62.6722045970334,11.7268711920779,-34.7423990436705));
#42774=CARTESIAN_POINT('Ctrl Pts',(-62.6726198912039,11.7276862042832,-35.2429609730206));
#42775=CARTESIAN_POINT('Ctrl Pts',(-62.6731482121727,11.7282453287308,-35.6190353193089));
#42776=CARTESIAN_POINT('Ctrl Pts',(-62.6735901991154,11.7286061377335,-35.8708877515963));
#42777=CARTESIAN_POINT('Ctrl Pts',(-62.6747833042721,11.7292760920224,-36.3738371005951));
#42778=CARTESIAN_POINT('Ctrl Pts',(-62.6775891060468,11.7303765850017,-37.252408178439));
#42779=CARTESIAN_POINT('Ctrl Pts',(-62.6851873348145,11.7323848629711,-39.0045498356469));
#42780=CARTESIAN_POINT('Ctrl Pts',(-62.692265882017,11.7347119494115,-40.5049667535654));
#42781=CARTESIAN_POINT('Ctrl Pts',(-62.695239949014,11.7377580254097,-41.7597505042597));
#42782=CARTESIAN_POINT('Ctrl Pts',(-62.6958792593676,11.738157075941,-42.1383079782095));
#42783=CARTESIAN_POINT('Ctrl Pts',(-62.6963815746102,11.7380731186388,-42.6406963780333));
#42784=CARTESIAN_POINT('Ctrl Pts',(-62.6966985552679,11.737727586151,-43.1433206750748));
#42785=CARTESIAN_POINT('Ctrl Pts',(-62.6968346575229,11.7370587036778,-43.770697111739));
#42786=CARTESIAN_POINT('Ctrl Pts',(-62.6968644079167,11.7367064246829,-44.522079902509));
#42787=CARTESIAN_POINT('Ctrl Pts',(-62.6970141184905,11.7374722068428,-45.1464142818122));
#42788=CARTESIAN_POINT('Ctrl Pts',(-62.6973494393679,11.7391167215345,-45.6445807164024));
#42789=CARTESIAN_POINT('Ctrl Pts',(-62.6977450145172,11.7409717862853,-46.0174655577079));
#42790=CARTESIAN_POINT('Ctrl Pts',(-62.6983200753203,11.7435488056649,-46.3895757692737));
#42791=CARTESIAN_POINT('Ctrl Pts',(-62.6993742294946,11.748076964468,-46.884520150013));
#42792=CARTESIAN_POINT('Ctrl Pts',(-62.7005405475063,11.7528632367589,-47.2544690340029));
#42793=CARTESIAN_POINT('Ctrl Pts',(-62.7020348968166,11.7587711374807,-47.6238212726955));
#42794=CARTESIAN_POINT('Ctrl Pts',(-62.7031217210978,11.763879089902,-47.8582798567994));
#42795=CARTESIAN_POINT('Ctrl Pts',(-62.7054764654297,11.7789149464117,-48.3400298774589));
#42796=CARTESIAN_POINT('Ctrl Pts',(-62.7100833225575,11.8153679604299,-49.1915642344275));
#42797=CARTESIAN_POINT('Ctrl Pts',(-62.717777994255,11.8843157202965,-50.4462399295271));
#42798=CARTESIAN_POINT('Ctrl Pts',(-62.7286999205461,11.9500069460353,-52.0062161071989));
#42799=CARTESIAN_POINT('Ctrl Pts',(-62.7374959362373,11.949687036557,-53.0838008351293));
#42800=CARTESIAN_POINT('Ctrl Pts',(-62.7437884983338,11.9241594855834,-53.7713208691149));
#42801=CARTESIAN_POINT('Ctrl Pts',(-62.7467611187832,11.907245159,-54.0769991327927));
#42802=CARTESIAN_POINT('Ctrl Pts',(-62.7534137736499,11.8563715973007,-54.6556565089427));
#42803=CARTESIAN_POINT('Ctrl Pts',(-62.7663322934056,11.7321812678653,-55.6380099133699));
#42804=CARTESIAN_POINT('Ctrl Pts',(-62.7934235036687,11.4145596951018,-57.4461871903748));
#42805=CARTESIAN_POINT('Ctrl Pts',(-62.8077245409834,11.2521219439642,-58.7332604275265));
#42806=CARTESIAN_POINT('Ctrl Pts',(-62.8180691335882,11.2993626248574,-59.4971603992213));
#42807=CARTESIAN_POINT('Ctrl Pts',(-62.8191556956144,11.3069755572714,-59.6104097894527));
#42808=CARTESIAN_POINT('Ctrl Pts',(-62.8213424963917,11.3246688368783,-59.8263651893896));
#42809=CARTESIAN_POINT('Ctrl Pts',(-62.8249355674505,11.3639328404393,-60.2121510219349));
#42810=CARTESIAN_POINT('Ctrl Pts',(-62.8314136747293,11.473195673799,-60.987579835687));
#42811=CARTESIAN_POINT('Ctrl Pts',(-62.8372132869808,11.6643200165725,-61.8925621015889));
#42812=CARTESIAN_POINT('Ctrl Pts',(-62.8418592680993,11.9107132299678,-62.8071417167703));
#42813=CARTESIAN_POINT('Ctrl Pts',(-62.8441621771561,12.067709855702,-63.3247106649581));
#42814=CARTESIAN_POINT('Ctrl Pts',(-62.8456207194592,12.1790564938607,-63.6704269131557));
#42815=CARTESIAN_POINT('Ctrl Pts',(-62.8465765977845,12.2550018209773,-63.9011003893636));
#42816=CARTESIAN_POINT('Ctrl Pts',(-62.8475177340291,12.3333834338942,-64.1318789040432));
#42817=CARTESIAN_POINT('Ctrl Pts',(-62.8483343466319,12.4039529527749,-64.3339667523024));
#42818=CARTESIAN_POINT('Ctrl Pts',(-62.8488008391134,12.4448171722134,-64.4494692201393));
#42819=CARTESIAN_POINT('Ctrl Pts',(-62.8495027592879,12.5066282910488,-64.6227144879154));
#42820=CARTESIAN_POINT('Ctrl Pts',(-62.8500889237322,12.5592167888116,-64.7671399538787));
#42821=CARTESIAN_POINT('Ctrl Pts',(-62.8511068271889,12.6473128402298,-65.0055997389676));
#42822=CARTESIAN_POINT('Ctrl Pts',(-62.8538567398629,12.7301855205883,-65.2185162513763));
#42823=CARTESIAN_POINT('Ctrl Pts',(-62.8580451703127,12.9195124929881,-65.6685342521179));
#42824=CARTESIAN_POINT('Ctrl Pts',(-62.8648618849641,13.2880586636127,-66.4580471169517));
#42825=CARTESIAN_POINT('Ctrl Pts',(-62.8730236038173,14.1681833963552,-68.0970356539531));
#42826=CARTESIAN_POINT('Ctrl Pts',(-62.8703297670018,15.0662044172692,-69.5915446237086));
#42827=CARTESIAN_POINT('Ctrl Pts',(-62.8649073183664,15.6976981063461,-70.7929892612915));
#42828=CARTESIAN_POINT('Ctrl Pts',(-62.8653830676195,15.8265847643315,-71.0375439352764));
#42829=CARTESIAN_POINT('Ctrl Pts',(-62.8653481645824,16.0919347801547,-71.5400606036235));
#42830=CARTESIAN_POINT('Ctrl Pts',(-62.8656690400584,16.4219330456641,-72.1627921270539));
#42831=CARTESIAN_POINT('Ctrl Pts',(-62.8657833950704,16.8209833597187,-72.9134781492287));
#42832=CARTESIAN_POINT('Ctrl Pts',(-62.8660354724408,17.620487045096,-74.4139670314268));
#42833=CARTESIAN_POINT('Ctrl Pts',(-62.8659980621607,18.2903711348304,-75.6668055103832));
#42834=CARTESIAN_POINT('Ctrl Pts',(-62.8657332857691,19.2620837088665,-77.494192794518));
#42835=CARTESIAN_POINT('Ctrl Pts',(-62.8658483368064,19.697783753344,-78.3134884153658));
#42836=CARTESIAN_POINT('Ctrl Pts',(-62.8658483368066,20.1343053407335,-79.1344661174665));
#42837=CARTESIAN_POINT('Ctrl Pts',(-61.1951504763405,6.62458514109144,24.8301509583975));
#42838=CARTESIAN_POINT('Ctrl Pts',(-61.1953568465687,6.62460289413373,24.7812567470511));
#42839=CARTESIAN_POINT('Ctrl Pts',(-61.1955732470009,6.62462155064825,24.7323633371));
#42840=CARTESIAN_POINT('Ctrl Pts',(-61.1981287247375,6.62484065059862,24.1815793110815));
#42841=CARTESIAN_POINT('Ctrl Pts',(-61.2005612044126,6.62486564311747,23.1773121540749));
#42842=CARTESIAN_POINT('Ctrl Pts',(-61.2065292919888,6.624845624491,21.1683493771042));
#42843=CARTESIAN_POINT('Ctrl Pts',(-61.2235178549665,6.62630144191226,19.6639204589936));
#42844=CARTESIAN_POINT('Ctrl Pts',(-61.2571829939099,6.63009485789897,18.4126497901983));
#42845=CARTESIAN_POINT('Ctrl Pts',(-61.2735182517976,6.63178904822752,17.9085919333625));
#42846=CARTESIAN_POINT('Ctrl Pts',(-61.3148582396206,6.63582087133403,16.9037625251246));
#42847=CARTESIAN_POINT('Ctrl Pts',(-61.4034039595603,6.64442515136615,15.1503355737336));
#42848=CARTESIAN_POINT('Ctrl Pts',(-61.4846424691607,6.65419630033967,13.6525696721531));
#42849=CARTESIAN_POINT('Ctrl Pts',(-61.5303696538949,6.66322521494574,12.4030927090508));
#42850=CARTESIAN_POINT('Ctrl Pts',(-61.5484916289262,6.66723912559534,11.9041681631621));
#42851=CARTESIAN_POINT('Ctrl Pts',(-61.5835940410652,6.6764350674265,10.9051885064317));
#42852=CARTESIAN_POINT('Ctrl Pts',(-61.6242295358563,6.68936722404817,9.65433962806701));
#42853=CARTESIAN_POINT('Ctrl Pts',(-61.6643034346199,6.70437569936267,8.14919086030427));
#42854=CARTESIAN_POINT('Ctrl Pts',(-61.6828526508977,6.71238820862013,7.14227280148821));
#42855=CARTESIAN_POINT('Ctrl Pts',(-61.691153893495,6.71622150470251,6.5125725955013));
#42856=CARTESIAN_POINT('Ctrl Pts',(-61.693975656162,6.71774731565301,6.26365110309824));
#42857=CARTESIAN_POINT('Ctrl Pts',(-61.6979000775793,6.72081792898549,5.76357738792179));
#42858=CARTESIAN_POINT('Ctrl Pts',(-61.7007460307582,6.72610541865317,4.88660297529398));
#42859=CARTESIAN_POINT('Ctrl Pts',(-61.6943584373772,6.73552427919849,3.12430421344482));
#42860=CARTESIAN_POINT('Ctrl Pts',(-61.6817135425056,6.73863874741957,1.60931204378402));
#42861=CARTESIAN_POINT('Ctrl Pts',(-61.6813928422738,6.73535180835137,0.537771163006079));
#42862=CARTESIAN_POINT('Ctrl Pts',(-61.6816981518373,6.73411327655994,0.3912714579851));
#42863=CARTESIAN_POINT('Ctrl Pts',(-61.68350649646,6.72869968547698,0.112541836839732));
#42864=CARTESIAN_POINT('Ctrl Pts',(-61.6894870030561,6.71240579224838,-0.372452970662816));
#42865=CARTESIAN_POINT('Ctrl Pts',(-61.7040975329937,6.67465326445107,-1.03804543785192));
#42866=CARTESIAN_POINT('Ctrl Pts',(-61.7253695647143,6.62146645629319,-1.80065539383669));
#42867=CARTESIAN_POINT('Ctrl Pts',(-61.7512793681603,6.55718283441924,-2.76679751972595));
#42868=CARTESIAN_POINT('Ctrl Pts',(-61.7656676096798,6.52083721095943,-3.88195177421976));
#42869=CARTESIAN_POINT('Ctrl Pts',(-61.7289403580524,6.58491345336716,-4.67530859774312));
#42870=CARTESIAN_POINT('Ctrl Pts',(-61.6838248946664,6.66300030427892,-5.14929721479892));
#42871=CARTESIAN_POINT('Ctrl Pts',(-61.6616341867744,6.70028622946335,-5.35061029919009));
#42872=CARTESIAN_POINT('Ctrl Pts',(-61.6045172022772,6.7892304110016,-5.7591672929034));
#42873=CARTESIAN_POINT('Ctrl Pts',(-61.4763898493465,6.98344413109923,-6.50509413113006));
#42874=CARTESIAN_POINT('Ctrl Pts',(-61.2473833659582,7.35409788266046,-7.64876931607059));
#42875=CARTESIAN_POINT('Ctrl Pts',(-61.0314320905569,7.81239046287047,-8.88225427570305));
#42876=CARTESIAN_POINT('Ctrl Pts',(-60.9163069811461,8.15953579844562,-9.77881172773552));
#42877=CARTESIAN_POINT('Ctrl Pts',(-60.8648618014957,8.3625242399895,-10.2991416545444));
#42878=CARTESIAN_POINT('Ctrl Pts',(-60.8446197878516,8.46523082053907,-10.5621314670901));
#42879=CARTESIAN_POINT('Ctrl Pts',(-60.8319172356274,8.54249578079412,-10.7601506448152));
#42880=CARTESIAN_POINT('Ctrl Pts',(-60.8294089355775,8.58445045011968,-10.8601835508611));
#42881=CARTESIAN_POINT('Ctrl Pts',(-60.8233475986099,8.68113721341898,-11.0821155945678));
#42882=CARTESIAN_POINT('Ctrl Pts',(-60.8191264510034,8.8622819506804,-11.4681317840093));
#42883=CARTESIAN_POINT('Ctrl Pts',(-60.825787087303,9.27900712280218,-12.2749049213649));
#42884=CARTESIAN_POINT('Ctrl Pts',(-60.8669206700503,9.97125551368284,-13.500531742468));
#42885=CARTESIAN_POINT('Ctrl Pts',(-60.9181470813914,10.5940713881071,-14.718901355251));
#42886=CARTESIAN_POINT('Ctrl Pts',(-60.9479815065831,10.9531558728833,-15.5960065118785));
#42887=CARTESIAN_POINT('Ctrl Pts',(-60.9654189278638,11.1726665720368,-16.1996779621415));
#42888=CARTESIAN_POINT('Ctrl Pts',(-60.9746669874423,11.3096398470889,-16.6748462364098));
#42889=CARTESIAN_POINT('Ctrl Pts',(-60.9784506935739,11.4013262488943,-17.0829887398642));
#42890=CARTESIAN_POINT('Ctrl Pts',(-60.9801153713349,11.4346064335128,-17.2394831842584));
#42891=CARTESIAN_POINT('Ctrl Pts',(-60.9835406317571,11.493183293384,-17.5530226881813));
#42892=CARTESIAN_POINT('Ctrl Pts',(-60.987154044757,11.5395859846949,-17.8619590869959));
#42893=CARTESIAN_POINT('Ctrl Pts',(-60.9907599742485,11.57555857648,-18.1673057259696));
#42894=CARTESIAN_POINT('Ctrl Pts',(-60.9930021503445,11.5939322244607,-18.3562342522241));
#42895=CARTESIAN_POINT('Ctrl Pts',(-60.9947717812819,11.6063715025536,-18.506301898915));
#42896=CARTESIAN_POINT('Ctrl Pts',(-60.996086104167,11.6146094490627,-18.6182731242901));
#42897=CARTESIAN_POINT('Ctrl Pts',(-60.9971686866792,11.6206033299365,-18.7111110077954));
#42898=CARTESIAN_POINT('Ctrl Pts',(-60.9980252446697,11.6249001658783,-18.7850844415051));
#42899=CARTESIAN_POINT('Ctrl Pts',(-61.0052655975391,11.658615375535,-19.4122754252571));
#42900=CARTESIAN_POINT('Ctrl Pts',(-61.0171580558027,11.6384378193482,-20.5586059913791));
#42901=CARTESIAN_POINT('Ctrl Pts',(-61.0268905636031,11.5302210404426,-22.0960107426974));
#42902=CARTESIAN_POINT('Ctrl Pts',(-61.0308003746837,11.4889047680634,-23.0205296925236));
#42903=CARTESIAN_POINT('Ctrl Pts',(-61.034268841733,11.4915868109434,-23.5669959069628));
#42904=CARTESIAN_POINT('Ctrl Pts',(-61.0354944060958,11.4926254194423,-23.8278637947768));
#42905=CARTESIAN_POINT('Ctrl Pts',(-61.0374774564534,11.4939939440805,-24.3248640057824));
#42906=CARTESIAN_POINT('Ctrl Pts',(-61.0397977550119,11.4949749112046,-25.2083710153304));
#42907=CARTESIAN_POINT('Ctrl Pts',(-61.0404249912444,11.4932218000262,-26.4644076265833));
#42908=CARTESIAN_POINT('Ctrl Pts',(-61.0387164910498,11.4895162222653,-27.9742630599744));
#42909=CARTESIAN_POINT('Ctrl Pts',(-61.0372248727665,11.4881938993359,-28.9760342398299));
#42910=CARTESIAN_POINT('Ctrl Pts',(-61.0366487955333,11.4884173372713,-29.537966544389));
#42911=CARTESIAN_POINT('Ctrl Pts',(-61.0364980446522,11.4884760063778,-29.6632426016537));
#42912=CARTESIAN_POINT('Ctrl Pts',(-61.0361127406127,11.4886160154417,-29.9136400903341));
#42913=CARTESIAN_POINT('Ctrl Pts',(-61.0352348851594,11.4889209698375,-30.3521843141996));
#42914=CARTESIAN_POINT('Ctrl Pts',(-61.0327943604326,11.4897472430984,-31.2298741115997));
#42915=CARTESIAN_POINT('Ctrl Pts',(-61.0280955236478,11.4914170504487,-32.4850496433206));
#42916=CARTESIAN_POINT('Ctrl Pts',(-61.0237560037054,11.4933884105369,-33.7398705006316));
#42917=CARTESIAN_POINT('Ctrl Pts',(-61.0216795012927,11.494928498429,-34.7422088794976));
#42918=CARTESIAN_POINT('Ctrl Pts',(-61.0213039587799,11.4956447572322,-35.2427959475687));
#42919=CARTESIAN_POINT('Ctrl Pts',(-61.0213443437813,11.4961496164705,-35.6188862471038));
#42920=CARTESIAN_POINT('Ctrl Pts',(-61.0214713523777,11.4964756971778,-35.8707395448149));
#42921=CARTESIAN_POINT('Ctrl Pts',(-61.0220817752789,11.4970873720578,-36.3736956800009));
#42922=CARTESIAN_POINT('Ctrl Pts',(-61.0239730980735,11.4980814232848,-37.2522838368669));
#42923=CARTESIAN_POINT('Ctrl Pts',(-61.0301360530368,11.49996694904,-39.0044607649581));
#42924=CARTESIAN_POINT('Ctrl Pts',(-61.0363929751217,11.5021747951859,-40.5049056867621));
#42925=CARTESIAN_POINT('Ctrl Pts',(-61.038688280218,11.5051403709043,-41.7597005904433));
#42926=CARTESIAN_POINT('Ctrl Pts',(-61.0391158413235,11.5055189117883,-42.1382542681091));
#42927=CARTESIAN_POINT('Ctrl Pts',(-61.0393328711263,11.5054108475311,-42.6406427225632));
#42928=CARTESIAN_POINT('Ctrl Pts',(-61.0393667119375,11.5050396412129,-43.143267376347));
#42929=CARTESIAN_POINT('Ctrl Pts',(-61.0391643540375,11.5043394908254,-43.7706474579098));
#42930=CARTESIAN_POINT('Ctrl Pts',(-61.0388463115252,11.5039544201184,-44.522038933998));
#42931=CARTESIAN_POINT('Ctrl Pts',(-61.0387830075111,11.5047001916358,-45.1463845156248));
#42932=CARTESIAN_POINT('Ctrl Pts',(-61.0390122327925,11.5063391844499,-45.6445644550148));
#42933=CARTESIAN_POINT('Ctrl Pts',(-61.0393640958474,11.5081942047304,-46.0174606131328));
#42934=CARTESIAN_POINT('Ctrl Pts',(-61.039935717522,11.5107763740768,-46.389583419531));
#42935=CARTESIAN_POINT('Ctrl Pts',(-61.0410444943961,11.5153183312048,-46.8845472445286));
#42936=CARTESIAN_POINT('Ctrl Pts',(-61.0423253344689,11.5201259784132,-47.2545104306091));
#42937=CARTESIAN_POINT('Ctrl Pts',(-61.0439915921777,11.5260610428822,-47.6238803016604));
#42938=CARTESIAN_POINT('Ctrl Pts',(-61.0452133055278,11.5311901476113,-47.8583558760436));
#42939=CARTESIAN_POINT('Ctrl Pts',(-61.0479070618055,11.5462780632115,-48.3401315118095));
#42940=CARTESIAN_POINT('Ctrl Pts',(-61.0532747093371,11.5828405598515,-49.191698673183));
#42941=CARTESIAN_POINT('Ctrl Pts',(-61.0624582839014,11.6520091930191,-50.4463827362363));
#42942=CARTESIAN_POINT('Ctrl Pts',(-61.0755553226412,11.7179771546967,-52.0063311577792));
#42943=CARTESIAN_POINT('Ctrl Pts',(-61.0859180795864,11.7178710496722,-53.0838827351573));
#42944=CARTESIAN_POINT('Ctrl Pts',(-61.0931759356651,11.6924606284119,-53.7713808569349));
#42945=CARTESIAN_POINT('Ctrl Pts',(-61.0965679740002,11.6755941460017,-54.0770527297992));
#42946=CARTESIAN_POINT('Ctrl Pts',(-61.1041373840954,11.6248246767352,-54.6557013892285));
#42947=CARTESIAN_POINT('Ctrl Pts',(-61.1188310121637,11.5008416036265,-55.6380514548762));
#42948=CARTESIAN_POINT('Ctrl Pts',(-61.1497851147588,11.1836495777128,-57.4462530429054));
#42949=CARTESIAN_POINT('Ctrl Pts',(-61.1670666897246,11.0216150152346,-58.7333503102741));
#42950=CARTESIAN_POINT('Ctrl Pts',(-61.1785196927827,11.0690156598972,-59.4972166156187));
#42951=CARTESIAN_POINT('Ctrl Pts',(-61.1797324035572,11.0766436804769,-59.610460938086));
#42952=CARTESIAN_POINT('Ctrl Pts',(-61.1821470349915,11.0943661075029,-59.826407298789));
#42953=CARTESIAN_POINT('Ctrl Pts',(-61.1860750911724,11.1336747416495,-60.2121792687574));
#42954=CARTESIAN_POINT('Ctrl Pts',(-61.1929940783206,11.2430043968676,-60.9875884813146));
#42955=CARTESIAN_POINT('Ctrl Pts',(-61.1988897348787,11.434166518421,-61.8925697160505));
#42956=CARTESIAN_POINT('Ctrl Pts',(-61.203454845895,11.6805800342668,-62.8071635715259));
#42957=CARTESIAN_POINT('Ctrl Pts',(-61.2056875777563,11.8375844710509,-63.3247444139147));
#42958=CARTESIAN_POINT('Ctrl Pts',(-61.207106559886,11.9489372873714,-63.6704701734733));
#42959=CARTESIAN_POINT('Ctrl Pts',(-61.2080390043346,12.0248867410563,-63.9011501929878));
#42960=CARTESIAN_POINT('Ctrl Pts',(-61.2089631312672,12.1032736056746,-64.1319359786747));
#42961=CARTESIAN_POINT('Ctrl Pts',(-61.2097731523333,12.1738481359528,-64.3340303511605));
#42962=CARTESIAN_POINT('Ctrl Pts',(-61.2102387008837,12.2147154843522,-64.4495366347599));
#42963=CARTESIAN_POINT('Ctrl Pts',(-61.2109422345935,12.2765315348749,-64.6227876819708));
#42964=CARTESIAN_POINT('Ctrl Pts',(-61.2115365416596,12.3291249368404,-64.7672181703169));
#42965=CARTESIAN_POINT('Ctrl Pts',(-61.2125793523105,12.4172299066177,-65.0056862298864));
#42966=CARTESIAN_POINT('Ctrl Pts',(-61.2153652508937,12.5001132674356,-65.218606727214));
#42967=CARTESIAN_POINT('Ctrl Pts',(-61.2196064879568,12.689457605908,-65.6686332701946));
#42968=CARTESIAN_POINT('Ctrl Pts',(-61.2264901285657,13.0580281190058,-66.4581561128385));
#42969=CARTESIAN_POINT('Ctrl Pts',(-61.2346767188754,13.9381728298099,-68.0971536023905));
#42970=CARTESIAN_POINT('Ctrl Pts',(-61.2318869813096,14.8361779057614,-69.5916616377109));
#42971=CARTESIAN_POINT('Ctrl Pts',(-61.2264190170371,15.4676581624523,-70.7931013307634));
#42972=CARTESIAN_POINT('Ctrl Pts',(-61.226897358886,15.5965462230223,-71.0376566986305));
#42973=CARTESIAN_POINT('Ctrl Pts',(-61.2268607544551,15.8618963803404,-71.540173633185));
#42974=CARTESIAN_POINT('Ctrl Pts',(-61.2271831423561,16.191895854752,-72.1629057961627));
#42975=CARTESIAN_POINT('Ctrl Pts',(-61.2272982744814,16.5909466691714,-72.9135921473858));
#42976=CARTESIAN_POINT('Ctrl Pts',(-61.2275535433326,17.3904512539708,-74.414081485479));
#42977=CARTESIAN_POINT('Ctrl Pts',(-61.2275189123817,18.0603357245619,-75.6669197390852));
#42978=CARTESIAN_POINT('Ctrl Pts',(-61.2272523446541,19.0320477916089,-77.4943063972569));
#42979=CARTESIAN_POINT('Ctrl Pts',(-61.2273683371954,19.4677484205143,-78.3136022825405));
#42980=CARTESIAN_POINT('Ctrl Pts',(-61.2273683371965,19.9042700079039,-79.1345799846401));
#42981=CARTESIAN_POINT('Ctrl Pts',(-58.8531122166346,6.29125272644766,24.8311203649996));
#42982=CARTESIAN_POINT('Ctrl Pts',(-58.8532961937455,6.29129086286412,24.7822564017764));
#42983=CARTESIAN_POINT('Ctrl Pts',(-58.8534891349777,6.29133083864146,24.7333938104296));
#42984=CARTESIAN_POINT('Ctrl Pts',(-58.8557674938895,6.29180286160571,24.1829644323862));
#42985=CARTESIAN_POINT('Ctrl Pts',(-58.8576561439393,6.29245164919413,23.1790663946222));
#42986=CARTESIAN_POINT('Ctrl Pts',(-58.8621437037072,6.29414891037338,21.1707766206951));
#42987=CARTESIAN_POINT('Ctrl Pts',(-58.8773005334509,6.29727974088763,19.6666102910973));
#42988=CARTESIAN_POINT('Ctrl Pts',(-58.9087343097988,6.30248678381129,18.4155063967086));
#42989=CARTESIAN_POINT('Ctrl Pts',(-58.9239208629026,6.30506753822643,17.9134491475579));
#42990=CARTESIAN_POINT('Ctrl Pts',(-58.9622603778399,6.31167889478455,16.9100151317855));
#42991=CARTESIAN_POINT('Ctrl Pts',(-59.0445014771969,6.32575615580128,15.156267729807));
#42992=CARTESIAN_POINT('Ctrl Pts',(-59.121227022368,6.33770163219755,13.6520274439723));
#42993=CARTESIAN_POINT('Ctrl Pts',(-59.1666781482765,6.34266844612933,12.3942057487324));
#42994=CARTESIAN_POINT('Ctrl Pts',(-59.1849569030176,6.34440140556946,11.8918622480249));
#42995=CARTESIAN_POINT('Ctrl Pts',(-59.2212603198012,6.34698803383082,10.887944920771));
#42996=CARTESIAN_POINT('Ctrl Pts',(-59.264744899169,6.34880576241689,9.63375633357624));
#42997=CARTESIAN_POINT('Ctrl Pts',(-59.309280904769,6.34943935722079,8.1292838841226));
#42998=CARTESIAN_POINT('Ctrl Pts',(-59.33080531134,6.3492938089834,7.12580691947219));
#42999=CARTESIAN_POINT('Ctrl Pts',(-59.3407250943735,6.34917190545594,6.49905229246299));
#43000=CARTESIAN_POINT('Ctrl Pts',(-59.344257855347,6.34902412143873,6.24814730896979));
#43001=CARTESIAN_POINT('Ctrl Pts',(-59.3497871505297,6.34837358937043,5.74656716465428));
#43002=CARTESIAN_POINT('Ctrl Pts',(-59.3558335964775,6.34644962358975,4.86753800339333));
#43003=CARTESIAN_POINT('Ctrl Pts',(-59.3564368234274,6.3407682801717,3.10841465155978));
#43004=CARTESIAN_POINT('Ctrl Pts',(-59.3481217387933,6.33680373878316,1.6064410335573));
#43005=CARTESIAN_POINT('Ctrl Pts',(-59.3485867412118,6.33898133936188,0.550249730022763));
#43006=CARTESIAN_POINT('Ctrl Pts',(-59.3488632899375,6.3388493940282,0.412544918647314));
#43007=CARTESIAN_POINT('Ctrl Pts',(-59.3502551323157,6.33706032033583,0.146038796302226));
#43008=CARTESIAN_POINT('Ctrl Pts',(-59.354636133616,6.33045187856548,-0.318799356198402));
#43009=CARTESIAN_POINT('Ctrl Pts',(-59.365101533094,6.31366265886565,-0.966398103144115));
#43010=CARTESIAN_POINT('Ctrl Pts',(-59.3800454526428,6.28976423518019,-1.72136052089009));
#43011=CARTESIAN_POINT('Ctrl Pts',(-59.3975400810526,6.26260085226075,-2.69704581639326));
#43012=CARTESIAN_POINT('Ctrl Pts',(-59.40450084396,6.2551724004228,-3.86020427199859));
#43013=CARTESIAN_POINT('Ctrl Pts',(-59.3732913183919,6.3105225319854,-4.7330162397558));
#43014=CARTESIAN_POINT('Ctrl Pts',(-59.3363236294509,6.3728634900837,-5.26471278144059));
#43015=CARTESIAN_POINT('Ctrl Pts',(-59.3183051330271,6.40277469599597,-5.50590057745168));
#43016=CARTESIAN_POINT('Ctrl Pts',(-59.2730143834109,6.46462282018107,-5.97073531772149));
#43017=CARTESIAN_POINT('Ctrl Pts',(-59.1724437406644,6.58512407701506,-6.78935181889418));
#43018=CARTESIAN_POINT('Ctrl Pts',(-58.9912299422981,6.78668033438211,-7.94607044258143));
#43019=CARTESIAN_POINT('Ctrl Pts',(-58.8223505883216,7.04768916551194,-9.1021062641336));
#43020=CARTESIAN_POINT('Ctrl Pts',(-58.7357216700054,7.28298798145105,-9.90635334776788));
#43021=CARTESIAN_POINT('Ctrl Pts',(-58.6977514493031,7.43538440915907,-10.3634137229407));
#43022=CARTESIAN_POINT('Ctrl Pts',(-58.6830441212754,7.51808105230493,-10.5911200580965));
#43023=CARTESIAN_POINT('Ctrl Pts',(-58.6738673485026,7.58258871876441,-10.7612008946215));
#43024=CARTESIAN_POINT('Ctrl Pts',(-58.6723385105303,7.61730140285522,-10.8454011907547));
#43025=CARTESIAN_POINT('Ctrl Pts',(-58.6676698986058,7.70231098946049,-11.0380112045874));
#43026=CARTESIAN_POINT('Ctrl Pts',(-58.6622822535284,7.87155800820933,-11.3815799766734));
#43027=CARTESIAN_POINT('Ctrl Pts',(-58.6531466112637,8.29798633581786,-12.130872232531));
#43028=CARTESIAN_POINT('Ctrl Pts',(-58.6342749136415,9.08897227873553,-13.3224838570275));
#43029=CARTESIAN_POINT('Ctrl Pts',(-58.6087950344317,9.85805749859873,-14.533148519742));
#43030=CARTESIAN_POINT('Ctrl Pts',(-58.5920541257189,10.3189466513491,-15.4242509616649));
#43031=CARTESIAN_POINT('Ctrl Pts',(-58.5811013201179,10.605186759511,-16.0451898751326));
#43032=CARTESIAN_POINT('Ctrl Pts',(-58.573432142254,10.7884568267168,-16.5447992998918));
#43033=CARTESIAN_POINT('Ctrl Pts',(-58.5676883080846,10.9110470070739,-16.9819084772538));
#43034=CARTESIAN_POINT('Ctrl Pts',(-58.5665924615939,10.9530157283704,-17.1389394785022));
#43035=CARTESIAN_POINT('Ctrl Pts',(-58.565186039239,11.0297212299339,-17.4603156750021));
#43036=CARTESIAN_POINT('Ctrl Pts',(-58.5657292503271,11.0918059668326,-17.775045312381));
#43037=CARTESIAN_POINT('Ctrl Pts',(-58.567631299581,11.1421440428145,-18.0875252669167));
#43038=CARTESIAN_POINT('Ctrl Pts',(-58.5693893143105,11.1687320979712,-18.2806147809453));
#43039=CARTESIAN_POINT('Ctrl Pts',(-58.5710784518379,11.1873827163689,-18.4340835752316));
#43040=CARTESIAN_POINT('Ctrl Pts',(-58.5724843464094,11.200079791777,-18.5485545419872));
#43041=CARTESIAN_POINT('Ctrl Pts',(-58.5737628074572,11.209637864024,-18.6434639623201));
#43042=CARTESIAN_POINT('Ctrl Pts',(-58.5748447036218,11.2166942132934,-18.7190720981452));
#43043=CARTESIAN_POINT('Ctrl Pts',(-58.5843889835097,11.2733702537564,-19.3600989807476));
#43044=CARTESIAN_POINT('Ctrl Pts',(-58.6122679980678,11.2811842135818,-20.5287343569894));
#43045=CARTESIAN_POINT('Ctrl Pts',(-58.6549092938124,11.1939846227444,-22.0800671830156));
#43046=CARTESIAN_POINT('Ctrl Pts',(-58.6746892880707,11.1633058977298,-23.002056987914));
#43047=CARTESIAN_POINT('Ctrl Pts',(-58.6822095587603,11.1727610649111,-23.5434804899239));
#43048=CARTESIAN_POINT('Ctrl Pts',(-58.684825910602,11.1767772453322,-23.8089158323289));
#43049=CARTESIAN_POINT('Ctrl Pts',(-58.68921806134,11.1825691191453,-24.3107277047849));
#43050=CARTESIAN_POINT('Ctrl Pts',(-58.6946743015338,11.1886601066525,-25.2031527090417));
#43051=CARTESIAN_POINT('Ctrl Pts',(-58.6972904418314,11.1878390504411,-26.4667907242899));
#43052=CARTESIAN_POINT('Ctrl Pts',(-58.695550935967,11.1802721927887,-27.9803331897321));
#43053=CARTESIAN_POINT('Ctrl Pts',(-58.6934375254854,11.1762187286891,-28.9803097901365));
#43054=CARTESIAN_POINT('Ctrl Pts',(-58.6926044024015,11.1757358086309,-29.5402059986131));
#43055=CARTESIAN_POINT('Ctrl Pts',(-58.6923786527866,11.175608118668,-29.6661970306196));
#43056=CARTESIAN_POINT('Ctrl Pts',(-58.691777738781,11.1752918400781,-29.9173102175387));
#43057=CARTESIAN_POINT('Ctrl Pts',(-58.6903597777594,11.1745838716585,-30.3573160737653));
#43058=CARTESIAN_POINT('Ctrl Pts',(-58.6862628275566,11.1726237782499,-31.2371633439593));
#43059=CARTESIAN_POINT('Ctrl Pts',(-58.6779893478998,11.1687102067029,-32.4941329293564));
#43060=CARTESIAN_POINT('Ctrl Pts',(-58.6696472868024,11.1644713794661,-33.7487245447044));
#43061=CARTESIAN_POINT('Ctrl Pts',(-58.6648294286161,11.1616084609084,-34.7497194105669));
#43062=CARTESIAN_POINT('Ctrl Pts',(-58.6633592706326,11.1604912904934,-35.2492446389077));
#43063=CARTESIAN_POINT('Ctrl Pts',(-58.6627234813872,11.1598108101496,-35.6244021496755));
#43064=CARTESIAN_POINT('Ctrl Pts',(-58.6624116018931,11.1593550428197,-35.876299419224));
#43065=CARTESIAN_POINT('Ctrl Pts',(-58.6621968791146,11.1584502265351,-36.3789602469091));
#43066=CARTESIAN_POINT('Ctrl Pts',(-58.6627792456753,11.1569364021083,-37.2572338064125));
#43067=CARTESIAN_POINT('Ctrl Pts',(-58.666775291758,11.1543027159659,-39.0085851302233));
#43068=CARTESIAN_POINT('Ctrl Pts',(-58.6717281129795,11.1535635448823,-40.5083721509013));
#43069=CARTESIAN_POINT('Ctrl Pts',(-58.6729665323629,11.1545275425125,-41.7625315481145));
#43070=CARTESIAN_POINT('Ctrl Pts',(-58.6730633843322,11.1543158533502,-42.1409928886693));
#43071=CARTESIAN_POINT('Ctrl Pts',(-58.6728300965074,11.1534692046473,-42.6431728214892));
#43072=CARTESIAN_POINT('Ctrl Pts',(-58.672416217241,11.152397036243,-43.145586346829));
#43073=CARTESIAN_POINT('Ctrl Pts',(-58.6716732984394,11.1509008480668,-43.7726642904261));
#43074=CARTESIAN_POINT('Ctrl Pts',(-58.6707842528653,11.1497187299375,-44.5236476183902));
#43075=CARTESIAN_POINT('Ctrl Pts',(-58.6703490091193,11.1499572785657,-45.1476122395524));
#43076=CARTESIAN_POINT('Ctrl Pts',(-58.6703668830272,11.1512972489388,-45.6454579126515));
#43077=CARTESIAN_POINT('Ctrl Pts',(-58.6706090718571,11.1529859202588,-46.0180910572761));
#43078=CARTESIAN_POINT('Ctrl Pts',(-58.6711257361361,11.1554629271224,-46.3899382025871));
#43079=CARTESIAN_POINT('Ctrl Pts',(-58.6722425500054,11.1599519212778,-46.8845154608703));
#43080=CARTESIAN_POINT('Ctrl Pts',(-58.6736282575498,11.1648205689537,-47.2541720644948));
#43081=CARTESIAN_POINT('Ctrl Pts',(-58.6754793287284,11.1708942736337,-47.6232145606296));
#43082=CARTESIAN_POINT('Ctrl Pts',(-58.6768511114755,11.1761435241196,-47.8573713658892));
#43083=CARTESIAN_POINT('Ctrl Pts',(-58.6799285636696,11.1915943224041,-48.3386218652533));
#43084=CARTESIAN_POINT('Ctrl Pts',(-58.6861752653204,11.2290893717988,-49.1893687745462));
#43085=CARTESIAN_POINT('Ctrl Pts',(-58.697103456101,11.3002976745431,-50.4432603072607));
#43086=CARTESIAN_POINT('Ctrl Pts',(-58.7128525538229,11.3694293772098,-52.0028309595));
#43087=CARTESIAN_POINT('Ctrl Pts',(-58.7252359840649,11.3714960879605,-53.0805742291338));
#43088=CARTESIAN_POINT('Ctrl Pts',(-58.7338122345408,11.3473454802483,-53.7683279890051));
#43089=CARTESIAN_POINT('Ctrl Pts',(-58.7377772621395,11.3310806389284,-54.0736961880198));
#43090=CARTESIAN_POINT('Ctrl Pts',(-58.7466365080233,11.2815592954844,-54.6520733062992));
#43091=CARTESIAN_POINT('Ctrl Pts',(-58.7638898698218,11.1598900367289,-55.6340505101549));
#43092=CARTESIAN_POINT('Ctrl Pts',(-58.8006108123127,10.8473623013647,-57.4422974072245));
#43093=CARTESIAN_POINT('Ctrl Pts',(-58.8224914382479,10.6879749092258,-58.7303365344381));
#43094=CARTESIAN_POINT('Ctrl Pts',(-58.835594620721,10.7363280185413,-59.4957081676448));
#43095=CARTESIAN_POINT('Ctrl Pts',(-58.836993637099,10.74408270014,-59.6091141407841));
#43096=CARTESIAN_POINT('Ctrl Pts',(-58.8397436281837,10.7620211453917,-59.8253766905018));
#43097=CARTESIAN_POINT('Ctrl Pts',(-58.8441588137794,10.8016412372195,-60.211651793111));
#43098=CARTESIAN_POINT('Ctrl Pts',(-58.8516989619916,10.9113266438308,-60.9878888234346));
#43099=CARTESIAN_POINT('Ctrl Pts',(-58.857685494782,11.1023842020238,-61.8934033624564));
#43100=CARTESIAN_POINT('Ctrl Pts',(-58.8620921377479,11.3484146029664,-62.8081655158882));
#43101=CARTESIAN_POINT('Ctrl Pts',(-58.864207460578,11.5051532444805,-63.3257123652384));
#43102=CARTESIAN_POINT('Ctrl Pts',(-58.8655630123144,11.6163287818732,-63.6713635074078));
#43103=CARTESIAN_POINT('Ctrl Pts',(-58.8664588288894,11.6921620009195,-63.9019800687117));
#43104=CARTESIAN_POINT('Ctrl Pts',(-58.8673574433335,11.7704370207402,-64.132681988696));
#43105=CARTESIAN_POINT('Ctrl Pts',(-58.8681593124706,11.8409222518968,-64.3346849727148));
#43106=CARTESIAN_POINT('Ctrl Pts',(-58.8686248863825,11.8817415053248,-64.4501338510522));
#43107=CARTESIAN_POINT('Ctrl Pts',(-58.8693334710135,11.9434887627976,-64.6232937862657));
#43108=CARTESIAN_POINT('Ctrl Pts',(-58.8699430590789,11.9960318969489,-64.7676371916027));
#43109=CARTESIAN_POINT('Ctrl Pts',(-58.871029597124,12.0840685274892,-65.0059504080628));
#43110=CARTESIAN_POINT('Ctrl Pts',(-58.8738720353503,12.1669625240645,-65.2189057880762));
#43111=CARTESIAN_POINT('Ctrl Pts',(-58.8782013908965,12.3562848247715,-65.6688933557686));
#43112=CARTESIAN_POINT('Ctrl Pts',(-58.8852010805029,12.7248446653879,-66.4584080929237));
#43113=CARTESIAN_POINT('Ctrl Pts',(-58.8934536686832,13.6049626308997,-68.0973591656563));
#43114=CARTESIAN_POINT('Ctrl Pts',(-58.890514373704,14.5029599787097,-69.5918846190804));
#43115=CARTESIAN_POINT('Ctrl Pts',(-58.8849533524291,15.1344094051463,-70.7933411325163));
#43116=CARTESIAN_POINT('Ctrl Pts',(-58.8854371813811,15.2632950509403,-71.0378928237048));
#43117=CARTESIAN_POINT('Ctrl Pts',(-58.8853973597922,15.5286395211488,-71.5404069143742));
#43118=CARTESIAN_POINT('Ctrl Pts',(-58.8857230037312,15.8586354644087,-72.1631350728754));
#43119=CARTESIAN_POINT('Ctrl Pts',(-58.885839920841,16.2576846620882,-72.9138181502591));
#43120=CARTESIAN_POINT('Ctrl Pts',(-58.8861019161312,17.0571910976897,-74.4143027371218));
#43121=CARTESIAN_POINT('Ctrl Pts',(-58.88607217105,17.727083913447,-75.667144537146));
#43122=CARTESIAN_POINT('Ctrl Pts',(-58.8858010083843,18.6987988142781,-77.4945400537225));
#43123=CARTESIAN_POINT('Ctrl Pts',(-58.8859188984952,19.1344987773697,-78.3138342787722));
#43124=CARTESIAN_POINT('Ctrl Pts',(-58.8859188984958,19.5710203647592,-79.1348119808692));
#43125=CARTESIAN_POINT('Ctrl Pts',(-56.0538590718158,5.89164146497962,24.8309570990425));
#43126=CARTESIAN_POINT('Ctrl Pts',(-56.0540143435333,5.89167115080391,24.7820881194473));
#43127=CARTESIAN_POINT('Ctrl Pts',(-56.0541771996283,5.89170228701854,24.7332204878178));
#43128=CARTESIAN_POINT('Ctrl Pts',(-56.0561007201811,5.89206946163348,24.1827303638316));
#43129=CARTESIAN_POINT('Ctrl Pts',(-56.0573372933614,5.89246395895494,23.1786704198053));
#43130=CARTESIAN_POINT('Ctrl Pts',(-56.0600560331059,5.89346177619444,21.170311115581));
#43131=CARTESIAN_POINT('Ctrl Pts',(-56.0728696004135,5.89589831524976,19.6662389302259));
#43132=CARTESIAN_POINT('Ctrl Pts',(-56.1012331131985,5.9004995024897,18.4152736671248));
#43133=CARTESIAN_POINT('Ctrl Pts',(-56.1147456695187,5.90278092892602,17.91322278237));
#43134=CARTESIAN_POINT('Ctrl Pts',(-56.1485274863742,5.90865048676361,16.909741050075));
#43135=CARTESIAN_POINT('Ctrl Pts',(-56.2210518374978,5.92123437931685,15.1557159402556));
#43136=CARTESIAN_POINT('Ctrl Pts',(-56.291361507408,5.93222838507849,13.6513443862109));
#43137=CARTESIAN_POINT('Ctrl Pts',(-56.3379466536074,5.93725400977883,12.3936626189808));
#43138=CARTESIAN_POINT('Ctrl Pts',(-56.3572553596225,5.93910149189236,11.8914224813623));
#43139=CARTESIAN_POINT('Ctrl Pts',(-56.397483859715,5.94219627272114,10.8877548182249));
#43140=CARTESIAN_POINT('Ctrl Pts',(-56.4485258936853,5.94505574783066,9.63391126524183));
#43141=CARTESIAN_POINT('Ctrl Pts',(-56.5037743046481,5.94707303303974,8.12966173762822));
#43142=CARTESIAN_POINT('Ctrl Pts',(-56.5317925643883,5.94767327443603,7.1260044365657));
#43143=CARTESIAN_POINT('Ctrl Pts',(-56.5450396626367,5.94786054042254,6.49901900310903));
#43144=CARTESIAN_POINT('Ctrl Pts',(-56.5500709620272,5.94782861036557,6.24784413173467));
#43145=CARTESIAN_POINT('Ctrl Pts',(-56.5591807391264,5.94742917467341,5.74591614945796));
#43146=CARTESIAN_POINT('Ctrl Pts',(-56.5726632237092,5.94597989349818,4.86635060028145));
#43147=CARTESIAN_POINT('Ctrl Pts',(-56.5901175188842,5.94129391697758,3.10695664261026));
#43148=CARTESIAN_POINT('Ctrl Pts',(-56.5898844598564,5.93815909136145,1.6053077669838));
#43149=CARTESIAN_POINT('Ctrl Pts',(-56.5833252757848,5.94003526968791,0.551394948598051));
#43150=CARTESIAN_POINT('Ctrl Pts',(-56.5825457545805,5.94003663591684,0.41880487008954));
#43151=CARTESIAN_POINT('Ctrl Pts',(-56.580982321595,5.93914199528337,0.158963928055661));
#43152=CARTESIAN_POINT('Ctrl Pts',(-56.5781752073396,5.93553475454912,-0.294696734365856));
#43153=CARTESIAN_POINT('Ctrl Pts',(-56.5736488125126,5.92602527432297,-0.932811606764838));
#43154=CARTESIAN_POINT('Ctrl Pts',(-56.5663733399661,5.91247012088004,-1.68504842023479));
#43155=CARTESIAN_POINT('Ctrl Pts',(-56.5529361709947,5.89741962355672,-2.67010185783887));
#43156=CARTESIAN_POINT('Ctrl Pts',(-56.5267030388217,5.89541906210424,-3.86922662353056));
#43157=CARTESIAN_POINT('Ctrl Pts',(-56.4904512572469,5.93200810912679,-4.7959249042925));
#43158=CARTESIAN_POINT('Ctrl Pts',(-56.4616453953466,5.97256296933579,-5.36841310784015));
#43159=CARTESIAN_POINT('Ctrl Pts',(-56.448551598945,5.99074380499537,-5.63975167835125));
#43160=CARTESIAN_POINT('Ctrl Pts',(-56.4190493601774,6.02058827887102,-6.14839873414667));
#43161=CARTESIAN_POINT('Ctrl Pts',(-56.3591263483878,6.06667792792076,-7.0278626699762));
#43162=CARTESIAN_POINT('Ctrl Pts',(-56.2580117170356,6.13756571361465,-8.20757162092261));
#43163=CARTESIAN_POINT('Ctrl Pts',(-56.1585687663277,6.27717431418544,-9.30115919905004));
#43164=CARTESIAN_POINT('Ctrl Pts',(-56.1031354938693,6.44040154776427,-10.0253960678308));
#43165=CARTESIAN_POINT('Ctrl Pts',(-56.0771896455893,6.55680114801948,-10.4300530054078));
#43166=CARTESIAN_POINT('Ctrl Pts',(-56.0663161167364,6.62353155550022,-10.6298104366514));
#43167=CARTESIAN_POINT('Ctrl Pts',(-56.0590770993462,6.67697368336153,-10.778573282487));
#43168=CARTESIAN_POINT('Ctrl Pts',(-56.0571992136534,6.70559636921108,-10.8520132861725));
#43169=CARTESIAN_POINT('Ctrl Pts',(-56.0515005149677,6.77917284717286,-11.0244204407004));
#43170=CARTESIAN_POINT('Ctrl Pts',(-56.0411345716577,6.93305537747737,-11.340343791566));
#43171=CARTESIAN_POINT('Ctrl Pts',(-56.011914768945,7.34958690420016,-12.0562955055699));
#43172=CARTESIAN_POINT('Ctrl Pts',(-55.9424747216657,8.1862460486787,-13.2319041224142));
#43173=CARTESIAN_POINT('Ctrl Pts',(-55.8608597038884,9.03453486786773,-14.4337444050702));
#43174=CARTESIAN_POINT('Ctrl Pts',(-55.8079568363992,9.55318525252669,-15.3235500042448));
#43175=CARTESIAN_POINT('Ctrl Pts',(-55.7740504317906,9.87883708879492,-15.9463018801817));
#43176=CARTESIAN_POINT('Ctrl Pts',(-55.7512662410359,10.0920056554103,-16.4518960126066));
#43177=CARTESIAN_POINT('Ctrl Pts',(-55.7359220297285,10.2374525790615,-16.8987888302202));
#43178=CARTESIAN_POINT('Ctrl Pts',(-55.7320689232897,10.2852545852319,-17.0517748945108));
#43179=CARTESIAN_POINT('Ctrl Pts',(-55.7251193981875,10.3761163494362,-17.3701681813707));
#43180=CARTESIAN_POINT('Ctrl Pts',(-55.7210961407007,10.4523015685782,-17.6808831787287));
#43181=CARTESIAN_POINT('Ctrl Pts',(-55.7191029346574,10.5175678738284,-17.9910276878221));
#43182=CARTESIAN_POINT('Ctrl Pts',(-55.7187684585226,10.5535306604547,-18.182771202428));
#43183=CARTESIAN_POINT('Ctrl Pts',(-55.7189610221274,10.5797643459227,-18.3354326496423));
#43184=CARTESIAN_POINT('Ctrl Pts',(-55.7193386864896,10.5981575542272,-18.4493730759027));
#43185=CARTESIAN_POINT('Ctrl Pts',(-55.719834105721,10.6124749611974,-18.5439261461873));
#43186=CARTESIAN_POINT('Ctrl Pts',(-55.7203345737224,10.6233387493865,-18.6192936042957));
#43187=CARTESIAN_POINT('Ctrl Pts',(-55.7251713925168,10.7123963481415,-19.2585240944519));
#43188=CARTESIAN_POINT('Ctrl Pts',(-55.7520250218645,10.7813072911956,-20.4319694878879));
#43189=CARTESIAN_POINT('Ctrl Pts',(-55.8032254818595,10.7625487878085,-22.0034771657111));
#43190=CARTESIAN_POINT('Ctrl Pts',(-55.8263661739389,10.7595625294605,-22.9457268569596));
#43191=CARTESIAN_POINT('Ctrl Pts',(-55.8329419755844,10.7812272868954,-23.5027977642127));
#43192=CARTESIAN_POINT('Ctrl Pts',(-55.8350007170921,10.7905800865703,-23.7745956206071));
#43193=CARTESIAN_POINT('Ctrl Pts',(-55.838224518375,10.8040442653164,-24.2876942535255));
#43194=CARTESIAN_POINT('Ctrl Pts',(-55.8413588798641,10.8183584472778,-25.1969624136924));
#43195=CARTESIAN_POINT('Ctrl Pts',(-55.8404949232791,10.8167877909337,-26.4759728986782));
#43196=CARTESIAN_POINT('Ctrl Pts',(-55.8360405173551,10.7998738602452,-27.9942653201028));
#43197=CARTESIAN_POINT('Ctrl Pts',(-55.8344655777984,10.7909493984571,-28.9881204599642));
#43198=CARTESIAN_POINT('Ctrl Pts',(-55.8350322006705,10.7900532279127,-29.5421574820583));
#43199=CARTESIAN_POINT('Ctrl Pts',(-55.8351543195557,10.7898179947142,-29.66907839006));
#43200=CARTESIAN_POINT('Ctrl Pts',(-55.8353793832605,10.7892186923991,-29.9207420642163));
#43201=CARTESIAN_POINT('Ctrl Pts',(-55.8357305677563,10.7878514107045,-30.3622249830816));
#43202=CARTESIAN_POINT('Ctrl Pts',(-55.8363226938693,10.7839957883729,-31.2440641162283));
#43203=CARTESIAN_POINT('Ctrl Pts',(-55.8371669269615,10.7762250372598,-32.502826336033));
#43204=CARTESIAN_POINT('Ctrl Pts',(-55.8388591106586,10.7678234114254,-33.7572186189596));
#43205=CARTESIAN_POINT('Ctrl Pts',(-55.841226804019,10.7620937741947,-34.7569628628096));
#43206=CARTESIAN_POINT('Ctrl Pts',(-55.8428227877759,10.7598001050066,-35.2554687285961));
#43207=CARTESIAN_POINT('Ctrl Pts',(-55.8442140874073,10.7583625563017,-35.6297323528476));
#43208=CARTESIAN_POINT('Ctrl Pts',(-55.8452512129642,10.7574031974616,-35.8816814900035));
#43209=CARTESIAN_POINT('Ctrl Pts',(-55.8476911991255,10.7555251923315,-36.3840681381157));
#43210=CARTESIAN_POINT('Ctrl Pts',(-55.8527753048416,10.7524095571393,-37.2620392783869));
#43211=CARTESIAN_POINT('Ctrl Pts',(-55.8651535433563,10.7468967612603,-39.012576118021));
#43212=CARTESIAN_POINT('Ctrl Pts',(-55.8758018000701,10.7443314436968,-40.5116970211463));
#43213=CARTESIAN_POINT('Ctrl Pts',(-55.8805818189657,10.7440559669415,-41.7652700730797));
#43214=CARTESIAN_POINT('Ctrl Pts',(-55.8816707004699,10.7434755783443,-42.1436749828539));
#43215=CARTESIAN_POINT('Ctrl Pts',(-55.8826253981071,10.742166861845,-42.6456815044681));
#43216=CARTESIAN_POINT('Ctrl Pts',(-55.883307740908,10.7406566540061,-43.1479163674791));
#43217=CARTESIAN_POINT('Ctrl Pts',(-55.8837622543073,10.7386623652207,-43.7747218600627));
#43218=CARTESIAN_POINT('Ctrl Pts',(-55.8840300940209,10.736978965313,-44.5253121513578));
#43219=CARTESIAN_POINT('Ctrl Pts',(-55.8843226463286,10.7368944092536,-45.1488873604603));
#43220=CARTESIAN_POINT('Ctrl Pts',(-55.8847786975065,10.7380347093961,-45.6463822046966));
#43221=CARTESIAN_POINT('Ctrl Pts',(-55.8852774009959,10.7396076611498,-46.0187333172631));
#43222=CARTESIAN_POINT('Ctrl Pts',(-55.8859781309581,10.742004341543,-46.3902795861577));
#43223=CARTESIAN_POINT('Ctrl Pts',(-55.8872418727823,10.7464351107409,-46.8844296309421));
#43224=CARTESIAN_POINT('Ctrl Pts',(-55.8886304800328,10.7513204207975,-47.2537390824915));
#43225=CARTESIAN_POINT('Ctrl Pts',(-55.8904071186326,10.7574518725442,-47.6224112719319));
#43226=CARTESIAN_POINT('Ctrl Pts',(-55.8916719305651,10.7627479026435,-47.8562235296186));
#43227=CARTESIAN_POINT('Ctrl Pts',(-55.8943472510965,10.7783554968543,-48.3369101694879));
#43228=CARTESIAN_POINT('Ctrl Pts',(-55.8994494045695,10.8162811003826,-49.1868020971753));
#43229=CARTESIAN_POINT('Ctrl Pts',(-55.9078479682809,10.8885388182956,-50.4399472811988));
#43230=CARTESIAN_POINT('Ctrl Pts',(-55.9200980636677,10.9594740604823,-51.999272177031));
#43231=CARTESIAN_POINT('Ctrl Pts',(-55.930488576419,10.9629006319631,-53.0772758084486));
#43232=CARTESIAN_POINT('Ctrl Pts',(-55.9381073316661,10.9395748779739,-53.7653056101449));
#43233=CARTESIAN_POINT('Ctrl Pts',(-55.9416528001124,10.9237215733015,-54.0704359512858));
#43234=CARTESIAN_POINT('Ctrl Pts',(-55.9496601025327,10.8750549527632,-54.6486009070764));
#43235=CARTESIAN_POINT('Ctrl Pts',(-55.9654123447332,10.7549969018306,-55.6302504324446));
#43236=CARTESIAN_POINT('Ctrl Pts',(-55.9994587470345,10.4458388026915,-57.4383823406074));
#43237=CARTESIAN_POINT('Ctrl Pts',(-56.0199533839382,10.2883173198432,-58.7272209294824));
#43238=CARTESIAN_POINT('Ctrl Pts',(-56.0326694572419,10.337296984968,-59.4940973816812));
#43239=CARTESIAN_POINT('Ctrl Pts',(-56.0340287334952,10.345141303396,-59.6076641521854));
#43240=CARTESIAN_POINT('Ctrl Pts',(-56.036730510265,10.3632314626706,-59.8242413083678));
#43241=CARTESIAN_POINT('Ctrl Pts',(-56.0411386361281,10.403075772758,-60.2110159317316));
#43242=CARTESIAN_POINT('Ctrl Pts',(-56.0489389363496,10.5130299230923,-60.9880655794156));
#43243=CARTESIAN_POINT('Ctrl Pts',(-56.0556792290518,10.7040268545881,-61.894066021176));
#43244=CARTESIAN_POINT('Ctrl Pts',(-56.0609547177322,10.9497591159132,-62.808920765965));
#43245=CARTESIAN_POINT('Ctrl Pts',(-56.0635408677761,11.106278666547,-63.326385277232));
#43246=CARTESIAN_POINT('Ctrl Pts',(-56.0651787688794,11.2173018142146,-63.6719298736204));
#43247=CARTESIAN_POINT('Ctrl Pts',(-56.0662527809051,11.2930332503178,-63.9024618429909));
#43248=CARTESIAN_POINT('Ctrl Pts',(-56.0673122919143,11.3712072941945,-64.133059681309));
#43249=CARTESIAN_POINT('Ctrl Pts',(-56.0682356952383,11.4416085466937,-64.3349546075141));
#43250=CARTESIAN_POINT('Ctrl Pts',(-56.0687646661073,11.4823814423657,-64.450336977776));
#43251=CARTESIAN_POINT('Ctrl Pts',(-56.0695619617873,11.544061119532,-64.6233925849231));
#43252=CARTESIAN_POINT('Ctrl Pts',(-56.0702317582838,11.5965520161077,-64.7676389886702));
#43253=CARTESIAN_POINT('Ctrl Pts',(-56.07139569208,11.6845120204599,-65.0057825717699));
#43254=CARTESIAN_POINT('Ctrl Pts',(-56.074264515776,11.767387288938,-65.2187502867463));
#43255=CARTESIAN_POINT('Ctrl Pts',(-56.0786397783873,11.9566422124607,-65.6686664407302));
#43256=CARTESIAN_POINT('Ctrl Pts',(-56.0856374180506,12.3251133559867,-66.4581304223345));
#43257=CARTESIAN_POINT('Ctrl Pts',(-56.09372093771,13.2051032634938,-68.0970024151852));
#43258=CARTESIAN_POINT('Ctrl Pts',(-56.0906321351764,14.1031093673489,-69.5915486423818));
#43259=CARTESIAN_POINT('Ctrl Pts',(-56.0851957454358,14.7345963774996,-70.7930412663358));
#43260=CARTESIAN_POINT('Ctrl Pts',(-56.0856737258281,14.8634736923075,-71.037586644955));
#43261=CARTESIAN_POINT('Ctrl Pts',(-56.0856398440421,15.1288129436771,-71.5400969655525));
#43262=CARTESIAN_POINT('Ctrl Pts',(-56.0859627501435,15.4588011640861,-72.1628188095271));
#43263=CARTESIAN_POINT('Ctrl Pts',(-56.0860780358828,15.8578470167035,-72.9134975508988));
#43264=CARTESIAN_POINT('Ctrl Pts',(-56.0863311102607,16.6573513988515,-74.413976018313));
#43265=CARTESIAN_POINT('Ctrl Pts',(-56.0862924185878,17.3272522841457,-75.6668224616729));
#43266=CARTESIAN_POINT('Ctrl Pts',(-56.0860259166991,18.2989737931892,-77.4942288644924));
#43267=CARTESIAN_POINT('Ctrl Pts',(-56.0861417091234,18.7346714090501,-78.3135205636837));
#43268=CARTESIAN_POINT('Ctrl Pts',(-56.0861417091228,19.1711929964396,-79.1344982657809));
#43269=CARTESIAN_POINT('Ctrl Pts',(-53.2695191090026,5.51412391624868,24.8304298636229));
#43270=CARTESIAN_POINT('Ctrl Pts',(-53.2696729804314,5.51413893918573,24.781544104745));
#43271=CARTESIAN_POINT('Ctrl Pts',(-53.2698343600099,5.51415470785899,24.7326593874112));
#43272=CARTESIAN_POINT('Ctrl Pts',(-53.2717402620553,5.51434076369697,24.1819722349007));
#43273=CARTESIAN_POINT('Ctrl Pts',(-53.2731264290575,5.51435894341818,23.1776970740902));
#43274=CARTESIAN_POINT('Ctrl Pts',(-53.2763014396343,5.51432310337358,21.1689687233707));
#43275=CARTESIAN_POINT('Ctrl Pts',(-53.2889904683357,5.51556557258312,19.6647568302414));
#43276=CARTESIAN_POINT('Ctrl Pts',(-53.3162754315305,5.518818802787,18.4137075492479));
#43277=CARTESIAN_POINT('Ctrl Pts',(-53.3293106107319,5.52034451434612,17.9105627879296));
#43278=CARTESIAN_POINT('Ctrl Pts',(-53.3619539357177,5.52412101015913,16.9063102282351));
#43279=CARTESIAN_POINT('Ctrl Pts',(-53.4319747813724,5.53225803755914,15.152428522052));
#43280=CARTESIAN_POINT('Ctrl Pts',(-53.4991679604305,5.54059971155965,13.6515466504369));
#43281=CARTESIAN_POINT('Ctrl Pts',(-53.5425107860897,5.54690481688883,12.3984165575284));
#43282=CARTESIAN_POINT('Ctrl Pts',(-53.5603706376019,5.54960764105437,11.8980142668053));
#43283=CARTESIAN_POINT('Ctrl Pts',(-53.5972312288389,5.55551650862214,10.8970295658701));
#43284=CARTESIAN_POINT('Ctrl Pts',(-53.6434679491633,5.56341564867434,9.64501806028444));
#43285=CARTESIAN_POINT('Ctrl Pts',(-53.6928486983768,5.57229632593769,8.14044610826101));
#43286=CARTESIAN_POINT('Ctrl Pts',(-53.7174705237535,5.57688272688435,7.13495869916707));
#43287=CARTESIAN_POINT('Ctrl Pts',(-53.7289266788192,5.57903837763239,6.50641411021376));
#43288=CARTESIAN_POINT('Ctrl Pts',(-53.7332088253681,5.57988413685081,6.25651562184119));
#43289=CARTESIAN_POINT('Ctrl Pts',(-53.7407031707429,5.58150267609513,5.75562639093175));
#43290=CARTESIAN_POINT('Ctrl Pts',(-53.7511456644898,5.58410243092635,4.87741752009759));
#43291=CARTESIAN_POINT('Ctrl Pts',(-53.7623560903057,5.58814369853549,3.11632311933031));
#43292=CARTESIAN_POINT('Ctrl Pts',(-53.7590470244509,5.58856175398403,1.6064679537484));
#43293=CARTESIAN_POINT('Ctrl Pts',(-53.7540980002488,5.58677338992612,0.543397417953566));
#43294=CARTESIAN_POINT('Ctrl Pts',(-53.753513348334,5.58635411736398,0.412074377092105));
#43295=CARTESIAN_POINT('Ctrl Pts',(-53.752352226417,5.58478397945459,0.153131956078355));
#43296=CARTESIAN_POINT('Ctrl Pts',(-53.7502960394157,5.58030638502699,-0.298962418503893));
#43297=CARTESIAN_POINT('Ctrl Pts',(-53.747041298155,5.57006430941205,-0.937293506954136));
#43298=CARTESIAN_POINT('Ctrl Pts',(-53.7418125431459,5.5551497800351,-1.69263172943391));
#43299=CARTESIAN_POINT('Ctrl Pts',(-53.7320405695537,5.536106807732,-2.68608904075444));
#43300=CARTESIAN_POINT('Ctrl Pts',(-53.7126486696442,5.52214075949863,-3.90323953145756));
#43301=CARTESIAN_POINT('Ctrl Pts',(-53.6857217408105,5.53762914818405,-4.85284196928096));
#43302=CARTESIAN_POINT('Ctrl Pts',(-53.6642023602138,5.56056015472782,-5.44207547801918));
#43303=CARTESIAN_POINT('Ctrl Pts',(-53.6548329760197,5.56915151054791,-5.72862142582819));
#43304=CARTESIAN_POINT('Ctrl Pts',(-53.6345397295929,5.57623641436791,-6.25851002643969));
#43305=CARTESIAN_POINT('Ctrl Pts',(-53.5946255286048,5.57365819050158,-7.16755236124054));
#43306=CARTESIAN_POINT('Ctrl Pts',(-53.5267824369403,5.56513849529919,-8.35954499643954));
#43307=CARTESIAN_POINT('Ctrl Pts',(-53.4528358806497,5.63531466714391,-9.42459253171312));
#43308=CARTESIAN_POINT('Ctrl Pts',(-53.4063569805158,5.75703994750273,-10.1070730340725));
#43309=CARTESIAN_POINT('Ctrl Pts',(-53.3826169629337,5.8516342288584,-10.4838875321135));
#43310=CARTESIAN_POINT('Ctrl Pts',(-53.3718033621994,5.9082272881835,-10.6687549503979));
#43311=CARTESIAN_POINT('Ctrl Pts',(-53.3641622492917,5.95443181047735,-10.806250048848));
#43312=CARTESIAN_POINT('Ctrl Pts',(-53.3609764178454,5.97942695957719,-10.8749681752605));
#43313=CARTESIAN_POINT('Ctrl Pts',(-53.3526198015811,6.04532819060391,-11.0376782273807));
#43314=CARTESIAN_POINT('Ctrl Pts',(-53.3361006816262,6.18733006109969,-11.3402774953735));
#43315=CARTESIAN_POINT('Ctrl Pts',(-53.2907959702171,6.58731155192089,-12.0388473668935));
#43316=CARTESIAN_POINT('Ctrl Pts',(-53.1924783584682,7.42521315073151,-13.2043467596497));
#43317=CARTESIAN_POINT('Ctrl Pts',(-53.0842900264596,8.29440822558255,-14.3989188175356));
#43318=CARTESIAN_POINT('Ctrl Pts',(-53.015262415626,8.83233778190795,-15.2828268594339));
#43319=CARTESIAN_POINT('Ctrl Pts',(-52.9712767444326,9.1723889427504,-15.9015569257269));
#43320=CARTESIAN_POINT('Ctrl Pts',(-52.941883462723,9.39814693567254,-16.404340394339));
#43321=CARTESIAN_POINT('Ctrl Pts',(-52.9221524344923,9.55495080979618,-16.8496642085187));
#43322=CARTESIAN_POINT('Ctrl Pts',(-52.9171702213878,9.60532703150434,-16.9974857947432));
#43323=CARTESIAN_POINT('Ctrl Pts',(-52.9077925126434,9.70384045488972,-17.3085378437202));
#43324=CARTESIAN_POINT('Ctrl Pts',(-52.9017119486451,9.7888502139978,-17.611479209509));
#43325=CARTESIAN_POINT('Ctrl Pts',(-52.8978643914528,9.86457371739576,-17.9151182244612));
#43326=CARTESIAN_POINT('Ctrl Pts',(-52.8964966777581,9.90752297295601,-18.1030131264597));
#43327=CARTESIAN_POINT('Ctrl Pts',(-52.8959255353737,9.93963575717371,-18.2528564737207));
#43328=CARTESIAN_POINT('Ctrl Pts',(-52.8957656598868,9.96255665128214,-18.3647826827941));
#43329=CARTESIAN_POINT('Ctrl Pts',(-52.8958406345935,9.98074558923007,-18.4577554651167));
#43330=CARTESIAN_POINT('Ctrl Pts',(-52.8960220828767,9.99475780550526,-18.5319159564531));
#43331=CARTESIAN_POINT('Ctrl Pts',(-52.8982398755439,10.1108798618789,-19.161197415467));
#43332=CARTESIAN_POINT('Ctrl Pts',(-52.9230826162276,10.2397643749445,-20.3264110372225));
#43333=CARTESIAN_POINT('Ctrl Pts',(-52.9776760452522,10.3009424686941,-21.9157318243612));
#43334=CARTESIAN_POINT('Ctrl Pts',(-53.0026397326956,10.3306613219927,-22.8884250543864));
#43335=CARTESIAN_POINT('Ctrl Pts',(-53.0078332433723,10.3640352479388,-23.4697077997478));
#43336=CARTESIAN_POINT('Ctrl Pts',(-53.0090207928301,10.3779232234325,-23.7492065296354));
#43337=CARTESIAN_POINT('Ctrl Pts',(-53.0101422632217,10.3965999748253,-24.2767246640981));
#43338=CARTESIAN_POINT('Ctrl Pts',(-53.0084606712719,10.4126262654147,-25.2060431411203));
#43339=CARTESIAN_POINT('Ctrl Pts',(-52.9989783339964,10.398230606303,-26.5002884694706));
#43340=CARTESIAN_POINT('Ctrl Pts',(-52.9857517356138,10.3609028968362,-28.0156324090607));
#43341=CARTESIAN_POINT('Ctrl Pts',(-52.9821696124883,10.3463072684496,-28.9935516511673));
#43342=CARTESIAN_POINT('Ctrl Pts',(-52.9834192251574,10.3472723357311,-29.5347726580737));
#43343=CARTESIAN_POINT('Ctrl Pts',(-52.9837372616693,10.3475112658483,-29.6609741299702));
#43344=CARTESIAN_POINT('Ctrl Pts',(-52.9845353643974,10.3481161356179,-29.9101521285755));
#43345=CARTESIAN_POINT('Ctrl Pts',(-52.986340876066,10.349480494944,-30.3482200575802));
#43346=CARTESIAN_POINT('Ctrl Pts',(-52.9914277859591,10.3532806040434,-31.2241592854396));
#43347=CARTESIAN_POINT('Ctrl Pts',(-53.0020924987196,10.3609199025555,-32.4786454126478));
#43348=CARTESIAN_POINT('Ctrl Pts',(-53.015062011775,10.3692826159378,-33.7336959612824));
#43349=CARTESIAN_POINT('Ctrl Pts',(-53.0254914065946,10.3752013019634,-34.7370311416471));
#43350=CARTESIAN_POINT('Ctrl Pts',(-53.0305261145087,10.3777432817774,-35.2383457278596));
#43351=CARTESIAN_POINT('Ctrl Pts',(-53.0341499042062,10.3794217654475,-35.6150639393877));
#43352=CARTESIAN_POINT('Ctrl Pts',(-53.0366808553066,10.3805297298129,-35.8668994441295));
#43353=CARTESIAN_POINT('Ctrl Pts',(-53.0420881296609,10.3826532259823,-36.3700528992668));
#43354=CARTESIAN_POINT('Ctrl Pts',(-53.0523371587987,10.386195572391,-37.2488687853845));
#43355=CARTESIAN_POINT('Ctrl Pts',(-53.0745845450279,10.3926516914606,-39.0015260691109));
#43356=CARTESIAN_POINT('Ctrl Pts',(-53.0924719215915,10.3979267436415,-40.5024720108467));
#43357=CARTESIAN_POINT('Ctrl Pts',(-53.1018001444244,10.4028349641943,-41.7577669805917));
#43358=CARTESIAN_POINT('Ctrl Pts',(-53.1041676838787,10.4037624619664,-42.136430142011));
#43359=CARTESIAN_POINT('Ctrl Pts',(-53.1066815827788,10.4043145535304,-42.6389847981761));
#43360=CARTESIAN_POINT('Ctrl Pts',(-53.1088301638818,10.4045597059282,-43.1417757799241));
#43361=CARTESIAN_POINT('Ctrl Pts',(-53.110939299965,10.4045416070056,-43.7693696339286));
#43362=CARTESIAN_POINT('Ctrl Pts',(-53.1129027891297,10.4048250580523,-44.5210196499416));
#43363=CARTESIAN_POINT('Ctrl Pts',(-53.1143623411914,10.4059949502891,-45.1455823564742));
#43364=CARTESIAN_POINT('Ctrl Pts',(-53.1155986256389,10.407885674506,-45.6439270779171));
#43365=CARTESIAN_POINT('Ctrl Pts',(-53.1166060629224,10.4098856947673,-46.0169470561475));
#43366=CARTESIAN_POINT('Ctrl Pts',(-53.1177377013386,10.4125673568949,-46.3891933597327));
#43367=CARTESIAN_POINT('Ctrl Pts',(-53.1194730531813,10.4171804267262,-46.8843198176108));
#43368=CARTESIAN_POINT('Ctrl Pts',(-53.1210917554422,10.4219674360715,-47.254411337671));
#43369=CARTESIAN_POINT('Ctrl Pts',(-53.1230216141993,10.4278328510612,-47.6239090432503));
#43370=CARTESIAN_POINT('Ctrl Pts',(-53.1243337754983,10.4328860199948,-47.8585325572095));
#43371=CARTESIAN_POINT('Ctrl Pts',(-53.1269381890424,10.4477144863777,-48.3405539590965));
#43372=CARTESIAN_POINT('Ctrl Pts',(-53.1315208014342,10.4835733437767,-49.1925394235593));
#43373=CARTESIAN_POINT('Ctrl Pts',(-53.1382805406101,10.5511535870157,-50.4477259469352));
#43374=CARTESIAN_POINT('Ctrl Pts',(-53.1478839894708,10.6148347212714,-52.0080606162247));
#43375=CARTESIAN_POINT('Ctrl Pts',(-53.1563545836586,10.6132655386803,-53.0856319446143));
#43376=CARTESIAN_POINT('Ctrl Pts',(-53.1628474808204,10.5871080946179,-53.7730506798432));
#43377=CARTESIAN_POINT('Ctrl Pts',(-53.1658809440165,10.5698873205239,-54.078978194353));
#43378=CARTESIAN_POINT('Ctrl Pts',(-53.172718225336,10.5184020731151,-54.6578777376874));
#43379=CARTESIAN_POINT('Ctrl Pts',(-53.186128484262,10.3931280910598,-55.6405469499418));
#43380=CARTESIAN_POINT('Ctrl Pts',(-53.2152647300223,10.073597963779,-57.4486599529017));
#43381=CARTESIAN_POINT('Ctrl Pts',(-53.2322648244722,9.91038299977115,-58.7349749671413));
#43382=CARTESIAN_POINT('Ctrl Pts',(-53.2438575714141,9.95727375411102,-59.497859872132));
#43383=CARTESIAN_POINT('Ctrl Pts',(-53.2451145053797,9.96484293104403,-59.6110104688653));
#43384=CARTESIAN_POINT('Ctrl Pts',(-53.2476494794711,9.98246534722492,-59.8267651893542));
#43385=CARTESIAN_POINT('Ctrl Pts',(-53.2518916147946,10.0216393104554,-60.2122308274534));
#43386=CARTESIAN_POINT('Ctrl Pts',(-53.2597849475336,10.1308552935276,-60.9871127641917));
#43387=CARTESIAN_POINT('Ctrl Pts',(-53.2673306041421,10.322172678003,-61.891687150218));
#43388=CARTESIAN_POINT('Ctrl Pts',(-53.2735732107563,10.5688715421272,-62.8060550616252));
#43389=CARTESIAN_POINT('Ctrl Pts',(-53.2766749767257,10.7260538805703,-63.3235783249706));
#43390=CARTESIAN_POINT('Ctrl Pts',(-53.2786068180125,10.8375187332017,-63.6692949698584));
#43391=CARTESIAN_POINT('Ctrl Pts',(-53.2798618887772,10.9135406655232,-63.8999771283551));
#43392=CARTESIAN_POINT('Ctrl Pts',(-53.2810746824334,10.9919940234548,-64.1307767366773));
#43393=CARTESIAN_POINT('Ctrl Pts',(-53.2821036920121,11.0626205110791,-64.3328945957961));
#43394=CARTESIAN_POINT('Ctrl Pts',(-53.2826838151074,11.1035153020404,-64.4484175619505));
#43395=CARTESIAN_POINT('Ctrl Pts',(-53.283548221091,11.1653700926799,-64.6216968474611));
#43396=CARTESIAN_POINT('Ctrl Pts',(-53.284252795929,11.2179902945138,-64.7661579752883));
#43397=CARTESIAN_POINT('Ctrl Pts',(-53.2854405442884,11.3061294590031,-65.0046841289595));
#43398=CARTESIAN_POINT('Ctrl Pts',(-53.2882199013159,11.3889600472922,-65.2175420671513));
#43399=CARTESIAN_POINT('Ctrl Pts',(-53.292448406723,11.5782434117156,-65.6675288390924));
#43400=CARTESIAN_POINT('Ctrl Pts',(-53.2991156029898,11.9466785795384,-66.4569755997879));
#43401=CARTESIAN_POINT('Ctrl Pts',(-53.3065839328934,12.8266158262504,-68.0959375031218));
#43402=CARTESIAN_POINT('Ctrl Pts',(-53.3034527100005,13.7246014984242,-69.5904403556736));
#43403=CARTESIAN_POINT('Ctrl Pts',(-53.298461024074,14.3562308772955,-70.7919116954683));
#43404=CARTESIAN_POINT('Ctrl Pts',(-53.2989079885199,14.4851082685386,-71.0364643141845));
#43405=CARTESIAN_POINT('Ctrl Pts',(-53.298884851345,14.7504619528231,-71.538981752293));
#43406=CARTESIAN_POINT('Ctrl Pts',(-53.299187908537,15.0804546178337,-72.1617121321261));
#43407=CARTESIAN_POINT('Ctrl Pts',(-53.2992942658897,15.4795028987994,-72.9123984874085));
#43408=CARTESIAN_POINT('Ctrl Pts',(-53.2995192454489,16.2789992759831,-74.4128876795658));
#43409=CARTESIAN_POINT('Ctrl Pts',(-53.2994656403349,16.9488786459547,-75.6657250237291));
#43410=CARTESIAN_POINT('Ctrl Pts',(-53.2992200346635,17.9205956470159,-77.4931101939678));
#43411=CARTESIAN_POINT('Ctrl Pts',(-53.2993262462524,18.356293084259,-78.3124054144669));
#43412=CARTESIAN_POINT('Ctrl Pts',(-53.2993262462519,18.7928146716484,-79.133383116566));
#43413=CARTESIAN_POINT('Ctrl Pts',(-50.4917882253004,5.17566710371987,24.8304874162273));
#43414=CARTESIAN_POINT('Ctrl Pts',(-50.4919422879461,5.17568106144213,24.7816034400889));
#43415=CARTESIAN_POINT('Ctrl Pts',(-50.4921038555884,5.17569570639061,24.732720517874));
#43416=CARTESIAN_POINT('Ctrl Pts',(-50.4940119203857,5.17586856599346,24.1820548339752));
#43417=CARTESIAN_POINT('Ctrl Pts',(-50.4955724909529,5.17593860157383,23.1778361008006));
#43418=CARTESIAN_POINT('Ctrl Pts',(-50.4992667335108,5.17606267776333,21.1691322613434));
#43419=CARTESIAN_POINT('Ctrl Pts',(-50.5119607466055,5.17721416687989,19.6648867929363));
#43420=CARTESIAN_POINT('Ctrl Pts',(-50.5383956361274,5.17996827678101,18.4137882022575));
#43421=CARTESIAN_POINT('Ctrl Pts',(-50.5511098675465,5.18125500287494,17.9106295924923));
#43422=CARTESIAN_POINT('Ctrl Pts',(-50.5830956060071,5.18442656664954,16.9063864387148));
#43423=CARTESIAN_POINT('Ctrl Pts',(-50.6516776928239,5.19123763326873,15.1526081475984));
#43424=CARTESIAN_POINT('Ctrl Pts',(-50.7162583676642,5.19817828286658,13.6518058482652));
#43425=CARTESIAN_POINT('Ctrl Pts',(-50.7557353079412,5.20339071244593,12.3986742928636));
#43426=CARTESIAN_POINT('Ctrl Pts',(-50.7717676670402,5.20561905708811,11.8982650828353));
#43427=CARTESIAN_POINT('Ctrl Pts',(-50.8041080415491,5.21047533733246,10.8972213333765));
#43428=CARTESIAN_POINT('Ctrl Pts',(-50.8435506882696,5.21694325198105,9.64509183781364));
#43429=CARTESIAN_POINT('Ctrl Pts',(-50.8845928089285,5.22422283738103,8.14041002755545));
#43430=CARTESIAN_POINT('Ctrl Pts',(-50.9045815330377,5.22799726787858,7.13494612707244));
#43431=CARTESIAN_POINT('Ctrl Pts',(-50.9137804798122,5.22978749172542,6.50645248630553));
#43432=CARTESIAN_POINT('Ctrl Pts',(-50.9171207652802,5.23048874545483,6.25663725309473));
#43433=CARTESIAN_POINT('Ctrl Pts',(-50.9226055832772,5.23184374261148,5.75586011385058));
#43434=CARTESIAN_POINT('Ctrl Pts',(-50.9293192198983,5.2340482166052,4.8778075754179));
#43435=CARTESIAN_POINT('Ctrl Pts',(-50.9332230963537,5.23757919640148,3.11687270565004));
#43436=CARTESIAN_POINT('Ctrl Pts',(-50.9271940666093,5.23816338383166,1.6066003813206));
#43437=CARTESIAN_POINT('Ctrl Pts',(-50.924944151531,5.23660003134025,0.543423623103098));
#43438=CARTESIAN_POINT('Ctrl Pts',(-50.9247138303533,5.2363056290163,0.414339096126991));
#43439=CARTESIAN_POINT('Ctrl Pts',(-50.9243864185811,5.23530944223134,0.158224698787665));
#43440=CARTESIAN_POINT('Ctrl Pts',(-50.9241068848092,5.23260255432325,-0.2891299684906));
#43441=CARTESIAN_POINT('Ctrl Pts',(-50.9242445619944,5.22653553940069,-0.923639989145307));
#43442=CARTESIAN_POINT('Ctrl Pts',(-50.9242394642031,5.2175972786583,-1.67831756883862));
#43443=CARTESIAN_POINT('Ctrl Pts',(-50.9227165665054,5.20579796768503,-2.67664338433093));
#43444=CARTESIAN_POINT('Ctrl Pts',(-50.9154444941589,5.19587448445967,-3.91038768968163));
#43445=CARTESIAN_POINT('Ctrl Pts',(-50.8985483027333,5.20214371572755,-4.88421643440741));
#43446=CARTESIAN_POINT('Ctrl Pts',(-50.8828450232104,5.21332010223727,-5.49185544560995));
#43447=CARTESIAN_POINT('Ctrl Pts',(-50.8764257048549,5.2150483326915,-5.78760510738548));
#43448=CARTESIAN_POINT('Ctrl Pts',(-50.8633447034513,5.20613721753072,-6.33252108952286));
#43449=CARTESIAN_POINT('Ctrl Pts',(-50.8389414588566,5.16930113279147,-7.26308501721412));
#43450=CARTESIAN_POINT('Ctrl Pts',(-50.7964756300872,5.10494006098571,-8.4711418915596));
#43451=CARTESIAN_POINT('Ctrl Pts',(-50.737747222281,5.12507030419363,-9.529298817259));
#43452=CARTESIAN_POINT('Ctrl Pts',(-50.6902034234311,5.21378862573971,-10.1917268936));
#43453=CARTESIAN_POINT('Ctrl Pts',(-50.6621507433786,5.28919873023719,-10.5537179772744));
#43454=CARTESIAN_POINT('Ctrl Pts',(-50.6479227661616,5.33605027741116,-10.7302607132582));
#43455=CARTESIAN_POINT('Ctrl Pts',(-50.6372113533515,5.37493309748007,-10.8614628809451));
#43456=CARTESIAN_POINT('Ctrl Pts',(-50.6307408610024,5.39714223544244,-10.9310589148788));
#43457=CARTESIAN_POINT('Ctrl Pts',(-50.615457868595,5.45499085945406,-11.0920476345774));
#43458=CARTESIAN_POINT('Ctrl Pts',(-50.5847067920761,5.5809826822393,-11.3922056187527));
#43459=CARTESIAN_POINT('Ctrl Pts',(-50.5066841896989,5.9405065242805,-12.0837419858941));
#43460=CARTESIAN_POINT('Ctrl Pts',(-50.3581920745141,6.71333282334061,-13.24143272121));
#43461=CARTESIAN_POINT('Ctrl Pts',(-50.2070844063659,7.53254968807352,-14.4264283964002));
#43462=CARTESIAN_POINT('Ctrl Pts',(-50.1143745831895,8.04622175930128,-15.2954922329237));
#43463=CARTESIAN_POINT('Ctrl Pts',(-50.0567907074399,8.37352615381154,-15.9005955895759));
#43464=CARTESIAN_POINT('Ctrl Pts',(-50.0203542727671,8.59476626467718,-16.3877449176251));
#43465=CARTESIAN_POINT('Ctrl Pts',(-49.9979142754099,8.75369398499996,-16.8155401572584));
#43466=CARTESIAN_POINT('Ctrl Pts',(-49.9932937554699,8.80427540492771,-16.9532446535472));
#43467=CARTESIAN_POINT('Ctrl Pts',(-49.9850391776131,8.90725677558605,-17.2463051810055));
#43468=CARTESIAN_POINT('Ctrl Pts',(-49.9818900096223,9.00097130090873,-17.5313844372905));
#43469=CARTESIAN_POINT('Ctrl Pts',(-49.9822865499116,9.08953544821376,-17.8187950252249));
#43470=CARTESIAN_POINT('Ctrl Pts',(-49.9841806466715,9.14198168186362,-17.997075773544));
#43471=CARTESIAN_POINT('Ctrl Pts',(-49.9865389808682,9.18252740910799,-18.1396657873466));
#43472=CARTESIAN_POINT('Ctrl Pts',(-49.9887415658394,9.21215644005256,-18.246358287446));
#43473=CARTESIAN_POINT('Ctrl Pts',(-49.9909150035896,9.23623998981229,-18.3351553365422));
#43474=CARTESIAN_POINT('Ctrl Pts',(-49.9928534025731,9.25513922998495,-18.4060925378598));
#43475=CARTESIAN_POINT('Ctrl Pts',(-50.0104080099896,9.41372406993346,-19.0085655115853));
#43476=CARTESIAN_POINT('Ctrl Pts',(-50.0785835779704,9.65166925678319,-20.1448867246259));
#43477=CARTESIAN_POINT('Ctrl Pts',(-50.2094455136225,9.86360570203751,-21.7593394035839));
#43478=CARTESIAN_POINT('Ctrl Pts',(-50.2695728798328,9.95364845399459,-22.7883530169235));
#43479=CARTESIAN_POINT('Ctrl Pts',(-50.2853974619132,10.0086808237604,-23.4174394581283));
#43480=CARTESIAN_POINT('Ctrl Pts',(-50.2905491917215,10.0307168845544,-23.7072050842054));
#43481=CARTESIAN_POINT('Ctrl Pts',(-50.2982535121411,10.059985098277,-24.2572722652478));
#43482=CARTESIAN_POINT('Ctrl Pts',(-50.3049354504982,10.0831641537804,-25.2170434829339));
#43483=CARTESIAN_POINT('Ctrl Pts',(-50.299090492575,10.0554482373577,-26.5365348741012));
#43484=CARTESIAN_POINT('Ctrl Pts',(-50.2804361269476,9.99211926516758,-28.0501492024477));
#43485=CARTESIAN_POINT('Ctrl Pts',(-50.2699104858743,9.96837189047219,-29.005969213032));
#43486=CARTESIAN_POINT('Ctrl Pts',(-50.2675102217974,9.96983147071442,-29.5291008868419));
#43487=CARTESIAN_POINT('Ctrl Pts',(-50.2669406729928,9.9702759020367,-29.6548785372973));
#43488=CARTESIAN_POINT('Ctrl Pts',(-50.2656765811437,9.97141249672459,-29.9013334019936));
#43489=CARTESIAN_POINT('Ctrl Pts',(-50.2631539222159,9.97412106283928,-30.3359632918983));
#43490=CARTESIAN_POINT('Ctrl Pts',(-50.2570939411495,9.98199525595261,-31.2055924825988));
#43491=CARTESIAN_POINT('Ctrl Pts',(-50.2467310549431,9.99874366664344,-32.4553294381363));
#43492=CARTESIAN_POINT('Ctrl Pts',(-50.2372638556452,10.0180406299146,-33.7105948576416));
#43493=CARTESIAN_POINT('Ctrl Pts',(-50.2321054601144,10.0318670608778,-34.7174137538182));
#43494=CARTESIAN_POINT('Ctrl Pts',(-50.2306260626996,10.037800648482,-35.2215261148078));
#43495=CARTESIAN_POINT('Ctrl Pts',(-50.23005283174,10.0416318474723,-35.6007176993595));
#43496=CARTESIAN_POINT('Ctrl Pts',(-50.2298354684155,10.0441425631425,-35.8523882463753));
#43497=CARTESIAN_POINT('Ctrl Pts',(-50.2299882230626,10.0490093971083,-36.3562680642938));
#43498=CARTESIAN_POINT('Ctrl Pts',(-50.2316173278082,10.0573057462866,-37.2358952215116));
#43499=CARTESIAN_POINT('Ctrl Pts',(-50.2389254191521,10.0723990884057,-38.9907229977759));
#43500=CARTESIAN_POINT('Ctrl Pts',(-50.2473114970814,10.0841162826904,-40.4935920088638));
#43501=CARTESIAN_POINT('Ctrl Pts',(-50.2501140904947,10.0932039565461,-41.7505062234857));
#43502=CARTESIAN_POINT('Ctrl Pts',(-50.2505809071243,10.0953249979928,-42.1293419423953));
#43503=CARTESIAN_POINT('Ctrl Pts',(-50.2507131066099,10.0973339515644,-42.632366127817));
#43504=CARTESIAN_POINT('Ctrl Pts',(-50.2505992437383,10.0989722141392,-43.1356438106316));
#43505=CARTESIAN_POINT('Ctrl Pts',(-50.2501451161471,10.100540748878,-43.7639698516428));
#43506=CARTESIAN_POINT('Ctrl Pts',(-50.2495854290043,10.102441873018,-44.5166707004118));
#43507=CARTESIAN_POINT('Ctrl Pts',(-50.2495106314317,10.1046844156364,-45.1422732594455));
#43508=CARTESIAN_POINT('Ctrl Pts',(-50.2499203773133,10.1072148812516,-45.6415285781111));
#43509=CARTESIAN_POINT('Ctrl Pts',(-50.2505268590744,10.1095939362813,-46.0152816765834));
#43510=CARTESIAN_POINT('Ctrl Pts',(-50.2514927039908,10.1125449059654,-46.3883095356268));
#43511=CARTESIAN_POINT('Ctrl Pts',(-50.2533375408547,10.1173643015842,-46.8845367359995));
#43512=CARTESIAN_POINT('Ctrl Pts',(-50.2554489682574,10.1221245401292,-47.2555408653554));
#43513=CARTESIAN_POINT('Ctrl Pts',(-50.2581634178688,10.1278349914596,-47.6259921783748));
#43514=CARTESIAN_POINT('Ctrl Pts',(-50.2601382453279,10.1327494655044,-47.8614537741923));
#43515=CARTESIAN_POINT('Ctrl Pts',(-50.2645669531397,10.1470848162755,-48.3448779496376));
#43516=CARTESIAN_POINT('Ctrl Pts',(-50.2735228646179,10.181589460592,-49.1990209944655));
#43517=CARTESIAN_POINT('Ctrl Pts',(-50.2892411015512,10.2458256924249,-50.4562472205667));
#43518=CARTESIAN_POINT('Ctrl Pts',(-50.3115704218278,10.3041487355604,-52.0175019206382));
#43519=CARTESIAN_POINT('Ctrl Pts',(-50.3283744489858,10.2985694370559,-53.0946911955599));
#43520=CARTESIAN_POINT('Ctrl Pts',(-50.3394854329771,10.2700744321005,-53.7815927083882));
#43521=CARTESIAN_POINT('Ctrl Pts',(-50.3444777023812,10.2516813158405,-54.0883431032896));
#43522=CARTESIAN_POINT('Ctrl Pts',(-50.3554547454227,10.1977742066435,-54.6680452815916));
#43523=CARTESIAN_POINT('Ctrl Pts',(-50.3766307896317,10.06795271147,-55.6518561088696));
#43524=CARTESIAN_POINT('Ctrl Pts',(-50.4220100454917,9.73932917875835,-57.4602542456734));
#43525=CARTESIAN_POINT('Ctrl Pts',(-50.4517174235069,9.5716293558584,-58.7437695560338));
#43526=CARTESIAN_POINT('Ctrl Pts',(-50.4672683941523,9.616802212515,-59.501807302348));
#43527=CARTESIAN_POINT('Ctrl Pts',(-50.4689891228026,9.62414747583199,-59.6144877527924));
#43528=CARTESIAN_POINT('Ctrl Pts',(-50.472309048858,9.64137944175633,-59.8292913302342));
#43529=CARTESIAN_POINT('Ctrl Pts',(-50.477602282877,9.67996605567735,-60.2132517968072));
#43530=CARTESIAN_POINT('Ctrl Pts',(-50.4864151011654,9.78843142638471,-60.9856425795006));
#43531=CARTESIAN_POINT('Ctrl Pts',(-50.4929757612956,9.97978760295941,-61.888626609612));
#43532=CARTESIAN_POINT('Ctrl Pts',(-50.4974662177313,10.2271615291421,-62.8025169538524));
#43533=CARTESIAN_POINT('Ctrl Pts',(-50.4995193297966,10.3848718063098,-63.3201554766683));
#43534=CARTESIAN_POINT('Ctrl Pts',(-50.5008191348443,10.4967073652988,-63.6660944985812));
#43535=CARTESIAN_POINT('Ctrl Pts',(-50.501676136481,10.5729794099748,-63.8969640514493));
#43536=CARTESIAN_POINT('Ctrl Pts',(-50.5025358148872,10.6516782376813,-64.1280050630122));
#43537=CARTESIAN_POINT('Ctrl Pts',(-50.5033099106476,10.7225113373282,-64.3303833066746));
#43538=CARTESIAN_POINT('Ctrl Pts',(-50.5037621554921,10.7635201092562,-64.4460686102444));
#43539=CARTESIAN_POINT('Ctrl Pts',(-50.5044534077156,10.8255411352936,-64.6196044834109));
#43540=CARTESIAN_POINT('Ctrl Pts',(-50.5050557817371,10.8782882713032,-64.7643078741904));
#43541=CARTESIAN_POINT('Ctrl Pts',(-50.5061377180057,10.9666119413916,-65.003260922051));
#43542=CARTESIAN_POINT('Ctrl Pts',(-50.508638492893,11.0493697468618,-65.2160015584756));
#43543=CARTESIAN_POINT('Ctrl Pts',(-50.5124241402302,11.2386522834735,-65.6660749449834));
#43544=CARTESIAN_POINT('Ctrl Pts',(-50.5183391803283,11.6070025105966,-66.4555156665412));
#43545=CARTESIAN_POINT('Ctrl Pts',(-50.5247662875685,12.4868488647233,-68.0945928971807));
#43546=CARTESIAN_POINT('Ctrl Pts',(-50.5217297342562,13.3848211445789,-69.5890408902695));
#43547=CARTESIAN_POINT('Ctrl Pts',(-50.5172962706906,14.0166187274579,-70.7904911454533));
#43548=CARTESIAN_POINT('Ctrl Pts',(-50.5176848766757,14.1454945205256,-71.0350535179694));
#43549=CARTESIAN_POINT('Ctrl Pts',(-50.517655798034,14.410863768523,-71.5375810908797));
#43550=CARTESIAN_POINT('Ctrl Pts',(-50.517917673406,14.7408594614161,-72.1603229363731));
#43551=CARTESIAN_POINT('Ctrl Pts',(-50.518010611717,15.1399102004369,-72.9110189371167));
#43552=CARTESIAN_POINT('Ctrl Pts',(-50.5182159283882,15.9393977459531,-74.4115205735121));
#43553=CARTESIAN_POINT('Ctrl Pts',(-50.5181862633849,16.6092508749019,-75.6643443595441));
#43554=CARTESIAN_POINT('Ctrl Pts',(-50.5179716192911,17.5809598952617,-77.4917029993533));
#43555=CARTESIAN_POINT('Ctrl Pts',(-50.5180655120236,18.0166559625962,-78.3110026508708));
#43556=CARTESIAN_POINT('Ctrl Pts',(-50.518065512024,18.4531775499857,-79.1319803529701));
#43557=CARTESIAN_POINT('Ctrl Pts',(-47.7140625860263,4.8827673795561,24.83071473666));
#43558=CARTESIAN_POINT('Ctrl Pts',(-47.7142056270501,4.88278315123272,24.7818380104655));
#43559=CARTESIAN_POINT('Ctrl Pts',(-47.7143556438381,4.88279969683197,24.7329624584372));
#43560=CARTESIAN_POINT('Ctrl Pts',(-47.7161271346974,4.88299471720164,24.1823823057849));
#43561=CARTESIAN_POINT('Ctrl Pts',(-47.7175219397781,4.88318692485811,23.1782622657522));
#43562=CARTESIAN_POINT('Ctrl Pts',(-47.7207922725251,4.88366739337577,21.1697171422517));
#43563=CARTESIAN_POINT('Ctrl Pts',(-47.7325810415589,4.8849613002945,19.6655362846526));
#43564=CARTESIAN_POINT('Ctrl Pts',(-47.7573975348289,4.88749005855023,18.4144717200027));
#43565=CARTESIAN_POINT('Ctrl Pts',(-47.769321527011,4.88871561455663,17.9117751017612));
#43566=CARTESIAN_POINT('Ctrl Pts',(-47.7993052830692,4.89181262920139,16.9078592146539));
#43567=CARTESIAN_POINT('Ctrl Pts',(-47.8636134358962,4.89843749421352,15.1540238664033));
#43568=CARTESIAN_POINT('Ctrl Pts',(-47.9244214182784,4.9045205544751,13.6517668992275));
#43569=CARTESIAN_POINT('Ctrl Pts',(-47.9619817440457,4.90795714804035,12.3967188770755));
#43570=CARTESIAN_POINT('Ctrl Pts',(-47.9772718407815,4.90931808413415,11.8955283110643));
#43571=CARTESIAN_POINT('Ctrl Pts',(-48.0082364270896,4.91195046187805,10.8933425971299));
#43572=CARTESIAN_POINT('Ctrl Pts',(-48.0462304403728,4.91499931755227,9.64044727576877));
#43573=CARTESIAN_POINT('Ctrl Pts',(-48.0860237179557,4.91801032724594,8.13590746288963));
#43574=CARTESIAN_POINT('Ctrl Pts',(-48.1056048462851,4.91941894175397,7.13125448252537));
#43575=CARTESIAN_POINT('Ctrl Pts',(-48.114686641634,4.92006091807443,6.50343758513863));
#43576=CARTESIAN_POINT('Ctrl Pts',(-48.1180230915424,4.92028147784815,6.25307816982595));
#43577=CARTESIAN_POINT('Ctrl Pts',(-48.1236516608096,4.92059287275183,5.75186189897002));
#43578=CARTESIAN_POINT('Ctrl Pts',(-48.1309515307269,4.92082784154472,4.87323677530985));
#43579=CARTESIAN_POINT('Ctrl Pts',(-48.1368414760995,4.92039644109217,3.11312011492933));
#43580=CARTESIAN_POINT('Ctrl Pts',(-48.1321571924445,4.91941407371968,1.60646228368251));
#43581=CARTESIAN_POINT('Ctrl Pts',(-48.129156544069,4.91953163485657,0.547584962884119));
#43582=CARTESIAN_POINT('Ctrl Pts',(-48.1287924961985,4.91952801215846,0.420815421233139));
#43583=CARTESIAN_POINT('Ctrl Pts',(-48.1280361619762,4.91943902897318,0.167950253877022));
#43584=CARTESIAN_POINT('Ctrl Pts',(-48.1266207283341,4.91909880758473,-0.274020854476047));
#43585=CARTESIAN_POINT('Ctrl Pts',(-48.1242402329894,4.91818580446943,-0.903549531841198));
#43586=CARTESIAN_POINT('Ctrl Pts',(-48.1205054012334,4.91686798226099,-1.65599660187086));
#43587=CARTESIAN_POINT('Ctrl Pts',(-48.1139402652433,4.91526753761711,-2.65656601275255));
#43588=CARTESIAN_POINT('Ctrl Pts',(-48.1020107258878,4.91468314017721,-3.90276616773367));
#43589=CARTESIAN_POINT('Ctrl Pts',(-48.0869522803996,4.91787671070461,-4.89718018300294));
#43590=CARTESIAN_POINT('Ctrl Pts',(-48.0753265931897,4.92184490707251,-5.52057074281727));
#43591=CARTESIAN_POINT('Ctrl Pts',(-48.071358629886,4.91998443516637,-5.81518912269095));
#43592=CARTESIAN_POINT('Ctrl Pts',(-48.065598030688,4.90444031378955,-6.36312258883095));
#43593=CARTESIAN_POINT('Ctrl Pts',(-48.0593098149811,4.8554734950931,-7.29936993447058));
#43594=CARTESIAN_POINT('Ctrl Pts',(-48.0512760304793,4.76954410211827,-8.52468295486078));
#43595=CARTESIAN_POINT('Ctrl Pts',(-48.0199706320373,4.75930038017222,-9.61057795434388));
#43596=CARTESIAN_POINT('Ctrl Pts',(-47.9753301070093,4.82177048553547,-10.2929213114712));
#43597=CARTESIAN_POINT('Ctrl Pts',(-47.9425518598432,4.87982047166548,-10.6643681872605));
#43598=CARTESIAN_POINT('Ctrl Pts',(-47.9236879911956,4.91686516645017,-10.8446063286549));
#43599=CARTESIAN_POINT('Ctrl Pts',(-47.9085602268087,4.94794884722439,-10.9784757588702));
#43600=CARTESIAN_POINT('Ctrl Pts',(-47.8977045764268,4.96879134742631,-11.0611503257524));
#43601=CARTESIAN_POINT('Ctrl Pts',(-47.8728032300964,5.01813210065941,-11.237347059156));
#43602=CARTESIAN_POINT('Ctrl Pts',(-47.8219732147258,5.12165285259022,-11.5584670494563));
#43603=CARTESIAN_POINT('Ctrl Pts',(-47.696862002376,5.39770009893267,-12.2615093154998));
#43604=CARTESIAN_POINT('Ctrl Pts',(-47.4801637820874,5.97029461539933,-13.409392442977));
#43605=CARTESIAN_POINT('Ctrl Pts',(-47.2858376380383,6.59337864600068,-14.5727985195787));
#43606=CARTESIAN_POINT('Ctrl Pts',(-47.1768883689351,7.00109873332153,-15.4001667508105));
#43607=CARTESIAN_POINT('Ctrl Pts',(-47.1119587725962,7.2675736093193,-15.9664123979976));
#43608=CARTESIAN_POINT('Ctrl Pts',(-47.0739610162134,7.45762098996782,-16.408466282203));
#43609=CARTESIAN_POINT('Ctrl Pts',(-47.0518262734791,7.60559604349496,-16.7855990350013));
#43610=CARTESIAN_POINT('Ctrl Pts',(-47.0491042389521,7.65322588539756,-16.9019857164455));
#43611=CARTESIAN_POINT('Ctrl Pts',(-47.0437189541059,7.75708675336488,-17.1545293646334));
#43612=CARTESIAN_POINT('Ctrl Pts',(-47.0439331697809,7.86091063353106,-17.4007379070685));
#43613=CARTESIAN_POINT('Ctrl Pts',(-47.0476351836161,7.96778846203953,-17.6519066560223));
#43614=CARTESIAN_POINT('Ctrl Pts',(-47.0517168740913,8.0348517437553,-17.8085785791225));
#43615=CARTESIAN_POINT('Ctrl Pts',(-47.0558659103499,8.08885825268645,-17.9346102696999));
#43616=CARTESIAN_POINT('Ctrl Pts',(-47.0594481061716,8.12943201619854,-18.0292450533832));
#43617=CARTESIAN_POINT('Ctrl Pts',(-47.0627989499055,8.16331558501532,-18.1083105118728));
#43618=CARTESIAN_POINT('Ctrl Pts',(-47.065699715029,8.19044455332856,-18.1716594129134));
#43619=CARTESIAN_POINT('Ctrl Pts',(-47.0915481899381,8.42112550168468,-18.7107584271862));
#43620=CARTESIAN_POINT('Ctrl Pts',(-47.1795150098835,8.86475935936997,-19.7614149232649));
#43621=CARTESIAN_POINT('Ctrl Pts',(-47.3620548986719,9.42469340784848,-21.4020513833473));
#43622=CARTESIAN_POINT('Ctrl Pts',(-47.4583992990562,9.68081121232479,-22.554207420914));
#43623=CARTESIAN_POINT('Ctrl Pts',(-47.4898086194942,9.79586248166539,-23.2865755238212));
#43624=CARTESIAN_POINT('Ctrl Pts',(-47.501349742819,9.83847812537408,-23.5883713749792));
#43625=CARTESIAN_POINT('Ctrl Pts',(-47.5222830062559,9.899624865415,-24.1758236534797));
#43626=CARTESIAN_POINT('Ctrl Pts',(-47.5525794688505,9.95672557240012,-25.1849747235455));
#43627=CARTESIAN_POINT('Ctrl Pts',(-47.5791316427958,9.93345826502849,-26.554952963881));
#43628=CARTESIAN_POINT('Ctrl Pts',(-47.5910145312468,9.84915846139396,-28.0887083936959));
#43629=CARTESIAN_POINT('Ctrl Pts',(-47.590154490986,9.81302209147109,-29.0338517263358));
#43630=CARTESIAN_POINT('Ctrl Pts',(-47.5885328811147,9.81147315537453,-29.5440203080735));
#43631=CARTESIAN_POINT('Ctrl Pts',(-47.5879832531315,9.81101342556759,-29.6742051600839));
#43632=CARTESIAN_POINT('Ctrl Pts',(-47.586159408563,9.80992869543475,-29.9250303861287));
#43633=CARTESIAN_POINT('Ctrl Pts',(-47.5811779859765,9.8074963975209,-30.3685920642081));
#43634=CARTESIAN_POINT('Ctrl Pts',(-47.5649066278992,9.80080875659515,-31.2513375375534));
#43635=CARTESIAN_POINT('Ctrl Pts',(-47.5285387694553,9.78697953291634,-32.5117857886755));
#43636=CARTESIAN_POINT('Ctrl Pts',(-47.487944364367,9.77080234221746,-33.7653306238441));
#43637=CARTESIAN_POINT('Ctrl Pts',(-47.4609716571189,9.75914312276783,-34.7638900742689));
#43638=CARTESIAN_POINT('Ctrl Pts',(-47.4506615003537,9.75421317547709,-35.2614394808298));
#43639=CARTESIAN_POINT('Ctrl Pts',(-47.4446011455489,9.75108103893098,-35.6349289491052));
#43640=CARTESIAN_POINT('Ctrl Pts',(-47.4407392943142,9.74903357004824,-35.886860521582));
#43641=CARTESIAN_POINT('Ctrl Pts',(-47.4337743681483,9.74501554106365,-36.3889623730522));
#43642=CARTESIAN_POINT('Ctrl Pts',(-47.4234052858481,9.73817027186817,-37.2665896791131));
#43643=CARTESIAN_POINT('Ctrl Pts',(-47.4086833908215,9.72585364518767,-39.016506618311));
#43644=CARTESIAN_POINT('Ctrl Pts',(-47.4018934869779,9.71812680820316,-40.5149077728951));
#43645=CARTESIAN_POINT('Ctrl Pts',(-47.3945431296122,9.71450015756152,-41.7677065187014));
#43646=CARTESIAN_POINT('Ctrl Pts',(-47.3920533546265,9.71297629043158,-42.1459383835886));
#43647=CARTESIAN_POINT('Ctrl Pts',(-47.3884471775193,9.7105222723979,-42.6476858082887));
#43648=CARTESIAN_POINT('Ctrl Pts',(-47.3847526214039,9.70792387566558,-43.1496599707732));
#43649=CARTESIAN_POINT('Ctrl Pts',(-47.380166200749,9.70470411107148,-43.7761346809352));
#43650=CARTESIAN_POINT('Ctrl Pts',(-47.3753391603478,9.70180347230122,-44.5263353855605));
#43651=CARTESIAN_POINT('Ctrl Pts',(-47.3724027140093,9.70095069186048,-45.1495947593217));
#43652=CARTESIAN_POINT('Ctrl Pts',(-47.3710255206844,9.70166790288393,-45.6468710869082));
#43653=CARTESIAN_POINT('Ctrl Pts',(-47.3705541460537,9.7030148028798,-46.0190618603836));
#43654=CARTESIAN_POINT('Ctrl Pts',(-47.3707232711661,9.70528492627313,-46.3904531500575));
#43655=CARTESIAN_POINT('Ctrl Pts',(-47.3719099595908,9.70968313810096,-46.8844091999811));
#43656=CARTESIAN_POINT('Ctrl Pts',(-47.3739920794671,9.71471544780657,-47.2535610007287));
#43657=CARTESIAN_POINT('Ctrl Pts',(-47.377042747569,9.72110569989881,-47.6220828227915));
#43658=CARTESIAN_POINT('Ctrl Pts',(-47.379394710066,9.72663118277781,-47.8555473010797));
#43659=CARTESIAN_POINT('Ctrl Pts',(-47.3850814028465,9.74293475389079,-48.3357425678953));
#43660=CARTESIAN_POINT('Ctrl Pts',(-47.3974607951798,9.78260342253114,-49.1848346622388));
#43661=CARTESIAN_POINT('Ctrl Pts',(-47.420861741289,9.85863948788479,-50.4372610284887));
#43662=CARTESIAN_POINT('Ctrl Pts',(-47.4551721471118,9.93471239285828,-51.9965477521186));
#43663=CARTESIAN_POINT('Ctrl Pts',(-47.4807755546611,9.94130590937094,-53.0752907530237));
#43664=CARTESIAN_POINT('Ctrl Pts',(-47.4973496509146,9.91947610813647,-53.7640655738369));
#43665=CARTESIAN_POINT('Ctrl Pts',(-47.504696395322,9.90424908173486,-54.0693324798308));
#43666=CARTESIAN_POINT('Ctrl Pts',(-47.5209704879564,9.85681016982776,-54.6478353651674));
#43667=CARTESIAN_POINT('Ctrl Pts',(-47.5527040090638,9.7389428317153,-55.6299312386107));
#43668=CARTESIAN_POINT('Ctrl Pts',(-47.6218994130365,9.43391335290437,-57.4385708087684));
#43669=CARTESIAN_POINT('Ctrl Pts',(-47.6718410018616,9.27979124975618,-58.7266178134533));
#43670=CARTESIAN_POINT('Ctrl Pts',(-47.6932325704654,9.32938585408278,-59.4923571602097));
#43671=CARTESIAN_POINT('Ctrl Pts',(-47.6956163076311,9.33731312674235,-59.6059273236726));
#43672=CARTESIAN_POINT('Ctrl Pts',(-47.7000531835202,9.35552167504649,-59.8224323611747));
#43673=CARTESIAN_POINT('Ctrl Pts',(-47.7067957930165,9.39549614861372,-60.2091251275057));
#43674=CARTESIAN_POINT('Ctrl Pts',(-47.7166992431684,9.50539796378372,-60.9859887116099));
#43675=CARTESIAN_POINT('Ctrl Pts',(-47.7214561246767,9.69581790910098,-61.8918098640388));
#43676=CARTESIAN_POINT('Ctrl Pts',(-47.7231340239658,9.94076524943754,-62.8064520549017));
#43677=CARTESIAN_POINT('Ctrl Pts',(-47.7235728164878,10.0968205414922,-63.3237784091988));
#43678=CARTESIAN_POINT('Ctrl Pts',(-47.7239244868068,10.2075530885451,-63.6692185723788));
#43679=CARTESIAN_POINT('Ctrl Pts',(-47.7241919849669,10.2830958246665,-63.8996767464525));
#43680=CARTESIAN_POINT('Ctrl Pts',(-47.7245395261178,10.3610953015556,-64.1301952062868));
#43681=CARTESIAN_POINT('Ctrl Pts',(-47.7249565011536,10.4313567498936,-64.3320134772627));
#43682=CARTESIAN_POINT('Ctrl Pts',(-47.725233940366,10.4720545332634,-64.4473499295881));
#43683=CARTESIAN_POINT('Ctrl Pts',(-47.7256936092775,10.533626264635,-64.6203343662188));
#43684=CARTESIAN_POINT('Ctrl Pts',(-47.7261710234038,10.5860392702119,-64.764516585462));
#43685=CARTESIAN_POINT('Ctrl Pts',(-47.7271481468912,10.6738842217373,-65.0025456548103));
#43686=CARTESIAN_POINT('Ctrl Pts',(-47.7292868500511,10.7565109011004,-65.2153884779408));
#43687=CARTESIAN_POINT('Ctrl Pts',(-47.7325281998836,10.9453778085396,-65.6651144802906));
#43688=CARTESIAN_POINT('Ctrl Pts',(-47.7375242496738,11.3132330337332,-66.4543442202597));
#43689=CARTESIAN_POINT('Ctrl Pts',(-47.742720043608,12.1924933283291,-68.093045861499));
#43690=CARTESIAN_POINT('Ctrl Pts',(-47.7397424623433,13.0906786878871,-69.5876056501862));
#43691=CARTESIAN_POINT('Ctrl Pts',(-47.7358676365723,13.7226372510541,-70.7892450656705));
#43692=CARTESIAN_POINT('Ctrl Pts',(-47.7361872582796,13.8514717103097,-71.0337783640329));
#43693=CARTESIAN_POINT('Ctrl Pts',(-47.7361421067603,14.1168124493924,-71.5362905071052));
#43694=CARTESIAN_POINT('Ctrl Pts',(-47.7363536649938,14.4467722109897,-72.1590041429464));
#43695=CARTESIAN_POINT('Ctrl Pts',(-47.7364328182178,14.8458083399649,-72.9096798690549));
#43696=CARTESIAN_POINT('Ctrl Pts',(-47.7366285550249,15.6452929518777,-74.4101506961281));
#43697=CARTESIAN_POINT('Ctrl Pts',(-47.7366429623231,16.3152035488193,-75.6629949469208));
#43698=CARTESIAN_POINT('Ctrl Pts',(-47.736456510601,17.286950025154,-77.4904073841466));
#43699=CARTESIAN_POINT('Ctrl Pts',(-47.7365375132694,17.7226385361246,-78.309695710462));
#43700=CARTESIAN_POINT('Ctrl Pts',(-47.7365375132698,18.1591601235141,-79.1306734125598));
#43701=CARTESIAN_POINT('Ctrl Pts',(-45.3967918070423,4.67699963232774,24.8307058930071));
#43702=CARTESIAN_POINT('Ctrl Pts',(-45.3969247453239,4.67701242909821,24.7818288627054));
#43703=CARTESIAN_POINT('Ctrl Pts',(-45.397064167043,4.67702585109274,24.7329529910232));
#43704=CARTESIAN_POINT('Ctrl Pts',(-45.3987107511635,4.67718419498956,24.1823696429735));
#43705=CARTESIAN_POINT('Ctrl Pts',(-45.399943482568,4.67733496035957,23.1782399075204));
#43706=CARTESIAN_POINT('Ctrl Pts',(-45.4027913014562,4.67770710281781,21.169693024752));
#43707=CARTESIAN_POINT('Ctrl Pts',(-45.4137513655735,4.67875883292481,19.6655344501099));
#43708=CARTESIAN_POINT('Ctrl Pts',(-45.4371439178203,4.68084188217039,18.4144909972096));
#43709=CARTESIAN_POINT('Ctrl Pts',(-45.4483529927258,4.68185556026981,17.9118184479246));
#43710=CARTESIAN_POINT('Ctrl Pts',(-45.4764839784317,4.6844273467736,16.9079162604237));
#43711=CARTESIAN_POINT('Ctrl Pts',(-45.5368339980899,4.68993785502906,15.1540506288512));
#43712=CARTESIAN_POINT('Ctrl Pts',(-45.5943262619857,4.69496910524554,13.651732361177));
#43713=CARTESIAN_POINT('Ctrl Pts',(-45.6306532223048,4.69773716630875,12.3966160910634));
#43714=CARTESIAN_POINT('Ctrl Pts',(-45.645533067266,4.69882553265937,11.8954011378803));
#43715=CARTESIAN_POINT('Ctrl Pts',(-45.6759652827717,4.70090494360455,10.8931907311465));
#43716=CARTESIAN_POINT('Ctrl Pts',(-45.7137310016318,4.70327483834507,9.64032794844271));
#43717=CARTESIAN_POINT('Ctrl Pts',(-45.7537367904843,4.70557261803631,8.13584025276354));
#43718=CARTESIAN_POINT('Ctrl Pts',(-45.7736012586385,4.70662765532891,7.13125052478055));
#43719=CARTESIAN_POINT('Ctrl Pts',(-45.7828654989878,4.70710029618373,6.50345235752316));
#43720=CARTESIAN_POINT('Ctrl Pts',(-45.786317932379,4.70725494412154,6.25304043598331));
#43721=CARTESIAN_POINT('Ctrl Pts',(-45.79232155606,4.70744926658238,5.75176951392184));
#43722=CARTESIAN_POINT('Ctrl Pts',(-45.8005821236953,4.70752015725955,4.87308667096534));
#43723=CARTESIAN_POINT('Ctrl Pts',(-45.8090583297727,4.70690178131339,3.11300099992041));
#43724=CARTESIAN_POINT('Ctrl Pts',(-45.8057997026327,4.70604569953201,1.60676663184952));
#43725=CARTESIAN_POINT('Ctrl Pts',(-45.801541792903,4.70626009274662,0.548402311047068));
#43726=CARTESIAN_POINT('Ctrl Pts',(-45.800987058998,4.70628635093447,0.422265412886293));
#43727=CARTESIAN_POINT('Ctrl Pts',(-45.7996982292011,4.70633332612108,0.170242135982571));
#43728=CARTESIAN_POINT('Ctrl Pts',(-45.7969864778771,4.70640749724397,-0.270319621179316));
#43729=CARTESIAN_POINT('Ctrl Pts',(-45.7919117308241,4.70649545803417,-0.898565940448079));
#43730=CARTESIAN_POINT('Ctrl Pts',(-45.7841763362845,4.70665066661472,-1.65059668736111));
#43731=CARTESIAN_POINT('Ctrl Pts',(-45.7720979368721,4.70695598006177,-2.65209326123843));
#43732=CARTESIAN_POINT('Ctrl Pts',(-45.7544067252159,4.70769649167174,-3.90228908918057));
#43733=CARTESIAN_POINT('Ctrl Pts',(-45.7390897014505,4.70882200721035,-4.90310426061235));
#43734=CARTESIAN_POINT('Ctrl Pts',(-45.7296261817282,4.70977477222109,-5.53090732296519));
#43735=CARTESIAN_POINT('Ctrl Pts',(-45.7268366532521,4.70748289314281,-5.8148845586905));
#43736=CARTESIAN_POINT('Ctrl Pts',(-45.7244657734331,4.69424688991172,-6.35268126287957));
#43737=CARTESIAN_POINT('Ctrl Pts',(-45.7265689277227,4.6545344809692,-7.27701819244823));
#43738=CARTESIAN_POINT('Ctrl Pts',(-45.7354526397734,4.58310519728748,-8.51387914878369));
#43739=CARTESIAN_POINT('Ctrl Pts',(-45.7212919559776,4.56554752860145,-9.64670319162602));
#43740=CARTESIAN_POINT('Ctrl Pts',(-45.6837627054695,4.60905344849388,-10.3800545643896));
#43741=CARTESIAN_POINT('Ctrl Pts',(-45.6525098638216,4.65242437433776,-10.7834717441486));
#43742=CARTESIAN_POINT('Ctrl Pts',(-45.6333676049592,4.68066429919607,-10.9800027379942));
#43743=CARTESIAN_POINT('Ctrl Pts',(-45.6175442952074,4.7045672444496,-11.1264413626487));
#43744=CARTESIAN_POINT('Ctrl Pts',(-45.6058880023824,4.72274561546546,-11.2308040278533));
#43745=CARTESIAN_POINT('Ctrl Pts',(-45.5793699186064,4.76188153157013,-11.4380718933958));
#43746=CARTESIAN_POINT('Ctrl Pts',(-45.5250898332709,4.83937214468783,-11.8069446789524));
#43747=CARTESIAN_POINT('Ctrl Pts',(-45.3906594720488,5.0258697792546,-12.5625029020933));
#43748=CARTESIAN_POINT('Ctrl Pts',(-45.158745326719,5.36769124802376,-13.7059503803668));
#43749=CARTESIAN_POINT('Ctrl Pts',(-44.969591291523,5.74461147330062,-14.8067575155667));
#43750=CARTESIAN_POINT('Ctrl Pts',(-44.8704275478205,6.01905615197813,-15.5628579938208));
#43751=CARTESIAN_POINT('Ctrl Pts',(-44.8123138665661,6.20768107447676,-16.0721633411231));
#43752=CARTESIAN_POINT('Ctrl Pts',(-44.7788699687686,6.35515843082492,-16.4599600676233));
#43753=CARTESIAN_POINT('Ctrl Pts',(-44.7583146261796,6.47997019558751,-16.7835552998439));
#43754=CARTESIAN_POINT('Ctrl Pts',(-44.7557554874463,6.52050151786484,-16.8810245148453));
#43755=CARTESIAN_POINT('Ctrl Pts',(-44.7489789344751,6.61425689484792,-17.0979643074361));
#43756=CARTESIAN_POINT('Ctrl Pts',(-44.7451500186526,6.71482824858523,-17.3131211918334));
#43757=CARTESIAN_POINT('Ctrl Pts',(-44.7421629759046,6.82454748409996,-17.536656251571));
#43758=CARTESIAN_POINT('Ctrl Pts',(-44.7409682498287,6.89588792145546,-17.6774709268476));
#43759=CARTESIAN_POINT('Ctrl Pts',(-44.7402504896582,6.95474132705015,-17.7915647827595));
#43760=CARTESIAN_POINT('Ctrl Pts',(-44.7398618658818,6.9996531379746,-17.8776153760358));
#43761=CARTESIAN_POINT('Ctrl Pts',(-44.7396424466105,7.03772449674589,-17.9498189774081));
#43762=CARTESIAN_POINT('Ctrl Pts',(-44.7395285895074,7.06853977631745,-18.0078479715581));
#43763=CARTESIAN_POINT('Ctrl Pts',(-44.738940858362,7.33248078330128,-18.5026887600909));
#43764=CARTESIAN_POINT('Ctrl Pts',(-44.7475478523009,7.89770799509759,-19.4959453393272));
#43765=CARTESIAN_POINT('Ctrl Pts',(-44.77859896707,8.75275826442582,-21.1108797897797));
#43766=CARTESIAN_POINT('Ctrl Pts',(-44.8079240027748,9.21771067855626,-22.3235170660312));
#43767=CARTESIAN_POINT('Ctrl Pts',(-44.822182301373,9.42261513598022,-23.1341165708057));
#43768=CARTESIAN_POINT('Ctrl Pts',(-44.8295413571494,9.49226918962049,-23.4355351762691));
#43769=CARTESIAN_POINT('Ctrl Pts',(-44.8486440692701,9.60622383888513,-24.0416682028876));
#43770=CARTESIAN_POINT('Ctrl Pts',(-44.8919587890394,9.73932723050289,-25.0765185835468));
#43771=CARTESIAN_POINT('Ctrl Pts',(-44.9691138795149,9.78755568820071,-26.4855691463327));
#43772=CARTESIAN_POINT('Ctrl Pts',(-45.0569316107679,9.74764456518795,-28.0488624674195));
#43773=CARTESIAN_POINT('Ctrl Pts',(-45.0988599204631,9.72631169784832,-29.0068894234387));
#43774=CARTESIAN_POINT('Ctrl Pts',(-45.1140632449712,9.73093911688483,-29.5227854550886));
#43775=CARTESIAN_POINT('Ctrl Pts',(-45.117241485544,9.73183657866296,-29.6591174681343));
#43776=CARTESIAN_POINT('Ctrl Pts',(-45.1228617630355,9.7323434200145,-29.9189198025019));
#43777=CARTESIAN_POINT('Ctrl Pts',(-45.1308676185089,9.73035583683325,-30.3782608199284));
#43778=CARTESIAN_POINT('Ctrl Pts',(-45.140335332486,9.71607778341234,-31.2861753032791));
#43779=CARTESIAN_POINT('Ctrl Pts',(-45.1397869098246,9.67435802849875,-32.5682626669705));
#43780=CARTESIAN_POINT('Ctrl Pts',(-45.1324405558967,9.62395212007861,-33.8230375358978));
#43781=CARTESIAN_POINT('Ctrl Pts',(-45.1295733860487,9.58976473289804,-34.8105640708621));
#43782=CARTESIAN_POINT('Ctrl Pts',(-45.130384517476,9.57657466323373,-35.2983868395446));
#43783=CARTESIAN_POINT('Ctrl Pts',(-45.1322694980909,9.56878906202912,-35.6631965396283));
#43784=CARTESIAN_POINT('Ctrl Pts',(-45.1336556288892,9.56343674678396,-35.9164128013516));
#43785=CARTESIAN_POINT('Ctrl Pts',(-45.1367645565076,9.55304305372151,-36.4169831933688));
#43786=CARTESIAN_POINT('Ctrl Pts',(-45.1430480250175,9.53547359998068,-37.2937852133888));
#43787=CARTESIAN_POINT('Ctrl Pts',(-45.1574629516336,9.50320056041596,-39.0397848560149));
#43788=CARTESIAN_POINT('Ctrl Pts',(-45.1692248551232,9.48228635093581,-40.5346106375694));
#43789=CARTESIAN_POINT('Ctrl Pts',(-45.1740013159767,9.47012749911255,-41.7837555766233));
#43790=CARTESIAN_POINT('Ctrl Pts',(-45.1749544288447,9.46608915424261,-42.1616592520973));
#43791=CARTESIAN_POINT('Ctrl Pts',(-45.1755256992377,9.46052268500198,-42.6624065251111));
#43792=CARTESIAN_POINT('Ctrl Pts',(-45.1757255102865,9.454990384937,-43.1633834694535));
#43793=CARTESIAN_POINT('Ctrl Pts',(-45.1754206775425,9.4484490105667,-43.7883710672532));
#43794=CARTESIAN_POINT('Ctrl Pts',(-45.1746548077921,9.44216516589298,-44.5364876519143));
#43795=CARTESIAN_POINT('Ctrl Pts',(-45.1740879321796,9.43903630354368,-45.1577233309101));
#43796=CARTESIAN_POINT('Ctrl Pts',(-45.1739047017952,9.43825076570018,-45.6531846096039));
#43797=CARTESIAN_POINT('Ctrl Pts',(-45.173970432579,9.43864791268071,-46.0239274066856));
#43798=CARTESIAN_POINT('Ctrl Pts',(-45.1742986039458,9.44014687421711,-46.393783701766));
#43799=CARTESIAN_POINT('Ctrl Pts',(-45.1751670329734,9.44376679547408,-46.8855678935479));
#43800=CARTESIAN_POINT('Ctrl Pts',(-45.1763968106901,9.44848910792274,-47.2529795752224));
#43801=CARTESIAN_POINT('Ctrl Pts',(-45.1781381234655,9.4547797656765,-47.6196453890339));
#43802=CARTESIAN_POINT('Ctrl Pts',(-45.1793506736816,9.46029382162677,-47.8514512849776));
#43803=CARTESIAN_POINT('Ctrl Pts',(-45.1818745708335,9.47688635047598,-48.3288845642534));
#43804=CARTESIAN_POINT('Ctrl Pts',(-45.1866624941977,9.51787745918839,-49.1737568330917));
#43805=CARTESIAN_POINT('Ctrl Pts',(-45.1948598210357,9.59793065018163,-50.4223165193547));
#43806=CARTESIAN_POINT('Ctrl Pts',(-45.2085164273352,9.68189629520511,-51.9798747925369));
#43807=CARTESIAN_POINT('Ctrl Pts',(-45.2214687681134,9.69459317093489,-53.0593760433816));
#43808=CARTESIAN_POINT('Ctrl Pts',(-45.231365032527,9.6765817016563,-53.7491408978133));
#43809=CARTESIAN_POINT('Ctrl Pts',(-45.235844382703,9.66329571846373,-54.0529210224869));
#43810=CARTESIAN_POINT('Ctrl Pts',(-45.2461663565889,9.61995793369472,-54.6299665971305));
#43811=CARTESIAN_POINT('Ctrl Pts',(-45.2670530690536,9.50987452788591,-55.6099392070727));
#43812=CARTESIAN_POINT('Ctrl Pts',(-45.3151012174976,9.22120407775639,-57.4179601559676));
#43813=CARTESIAN_POINT('Ctrl Pts',(-45.3510003949752,9.07568722001837,-58.7106356831304));
#43814=CARTESIAN_POINT('Ctrl Pts',(-45.3673316143288,9.12817116247798,-59.484360913267));
#43815=CARTESIAN_POINT('Ctrl Pts',(-45.3691636132104,9.13652638436252,-59.5987350105386));
#43816=CARTESIAN_POINT('Ctrl Pts',(-45.3726709599828,9.15544384876885,-59.8168408868926));
#43817=CARTESIAN_POINT('Ctrl Pts',(-45.3782408371613,9.1964363465885,-60.206054760062));
#43818=CARTESIAN_POINT('Ctrl Pts',(-45.3874159203442,9.30742768779234,-60.9870282365347));
#43819=CARTESIAN_POINT('Ctrl Pts',(-45.3941164500462,9.49720122186125,-61.8953425943457));
#43820=CARTESIAN_POINT('Ctrl Pts',(-45.3986858966782,9.74037100393175,-62.810549390693));
#43821=CARTESIAN_POINT('Ctrl Pts',(-45.4007811970171,9.89520149739856,-63.3275246686143));
#43822=CARTESIAN_POINT('Ctrl Pts',(-45.4021139182939,10.0050961863,-63.672469087878));
#43823=CARTESIAN_POINT('Ctrl Pts',(-45.4029951100338,10.0800837113633,-63.902528470281));
#43824=CARTESIAN_POINT('Ctrl Pts',(-45.4038793121767,10.1575337164629,-64.1325474137763));
#43825=CARTESIAN_POINT('Ctrl Pts',(-45.4046791309213,10.2273415532064,-64.3338420419547));
#43826=CARTESIAN_POINT('Ctrl Pts',(-45.4051469880807,10.2677891911925,-64.4488546655427));
#43827=CARTESIAN_POINT('Ctrl Pts',(-45.4058623292339,10.3289966359398,-64.6213298159851));
#43828=CARTESIAN_POINT('Ctrl Pts',(-45.40648665549,10.3811273464558,-64.7650352495097));
#43829=CARTESIAN_POINT('Ctrl Pts',(-45.4075997403387,10.4685582900223,-65.0022279615426));
#43830=CARTESIAN_POINT('Ctrl Pts',(-45.4096705636337,10.5510978670919,-65.2151667368062));
#43831=CARTESIAN_POINT('Ctrl Pts',(-45.4128271094035,10.7396355313408,-65.6645805689296));
#43832=CARTESIAN_POINT('Ctrl Pts',(-45.4175108483084,11.1070949519467,-66.4536193008161));
#43833=CARTESIAN_POINT('Ctrl Pts',(-45.4219924228712,11.9858538302058,-68.0919758206631));
#43834=CARTESIAN_POINT('Ctrl Pts',(-45.4188767922422,12.8841409741353,-69.5866322626632));
#43835=CARTESIAN_POINT('Ctrl Pts',(-45.415583326104,13.516191818909,-70.7884170998586));
#43836=CARTESIAN_POINT('Ctrl Pts',(-45.4158701096126,13.6449908510542,-71.0329220887169));
#43837=CARTESIAN_POINT('Ctrl Pts',(-45.415847067481,13.910302727703,-71.5354152219409));
#43838=CARTESIAN_POINT('Ctrl Pts',(-45.4160399532874,14.2402265724916,-72.1580992078819));
#43839=CARTESIAN_POINT('Ctrl Pts',(-45.4161097683259,14.6392468323838,-72.9087535210569));
#43840=CARTESIAN_POINT('Ctrl Pts',(-45.416265759434,15.4387251486653,-74.4091941654481));
#43841=CARTESIAN_POINT('Ctrl Pts',(-45.4162454052114,16.1086751496886,-75.6620602523283));
#43842=CARTESIAN_POINT('Ctrl Pts',(-45.4160811373678,17.0804492222374,-77.4895263141691));
#43843=CARTESIAN_POINT('Ctrl Pts',(-45.4161506449042,17.5161264810383,-78.3088023967617));
#43844=CARTESIAN_POINT('Ctrl Pts',(-45.416150644904,17.9526480684277,-79.1297800988595));
#43845=CARTESIAN_POINT('Ctrl Pts',(-43.5414773952673,4.53448753146326,24.8306508196532));
#43846=CARTESIAN_POINT('Ctrl Pts',(-43.5416047669445,4.53449721364328,24.7817720471109));
#43847=CARTESIAN_POINT('Ctrl Pts',(-43.5417383544304,4.53450737193678,24.7328943885228));
#43848=CARTESIAN_POINT('Ctrl Pts',(-43.543315880609,4.53462714710031,24.1822910231318));
#43849=CARTESIAN_POINT('Ctrl Pts',(-43.5444934277257,4.53472020364173,23.1781405139521));
#43850=CARTESIAN_POINT('Ctrl Pts',(-43.547213232334,4.5349402426484,21.1695567924396));
#43851=CARTESIAN_POINT('Ctrl Pts',(-43.5577141297553,4.53573626681342,19.665396739518));
#43852=CARTESIAN_POINT('Ctrl Pts',(-43.580141872167,4.53741690684206,18.4143536264076));
#43853=CARTESIAN_POINT('Ctrl Pts',(-43.5908845213517,4.53822766910346,17.9115809741758));
#43854=CARTESIAN_POINT('Ctrl Pts',(-43.6178388001956,4.54027275181146,16.9076098476224));
#43855=CARTESIAN_POINT('Ctrl Pts',(-43.6756604074524,4.54466059694902,15.1537552531732));
#43856=CARTESIAN_POINT('Ctrl Pts',(-43.7308046180445,4.54878265955304,13.6517813104176));
#43857=CARTESIAN_POINT('Ctrl Pts',(-43.7657324230018,4.55126962212829,12.3970993819365));
#43858=CARTESIAN_POINT('Ctrl Pts',(-43.7800502239518,4.55227609946025,11.8960613948514));
#43859=CARTESIAN_POINT('Ctrl Pts',(-43.8093651510474,4.55429402046486,10.8941089443398));
#43860=CARTESIAN_POINT('Ctrl Pts',(-43.845806874139,4.55674166000825,9.64145045637587));
#43861=CARTESIAN_POINT('Ctrl Pts',(-43.8844367131125,4.55926806744004,8.1369499361624));
#43862=CARTESIAN_POINT('Ctrl Pts',(-43.9036277914651,4.56049111790417,7.13221967877992));
#43863=CARTESIAN_POINT('Ctrl Pts',(-43.9125642966023,4.56105117356098,6.5042781166866));
#43864=CARTESIAN_POINT('Ctrl Pts',(-43.9158997499813,4.56125301868147,6.25398521843682));
#43865=CARTESIAN_POINT('Ctrl Pts',(-43.9217210164265,4.56157889868081,5.75280983079089));
#43866=CARTESIAN_POINT('Ctrl Pts',(-43.9297820679564,4.56195876363265,4.87427062012176));
#43867=CARTESIAN_POINT('Ctrl Pts',(-43.938205566208,4.56211186615648,3.11402949048081));
#43868=CARTESIAN_POINT('Ctrl Pts',(-43.9350456348124,4.56163244268552,1.60721235589409));
#43869=CARTESIAN_POINT('Ctrl Pts',(-43.9305449025619,4.56149728983932,0.548044744225739));
#43870=CARTESIAN_POINT('Ctrl Pts',(-43.92995163912,4.56148146887285,0.421924264229309));
#43871=CARTESIAN_POINT('Ctrl Pts',(-43.9285495522382,4.56144306894868,0.169861106284108));
#43872=CARTESIAN_POINT('Ctrl Pts',(-43.9255547920404,4.56136199309973,-0.270760078205373));
#43873=CARTESIAN_POINT('Ctrl Pts',(-43.9198775066915,4.56119887486765,-0.899129331533509));
#43874=CARTESIAN_POINT('Ctrl Pts',(-43.911291515231,4.56096508359156,-1.65145592914514));
#43875=CARTESIAN_POINT('Ctrl Pts',(-43.8981044383047,4.56057963339869,-2.65340542950447));
#43876=CARTESIAN_POINT('Ctrl Pts',(-43.8795254386815,4.56002921357857,-3.90436111785173));
#43877=CARTESIAN_POINT('Ctrl Pts',(-43.8649534269833,4.55953271096634,-4.90614818740102));
#43878=CARTESIAN_POINT('Ctrl Pts',(-43.8567126149039,4.55926409820865,-5.5342146452382));
#43879=CARTESIAN_POINT('Ctrl Pts',(-43.8543503288117,4.55733097510175,-5.80798547657267));
#43880=CARTESIAN_POINT('Ctrl Pts',(-43.8526460470249,4.5476465780853,-6.33496129077482));
#43881=CARTESIAN_POINT('Ctrl Pts',(-43.8556772819808,4.51933786023616,-7.24583280436193));
#43882=CARTESIAN_POINT('Ctrl Pts',(-43.8664394386739,4.46763897095714,-8.48976964485138));
#43883=CARTESIAN_POINT('Ctrl Pts',(-43.8575645087604,4.45187518229086,-9.66162616485918));
#43884=CARTESIAN_POINT('Ctrl Pts',(-43.8264841504034,4.4812317939519,-10.439780141466));
#43885=CARTESIAN_POINT('Ctrl Pts',(-43.7996564267498,4.51183958327011,-10.8729601445167));
#43886=CARTESIAN_POINT('Ctrl Pts',(-43.7829273783394,4.53207292227548,-11.0855147011133));
#43887=CARTESIAN_POINT('Ctrl Pts',(-43.7689707331577,4.54933119378543,-11.2445899642726));
#43888=CARTESIAN_POINT('Ctrl Pts',(-43.7588133500233,4.56283159515784,-11.3649302891771));
#43889=CARTESIAN_POINT('Ctrl Pts',(-43.7361617811776,4.59013029690435,-11.5975385803844));
#43890=CARTESIAN_POINT('Ctrl Pts',(-43.6905885533692,4.64136130536106,-12.0073322160453));
#43891=CARTESIAN_POINT('Ctrl Pts',(-43.5793977696364,4.75541578831326,-12.8203071653748));
#43892=CARTESIAN_POINT('Ctrl Pts',(-43.3841981059185,4.9490682713273,-13.9775243432551));
#43893=CARTESIAN_POINT('Ctrl Pts',(-43.2172359706947,5.17142115793501,-15.0210579656182));
#43894=CARTESIAN_POINT('Ctrl Pts',(-43.1255566330017,5.35275489925325,-15.7202982956007));
#43895=CARTESIAN_POINT('Ctrl Pts',(-43.0701105163936,5.48340085420829,-16.187028048169));
#43896=CARTESIAN_POINT('Ctrl Pts',(-43.0357728430286,5.59339004773325,-16.5380745918997));
#43897=CARTESIAN_POINT('Ctrl Pts',(-43.0120736898623,5.69205831004088,-16.828969321626));
#43898=CARTESIAN_POINT('Ctrl Pts',(-43.0064495536189,5.72452332379515,-16.9184974593357));
#43899=CARTESIAN_POINT('Ctrl Pts',(-42.9929620042525,5.80202720051158,-17.1189555795941));
#43900=CARTESIAN_POINT('Ctrl Pts',(-42.9800430618435,5.88864111055256,-17.3213604480838));
#43901=CARTESIAN_POINT('Ctrl Pts',(-42.9661972175604,5.98623251149259,-17.5339384305494));
#43902=CARTESIAN_POINT('Ctrl Pts',(-42.9574124453944,6.05092529343878,-17.6688699894998));
#43903=CARTESIAN_POINT('Ctrl Pts',(-42.9501947049534,6.10496966356968,-17.7786718266522));
#43904=CARTESIAN_POINT('Ctrl Pts',(-42.944713353776,6.14654508271073,-17.861727557838));
#43905=CARTESIAN_POINT('Ctrl Pts',(-42.9400770881554,6.18205237853153,-17.9315973336786));
#43906=CARTESIAN_POINT('Ctrl Pts',(-42.9363275774573,6.21094945034024,-17.987854648448));
#43907=CARTESIAN_POINT('Ctrl Pts',(-42.9042578360259,6.45927552362335,-18.4681475521462));
#43908=CARTESIAN_POINT('Ctrl Pts',(-42.8354204510704,7.01884438328396,-19.4483385870696));
#43909=CARTESIAN_POINT('Ctrl Pts',(-42.7235818122568,7.91026567127129,-21.0487658406634));
#43910=CARTESIAN_POINT('Ctrl Pts',(-42.6615545965536,8.4235782780184,-22.2516132514597));
#43911=CARTESIAN_POINT('Ctrl Pts',(-42.6397937596963,8.66346632602533,-23.0651674066825));
#43912=CARTESIAN_POINT('Ctrl Pts',(-42.6373184823834,8.74403332351748,-23.3530168149133));
#43913=CARTESIAN_POINT('Ctrl Pts',(-42.6400465652739,8.88929551511328,-23.9425206307659));
#43914=CARTESIAN_POINT('Ctrl Pts',(-42.6686855051693,9.09087494114976,-24.9504735243279));
#43915=CARTESIAN_POINT('Ctrl Pts',(-42.7586291051712,9.26186522797534,-26.3468890062045));
#43916=CARTESIAN_POINT('Ctrl Pts',(-42.8930054067009,9.35687651394788,-27.9245675859953));
#43917=CARTESIAN_POINT('Ctrl Pts',(-42.9668170921629,9.39917625537599,-28.9088150521134));
#43918=CARTESIAN_POINT('Ctrl Pts',(-42.9956359053881,9.43022741933181,-29.443973003435));
#43919=CARTESIAN_POINT('Ctrl Pts',(-43.0017926813387,9.43761783172049,-29.5826600934523));
#43920=CARTESIAN_POINT('Ctrl Pts',(-43.0138136196532,9.4499284676199,-29.8480333340984));
#43921=CARTESIAN_POINT('Ctrl Pts',(-43.0338459223275,9.46699420480363,-30.3160542990129));
#43922=CARTESIAN_POINT('Ctrl Pts',(-43.0703214349251,9.48410743700334,-31.2394572305364));
#43923=CARTESIAN_POINT('Ctrl Pts',(-43.1136297167087,9.47282905295429,-32.5365077571059));
#43924=CARTESIAN_POINT('Ctrl Pts',(-43.1505483501123,9.4437724363275,-33.7968559783388));
#43925=CARTESIAN_POINT('Ctrl Pts',(-43.179756915703,9.42602709605934,-34.7830704643692));
#43926=CARTESIAN_POINT('Ctrl Pts',(-43.1948523344428,9.42133520497665,-35.268262685831));
#43927=CARTESIAN_POINT('Ctrl Pts',(-43.2066091516522,9.42030918799427,-35.6304498875428));
#43928=CARTESIAN_POINT('Ctrl Pts',(-43.2145227328819,9.41945632756122,-35.8853449854496));
#43929=CARTESIAN_POINT('Ctrl Pts',(-43.2304076818416,9.41760776333118,-36.3872449299346));
#43930=CARTESIAN_POINT('Ctrl Pts',(-43.2581874912136,9.41378261879008,-37.2671370953687));
#43931=CARTESIAN_POINT('Ctrl Pts',(-43.3123675870467,9.40523996947063,-39.0179770168176));
#43932=CARTESIAN_POINT('Ctrl Pts',(-43.3516470087399,9.3984466337369,-40.5163790979968));
#43933=CARTESIAN_POINT('Ctrl Pts',(-43.3751017626546,9.39620560352966,-41.7682292525567));
#43934=CARTESIAN_POINT('Ctrl Pts',(-43.3814199683655,9.39507916206091,-42.1468284953897));
#43935=CARTESIAN_POINT('Ctrl Pts',(-43.3886805914299,9.39311251970767,-42.648723821498));
#43936=CARTESIAN_POINT('Ctrl Pts',(-43.3952225192057,9.39095754326053,-43.1509067571471));
#43937=CARTESIAN_POINT('Ctrl Pts',(-43.4021768476301,9.3881987826084,-43.7775575981803));
#43938=CARTESIAN_POINT('Ctrl Pts',(-43.4089425171841,9.38565114231246,-44.5278758127687));
#43939=CARTESIAN_POINT('Ctrl Pts',(-43.4135801355141,9.38488373368826,-45.1511124442861));
#43940=CARTESIAN_POINT('Ctrl Pts',(-43.4168965709671,9.38552163166002,-45.6482817329203));
#43941=CARTESIAN_POINT('Ctrl Pts',(-43.4192263128526,9.38672700188353,-46.0203539813832));
#43942=CARTESIAN_POINT('Ctrl Pts',(-43.4214469215391,9.38876730446991,-46.3915879436735));
#43943=CARTESIAN_POINT('Ctrl Pts',(-43.4243304847402,9.39273174188816,-46.8852820141213));
#43944=CARTESIAN_POINT('Ctrl Pts',(-43.4264592644717,9.39728689787286,-47.2541897357405));
#43945=CARTESIAN_POINT('Ctrl Pts',(-43.4286836829519,9.40308146710722,-47.6224425609724));
#43946=CARTESIAN_POINT('Ctrl Pts',(-43.429990352853,9.40814613749297,-47.8560422350782));
#43947=CARTESIAN_POINT('Ctrl Pts',(-43.4319672217862,9.42328710943704,-48.3363028422295));
#43948=CARTESIAN_POINT('Ctrl Pts',(-43.4339862099306,9.46037407270681,-49.1855495348585));
#43949=CARTESIAN_POINT('Ctrl Pts',(-43.4341047106985,9.53162435862161,-50.4380086570674));
#43950=CARTESIAN_POINT('Ctrl Pts',(-43.4341668879683,9.60155648143506,-51.9969456558317));
#43951=CARTESIAN_POINT('Ctrl Pts',(-43.4371547465252,9.60478703772803,-53.0749378134565));
#43952=CARTESIAN_POINT('Ctrl Pts',(-43.4410236568199,9.5814192426866,-53.763015054666));
#43953=CARTESIAN_POINT('Ctrl Pts',(-43.4428228358991,9.56558565266787,-54.0680510784552));
#43954=CARTESIAN_POINT('Ctrl Pts',(-43.4470784464119,9.51700097357967,-54.646136857561));
#43955=CARTESIAN_POINT('Ctrl Pts',(-43.4558884498313,9.39728206386044,-55.6276963317156));
#43956=CARTESIAN_POINT('Ctrl Pts',(-43.4773355348517,9.08917547582348,-57.435843844612));
#43957=CARTESIAN_POINT('Ctrl Pts',(-43.4929180935316,8.93280683980113,-58.7247135338309));
#43958=CARTESIAN_POINT('Ctrl Pts',(-43.502951944175,8.98141711200675,-59.4917463672902));
#43959=CARTESIAN_POINT('Ctrl Pts',(-43.5040887115791,8.98923400294946,-59.6053713579836));
#43960=CARTESIAN_POINT('Ctrl Pts',(-43.5064241734618,9.00724889639743,-59.822026795714));
#43961=CARTESIAN_POINT('Ctrl Pts',(-43.5105090660535,9.04695435480541,-60.208917902705));
#43962=CARTESIAN_POINT('Ctrl Pts',(-43.5187094594682,9.15655669920001,-60.9860555524913));
#43963=CARTESIAN_POINT('Ctrl Pts',(-43.5276864039261,9.34700515261771,-61.8918809221699));
#43964=CARTESIAN_POINT('Ctrl Pts',(-43.5356257866396,9.59205287880273,-62.8063113263271));
#43965=CARTESIAN_POINT('Ctrl Pts',(-43.5396263340133,9.74814896875034,-63.3234516794069));
#43966=CARTESIAN_POINT('Ctrl Pts',(-43.5420730449082,9.85888623633741,-63.668749484404));
#43967=CARTESIAN_POINT('Ctrl Pts',(-43.543644714704,9.93442527720585,-63.8991082023449));
#43968=CARTESIAN_POINT('Ctrl Pts',(-43.5451267245491,10.0124096431432,-64.1295221636211));
#43969=CARTESIAN_POINT('Ctrl Pts',(-43.5463409253479,10.0826455753854,-64.3312457131275));
#43970=CARTESIAN_POINT('Ctrl Pts',(-43.5470109321769,10.1233250296039,-64.4465274780185));
#43971=CARTESIAN_POINT('Ctrl Pts',(-43.5479928422882,10.184865352795,-64.6194294836793));
#43972=CARTESIAN_POINT('Ctrl Pts',(-43.5487597636013,10.2372439185951,-64.7635425338402));
#43973=CARTESIAN_POINT('Ctrl Pts',(-43.5499804671287,10.325018907116,-65.001458961203));
#43974=CARTESIAN_POINT('Ctrl Pts',(-43.5520500501327,10.4075489819384,-65.2142421704268));
#43975=CARTESIAN_POINT('Ctrl Pts',(-43.555204266958,10.5962475318124,-65.6638448096376));
#43976=CARTESIAN_POINT('Ctrl Pts',(-43.5597525060502,10.9638366542822,-66.4529293315174));
#43977=CARTESIAN_POINT('Ctrl Pts',(-43.5638198409699,11.8427641573275,-68.0914988092095));
#43978=CARTESIAN_POINT('Ctrl Pts',(-43.5606853444821,12.7410165411229,-69.5860763169363));
#43979=CARTESIAN_POINT('Ctrl Pts',(-43.5579024385739,13.37315894584,-70.7877805666056));
#43980=CARTESIAN_POINT('Ctrl Pts',(-43.5581710713026,13.5019721513977,-71.0323018745553));
#43981=CARTESIAN_POINT('Ctrl Pts',(-43.5581777217519,13.767308255904,-71.5348068904238));
#43982=CARTESIAN_POINT('Ctrl Pts',(-43.558363918352,14.0972510551101,-72.1575083352297));
#43983=CARTESIAN_POINT('Ctrl Pts',(-43.5584264256019,14.4962797472263,-72.908176648061));
#43984=CARTESIAN_POINT('Ctrl Pts',(-43.5585385417129,15.2957534471709,-74.4086378087151));
#43985=CARTESIAN_POINT('Ctrl Pts',(-43.558469611058,15.9656725151421,-75.6614891722437));
#43986=CARTESIAN_POINT('Ctrl Pts',(-43.5583278325102,16.9374352319471,-77.4889175968542));
#43987=CARTESIAN_POINT('Ctrl Pts',(-43.5583885600327,17.3731177442317,-78.3082009283048));
#43988=CARTESIAN_POINT('Ctrl Pts',(-43.5583885600325,17.8096393316212,-79.1291786304031));
#43989=CARTESIAN_POINT('Ctrl Pts',(-41.6855749463137,4.40659539398005,24.8306029215866));
#43990=CARTESIAN_POINT('Ctrl Pts',(-41.685697662467,4.40660227643802,24.7817226223589));
#43991=CARTESIAN_POINT('Ctrl Pts',(-41.6858263644354,4.40660949804129,24.7328433953815));
#43992=CARTESIAN_POINT('Ctrl Pts',(-41.687346263331,4.40669468880106,24.1822225641872));
#43993=CARTESIAN_POINT('Ctrl Pts',(-41.6884979401384,4.40673956543124,23.1780567543321));
#43994=CARTESIAN_POINT('Ctrl Pts',(-41.691168825236,4.40683205281526,21.1694396153191));
#43995=CARTESIAN_POINT('Ctrl Pts',(-41.7012849291027,4.40739933760772,19.6652749989752));
#43996=CARTESIAN_POINT('Ctrl Pts',(-41.7228065880957,4.4087035664667,18.4142278522954));
#43997=CARTESIAN_POINT('Ctrl Pts',(-41.7331204592441,4.40932365972109,17.9113569622441));
#43998=CARTESIAN_POINT('Ctrl Pts',(-41.7590060536787,4.41087272201821,16.907319682426));
#43999=CARTESIAN_POINT('Ctrl Pts',(-41.8145312035812,4.414201634924,15.1534845454099));
#44000=CARTESIAN_POINT('Ctrl Pts',(-41.8673890990281,4.41746314725499,13.651850155213));
#44001=CARTESIAN_POINT('Ctrl Pts',(-41.9007195299706,4.4196756879196,12.3975888332274));
#44002=CARTESIAN_POINT('Ctrl Pts',(-41.9143680521242,4.42060006605874,11.8967219557013));
#44003=CARTESIAN_POINT('Ctrl Pts',(-41.9422657521244,4.4225475988363,10.8950145380524));
#44004=CARTESIAN_POINT('Ctrl Pts',(-41.9768607225259,4.4250514613291,9.6425418442172));
#44005=CARTESIAN_POINT('Ctrl Pts',(-42.0134492212083,4.42777879406171,8.13801797377742));
#44006=CARTESIAN_POINT('Ctrl Pts',(-42.031566864206,4.42915768851939,7.13314986501666));
#44007=CARTESIAN_POINT('Ctrl Pts',(-42.0399866776811,4.4298009317554,6.50507269877867));
#44008=CARTESIAN_POINT('Ctrl Pts',(-42.0431248666837,4.43004717070963,6.25491000507619));
#44009=CARTESIAN_POINT('Ctrl Pts',(-42.0485825634162,4.43050090764894,5.75384465386732));
#44010=CARTESIAN_POINT('Ctrl Pts',(-42.0560865636054,4.43118750202483,4.87546769899893));
#44011=CARTESIAN_POINT('Ctrl Pts',(-42.063708946106,4.43212033692018,3.11507335553097));
#44012=CARTESIAN_POINT('Ctrl Pts',(-42.0603647805318,4.43205410986387,1.60759953127178));
#44013=CARTESIAN_POINT('Ctrl Pts',(-42.0559272801265,4.43154123524431,0.547546226208736));
#44014=CARTESIAN_POINT('Ctrl Pts',(-42.0553411834889,4.43147526155733,0.421316876104222));
#44015=CARTESIAN_POINT('Ctrl Pts',(-42.0539523129837,4.43131874832274,0.169050265537001));
#44016=CARTESIAN_POINT('Ctrl Pts',(-42.0509798249934,4.43098586061686,-0.271900904983259));
#44017=CARTESIAN_POINT('Ctrl Pts',(-42.0453476764959,4.43035149565878,-0.900620055919381));
#44018=CARTESIAN_POINT('Ctrl Pts',(-42.0368686096194,4.42941053987935,-1.65330233669832));
#44019=CARTESIAN_POINT('Ctrl Pts',(-42.0239588406089,4.42796549860846,-2.65549737470179));
#44020=CARTESIAN_POINT('Ctrl Pts',(-42.0060682271433,4.42597160743345,-3.90642587730085));
#44021=CARTESIAN_POINT('Ctrl Pts',(-41.9926014280487,4.4244184970362,-4.90790089596296));
#44022=CARTESIAN_POINT('Ctrl Pts',(-41.9852842444455,4.42356328852968,-5.53526790519391));
#44023=CARTESIAN_POINT('Ctrl Pts',(-41.9830897219956,4.42221824706501,-5.79917433259166));
#44024=CARTESIAN_POINT('Ctrl Pts',(-41.9810825063314,4.41633986280381,-6.315422455717));
#44025=CARTESIAN_POINT('Ctrl Pts',(-41.9823681306211,4.39969099804006,-7.21277145484061));
#44026=CARTESIAN_POINT('Ctrl Pts',(-41.9896449906298,4.36892455429229,-8.46250372528066));
#44027=CARTESIAN_POINT('Ctrl Pts',(-41.9821520153673,4.35789994862493,-9.67049901943245));
#44028=CARTESIAN_POINT('Ctrl Pts',(-41.9576210819876,4.3745848449589,-10.4909114220271));
#44029=CARTESIAN_POINT('Ctrl Pts',(-41.9364549378075,4.39279740316707,-10.9526158538038));
#44030=CARTESIAN_POINT('Ctrl Pts',(-41.9232258854634,4.40503170868416,-11.1807898585064));
#44031=CARTESIAN_POINT('Ctrl Pts',(-41.9121637037425,4.41554754816524,-11.3522122103185));
#44032=CARTESIAN_POINT('Ctrl Pts',(-41.9043363905,4.42361119608237,-11.4848721190377));
#44033=CARTESIAN_POINT('Ctrl Pts',(-41.8875072833387,4.4384065006293,-11.7382331079967));
#44034=CARTESIAN_POINT('Ctrl Pts',(-41.8549592713017,4.46324441376506,-12.1817395961442));
#44035=CARTESIAN_POINT('Ctrl Pts',(-41.7787962092932,4.50967578248564,-13.0456684600629));
#44036=CARTESIAN_POINT('Ctrl Pts',(-41.644491098764,4.58263430774086,-14.2285222813806));
#44037=CARTESIAN_POINT('Ctrl Pts',(-41.5123917809733,4.68998798291981,-15.2366382479619));
#44038=CARTESIAN_POINT('Ctrl Pts',(-41.4287824925274,4.79553689828114,-15.8936194208614));
#44039=CARTESIAN_POINT('Ctrl Pts',(-41.3747256809767,4.87640790074795,-16.3280864374078));
#44040=CARTESIAN_POINT('Ctrl Pts',(-41.3366524575088,4.95035921181498,-16.6510048310789));
#44041=CARTESIAN_POINT('Ctrl Pts',(-41.306835620299,5.02081124413835,-16.9176146481003));
#44042=CARTESIAN_POINT('Ctrl Pts',(-41.29636387782,5.04509520112619,-17.0047436605908));
#44043=CARTESIAN_POINT('Ctrl Pts',(-41.2730346722212,5.10353261298984,-17.196868830241));
#44044=CARTESIAN_POINT('Ctrl Pts',(-41.2480790791988,5.17084493684142,-17.3934626491004));
#44045=CARTESIAN_POINT('Ctrl Pts',(-41.221105495172,5.24831389192612,-17.6003988774604));
#44046=CARTESIAN_POINT('Ctrl Pts',(-41.2035751962912,5.30040427107532,-17.7323825235609));
#44047=CARTESIAN_POINT('Ctrl Pts',(-41.1891277198281,5.34431580294902,-17.8399805850786));
#44048=CARTESIAN_POINT('Ctrl Pts',(-41.1781000088454,5.37829931059263,-17.9215089454721));
#44049=CARTESIAN_POINT('Ctrl Pts',(-41.1687506376316,5.40748252995808,-17.9901864120133));
#44050=CARTESIAN_POINT('Ctrl Pts',(-41.1611793212934,5.43133205518555,-18.0455404137636));
#44051=CARTESIAN_POINT('Ctrl Pts',(-41.0963218209191,5.63677452637474,-18.5184584440352));
#44052=CARTESIAN_POINT('Ctrl Pts',(-40.9564136843565,6.11712912367197,-19.4926969375005));
#44053=CARTESIAN_POINT('Ctrl Pts',(-40.7364366289171,6.9157475288387,-21.0886818032411));
#44054=CARTESIAN_POINT('Ctrl Pts',(-40.6149000229783,7.38772813226633,-22.2673531899013));
#44055=CARTESIAN_POINT('Ctrl Pts',(-40.5669825701007,7.62255736913357,-23.0490607398952));
#44056=CARTESIAN_POINT('Ctrl Pts',(-40.556831256611,7.70335393494949,-23.3180003280109));
#44057=CARTESIAN_POINT('Ctrl Pts',(-40.5433299693075,7.86078183394624,-23.8747078218839));
#44058=CARTESIAN_POINT('Ctrl Pts',(-40.5459948282985,8.11005511183186,-24.8289667580384));
#44059=CARTESIAN_POINT('Ctrl Pts',(-40.6076287795505,8.40807181386579,-26.1759437191406));
#44060=CARTESIAN_POINT('Ctrl Pts',(-40.7347495145975,8.68290591483088,-27.7493495807299));
#44061=CARTESIAN_POINT('Ctrl Pts',(-40.8164187078509,8.82327999821301,-28.7669616509389));
#44062=CARTESIAN_POINT('Ctrl Pts',(-40.8492236913612,8.89606935974853,-29.3296269754071));
#44063=CARTESIAN_POINT('Ctrl Pts',(-40.8559901601149,8.91325409450142,-29.4678481197618));
#44064=CARTESIAN_POINT('Ctrl Pts',(-40.8700356227369,8.94447667853886,-29.73607891955));
#44065=CARTESIAN_POINT('Ctrl Pts',(-40.8949093233339,8.99390826626215,-30.2073921688695));
#44066=CARTESIAN_POINT('Ctrl Pts',(-40.9461990154241,9.0718486267278,-31.1392426571425));
#44067=CARTESIAN_POINT('Ctrl Pts',(-41.0213279503794,9.13631858149522,-32.4475458748229));
#44068=CARTESIAN_POINT('Ctrl Pts',(-41.0947609597759,9.16910478169614,-33.7171654407122));
#44069=CARTESIAN_POINT('Ctrl Pts',(-41.1509081769705,9.19432417390162,-34.7085603115485));
#44070=CARTESIAN_POINT('Ctrl Pts',(-41.1779978329913,9.20935303612885,-35.1956042420512));
#44071=CARTESIAN_POINT('Ctrl Pts',(-41.1979259101171,9.22261206042192,-35.5589384775174));
#44072=CARTESIAN_POINT('Ctrl Pts',(-41.211274985297,9.23163148260346,-35.815843256208));
#44073=CARTESIAN_POINT('Ctrl Pts',(-41.2379556572264,9.24831886907607,-36.3209572959123));
#44074=CARTESIAN_POINT('Ctrl Pts',(-41.2843674816221,9.2749306091751,-37.206592034575));
#44075=CARTESIAN_POINT('Ctrl Pts',(-41.374064639626,9.31856056441366,-38.9678356583997));
#44076=CARTESIAN_POINT('Ctrl Pts',(-41.4394366532432,9.34455345009808,-40.4743298755513));
#44077=CARTESIAN_POINT('Ctrl Pts',(-41.4804556071417,9.36439928361108,-41.7326381762914));
#44078=CARTESIAN_POINT('Ctrl Pts',(-41.4917681728629,9.36962188655343,-42.1126309299343));
#44079=CARTESIAN_POINT('Ctrl Pts',(-41.5052363141583,9.37537120989589,-42.6169053118342));
#44080=CARTESIAN_POINT('Ctrl Pts',(-41.5177026046486,9.38048383318957,-43.1215402313297));
#44081=CARTESIAN_POINT('Ctrl Pts',(-41.5315381423871,9.385893671131,-43.7515528341479));
#44082=CARTESIAN_POINT('Ctrl Pts',(-41.5457753993936,9.39159865784897,-44.5062999306404));
#44083=CARTESIAN_POINT('Ctrl Pts',(-41.5560294813494,9.39633244195201,-45.1335791991821));
#44084=CARTESIAN_POINT('Ctrl Pts',(-41.5634795732993,9.40047075649581,-45.6341556731554));
#44085=CARTESIAN_POINT('Ctrl Pts',(-41.5687465317506,9.40384986790816,-46.0088895953954));
#44086=CARTESIAN_POINT('Ctrl Pts',(-41.5737465074904,9.40759620424152,-46.3828880382925));
#44087=CARTESIAN_POINT('Ctrl Pts',(-41.5801306758304,9.41319667576749,-46.88040080413));
#44088=CARTESIAN_POINT('Ctrl Pts',(-41.5846779335584,9.41823077142094,-47.2523538003496));
#44089=CARTESIAN_POINT('Ctrl Pts',(-41.5891880026032,9.42398765962361,-47.6237819174283));
#44090=CARTESIAN_POINT('Ctrl Pts',(-41.5919840811149,9.42881699202896,-47.8606476760656));
#44091=CARTESIAN_POINT('Ctrl Pts',(-41.5967687945331,9.4425848061764,-48.3462104845544));
#44092=CARTESIAN_POINT('Ctrl Pts',(-41.6032500935833,9.47507599431753,-49.2037625717664));
#44093=CARTESIAN_POINT('Ctrl Pts',(-41.6083296045376,9.53401971082211,-50.4641957400867));
#44094=CARTESIAN_POINT('Ctrl Pts',(-41.6115416025726,9.58327908023829,-52.0270286219866));
#44095=CARTESIAN_POINT('Ctrl Pts',(-41.6142570143924,9.57141240308287,-53.1035174134462));
#44096=CARTESIAN_POINT('Ctrl Pts',(-41.6170842694937,9.53940035558117,-53.7894131631721));
#44097=CARTESIAN_POINT('Ctrl Pts',(-41.6181932184546,9.51929615382017,-54.097309136534));
#44098=CARTESIAN_POINT('Ctrl Pts',(-41.6204158196274,9.46175833377061,-54.6781916945254));
#44099=CARTESIAN_POINT('Ctrl Pts',(-41.6241355094009,9.32499922588705,-55.6639665235512));
#44100=CARTESIAN_POINT('Ctrl Pts',(-41.6321391320519,8.98141565581387,-57.4737578573867));
#44101=CARTESIAN_POINT('Ctrl Pts',(-41.6352564780507,8.80416763399032,-58.7542741719814));
#44102=CARTESIAN_POINT('Ctrl Pts',(-41.6419319708265,8.84554828365744,-59.5066281603445));
#44103=CARTESIAN_POINT('Ctrl Pts',(-41.6427197098762,8.85240436315506,-59.6187556373831));
#44104=CARTESIAN_POINT('Ctrl Pts',(-41.6444588222317,8.86878566359322,-59.8324321931772));
#44105=CARTESIAN_POINT('Ctrl Pts',(-41.6477959507849,8.906130579617,-60.2145958717469));
#44106=CARTESIAN_POINT('Ctrl Pts',(-41.6555290946326,9.01309581026938,-60.9839390616392));
#44107=CARTESIAN_POINT('Ctrl Pts',(-41.6656789092045,9.2046257784976,-61.884804523698));
#44108=CARTESIAN_POINT('Ctrl Pts',(-41.6752684815886,9.45314319759352,-62.7978123507762));
#44109=CARTESIAN_POINT('Ctrl Pts',(-41.6801807428335,9.61165849753839,-63.3153935693162));
#44110=CARTESIAN_POINT('Ctrl Pts',(-41.6831468915368,9.72402519255565,-63.661473322807));
#44111=CARTESIAN_POINT('Ctrl Pts',(-41.6850374865527,9.80064280446529,-63.8924835916954));
#44112=CARTESIAN_POINT('Ctrl Pts',(-41.6867870113969,9.87966992968769,-64.1237362136409));
#44113=CARTESIAN_POINT('Ctrl Pts',(-41.6881799527362,9.95075883245909,-64.3263615763983));
#44114=CARTESIAN_POINT('Ctrl Pts',(-41.688934145285,9.9919032359808,-64.4422061061361));
#44115=CARTESIAN_POINT('Ctrl Pts',(-41.6900235328282,10.054115637533,-64.6159981699555));
#44116=CARTESIAN_POINT('Ctrl Pts',(-41.6908383052638,10.1069972284883,-64.7609540810492));
#44117=CARTESIAN_POINT('Ctrl Pts',(-41.6920728116426,10.195489344907,-65.0003621966698));
#44118=CARTESIAN_POINT('Ctrl Pts',(-41.6940697097662,10.2780415895599,-65.2128739119397));
#44119=CARTESIAN_POINT('Ctrl Pts',(-41.6971009990176,10.467137609276,-65.6629225402255));
#44120=CARTESIAN_POINT('Ctrl Pts',(-41.7013784550244,10.835093913543,-66.4521842042188));
#44121=CARTESIAN_POINT('Ctrl Pts',(-41.7049787078459,11.7144976447062,-68.0912567734202));
#44122=CARTESIAN_POINT('Ctrl Pts',(-41.7019352411704,12.6125834775925,-69.585655539249));
#44123=CARTESIAN_POINT('Ctrl Pts',(-41.6996350389558,13.2448030238341,-70.7871589920456));
#44124=CARTESIAN_POINT('Ctrl Pts',(-41.6998795464537,13.3736551022578,-71.0317206123756));
#44125=CARTESIAN_POINT('Ctrl Pts',(-41.6999072801692,13.6390412747428,-71.5342543097902));
#44126=CARTESIAN_POINT('Ctrl Pts',(-41.7000799865726,13.9690255241614,-72.1569980731772));
#44127=CARTESIAN_POINT('Ctrl Pts',(-41.7001336613318,14.36807282733,-72.9076991264268));
#44128=CARTESIAN_POINT('Ctrl Pts',(-41.7002071861,15.1675386808873,-74.4082071762659));
#44129=CARTESIAN_POINT('Ctrl Pts',(-41.7001019708216,15.837371218953,-75.6610214368742));
#44130=CARTESIAN_POINT('Ctrl Pts',(-41.6999820122622,16.809089882623,-77.4883620781338));
#44131=CARTESIAN_POINT('Ctrl Pts',(-41.7000326001874,17.2447800067055,-78.3076624344991));
#44132=CARTESIAN_POINT('Ctrl Pts',(-41.7000326001874,17.681301594095,-79.1286401365976));
#44133=CARTESIAN_POINT('Ctrl Pts',(-39.8297931480168,4.30089380366595,24.830602047834));
#44134=CARTESIAN_POINT('Ctrl Pts',(-39.8299114630833,4.3008990929334,24.78172171557));
#44135=CARTESIAN_POINT('Ctrl Pts',(-39.8300355500048,4.30090464320175,24.7328424414219));
#44136=CARTESIAN_POINT('Ctrl Pts',(-39.8315008348087,4.30097010912121,24.1822216618942));
#44137=CARTESIAN_POINT('Ctrl Pts',(-39.8326341752565,4.30100217254688,23.1780621652815));
#44138=CARTESIAN_POINT('Ctrl Pts',(-39.8352790867674,4.30106615227246,21.1694431088377));
#44139=CARTESIAN_POINT('Ctrl Pts',(-39.8450305426849,4.30150215534326,19.6652809261295));
#44140=CARTESIAN_POINT('Ctrl Pts',(-39.8656602898903,4.30251651664904,18.4142310178032));
#44141=CARTESIAN_POINT('Ctrl Pts',(-39.8755574820151,4.30299596277146,17.9113461412146));
#44142=CARTESIAN_POINT('Ctrl Pts',(-39.9004164841773,4.30418812240353,16.9073028735776));
#44143=CARTESIAN_POINT('Ctrl Pts',(-39.9537335816,4.30674885227799,15.1534825452192));
#44144=CARTESIAN_POINT('Ctrl Pts',(-40.0043389427622,4.3092914420343,13.6519164127763));
#44145=CARTESIAN_POINT('Ctrl Pts',(-40.0359637219453,4.31108023983322,12.3977176469952));
#44146=CARTESIAN_POINT('Ctrl Pts',(-40.0488823383933,4.31183394637067,11.8968749770987));
#44147=CARTESIAN_POINT('Ctrl Pts',(-40.0751861247578,4.31344186128328,10.8951953012143));
#44148=CARTESIAN_POINT('Ctrl Pts',(-40.1076610674584,4.31553762482537,9.64275117357418));
#44149=CARTESIAN_POINT('Ctrl Pts',(-40.1418550022536,4.31784800138233,8.13821998910642));
#44150=CARTESIAN_POINT('Ctrl Pts',(-40.1587271976532,4.31902826059171,7.13335908880077));
#44151=CARTESIAN_POINT('Ctrl Pts',(-40.1665508599929,4.31958193706928,6.50527516075616));
#44152=CARTESIAN_POINT('Ctrl Pts',(-40.1694560805316,4.31979833457379,6.25515470745086));
#44153=CARTESIAN_POINT('Ctrl Pts',(-40.1744696474126,4.32021173111455,5.7541330082611));
#44154=CARTESIAN_POINT('Ctrl Pts',(-40.1812597490853,4.32087297286246,4.87583060632696));
#44155=CARTESIAN_POINT('Ctrl Pts',(-40.1877615170938,4.32187781283288,3.11542901410488));
#44156=CARTESIAN_POINT('Ctrl Pts',(-40.1841517730371,4.3219093923555,1.60788699549147));
#44157=CARTESIAN_POINT('Ctrl Pts',(-40.1800414129611,4.32131088132128,0.547597544998743));
#44158=CARTESIAN_POINT('Ctrl Pts',(-40.1795013359313,4.32123244923683,0.421302512279844));
#44159=CARTESIAN_POINT('Ctrl Pts',(-40.1782294712075,4.32104491163839,0.168935192359385));
#44160=CARTESIAN_POINT('Ctrl Pts',(-40.175524627641,4.32064205722609,-0.27218276183076));
#44161=CARTESIAN_POINT('Ctrl Pts',(-40.1704276659856,4.31987394138445,-0.901034338282424));
#44162=CARTESIAN_POINT('Ctrl Pts',(-40.1627832733404,4.31873536139517,-1.65383635728535));
#44163=CARTESIAN_POINT('Ctrl Pts',(-40.1511337820403,4.31702074322043,-2.65598405249863));
#44164=CARTESIAN_POINT('Ctrl Pts',(-40.1349501757378,4.31472508907572,-3.90657868690618));
#44165=CARTESIAN_POINT('Ctrl Pts',(-40.1226251363579,4.3131393526332,-4.90749312754089));
#44166=CARTESIAN_POINT('Ctrl Pts',(-40.1158543990754,4.31237494775209,-5.53413996057266));
#44167=CARTESIAN_POINT('Ctrl Pts',(-40.1135869601886,4.31165753439819,-5.79060421533873));
#44168=CARTESIAN_POINT('Ctrl Pts',(-40.1104842025132,4.30889665464121,-6.29867272758451));
#44169=CARTESIAN_POINT('Ctrl Pts',(-40.1079320500244,4.30140928720403,-7.18557117664585));
#44170=CARTESIAN_POINT('Ctrl Pts',(-40.1075002949748,4.28773211170499,-8.43919536745521));
#44171=CARTESIAN_POINT('Ctrl Pts',(-40.0979431800538,4.28250603011998,-9.6737737294806));
#44172=CARTESIAN_POINT('Ctrl Pts',(-40.0794180589679,4.2896159913547,-10.5256234324252));
#44173=CARTESIAN_POINT('Ctrl Pts',(-40.0644505017986,4.29757952688169,-11.0088597276714));
#44174=CARTESIAN_POINT('Ctrl Pts',(-40.0553407674673,4.30298489891383,-11.2490523951628));
#44175=CARTESIAN_POINT('Ctrl Pts',(-40.0478046614143,4.30765034982014,-11.4299264392524));
#44176=CARTESIAN_POINT('Ctrl Pts',(-40.0427004166551,4.31074429421119,-11.5669600302684));
#44177=CARTESIAN_POINT('Ctrl Pts',(-40.0323767708002,4.31529495958614,-11.8298741459896));
#44178=CARTESIAN_POINT('Ctrl Pts',(-40.0138927680509,4.32018324612044,-12.288832822566));
#44179=CARTESIAN_POINT('Ctrl Pts',(-39.9745792624865,4.3211634986152,-13.1809544205443));
#44180=CARTESIAN_POINT('Ctrl Pts',(-39.9075100857676,4.32116438958334,-14.3942739237789));
#44181=CARTESIAN_POINT('Ctrl Pts',(-39.8243636709521,4.36339195578311,-15.4141826122897));
#44182=CARTESIAN_POINT('Ctrl Pts',(-39.7568993275666,4.42274128845835,-16.0696027064544));
#44183=CARTESIAN_POINT('Ctrl Pts',(-39.7088063807627,4.47133204515602,-16.5006483077442));
#44184=CARTESIAN_POINT('Ctrl Pts',(-39.6692619585097,4.51884981766233,-16.8181705647147));
#44185=CARTESIAN_POINT('Ctrl Pts',(-39.6346316045092,4.5655688528116,-17.0796880689598));
#44186=CARTESIAN_POINT('Ctrl Pts',(-39.6204120795866,4.58382912268261,-17.175690740393));
#44187=CARTESIAN_POINT('Ctrl Pts',(-39.5894669012688,4.62516231987957,-17.3766146318054));
#44188=CARTESIAN_POINT('Ctrl Pts',(-39.5553158916272,4.67215116259866,-17.5815260242127));
#44189=CARTESIAN_POINT('Ctrl Pts',(-39.5185800153218,4.72485428291418,-17.7931822188726));
#44190=CARTESIAN_POINT('Ctrl Pts',(-39.4946952607774,4.75998745770387,-17.9275952541007));
#44191=CARTESIAN_POINT('Ctrl Pts',(-39.4751042176496,4.78938719031116,-18.0366034819522));
#44192=CARTESIAN_POINT('Ctrl Pts',(-39.4601907595611,4.81205896222492,-18.1190253381994));
#44193=CARTESIAN_POINT('Ctrl Pts',(-39.4475935447712,4.83146010520306,-18.1882840561084));
#44194=CARTESIAN_POINT('Ctrl Pts',(-39.4374244274026,4.8472792986152,-18.244027993542));
#44195=CARTESIAN_POINT('Ctrl Pts',(-39.3504688559995,4.98336628900204,-18.719720209416));
#44196=CARTESIAN_POINT('Ctrl Pts',(-39.1701471321289,5.29569390328575,-19.6878533559967));
#44197=CARTESIAN_POINT('Ctrl Pts',(-38.9242229480404,5.82689686466538,-21.2532366026309));
#44198=CARTESIAN_POINT('Ctrl Pts',(-38.8059077773893,6.16859330004726,-22.3670328740001));
#44199=CARTESIAN_POINT('Ctrl Pts',(-38.7570216643074,6.36015803481956,-23.0814111966791));
#44200=CARTESIAN_POINT('Ctrl Pts',(-38.7447800238885,6.42923735981035,-23.328423449339));
#44201=CARTESIAN_POINT('Ctrl Pts',(-38.723820624919,6.57429412002019,-23.8426500143035));
#44202=CARTESIAN_POINT('Ctrl Pts',(-38.7039991705238,6.83111560382248,-24.7331385960951));
#44203=CARTESIAN_POINT('Ctrl Pts',(-38.7099306974958,7.20325016995822,-26.0161853728573));
#44204=CARTESIAN_POINT('Ctrl Pts',(-38.7505792606654,7.62202264051377,-27.5675741391084));
#44205=CARTESIAN_POINT('Ctrl Pts',(-38.7797668023837,7.86054302302213,-28.6152446982086));
#44206=CARTESIAN_POINT('Ctrl Pts',(-38.7892658775211,7.97746624359547,-29.2076491505204));
#44207=CARTESIAN_POINT('Ctrl Pts',(-38.7911525363579,8.00347609994022,-29.3415640528822));
#44208=CARTESIAN_POINT('Ctrl Pts',(-38.795568900938,8.05340115514498,-29.6075879530807));
#44209=CARTESIAN_POINT('Ctrl Pts',(-38.8043527904606,8.13629703152824,-30.0725680034506));
#44210=CARTESIAN_POINT('Ctrl Pts',(-38.8263682508179,8.28492022380721,-30.9967695748171));
#44211=CARTESIAN_POINT('Ctrl Pts',(-38.8686709923634,8.45617305599503,-32.3008431646847));
#44212=CARTESIAN_POINT('Ctrl Pts',(-38.9203939555227,8.59310886872018,-33.5776947955661));
#44213=CARTESIAN_POINT('Ctrl Pts',(-38.9637989885803,8.69480564673521,-34.5803683821298));
#44214=CARTESIAN_POINT('Ctrl Pts',(-38.9855148236409,8.74510155541343,-35.0749037451322));
#44215=CARTESIAN_POINT('Ctrl Pts',(-39.0016350899177,8.78356692726934,-35.4444375768675));
#44216=CARTESIAN_POINT('Ctrl Pts',(-39.0123957027471,8.80985696054819,-35.7026593968134));
#44217=CARTESIAN_POINT('Ctrl Pts',(-39.0349110126382,8.85998494195932,-36.2120466346827));
#44218=CARTESIAN_POINT('Ctrl Pts',(-39.0759897514108,8.94313733967483,-37.104355852086));
#44219=CARTESIAN_POINT('Ctrl Pts',(-39.1626367000569,9.09070470507714,-38.8797197070461));
#44220=CARTESIAN_POINT('Ctrl Pts',(-39.2343498384004,9.1889654345898,-40.3979241974921));
#44221=CARTESIAN_POINT('Ctrl Pts',(-39.2818954499488,9.25877965806356,-41.6660339213601));
#44222=CARTESIAN_POINT('Ctrl Pts',(-39.2950638878413,9.27834154057425,-42.0486116434629));
#44223=CARTESIAN_POINT('Ctrl Pts',(-39.3110379056122,9.3017834411066,-42.5567161560632));
#44224=CARTESIAN_POINT('Ctrl Pts',(-39.326088661976,9.32368226929647,-43.0652356268463));
#44225=CARTESIAN_POINT('Ctrl Pts',(-39.3434458658797,9.34832447909361,-43.7003231605712));
#44226=CARTESIAN_POINT('Ctrl Pts',(-39.362809408335,9.37425457532264,-44.4614473516942));
#44227=CARTESIAN_POINT('Ctrl Pts',(-39.3784480905642,9.39339504305688,-45.0942864763365));
#44228=CARTESIAN_POINT('Ctrl Pts',(-39.3910942576435,9.4075375084826,-45.5994493536755));
#44229=CARTESIAN_POINT('Ctrl Pts',(-39.4007552007379,9.41765522041657,-45.9776910996982));
#44230=CARTESIAN_POINT('Ctrl Pts',(-39.4107012674894,9.42736606118332,-46.3552617040635));
#44231=CARTESIAN_POINT('Ctrl Pts',(-39.4244828041639,9.43987014279348,-46.8576199079467));
#44232=CARTESIAN_POINT('Ctrl Pts',(-39.4355796726667,9.44891064666244,-47.2332959012991));
#44233=CARTESIAN_POINT('Ctrl Pts',(-39.4474131679077,9.45786884799196,-47.608522670452));
#44234=CARTESIAN_POINT('Ctrl Pts',(-39.4555075039778,9.46441277966897,-47.8486933692234));
#44235=CARTESIAN_POINT('Ctrl Pts',(-39.4722691301041,9.48038854409172,-48.3400075043167));
#44236=CARTESIAN_POINT('Ctrl Pts',(-39.5028365388771,9.51357355094779,-49.2068771604531));
#44237=CARTESIAN_POINT('Ctrl Pts',(-39.5486702333604,9.56588051029713,-50.4776982592062));
#44238=CARTESIAN_POINT('Ctrl Pts',(-39.6027707836672,9.59908376373866,-52.0484437744134));
#44239=CARTESIAN_POINT('Ctrl Pts',(-39.6355429012624,9.57401187231233,-53.1270087990632));
#44240=CARTESIAN_POINT('Ctrl Pts',(-39.6540971477978,9.53365496047467,-53.8133957215356));
#44241=CARTESIAN_POINT('Ctrl Pts',(-39.6616800978402,9.50902042983665,-54.1258915107586));
#44242=CARTESIAN_POINT('Ctrl Pts',(-39.6767805853012,9.44146978560207,-54.7119512819459));
#44243=CARTESIAN_POINT('Ctrl Pts',(-39.7028304779311,9.28487457519746,-55.7048841033207));
#44244=CARTESIAN_POINT('Ctrl Pts',(-39.7523611380775,8.89899646706934,-57.5182886098759));
#44245=CARTESIAN_POINT('Ctrl Pts',(-39.7831463768863,8.70030675270623,-58.7896356166503));
#44246=CARTESIAN_POINT('Ctrl Pts',(-39.7997801411076,8.73508473009655,-59.5229656801026));
#44247=CARTESIAN_POINT('Ctrl Pts',(-39.8016896555854,8.741017361795,-59.6336104409786));
#44248=CARTESIAN_POINT('Ctrl Pts',(-39.8052901413032,8.75581682568381,-59.8440440927058));
#44249=CARTESIAN_POINT('Ctrl Pts',(-39.8109597621908,8.79080107943052,-60.2212073384165));
#44250=CARTESIAN_POINT('Ctrl Pts',(-39.8200282135911,8.89479056849624,-60.9822394237097));
#44251=CARTESIAN_POINT('Ctrl Pts',(-39.8260360532955,9.0865192287289,-61.8779760087666));
#44252=CARTESIAN_POINT('Ctrl Pts',(-39.8295731896413,9.33765559955061,-62.7895320369173));
#44253=CARTESIAN_POINT('Ctrl Pts',(-39.8310212942597,9.49817191638174,-63.3075735756629));
#44254=CARTESIAN_POINT('Ctrl Pts',(-39.8319255508167,9.61193685091784,-63.6544547583156));
#44255=CARTESIAN_POINT('Ctrl Pts',(-39.8325232750647,9.68948855333687,-63.8861306959977));
#44256=CARTESIAN_POINT('Ctrl Pts',(-39.8331318185583,9.76943793851357,-64.1182399850882));
#44257=CARTESIAN_POINT('Ctrl Pts',(-39.8337018758477,9.84128825163668,-64.3217838167787));
#44258=CARTESIAN_POINT('Ctrl Pts',(-39.8340427347527,9.88285030071759,-64.4382012244413));
#44259=CARTESIAN_POINT('Ctrl Pts',(-39.8345719320016,9.9456683768302,-64.6128988734076));
#44260=CARTESIAN_POINT('Ctrl Pts',(-39.8350523314316,9.99900995718296,-64.7587123480466));
#44261=CARTESIAN_POINT('Ctrl Pts',(-39.8359396646288,10.0881584837466,-64.9996352209183));
#44262=CARTESIAN_POINT('Ctrl Pts',(-39.8374902700331,10.1706399387457,-65.2117876939817));
#44263=CARTESIAN_POINT('Ctrl Pts',(-39.8398170196311,10.3600045172887,-65.6621891819383));
#44264=CARTESIAN_POINT('Ctrl Pts',(-39.843131858082,10.7281843839988,-66.4514728099116));
#44265=CARTESIAN_POINT('Ctrl Pts',(-39.845876871811,11.6080767952086,-68.0909065229435));
#44266=CARTESIAN_POINT('Ctrl Pts',(-39.843327687577,12.5062924443932,-69.5851576688017));
#44267=CARTESIAN_POINT('Ctrl Pts',(-39.8413504014661,13.1386697797965,-70.7866057521726));
#44268=CARTESIAN_POINT('Ctrl Pts',(-39.8415361597441,13.2675599635809,-71.0312033519439));
#44269=CARTESIAN_POINT('Ctrl Pts',(-39.8415353492584,13.5330038135489,-71.5337768994219));
#44270=CARTESIAN_POINT('Ctrl Pts',(-39.8416622329038,13.8630346117925,-72.1565663160765));
#44271=CARTESIAN_POINT('Ctrl Pts',(-39.8417041928247,14.2621049670467,-72.907306052374));
#44272=CARTESIAN_POINT('Ctrl Pts',(-39.8417838427976,15.0615664520001,-74.4078651633378));
#44273=CARTESIAN_POINT('Ctrl Pts',(-39.8417435694573,15.7313146331549,-75.6606366493089));
#44274=CARTESIAN_POINT('Ctrl Pts',(-39.841647950285,16.7029874268988,-77.4878785996119));
#44275=CARTESIAN_POINT('Ctrl Pts',(-39.8416897698438,17.1386891158188,-78.307198653046));
#44276=CARTESIAN_POINT('Ctrl Pts',(-39.8416897698439,17.5752107032083,-79.1281763551445));
#44277=CARTESIAN_POINT('Ctrl Pts',(-37.9743804869919,4.21861863427918,24.8306265576595));
#44278=CARTESIAN_POINT('Ctrl Pts',(-37.9744933412749,4.21862296368332,24.781747004875));
#44279=CARTESIAN_POINT('Ctrl Pts',(-37.9746116996787,4.21862750610694,24.7328685159225));
#44280=CARTESIAN_POINT('Ctrl Pts',(-37.9760093878018,4.21868107839185,24.1822571666999));
#44281=CARTESIAN_POINT('Ctrl Pts',(-37.9770928025108,4.21871687976674,23.1781116141306));
#44282=CARTESIAN_POINT('Ctrl Pts',(-37.9796222523406,4.21879772051816,21.1695091063699));
#44283=CARTESIAN_POINT('Ctrl Pts',(-37.988923418268,4.21915417447705,19.6653556871867));
#44284=CARTESIAN_POINT('Ctrl Pts',(-38.0085896781781,4.21993578500939,18.4143085580057));
#44285=CARTESIAN_POINT('Ctrl Pts',(-38.0180265439753,4.2203080448418,17.9114693439527));
#44286=CARTESIAN_POINT('Ctrl Pts',(-38.0417320316029,4.22123855332113,16.9074600931303));
#44287=CARTESIAN_POINT('Ctrl Pts',(-38.092576449602,4.22323443097777,15.1536393156253));
#44288=CARTESIAN_POINT('Ctrl Pts',(-38.1408051880377,4.22516989518677,13.6519419426153));
#44289=CARTESIAN_POINT('Ctrl Pts',(-38.170903396427,4.22644947705509,12.3975570868814));
#44290=CARTESIAN_POINT('Ctrl Pts',(-38.1831929699881,4.22698018707274,11.8966377111797));
#44291=CARTESIAN_POINT('Ctrl Pts',(-38.2081999459129,4.22808605464995,10.8948432547909));
#44292=CARTESIAN_POINT('Ctrl Pts',(-38.2390434108757,4.2294918983112,9.64232897953741));
#44293=CARTESIAN_POINT('Ctrl Pts',(-38.2715056140244,4.23100759531148,8.13781350830912));
#44294=CARTESIAN_POINT('Ctrl Pts',(-38.2875179676639,4.2317702569467,7.13304930191504));
#44295=CARTESIAN_POINT('Ctrl Pts',(-38.2949489018608,4.23212573179239,6.50503800955867));
#44296=CARTESIAN_POINT('Ctrl Pts',(-38.2977099300648,4.23226189994421,6.25485919894676));
#44297=CARTESIAN_POINT('Ctrl Pts',(-38.3024790164624,4.23251304482732,5.75379011111632));
#44298=CARTESIAN_POINT('Ctrl Pts',(-38.3089479453886,4.23289290544923,4.8754362249382));
#44299=CARTESIAN_POINT('Ctrl Pts',(-38.3151739057549,4.23340331481503,3.11513220656035));
#44300=CARTESIAN_POINT('Ctrl Pts',(-38.3117375096816,4.23332952842037,1.60807604480747));
#44301=CARTESIAN_POINT('Ctrl Pts',(-38.3077338232431,4.23299020488926,0.548264881323011));
#44302=CARTESIAN_POINT('Ctrl Pts',(-38.3072081561105,4.23294628726474,0.422037778870473));
#44303=CARTESIAN_POINT('Ctrl Pts',(-38.3059713749947,4.23284144102519,0.169792824938136));
#44304=CARTESIAN_POINT('Ctrl Pts',(-38.3033435895393,4.23261728659212,-0.271125465382427));
#44305=CARTESIAN_POINT('Ctrl Pts',(-38.2983999561383,4.23218967685735,-0.899719883146217));
#44306=CARTESIAN_POINT('Ctrl Pts',(-38.2909903793428,4.23156156894473,-1.6523352386966));
#44307=CARTESIAN_POINT('Ctrl Pts',(-38.2797133192693,4.23061375891271,-2.65430127585317));
#44308=CARTESIAN_POINT('Ctrl Pts',(-38.2640680641888,4.22935135029831,-3.90488850894447));
#44309=CARTESIAN_POINT('Ctrl Pts',(-38.2521812332404,4.22846831850042,-4.90598421604601));
#44310=CARTESIAN_POINT('Ctrl Pts',(-38.245662932773,4.22803832190949,-5.53266413366317));
#44311=CARTESIAN_POINT('Ctrl Pts',(-38.2432660770742,4.22776094337687,-5.7850702330293));
#44312=CARTESIAN_POINT('Ctrl Pts',(-38.239157279881,4.22686154318823,-6.28877538383063));
#44313=CARTESIAN_POINT('Ctrl Pts',(-38.2333400682135,4.22459584850577,-7.1701007369905));
#44314=CARTESIAN_POINT('Ctrl Pts',(-38.2265369799843,4.22056807197913,-8.42604530220827));
#44315=CARTESIAN_POINT('Ctrl Pts',(-38.2152635068069,4.21879488566088,-9.67537062573929));
#44316=CARTESIAN_POINT('Ctrl Pts',(-38.2016123736228,4.22048906463511,-10.5446281636035));
#44317=CARTESIAN_POINT('Ctrl Pts',(-38.1916770114935,4.22252872692914,-11.0397205111789));
#44318=CARTESIAN_POINT('Ctrl Pts',(-38.1859173687779,4.22393808368096,-11.2865534428756));
#44319=CARTESIAN_POINT('Ctrl Pts',(-38.1812503236375,4.22516215592496,-11.4725327889825));
#44320=CARTESIAN_POINT('Ctrl Pts',(-38.1782132664989,4.22569598471026,-11.6083006574023));
#44321=CARTESIAN_POINT('Ctrl Pts',(-38.1724963236154,4.22539253894241,-11.8717389184555));
#44322=CARTESIAN_POINT('Ctrl Pts',(-38.1632652605988,4.22184588540865,-12.3312268093402));
#44323=CARTESIAN_POINT('Ctrl Pts',(-38.146644928951,4.2057839670911,-13.2294108148301));
#44324=CARTESIAN_POINT('Ctrl Pts',(-38.1209532574981,4.17591208670593,-14.462707710516));
#44325=CARTESIAN_POINT('Ctrl Pts',(-38.078515050113,4.17918427375947,-15.5158363917128));
#44326=CARTESIAN_POINT('Ctrl Pts',(-38.0352829832334,4.20693258492168,-16.1977362964252));
#44327=CARTESIAN_POINT('Ctrl Pts',(-38.0020608049623,4.23285504278592,-16.6472440721846));
#44328=CARTESIAN_POINT('Ctrl Pts',(-37.9717172227133,4.2613947474326,-16.9790036420799));
#44329=CARTESIAN_POINT('Ctrl Pts',(-37.9430624290585,4.29089588194445,-17.2524972836078));
#44330=CARTESIAN_POINT('Ctrl Pts',(-37.9310944384756,4.30340318167128,-17.3624838714222));
#44331=CARTESIAN_POINT('Ctrl Pts',(-37.9049516670918,4.33043376104169,-17.5832900565561));
#44332=CARTESIAN_POINT('Ctrl Pts',(-37.8757206533561,4.36056488940581,-17.8067425951866));
#44333=CARTESIAN_POINT('Ctrl Pts',(-37.8439229501231,4.39335377727898,-18.0324728092801));
#44334=CARTESIAN_POINT('Ctrl Pts',(-37.8230876353914,4.41489277682979,-18.1745891414915));
#44335=CARTESIAN_POINT('Ctrl Pts',(-37.8059091120036,4.43270415477703,-18.288878512028));
#44336=CARTESIAN_POINT('Ctrl Pts',(-37.7927864478151,4.4463428369108,-18.3749011727451));
#44337=CARTESIAN_POINT('Ctrl Pts',(-37.7816662610051,4.4579337525335,-18.4468361470788));
#44338=CARTESIAN_POINT('Ctrl Pts',(-37.7726670462702,4.46733538452826,-18.5045381817367));
#44339=CARTESIAN_POINT('Ctrl Pts',(-37.6956240797217,4.5479987181198,-18.9958335683562));
#44340=CARTESIAN_POINT('Ctrl Pts',(-37.531578810134,4.72380138407194,-19.9617965245065));
#44341=CARTESIAN_POINT('Ctrl Pts',(-37.3071222493637,5.01839492298006,-21.4593889396249));
#44342=CARTESIAN_POINT('Ctrl Pts',(-37.1979292243293,5.23114314143361,-22.492559477754));
#44343=CARTESIAN_POINT('Ctrl Pts',(-37.1477785057481,5.3663840162175,-23.143767430772));
#44344=CARTESIAN_POINT('Ctrl Pts',(-37.1317756722386,5.41682183827126,-23.374560641058));
#44345=CARTESIAN_POINT('Ctrl Pts',(-37.1010420548658,5.52904087143839,-23.8568415378094));
#44346=CARTESIAN_POINT('Ctrl Pts',(-37.0546893039173,5.74296592891402,-24.7049493973709));
#44347=CARTESIAN_POINT('Ctrl Pts',(-37.0012049893423,6.08801716179193,-25.9535934320049));
#44348=CARTESIAN_POINT('Ctrl Pts',(-36.9470279644122,6.51018306820065,-27.4977922697091));
#44349=CARTESIAN_POINT('Ctrl Pts',(-36.9130693803763,6.76162478093457,-28.5617199323548));
#44350=CARTESIAN_POINT('Ctrl Pts',(-36.8938132746591,6.8835366097984,-29.1698009783583));
#44351=CARTESIAN_POINT('Ctrl Pts',(-36.8900864116145,6.90952801988863,-29.3003038722774));
#44352=CARTESIAN_POINT('Ctrl Pts',(-36.8827560528828,6.96066199356787,-29.5634991228843));
#44353=CARTESIAN_POINT('Ctrl Pts',(-36.8710543183909,7.0467001782728,-30.0218644761164));
#44354=CARTESIAN_POINT('Ctrl Pts',(-36.851341532771,7.20700354283504,-30.9356587905047));
#44355=CARTESIAN_POINT('Ctrl Pts',(-36.8333810382757,7.40736751552731,-32.2288073399679));
#44356=CARTESIAN_POINT('Ctrl Pts',(-36.826924086164,7.58396623130391,-33.5044465690719));
#44357=CARTESIAN_POINT('Ctrl Pts',(-36.8272877347697,7.71909430657529,-34.5127169328848));
#44358=CARTESIAN_POINT('Ctrl Pts',(-36.8291349703753,7.78592356887283,-35.0124871732846));
#44359=CARTESIAN_POINT('Ctrl Pts',(-36.8309931623893,7.83642439587603,-35.3867717541854));
#44360=CARTESIAN_POINT('Ctrl Pts',(-36.832274469254,7.87064395520631,-35.6443002734807));
#44361=CARTESIAN_POINT('Ctrl Pts',(-36.8366281141019,7.93732800623012,-36.1545335368831));
#44362=CARTESIAN_POINT('Ctrl Pts',(-36.8480097321712,8.05060401090947,-37.0473268414636));
#44363=CARTESIAN_POINT('Ctrl Pts',(-36.8830256946237,8.26262751388984,-38.8247059011497));
#44364=CARTESIAN_POINT('Ctrl Pts',(-36.9240274059898,8.4190591370404,-40.3445738849485));
#44365=CARTESIAN_POINT('Ctrl Pts',(-36.9521838192205,8.53490390652826,-41.6142113403113));
#44366=CARTESIAN_POINT('Ctrl Pts',(-36.9595866936516,8.56769269468203,-41.9993803748625));
#44367=CARTESIAN_POINT('Ctrl Pts',(-36.9686014748246,8.60762379522345,-42.5092105260691));
#44368=CARTESIAN_POINT('Ctrl Pts',(-36.9772121426193,8.64550080422054,-43.0193369830249));
#44369=CARTESIAN_POINT('Ctrl Pts',(-36.987702670631,8.68941259692222,-43.6555519495176));
#44370=CARTESIAN_POINT('Ctrl Pts',(-37.0012727711582,8.73833577638218,-44.4168683480898));
#44371=CARTESIAN_POINT('Ctrl Pts',(-37.0146294238036,8.77731233846491,-45.048789040518));
#44372=CARTESIAN_POINT('Ctrl Pts',(-37.0272992448317,8.80823108976467,-45.5525785506231));
#44373=CARTESIAN_POINT('Ctrl Pts',(-37.0379798249283,8.83147635912366,-45.9294512079208));
#44374=CARTESIAN_POINT('Ctrl Pts',(-37.0500287686793,8.85497269830543,-46.3053079102783));
#44375=CARTESIAN_POINT('Ctrl Pts',(-37.0681863270722,8.88687733082516,-46.8049009793023));
#44376=CARTESIAN_POINT('Ctrl Pts',(-37.0844161301337,8.91174571627579,-47.1779366605091));
#44377=CARTESIAN_POINT('Ctrl Pts',(-37.102864789622,8.93761822369083,-47.5500895309825));
#44378=CARTESIAN_POINT('Ctrl Pts',(-37.1161923388764,8.95566301568517,-47.787728821962));
#44379=CARTESIAN_POINT('Ctrl Pts',(-37.1455454527048,8.99655532667588,-48.2747802767314));
#44380=CARTESIAN_POINT('Ctrl Pts',(-37.2034973491576,9.07697651567799,-49.1353231676698));
#44381=CARTESIAN_POINT('Ctrl Pts',(-37.3001167446471,9.20299194423899,-50.4014516292164));
#44382=CARTESIAN_POINT('Ctrl Pts',(-37.424112639288,9.32146046985706,-51.9759769909471));
#44383=CARTESIAN_POINT('Ctrl Pts',(-37.5026213956257,9.34328952661308,-53.0650482694175));
#44384=CARTESIAN_POINT('Ctrl Pts',(-37.5476337506195,9.32683669469911,-53.7605884615843));
#44385=CARTESIAN_POINT('Ctrl Pts',(-37.5665661126474,9.31272464671798,-54.0738284532984));
#44386=CARTESIAN_POINT('Ctrl Pts',(-37.6057031913977,9.26414962921768,-54.663337487995));
#44387=CARTESIAN_POINT('Ctrl Pts',(-37.6764662088264,9.13742110622336,-55.6615785587876));
#44388=CARTESIAN_POINT('Ctrl Pts',(-37.8164949562745,8.79806780322109,-57.4845265225189));
#44389=CARTESIAN_POINT('Ctrl Pts',(-37.9141915114532,8.61952768235194,-58.761476841605));
#44390=CARTESIAN_POINT('Ctrl Pts',(-37.9541952896336,8.66244269536972,-59.5035309748523));
#44391=CARTESIAN_POINT('Ctrl Pts',(-37.9587592236704,8.66957094444295,-59.6163026306148));
#44392=CARTESIAN_POINT('Ctrl Pts',(-37.9669276688694,8.68634443524689,-59.8301967046942));
#44393=CARTESIAN_POINT('Ctrl Pts',(-37.9787510920646,8.72419183715132,-60.2132581371599));
#44394=CARTESIAN_POINT('Ctrl Pts',(-37.9935384811198,8.83135451601754,-60.9838245730438));
#44395=CARTESIAN_POINT('Ctrl Pts',(-37.9948051042161,9.02173398324445,-61.885731569312));
#44396=CARTESIAN_POINT('Ctrl Pts',(-37.989617077741,9.26845024412025,-62.7989711447217));
#44397=CARTESIAN_POINT('Ctrl Pts',(-37.9859198864002,9.42587180626457,-63.3164647629597));
#44398=CARTESIAN_POINT('Ctrl Pts',(-37.9838015485123,9.53754686050424,-63.6623771036356));
#44399=CARTESIAN_POINT('Ctrl Pts',(-37.9825249382728,9.61371634326418,-63.8932483834881));
#44400=CARTESIAN_POINT('Ctrl Pts',(-37.9815185946865,9.69232843708823,-64.1243218214184));
#44401=CARTESIAN_POINT('Ctrl Pts',(-37.9809875763424,9.76308889151633,-64.3267502887585));
#44402=CARTESIAN_POINT('Ctrl Pts',(-37.9808002426337,9.80405805079477,-64.4424707032604));
#44403=CARTESIAN_POINT('Ctrl Pts',(-37.9806439053292,9.86602059892453,-64.6160649186278));
#44404=CARTESIAN_POINT('Ctrl Pts',(-37.9807887081246,9.91872513061641,-64.760831311268));
#44405=CARTESIAN_POINT('Ctrl Pts',(-37.9814928352743,10.0069714773366,-64.9998936835609));
#44406=CARTESIAN_POINT('Ctrl Pts',(-37.9826490650251,10.0893718431465,-65.2123548953848));
#44407=CARTESIAN_POINT('Ctrl Pts',(-37.9843492455442,10.2781728978025,-65.6621712721371));
#44408=CARTESIAN_POINT('Ctrl Pts',(-37.9866286590482,10.645795689941,-66.4512015386042));
#44409=CARTESIAN_POINT('Ctrl Pts',(-37.9879000851148,11.5250521960472,-68.0900185972829));
#44410=CARTESIAN_POINT('Ctrl Pts',(-37.9850730271635,12.423642682094,-69.5845303134357));
#44411=CARTESIAN_POINT('Ctrl Pts',(-37.9833124268618,13.0561024586398,-70.7862856454141));
#44412=CARTESIAN_POINT('Ctrl Pts',(-37.9834167705123,13.1849450671358,-71.0308400933947));
#44413=CARTESIAN_POINT('Ctrl Pts',(-37.9833552700991,13.4503457396783,-71.5333931190796));
#44414=CARTESIAN_POINT('Ctrl Pts',(-37.9834148605826,13.7803328254118,-72.1561449947392));
#44415=CARTESIAN_POINT('Ctrl Pts',(-37.9834441005009,14.1793852288138,-72.9068571737646));
#44416=CARTESIAN_POINT('Ctrl Pts',(-37.9835609738141,14.9788505997464,-74.4073744667933));
#44417=CARTESIAN_POINT('Ctrl Pts',(-37.9836479048135,15.6486830122308,-75.6601882148424));
#44418=CARTESIAN_POINT('Ctrl Pts',(-37.9835718534664,16.6204025035737,-77.4875159095769));
#44419=CARTESIAN_POINT('Ctrl Pts',(-37.9836050954401,17.0560964081388,-78.3068234984452));
#44420=CARTESIAN_POINT('Ctrl Pts',(-37.9836050954401,17.4926179955282,-79.1278012005436));
#44421=CARTESIAN_POINT('Ctrl Pts',(-36.8145414704191,4.17706810938354,24.8306393376479));
#44422=CARTESIAN_POINT('Ctrl Pts',(-36.8146506950273,4.17707182564265,24.7817601788696));
#44423=CARTESIAN_POINT('Ctrl Pts',(-36.8147652478949,4.17707572405304,24.7328820877382));
#44424=CARTESIAN_POINT('Ctrl Pts',(-36.8161179581993,4.17712171263977,24.182275474903));
#44425=CARTESIAN_POINT('Ctrl Pts',(-36.8171627107515,4.17715798726589,23.1781363569847));
#44426=CARTESIAN_POINT('Ctrl Pts',(-36.8195998551861,4.17724371941347,21.1695423782853));
#44427=CARTESIAN_POINT('Ctrl Pts',(-36.8286020356479,4.17754948633292,19.66539321355));
#44428=CARTESIAN_POINT('Ctrl Pts',(-36.8476544376428,4.17819248391852,18.4143478831888));
#44429=CARTESIAN_POINT('Ctrl Pts',(-36.8567956666284,4.17850085887141,17.9115338606246));
#44430=CARTESIAN_POINT('Ctrl Pts',(-36.8797573378532,4.17927517531058,16.9075428284866));
#44431=CARTESIAN_POINT('Ctrl Pts',(-36.9290069124392,4.18093483608638,15.1537199901826));
#44432=CARTESIAN_POINT('Ctrl Pts',(-36.9757452497305,4.18251067564459,13.6519464718781));
#44433=CARTESIAN_POINT('Ctrl Pts',(-37.0049439033556,4.18349506199556,12.3974580494044));
#44434=CARTESIAN_POINT('Ctrl Pts',(-37.0168690655117,4.18389716709014,11.896496347134));
#44435=CARTESIAN_POINT('Ctrl Pts',(-37.0411436577337,4.18471547900478,10.8946396040635));
#44436=CARTESIAN_POINT('Ctrl Pts',(-37.0711039027786,4.18572677788779,9.64208784240444));
#44437=CARTESIAN_POINT('Ctrl Pts',(-37.1026535454665,4.18679000665914,8.13758235446264));
#44438=CARTESIAN_POINT('Ctrl Pts',(-37.1182314109417,4.18731418915677,7.13287015374521));
#44439=CARTESIAN_POINT('Ctrl Pts',(-37.1254642281502,4.1875565209857,6.50489713067809));
#44440=CARTESIAN_POINT('Ctrl Pts',(-37.128155112656,4.18764613376774,6.25467125009352));
#44441=CARTESIAN_POINT('Ctrl Pts',(-37.1328167164426,4.18779971642136,5.75355956197867));
#44442=CARTESIAN_POINT('Ctrl Pts',(-37.1391750727683,4.18800414638075,4.87515574383194));
#44443=CARTESIAN_POINT('Ctrl Pts',(-37.1454177456287,4.18819017072339,3.11491456727999));
#44444=CARTESIAN_POINT('Ctrl Pts',(-37.1421588108841,4.18806139037958,1.60821253231155));
#44445=CARTESIAN_POINT('Ctrl Pts',(-37.1381315205537,4.18794334293428,0.548768836768961));
#44446=CARTESIAN_POINT('Ctrl Pts',(-37.1376027122731,4.18792827716166,0.422597518332732));
#44447=CARTESIAN_POINT('Ctrl Pts',(-37.1363583452212,4.18789230873776,0.170450774630366));
#44448=CARTESIAN_POINT('Ctrl Pts',(-37.1337143965635,4.18781547475265,-0.270307417104572));
#44449=CARTESIAN_POINT('Ctrl Pts',(-37.128739477224,4.18766826957105,-0.898708045971484));
#44450=CARTESIAN_POINT('Ctrl Pts',(-37.1212908405087,4.18744931772557,-1.65117956824175));
#44451=CARTESIAN_POINT('Ctrl Pts',(-37.1099619032053,4.1871129344279,-2.65302799518834));
#44452=CARTESIAN_POINT('Ctrl Pts',(-37.09427463321,4.1866465079283,-3.90365427999558));
#44453=CARTESIAN_POINT('Ctrl Pts',(-37.0824128175559,4.18629030821057,-4.90495429670346));
#44454=CARTESIAN_POINT('Ctrl Pts',(-37.0759419900389,4.18609948224038,-5.53177471628879));
#44455=CARTESIAN_POINT('Ctrl Pts',(-37.0734490733729,4.18601901608428,-5.78278322973631));
#44456=CARTESIAN_POINT('Ctrl Pts',(-37.068774466851,4.18584253793842,-6.28501209766204));
#44457=CARTESIAN_POINT('Ctrl Pts',(-37.0612153049882,4.18550176203556,-7.16444418145535));
#44458=CARTESIAN_POINT('Ctrl Pts',(-37.051088171976,4.18497049210318,-8.42122512102502));
#44459=CARTESIAN_POINT('Ctrl Pts',(-37.038885514991,4.18453356806039,-9.67567405245044));
#44460=CARTESIAN_POINT('Ctrl Pts',(-37.0276914499488,4.18435986985205,-10.5509869279345));
#44461=CARTESIAN_POINT('Ctrl Pts',(-37.0203151196171,4.18430562699315,-11.0502134500236));
#44462=CARTESIAN_POINT('Ctrl Pts',(-37.0162634821171,4.18429470100516,-11.2993853814344));
#44463=CARTESIAN_POINT('Ctrl Pts',(-37.0130611661426,4.18429260457632,-11.4871271373884));
#44464=CARTESIAN_POINT('Ctrl Pts',(-37.0110448690885,4.18398173723689,-11.6210508779523));
#44465=CARTESIAN_POINT('Ctrl Pts',(-37.0074948447866,4.18227085814457,-11.8829086291118));
#44466=CARTESIAN_POINT('Ctrl Pts',(-37.0023895368805,4.1767444699889,-12.3396792789109));
#44467=CARTESIAN_POINT('Ctrl Pts',(-36.9953355747988,4.15807514016592,-13.2368410977104));
#44468=CARTESIAN_POINT('Ctrl Pts',(-36.98692719984,4.1239517633785,-14.4787967330387));
#44469=CARTESIAN_POINT('Ctrl Pts',(-36.9639435464291,4.11490441611126,-15.552347252464));
#44470=CARTESIAN_POINT('Ctrl Pts',(-36.9350271873072,4.12865937629905,-16.252631627403));
#44471=CARTESIAN_POINT('Ctrl Pts',(-36.9116737747744,4.14363804540266,-16.7156276685256));
#44472=CARTESIAN_POINT('Ctrl Pts',(-36.8890848383236,4.16207307191748,-17.0587999422591));
#44473=CARTESIAN_POINT('Ctrl Pts',(-36.8669552974436,4.18202463484443,-17.3424822046825));
#44474=CARTESIAN_POINT('Ctrl Pts',(-36.8577331954662,4.19063519194624,-17.4597987335548));
#44475=CARTESIAN_POINT('Ctrl Pts',(-36.837750631618,4.20884846416802,-17.6922569789042));
#44476=CARTESIAN_POINT('Ctrl Pts',(-36.8155634200376,4.22888625981175,-17.9267206097568));
#44477=CARTESIAN_POINT('Ctrl Pts',(-36.7914693697599,4.25044510162083,-18.1616254051611));
#44478=CARTESIAN_POINT('Ctrl Pts',(-36.7756778369371,4.26454517607042,-18.308973522781));
#44479=CARTESIAN_POINT('Ctrl Pts',(-36.7626422312317,4.27617033658842,-18.4270538895154));
#44480=CARTESIAN_POINT('Ctrl Pts',(-36.7526738439219,4.28505922055653,-18.5157491412756));
#44481=CARTESIAN_POINT('Ctrl Pts',(-36.7442156277307,4.29260330675946,-18.5897585461262));
#44482=CARTESIAN_POINT('Ctrl Pts',(-36.7373621096969,4.29871796800706,-18.6490303045467));
#44483=CARTESIAN_POINT('Ctrl Pts',(-36.6786435611264,4.35114684308371,-19.1531722422004));
#44484=CARTESIAN_POINT('Ctrl Pts',(-36.5517941291924,4.4648025218755,-20.1274966208569));
#44485=CARTESIAN_POINT('Ctrl Pts',(-36.3629902843748,4.65825546096279,-21.5949066389794));
#44486=CARTESIAN_POINT('Ctrl Pts',(-36.258482687298,4.80650647098656,-22.5868678297255));
#44487=CARTESIAN_POINT('Ctrl Pts',(-36.2041312424173,4.90714442404014,-23.2071548394697));
#44488=CARTESIAN_POINT('Ctrl Pts',(-36.1842954084408,4.94560004507131,-23.4322288054636));
#44489=CARTESIAN_POINT('Ctrl Pts',(-36.1439879759796,5.03312209851521,-23.901369364868));
#44490=CARTESIAN_POINT('Ctrl Pts',(-36.0745253032527,5.20540870627714,-24.7326154565184));
#44491=CARTESIAN_POINT('Ctrl Pts',(-35.9763792540907,5.4960732899547,-25.967198555433));
#44492=CARTESIAN_POINT('Ctrl Pts',(-35.8638730883827,5.86559758195893,-27.5074586456592));
#44493=CARTESIAN_POINT('Ctrl Pts',(-35.7970238913048,6.08933924924599,-28.5741940065593));
#44494=CARTESIAN_POINT('Ctrl Pts',(-35.7639743896009,6.19771303571068,-29.1848272516722));
#44495=CARTESIAN_POINT('Ctrl Pts',(-35.7573496776361,6.22054498842897,-29.3138091203023));
#44496=CARTESIAN_POINT('Ctrl Pts',(-35.744157507517,6.26582226975952,-29.5752104980963));
#44497=CARTESIAN_POINT('Ctrl Pts',(-35.7222727087314,6.34236043846015,-30.0300178405691));
#44498=CARTESIAN_POINT('Ctrl Pts',(-35.6823716163915,6.48680121409233,-30.9378995013247));
#44499=CARTESIAN_POINT('Ctrl Pts',(-35.6360682369693,6.67203034121833,-32.2246917237026));
#44500=CARTESIAN_POINT('Ctrl Pts',(-35.602424279164,6.84043243075705,-33.4980677505866));
#44501=CARTESIAN_POINT('Ctrl Pts',(-35.5825233522388,6.97146434574046,-34.5073233082595));
#44502=CARTESIAN_POINT('Ctrl Pts',(-35.5747656005365,7.03676380952808,-35.0086292126765));
#44503=CARTESIAN_POINT('Ctrl Pts',(-35.5697386951994,7.08620366384295,-35.3844250261613));
#44504=CARTESIAN_POINT('Ctrl Pts',(-35.5665433265602,7.11965891412784,-35.6410715501154));
#44505=CARTESIAN_POINT('Ctrl Pts',(-35.562152378891,7.18553225339312,-36.150621600417));
#44506=CARTESIAN_POINT('Ctrl Pts',(-35.5587186405156,7.29894277838356,-37.0416973417176));
#44507=CARTESIAN_POINT('Ctrl Pts',(-35.5663553325028,7.51681414684123,-38.8159662755505));
#44508=CARTESIAN_POINT('Ctrl Pts',(-35.5869256269565,7.6868654242813,-40.3327515990101));
#44509=CARTESIAN_POINT('Ctrl Pts',(-35.600071936512,7.81648886757626,-41.5997097363398));
#44510=CARTESIAN_POINT('Ctrl Pts',(-35.6029973034266,7.85315812159936,-41.9863157305565));
#44511=CARTESIAN_POINT('Ctrl Pts',(-35.6065402637938,7.89782342059797,-42.4960833951206));
#44512=CARTESIAN_POINT('Ctrl Pts',(-35.6099161058435,7.94043513506824,-43.0059427141509));
#44513=CARTESIAN_POINT('Ctrl Pts',(-35.6143750775419,7.99051271915899,-43.6407347128252));
#44514=CARTESIAN_POINT('Ctrl Pts',(-35.6215523453426,8.04830994811261,-44.398876931035));
#44515=CARTESIAN_POINT('Ctrl Pts',(-35.6303514970611,8.09677619833867,-45.0268145521791));
#44516=CARTESIAN_POINT('Ctrl Pts',(-35.6398718628481,8.13700691506071,-45.5266306469361));
#44517=CARTESIAN_POINT('Ctrl Pts',(-35.648468541391,8.1682473135573,-45.9001070187702));
#44518=CARTESIAN_POINT('Ctrl Pts',(-35.6587338366661,8.2008710525493,-46.2721457927705));
#44519=CARTESIAN_POINT('Ctrl Pts',(-35.6749387045069,8.24660419070035,-46.7660688678912));
#44520=CARTESIAN_POINT('Ctrl Pts',(-35.6902809195264,8.28392755781832,-47.1341623966199));
#44521=CARTESIAN_POINT('Ctrl Pts',(-35.7082692818551,8.32385161219814,-47.500860791251));
#44522=CARTESIAN_POINT('Ctrl Pts',(-35.7216788552181,8.35174113882669,-47.7342227588538));
#44523=CARTESIAN_POINT('Ctrl Pts',(-35.7515901662072,8.41505553960775,-48.2137123367135));
#44524=CARTESIAN_POINT('Ctrl Pts',(-35.8120627570416,8.54067956461536,-49.0623306215748));
#44525=CARTESIAN_POINT('Ctrl Pts',(-35.9170717556947,8.74428194334892,-50.3163275049105));
#44526=CARTESIAN_POINT('Ctrl Pts',(-36.0593740981134,8.96238047461758,-51.8872068047178));
#44527=CARTESIAN_POINT('Ctrl Pts',(-36.1553810000668,9.04507524266935,-52.9838173650416));
#44528=CARTESIAN_POINT('Ctrl Pts',(-36.2124020013169,9.06172995327984,-53.6873700494853));
#44529=CARTESIAN_POINT('Ctrl Pts',(-36.2364593892998,9.06239337045504,-53.9978055411204));
#44530=CARTESIAN_POINT('Ctrl Pts',(-36.2877503511432,9.04237784569512,-54.5868399174417));
#44531=CARTESIAN_POINT('Ctrl Pts',(-36.3835699740437,8.9640044494523,-55.5855825795852));
#44532=CARTESIAN_POINT('Ctrl Pts',(-36.5813073250735,8.70846064059012,-57.4175989887824));
#44533=CARTESIAN_POINT('Ctrl Pts',(-36.7259019766856,8.56770686894578,-58.7072698807721));
#44534=CARTESIAN_POINT('Ctrl Pts',(-36.782338123889,8.62482634667821,-59.4707756675742));
#44535=CARTESIAN_POINT('Ctrl Pts',(-36.7887634890227,8.63400662213569,-59.5865773895651));
#44536=CARTESIAN_POINT('Ctrl Pts',(-36.8002731557661,8.65423114517781,-59.8059753328883));
#44537=CARTESIAN_POINT('Ctrl Pts',(-36.8169541787248,8.69719905574384,-60.1980565910176));
#44538=CARTESIAN_POINT('Ctrl Pts',(-36.8379285804888,8.81069057980454,-60.983438205225));
#44539=CARTESIAN_POINT('Ctrl Pts',(-36.8400324690854,9.0008653106084,-61.895075215011));
#44540=CARTESIAN_POINT('Ctrl Pts',(-36.833025237701,9.2428331962055,-62.8113508141628));
#44541=CARTESIAN_POINT('Ctrl Pts',(-36.8279560631062,9.39662372468876,-63.3282484325131));
#44542=CARTESIAN_POINT('Ctrl Pts',(-36.8250506657004,9.50579153322136,-63.6728480522941));
#44543=CARTESIAN_POINT('Ctrl Pts',(-36.8232987567908,9.58029320294315,-63.9026020207381));
#44544=CARTESIAN_POINT('Ctrl Pts',(-36.8219207850234,9.65727402391867,-64.1322082227681));
#44545=CARTESIAN_POINT('Ctrl Pts',(-36.8211968688644,9.72670407409752,-64.3330399111182));
#44546=CARTESIAN_POINT('Ctrl Pts',(-36.8209436600969,9.76694921258375,-64.4477593319922));
#44547=CARTESIAN_POINT('Ctrl Pts',(-36.8207356143094,9.827867991798,-64.6197666251074));
#44548=CARTESIAN_POINT('Ctrl Pts',(-36.820943020463,9.87979354233477,-64.7630215620431));
#44549=CARTESIAN_POINT('Ctrl Pts',(-36.8219192494767,9.96695386528716,-64.9994059056064));
#44550=CARTESIAN_POINT('Ctrl Pts',(-36.8231725041911,10.0495336392164,-65.2126160893504));
#44551=CARTESIAN_POINT('Ctrl Pts',(-36.82499495272,10.2379636953157,-65.6619525374483));
#44552=CARTESIAN_POINT('Ctrl Pts',(-36.8271181992213,10.6053251831302,-66.4511851584012));
#44553=CARTESIAN_POINT('Ctrl Pts',(-36.8272923782176,11.4838409823459,-68.0896332538814));
#44554=CARTESIAN_POINT('Ctrl Pts',(-36.8234065807366,12.3821608378723,-69.5844108199255));
#44555=CARTESIAN_POINT('Ctrl Pts',(-36.8218354649019,13.0144506626477,-70.786159996006));
#44556=CARTESIAN_POINT('Ctrl Pts',(-36.8218980779087,13.1432412485324,-71.0306777115429));
#44557=CARTESIAN_POINT('Ctrl Pts',(-36.8218129450693,13.4085677772461,-71.5331812361234));
#44558=CARTESIAN_POINT('Ctrl Pts',(-36.8218398088373,13.7384930297767,-72.1558847530838));
#44559=CARTESIAN_POINT('Ctrl Pts',(-36.8218623967062,14.137515020371,-72.9065507501415));
#44560=CARTESIAN_POINT('Ctrl Pts',(-36.8219908398845,14.936984438163,-74.4070081525254));
#44561=CARTESIAN_POINT('Ctrl Pts',(-36.8221312065847,15.6069267144729,-75.6598871290026));
#44562=CARTESIAN_POINT('Ctrl Pts',(-36.8220673386195,16.5787078435202,-77.4873463549366));
#44563=CARTESIAN_POINT('Ctrl Pts',(-36.8220955884565,17.0143863943048,-78.3066347591213));
#44564=CARTESIAN_POINT('Ctrl Pts',(-36.8220955884566,17.4509079816942,-79.1276124612196));
#44565=CARTESIAN_POINT('Ctrl Pts',(-35.8862883815749,4.14964241231811,24.8306453611339));
#44566=CARTESIAN_POINT('Ctrl Pts',(-35.8863946402816,4.14964559583046,24.781766398004));
#44567=CARTESIAN_POINT('Ctrl Pts',(-35.8865060824592,4.14964893562382,24.7328885041874));
#44568=CARTESIAN_POINT('Ctrl Pts',(-35.8878220796098,4.14968831258694,24.182284251377));
#44569=CARTESIAN_POINT('Ctrl Pts',(-35.8888338622136,4.1497223590721,23.1781482479736));
#44570=CARTESIAN_POINT('Ctrl Pts',(-35.8911909796499,4.14980495718219,21.1695585828577));
#44571=CARTESIAN_POINT('Ctrl Pts',(-35.8999488466652,4.15006655052355,19.6654120350873));
#44572=CARTESIAN_POINT('Ctrl Pts',(-35.918507596782,4.1506015914958,18.4143681228999));
#44573=CARTESIAN_POINT('Ctrl Pts',(-35.9274101115364,4.15085968205004,17.9115681746897));
#44574=CARTESIAN_POINT('Ctrl Pts',(-35.9497686326789,4.15151040993799,16.907587303699));
#44575=CARTESIAN_POINT('Ctrl Pts',(-35.9977262208149,4.15290448218856,15.1537628190788));
#44576=CARTESIAN_POINT('Ctrl Pts',(-36.0432641073147,4.1542076681852,13.651948151249));
#44577=CARTESIAN_POINT('Ctrl Pts',(-36.0717655121545,4.15498251426331,12.3974030081685));
#44578=CARTESIAN_POINT('Ctrl Pts',(-36.0834116029276,4.15529458500124,11.8964181254143));
#44579=CARTESIAN_POINT('Ctrl Pts',(-36.1071370294188,4.15591534395308,10.8945279252343));
#44580=CARTESIAN_POINT('Ctrl Pts',(-36.136444163004,4.1566621270959,9.6419569332076));
#44581=CARTESIAN_POINT('Ctrl Pts',(-36.1673368895585,4.15742625530908,8.13745839911925));
#44582=CARTESIAN_POINT('Ctrl Pts',(-36.1826020917766,4.1577946577808,7.13277408159323));
#44583=CARTESIAN_POINT('Ctrl Pts',(-36.1896949520552,4.15796306023695,6.50482106525867));
#44584=CARTESIAN_POINT('Ctrl Pts',(-36.1923388683203,4.15802189763918,6.25455986045041));
#44585=CARTESIAN_POINT('Ctrl Pts',(-36.1969369263861,4.1581106296951,5.75341435659549));
#44586=CARTESIAN_POINT('Ctrl Pts',(-36.2032535362139,4.15819691448695,4.87496918784217));
#44587=CARTESIAN_POINT('Ctrl Pts',(-36.2096128412279,4.15816654078512,3.11476734483232));
#44588=CARTESIAN_POINT('Ctrl Pts',(-36.2065231000555,4.15800477907593,1.60830836530141));
#44589=CARTESIAN_POINT('Ctrl Pts',(-36.2023901977377,4.15805498954621,0.549132646374202));
#44590=CARTESIAN_POINT('Ctrl Pts',(-36.2018474091026,4.15806236256343,0.423005400853475));
#44591=CARTESIAN_POINT('Ctrl Pts',(-36.2005696253334,4.15807930101949,0.170934716825099));
#44592=CARTESIAN_POINT('Ctrl Pts',(-36.1978539375442,4.15811533846752,-0.269699105975777));
#44593=CARTESIAN_POINT('Ctrl Pts',(-36.1927454283527,4.15817800690684,-0.897953119275321));
#44594=CARTESIAN_POINT('Ctrl Pts',(-36.185103668902,4.15827024278405,-1.65031602714938));
#44595=CARTESIAN_POINT('Ctrl Pts',(-36.1735015690339,4.15838989116868,-2.6520843755158));
#44596=CARTESIAN_POINT('Ctrl Pts',(-36.1574887428905,4.15852036661871,-3.90276838449031));
#44597=CARTESIAN_POINT('Ctrl Pts',(-36.1454832904363,4.15853186877887,-4.90425270890406));
#44598=CARTESIAN_POINT('Ctrl Pts',(-36.1389903705117,4.15849989683032,-5.53122578067775));
#44599=CARTESIAN_POINT('Ctrl Pts',(-36.1364213474791,4.15852132331837,-5.78169150779713));
#44600=CARTESIAN_POINT('Ctrl Pts',(-36.1313777044444,4.15867155979321,-6.28336956168771));
#44601=CARTESIAN_POINT('Ctrl Pts',(-36.122741714016,4.15914649121972,-7.16209558041097));
#44602=CARTESIAN_POINT('Ctrl Pts',(-36.11062700423,4.16002563108501,-8.41924559593771));
#44603=CARTESIAN_POINT('Ctrl Pts',(-36.0979378721441,4.16011467591934,-9.67574382559009));
#44604=CARTESIAN_POINT('Ctrl Pts',(-36.0882951212805,4.15920632450633,-10.5534752798069));
#44605=CARTESIAN_POINT('Ctrl Pts',(-36.0825016438357,4.1583296753329,-11.0543357491708));
#44606=CARTESIAN_POINT('Ctrl Pts',(-36.0794997434348,4.15775737267943,-11.3044371099148));
#44607=CARTESIAN_POINT('Ctrl Pts',(-36.0771950437572,4.15727094088865,-11.4928473165457));
#44608=CARTESIAN_POINT('Ctrl Pts',(-36.0757841290909,4.15669504852568,-11.6250424614838));
#44609=CARTESIAN_POINT('Ctrl Pts',(-36.0734605672477,4.1546897995167,-11.8849898120977));
#44610=CARTESIAN_POINT('Ctrl Pts',(-36.0705582594424,4.1491611106547,-12.338529623164));
#44611=CARTESIAN_POINT('Ctrl Pts',(-36.0682616272298,4.13188215694291,-13.232714440791));
#44612=CARTESIAN_POINT('Ctrl Pts',(-36.0684238134283,4.09998213405072,-14.4789694954568));
#44613=CARTESIAN_POINT('Ctrl Pts',(-36.0570757827599,4.08628902253444,-15.5672532812383));
#44614=CARTESIAN_POINT('Ctrl Pts',(-36.0381982641581,4.09230382197452,-16.2816087198696));
#44615=CARTESIAN_POINT('Ctrl Pts',(-36.0221580751819,4.10083040385787,-16.7550758926505));
#44616=CARTESIAN_POINT('Ctrl Pts',(-36.0057514960225,4.11285987052124,-17.1072248415648));
#44617=CARTESIAN_POINT('Ctrl Pts',(-35.9891607297069,4.12653843794509,-17.3989493347664));
#44618=CARTESIAN_POINT('Ctrl Pts',(-35.9823198969599,4.13242701942715,-17.5205098832969));
#44619=CARTESIAN_POINT('Ctrl Pts',(-35.9676474843925,4.1447016794492,-17.7602658762473));
#44620=CARTESIAN_POINT('Ctrl Pts',(-35.9515412202045,4.15801546224031,-18.001525451086));
#44621=CARTESIAN_POINT('Ctrl Pts',(-35.9341397743477,4.17221689876555,-18.2423215927065));
#44622=CARTESIAN_POINT('Ctrl Pts',(-35.9227524102192,4.18147118565899,-18.3930619490067));
#44623=CARTESIAN_POINT('Ctrl Pts',(-35.9133537783526,4.18908839335587,-18.513651392042));
#44624=CARTESIAN_POINT('Ctrl Pts',(-35.9061647785332,4.19490847302005,-18.6041351482638));
#44625=CARTESIAN_POINT('Ctrl Pts',(-35.9000612943855,4.19984592113213,-18.6795538907485));
#44626=CARTESIAN_POINT('Ctrl Pts',(-35.8951128771809,4.20384764031546,-18.7399050267767));
#44627=CARTESIAN_POINT('Ctrl Pts',(-35.8526921669526,4.2381583887282,-19.2529529861667));
#44628=CARTESIAN_POINT('Ctrl Pts',(-35.760254812392,4.31271623368857,-20.2358611422357));
#44629=CARTESIAN_POINT('Ctrl Pts',(-35.6112529180016,4.44665882940044,-21.6930146193082));
#44630=CARTESIAN_POINT('Ctrl Pts',(-35.5154493742871,4.55651940675062,-22.6659175228438));
#44631=CARTESIAN_POINT('Ctrl Pts',(-35.4592812336553,4.63398076469743,-23.2716923919344));
#44632=CARTESIAN_POINT('Ctrl Pts',(-35.4372505995826,4.66424453213448,-23.4962824133311));
#44633=CARTESIAN_POINT('Ctrl Pts',(-35.3907531102402,4.73347007409692,-23.9615642265644));
#44634=CARTESIAN_POINT('Ctrl Pts',(-35.305277650528,4.87131590316984,-24.7878810585807));
#44635=CARTESIAN_POINT('Ctrl Pts',(-35.1758847760366,5.10698704564035,-26.0159825559886));
#44636=CARTESIAN_POINT('Ctrl Pts',(-35.0251617842373,5.40948230024783,-27.5504638123744));
#44637=CARTESIAN_POINT('Ctrl Pts',(-34.9390560374465,5.59420259744437,-28.6124002756524));
#44638=CARTESIAN_POINT('Ctrl Pts',(-34.8983911824391,5.68406100232119,-29.2195884874086));
#44639=CARTESIAN_POINT('Ctrl Pts',(-34.8900265532928,5.70288570916111,-29.3476037983399));
#44640=CARTESIAN_POINT('Ctrl Pts',(-34.8734077068156,5.74036969201598,-29.6072368148802));
#44641=CARTESIAN_POINT('Ctrl Pts',(-34.845590131241,5.80393710757317,-30.0590182597113));
#44642=CARTESIAN_POINT('Ctrl Pts',(-34.7940841644091,5.92489230913247,-30.9614069392673));
#44643=CARTESIAN_POINT('Ctrl Pts',(-34.7319608996809,6.08300768791716,-32.2419080216104));
#44644=CARTESIAN_POINT('Ctrl Pts',(-34.6836000442781,6.2310247072079,-33.5114953241617));
#44645=CARTESIAN_POINT('Ctrl Pts',(-34.6527570741318,6.34855643808978,-34.5193896260131));
#44646=CARTESIAN_POINT('Ctrl Pts',(-34.6399400714304,6.40788861012915,-35.0206377216183));
#44647=CARTESIAN_POINT('Ctrl Pts',(-34.6312477397019,6.45304449511186,-35.3965836686083));
#44648=CARTESIAN_POINT('Ctrl Pts',(-34.6256995318638,6.48363888487945,-35.6521654141448));
#44649=CARTESIAN_POINT('Ctrl Pts',(-34.6166756023149,6.54450478408635,-36.1602930070773));
#44650=CARTESIAN_POINT('Ctrl Pts',(-34.6054976367161,6.65064325450614,-37.0486813865334));
#44651=CARTESIAN_POINT('Ctrl Pts',(-34.5985929019923,6.85999883007196,-38.8181150574146));
#44652=CARTESIAN_POINT('Ctrl Pts',(-34.6079843194644,7.03094019656917,-40.3310612298055));
#44653=CARTESIAN_POINT('Ctrl Pts',(-34.6122469819752,7.16449148557296,-41.5949163129102));
#44654=CARTESIAN_POINT('Ctrl Pts',(-34.6124779151437,7.20222495561867,-41.9827092555688));
#44655=CARTESIAN_POINT('Ctrl Pts',(-34.6127388112367,7.24813890723205,-42.4921260116324));
#44656=CARTESIAN_POINT('Ctrl Pts',(-34.6129391610133,7.29206616231259,-43.001417825639));
#44657=CARTESIAN_POINT('Ctrl Pts',(-34.6136397961648,7.34415615870572,-43.6344264110089));
#44658=CARTESIAN_POINT('Ctrl Pts',(-34.6164895533612,7.40579628834921,-44.388988882819));
#44659=CARTESIAN_POINT('Ctrl Pts',(-34.6217374437153,7.45932871493727,-45.0126410170983));
#44660=CARTESIAN_POINT('Ctrl Pts',(-34.6284138968991,7.50518355301202,-45.5082695504738));
#44661=CARTESIAN_POINT('Ctrl Pts',(-34.6348593583171,7.54150340913437,-45.8782017769925));
#44662=CARTESIAN_POINT('Ctrl Pts',(-34.642947844707,7.58017136010169,-46.2462884260783));
#44663=CARTESIAN_POINT('Ctrl Pts',(-34.65622333736,7.63538868340226,-46.7343837912956));
#44664=CARTESIAN_POINT('Ctrl Pts',(-34.6693039888815,7.68154214126522,-47.0974376750828));
#44665=CARTESIAN_POINT('Ctrl Pts',(-34.68504086039,7.7316813158421,-47.4586081772142));
#44666=CARTESIAN_POINT('Ctrl Pts',(-34.6971135255681,7.76674535176387,-47.6876879712688));
#44667=CARTESIAN_POINT('Ctrl Pts',(-34.7238675511503,7.84665764000097,-48.1596138295459));
#44668=CARTESIAN_POINT('Ctrl Pts',(-34.7781729950287,8.00639497600336,-48.9963097167226));
#44669=CARTESIAN_POINT('Ctrl Pts',(-34.8731749732318,8.27109386541086,-50.2376278605034));
#44670=CARTESIAN_POINT('Ctrl Pts',(-35.0063319813504,8.57410681218887,-51.8015718655458));
#44671=CARTESIAN_POINT('Ctrl Pts',(-35.1015618374688,8.71420329995202,-52.9017018699587));
#44672=CARTESIAN_POINT('Ctrl Pts',(-35.160871970943,8.76411916709648,-53.6106120097621));
#44673=CARTESIAN_POINT('Ctrl Pts',(-35.1860374687326,8.77929721972541,-53.9163395189235));
#44674=CARTESIAN_POINT('Ctrl Pts',(-35.2413576732862,8.78877244981892,-54.5018843049029));
#44675=CARTESIAN_POINT('Ctrl Pts',(-35.3480660504264,8.76265769681329,-55.4966936433364));
#44676=CARTESIAN_POINT('Ctrl Pts',(-35.5794804576178,8.6047778550797,-57.3345419063183));
#44677=CARTESIAN_POINT('Ctrl Pts',(-35.7570859886107,8.51263157414461,-58.6417003743386));
#44678=CARTESIAN_POINT('Ctrl Pts',(-35.8255593211804,8.58858922534792,-59.4316201891843));
#44679=CARTESIAN_POINT('Ctrl Pts',(-35.8333837380864,8.60041583723261,-59.550567178602));
#44680=CARTESIAN_POINT('Ctrl Pts',(-35.8475295837383,8.62516120799974,-59.7759386231754));
#44681=CARTESIAN_POINT('Ctrl Pts',(-35.8683787863595,8.67492305574173,-60.1776568829463));
#44682=CARTESIAN_POINT('Ctrl Pts',(-35.8961044631683,8.79731615480497,-60.9790075033711));
#44683=CARTESIAN_POINT('Ctrl Pts',(-35.9029595858914,8.98912101592088,-61.9014292473522));
#44684=CARTESIAN_POINT('Ctrl Pts',(-35.8990024346742,9.2278237708258,-62.8215390008787));
#44685=CARTESIAN_POINT('Ctrl Pts',(-35.895251208417,9.37872568359486,-63.3381346355321));
#44686=CARTESIAN_POINT('Ctrl Pts',(-35.8931550250171,9.48585299121616,-63.6815553093281));
#44687=CARTESIAN_POINT('Ctrl Pts',(-35.8919311575114,9.55898789419036,-63.9102650053807));
#44688=CARTESIAN_POINT('Ctrl Pts',(-35.891071831239,9.63462927284979,-64.138454184385));
#44689=CARTESIAN_POINT('Ctrl Pts',(-35.8908108483524,9.70296866963137,-64.337716001437));
#44690=CARTESIAN_POINT('Ctrl Pts',(-35.8908267513662,9.74262284984297,-64.4514456344633));
#44691=CARTESIAN_POINT('Ctrl Pts',(-35.8910279680724,9.8026931488241,-64.6218793627845));
#44692=CARTESIAN_POINT('Ctrl Pts',(-35.8915904528576,9.85399574762302,-64.7636268710383));
#44693=CARTESIAN_POINT('Ctrl Pts',(-35.8931818333317,9.94031508235885,-64.9973428837816));
#44694=CARTESIAN_POINT('Ctrl Pts',(-35.8948850335373,10.0234095492546,-65.2116626864872));
#44695=CARTESIAN_POINT('Ctrl Pts',(-35.8973657395788,10.2119700047034,-65.6609565696931));
#44696=CARTESIAN_POINT('Ctrl Pts',(-35.8999362720341,10.5797136472901,-66.4510848059395));
#44697=CARTESIAN_POINT('Ctrl Pts',(-35.8991950183312,11.4577636528938,-68.0898218646214));
#44698=CARTESIAN_POINT('Ctrl Pts',(-35.8936551391635,12.3550480594595,-69.5847771214724));
#44699=CARTESIAN_POINT('Ctrl Pts',(-35.8923188051878,12.9869272447527,-70.786025649498));
#44700=CARTESIAN_POINT('Ctrl Pts',(-35.8923642823853,13.1156897729242,-71.0305436169681));
#44701=CARTESIAN_POINT('Ctrl Pts',(-35.8922843116259,13.3809422470354,-71.5329860629288));
#44702=CARTESIAN_POINT('Ctrl Pts',(-35.8923005572825,13.7108226122191,-72.1556622624769));
#44703=CARTESIAN_POINT('Ctrl Pts',(-35.8923192925645,14.1098170297801,-72.9062849496283));
#44704=CARTESIAN_POINT('Ctrl Pts',(-35.8924355644065,14.9092943937856,-74.4066960770161));
#44705=CARTESIAN_POINT('Ctrl Pts',(-35.8925703043616,15.5793453086214,-75.6596486297005));
#44706=CARTESIAN_POINT('Ctrl Pts',(-35.8925151429371,16.5511896341262,-77.4872367171815));
#44707=CARTESIAN_POINT('Ctrl Pts',(-35.8925387824741,16.9868585707651,-78.3065132863522));
#44708=CARTESIAN_POINT('Ctrl Pts',(-35.8925387824741,17.4233801581546,-79.1274909884505));
#44709=CARTESIAN_POINT('Ctrl Pts',(-34.9576691493447,4.12599202383782,24.8306481986048));
#44710=CARTESIAN_POINT('Ctrl Pts',(-34.9577724821763,4.12599463491672,24.7817693216754));
#44711=CARTESIAN_POINT('Ctrl Pts',(-34.9578808561587,4.12599737399079,24.7328915142085));
#44712=CARTESIAN_POINT('Ctrl Pts',(-34.959160618967,4.12602966925197,24.1822883198965));
#44713=CARTESIAN_POINT('Ctrl Pts',(-34.9601402896146,4.12605960361354,23.1781538414392));
#44714=CARTESIAN_POINT('Ctrl Pts',(-34.9624198041354,4.12613330893548,21.1695660953823));
#44715=CARTESIAN_POINT('Ctrl Pts',(-34.9709368942797,4.12634777941475,19.6654208634938));
#44716=CARTESIAN_POINT('Ctrl Pts',(-34.9890064171506,4.12677640976453,18.4143777378113));
#44717=CARTESIAN_POINT('Ctrl Pts',(-34.9976724232657,4.12698427523286,17.9115850253704));
#44718=CARTESIAN_POINT('Ctrl Pts',(-35.0194340808931,4.12751030302748,16.9076093890702));
#44719=CARTESIAN_POINT('Ctrl Pts',(-35.0661121179879,4.12863692295904,15.1537840479596));
#44720=CARTESIAN_POINT('Ctrl Pts',(-35.1104636563205,4.12967484246056,13.6519484369461));
#44721=CARTESIAN_POINT('Ctrl Pts',(-35.1382705165157,4.13026347554627,12.3973742129691));
#44722=CARTESIAN_POINT('Ctrl Pts',(-35.1496380098962,4.1304972005787,11.8963776288467));
#44723=CARTESIAN_POINT('Ctrl Pts',(-35.1728125176182,4.13095111489406,10.8944707442092));
#44724=CARTESIAN_POINT('Ctrl Pts',(-35.2014663540684,4.13148068919542,9.64189165468456));
#44725=CARTESIAN_POINT('Ctrl Pts',(-35.231695669004,4.1320053583098,8.13739771584359));
#44726=CARTESIAN_POINT('Ctrl Pts',(-35.2466465556333,4.13225112713584,7.13272917219859));
#44727=CARTESIAN_POINT('Ctrl Pts',(-35.2535960572394,4.13236173488828,6.50478605588964));
#44728=CARTESIAN_POINT('Ctrl Pts',(-35.2561917324509,4.13239682594394,6.25449834718108));
#44729=CARTESIAN_POINT('Ctrl Pts',(-35.2607250047413,4.13243619754277,5.75332634083619));
#44730=CARTESIAN_POINT('Ctrl Pts',(-35.2670008280034,4.13243489544792,4.87484930711644));
#44731=CARTESIAN_POINT('Ctrl Pts',(-35.2734810059904,4.13224916658778,3.11467453054322));
#44732=CARTESIAN_POINT('Ctrl Pts',(-35.2705451432604,4.13208318410456,1.60840138381734));
#44733=CARTESIAN_POINT('Ctrl Pts',(-35.2662635206709,4.13227417673443,0.549427262601267));
#44734=CARTESIAN_POINT('Ctrl Pts',(-35.2657011781966,4.13229985044802,0.423333021829396));
#44735=CARTESIAN_POINT('Ctrl Pts',(-35.2643776199116,4.13235997560226,0.171319319719332));
#44736=CARTESIAN_POINT('Ctrl Pts',(-35.2615655281153,4.13248745582765,-0.269221346405241));
#44737=CARTESIAN_POINT('Ctrl Pts',(-35.256279454833,4.13272155600912,-0.897365165415799));
#44738=CARTESIAN_POINT('Ctrl Pts',(-35.2483844930824,4.1330622803331,-1.64964663634109));
#44739=CARTESIAN_POINT('Ctrl Pts',(-35.2364204078958,4.13354951665574,-2.65135422488508));
#44740=CARTESIAN_POINT('Ctrl Pts',(-35.2199669650849,4.13415426865972,-3.90208166627547));
#44741=CARTESIAN_POINT('Ctrl Pts',(-35.2077434624494,4.13446721075594,-4.90370529466454));
#44742=CARTESIAN_POINT('Ctrl Pts',(-35.2011938313991,4.1345652959299,-5.53080166020367));
#44743=CARTESIAN_POINT('Ctrl Pts',(-35.1985491560877,4.13465597637713,-5.78100351140501));
#44744=CARTESIAN_POINT('Ctrl Pts',(-35.193184404245,4.13500168172685,-6.28242334417115));
#44745=CARTESIAN_POINT('Ctrl Pts',(-35.1836501601607,4.13592996924364,-7.16081498294365));
#44746=CARTESIAN_POINT('Ctrl Pts',(-35.1699203342702,4.1375650349294,-8.41814973146324));
#44747=CARTESIAN_POINT('Ctrl Pts',(-35.1568489763635,4.13796350444972,-9.67565452057935));
#44748=CARTESIAN_POINT('Ctrl Pts',(-35.1484688577657,4.13672010875848,-10.5545861827495));
#44749=CARTESIAN_POINT('Ctrl Pts',(-35.1439609354925,4.13544997937989,-11.0562588986197));
#44750=CARTESIAN_POINT('Ctrl Pts',(-35.141810878656,4.13460750086697,-11.306833411016));
#44751=CARTESIAN_POINT('Ctrl Pts',(-35.1402343761306,4.13388694757193,-11.4955612126141));
#44752=CARTESIAN_POINT('Ctrl Pts',(-35.1393081495296,4.13321410289795,-11.6260501035739));
#44753=CARTESIAN_POINT('Ctrl Pts',(-35.1379408867715,4.13125114945088,-11.8839744204317));
#44754=CARTESIAN_POINT('Ctrl Pts',(-35.1366985116337,4.12632895965004,-12.3341277104814));
#44755=CARTESIAN_POINT('Ctrl Pts',(-35.1378308936329,4.11182271700753,-13.2248318815983));
#44756=CARTESIAN_POINT('Ctrl Pts',(-35.1441065414938,4.08496712983523,-14.4741394283709));
#44757=CARTESIAN_POINT('Ctrl Pts',(-35.1418197055586,4.07014756164377,-15.5751678386826));
#44758=CARTESIAN_POINT('Ctrl Pts',(-35.1313495071724,4.07073710575434,-16.3019891761704));
#44759=CARTESIAN_POINT('Ctrl Pts',(-35.121608184413,4.07430272641184,-16.7848166575302));
#44760=CARTESIAN_POINT('Ctrl Pts',(-35.1107864857476,4.08097893857506,-17.1451542089021));
#44761=CARTESIAN_POINT('Ctrl Pts',(-35.0993698341385,4.08919513124322,-17.444274461113));
#44762=CARTESIAN_POINT('Ctrl Pts',(-35.0947277707573,4.09267256341334,-17.5688300168412));
#44763=CARTESIAN_POINT('Ctrl Pts',(-35.0849897417642,4.09975826024745,-17.8141846015044));
#44764=CARTESIAN_POINT('Ctrl Pts',(-35.0745689837778,4.10725125569426,-18.0606167367435));
#44765=CARTESIAN_POINT('Ctrl Pts',(-35.0634683762102,4.11514971682738,-18.3060977674861));
#44766=CARTESIAN_POINT('Ctrl Pts',(-35.0562489157122,4.12027724003972,-18.4595759289252));
#44767=CARTESIAN_POINT('Ctrl Pts',(-35.0503046554234,4.12449618803505,-18.5822356495345));
#44768=CARTESIAN_POINT('Ctrl Pts',(-35.0457624107642,4.12772149878551,-18.6742136748583));
#44769=CARTESIAN_POINT('Ctrl Pts',(-35.0419073345998,4.13046087627797,-18.7508285633372));
#44770=CARTESIAN_POINT('Ctrl Pts',(-35.0387813322475,4.13268440455978,-18.8121067243344));
#44771=CARTESIAN_POINT('Ctrl Pts',(-35.0119742796186,4.15176585766008,-19.3328704769047));
#44772=CARTESIAN_POINT('Ctrl Pts',(-34.9532535258076,4.19404968236951,-20.3253393265434));
#44773=CARTESIAN_POINT('Ctrl Pts',(-34.8461218146786,4.27942771662531,-21.7816710285928));
#44774=CARTESIAN_POINT('Ctrl Pts',(-34.7622578092432,4.35679604434441,-22.7453677417508));
#44775=CARTESIAN_POINT('Ctrl Pts',(-34.706406162113,4.41359504135659,-23.3433389942894));
#44776=CARTESIAN_POINT('Ctrl Pts',(-34.6833510241288,4.43645887396516,-23.569994506372));
#44777=CARTESIAN_POINT('Ctrl Pts',(-34.6330016880252,4.4885780630418,-24.0356330706474));
#44778=CARTESIAN_POINT('Ctrl Pts',(-34.5360070120987,4.59281761600238,-24.8623897228399));
#44779=CARTESIAN_POINT('Ctrl Pts',(-34.3820291507108,4.77043318206014,-26.0866615025097));
#44780=CARTESIAN_POINT('Ctrl Pts',(-34.2022501573895,4.99816048642765,-27.6132729740688));
#44781=CARTESIAN_POINT('Ctrl Pts',(-34.1027071534334,5.1379235449416,-28.6661517966464));
#44782=CARTESIAN_POINT('Ctrl Pts',(-34.0571678319435,5.20670175305063,-29.2667089999963));
#44783=CARTESIAN_POINT('Ctrl Pts',(-34.0475707497204,5.22111959663242,-29.3938797417371));
#44784=CARTESIAN_POINT('Ctrl Pts',(-34.028604724881,5.24989871176608,-29.6515276224334));
#44785=CARTESIAN_POINT('Ctrl Pts',(-33.9966956201125,5.29886863680857,-30.1001465639621));
#44786=CARTESIAN_POINT('Ctrl Pts',(-33.9373100165154,5.39282960398277,-30.9966143632554));
#44787=CARTESIAN_POINT('Ctrl Pts',(-33.8645874739112,5.51821529383873,-32.2702458590929));
#44788=CARTESIAN_POINT('Ctrl Pts',(-33.8064510099774,5.63971813877035,-33.5349589050601));
#44789=CARTESIAN_POINT('Ctrl Pts',(-33.7683455906899,5.7389447926161,-34.5402288448051));
#44790=CARTESIAN_POINT('Ctrl Pts',(-33.7520623330603,5.7898959112938,-35.0406188720943));
#44791=CARTESIAN_POINT('Ctrl Pts',(-33.7408550265922,5.82900185369701,-35.4160583242001));
#44792=CARTESIAN_POINT('Ctrl Pts',(-33.7337120782534,5.85558598327124,-35.6703707812536));
#44793=CARTESIAN_POINT('Ctrl Pts',(-33.7214975953452,5.90909851202696,-36.1765585679139));
#44794=CARTESIAN_POINT('Ctrl Pts',(-33.7048437401063,6.00391340131153,-37.0614840895988));
#44795=CARTESIAN_POINT('Ctrl Pts',(-33.6871930062667,6.19640568017478,-38.8247048152405));
#44796=CARTESIAN_POINT('Ctrl Pts',(-33.6875279344711,6.36198945552724,-40.3331023868815));
#44797=CARTESIAN_POINT('Ctrl Pts',(-33.6841924063127,6.49458121699268,-41.5934174987506));
#44798=CARTESIAN_POINT('Ctrl Pts',(-33.6821137715501,6.53196170930422,-41.9824794946003));
#44799=CARTESIAN_POINT('Ctrl Pts',(-33.679556733124,6.5772536395265,-42.4914256240316));
#44800=CARTESIAN_POINT('Ctrl Pts',(-33.6770099690003,6.620695310972,-43.0000005480967));
#44801=CARTESIAN_POINT('Ctrl Pts',(-33.6743938165608,6.67262545242617,-43.6309140576139));
#44802=CARTESIAN_POINT('Ctrl Pts',(-33.6732482990849,6.73562411321624,-44.3813762849106));
#44803=CARTESIAN_POINT('Ctrl Pts',(-33.6750148369926,6.79223088432819,-45.0001966598899));
#44804=CARTESIAN_POINT('Ctrl Pts',(-33.6787189503938,6.84204581217287,-45.4911432491135));
#44805=CARTESIAN_POINT('Ctrl Pts',(-33.6828304981533,6.88220169762101,-45.8571387897004));
#44806=CARTESIAN_POINT('Ctrl Pts',(-33.6884615838597,6.92566096901639,-46.2208631850937));
#44807=CARTESIAN_POINT('Ctrl Pts',(-33.6982732935283,6.98864642005644,-46.7025690396419));
#44808=CARTESIAN_POINT('Ctrl Pts',(-33.7085346202646,7.04235764800512,-47.0601519723601));
#44809=CARTESIAN_POINT('Ctrl Pts',(-33.7212722467874,7.10134745665142,-47.4153765739217));
#44810=CARTESIAN_POINT('Ctrl Pts',(-33.7314208231614,7.14258540636038,-47.6399758670332));
#44811=CARTESIAN_POINT('Ctrl Pts',(-33.7534691984642,7.23698283658163,-48.1040531003266));
#44812=CARTESIAN_POINT('Ctrl Pts',(-33.7979240267016,7.42695396238463,-48.92862246813));
#44813=CARTESIAN_POINT('Ctrl Pts',(-33.8750212652659,7.74746631799993,-50.1571729190925));
#44814=CARTESIAN_POINT('Ctrl Pts',(-33.9860074859701,8.13149946354455,-51.7127427401713));
#44815=CARTESIAN_POINT('Ctrl Pts',(-34.0713501839444,8.32979075078484,-52.8140558450433));
#44816=CARTESIAN_POINT('Ctrl Pts',(-34.1279026169198,8.41488069409226,-53.5266584439897));
#44817=CARTESIAN_POINT('Ctrl Pts',(-34.1521464533961,8.44513849395254,-53.8262267687612));
#44818=CARTESIAN_POINT('Ctrl Pts',(-34.207293150626,8.48620986701366,-54.4060453279635));
#44819=CARTESIAN_POINT('Ctrl Pts',(-34.3175688808009,8.51763639437878,-55.3935232737951));
#44820=CARTESIAN_POINT('Ctrl Pts',(-34.5699847343345,8.47249989383399,-57.2344911268215));
#44821=CARTESIAN_POINT('Ctrl Pts',(-34.7746778991959,8.44131811526072,-58.5633838426194));
#44822=CARTESIAN_POINT('Ctrl Pts',(-34.8537635343935,8.54158719923408,-59.3846211416249));
#44823=CARTESIAN_POINT('Ctrl Pts',(-34.8628060411605,8.55674888349594,-59.5069065816396));
#44824=CARTESIAN_POINT('Ctrl Pts',(-34.8793880214111,8.58728052614665,-59.7388357980033));
#44825=CARTESIAN_POINT('Ctrl Pts',(-34.9043889070503,8.64584732171681,-60.1510438483319));
#44826=CARTESIAN_POINT('Ctrl Pts',(-34.9400432330761,8.78036742190039,-60.9699513878294));
#44827=CARTESIAN_POINT('Ctrl Pts',(-34.9549177016221,8.9761062550776,-61.9045297714664));
#44828=CARTESIAN_POINT('Ctrl Pts',(-34.9577338936852,9.21318808548523,-62.8293999036441));
#44829=CARTESIAN_POINT('Ctrl Pts',(-34.9573014231098,9.36195520020049,-63.346014853301));
#44830=CARTESIAN_POINT('Ctrl Pts',(-34.9572064571472,9.46749706221942,-63.6883948443447));
#44831=CARTESIAN_POINT('Ctrl Pts',(-34.9572605397201,9.53955730596001,-63.9161318348065));
#44832=CARTESIAN_POINT('Ctrl Pts',(-34.9575908470543,9.61413235727968,-64.1429475604759));
#44833=CARTESIAN_POINT('Ctrl Pts',(-34.9582951148639,9.68160942583985,-64.3406542831807));
#44834=CARTESIAN_POINT('Ctrl Pts',(-34.9588401780772,9.72079980598956,-64.4533965094004));
#44835=CARTESIAN_POINT('Ctrl Pts',(-34.9598126220336,9.78020955611649,-64.6222548455309));
#44836=CARTESIAN_POINT('Ctrl Pts',(-34.9609690699538,9.83103756829643,-64.7624807874525));
#44837=CARTESIAN_POINT('Ctrl Pts',(-34.9634776811836,9.91675954430774,-64.9935028616406));
#44838=CARTESIAN_POINT('Ctrl Pts',(-34.96591894868,10.0007393764809,-65.2093463422365));
#44839=CARTESIAN_POINT('Ctrl Pts',(-34.9694931577729,10.1899720025443,-65.6590816875894));
#44840=CARTESIAN_POINT('Ctrl Pts',(-34.9729628294964,10.5587860036188,-66.4508818038113));
#44841=CARTESIAN_POINT('Ctrl Pts',(-34.9713192854846,11.4366459032312,-68.0906323997746));
#44842=CARTESIAN_POINT('Ctrl Pts',(-34.9635298547312,12.3319946487882,-69.5856482008091));
#44843=CARTESIAN_POINT('Ctrl Pts',(-34.9624949509692,12.963182570155,-70.7858400367887));
#44844=CARTESIAN_POINT('Ctrl Pts',(-34.9625378096041,13.0919432799083,-71.0304000935673));
#44845=CARTESIAN_POINT('Ctrl Pts',(-34.9624838804023,13.3571207722334,-71.5327690442754));
#44846=CARTESIAN_POINT('Ctrl Pts',(-34.9625019627237,13.6869700850091,-72.1554406364071));
#44847=CARTESIAN_POINT('Ctrl Pts',(-34.9625174690599,14.0859380620031,-72.9060232117717));
#44848=CARTESIAN_POINT('Ctrl Pts',(-34.9626013152313,14.8854237837734,-74.4064026651871));
#44849=CARTESIAN_POINT('Ctrl Pts',(-34.9626837410002,15.5555645254436,-75.6594313764821));
#44850=CARTESIAN_POINT('Ctrl Pts',(-34.9626343711923,16.5274626633202,-77.4871400248605));
#44851=CARTESIAN_POINT('Ctrl Pts',(-34.962651678487,16.9631231181656,-78.3064115555001));
#44852=CARTESIAN_POINT('Ctrl Pts',(-34.9626516784869,17.399644705555,-79.1273892575985));
#44853=CARTESIAN_POINT('Ctrl Pts',(-33.6411326911163,4.10026185094264,24.8306459276114));
#44854=CARTESIAN_POINT('Ctrl Pts',(-33.6412319642584,4.10026360106523,24.7817669795734));
#44855=CARTESIAN_POINT('Ctrl Pts',(-33.6413360808126,4.10026543744567,24.7328890984256));
#44856=CARTESIAN_POINT('Ctrl Pts',(-33.6425655719406,4.10028706581328,24.1822851100102));
#44857=CARTESIAN_POINT('Ctrl Pts',(-33.6435016984766,4.10030759411697,23.1781500341781));
#44858=CARTESIAN_POINT('Ctrl Pts',(-33.6456766501809,4.10035873990036,21.1695607665509));
#44859=CARTESIAN_POINT('Ctrl Pts',(-33.6538592406256,4.10050219788364,19.6654154519402));
#44860=CARTESIAN_POINT('Ctrl Pts',(-33.6712444936077,4.10078633831224,18.4143725466167));
#44861=CARTESIAN_POINT('Ctrl Pts',(-33.6795800814252,4.10092488279933,17.9115781933392));
#44862=CARTESIAN_POINT('Ctrl Pts',(-33.7005079290768,4.10127689066396,16.9076016065011));
#44863=CARTESIAN_POINT('Ctrl Pts',(-33.7453987627603,4.10203095679594,15.1537767319238));
#44864=CARTESIAN_POINT('Ctrl Pts',(-33.7880838027813,4.10271762577904,13.6519492833216));
#44865=CARTESIAN_POINT('Ctrl Pts',(-33.8149066064565,4.10309050489671,12.3973832444834));
#44866=CARTESIAN_POINT('Ctrl Pts',(-33.8258787168521,4.1032365923497,11.8963903279294));
#44867=CARTESIAN_POINT('Ctrl Pts',(-33.8482694459468,4.10351371263629,10.894489599616));
#44868=CARTESIAN_POINT('Ctrl Pts',(-33.8759851887753,4.10382707692016,9.64191824077783));
#44869=CARTESIAN_POINT('Ctrl Pts',(-33.9052571194612,4.10412628544038,8.13742690599753));
#44870=CARTESIAN_POINT('Ctrl Pts',(-33.9197457328913,4.10426097418009,7.13275747992258));
#44871=CARTESIAN_POINT('Ctrl Pts',(-33.9264832272774,4.10432008724947,6.5048104286386));
#44872=CARTESIAN_POINT('Ctrl Pts',(-33.9290082793269,4.10433492266779,6.25450674375847));
#44873=CARTESIAN_POINT('Ctrl Pts',(-33.9334483969372,4.10433539753158,5.75331657478791));
#44874=CARTESIAN_POINT('Ctrl Pts',(-33.9396696168259,4.10427149430696,4.87481780318893));
#44875=CARTESIAN_POINT('Ctrl Pts',(-33.9463360604202,4.10399671666449,3.11465231775271));
#44876=CARTESIAN_POINT('Ctrl Pts',(-33.9435846569382,4.10385606244802,1.60848592985718));
#44877=CARTESIAN_POINT('Ctrl Pts',(-33.9389933726073,4.10415579520968,0.549631462269671));
#44878=CARTESIAN_POINT('Ctrl Pts',(-33.9383908140295,4.10419580157567,0.42355837231207));
#44879=CARTESIAN_POINT('Ctrl Pts',(-33.9369740111061,4.10428919894098,0.171580645918622));
#44880=CARTESIAN_POINT('Ctrl Pts',(-33.9339675769833,4.10448653180307,-0.26890088168996));
#44881=CARTESIAN_POINT('Ctrl Pts',(-33.9283281005373,4.10484830380246,-0.896973413154935));
#44882=CARTESIAN_POINT('Ctrl Pts',(-33.9199306318175,4.10537599982153,-1.6492033384174));
#44883=CARTESIAN_POINT('Ctrl Pts',(-33.9072484325072,4.10613579640971,-2.65086985568805));
#44884=CARTESIAN_POINT('Ctrl Pts',(-33.8899141021628,4.10709449182581,-3.9016334018584));
#44885=CARTESIAN_POINT('Ctrl Pts',(-33.8772276156682,4.10762512106839,-4.90334621637353));
#44886=CARTESIAN_POINT('Ctrl Pts',(-33.870536464046,4.10781629048305,-5.53054386391947));
#44887=CARTESIAN_POINT('Ctrl Pts',(-33.8677938414917,4.10793359346624,-5.78086565463426));
#44888=CARTESIAN_POINT('Ctrl Pts',(-33.8621020242897,4.10829656757102,-6.28243488902562));
#44889=CARTESIAN_POINT('Ctrl Pts',(-33.8517440194913,4.10917896514089,-7.16101104825188));
#44890=CARTESIAN_POINT('Ctrl Pts',(-33.8366414601763,4.11063653194915,-8.41828561880177));
#44891=CARTESIAN_POINT('Ctrl Pts',(-33.8233433932831,4.11099976811112,-9.67537954825846));
#44892=CARTESIAN_POINT('Ctrl Pts',(-33.8161444164405,4.10996469475177,-10.5538587598376));
#44893=CARTESIAN_POINT('Ctrl Pts',(-33.8127994565897,4.10890199074922,-11.0552106007861));
#44894=CARTESIAN_POINT('Ctrl Pts',(-33.8114108089721,4.10819573101564,-11.3056275282183));
#44895=CARTESIAN_POINT('Ctrl Pts',(-33.8104823372999,4.10759167960374,-11.4941670743556));
#44896=CARTESIAN_POINT('Ctrl Pts',(-33.8099681540024,4.10709912694592,-11.6224051077876));
#44897=CARTESIAN_POINT('Ctrl Pts',(-33.8093466060482,4.10580528279857,-11.8773977646603));
#44898=CARTESIAN_POINT('Ctrl Pts',(-33.8092393917502,4.10279420483067,-12.3226678483256));
#44899=CARTESIAN_POINT('Ctrl Pts',(-33.8122458515501,4.09433979998904,-13.2075524799972));
#44900=CARTESIAN_POINT('Ctrl Pts',(-33.8217592897651,4.07845534668309,-14.4585286523619));
#44901=CARTESIAN_POINT('Ctrl Pts',(-33.826957607454,4.06742061966935,-15.5735444655491));
#44902=CARTESIAN_POINT('Ctrl Pts',(-33.8249946539307,4.06478942374908,-16.3146866760876));
#44903=CARTESIAN_POINT('Ctrl Pts',(-33.8219696167977,4.06451266184445,-16.8083714860037));
#44904=CARTESIAN_POINT('Ctrl Pts',(-33.8174632618617,4.06620198770372,-17.1783068288034));
#44905=CARTESIAN_POINT('Ctrl Pts',(-33.8121471833676,4.06891067784961,-17.4860839934021));
#44906=CARTESIAN_POINT('Ctrl Pts',(-33.8100849824204,4.06996587647673,-17.6124840694276));
#44907=CARTESIAN_POINT('Ctrl Pts',(-33.806081214047,4.0719464040068,-17.8623067622636));
#44908=CARTESIAN_POINT('Ctrl Pts',(-33.8022014354793,4.07380820348422,-18.1126804113533));
#44909=CARTESIAN_POINT('Ctrl Pts',(-33.7983301480892,4.07565030346945,-18.362086011253));
#44910=CARTESIAN_POINT('Ctrl Pts',(-33.7958893750828,4.07681658210632,-18.5178991825193));
#44911=CARTESIAN_POINT('Ctrl Pts',(-33.7939097121451,4.07777090382214,-18.6423949041297));
#44912=CARTESIAN_POINT('Ctrl Pts',(-33.7924076996464,4.07850068069895,-18.7357232360661));
#44913=CARTESIAN_POINT('Ctrl Pts',(-33.7911385497741,4.0791231282861,-18.8134464020888));
#44914=CARTESIAN_POINT('Ctrl Pts',(-33.7901110297683,4.07963123050946,-18.8755990867573));
#44915=CARTESIAN_POINT('Ctrl Pts',(-33.7813013508289,4.08401178691256,-19.4037380359828));
#44916=CARTESIAN_POINT('Ctrl Pts',(-33.7619344413257,4.0945523600764,-20.4085240838739));
#44917=CARTESIAN_POINT('Ctrl Pts',(-33.7108942174128,4.12835178280623,-21.8787507168737));
#44918=CARTESIAN_POINT('Ctrl Pts',(-33.6512903133875,4.1694546614518,-22.8494396287991));
#44919=CARTESIAN_POINT('Ctrl Pts',(-33.6029153793199,4.20211921413237,-23.4511320389435));
#44920=CARTESIAN_POINT('Ctrl Pts',(-33.5820342108033,4.21590135193268,-23.6858582587801));
#44921=CARTESIAN_POINT('Ctrl Pts',(-33.5341979212337,4.2467529824973,-24.1612926439125));
#44922=CARTESIAN_POINT('Ctrl Pts',(-33.4367464051988,4.30772793100384,-25.0014216097737));
#44923=CARTESIAN_POINT('Ctrl Pts',(-33.2713525856663,4.40626964399774,-26.2283412604594));
#44924=CARTESIAN_POINT('Ctrl Pts',(-33.0732000001619,4.52288389107786,-27.7394229849092));
#44925=CARTESIAN_POINT('Ctrl Pts',(-32.966153269682,4.59294847833412,-28.7702324944338));
#44926=CARTESIAN_POINT('Ctrl Pts',(-32.9185127843775,4.62901401097156,-29.3551201315721));
#44927=CARTESIAN_POINT('Ctrl Pts',(-32.9081220344998,4.63671765787494,-29.4812765337408));
#44928=CARTESIAN_POINT('Ctrl Pts',(-32.8877533460928,4.65204508403021,-29.7355888702512));
#44929=CARTESIAN_POINT('Ctrl Pts',(-32.8533178540442,4.67828853827645,-30.1792586022513));
#44930=CARTESIAN_POINT('Ctrl Pts',(-32.7890377277273,4.72927355630562,-31.0660416354241));
#44931=CARTESIAN_POINT('Ctrl Pts',(-32.7096945706555,4.80034467398294,-32.3281471555683));
#44932=CARTESIAN_POINT('Ctrl Pts',(-32.645543075087,4.87557053433749,-33.5835486060134));
#44933=CARTESIAN_POINT('Ctrl Pts',(-32.6028255393445,4.94170126882913,-34.5827075325046));
#44934=CARTESIAN_POINT('Ctrl Pts',(-32.5843091448841,4.9773109596408,-35.0804869953707));
#44935=CARTESIAN_POINT('Ctrl Pts',(-32.5714311729237,5.00524972267996,-35.4540879938655));
#44936=CARTESIAN_POINT('Ctrl Pts',(-32.5632505675272,5.0244507512656,-35.7062386614517));
#44937=CARTESIAN_POINT('Ctrl Pts',(-32.5488818356357,5.06409381237342,-36.2088033664596));
#44938=CARTESIAN_POINT('Ctrl Pts',(-32.5283727865902,5.13675175346187,-37.0875504480415));
#44939=CARTESIAN_POINT('Ctrl Pts',(-32.5024985675524,5.29328057889031,-38.8399712834976));
#44940=CARTESIAN_POINT('Ctrl Pts',(-32.4943551753827,5.44071029761429,-40.3411442865328));
#44941=CARTESIAN_POINT('Ctrl Pts',(-32.4830885255742,5.56383169955982,-41.5961824692435));
#44942=CARTESIAN_POINT('Ctrl Pts',(-32.4785943977942,5.5983872109969,-41.987177810346));
#44943=CARTESIAN_POINT('Ctrl Pts',(-32.4730549529468,5.63986342477469,-42.4954123978076));
#44944=CARTESIAN_POINT('Ctrl Pts',(-32.4675331943491,5.67971433766435,-43.0028939982844));
#44945=CARTESIAN_POINT('Ctrl Pts',(-32.4611691477671,5.72785009583342,-43.6306186242469));
#44946=CARTESIAN_POINT('Ctrl Pts',(-32.4551335658941,5.78839748470127,-44.3748615626198));
#44947=CARTESIAN_POINT('Ctrl Pts',(-32.4522485725628,5.84546817355414,-44.9863862996825));
#44948=CARTESIAN_POINT('Ctrl Pts',(-32.4517460422648,5.89764344956478,-45.4703023591762));
#44949=CARTESIAN_POINT('Ctrl Pts',(-32.4524203330941,5.94064103534309,-45.8304087771301));
#44950=CARTESIAN_POINT('Ctrl Pts',(-32.4542962913942,5.98811752979867,-46.1876370266157));
#44951=CARTESIAN_POINT('Ctrl Pts',(-32.4586341263884,6.05816853842575,-46.6598808527028));
#44952=CARTESIAN_POINT('Ctrl Pts',(-32.4642005198337,6.11918888790148,-47.009441058689));
#44953=CARTESIAN_POINT('Ctrl Pts',(-32.4717830091301,6.18707038495651,-47.3560463636611));
#44954=CARTESIAN_POINT('Ctrl Pts',(-32.4784343104161,6.23444778201298,-47.5746165913903));
#44955=CARTESIAN_POINT('Ctrl Pts',(-32.491738375135,6.34340193121187,-48.0281241302287));
#44956=CARTESIAN_POINT('Ctrl Pts',(-32.5171296125407,6.56412915175324,-48.8368831289162));
#44957=CARTESIAN_POINT('Ctrl Pts',(-32.5571918409076,6.94345938666132,-50.0494377073212));
#44958=CARTESIAN_POINT('Ctrl Pts',(-32.6163517692873,7.419793013619,-51.5919017767001));
#44959=CARTESIAN_POINT('Ctrl Pts',(-32.671173221184,7.69197796679143,-52.6890339309171));
#44960=CARTESIAN_POINT('Ctrl Pts',(-32.7140153006268,7.82566351500892,-53.4017620163245));
#44961=CARTESIAN_POINT('Ctrl Pts',(-32.7331936544609,7.87607349739887,-53.6899524232844));
#44962=CARTESIAN_POINT('Ctrl Pts',(-32.7796961693441,7.96173857270317,-54.2566674391624));
#44963=CARTESIAN_POINT('Ctrl Pts',(-32.8792227654141,8.07816823912663,-55.2254883969868));
#44964=CARTESIAN_POINT('Ctrl Pts',(-33.1306365058374,8.21417318520405,-57.061460046734));
#44965=CARTESIAN_POINT('Ctrl Pts',(-33.3578423373758,8.29468476161207,-58.4293603073941));
#44966=CARTESIAN_POINT('Ctrl Pts',(-33.4479574718128,8.44121786586595,-59.3029834712513));
#44967=CARTESIAN_POINT('Ctrl Pts',(-33.4582700939901,8.46254072077173,-59.4299480885089));
#44968=CARTESIAN_POINT('Ctrl Pts',(-33.4777130686063,8.50398485229622,-59.6716354324499));
#44969=CARTESIAN_POINT('Ctrl Pts',(-33.5082643182909,8.57944022538127,-60.0992251957493));
#44970=CARTESIAN_POINT('Ctrl Pts',(-33.5569795000898,8.7387053594895,-60.9443011477612));
#44971=CARTESIAN_POINT('Ctrl Pts',(-33.5894256340183,8.94660383900336,-61.8977200611756));
#44972=CARTESIAN_POINT('Ctrl Pts',(-33.6092077650122,9.18702922879557,-62.8311702464978));
#44973=CARTESIAN_POINT('Ctrl Pts',(-33.6175011214833,9.33564698997536,-63.348830090218));
#44974=CARTESIAN_POINT('Ctrl Pts',(-33.6226392855976,9.44073841860971,-63.6904094221816));
#44975=CARTESIAN_POINT('Ctrl Pts',(-33.6260111407969,9.51243779257545,-63.9172154175434));
#44976=CARTESIAN_POINT('Ctrl Pts',(-33.6293782288212,9.58661034444336,-64.1425323012807));
#44977=CARTESIAN_POINT('Ctrl Pts',(-33.6324528341531,9.65378130604465,-64.3384287527984));
#44978=CARTESIAN_POINT('Ctrl Pts',(-33.6342644595799,9.69282161070932,-64.4499981222251));
#44979=CARTESIAN_POINT('Ctrl Pts',(-33.6370457909584,9.75203945725312,-64.6169660163557));
#44980=CARTESIAN_POINT('Ctrl Pts',(-33.6395144700785,9.80277974980643,-64.7553260994723));
#44981=CARTESIAN_POINT('Ctrl Pts',(-33.643901811797,9.88857364994285,-64.9830350846743));
#44982=CARTESIAN_POINT('Ctrl Pts',(-33.64795082258,9.97481551633586,-65.2020234088409));
#44983=CARTESIAN_POINT('Ctrl Pts',(-33.6539259758458,10.1666026322723,-65.6538302753117));
#44984=CARTESIAN_POINT('Ctrl Pts',(-33.6595924304936,10.5389370692624,-66.450124424042));
#44985=CARTESIAN_POINT('Ctrl Pts',(-33.6568032203678,11.4174925225938,-68.0934461183711));
#44986=CARTESIAN_POINT('Ctrl Pts',(-33.6448003690798,12.3077449575316,-69.5882021446881));
#44987=CARTESIAN_POINT('Ctrl Pts',(-33.6443502923429,12.9372441435451,-70.78536641954));
#44988=CARTESIAN_POINT('Ctrl Pts',(-33.644421177294,13.0660882833516,-71.0301126250275));
#44989=CARTESIAN_POINT('Ctrl Pts',(-33.6444502761828,13.3311776194155,-71.5323573056357));
#44990=CARTESIAN_POINT('Ctrl Pts',(-33.6445039851306,13.6610432733458,-72.1551025215315));
#44991=CARTESIAN_POINT('Ctrl Pts',(-33.6445190387081,14.0599875174264,-72.905650919379));
#44992=CARTESIAN_POINT('Ctrl Pts',(-33.6445189626518,14.8594904448648,-74.4060444270055));
#44993=CARTESIAN_POINT('Ctrl Pts',(-33.6444474180559,15.5296998311147,-75.6591844317331));
#44994=CARTESIAN_POINT('Ctrl Pts',(-33.6444118288596,16.5016455819358,-77.4870156479218));
#44995=CARTESIAN_POINT('Ctrl Pts',(-33.6444226998529,16.937307679145,-78.3063082760182));
#44996=CARTESIAN_POINT('Ctrl Pts',(-33.6444226998529,17.3738292665345,-79.1272859781166));
#44997=CARTESIAN_POINT('Ctrl Pts',(-31.9345162052867,4.08110750609352,24.8306358879163));
#44998=CARTESIAN_POINT('Ctrl Pts',(-31.9346105672387,4.08110819548476,24.7817566190947));
#44999=CARTESIAN_POINT('Ctrl Pts',(-31.9347095334598,4.08110891921601,24.7328784098582));
#45000=CARTESIAN_POINT('Ctrl Pts',(-31.9358781874058,4.08111743380434,24.1822706987579));
#45001=CARTESIAN_POINT('Ctrl Pts',(-31.9367672433101,4.08112326086448,23.1781322117713));
#45002=CARTESIAN_POINT('Ctrl Pts',(-31.9388326194472,4.08113679606785,21.1695357424094));
#45003=CARTESIAN_POINT('Ctrl Pts',(-31.946610252159,4.08119335240847,19.6653873712976));
#45004=CARTESIAN_POINT('Ctrl Pts',(-31.9631386790618,4.08131650188692,18.4143428073606));
#45005=CARTESIAN_POINT('Ctrl Pts',(-31.9710628413259,4.08137603223171,17.9115301783847));
#45006=CARTESIAN_POINT('Ctrl Pts',(-31.9909565725438,4.08152662960907,16.9075412729775));
#45007=CARTESIAN_POINT('Ctrl Pts',(-32.0336289154702,4.08185001958378,15.1537208236703));
#45008=CARTESIAN_POINT('Ctrl Pts',(-32.0742120066795,4.08215507985313,13.6519552942647));
#45009=CARTESIAN_POINT('Ctrl Pts',(-32.0997282221007,4.08233864079097,12.3974657568081));
#45010=CARTESIAN_POINT('Ctrl Pts',(-32.110167841507,4.0824130160868,11.8965046392989));
#45011=CARTESIAN_POINT('Ctrl Pts',(-32.1314779092244,4.08256217926155,10.894650705752));
#45012=CARTESIAN_POINT('Ctrl Pts',(-32.1578644090397,4.08274427283381,9.64211396348586));
#45013=CARTESIAN_POINT('Ctrl Pts',(-32.185737655173,4.08293120790136,8.13761947351068));
#45014=CARTESIAN_POINT('Ctrl Pts',(-32.1995331755596,4.08302108192031,7.13291957650245));
#45015=CARTESIAN_POINT('Ctrl Pts',(-32.2059464348698,4.08306126353903,6.50494606817195));
#45016=CARTESIAN_POINT('Ctrl Pts',(-32.2083604990054,4.08307323060974,6.25468682633457));
#45017=CARTESIAN_POINT('Ctrl Pts',(-32.2126422905571,4.0830836800604,5.75353858246067));
#45018=CARTESIAN_POINT('Ctrl Pts',(-32.2187298472004,4.08307184393253,4.87509428458592));
#45019=CARTESIAN_POINT('Ctrl Pts',(-32.2255176385181,4.08297792425966,3.11487633929514));
#45020=CARTESIAN_POINT('Ctrl Pts',(-32.2228927810643,4.0829308868657,1.6084311816116));
#45021=CARTESIAN_POINT('Ctrl Pts',(-32.217800225808,4.08307339977907,0.549250313299977));
#45022=CARTESIAN_POINT('Ctrl Pts',(-32.2171333159763,4.08309239505471,0.423122664200472));
#45023=CARTESIAN_POINT('Ctrl Pts',(-32.2155698373408,4.08313646376419,0.171051744769676));
#45024=CARTESIAN_POINT('Ctrl Pts',(-32.2122631461247,4.0832289645913,-0.269581450850985));
#45025=CARTESIAN_POINT('Ctrl Pts',(-32.2060878540656,4.08339696087033,-0.897818447216643));
#45026=CARTESIAN_POINT('Ctrl Pts',(-32.1969399867877,4.08363936646349,-1.65017409988339));
#45027=CARTESIAN_POINT('Ctrl Pts',(-32.183190880734,4.08398461266246,-2.65190200041652));
#45028=CARTESIAN_POINT('Ctrl Pts',(-32.1645543960765,4.08441089388571,-3.90256933832878));
#45029=CARTESIAN_POINT('Ctrl Pts',(-32.1511779928535,4.08463278729394,-4.90399868829054));
#45030=CARTESIAN_POINT('Ctrl Pts',(-32.1442675643117,4.08470349532937,-5.5310003029722));
#45031=CARTESIAN_POINT('Ctrl Pts',(-32.141443450968,4.08473411273331,-5.78184669019702));
#45032=CARTESIAN_POINT('Ctrl Pts',(-32.1356144713648,4.08479989308598,-6.28393036002289));
#45033=CARTESIAN_POINT('Ctrl Pts',(-32.1250866926104,4.08491789176519,-7.16315027258674));
#45034=CARTESIAN_POINT('Ctrl Pts',(-32.1099595557051,4.08504477551121,-8.41994436870759));
#45035=CARTESIAN_POINT('Ctrl Pts',(-32.0969731510966,4.08498556154858,-9.67493422699999));
#45036=CARTESIAN_POINT('Ctrl Pts',(-32.0901934533112,4.08477864334628,-10.5510367326364));
#45037=CARTESIAN_POINT('Ctrl Pts',(-32.0871489980332,4.08460301614872,-11.0507722276167));
#45038=CARTESIAN_POINT('Ctrl Pts',(-32.0859314968414,4.08449419906031,-11.300307995852));
#45039=CARTESIAN_POINT('Ctrl Pts',(-32.0851400403632,4.08440378635289,-11.4881079878802));
#45040=CARTESIAN_POINT('Ctrl Pts',(-32.084676479878,4.08433773003485,-11.6143548417818));
#45041=CARTESIAN_POINT('Ctrl Pts',(-32.0840061718684,4.08418441062924,-11.8665103449061));
#45042=CARTESIAN_POINT('Ctrl Pts',(-32.0834632744573,4.08386376022149,-12.3070815468493));
#45043=CARTESIAN_POINT('Ctrl Pts',(-32.0845437962985,4.08303573650382,-13.1857153042442));
#45044=CARTESIAN_POINT('Ctrl Pts',(-32.0902649196552,4.08146129759508,-14.4359144556652));
#45045=CARTESIAN_POINT('Ctrl Pts',(-32.0955399985264,4.07998696870516,-15.5604071811699));
#45046=CARTESIAN_POINT('Ctrl Pts',(-32.0970593246399,4.07920603201527,-16.3119948403646));
#45047=CARTESIAN_POINT('Ctrl Pts',(-32.0974049409017,4.07875737974352,-16.8137204991877));
#45048=CARTESIAN_POINT('Ctrl Pts',(-32.0967612035114,4.07851820934122,-17.1909384303492));
#45049=CARTESIAN_POINT('Ctrl Pts',(-32.0955591458867,4.0783944756999,-17.5052480643049));
#45050=CARTESIAN_POINT('Ctrl Pts',(-32.0951785331263,4.07830893422186,-17.6307678456597));
#45051=CARTESIAN_POINT('Ctrl Pts',(-32.0947611684075,4.07802153391888,-17.8811283588127));
#45052=CARTESIAN_POINT('Ctrl Pts',(-32.0947914435315,4.07757715679901,-18.1316402221286));
#45053=CARTESIAN_POINT('Ctrl Pts',(-32.0951376483372,4.07701687846767,-18.3819470814422));
#45054=CARTESIAN_POINT('Ctrl Pts',(-32.0954576236565,4.07662708311104,-18.5383852023367));
#45055=CARTESIAN_POINT('Ctrl Pts',(-32.0957593633384,4.07629641603794,-18.6635057855418));
#45056=CARTESIAN_POINT('Ctrl Pts',(-32.096004322397,4.0760403347023,-18.757339774025));
#45057=CARTESIAN_POINT('Ctrl Pts',(-32.0962205631789,4.07582129407088,-18.8355262789798));
#45058=CARTESIAN_POINT('Ctrl Pts',(-32.0963987625299,4.07564322482876,-18.898071110931));
#45059=CARTESIAN_POINT('Ctrl Pts',(-32.0979374503577,4.07411618025336,-19.4296779691492));
#45060=CARTESIAN_POINT('Ctrl Pts',(-32.1014062968753,4.07083947111897,-20.4453275036986));
#45061=CARTESIAN_POINT('Ctrl Pts',(-32.091375535163,4.07003834507895,-21.9437487586712));
#45062=CARTESIAN_POINT('Ctrl Pts',(-32.0634510847159,4.07541445937402,-22.9421936934073));
#45063=CARTESIAN_POINT('Ctrl Pts',(-32.0357377032757,4.08123731860324,-23.5642997091225));
#45064=CARTESIAN_POINT('Ctrl Pts',(-32.0234900765614,4.08369712503767,-23.8126150139849));
#45065=CARTESIAN_POINT('Ctrl Pts',(-31.9943240335294,4.08879366254401,-24.3087785223559));
#45066=CARTESIAN_POINT('Ctrl Pts',(-31.932439911088,4.09805349845175,-25.1792554912224));
#45067=CARTESIAN_POINT('Ctrl Pts',(-31.8208573144408,4.11046809917765,-26.4257905384195));
#45068=CARTESIAN_POINT('Ctrl Pts',(-31.6775527195453,4.12193231169977,-27.9237041412625));
#45069=CARTESIAN_POINT('Ctrl Pts',(-31.595374453496,4.13049764031296,-28.9218954202539));
#45070=CARTESIAN_POINT('Ctrl Pts',(-31.5582386843568,4.13771925254717,-29.4826943506793));
#45071=CARTESIAN_POINT('Ctrl Pts',(-31.5500189555754,4.13942333750784,-29.6081027205929));
#45072=CARTESIAN_POINT('Ctrl Pts',(-31.5338402768096,4.14276647064553,-29.8583896078162));
#45073=CARTESIAN_POINT('Ctrl Pts',(-31.5061516712207,4.14866697415491,-30.2964630238362));
#45074=CARTESIAN_POINT('Ctrl Pts',(-31.4533147605832,4.16085422920267,-31.1716237260119));
#45075=CARTESIAN_POINT('Ctrl Pts',(-31.3849763731538,4.18120722630591,-32.4191800851958));
#45076=CARTESIAN_POINT('Ctrl Pts',(-31.3259998043518,4.20990488447638,-33.6612396502691));
#45077=CARTESIAN_POINT('Ctrl Pts',(-31.2843934817152,4.2403661598899,-34.6505294036576));
#45078=CARTESIAN_POINT('Ctrl Pts',(-31.2654290237822,4.25847727968631,-35.1436267850304));
#45079=CARTESIAN_POINT('Ctrl Pts',(-31.2518693088976,4.2733344706328,-35.5137598748512));
#45080=CARTESIAN_POINT('Ctrl Pts',(-31.2431724656845,4.2837527640997,-35.7627596706265));
#45081=CARTESIAN_POINT('Ctrl Pts',(-31.2272701574211,4.30616475121193,-36.2597407094396));
#45082=CARTESIAN_POINT('Ctrl Pts',(-31.2029776219995,4.34943726527796,-37.1291764656129));
#45083=CARTESIAN_POINT('Ctrl Pts',(-31.165823696557,4.45072053840333,-38.8655146397168));
#45084=CARTESIAN_POINT('Ctrl Pts',(-31.1438789037403,4.55812564531563,-40.3573310700045));
#45085=CARTESIAN_POINT('Ctrl Pts',(-31.120153611262,4.65319699374158,-41.6062548905775));
#45086=CARTESIAN_POINT('Ctrl Pts',(-31.1120757642504,4.67970788253575,-42.0003677896081));
#45087=CARTESIAN_POINT('Ctrl Pts',(-31.1018334345682,4.71029481371404,-42.5080905849168));
#45088=CARTESIAN_POINT('Ctrl Pts',(-31.0915812944133,4.73947823418146,-43.0145361140732));
#45089=CARTESIAN_POINT('Ctrl Pts',(-31.0791134656114,4.77477568815216,-43.6384222354851));
#45090=CARTESIAN_POINT('Ctrl Pts',(-31.0650476942155,4.82135939840442,-44.3748291118715));
#45091=CARTESIAN_POINT('Ctrl Pts',(-31.0545718522228,4.86839730274684,-44.9770961573069));
#45092=CARTESIAN_POINT('Ctrl Pts',(-31.0472371746296,4.91371893662283,-45.4521586633428));
#45093=CARTESIAN_POINT('Ctrl Pts',(-31.0423675599914,4.95221094591703,-45.8049431946864));
#45094=CARTESIAN_POINT('Ctrl Pts',(-31.0382216264648,4.9958618067405,-46.1542263022132));
#45095=CARTESIAN_POINT('Ctrl Pts',(-31.0337940880935,5.06177203847355,-46.6151421119406));
#45096=CARTESIAN_POINT('Ctrl Pts',(-31.0318867398553,5.12083678396936,-46.955470509921));
#45097=CARTESIAN_POINT('Ctrl Pts',(-31.0311517246586,5.18760011055548,-47.2926014112459));
#45098=CARTESIAN_POINT('Ctrl Pts',(-31.0314818945205,5.23383985222584,-47.506807402411));
#45099=CARTESIAN_POINT('Ctrl Pts',(-31.0296295308109,5.34123088284672,-47.9522952786476));
#45100=CARTESIAN_POINT('Ctrl Pts',(-31.0223479986209,5.56141891612971,-48.7510880924636));
#45101=CARTESIAN_POINT('Ctrl Pts',(-31.0016701388276,5.95147806528555,-49.9552708220521));
#45102=CARTESIAN_POINT('Ctrl Pts',(-30.978041716002,6.46745316602708,-51.4855159642758));
#45103=CARTESIAN_POINT('Ctrl Pts',(-30.9811428160557,6.78945791405842,-52.5670112445759));
#45104=CARTESIAN_POINT('Ctrl Pts',(-30.9970510764194,6.96480480004668,-53.2670657700029));
#45105=CARTESIAN_POINT('Ctrl Pts',(-31.0064285723702,7.03170351427957,-53.5392492637444));
#45106=CARTESIAN_POINT('Ctrl Pts',(-31.0326877123139,7.15826974874841,-54.0831438919574));
#45107=CARTESIAN_POINT('Ctrl Pts',(-31.0979191767971,7.36020117964626,-55.0168985615787));
#45108=CARTESIAN_POINT('Ctrl Pts',(-31.2896973541456,7.70799341593398,-56.8222191651518));
#45109=CARTESIAN_POINT('Ctrl Pts',(-31.497485286898,7.96396009958822,-58.2388060297082));
#45110=CARTESIAN_POINT('Ctrl Pts',(-31.5887272365142,8.19120176241539,-59.1805492639164));
#45111=CARTESIAN_POINT('Ctrl Pts',(-31.5990764671936,8.2224649382114,-59.3108895456909));
#45112=CARTESIAN_POINT('Ctrl Pts',(-31.6197333534618,8.28260653878693,-59.5617233241845));
#45113=CARTESIAN_POINT('Ctrl Pts',(-31.6546315166755,8.38839280464436,-60.0031196869982));
#45114=CARTESIAN_POINT('Ctrl Pts',(-31.7201519725577,8.59874712174735,-60.8735024669699));
#45115=CARTESIAN_POINT('Ctrl Pts',(-31.7844306350037,8.84623710641239,-61.8476249668478));
#45116=CARTESIAN_POINT('Ctrl Pts',(-31.8381023844806,9.11392474038865,-62.7945648109811));
#45117=CARTESIAN_POINT('Ctrl Pts',(-31.86434745316,9.27444966434412,-63.3170202209645));
#45118=CARTESIAN_POINT('Ctrl Pts',(-31.88021843648,9.38649190763133,-63.660719691302));
#45119=CARTESIAN_POINT('Ctrl Pts',(-31.8903662560553,9.46259095181462,-63.8886476577213));
#45120=CARTESIAN_POINT('Ctrl Pts',(-31.8998665590296,9.54085525566165,-64.1146813512576));
#45121=CARTESIAN_POINT('Ctrl Pts',(-31.9076150710329,9.611406861697,-64.3108408424311));
#45122=CARTESIAN_POINT('Ctrl Pts',(-31.9118818780292,9.65233176333279,-64.4224604598438));
#45123=CARTESIAN_POINT('Ctrl Pts',(-31.9181213851423,9.7143368276467,-64.5894108045165));
#45124=CARTESIAN_POINT('Ctrl Pts',(-31.9229860229439,9.76731811762333,-64.7275449754731));
#45125=CARTESIAN_POINT('Ctrl Pts',(-31.9306003920534,9.85682715760974,-64.9547647015626));
#45126=CARTESIAN_POINT('Ctrl Pts',(-31.9375255667317,9.94891926487566,-65.1800840300211));
#45127=CARTESIAN_POINT('Ctrl Pts',(-31.9478464044456,10.1491387361118,-65.6392670359826));
#45128=CARTESIAN_POINT('Ctrl Pts',(-31.9578012633066,10.532255897598,-66.4475219583118));
#45129=CARTESIAN_POINT('Ctrl Pts',(-31.9541438804769,11.4152325015982,-68.1022353353483));
#45130=CARTESIAN_POINT('Ctrl Pts',(-31.9354552882024,12.2921436404521,-69.5953401290514));
#45131=CARTESIAN_POINT('Ctrl Pts',(-31.9359968812566,12.9175177203876,-70.7840181532909));
#45132=CARTESIAN_POINT('Ctrl Pts',(-31.9361668766121,13.0467763077856,-71.0294219679257));
#45133=CARTESIAN_POINT('Ctrl Pts',(-31.9363879221274,13.3118785132307,-71.5314973325199));
#45134=CARTESIAN_POINT('Ctrl Pts',(-31.9365470443432,13.6420033726205,-72.1546266983309));
#45135=CARTESIAN_POINT('Ctrl Pts',(-31.9365676954674,14.0409873041072,-72.9052454390513));
#45136=CARTESIAN_POINT('Ctrl Pts',(-31.9363854854439,14.8405233797907,-74.4058924595146));
#45137=CARTESIAN_POINT('Ctrl Pts',(-31.9359498821979,15.5105306107026,-75.6591137597579));
#45138=CARTESIAN_POINT('Ctrl Pts',(-31.9359321500433,16.4823855390668,-77.4868224586133));
#45139=CARTESIAN_POINT('Ctrl Pts',(-31.9359354932352,16.9181033333288,-78.3062452673089));
#45140=CARTESIAN_POINT('Ctrl Pts',(-31.9359354932352,17.3546249207183,-79.1272229694073));
#45141=CARTESIAN_POINT('Ctrl Pts',(-30.0675473741683,4.07402549386851,24.830628633993));
#45142=CARTESIAN_POINT('Ctrl Pts',(-30.0676366759476,4.07402543500512,24.7817491347503));
#45143=CARTESIAN_POINT('Ctrl Pts',(-30.067730334401,4.07402537490366,24.7328706888072));
#45144=CARTESIAN_POINT('Ctrl Pts',(-30.0688363277657,4.07402460311166,24.1822603333702));
#45145=CARTESIAN_POINT('Ctrl Pts',(-30.069681950142,4.07402006626856,23.1781204513434));
#45146=CARTESIAN_POINT('Ctrl Pts',(-30.0716489051951,4.07400793801025,21.1695184120988));
#45147=CARTESIAN_POINT('Ctrl Pts',(-30.0790094820679,4.07400246356816,19.6653665885618));
#45148=CARTESIAN_POINT('Ctrl Pts',(-30.0946304835923,4.0740102214446,18.4143194714129));
#45149=CARTESIAN_POINT('Ctrl Pts',(-30.1021211614365,4.07401293360225,17.9114920744124));
#45150=CARTESIAN_POINT('Ctrl Pts',(-30.1209291982291,4.07401803581239,16.9074937602044));
#45151=CARTESIAN_POINT('Ctrl Pts',(-30.1612714480777,4.074030090798,15.1536795468699));
#45152=CARTESIAN_POINT('Ctrl Pts',(-30.1996133066813,4.07405994681501,13.651966132142));
#45153=CARTESIAN_POINT('Ctrl Pts',(-30.2236762095638,4.07411155133605,12.3975373877242));
#45154=CARTESIAN_POINT('Ctrl Pts',(-30.2335165820057,4.07413652326603,11.8966014769226));
#45155=CARTESIAN_POINT('Ctrl Pts',(-30.2535882688967,4.07419984851666,10.8947841219751));
#45156=CARTESIAN_POINT('Ctrl Pts',(-30.2784183179358,4.07429593923365,9.64227346611599));
#45157=CARTESIAN_POINT('Ctrl Pts',(-30.3046226897621,4.0744145370772,8.13777604509942));
#45158=CARTESIAN_POINT('Ctrl Pts',(-30.3175799472559,4.07447773461984,7.13305118041901));
#45159=CARTESIAN_POINT('Ctrl Pts',(-30.3235995672069,4.07450799535757,6.50506041678156));
#45160=CARTESIAN_POINT('Ctrl Pts',(-30.3258729588873,4.07452529032412,6.25491067506208));
#45161=CARTESIAN_POINT('Ctrl Pts',(-30.3299307987399,4.07457685129505,5.75387614073744));
#45162=CARTESIAN_POINT('Ctrl Pts',(-30.3357596574654,4.07469880379446,4.87557589426331));
#45163=CARTESIAN_POINT('Ctrl Pts',(-30.3424189826996,4.07499137876109,3.11525589207107));
#45164=CARTESIAN_POINT('Ctrl Pts',(-30.3398667713788,4.07500554796219,1.60812326185725));
#45165=CARTESIAN_POINT('Ctrl Pts',(-30.3344478538389,4.07463707762726,0.548138186438529));
#45166=CARTESIAN_POINT('Ctrl Pts',(-30.3337393879005,4.07458997060624,0.421871593996724));
#45167=CARTESIAN_POINT('Ctrl Pts',(-30.332083641622,4.07447996188512,0.169564940125542));
#45168=CARTESIAN_POINT('Ctrl Pts',(-30.3285930551385,4.07425009251407,-0.271453082833765));
#45169=CARTESIAN_POINT('Ctrl Pts',(-30.3221036411615,4.0738244063566,-0.900113259040177));
#45170=CARTESIAN_POINT('Ctrl Pts',(-30.3125287108398,4.0732171318043,-1.65278904064886));
#45171=CARTESIAN_POINT('Ctrl Pts',(-30.2981953567222,4.07232465713225,-2.65468422165601));
#45172=CARTESIAN_POINT('Ctrl Pts',(-30.2788828023857,4.07118793598993,-3.90508783659838));
#45173=CARTESIAN_POINT('Ctrl Pts',(-30.2652180597821,4.07048380211638,-4.90578336174276));
#45174=CARTESIAN_POINT('Ctrl Pts',(-30.2582638943793,4.07019480836563,-5.5321987470797));
#45175=CARTESIAN_POINT('Ctrl Pts',(-30.2554674208861,4.07006342905616,-5.78335271280684));
#45176=CARTESIAN_POINT('Ctrl Pts',(-30.2498451412354,4.06974933691546,-6.28562567869495));
#45177=CARTESIAN_POINT('Ctrl Pts',(-30.2399996373138,4.0691059874119,-7.16506706819149));
#45178=CARTESIAN_POINT('Ctrl Pts',(-30.2263213749604,4.0681550594497,-8.42127536722444));
#45179=CARTESIAN_POINT('Ctrl Pts',(-30.2142344838837,4.06779375757901,-9.6746658182018));
#45180=CARTESIAN_POINT('Ctrl Pts',(-30.2071749736404,4.06818177662064,-10.5490624344194));
#45181=CARTESIAN_POINT('Ctrl Pts',(-30.2036219784775,4.0686333078625,-11.047660424527));
#45182=CARTESIAN_POINT('Ctrl Pts',(-30.2020193523223,4.06894315636935,-11.2965754227479));
#45183=CARTESIAN_POINT('Ctrl Pts',(-30.2008828480245,4.06921141590645,-11.4838718769006));
#45184=CARTESIAN_POINT('Ctrl Pts',(-30.2001418485536,4.06942052903896,-11.6092503899531));
#45185=CARTESIAN_POINT('Ctrl Pts',(-30.1987489579567,4.06994714066987,-11.8600866123641));
#45186=CARTESIAN_POINT('Ctrl Pts',(-30.1965370296849,4.07113030733344,-12.2984702198424));
#45187=CARTESIAN_POINT('Ctrl Pts',(-30.1929519161861,4.07435959782404,-13.1739479246322));
#45188=CARTESIAN_POINT('Ctrl Pts',(-30.1898527505392,4.08044633503893,-14.4229139491848));
#45189=CARTESIAN_POINT('Ctrl Pts',(-30.1886103060245,4.08523009014515,-15.5503981026885));
#45190=CARTESIAN_POINT('Ctrl Pts',(-30.1880553727537,4.08710042461392,-16.3056759814081));
#45191=CARTESIAN_POINT('Ctrl Pts',(-30.1877324707432,4.0879276757656,-16.8102984030727));
#45192=CARTESIAN_POINT('Ctrl Pts',(-30.1875161787576,4.08798924987499,-17.1902005082812));
#45193=CARTESIAN_POINT('Ctrl Pts',(-30.1873176376361,4.087649726645,-17.5068895628413));
#45194=CARTESIAN_POINT('Ctrl Pts',(-30.1872864991048,4.08753026540084,-17.6309577100965));
#45195=CARTESIAN_POINT('Ctrl Pts',(-30.1873954803442,4.08732989101367,-17.8801050928944));
#45196=CARTESIAN_POINT('Ctrl Pts',(-30.1877395017226,4.08717171477966,-18.1292535832108));
#45197=CARTESIAN_POINT('Ctrl Pts',(-30.188272206513,4.08702454294921,-18.3788607310938));
#45198=CARTESIAN_POINT('Ctrl Pts',(-30.1886744597833,4.08692973609548,-18.5349573794094));
#45199=CARTESIAN_POINT('Ctrl Pts',(-30.1890320505783,4.08684843166254,-18.6599241566505));
#45200=CARTESIAN_POINT('Ctrl Pts',(-30.1893167576907,4.08678357731685,-18.7536843811132));
#45201=CARTESIAN_POINT('Ctrl Pts',(-30.1895665721995,4.08672547288396,-18.8318516893039));
#45202=CARTESIAN_POINT('Ctrl Pts',(-30.1897732558483,4.08667606963648,-18.8944041645065));
#45203=CARTESIAN_POINT('Ctrl Pts',(-30.1915663197643,4.08623841124574,-19.4262122114691));
#45204=CARTESIAN_POINT('Ctrl Pts',(-30.1961051285031,4.084756062735,-20.4465526066575));
#45205=CARTESIAN_POINT('Ctrl Pts',(-30.2000726864718,4.0767318936048,-21.9637745112584));
#45206=CARTESIAN_POINT('Ctrl Pts',(-30.1970612147022,4.06469762621023,-22.9826839794627));
#45207=CARTESIAN_POINT('Ctrl Pts',(-30.1922398076992,4.05430688545523,-23.6202436765408));
#45208=CARTESIAN_POINT('Ctrl Pts',(-30.1900841185594,4.04954170941843,-23.8762747110122));
#45209=CARTESIAN_POINT('Ctrl Pts',(-30.1849026782126,4.038054721385,-24.3851642562897));
#45210=CARTESIAN_POINT('Ctrl Pts',(-30.1737620723978,4.01359240397717,-25.2744023890998));
#45211=CARTESIAN_POINT('Ctrl Pts',(-30.153374942618,3.97123564483179,-26.5359941979714));
#45212=CARTESIAN_POINT('Ctrl Pts',(-30.125265030707,3.92399396408896,-28.0332589680397));
#45213=CARTESIAN_POINT('Ctrl Pts',(-30.1064831648513,3.90367821899851,-29.017034788648));
#45214=CARTESIAN_POINT('Ctrl Pts',(-30.0966406455218,3.89767197354323,-29.5657610185313));
#45215=CARTESIAN_POINT('Ctrl Pts',(-30.0944609291319,3.89633147642119,-29.6910552886119));
#45216=CARTESIAN_POINT('Ctrl Pts',(-30.0900751736587,3.89382702416348,-29.9397090057612));
#45217=CARTESIAN_POINT('Ctrl Pts',(-30.0823646844887,3.88984108615631,-30.3757454776289));
#45218=CARTESIAN_POINT('Ctrl Pts',(-30.0667267592323,3.8836768128489,-31.2466347196678));
#45219=CARTESIAN_POINT('Ctrl Pts',(-30.0437366592632,3.88081109793407,-32.4893336913118));
#45220=CARTESIAN_POINT('Ctrl Pts',(-30.0195566094771,3.88798774614015,-33.7272588745916));
#45221=CARTESIAN_POINT('Ctrl Pts',(-29.99929937702,3.90098056847106,-34.713666847604));
#45222=CARTESIAN_POINT('Ctrl Pts',(-29.9889033231973,3.91007156124506,-35.205463866196));
#45223=CARTESIAN_POINT('Ctrl Pts',(-29.9809496953176,3.91795641437902,-35.5746304575847));
#45224=CARTESIAN_POINT('Ctrl Pts',(-29.9757247956522,3.92359657690754,-35.8222355664664));
#45225=CARTESIAN_POINT('Ctrl Pts',(-29.9655909133275,3.93621230622192,-36.3168732239133));
#45226=CARTESIAN_POINT('Ctrl Pts',(-29.9485042705045,3.96170418644016,-37.1822130401085));
#45227=CARTESIAN_POINT('Ctrl Pts',(-29.9148282975304,4.02477077950527,-38.9112115550624));
#45228=CARTESIAN_POINT('Ctrl Pts',(-29.8803151829792,4.09588590235412,-40.3991715419146));
#45229=CARTESIAN_POINT('Ctrl Pts',(-29.8409368948539,4.16016983935756,-41.645949356613));
#45230=CARTESIAN_POINT('Ctrl Pts',(-29.8287653164624,4.17737158193141,-42.0423769521704));
#45231=CARTESIAN_POINT('Ctrl Pts',(-29.812285671004,4.19545129807948,-42.550403082089));
#45232=CARTESIAN_POINT('Ctrl Pts',(-29.7954272548127,4.21204061790188,-43.0568282251492));
#45233=CARTESIAN_POINT('Ctrl Pts',(-29.7736265859651,4.23139475890916,-43.679106759112));
#45234=CARTESIAN_POINT('Ctrl Pts',(-29.7459868576208,4.25826632456728,-44.4114653271861));
#45235=CARTESIAN_POINT('Ctrl Pts',(-29.7216040642617,4.28808117317888,-45.0085382005776));
#45236=CARTESIAN_POINT('Ctrl Pts',(-29.7013125022927,4.31888083235695,-45.4784239432683));
#45237=CARTESIAN_POINT('Ctrl Pts',(-29.6856987012504,4.34606221934751,-45.8268876643508));
#45238=CARTESIAN_POINT('Ctrl Pts',(-29.6697101706248,4.37791652624086,-46.1714516272928));
#45239=CARTESIAN_POINT('Ctrl Pts',(-29.6479468882477,4.42737618133044,-46.6256554120005));
#45240=CARTESIAN_POINT('Ctrl Pts',(-29.6311296267172,4.4732106611538,-46.9605697088143));
#45241=CARTESIAN_POINT('Ctrl Pts',(-29.6140874606994,4.52607833559169,-47.2924570705504));
#45242=CARTESIAN_POINT('Ctrl Pts',(-29.601454255548,4.56334903637515,-47.5109312911585));
#45243=CARTESIAN_POINT('Ctrl Pts',(-29.5715572021337,4.64912737284354,-47.9589282930229));
#45244=CARTESIAN_POINT('Ctrl Pts',(-29.5095826736441,4.82546368650228,-48.7609818353961));
#45245=CARTESIAN_POINT('Ctrl Pts',(-29.4060280130564,5.14309673276399,-49.9598599459976));
#45246=CARTESIAN_POINT('Ctrl Pts',(-29.2939203496264,5.5865688094809,-51.4683674505085));
#45247=CARTESIAN_POINT('Ctrl Pts',(-29.2506392080023,5.89078625919428,-52.5164596458079));
#45248=CARTESIAN_POINT('Ctrl Pts',(-29.2424084661624,6.07296061824513,-53.1860502356983));
#45249=CARTESIAN_POINT('Ctrl Pts',(-29.2423888404739,6.14330686674367,-53.4427131291745));
#45250=CARTESIAN_POINT('Ctrl Pts',(-29.2484601891129,6.28494795741891,-53.9603595226558));
#45251=CARTESIAN_POINT('Ctrl Pts',(-29.2762156007057,6.53032030038241,-54.8545936563589));
#45252=CARTESIAN_POINT('Ctrl Pts',(-29.386306161652,7.01946605134849,-56.6135247633875));
#45253=CARTESIAN_POINT('Ctrl Pts',(-29.5327218189415,7.43982329257562,-58.0587381433518));
#45254=CARTESIAN_POINT('Ctrl Pts',(-29.6071951435415,7.75666376505009,-59.0529229961379));
#45255=CARTESIAN_POINT('Ctrl Pts',(-29.6158112741558,7.79760401764963,-59.1815399771206));
#45256=CARTESIAN_POINT('Ctrl Pts',(-29.6340659881628,7.87795458167348,-59.433655151946));
#45257=CARTESIAN_POINT('Ctrl Pts',(-29.6674699345856,8.01899017550212,-59.8754139377655));
#45258=CARTESIAN_POINT('Ctrl Pts',(-29.7397624843917,8.30013581198258,-60.7500981697734));
#45259=CARTESIAN_POINT('Ctrl Pts',(-29.8288267579884,8.62401116474369,-61.7328369750638));
#45260=CARTESIAN_POINT('Ctrl Pts',(-29.9122990683941,8.9582165401791,-62.6941998000547));
#45261=CARTESIAN_POINT('Ctrl Pts',(-29.9548376484439,9.15202992907867,-63.2266334707154));
#45262=CARTESIAN_POINT('Ctrl Pts',(-29.9804497778331,9.28441793274911,-63.5777856666572));
#45263=CARTESIAN_POINT('Ctrl Pts',(-29.9967341462232,9.37358979794334,-63.8108739102784));
#45264=CARTESIAN_POINT('Ctrl Pts',(-30.0117427869623,9.46418362784269,-64.0423652390109));
#45265=CARTESIAN_POINT('Ctrl Pts',(-30.0236146379465,9.54486559698578,-64.2435224642254));
#45266=CARTESIAN_POINT('Ctrl Pts',(-30.0300177327675,9.5913903607628,-64.3580586040495));
#45267=CARTESIAN_POINT('Ctrl Pts',(-30.0392317902084,9.6616067090032,-64.5294440809629));
#45268=CARTESIAN_POINT('Ctrl Pts',(-30.0460738261263,9.72103464484501,-64.6713910113177));
#45269=CARTESIAN_POINT('Ctrl Pts',(-30.056193231707,9.82070532959067,-64.9051026213648));
#45270=CARTESIAN_POINT('Ctrl Pts',(-30.0654035719528,9.92328050974094,-65.1394534429073));
#45271=CARTESIAN_POINT('Ctrl Pts',(-30.0792738868105,10.1403139254679,-65.6129717102997));
#45272=CARTESIAN_POINT('Ctrl Pts',(-30.0930380186134,10.5441203219372,-66.4419902424388));
#45273=CARTESIAN_POINT('Ctrl Pts',(-30.0897570522684,11.4372879264921,-68.1188888326908));
#45274=CARTESIAN_POINT('Ctrl Pts',(-30.0662549327026,12.2908443686912,-69.6081388008406));
#45275=CARTESIAN_POINT('Ctrl Pts',(-30.0677206779153,12.9093005226094,-70.781419220543));
#45276=CARTESIAN_POINT('Ctrl Pts',(-30.0680132094674,13.0394825228367,-71.0281447542001));
#45277=CARTESIAN_POINT('Ctrl Pts',(-30.068443337793,13.3048534320091,-71.5300820404047));
#45278=CARTESIAN_POINT('Ctrl Pts',(-30.0687264348823,13.6356514928772,-72.1540785489046));
#45279=CARTESIAN_POINT('Ctrl Pts',(-30.0687559042375,14.0348079013757,-72.9049827833199));
#45280=CARTESIAN_POINT('Ctrl Pts',(-30.0683798170397,14.8343904396941,-74.4062939876644));
#45281=CARTESIAN_POINT('Ctrl Pts',(-30.0675396968737,15.503662396096,-75.6594521589913));
#45282=CARTESIAN_POINT('Ctrl Pts',(-30.0675325757361,16.475143996278,-77.4865030812836));
#45283=CARTESIAN_POINT('Ctrl Pts',(-30.0675297169312,16.9110122292074,-78.3062315870108));
#45284=CARTESIAN_POINT('Ctrl Pts',(-30.0675297169313,17.3475338165968,-79.1272092891091));
#45285=CARTESIAN_POINT('Ctrl Pts',(-28.5063700143004,4.0751307694223,24.8306290855513));
#45286=CARTESIAN_POINT('Ctrl Pts',(-28.5064550410518,4.0751305156724,24.7817495992412));
#45287=CARTESIAN_POINT('Ctrl Pts',(-28.5065442166203,4.07513025010105,24.7328711645537));
#45288=CARTESIAN_POINT('Ctrl Pts',(-28.5075972303578,4.07512709922709,24.1822610181398));
#45289=CARTESIAN_POINT('Ctrl Pts',(-28.5084048846699,4.07512163837621,23.1781227303733));
#45290=CARTESIAN_POINT('Ctrl Pts',(-28.5102858747354,4.0751071477093,21.1695205266819));
#45291=CARTESIAN_POINT('Ctrl Pts',(-28.5172933353407,4.0750862730656,19.6653675836014));
#45292=CARTESIAN_POINT('Ctrl Pts',(-28.5321520913383,4.07505702437731,18.4143191318779));
#45293=CARTESIAN_POINT('Ctrl Pts',(-28.5392785618885,4.07504184758454,17.9114918157889));
#45294=CARTESIAN_POINT('Ctrl Pts',(-28.5571741550791,4.07500190159066,16.9074943019247));
#45295=CARTESIAN_POINT('Ctrl Pts',(-28.5955586169002,4.07491678343083,15.1536833936334));
#45296=CARTESIAN_POINT('Ctrl Pts',(-28.6320203529255,4.07485449752761,13.6519735110304));
#45297=CARTESIAN_POINT('Ctrl Pts',(-28.6548705454507,4.07484721171388,12.3975437498382));
#45298=CARTESIAN_POINT('Ctrl Pts',(-28.6642113546693,4.07484787230247,11.896607515957));
#45299=CARTESIAN_POINT('Ctrl Pts',(-28.6832524227466,4.07486075549552,10.8947894472725));
#45300=CARTESIAN_POINT('Ctrl Pts',(-28.706789245084,4.07489478299759,9.64227929161552));
#45301=CARTESIAN_POINT('Ctrl Pts',(-28.7316119959556,4.07494686114839,8.13778312608962));
#45302=CARTESIAN_POINT('Ctrl Pts',(-28.7438779121553,4.07497928221181,7.13306000887749));
#45303=CARTESIAN_POINT('Ctrl Pts',(-28.7495750949822,4.07499518723171,6.5050732982054));
#45304=CARTESIAN_POINT('Ctrl Pts',(-28.7517254796684,4.07501222499112,6.25499083013756));
#45305=CARTESIAN_POINT('Ctrl Pts',(-28.7555591252596,4.07508135353952,5.75402907367263));
#45306=CARTESIAN_POINT('Ctrl Pts',(-28.7610532102808,4.07527284770306,4.8758210208063));
#45307=CARTESIAN_POINT('Ctrl Pts',(-28.7672864360839,4.07577030561028,3.11544649156435));
#45308=CARTESIAN_POINT('Ctrl Pts',(-28.7648084158001,4.0758076728453,1.60790548044939));
#45309=CARTESIAN_POINT('Ctrl Pts',(-28.759685738567,4.07510385438478,0.547427834192141));
#45310=CARTESIAN_POINT('Ctrl Pts',(-28.7590167480848,4.07501238119254,0.421072873216588));
#45311=CARTESIAN_POINT('Ctrl Pts',(-28.7574541748833,4.07480022248746,0.168617210843751));
#45312=CARTESIAN_POINT('Ctrl Pts',(-28.7541625555416,4.0743573888518,-0.27264522366889));
#45313=CARTESIAN_POINT('Ctrl Pts',(-28.7480452405828,4.0735475875382,-0.901576117862987));
#45314=CARTESIAN_POINT('Ctrl Pts',(-28.7390252374076,4.07238446689408,-1.65445988487398));
#45315=CARTESIAN_POINT('Ctrl Pts',(-28.7255170393529,4.07069572979033,-2.65646957341181));
#45316=CARTESIAN_POINT('Ctrl Pts',(-28.7073114843065,4.0685533590852,-3.90670358762708));
#45317=CARTESIAN_POINT('Ctrl Pts',(-28.6943975210421,4.06728409919296,-4.90692352017473));
#45318=CARTESIAN_POINT('Ctrl Pts',(-28.6878098793571,4.06678114894455,-5.5329357353639));
#45319=CARTESIAN_POINT('Ctrl Pts',(-28.6851829138752,4.06657269379081,-5.7840063726452));
#45320=CARTESIAN_POINT('Ctrl Pts',(-28.6799716070688,4.06614085446737,-6.28609299293432));
#45321=CARTESIAN_POINT('Ctrl Pts',(-28.6709850712771,4.06537575387857,-7.16528470639284));
#45322=CARTESIAN_POINT('Ctrl Pts',(-28.6586549502862,4.06443450811702,-8.42127718018226));
#45323=CARTESIAN_POINT('Ctrl Pts',(-28.6473426314964,4.06416607144442,-9.6746534608699));
#45324=CARTESIAN_POINT('Ctrl Pts',(-28.6401376477395,4.06457818071917,-10.5491379927501));
#45325=CARTESIAN_POINT('Ctrl Pts',(-28.6362491756948,4.06502038333421,-11.0478169769201));
#45326=CARTESIAN_POINT('Ctrl Pts',(-28.6343852406347,4.06531621003876,-11.2967818689912));
#45327=CARTESIAN_POINT('Ctrl Pts',(-28.6330134062058,4.06556938824069,-11.4841215256739));
#45328=CARTESIAN_POINT('Ctrl Pts',(-28.6320889975595,4.06576455600266,-11.6095836028888));
#45329=CARTESIAN_POINT('Ctrl Pts',(-28.6302349510895,4.06625052056912,-11.860540528078));
#45330=CARTESIAN_POINT('Ctrl Pts',(-28.626986601601,4.06733209686087,-12.2991155322276));
#45331=CARTESIAN_POINT('Ctrl Pts',(-28.620553195512,4.0702680235487,-13.1748182689849));
#45332=CARTESIAN_POINT('Ctrl Pts',(-28.6120116468468,4.07581010149929,-14.4236955364312));
#45333=CARTESIAN_POINT('Ctrl Pts',(-28.6062014687261,4.08032597813081,-15.5505911344308));
#45334=CARTESIAN_POINT('Ctrl Pts',(-28.6035717107567,4.08226334584899,-16.3052735984145));
#45335=CARTESIAN_POINT('Ctrl Pts',(-28.6021821982076,4.08321002851602,-16.809445977369));
#45336=CARTESIAN_POINT('Ctrl Pts',(-28.6015792694236,4.08346631588465,-17.1889521925233));
#45337=CARTESIAN_POINT('Ctrl Pts',(-28.6013643203449,4.08335371643104,-17.5052794437319));
#45338=CARTESIAN_POINT('Ctrl Pts',(-28.6012901999452,4.08333057890033,-17.6291360036696));
#45339=CARTESIAN_POINT('Ctrl Pts',(-28.601189881543,4.08335630502948,-17.8779284626584));
#45340=CARTESIAN_POINT('Ctrl Pts',(-28.6011630597932,4.08347247635335,-18.1267423503286));
#45341=CARTESIAN_POINT('Ctrl Pts',(-28.6012200531399,4.08363962845014,-18.3760617391668));
#45342=CARTESIAN_POINT('Ctrl Pts',(-28.6012912010045,4.08375797076782,-18.5319920711977));
#45343=CARTESIAN_POINT('Ctrl Pts',(-28.601370882673,4.08385588435406,-18.6568361478655));
#45344=CARTESIAN_POINT('Ctrl Pts',(-28.6014420633411,4.08392986485814,-18.7505088520711));
#45345=CARTESIAN_POINT('Ctrl Pts',(-28.6015110779462,4.08399098076577,-18.8286071854719));
#45346=CARTESIAN_POINT('Ctrl Pts',(-28.6015723337452,4.08403888408376,-18.8911068965197));
#45347=CARTESIAN_POINT('Ctrl Pts',(-28.6021268874594,4.08443912596546,-19.4224795120135));
#45348=CARTESIAN_POINT('Ctrl Pts',(-28.6042230114293,4.08496632011906,-20.4423636620365));
#45349=CARTESIAN_POINT('Ctrl Pts',(-28.6114274699414,4.07995838922308,-21.9601597456664));
#45350=CARTESIAN_POINT('Ctrl Pts',(-28.619503512616,4.06945508613115,-22.9801762124166));
#45351=CARTESIAN_POINT('Ctrl Pts',(-28.6257698020092,4.05959453037469,-23.6185528436904));
#45352=CARTESIAN_POINT('Ctrl Pts',(-28.6285572713742,4.05511040085929,-23.8738673293465));
#45353=CARTESIAN_POINT('Ctrl Pts',(-28.6351809674563,4.04428158215644,-24.3821280903121));
#45354=CARTESIAN_POINT('Ctrl Pts',(-28.6491269721366,4.02108099402648,-25.2704435909963));
#45355=CARTESIAN_POINT('Ctrl Pts',(-28.6732965824566,3.97993891514751,-26.5323065338286));
#45356=CARTESIAN_POINT('Ctrl Pts',(-28.7018521611686,3.93045200794019,-28.032558331282));
#45357=CARTESIAN_POINT('Ctrl Pts',(-28.7155747876185,3.90598509535247,-29.0207512993479));
#45358=CARTESIAN_POINT('Ctrl Pts',(-28.7204154682032,3.89695414396225,-29.5726464466516));
#45359=CARTESIAN_POINT('Ctrl Pts',(-28.7214583076406,3.89493494175957,-29.6979807591885));
#45360=CARTESIAN_POINT('Ctrl Pts',(-28.7234270387298,3.89104592353962,-29.9471303392517));
#45361=CARTESIAN_POINT('Ctrl Pts',(-28.7265480220933,3.88457570068822,-30.3839372380476));
#45362=CARTESIAN_POINT('Ctrl Pts',(-28.7315487045443,3.87312760492994,-31.2568834820553));
#45363=CARTESIAN_POINT('Ctrl Pts',(-28.7351751217934,3.86160851200574,-32.5034492176154));
#45364=CARTESIAN_POINT('Ctrl Pts',(-28.7343820386309,3.85810067807707,-33.7465790637076));
#45365=CARTESIAN_POINT('Ctrl Pts',(-28.7312693881602,3.86096952008346,-34.7378806771447));
#45366=CARTESIAN_POINT('Ctrl Pts',(-28.7288549713757,3.86444576642746,-35.232363519754));
#45367=CARTESIAN_POINT('Ctrl Pts',(-28.7267473971563,3.86787391775565,-35.6036315420276));
#45368=CARTESIAN_POINT('Ctrl Pts',(-28.7253477432298,3.87043906327854,-35.8524203389833));
#45369=CARTESIAN_POINT('Ctrl Pts',(-28.7225122816699,3.87659960051719,-36.349454367607));
#45370=CARTESIAN_POINT('Ctrl Pts',(-28.7171595060761,3.88996398124818,-37.2187366227478));
#45371=CARTESIAN_POINT('Ctrl Pts',(-28.7029719475229,3.92628709148851,-38.9548294958871));
#45372=CARTESIAN_POINT('Ctrl Pts',(-28.6779204357281,3.97080216786415,-40.4478543681075));
#45373=CARTESIAN_POINT('Ctrl Pts',(-28.6423881509124,4.01235594105461,-41.6981476026289));
#45374=CARTESIAN_POINT('Ctrl Pts',(-28.6315352422751,4.02217894774256,-42.0944833673719));
#45375=CARTESIAN_POINT('Ctrl Pts',(-28.6162226999484,4.03096771433208,-42.6034857846265));
#45376=CARTESIAN_POINT('Ctrl Pts',(-28.6002399953221,4.03821538774407,-43.1110327947022));
#45377=CARTESIAN_POINT('Ctrl Pts',(-28.5787798709528,4.04592744712491,-43.7353041116043));
#45378=CARTESIAN_POINT('Ctrl Pts',(-28.5499946061509,4.05846176348219,-44.4707212417988));
#45379=CARTESIAN_POINT('Ctrl Pts',(-28.5229565217032,4.07575591946211,-45.0708121467108));
#45380=CARTESIAN_POINT('Ctrl Pts',(-28.499168294948,4.09601759532599,-45.5431560064207));
#45381=CARTESIAN_POINT('Ctrl Pts',(-28.4802145464749,4.11495795764875,-45.8935119207955));
#45382=CARTESIAN_POINT('Ctrl Pts',(-28.460093112664,4.13816692206255,-46.2399527998875));
#45383=CARTESIAN_POINT('Ctrl Pts',(-28.4316329521809,4.17547161434323,-46.6966010435509));
#45384=CARTESIAN_POINT('Ctrl Pts',(-28.4084746211153,4.21132347192227,-47.0332160567307));
#45385=CARTESIAN_POINT('Ctrl Pts',(-28.3839470210442,4.25348435717159,-47.3668895389636));
#45386=CARTESIAN_POINT('Ctrl Pts',(-28.3656221545791,4.28446593068285,-47.5965828274277));
#45387=CARTESIAN_POINT('Ctrl Pts',(-28.3233891553743,4.35294575955154,-48.0565547357988));
#45388=CARTESIAN_POINT('Ctrl Pts',(-28.2373456970307,4.49024962874069,-48.8723990065144));
#45389=CARTESIAN_POINT('Ctrl Pts',(-28.0963832536994,4.72878871184675,-50.0638539523906));
#45390=CARTESIAN_POINT('Ctrl Pts',(-27.945559766733,5.06821689546968,-51.5342689199645));
#45391=CARTESIAN_POINT('Ctrl Pts',(-27.8839986235443,5.32293710473205,-52.5363887393521));
#45392=CARTESIAN_POINT('Ctrl Pts',(-27.8657892882708,5.48881051509036,-53.1689845861308));
#45393=CARTESIAN_POINT('Ctrl Pts',(-27.8608639796447,5.55444069071902,-53.414115153262));
#45394=CARTESIAN_POINT('Ctrl Pts',(-27.8561704081986,5.69137441975848,-53.9096594814404));
#45395=CARTESIAN_POINT('Ctrl Pts',(-27.8618563300706,5.94089897593999,-54.7725158528541));
#45396=CARTESIAN_POINT('Ctrl Pts',(-27.9177646884999,6.47867009676407,-56.49260068047));
#45397=CARTESIAN_POINT('Ctrl Pts',(-28.0108984258091,6.98600845197756,-57.9460750333808));
#45398=CARTESIAN_POINT('Ctrl Pts',(-28.0643986211443,7.3589749222962,-58.9632438768764));
#45399=CARTESIAN_POINT('Ctrl Pts',(-28.0710994995596,7.40486849700483,-59.087683827155));
#45400=CARTESIAN_POINT('Ctrl Pts',(-28.0855759991836,7.49712864453928,-59.3358262755601));
#45401=CARTESIAN_POINT('Ctrl Pts',(-28.113424438541,7.66043095015801,-59.7697091382071));
#45402=CARTESIAN_POINT('Ctrl Pts',(-28.1777711656,7.99344520754302,-60.6345834620239));
#45403=CARTESIAN_POINT('Ctrl Pts',(-28.263998444937,8.38646109980859,-61.6159036784955));
#45404=CARTESIAN_POINT('Ctrl Pts',(-28.3476765614693,8.78976844974455,-62.5875275250034));
#45405=CARTESIAN_POINT('Ctrl Pts',(-28.3908407896533,9.02066613610083,-63.1297655617631));
#45406=CARTESIAN_POINT('Ctrl Pts',(-28.4168182778754,9.17636660806815,-63.4891354787894));
#45407=CARTESIAN_POINT('Ctrl Pts',(-28.4333132625767,9.28066163268648,-63.7281312770182));
#45408=CARTESIAN_POINT('Ctrl Pts',(-28.4484611031149,9.38568378540385,-63.9661714729316));
#45409=CARTESIAN_POINT('Ctrl Pts',(-28.460340289617,9.47827546540508,-64.1735973287607));
#45410=CARTESIAN_POINT('Ctrl Pts',(-28.4667085162954,9.53138580096016,-64.2918666428035));
#45411=CARTESIAN_POINT('Ctrl Pts',(-28.4758274218159,9.61125209852722,-64.4689996591551));
#45412=CARTESIAN_POINT('Ctrl Pts',(-28.4824955134669,9.67823324425495,-64.6160482596983));
#45413=CARTESIAN_POINT('Ctrl Pts',(-28.4921574987008,9.78965958501148,-64.8585661182835));
#45414=CARTESIAN_POINT('Ctrl Pts',(-28.5009939422513,9.90260723979942,-65.1003323094549));
#45415=CARTESIAN_POINT('Ctrl Pts',(-28.5144236103671,10.1370570244854,-65.5875989379661));
#45416=CARTESIAN_POINT('Ctrl Pts',(-28.5280998476002,10.5618541082785,-66.4359100148839));
#45417=CARTESIAN_POINT('Ctrl Pts',(-28.5261452105889,11.4659601810288,-68.1353068432759));
#45418=CARTESIAN_POINT('Ctrl Pts',(-28.5042603208831,12.2971910227302,-69.6204181568186));
#45419=CARTESIAN_POINT('Ctrl Pts',(-28.5059868748442,12.9092160196114,-70.7787578014154));
#45420=CARTESIAN_POINT('Ctrl Pts',(-28.5063176518591,13.0403881297786,-71.026833006938));
#45421=CARTESIAN_POINT('Ctrl Pts',(-28.506810343618,13.3061510584708,-71.5287248539541));
#45422=CARTESIAN_POINT('Ctrl Pts',(-28.5071342080593,13.6377122596,-72.1536545062716));
#45423=CARTESIAN_POINT('Ctrl Pts',(-28.5071681221449,14.0370893088904,-72.9049205376012));
#45424=CARTESIAN_POINT('Ctrl Pts',(-28.5067378086829,14.8367082476652,-74.4069878530215));
#45425=CARTESIAN_POINT('Ctrl Pts',(-28.505786105334,15.5050694448925,-75.6599826656687));
#45426=CARTESIAN_POINT('Ctrl Pts',(-28.5057865286928,16.4760794038801,-77.486169472289));
#45427=CARTESIAN_POINT('Ctrl Pts',(-28.5057850703907,16.9121202092292,-78.306234167581));
#45428=CARTESIAN_POINT('Ctrl Pts',(-28.5057850703907,17.3486417966187,-79.1272118696792));
#45429=CARTESIAN_POINT('Ctrl Pts',(-27.2546101003228,4.0774086805339,24.8306314676615));
#45430=CARTESIAN_POINT('Ctrl Pts',(-27.2546915815672,4.07740844455158,24.781752056975));
#45431=CARTESIAN_POINT('Ctrl Pts',(-27.2547770374123,4.07740819882894,24.7328736991936));
#45432=CARTESIAN_POINT('Ctrl Pts',(-27.2557861793606,4.07740522247428,24.1822644399479));
#45433=CARTESIAN_POINT('Ctrl Pts',(-27.256561323909,4.07740099708737,23.17812767054));
#45434=CARTESIAN_POINT('Ctrl Pts',(-27.2583664216711,4.07739113571785,21.1695268379285));
#45435=CARTESIAN_POINT('Ctrl Pts',(-27.2650824454299,4.07737074475774,19.665373131343));
#45436=CARTESIAN_POINT('Ctrl Pts',(-27.2793176058701,4.07733690464952,18.4143239105435));
#45437=CARTESIAN_POINT('Ctrl Pts',(-27.2861452978621,4.07732008576429,17.911500928659));
#45438=CARTESIAN_POINT('Ctrl Pts',(-27.3032914192145,4.07727658330968,16.9075066894004));
#45439=CARTESIAN_POINT('Ctrl Pts',(-27.3400678380425,4.07718367084803,15.1536967473203));
#45440=CARTESIAN_POINT('Ctrl Pts',(-27.3749973994861,4.07710478697132,13.6519734005915));
#45441=CARTESIAN_POINT('Ctrl Pts',(-27.3968760234158,4.07707457179911,12.3975242999686));
#45442=CARTESIAN_POINT('Ctrl Pts',(-27.4058182811068,4.07706441082617,11.8965802318231));
#45443=CARTESIAN_POINT('Ctrl Pts',(-27.424042248115,4.07705098316843,10.894750841519));
#45444=CARTESIAN_POINT('Ctrl Pts',(-27.446564569103,4.07704337196664,9.64223235776427));
#45445=CARTESIAN_POINT('Ctrl Pts',(-27.470310851357,4.07704633646212,8.1377372100784));
#45446=CARTESIAN_POINT('Ctrl Pts',(-27.4820456322472,4.07704917215681,7.13302130766815));
#45447=CARTESIAN_POINT('Ctrl Pts',(-27.4874955577965,4.07705183733921,6.50504059377069));
#45448=CARTESIAN_POINT('Ctrl Pts',(-27.4895482840546,4.07706236045641,6.25493841669784));
#45449=CARTESIAN_POINT('Ctrl Pts',(-27.4931929702868,4.07711424196008,5.75395658505462));
#45450=CARTESIAN_POINT('Ctrl Pts',(-27.4983826152909,4.07726499461672,4.87572219825504));
#45451=CARTESIAN_POINT('Ctrl Pts',(-27.504164316388,4.0776733222571,3.11536628642292));
#45452=CARTESIAN_POINT('Ctrl Pts',(-27.5017982447368,4.07767661882587,1.6079464273222));
#45453=CARTESIAN_POINT('Ctrl Pts',(-27.4971755625774,4.07706353984626,0.547608728350889));
#45454=CARTESIAN_POINT('Ctrl Pts',(-27.4965710434973,4.07698495250432,0.421276638990806));
#45455=CARTESIAN_POINT('Ctrl Pts',(-27.4951593133511,4.07680194783564,0.168859992086856));
#45456=CARTESIAN_POINT('Ctrl Pts',(-27.4921842812917,4.07642036620931,-0.27233989131527));
#45457=CARTESIAN_POINT('Ctrl Pts',(-27.4866554523826,4.0757177072624,-0.901204689572938));
#45458=CARTESIAN_POINT('Ctrl Pts',(-27.4784840998671,4.07471961851841,-1.65404408891485));
#45459=CARTESIAN_POINT('Ctrl Pts',(-27.4662302513185,4.07326488974287,-2.65603895285884));
#45460=CARTESIAN_POINT('Ctrl Pts',(-27.4496442700658,4.0714363481666,-3.90633192945388));
#45461=CARTESIAN_POINT('Ctrl Pts',(-27.4377683739882,4.07035056189753,-4.90666001983112));
#45462=CARTESIAN_POINT('Ctrl Pts',(-27.4316383677891,4.06993201648509,-5.53275069722329));
#45463=CARTESIAN_POINT('Ctrl Pts',(-27.4291952297676,4.06976708145305,-5.78370899132702));
#45464=CARTESIAN_POINT('Ctrl Pts',(-27.4243521139342,4.06944661825676,-6.28569409154177));
#45465=CARTESIAN_POINT('Ctrl Pts',(-27.4160008254043,4.06892327742794,-7.16475965770132));
#45466=CARTESIAN_POINT('Ctrl Pts',(-27.4044868074976,4.06835875013137,-8.42087325927019));
#45467=CARTESIAN_POINT('Ctrl Pts',(-27.3936832198069,4.06824645545923,-9.67472110418459));
#45468=CARTESIAN_POINT('Ctrl Pts',(-27.3865749697245,4.06851597506718,-10.5497357044532));
#45469=CARTESIAN_POINT('Ctrl Pts',(-27.3826548941153,4.06878389138936,-11.0487735960245));
#45470=CARTESIAN_POINT('Ctrl Pts',(-27.3807442126837,4.06895811317885,-11.2979355567401));
#45471=CARTESIAN_POINT('Ctrl Pts',(-27.3793244097686,4.06910569315751,-11.4854355948755));
#45472=CARTESIAN_POINT('Ctrl Pts',(-27.3783585030531,4.06921942120932,-11.6111678989742));
#45473=CARTESIAN_POINT('Ctrl Pts',(-27.3763872065056,4.06950129246306,-11.8625350299554));
#45474=CARTESIAN_POINT('Ctrl Pts',(-27.3728503594407,4.07012625568385,-12.3017858467383));
#45475=CARTESIAN_POINT('Ctrl Pts',(-27.3655598205339,4.07181273452347,-13.1784443345948));
#45476=CARTESIAN_POINT('Ctrl Pts',(-27.3552722600769,4.07499453777574,-14.427651994048));
#45477=CARTESIAN_POINT('Ctrl Pts',(-27.3479622490176,4.07760858671024,-15.5535739483884));
#45478=CARTESIAN_POINT('Ctrl Pts',(-27.3446497885251,4.07876798806127,-16.307088587635));
#45479=CARTESIAN_POINT('Ctrl Pts',(-27.342907585337,4.07935477734326,-16.8103475162039));
#45480=CARTESIAN_POINT('Ctrl Pts',(-27.3421791743516,4.07954249347778,-17.1890064902595));
#45481=CARTESIAN_POINT('Ctrl Pts',(-27.3419588704251,4.07952326588427,-17.5045746536951));
#45482=CARTESIAN_POINT('Ctrl Pts',(-27.3418752611563,4.07953007569022,-17.6287095806376));
#45483=CARTESIAN_POINT('Ctrl Pts',(-27.3417287621694,4.07959279821592,-17.8776598485618));
#45484=CARTESIAN_POINT('Ctrl Pts',(-27.3416217867385,4.07971620085526,-18.1266789982541));
#45485=CARTESIAN_POINT('Ctrl Pts',(-27.3415769078325,4.0798783484122,-18.3760568720131));
#45486=CARTESIAN_POINT('Ctrl Pts',(-27.3415780390966,4.07999031882576,-18.5320055063777));
#45487=CARTESIAN_POINT('Ctrl Pts',(-27.3415994740873,4.08008358626996,-18.6568386635698));
#45488=CARTESIAN_POINT('Ctrl Pts',(-27.3416262524713,4.08015453248145,-18.7504946446562));
#45489=CARTESIAN_POINT('Ctrl Pts',(-27.3416579949172,4.08021387882802,-18.8285700716364));
#45490=CARTESIAN_POINT('Ctrl Pts',(-27.3416894772009,4.0802611446212,-18.8910467255343));
#45491=CARTESIAN_POINT('Ctrl Pts',(-27.341991802707,4.08066067875279,-19.4221941757928));
#45492=CARTESIAN_POINT('Ctrl Pts',(-27.3436410578754,4.08129684321048,-20.440725937771));
#45493=CARTESIAN_POINT('Ctrl Pts',(-27.351961923784,4.07891025829886,-21.953997325392));
#45494=CARTESIAN_POINT('Ctrl Pts',(-27.3630621133216,4.07297610046509,-22.9693110673969));
#45495=CARTESIAN_POINT('Ctrl Pts',(-27.3722796464463,4.06725958282786,-23.6042261310723));
#45496=CARTESIAN_POINT('Ctrl Pts',(-27.3763643044384,4.0646734681043,-23.8569164199335));
#45497=CARTESIAN_POINT('Ctrl Pts',(-27.3860541716508,4.05838892454659,-24.3613801869045));
#45498=CARTESIAN_POINT('Ctrl Pts',(-27.4064446332014,4.04484082022933,-25.2443384429749));
#45499=CARTESIAN_POINT('Ctrl Pts',(-27.4420556226772,4.02029323011283,-26.5035495796231));
#45500=CARTESIAN_POINT('Ctrl Pts',(-27.4848968440096,3.98986151530367,-28.0078199110668));
#45501=CARTESIAN_POINT('Ctrl Pts',(-27.5067731539225,3.97402841603677,-29.0035660851326));
#45502=CARTESIAN_POINT('Ctrl Pts',(-27.5154451374984,3.96791231174987,-29.560992238552));
#45503=CARTESIAN_POINT('Ctrl Pts',(-27.5173370691358,3.96655872264482,-29.6863747424985));
#45504=CARTESIAN_POINT('Ctrl Pts',(-27.5209678542977,3.9639284711308,-29.9363122547117));
#45505=CARTESIAN_POINT('Ctrl Pts',(-27.5269263449902,3.95950868834027,-30.3742227049902));
#45506=CARTESIAN_POINT('Ctrl Pts',(-27.5373167256218,3.95148861588675,-31.2498686218677));
#45507=CARTESIAN_POINT('Ctrl Pts',(-27.5480809685386,3.94270291613348,-32.5008060849347));
#45508=CARTESIAN_POINT('Ctrl Pts',(-27.5541815642533,3.93838291801496,-33.7492714989798));
#45509=CARTESIAN_POINT('Ctrl Pts',(-27.556738020654,3.93812425981094,-34.7453564932264));
#45510=CARTESIAN_POINT('Ctrl Pts',(-27.5573055494602,3.9391294137175,-35.2424175058302));
#45511=CARTESIAN_POINT('Ctrl Pts',(-27.557494604669,3.94034033135259,-35.6156931631465));
#45512=CARTESIAN_POINT('Ctrl Pts',(-27.5576458724682,3.94128873126373,-35.8658549594538));
#45513=CARTESIAN_POINT('Ctrl Pts',(-27.5579450503163,3.94371014608695,-36.3654927635573));
#45514=CARTESIAN_POINT('Ctrl Pts',(-27.5582209322075,3.94934036350232,-37.2390728137141));
#45515=CARTESIAN_POINT('Ctrl Pts',(-27.5556802719258,3.96573535501417,-38.9826258473562));
#45516=CARTESIAN_POINT('Ctrl Pts',(-27.5413304064018,3.98804089509753,-40.4803287991562));
#45517=CARTESIAN_POINT('Ctrl Pts',(-27.5148059809254,4.01012355087822,-41.7335732325126));
#45518=CARTESIAN_POINT('Ctrl Pts',(-27.506614799977,4.01382313814948,-42.1294899173214));
#45519=CARTESIAN_POINT('Ctrl Pts',(-27.4948038728113,4.01475197238754,-42.6392652194878));
#45520=CARTESIAN_POINT('Ctrl Pts',(-27.4823100500975,4.01410807310616,-43.1478052204435));
#45521=CARTESIAN_POINT('Ctrl Pts',(-27.4652056523953,4.01188834921534,-43.7741459445469));
#45522=CARTESIAN_POINT('Ctrl Pts',(-27.4416686637682,4.01205030286353,-44.5131850793774));
#45523=CARTESIAN_POINT('Ctrl Pts',(-27.4190118436299,4.01846618553771,-45.1172726644237));
#45524=CARTESIAN_POINT('Ctrl Pts',(-27.3987206949338,4.02951859982369,-45.5932733110073));
#45525=CARTESIAN_POINT('Ctrl Pts',(-27.3823587370145,4.04130353601179,-45.946621494624));
#45526=CARTESIAN_POINT('Ctrl Pts',(-27.3647800503514,4.05707927954136,-46.2962615516113));
#45527=CARTESIAN_POINT('Ctrl Pts',(-27.3396207882002,4.08405630656236,-46.757424891615));
#45528=CARTESIAN_POINT('Ctrl Pts',(-27.3187605625721,4.11169988508255,-47.0976336407574));
#45529=CARTESIAN_POINT('Ctrl Pts',(-27.2963805619571,4.14521705812,-47.4351463426626));
#45530=CARTESIAN_POINT('Ctrl Pts',(-27.2797829769067,4.17028343828459,-47.6747586518392));
#45531=CARTESIAN_POINT('Ctrl Pts',(-27.2414790687407,4.22420761329892,-48.1470192771235));
#45532=CARTESIAN_POINT('Ctrl Pts',(-27.1631572478958,4.33065416927353,-48.978912160315));
#45533=CARTESIAN_POINT('Ctrl Pts',(-27.0323943570625,4.51336562870429,-50.1699149604666));
#45534=CARTESIAN_POINT('Ctrl Pts',(-26.8879168085563,4.78197800293409,-51.6087945648171));
#45535=CARTESIAN_POINT('Ctrl Pts',(-26.8258901135032,4.99983547607388,-52.5715476767348));
#45536=CARTESIAN_POINT('Ctrl Pts',(-26.8050492994794,5.1504403653152,-53.1743205901841));
#45537=CARTESIAN_POINT('Ctrl Pts',(-26.7981595044316,5.21154340576477,-53.4118332759869));
#45538=CARTESIAN_POINT('Ctrl Pts',(-26.788298589805,5.34149963276008,-53.8916837498143));
#45539=CARTESIAN_POINT('Ctrl Pts',(-26.7811782829475,5.58568815680499,-54.7327463636641));
#45540=CARTESIAN_POINT('Ctrl Pts',(-26.8002012452745,6.13595090561274,-56.4249561946581));
#45541=CARTESIAN_POINT('Ctrl Pts',(-26.852938438552,6.68507130930734,-57.8797527558067));
#45542=CARTESIAN_POINT('Ctrl Pts',(-26.8887442028565,7.08853302756357,-58.906082215184));
#45543=CARTESIAN_POINT('Ctrl Pts',(-26.8936556302131,7.13656932665945,-59.0270937517182));
#45544=CARTESIAN_POINT('Ctrl Pts',(-26.9043644557737,7.23481899580833,-59.2714068910028));
#45545=CARTESIAN_POINT('Ctrl Pts',(-26.9257340549756,7.40989753960044,-59.698336006939));
#45546=CARTESIAN_POINT('Ctrl Pts',(-26.977105952746,7.77323377402914,-60.5544351623106));
#45547=CARTESIAN_POINT('Ctrl Pts',(-27.0487369914947,8.21176114729655,-61.5339877132366));
#45548=CARTESIAN_POINT('Ctrl Pts',(-27.1191502767737,8.66420917288523,-62.5122919003745));
#45549=CARTESIAN_POINT('Ctrl Pts',(-27.1556698679012,8.92247578068374,-63.0612434193802));
#45550=CARTESIAN_POINT('Ctrl Pts',(-27.1776461428923,9.09566073391902,-63.4263573086767));
#45551=CARTESIAN_POINT('Ctrl Pts',(-27.1915965005875,9.21136121266743,-63.6695170955314));
#45552=CARTESIAN_POINT('Ctrl Pts',(-27.2043815764802,9.32733994357597,-63.9122250866032));
#45553=CARTESIAN_POINT('Ctrl Pts',(-27.2143717790303,9.42901319226746,-64.1241851694408));
#45554=CARTESIAN_POINT('Ctrl Pts',(-27.2197112470884,9.48715099835241,-64.2451752724045));
#45555=CARTESIAN_POINT('Ctrl Pts',(-27.227338582932,9.57438723927106,-64.4265181282341));
#45556=CARTESIAN_POINT('Ctrl Pts',(-27.2328678760352,9.64713745024055,-64.5773521359468));
#45557=CARTESIAN_POINT('Ctrl Pts',(-27.2407911835927,9.76750941850949,-64.8264712414182));
#45558=CARTESIAN_POINT('Ctrl Pts',(-27.2480703587409,9.88789116991536,-65.0729942285441));
#45559=CARTESIAN_POINT('Ctrl Pts',(-27.2592171476814,10.13507491431,-65.5696917896668));
#45560=CARTESIAN_POINT('Ctrl Pts',(-27.2707948775918,10.5751087883559,-66.4312179139581));
#45561=CARTESIAN_POINT('Ctrl Pts',(-27.2700304119169,11.4873858665043,-68.1468579632658));
#45562=CARTESIAN_POINT('Ctrl Pts',(-27.2525109126437,12.3030078621601,-69.6289538873663));
#45563=CARTESIAN_POINT('Ctrl Pts',(-27.2541201495845,12.9106217789162,-70.7767840803218));
#45564=CARTESIAN_POINT('Ctrl Pts',(-27.2544305738434,13.0425342299894,-71.0258395726878));
#45565=CARTESIAN_POINT('Ctrl Pts',(-27.2548923449946,13.3086323235748,-71.5277397348066));
#45566=CARTESIAN_POINT('Ctrl Pts',(-27.2551935210388,13.6407795601621,-72.1533706167213));
#45567=CARTESIAN_POINT('Ctrl Pts',(-27.2552241432152,14.0403353165931,-72.9049310243895));
#45568=CARTESIAN_POINT('Ctrl Pts',(-27.2548176665827,14.839974311778,-74.4075839612337));
#45569=CARTESIAN_POINT('Ctrl Pts',(-27.2539131733232,15.5075997838829,-75.6604288636657));
#45570=CARTESIAN_POINT('Ctrl Pts',(-27.2539071141013,16.4782256544517,-77.4859121791665));
#45571=CARTESIAN_POINT('Ctrl Pts',(-27.2539024723065,16.9143985081388,-78.3062348671697));
#45572=CARTESIAN_POINT('Ctrl Pts',(-27.2539024723065,17.3509200955282,-79.1272125692679));
#45573=CARTESIAN_POINT('Ctrl Pts',(-26.0013011106398,4.07985819352921,24.8306343146944));
#45574=CARTESIAN_POINT('Ctrl Pts',(-26.0013789529674,4.07985804951133,24.7817549932913));
#45575=CARTESIAN_POINT('Ctrl Pts',(-26.0014605947771,4.07985789809793,24.7328767261139));
#45576=CARTESIAN_POINT('Ctrl Pts',(-26.0024245885624,4.07985612747913,24.1822685228224));
#45577=CARTESIAN_POINT('Ctrl Pts',(-26.0031642737342,4.07985491125827,23.1781333336685));
#45578=CARTESIAN_POINT('Ctrl Pts',(-26.0048881842587,4.07985181195996,21.1695342768379));
#45579=CARTESIAN_POINT('Ctrl Pts',(-26.0113025736306,4.07984033585152,19.6653805292443));
#45580=CARTESIAN_POINT('Ctrl Pts',(-26.0249020614195,4.07981521286216,18.4143310323347));
#45581=CARTESIAN_POINT('Ctrl Pts',(-26.0314251371612,4.07980293276608,17.9115134907684));
#45582=CARTESIAN_POINT('Ctrl Pts',(-26.0478061265009,4.07977192289328,16.9075232341124));
#45583=CARTESIAN_POINT('Ctrl Pts',(-26.082942053095,4.07970491200509,15.153713540109));
#45584=CARTESIAN_POINT('Ctrl Pts',(-26.1163096414983,4.07964468448795,13.6519733108666));
#45585=CARTESIAN_POINT('Ctrl Pts',(-26.1372103910028,4.07960974585599,12.3975008589439));
#45586=CARTESIAN_POINT('Ctrl Pts',(-26.1457529910553,4.07959572525298,11.8965472956601));
#45587=CARTESIAN_POINT('Ctrl Pts',(-26.1631632522454,4.07956765728665,10.8947040346659));
#45588=CARTESIAN_POINT('Ctrl Pts',(-26.1846759019604,4.0795364209103,9.64217637151487));
#45589=CARTESIAN_POINT('Ctrl Pts',(-26.2073607059512,4.07950398038011,8.13768241570142));
#45590=CARTESIAN_POINT('Ctrl Pts',(-26.2185663909266,4.07949098160033,7.13297738461757));
#45591=CARTESIAN_POINT('Ctrl Pts',(-26.2237726343733,4.07948462062371,6.50500244631245));
#45592=CARTESIAN_POINT('Ctrl Pts',(-26.225727981951,4.07948619840636,6.25483282875101));
#45593=CARTESIAN_POINT('Ctrl Pts',(-26.2291798508411,4.07950316165294,5.7537796075322));
#45594=CARTESIAN_POINT('Ctrl Pts',(-26.2340434904564,4.07956239453138,4.87545560005647));
#45595=CARTESIAN_POINT('Ctrl Pts',(-26.2393234114807,4.0797290922924,3.11516020236738));
#45596=CARTESIAN_POINT('Ctrl Pts',(-26.237030454936,4.07974833926762,1.60817566708211));
#45597=CARTESIAN_POINT('Ctrl Pts',(-26.2330023014032,4.07948610402459,0.548332138737982));
#45598=CARTESIAN_POINT('Ctrl Pts',(-26.2324770878948,4.07945134405716,0.422083829682385));
#45599=CARTESIAN_POINT('Ctrl Pts',(-26.2312481821157,4.07937089598177,0.169809390305926));
#45600=CARTESIAN_POINT('Ctrl Pts',(-26.2286559185981,4.07920222706464,-0.27115977582926));
#45601=CARTESIAN_POINT('Ctrl Pts',(-26.2238184296938,4.07889540886044,-0.899774172662865));
#45602=CARTESIAN_POINT('Ctrl Pts',(-26.2166636663486,4.07844774619556,-1.65243157223408));
#45603=CARTESIAN_POINT('Ctrl Pts',(-26.2058812029711,4.07780173875976,-2.65434197500388));
#45604=CARTESIAN_POINT('Ctrl Pts',(-26.1912186942687,4.07697792765496,-3.90481027092992));
#45605=CARTESIAN_POINT('Ctrl Pts',(-26.1805376495462,4.0765172745372,-4.90557994986776));
#45606=CARTESIAN_POINT('Ctrl Pts',(-26.1749400951133,4.07635014998955,-5.53202086932197));
#45607=CARTESIAN_POINT('Ctrl Pts',(-26.1727011491545,4.07628811967238,-5.78288697526722));
#45608=CARTESIAN_POINT('Ctrl Pts',(-26.1682289140555,4.07618740313827,-6.28485799474117));
#45609=CARTESIAN_POINT('Ctrl Pts',(-26.1604325178287,4.07606775162831,-7.16391906466739));
#45610=CARTESIAN_POINT('Ctrl Pts',(-26.1494816680626,4.07603758491267,-8.42033007674828));
#45611=CARTESIAN_POINT('Ctrl Pts',(-26.1390583937814,4.07613309366833,-9.67479848719443));
#45612=CARTESIAN_POINT('Ctrl Pts',(-26.1321868318539,4.07623167871274,-10.5504384656346));
#45613=CARTESIAN_POINT('Ctrl Pts',(-26.1284001112086,4.07629308869807,-11.0498864309384));
#45614=CARTESIAN_POINT('Ctrl Pts',(-26.1265564850085,4.07632463227181,-11.2992701474647));
#45615=CARTESIAN_POINT('Ctrl Pts',(-26.1251882913001,4.07634839740299,-11.4869495146409));
#45616=CARTESIAN_POINT('Ctrl Pts',(-26.1242555799087,4.07636641590398,-11.6129935292225));
#45617=CARTESIAN_POINT('Ctrl Pts',(-26.1223445077193,4.07640971360248,-11.8648337223802));
#45618=CARTESIAN_POINT('Ctrl Pts',(-26.1188970858275,4.07650331865429,-12.3048696473225));
#45619=CARTESIAN_POINT('Ctrl Pts',(-26.1117260730017,4.07674902706291,-13.1826603926455));
#45620=CARTESIAN_POINT('Ctrl Pts',(-26.101497548318,4.07719956532485,-14.4323339566743));
#45621=CARTESIAN_POINT('Ctrl Pts',(-26.094209581299,4.07757043836075,-15.5572475817683));
#45622=CARTESIAN_POINT('Ctrl Pts',(-26.0909394569588,4.07774555434298,-16.3095070995799));
#45623=CARTESIAN_POINT('Ctrl Pts',(-26.0892367197142,4.077839471914,-16.8117785888063));
#45624=CARTESIAN_POINT('Ctrl Pts',(-26.0885535312242,4.07788117066302,-17.1895156247893));
#45625=CARTESIAN_POINT('Ctrl Pts',(-26.0883821177462,4.07789384316656,-17.5042618733334));
#45626=CARTESIAN_POINT('Ctrl Pts',(-26.0883230229287,4.07790111607961,-17.628808694147));
#45627=CARTESIAN_POINT('Ctrl Pts',(-26.0882450051653,4.07792362052946,-17.8780681622715));
#45628=CARTESIAN_POINT('Ctrl Pts',(-26.0882341952123,4.07795736618271,-18.1274489041177));
#45629=CARTESIAN_POINT('Ctrl Pts',(-26.088304936263,4.0779971328375,-18.3769928741742));
#45630=CARTESIAN_POINT('Ctrl Pts',(-26.0883860806377,4.07802434284426,-18.5330186180899));
#45631=CARTESIAN_POINT('Ctrl Pts',(-26.0884749174287,4.07804674968717,-18.6578788062151));
#45632=CARTESIAN_POINT('Ctrl Pts',(-26.0885539625203,4.07806388881347,-18.7515431416536));
#45633=CARTESIAN_POINT('Ctrl Pts',(-26.0886305534487,4.07807837511368,-18.8296132271757));
#45634=CARTESIAN_POINT('Ctrl Pts',(-26.0886984753022,4.07808994493893,-18.8920790549508));
#45635=CARTESIAN_POINT('Ctrl Pts',(-26.0893139685706,4.07818866471405,-19.4230945168937));
#45636=CARTESIAN_POINT('Ctrl Pts',(-26.0917330611588,4.07841063103444,-20.4400949792451));
#45637=CARTESIAN_POINT('Ctrl Pts',(-26.1006601571851,4.07826175095829,-21.9476412695908));
#45638=CARTESIAN_POINT('Ctrl Pts',(-26.1114730684071,4.07759859850918,-22.9568095349218));
#45639=CARTESIAN_POINT('Ctrl Pts',(-26.1200732731373,4.07685326303561,-23.5871603310035));
#45640=CARTESIAN_POINT('Ctrl Pts',(-26.1238447233394,4.07651791001592,-23.8368150555011));
#45641=CARTESIAN_POINT('Ctrl Pts',(-26.1326887293755,4.07567329563507,-24.336735111528));
#45642=CARTESIAN_POINT('Ctrl Pts',(-26.1510952602828,4.07375702558255,-25.2132310967213));
#45643=CARTESIAN_POINT('Ctrl Pts',(-26.1830001890633,4.06986262685334,-26.468802499517));
#45644=CARTESIAN_POINT('Ctrl Pts',(-26.2215211544865,4.06399270040154,-27.9769098624109));
#45645=CARTESIAN_POINT('Ctrl Pts',(-26.2418385192627,4.06041574406107,-28.9807911429983));
#45646=CARTESIAN_POINT('Ctrl Pts',(-26.2502429726783,4.05888649081813,-29.5442314297393));
#45647=CARTESIAN_POINT('Ctrl Pts',(-26.2520732505535,4.05855306998243,-29.6696430577692));
#45648=CARTESIAN_POINT('Ctrl Pts',(-26.2555970918632,4.05789153584461,-29.9203997673132));
#45649=CARTESIAN_POINT('Ctrl Pts',(-26.261410577545,4.05676154246959,-30.3594301535443));
#45650=CARTESIAN_POINT('Ctrl Pts',(-26.2717052240543,4.05461490675908,-31.2378241849018));
#45651=CARTESIAN_POINT('Ctrl Pts',(-26.2830148460803,4.05196591433397,-32.4931655030781));
#45652=CARTESIAN_POINT('Ctrl Pts',(-26.2909663449978,4.0501119239892,-33.7469906547072));
#45653=CARTESIAN_POINT('Ctrl Pts',(-26.2960159444366,4.04922281675521,-34.7478634587198));
#45654=CARTESIAN_POINT('Ctrl Pts',(-26.2982099355632,4.04899711046201,-35.2475023730581));
#45655=CARTESIAN_POINT('Ctrl Pts',(-26.2997826761264,4.0489154594892,-35.6227846526373));
#45656=CARTESIAN_POINT('Ctrl Pts',(-26.3009025087611,4.04886072072356,-35.8743950226809));
#45657=CARTESIAN_POINT('Ctrl Pts',(-26.3033140765469,4.0487766255127,-36.3767187361697));
#45658=CARTESIAN_POINT('Ctrl Pts',(-26.3077126946144,4.048701942534,-37.2547021301723));
#45659=CARTESIAN_POINT('Ctrl Pts',(-26.3151948391617,4.04931673891994,-39.0056140064209));
#45660=CARTESIAN_POINT('Ctrl Pts',(-26.3121081978818,4.05196032314691,-40.507437776701));
#45661=CARTESIAN_POINT('Ctrl Pts',(-26.2962978934717,4.05673709347293,-41.7629658680623));
#45662=CARTESIAN_POINT('Ctrl Pts',(-26.2912875139118,4.05507580219809,-42.1583486673137));
#45663=CARTESIAN_POINT('Ctrl Pts',(-26.283791863667,4.0491342464197,-42.6687098541352));
#45664=CARTESIAN_POINT('Ctrl Pts',(-26.2756834339648,4.04155010070283,-43.1780724170856));
#45665=CARTESIAN_POINT('Ctrl Pts',(-26.2642595673674,4.03052052051979,-43.8062806290324));
#45666=CARTESIAN_POINT('Ctrl Pts',(-26.2480330835504,4.0194952467161,-44.5487497045344));
#45667=CARTESIAN_POINT('Ctrl Pts',(-26.2320172183841,4.0158442331942,-45.1567415924084));
#45668=CARTESIAN_POINT('Ctrl Pts',(-26.2174638323169,4.01834227502156,-45.6363901948794));
#45669=CARTESIAN_POINT('Ctrl Pts',(-26.2056203435843,4.02341069113659,-45.9927657037704));
#45670=CARTESIAN_POINT('Ctrl Pts',(-26.1927889704637,4.03215314673909,-46.3456933378785));
#45671=CARTESIAN_POINT('Ctrl Pts',(-26.1742863860446,4.04932860164585,-46.8115670714307));
#45672=CARTESIAN_POINT('Ctrl Pts',(-26.1587617170671,4.06906009399286,-47.1556407818341));
#45673=CARTESIAN_POINT('Ctrl Pts',(-26.1419956568944,4.09431737965409,-47.4973171236936));
#45674=CARTESIAN_POINT('Ctrl Pts',(-26.1296745959103,4.11338925269087,-47.7457981442306));
#45675=CARTESIAN_POINT('Ctrl Pts',(-26.1013205493372,4.15316604518592,-48.2295842951589));
#45676=CARTESIAN_POINT('Ctrl Pts',(-26.043416140312,4.23037271286573,-49.0771569518487));
#45677=CARTESIAN_POINT('Ctrl Pts',(-25.9455247181537,4.36377552848887,-50.2707023199233));
#45678=CARTESIAN_POINT('Ctrl Pts',(-25.8328678181711,4.574975096906,-51.6834281820652));
#45679=CARTESIAN_POINT('Ctrl Pts',(-25.7807568251049,4.76266701885439,-52.6109487298273));
#45680=CARTESIAN_POINT('Ctrl Pts',(-25.761061240267,4.89944564339107,-53.1875046786558));
#45681=CARTESIAN_POINT('Ctrl Pts',(-25.7537316641207,4.95647452053676,-53.4190926834034));
#45682=CARTESIAN_POINT('Ctrl Pts',(-25.7413216255973,5.07937523522014,-53.8860406962918));
#45683=CARTESIAN_POINT('Ctrl Pts',(-25.7251768408865,5.31590876729731,-54.7092722248442));
#45684=CARTESIAN_POINT('Ctrl Pts',(-25.7125117551334,5.86695869123698,-56.377799583334));
#45685=CARTESIAN_POINT('Ctrl Pts',(-25.7272665769259,6.4412901900278,-57.8308948707272));
#45686=CARTESIAN_POINT('Ctrl Pts',(-25.7450834120612,6.86571500273623,-58.861081018843));
#45687=CARTESIAN_POINT('Ctrl Pts',(-25.7479653604283,6.91488381928122,-58.9789732806086));
#45688=CARTESIAN_POINT('Ctrl Pts',(-25.7543567837446,7.0169659084858,-59.2195463362856));
#45689=CARTESIAN_POINT('Ctrl Pts',(-25.7678613171999,7.20000915828807,-59.6399468852958));
#45690=CARTESIAN_POINT('Ctrl Pts',(-25.8021625084514,7.58581364664845,-60.4878171982801));
#45691=CARTESIAN_POINT('Ctrl Pts',(-25.8524352509597,8.0611970776665,-61.4656187046925));
#45692=CARTESIAN_POINT('Ctrl Pts',(-25.90252465855,8.55513729052697,-62.4492671574831));
#45693=CARTESIAN_POINT('Ctrl Pts',(-25.928651178022,8.83691687892463,-63.0037282242701));
#45694=CARTESIAN_POINT('Ctrl Pts',(-25.944371873633,9.02523196372997,-63.373608830517));
#45695=CARTESIAN_POINT('Ctrl Pts',(-25.9543434819169,9.15082245505529,-63.6202400576412));
#45696=CARTESIAN_POINT('Ctrl Pts',(-25.9634734726841,9.27634197235377,-63.8668663154678));
#45697=CARTESIAN_POINT('Ctrl Pts',(-25.9705707619772,9.38593094629149,-64.0826638689853));
#45698=CARTESIAN_POINT('Ctrl Pts',(-25.9743509373666,9.44845327423451,-64.205966795196));
#45699=CARTESIAN_POINT('Ctrl Pts',(-25.9797346364237,9.54211734605829,-64.3908984026352));
#45700=CARTESIAN_POINT('Ctrl Pts',(-25.9836044565101,9.61990677396525,-64.5449847761923));
#45701=CARTESIAN_POINT('Ctrl Pts',(-25.9890686033632,9.74807232430769,-64.7998073145916));
#45702=CARTESIAN_POINT('Ctrl Pts',(-25.9941273732596,9.8747278984663,-65.0500852591708));
#45703=CARTESIAN_POINT('Ctrl Pts',(-26.0019533277936,10.1327864314665,-65.5545426485505));
#45704=CARTESIAN_POINT('Ctrl Pts',(-26.0103402635887,10.5858336795818,-66.4269375967908));
#45705=CARTESIAN_POINT('Ctrl Pts',(-26.0107942689654,11.5053252365357,-68.1563355054035));
#45706=CARTESIAN_POINT('Ctrl Pts',(-25.999427322288,12.3081687393399,-69.635923753248));
#45707=CARTESIAN_POINT('Ctrl Pts',(-26.0007804305651,12.9122366459945,-70.7750284298339));
#45708=CARTESIAN_POINT('Ctrl Pts',(-26.0010398240432,13.0447978230638,-71.0249228148133));
#45709=CARTESIAN_POINT('Ctrl Pts',(-26.0014260269405,13.3112219759726,-71.5268614383352));
#45710=CARTESIAN_POINT('Ctrl Pts',(-26.0016831772529,13.6439024713188,-72.1531133439487));
#45711=CARTESIAN_POINT('Ctrl Pts',(-26.0017116603525,14.0436285487339,-72.904950139645));
#45712=CARTESIAN_POINT('Ctrl Pts',(-26.001378475861,14.8432872869915,-74.4081331829722));
#45713=CARTESIAN_POINT('Ctrl Pts',(-26.0006442548659,15.5102605444829,-75.6608410472288));
#45714=CARTESIAN_POINT('Ctrl Pts',(-26.0006503198601,16.4805469958596,-77.4856768722736));
#45715=CARTESIAN_POINT('Ctrl Pts',(-26.0006527044304,16.9168473443495,-78.3062345927038));
#45716=CARTESIAN_POINT('Ctrl Pts',(-26.0006527044303,17.353368931739,-79.1272122948021));
#45717=CARTESIAN_POINT('Ctrl Pts',(-24.4328318080232,4.08203882016111,24.8306371264184));
#45718=CARTESIAN_POINT('Ctrl Pts',(-24.4329049339045,4.0820388383689,24.7817578938191));
#45719=CARTESIAN_POINT('Ctrl Pts',(-24.4329816263336,4.08203885856826,24.7328797194657));
#45720=CARTESIAN_POINT('Ctrl Pts',(-24.4338873085871,4.08203904250686,24.1822724775926));
#45721=CARTESIAN_POINT('Ctrl Pts',(-24.4345815096013,4.08204034390179,23.1781378187383));
#45722=CARTESIAN_POINT('Ctrl Pts',(-24.4361966771044,4.08204501789817,21.1695406054735));
#45723=CARTESIAN_POINT('Ctrl Pts',(-24.4422245118959,4.08204573173726,19.6653857265717));
#45724=CARTESIAN_POINT('Ctrl Pts',(-24.4550083596785,4.08204123836197,18.4143357624134));
#45725=CARTESIAN_POINT('Ctrl Pts',(-24.461139366778,4.08203963145082,17.9115238657484));
#45726=CARTESIAN_POINT('Ctrl Pts',(-24.4765351484309,4.08203632002672,16.9075371526626));
#45727=CARTESIAN_POINT('Ctrl Pts',(-24.5095575369227,4.08202883184548,15.1537261634006));
#45728=CARTESIAN_POINT('Ctrl Pts',(-24.5409310461033,4.08201346651148,13.6519635833544));
#45729=CARTESIAN_POINT('Ctrl Pts',(-24.5605971654187,4.08199050068771,12.3974651968261));
#45730=CARTESIAN_POINT('Ctrl Pts',(-24.5686366192223,4.08197955945333,11.8965012353701));
#45731=CARTESIAN_POINT('Ctrl Pts',(-24.5850253084715,4.08195250599241,10.8946432184679));
#45732=CARTESIAN_POINT('Ctrl Pts',(-24.6052886162435,4.08191075176859,9.64210302146757));
#45733=CARTESIAN_POINT('Ctrl Pts',(-24.6266610628654,4.08186049614118,8.13760746381553));
#45734=CARTESIAN_POINT('Ctrl Pts',(-24.6372300407483,4.08183116969183,7.13291059862724));
#45735=CARTESIAN_POINT('Ctrl Pts',(-24.6421399318701,4.08181766181541,6.50493464946377));
#45736=CARTESIAN_POINT('Ctrl Pts',(-24.6439794711074,4.08180069432847,6.25456031789306));
#45737=CARTESIAN_POINT('Ctrl Pts',(-24.6472120730065,4.08172914744407,5.7532871677214));
#45738=CARTESIAN_POINT('Ctrl Pts',(-24.6517372559496,4.08152611618778,4.87468424116016));
#45739=CARTESIAN_POINT('Ctrl Pts',(-24.6565509082759,4.08100382920229,3.11456026023057));
#45740=CARTESIAN_POINT('Ctrl Pts',(-24.6544724421558,4.08096941635004,1.60884222114878));
#45741=CARTESIAN_POINT('Ctrl Pts',(-24.6510280232343,4.08176327560631,0.550492677300362));
#45742=CARTESIAN_POINT('Ctrl Pts',(-24.6505764402692,4.0818674887422,0.424505967923186));
#45743=CARTESIAN_POINT('Ctrl Pts',(-24.6495208106213,4.08210721288495,0.172673872967497));
#45744=CARTESIAN_POINT('Ctrl Pts',(-24.6472916185596,4.08260571194979,-0.267573473778777));
#45745=CARTESIAN_POINT('Ctrl Pts',(-24.6431379587548,4.08350722699859,-0.89539679214541));
#45746=CARTESIAN_POINT('Ctrl Pts',(-24.6369546732155,4.08481003070192,-1.64746533107212));
#45747=CARTESIAN_POINT('Ctrl Pts',(-24.6276191157051,4.08669315246911,-2.6490839377641));
#45748=CARTESIAN_POINT('Ctrl Pts',(-24.6147929138544,4.08909943830927,-3.90010599264371));
#45749=CARTESIAN_POINT('Ctrl Pts',(-24.6052760567306,4.09052613332115,-4.90226333565535));
#45750=CARTESIAN_POINT('Ctrl Pts',(-24.6001745652444,4.0911094069591,-5.52984284895121));
#45751=CARTESIAN_POINT('Ctrl Pts',(-24.5981139992996,4.09133854899239,-5.78075163694452));
#45752=CARTESIAN_POINT('Ctrl Pts',(-24.5939307763709,4.09176691364529,-6.28304411230748));
#45753=CARTESIAN_POINT('Ctrl Pts',(-24.5864961556743,4.0924340328852,-7.16255514817445));
#45754=CARTESIAN_POINT('Ctrl Pts',(-24.5758102198082,4.09311888145363,-8.41971103227847));
#45755=CARTESIAN_POINT('Ctrl Pts',(-24.5657198327711,4.09336487731083,-9.67493210132952));
#45756=CARTESIAN_POINT('Ctrl Pts',(-24.5593270395084,4.09326574663779,-10.5511417958087));
#45757=CARTESIAN_POINT('Ctrl Pts',(-24.5559184005747,4.09312458412497,-11.0509217702293));
#45758=CARTESIAN_POINT('Ctrl Pts',(-24.5543044100236,4.09302472042004,-11.3004728765148));
#45759=CARTESIAN_POINT('Ctrl Pts',(-24.5531258794835,4.09293825499699,-11.4882861671064));
#45760=CARTESIAN_POINT('Ctrl Pts',(-24.5523292371509,4.09286885279553,-11.6146582364255));
#45761=CARTESIAN_POINT('Ctrl Pts',(-24.5507230495914,4.09268856485644,-11.8669790977079));
#45762=CARTESIAN_POINT('Ctrl Pts',(-24.5478895447913,4.0922717256907,-12.3078288871903));
#45763=CARTESIAN_POINT('Ctrl Pts',(-24.5422194094636,4.09109236813779,-13.1868118100637));
#45764=CARTESIAN_POINT('Ctrl Pts',(-24.5345995785184,4.08879228071369,-14.4370658744763));
#45765=CARTESIAN_POINT('Ctrl Pts',(-24.5295037913775,4.08683613387482,-15.5611030676991));
#45766=CARTESIAN_POINT('Ctrl Pts',(-24.5273395914017,4.08593960406076,-16.3122009915398));
#45767=CARTESIAN_POINT('Ctrl Pts',(-24.5262586921781,4.08547557780888,-16.81354768392));
#45768=CARTESIAN_POINT('Ctrl Pts',(-24.5258891314335,4.08529768429567,-17.1904158183016));
#45769=CARTESIAN_POINT('Ctrl Pts',(-24.525871558669,4.08527938997473,-17.5043838498736));
#45770=CARTESIAN_POINT('Ctrl Pts',(-24.5258950789288,4.08526014193185,-17.6294009867654));
#45771=CARTESIAN_POINT('Ctrl Pts',(-24.5260591397072,4.08517981266925,-17.8790538820908));
#45772=CARTESIAN_POINT('Ctrl Pts',(-24.5263888608286,4.08504415175307,-18.1288802872769));
#45773=CARTESIAN_POINT('Ctrl Pts',(-24.5268735697162,4.08487513717692,-18.3786568942798));
#45774=CARTESIAN_POINT('Ctrl Pts',(-24.5272366949415,4.08475852743056,-18.5347981650712));
#45775=CARTESIAN_POINT('Ctrl Pts',(-24.5275622637412,4.08466156176116,-18.6597126134333));
#45776=CARTESIAN_POINT('Ctrl Pts',(-24.5278232220106,4.08458737978976,-18.7534044844896));
#45777=CARTESIAN_POINT('Ctrl Pts',(-24.5280542699026,4.08452484047191,-18.8314840644228));
#45778=CARTESIAN_POINT('Ctrl Pts',(-24.528247206293,4.08447476208227,-18.8939501719104));
#45779=CARTESIAN_POINT('Ctrl Pts',(-24.5299314546868,4.084049330607,-19.42492452698));
#45780=CARTESIAN_POINT('Ctrl Pts',(-24.5344449948442,4.08321387971141,-20.440489043094));
#45781=CARTESIAN_POINT('Ctrl Pts',(-24.543292732778,4.08453791394782,-21.9420823662568));
#45782=CARTESIAN_POINT('Ctrl Pts',(-24.5492197690682,4.0886038396778,-22.9447655341206));
#45783=CARTESIAN_POINT('Ctrl Pts',(-24.5526086662065,4.09268061333238,-23.5702445968926));
#45784=CARTESIAN_POINT('Ctrl Pts',(-24.5540154132293,4.09451599983593,-23.8169099228532));
#45785=CARTESIAN_POINT('Ctrl Pts',(-24.5570285573681,4.09898656854328,-24.3122487178896));
#45786=CARTESIAN_POINT('Ctrl Pts',(-24.56276692588,4.1086444896345,-25.1821960973038));
#45787=CARTESIAN_POINT('Ctrl Pts',(-24.5717213878898,4.1260537718618,-26.4337457009266));
#45788=CARTESIAN_POINT('Ctrl Pts',(-24.5823806002763,4.14782107631549,-27.9449849114494));
#45789=CARTESIAN_POINT('Ctrl Pts',(-24.5882113254279,4.15925502228168,-28.9563911373271));
#45790=CARTESIAN_POINT('Ctrl Pts',(-24.5909041335844,4.16385336794095,-29.5254986098915));
#45791=CARTESIAN_POINT('Ctrl Pts',(-24.5914883029049,4.16486110508338,-29.6508494551747));
#45792=CARTESIAN_POINT('Ctrl Pts',(-24.5925818190287,4.16684169819357,-29.9022586813579));
#45793=CARTESIAN_POINT('Ctrl Pts',(-24.5943078067308,4.17019215812943,-30.3421240539426));
#45794=CARTESIAN_POINT('Ctrl Pts',(-24.5971328074952,4.17640539766817,-31.222757091628));
#45795=CARTESIAN_POINT('Ctrl Pts',(-24.5999405591706,4.18360004719004,-32.4819446905374));
#45796=CARTESIAN_POINT('Ctrl Pts',(-24.6026962750198,4.18782846510269,-33.7408644899318));
#45797=CARTESIAN_POINT('Ctrl Pts',(-24.6058556550442,4.18902405819699,-34.7465161247673));
#45798=CARTESIAN_POINT('Ctrl Pts',(-24.6078798771038,4.18880809483548,-35.2487775798259));
#45799=CARTESIAN_POINT('Ctrl Pts',(-24.6096428164083,4.18831568843446,-35.6261321945983));
#45800=CARTESIAN_POINT('Ctrl Pts',(-24.6109922385861,4.18783075681031,-35.8793571817228));
#45801=CARTESIAN_POINT('Ctrl Pts',(-24.6142480612817,4.18627899067943,-36.3845573802002));
#45802=CARTESIAN_POINT('Ctrl Pts',(-24.6211264422861,4.18222070996565,-37.2671076307625));
#45803=CARTESIAN_POINT('Ctrl Pts',(-24.6373570395079,4.16961321135485,-39.0249602698805));
#45804=CARTESIAN_POINT('Ctrl Pts',(-24.6481151660576,4.15524941752727,-40.529029949255));
#45805=CARTESIAN_POINT('Ctrl Pts',(-24.6468650886017,4.14524912570874,-41.7847319913609));
#45806=CARTESIAN_POINT('Ctrl Pts',(-24.6461897055816,4.13911340038055,-42.1793898963392));
#45807=CARTESIAN_POINT('Ctrl Pts',(-24.644668791987,4.12738681795716,-42.6898623098505));
#45808=CARTESIAN_POINT('Ctrl Pts',(-24.6427330915817,4.11399518827006,-43.1996065381906));
#45809=CARTESIAN_POINT('Ctrl Pts',(-24.6395043903164,4.09555658875821,-43.8290856052551));
#45810=CARTESIAN_POINT('Ctrl Pts',(-24.6342765471189,4.0749930739795,-44.5742566312117));
#45811=CARTESIAN_POINT('Ctrl Pts',(-24.628737628711,4.062590230283,-45.1855434242497));
#45812=CARTESIAN_POINT('Ctrl Pts',(-24.6235099419859,4.0573912958463,-45.668414193604));
#45813=CARTESIAN_POINT('Ctrl Pts',(-24.6192060886881,4.05635426243155,-46.0275212789887));
#45814=CARTESIAN_POINT('Ctrl Pts',(-24.6145069503963,4.05863219077922,-46.383481956892));
#45815=CARTESIAN_POINT('Ctrl Pts',(-24.6076814086831,4.06666093590869,-46.8537993280201));
#45816=CARTESIAN_POINT('Ctrl Pts',(-24.6019872099252,4.07901552762075,-47.2016372979207));
#45817=CARTESIAN_POINT('Ctrl Pts',(-24.5958055099508,4.09641618661044,-47.5474421678294));
#45818=CARTESIAN_POINT('Ctrl Pts',(-24.5913712683569,4.10934105902638,-47.8029417046537));
#45819=CARTESIAN_POINT('Ctrl Pts',(-24.5814056235319,4.13531445476801,-48.2963911892102));
#45820=CARTESIAN_POINT('Ctrl Pts',(-24.56146850896,4.18490193876664,-49.1575863425959));
#45821=CARTESIAN_POINT('Ctrl Pts',(-24.5279458200227,4.27556608531903,-50.3562070638942));
#45822=CARTESIAN_POINT('Ctrl Pts',(-24.4858938315039,4.4428837539764,-51.7517739671845));
#45823=CARTESIAN_POINT('Ctrl Pts',(-24.461390157077,4.60900827143757,-52.6525716423806));
#45824=CARTESIAN_POINT('Ctrl Pts',(-24.4484905108795,4.73487136224401,-53.209174977372));
#45825=CARTESIAN_POINT('Ctrl Pts',(-24.4430521465422,4.7887282884734,-53.4373806697681));
#45826=CARTESIAN_POINT('Ctrl Pts',(-24.4317192066847,4.90549509712483,-53.8956606386991));
#45827=CARTESIAN_POINT('Ctrl Pts',(-24.4109944470492,5.13372131329,-54.7067363051391));
#45828=CARTESIAN_POINT('Ctrl Pts',(-24.3692471227293,5.6763881660845,-56.3563509132911));
#45829=CARTESIAN_POINT('Ctrl Pts',(-24.3437675480632,6.25879991271785,-57.8032062975063));
#45830=CARTESIAN_POINT('Ctrl Pts',(-24.341029342272,6.69397786084169,-58.8307086524388));
#45831=CARTESIAN_POINT('Ctrl Pts',(-24.3411208671879,6.74332718681714,-58.9458372518527));
#45832=CARTESIAN_POINT('Ctrl Pts',(-24.3417062019115,6.84711130653536,-59.1827509561341));
#45833=CARTESIAN_POINT('Ctrl Pts',(-24.3441622193476,7.03433766881384,-59.597104178985));
#45834=CARTESIAN_POINT('Ctrl Pts',(-24.3536724791938,7.43467527392181,-60.4373789937337));
#45835=CARTESIAN_POINT('Ctrl Pts',(-24.3717943585678,7.93771663556469,-61.4133876658175));
#45836=CARTESIAN_POINT('Ctrl Pts',(-24.3912062535787,8.46470278441751,-62.4007111868074));
#45837=CARTESIAN_POINT('Ctrl Pts',(-24.4015908839533,8.76565248391554,-62.9592074918713));
#45838=CARTESIAN_POINT('Ctrl Pts',(-24.4078408521788,8.96641401262123,-63.3326671659236));
#45839=CARTESIAN_POINT('Ctrl Pts',(-24.4118013418662,9.10017247081078,-63.5819311992385));
#45840=CARTESIAN_POINT('Ctrl Pts',(-24.4153964693371,9.23358342739155,-63.8315662393309));
#45841=CARTESIAN_POINT('Ctrl Pts',(-24.4181517556313,9.34974746755446,-64.0503614778889));
#45842=CARTESIAN_POINT('Ctrl Pts',(-24.4196013510527,9.41591411187275,-64.1754862316753));
#45843=CARTESIAN_POINT('Ctrl Pts',(-24.4216454967201,9.5149237269704,-64.363260414974));
#45844=CARTESIAN_POINT('Ctrl Pts',(-24.4230600410192,9.59689381836826,-64.5199556443652));
#45845=CARTESIAN_POINT('Ctrl Pts',(-24.4249609908961,9.73152040519062,-64.7794075712368));
#45846=CARTESIAN_POINT('Ctrl Pts',(-24.4267618223247,9.86311129565224,-65.0323219641432));
#45847=CARTESIAN_POINT('Ctrl Pts',(-24.4296434015535,10.1299209242335,-65.5426374353664));
#45848=CARTESIAN_POINT('Ctrl Pts',(-24.4330147835845,10.5934173267333,-66.4232263642777));
#45849=CARTESIAN_POINT('Ctrl Pts',(-24.4345492745441,11.5191264205175,-68.1634877083546));
#45850=CARTESIAN_POINT('Ctrl Pts',(-24.4318062287518,12.3123138158534,-69.6410995187623));
#45851=CARTESIAN_POINT('Ctrl Pts',(-24.432600721665,12.9138097618783,-70.7735299662248));
#45852=CARTESIAN_POINT('Ctrl Pts',(-24.4327582500792,13.0469292258093,-71.0241120680269));
#45853=CARTESIAN_POINT('Ctrl Pts',(-24.4329908948791,13.3136862027866,-71.5261396769025));
#45854=CARTESIAN_POINT('Ctrl Pts',(-24.4331415881787,13.6468365578975,-72.1529333484963));
#45855=CARTESIAN_POINT('Ctrl Pts',(-24.4331565772736,14.0467232319219,-72.9050401218054));
#45856=CARTESIAN_POINT('Ctrl Pts',(-24.4329502855999,14.8463826590023,-74.4087072420885));
#45857=CARTESIAN_POINT('Ctrl Pts',(-24.4324854674872,15.5126901449289,-75.661261113541));
#45858=CARTESIAN_POINT('Ctrl Pts',(-24.4324768503252,16.4826221707385,-77.4854635085514));
#45859=CARTESIAN_POINT('Ctrl Pts',(-24.4324724381068,16.9190261641936,-78.3062332170589));
#45860=CARTESIAN_POINT('Ctrl Pts',(-24.4324724381067,17.3555477515831,-79.1272109191574));
#45861=CARTESIAN_POINT('Ctrl Pts',(-21.9235774316919,4.08176546808655,24.8306369193277));
#45862=CARTESIAN_POINT('Ctrl Pts',(-21.9236428686436,4.08176559550084,24.7817576776117));
#45863=CARTESIAN_POINT('Ctrl Pts',(-21.9237115034019,4.08176572794409,24.7328794977117));
#45864=CARTESIAN_POINT('Ctrl Pts',(-21.9245217528927,4.08176734214813,24.1822720255645));
#45865=CARTESIAN_POINT('Ctrl Pts',(-21.9251390018536,4.08177000133521,23.1781358417132));
#45866=CARTESIAN_POINT('Ctrl Pts',(-21.9265775308832,4.08177621167794,21.1695385153907));
#45867=CARTESIAN_POINT('Ctrl Pts',(-21.931967300021,4.08178749152863,19.6653818684061));
#45868=CARTESIAN_POINT('Ctrl Pts',(-21.9434164377662,4.08180437977525,18.4143314897164));
#45869=CARTESIAN_POINT('Ctrl Pts',(-21.9489070469889,4.08181284441495,17.9115194314412));
#45870=CARTESIAN_POINT('Ctrl Pts',(-21.962692535589,4.08183510532099,16.9075317986474));
#45871=CARTESIAN_POINT('Ctrl Pts',(-21.9922632008758,4.08188221339639,15.1537188588092));
#45872=CARTESIAN_POINT('Ctrl Pts',(-22.0203613754922,4.08192202667274,13.6519498725972));
#45873=CARTESIAN_POINT('Ctrl Pts',(-22.0380013105594,4.08193332806647,12.3974494658034));
#45874=CARTESIAN_POINT('Ctrl Pts',(-22.0452156220464,4.08193637672117,11.8964850375535));
#45875=CARTESIAN_POINT('Ctrl Pts',(-22.0599343937993,4.08193706348693,10.8946266597817));
#45876=CARTESIAN_POINT('Ctrl Pts',(-22.0781357558683,4.08193323531193,9.64208318336994));
#45877=CARTESIAN_POINT('Ctrl Pts',(-22.0973540656548,4.08192056571144,8.13758194942714));
#45878=CARTESIAN_POINT('Ctrl Pts',(-22.1068473001385,4.08191491682695,7.13288362235554));
#45879=CARTESIAN_POINT('Ctrl Pts',(-22.1112625152373,4.08191090019794,6.50489136045323));
#45880=CARTESIAN_POINT('Ctrl Pts',(-22.1129339805934,4.08187071317327,6.2541756805871));
#45881=CARTESIAN_POINT('Ctrl Pts',(-22.1159302305084,4.08166530353184,5.75253329691742));
#45882=CARTESIAN_POINT('Ctrl Pts',(-22.1202552130462,4.08105636817354,4.87346500119448));
#45883=CARTESIAN_POINT('Ctrl Pts',(-22.1252904987501,4.07943127155768,3.11362229719922));
#45884=CARTESIAN_POINT('Ctrl Pts',(-22.1233486580589,4.07943847898292,1.61002085166886));
#45885=CARTESIAN_POINT('Ctrl Pts',(-22.1191273452128,4.08201502643112,0.554171951867155));
#45886=CARTESIAN_POINT('Ctrl Pts',(-22.1185809770122,4.08234757373234,0.428627811525919));
#45887=CARTESIAN_POINT('Ctrl Pts',(-22.1173048402443,4.08311757684658,0.17754258976633));
#45888=CARTESIAN_POINT('Ctrl Pts',(-22.1146233333163,4.08471885183798,-0.261483756755618));
#45889=CARTESIAN_POINT('Ctrl Pts',(-22.1096271138227,4.08763792655448,-0.887964206484821));
#45890=CARTESIAN_POINT('Ctrl Pts',(-22.1023004342366,4.09180755483889,-1.63901543576647));
#45891=CARTESIAN_POINT('Ctrl Pts',(-22.0912885877694,4.09784759942708,-2.6400937353228));
#45892=CARTESIAN_POINT('Ctrl Pts',(-22.0764800317693,4.10546290482369,-3.89197073679173));
#45893=CARTESIAN_POINT('Ctrl Pts',(-22.0658875624004,4.10997294524229,-4.89651629795362));
#45894=CARTESIAN_POINT('Ctrl Pts',(-22.0604649547566,4.11175755709603,-5.52609779188864));
#45895=CARTESIAN_POINT('Ctrl Pts',(-22.0582785674025,4.11241613965768,-5.77736459149553));
#45896=CARTESIAN_POINT('Ctrl Pts',(-22.0538560973387,4.11355327378553,-6.28052764005114));
#45897=CARTESIAN_POINT('Ctrl Pts',(-22.0460405611013,4.11509599517109,-7.16122110620086));
#45898=CARTESIAN_POINT('Ctrl Pts',(-22.035023317356,4.11621653725926,-8.41952646924223));
#45899=CARTESIAN_POINT('Ctrl Pts',(-22.0252072449018,4.11638702652465,-9.67504511381552));
#45900=CARTESIAN_POINT('Ctrl Pts',(-22.0195001493991,4.11626305230175,-10.551046327456));
#45901=CARTESIAN_POINT('Ctrl Pts',(-22.0166399907367,4.11616099750827,-11.0505806179339));
#45902=CARTESIAN_POINT('Ctrl Pts',(-22.0153552585612,4.11610556640313,-11.2999664615218));
#45903=CARTESIAN_POINT('Ctrl Pts',(-22.0144478134254,4.11606442341051,-11.4876435024608));
#45904=CARTESIAN_POINT('Ctrl Pts',(-22.0138540387184,4.11602448348753,-11.6140705917933));
#45905=CARTESIAN_POINT('Ctrl Pts',(-22.0127286463286,4.1158983005132,-11.8664185595357));
#45906=CARTESIAN_POINT('Ctrl Pts',(-22.0109169925421,4.11556438990738,-12.3073563182658));
#45907=CARTESIAN_POINT('Ctrl Pts',(-22.0078885129695,4.11451108817903,-13.1864755014533));
#45908=CARTESIAN_POINT('Ctrl Pts',(-22.0051097943091,4.11227698280468,-14.4369204185599));
#45909=CARTESIAN_POINT('Ctrl Pts',(-22.0040372306832,4.11030463130404,-15.5610660660364));
#45910=CARTESIAN_POINT('Ctrl Pts',(-22.0037316517172,4.10937886081918,-16.3122209837995));
#45911=CARTESIAN_POINT('Ctrl Pts',(-22.0036266412943,4.1088893913568,-16.8136025089925));
#45912=CARTESIAN_POINT('Ctrl Pts',(-22.0036438981547,4.10870264560642,-17.1904843263817));
#45913=CARTESIAN_POINT('Ctrl Pts',(-22.0036951917498,4.10867018543604,-17.504465564421));
#45914=CARTESIAN_POINT('Ctrl Pts',(-22.0037659889596,4.10864491725128,-17.6294775934659));
#45915=CARTESIAN_POINT('Ctrl Pts',(-22.0040932027344,4.10855121224841,-17.8791295662324));
#45916=CARTESIAN_POINT('Ctrl Pts',(-22.0046769151716,4.10840623448712,-18.128953820262));
#45917=CARTESIAN_POINT('Ctrl Pts',(-22.0054653914267,4.10822204803957,-18.3787349404948));
#45918=CARTESIAN_POINT('Ctrl Pts',(-22.0060346622479,4.10809664613784,-18.5348796170474));
#45919=CARTESIAN_POINT('Ctrl Pts',(-22.0065291810761,4.10799121967166,-18.6597981955137));
#45920=CARTESIAN_POINT('Ctrl Pts',(-22.0069183975559,4.10791064669469,-18.7534935134071));
#45921=CARTESIAN_POINT('Ctrl Pts',(-22.0072567799537,4.10784275398157,-18.8315762882781));
#45922=CARTESIAN_POINT('Ctrl Pts',(-22.0075349816406,4.10778802035585,-18.894045286408));
#45923=CARTESIAN_POINT('Ctrl Pts',(-22.0099407089767,4.10732251351153,-19.4250452507967));
#45924=CARTESIAN_POINT('Ctrl Pts',(-22.0158676273032,4.10658108446762,-20.4406319853658));
#45925=CARTESIAN_POINT('Ctrl Pts',(-22.0218521912948,4.1077345212265,-21.9424997642546));
#45926=CARTESIAN_POINT('Ctrl Pts',(-22.0200896140808,4.11183365881191,-22.9454014931823));
#45927=CARTESIAN_POINT('Ctrl Pts',(-22.0158233431142,4.11578937010123,-23.5710372694473));
#45928=CARTESIAN_POINT('Ctrl Pts',(-22.0137758059422,4.11755454093115,-23.8178873383974));
#45929=CARTESIAN_POINT('Ctrl Pts',(-22.0084421212236,4.12185513611334,-24.313458612243));
#45930=CARTESIAN_POINT('Ctrl Pts',(-21.996249555066,4.13108818609894,-25.183677492712));
#45931=CARTESIAN_POINT('Ctrl Pts',(-21.9731850864931,4.14778597539684,-26.435164267108));
#45932=CARTESIAN_POINT('Ctrl Pts',(-21.9439116701733,4.16816279907211,-27.9458140794481));
#45933=CARTESIAN_POINT('Ctrl Pts',(-21.9287075806292,4.17906693665825,-28.9567014536259));
#45934=CARTESIAN_POINT('Ctrl Pts',(-21.9227518086004,4.18345337480103,-29.5254560071513));
#45935=CARTESIAN_POINT('Ctrl Pts',(-21.9214223740837,4.18441027764442,-29.6505983758409));
#45936=CARTESIAN_POINT('Ctrl Pts',(-21.9187727102683,4.1863190461755,-29.9016929409507));
#45937=CARTESIAN_POINT('Ctrl Pts',(-21.9141834554257,4.1896264486792,-30.3410451571695));
#45938=CARTESIAN_POINT('Ctrl Pts',(-21.9053248870368,4.19600438719776,-31.2209681407571));
#45939=CARTESIAN_POINT('Ctrl Pts',(-21.8944820204112,4.20391937808385,-32.4800239120499));
#45940=CARTESIAN_POINT('Ctrl Pts',(-21.8883548098301,4.20881889042443,-33.7400425912776));
#45941=CARTESIAN_POINT('Ctrl Pts',(-21.887617639785,4.2100143207476,-34.7472698398653));
#45942=CARTESIAN_POINT('Ctrl Pts',(-21.8889042016303,4.20958736160925,-35.2505797237338));
#45943=CARTESIAN_POINT('Ctrl Pts',(-21.8905619685024,4.20881940597667,-35.6288061396665));
#45944=CARTESIAN_POINT('Ctrl Pts',(-21.8920068332931,4.20808942994181,-35.8828728206073));
#45945=CARTESIAN_POINT('Ctrl Pts',(-21.8961129240444,4.20589306531138,-36.3893572918887));
#45946=CARTESIAN_POINT('Ctrl Pts',(-21.9061707588451,4.20023175270841,-37.2737103685978));
#45947=CARTESIAN_POINT('Ctrl Pts',(-21.9349294377932,4.18375091830845,-39.0326417841188));
#45948=CARTESIAN_POINT('Ctrl Pts',(-21.9646241043132,4.16583014116949,-40.5339723279037));
#45949=CARTESIAN_POINT('Ctrl Pts',(-21.9813682042444,4.15557559944031,-41.7856626536357));
#45950=CARTESIAN_POINT('Ctrl Pts',(-21.9860152656383,4.1495633104421,-42.1793854201093));
#45951=CARTESIAN_POINT('Ctrl Pts',(-21.9917218274079,4.1383477020153,-42.6888104928429));
#45952=CARTESIAN_POINT('Ctrl Pts',(-21.9971702168111,4.12558636061383,-43.1977055694632));
#45953=CARTESIAN_POINT('Ctrl Pts',(-22.0036410011809,4.10815216686057,-43.8264437346378));
#45954=CARTESIAN_POINT('Ctrl Pts',(-22.0112963508797,4.08889718092569,-44.5712397154641));
#45955=CARTESIAN_POINT('Ctrl Pts',(-22.0179509165056,4.07749348765273,-45.1826267742738));
#45956=CARTESIAN_POINT('Ctrl Pts',(-22.0237023803601,4.07311486143883,-45.6657982945412));
#45957=CARTESIAN_POINT('Ctrl Pts',(-22.0282650992984,4.07260145483311,-46.0252489840544));
#45958=CARTESIAN_POINT('Ctrl Pts',(-22.0331340331778,4.07530161386567,-46.3816695806118));
#45959=CARTESIAN_POINT('Ctrl Pts',(-22.0401242868195,4.0837933675503,-46.8527419744537));
#45960=CARTESIAN_POINT('Ctrl Pts',(-22.0459496522703,4.09616001883859,-47.2013306630543));
#45961=CARTESIAN_POINT('Ctrl Pts',(-22.0523457940746,4.11353119813929,-47.5479470185623));
#45962=CARTESIAN_POINT('Ctrl Pts',(-22.0571608519188,4.12645431671799,-47.8028791297642));
#45963=CARTESIAN_POINT('Ctrl Pts',(-22.0685778662445,4.15244870291563,-48.296016830207));
#45964=CARTESIAN_POINT('Ctrl Pts',(-22.0923296902346,4.20194781231465,-49.1568596486614));
#45965=CARTESIAN_POINT('Ctrl Pts',(-22.1317430375304,4.29109922835001,-50.3567511143593));
#45966=CARTESIAN_POINT('Ctrl Pts',(-22.1713398710979,4.4542309928279,-51.7572733996303));
#45967=CARTESIAN_POINT('Ctrl Pts',(-22.181252446771,4.61655584852366,-52.6633750773003));
#45968=CARTESIAN_POINT('Ctrl Pts',(-22.1790138673735,4.7402119578729,-53.2236003657393));
#45969=CARTESIAN_POINT('Ctrl Pts',(-22.1773613312003,4.79340059150215,-53.4548939485341));
#45970=CARTESIAN_POINT('Ctrl Pts',(-22.1710616093439,4.90792124447746,-53.9173152546218));
#45971=CARTESIAN_POINT('Ctrl Pts',(-22.1532457320423,5.1306025270621,-54.7336427674677));
#45972=CARTESIAN_POINT('Ctrl Pts',(-22.097832810942,5.65648884714921,-56.3839152515343));
#45973=CARTESIAN_POINT('Ctrl Pts',(-22.0412804464425,6.22052514945947,-57.8189670582374));
#45974=CARTESIAN_POINT('Ctrl Pts',(-22.0189286249449,6.64905674783341,-58.8339790672758));
#45975=CARTESIAN_POINT('Ctrl Pts',(-22.0160598135343,6.6977875963569,-58.9478428819848));
#45976=CARTESIAN_POINT('Ctrl Pts',(-22.0104898930308,6.80055946754283,-59.1823098250968));
#45977=CARTESIAN_POINT('Ctrl Pts',(-22.0009046471323,6.98681000058887,-59.5929273377654));
#45978=CARTESIAN_POINT('Ctrl Pts',(-21.982673689945,7.38793968462431,-60.4275067502826));
#45979=CARTESIAN_POINT('Ctrl Pts',(-21.9642676050404,7.89731311453462,-61.4005064487699));
#45980=CARTESIAN_POINT('Ctrl Pts',(-21.9486371893967,8.4331972379869,-62.3874427884229));
#45981=CARTESIAN_POINT('Ctrl Pts',(-21.9409298355057,8.73956202027487,-62.9466873437175));
#45982=CARTESIAN_POINT('Ctrl Pts',(-21.9362778305471,8.94388529536134,-63.3210484177726));
#45983=CARTESIAN_POINT('Ctrl Pts',(-21.9333047699389,9.07997994977837,-63.5710250472529));
#45984=CARTESIAN_POINT('Ctrl Pts',(-21.9305422257701,9.21568664341698,-63.8215442929583));
#45985=CARTESIAN_POINT('Ctrl Pts',(-21.9283022575873,9.33374338713387,-64.0412705670625));
#45986=CARTESIAN_POINT('Ctrl Pts',(-21.9270760103423,9.40095793915379,-64.1669746443105));
#45987=CARTESIAN_POINT('Ctrl Pts',(-21.9252902074149,9.50149970378208,-64.355664476691));
#45988=CARTESIAN_POINT('Ctrl Pts',(-21.9239217402965,9.5846818151938,-64.5132321112613));
#45989=CARTESIAN_POINT('Ctrl Pts',(-21.9218097860302,9.72113866943812,-64.7742454997469));
#45990=CARTESIAN_POINT('Ctrl Pts',(-21.9199176222883,9.85377102502329,-65.0273934732946));
#45991=CARTESIAN_POINT('Ctrl Pts',(-21.9171231090912,10.122766700094,-65.5388654369393));
#45992=CARTESIAN_POINT('Ctrl Pts',(-21.914604314553,10.5891346610821,-66.4208834436944));
#45993=CARTESIAN_POINT('Ctrl Pts',(-21.9167516425982,11.518063809149,-68.1633649555777));
#45994=CARTESIAN_POINT('Ctrl Pts',(-21.9235258434315,12.3111662021817,-69.6409891056379));
#45995=CARTESIAN_POINT('Ctrl Pts',(-21.923595127208,12.9129986925668,-70.7726319617749));
#45996=CARTESIAN_POINT('Ctrl Pts',(-21.9236052602591,13.0463776976675,-71.0234454630726));
#45997=CARTESIAN_POINT('Ctrl Pts',(-21.9236212938625,13.3134462292093,-71.5256714763303));
#45998=CARTESIAN_POINT('Ctrl Pts',(-21.9236369455585,13.6469034947314,-72.1527626977125));
#45999=CARTESIAN_POINT('Ctrl Pts',(-21.9236407216763,14.0469291203077,-72.9050903947083));
#46000=CARTESIAN_POINT('Ctrl Pts',(-21.9236332599525,14.8465939166301,-74.4090732064259));
#46001=CARTESIAN_POINT('Ctrl Pts',(-21.9236258769294,15.5125217173332,-75.6615475097951));
#46002=CARTESIAN_POINT('Ctrl Pts',(-21.9236382256523,16.4822523474001,-77.4853125317373));
#46003=CARTESIAN_POINT('Ctrl Pts',(-21.9236445933878,16.9187529102801,-78.3062336744952));
#46004=CARTESIAN_POINT('Ctrl Pts',(-21.9236445933879,17.3552744976696,-79.1272113765938));
#46005=CARTESIAN_POINT('Ctrl Pts',(-19.4188565084394,4.07909071047731,24.8306335196013));
#46006=CARTESIAN_POINT('Ctrl Pts',(-19.4189144201637,4.07909071025974,24.7817541701314));
#46007=CARTESIAN_POINT('Ctrl Pts',(-19.4189751571496,4.0790907049392,24.7328758768994));
#46008=CARTESIAN_POINT('Ctrl Pts',(-19.4196923876615,4.07909087600898,24.1822672626248));
#46009=CARTESIAN_POINT('Ctrl Pts',(-19.4202407064515,4.07909166990852,23.1781304961313));
#46010=CARTESIAN_POINT('Ctrl Pts',(-19.4215160787714,4.07908986719448,21.1695310296501));
#46011=CARTESIAN_POINT('Ctrl Pts',(-19.426289339984,4.07909351817457,19.6653765872538));
#46012=CARTESIAN_POINT('Ctrl Pts',(-19.4364196794994,4.07909840105154,18.4143272842976));
#46013=CARTESIAN_POINT('Ctrl Pts',(-19.4412776063029,4.07910001848308,17.9115087189125));
#46014=CARTESIAN_POINT('Ctrl Pts',(-19.4534754210926,4.07910422482297,16.9075170749824));
#46015=CARTESIAN_POINT('Ctrl Pts',(-19.4796391806934,4.0791122270718,15.1537053608657));
#46016=CARTESIAN_POINT('Ctrl Pts',(-19.5045032710635,4.07913096690056,13.6519635683124));
#46017=CARTESIAN_POINT('Ctrl Pts',(-19.5201045959927,4.07914726620125,12.3974942144212));
#46018=CARTESIAN_POINT('Ctrl Pts',(-19.5264842586753,4.07915434258511,11.896542204204));
#46019=CARTESIAN_POINT('Ctrl Pts',(-19.5394958902427,4.07916874348645,10.8947012600692));
#46020=CARTESIAN_POINT('Ctrl Pts',(-19.5555899316981,4.07919772714864,9.64217422998216));
#46021=CARTESIAN_POINT('Ctrl Pts',(-19.5725737761371,4.07922586275185,8.13767545606689));
#46022=CARTESIAN_POINT('Ctrl Pts',(-19.5809711503705,4.07925222390256,7.13297024095191));
#46023=CARTESIAN_POINT('Ctrl Pts',(-19.5848728343503,4.07926169557044,6.50497879949647));
#46024=CARTESIAN_POINT('Ctrl Pts',(-19.5864491654674,4.0792439713941,6.25448301513597));
#46025=CARTESIAN_POINT('Ctrl Pts',(-19.5896190891136,4.07913977975641,5.75307864744289));
#46026=CARTESIAN_POINT('Ctrl Pts',(-19.5950152883982,4.07882488805074,4.8743156679763));
#46027=CARTESIAN_POINT('Ctrl Pts',(-19.6036496630048,4.07796294666085,3.11429706875541));
#46028=CARTESIAN_POINT('Ctrl Pts',(-19.6019882907535,4.07803371099858,1.6093259597056));
#46029=CARTESIAN_POINT('Ctrl Pts',(-19.5914809645,4.07953662306137,0.55191876525641));
#46030=CARTESIAN_POINT('Ctrl Pts',(-19.5901156534471,4.07973084939819,0.426115855158161));
#46031=CARTESIAN_POINT('Ctrl Pts',(-19.5869560461142,4.08018266915907,0.174592789548162));
#46032=CARTESIAN_POINT('Ctrl Pts',(-19.5803692316278,4.08112680912326,-0.2651329658887));
#46033=CARTESIAN_POINT('Ctrl Pts',(-19.5683254774567,4.08287488315803,-0.892339759225695));
#46034=CARTESIAN_POINT('Ctrl Pts',(-19.5508973207309,4.08537642564393,-1.64387354498816));
#46035=CARTESIAN_POINT('Ctrl Pts',(-19.5253228951273,4.08905894197638,-2.64510896972974));
#46036=CARTESIAN_POINT('Ctrl Pts',(-19.4920303955031,4.09375623345862,-3.89635263559461));
#46037=CARTESIAN_POINT('Ctrl Pts',(-19.4705336110349,4.09651502910892,-4.89961645688803));
#46038=CARTESIAN_POINT('Ctrl Pts',(-19.4608138031559,4.09751505218955,-5.52819109994924));
#46039=CARTESIAN_POINT('Ctrl Pts',(-19.4570673380576,4.09787183139317,-5.77948023960965));
#46040=CARTESIAN_POINT('Ctrl Pts',(-19.4500850879881,4.09840732325652,-6.2824257765495));
#46041=CARTESIAN_POINT('Ctrl Pts',(-19.4391418185303,4.09894170854077,-7.16281346606619));
#46042=CARTESIAN_POINT('Ctrl Pts',(-19.4266986568119,4.09882741407656,-8.42044957381485));
#46043=CARTESIAN_POINT('Ctrl Pts',(-19.4173000333354,4.09830972651637,-9.6751036262812));
#46044=CARTESIAN_POINT('Ctrl Pts',(-19.411683681216,4.09813931643307,-10.550346813374));
#46045=CARTESIAN_POINT('Ctrl Pts',(-19.4086593216313,4.09815973988217,-11.049410070983));
#46046=CARTESIAN_POINT('Ctrl Pts',(-19.4071935988682,4.09821928491534,-11.2985484047833));
#46047=CARTESIAN_POINT('Ctrl Pts',(-19.4061016703888,4.09828621552437,-11.4860268244713));
#46048=CARTESIAN_POINT('Ctrl Pts',(-19.4053889610689,4.09833451669103,-11.6120758387663));
#46049=CARTESIAN_POINT('Ctrl Pts',(-19.4040478993421,4.09844474528975,-11.8638542487384));
#46050=CARTESIAN_POINT('Ctrl Pts',(-19.4019142713054,4.09867082756035,-12.3038372498591));
#46051=CARTESIAN_POINT('Ctrl Pts',(-19.3984419752592,4.09923523312725,-13.1815572929444));
#46052=CARTESIAN_POINT('Ctrl Pts',(-19.3954236776363,4.10022022112895,-14.4313183962024));
#46053=CARTESIAN_POINT('Ctrl Pts',(-19.3942430125099,4.10101548245803,-15.5564931439516));
#46054=CARTESIAN_POINT('Ctrl Pts',(-19.3937611428457,4.10138097884389,-16.3090052985942));
#46055=CARTESIAN_POINT('Ctrl Pts',(-19.3934990598768,4.10157134265437,-16.8114637197718));
#46056=CARTESIAN_POINT('Ctrl Pts',(-19.3933453844142,4.10164968431484,-17.1893673535936));
#46057=CARTESIAN_POINT('Ctrl Pts',(-19.3932120541238,4.10166468090102,-17.5042559018109));
#46058=CARTESIAN_POINT('Ctrl Pts',(-19.3931882586075,4.10167787745367,-17.6286958130394));
#46059=CARTESIAN_POINT('Ctrl Pts',(-19.3932482448541,4.10172972165035,-17.8778588266014));
#46060=CARTESIAN_POINT('Ctrl Pts',(-19.393458056388,4.10181608223137,-18.1271358502433));
#46061=CARTESIAN_POINT('Ctrl Pts',(-19.3937911139831,4.10192414140768,-18.3766235315614));
#46062=CARTESIAN_POINT('Ctrl Pts',(-19.3940459177017,4.10199930922547,-18.532621742218));
#46063=CARTESIAN_POINT('Ctrl Pts',(-19.3942743151561,4.10206229662538,-18.6574686311859));
#46064=CARTESIAN_POINT('Ctrl Pts',(-19.3944572207307,4.10211079231994,-18.7511261562));
#46065=CARTESIAN_POINT('Ctrl Pts',(-19.3946186656907,4.10215198667377,-18.8291937325066));
#46066=CARTESIAN_POINT('Ctrl Pts',(-19.3947527847797,4.10218516304723,-18.8916592729327));
#46067=CARTESIAN_POINT('Ctrl Pts',(-19.3959200298335,4.10246849959459,-19.422682847279));
#46068=CARTESIAN_POINT('Ctrl Pts',(-19.3990121909925,4.10306965440659,-20.4400186150423));
#46069=CARTESIAN_POINT('Ctrl Pts',(-19.4026974986641,4.10265013343473,-21.9490122710558));
#46070=CARTESIAN_POINT('Ctrl Pts',(-19.4025081334354,4.1006829999806,-22.959760455145));
#46071=CARTESIAN_POINT('Ctrl Pts',(-19.4008678069037,4.09862369634203,-23.5912798455614));
#46072=CARTESIAN_POINT('Ctrl Pts',(-19.4000563059062,4.09769125775524,-23.8416787264623));
#46073=CARTESIAN_POINT('Ctrl Pts',(-19.3978729269907,4.09541369523697,-24.3427273431573));
#46074=CARTESIAN_POINT('Ctrl Pts',(-19.3927666416296,4.09048021303807,-25.2208302452691));
#46075=CARTESIAN_POINT('Ctrl Pts',(-19.382960522823,4.08155628938632,-26.4773520158594));
#46076=CARTESIAN_POINT('Ctrl Pts',(-19.3706483773465,4.0703783508801,-27.9846482869812));
#46077=CARTESIAN_POINT('Ctrl Pts',(-19.3645265659457,4.06445530686772,-28.9867106559561));
#46078=CARTESIAN_POINT('Ctrl Pts',(-19.3623143059621,4.06204892202967,-29.5487718058104));
#46079=CARTESIAN_POINT('Ctrl Pts',(-19.3617887426652,4.06152821541918,-29.6739785277925));
#46080=CARTESIAN_POINT('Ctrl Pts',(-19.3606271661027,4.06052591044494,-29.924295428993));
#46081=CARTESIAN_POINT('Ctrl Pts',(-19.3583456092779,4.05887871158711,-30.3626493341679));
#46082=CARTESIAN_POINT('Ctrl Pts',(-19.3531065570849,4.05597509268942,-31.2399346833751));
#46083=CARTESIAN_POINT('Ctrl Pts',(-19.3455509589286,4.05277684067842,-32.4945228341436));
#46084=CARTESIAN_POINT('Ctrl Pts',(-19.342886321836,4.05050865357068,-33.7487538153502));
#46085=CARTESIAN_POINT('Ctrl Pts',(-19.3466959544024,4.04908784624401,-34.7506312934264));
#46086=CARTESIAN_POINT('Ctrl Pts',(-19.3510933821798,4.04847947531361,-35.2509902487381));
#46087=CARTESIAN_POINT('Ctrl Pts',(-19.3555228250233,4.04805620740768,-35.6268907199721));
#46088=CARTESIAN_POINT('Ctrl Pts',(-19.3590680438941,4.04775668024797,-35.8791435250017));
#46089=CARTESIAN_POINT('Ctrl Pts',(-19.36816067504,4.04710559137667,-36.382362044537));
#46090=CARTESIAN_POINT('Ctrl Pts',(-19.3886133016165,4.04585131481258,-37.2613946857405));
#46091=CARTESIAN_POINT('Ctrl Pts',(-19.4419700485823,4.04379142196048,-39.0119443279322));
#46092=CARTESIAN_POINT('Ctrl Pts',(-19.4897443702684,4.04450815238889,-40.5099559810813));
#46093=CARTESIAN_POINT('Ctrl Pts',(-19.5092037083466,4.04898130135962,-41.7616588739113));
#46094=CARTESIAN_POINT('Ctrl Pts',(-19.5141254539957,4.04751785876212,-42.1556346767663));
#46095=CARTESIAN_POINT('Ctrl Pts',(-19.519258397388,4.04216514831402,-42.6647192527348));
#46096=CARTESIAN_POINT('Ctrl Pts',(-19.5235371682125,4.03534398895192,-43.173000899783));
#46097=CARTESIAN_POINT('Ctrl Pts',(-19.5274942672393,4.0254984979779,-43.8003461392944));
#46098=CARTESIAN_POINT('Ctrl Pts',(-19.5306677744146,4.01601169365967,-44.5425023123782));
#46099=CARTESIAN_POINT('Ctrl Pts',(-19.5325488160087,4.01356414554306,-45.1508563034701));
#46100=CARTESIAN_POINT('Ctrl Pts',(-19.5339462963064,4.01691209593236,-45.6311767756409));
#46101=CARTESIAN_POINT('Ctrl Pts',(-19.5350135354646,4.0225413178937,-45.988244691636));
#46102=CARTESIAN_POINT('Ctrl Pts',(-19.5361832905115,4.03175746973702,-46.3420566735754));
#46103=CARTESIAN_POINT('Ctrl Pts',(-19.537995792819,4.04944337200258,-46.8093552824749));
#46104=CARTESIAN_POINT('Ctrl Pts',(-19.5397356363166,4.06940154039066,-47.1547886134318));
#46105=CARTESIAN_POINT('Ctrl Pts',(-19.5419182619491,4.09479685435151,-47.4979406828226));
#46106=CARTESIAN_POINT('Ctrl Pts',(-19.5435334867921,4.1138493185823,-47.7456057168678));
#46107=CARTESIAN_POINT('Ctrl Pts',(-19.5472777159859,4.15410363555502,-48.2292431210855));
#46108=CARTESIAN_POINT('Ctrl Pts',(-19.5548283176533,4.23316883664525,-49.0770214660487));
#46109=CARTESIAN_POINT('Ctrl Pts',(-19.5665014862628,4.37257037850929,-50.273815532423));
#46110=CARTESIAN_POINT('Ctrl Pts',(-19.5759347453678,4.59321970380592,-51.6928488604303));
#46111=CARTESIAN_POINT('Ctrl Pts',(-19.5753145264093,4.78270750833221,-52.6256970027234));
#46112=CARTESIAN_POINT('Ctrl Pts',(-19.5717048935925,4.91701513352802,-53.2063435376452));
#46113=CARTESIAN_POINT('Ctrl Pts',(-19.5698774486865,4.97335057603374,-53.4432071091416));
#46114=CARTESIAN_POINT('Ctrl Pts',(-19.564839020945,5.09200111043759,-53.9168187775379));
#46115=CARTESIAN_POINT('Ctrl Pts',(-19.5528544887985,5.315862262297,-54.7488188928104));
#46116=CARTESIAN_POINT('Ctrl Pts',(-19.519714948239,5.82468467822303,-56.4189019825902));
#46117=CARTESIAN_POINT('Ctrl Pts',(-19.4875512323991,6.35507020672527,-57.8515777580455));
#46118=CARTESIAN_POINT('Ctrl Pts',(-19.4739216276912,6.76494875051892,-58.8574606822304));
#46119=CARTESIAN_POINT('Ctrl Pts',(-19.4722267612937,6.81250672350762,-58.9726691727967));
#46120=CARTESIAN_POINT('Ctrl Pts',(-19.4689282701839,6.91201454254276,-59.2082470192108));
#46121=CARTESIAN_POINT('Ctrl Pts',(-19.4633090465908,7.09221172375984,-59.6210873424176));
#46122=CARTESIAN_POINT('Ctrl Pts',(-19.4527741824522,7.47861963072649,-60.4579968506153));
#46123=CARTESIAN_POINT('Ctrl Pts',(-19.4424270794853,7.96727305279303,-61.4310058399773));
#46124=CARTESIAN_POINT('Ctrl Pts',(-19.4337880037515,8.4815689226549,-62.415404281155));
#46125=CARTESIAN_POINT('Ctrl Pts',(-19.42955639736,8.77612817315247,-62.9723177505061));
#46126=CARTESIAN_POINT('Ctrl Pts',(-19.4269982550432,8.97296445687754,-63.3446966839675));
#46127=CARTESIAN_POINT('Ctrl Pts',(-19.4253615222896,9.10419333608518,-63.5932357054671));
#46128=CARTESIAN_POINT('Ctrl Pts',(-19.423833517323,9.2352300133487,-63.8421327758543));
#46129=CARTESIAN_POINT('Ctrl Pts',(-19.422586985817,9.34943527202489,-64.0602672270396));
#46130=CARTESIAN_POINT('Ctrl Pts',(-19.421901420598,9.41452027800235,-64.18500938873));
#46131=CARTESIAN_POINT('Ctrl Pts',(-19.4208996084222,9.51194377766199,-64.3722033831314));
#46132=CARTESIAN_POINT('Ctrl Pts',(-19.420122800325,9.59268180683019,-64.5284065828826));
#46133=CARTESIAN_POINT('Ctrl Pts',(-19.4189102932834,9.72535993830748,-64.7870027589046));
#46134=CARTESIAN_POINT('Ctrl Pts',(-19.417812089868,9.85477348590642,-65.0381168227013));
#46135=CARTESIAN_POINT('Ctrl Pts',(-19.4161674651852,10.1184235473867,-65.5456921147163));
#46136=CARTESIAN_POINT('Ctrl Pts',(-19.4145954672988,10.5786112295253,-66.4220152425714));
#46137=CARTESIAN_POINT('Ctrl Pts',(-19.4154119518332,11.5053109976952,-68.1572980681037));
#46138=CARTESIAN_POINT('Ctrl Pts',(-19.4188586142071,12.3063044713339,-69.6365282019122));
#46139=CARTESIAN_POINT('Ctrl Pts',(-19.4187886877509,12.9106168296157,-70.7731110993884));
#46140=CARTESIAN_POINT('Ctrl Pts',(-19.4187743904881,13.0437826002373,-71.0235704261403));
#46141=CARTESIAN_POINT('Ctrl Pts',(-19.4187532716427,13.3108824368978,-71.5259270802934));
#46142=CARTESIAN_POINT('Ctrl Pts',(-19.4187412531874,13.6442196591592,-72.1528487987563));
#46143=CARTESIAN_POINT('Ctrl Pts',(-19.4187406843765,14.0442371429415,-72.9051710091742));
#46144=CARTESIAN_POINT('Ctrl Pts',(-19.4187613474451,14.8438780416534,-74.4090580694602));
#46145=CARTESIAN_POINT('Ctrl Pts',(-19.4188107046995,15.5098573501397,-75.6615328720702));
#46146=CARTESIAN_POINT('Ctrl Pts',(-19.4188153389072,16.4796045062356,-77.4853508948796));
#46147=CARTESIAN_POINT('Ctrl Pts',(-19.4188177230362,16.9160785638965,-78.3062334798541));
#46148=CARTESIAN_POINT('Ctrl Pts',(-19.4188177230362,17.3526001512859,-79.1272111819523));
#46149=CARTESIAN_POINT('Ctrl Pts',(-16.9146734095705,4.07920360686077,24.830633653217));
#46150=CARTESIAN_POINT('Ctrl Pts',(-16.9147239272192,4.07920356885915,24.78175430811));
#46151=CARTESIAN_POINT('Ctrl Pts',(-16.9147769162984,4.0792035341183,24.7328759880602));
#46152=CARTESIAN_POINT('Ctrl Pts',(-16.9154023366309,4.07920289336669,24.1822684761053));
#46153=CARTESIAN_POINT('Ctrl Pts',(-16.9158796858389,4.07920058846839,23.1781406679383));
#46154=CARTESIAN_POINT('Ctrl Pts',(-16.9169949468356,4.07919802534268,21.1695421788302));
#46155=CARTESIAN_POINT('Ctrl Pts',(-16.9211539003465,4.07919142487426,19.6654092661205));
#46156=CARTESIAN_POINT('Ctrl Pts',(-16.9299836755634,4.07918594088012,18.4143692135952));
#46157=CARTESIAN_POINT('Ctrl Pts',(-16.9342190088254,4.07918359559448,17.911552167174));
#46158=CARTESIAN_POINT('Ctrl Pts',(-16.944853731395,4.0791769820853,16.9075667994273));
#46159=CARTESIAN_POINT('Ctrl Pts',(-16.9676658429407,4.07916395102957,15.1537619834732));
#46160=CARTESIAN_POINT('Ctrl Pts',(-16.9893295738655,4.07914805388708,13.6520698339233));
#46161=CARTESIAN_POINT('Ctrl Pts',(-17.0029134267273,4.07914506892092,12.3976233718372));
#46162=CARTESIAN_POINT('Ctrl Pts',(-17.0084672384419,4.07914475479534,11.8966774963043));
#46163=CARTESIAN_POINT('Ctrl Pts',(-17.0197930215528,4.07914818539066,10.8948438791706));
#46164=CARTESIAN_POINT('Ctrl Pts',(-17.0337871110875,4.07914865402405,9.64235194184012));
#46165=CARTESIAN_POINT('Ctrl Pts',(-17.0485553653208,4.07915702810575,8.13790849406833));
#46166=CARTESIAN_POINT('Ctrl Pts',(-17.0558421657869,4.07915203742613,7.13321404971454));
#46167=CARTESIAN_POINT('Ctrl Pts',(-17.0592306979639,4.07915243507481,6.50537190516661));
#46168=CARTESIAN_POINT('Ctrl Pts',(-17.0608323426246,4.07937877383712,6.2580752164868));
#46169=CARTESIAN_POINT('Ctrl Pts',(-17.0648048542448,4.08056269253945,5.76013765874217));
#46170=CARTESIAN_POINT('Ctrl Pts',(-17.073138987226,4.08411724516116,4.88575206743614));
#46171=CARTESIAN_POINT('Ctrl Pts',(-17.0903689206984,4.09355139007925,3.12310947319482));
#46172=CARTESIAN_POINT('Ctrl Pts',(-17.0888209075592,4.09356162540644,1.59817064052181));
#46173=CARTESIAN_POINT('Ctrl Pts',(-17.0638392445282,4.07800224041429,0.517411790217176));
#46174=CARTESIAN_POINT('Ctrl Pts',(-17.0605983359294,4.07597591758405,0.387514432140873));
#46175=CARTESIAN_POINT('Ctrl Pts',(-17.0531021045699,4.07129525632049,0.129079376660313));
#46176=CARTESIAN_POINT('Ctrl Pts',(-17.0374966370187,4.0615425736139,-0.321907681662813));
#46177=CARTESIAN_POINT('Ctrl Pts',(-17.0090210424416,4.04369114790545,-0.961387761059511));
#46178=CARTESIAN_POINT('Ctrl Pts',(-16.9681086459772,4.01780806705043,-1.72194422763307));
#46179=CARTESIAN_POINT('Ctrl Pts',(-16.908583693265,3.97976448878331,-2.72744523146189));
#46180=CARTESIAN_POINT('Ctrl Pts',(-16.8327228434125,3.93040577419916,-3.96971456218046));
#46181=CARTESIAN_POINT('Ctrl Pts',(-16.7866766418018,3.90033598244312,-4.95111724077728));
#46182=CARTESIAN_POINT('Ctrl Pts',(-16.7675066186055,3.88833732536696,-5.56177000535768));
#46183=CARTESIAN_POINT('Ctrl Pts',(-16.7603205981865,3.88388173809189,-5.80991553107169));
#46184=CARTESIAN_POINT('Ctrl Pts',(-16.7477446490098,3.87636163463991,-6.3051397414101));
#46185=CARTESIAN_POINT('Ctrl Pts',(-16.7300208455842,3.86649997340302,-7.17503824389738));
#46186=CARTESIAN_POINT('Ctrl Pts',(-16.7146210384598,3.86009960228098,-8.42235446624796));
#46187=CARTESIAN_POINT('Ctrl Pts',(-16.7063299309972,3.85895696124205,-9.67406515743436));
#46188=CARTESIAN_POINT('Ctrl Pts',(-16.7010623786273,3.85823357875107,-10.5508147844575));
#46189=CARTESIAN_POINT('Ctrl Pts',(-16.6977378741451,3.85745234181625,-11.0518219182477));
#46190=CARTESIAN_POINT('Ctrl Pts',(-16.6958938377715,3.85687410082937,-11.3022954189243));
#46191=CARTESIAN_POINT('Ctrl Pts',(-16.6944082136604,3.85634386019955,-11.4908747518974));
#46192=CARTESIAN_POINT('Ctrl Pts',(-16.6934391066798,3.85601265813483,-11.6162364634123));
#46193=CARTESIAN_POINT('Ctrl Pts',(-16.6916127399259,3.85544149913119,-11.867480742801));
#46194=CARTESIAN_POINT('Ctrl Pts',(-16.6887003015182,3.85467069657949,-12.3062120146968));
#46195=CARTESIAN_POINT('Ctrl Pts',(-16.6839294279526,3.85394295505111,-13.1820737698753));
#46196=CARTESIAN_POINT('Ctrl Pts',(-16.6797255183182,3.8546942229523,-14.4300495819467));
#46197=CARTESIAN_POINT('Ctrl Pts',(-16.6780423749029,3.85617929848326,-15.5549559973584));
#46198=CARTESIAN_POINT('Ctrl Pts',(-16.6773678851618,3.8569475200662,-16.3077964022937));
#46199=CARTESIAN_POINT('Ctrl Pts',(-16.6770114378945,3.85736444136179,-16.8106178945354));
#46200=CARTESIAN_POINT('Ctrl Pts',(-16.6768069891574,3.8575226412861,-17.1889465823843));
#46201=CARTESIAN_POINT('Ctrl Pts',(-16.6766437114414,3.85752565497502,-17.5042654103635));
#46202=CARTESIAN_POINT('Ctrl Pts',(-16.6765941790477,3.85753490940607,-17.6286496634979));
#46203=CARTESIAN_POINT('Ctrl Pts',(-16.676553307684,3.85758249987073,-17.8778326479976));
#46204=CARTESIAN_POINT('Ctrl Pts',(-16.6765944303759,3.85766789456493,-18.1270789699173));
#46205=CARTESIAN_POINT('Ctrl Pts',(-16.6767149275073,3.85778279386269,-18.3765614210905));
#46206=CARTESIAN_POINT('Ctrl Pts',(-16.6768209495527,3.85786444593357,-18.5325500358368));
#46207=CARTESIAN_POINT('Ctrl Pts',(-16.6769240126647,3.85793466997555,-18.6573913142302));
#46208=CARTESIAN_POINT('Ctrl Pts',(-16.6770100315899,3.85798940704359,-18.7510439476394));
#46209=CARTESIAN_POINT('Ctrl Pts',(-16.6770888212736,3.85803649701773,-18.8291075849918));
#46210=CARTESIAN_POINT('Ctrl Pts',(-16.6771561255174,3.85807492954543,-18.8915698592054));
#46211=CARTESIAN_POINT('Ctrl Pts',(-16.6777514591514,3.85840532900616,-19.4225653497714));
#46212=CARTESIAN_POINT('Ctrl Pts',(-16.6795788425869,3.85912931741145,-20.4398404028269));
#46213=CARTESIAN_POINT('Ctrl Pts',(-16.6836451022944,3.8592636505166,-21.9487053700047));
#46214=CARTESIAN_POINT('Ctrl Pts',(-16.686670540002,3.85786544788114,-22.9593455552285));
#46215=CARTESIAN_POINT('Ctrl Pts',(-16.6885257593456,3.85628204344558,-23.5907847375866));
#46216=CARTESIAN_POINT('Ctrl Pts',(-16.6893050970785,3.85555855841181,-23.8410988560408));
#46217=CARTESIAN_POINT('Ctrl Pts',(-16.6910099656135,3.85377419173882,-24.3420261589137));
#46218=CARTESIAN_POINT('Ctrl Pts',(-16.6943343835605,3.84988498908126,-25.2199567032052));
#46219=CARTESIAN_POINT('Ctrl Pts',(-16.6997260151302,3.84281878110687,-26.4763414811346));
#46220=CARTESIAN_POINT('Ctrl Pts',(-16.7063745797174,3.83412124678864,-27.9837612304857));
#46221=CARTESIAN_POINT('Ctrl Pts',(-16.7102487178192,3.82957501937168,-28.9859581556077));
#46222=CARTESIAN_POINT('Ctrl Pts',(-16.7121190144433,3.82776231710041,-29.5483117409518));
#46223=CARTESIAN_POINT('Ctrl Pts',(-16.7124390843753,3.8272861697604,-29.6752367072504));
#46224=CARTESIAN_POINT('Ctrl Pts',(-16.7127211941321,3.82611062581586,-29.9277638206352));
#46225=CARTESIAN_POINT('Ctrl Pts',(-16.712372166923,3.82351988117654,-30.3697764617688));
#46226=CARTESIAN_POINT('Ctrl Pts',(-16.7090563975436,3.81676731864626,-31.2512803990046));
#46227=CARTESIAN_POINT('Ctrl Pts',(-16.7011820320115,3.80576715739035,-32.504239566492));
#46228=CARTESIAN_POINT('Ctrl Pts',(-16.7005638350862,3.80132834083306,-33.7463250851312));
#46229=CARTESIAN_POINT('Ctrl Pts',(-16.7112561468823,3.80667288732683,-34.7322118103997));
#46230=CARTESIAN_POINT('Ctrl Pts',(-16.7214848608452,3.81311635167405,-35.2223970544754));
#46231=CARTESIAN_POINT('Ctrl Pts',(-16.731439234743,3.8196556960259,-35.5897483194025));
#46232=CARTESIAN_POINT('Ctrl Pts',(-16.7392623374465,3.82483202377554,-35.8335364392361));
#46233=CARTESIAN_POINT('Ctrl Pts',(-16.7589744320517,3.83802309018381,-36.3235593738663));
#46234=CARTESIAN_POINT('Ctrl Pts',(-16.8026965129352,3.86750392921385,-37.1835674124926));
#46235=CARTESIAN_POINT('Ctrl Pts',(-16.9147604342526,3.94311926201518,-38.9174593726877));
#46236=CARTESIAN_POINT('Ctrl Pts',(-17.0108408419884,4.00831363951242,-40.4386822878126));
#46237=CARTESIAN_POINT('Ctrl Pts',(-17.0428387141216,4.03597245536776,-41.7311804966786));
#46238=CARTESIAN_POINT('Ctrl Pts',(-17.0502703194235,4.0401683438514,-42.1300884229979));
#46239=CARTESIAN_POINT('Ctrl Pts',(-17.0566388284558,4.03976300543393,-42.6475183153195));
#46240=CARTESIAN_POINT('Ctrl Pts',(-17.0608900330414,4.03653857718181,-43.1624867273373));
#46241=CARTESIAN_POINT('Ctrl Pts',(-17.0626425437171,4.02893033341949,-43.7968719369589));
#46242=CARTESIAN_POINT('Ctrl Pts',(-17.0604043454077,4.01967372408898,-44.5446528351534));
#46243=CARTESIAN_POINT('Ctrl Pts',(-17.0560465675541,4.01620165395783,-45.1555878484918));
#46244=CARTESIAN_POINT('Ctrl Pts',(-17.0516948081744,4.0183894712776,-45.6366450360375));
#46245=CARTESIAN_POINT('Ctrl Pts',(-17.0481868260204,4.02311208554269,-45.9936189369653));
#46246=CARTESIAN_POINT('Ctrl Pts',(-17.0446004597252,4.03148077372419,-46.3466764435411));
#46247=CARTESIAN_POINT('Ctrl Pts',(-17.0399245092123,4.04822086533075,-46.8121131557728));
#46248=CARTESIAN_POINT('Ctrl Pts',(-17.0368366978271,4.06787393045612,-47.1551568300095));
#46249=CARTESIAN_POINT('Ctrl Pts',(-17.0343068286104,4.09333570883227,-47.4953825531079));
#46250=CARTESIAN_POINT('Ctrl Pts',(-17.0323684226327,4.11260883491083,-47.7444525481771));
#46251=CARTESIAN_POINT('Ctrl Pts',(-17.027621205699,4.15295468238058,-48.2288090773729));
#46252=CARTESIAN_POINT('Ctrl Pts',(-17.017323823215,4.23179762527297,-49.0783707505405));
#46253=CARTESIAN_POINT('Ctrl Pts',(-16.9986226932743,4.37015641608352,-50.2759118463673));
#46254=CARTESIAN_POINT('Ctrl Pts',(-16.974839604241,4.58949006108651,-51.6943299428451));
#46255=CARTESIAN_POINT('Ctrl Pts',(-16.9615417398334,4.77851385430702,-52.6257397035579));
#46256=CARTESIAN_POINT('Ctrl Pts',(-16.954964164518,4.91266531028849,-53.2053103446949));
#46257=CARTESIAN_POINT('Ctrl Pts',(-16.9523001823878,4.96899968854369,-53.4420760996642));
#46258=CARTESIAN_POINT('Ctrl Pts',(-16.9470116768378,5.08761857516938,-53.9153594023399));
#46259=CARTESIAN_POINT('Ctrl Pts',(-16.9379222492454,5.31147588450487,-54.7470295920851));
#46260=CARTESIAN_POINT('Ctrl Pts',(-16.920927864664,5.82039604793575,-56.4168686594285));
#46261=CARTESIAN_POINT('Ctrl Pts',(-16.9102911907989,6.35114099148479,-57.8500060872888));
#46262=CARTESIAN_POINT('Ctrl Pts',(-16.9065358465525,6.76139515416387,-58.8561565137549));
#46263=CARTESIAN_POINT('Ctrl Pts',(-16.9061445217287,6.80895991225671,-58.9713364239509));
#46264=CARTESIAN_POINT('Ctrl Pts',(-16.90550255376,6.90851827002603,-59.2069006559096));
#46265=CARTESIAN_POINT('Ctrl Pts',(-16.9047646267965,7.08881899845472,-59.6197202484487));
#46266=CARTESIAN_POINT('Ctrl Pts',(-16.9046305846275,7.47557253268014,-60.4566671436843));
#46267=CARTESIAN_POINT('Ctrl Pts',(-16.9067386267066,7.96483632081048,-61.4297876094401));
#46268=CARTESIAN_POINT('Ctrl Pts',(-16.9096057624689,8.47990584339476,-62.4143366719387));
#46269=CARTESIAN_POINT('Ctrl Pts',(-16.911225990679,8.77492881447765,-62.9713548920425));
#46270=CARTESIAN_POINT('Ctrl Pts',(-16.9121898023996,8.97207021405464,-63.3438190469933));
#46271=CARTESIAN_POINT('Ctrl Pts',(-16.912794811064,9.1035031542903,-63.5924195313673));
#46272=CARTESIAN_POINT('Ctrl Pts',(-16.9133261407537,9.23473080571758,-63.8413848735041));
#46273=CARTESIAN_POINT('Ctrl Pts',(-16.9137109132029,9.34910125829025,-64.0595880294941));
#46274=CARTESIAN_POINT('Ctrl Pts',(-16.9139041360755,9.41427802137335,-64.1843721158538));
#46275=CARTESIAN_POINT('Ctrl Pts',(-16.9141661003506,9.5118369834402,-64.3716318601805));
#46276=CARTESIAN_POINT('Ctrl Pts',(-16.9143206201335,9.59267662726585,-64.5278947897286));
#46277=CARTESIAN_POINT('Ctrl Pts',(-16.9144796684479,9.72551688476094,-64.786600053596));
#46278=CARTESIAN_POINT('Ctrl Pts',(-16.9146214511875,9.85505637385379,-65.0377894321718));
#46279=CARTESIAN_POINT('Ctrl Pts',(-16.914834479387,10.1189220825822,-65.545521407322));
#46280=CARTESIAN_POINT('Ctrl Pts',(-16.9150312999542,10.5793317586482,-66.4220661365077));
#46281=CARTESIAN_POINT('Ctrl Pts',(-16.914926439779,11.5060543253365,-68.1576437448239));
#46282=CARTESIAN_POINT('Ctrl Pts',(-16.9144808086033,12.3066091050813,-69.6367687451921));
#46283=CARTESIAN_POINT('Ctrl Pts',(-16.914488061616,12.9107783194121,-70.7731245831863));
#46284=CARTESIAN_POINT('Ctrl Pts',(-16.9144905361333,13.0439496335314,-71.0235966846109));
#46285=CARTESIAN_POINT('Ctrl Pts',(-16.9144939206435,13.3110413128027,-71.5259434402883));
#46286=CARTESIAN_POINT('Ctrl Pts',(-16.9144943255004,13.6443733781517,-72.1528660310182));
#46287=CARTESIAN_POINT('Ctrl Pts',(-16.9144936325431,14.0443864387566,-72.9051840662007));
#46288=CARTESIAN_POINT('Ctrl Pts',(-16.9144883889213,14.8440237580498,-74.4090689669014));
#46289=CARTESIAN_POINT('Ctrl Pts',(-16.9144733780915,15.5099868122522,-75.661536888092));
#46290=CARTESIAN_POINT('Ctrl Pts',(-16.9144688934797,16.4797239446511,-77.485353891126));
#46291=CARTESIAN_POINT('Ctrl Pts',(-16.9144665841287,16.9161914735935,-78.3062333820799));
#46292=CARTESIAN_POINT('Ctrl Pts',(-16.9144665841287,17.3527130609829,-79.1272110841781));
#46293=CARTESIAN_POINT('Ctrl Pts',(-15.0355537871551,4.07980364542041,24.8306344346923));
#46294=CARTESIAN_POINT('Ctrl Pts',(-15.0355987159917,4.0798036226416,24.7817551132038));
#46295=CARTESIAN_POINT('Ctrl Pts',(-15.0356458337054,4.07980358298019,24.732876760882));
#46296=CARTESIAN_POINT('Ctrl Pts',(-15.0362023699372,4.07980383215307,24.1822714211911));
#46297=CARTESIAN_POINT('Ctrl Pts',(-15.0366296099556,4.07980792182674,23.1781597882922));
#46298=CARTESIAN_POINT('Ctrl Pts',(-15.0376222054118,4.07980751034299,21.1695635006398));
#46299=CARTESIAN_POINT('Ctrl Pts',(-15.0413273538726,4.07981667851586,19.6654699357026));
#46300=CARTESIAN_POINT('Ctrl Pts',(-15.0491822708977,4.07981816742211,18.4144469747709));
#46301=CARTESIAN_POINT('Ctrl Pts',(-15.0529491711425,4.07981724239166,17.9116339513916));
#46302=CARTESIAN_POINT('Ctrl Pts',(-15.0624084365526,4.0798161087169,16.907660694229));
#46303=CARTESIAN_POINT('Ctrl Pts',(-15.0826972523316,4.07981019820557,15.1538675175825));
#46304=CARTESIAN_POINT('Ctrl Pts',(-15.1019756384676,4.07982792821452,13.6522604636661));
#46305=CARTESIAN_POINT('Ctrl Pts',(-15.1140599265239,4.07983658797161,12.3978501330781));
#46306=CARTESIAN_POINT('Ctrl Pts',(-15.118999927868,4.07983948633581,11.8969137604361));
#46307=CARTESIAN_POINT('Ctrl Pts',(-15.1290699569862,4.07983945762267,10.8950887987764));
#46308=CARTESIAN_POINT('Ctrl Pts',(-15.1415231892606,4.07986321498447,9.64266293595803));
#46309=CARTESIAN_POINT('Ctrl Pts',(-15.1546563515223,4.0798728821423,8.13830711977429));
#46310=CARTESIAN_POINT('Ctrl Pts',(-15.1611533789286,4.07991162203139,7.13365716272063));
#46311=CARTESIAN_POINT('Ctrl Pts',(-15.1641703541679,4.07992053271181,6.50603943843838));
#46312=CARTESIAN_POINT('Ctrl Pts',(-15.1658166076348,4.08049707291913,6.26337464950295));
#46313=CARTESIAN_POINT('Ctrl Pts',(-15.1705110079943,4.0835139590614,5.77045446573432));
#46314=CARTESIAN_POINT('Ctrl Pts',(-15.1814161643698,4.09267154088208,4.90241598307794));
#46315=CARTESIAN_POINT('Ctrl Pts',(-15.2060220994827,4.11704547635916,3.13599603857746));
#46316=CARTESIAN_POINT('Ctrl Pts',(-15.2047643807156,4.11788885254558,1.58241888815762));
#46317=CARTESIAN_POINT('Ctrl Pts',(-15.1675668382405,4.0764560708923,0.467940949357721));
#46318=CARTESIAN_POINT('Ctrl Pts',(-15.1627329495942,4.07095125001953,0.332095056170709));
#46319=CARTESIAN_POINT('Ctrl Pts',(-15.1515618273976,4.05832775712855,0.0636346843564117));
#46320=CARTESIAN_POINT('Ctrl Pts',(-15.1283184960179,4.03207150092787,-0.403681010059032));
#46321=CARTESIAN_POINT('Ctrl Pts',(-15.0860236033019,3.9844390875535,-1.06091900375415));
#46322=CARTESIAN_POINT('Ctrl Pts',(-15.0253548820853,3.91589806628914,-1.83452126081223));
#46323=CARTESIAN_POINT('Ctrl Pts',(-14.9374539251796,3.81626383930631,-2.84620724666584));
#46324=CARTESIAN_POINT('Ctrl Pts',(-14.8260214252139,3.68880024344429,-4.07548581332824));
#46325=CARTESIAN_POINT('Ctrl Pts',(-14.7594363908475,3.61301318315625,-5.02518833160673));
#46326=CARTESIAN_POINT('Ctrl Pts',(-14.732296786269,3.58308427120848,-5.60980532717593));
#46327=CARTESIAN_POINT('Ctrl Pts',(-14.7222950121233,3.57175513847179,-5.85331734149995));
#46328=CARTESIAN_POINT('Ctrl Pts',(-14.7051522824233,3.55288734903858,-6.3372651837452));
#46329=CARTESIAN_POINT('Ctrl Pts',(-14.6820755031784,3.52849851665087,-7.19188587500867));
#46330=CARTESIAN_POINT('Ctrl Pts',(-14.6648046124832,3.51403102114489,-8.42435063298136));
#46331=CARTESIAN_POINT('Ctrl Pts',(-14.6581099236016,3.51313576173022,-9.67204027371791));
#46332=CARTESIAN_POINT('Ctrl Pts',(-14.6536278741172,3.51217596509686,-10.5512063673995));
#46333=CARTESIAN_POINT('Ctrl Pts',(-14.6503694622625,3.51044997141002,-11.0551883304677));
#46334=CARTESIAN_POINT('Ctrl Pts',(-14.6483819555578,3.50901243037069,-11.3076840335205));
#46335=CARTESIAN_POINT('Ctrl Pts',(-14.6467027667886,3.50764329676335,-11.4979269040331));
#46336=CARTESIAN_POINT('Ctrl Pts',(-14.6456093912494,3.50678869858926,-11.6223550640012));
#46337=CARTESIAN_POINT('Ctrl Pts',(-14.6435757682735,3.50526761061104,-11.8729327016961));
#46338=CARTESIAN_POINT('Ctrl Pts',(-14.6403980129151,3.50310280032409,-12.3100266747562));
#46339=CARTESIAN_POINT('Ctrl Pts',(-14.6354559223704,3.50055398087762,-13.1834847279314));
#46340=CARTESIAN_POINT('Ctrl Pts',(-14.6317533744831,3.50086511785969,-14.4290661100897));
#46341=CARTESIAN_POINT('Ctrl Pts',(-14.6308576624301,3.50318988050142,-15.5534808436544));
#46342=CARTESIAN_POINT('Ctrl Pts',(-14.6306099354699,3.50445651101314,-16.3066179862937));
#46343=CARTESIAN_POINT('Ctrl Pts',(-14.6304928384944,3.50514632219001,-16.8098153537103));
#46344=CARTESIAN_POINT('Ctrl Pts',(-14.6304146638658,3.50541618468216,-17.1886154981013));
#46345=CARTESIAN_POINT('Ctrl Pts',(-14.6302952156756,3.50539935393863,-17.5044281144483));
#46346=CARTESIAN_POINT('Ctrl Pts',(-14.6302612721091,3.50539702227164,-17.6288670554403));
#46347=CARTESIAN_POINT('Ctrl Pts',(-14.6302453022539,3.50540897852697,-17.8782159379193));
#46348=CARTESIAN_POINT('Ctrl Pts',(-14.6303068483174,3.50544687608919,-18.127563739392));
#46349=CARTESIAN_POINT('Ctrl Pts',(-14.6304382209476,3.50550318977588,-18.377130410457));
#46350=CARTESIAN_POINT('Ctrl Pts',(-14.6305494440017,3.50554667481252,-18.5331538178356));
#46351=CARTESIAN_POINT('Ctrl Pts',(-14.6306547530545,3.50558531974963,-18.6580160550547));
#46352=CARTESIAN_POINT('Ctrl Pts',(-14.6307419615824,3.50561638167107,-18.7516798291178));
#46353=CARTESIAN_POINT('Ctrl Pts',(-14.6308213744854,3.50564391289322,-18.8297493429282));
#46354=CARTESIAN_POINT('Ctrl Pts',(-14.6308887686871,3.50566675064361,-18.8922142432608));
#46355=CARTESIAN_POINT('Ctrl Pts',(-14.6314838374563,3.50586612291774,-19.423219916044));
#46356=CARTESIAN_POINT('Ctrl Pts',(-14.6333692311182,3.50645317370486,-20.4401021876619));
#46357=CARTESIAN_POINT('Ctrl Pts',(-14.637476383763,3.50727050936296,-21.9473554866998));
#46358=CARTESIAN_POINT('Ctrl Pts',(-14.640808196621,3.50759270313843,-22.9561906327422));
#46359=CARTESIAN_POINT('Ctrl Pts',(-14.6428984515547,3.50759068760652,-23.5862944233562));
#46360=CARTESIAN_POINT('Ctrl Pts',(-14.643776352525,3.5075725191586,-23.8358209976824));
#46361=CARTESIAN_POINT('Ctrl Pts',(-14.6457331369259,3.50748751849172,-24.3355293750873));
#46362=CARTESIAN_POINT('Ctrl Pts',(-14.6496020318851,3.50721605211125,-25.2117220717688));
#46363=CARTESIAN_POINT('Ctrl Pts',(-14.656062504619,3.50660548397868,-26.4670089019858));
#46364=CARTESIAN_POINT('Ctrl Pts',(-14.6638903330453,3.50569606625201,-27.9752590018877));
#46365=CARTESIAN_POINT('Ctrl Pts',(-14.6683851504733,3.50527204895064,-28.9793144013429));
#46366=CARTESIAN_POINT('Ctrl Pts',(-14.6704277006154,3.50512795918196,-29.5433007449167));
#46367=CARTESIAN_POINT('Ctrl Pts',(-14.6707365850827,3.50490718889653,-29.6726937137558));
#46368=CARTESIAN_POINT('Ctrl Pts',(-14.6708316651918,3.50381704401876,-29.9285479609433));
#46369=CARTESIAN_POINT('Ctrl Pts',(-14.669766140098,3.50037881001467,-30.3760195620317));
#46370=CARTESIAN_POINT('Ctrl Pts',(-14.6637912291401,3.48885467862556,-31.2640688745989));
#46371=CARTESIAN_POINT('Ctrl Pts',(-14.6505638037055,3.46726542975816,-32.5155080392028));
#46372=CARTESIAN_POINT('Ctrl Pts',(-14.6478928861451,3.46031026411328,-33.7412400276083));
#46373=CARTESIAN_POINT('Ctrl Pts',(-14.6622999885151,3.47585215242021,-34.7050909198485));
#46374=CARTESIAN_POINT('Ctrl Pts',(-14.6767699741126,3.4925415200364,-35.1811795603407));
#46375=CARTESIAN_POINT('Ctrl Pts',(-14.6910527445473,3.5091074255739,-35.5366216765077));
#46376=CARTESIAN_POINT('Ctrl Pts',(-14.7023761429481,3.5219724789133,-35.7685022859579));
#46377=CARTESIAN_POINT('Ctrl Pts',(-14.730937498059,3.55480412742927,-36.2400471584948));
#46378=CARTESIAN_POINT('Ctrl Pts',(-14.7942510401053,3.62778769933195,-37.0735872305291));
#46379=CARTESIAN_POINT('Ctrl Pts',(-14.9567147007777,3.81530290395057,-38.7854056166029));
#46380=CARTESIAN_POINT('Ctrl Pts',(-15.0959365109023,3.97608959573285,-40.3405038655363));
#46381=CARTESIAN_POINT('Ctrl Pts',(-15.143164900117,4.03760057498106,-41.6917264284665));
#46382=CARTESIAN_POINT('Ctrl Pts',(-15.1542138680894,4.04952544452372,-42.0977073649019));
#46383=CARTESIAN_POINT('Ctrl Pts',(-15.1638448099992,4.05573631238654,-42.6272440819555));
#46384=CARTESIAN_POINT('Ctrl Pts',(-15.1704002909234,4.05695035430358,-43.1519747485755));
#46385=CARTESIAN_POINT('Ctrl Pts',(-15.1734737725596,4.05143422664606,-43.7967650097556));
#46386=CARTESIAN_POINT('Ctrl Pts',(-15.170994477228,4.04083420994993,-44.553127516674));
#46387=CARTESIAN_POINT('Ctrl Pts',(-15.1654680262509,4.03426710769119,-45.1683279110718));
#46388=CARTESIAN_POINT('Ctrl Pts',(-15.1600154170591,4.03353776034087,-45.6509597754355));
#46389=CARTESIAN_POINT('Ctrl Pts',(-15.1556442267631,4.03595897748892,-46.0082226248127));
#46390=CARTESIAN_POINT('Ctrl Pts',(-15.1512467507119,4.04205999799744,-46.3606502180971));
#46391=CARTESIAN_POINT('Ctrl Pts',(-15.1457005016869,4.05602078723531,-46.8240512717451));
#46392=CARTESIAN_POINT('Ctrl Pts',(-15.1422353107102,4.07396288140231,-47.1641699149808));
#46393=CARTESIAN_POINT('Ctrl Pts',(-15.139783459693,4.09827668768204,-47.5007304572948));
#46394=CARTESIAN_POINT('Ctrl Pts',(-15.1378420733016,4.11697806106922,-47.7531191415305));
#46395=CARTESIAN_POINT('Ctrl Pts',(-15.1328692251381,4.15525952282944,-48.2402312180556));
#46396=CARTESIAN_POINT('Ctrl Pts',(-15.1216753544551,4.22898695996459,-49.0948921174904));
#46397=CARTESIAN_POINT('Ctrl Pts',(-15.100570697442,4.35657973853331,-50.2945599673458));
#46398=CARTESIAN_POINT('Ctrl Pts',(-15.0740064986484,4.56209516926598,-51.7096344631151));
#46399=CARTESIAN_POINT('Ctrl Pts',(-15.0599764883946,4.74406573161041,-52.6344612450797));
#46400=CARTESIAN_POINT('Ctrl Pts',(-15.0537823319715,4.87549664531731,-53.208858641316));
#46401=CARTESIAN_POINT('Ctrl Pts',(-15.0513274604829,4.93110049792611,-53.444560390365));
#46402=CARTESIAN_POINT('Ctrl Pts',(-15.0466664614285,5.04865651751058,-53.9154426794593));
#46403=CARTESIAN_POINT('Ctrl Pts',(-15.0391166960127,5.2719822782236,-54.7438660195013));
#46404=CARTESIAN_POINT('Ctrl Pts',(-15.0265276021994,5.78405374259164,-56.409570029445));
#46405=CARTESIAN_POINT('Ctrl Pts',(-15.0201709336733,6.32184752352393,-57.8432803524839));
#46406=CARTESIAN_POINT('Ctrl Pts',(-15.0182848745529,6.73606148976995,-58.8513097528353));
#46407=CARTESIAN_POINT('Ctrl Pts',(-15.0181457177407,6.78388562980237,-58.9661899051116));
#46408=CARTESIAN_POINT('Ctrl Pts',(-15.0179891980911,6.88415653941591,-59.2014913298822));
#46409=CARTESIAN_POINT('Ctrl Pts',(-15.0181027948521,7.06579558906368,-59.6137866798083));
#46410=CARTESIAN_POINT('Ctrl Pts',(-15.0196034230197,7.45580435909341,-60.4501270204543));
#46411=CARTESIAN_POINT('Ctrl Pts',(-15.0234366830025,7.94966348909133,-61.4231487032632));
#46412=CARTESIAN_POINT('Ctrl Pts',(-15.0277521223662,8.46944302555454,-62.4082043767788));
#46413=CARTESIAN_POINT('Ctrl Pts',(-15.0300772962333,8.76701551587498,-62.9657228405259));
#46414=CARTESIAN_POINT('Ctrl Pts',(-15.0314650428341,8.96576570835786,-63.3386197971633));
#46415=CARTESIAN_POINT('Ctrl Pts',(-15.0323370111439,9.09823921246122,-63.5875349222999));
#46416=CARTESIAN_POINT('Ctrl Pts',(-15.0331248233671,9.2304705284566,-63.8368589352409));
#46417=CARTESIAN_POINT('Ctrl Pts',(-15.0337110597418,9.34566130836768,-64.0554130119618));
#46418=CARTESIAN_POINT('Ctrl Pts',(-15.0340144772916,9.41129110852897,-64.1804091802084));
#46419=CARTESIAN_POINT('Ctrl Pts',(-15.0344360007435,9.50951220481309,-64.3679984751364));
#46420=CARTESIAN_POINT('Ctrl Pts',(-15.0347177360903,9.59087461061657,-64.5245636207363));
#46421=CARTESIAN_POINT('Ctrl Pts',(-15.035067183854,9.72451684020435,-64.7838009731992));
#46422=CARTESIAN_POINT('Ctrl Pts',(-15.0353848133514,9.85473546692574,-65.0354253794396));
#46423=CARTESIAN_POINT('Ctrl Pts',(-15.0358612467763,10.1197277183049,-65.5439941961108));
#46424=CARTESIAN_POINT('Ctrl Pts',(-15.036335484482,10.5814515751937,-66.4217577653916));
#46425=CARTESIAN_POINT('Ctrl Pts',(-15.0361595669505,11.5086582574723,-68.1588609058033));
#46426=CARTESIAN_POINT('Ctrl Pts',(-15.0352657890704,12.3076050285516,-69.6376806593423));
#46427=CARTESIAN_POINT('Ctrl Pts',(-15.0353109350272,12.9112669501562,-70.7730023962225));
#46428=CARTESIAN_POINT('Ctrl Pts',(-15.035317222821,13.0444823135873,-71.0235484969299));
#46429=CARTESIAN_POINT('Ctrl Pts',(-15.0353274433012,13.3115672104804,-71.5258671392746));
#46430=CARTESIAN_POINT('Ctrl Pts',(-15.035336734874,13.6449287129749,-72.1528267593996));
#46431=CARTESIAN_POINT('Ctrl Pts',(-15.0353388634009,14.0449452184326,-72.9051457867444));
#46432=CARTESIAN_POINT('Ctrl Pts',(-15.0353334562094,14.8445920828781,-74.409051124372));
#46433=CARTESIAN_POINT('Ctrl Pts',(-15.0353264001462,15.5105658529013,-75.6615289922393));
#46434=CARTESIAN_POINT('Ctrl Pts',(-15.0353329405934,16.480312824235,-77.4853437224222));
#46435=CARTESIAN_POINT('Ctrl Pts',(-15.0353363076073,16.9167915016479,-78.3062334786655));
#46436=CARTESIAN_POINT('Ctrl Pts',(-15.0353363076072,17.3533130890374,-79.1272111807638));
#46437=CARTESIAN_POINT('Ctrl Pts',(-13.1557741379781,4.0803530524235,24.8306351545581));
#46438=CARTESIAN_POINT('Ctrl Pts',(-13.155813449685,4.08035305770157,24.7817558560973));
#46439=CARTESIAN_POINT('Ctrl Pts',(-13.1558546955356,4.08035307132234,24.7328774658928));
#46440=CARTESIAN_POINT('Ctrl Pts',(-13.1563410160438,4.08035286385746,24.1822744603286));
#46441=CARTESIAN_POINT('Ctrl Pts',(-13.1567093000387,4.0803508857895,23.1781803757718));
#46442=CARTESIAN_POINT('Ctrl Pts',(-13.1575765152318,4.08035147881019,21.1695864438393));
#46443=CARTESIAN_POINT('Ctrl Pts',(-13.1608052881424,4.08034627445879,19.6655358129393));
#46444=CARTESIAN_POINT('Ctrl Pts',(-13.1676736389584,4.08034350989803,18.414531537443));
#46445=CARTESIAN_POINT('Ctrl Pts',(-13.1709691910712,4.08034306295088,17.9117228044668));
#46446=CARTESIAN_POINT('Ctrl Pts',(-13.1792431927653,4.08034143992823,16.9077626620281));
#46447=CARTESIAN_POINT('Ctrl Pts',(-13.1969938389414,4.08033960128086,15.1539821060121));
#46448=CARTESIAN_POINT('Ctrl Pts',(-13.2138360265775,4.08032543633712,13.6524680930802));
#46449=CARTESIAN_POINT('Ctrl Pts',(-13.2244006454422,4.0803162635778,12.3980978193184));
#46450=CARTESIAN_POINT('Ctrl Pts',(-13.2287206857489,4.08031267404826,11.8971713269556));
#46451=CARTESIAN_POINT('Ctrl Pts',(-13.2375352633826,4.08030766451321,10.8953582505344));
#46452=CARTESIAN_POINT('Ctrl Pts',(-13.248411252422,4.08028902017245,9.64299864571605));
#46453=CARTESIAN_POINT('Ctrl Pts',(-13.2599009573185,4.08027574336008,8.13875529480386));
#46454=CARTESIAN_POINT('Ctrl Pts',(-13.2655477218758,4.0802526817982,7.13412346351715));
#46455=CARTESIAN_POINT('Ctrl Pts',(-13.2681799922693,4.0802448409878,6.50681185355107));
#46456=CARTESIAN_POINT('Ctrl Pts',(-13.2698019650851,4.08129294003242,6.27069253695577));
#46457=CARTESIAN_POINT('Ctrl Pts',(-13.274869162831,4.08682299769191,5.78485948929902));
#46458=CARTESIAN_POINT('Ctrl Pts',(-13.2872608605326,4.10369449867301,4.9257321017469));
#46459=CARTESIAN_POINT('Ctrl Pts',(-13.3164404286073,4.14919628450794,3.15395855145886));
#46460=CARTESIAN_POINT('Ctrl Pts',(-13.315061179104,4.15106871629214,1.55950246456322));
#46461=CARTESIAN_POINT('Ctrl Pts',(-13.270022580591,4.07031984608163,0.397516099160289));
#46462=CARTESIAN_POINT('Ctrl Pts',(-13.2641837990596,4.05942680369637,0.253300780986643));
#46463=CARTESIAN_POINT('Ctrl Pts',(-13.2506873468413,4.0346271829898,-0.0292291062131075));
#46464=CARTESIAN_POINT('Ctrl Pts',(-13.2226347076824,3.98323177920193,-0.519379279762533));
#46465=CARTESIAN_POINT('Ctrl Pts',(-13.1716378979934,3.8908084463512,-1.20123437706951));
#46466=CARTESIAN_POINT('Ctrl Pts',(-13.0989093337486,3.76003838001366,-1.99266219901469));
#46467=CARTESIAN_POINT('Ctrl Pts',(-12.9938191153109,3.57258968988866,-3.0124316173263));
#46468=CARTESIAN_POINT('Ctrl Pts',(-12.8614488653646,3.33863883231242,-4.22335814509426));
#46469=CARTESIAN_POINT('Ctrl Pts',(-12.7828099642305,3.20391268284202,-5.12908160087711));
#46470=CARTESIAN_POINT('Ctrl Pts',(-12.7511993924182,3.15155164599807,-5.67737368538212));
#46471=CARTESIAN_POINT('Ctrl Pts',(-12.7397758415395,3.13119206439564,-5.91439685386655));
#46472=CARTESIAN_POINT('Ctrl Pts',(-12.7203920322258,3.09763464973176,-6.38256542323508));
#46473=CARTESIAN_POINT('Ctrl Pts',(-12.695007138571,3.05430418906382,-7.2157590598277));
#46474=CARTESIAN_POINT('Ctrl Pts',(-12.6776718135492,3.02944506063389,-8.42731350929475));
#46475=CARTESIAN_POINT('Ctrl Pts',(-12.6727238131215,3.02933833013982,-9.66922524532342));
#46476=CARTESIAN_POINT('Ctrl Pts',(-12.6693075261318,3.02850998640237,-10.5517126348689));
#46477=CARTESIAN_POINT('Ctrl Pts',(-12.6664440131268,3.0257287217791,-11.059826352415));
#46478=CARTESIAN_POINT('Ctrl Pts',(-12.6645572626772,3.02322189370004,-11.3151362286705));
#46479=CARTESIAN_POINT('Ctrl Pts',(-12.6629101700705,3.02078100540286,-11.5076955248054));
#46480=CARTESIAN_POINT('Ctrl Pts',(-12.6618363318287,3.01928578080132,-11.6307891682924));
#46481=CARTESIAN_POINT('Ctrl Pts',(-12.6598686173034,3.01660753345846,-11.8803936099287));
#46482=CARTESIAN_POINT('Ctrl Pts',(-12.6568544052628,3.01279400055832,-12.3151264615418));
#46483=CARTESIAN_POINT('Ctrl Pts',(-12.6524002126988,3.00824205225206,-13.1851012690669));
#46484=CARTESIAN_POINT('Ctrl Pts',(-12.6497510856662,3.00868004220166,-14.4272726811341));
#46485=CARTESIAN_POINT('Ctrl Pts',(-12.6498267002527,3.01268518483088,-15.5510916707221));
#46486=CARTESIAN_POINT('Ctrl Pts',(-12.6500765443154,3.01488093698965,-16.3047646394304));
#46487=CARTESIAN_POINT('Ctrl Pts',(-12.6502466351578,3.01608794512074,-16.8085885957819));
#46488=CARTESIAN_POINT('Ctrl Pts',(-12.6502978693836,3.01654274968049,-17.1881348839868));
#46489=CARTESIAN_POINT('Ctrl Pts',(-12.650242819155,3.01651275050804,-17.5047195654652));
#46490=CARTESIAN_POINT('Ctrl Pts',(-12.6502371990516,3.01650268132953,-17.6291867393314));
#46491=CARTESIAN_POINT('Ctrl Pts',(-12.6502869006965,3.01648961217202,-17.878728330494));
#46492=CARTESIAN_POINT('Ctrl Pts',(-12.6504204710308,3.01648624162333,-18.1281731377591));
#46493=CARTESIAN_POINT('Ctrl Pts',(-12.6506330434434,3.01649653244229,-18.3778357309691));
#46494=CARTESIAN_POINT('Ctrl Pts',(-12.6507955528867,3.01650821404336,-18.5338973524979));
#46495=CARTESIAN_POINT('Ctrl Pts',(-12.6509428358872,3.01652123263419,-18.6587846325459));
#46496=CARTESIAN_POINT('Ctrl Pts',(-12.6510614160913,3.01653275679845,-18.7524622004311));
#46497=CARTESIAN_POINT('Ctrl Pts',(-12.6511667650687,3.01654387489522,-18.8305399070751));
#46498=CARTESIAN_POINT('Ctrl Pts',(-12.6512549082132,3.01655373743753,-18.893009216131));
#46499=CARTESIAN_POINT('Ctrl Pts',(-12.6520247925854,3.01664273458606,-19.4240399806288));
#46500=CARTESIAN_POINT('Ctrl Pts',(-12.6541237713984,3.01697758963585,-20.4405711730087));
#46501=CARTESIAN_POINT('Ctrl Pts',(-12.6579294211245,3.01815475287891,-21.9462443601063));
#46502=CARTESIAN_POINT('Ctrl Pts',(-12.6601102583778,3.01950882106249,-22.9533052565657));
#46503=CARTESIAN_POINT('Ctrl Pts',(-12.6611267318529,3.0205721594055,-23.5820735238017));
#46504=CARTESIAN_POINT('Ctrl Pts',(-12.6615286489473,3.021036564125,-23.8308286121961));
#46505=CARTESIAN_POINT('Ctrl Pts',(-12.6623261605263,3.02212153715255,-24.3293299145022));
#46506=CARTESIAN_POINT('Ctrl Pts',(-12.6637013086328,3.0243729156782,-25.2038048961164));
#46507=CARTESIAN_POINT('Ctrl Pts',(-12.6656051280685,3.0282974288727,-26.4579245903748));
#46508=CARTESIAN_POINT('Ctrl Pts',(-12.6677582628302,3.03312831756597,-27.966944419098));
#46509=CARTESIAN_POINT('Ctrl Pts',(-12.6691030075266,3.03577301881281,-28.9727051263296));
#46510=CARTESIAN_POINT('Ctrl Pts',(-12.6698168999596,3.03689787633675,-29.538357854649));
#46511=CARTESIAN_POINT('Ctrl Pts',(-12.6698132891089,3.03681104734995,-29.6711654578784));
#46512=CARTESIAN_POINT('Ctrl Pts',(-12.6692264069125,3.0353901770263,-29.9315464351366));
#46513=CARTESIAN_POINT('Ctrl Pts',(-12.6668345501107,3.03000301729997,-30.3864535953205));
#46514=CARTESIAN_POINT('Ctrl Pts',(-12.6578010215643,3.01039128155299,-31.2832523688234));
#46515=CARTESIAN_POINT('Ctrl Pts',(-12.6400066653409,2.97271146032919,-32.5320185755455));
#46516=CARTESIAN_POINT('Ctrl Pts',(-12.634845042572,2.96155909789071,-33.7345365602532));
#46517=CARTESIAN_POINT('Ctrl Pts',(-12.6501589419524,2.99012090783457,-34.6675071863071));
#46518=CARTESIAN_POINT('Ctrl Pts',(-12.6664685503625,3.02013697144729,-35.1238909076441));
#46519=CARTESIAN_POINT('Ctrl Pts',(-12.6827882943889,3.049667945086,-35.4627784713065));
#46520=CARTESIAN_POINT('Ctrl Pts',(-12.6958962012237,3.07215903548757,-35.6781859331147));
#46521=CARTESIAN_POINT('Ctrl Pts',(-12.7289805976222,3.13026629146692,-36.1242333697363));
#46522=CARTESIAN_POINT('Ctrl Pts',(-12.8028819866128,3.26100972646761,-36.9212545038253));
#46523=CARTESIAN_POINT('Ctrl Pts',(-12.9933548010237,3.60308348033867,-38.6016123397764));
#46524=CARTESIAN_POINT('Ctrl Pts',(-13.1613535575174,3.91182696291085,-40.201227918605));
#46525=CARTESIAN_POINT('Ctrl Pts',(-13.2211242393456,4.0282859866978,-41.6340139791982));
#46526=CARTESIAN_POINT('Ctrl Pts',(-13.2353144482749,4.05210923693267,-42.049869291881));
#46527=CARTESIAN_POINT('Ctrl Pts',(-13.2481818620755,4.06877955506982,-42.5962981492808));
#46528=CARTESIAN_POINT('Ctrl Pts',(-13.2574554867026,4.07711819302276,-43.1346449505987));
#46529=CARTESIAN_POINT('Ctrl Pts',(-13.2630683506023,4.0753602797487,-43.7938911993317));
#46530=CARTESIAN_POINT('Ctrl Pts',(-13.2627669354662,4.06365334098689,-44.5620551546818));
#46531=CARTESIAN_POINT('Ctrl Pts',(-13.2587465444613,4.05346862938487,-45.182994918791));
#46532=CARTESIAN_POINT('Ctrl Pts',(-13.2544578172475,4.04912257365654,-45.6676124144258));
#46533=CARTESIAN_POINT('Ctrl Pts',(-13.2510435147074,4.0487418057528,-46.0251003309895));
#46534=CARTESIAN_POINT('Ctrl Pts',(-13.2477397541082,4.05214987408337,-46.3764502468696));
#46535=CARTESIAN_POINT('Ctrl Pts',(-13.2438843323439,4.06288446089586,-46.8367149905799));
#46536=CARTESIAN_POINT('Ctrl Pts',(-13.2421308030081,4.07915836117823,-47.1724957266347));
#46537=CARTESIAN_POINT('Ctrl Pts',(-13.2417038676613,4.10249590966452,-47.5036559955688));
#46538=CARTESIAN_POINT('Ctrl Pts',(-13.2412069334258,4.12079522222734,-47.7601351750562));
#46539=CARTESIAN_POINT('Ctrl Pts',(-13.2394376932609,4.15718998577154,-48.2503877348323));
#46540=CARTESIAN_POINT('Ctrl Pts',(-13.2345417506537,4.22597034088981,-49.1111956569178));
#46541=CARTESIAN_POINT('Ctrl Pts',(-13.2236926141566,4.34316506975111,-50.3137302436462));
#46542=CARTESIAN_POINT('Ctrl Pts',(-13.2084156954445,4.53571596044538,-51.7255112759695));
#46543=CARTESIAN_POINT('Ctrl Pts',(-13.1995064977252,4.71143017567789,-52.6432201079995));
#46544=CARTESIAN_POINT('Ctrl Pts',(-13.1950938359785,4.84036713241892,-53.2119901498542));
#46545=CARTESIAN_POINT('Ctrl Pts',(-13.1932531878942,4.89533619012327,-53.446669547819));
#46546=CARTESIAN_POINT('Ctrl Pts',(-13.1894471040342,5.01193375313325,-53.9151122049486));
#46547=CARTESIAN_POINT('Ctrl Pts',(-13.18252847065,5.2347879202242,-54.7403346482864));
#46548=CARTESIAN_POINT('Ctrl Pts',(-13.1683828939882,5.74963013160343,-56.4019610873787));
#46549=CARTESIAN_POINT('Ctrl Pts',(-13.1582582282907,6.29384249941408,-57.8364241727682));
#46550=CARTESIAN_POINT('Ctrl Pts',(-13.154613161905,6.71177253080708,-58.8463268050262));
#46551=CARTESIAN_POINT('Ctrl Pts',(-13.1542220352886,6.75981670567772,-58.9609073836496));
#46552=CARTESIAN_POINT('Ctrl Pts',(-13.1535344633131,6.86072859200631,-59.1959507798566));
#46553=CARTESIAN_POINT('Ctrl Pts',(-13.1526023913756,7.04356752142575,-59.6077438258746));
#46554=CARTESIAN_POINT('Ctrl Pts',(-13.1516823831064,7.43658361850669,-60.4435582936179));
#46555=CARTESIAN_POINT('Ctrl Pts',(-13.1522569428826,7.93476027138594,-61.4165822262003));
#46556=CARTESIAN_POINT('Ctrl Pts',(-13.1534691360712,8.45913900066764,-62.402197109673));
#46557=CARTESIAN_POINT('Ctrl Pts',(-13.1542076397542,8.75925507630414,-62.9602249755118));
#46558=CARTESIAN_POINT('Ctrl Pts',(-13.15464405715,8.95962476308872,-63.3335566079143));
#46559=CARTESIAN_POINT('Ctrl Pts',(-13.1549160091587,9.09315589969736,-63.5827869386175));
#46560=CARTESIAN_POINT('Ctrl Pts',(-13.1551470658275,9.22639420779388,-63.8324666552708));
#46561=CARTESIAN_POINT('Ctrl Pts',(-13.1553038367501,9.34242301433713,-64.0513705625043));
#46562=CARTESIAN_POINT('Ctrl Pts',(-13.1553778405755,9.40851629243358,-64.1765783028481));
#46563=CARTESIAN_POINT('Ctrl Pts',(-13.1554724963636,9.50741702443271,-64.3644968293088));
#46564=CARTESIAN_POINT('Ctrl Pts',(-13.1555131491166,9.58930603781651,-64.5213614335515));
#46565=CARTESIAN_POINT('Ctrl Pts',(-13.155522246675,9.72376824731968,-64.7811308655079));
#46566=CARTESIAN_POINT('Ctrl Pts',(-13.1555299564657,9.85467392491661,-65.0331856010803));
#46567=CARTESIAN_POINT('Ctrl Pts',(-13.1555456366966,10.1208173755968,-65.5425902208122));
#46568=CARTESIAN_POINT('Ctrl Pts',(-13.1555658222632,10.5838519520742,-66.4215649205693));
#46569=CARTESIAN_POINT('Ctrl Pts',(-13.1556095707056,11.5115232537443,-68.1602044429875));
#46570=CARTESIAN_POINT('Ctrl Pts',(-13.155630456193,12.3087055590539,-69.6386566768396));
#46571=CARTESIAN_POINT('Ctrl Pts',(-13.1556403819816,12.9118168263674,-70.7729135669995));
#46572=CARTESIAN_POINT('Ctrl Pts',(-13.1556432693842,13.045079585473,-71.02353707039));
#46573=CARTESIAN_POINT('Ctrl Pts',(-13.1556472608338,13.3121586661121,-71.5258293803497));
#46574=CARTESIAN_POINT('Ctrl Pts',(-13.1556485304927,13.6455411657879,-72.1528256372706));
#46575=CARTESIAN_POINT('Ctrl Pts',(-13.1556480993221,14.0455574812149,-72.9051471364947));
#46576=CARTESIAN_POINT('Ctrl Pts',(-13.1556428636615,14.8452036750472,-74.4090743177834));
#46577=CARTESIAN_POINT('Ctrl Pts',(-13.1556286022721,15.5111376687713,-75.6615429776088));
#46578=CARTESIAN_POINT('Ctrl Pts',(-13.1556251422331,16.4808633570863,-77.4853364516287));
#46579=CARTESIAN_POINT('Ctrl Pts',(-13.1556233624458,16.917340718603,-78.306233401254));
#46580=CARTESIAN_POINT('Ctrl Pts',(-13.1556233624458,17.3538623059925,-79.1272111033524));
#46581=CARTESIAN_POINT('Ctrl Pts',(-10.6492819238592,4.08038167169719,24.8306351998132));
#46582=CARTESIAN_POINT('Ctrl Pts',(-10.6493137195392,4.08038168982262,24.7817559021637));
#46583=CARTESIAN_POINT('Ctrl Pts',(-10.6493470556338,4.08038166878299,24.7328773938009));
#46584=CARTESIAN_POINT('Ctrl Pts',(-10.6497412032544,4.08038324018666,24.1822784019949));
#46585=CARTESIAN_POINT('Ctrl Pts',(-10.6500453740232,4.0803948996082,23.1782177160824));
#46586=CARTESIAN_POINT('Ctrl Pts',(-10.6507462455772,4.08039723979176,21.1696274351929));
#46587=CARTESIAN_POINT('Ctrl Pts',(-10.6533744236306,4.08042667579571,19.6656599209132));
#46588=CARTESIAN_POINT('Ctrl Pts',(-10.6589390571556,4.0804407818347,18.4146918653329));
#46589=CARTESIAN_POINT('Ctrl Pts',(-10.6616065234231,4.08044366935237,17.9118887952537));
#46590=CARTESIAN_POINT('Ctrl Pts',(-10.6683052245384,4.08045433741086,16.9079522161296));
#46591=CARTESIAN_POINT('Ctrl Pts',(-10.6826712896214,4.08046841990858,15.1541963112138));
#46592=CARTESIAN_POINT('Ctrl Pts',(-10.6963377737673,4.08053651180721,13.6528713310165));
#46593=CARTESIAN_POINT('Ctrl Pts',(-10.7049088628403,4.08056603843003,12.3985897102618));
#46594=CARTESIAN_POINT('Ctrl Pts',(-10.7084129630787,4.08057570316825,11.8976881183865));
#46595=CARTESIAN_POINT('Ctrl Pts',(-10.7155548414695,4.08057795085157,10.8959012527467));
#46596=CARTESIAN_POINT('Ctrl Pts',(-10.7244027862711,4.08063665394617,9.64368478691638));
#46597=CARTESIAN_POINT('Ctrl Pts',(-10.7337288856492,4.08065595706751,8.13963068459924));
#46598=CARTESIAN_POINT('Ctrl Pts',(-10.7383620587042,4.08074986366022,7.13507936017797));
#46599=CARTESIAN_POINT('Ctrl Pts',(-10.7405096838567,4.08076913956257,6.50825519786931));
#46600=CARTESIAN_POINT('Ctrl Pts',(-10.741909153158,4.08252227758183,6.28231854453814));
#46601=CARTESIAN_POINT('Ctrl Pts',(-10.746456212477,4.09181511766032,5.80751570745706));
#46602=CARTESIAN_POINT('Ctrl Pts',(-10.7578124704736,4.12054662565677,4.96219824056498));
#46603=CARTESIAN_POINT('Ctrl Pts',(-10.784998696866,4.19944237288572,3.18240041367406));
#46604=CARTESIAN_POINT('Ctrl Pts',(-10.7841087575516,4.20563462630991,1.52424222051406));
#46605=CARTESIAN_POINT('Ctrl Pts',(-10.7423817296544,4.05827404435424,0.290146045282327));
#46606=CARTESIAN_POINT('Ctrl Pts',(-10.7369639268377,4.03787106784976,0.13323147767058));
#46607=CARTESIAN_POINT('Ctrl Pts',(-10.7245029251417,3.99201318730094,-0.170415006145854));
#46608=CARTESIAN_POINT('Ctrl Pts',(-10.6987448320663,3.89762597078122,-0.694336325539465));
#46609=CARTESIAN_POINT('Ctrl Pts',(-10.6526167146807,3.73129383433858,-1.4112761495687));
#46610=CARTESIAN_POINT('Ctrl Pts',(-10.5873503968315,3.50241778183169,-2.2275339890855));
#46611=CARTESIAN_POINT('Ctrl Pts',(-10.4931468457969,3.18400912617635,-3.25905161930202));
#46612=CARTESIAN_POINT('Ctrl Pts',(-10.3710530115233,2.80490032403984,-4.44792213541537));
#46613=CARTESIAN_POINT('Ctrl Pts',(-10.291981634001,2.60132190971847,-5.29067996192501));
#46614=CARTESIAN_POINT('Ctrl Pts',(-10.259322478708,2.52389752423809,-5.78301376090809));
#46615=CARTESIAN_POINT('Ctrl Pts',(-10.2482225058791,2.49208086099759,-6.01004845414477));
#46616=CARTESIAN_POINT('Ctrl Pts',(-10.2292708277151,2.44043284506256,-6.45365676938782));
#46617=CARTESIAN_POINT('Ctrl Pts',(-10.205360681967,2.37340808795552,-7.2531223258534));
#46618=CARTESIAN_POINT('Ctrl Pts',(-10.1910379110981,2.3361078750475,-8.43147609383172));
#46619=CARTESIAN_POINT('Ctrl Pts',(-10.1890967787696,2.33838464644536,-9.66414306851534));
#46620=CARTESIAN_POINT('Ctrl Pts',(-10.1873900792642,2.33855686624078,-10.551771751452));
#46621=CARTESIAN_POINT('Ctrl Pts',(-10.1854661676253,2.33473549177642,-11.066367517675));
#46622=CARTESIAN_POINT('Ctrl Pts',(-10.184042692168,2.33093798611811,-11.3261071331523));
#46623=CARTESIAN_POINT('Ctrl Pts',(-10.1827439703201,2.32713737341463,-11.5223106200541));
#46624=CARTESIAN_POINT('Ctrl Pts',(-10.1818623385683,2.32489346802413,-11.6431857937223));
#46625=CARTESIAN_POINT('Ctrl Pts',(-10.1802954994666,2.32086307815761,-11.8911005848554));
#46626=CARTESIAN_POINT('Ctrl Pts',(-10.1779607276946,2.31523914030324,-12.3218418170449));
#46627=CARTESIAN_POINT('Ctrl Pts',(-10.1748417521086,2.30894474871518,-13.1859670501784));
#46628=CARTESIAN_POINT('Ctrl Pts',(-10.1738155008547,2.31102400307239,-14.4226015029144));
#46629=CARTESIAN_POINT('Ctrl Pts',(-10.1749096307113,2.31844253624813,-15.5457906685208));
#46630=CARTESIAN_POINT('Ctrl Pts',(-10.1756110161507,2.32242724348455,-16.3007012118884));
#46631=CARTESIAN_POINT('Ctrl Pts',(-10.1760099430421,2.32459889120294,-16.8058145157111));
#46632=CARTESIAN_POINT('Ctrl Pts',(-10.1761869447333,2.32545056715243,-17.1868384155883));
#46633=CARTESIAN_POINT('Ctrl Pts',(-10.1761822187404,2.32543659934831,-17.5048968202555));
#46634=CARTESIAN_POINT('Ctrl Pts',(-10.1761964886654,2.32543216834755,-17.6291972230455));
#46635=CARTESIAN_POINT('Ctrl Pts',(-10.1762858482566,2.32542812266568,-17.8788418177221));
#46636=CARTESIAN_POINT('Ctrl Pts',(-10.1764633139881,2.32543489780847,-18.1282238990403));
#46637=CARTESIAN_POINT('Ctrl Pts',(-10.176709640203,2.32544837257372,-18.3779084247801));
#46638=CARTESIAN_POINT('Ctrl Pts',(-10.1768912054176,2.32546123226444,-18.5339633782873));
#46639=CARTESIAN_POINT('Ctrl Pts',(-10.1770504328865,2.32547350977745,-18.6588523774397));
#46640=CARTESIAN_POINT('Ctrl Pts',(-10.1771767398731,2.32548401121934,-18.7525291247011));
#46641=CARTESIAN_POINT('Ctrl Pts',(-10.1772873744373,2.32549385467383,-18.8306067078381));
#46642=CARTESIAN_POINT('Ctrl Pts',(-10.1773787570869,2.3255022748062,-18.893075633532));
#46643=CARTESIAN_POINT('Ctrl Pts',(-10.1781722001408,2.32557784693258,-19.4241027318974));
#46644=CARTESIAN_POINT('Ctrl Pts',(-10.1802391085788,2.32588556059833,-20.4405830164739));
#46645=CARTESIAN_POINT('Ctrl Pts',(-10.1829097809687,2.32671242001792,-21.9461597427201));
#46646=CARTESIAN_POINT('Ctrl Pts',(-10.1833711322145,2.32765213655555,-22.9531075140253));
#46647=CARTESIAN_POINT('Ctrl Pts',(-10.1828438775792,2.32834169386881,-23.5818011088191));
#46648=CARTESIAN_POINT('Ctrl Pts',(-10.182556795248,2.32863831763781,-23.8305131431512));
#46649=CARTESIAN_POINT('Ctrl Pts',(-10.1817206536772,2.32932917945615,-24.3289448593721));
#46650=CARTESIAN_POINT('Ctrl Pts',(-10.1796488766789,2.33075497774474,-25.2033338196031));
#46651=CARTESIAN_POINT('Ctrl Pts',(-10.1754960322699,2.33324047082322,-26.4573585609411));
#46652=CARTESIAN_POINT('Ctrl Pts',(-10.1701133843866,2.33624987105413,-27.9665370845329));
#46653=CARTESIAN_POINT('Ctrl Pts',(-10.167392028961,2.33789044740065,-28.9722307369851));
#46654=CARTESIAN_POINT('Ctrl Pts',(-10.1663804217523,2.33858566329863,-29.538352557414));
#46655=CARTESIAN_POINT('Ctrl Pts',(-10.1660110912668,2.33819003936893,-29.6765341761858));
#46656=CARTESIAN_POINT('Ctrl Pts',(-10.164777103551,2.33532769799564,-29.9437575708518));
#46657=CARTESIAN_POINT('Ctrl Pts',(-10.1614248907804,2.32554339954716,-30.4100054116301));
#46658=CARTESIAN_POINT('Ctrl Pts',(-10.1509829711924,2.29164239193802,-31.3196602435576));
#46659=CARTESIAN_POINT('Ctrl Pts',(-10.1314429635782,2.22865322636961,-32.5630530289834));
#46660=CARTESIAN_POINT('Ctrl Pts',(-10.1239578463117,2.20990497774048,-33.7276319436604));
#46661=CARTESIAN_POINT('Ctrl Pts',(-10.1382272091451,2.25365471385146,-34.6108266770133));
#46662=CARTESIAN_POINT('Ctrl Pts',(-10.1545213545452,2.2995154614481,-35.0359677653007));
#46663=CARTESIAN_POINT('Ctrl Pts',(-10.1711414781042,2.34440310676093,-35.3489526983482));
#46664=CARTESIAN_POINT('Ctrl Pts',(-10.1851098617071,2.37744042159386,-35.5389379447642));
#46665=CARTESIAN_POINT('Ctrl Pts',(-10.219077321318,2.46500957214916,-35.9465551226477));
#46666=CARTESIAN_POINT('Ctrl Pts',(-10.2925513678124,2.66590288201721,-36.6907927120213));
#46667=CARTESIAN_POINT('Ctrl Pts',(-10.4672915221739,3.21377553661836,-38.3318422142825));
#46668=CARTESIAN_POINT('Ctrl Pts',(-10.6127099001957,3.76161631783265,-39.985236248682));
#46669=CARTESIAN_POINT('Ctrl Pts',(-10.669499445744,3.97735825964587,-41.5392455494394));
#46670=CARTESIAN_POINT('Ctrl Pts',(-10.6834790497686,4.02170688238063,-41.9700526817855));
#46671=CARTESIAN_POINT('Ctrl Pts',(-10.6968123531277,4.05775966332809,-42.5420665740536));
#46672=CARTESIAN_POINT('Ctrl Pts',(-10.7069670754181,4.07969938553161,-43.1010554995864));
#46673=CARTESIAN_POINT('Ctrl Pts',(-10.7143533231186,4.08658995129601,-43.7820402933545));
#46674=CARTESIAN_POINT('Ctrl Pts',(-10.7170251331761,4.07621708661553,-44.5674691109912));
#46675=CARTESIAN_POINT('Ctrl Pts',(-10.7160390580498,4.06305808236085,-45.1962275583449));
#46676=CARTESIAN_POINT('Ctrl Pts',(-10.7145238579317,4.05561185326259,-45.6829976418167));
#46677=CARTESIAN_POINT('Ctrl Pts',(-10.7133007288124,4.05286283457337,-46.040081421822));
#46678=CARTESIAN_POINT('Ctrl Pts',(-10.7122864672143,4.05418486041162,-46.3889558225569));
#46679=CARTESIAN_POINT('Ctrl Pts',(-10.7116148380017,4.06290648666823,-46.8432204483996));
#46680=CARTESIAN_POINT('Ctrl Pts',(-10.7122825915524,4.07881746233585,-47.1713383938465));
#46681=CARTESIAN_POINT('Ctrl Pts',(-10.7143508228806,4.10302756806235,-47.4931458846201));
#46682=CARTESIAN_POINT('Ctrl Pts',(-10.715686897772,4.12265857937166,-47.753639792098));
#46683=CARTESIAN_POINT('Ctrl Pts',(-10.718164607178,4.16057100812037,-48.2457370669567));
#46684=CARTESIAN_POINT('Ctrl Pts',(-10.7219473309798,4.23079720928861,-49.1118649713687));
#46685=CARTESIAN_POINT('Ctrl Pts',(-10.7255526649831,4.34667077707044,-50.3176218146149));
#46686=CARTESIAN_POINT('Ctrl Pts',(-10.7265601494607,4.53579485376256,-51.7301734409053));
#46687=CARTESIAN_POINT('Ctrl Pts',(-10.7245563309438,4.70950264467719,-52.6453714483989));
#46688=CARTESIAN_POINT('Ctrl Pts',(-10.7223848813205,4.83783044140274,-53.2119653734534));
#46689=CARTESIAN_POINT('Ctrl Pts',(-10.7213419894687,4.89280876274709,-53.4468056233345));
#46690=CARTESIAN_POINT('Ctrl Pts',(-10.7185909308167,5.00933732238949,-53.9149973687165));
#46691=CARTESIAN_POINT('Ctrl Pts',(-10.7122736331623,5.23224005705955,-54.7401180405057));
#46692=CARTESIAN_POINT('Ctrl Pts',(-10.6953636514727,5.74746593397295,-56.4013982419585));
#46693=CARTESIAN_POINT('Ctrl Pts',(-10.6795026822741,6.29233680493474,-57.8359715964635));
#46694=CARTESIAN_POINT('Ctrl Pts',(-10.6729996788152,6.71055227811244,-58.8460496147919));
#46695=CARTESIAN_POINT('Ctrl Pts',(-10.6721930196659,6.75861817572571,-58.9606199063025));
#46696=CARTESIAN_POINT('Ctrl Pts',(-10.6706386559564,6.85958025905996,-59.1956605069516));
#46697=CARTESIAN_POINT('Ctrl Pts',(-10.6680297375051,7.04250853252697,-59.6074430378433));
#46698=CARTESIAN_POINT('Ctrl Pts',(-10.6632723032891,7.43570291173815,-60.4432491785754));
#46699=CARTESIAN_POINT('Ctrl Pts',(-10.6588558170839,7.93410394761738,-61.4162871376521));
#46700=CARTESIAN_POINT('Ctrl Pts',(-10.6552771893509,8.45866189811967,-62.4019273521771));
#46701=CARTESIAN_POINT('Ctrl Pts',(-10.6535421547273,8.75885908803885,-62.9599707044205));
#46702=CARTESIAN_POINT('Ctrl Pts',(-10.6524909466147,8.9592766719587,-63.3333135438091));
#46703=CARTESIAN_POINT('Ctrl Pts',(-10.6518156015038,9.09283556102529,-63.5825506072565));
#46704=CARTESIAN_POINT('Ctrl Pts',(-10.651184724697,9.22610620049791,-63.8322398641344));
#46705=CARTESIAN_POINT('Ctrl Pts',(-10.6506626166579,9.34215666827589,-64.0511504440258));
#46706=CARTESIAN_POINT('Ctrl Pts',(-10.6503735525664,9.40826187449771,-64.1763620347625));
#46707=CARTESIAN_POINT('Ctrl Pts',(-10.6499487261179,9.50717944570217,-64.364286131224));
#46708=CARTESIAN_POINT('Ctrl Pts',(-10.649616156931,9.5890857669874,-64.5211573177303));
#46709=CARTESIAN_POINT('Ctrl Pts',(-10.6490865991625,9.72357093821706,-64.7809357767682));
#46710=CARTESIAN_POINT('Ctrl Pts',(-10.6486084730312,9.85450403883141,-65.0330096286938));
#46711=CARTESIAN_POINT('Ctrl Pts',(-10.6478935030841,10.1206875040802,-65.5424428653429));
#46712=CARTESIAN_POINT('Ctrl Pts',(-10.6472235238906,10.5837849990798,-66.4214697243471));
#46713=CARTESIAN_POINT('Ctrl Pts',(-10.6476327795485,11.5114983625212,-68.1601729075373));
#46714=CARTESIAN_POINT('Ctrl Pts',(-10.6492165339314,12.3086856507892,-69.6386485829911));
#46715=CARTESIAN_POINT('Ctrl Pts',(-10.6492051597913,12.911799051916,-70.7728833401244));
#46716=CARTESIAN_POINT('Ctrl Pts',(-10.6492012024291,13.04506371583,-71.0235095231732));
#46717=CARTESIAN_POINT('Ctrl Pts',(-10.6491958831625,13.3121443479147,-71.5258020179872));
#46718=CARTESIAN_POINT('Ctrl Pts',(-10.6491947187677,13.6455327598224,-72.1528025111679));
#46719=CARTESIAN_POINT('Ctrl Pts',(-10.6491955778798,14.0455513877889,-72.9051254391018));
#46720=CARTESIAN_POINT('Ctrl Pts',(-10.6492032628139,14.8452014831371,-74.4090555915023));
#46721=CARTESIAN_POINT('Ctrl Pts',(-10.649224822732,15.5111509976849,-75.6615339080009));
#46722=CARTESIAN_POINT('Ctrl Pts',(-10.6492307550641,16.4808865796188,-77.4853330368044));
#46723=CARTESIAN_POINT('Ctrl Pts',(-10.6492338083976,16.91736931297,-78.3062334180857));
#46724=CARTESIAN_POINT('Ctrl Pts',(-10.6492338083975,17.3538909003594,-79.1272111201841));
#46725=CARTESIAN_POINT('Ctrl Pts',(-8.14359067365561,4.07985970540613,24.8306345375628));
#46726=CARTESIAN_POINT('Ctrl Pts',(-8.14361498400114,4.07985970354231,24.7817552188885));
#46727=CARTESIAN_POINT('Ctrl Pts',(-8.14364047300421,4.07985966976465,24.7328766250053));
#46728=CARTESIAN_POINT('Ctrl Pts',(-8.14394180053891,4.07986071796207,24.1822795439549));
#46729=CARTESIAN_POINT('Ctrl Pts',(-8.14417414872545,4.0798695436064,23.1782365679108));
#46730=CARTESIAN_POINT('Ctrl Pts',(-8.14471009420409,4.07987017975739,21.1696477877977));
#46731=CARTESIAN_POINT('Ctrl Pts',(-8.14671893325979,4.07989225735344,19.6657249052665));
#46732=CARTESIAN_POINT('Ctrl Pts',(-8.15097310704072,4.07990210697193,18.4147762947717));
#46733=CARTESIAN_POINT('Ctrl Pts',(-8.15301249508394,4.07990363804429,17.9119749489971));
#46734=CARTESIAN_POINT('Ctrl Pts',(-8.15813390489173,4.07991001310458,16.9080501386704));
#46735=CARTESIAN_POINT('Ctrl Pts',(-8.16911747042228,4.07991677228478,15.1543077434332));
#46736=CARTESIAN_POINT('Ctrl Pts',(-8.17956482346294,4.07996837376312,13.653088880244));
#46737=CARTESIAN_POINT('Ctrl Pts',(-8.18611672759872,4.07999333067391,12.3988607914225));
#46738=CARTESIAN_POINT('Ctrl Pts',(-8.18879534967467,4.08000198216328,11.897974147008));
#46739=CARTESIAN_POINT('Ctrl Pts',(-8.1942549631774,4.08000682487738,10.896207146212));
#46740=CARTESIAN_POINT('Ctrl Pts',(-8.20101754403269,4.08005903324089,9.64406333425493));
#46741=CARTESIAN_POINT('Ctrl Pts',(-8.20814595172556,4.08008149013275,8.14012995143153));
#46742=CARTESIAN_POINT('Ctrl Pts',(-8.21168550255051,4.08016083230667,7.13558566831604));
#46743=CARTESIAN_POINT('Ctrl Pts',(-8.21332645458666,4.08017726326418,6.50909204522029));
#46744=CARTESIAN_POINT('Ctrl Pts',(-8.21413897927589,4.08237190936357,6.29028482577281));
#46745=CARTESIAN_POINT('Ctrl Pts',(-8.21626693784459,4.09412056112342,5.82321881151269));
#46746=CARTESIAN_POINT('Ctrl Pts',(-8.22090193607751,4.13075485442928,4.98737536189332));
#46747=CARTESIAN_POINT('Ctrl Pts',(-8.23093289196322,4.2335233754299,3.20246421710022));
#46748=CARTESIAN_POINT('Ctrl Pts',(-8.23022472659282,4.24340874447766,1.49794937469472));
#46749=CARTESIAN_POINT('Ctrl Pts',(-8.21578280303809,4.04343673099212,0.216408376068755));
#46750=CARTESIAN_POINT('Ctrl Pts',(-8.2139091204433,4.01529420171371,0.0512402447371398));
#46751=CARTESIAN_POINT('Ctrl Pts',(-8.20962119499329,3.95270323742799,-0.265737629226556));
#46752=CARTESIAN_POINT('Ctrl Pts',(-8.20081942730489,3.82480741036837,-0.810098156167453));
#46753=CARTESIAN_POINT('Ctrl Pts',(-8.18531801461245,3.60340048820505,-1.54625681655442));
#46754=CARTESIAN_POINT('Ctrl Pts',(-8.16359583366465,3.30577257714691,-2.37574729524026));
#46755=CARTESIAN_POINT('Ctrl Pts',(-8.13205640026516,2.90059244028148,-3.41528007458188));
#46756=CARTESIAN_POINT('Ctrl Pts',(-8.08937811281637,2.4355293602073,-4.60151152308765));
#46757=CARTESIAN_POINT('Ctrl Pts',(-8.05746883191124,2.20819553877365,-5.41164033896553));
#46758=CARTESIAN_POINT('Ctrl Pts',(-8.04345040864611,2.1263656741961,-5.86462386581994));
#46759=CARTESIAN_POINT('Ctrl Pts',(-8.03895818083086,2.08989753972466,-6.08463724447221));
#46760=CARTESIAN_POINT('Ctrl Pts',(-8.03108232980876,2.03198126703692,-6.51016269028769));
#46761=CARTESIAN_POINT('Ctrl Pts',(-8.02117765134921,1.95592016996364,-7.28340190344963));
#46762=CARTESIAN_POINT('Ctrl Pts',(-8.01522206297929,1.91357126242899,-8.43458939573691));
#46763=CARTESIAN_POINT('Ctrl Pts',(-8.01425114707161,1.91732011821017,-9.65957978464447));
#46764=CARTESIAN_POINT('Ctrl Pts',(-8.01335348109672,1.91845193485591,-10.5513493386686));
#46765=CARTESIAN_POINT('Ctrl Pts',(-8.01248383477213,1.9142489375257,-11.0712064747836));
#46766=CARTESIAN_POINT('Ctrl Pts',(-8.0118763575149,1.90981310339595,-11.33455059115));
#46767=CARTESIAN_POINT('Ctrl Pts',(-8.01133566115346,1.90530015540803,-11.5337232509074));
#46768=CARTESIAN_POINT('Ctrl Pts',(-8.01094689215894,1.90277321047312,-11.6527536236799));
#46769=CARTESIAN_POINT('Ctrl Pts',(-8.01025266008061,1.89818676723235,-11.8992409803262));
#46770=CARTESIAN_POINT('Ctrl Pts',(-8.00918009773255,1.89189696236533,-12.3266360319494));
#46771=CARTESIAN_POINT('Ctrl Pts',(-8.00761285103791,1.88516044318482,-13.1858364518625));
#46772=CARTESIAN_POINT('Ctrl Pts',(-8.00664309424968,1.88871336098231,-14.4179058392809));
#46773=CARTESIAN_POINT('Ctrl Pts',(-8.00659588312024,1.89837865245115,-15.5407647870117));
#46774=CARTESIAN_POINT('Ctrl Pts',(-8.00662679781179,1.90352367064465,-16.2968921892087));
#46775=CARTESIAN_POINT('Ctrl Pts',(-8.00664346099735,1.90632656545951,-16.8032216726378));
#46776=CARTESIAN_POINT('Ctrl Pts',(-8.00664413152868,1.90742099344714,-17.1855914707571));
#46777=CARTESIAN_POINT('Ctrl Pts',(-8.00660749593276,1.90742145720269,-17.5049782515705));
#46778=CARTESIAN_POINT('Ctrl Pts',(-8.00660252735443,1.90742315116677,-17.6290173248691));
#46779=CARTESIAN_POINT('Ctrl Pts',(-8.0066285599827,1.90743215431583,-17.8786228825783));
#46780=CARTESIAN_POINT('Ctrl Pts',(-8.00670679073166,1.90744943452059,-18.1278229010574));
#46781=CARTESIAN_POINT('Ctrl Pts',(-8.00682588342566,1.90747185469976,-18.3774486894127));
#46782=CARTESIAN_POINT('Ctrl Pts',(-8.00691672070047,1.90748801250143,-18.533459000571));
#46783=CARTESIAN_POINT('Ctrl Pts',(-8.00699772411189,1.90750178011767,-18.6583280627768));
#46784=CARTESIAN_POINT('Ctrl Pts',(-8.00706258068671,1.90751254413139,-18.7519917259217));
#46785=CARTESIAN_POINT('Ctrl Pts',(-8.00711983429507,1.90752183146061,-18.8300624342547));
#46786=CARTESIAN_POINT('Ctrl Pts',(-8.00716736235425,1.90752938420153,-18.8925276007566));
#46787=CARTESIAN_POINT('Ctrl Pts',(-8.00758134301623,1.90759445283299,-19.4235338608292));
#46788=CARTESIAN_POINT('Ctrl Pts',(-8.0086962754387,1.90775669668981,-20.4403124276682));
#46789=CARTESIAN_POINT('Ctrl Pts',(-8.01014433860419,1.90779978173849,-21.9473206928697));
#46790=CARTESIAN_POINT('Ctrl Pts',(-8.01034363847009,1.90756341118158,-22.9558654320696));
#46791=CARTESIAN_POINT('Ctrl Pts',(-8.00999713654423,1.90727111718054,-23.5857649516545));
#46792=CARTESIAN_POINT('Ctrl Pts',(-8.00981335169339,1.90713624766546,-23.8351803292311));
#46793=CARTESIAN_POINT('Ctrl Pts',(-8.00928852377032,1.90680231431617,-24.3347012742357));
#46794=CARTESIAN_POINT('Ctrl Pts',(-8.00800826908139,1.90607221168703,-25.2106658285509));
#46795=CARTESIAN_POINT('Ctrl Pts',(-8.0054751748871,1.90473976488522,-26.4656402154394));
#46796=CARTESIAN_POINT('Ctrl Pts',(-8.00226388458962,1.90307892723492,-27.9742477266283));
#46797=CARTESIAN_POINT('Ctrl Pts',(-8.00069638142823,1.90219781638892,-28.9780396393795));
#46798=CARTESIAN_POINT('Ctrl Pts',(-8.00015292486548,1.90184633791688,-29.5431662744624));
#46799=CARTESIAN_POINT('Ctrl Pts',(-7.99998955053817,1.90105102284858,-29.6857229368641));
#46800=CARTESIAN_POINT('Ctrl Pts',(-7.99949651434298,1.89694107561718,-29.9583428203848));
#46801=CARTESIAN_POINT('Ctrl Pts',(-7.99822851669594,1.8839487287467,-30.4336135537794));
#46802=CARTESIAN_POINT('Ctrl Pts',(-7.99437868132817,1.84095506174159,-31.3532492515463));
#46803=CARTESIAN_POINT('Ctrl Pts',(-7.98693475241986,1.76463960510802,-32.5918758214193));
#46804=CARTESIAN_POINT('Ctrl Pts',(-7.98386044087593,1.74322772090953,-33.7234925777175));
#46805=CARTESIAN_POINT('Ctrl Pts',(-7.99005560425241,1.7911516553672,-34.5645435207993));
#46806=CARTESIAN_POINT('Ctrl Pts',(-7.99711971545115,1.84073247083906,-34.9647455338871));
#46807=CARTESIAN_POINT('Ctrl Pts',(-8.00427652327302,1.88895588939534,-35.2583124376742));
#46808=CARTESIAN_POINT('Ctrl Pts',(-8.01052992775479,1.92243043124532,-35.4299041084946));
#46809=CARTESIAN_POINT('Ctrl Pts',(-8.02486144232338,2.01643622035667,-35.8128967008395));
#46810=CARTESIAN_POINT('Ctrl Pts',(-8.05402181482127,2.24231511479637,-36.5298589220037));
#46811=CARTESIAN_POINT('Ctrl Pts',(-8.11431219801583,2.90130270715427,-38.1671665136789));
#46812=CARTESIAN_POINT('Ctrl Pts',(-8.15836776367972,3.61801973043291,-39.8396120423116));
#46813=CARTESIAN_POINT('Ctrl Pts',(-8.17719495330526,3.91520482254767,-41.4700177478095));
#46814=CARTESIAN_POINT('Ctrl Pts',(-8.18205149246931,3.97542999084137,-41.910711262013));
#46815=CARTESIAN_POINT('Ctrl Pts',(-8.1868566749838,4.02740123566261,-42.499800897281));
#46816=CARTESIAN_POINT('Ctrl Pts',(-8.19066643647986,4.06077088406066,-43.0727636686921));
#46817=CARTESIAN_POINT('Ctrl Pts',(-8.19371029383873,4.07580536115162,-43.7684561040316));
#46818=CARTESIAN_POINT('Ctrl Pts',(-8.19530062342225,4.06862371922948,-44.5653141924112));
#46819=CARTESIAN_POINT('Ctrl Pts',(-8.19551033397204,4.05540999605244,-45.1988643282004));
#46820=CARTESIAN_POINT('Ctrl Pts',(-8.19539543435627,4.04743325365432,-45.6865563975787));
#46821=CARTESIAN_POINT('Ctrl Pts',(-8.1952518247706,4.0443339961423,-46.042885636124));
#46822=CARTESIAN_POINT('Ctrl Pts',(-8.19514514727457,4.04556228771761,-46.3895285851106));
#46823=CARTESIAN_POINT('Ctrl Pts',(-8.19518123664623,4.05472027090549,-46.8388990362217));
#46824=CARTESIAN_POINT('Ctrl Pts',(-8.19553163699906,4.07185001917136,-47.1611021829135));
#46825=CARTESIAN_POINT('Ctrl Pts',(-8.19629659062148,4.09802470116959,-47.4758325557082));
#46826=CARTESIAN_POINT('Ctrl Pts',(-8.19679452923414,4.11986249700318,-47.7376494555348));
#46827=CARTESIAN_POINT('Ctrl Pts',(-8.19773917498253,4.16167351614696,-48.2291392276498));
#46828=CARTESIAN_POINT('Ctrl Pts',(-8.19920722922556,4.23888748557492,-49.0963063923987));
#46829=CARTESIAN_POINT('Ctrl Pts',(-8.20054154878142,4.36400652509188,-50.3035936590456));
#46830=CARTESIAN_POINT('Ctrl Pts',(-8.20025279113926,4.56221439394529,-51.720273945602));
#46831=CARTESIAN_POINT('Ctrl Pts',(-8.19827155368996,4.74008618271685,-52.6391087835333));
#46832=CARTESIAN_POINT('Ctrl Pts',(-8.19633734306815,4.87024377764062,-53.2082681627338));
#46833=CARTESIAN_POINT('Ctrl Pts',(-8.1954469406703,4.92590316907518,-53.4443026616136));
#46834=CARTESIAN_POINT('Ctrl Pts',(-8.19322130190796,5.04332674104089,-53.9145154326853));
#46835=CARTESIAN_POINT('Ctrl Pts',(-8.1883333481497,5.26676583637175,-54.7426361152984));
#46836=CARTESIAN_POINT('Ctrl Pts',(-8.1757679372123,5.77947514538758,-56.407552918538));
#46837=CARTESIAN_POINT('Ctrl Pts',(-8.16434196831385,6.31847818783456,-57.8418435904684));
#46838=CARTESIAN_POINT('Ctrl Pts',(-8.15963822163446,6.73329256363275,-58.8503748905591));
#46839=CARTESIAN_POINT('Ctrl Pts',(-8.15905775023175,6.78114781912818,-58.9652211373289));
#46840=CARTESIAN_POINT('Ctrl Pts',(-8.1579455881897,6.88150913430379,-59.2005123816663));
#46841=CARTESIAN_POINT('Ctrl Pts',(-8.15609615307335,7.06330301541337,-59.6127829607361));
#46842=CARTESIAN_POINT('Ctrl Pts',(-8.15278801562376,7.45367427950311,-60.4491444615007));
#46843=CARTESIAN_POINT('Ctrl Pts',(-8.14983256375181,7.94800603254326,-61.4222671566292));
#46844=CARTESIAN_POINT('Ctrl Pts',(-8.14750217146235,8.4682998967399,-62.4074483788712));
#46845=CARTESIAN_POINT('Ctrl Pts',(-8.14638568785422,8.76616086589802,-62.9650380015432));
#46846=CARTESIAN_POINT('Ctrl Pts',(-8.14570869227385,8.96509688931052,-63.337988342902));
#46847=CARTESIAN_POINT('Ctrl Pts',(-8.14527332588339,9.09769332760823,-63.5869388592505));
#46848=CARTESIAN_POINT('Ctrl Pts',(-8.14486437782742,9.2300394234522,-63.8363037865726));
#46849=CARTESIAN_POINT('Ctrl Pts',(-8.14452353060581,9.34532853518197,-64.0548942082687));
#46850=CARTESIAN_POINT('Ctrl Pts',(-8.14433379730441,9.41101293112661,-64.1799120519233));
#46851=CARTESIAN_POINT('Ctrl Pts',(-8.14405386623975,9.50931459878488,-64.3675345624609));
#46852=CARTESIAN_POINT('Ctrl Pts',(-8.14383173923921,9.59073785194436,-64.5241303521888));
#46853=CARTESIAN_POINT('Ctrl Pts',(-8.14347388326224,9.72447785071259,-64.7834206217065));
#46854=CARTESIAN_POINT('Ctrl Pts',(-8.14315059498215,9.85478583013289,-65.0351043708353));
#46855=CARTESIAN_POINT('Ctrl Pts',(-8.1426673769054,10.1199249327764,-65.5437777065966));
#46856=CARTESIAN_POINT('Ctrl Pts',(-8.14221292863375,10.5818120711918,-66.421701667515));
#46857=CARTESIAN_POINT('Ctrl Pts',(-8.14248547303518,11.5090685253749,-68.159007849325));
#46858=CARTESIAN_POINT('Ctrl Pts',(-8.14354628768597,12.307761001971,-69.6377922875381));
#46859=CARTESIAN_POINT('Ctrl Pts',(-8.14353620190536,12.911344014831,-70.772980942748));
#46860=CARTESIAN_POINT('Ctrl Pts',(-8.14353341552564,13.0445655981629,-71.0235373309712));
#46861=CARTESIAN_POINT('Ctrl Pts',(-8.14352953341891,13.3116493812976,-71.5258532489965));
#46862=CARTESIAN_POINT('Ctrl Pts',(-8.14352815373002,13.6450115100796,-72.1528189545927));
#46863=CARTESIAN_POINT('Ctrl Pts',(-8.14352849833392,14.0450270936495,-72.9051390601201));
#46864=CARTESIAN_POINT('Ctrl Pts',(-8.14353340536773,14.844672016046,-74.4090483631363));
#46865=CARTESIAN_POINT('Ctrl Pts',(-8.14354658110851,15.510632305582,-75.6615281122465));
#46866=CARTESIAN_POINT('Ctrl Pts',(-8.14354957689417,16.4803713305245,-77.4853414851555));
#46867=CARTESIAN_POINT('Ctrl Pts',(-8.1435511206182,16.9168474424909,-78.3062334150556));
#46868=CARTESIAN_POINT('Ctrl Pts',(-8.14355112061824,17.3533690298803,-79.1272111171539));
#46869=CARTESIAN_POINT('Ctrl Pts',(-5.63811983077158,4.0798110453911,24.8306344764173));
#46870=CARTESIAN_POINT('Ctrl Pts',(-5.63813667009515,4.07981103868737,24.7817551557504));
#46871=CARTESIAN_POINT('Ctrl Pts',(-5.63815433701764,4.07981101700637,24.7328765654611));
#46872=CARTESIAN_POINT('Ctrl Pts',(-5.63836268468167,4.07981142746535,24.1822792717705));
#46873=CARTESIAN_POINT('Ctrl Pts',(-5.63852065580303,4.07981535515741,23.1782346942006));
#46874=CARTESIAN_POINT('Ctrl Pts',(-5.63889205174658,4.07981527489587,21.1696456974601));
#46875=CARTESIAN_POINT('Ctrl Pts',(-5.64027572822364,4.07982496773713,19.6657188641483));
#46876=CARTESIAN_POINT('Ctrl Pts',(-5.64321826748117,4.07982890067983,18.4147685276945));
#46877=CARTESIAN_POINT('Ctrl Pts',(-5.64463005020993,4.07982928332439,17.9119667849834));
#46878=CARTESIAN_POINT('Ctrl Pts',(-5.6481745914777,4.07983135640826,16.9080407682842));
#46879=CARTESIAN_POINT('Ctrl Pts',(-5.65577873214206,4.07983263368459,15.154297247445));
#46880=CARTESIAN_POINT('Ctrl Pts',(-5.66299499426907,4.07985516961286,13.653069830235));
#46881=CARTESIAN_POINT('Ctrl Pts',(-5.66752169513739,4.07986678165392,12.3988381804721));
#46882=CARTESIAN_POINT('Ctrl Pts',(-5.66937274434828,4.07987093327248,11.89795019356));
#46883=CARTESIAN_POINT('Ctrl Pts',(-5.67314947714156,4.07987374563993,10.8961834958768));
#46884=CARTESIAN_POINT('Ctrl Pts',(-5.6778107271837,4.07989921039916,9.64402970194642));
#46885=CARTESIAN_POINT('Ctrl Pts',(-5.68273433584236,4.07991095381561,8.14009705099834));
#46886=CARTESIAN_POINT('Ctrl Pts',(-5.68515560070412,4.07994929304356,7.13553148672606));
#46887=CARTESIAN_POINT('Ctrl Pts',(-5.68628369286022,4.0799558810801,6.50905008299334));
#46888=CARTESIAN_POINT('Ctrl Pts',(-5.68661227828105,4.0821707734076,6.29061534047278));
#46889=CARTESIAN_POINT('Ctrl Pts',(-5.68685741652079,4.09404275133035,5.82395335480346));
#46890=CARTESIAN_POINT('Ctrl Pts',(-5.68640262743183,4.131057365138,4.98858149230052));
#46891=CARTESIAN_POINT('Ctrl Pts',(-5.68350530942708,4.23503160832966,3.2034216507204));
#46892=CARTESIAN_POINT('Ctrl Pts',(-5.68296470658803,4.24486610544271,1.49622009174376));
#46893=CARTESIAN_POINT('Ctrl Pts',(-5.68852203732585,4.04203039227358,0.212287520177693));
#46894=CARTESIAN_POINT('Ctrl Pts',(-5.68924321529777,4.01347849406751,0.046709235164253));
#46895=CARTESIAN_POINT('Ctrl Pts',(-5.69088416757088,3.9499993638592,-0.270911948875149));
#46896=CARTESIAN_POINT('Ctrl Pts',(-5.69423798732707,3.82032929950973,-0.816214955379421));
#46897=CARTESIAN_POINT('Ctrl Pts',(-5.70010751539234,3.59593446010334,-1.5531574030428));
#46898=CARTESIAN_POINT('Ctrl Pts',(-5.70831033464785,3.29442582652292,-2.38303934284124));
#46899=CARTESIAN_POINT('Ctrl Pts',(-5.72007629462961,2.8838231834602,-3.42257142321862));
#46900=CARTESIAN_POINT('Ctrl Pts',(-5.73560085827451,2.41218424234636,-4.60822872165754));
#46901=CARTESIAN_POINT('Ctrl Pts',(-5.74639098412996,2.18193168509263,-5.41705257416455));
#46902=CARTESIAN_POINT('Ctrl Pts',(-5.75084932986925,2.09939451036815,-5.86836611662692));
#46903=CARTESIAN_POINT('Ctrl Pts',(-5.75224887165708,2.06251312929618,-6.08806225844426));
#46904=CARTESIAN_POINT('Ctrl Pts',(-5.75455662346494,2.00400564527647,-6.51278227068597));
#46905=CARTESIAN_POINT('Ctrl Pts',(-5.75704323174046,1.92716346979754,-7.28481605243417));
#46906=CARTESIAN_POINT('Ctrl Pts',(-5.75728937144342,1.88443606838965,-8.43471994322465));
#46907=CARTESIAN_POINT('Ctrl Pts',(-5.75559647584818,1.88839172766654,-9.65933007796948));
#46908=CARTESIAN_POINT('Ctrl Pts',(-5.75460419604941,1.88968255320358,-10.551294966269));
#46909=CARTESIAN_POINT('Ctrl Pts',(-5.75422580639182,1.88549557238442,-11.0713987092988));
#46910=CARTESIAN_POINT('Ctrl Pts',(-5.75412343706888,1.88103143023836,-11.3349108742082));
#46911=CARTESIAN_POINT('Ctrl Pts',(-5.75408795885295,1.87647917972426,-11.5342224131919));
#46912=CARTESIAN_POINT('Ctrl Pts',(-5.75406875447422,1.87393821481755,-11.6531700417011));
#46913=CARTESIAN_POINT('Ctrl Pts',(-5.75399196516393,1.86932816043943,-11.8995959559439));
#46914=CARTESIAN_POINT('Ctrl Pts',(-5.7537833470847,1.86302260711046,-12.3268436624762));
#46915=CARTESIAN_POINT('Ctrl Pts',(-5.75309093117271,1.85632747869761,-13.1858188002743));
#46916=CARTESIAN_POINT('Ctrl Pts',(-5.75161172540509,1.86012550832003,-14.4176857778353));
#46917=CARTESIAN_POINT('Ctrl Pts',(-5.7502891758143,1.87006941090163,-15.5405400231519));
#46918=CARTESIAN_POINT('Ctrl Pts',(-5.74965739204831,1.87535308030911,-16.2967352293748));
#46919=CARTESIAN_POINT('Ctrl Pts',(-5.74932122610216,1.87823317940958,-16.8031330828915));
#46920=CARTESIAN_POINT('Ctrl Pts',(-5.74917455039559,1.879353507465,-17.185567783641));
#46921=CARTESIAN_POINT('Ctrl Pts',(-5.74913660367459,1.87935773662425,-17.5050226590233));
#46922=CARTESIAN_POINT('Ctrl Pts',(-5.74912715497621,1.87936050099831,-17.6290501583932));
#46923=CARTESIAN_POINT('Ctrl Pts',(-5.74912915980342,1.87936960977166,-17.8786570132928));
#46924=CARTESIAN_POINT('Ctrl Pts',(-5.74915993777671,1.87938259823583,-18.1278504175768));
#46925=CARTESIAN_POINT('Ctrl Pts',(-5.74921789244708,1.87939863353372,-18.3774774876771));
#46926=CARTESIAN_POINT('Ctrl Pts',(-5.74926434468946,1.87940930689548,-18.5334881547362));
#46927=CARTESIAN_POINT('Ctrl Pts',(-5.74930744438421,1.87941812042794,-18.6583586298963));
#46928=CARTESIAN_POINT('Ctrl Pts',(-5.74934257466472,1.87942477883083,-18.7520234824479));
#46929=CARTESIAN_POINT('Ctrl Pts',(-5.74937411282463,1.87943032838155,-18.8300954190059));
#46930=CARTESIAN_POINT('Ctrl Pts',(-5.74940066971533,1.87943474528755,-18.8925617257007));
#46931=CARTESIAN_POINT('Ctrl Pts',(-5.74963349497633,1.87947194613293,-19.4235781652291));
#46932=CARTESIAN_POINT('Ctrl Pts',(-5.75030680770628,1.87953828501115,-20.4403864579149));
#46933=CARTESIAN_POINT('Ctrl Pts',(-5.75154253932412,1.87937850948638,-21.9475145185662));
#46934=CARTESIAN_POINT('Ctrl Pts',(-5.75227231363554,1.8789637696449,-22.9561714893139));
#46935=CARTESIAN_POINT('Ctrl Pts',(-5.75260896559746,1.87855701901834,-23.5861600617612));
#46936=CARTESIAN_POINT('Ctrl Pts',(-5.75274090704472,1.8783738852912,-23.8356407747635));
#46937=CARTESIAN_POINT('Ctrl Pts',(-5.7530035915229,1.87793175921572,-24.3352573609035));
#46938=CARTESIAN_POINT('Ctrl Pts',(-5.75345623247728,1.87698444246526,-25.2113610809742));
#46939=CARTESIAN_POINT('Ctrl Pts',(-5.75410335253425,1.87529370544626,-26.466402231886));
#46940=CARTESIAN_POINT('Ctrl Pts',(-5.75485157533096,1.87319974044047,-27.9749319318986));
#46941=CARTESIAN_POINT('Ctrl Pts',(-5.75536475828074,1.8720902164559,-28.978520248079));
#46942=CARTESIAN_POINT('Ctrl Pts',(-5.75564477714037,1.87163363136333,-29.5435243172313));
#46943=CARTESIAN_POINT('Ctrl Pts',(-5.75572710239254,1.87079791844986,-29.6862583907702));
#46944=CARTESIAN_POINT('Ctrl Pts',(-5.7559732761709,1.86657647359971,-29.9590863694963));
#46945=CARTESIAN_POINT('Ctrl Pts',(-5.75660291355869,1.85331399580364,-30.4347040823306));
#46946=CARTESIAN_POINT('Ctrl Pts',(-5.75849635156875,1.80957603802193,-31.354691687085));
#46947=CARTESIAN_POINT('Ctrl Pts',(-5.76213394704484,1.73216882177498,-32.593021500266));
#46948=CARTESIAN_POINT('Ctrl Pts',(-5.76395912661161,1.71051409224138,-33.7231624390665));
#46949=CARTESIAN_POINT('Ctrl Pts',(-5.76191446825069,1.75882557122053,-34.5624086421025));
#46950=CARTESIAN_POINT('Ctrl Pts',(-5.75931374360727,1.80882201987154,-34.9615780699163));
#46951=CARTESIAN_POINT('Ctrl Pts',(-5.75661140344506,1.85745189559095,-35.2543857289109));
#46952=CARTESIAN_POINT('Ctrl Pts',(-5.75427502016558,1.89113913253961,-35.4252911706769));
#46953=CARTESIAN_POINT('Ctrl Pts',(-5.74877203670678,1.98604763646328,-35.8074191182881));
#46954=CARTESIAN_POINT('Ctrl Pts',(-5.73730659438168,2.21474178036547,-36.5234184675721));
#46955=CARTESIAN_POINT('Ctrl Pts',(-5.7120749720574,2.88286698981103,-38.1598829728828));
#46956=CARTESIAN_POINT('Ctrl Pts',(-5.69254673513104,3.60881415531633,-39.8324051191482));
#46957=CARTESIAN_POINT('Ctrl Pts',(-5.68452159299678,3.91054498186973,-41.4662679038483));
#46958=CARTESIAN_POINT('Ctrl Pts',(-5.68254013735191,3.97166842840602,-41.9074238116326));
#46959=CARTESIAN_POINT('Ctrl Pts',(-5.68068243579163,4.02453622596769,-42.4973296815815));
#46960=CARTESIAN_POINT('Ctrl Pts',(-5.67928607379443,4.0585773765675,-43.0709771707241));
#46961=CARTESIAN_POINT('Ctrl Pts',(-5.67830151490437,4.07413410278548,-43.7673981168678));
#46962=CARTESIAN_POINT('Ctrl Pts',(-5.6779462875509,4.06725357191368,-44.5648212529693));
#46963=CARTESIAN_POINT('Ctrl Pts',(-5.6780039507709,4.0541686872801,-45.1986001289027));
#46964=CARTESIAN_POINT('Ctrl Pts',(-5.67805168872495,4.04624934430059,-45.6863132704687));
#46965=CARTESIAN_POINT('Ctrl Pts',(-5.67804111261185,4.04319948342737,-46.0425841801101));
#46966=CARTESIAN_POINT('Ctrl Pts',(-5.6779325512445,4.04449142376855,-46.3890923889201));
#46967=CARTESIAN_POINT('Ctrl Pts',(-5.67758811612929,4.0537583517493,-46.8381819987723));
#46968=CARTESIAN_POINT('Ctrl Pts',(-5.67703248391526,4.07102816651889,-47.1600641227476));
#46969=CARTESIAN_POINT('Ctrl Pts',(-5.67617262740912,4.09736871655714,-47.4744092201946));
#46970=CARTESIAN_POINT('Ctrl Pts',(-5.67557902458743,4.11938395574063,-47.7362172898861));
#46971=CARTESIAN_POINT('Ctrl Pts',(-5.67432229286351,4.1615378138823,-48.2275780346156));
#46972=CARTESIAN_POINT('Ctrl Pts',(-5.67196155999899,4.2394187879887,-49.0946582274887));
#46973=CARTESIAN_POINT('Ctrl Pts',(-5.66822236433425,4.36555257025762,-50.3019818330166));
#46974=CARTESIAN_POINT('Ctrl Pts',(-5.66346122247667,4.56483521974948,-51.7190419955286));
#46975=CARTESIAN_POINT('Ctrl Pts',(-5.66031908717494,4.7432141219391,-52.6383322139147));
#46976=CARTESIAN_POINT('Ctrl Pts',(-5.65842641225892,4.87357529674077,-53.2078297316513));
#46977=CARTESIAN_POINT('Ctrl Pts',(-5.65763279334113,4.92930042573472,-53.443979103778));
#46978=CARTESIAN_POINT('Ctrl Pts',(-5.65595953066154,5.04680714972081,-53.9144063560435));
#46979=CARTESIAN_POINT('Ctrl Pts',(-5.65284695680694,5.27027637536506,-54.7428396598825));
#46980=CARTESIAN_POINT('Ctrl Pts',(-5.64627494076859,5.78265301008943,-56.4081584805099));
#46981=CARTESIAN_POINT('Ctrl Pts',(-5.64135921227858,6.32101790767107,-57.8424309602114));
#46982=CARTESIAN_POINT('Ctrl Pts',(-5.63949652665682,6.73547863584439,-58.8507904213972));
#46983=CARTESIAN_POINT('Ctrl Pts',(-5.63928653869847,6.78331076444176,-58.9656636362908));
#46984=CARTESIAN_POINT('Ctrl Pts',(-5.63890771027011,6.88360892110182,-59.2009780371113));
#46985=CARTESIAN_POINT('Ctrl Pts',(-5.63835540921954,7.0652864652122,-59.6132948878965));
#46986=CARTESIAN_POINT('Ctrl Pts',(-5.63764220325501,7.45537724520633,-60.4497076603056));
#46987=CARTESIAN_POINT('Ctrl Pts',(-5.63752431161293,7.94931941092904,-61.4228364605725));
#46988=CARTESIAN_POINT('Ctrl Pts',(-5.63770957434784,8.46920822877576,-62.407972028973));
#46989=CARTESIAN_POINT('Ctrl Pts',(-5.63785544356127,8.76684757852313,-62.9655179354984));
#46990=CARTESIAN_POINT('Ctrl Pts',(-5.63793954007321,8.96564323452173,-63.3384309712243));
#46991=CARTESIAN_POINT('Ctrl Pts',(-5.63799004492039,9.0981483133153,-63.587354346538));
#46992=CARTESIAN_POINT('Ctrl Pts',(-5.6380293700383,9.23040715162897,-63.8366888380974));
#46993=CARTESIAN_POINT('Ctrl Pts',(-5.63804839120191,9.34562407058914,-64.0552493238614));
#46994=CARTESIAN_POINT('Ctrl Pts',(-5.63805412223214,9.41126855868899,-64.1802491025035));
#46995=CARTESIAN_POINT('Ctrl Pts',(-5.63805717980536,9.50951176212536,-64.367843532021));
#46996=CARTESIAN_POINT('Ctrl Pts',(-5.6380475231002,9.59088940584664,-64.5244138604548));
#46997=CARTESIAN_POINT('Ctrl Pts',(-5.63801079305937,9.72455865382169,-64.7836590069625));
#46998=CARTESIAN_POINT('Ctrl Pts',(-5.63797762980282,9.85480612401591,-65.0353043348998));
#46999=CARTESIAN_POINT('Ctrl Pts',(-5.63792896814358,10.1198445789927,-65.5439043825807));
#47000=CARTESIAN_POINT('Ctrl Pts',(-5.63788600675246,10.5816154268398,-66.4217215340489));
#47001=CARTESIAN_POINT('Ctrl Pts',(-5.63793010151783,11.5088280393636,-68.1588933370336));
#47002=CARTESIAN_POINT('Ctrl Pts',(-5.63805867663479,12.3076693165761,-69.6377086440991));
#47003=CARTESIAN_POINT('Ctrl Pts',(-5.63806207846908,12.9112986908887,-70.7729897237731));
#47004=CARTESIAN_POINT('Ctrl Pts',(-5.63806259215821,13.0445160360343,-71.0235393008888));
#47005=CARTESIAN_POINT('Ctrl Pts',(-5.63806340997343,13.3116000922036,-71.5258574053085));
#47006=CARTESIAN_POINT('Ctrl Pts',(-5.63806407959717,13.6449599288231,-72.1528197375819));
#47007=CARTESIAN_POINT('Ctrl Pts',(-5.63806420954367,14.0449753198509,-72.9051395116483));
#47008=CARTESIAN_POINT('Ctrl Pts',(-5.63806367905351,14.8446200315156,-74.4090467420857));
#47009=CARTESIAN_POINT('Ctrl Pts',(-5.63806272604161,15.5105827584323,-75.6615270456325));
#47010=CARTESIAN_POINT('Ctrl Pts',(-5.63806304115205,16.480322977286,-77.4853422474358));
#47011=CARTESIAN_POINT('Ctrl Pts',(-5.63806320330682,16.9167987952306,-78.3062334097084));
#47012=CARTESIAN_POINT('Ctrl Pts',(-5.6380632033068,17.3533203826201,-79.1272111118068));
#47013=CARTESIAN_POINT('Ctrl Pts',(-3.13246153243128,4.07997651007201,24.8306346929376));
#47014=CARTESIAN_POINT('Ctrl Pts',(-3.13247089418538,4.07997650841963,24.7817553791099));
#47015=CARTESIAN_POINT('Ctrl Pts',(-3.13248073019575,4.0799764999824,24.7328768125166));
#47016=CARTESIAN_POINT('Ctrl Pts',(-3.13259608346308,4.07997670521336,24.182279036014));
#47017=CARTESIAN_POINT('Ctrl Pts',(-3.13268004192053,4.07997855846402,23.1782298566771));
#47018=CARTESIAN_POINT('Ctrl Pts',(-3.13288642205627,4.07997867910101,21.1696404964704));
#47019=CARTESIAN_POINT('Ctrl Pts',(-3.13364578221095,4.0799832324987,19.6657020199627));
#47020=CARTESIAN_POINT('Ctrl Pts',(-3.13527679700413,4.07998506525854,18.4147466082921));
#47021=CARTESIAN_POINT('Ctrl Pts',(-3.13606077657042,4.07998526998077,17.9119444889898));
#47022=CARTESIAN_POINT('Ctrl Pts',(-3.13802802788143,4.079986323548,16.9080154538795));
#47023=CARTESIAN_POINT('Ctrl Pts',(-3.14225142760585,4.07998710858101,15.1542683993348));
#47024=CARTESIAN_POINT('Ctrl Pts',(-3.14623899167219,4.07999743609788,13.6530130576789));
#47025=CARTESIAN_POINT('Ctrl Pts',(-3.14874291676554,4.08000231729095,12.3987670988987));
#47026=CARTESIAN_POINT('Ctrl Pts',(-3.14976743684663,4.08000400625095,11.8978751789854));
#47027=CARTESIAN_POINT('Ctrl Pts',(-3.15186309537897,4.08000461207694,10.8961027948064));
#47028=CARTESIAN_POINT('Ctrl Pts',(-3.15442891598582,4.08001544469706,9.64393077047484));
#47029=CARTESIAN_POINT('Ctrl Pts',(-3.15715276547804,4.08001919774166,8.13996416710522));
#47030=CARTESIAN_POINT('Ctrl Pts',(-3.15846279414889,4.08003674923533,7.13540126819946));
#47031=CARTESIAN_POINT('Ctrl Pts',(-3.15908062329773,4.08003816023285,6.50882474162827));
#47032=CARTESIAN_POINT('Ctrl Pts',(-3.15911526939308,4.08212367410461,6.28831552518569));
#47033=CARTESIAN_POINT('Ctrl Pts',(-3.15848048672026,4.09328390772445,5.81940001756711));
#47034=CARTESIAN_POINT('Ctrl Pts',(-3.15591326515943,4.12798838607392,4.98127924385807));
#47035=CARTESIAN_POINT('Ctrl Pts',(-3.14813166420412,4.22506805010056,3.1975816317331));
#47036=CARTESIAN_POINT('Ctrl Pts',(-3.14767244725756,4.23363944617766,1.50398696059777));
#47037=CARTESIAN_POINT('Ctrl Pts',(-3.16052292115839,4.04611907631244,0.233676737286712));
#47038=CARTESIAN_POINT('Ctrl Pts',(-3.16219766233936,4.01982942180956,0.0704551119528957));
#47039=CARTESIAN_POINT('Ctrl Pts',(-3.16602623261079,3.96123348196748,-0.243381219684303));
#47040=CARTESIAN_POINT('Ctrl Pts',(-3.17389848003272,3.84135099620151,-0.782942923159161));
#47041=CARTESIAN_POINT('Ctrl Pts',(-3.18779167569196,3.63307987540551,-1.51464036672391));
#47042=CARTESIAN_POINT('Ctrl Pts',(-3.20735638942522,3.35219275299679,-2.34117066500064));
#47043=CARTESIAN_POINT('Ctrl Pts',(-3.235439752456,2.96839254434012,-3.37911107320271));
#47044=CARTESIAN_POINT('Ctrl Pts',(-3.27229518195219,2.52562813688982,-4.56654235231478));
#47045=CARTESIAN_POINT('Ctrl Pts',(-3.29720237517238,2.30579650243325,-5.38435096611615));
#47046=CARTESIAN_POINT('Ctrl Pts',(-3.30756077574448,2.22596212631942,-5.84630274445772));
#47047=CARTESIAN_POINT('Ctrl Pts',(-3.31093007785766,2.19093741307251,-6.06793896740053));
#47048=CARTESIAN_POINT('Ctrl Pts',(-3.31658942747022,2.1351222476834,-6.49759373842264));
#47049=CARTESIAN_POINT('Ctrl Pts',(-3.32319163754923,2.06203087472526,-7.27678156850551));
#47050=CARTESIAN_POINT('Ctrl Pts',(-3.32558236466508,2.02145012095799,-8.43403990693677));
#47051=CARTESIAN_POINT('Ctrl Pts',(-3.32378280330904,2.02503484919292,-9.66070491288416));
#47052=CARTESIAN_POINT('Ctrl Pts',(-3.32287201840796,2.02613264416804,-10.5515289245055));
#47053=CARTESIAN_POINT('Ctrl Pts',(-3.3227346144408,2.02215742955986,-11.0701974470837));
#47054=CARTESIAN_POINT('Ctrl Pts',(-3.32284448389422,2.01795424274816,-11.332729479163));
#47055=CARTESIAN_POINT('Ctrl Pts',(-3.32301404466847,2.01367939488763,-11.53123457802));
#47056=CARTESIAN_POINT('Ctrl Pts',(-3.32313722498826,2.0112677782415,-11.6506787843114));
#47057=CARTESIAN_POINT('Ctrl Pts',(-3.32331103943599,2.00690467237838,-11.89748565759));
#47058=CARTESIAN_POINT('Ctrl Pts',(-3.32347258593085,2.00092018770441,-12.3256288866842));
#47059=CARTESIAN_POINT('Ctrl Pts',(-3.32325066510606,1.99451852403883,-13.1859183629539));
#47060=CARTESIAN_POINT('Ctrl Pts',(-3.32188896287377,1.99795361317701,-14.4189916107135));
#47061=CARTESIAN_POINT('Ctrl Pts',(-3.32036839223327,2.00719741951532,-15.5419137868954));
#47062=CARTESIAN_POINT('Ctrl Pts',(-3.31962915770245,2.0121124570523,-16.2977655403261));
#47063=CARTESIAN_POINT('Ctrl Pts',(-3.31924152176754,2.01479460229474,-16.8038237906487));
#47064=CARTESIAN_POINT('Ctrl Pts',(-3.31907592200134,2.0158314682654,-17.1858894679804));
#47065=CARTESIAN_POINT('Ctrl Pts',(-3.31905512549647,2.01583203163852,-17.5049792714126));
#47066=CARTESIAN_POINT('Ctrl Pts',(-3.31905012686686,2.01583245129892,-17.6290757830511));
#47067=CARTESIAN_POINT('Ctrl Pts',(-3.31905184801735,2.01583331426224,-17.8786891251921));
#47068=CARTESIAN_POINT('Ctrl Pts',(-3.31906757056976,2.0158323002434,-18.1279282353765));
#47069=CARTESIAN_POINT('Ctrl Pts',(-3.3191013384169,2.01583191589402,-18.3775666952059));
#47070=CARTESIAN_POINT('Ctrl Pts',(-3.31912836294918,2.0158310957928,-18.5335866639419));
#47071=CARTESIAN_POINT('Ctrl Pts',(-3.31915410127115,2.01583041472837,-18.6584601282889));
#47072=CARTESIAN_POINT('Ctrl Pts',(-3.31917520496812,2.01582976162608,-18.7521266979761));
#47073=CARTESIAN_POINT('Ctrl Pts',(-3.31919428468052,2.01582910533478,-18.8301989563573));
#47074=CARTESIAN_POINT('Ctrl Pts',(-3.31921051348002,2.01582854200645,-18.8926650096216));
#47075=CARTESIAN_POINT('Ctrl Pts',(-3.31935299454499,2.0158230802846,-19.4236763218564));
#47076=CARTESIAN_POINT('Ctrl Pts',(-3.31977038350789,2.01580030672302,-20.4403885523284));
#47077=CARTESIAN_POINT('Ctrl Pts',(-3.32075106855808,2.01570023176383,-21.9470893374715));
#47078=CARTESIAN_POINT('Ctrl Pts',(-3.32157181599372,2.01557941182674,-22.95528802852));
#47079=CARTESIAN_POINT('Ctrl Pts',(-3.32211753059002,2.01547700548503,-23.5849287034935));
#47080=CARTESIAN_POINT('Ctrl Pts',(-3.32234988652394,2.01543157385401,-23.8341936474416));
#47081=CARTESIAN_POINT('Ctrl Pts',(-3.32287360422468,2.0153254693473,-24.3334809007202));
#47082=CARTESIAN_POINT('Ctrl Pts',(-3.32391775778534,2.015101851755,-25.2091088476071));
#47083=CARTESIAN_POINT('Ctrl Pts',(-3.32568020140797,2.01471957590141,-26.4638705192032));
#47084=CARTESIAN_POINT('Ctrl Pts',(-3.32780197716411,2.01423265478938,-27.972595312808));
#47085=CARTESIAN_POINT('Ctrl Pts',(-3.32900799672057,2.01398247390041,-28.9767733412754));
#47086=CARTESIAN_POINT('Ctrl Pts',(-3.32953413642664,2.01387212968397,-29.5421018627301));
#47087=CARTESIAN_POINT('Ctrl Pts',(-3.3296939340843,2.01317464310576,-29.6836563222014));
#47088=CARTESIAN_POINT('Ctrl Pts',(-3.33017578351236,2.00938412158686,-29.9550375559271));
#47089=CARTESIAN_POINT('Ctrl Pts',(-3.3314167404306,1.99724251365359,-30.4282373494448));
#47090=CARTESIAN_POINT('Ctrl Pts',(-3.335147244172,1.95671829490059,-31.3455852780583));
#47091=CARTESIAN_POINT('Ctrl Pts',(-3.34221805110568,1.88426174339899,-32.5852768887308));
#47092=CARTESIAN_POINT('Ctrl Pts',(-3.34538128669468,1.86377396555026,-33.7243082369932));
#47093=CARTESIAN_POINT('Ctrl Pts',(-3.34072556069709,1.9101320036685,-34.5749221415604));
#47094=CARTESIAN_POINT('Ctrl Pts',(-3.33517800218729,1.95825190715931,-34.980815480244));
#47095=CARTESIAN_POINT('Ctrl Pts',(-3.32946088735476,2.00508871093003,-35.2788486519617));
#47096=CARTESIAN_POINT('Ctrl Pts',(-3.32456081222768,2.0379715366224,-35.4546634245683));
#47097=CARTESIAN_POINT('Ctrl Pts',(-3.31293460674144,2.12929789170878,-35.8433961205832));
#47098=CARTESIAN_POINT('Ctrl Pts',(-3.28853996207654,2.34714506486481,-36.5669426610266));
#47099=CARTESIAN_POINT('Ctrl Pts',(-3.23364031644196,2.97565071964737,-38.2060920481217));
#47100=CARTESIAN_POINT('Ctrl Pts',(-3.19027619222017,3.65154768324503,-39.8744107469863));
#47101=CARTESIAN_POINT('Ctrl Pts',(-3.17249759774021,3.92919268912927,-41.4864989281616));
#47102=CARTESIAN_POINT('Ctrl Pts',(-3.16803503881843,3.98560986978033,-41.924808302215));
#47103=CARTESIAN_POINT('Ctrl Pts',(-3.16371082319947,4.03374733958927,-42.50977881643));
#47104=CARTESIAN_POINT('Ctrl Pts',(-3.16036569044979,4.06439536447749,-43.0793682933223));
#47105=CARTESIAN_POINT('Ctrl Pts',(-3.15781356584725,4.0775254173288,-43.7715087583553));
#47106=CARTESIAN_POINT('Ctrl Pts',(-3.15660863415327,4.06967246134424,-44.565604580691));
#47107=CARTESIAN_POINT('Ctrl Pts',(-3.15650839641553,4.05658252237076,-45.1979952075419));
#47108=CARTESIAN_POINT('Ctrl Pts',(-3.1565435502555,4.04877553148677,-45.6854537913944));
#47109=CARTESIAN_POINT('Ctrl Pts',(-3.15654584245324,4.04580005442802,-46.041956843755));
#47110=CARTESIAN_POINT('Ctrl Pts',(-3.15642264233075,4.04709350286183,-46.3891292965313));
#47111=CARTESIAN_POINT('Ctrl Pts',(-3.15595207495515,4.05619279220323,-46.8396663700083));
#47112=CARTESIAN_POINT('Ctrl Pts',(-3.15513097215849,4.07310082458682,-47.1632866091112));
#47113=CARTESIAN_POINT('Ctrl Pts',(-3.15377542439868,4.09884678590371,-47.479707997432));
#47114=CARTESIAN_POINT('Ctrl Pts',(-3.15285511663029,4.12018476751298,-47.7411685674074));
#47115=CARTESIAN_POINT('Ctrl Pts',(-3.15096410426876,4.16112998813786,-48.2327556738879));
#47116=CARTESIAN_POINT('Ctrl Pts',(-3.14756930875271,4.23681882402646,-49.0995994041402));
#47117=CARTESIAN_POINT('Ctrl Pts',(-3.14267760636433,4.36001820587265,-50.306498772196));
#47118=CARTESIAN_POINT('Ctrl Pts',(-3.13732213977395,4.55632511369512,-51.7222573422902));
#47119=CARTESIAN_POINT('Ctrl Pts',(-3.13455778158426,4.73336117998014,-52.6403571490209));
#47120=CARTESIAN_POINT('Ctrl Pts',(-3.13319134074485,4.86313021560044,-53.2089975544419));
#47121=CARTESIAN_POINT('Ctrl Pts',(-3.13265006762838,4.9186361337781,-53.4447701301428));
#47122=CARTESIAN_POINT('Ctrl Pts',(-3.13165517397761,5.0358537111696,-53.9145483609616));
#47123=CARTESIAN_POINT('Ctrl Pts',(-3.13012078195967,5.25915546982874,-54.7420249668827));
#47124=CARTESIAN_POINT('Ctrl Pts',(-3.12782238958505,5.77235304821454,-56.4061734854649));
#47125=CARTESIAN_POINT('Ctrl Pts',(-3.12698248255127,6.31259359307923,-57.8405523875656));
#47126=CARTESIAN_POINT('Ctrl Pts',(-3.12685681546202,6.72814653701198,-58.849405680646));
#47127=CARTESIAN_POINT('Ctrl Pts',(-3.12686554296575,6.77604672446337,-58.9641874740558));
#47128=CARTESIAN_POINT('Ctrl Pts',(-3.12691057834388,6.87653925030669,-59.1994174594256));
#47129=CARTESIAN_POINT('Ctrl Pts',(-3.12707983102319,7.05858307805198,-59.6115712603959));
#47130=CARTESIAN_POINT('Ctrl Pts',(-3.12771527570457,7.44958961654466,-60.4477976005926));
#47131=CARTESIAN_POINT('Ctrl Pts',(-3.12891079783518,7.94484369168065,-61.4208959414217));
#47132=CARTESIAN_POINT('Ctrl Pts',(-3.13018924482141,8.46611794513808,-62.4061818623611));
#47133=CARTESIAN_POINT('Ctrl Pts',(-3.13087047740976,8.76452013934969,-62.9638769612226));
#47134=CARTESIAN_POINT('Ctrl Pts',(-3.13127832354795,8.96380018570062,-63.3369195977));
#47135=CARTESIAN_POINT('Ctrl Pts',(-3.13153624858351,9.09662106248193,-63.5859376992535));
#47136=CARTESIAN_POINT('Ctrl Pts',(-3.13176873496221,9.2291808216599,-63.83537918543));
#47137=CARTESIAN_POINT('Ctrl Pts',(-3.13194584755131,9.34464736072837,-64.0540456196372));
#47138=CARTESIAN_POINT('Ctrl Pts',(-3.13203856099171,9.41042981104675,-64.1791095351821));
#47139=CARTESIAN_POINT('Ctrl Pts',(-3.13216881558075,9.50887516367422,-64.366803852895));
#47140=CARTESIAN_POINT('Ctrl Pts',(-3.13225753513511,9.59040972990737,-64.5234650042444));
#47141=CARTESIAN_POINT('Ctrl Pts',(-3.13237482956374,9.72432258242432,-64.7828716127369));
#47142=CARTESIAN_POINT('Ctrl Pts',(-3.13248085500744,9.85477252074289,-65.034643864059));
#47143=CARTESIAN_POINT('Ctrl Pts',(-3.13264062512874,10.1201508479262,-65.5434924893009));
#47144=CARTESIAN_POINT('Ctrl Pts',(-3.1327947935228,10.5823097329533,-66.4216676465916));
#47145=CARTESIAN_POINT('Ctrl Pts',(-3.13272766180581,11.5096631589717,-68.1592918173623));
#47146=CARTESIAN_POINT('Ctrl Pts',(-3.13240624429524,12.3079906420031,-69.6379977184845));
#47147=CARTESIAN_POINT('Ctrl Pts',(-3.13241552222347,12.9114595629432,-70.7729642751072));
#47148=CARTESIAN_POINT('Ctrl Pts',(-3.13241753864319,13.0446909444888,-71.0235366909736));
#47149=CARTESIAN_POINT('Ctrl Pts',(-3.13242047804576,13.3117734755119,-71.5258470058919));
#47150=CARTESIAN_POINT('Ctrl Pts',(-3.13242201833982,13.6451400591592,-72.1528200751521));
#47151=CARTESIAN_POINT('Ctrl Pts',(-3.13242202368236,14.0451556384799,-72.9051405493436));
#47152=CARTESIAN_POINT('Ctrl Pts',(-3.13241896755619,14.8448005576505,-74.4090541744763));
#47153=CARTESIAN_POINT('Ctrl Pts',(-3.13241140148778,15.5107532458981,-75.6615314781162));
#47154=CARTESIAN_POINT('Ctrl Pts',(-3.13241038779428,16.4804882519172,-77.4853402167882));
#47155=CARTESIAN_POINT('Ctrl Pts',(-3.13240986624166,16.9169642383694,-78.3062334166578));
#47156=CARTESIAN_POINT('Ctrl Pts',(-3.13240986624168,17.3534858257588,-79.1272111187562));
#47157=CARTESIAN_POINT('Ctrl Pts',(-0.626489942748934,4.0801671767227,24.8306349417617));
#47158=CARTESIAN_POINT('Ctrl Pts',(-0.626491814773436,4.08016718222176,
24.7817556358665));
#47159=CARTESIAN_POINT('Ctrl Pts',(-0.626493779413045,4.08016720727904,
24.7328771092215));
#47160=CARTESIAN_POINT('Ctrl Pts',(-0.626516920716058,4.08016662587312,
24.182278353298));
#47161=CARTESIAN_POINT('Ctrl Pts',(-0.626534327747216,4.08016137226147,
23.1782203340369));
#47162=CARTESIAN_POINT('Ctrl Pts',(-0.626575654255332,4.08016124138042,
21.1696301744221));
#47163=CARTESIAN_POINT('Ctrl Pts',(-0.626729038647951,4.08014822905217,
19.6656695004389));
#47164=CARTESIAN_POINT('Ctrl Pts',(-0.627055871811892,4.08014275662489,
18.4147044193244));
#47165=CARTESIAN_POINT('Ctrl Pts',(-0.62721275050798,4.08014208569092,17.9119012894618));
#47166=CARTESIAN_POINT('Ctrl Pts',(-0.62760657371311,4.08013891698227,16.9079662909586));
#47167=CARTESIAN_POINT('Ctrl Pts',(-0.628451593361296,4.08013626969629,
15.1542125529137));
#47168=CARTESIAN_POINT('Ctrl Pts',(-0.62925243724752,4.08010618381641,13.6529049111324));
#47169=CARTESIAN_POINT('Ctrl Pts',(-0.629754803362929,4.08009117188779,
12.3986331440833));
#47170=CARTESIAN_POINT('Ctrl Pts',(-0.629960240843974,4.08008594873699,
11.897733474683));
#47171=CARTESIAN_POINT('Ctrl Pts',(-0.630379618087822,4.08008258640544,
10.8959534737225));
#47172=CARTESIAN_POINT('Ctrl Pts',(-0.630896102434399,4.08005075094835,
9.64374037929921));
#47173=CARTESIAN_POINT('Ctrl Pts',(-0.631442292110968,4.08003511285241,
8.13972854909915));
#47174=CARTESIAN_POINT('Ctrl Pts',(-0.631709402747086,4.0799883832829,7.13513557854196));
#47175=CARTESIAN_POINT('Ctrl Pts',(-0.631834242062847,4.07997432028845,
6.50844855969211));
#47176=CARTESIAN_POINT('Ctrl Pts',(-0.631844614514806,4.08191249849963,
6.28569231433929));
#47177=CARTESIAN_POINT('Ctrl Pts',(-0.631735142604194,4.09228480802917,
5.81433836489286));
#47178=CARTESIAN_POINT('Ctrl Pts',(-0.631274195858156,4.12442247278467,
4.97319700222089));
#47179=CARTESIAN_POINT('Ctrl Pts',(-0.629860619545034,4.21411506066098,
3.19112813899561));
#47180=CARTESIAN_POINT('Ctrl Pts',(-0.629791657573271,4.22109561476111,
1.51180927237363));
#47181=CARTESIAN_POINT('Ctrl Pts',(-0.632171170914168,4.04961537706138,
0.256602357936203));
#47182=CARTESIAN_POINT('Ctrl Pts',(-0.632480675376951,4.02569735160545,
0.0960267302433405));
#47183=CARTESIAN_POINT('Ctrl Pts',(-0.633192562617259,3.97225933444396,
-0.213513276617349));
#47184=CARTESIAN_POINT('Ctrl Pts',(-0.634665809148591,3.86280982150925,
-0.746439893912946));
#47185=CARTESIAN_POINT('Ctrl Pts',(-0.637309271984396,3.67201501892076,
-1.47185578101335));
#47186=CARTESIAN_POINT('Ctrl Pts',(-0.641060370430275,3.41398006846141,
-2.29439316562927));
#47187=CARTESIAN_POINT('Ctrl Pts',(-0.646459524138124,3.0603623086103,-3.33078441011147));
#47188=CARTESIAN_POINT('Ctrl Pts',(-0.653388431714947,2.65109651410505,
-4.52187255833751));
#47189=CARTESIAN_POINT('Ctrl Pts',(-0.657692228357949,2.44619870872637,
-5.35101148090401));
#47190=CARTESIAN_POINT('Ctrl Pts',(-0.659392538492093,2.37141568249575,
-5.82433526064073));
#47191=CARTESIAN_POINT('Ctrl Pts',(-0.659974674390838,2.33899498785793,
-6.04804706925782));
#47192=CARTESIAN_POINT('Ctrl Pts',(-0.660931900586046,2.28720350004628,
-6.4828345029374));
#47193=CARTESIAN_POINT('Ctrl Pts',(-0.662055433531732,2.21949663209103,
-7.26920638472244));
#47194=CARTESIAN_POINT('Ctrl Pts',(-0.662459190736586,2.18173152333761,
-8.43357231943025));
#47195=CARTESIAN_POINT('Ctrl Pts',(-0.662129105637019,2.18458676173904,
-9.66218372788113));
#47196=CARTESIAN_POINT('Ctrl Pts',(-0.661950743587544,2.18532888680784,
-10.5518893013257));
#47197=CARTESIAN_POINT('Ctrl Pts',(-0.661920949871916,2.18155228774363,
-11.0691565471711));
#47198=CARTESIAN_POINT('Ctrl Pts',(-0.661939777952425,2.1776415075515,-11.3307324556826));
#47199=CARTESIAN_POINT('Ctrl Pts',(-0.661970318081918,2.17368544069136,
-11.528452907198));
#47200=CARTESIAN_POINT('Ctrl Pts',(-0.661990145017018,2.17143769689881,
-11.6483872617774));
#47201=CARTESIAN_POINT('Ctrl Pts',(-0.662018178672468,2.16737085478223,
-11.8955738266779));
#47202=CARTESIAN_POINT('Ctrl Pts',(-0.662041705006974,2.16176155662304,
-12.3246017479885));
#47203=CARTESIAN_POINT('Ctrl Pts',(-0.661995639177148,2.15563339321882,
-13.186166875794));
#47204=CARTESIAN_POINT('Ctrl Pts',(-0.661743624243537,2.15842740530346,
-14.4204024640238));
#47205=CARTESIAN_POINT('Ctrl Pts',(-0.661466000143103,2.16664586238682,
-15.5433657694493));
#47206=CARTESIAN_POINT('Ctrl Pts',(-0.661331657161525,2.17103469169633,
-16.2988620090364));
#47207=CARTESIAN_POINT('Ctrl Pts',(-0.661260755828687,2.17343601808264,
-16.8045796697433));
#47208=CARTESIAN_POINT('Ctrl Pts',(-0.661232601289069,2.17435470474185,
-17.1862644825228));
#47209=CARTESIAN_POINT('Ctrl Pts',(-0.661229808429,2.17434774916163,-17.504987389934));
#47210=CARTESIAN_POINT('Ctrl Pts',(-0.661229375315021,2.17434446174097,
-17.6291628974737));
#47211=CARTESIAN_POINT('Ctrl Pts',(-0.661231038625573,2.17433502257422,
-17.8787952656615));
#47212=CARTESIAN_POINT('Ctrl Pts',(-0.661236308189677,2.17431832730332,
-18.1280903669047));
#47213=CARTESIAN_POINT('Ctrl Pts',(-0.661245023730644,2.17430181783555,
-18.3777490651285));
#47214=CARTESIAN_POINT('Ctrl Pts',(-0.661251840931363,2.17429020416771,
-18.5337827354254));
#47215=CARTESIAN_POINT('Ctrl Pts',(-0.66125807792693,2.17428113906084,-18.6586623836088));
#47216=CARTESIAN_POINT('Ctrl Pts',(-0.661263144357075,2.17427422324021,
-18.7523327597983));
#47217=CARTESIAN_POINT('Ctrl Pts',(-0.661267684128452,2.17426842469942,
-18.8304068037653));
#47218=CARTESIAN_POINT('Ctrl Pts',(-0.661271499064604,2.17426388385676,
-18.8928736980894));
#47219=CARTESIAN_POINT('Ctrl Pts',(-0.661304869403966,2.17422491496471,
-19.4238879371911));
#47220=CARTESIAN_POINT('Ctrl Pts',(-0.661408696326335,2.1741421121425,-20.4404752420419));
#47221=CARTESIAN_POINT('Ctrl Pts',(-0.661612851666169,2.17427137833039,
-21.9466489991897));
#47222=CARTESIAN_POINT('Ctrl Pts',(-0.661780504171708,2.17465166882404,
-22.9542604711863));
#47223=CARTESIAN_POINT('Ctrl Pts',(-0.661879102679922,2.17503052377509,
-23.5834625714101));
#47224=CARTESIAN_POINT('Ctrl Pts',(-0.661919681293023,2.17520111792069,
-23.8324682152386));
#47225=CARTESIAN_POINT('Ctrl Pts',(-0.662010577041759,2.17561554973492,
-24.3313537864961));
#47226=CARTESIAN_POINT('Ctrl Pts',(-0.662187905112522,2.17650319209165,
-25.2064036746852));
#47227=CARTESIAN_POINT('Ctrl Pts',(-0.662493004231223,2.17811119590231,
-26.4607956985645));
#47228=CARTESIAN_POINT('Ctrl Pts',(-0.662845425188931,2.1800960472974,-27.969739115956));
#47229=CARTESIAN_POINT('Ctrl Pts',(-0.663056991857019,2.18117899739333,
-28.9745709795876));
#47230=CARTESIAN_POINT('Ctrl Pts',(-0.663146177495585,2.18161630695882,
-29.5402963951528));
#47231=CARTESIAN_POINT('Ctrl Pts',(-0.663174331064102,2.18110727130679,
-29.6807158367692));
#47232=CARTESIAN_POINT('Ctrl Pts',(-0.663261355597737,2.17788395250686,
-29.9507176610373));
#47233=CARTESIAN_POINT('Ctrl Pts',(-0.663488486205343,2.16718741222019,
-30.4216090598993));
#47234=CARTESIAN_POINT('Ctrl Pts',(-0.664171713171707,2.13081229108742,
-31.3364747557897));
#47235=CARTESIAN_POINT('Ctrl Pts',(-0.665424904517377,2.06516675737071,
-32.5775794288945));
#47236=CARTESIAN_POINT('Ctrl Pts',(-0.665939168101847,2.04682008967083,
-33.724921159572));
#47237=CARTESIAN_POINT('Ctrl Pts',(-0.665151885456072,2.08990577602317,
-34.5863090658768));
#47238=CARTESIAN_POINT('Ctrl Pts',(-0.664231052307106,2.13458516649471,
-34.9988077951298));
#47239=CARTESIAN_POINT('Ctrl Pts',(-0.663286717012051,2.17810461561118,
-35.3021916075847));
#47240=CARTESIAN_POINT('Ctrl Pts',(-0.662504202219517,2.20886847117035,
-35.4831201754591));
#47241=CARTESIAN_POINT('Ctrl Pts',(-0.660573758768274,2.29385816431863,
-35.879283915027));
#47242=CARTESIAN_POINT('Ctrl Pts',(-0.656358451963326,2.49604065491868,
-36.6124714084662));
#47243=CARTESIAN_POINT('Ctrl Pts',(-0.646125278213893,3.07686033436265,
-38.2580869723516));
#47244=CARTESIAN_POINT('Ctrl Pts',(-0.637514600615515,3.69735238323864,
-39.9207196729455));
#47245=CARTESIAN_POINT('Ctrl Pts',(-0.634131214466014,3.94947125472227,
-41.5084348507479));
#47246=CARTESIAN_POINT('Ctrl Pts',(-0.633299524802236,4.00082265203612,
-41.9436263914889));
#47247=CARTESIAN_POINT('Ctrl Pts',(-0.632497763223773,4.04390306304625,
-42.5232040466185));
#47248=CARTESIAN_POINT('Ctrl Pts',(-0.631877942908767,4.07091687109544,
-43.0884028834181));
#47249=CARTESIAN_POINT('Ctrl Pts',(-0.631403866133522,4.08143863771991,
-43.7759368949309));
#47250=CARTESIAN_POINT('Ctrl Pts',(-0.631173823256158,4.07251593555644,
-44.5664798657698));
#47251=CARTESIAN_POINT('Ctrl Pts',(-0.631144921188736,4.05940256355705,
-45.1974103929395));
#47252=CARTESIAN_POINT('Ctrl Pts',(-0.631151658052729,4.0516753068334,-45.6846131613201));
#47253=CARTESIAN_POINT('Ctrl Pts',(-0.631151885609456,4.04874981742623,
-46.0413830804863));
#47254=CARTESIAN_POINT('Ctrl Pts',(-0.63112949477881,4.05001188630386,-46.3892896948824));
#47255=CARTESIAN_POINT('Ctrl Pts',(-0.631047652199094,4.05887470331206,
-46.8414111240637));
#47256=CARTESIAN_POINT('Ctrl Pts',(-0.630894301455481,4.0753520081225,-47.1669327535106));
#47257=CARTESIAN_POINT('Ctrl Pts',(-0.630651332879306,4.10039201692055,
-47.4856239270558));
#47258=CARTESIAN_POINT('Ctrl Pts',(-0.630487551701003,4.12096948175222,
-47.7467517270561));
#47259=CARTESIAN_POINT('Ctrl Pts',(-0.630154495654072,4.16053412003427,
-48.2386420047998));
#47260=CARTESIAN_POINT('Ctrl Pts',(-0.62956310707126,4.23372113623803,-49.1053130915966));
#47261=CARTESIAN_POINT('Ctrl Pts',(-0.628705658823615,4.35357045286472,
-50.3117921743022));
#47262=CARTESIAN_POINT('Ctrl Pts',(-0.627777228097765,4.54650043282676,
-51.7260360891742));
#47263=CARTESIAN_POINT('Ctrl Pts',(-0.627265563061771,4.72202453586099,
-52.6426923320876));
#47264=CARTESIAN_POINT('Ctrl Pts',(-0.627007232715583,4.85111897731866,
-53.21028566008));
#47265=CARTESIAN_POINT('Ctrl Pts',(-0.626905395879994,4.90637750017685,
-53.4456175769788));
#47266=CARTESIAN_POINT('Ctrl Pts',(-0.626712820260931,5.02326501300372,
-53.9146294532301));
#47267=CARTESIAN_POINT('Ctrl Pts',(-0.626400013410281,5.2463741033518,-54.740988576581));
#47268=CARTESIAN_POINT('Ctrl Pts',(-0.625884681626927,5.76048931055464,
-56.4037876031312));
#47269=CARTESIAN_POINT('Ctrl Pts',(-0.625628602711532,6.30290639745082,
-57.8383262442653));
#47270=CARTESIAN_POINT('Ctrl Pts',(-0.62556760393444,6.71972642508893,-58.8477735636256));
#47271=CARTESIAN_POINT('Ctrl Pts',(-0.625565074343473,6.76770295818769,
-58.9624515883609));
#47272=CARTESIAN_POINT('Ctrl Pts',(-0.625564963139768,6.86841667036773,
-59.1975883170748));
#47273=CARTESIAN_POINT('Ctrl Pts',(-0.625582440524659,7.05087714573764,
-59.6095610877));
#47274=CARTESIAN_POINT('Ctrl Pts',(-0.625673206560115,7.44292862931509,
-60.4455864505415));
#47275=CARTESIAN_POINT('Ctrl Pts',(-0.625872074682469,7.93968636878086,
-61.4186616931697));
#47276=CARTESIAN_POINT('Ctrl Pts',(-0.626087693556141,8.46255259730151,
-62.4041259227318));
#47277=CARTESIAN_POINT('Ctrl Pts',(-0.626202559137751,8.76183196942706,
-62.9619931718646));
#47278=CARTESIAN_POINT('Ctrl Pts',(-0.626271105041649,8.96166958627571,
-63.3351844249496));
#47279=CARTESIAN_POINT('Ctrl Pts',(-0.626314051407471,9.09485393613067,
-63.5843109543157));
#47280=CARTESIAN_POINT('Ctrl Pts',(-0.626353422975541,9.22776053699843,
-63.8338747428221));
#47281=CARTESIAN_POINT('Ctrl Pts',(-0.626382660366308,9.34351472712429,
-64.0526621517202));
#47282=CARTESIAN_POINT('Ctrl Pts',(-0.626397882303084,9.40945620428944,
-64.1777992852074));
#47283=CARTESIAN_POINT('Ctrl Pts',(-0.626419095447353,9.50813458955278,
-64.3656076235132));
#47284=CARTESIAN_POINT('Ctrl Pts',(-0.626433803134328,9.58985026494963,
-64.5223724391017));
#47285=CARTESIAN_POINT('Ctrl Pts',(-0.62645237198052,9.72404424936194,-64.781963414885));
#47286=CARTESIAN_POINT('Ctrl Pts',(-0.626469427968082,9.85472875964012,
-65.0338821160099));
#47287=CARTESIAN_POINT('Ctrl Pts',(-0.62649494875858,10.120500285871,-65.5430168405376));
#47288=CARTESIAN_POINT('Ctrl Pts',(-0.626521563386984,10.583108636538,-66.4216051356352));
#47289=CARTESIAN_POINT('Ctrl Pts',(-0.626514660886955,11.5106242457288,
-68.159752861177));
#47290=CARTESIAN_POINT('Ctrl Pts',(-0.626471931535449,12.3083591820501,
-69.6383321739738));
#47291=CARTESIAN_POINT('Ctrl Pts',(-0.626475713088361,12.9116431096455,
-70.772934983678));
#47292=CARTESIAN_POINT('Ctrl Pts',(-0.62647610542718,13.0448906637832,-71.0235337534905));
#47293=CARTESIAN_POINT('Ctrl Pts',(-0.626476804845756,13.3119713946603,
-71.5258349837059));
#47294=CARTESIAN_POINT('Ctrl Pts',(-0.626477660859164,13.6453459070808,
-72.1528203904278));
#47295=CARTESIAN_POINT('Ctrl Pts',(-0.626477922591584,14.0453617548795,
-72.9051416022612));
#47296=CARTESIAN_POINT('Ctrl Pts',(-0.626477840681796,14.8450070813496,
-74.4090625301667));
#47297=CARTESIAN_POINT('Ctrl Pts',(-0.626478397258742,15.5109489945228,
-75.6615364417598));
#47298=CARTESIAN_POINT('Ctrl Pts',(-0.626479385432316,16.4806784860373,
-77.4853378891171));
#47299=CARTESIAN_POINT('Ctrl Pts',(-0.626479894410933,16.9171548624124,
-78.306233408562));
#47300=CARTESIAN_POINT('Ctrl Pts',(-0.626479894410927,17.3536764498018,
-79.1272111106602));
#47301=CARTESIAN_POINT('Ctrl Pts',(1.87947659458304,4.08007594746654,24.8306348252651));
#47302=CARTESIAN_POINT('Ctrl Pts',(1.87948221099211,4.08007594968897,24.7817555155472));
#47303=CARTESIAN_POINT('Ctrl Pts',(1.87948805643874,4.08007595214576,24.7328769635291));
#47304=CARTESIAN_POINT('Ctrl Pts',(1.87955912761084,4.08007597527773,24.1822788856086));
#47305=CARTESIAN_POINT('Ctrl Pts',(1.87962507094508,4.08007601162104,23.1782268448629));
#47306=CARTESIAN_POINT('Ctrl Pts',(1.87975055067327,4.08007620678542,21.1696372570538));
#47307=CARTESIAN_POINT('Ctrl Pts',(1.88024483547882,4.08007630445103,19.6656915530713));
#47308=CARTESIAN_POINT('Ctrl Pts',(1.88124023009051,4.08007640018488,18.4147329928714));
#47309=CARTESIAN_POINT('Ctrl Pts',(1.88171316333228,4.08007647531142,17.9119306359609));
#47310=CARTESIAN_POINT('Ctrl Pts',(1.88290437608708,4.08007669263161,16.9079997217721));
#47311=CARTESIAN_POINT('Ctrl Pts',(1.88544967491957,4.08007715433846,15.1542504685811));
#47312=CARTESIAN_POINT('Ctrl Pts',(1.88793047536297,4.08007721488852,13.6529777849061));
#47313=CARTESIAN_POINT('Ctrl Pts',(1.88947377904792,4.08007674283328,12.3987229743159));
#47314=CARTESIAN_POINT('Ctrl Pts',(1.8901022907834,4.08007652487329,11.8978285550643));
#47315=CARTESIAN_POINT('Ctrl Pts',(1.89136530752485,4.08007577694653,10.8960528593377));
#47316=CARTESIAN_POINT('Ctrl Pts',(1.89299043191257,4.08007482542856,9.64386894862191));
#47317=CARTESIAN_POINT('Ctrl Pts',(1.89465944971945,4.08007271810909,8.13988290786252));
#47318=CARTESIAN_POINT('Ctrl Pts',(1.8955778547512,4.0800729105106,7.13531874534234));
#47319=CARTESIAN_POINT('Ctrl Pts',(1.89598038811047,4.08007012513435,6.50868913529077));
#47320=CARTESIAN_POINT('Ctrl Pts',(1.89601487495568,4.0820814863956,6.28703299979524));
#47321=CARTESIAN_POINT('Ctrl Pts',(1.89567557410536,4.09284104044257,5.81687291560801));
#47322=CARTESIAN_POINT('Ctrl Pts',(1.89432085510484,4.12624777332536,4.97722214089179));
#47323=CARTESIAN_POINT('Ctrl Pts',(1.88997973046473,4.21956716125387,3.19436157629692));
#47324=CARTESIAN_POINT('Ctrl Pts',(1.89051464550626,4.2274313393854,1.50818455468003));
#47325=CARTESIAN_POINT('Ctrl Pts',(1.89814047422308,4.04814526942004,0.24558502820507));
#47326=CARTESIAN_POINT('Ctrl Pts',(1.89909636332055,4.02306735979135,0.0837071483672661));
#47327=CARTESIAN_POINT('Ctrl Pts',(1.90131393495655,3.96710837696693,-0.227949918977011));
#47328=CARTESIAN_POINT('Ctrl Pts',(1.90587879504138,3.85255773904514,-0.764156068895517));
#47329=CARTESIAN_POINT('Ctrl Pts',(1.91420954102354,3.65323868491061,-1.49269331038278));
#47330=CARTESIAN_POINT('Ctrl Pts',(1.92566809001345,3.38408538280297,-2.31724895313642));
#47331=CARTESIAN_POINT('Ctrl Pts',(1.94250971673815,3.01590503454656,-3.35448813837129));
#47332=CARTESIAN_POINT('Ctrl Pts',(1.96404049201351,2.5907524101948,-4.543864836452));
#47333=CARTESIAN_POINT('Ctrl Pts',(1.97858408945532,2.37892223453074,-5.36738331377946));
#47334=CARTESIAN_POINT('Ctrl Pts',(1.98431559394949,2.301777985992,-5.83505938258291));
#47335=CARTESIAN_POINT('Ctrl Pts',(1.98619310963592,2.26812487877299,-6.05774566153013));
#47336=CARTESIAN_POINT('Ctrl Pts',(1.98933774331585,2.21443117732476,-6.48999499635696));
#47337=CARTESIAN_POINT('Ctrl Pts',(1.99312146425114,2.14417478968173,-7.27282828987392));
#47338=CARTESIAN_POINT('Ctrl Pts',(1.99484765517173,2.10508432184969,-8.43371821930893));
#47339=CARTESIAN_POINT('Ctrl Pts',(1.99424722760277,2.10829809461501,-9.6613988767828));
#47340=CARTESIAN_POINT('Ctrl Pts',(1.99381843790417,2.10921397899,-10.5516621456655));
#47341=CARTESIAN_POINT('Ctrl Pts',(1.99377849010985,2.10534531638977,-11.0696232807361));
#47342=CARTESIAN_POINT('Ctrl Pts',(1.99385757119846,2.10129650540405,-11.3316723035792));
#47343=CARTESIAN_POINT('Ctrl Pts',(1.99396021712955,2.09718960351093,-11.5297803969733));
#47344=CARTESIAN_POINT('Ctrl Pts',(1.99402955970695,2.09486460711147,-11.6494722329179));
#47345=CARTESIAN_POINT('Ctrl Pts',(1.99412849328614,2.09065807860872,-11.8964705807442));
#47346=CARTESIAN_POINT('Ctrl Pts',(1.99422975986236,2.08487238506963,-12.3250611021437));
#47347=CARTESIAN_POINT('Ctrl Pts',(1.99420175990704,2.07861770114086,-13.1860047724658));
#47348=CARTESIAN_POINT('Ctrl Pts',(1.99355029263019,2.08171997518577,-14.4196756638712));
#47349=CARTESIAN_POINT('Ctrl Pts',(1.99277695148483,2.09042777614687,-15.5426265039093));
#47350=CARTESIAN_POINT('Ctrl Pts',(1.99239862064165,2.09506734930592,-16.2983011418255));
#47351=CARTESIAN_POINT('Ctrl Pts',(1.99218242082944,2.09760234861235,-16.8041858254556));
#47352=CARTESIAN_POINT('Ctrl Pts',(1.99212726152234,2.09857751742776,-17.1860629660676));
#47353=CARTESIAN_POINT('Ctrl Pts',(1.99212324243369,2.09857411333236,-17.5049672230762));
#47354=CARTESIAN_POINT('Ctrl Pts',(1.99212260694304,2.09857258119165,-17.629102871608));
#47355=CARTESIAN_POINT('Ctrl Pts',(1.99212711575014,2.09856799767051,-17.8787244471707));
#47356=CARTESIAN_POINT('Ctrl Pts',(1.99214707955899,2.09855884278737,-18.1279914322703));
#47357=CARTESIAN_POINT('Ctrl Pts',(1.99217121064863,2.09854993548065,-18.3776388365096));
#47358=CARTESIAN_POINT('Ctrl Pts',(1.99219109351607,2.09854343429611,-18.5336651340886));
#47359=CARTESIAN_POINT('Ctrl Pts',(1.99220833699324,2.09853830249942,-18.6585410991645));
#47360=CARTESIAN_POINT('Ctrl Pts',(1.99222244021897,2.09853432338726,-18.7522091484825));
#47361=CARTESIAN_POINT('Ctrl Pts',(1.99223512176153,2.09853093513328,-18.8302819559127));
#47362=CARTESIAN_POINT('Ctrl Pts',(1.9922456377348,2.09852824720193,-18.8927481245961));
#47363=CARTESIAN_POINT('Ctrl Pts',(1.99233906194416,2.09850488269869,-19.423758499618));
#47364=CARTESIAN_POINT('Ctrl Pts',(1.99263748504989,2.09845420519683,-20.4404115015207));
#47365=CARTESIAN_POINT('Ctrl Pts',(1.99324071658104,2.0984714180227,-21.9468464155744));
#47366=CARTESIAN_POINT('Ctrl Pts',(1.99372053067635,2.09861418681217,-22.9547557228035));
#47367=CARTESIAN_POINT('Ctrl Pts',(1.99402170436847,2.0987614672874,-23.5841774312742));
#47368=CARTESIAN_POINT('Ctrl Pts',(1.99414888338287,2.09882784153572,-23.8333094826695));
#47369=CARTESIAN_POINT('Ctrl Pts',(1.99442808139027,2.09899124156944,-24.3323927034768));
#47370=CARTESIAN_POINT('Ctrl Pts',(1.9949894335052,2.09934240565073,-25.207726496462));
#47371=CARTESIAN_POINT('Ctrl Pts',(1.99586532682244,2.09998984977607,-26.4623110682351));
#47372=CARTESIAN_POINT('Ctrl Pts',(1.99696734244082,2.10077165076235,-27.9711556415455));
#47373=CARTESIAN_POINT('Ctrl Pts',(1.99748202186661,2.10120441087972,-28.9756868843356));
#47374=CARTESIAN_POINT('Ctrl Pts',(1.99773809301026,2.10137348076256,-29.5412243672071));
#47375=CARTESIAN_POINT('Ctrl Pts',(1.99782461908708,2.10077377950784,-29.6822068893583));
#47376=CARTESIAN_POINT('Ctrl Pts',(1.99809062042496,2.09727817819766,-29.9528940217472));
#47377=CARTESIAN_POINT('Ctrl Pts',(1.99876117898229,2.08588995074677,-30.424934709598));
#47378=CARTESIAN_POINT('Ctrl Pts',(2.00080463385646,2.04753260577408,-31.341042499164));
#47379=CARTESIAN_POINT('Ctrl Pts',(2.00443833713365,1.97863167455129,-32.5814847638249));
#47380=CARTESIAN_POINT('Ctrl Pts',(2.00575704994606,1.95924823295857,-33.7247553979965));
#47381=CARTESIAN_POINT('Ctrl Pts',(2.00310055141625,2.00388697303159,-34.5808237926425));
#47382=CARTESIAN_POINT('Ctrl Pts',(1.99994623957741,2.05019955009036,-34.9900584642322));
#47383=CARTESIAN_POINT('Ctrl Pts',(1.99683464745504,2.0952884493422,-35.2907818633749));
#47384=CARTESIAN_POINT('Ctrl Pts',(1.99420955065897,2.12704744684203,-35.4691589148058));
#47385=CARTESIAN_POINT('Ctrl Pts',(1.98793892913517,2.215006136549,-35.8616030816837));
#47386=CARTESIAN_POINT('Ctrl Pts',(1.9741086581221,2.42449271247474,-36.5899729258883));
#47387=CARTESIAN_POINT('Ctrl Pts',(1.94235791924633,3.02780501619578,-38.2325436184006));
#47388=CARTESIAN_POINT('Ctrl Pts',(1.91493319356227,3.67522197999023,-39.8980747271658));
#47389=CARTESIAN_POINT('Ctrl Pts',(1.90390518409755,3.93974100445547,-41.4977896434242));
#47390=CARTESIAN_POINT('Ctrl Pts',(1.90123344083393,3.99355337234143,-41.9345096696509));
#47391=CARTESIAN_POINT('Ctrl Pts',(1.89871335543755,4.03909746335217,-42.5167344189122));
#47392=CARTESIAN_POINT('Ctrl Pts',(1.89673229126996,4.06787736429817,-43.0840821363168));
#47393=CARTESIAN_POINT('Ctrl Pts',(1.89519489619482,4.07966267988032,-43.7738675543103));
#47394=CARTESIAN_POINT('Ctrl Pts',(1.89438522140316,4.07124691226921,-44.5661414710187));
#47395=CARTESIAN_POINT('Ctrl Pts',(1.89418118018047,4.05812745696965,-45.1977774831885));
#47396=CARTESIAN_POINT('Ctrl Pts',(1.8941899847956,4.05035676149492,-45.6851056130695));
#47397=CARTESIAN_POINT('Ctrl Pts',(1.89417050151014,4.04740249946183,-46.0417443946409));
#47398=CARTESIAN_POINT('Ctrl Pts',(1.89407717984001,4.04867558437408,-46.3892911665539));
#47399=CARTESIAN_POINT('Ctrl Pts',(1.89380533637415,4.0576506306873,-46.8406378683643));
#47400=CARTESIAN_POINT('Ctrl Pts',(1.89326484112894,4.07433109677534,-47.16522580503));
#47401=CARTESIAN_POINT('Ctrl Pts',(1.89248217238794,4.0997139568233,-47.4828054835067));
#47402=CARTESIAN_POINT('Ctrl Pts',(1.89195427391836,4.12065987577668,-47.7440998580142));
#47403=CARTESIAN_POINT('Ctrl Pts',(1.8908787918323,4.16089174064189,-48.235845718434));
#47404=CARTESIAN_POINT('Ctrl Pts',(1.88894392970756,4.23527963439326,-49.1026062613519));
#47405=CARTESIAN_POINT('Ctrl Pts',(1.88608565034801,4.35671213750319,-50.3092845028095));
#47406=CARTESIAN_POINT('Ctrl Pts',(1.88303048014428,4.55121233841588,-51.7242608361643));
#47407=CARTESIAN_POINT('Ctrl Pts',(1.88135443518853,4.7274313373995,-52.6416057279167));
#47408=CARTESIAN_POINT('Ctrl Pts',(1.88053521133268,4.85684152954458,-53.2096995393921));
#47409=CARTESIAN_POINT('Ctrl Pts',(1.88021774466022,4.91221706540757,-53.4452444549671));
#47410=CARTESIAN_POINT('Ctrl Pts',(1.87962430010965,5.02926173532985,-53.9146251526131));
#47411=CARTESIAN_POINT('Ctrl Pts',(1.87867687116386,5.25246543255048,-54.7415196101994));
#47412=CARTESIAN_POINT('Ctrl Pts',(1.87717820026664,5.76616052127753,-56.4049580061723));
#47413=CARTESIAN_POINT('Ctrl Pts',(1.87653737221588,6.30754371972887,-57.839407555238));
#47414=CARTESIAN_POINT('Ctrl Pts',(1.87640334479534,6.72375863927511,-58.8485669790888));
#47415=CARTESIAN_POINT('Ctrl Pts',(1.87640011896581,6.77169968585435,-58.9632945249556));
#47416=CARTESIAN_POINT('Ctrl Pts',(1.87640981753854,6.87230907632589,-59.1984753526718));
#47417=CARTESIAN_POINT('Ctrl Pts',(1.87648229107633,7.05457266535652,-59.6105336799863));
#47418=CARTESIAN_POINT('Ctrl Pts',(1.87680035709759,7.44612737564027,-60.4466524112431));
#47419=CARTESIAN_POINT('Ctrl Pts',(1.87746091747657,7.94216601405338,-61.4197358246611));
#47420=CARTESIAN_POINT('Ctrl Pts',(1.87816443196974,8.46426789803593,-62.4051128652444));
#47421=CARTESIAN_POINT('Ctrl Pts',(1.87853578964412,8.76312548481773,-62.9628970204466));
#47422=CARTESIAN_POINT('Ctrl Pts',(1.87875745517044,8.96269469371772,-63.3360167182748));
#47423=CARTESIAN_POINT('Ctrl Pts',(1.87889594354275,9.09570400878161,-63.5850910655754));
#47424=CARTESIAN_POINT('Ctrl Pts',(1.87902391190774,9.22844354699239,-63.8345960668322));
#47425=CARTESIAN_POINT('Ctrl Pts',(1.87911865784649,9.34405909156172,-64.0533253020349));
#47426=CARTESIAN_POINT('Ctrl Pts',(1.87916810345619,9.40992390351972,-64.1784272248205));
#47427=CARTESIAN_POINT('Ctrl Pts',(1.87923707273549,9.50848992668408,-64.3661807228412));
#47428=CARTESIAN_POINT('Ctrl Pts',(1.87928562178054,9.59011831493283,-64.5228957103385));
#47429=CARTESIAN_POINT('Ctrl Pts',(1.87934726761746,9.72417672732782,-64.7823979902518));
#47430=CARTESIAN_POINT('Ctrl Pts',(1.87940408839605,9.85474818543953,-65.0342463738239));
#47431=CARTESIAN_POINT('Ctrl Pts',(1.87948883825274,10.1203301393946,-65.5432435490755));
#47432=CARTESIAN_POINT('Ctrl Pts',(1.87957813188275,10.5827220547072,-66.4216332770441));
#47433=CARTESIAN_POINT('Ctrl Pts',(1.87955592502107,11.5101601419476,-68.1595288613347));
#47434=CARTESIAN_POINT('Ctrl Pts',(1.87941633705314,12.308181502804,-69.638170043014));
#47435=CARTESIAN_POINT('Ctrl Pts',(1.87942945470135,12.9115548163983,-70.7729484576077));
#47436=CARTESIAN_POINT('Ctrl Pts',(1.87943072721303,13.0447945853888,-71.023534534485));
#47437=CARTESIAN_POINT('Ctrl Pts',(1.87943305073928,13.3118762099186,-71.5258401738176));
#47438=CARTESIAN_POINT('Ctrl Pts',(1.87943606223055,13.6452469615933,-72.1528197111203));
#47439=CARTESIAN_POINT('Ctrl Pts',(1.8794370299544,14.0452627075202,-72.9051406045083));
#47440=CARTESIAN_POINT('Ctrl Pts',(1.8794369920951,14.8449078780946,-74.4090580719077));
#47441=CARTESIAN_POINT('Ctrl Pts',(1.87943984359169,15.5108551515139,-75.6615338419008));
#47442=CARTESIAN_POINT('Ctrl Pts',(1.87944367170075,16.4805874064928,-77.4853389352122));
#47443=CARTESIAN_POINT('Ctrl Pts',(1.87944564302009,16.9170636542885,-78.3062334138863));
#47444=CARTESIAN_POINT('Ctrl Pts',(1.8794456430201,17.3535852416779,-79.1272111159846));
#47445=CARTESIAN_POINT('Ctrl Pts',(4.38536333748957,4.07987500441129,24.8306345674609));
#47446=CARTESIAN_POINT('Ctrl Pts',(4.38537644142124,4.07987499919676,24.7817552497562));
#47447=CARTESIAN_POINT('Ctrl Pts',(4.38539019131228,4.07987502084466,24.7328766839669));
#47448=CARTESIAN_POINT('Ctrl Pts',(4.38555225646271,4.07987404404021,24.1822787020537));
#47449=CARTESIAN_POINT('Ctrl Pts',(4.3856747483447,4.07986630447217,23.1782281351487));
#47450=CARTESIAN_POINT('Ctrl Pts',(4.38596401523434,4.07986513301286,21.1696385469548));
#47451=CARTESIAN_POINT('Ctrl Pts',(4.38703941713429,4.07984579442867,19.6656967303803));
#47452=CARTESIAN_POINT('Ctrl Pts',(4.3893281034198,4.07983704306533,18.4147398652079));
#47453=CARTESIAN_POINT('Ctrl Pts',(4.39042640426722,4.07983550220427,17.9119372926431));
#47454=CARTESIAN_POINT('Ctrl Pts',(4.39318382647735,4.07982939511974,16.9080071514512));
#47455=CARTESIAN_POINT('Ctrl Pts',(4.39909969012431,4.07982219497109,15.1542591595331));
#47456=CARTESIAN_POINT('Ctrl Pts',(4.40471075664177,4.07977796237531,13.6529969540059));
#47457=CARTESIAN_POINT('Ctrl Pts',(4.40822987883419,4.07975814035652,12.3987485900475));
#47458=CARTESIAN_POINT('Ctrl Pts',(4.40966888530907,4.07975160201974,11.8978553946956));
#47459=CARTESIAN_POINT('Ctrl Pts',(4.41260517655036,4.07974945549079,10.8960846994662));
#47460=CARTESIAN_POINT('Ctrl Pts',(4.41622620052564,4.07970917257484,9.64390133458129));
#47461=CARTESIAN_POINT('Ctrl Pts',(4.42005210494712,4.07969335842138,8.13994421962362));
#47462=CARTESIAN_POINT('Ctrl Pts',(4.42192997405278,4.07963098116463,7.13534735212569));
#47463=CARTESIAN_POINT('Ctrl Pts',(4.42280559066173,4.07961328863103,6.50881337281083));
#47464=CARTESIAN_POINT('Ctrl Pts',(4.42293307896198,4.08176225758811,6.28940021210922));
#47465=CARTESIAN_POINT('Ctrl Pts',(4.42244849043344,4.0932928132071,5.82167475603086));
#47466=CARTESIAN_POINT('Ctrl Pts',(4.4200863997875,4.12915550142465,4.9849811635924));
#47467=CARTESIAN_POINT('Ctrl Pts',(4.41241717172237,4.22980045467592,3.2004838586177));
#47468=CARTESIAN_POINT('Ctrl Pts',(4.41204017706113,4.23846381586494,1.49941031600799));
#47469=CARTESIAN_POINT('Ctrl Pts',(4.42494515964956,4.04271426178755,0.221825490814583));
#47470=CARTESIAN_POINT('Ctrl Pts',(4.42661641531885,4.0152420162272,0.0573597170611306));
#47471=CARTESIAN_POINT('Ctrl Pts',(4.4304302399912,3.9540711684284,-0.258476534902446));
#47472=CARTESIAN_POINT('Ctrl Pts',(4.43823658554011,3.82901928023654,-0.801066190085443));
#47473=CARTESIAN_POINT('Ctrl Pts',(4.45194015309164,3.61203368465594,-1.53552136893551));
#47474=CARTESIAN_POINT('Ctrl Pts',(4.47106293497066,3.3199525683178,-2.36372384087933));
#47475=CARTESIAN_POINT('Ctrl Pts',(4.49864317522206,2.92101932090935,-3.40223334408898));
#47476=CARTESIAN_POINT('Ctrl Pts',(4.53542070388085,2.46108360630587,-4.58820248705211));
#47477=CARTESIAN_POINT('Ctrl Pts',(4.56191929905351,2.23372943426866,-5.40116324087532));
#47478=CARTESIAN_POINT('Ctrl Pts',(4.57315509374485,2.15171291670083,-5.85772518827808));
#47479=CARTESIAN_POINT('Ctrl Pts',(4.57670152996441,2.11547655848202,-6.07836468920828));
#47480=CARTESIAN_POINT('Ctrl Pts',(4.582716130402,2.05783159343524,-6.50551317008511));
#47481=CARTESIAN_POINT('Ctrl Pts',(4.58968617993058,1.98221611247772,-7.28107077938575));
#47482=CARTESIAN_POINT('Ctrl Pts',(4.59211110960528,1.9400984689788,-8.43457496086372));
#47483=CARTESIAN_POINT('Ctrl Pts',(4.59006804493711,1.94376555103631,-9.66013921101102));
#47484=CARTESIAN_POINT('Ctrl Pts',(4.58898801115239,1.94494955250666,-10.5515189657516));
#47485=CARTESIAN_POINT('Ctrl Pts',(4.58876503502354,1.94083551824235,-11.0708986295732));
#47486=CARTESIAN_POINT('Ctrl Pts',(4.5888378182298,1.93647095036939,-11.3339173258097));
#47487=CARTESIAN_POINT('Ctrl Pts',(4.58898044581554,1.9320289308661,-11.5328241242325));
#47488=CARTESIAN_POINT('Ctrl Pts',(4.58909258905083,1.92953498247887,-11.6520206994036));
#47489=CARTESIAN_POINT('Ctrl Pts',(4.58923477242463,1.92501889552757,-11.8986379229506));
#47490=CARTESIAN_POINT('Ctrl Pts',(4.58933380737592,1.91883182976867,-12.3263335876568));
#47491=CARTESIAN_POINT('Ctrl Pts',(4.5889612591559,1.91221848125152,-13.1859475603198));
#47492=CARTESIAN_POINT('Ctrl Pts',(4.587318679081,1.9158525167072,-14.418398477512));
#47493=CARTESIAN_POINT('Ctrl Pts',(4.5855655965159,1.92551125242793,-15.5412749212642));
#47494=CARTESIAN_POINT('Ctrl Pts',(4.58471565917111,1.93064565913078,-16.2972959138459));
#47495=CARTESIAN_POINT('Ctrl Pts',(4.58426483520442,1.93345284275731,-16.8035285788579));
#47496=CARTESIAN_POINT('Ctrl Pts',(4.58407707180408,1.93452735537964,-17.1857733190268));
#47497=CARTESIAN_POINT('Ctrl Pts',(4.5840470977447,1.93452805010875,-17.5050472253787));
#47498=CARTESIAN_POINT('Ctrl Pts',(4.58403936442119,1.93452939854136,-17.629109521674));
#47499=CARTESIAN_POINT('Ctrl Pts',(4.58403953885549,1.93453465720278,-17.878721089651));
#47500=CARTESIAN_POINT('Ctrl Pts',(4.58406047028114,1.93453815462779,-18.1279372137167));
#47501=CARTESIAN_POINT('Ctrl Pts',(4.58410385317871,1.93454639285833,-18.3775718376653));
#47502=CARTESIAN_POINT('Ctrl Pts',(4.58413908782597,1.9345510030292,-18.5335880862641));
#47503=CARTESIAN_POINT('Ctrl Pts',(4.58417245068831,1.93455529671514,-18.6584611447923));
#47504=CARTESIAN_POINT('Ctrl Pts',(4.58419984423577,1.93455840446897,-18.7521276726347));
#47505=CARTESIAN_POINT('Ctrl Pts',(4.58422461966875,1.93456089354058,-18.8302004655324));
#47506=CARTESIAN_POINT('Ctrl Pts',(4.5842456542114,1.93456293899492,-18.8926672614959));
#47507=CARTESIAN_POINT('Ctrl Pts',(4.58443082577052,1.9345792498428,-19.423686178086));
#47508=CARTESIAN_POINT('Ctrl Pts',(4.58496027623401,1.93456884799325,-20.4404491402449));
#47509=CARTESIAN_POINT('Ctrl Pts',(4.58618165970048,1.9344005047072,-21.9473837554038));
#47510=CARTESIAN_POINT('Ctrl Pts',(4.58711829273437,1.93405548562601,-22.9558218416924));
#47511=CARTESIAN_POINT('Ctrl Pts',(4.58772761688267,1.9337519453812,-23.5856474626337));
#47512=CARTESIAN_POINT('Ctrl Pts',(4.58798722362885,1.93361765012697,-23.8350334454882));
#47513=CARTESIAN_POINT('Ctrl Pts',(4.58856197923874,1.93329611518799,-24.3345016458647));
#47514=CARTESIAN_POINT('Ctrl Pts',(4.5896991750285,1.93260966205005,-25.2103932074912));
#47515=CARTESIAN_POINT('Ctrl Pts',(4.591550770956,1.93139848748939,-26.465283098573));
#47516=CARTESIAN_POINT('Ctrl Pts',(4.59382185748777,1.92990784656879,-27.9738813170967));
#47517=CARTESIAN_POINT('Ctrl Pts',(4.59507579392218,1.92914138268994,-28.9776841894854));
#47518=CARTESIAN_POINT('Ctrl Pts',(4.59565480542664,1.92882029442061,-29.5428136074289));
#47519=CARTESIAN_POINT('Ctrl Pts',(4.59582783748557,1.92803885515975,-29.684947655115));
#47520=CARTESIAN_POINT('Ctrl Pts',(4.59634175778087,1.92398854183494,-29.9570348851275));
#47521=CARTESIAN_POINT('Ctrl Pts',(4.59764796517775,1.9111777944852,-30.4314080380904));
#47522=CARTESIAN_POINT('Ctrl Pts',(4.60157654881394,1.86871729029142,-31.3500132358661));
#47523=CARTESIAN_POINT('Ctrl Pts',(4.60911287557201,1.79325708873194,-32.5889100139117));
#47524=CARTESIAN_POINT('Ctrl Pts',(4.61261035047527,1.7720747183762,-33.7234649575452));
#47525=CARTESIAN_POINT('Ctrl Pts',(4.60753754323484,1.81984412989276,-34.5684483652512));
#47526=CARTESIAN_POINT('Ctrl Pts',(4.60140294800719,1.86939920594346,-34.9709802963835));
#47527=CARTESIAN_POINT('Ctrl Pts',(4.59511193844088,1.91758874644636,-35.2664108115237));
#47528=CARTESIAN_POINT('Ctrl Pts',(4.58963954516065,1.95124546012824,-35.439790623163));
#47529=CARTESIAN_POINT('Ctrl Pts',(4.57693004491039,2.04526178261014,-35.8251973478166));
#47530=CARTESIAN_POINT('Ctrl Pts',(4.55072141029509,2.270694842524,-36.5447481259702));
#47531=CARTESIAN_POINT('Ctrl Pts',(4.49479158256959,2.92339492318843,-38.1815208936028));
#47532=CARTESIAN_POINT('Ctrl Pts',(4.45249879856879,3.62724493168932,-39.8519362779289));
#47533=CARTESIAN_POINT('Ctrl Pts',(4.43466967627358,3.91809437366026,-41.4754857864873));
#47534=CARTESIAN_POINT('Ctrl Pts',(4.43017000357502,3.97709485988986,-41.9152990727862));
#47535=CARTESIAN_POINT('Ctrl Pts',(4.425827541932,4.02777358199978,-42.5028677550952));
#47536=CARTESIAN_POINT('Ctrl Pts',(4.42246125187646,4.06027634685567,-43.0746021926373));
#47537=CARTESIAN_POINT('Ctrl Pts',(4.41989661915659,4.07476176701532,-43.7690088010663));
#47538=CARTESIAN_POINT('Ctrl Pts',(4.41868148866089,4.06753369221726,-44.5648753139305));
#47539=CARTESIAN_POINT('Ctrl Pts',(4.41855604666776,4.05457249544316,-45.1980149881577));
#47540=CARTESIAN_POINT('Ctrl Pts',(4.41856191984839,4.04673730074029,-45.6856037469499));
#47541=CARTESIAN_POINT('Ctrl Pts',(4.4185280849828,4.0437552693733,-46.0419819892028));
#47542=CARTESIAN_POINT('Ctrl Pts',(4.41835264491565,4.04508359659981,-46.3888010287877));
#47543=CARTESIAN_POINT('Ctrl Pts',(4.41778696449461,4.05430232211172,-46.8385669942812));
#47544=CARTESIAN_POINT('Ctrl Pts',(4.41685949765896,4.07147622244023,-47.1612706663254));
#47545=CARTESIAN_POINT('Ctrl Pts',(4.41536946806902,4.09757043631557,-47.4765909598496));
#47546=CARTESIAN_POINT('Ctrl Pts',(4.41435203698925,4.11929124632499,-47.7382165277383));
#47547=CARTESIAN_POINT('Ctrl Pts',(4.4122399511489,4.16093071003005,-48.2296622826269));
#47548=CARTESIAN_POINT('Ctrl Pts',(4.40839107586531,4.23790657624569,-49.0965996831726));
#47549=CARTESIAN_POINT('Ctrl Pts',(4.40271949235705,4.36296011274574,-50.303743139869));
#47550=CARTESIAN_POINT('Ctrl Pts',(4.39630422969031,4.56115621044263,-51.7202397963496));
#47551=CARTESIAN_POINT('Ctrl Pts',(4.39285149901682,4.73911963744755,-52.6390688392893));
#47552=CARTESIAN_POINT('Ctrl Pts',(4.39107069326482,4.86926846690536,-53.208222653553));
#47553=CARTESIAN_POINT('Ctrl Pts',(4.39035315731622,4.92490591277966,-53.4442090160124));
#47554=CARTESIAN_POINT('Ctrl Pts',(4.38898384735229,5.0422973626307,-53.91436147999));
#47555=CARTESIAN_POINT('Ctrl Pts',(4.38674847868596,5.2657075848358,-54.7423984527176));
#47556=CARTESIAN_POINT('Ctrl Pts',(4.38294788630294,5.77841808917209,-56.4072487986332));
#47557=CARTESIAN_POINT('Ctrl Pts',(4.38096907610789,6.31757183978602,-57.8416242539194));
#47558=CARTESIAN_POINT('Ctrl Pts',(4.38039617593613,6.73249390457944,-58.8502076860662));
#47559=CARTESIAN_POINT('Ctrl Pts',(4.38035268196383,6.78035283114945,-58.9650419437206));
#47560=CARTESIAN_POINT('Ctrl Pts',(4.38030271467523,6.88073060928624,-59.2003213018297));
#47561=CARTESIAN_POINT('Ctrl Pts',(4.38032783148236,7.06255659537741,-59.6125709230305));
#47562=CARTESIAN_POINT('Ctrl Pts',(4.38075906502676,7.45302567903753,-60.4489111504564));
#47563=CARTESIAN_POINT('Ctrl Pts',(4.3818642947659,7.94750072908113,-61.42203394979));
#47564=CARTESIAN_POINT('Ctrl Pts',(4.38312813103595,8.46796870792654,-62.4072381816166));
#47565=CARTESIAN_POINT('Ctrl Pts',(4.38381483419207,8.76593203701963,-62.9648487067993));
#47566=CARTESIAN_POINT('Ctrl Pts',(4.38422545017223,8.96493468569735,-63.3378178866081));
#47567=CARTESIAN_POINT('Ctrl Pts',(4.38448507376358,9.09757619626695,-63.5867822852778));
#47568=CARTESIAN_POINT('Ctrl Pts',(4.38471622829962,9.22996208210611,-63.836162652083));
#47569=CARTESIAN_POINT('Ctrl Pts',(4.38489057482387,9.34528683550233,-64.0547689414924));
#47570=CARTESIAN_POINT('Ctrl Pts',(4.38498080317418,9.4109909530479,-64.179796468545));
#47571=CARTESIAN_POINT('Ctrl Pts',(4.38510646844273,9.50932185593333,-64.3674341859458));
#47572=CARTESIAN_POINT('Ctrl Pts',(4.38518833568825,9.59076550330329,-64.5240432970581));
#47573=CARTESIAN_POINT('Ctrl Pts',(4.38529138354864,9.72453937360013,-64.7833581652172));
#47574=CARTESIAN_POINT('Ctrl Pts',(4.38538407252477,9.85487227307931,-65.035057292464));
#47575=CARTESIAN_POINT('Ctrl Pts',(4.38552442823488,10.1200556226403,-65.5437636921788));
#47576=CARTESIAN_POINT('Ctrl Pts',(4.3856575075042,10.5819839959435,-66.4217312990546));
#47577=CARTESIAN_POINT('Ctrl Pts',(4.38559842036056,11.5092437243743,-68.1590931464431));
#47578=CARTESIAN_POINT('Ctrl Pts',(4.38530922003596,12.3078328578379,-69.6378481640055));
#47579=CARTESIAN_POINT('Ctrl Pts',(4.38531495596378,12.9113831497213,-70.7729887387607));
#47580=CARTESIAN_POINT('Ctrl Pts',(4.3853169169871,13.0446063543478,-71.023548114357));
#47581=CARTESIAN_POINT('Ctrl Pts',(4.38531956388404,13.3116888718657,-71.525862452528));
#47582=CARTESIAN_POINT('Ctrl Pts',(4.38532013350853,13.6450490574467,-72.1528282923326));
#47583=CARTESIAN_POINT('Ctrl Pts',(4.38531970441808,14.0450633921025,-72.9051478568788));
#47584=CARTESIAN_POINT('Ctrl Pts',(4.38531587669047,14.8447062959071,-74.4090569962067));
#47585=CARTESIAN_POINT('Ctrl Pts',(4.385305149308,15.5106566049086,-75.6615323927856));
#47586=CARTESIAN_POINT('Ctrl Pts',(4.38530219686728,16.4803894785991,-77.4853425381236));
#47587=CARTESIAN_POINT('Ctrl Pts',(4.38530067674068,16.9168627416068,-78.3062334060089));
#47588=CARTESIAN_POINT('Ctrl Pts',(4.3853006767407,17.3533843289963,-79.1272111081073));
#47589=CARTESIAN_POINT('Ctrl Pts',(7.51718551955428,4.07971249010422,24.8306343608847));
#47590=CARTESIAN_POINT('Ctrl Pts',(7.51720795965804,4.07971248230645,24.7817550363318));
#47591=CARTESIAN_POINT('Ctrl Pts',(7.51723151850014,4.07971246428584,24.7328764315142));
#47592=CARTESIAN_POINT('Ctrl Pts',(7.51750862931441,4.07971269960442,24.1822794479906));
#47593=CARTESIAN_POINT('Ctrl Pts',(7.51771450023927,4.07971520126788,23.178237778938));
#47594=CARTESIAN_POINT('Ctrl Pts',(7.51820836771084,4.07971475633899,21.1696490239213));
#47595=CARTESIAN_POINT('Ctrl Pts',(7.52004122986227,4.07972100155323,19.6657295586513));
#47596=CARTESIAN_POINT('Ctrl Pts',(7.52395863738461,4.07972361209946,18.4147824381763));
#47597=CARTESIAN_POINT('Ctrl Pts',(7.52583963789275,4.07972381789213,17.9119809679059));
#47598=CARTESIAN_POINT('Ctrl Pts',(7.53056086896264,4.07972501141388,16.9080568779214));
#47599=CARTESIAN_POINT('Ctrl Pts',(7.54069280565535,4.07972549092514,15.1543155686738));
#47600=CARTESIAN_POINT('Ctrl Pts',(7.55028728769419,4.07974077033179,13.6531056527217));
#47601=CARTESIAN_POINT('Ctrl Pts',(7.55631193962428,4.07974973893671,12.3988829128982));
#47602=CARTESIAN_POINT('Ctrl Pts',(7.55877660319472,4.07975313865664,11.8979973028344));
#47603=CARTESIAN_POINT('Ctrl Pts',(7.56381238794902,4.07975664999347,10.8962342796642));
#47604=CARTESIAN_POINT('Ctrl Pts',(7.57000663770048,4.07977634071094,9.64409150183717));
#47605=CARTESIAN_POINT('Ctrl Pts',(7.57656628504353,4.07978723733203,8.14018162411911));
#47606=CARTESIAN_POINT('Ctrl Pts',(7.57976001741483,4.07981510291455,7.13561214357882));
#47607=CARTESIAN_POINT('Ctrl Pts',(7.58125680054209,4.07981937530554,6.50919565034343));
#47608=CARTESIAN_POINT('Ctrl Pts',(7.58190445541536,4.08212174401879,6.29218907834675));
#47609=CARTESIAN_POINT('Ctrl Pts',(7.58334841215747,4.09448343752714,5.82707715320434));
#47610=CARTESIAN_POINT('Ctrl Pts',(7.58603525732085,4.13307212013271,4.99360215410308));
#47611=CARTESIAN_POINT('Ctrl Pts',(7.59114415438726,4.24184534711902,3.20739308478373));
#47612=CARTESIAN_POINT('Ctrl Pts',(7.59004899911565,4.25238286087194,1.49090484084568));
#47613=CARTESIAN_POINT('Ctrl Pts',(7.58318134817281,4.03889895130787,0.197408840081295));
#47614=CARTESIAN_POINT('Ctrl Pts',(7.58231136318647,4.0087808203859,0.0301756810361527));
#47615=CARTESIAN_POINT('Ctrl Pts',(7.58031603100438,3.94191656764389,-0.290127652373105));
#47616=CARTESIAN_POINT('Ctrl Pts',(7.57625546587106,3.80547464262213,-0.839555082672826));
#47617=CARTESIAN_POINT('Ctrl Pts',(7.56912588627309,3.56998135672488,-1.58040980943646));
#47618=CARTESIAN_POINT('Ctrl Pts',(7.55942200879824,3.25483991395464,-2.41305020166659));
#47619=CARTESIAN_POINT('Ctrl Pts',(7.54501194597211,2.82737969524278,-3.4543956916464));
#47620=CARTESIAN_POINT('Ctrl Pts',(7.52463208509811,2.33996709990814,-4.63990578299861));
#47621=CARTESIAN_POINT('Ctrl Pts',(7.50678308517936,2.10606535617851,-5.44201721582885));
#47622=CARTESIAN_POINT('Ctrl Pts',(7.49865343326163,2.02298974534607,-5.88524536138439));
#47623=CARTESIAN_POINT('Ctrl Pts',(7.4961743744293,1.98529253310316,-6.10350764048164));
#47624=CARTESIAN_POINT('Ctrl Pts',(7.49170906930816,1.92570574334559,-6.52452416988688));
#47625=CARTESIAN_POINT('Ctrl Pts',(7.48600371876777,1.84722654992848,-7.29119138736624));
#47626=CARTESIAN_POINT('Ctrl Pts',(7.48223921884591,1.80346041576881,-8.43552251871391));
#47627=CARTESIAN_POINT('Ctrl Pts',(7.48114785215769,1.80751161779657,-9.65853465431959));
#47628=CARTESIAN_POINT('Ctrl Pts',(7.48034069466382,1.8088735491368,-10.5513280174558));
#47629=CARTESIAN_POINT('Ctrl Pts',(7.47971069675407,1.80456152724868,-11.0724961195177));
#47630=CARTESIAN_POINT('Ctrl Pts',(7.47931248800309,1.79995476801641,-11.3367392235495));
#47631=CARTESIAN_POINT('Ctrl Pts',(7.47897576300961,1.79525363342574,-11.5366535550938));
#47632=CARTESIAN_POINT('Ctrl Pts',(7.47872605975369,1.79265101902759,-11.6552228910092));
#47633=CARTESIAN_POINT('Ctrl Pts',(7.47827238577484,1.78791663242365,-11.9013536899149));
#47634=CARTESIAN_POINT('Ctrl Pts',(7.47753715478061,1.78144720805231,-12.3279114350663));
#47635=CARTESIAN_POINT('Ctrl Pts',(7.47631034478809,1.77457410597943,-13.1858634282511));
#47636=CARTESIAN_POINT('Ctrl Pts',(7.47519368111145,1.77849238136237,-14.4167742231908));
#47637=CARTESIAN_POINT('Ctrl Pts',(7.47469258483126,1.78873356384644,-15.5395400353667));
#47638=CARTESIAN_POINT('Ctrl Pts',(7.47447448713808,1.79417730311737,-16.2959696860391));
#47639=CARTESIAN_POINT('Ctrl Pts',(7.47436135191072,1.7971460417357,-16.8026074185616));
#47640=CARTESIAN_POINT('Ctrl Pts',(7.47428469225115,1.79829761012166,-17.1853088109618));
#47641=CARTESIAN_POINT('Ctrl Pts',(7.47423445214067,1.79830077211436,-17.5050291743713));
#47642=CARTESIAN_POINT('Ctrl Pts',(7.47422280456671,1.798303905888,-17.6290014884559));
#47643=CARTESIAN_POINT('Ctrl Pts',(7.4742295721944,1.79831639151149,-17.8785965052693));
#47644=CARTESIAN_POINT('Ctrl Pts',(7.47427497297558,1.79833527958903,-18.1277486173107));
#47645=CARTESIAN_POINT('Ctrl Pts',(7.47435786033162,1.79836039462119,-18.3773597741528));
#47646=CARTESIAN_POINT('Ctrl Pts',(7.47442244316509,1.79837741451397,-18.5333588142296));
#47647=CARTESIAN_POINT('Ctrl Pts',(7.47448174564885,1.7983918361177,-18.6582232456114));
#47648=CARTESIAN_POINT('Ctrl Pts',(7.47452957608076,1.79840285346194,-18.7518839382005));
#47649=CARTESIAN_POINT('Ctrl Pts',(7.47457208182688,1.79841214200524,-18.8299532242847));
#47650=CARTESIAN_POINT('Ctrl Pts',(7.4746076747586,1.79841963674975,-18.8924177727002));
#47651=CARTESIAN_POINT('Ctrl Pts',(7.47491817122276,1.79848316570936,-19.4234214886521));
#47652=CARTESIAN_POINT('Ctrl Pts',(7.47573077242387,1.798595156224,-20.4402710521663));
#47653=CARTESIAN_POINT('Ctrl Pts',(7.4768952047759,1.79842921761441,-21.9476656360667));
#47654=CARTESIAN_POINT('Ctrl Pts',(7.47706144613008,1.79786860312304,-22.9566283715109));
#47655=CARTESIAN_POINT('Ctrl Pts',(7.47683450636963,1.79731318435664,-23.586850451328));
#47656=CARTESIAN_POINT('Ctrl Pts',(7.47671387984677,1.79706369455515,-23.8364592611807));
#47657=CARTESIAN_POINT('Ctrl Pts',(7.47635510879953,1.79645667756257,-24.3362770759908));
#47658=CARTESIAN_POINT('Ctrl Pts',(7.47545952068536,1.79514926597529,-25.2126720882539));
#47659=CARTESIAN_POINT('Ctrl Pts',(7.4736450424381,1.79278506910037,-26.4678871554683));
#47660=CARTESIAN_POINT('Ctrl Pts',(7.47138283293608,1.78984400962715,-27.9763225649068));
#47661=CARTESIAN_POINT('Ctrl Pts',(7.47032691179317,1.78826943081053,-28.9795605867428));
#47662=CARTESIAN_POINT('Ctrl Pts',(7.46999420387175,1.78762815323461,-29.5443956378212));
#47663=CARTESIAN_POINT('Ctrl Pts',(7.46990607068809,1.78672312463406,-29.6880393564753));
#47664=CARTESIAN_POINT('Ctrl Pts',(7.46965834635643,1.78227818555402,-29.9619945701119));
#47665=CARTESIAN_POINT('Ctrl Pts',(7.46905787927587,1.76843599696719,-30.439494351754));
#47666=CARTESIAN_POINT('Ctrl Pts',(7.46726279487216,1.72304890119731,-31.3615763778818));
#47667=CARTESIAN_POINT('Ctrl Pts',(7.46375939358869,1.64326849658029,-32.5989290413864));
#47668=CARTESIAN_POINT('Ctrl Pts',(7.46238748486115,1.62120267413446,-33.7222449914166));
#47669=CARTESIAN_POINT('Ctrl Pts',(7.46601907277839,1.67023374333108,-34.5527699895573));
#47670=CARTESIAN_POINT('Ctrl Pts',(7.47010888017429,1.72081975290891,-34.9467534976082));
#47671=CARTESIAN_POINT('Ctrl Pts',(7.47415782070678,1.76993633235586,-35.2355142231742));
#47672=CARTESIAN_POINT('Ctrl Pts',(7.4777999551406,1.80355688229369,-35.4025766836103));
#47673=CARTESIAN_POINT('Ctrl Pts',(7.48573753704329,1.89930931743001,-35.7795483373344));
#47674=CARTESIAN_POINT('Ctrl Pts',(7.50131995334051,2.13196249717656,-36.4898823831495));
#47675=CARTESIAN_POINT('Ctrl Pts',(7.52885994573029,2.81990008131359,-38.1261297125887));
#47676=CARTESIAN_POINT('Ctrl Pts',(7.54646135782687,3.57997481633,-39.8028011410274));
#47677=CARTESIAN_POINT('Ctrl Pts',(7.55506134819746,3.89828012158619,-41.4522755413143));
#47678=CARTESIAN_POINT('Ctrl Pts',(7.55738012845925,3.96260520846499,-41.8954550225072));
#47679=CARTESIAN_POINT('Ctrl Pts',(7.55974983873441,4.01868373996087,-42.4888348031539));
#47680=CARTESIAN_POINT('Ctrl Pts',(7.56174736166402,4.05502464972836,-43.0653222631363));
#47681=CARTESIAN_POINT('Ctrl Pts',(7.56352824653193,4.07221139566532,-43.7647290043707));
#47682=CARTESIAN_POINT('Ctrl Pts',(7.56478227701937,4.06595245960517,-44.5644779518473));
#47683=CARTESIAN_POINT('Ctrl Pts',(7.56533148651779,4.05283857703286,-45.1992427947033));
#47684=CARTESIAN_POINT('Ctrl Pts',(7.56553354918689,4.04478798258784,-45.6871550449717));
#47685=CARTESIAN_POINT('Ctrl Pts',(7.5656428385536,4.04165025393199,-46.043284316581));
#47686=CARTESIAN_POINT('Ctrl Pts',(7.56574019074214,4.04290621007078,-46.3893532108146));
#47687=CARTESIAN_POINT('Ctrl Pts',(7.56588033119948,4.05223544847548,-46.8374697517941));
#47688=CARTESIAN_POINT('Ctrl Pts',(7.56612231469326,4.06973784094667,-47.1581709597959));
#47689=CARTESIAN_POINT('Ctrl Pts',(7.56644470873198,4.09645379880801,-47.4711009352875));
#47690=CARTESIAN_POINT('Ctrl Pts',(7.56664923644244,4.11889435515154,-47.7332118947828));
#47691=CARTESIAN_POINT('Ctrl Pts',(7.56702704076722,4.16178288413229,-48.22449728));
#47692=CARTESIAN_POINT('Ctrl Pts',(7.56757644835753,4.24095012196946,-49.0918571760979));
#47693=CARTESIAN_POINT('Ctrl Pts',(7.56790794403495,4.36869434493729,-50.2995294266277));
#47694=CARTESIAN_POINT('Ctrl Pts',(7.56674498299714,4.56943457631291,-51.7173816663438));
#47695=CARTESIAN_POINT('Ctrl Pts',(7.56463708563956,4.74847674481168,-52.6373167573546));
#47696=CARTESIAN_POINT('Ctrl Pts',(7.56272848288763,4.87914678571234,-53.2072484319363));
#47697=CARTESIAN_POINT('Ctrl Pts',(7.56186059988464,4.93499175495422,-53.443617226946));
#47698=CARTESIAN_POINT('Ctrl Pts',(7.55976715503288,5.05266256760958,-53.9144056700956));
#47699=CARTESIAN_POINT('Ctrl Pts',(7.55531846507066,5.2762603192113,-54.7433752709434));
#47700=CARTESIAN_POINT('Ctrl Pts',(7.54421884355346,5.78831119318727,-56.4093170580287));
#47701=CARTESIAN_POINT('Ctrl Pts',(7.53434277323058,6.32574074251072,-57.8435279363008));
#47702=CARTESIAN_POINT('Ctrl Pts',(7.53028057508383,6.73962490994349,-58.8516240716937));
#47703=CARTESIAN_POINT('Ctrl Pts',(7.5297836098851,6.7874239169442,-58.9665470204583));
#47704=CARTESIAN_POINT('Ctrl Pts',(7.52883630432498,6.88762233423541,-59.2019071068476));
#47705=CARTESIAN_POINT('Ctrl Pts',(7.5272717350224,7.06910816068731,-59.6143115109346));
#47706=CARTESIAN_POINT('Ctrl Pts',(7.52452689433495,7.45870700081999,-60.4508213037396));
#47707=CARTESIAN_POINT('Ctrl Pts',(7.52214269466404,7.95191257071366,-61.4239593595716));
#47708=CARTESIAN_POINT('Ctrl Pts',(7.52032781922298,8.47101662510095,-62.4090068565059));
#47709=CARTESIAN_POINT('Ctrl Pts',(7.51947604021343,8.76822269947309,-62.9664674348229));
#47710=CARTESIAN_POINT('Ctrl Pts',(7.51895952889291,8.96674264835317,-63.339307001888));
#47711=CARTESIAN_POINT('Ctrl Pts',(7.51862913853834,9.09906857249673,-63.588176763506));
#47712=CARTESIAN_POINT('Ctrl Pts',(7.51831176641175,9.23115450301005,-63.837450489128));
#47713=CARTESIAN_POINT('Ctrl Pts',(7.51804847893112,9.34622920040807,-64.0559509774442));
#47714=CARTESIAN_POINT('Ctrl Pts',(7.51790092374494,9.41179504082436,-64.1809144183687));
#47715=CARTESIAN_POINT('Ctrl Pts',(7.51768262198302,9.50992314869041,-64.3684522626355));
#47716=CARTESIAN_POINT('Ctrl Pts',(7.51750366928883,9.59121012018809,-64.5249707181327));
#47717=CARTESIAN_POINT('Ctrl Pts',(7.51721456528255,9.72473987575942,-64.7841239316579));
#47718=CARTESIAN_POINT('Ctrl Pts',(7.51695154925424,9.85487124438173,-65.0356980537645));
#47719=CARTESIAN_POINT('Ctrl Pts',(7.51655986773369,10.1197152427305,-65.5441577753383));
#47720=CARTESIAN_POINT('Ctrl Pts',(7.51617932888529,10.5812597640262,-66.4217711154117));
#47721=CARTESIAN_POINT('Ctrl Pts',(7.51637926889889,11.5083859878242,-68.1586823730641));
#47722=CARTESIAN_POINT('Ctrl Pts',(7.51718838686394,12.3075015417636,-69.6375526163581));
#47723=CARTESIAN_POINT('Ctrl Pts',(7.51716645787803,12.9112162672006,-70.7730095811495));
#47724=CARTESIAN_POINT('Ctrl Pts',(7.51716390165521,13.0444256040857,-71.0235462226635));
#47725=CARTESIAN_POINT('Ctrl Pts',(7.51715952057163,13.3115101026409,-71.5258686016946));
#47726=CARTESIAN_POINT('Ctrl Pts',(7.51715469827561,13.6448646470806,-72.1528242965523));
#47727=CARTESIAN_POINT('Ctrl Pts',(7.5171533384676,14.0448792873963,-72.9051434628418));
#47728=CARTESIAN_POINT('Ctrl Pts',(7.51715455299824,14.8445227247772,-74.4090466856942));
#47729=CARTESIAN_POINT('Ctrl Pts',(7.51715350869284,15.5104861014003,-75.6615266096123));
#47730=CARTESIAN_POINT('Ctrl Pts',(7.51714857446979,16.4802261084657,-77.4853440369576));
#47731=CARTESIAN_POINT('Ctrl Pts',(7.51714603172462,16.9167002668011,-78.306233429594));
#47732=CARTESIAN_POINT('Ctrl Pts',(7.5171460317246,17.3532218541906,-79.1272111316924));
#47733=CARTESIAN_POINT('Ctrl Pts',(10.9624646798336,4.08045736333527,24.8306353233982));
#47734=CARTESIAN_POINT('Ctrl Pts',(10.9624974112732,4.08045738492077,24.7817560292463));
#47735=CARTESIAN_POINT('Ctrl Pts',(10.9625317350798,4.0804573829706,24.7328775366951));
#47736=CARTESIAN_POINT('Ctrl Pts',(10.9629372601565,4.08045847670549,24.1822781736734));
#47737=CARTESIAN_POINT('Ctrl Pts',(10.9632485186784,4.08046588120829,23.1782140967866));
#47738=CARTESIAN_POINT('Ctrl Pts',(10.9639697700664,4.08046799907804,21.1696235179717));
#47739=CARTESIAN_POINT('Ctrl Pts',(10.9666707335973,4.08048691112784,19.6656474654337));
#47740=CARTESIAN_POINT('Ctrl Pts',(10.9723972261602,4.0804966227945,18.4146756888765));
#47741=CARTESIAN_POINT('Ctrl Pts',(10.9751429165286,4.08049896285481,17.9118722585523));
#47742=CARTESIAN_POINT('Ctrl Pts',(10.9820375662411,4.08050702316906,16.9079334045807));
#47743=CARTESIAN_POINT('Ctrl Pts',(10.9968251949538,4.08051890113854,15.1541749240292));
#47744=CARTESIAN_POINT('Ctrl Pts',(11.0108841762241,4.08056270929919,13.6528297088379));
#47745=CARTESIAN_POINT('Ctrl Pts',(11.0197032179328,4.08058047523023,12.3985380152264));
#47746=CARTESIAN_POINT('Ctrl Pts',(11.0233090516766,4.0805860831325,11.8976334291727));
#47747=CARTESIAN_POINT('Ctrl Pts',(11.0306607980321,4.08058621139806,10.8958434397728));
#47748=CARTESIAN_POINT('Ctrl Pts',(11.0397602248644,4.08061971854824,9.64361147068879));
#47749=CARTESIAN_POINT('Ctrl Pts',(11.049357601229,4.08062788610815,8.13953906117807));
#47750=CARTESIAN_POINT('Ctrl Pts',(11.0541129858031,4.08068358210231,7.13497790928695));
#47751=CARTESIAN_POINT('Ctrl Pts',(11.0563205349784,4.08069356878045,6.50810793756284));
#47752=CARTESIAN_POINT('Ctrl Pts',(11.0578003392729,4.08238703533895,6.2812286397764));
#47753=CARTESIAN_POINT('Ctrl Pts',(11.0626898963694,4.09135641957855,5.80540232705015));
#47754=CARTESIAN_POINT('Ctrl Pts',(11.0749984328579,4.11902224542694,4.95882848560147));
#47755=CARTESIAN_POINT('Ctrl Pts',(11.1046504104053,4.19473247930313,3.17968685652564));
#47756=CARTESIAN_POINT('Ctrl Pts',(11.1036402821399,4.20015554547666,1.5276097462183));
#47757=CARTESIAN_POINT('Ctrl Pts',(11.0579407115821,4.05981651715574,0.299696259065808));
#47758=CARTESIAN_POINT('Ctrl Pts',(11.0520116181057,4.04046613063924,0.143859829319175));
#47759=CARTESIAN_POINT('Ctrl Pts',(11.0383688353589,3.99686870684385,-0.15805611788381));
#47760=CARTESIAN_POINT('Ctrl Pts',(11.0101613797018,3.90700136384924,-0.679347896305351));
#47761=CARTESIAN_POINT('Ctrl Pts',(10.9595892987304,3.74798647031421,-1.39388395716988));
#47762=CARTESIAN_POINT('Ctrl Pts',(10.8880526310442,3.52822646669199,-2.20853931547687));
#47763=CARTESIAN_POINT('Ctrl Pts',(10.7848130904019,3.22105878258507,-3.2390988854101));
#47764=CARTESIAN_POINT('Ctrl Pts',(10.6513887040697,2.85284672812267,-4.42823588303147));
#47765=CARTESIAN_POINT('Ctrl Pts',(10.5655199263466,2.65190863334669,-5.27510542835426));
#47766=CARTESIAN_POINT('Ctrl Pts',(10.5301425486311,2.57492197176225,-5.77252875520469));
#47767=CARTESIAN_POINT('Ctrl Pts',(10.5180961403591,2.54369111238152,-6.00047614868717));
#47768=CARTESIAN_POINT('Ctrl Pts',(10.4975524844,2.49281502581667,-6.44643200010511));
#47769=CARTESIAN_POINT('Ctrl Pts',(10.4716388096329,2.42689514909976,-7.24930178718183));
#47770=CARTESIAN_POINT('Ctrl Pts',(10.4561427601609,2.39011928274206,-8.4311631487814));
#47771=CARTESIAN_POINT('Ctrl Pts',(10.454094044526,2.39207050169796,-9.66480471721667));
#47772=CARTESIAN_POINT('Ctrl Pts',(10.4522985336733,2.39207600035412,-10.5518894638563));
#47773=CARTESIAN_POINT('Ctrl Pts',(10.4502394625745,2.38828612858452,-11.0657987432211));
#47774=CARTESIAN_POINT('Ctrl Pts',(10.4487075309053,2.38456441505993,-11.3250687490037));
#47775=CARTESIAN_POINT('Ctrl Pts',(10.4473070301966,2.38085337186641,-11.5208859320258));
#47776=CARTESIAN_POINT('Ctrl Pts',(10.4463583875329,2.37864387283397,-11.6420016120887));
#47777=CARTESIAN_POINT('Ctrl Pts',(10.4446744419706,2.37468153201103,-11.8901027852085));
#47778=CARTESIAN_POINT('Ctrl Pts',(10.4421721669975,2.36913398587217,-12.3212797555185));
#47779=CARTESIAN_POINT('Ctrl Pts',(10.4388561688442,2.36285626689449,-13.1860420530998));
#47780=CARTESIAN_POINT('Ctrl Pts',(10.4378552861942,2.36469137873023,-14.423262317235));
#47781=CARTESIAN_POINT('Ctrl Pts',(10.4391338276668,2.37177576636951,-15.5464880771636));
#47782=CARTESIAN_POINT('Ctrl Pts',(10.4399406768736,2.37559028962932,-16.3012341882906));
#47783=CARTESIAN_POINT('Ctrl Pts',(10.4403999741264,2.37767480820586,-16.8061852749493));
#47784=CARTESIAN_POINT('Ctrl Pts',(10.44060257823,2.37848080144773,-17.1870308097338));
#47785=CARTESIAN_POINT('Ctrl Pts',(10.440603319085,2.37846229885705,-17.5049134003353));
#47786=CARTESIAN_POINT('Ctrl Pts',(10.4406208058462,2.37845624979895,-17.6292519804825));
#47787=CARTESIAN_POINT('Ctrl Pts',(10.4407204731566,2.3784494134481,-17.8789060526275));
#47788=CARTESIAN_POINT('Ctrl Pts',(10.4409123918676,2.37845080985169,-18.1283166835446));
#47789=CARTESIAN_POINT('Ctrl Pts',(10.4411782512159,2.37846197013343,-18.3780117776051));
#47790=CARTESIAN_POINT('Ctrl Pts',(10.4413733035248,2.37847312744644,-18.5340741512269));
#47791=CARTESIAN_POINT('Ctrl Pts',(10.441544359038,2.37848476145854,-18.6589666563742));
#47792=CARTESIAN_POINT('Ctrl Pts',(10.4416798768071,2.37849485565446,-18.7526456803256));
#47793=CARTESIAN_POINT('Ctrl Pts',(10.4417984461137,2.3785044379206,-18.8307245329558));
#47794=CARTESIAN_POINT('Ctrl Pts',(10.4418963892107,2.37851283166161,-18.8931941630973));
#47795=CARTESIAN_POINT('Ctrl Pts',(10.4427467029551,2.37858826050148,-19.4242255273232));
#47796=CARTESIAN_POINT('Ctrl Pts',(10.4448940853641,2.37886351740411,-20.440668336297));
#47797=CARTESIAN_POINT('Ctrl Pts',(10.4477033212108,2.37979135147078,-21.9460157760457));
#47798=CARTESIAN_POINT('Ctrl Pts',(10.4480698678651,2.38084786701659,-22.9527105822916));
#47799=CARTESIAN_POINT('Ctrl Pts',(10.4474558488072,2.38167163198556,-23.5812081457634));
#47800=CARTESIAN_POINT('Ctrl Pts',(10.4471330270657,2.38203091629453,-23.8298055877299));
#47801=CARTESIAN_POINT('Ctrl Pts',(10.4461958941223,2.38286906347281,-24.3280584766635));
#47802=CARTESIAN_POINT('Ctrl Pts',(10.4438980219011,2.3846101529119,-25.2021910563275));
#47803=CARTESIAN_POINT('Ctrl Pts',(10.4392357405293,2.38763519968205,-26.4560467041742));
#47804=CARTESIAN_POINT('Ctrl Pts',(10.433280894909,2.39137954388358,-27.9653174676155));
#47805=CARTESIAN_POINT('Ctrl Pts',(10.4301731559634,2.39340640289701,-28.9712942079044));
#47806=CARTESIAN_POINT('Ctrl Pts',(10.4290290267676,2.39427462377435,-29.5375862367704));
#47807=CARTESIAN_POINT('Ctrl Pts',(10.4286212480674,2.3939419742561,-29.6752033047866));
#47808=CARTESIAN_POINT('Ctrl Pts',(10.4272628698591,2.39126233326746,-29.941736351058));
#47809=CARTESIAN_POINT('Ctrl Pts',(10.4235781498688,2.38193132510707,-30.4068259305923));
#47810=CARTESIAN_POINT('Ctrl Pts',(10.4121237168613,2.3492732871545,-31.3152106151894));
#47811=CARTESIAN_POINT('Ctrl Pts',(10.3907411254912,2.28811111526887,-32.559221395248));
#47812=CARTESIAN_POINT('Ctrl Pts',(10.3825197668055,2.26979831419424,-33.7280316465651));
#47813=CARTESIAN_POINT('Ctrl Pts',(10.39795839888,2.31307366271173,-34.6166593913203));
#47814=CARTESIAN_POINT('Ctrl Pts',(10.4156112942381,2.35851940812219,-35.0450053773708));
#47815=CARTESIAN_POINT('Ctrl Pts',(10.4336262420655,2.40301971240747,-35.3604888544365));
#47816=CARTESIAN_POINT('Ctrl Pts',(10.4487446471554,2.43604685187258,-35.5528315719723));
#47817=CARTESIAN_POINT('Ctrl Pts',(10.4855848805768,2.52287245628984,-35.9635953787419));
#47818=CARTESIAN_POINT('Ctrl Pts',(10.5654929538693,2.72085013989271,-36.7112829926298));
#47819=CARTESIAN_POINT('Ctrl Pts',(10.7565856506919,3.25488597070165,-38.3527194747804));
#47820=CARTESIAN_POINT('Ctrl Pts',(10.9170481196781,3.78092103798195,-40.0042489860928));
#47821=CARTESIAN_POINT('Ctrl Pts',(10.9795150310049,3.98577979631989,-41.5483666219995));
#47822=CARTESIAN_POINT('Ctrl Pts',(10.9948567121963,4.028017025414,-41.9778845998627));
#47823=CARTESIAN_POINT('Ctrl Pts',(11.0094600365173,4.06189769773347,-42.547662950352));
#47824=CARTESIAN_POINT('Ctrl Pts',(11.020579781767,4.08228371762755,-43.1048191371307));
#47825=CARTESIAN_POINT('Ctrl Pts',(11.0286564301021,4.08804953783849,-43.783876357993));
#47826=CARTESIAN_POINT('Ctrl Pts',(11.0315794804677,4.07721734166889,-44.5678175389575));
#47827=CARTESIAN_POINT('Ctrl Pts',(11.0305256425759,4.064054799379,-45.1959666455832));
#47828=CARTESIAN_POINT('Ctrl Pts',(11.0288587160196,4.05661717032617,-45.6826348738755));
#47829=CARTESIAN_POINT('Ctrl Pts',(11.0275262074785,4.05387433928492,-46.0398346180674));
#47830=CARTESIAN_POINT('Ctrl Pts',(11.0264331705636,4.0551708360785,-46.3890211810534));
#47831=CARTESIAN_POINT('Ctrl Pts',(11.0257195434411,4.06376907747683,-46.8439571389145));
#47832=CARTESIAN_POINT('Ctrl Pts',(11.0265249261146,4.07951702892443,-47.1728757993545));
#47833=CARTESIAN_POINT('Ctrl Pts',(11.0288417663362,4.10343060615818,-47.4956385365803));
#47834=CARTESIAN_POINT('Ctrl Pts',(11.0303413896298,4.12272689329889,-47.7560094569819));
#47835=CARTESIAN_POINT('Ctrl Pts',(11.033139264776,4.16003680841996,-48.248255683235));
#47836=CARTESIAN_POINT('Ctrl Pts',(11.0374645879716,4.22917939920677,-49.1143392464993));
#47837=CARTESIAN_POINT('Ctrl Pts',(11.04184899311,4.34372908818247,-50.3199340632308));
#47838=CARTESIAN_POINT('Ctrl Pts',(11.0435083236951,4.53158843368009,-51.7317826449608));
#47839=CARTESIAN_POINT('Ctrl Pts',(11.0417924431526,4.70482052662216,-52.646310903103));
#47840=CARTESIAN_POINT('Ctrl Pts',(11.039663329745,4.83290160929832,-53.2124171963205));
#47841=CARTESIAN_POINT('Ctrl Pts',(11.0386162679699,4.88778364060814,-53.4470591412272));
#47842=CARTESIAN_POINT('Ctrl Pts',(11.0358085502369,5.00418278352712,-53.9149045068776));
#47843=CARTESIAN_POINT('Ctrl Pts',(11.0292893597981,5.22701505697702,-54.7395333124799));
#47844=CARTESIAN_POINT('Ctrl Pts',(11.0116266608252,5.7426033353743,-56.400240346654));
#47845=CARTESIAN_POINT('Ctrl Pts',(10.9949335907642,6.28836758405837,-57.8349512527431));
#47846=CARTESIAN_POINT('Ctrl Pts',(10.988087935204,6.70711748343476,-58.8453134842339));
#47847=CARTESIAN_POINT('Ctrl Pts',(10.9872366677291,6.75521207647722,-58.959839211309));
#47848=CARTESIAN_POINT('Ctrl Pts',(10.9855946313238,6.85626298130136,-59.1948421885943));
#47849=CARTESIAN_POINT('Ctrl Pts',(10.9828275348998,7.03935578536294,-59.6065522268112));
#47850=CARTESIAN_POINT('Ctrl Pts',(10.9777571326992,7.43297483611379,-60.4422881173784));
#47851=CARTESIAN_POINT('Ctrl Pts',(10.9729723326619,7.93198121156931,-61.4153348277046));
#47852=CARTESIAN_POINT('Ctrl Pts',(10.9690819296197,8.45721017371796,-62.4010643447095));
#47853=CARTESIAN_POINT('Ctrl Pts',(10.96719703468,8.75778667494156,-62.9591856758838));
#47854=CARTESIAN_POINT('Ctrl Pts',(10.9660565033908,8.95844769089226,-63.332594904036));
#47855=CARTESIAN_POINT('Ctrl Pts',(10.9653263751097,9.09216753085925,-63.5818802113062));
#47856=CARTESIAN_POINT('Ctrl Pts',(10.9646401134821,9.22558789845036,-63.8316230488872));
#47857=CARTESIAN_POINT('Ctrl Pts',(10.9640769863299,9.34176608562326,-64.0505869757395));
#47858=CARTESIAN_POINT('Ctrl Pts',(10.9637656030705,9.40794198473294,-64.1758308493704));
#47859=CARTESIAN_POINT('Ctrl Pts',(10.9633088727675,9.50696363874219,-64.3638052868478));
#47860=CARTESIAN_POINT('Ctrl Pts',(10.9629492508971,9.58894814837339,-64.520721446415));
#47861=CARTESIAN_POINT('Ctrl Pts',(10.9623815065997,9.72355770937703,-64.7805808924906));
#47862=CARTESIAN_POINT('Ctrl Pts',(10.961867348382,9.85459317907115,-65.0327186415835));
#47863=CARTESIAN_POINT('Ctrl Pts',(10.961100025666,10.1209500852642,-65.5422775660664));
#47864=CARTESIAN_POINT('Ctrl Pts',(10.9603700836074,10.5842356687815,-66.4214830775254));
#47865=CARTESIAN_POINT('Ctrl Pts',(10.960791456899,11.5120040023041,-68.1604138179985));
#47866=CARTESIAN_POINT('Ctrl Pts',(10.962444386315,12.3088852940989,-69.63881635891));
#47867=CARTESIAN_POINT('Ctrl Pts',(10.9624193577822,12.9119028977147,-70.7728829833708));
#47868=CARTESIAN_POINT('Ctrl Pts',(10.9624149235793,13.0451745975293,-71.0235209119673));
#47869=CARTESIAN_POINT('Ctrl Pts',(10.9624081676807,13.3122533538826,-71.525808947084));
#47870=CARTESIAN_POINT('Ctrl Pts',(10.9624034364209,13.6456418223831,-72.1528135877663));
#47871=CARTESIAN_POINT('Ctrl Pts',(10.962402792736,14.0456590372664,-72.9051362844501));
#47872=CARTESIAN_POINT('Ctrl Pts',(10.9624082559957,14.8453066308756,-74.4090687157949));
#47873=CARTESIAN_POINT('Ctrl Pts',(10.9624198923528,15.5112398060805,-75.6615407410724));
#47874=CARTESIAN_POINT('Ctrl Pts',(10.9624192066963,16.4809656828406,-77.4853334277387));
#47875=CARTESIAN_POINT('Ctrl Pts',(10.962418854705,16.9174449520636,-78.306233377601));
#47876=CARTESIAN_POINT('Ctrl Pts',(10.9624188547049,17.3539665394531,-79.1272110796992));
#47877=CARTESIAN_POINT('Ctrl Pts',(14.0957722616046,4.08025224202491,24.8306350534813));
#47878=CARTESIAN_POINT('Ctrl Pts',(14.0958143929042,4.08025223777848,24.7817557508935));
#47879=CARTESIAN_POINT('Ctrl Pts',(14.0958586147606,4.08025224020083,24.7328773999137));
#47880=CARTESIAN_POINT('Ctrl Pts',(14.0963792203118,4.08025195558791,24.1822728844133));
#47881=CARTESIAN_POINT('Ctrl Pts',(14.0967691662794,4.08025016189665,23.1781665546079));
#47882=CARTESIAN_POINT('Ctrl Pts',(14.0976986663016,4.08025040075573,21.1695712092763));
#47883=CARTESIAN_POINT('Ctrl Pts',(14.1011467099489,4.08024523061615,19.6654902060134));
#47884=CARTESIAN_POINT('Ctrl Pts',(14.1085012613688,4.08024146562352,18.4144726949287));
#47885=CARTESIAN_POINT('Ctrl Pts',(14.112031928167,4.08024039800909,17.9116616565299));
#47886=CARTESIAN_POINT('Ctrl Pts',(14.1208949819925,4.08023722409591,16.9076927383382));
#47887=CARTESIAN_POINT('Ctrl Pts',(14.1399130451043,4.0802318870913,15.1539031954854));
#47888=CARTESIAN_POINT('Ctrl Pts',(14.1579323195343,4.08021608260615,13.6523208445742));
#47889=CARTESIAN_POINT('Ctrl Pts',(14.1692375188454,4.08020641551546,12.3979191365052));
#47890=CARTESIAN_POINT('Ctrl Pts',(14.1738610753222,4.08020264368447,11.8969840543586));
#47891=CARTESIAN_POINT('Ctrl Pts',(14.1833011346846,4.08019722714216,10.8951616868544));
#47892=CARTESIAN_POINT('Ctrl Pts',(14.1949232190994,4.08017961625232,9.64275109698061));
#47893=CARTESIAN_POINT('Ctrl Pts',(14.2072172257641,4.08016715485986,8.13843619450838));
#47894=CARTESIAN_POINT('Ctrl Pts',(14.2132228690599,4.08014617977765,7.13377888058149));
#47895=CARTESIAN_POINT('Ctrl Pts',(14.2160315118066,4.08013942757265,6.50628030649056));
#47896=CARTESIAN_POINT('Ctrl Pts',(14.2176986615796,4.08091122936134,6.26622708525673));
#47897=CARTESIAN_POINT('Ctrl Pts',(14.2227661810843,4.08496578782836,5.77613445723852));
#47898=CARTESIAN_POINT('Ctrl Pts',(14.234951250782,4.09724160665188,4.91165706708067));
#47899=CARTESIAN_POINT('Ctrl Pts',(14.2633316246722,4.1299454694222,3.14305425317667));
#47900=CARTESIAN_POINT('Ctrl Pts',(14.26163274653,4.13064083791219,1.57311169508529));
#47901=CARTESIAN_POINT('Ctrl Pts',(14.217808675051,4.07483069290229,0.4393870841717));
#47902=CARTESIAN_POINT('Ctrl Pts',(14.2121377388243,4.06744144356774,0.300155285117995));
#47903=CARTESIAN_POINT('Ctrl Pts',(14.1990028839386,4.05046808579315,0.0259639762829477));
#47904=CARTESIAN_POINT('Ctrl Pts',(14.1716535834632,4.01513330090296,-0.45073499273355));
#47905=CARTESIAN_POINT('Ctrl Pts',(14.1216470640614,3.95077230622961,-1.11832601035692));
#47906=CARTESIAN_POINT('Ctrl Pts',(14.0501571326149,3.85790200844971,-1.89955855307956));
#47907=CARTESIAN_POINT('Ctrl Pts',(13.9466278931188,3.72218464731662,-2.91468587912626));
#47908=CARTESIAN_POINT('Ctrl Pts',(13.8170860215073,3.54757776024588,-4.1356917687126));
#47909=CARTESIAN_POINT('Ctrl Pts',(13.7417991770219,3.44328100973835,-5.06703193017387));
#47910=CARTESIAN_POINT('Ctrl Pts',(13.711768974192,3.4023133314411,-5.63700537744905));
#47911=CARTESIAN_POINT('Ctrl Pts',(13.7006597439476,3.38683006257498,-5.87789745435641));
#47912=CARTESIAN_POINT('Ctrl Pts',(13.6818070884903,3.36109180040963,-6.35550542504808));
#47913=CARTESIAN_POINT('Ctrl Pts',(13.6566827315685,3.32792252231433,-7.20154490850171));
#47914=CARTESIAN_POINT('Ctrl Pts',(13.6385492426767,3.30849333959344,-8.4256484574165));
#47915=CARTESIAN_POINT('Ctrl Pts',(13.6323192556659,3.30761361742229,-9.67105362490119));
#47916=CARTESIAN_POINT('Ctrl Pts',(13.6281947514418,3.30648369164368,-10.5515920750503));
#47917=CARTESIAN_POINT('Ctrl Pts',(13.6249884359623,3.30417686766909,-11.0572537158354));
#47918=CARTESIAN_POINT('Ctrl Pts',(13.6229551503502,3.30221720858706,-11.3108889561999));
#47919=CARTESIAN_POINT('Ctrl Pts',(13.621209461118,3.30034221345478,-11.5020704562404));
#47920=CARTESIAN_POINT('Ctrl Pts',(13.62008300239,3.29917053339368,-11.6259943206145));
#47921=CARTESIAN_POINT('Ctrl Pts',(13.6179969710272,3.29707286346251,-11.8762260717926));
#47922=CARTESIAN_POINT('Ctrl Pts',(13.6147649750364,3.29405214925987,-12.3124479418529));
#47923=CARTESIAN_POINT('Ctrl Pts',(13.609813655358,3.29032832992611,-13.1846089255078));
#47924=CARTESIAN_POINT('Ctrl Pts',(13.6064272849751,3.29024237402413,-14.4288653820665));
#47925=CARTESIAN_POINT('Ctrl Pts',(13.6059488544036,3.29295603188387,-15.552953552654));
#47926=CARTESIAN_POINT('Ctrl Pts',(13.605935987415,3.29446857233125,-16.3061936218231));
#47927=CARTESIAN_POINT('Ctrl Pts',(13.6059686566929,3.29530204022143,-16.809555982347));
#47928=CARTESIAN_POINT('Ctrl Pts',(13.6059428832185,3.29561151559316,-17.1885703521757));
#47929=CARTESIAN_POINT('Ctrl Pts',(13.6058577881079,3.29557809642926,-17.5046193636793));
#47930=CARTESIAN_POINT('Ctrl Pts',(13.6058394331441,3.29556697172451,-17.6291257712303));
#47931=CARTESIAN_POINT('Ctrl Pts',(13.6058606477582,3.29555273863726,-17.8786039504253));
#47932=CARTESIAN_POINT('Ctrl Pts',(13.6059585834602,3.29554968779625,-18.1280470931691));
#47933=CARTESIAN_POINT('Ctrl Pts',(13.6061371979844,3.29556150239626,-18.3776851657281));
#47934=CARTESIAN_POINT('Ctrl Pts',(13.606277848496,3.29557461284349,-18.5337408186998));
#47935=CARTESIAN_POINT('Ctrl Pts',(13.6064085950517,3.29558906102363,-18.6586223633998));
#47936=CARTESIAN_POINT('Ctrl Pts',(13.6065149691708,3.2956017869801,-18.7522970792157));
#47937=CARTESIAN_POINT('Ctrl Pts',(13.6066103946943,3.29561400434787,-18.8303728404865));
#47938=CARTESIAN_POINT('Ctrl Pts',(13.6066909378835,3.29562481863403,-18.8928410419629));
#47939=CARTESIAN_POINT('Ctrl Pts',(13.6073975306193,3.29572224056636,-19.4238647637186));
#47940=CARTESIAN_POINT('Ctrl Pts',(13.6093482782903,3.29607453019957,-20.4404632592027));
#47941=CARTESIAN_POINT('Ctrl Pts',(13.613515444394,3.29730127902555,-21.9464317716729));
#47942=CARTESIAN_POINT('Ctrl Pts',(13.6164149373181,3.29868046736958,-22.9538279358975));
#47943=CARTESIAN_POINT('Ctrl Pts',(13.6181684020297,3.2997613576573,-23.5828481007943));
#47944=CARTESIAN_POINT('Ctrl Pts',(13.6189062948723,3.30023460562879,-23.8317453714256));
#47945=CARTESIAN_POINT('Ctrl Pts',(13.6205041705563,3.30133462782811,-24.3304715166219));
#47946=CARTESIAN_POINT('Ctrl Pts',(13.6235890300596,3.30361070112582,-25.2052634597723));
#47947=CARTESIAN_POINT('Ctrl Pts',(13.6284676637919,3.30752238854275,-26.4596112213963));
#47948=CARTESIAN_POINT('Ctrl Pts',(13.634391932039,3.31228885898376,-27.9684620455715));
#47949=CARTESIAN_POINT('Ctrl Pts',(13.6377145543258,3.31484211483178,-28.9739530226395));
#47950=CARTESIAN_POINT('Ctrl Pts',(13.6392827711463,3.31593712679648,-29.5391966731624));
#47951=CARTESIAN_POINT('Ctrl Pts',(13.6394729395101,3.31592737394666,-29.6699683072265));
#47952=CARTESIAN_POINT('Ctrl Pts',(13.6392609164336,3.31499860145106,-29.9277267142216));
#47953=CARTESIAN_POINT('Ctrl Pts',(13.6375060047046,3.31123579619119,-30.3782995864193));
#47954=CARTESIAN_POINT('Ctrl Pts',(13.6296869144124,3.29716631537485,-31.2701338041608));
#47955=CARTESIAN_POINT('Ctrl Pts',(13.6136132998802,3.26961315261814,-32.5208407448675));
#47956=CARTESIAN_POINT('Ctrl Pts',(13.6098028170218,3.26146264647698,-33.7375415486611));
#47957=CARTESIAN_POINT('Ctrl Pts',(13.6251691852064,3.28331170129501,-34.6892215501438));
#47958=CARTESIAN_POINT('Ctrl Pts',(13.6409911101313,3.3062856843424,-35.1574771360631));
#47959=CARTESIAN_POINT('Ctrl Pts',(13.6566505661323,3.32898166052496,-35.506308737971));
#47960=CARTESIAN_POINT('Ctrl Pts',(13.668999090906,3.34657459397007,-35.7315463147679));
#47961=CARTESIAN_POINT('Ctrl Pts',(13.7005318287958,3.39149074550588,-36.192735153184));
#47962=CARTESIAN_POINT('Ctrl Pts',(13.7716810680424,3.49154222603004,-37.0111939547442));
#47963=CARTESIAN_POINT('Ctrl Pts',(13.9588609326516,3.74776357601237,-38.7093739498868));
#47964=CARTESIAN_POINT('Ctrl Pts',(14.1256135782939,3.96387662432988,-40.2853147475507));
#47965=CARTESIAN_POINT('Ctrl Pts',(14.1827832858029,4.0436959918171,-41.6701713771011));
#47966=CARTESIAN_POINT('Ctrl Pts',(14.1961412729749,4.05981198579182,-42.080172583266));
#47967=CARTESIAN_POINT('Ctrl Pts',(14.2079179531119,4.06939224831422,-42.616605568901));
#47968=CARTESIAN_POINT('Ctrl Pts',(14.2161502176523,4.0727928413343,-43.1469071634193));
#47969=CARTESIAN_POINT('Ctrl Pts',(14.2205227502483,4.068049750572,-43.7976710866968));
#47970=CARTESIAN_POINT('Ctrl Pts',(14.2187737413236,4.05621093007814,-44.5590470961975));
#47971=CARTESIAN_POINT('Ctrl Pts',(14.2135158820145,4.0475021396245,-45.1768425637423));
#47972=CARTESIAN_POINT('Ctrl Pts',(14.2080910805333,4.04466830914136,-45.6605239026345));
#47973=CARTESIAN_POINT('Ctrl Pts',(14.2037801847839,4.04544563623318,-46.0180830518693));
#47974=CARTESIAN_POINT('Ctrl Pts',(14.1995182434366,4.04991129743658,-46.3702990795996));
#47975=CARTESIAN_POINT('Ctrl Pts',(14.1942624653917,4.06177576419791,-46.8327555084787));
#47976=CARTESIAN_POINT('Ctrl Pts',(14.1913862340194,4.07843457326759,-47.1713943500007));
#47977=CARTESIAN_POINT('Ctrl Pts',(14.1896746126773,4.10168956138419,-47.5060662243987));
#47978=CARTESIAN_POINT('Ctrl Pts',(14.1882421443729,4.11971388651359,-47.7607279322735));
#47979=CARTESIAN_POINT('Ctrl Pts',(14.1843422192657,4.15604054285058,-48.2499237009795));
#47980=CARTESIAN_POINT('Ctrl Pts',(14.1751633013163,4.22530318057308,-49.1081940334974));
#47981=CARTESIAN_POINT('Ctrl Pts',(14.1573527711649,4.34454619162834,-50.3093484640539));
#47982=CARTESIAN_POINT('Ctrl Pts',(14.1342139911527,4.53993015134586,-51.7215503416932));
#47983=CARTESIAN_POINT('Ctrl Pts',(14.1220648297914,4.71705492839944,-52.6412484343876));
#47984=CARTESIAN_POINT('Ctrl Pts',(14.1166308064331,4.84652873809678,-53.2116158079059));
#47985=CARTESIAN_POINT('Ctrl Pts',(14.1144335582758,4.90158703428815,-53.4464345864701));
#47986=CARTESIAN_POINT('Ctrl Pts',(14.1102019568884,5.01835112087333,-53.9153774892103));
#47987=CARTESIAN_POINT('Ctrl Pts',(14.1032136620098,5.24128557042568,-54.7411838437102));
#47988=CARTESIAN_POINT('Ctrl Pts',(14.0910217927261,5.75569340563091,-56.4035773722642));
#47989=CARTESIAN_POINT('Ctrl Pts',(14.0842516957791,6.29879311260299,-57.8378372308137));
#47990=CARTESIAN_POINT('Ctrl Pts',(14.0821871841893,6.71606534019326,-58.847357500806));
#47991=CARTESIAN_POINT('Ctrl Pts',(14.0820201446177,6.76407497581951,-58.9619890616024));
#47992=CARTESIAN_POINT('Ctrl Pts',(14.0817963392215,6.86488035175096,-59.1970713693669));
#47993=CARTESIAN_POINT('Ctrl Pts',(14.0817453597218,7.04752046534795,-59.6089408651268));
#47994=CARTESIAN_POINT('Ctrl Pts',(14.0828023551031,7.44003213478346,-60.4448202950792));
#47995=CARTESIAN_POINT('Ctrl Pts',(14.0858669857287,7.93746207099117,-61.4178104786779));
#47996=CARTESIAN_POINT('Ctrl Pts',(14.0894545601233,8.46103266591766,-62.4033076833214));
#47997=CARTESIAN_POINT('Ctrl Pts',(14.0914184630386,8.76069829853051,-62.9612408477037));
#47998=CARTESIAN_POINT('Ctrl Pts',(14.0925922460478,8.96077987034812,-63.3344945335607));
#47999=CARTESIAN_POINT('Ctrl Pts',(14.0933353002373,9.09412300562768,-63.5836692652343));
#48000=CARTESIAN_POINT('Ctrl Pts',(14.0939919971598,9.22718035069599,-63.8332859109708));
#48001=CARTESIAN_POINT('Ctrl Pts',(14.0944870410185,9.34305914081278,-64.0521290136193));
#48002=CARTESIAN_POINT('Ctrl Pts',(14.0947422228291,9.40906933161946,-64.1773000676098));
#48003=CARTESIAN_POINT('Ctrl Pts',(14.0950967381913,9.50784824011138,-64.3651616698595));
#48004=CARTESIAN_POINT('Ctrl Pts',(14.0953227844898,9.58964162844254,-64.5219739377058));
#48005=CARTESIAN_POINT('Ctrl Pts',(14.0956028563449,9.72395560691955,-64.7816511915711));
#48006=CARTESIAN_POINT('Ctrl Pts',(14.0958535991115,9.85473427639552,-65.0336275755987));
#48007=CARTESIAN_POINT('Ctrl Pts',(14.0962351499526,10.1206663563831,-65.5428821753181));
#48008=CARTESIAN_POINT('Ctrl Pts',(14.0965914144919,10.5834552915213,-66.421634553396));
#48009=CARTESIAN_POINT('Ctrl Pts',(14.0964307007463,11.5110342044253,-68.1599880905661));
#48010=CARTESIAN_POINT('Ctrl Pts',(14.0956266991408,12.3085214622441,-69.638494485163));
#48011=CARTESIAN_POINT('Ctrl Pts',(14.0956363216235,12.9117270788187,-70.7729400381487));
#48012=CARTESIAN_POINT('Ctrl Pts',(14.0956420689467,13.0449809453102,-71.0235492813001));
#48013=CARTESIAN_POINT('Ctrl Pts',(14.0956493556449,13.3120603585623,-71.5258457831659));
#48014=CARTESIAN_POINT('Ctrl Pts',(14.0956490445603,13.6454375622873,-72.1528340724319));
#48015=CARTESIAN_POINT('Ctrl Pts',(14.0956468516569,14.0454532421441,-72.9051544342605));
#48016=CARTESIAN_POINT('Ctrl Pts',(14.0956338135297,14.8450986579214,-74.4090765669485));
#48017=CARTESIAN_POINT('Ctrl Pts',(14.0955950884391,15.5110363957072,-75.6615435151467));
#48018=CARTESIAN_POINT('Ctrl Pts',(14.0955821654805,16.4807637197097,-77.4853390728469));
#48019=CARTESIAN_POINT('Ctrl Pts',(14.0955755061043,16.9172399919993,-78.3062334631458));
#48020=CARTESIAN_POINT('Ctrl Pts',(14.0955755061044,17.3537615793888,-79.127211165244));
#48021=CARTESIAN_POINT('Ctrl Pts',(16.9149146750659,4.07897667199088,24.8306334110303));
#48022=CARTESIAN_POINT('Ctrl Pts',(16.9149651977252,4.07897662056641,24.7817540574022));
#48023=CARTESIAN_POINT('Ctrl Pts',(16.9150181737118,4.0789765654222,24.7328757294337));
#48024=CARTESIAN_POINT('Ctrl Pts',(16.9156442730076,4.07897597177255,24.1822680919074));
#48025=CARTESIAN_POINT('Ctrl Pts',(16.9161269734332,4.07897518447184,23.1781399571955));
#48026=CARTESIAN_POINT('Ctrl Pts',(16.9172433640999,4.07897211690891,21.1695412597421));
#48027=CARTESIAN_POINT('Ctrl Pts',(16.9214155178135,4.07896883877421,19.6654077412023));
#48028=CARTESIAN_POINT('Ctrl Pts',(16.9302509496875,4.07896362085564,18.4143674188174));
#48029=CARTESIAN_POINT('Ctrl Pts',(16.9344872446245,4.07896071419103,17.911549791888));
#48030=CARTESIAN_POINT('Ctrl Pts',(16.9451259341652,4.07895312756752,16.9075638897551));
#48031=CARTESIAN_POINT('Ctrl Pts',(16.9679426050505,4.07893661648641,15.1537589849107));
#48032=CARTESIAN_POINT('Ctrl Pts',(16.9896349955101,4.0789273818902,13.652067309321));
#48033=CARTESIAN_POINT('Ctrl Pts',(17.003230380445,4.07892843819468,12.3976224720681));
#48034=CARTESIAN_POINT('Ctrl Pts',(17.0087877338512,4.0789296402581,11.8966775230641));
#48035=CARTESIAN_POINT('Ctrl Pts',(17.0201128766379,4.07893398003655,10.8948445658532));
#48036=CARTESIAN_POINT('Ctrl Pts',(17.0341306376338,4.07894601370972,9.6423540468266));
#48037=CARTESIAN_POINT('Ctrl Pts',(17.0489049863049,4.07896057755439,8.13790518564467));
#48038=CARTESIAN_POINT('Ctrl Pts',(17.056231342848,4.0789732683848,7.13321645454046));
#48039=CARTESIAN_POINT('Ctrl Pts',(17.0596285869194,4.07897831227912,6.50535580676845));
#48040=CARTESIAN_POINT('Ctrl Pts',(17.0612262769992,4.07917336989423,6.25763836117411));
#48041=CARTESIAN_POINT('Ctrl Pts',(17.0651710787483,4.08018959764778,5.7592455610475));
#48042=CARTESIAN_POINT('Ctrl Pts',(17.0734407068839,4.08324547128552,4.88428910557113));
#48043=CARTESIAN_POINT('Ctrl Pts',(17.0904584133639,4.09135539448048,3.1220081935595));
#48044=CARTESIAN_POINT('Ctrl Pts',(17.0891533677877,4.09145541777562,1.59973877304789));
#48045=CARTESIAN_POINT('Ctrl Pts',(17.0646709071443,4.07817954636044,0.522128338721078));
#48046=CARTESIAN_POINT('Ctrl Pts',(17.0614837486151,4.07644673010588,0.392785044077598));
#48047=CARTESIAN_POINT('Ctrl Pts',(17.0541257053017,4.0724504864719,0.135292485977696));
#48048=CARTESIAN_POINT('Ctrl Pts',(17.0388178453858,4.06413593022721,-0.314140200815017));
#48049=CARTESIAN_POINT('Ctrl Pts',(17.0110024464137,4.0489904422446,-0.951871992683431));
#48050=CARTESIAN_POINT('Ctrl Pts',(16.9709419512572,4.02715354110494,-1.71113231692929));
#48051=CARTESIAN_POINT('Ctrl Pts',(16.912684360406,3.99528529045317,-2.7160831512387));
#48052=CARTESIAN_POINT('Ctrl Pts',(16.8377628728703,3.95432262381237,-3.95990686830802));
#48053=CARTESIAN_POINT('Ctrl Pts',(16.7915419611338,3.92943076972257,-4.94437343056028));
#48054=CARTESIAN_POINT('Ctrl Pts',(16.772086427439,3.9194044335412,-5.55738411087098));
#48055=CARTESIAN_POINT('Ctrl Pts',(16.7648299758058,3.91568536083192,-5.80596409311825));
#48056=CARTESIAN_POINT('Ctrl Pts',(16.7521031374105,3.90937504184032,-6.30221922227335));
#48057=CARTESIAN_POINT('Ctrl Pts',(16.7342146873742,3.90103532864856,-7.17351055723086));
#48058=CARTESIAN_POINT('Ctrl Pts',(16.7188093989426,3.89544229392706,-8.42216908296638));
#48059=CARTESIAN_POINT('Ctrl Pts',(16.7105978259963,3.8942327556059,-9.6742176186002));
#48060=CARTESIAN_POINT('Ctrl Pts',(16.7052879353651,3.89351915368516,-10.5507039889754));
#48061=CARTESIAN_POINT('Ctrl Pts',(16.7019251356697,3.89283922134315,-11.0514122978929));
#48062=CARTESIAN_POINT('Ctrl Pts',(16.7000571407005,3.89235689075373,-11.3016868957108));
#48063=CARTESIAN_POINT('Ctrl Pts',(16.6985494828742,3.89192044803081,-11.4901024956647));
#48064=CARTESIAN_POINT('Ctrl Pts',(16.6975614038115,3.89164881404471,-11.6155271159647));
#48065=CARTESIAN_POINT('Ctrl Pts',(16.6956971873959,3.89118926092637,-11.8667984874337));
#48066=CARTESIAN_POINT('Ctrl Pts',(16.6927173666452,3.89059333721637,-12.305622960348));
#48067=CARTESIAN_POINT('Ctrl Pts',(16.6878322157708,3.89014397323601,-13.181630887958));
#48068=CARTESIAN_POINT('Ctrl Pts',(16.6834373461523,3.89110638138056,-14.4297904636907));
#48069=CARTESIAN_POINT('Ctrl Pts',(16.6816042897392,3.89263633585584,-15.5548111776018));
#48070=CARTESIAN_POINT('Ctrl Pts',(16.6808466165555,3.89341434739833,-16.3077059042397));
#48071=CARTESIAN_POINT('Ctrl Pts',(16.6804318274288,3.89383440847301,-16.8105532211299));
#48072=CARTESIAN_POINT('Ctrl Pts',(16.6802159758175,3.89399167832577,-17.1889053690298));
#48073=CARTESIAN_POINT('Ctrl Pts',(16.6800358900155,3.89399901650942,-17.5042315594726));
#48074=CARTESIAN_POINT('Ctrl Pts',(16.6799767886698,3.89401121920815,-17.628572830162));
#48075=CARTESIAN_POINT('Ctrl Pts',(16.6799068875002,3.89407032502083,-17.8777057176927));
#48076=CARTESIAN_POINT('Ctrl Pts',(16.679913398416,3.89417129025278,-18.1269066907719));
#48077=CARTESIAN_POINT('Ctrl Pts',(16.6799851027977,3.89430841468651,-18.3763595048988));
#48078=CARTESIAN_POINT('Ctrl Pts',(16.6800590290734,3.89440466408374,-18.5323341229066));
#48079=CARTESIAN_POINT('Ctrl Pts',(16.6801339494268,3.89448767657968,-18.6571673554093));
#48080=CARTESIAN_POINT('Ctrl Pts',(16.6801984108401,3.89455213286529,-18.7508154517068));
#48081=CARTESIAN_POINT('Ctrl Pts',(16.6802589473794,3.89460735325547,-18.8288767069996));
#48082=CARTESIAN_POINT('Ctrl Pts',(16.6803111947214,3.89465248203599,-18.8913377344271));
#48083=CARTESIAN_POINT('Ctrl Pts',(16.6807786103057,3.89503986621869,-19.4223275899097));
#48084=CARTESIAN_POINT('Ctrl Pts',(16.6824568240971,3.89575916697941,-20.439776571058));
#48085=CARTESIAN_POINT('Ctrl Pts',(16.6864874400154,3.89574282887653,-21.9492402018461));
#48086=CARTESIAN_POINT('Ctrl Pts',(16.6900714332117,3.89373179158201,-22.9605693115645));
#48087=CARTESIAN_POINT('Ctrl Pts',(16.6924571036858,3.89164348899801,-23.5925093952893));
#48088=CARTESIAN_POINT('Ctrl Pts',(16.6934692462877,3.89070366993123,-23.8431111230596));
#48089=CARTESIAN_POINT('Ctrl Pts',(16.6957568714141,3.88838138009332,-24.344487023896));
#48090=CARTESIAN_POINT('Ctrl Pts',(16.7003586297709,3.88334097133003,-25.2230673320503));
#48091=CARTESIAN_POINT('Ctrl Pts',(16.7081644394295,3.87406933870138,-26.479880505014));
#48092=CARTESIAN_POINT('Ctrl Pts',(16.7177935931692,3.86276510361262,-27.9870543427907));
#48093=CARTESIAN_POINT('Ctrl Pts',(16.7233193953658,3.85669854106861,-28.9885471470297));
#48094=CARTESIAN_POINT('Ctrl Pts',(16.7258535540266,3.85430623269711,-29.5503462654312));
#48095=CARTESIAN_POINT('Ctrl Pts',(16.7263168576138,3.85372101518925,-29.6770508651879));
#48096=CARTESIAN_POINT('Ctrl Pts',(16.7268790701398,3.85237600033726,-29.9292284771417));
#48097=CARTESIAN_POINT('Ctrl Pts',(16.7269982851966,3.84959656653962,-30.3706843069735));
#48098=CARTESIAN_POINT('Ctrl Pts',(16.7245363433686,3.84283451302849,-31.2514329399704));
#48099=CARTESIAN_POINT('Ctrl Pts',(16.7175349032075,3.83231245730799,-32.5042685138076));
#48100=CARTESIAN_POINT('Ctrl Pts',(16.7174964875878,3.82765847457322,-33.7475171559131));
#48101=CARTESIAN_POINT('Ctrl Pts',(16.7287497672298,3.83172266819031,-34.7351162525985));
#48102=CARTESIAN_POINT('Ctrl Pts',(16.7392901152939,3.83699566582681,-35.2264235346435));
#48103=CARTESIAN_POINT('Ctrl Pts',(16.7495253964372,3.84242433343839,-35.594735035358));
#48104=CARTESIAN_POINT('Ctrl Pts',(16.757597882556,3.84675307570527,-35.839518727925));
#48105=CARTESIAN_POINT('Ctrl Pts',(16.7777503546989,3.8577716135805,-36.3310864798155));
#48106=CARTESIAN_POINT('Ctrl Pts',(16.8218420325679,3.88242389109144,-37.1933485584074));
#48107=CARTESIAN_POINT('Ctrl Pts',(16.932759743038,3.94586133891672,-38.9293707178973));
#48108=CARTESIAN_POINT('Ctrl Pts',(17.0248342837548,4.00264192802993,-40.4465622192129));
#48109=CARTESIAN_POINT('Ctrl Pts',(17.0548534638343,4.02815505439204,-41.7334021407456));
#48110=CARTESIAN_POINT('Ctrl Pts',(17.0617900002719,4.0319026324534,-42.1316506025687));
#48111=CARTESIAN_POINT('Ctrl Pts',(17.0675846318347,4.03125442328988,-42.6479199311238));
#48112=CARTESIAN_POINT('Ctrl Pts',(17.0712609357292,4.02799382577384,-43.1619316799385));
#48113=CARTESIAN_POINT('Ctrl Pts',(17.0723042754547,4.02067663238492,-43.7952514515751));
#48114=CARTESIAN_POINT('Ctrl Pts',(17.0691441837673,4.01218212961586,-44.5420517787092));
#48115=CARTESIAN_POINT('Ctrl Pts',(17.0638977866498,4.00960088327479,-45.1523786175568));
#48116=CARTESIAN_POINT('Ctrl Pts',(17.0588510491071,4.01255629312146,-45.6331084565198));
#48117=CARTESIAN_POINT('Ctrl Pts',(17.0547671612117,4.01789369453871,-45.9899028044721));
#48118=CARTESIAN_POINT('Ctrl Pts',(17.0505511977916,4.02690254845307,-46.3428518603264));
#48119=CARTESIAN_POINT('Ctrl Pts',(17.0449963708357,4.0444916672167,-46.8082413517047));
#48120=CARTESIAN_POINT('Ctrl Pts',(17.0410653648893,4.06483665626451,-47.1513493295494));
#48121=CARTESIAN_POINT('Ctrl Pts',(17.0376999000655,4.09092409317607,-47.4917006453254));
#48122=CARTESIAN_POINT('Ctrl Pts',(17.0351503357226,4.11065377767826,-47.7400159897784));
#48123=CARTESIAN_POINT('Ctrl Pts',(17.0289836561659,4.15212670812739,-48.2235284994233));
#48124=CARTESIAN_POINT('Ctrl Pts',(17.0157609678126,4.23337229511935,-49.0717867229332));
#48125=CARTESIAN_POINT('Ctrl Pts',(16.9919464655623,4.37612993656612,-50.2688586222703));
#48126=CARTESIAN_POINT('Ctrl Pts',(16.9626550785882,4.60038614223337,-51.6886041014199));
#48127=CARTESIAN_POINT('Ctrl Pts',(16.9469695415295,4.79192210163469,-52.6222521044942));
#48128=CARTESIAN_POINT('Ctrl Pts',(16.9397627089671,4.92703807383931,-53.2035467307471));
#48129=CARTESIAN_POINT('Ctrl Pts',(16.9369146755773,4.98364117268894,-53.440722973793));
#48130=CARTESIAN_POINT('Ctrl Pts',(16.9314745786511,5.10264327431612,-53.9148837756041));
#48131=CARTESIAN_POINT('Ctrl Pts',(16.922607945119,5.32672256459404,-54.747790768806));
#48132=CARTESIAN_POINT('Ctrl Pts',(16.9076194942708,5.83458111882296,-56.4192674493408));
#48133=CARTESIAN_POINT('Ctrl Pts',(16.8999356945503,6.36284906266773,-57.8524303513783));
#48134=CARTESIAN_POINT('Ctrl Pts',(16.8974805636034,6.77168043251319,-58.8580127366239));
#48135=CARTESIAN_POINT('Ctrl Pts',(16.8972648103021,6.81915928483857,-58.9733155701948));
#48136=CARTESIAN_POINT('Ctrl Pts',(16.8969802126965,6.91846895958593,-59.2089983557977));
#48137=CARTESIAN_POINT('Ctrl Pts',(16.896917944298,7.09828865112667,-59.6220435374114));
#48138=CARTESIAN_POINT('Ctrl Pts',(16.8982412500171,7.48383323680778,-60.4592532906179));
#48139=CARTESIAN_POINT('Ctrl Pts',(16.9021949253572,7.97127227018086,-61.4324272317552));
#48140=CARTESIAN_POINT('Ctrl Pts',(16.9067378748187,8.48444954617013,-62.4167904717263));
#48141=CARTESIAN_POINT('Ctrl Pts',(16.9091943680861,8.77844615812734,-62.9736158842109));
#48142=CARTESIAN_POINT('Ctrl Pts',(16.9106594487652,8.97493743578547,-63.3459133746306));
#48143=CARTESIAN_POINT('Ctrl Pts',(16.911577598122,9.10595214562086,-63.5943917097937));
#48144=CARTESIAN_POINT('Ctrl Pts',(16.9124086561989,9.23676839272102,-63.8432182552755));
#48145=CARTESIAN_POINT('Ctrl Pts',(16.9130215853273,9.35080672825771,-64.0612843748139));
#48146=CARTESIAN_POINT('Ctrl Pts',(16.9133375675906,9.41579986074407,-64.1859854625765));
#48147=CARTESIAN_POINT('Ctrl Pts',(16.9137747317867,9.51309088246509,-64.3731159900114));
#48148=CARTESIAN_POINT('Ctrl Pts',(16.9140652969669,9.59371446454079,-64.529259559438));
#48149=CARTESIAN_POINT('Ctrl Pts',(16.9144167279272,9.72622726928115,-64.787754105224));
#48150=CARTESIAN_POINT('Ctrl Pts',(16.9147363867585,9.85549051025473,-65.0387769469754));
#48151=CARTESIAN_POINT('Ctrl Pts',(16.9152124179813,10.1188956091204,-65.5461829041274));
#48152=CARTESIAN_POINT('Ctrl Pts',(16.915685918939,10.5787468651793,-66.4222485940659));
#48153=CARTESIAN_POINT('Ctrl Pts',(16.9154868474475,11.5052148408086,-68.1572132791816));
#48154=CARTESIAN_POINT('Ctrl Pts',(16.914587493052,12.3063136758984,-69.6364416210659));
#48155=CARTESIAN_POINT('Ctrl Pts',(16.914633424635,12.9106480847908,-70.7731930265593));
#48156=CARTESIAN_POINT('Ctrl Pts',(16.9146383518857,13.0437985626505,-71.0236338700303));
#48157=CARTESIAN_POINT('Ctrl Pts',(16.9146470758778,13.3108863200786,-71.5259878708771));
#48158=CARTESIAN_POINT('Ctrl Pts',(16.9146570930598,13.6441973881165,-72.1528910927276));
#48159=CARTESIAN_POINT('Ctrl Pts',(16.9146600572098,14.0442047153699,-72.9052049952523));
#48160=CARTESIAN_POINT('Ctrl Pts',(16.9146582758106,14.8438344056538,-74.4090767084999));
#48161=CARTESIAN_POINT('Ctrl Pts',(16.9146627373669,15.5097822694014,-75.6615387328973));
#48162=CARTESIAN_POINT('Ctrl Pts',(16.9146737757476,16.4795080936937,-77.4853610045239));
#48163=CARTESIAN_POINT('Ctrl Pts',(16.9146794696564,16.9159645367713,-78.3062333142393));
#48164=CARTESIAN_POINT('Ctrl Pts',(16.9146794696565,17.3524861241607,-79.1272110163379));
#48165=CARTESIAN_POINT('Ctrl Pts',(19.7316905697294,4.07935448938162,24.830633935914));
#48166=CARTESIAN_POINT('Ctrl Pts',(19.731749408434,4.07935450933349,24.7817545980753));
#48167=CARTESIAN_POINT('Ctrl Pts',(19.73181113422,4.07935453691546,24.7328763236576));
#48168=CARTESIAN_POINT('Ctrl Pts',(19.7325392880933,4.07935456156444,24.1822676113171));
#48169=CARTESIAN_POINT('Ctrl Pts',(19.7330915102349,4.07935241872843,23.1781290371801));
#48170=CARTESIAN_POINT('Ctrl Pts',(19.734386066713,4.07935125552519,21.16952961444));
#48171=CARTESIAN_POINT('Ctrl Pts',(19.7392243248583,4.07934829382183,19.6653703770963));
#48172=CARTESIAN_POINT('Ctrl Pts',(19.7495130845821,4.0793521589517,18.4143189930037));
#48173=CARTESIAN_POINT('Ctrl Pts',(19.7544484885452,4.07935455477466,17.9115008539396));
#48174=CARTESIAN_POINT('Ctrl Pts',(19.766839498765,4.07935982008661,16.9075083417517));
#48175=CARTESIAN_POINT('Ctrl Pts',(19.7934209949296,4.07937279166992,15.1536950428428));
#48176=CARTESIAN_POINT('Ctrl Pts',(19.8186621736851,4.07937766165514,13.6519395529123));
#48177=CARTESIAN_POINT('Ctrl Pts',(19.834506757662,4.07938630977482,12.3974618327996));
#48178=CARTESIAN_POINT('Ctrl Pts',(19.8409870511261,4.07939063207221,11.896506822936));
#48179=CARTESIAN_POINT('Ctrl Pts',(19.8542109084696,4.07940376416714,10.8946632038776));
#48180=CARTESIAN_POINT('Ctrl Pts',(19.8705476717958,4.07941204516816,9.64212444575423));
#48181=CARTESIAN_POINT('Ctrl Pts',(19.887804112216,4.07942989188445,8.1376208453681));
#48182=CARTESIAN_POINT('Ctrl Pts',(19.8963059268321,4.07942448829874,7.13290173233056));
#48183=CARTESIAN_POINT('Ctrl Pts',(19.9002643271173,4.07942588898193,6.50490471479));
#48184=CARTESIAN_POINT('Ctrl Pts',(19.9018435195747,4.07940107803301,6.25434123804895));
#48185=CARTESIAN_POINT('Ctrl Pts',(19.9049508975073,4.07926731921548,5.75286295607368));
#48186=CARTESIAN_POINT('Ctrl Pts',(19.9100753780821,4.07884861781295,4.87399706060382));
#48187=CARTESIAN_POINT('Ctrl Pts',(19.9179299517214,4.07773750234611,3.11401396013838));
#48188=CARTESIAN_POINT('Ctrl Pts',(19.9160327000162,4.07760589988365,1.60935695765296));
#48189=CARTESIAN_POINT('Ctrl Pts',(19.9067271157157,4.07942683025897,0.552365774248749));
#48190=CARTESIAN_POINT('Ctrl Pts',(19.9055276056199,4.07967354567833,0.426638999775616));
#48191=CARTESIAN_POINT('Ctrl Pts',(19.9027400321877,4.08023663483943,0.175238431751414));
#48192=CARTESIAN_POINT('Ctrl Pts',(19.8969210328009,4.0814046752406,-0.264300184378953));
#48193=CARTESIAN_POINT('Ctrl Pts',(19.8861804513372,4.08348190805184,-0.891342867381702));
#48194=CARTESIAN_POINT('Ctrl Pts',(19.8707003983181,4.08640779973263,-1.64276387359526));
#48195=CARTESIAN_POINT('Ctrl Pts',(19.8478739867681,4.09051387445938,-2.64390761035535));
#48196=CARTESIAN_POINT('Ctrl Pts',(19.8184602098816,4.09548305738938,-3.89512046614111));
#48197=CARTESIAN_POINT('Ctrl Pts',(19.7995658555875,4.09828589820852,-4.8986886576812));
#48198=CARTESIAN_POINT('Ctrl Pts',(19.7910048215388,4.09935782538962,-5.52762127940719));
#48199=CARTESIAN_POINT('Ctrl Pts',(19.7876614372912,4.09974712809936,-5.77894874591882));
#48200=CARTESIAN_POINT('Ctrl Pts',(19.7813542100678,4.10035194775432,-6.28202511088013));
#48201=CARTESIAN_POINT('Ctrl Pts',(19.7712007143656,4.10100695113103,-7.16258996222176));
#48202=CARTESIAN_POINT('Ctrl Pts',(19.7590139140574,4.10104245326206,-8.42041961138705));
#48203=CARTESIAN_POINT('Ctrl Pts',(19.7493961943797,4.10061964535909,-9.67517807562287));
#48204=CARTESIAN_POINT('Ctrl Pts',(19.7437605557968,4.10047778183881,-10.5504750025485));
#48205=CARTESIAN_POINT('Ctrl Pts',(19.7407885077789,4.10049626661812,-11.0495578008507));
#48206=CARTESIAN_POINT('Ctrl Pts',(19.7393771920844,4.10054805882285,-11.2987018195911));
#48207=CARTESIAN_POINT('Ctrl Pts',(19.7383407909855,4.10060663713044,-11.4861849899995));
#48208=CARTESIAN_POINT('Ctrl Pts',(19.737667358513,4.10064799464512,-11.6122859436781));
#48209=CARTESIAN_POINT('Ctrl Pts',(19.7364020395687,4.10073774603204,-11.8641351428825));
#48210=CARTESIAN_POINT('Ctrl Pts',(19.7343937719702,4.10091189806865,-12.3042414007394));
#48211=CARTESIAN_POINT('Ctrl Pts',(19.7311318713114,4.10131291049498,-13.1821365759618));
#48212=CARTESIAN_POINT('Ctrl Pts',(19.7283662371774,4.10196984298857,-14.4319944615007));
#48213=CARTESIAN_POINT('Ctrl Pts',(19.7273504799056,4.10247530938435,-15.5570659964618));
#48214=CARTESIAN_POINT('Ctrl Pts',(19.7269580604332,4.10270448918149,-16.309427149594));
#48215=CARTESIAN_POINT('Ctrl Pts',(19.7267559570064,4.10282451667879,-16.8117648997344));
#48216=CARTESIAN_POINT('Ctrl Pts',(19.7266245428868,4.10286667409472,-17.1895525871661));
#48217=CARTESIAN_POINT('Ctrl Pts',(19.7265160857273,4.10287396504927,-17.5043370351011));
#48218=CARTESIAN_POINT('Ctrl Pts',(19.7265064163444,4.10288245535858,-17.6288438629665));
#48219=CARTESIAN_POINT('Ctrl Pts',(19.7266103048185,4.10291733055289,-17.8780646836674));
#48220=CARTESIAN_POINT('Ctrl Pts',(19.7268781409595,4.10297412970388,-18.1274070504594));
#48221=CARTESIAN_POINT('Ctrl Pts',(19.7272886495818,4.10304802339381,-18.3769304058717));
#48222=CARTESIAN_POINT('Ctrl Pts',(19.7275955378439,4.10309899866357,-18.5329468870759));
#48223=CARTESIAN_POINT('Ctrl Pts',(19.7278690490042,4.10314218015061,-18.6578030814957));
#48224=CARTESIAN_POINT('Ctrl Pts',(19.7280866533016,4.10317537676589,-18.7514657853085));
#48225=CARTESIAN_POINT('Ctrl Pts',(19.7282776058114,4.10320352312179,-18.8295358423443));
#48226=CARTESIAN_POINT('Ctrl Pts',(19.7284359336775,4.10322629604098,-18.8920023401028));
#48227=CARTESIAN_POINT('Ctrl Pts',(19.7298109404199,4.10342047933287,-19.4230282642657));
#48228=CARTESIAN_POINT('Ctrl Pts',(19.7331572114862,4.10377137295389,-20.4401908236404));
#48229=CARTESIAN_POINT('Ctrl Pts',(19.7369494432878,4.10344189876844,-21.9484042415267));
#48230=CARTESIAN_POINT('Ctrl Pts',(19.7358394579444,4.10198821210429,-22.9582963768966));
#48231=CARTESIAN_POINT('Ctrl Pts',(19.7333544804705,4.10053776327126,-23.5891593966175));
#48232=CARTESIAN_POINT('Ctrl Pts',(19.7321760621842,4.09988629850747,-23.8391695437685));
#48233=CARTESIAN_POINT('Ctrl Pts',(19.7290616593307,4.09829137473462,-24.339613135241));
#48234=CARTESIAN_POINT('Ctrl Pts',(19.7219239461885,4.09484772201759,-25.2168463500179));
#48235=CARTESIAN_POINT('Ctrl Pts',(19.7081538012807,4.08854495688428,-26.4727754554355));
#48236=CARTESIAN_POINT('Ctrl Pts',(19.6910680763066,4.08070275774671,-27.9803984717941));
#48237=CARTESIAN_POINT('Ctrl Pts',(19.682181615747,4.07644882190675,-28.9833847666746));
#48238=CARTESIAN_POINT('Ctrl Pts',(19.6789063358229,4.07474992627841,-29.5461747236964));
#48239=CARTESIAN_POINT('Ctrl Pts',(19.6781643290644,4.07439003395089,-29.6713449100555));
#48240=CARTESIAN_POINT('Ctrl Pts',(19.6765979656164,4.07370056899209,-29.9217094990869));
#48241=CARTESIAN_POINT('Ctrl Pts',(19.6736761126337,4.07257592588719,-30.3601050028827));
#48242=CARTESIAN_POINT('Ctrl Pts',(19.6674110815844,4.07062996206372,-31.2375938981368));
#48243=CARTESIAN_POINT('Ctrl Pts',(19.6589600545705,4.06853967488443,-32.4926327690216));
#48244=CARTESIAN_POINT('Ctrl Pts',(19.6554404212508,4.06698916538458,-33.7476184880732));
#48245=CARTESIAN_POINT('Ctrl Pts',(19.6580885878912,4.065868905903,-34.7503127027266));
#48246=CARTESIAN_POINT('Ctrl Pts',(19.6616531760529,4.06529455477844,-35.2511296095717));
#48247=CARTESIAN_POINT('Ctrl Pts',(19.665317861005,4.06485642982007,-35.6274105267477));
#48248=CARTESIAN_POINT('Ctrl Pts',(19.6682557022879,4.06452735058168,-35.8799831172533));
#48249=CARTESIAN_POINT('Ctrl Pts',(19.6759570604248,4.06377152046226,-36.3837372228955));
#48250=CARTESIAN_POINT('Ctrl Pts',(19.6938393828171,4.062297043252,-37.26353505748));
#48251=CARTESIAN_POINT('Ctrl Pts',(19.7419383911154,4.0591779187408,-39.014885353225));
#48252=CARTESIAN_POINT('Ctrl Pts',(19.787835736678,4.05803854631324,-40.5132616492215));
#48253=CARTESIAN_POINT('Ctrl Pts',(19.8076592637585,4.06081185444712,-41.7644661924603));
#48254=CARTESIAN_POINT('Ctrl Pts',(19.8127401621175,4.05882529185606,-42.1583425608284));
#48255=CARTESIAN_POINT('Ctrl Pts',(19.8182210067088,4.0527771384098,-42.6673496342845));
#48256=CARTESIAN_POINT('Ctrl Pts',(19.8229989227837,4.04528573324617,-43.1756057463211));
#48257=CARTESIAN_POINT('Ctrl Pts',(19.8278103195324,4.03460887261985,-43.8030097224572));
#48258=CARTESIAN_POINT('Ctrl Pts',(19.8323913480545,4.02410301328588,-44.545389174707));
#48259=CARTESIAN_POINT('Ctrl Pts',(19.8357640253749,4.02076109607437,-45.1540565174229));
#48260=CARTESIAN_POINT('Ctrl Pts',(19.8383792636965,4.02326144297558,-45.6346936020065));
#48261=CARTESIAN_POINT('Ctrl Pts',(19.8404448287581,4.02822588709096,-45.992036286084));
#48262=CARTESIAN_POINT('Ctrl Pts',(19.8426848273797,4.03673804444104,-46.3461583074312));
#48263=CARTESIAN_POINT('Ctrl Pts',(19.8459593924335,4.0534007785814,-46.8139160110249));
#48264=CARTESIAN_POINT('Ctrl Pts',(19.8490102862601,4.0725780024727,-47.1597454447569));
#48265=CARTESIAN_POINT('Ctrl Pts',(19.8524421822243,4.09707767505399,-47.5033352104608));
#48266=CARTESIAN_POINT('Ctrl Pts',(19.8549821621875,4.1154308208764,-47.7517883290858));
#48267=CARTESIAN_POINT('Ctrl Pts',(19.8609128581012,4.15406663927081,-48.2364844060615));
#48268=CARTESIAN_POINT('Ctrl Pts',(19.8730354455658,4.22979398838813,-49.0857137837747));
#48269=CARTESIAN_POINT('Ctrl Pts',(19.8928105255737,4.36366137946812,-50.2829982698093));
#48270=CARTESIAN_POINT('Ctrl Pts',(19.9110158584986,4.57797201329531,-51.7001736054087));
#48271=CARTESIAN_POINT('Ctrl Pts',(19.9140889565939,4.76458586101715,-52.6302330956112));
#48272=CARTESIAN_POINT('Ctrl Pts',(19.9113288594367,4.89772463046567,-53.2086743982499));
#48273=CARTESIAN_POINT('Ctrl Pts',(19.9097330121159,4.9537090997724,-53.4449852387809));
#48274=CARTESIAN_POINT('Ctrl Pts',(19.9047889632458,5.07187747957425,-53.917432226375));
#48275=CARTESIAN_POINT('Ctrl Pts',(19.8921640234306,5.29553920307492,-54.7478003303291));
#48276=CARTESIAN_POINT('Ctrl Pts',(19.8551417665773,5.8059701002291,-56.4156742081449));
#48277=CARTESIAN_POINT('Ctrl Pts',(19.8179048087849,6.33969776481573,-57.8484357420634));
#48278=CARTESIAN_POINT('Ctrl Pts',(19.8020555987685,6.75149430652742,-58.8550852625136));
#48279=CARTESIAN_POINT('Ctrl Pts',(19.8000495326012,6.79916648367612,-58.9701141739038));
#48280=CARTESIAN_POINT('Ctrl Pts',(19.7961289086579,6.89901093073692,-59.2055141726096));
#48281=CARTESIAN_POINT('Ctrl Pts',(19.7893504671894,7.07984491459817,-59.6180253267165));
#48282=CARTESIAN_POINT('Ctrl Pts',(19.7763661962944,7.46788194576182,-60.4545612854285));
#48283=CARTESIAN_POINT('Ctrl Pts',(19.7630048641413,7.95890168870625,-61.4275068436025));
#48284=CARTESIAN_POINT('Ctrl Pts',(19.7516453032531,8.47575416449995,-62.4121765161391));
#48285=CARTESIAN_POINT('Ctrl Pts',(19.7460529641767,8.77173687932521,-62.9693603278665));
#48286=CARTESIAN_POINT('Ctrl Pts',(19.7426787391143,8.96948177555833,-63.3419757199963));
#48287=CARTESIAN_POINT('Ctrl Pts',(19.7405303622212,9.10130626640622,-63.590688332912));
#48288=CARTESIAN_POINT('Ctrl Pts',(19.7385146449095,9.23290572032763,-63.8397804006721));
#48289=CARTESIAN_POINT('Ctrl Pts',(19.7368938568286,9.3475829472815,-64.0581101092336));
#48290=CARTESIAN_POINT('Ctrl Pts',(19.736006538874,9.41292900959727,-64.1829707544759));
#48291=CARTESIAN_POINT('Ctrl Pts',(19.734716083465,9.51073577429339,-64.370349741563));
#48292=CARTESIAN_POINT('Ctrl Pts',(19.7337155215584,9.59176751053624,-64.5267201302611));
#48293=CARTESIAN_POINT('Ctrl Pts',(19.7321833122377,9.72490590884203,-64.785616544752));
#48294=CARTESIAN_POINT('Ctrl Pts',(19.7307903414362,9.8546954230295,-65.0369589505087));
#48295=CARTESIAN_POINT('Ctrl Pts',(19.7287090777181,10.1189851698039,-65.5449893060533));
#48296=CARTESIAN_POINT('Ctrl Pts',(19.7266829189429,10.5798955165842,-66.4219623980084));
#48297=CARTESIAN_POINT('Ctrl Pts',(19.7276676576506,11.5068788766144,-68.1580753862004));
#48298=CARTESIAN_POINT('Ctrl Pts',(19.7318934421853,12.3068965513959,-69.6370766309225));
#48299=CARTESIAN_POINT('Ctrl Pts',(19.7317655953638,12.9109104740048,-70.7730753050621));
#48300=CARTESIAN_POINT('Ctrl Pts',(19.731747534186,13.0441058105992,-71.0235794241767));
#48301=CARTESIAN_POINT('Ctrl Pts',(19.7317183219463,13.3112072443434,-71.5259251673118));
#48302=CARTESIAN_POINT('Ctrl Pts',(19.7316918915079,13.6445569377086,-72.1528687312019));
#48303=CARTESIAN_POINT('Ctrl Pts',(19.7316858882025,14.0445750481121,-72.9051951966746));
#48304=CARTESIAN_POINT('Ctrl Pts',(19.731701553499,14.8442122836675,-74.4090975500849));
#48305=CARTESIAN_POINT('Ctrl Pts',(19.7317226301597,15.510148776986,-75.6615557162998));
#48306=CARTESIAN_POINT('Ctrl Pts',(19.7317044242158,16.479871690132,-77.4853474815518));
#48307=CARTESIAN_POINT('Ctrl Pts',(19.7316950307522,16.9163422836949,-78.3062335121641));
#48308=CARTESIAN_POINT('Ctrl Pts',(19.7316950307521,17.3528638710844,-79.1272112142626));
#48309=CARTESIAN_POINT('Ctrl Pts',(22.0806872581769,4.0817112774535,24.8306369402783));
#48310=CARTESIAN_POINT('Ctrl Pts',(22.0807531893061,4.08171138793248,24.7817576970255));
#48311=CARTESIAN_POINT('Ctrl Pts',(22.0808223364565,4.08171150089068,24.7328795140129));
#48312=CARTESIAN_POINT('Ctrl Pts',(22.0816389036773,4.08171296325905,24.1822720755345));
#48313=CARTESIAN_POINT('Ctrl Pts',(22.0822628297011,4.08171593727744,23.1781363452397));
#48314=CARTESIAN_POINT('Ctrl Pts',(22.0837134257396,4.0817218195251,21.1695390105029));
#48315=CARTESIAN_POINT('Ctrl Pts',(22.0891480761944,4.08173286928369,19.6653832895225));
#48316=CARTESIAN_POINT('Ctrl Pts',(22.1006837454411,4.0817473182421,18.4143332656791));
#48317=CARTESIAN_POINT('Ctrl Pts',(22.106215392913,4.08175442852641,17.9115211063208));
#48318=CARTESIAN_POINT('Ctrl Pts',(22.1201046843955,4.0817733584488,16.9075336614081));
#48319=CARTESIAN_POINT('Ctrl Pts',(22.1498965369521,4.08181298878673,15.1537211775948));
#48320=CARTESIAN_POINT('Ctrl Pts',(22.1782115772056,4.08184803808263,13.6519550007739));
#48321=CARTESIAN_POINT('Ctrl Pts',(22.1959821252523,4.08185640482049,12.3974562400484));
#48322=CARTESIAN_POINT('Ctrl Pts',(22.2032490945125,4.08185823625986,11.8964924068614));
#48323=CARTESIAN_POINT('Ctrl Pts',(22.2180712991417,4.08185590403518,10.8946345861558));
#48324=CARTESIAN_POINT('Ctrl Pts',(22.2364075742634,4.08185096497192,9.64209341000557));
#48325=CARTESIAN_POINT('Ctrl Pts',(22.2557598888455,4.08183561206296,8.13759363954354));
#48326=CARTESIAN_POINT('Ctrl Pts',(22.2653316985992,4.08183262212613,7.13289760894556));
#48327=CARTESIAN_POINT('Ctrl Pts',(22.2697798697298,4.08182891552378,6.50490839933043));
#48328=CARTESIAN_POINT('Ctrl Pts',(22.2714680039726,4.08179307578173,6.25425061006605));
#48329=CARTESIAN_POINT('Ctrl Pts',(22.2745101250835,4.08161068554481,5.75267104405992));
#48330=CARTESIAN_POINT('Ctrl Pts',(22.2789478637005,4.08107443746193,4.87368318059426));
#48331=CARTESIAN_POINT('Ctrl Pts',(22.2842233509257,4.07964539768461,3.11379727390321));
#48332=CARTESIAN_POINT('Ctrl Pts',(22.2823498152796,4.07968863300819,1.60985064855089));
#48333=CARTESIAN_POINT('Ctrl Pts',(22.2778081809785,4.08195512191518,0.553599358401225));
#48334=CARTESIAN_POINT('Ctrl Pts',(22.2772161841593,4.0822448224232,0.427984441741552));
#48335=CARTESIAN_POINT('Ctrl Pts',(22.275838864125,4.08291878036556,0.176781772273433));
#48336=CARTESIAN_POINT('Ctrl Pts',(22.2729491009355,4.08432382985036,-0.262431355723268));
#48337=CARTESIAN_POINT('Ctrl Pts',(22.2676105494159,4.08691133652606,-0.889101992934185));
#48338=CARTESIAN_POINT('Ctrl Pts',(22.2597610041138,4.09064398215328,-1.64029242724309));
#48339=CARTESIAN_POINT('Ctrl Pts',(22.2480116337292,4.09613028427393,-2.64145813674392));
#48340=CARTESIAN_POINT('Ctrl Pts',(22.2320940873357,4.10317395660869,-3.89327783208695));
#48341=CARTESIAN_POINT('Ctrl Pts',(22.2206681795821,4.10740367299369,-4.89747150057058));
#48342=CARTESIAN_POINT('Ctrl Pts',(22.2148552608892,4.10905808987711,-5.52672152324843));
#48343=CARTESIAN_POINT('Ctrl Pts',(22.2125378664224,4.10966736971728,-5.77793552878553));
#48344=CARTESIAN_POINT('Ctrl Pts',(22.2078972997522,4.11071887719346,-6.28095978966975));
#48345=CARTESIAN_POINT('Ctrl Pts',(22.1998362198795,4.11214569764531,-7.16146359659875));
#48346=CARTESIAN_POINT('Ctrl Pts',(22.1887604553002,4.11318625410649,-8.41957491079932));
#48347=CARTESIAN_POINT('Ctrl Pts',(22.1789920192977,4.11333851024897,-9.6750259227349));
#48348=CARTESIAN_POINT('Ctrl Pts',(22.1732201097211,4.11320661362161,-10.5510379086196));
#48349=CARTESIAN_POINT('Ctrl Pts',(22.1702828176501,4.11309903099946,-11.0505969687109));
#48350=CARTESIAN_POINT('Ctrl Pts',(22.1689438897613,4.11304030179607,-11.3000015048504));
#48351=CARTESIAN_POINT('Ctrl Pts',(22.1679877770531,4.11299599543326,-11.4876940375807));
#48352=CARTESIAN_POINT('Ctrl Pts',(22.1673581839659,4.11295442151722,-11.6141016365983));
#48353=CARTESIAN_POINT('Ctrl Pts',(22.1661543332355,4.11282692441663,-11.8664290867861));
#48354=CARTESIAN_POINT('Ctrl Pts',(22.1641885750189,4.1124961281729,-12.3073258727564));
#48355=CARTESIAN_POINT('Ctrl Pts',(22.1608085968938,4.11146884907708,-13.1863892779554));
#48356=CARTESIAN_POINT('Ctrl Pts',(22.1574251842106,4.10930348790506,-14.4367873212243));
#48357=CARTESIAN_POINT('Ctrl Pts',(22.1558729907192,4.10738504447621,-15.5609562570509));
#48358=CARTESIAN_POINT('Ctrl Pts',(22.155340060491,4.10648741718098,-16.3121472359132));
#48359=CARTESIAN_POINT('Ctrl Pts',(22.1551084149864,4.10601442669833,-16.8135559816661));
#48360=CARTESIAN_POINT('Ctrl Pts',(22.1550828627036,4.10582997028817,-17.1904736305975));
#48361=CARTESIAN_POINT('Ctrl Pts',(22.1551183195028,4.1058005333167,-17.5044814660014));
#48362=CARTESIAN_POINT('Ctrl Pts',(22.155179274139,4.10577633105441,-17.6294802209848));
#48363=CARTESIAN_POINT('Ctrl Pts',(22.1554734941708,4.10568791669081,-17.8791216720373));
#48364=CARTESIAN_POINT('Ctrl Pts',(22.1560114778335,4.10554739946089,-18.12893591468));
#48365=CARTESIAN_POINT('Ctrl Pts',(22.1567400996841,4.10537329353691,-18.3787108686903));
#48366=CARTESIAN_POINT('Ctrl Pts',(22.1572692425485,4.10525407920985,-18.5348529247192));
#48367=CARTESIAN_POINT('Ctrl Pts',(22.1577296457834,4.10515479122478,-18.6597699978175));
#48368=CARTESIAN_POINT('Ctrl Pts',(22.1580928061923,4.10507890335121,-18.7534645699545));
#48369=CARTESIAN_POINT('Ctrl Pts',(22.1584092338762,4.10501494381649,-18.8315471216055));
#48370=CARTESIAN_POINT('Ctrl Pts',(22.1586696170516,4.10496364273465,-18.8940160178554));
#48371=CARTESIAN_POINT('Ctrl Pts',(22.1609244923333,4.10452743167003,-19.4250166780277));
#48372=CARTESIAN_POINT('Ctrl Pts',(22.1666117086279,4.10371393162455,-20.4406887452964));
#48373=CARTESIAN_POINT('Ctrl Pts',(22.1728486493173,4.1048750925385,-21.9427050549345));
#48374=CARTESIAN_POINT('Ctrl Pts',(22.1721548195285,4.10870954669947,-22.9457918178194));
#48375=CARTESIAN_POINT('Ctrl Pts',(22.1689681366907,4.11250052261211,-23.5715577180345));
#48376=CARTESIAN_POINT('Ctrl Pts',(22.1674053242735,4.11420424041461,-23.8184716543449));
#48377=CARTESIAN_POINT('Ctrl Pts',(22.1632586022422,4.11833524471003,-24.3141483484936));
#48378=CARTESIAN_POINT('Ctrl Pts',(22.1536481125674,4.12720731324701,-25.184535378242));
#48379=CARTESIAN_POINT('Ctrl Pts',(22.135280394341,4.14306970300957,-26.4361733232101));
#48380=CARTESIAN_POINT('Ctrl Pts',(22.1119075504369,4.16259534336498,-27.9468610752968));
#48381=CARTESIAN_POINT('Ctrl Pts',(22.0998150320629,4.17286510122039,-28.9575801470414));
#48382=CARTESIAN_POINT('Ctrl Pts',(22.095134968522,4.1770426651094,-29.5262025538896));
#48383=CARTESIAN_POINT('Ctrl Pts',(22.0940862306972,4.17796210642411,-29.6513811403136));
#48384=CARTESIAN_POINT('Ctrl Pts',(22.0919769998257,4.17979334736485,-29.9025054603524));
#48385=CARTESIAN_POINT('Ctrl Pts',(22.0882790979027,4.18294814217091,-30.3419115460975));
#48386=CARTESIAN_POINT('Ctrl Pts',(22.0810018498695,4.18900722017071,-31.2218692521629));
#48387=CARTESIAN_POINT('Ctrl Pts',(22.0718693716956,4.19641679166098,-32.480798983417));
#48388=CARTESIAN_POINT('Ctrl Pts',(22.0669315823576,4.20090765113935,-33.7404563518645));
#48389=CARTESIAN_POINT('Ctrl Pts',(22.067020405947,4.20200039738248,-34.7472756017462));
#48390=CARTESIAN_POINT('Ctrl Pts',(22.0686865258567,4.20154261960756,-35.25032782635));
#48391=CARTESIAN_POINT('Ctrl Pts',(22.0706369822072,4.20079212635281,-35.6283477330854));
#48392=CARTESIAN_POINT('Ctrl Pts',(22.0722987978,4.20008504708062,-35.8822278341604));
#48393=CARTESIAN_POINT('Ctrl Pts',(22.0768288687233,4.19795632805282,-36.3884193841766));
#48394=CARTESIAN_POINT('Ctrl Pts',(22.0875114482299,4.19246069123774,-37.2723454492449));
#48395=CARTESIAN_POINT('Ctrl Pts',(22.1168195499966,4.17645376142218,-39.0309713117747));
#48396=CARTESIAN_POINT('Ctrl Pts',(22.1452208937072,4.15960897852894,-40.5324084559771));
#48397=CARTESIAN_POINT('Ctrl Pts',(22.160021497551,4.14994809813247,-41.7846755817295));
#48398=CARTESIAN_POINT('Ctrl Pts',(22.1640731974279,4.14408605348006,-42.1785184250812));
#48399=CARTESIAN_POINT('Ctrl Pts',(22.1689234073965,4.13301313193747,-42.688083469762));
#48400=CARTESIAN_POINT('Ctrl Pts',(22.1734502659695,4.12038747736818,-43.1970812016711));
#48401=CARTESIAN_POINT('Ctrl Pts',(22.1786439586059,4.10309924576169,-43.8258929583668));
#48402=CARTESIAN_POINT('Ctrl Pts',(22.184512600668,4.08404155036858,-44.5706823058272));
#48403=CARTESIAN_POINT('Ctrl Pts',(22.1894231114516,4.07286395725458,-45.1819851922531));
#48404=CARTESIAN_POINT('Ctrl Pts',(22.1936410112016,4.06864047791503,-45.665058999565));
#48405=CARTESIAN_POINT('Ctrl Pts',(22.1969596251638,4.06827562019768,-46.0244133809164));
#48406=CARTESIAN_POINT('Ctrl Pts',(22.2004867382473,4.07115636050592,-46.38071592816));
#48407=CARTESIAN_POINT('Ctrl Pts',(22.2055651893566,4.07990004759,-46.8516072133082));
#48408=CARTESIAN_POINT('Ctrl Pts',(22.2097599807653,4.09259101321018,-47.2000174156823));
#48409=CARTESIAN_POINT('Ctrl Pts',(22.2144340942165,4.11025304607408,-47.5464448219065));
#48410=CARTESIAN_POINT('Ctrl Pts',(22.2179845343943,4.1234000695629,-47.8012542930714));
#48411=CARTESIAN_POINT('Ctrl Pts',(22.2264508375367,4.14990942280532,-48.2941815322197));
#48412=CARTESIAN_POINT('Ctrl Pts',(22.2441171102791,4.2004838021227,-49.1547161665545));
#48413=CARTESIAN_POINT('Ctrl Pts',(22.2730861939326,4.29174641565724,-50.3543134049614));
#48414=CARTESIAN_POINT('Ctrl Pts',(22.3009319069203,4.45713611655791,-51.7546452965729));
#48415=CARTESIAN_POINT('Ctrl Pts',(22.3058715633566,4.62077825109781,-52.6609037956568));
#48416=CARTESIAN_POINT('Ctrl Pts',(22.3022024873703,4.74496293333649,-53.22130732141));
#48417=CARTESIAN_POINT('Ctrl Pts',(22.3000586188446,4.79829552597872,-53.4524280611144));
#48418=CARTESIAN_POINT('Ctrl Pts',(22.2931776516886,4.91313174392385,-53.91472992067));
#48419=CARTESIAN_POINT('Ctrl Pts',(22.27525507018,5.13638845677519,-54.7309787844978));
#48420=CARTESIAN_POINT('Ctrl Pts',(22.2225551369417,5.66344503276242,-56.3818257352234));
#48421=CARTESIAN_POINT('Ctrl Pts',(22.1709802552974,6.22850461206744,-57.8181758712166));
#48422=CARTESIAN_POINT('Ctrl Pts',(22.1514149325893,6.65724598612538,-58.8342802240781));
#48423=CARTESIAN_POINT('Ctrl Pts',(22.1489595264732,6.70600875414962,-58.9483090109368));
#48424=CARTESIAN_POINT('Ctrl Pts',(22.1442400202983,6.80879920661242,-59.1830571507315));
#48425=CARTESIAN_POINT('Ctrl Pts',(22.1363028643529,6.99498442952442,-59.5941165420173));
#48426=CARTESIAN_POINT('Ctrl Pts',(22.1217946990428,7.3956306795507,-60.4293377456673));
#48427=CARTESIAN_POINT('Ctrl Pts',(22.1082118821127,7.90372222660544,-61.4026487287963));
#48428=CARTESIAN_POINT('Ctrl Pts',(22.097131910433,8.43806063047352,-62.3895723906743));
#48429=CARTESIAN_POINT('Ctrl Pts',(22.091753128424,8.74353415108705,-62.9486874843298));
#48430=CARTESIAN_POINT('Ctrl Pts',(22.0885029341397,8.9472809575208,-63.3229122276346));
#48431=CARTESIAN_POINT('Ctrl Pts',(22.0864181423634,9.083002586351,-63.5727833041763));
#48432=CARTESIAN_POINT('Ctrl Pts',(22.0844775815037,9.21833703742369,-63.82317503393));
#48433=CARTESIAN_POINT('Ctrl Pts',(22.0828795252351,9.33609318052984,-64.0427690708459));
#48434=CARTESIAN_POINT('Ctrl Pts',(22.081997554122,9.40314135852388,-64.1683913455471));
#48435=CARTESIAN_POINT('Ctrl Pts',(22.0807043366672,9.50344054266713,-64.3569522702284));
#48436=CARTESIAN_POINT('Ctrl Pts',(22.079698989849,9.58642565845107,-64.5143969331008));
#48437=CARTESIAN_POINT('Ctrl Pts',(22.0781088241658,9.72258813692965,-64.7751907809016));
#48438=CARTESIAN_POINT('Ctrl Pts',(22.076697740684,9.85502070351906,-65.0282610850301));
#48439=CARTESIAN_POINT('Ctrl Pts',(22.0746378008923,10.1236397871968,-65.5395128310741));
#48440=CARTESIAN_POINT('Ctrl Pts',(22.0728859065854,10.5895145738863,-66.4212273936681));
#48441=CARTESIAN_POINT('Ctrl Pts',(22.0749234104754,11.5180077313772,-68.1632758098855));
#48442=CARTESIAN_POINT('Ctrl Pts',(22.0804594529303,12.3112391469442,-69.6409149901483));
#48443=CARTESIAN_POINT('Ctrl Pts',(22.0806257779101,12.9130724883053,-70.7727596451814));
#48444=CARTESIAN_POINT('Ctrl Pts',(22.0806527519314,13.0464178125152,-71.0235393205986));
#48445=CARTESIAN_POINT('Ctrl Pts',(22.0806944391854,13.3134515585615,-71.5257468364649));
#48446=CARTESIAN_POINT('Ctrl Pts',(22.0807296412911,13.6468658286295,-72.1527998158485));
#48447=CARTESIAN_POINT('Ctrl Pts',(22.0807366569763,14.0468732661696,-72.9051028689926));
#48448=CARTESIAN_POINT('Ctrl Pts',(22.0807103639373,14.8465315061039,-74.4090479193263));
#48449=CARTESIAN_POINT('Ctrl Pts',(22.0806660938293,15.5124783026127,-75.6615235028954));
#48450=CARTESIAN_POINT('Ctrl Pts',(22.0806849652143,16.4822164609512,-77.4853318752546));
#48451=CARTESIAN_POINT('Ctrl Pts',(22.0806947236768,16.9186987050899,-78.3062336020347));
#48452=CARTESIAN_POINT('Ctrl Pts',(22.0806947236768,17.3552202924793,-79.1272113041328));
#48453=CARTESIAN_POINT('Ctrl Pts',(23.9622955648791,4.08200208292847,24.8306372289488));
#48454=CARTESIAN_POINT('Ctrl Pts',(23.9623672448828,4.08200212320931,24.7817579944141));
#48455=CARTESIAN_POINT('Ctrl Pts',(23.9624424300683,4.08200216777709,24.7328798208572));
#48456=CARTESIAN_POINT('Ctrl Pts',(23.9633298985665,4.08200258379766,24.1822724635428));
#48457=CARTESIAN_POINT('Ctrl Pts',(23.9640073494789,4.08200366899808,23.1781369203715));
#48458=CARTESIAN_POINT('Ctrl Pts',(23.9655889010078,4.08200861120864,21.1695396264063));
#48459=CARTESIAN_POINT('Ctrl Pts',(23.9714912585163,4.08201016296143,19.6653829285451));
#48460=CARTESIAN_POINT('Ctrl Pts',(23.9840219927533,4.08200941516488,18.4143322408156));
#48461=CARTESIAN_POINT('Ctrl Pts',(23.9900323092972,4.08200976742032,17.9115202128027));
#48462=CARTESIAN_POINT('Ctrl Pts',(24.0051239731149,4.08201119176686,16.9075328742348));
#48463=CARTESIAN_POINT('Ctrl Pts',(24.037496132628,4.0820144081645,15.1537210085095));
#48464=CARTESIAN_POINT('Ctrl Pts',(24.068242343924,4.08200623174243,13.6519534556492));
#48465=CARTESIAN_POINT('Ctrl Pts',(24.0875228981722,4.08198831338579,12.3974529705996));
#48466=CARTESIAN_POINT('Ctrl Pts',(24.0954058032681,4.08197955514058,11.8964883932064));
#48467=CARTESIAN_POINT('Ctrl Pts',(24.1114809640743,4.08195780220778,10.8946300282762));
#48468=CARTESIAN_POINT('Ctrl Pts',(24.1313466678573,4.08191971253225,9.64208610714998));
#48469=CARTESIAN_POINT('Ctrl Pts',(24.1523116190628,4.08187527364994,8.1375880305666));
#48470=CARTESIAN_POINT('Ctrl Pts',(24.162661272085,4.08184505251405,7.13288645161328));
#48471=CARTESIAN_POINT('Ctrl Pts',(24.1674743487717,4.08183210280749,6.50490582828351));
#48472=CARTESIAN_POINT('Ctrl Pts',(24.1692799771994,4.0818096792317,6.25445557044036));
#48473=CARTESIAN_POINT('Ctrl Pts',(24.1724595365447,4.08170829787728,5.75310012246982));
#48474=CARTESIAN_POINT('Ctrl Pts',(24.1769118524244,4.08141173075345,4.87439057217338));
#48475=CARTESIAN_POINT('Ctrl Pts',(24.1816968570422,4.08064089883581,3.11432371976836));
#48476=CARTESIAN_POINT('Ctrl Pts',(24.1795300230087,4.08057722320863,1.60904293781249));
#48477=CARTESIAN_POINT('Ctrl Pts',(24.1759953565136,4.08176721012071,0.551230943523595));
#48478=CARTESIAN_POINT('Ctrl Pts',(24.1755386312866,4.08192464213912,0.425341023486164));
#48479=CARTESIAN_POINT('Ctrl Pts',(24.174466431991,4.08228588949836,0.173670854360428));
#48480=CARTESIAN_POINT('Ctrl Pts',(24.1722042923348,4.08303543284079,-0.266313863042626));
#48481=CARTESIAN_POINT('Ctrl Pts',(24.1679500685005,4.08438399185807,-0.893856249545121));
#48482=CARTESIAN_POINT('Ctrl Pts',(24.1616828022971,4.08630908814705,-1.64571238473509));
#48483=CARTESIAN_POINT('Ctrl Pts',(24.1521684529351,4.08906946798073,-2.6472116329457));
#48484=CARTESIAN_POINT('Ctrl Pts',(24.1392409619321,4.09252064208642,-3.89838880524634));
#48485=CARTESIAN_POINT('Ctrl Pts',(24.1296595937059,4.09456326651587,-4.90104830521301));
#48486=CARTESIAN_POINT('Ctrl Pts',(24.1245921150774,4.0953892226464,-5.52907006867696));
#48487=CARTESIAN_POINT('Ctrl Pts',(24.122543135074,4.09570581151499,-5.78005730609914));
#48488=CARTESIAN_POINT('Ctrl Pts',(24.1183711475979,4.09627961290835,-6.28254171768649));
#48489=CARTESIAN_POINT('Ctrl Pts',(24.110912934954,4.09713082267407,-7.162312337955));
#48490=CARTESIAN_POINT('Ctrl Pts',(24.1001218654103,4.09791704539196,-8.41971430174056));
#48491=CARTESIAN_POINT('Ctrl Pts',(24.0900005940753,4.09816054654107,-9.67499262570322));
#48492=CARTESIAN_POINT('Ctrl Pts',(24.0837261929461,4.09806168192696,-10.551155153125));
#48493=CARTESIAN_POINT('Ctrl Pts',(24.0804251175495,4.09793095582491,-11.0508803093238));
#48494=CARTESIAN_POINT('Ctrl Pts',(24.0788794798348,4.09784105346742,-11.3003946775157));
#48495=CARTESIAN_POINT('Ctrl Pts',(24.0777594081461,4.09776436119308,-11.4881778539406));
#48496=CARTESIAN_POINT('Ctrl Pts',(24.0770066256652,4.09770108469074,-11.6145632672188));
#48497=CARTESIAN_POINT('Ctrl Pts',(24.075502944022,4.09753197255658,-11.8668916405279));
#48498=CARTESIAN_POINT('Ctrl Pts',(24.072882864956,4.09713203653876,-12.3077631563438));
#48499=CARTESIAN_POINT('Ctrl Pts',(24.0677487709978,4.09597723281603,-13.1867776263164));
#48500=CARTESIAN_POINT('Ctrl Pts',(24.0611063576802,4.09369426111681,-14.4370753980823));
#48501=CARTESIAN_POINT('Ctrl Pts',(24.0568300528932,4.0917465099413,-15.5611346823936));
#48502=CARTESIAN_POINT('Ctrl Pts',(24.055047903523,4.09084877125918,-16.312237806251));
#48503=CARTESIAN_POINT('Ctrl Pts',(24.0541711416194,4.09038135679613,-16.8135860569128));
#48504=CARTESIAN_POINT('Ctrl Pts',(24.0538868311995,4.09020069604123,-17.1904517707465));
#48505=CARTESIAN_POINT('Ctrl Pts',(24.0538902418915,4.09017721932461,-17.504417356177));
#48506=CARTESIAN_POINT('Ctrl Pts',(24.0539261147657,4.09015693885285,-17.6294314542331));
#48507=CARTESIAN_POINT('Ctrl Pts',(24.0541305633638,4.09007310391961,-17.8790800058834));
#48508=CARTESIAN_POINT('Ctrl Pts',(24.0545220869184,4.08993459007116,-18.1289017837817));
#48509=CARTESIAN_POINT('Ctrl Pts',(24.055079936961,4.08976038112565,-18.3786753221093));
#48510=CARTESIAN_POINT('Ctrl Pts',(24.0554929637826,4.08964046612317,-18.534814836201));
#48511=CARTESIAN_POINT('Ctrl Pts',(24.0558594922731,4.08954025765299,-18.6597282953941));
#48512=CARTESIAN_POINT('Ctrl Pts',(24.0561516636267,4.08946354742096,-18.7534195243898));
#48513=CARTESIAN_POINT('Ctrl Pts',(24.0564089854875,4.08939881893064,-18.8314986568552));
#48514=CARTESIAN_POINT('Ctrl Pts',(24.0566228183052,4.08934683325637,-18.8939645198468));
#48515=CARTESIAN_POINT('Ctrl Pts',(24.0584852768486,4.08890451612297,-19.4249374335339));
#48516=CARTESIAN_POINT('Ctrl Pts',(24.0633643670787,4.08809475111636,-20.4404636917259));
#48517=CARTESIAN_POINT('Ctrl Pts',(24.0717452079226,4.08931496172151,-21.9421262926985));
#48518=CARTESIAN_POINT('Ctrl Pts',(24.0761460116141,4.09339376732741,-22.9448491109531));
#48519=CARTESIAN_POINT('Ctrl Pts',(24.0779762230367,4.0974562092785,-23.5703671053928));
#48520=CARTESIAN_POINT('Ctrl Pts',(24.0786796961305,4.09927817321484,-23.8170761770731));
#48521=CARTESIAN_POINT('Ctrl Pts',(24.0799760497679,4.10373186863751,-24.3124706455005));
#48522=CARTESIAN_POINT('Ctrl Pts',(24.0819970407477,4.11337074967939,-25.1824729583923));
#48523=CARTESIAN_POINT('Ctrl Pts',(24.0842021198426,4.1308454136294,-26.4339700730892));
#48524=CARTESIAN_POINT('Ctrl Pts',(24.0864078697437,4.15263365321005,-27.9450038672982));
#48525=CARTESIAN_POINT('Ctrl Pts',(24.0877812226619,4.16412692188707,-28.9562923588698));
#48526=CARTESIAN_POINT('Ctrl Pts',(24.0886514726177,4.1687482944764,-29.5253334387894));
#48527=CARTESIAN_POINT('Ctrl Pts',(24.0888326397504,4.16975911269941,-29.6506348041106));
#48528=CARTESIAN_POINT('Ctrl Pts',(24.0891409486858,4.17175142993273,-29.9019716591638));
#48529=CARTESIAN_POINT('Ctrl Pts',(24.0895498987179,4.17513461975883,-30.3417198488222));
#48530=CARTESIAN_POINT('Ctrl Pts',(24.0899602386112,4.18145381343337,-31.2221966398746));
#48531=CARTESIAN_POINT('Ctrl Pts',(24.0900269745172,4.18884650516548,-32.4813785165483));
#48532=CARTESIAN_POINT('Ctrl Pts',(24.0910174225162,4.19322095175136,-33.7405815354532));
#48533=CARTESIAN_POINT('Ctrl Pts',(24.0933253133805,4.19441944678141,-34.7466124020879));
#48534=CARTESIAN_POINT('Ctrl Pts',(24.0951479965203,4.19414850076315,-35.2491273596588));
#48535=CARTESIAN_POINT('Ctrl Pts',(24.0968191041055,4.1935978845164,-35.6266887560775));
#48536=CARTESIAN_POINT('Ctrl Pts',(24.0981285479769,4.19306099669884,-35.8801114343427));
#48537=CARTESIAN_POINT('Ctrl Pts',(24.1014087904296,4.19138300845976,-36.3856118091494));
#48538=CARTESIAN_POINT('Ctrl Pts',(24.1087164830883,4.18698244390804,-37.2685998966351));
#48539=CARTESIAN_POINT('Ctrl Pts',(24.1269844698749,4.17360041191136,-39.026696961175));
#48540=CARTESIAN_POINT('Ctrl Pts',(24.1415905609808,4.15823646272699,-40.530354778854));
#48541=CARTESIAN_POINT('Ctrl Pts',(24.143961339622,4.14796103186066,-41.7852242144327));
#48542=CARTESIAN_POINT('Ctrl Pts',(24.1443439544137,4.14179468730075,-42.1797011452874));
#48543=CARTESIAN_POINT('Ctrl Pts',(24.1442498711312,4.13010473975566,-42.6899536899554));
#48544=CARTESIAN_POINT('Ctrl Pts',(24.14378449886,4.11677123523734,-43.1995233294011));
#48545=CARTESIAN_POINT('Ctrl Pts',(24.1424974647182,4.09844750714945,-43.8288475600246));
#48546=CARTESIAN_POINT('Ctrl Pts',(24.139866251443,4.07803004113037,-44.5739413341453));
#48547=CARTESIAN_POINT('Ctrl Pts',(24.1367976109779,4.06571129506959,-45.18525201338));
#48548=CARTESIAN_POINT('Ctrl Pts',(24.133772595606,4.06058762318336,-45.6681760139594));
#48549=CARTESIAN_POINT('Ctrl Pts',(24.1312507499958,4.05958009324959,-46.0273487349289));
#48550=CARTESIAN_POINT('Ctrl Pts',(24.1284755233732,4.06185881345286,-46.38339949684));
#48551=CARTESIAN_POINT('Ctrl Pts',(24.1244252548433,4.06986374479445,-46.8538654027403));
#48552=CARTESIAN_POINT('Ctrl Pts',(24.1210589308145,4.08210270223804,-47.2018603071012));
#48553=CARTESIAN_POINT('Ctrl Pts',(24.1174132533512,4.0993842933789,-47.5478343049022));
#48554=CARTESIAN_POINT('Ctrl Pts',(24.1148393446767,4.11220700729379,-47.8032316024947));
#48555=CARTESIAN_POINT('Ctrl Pts',(24.1091958067937,4.13796629168275,-48.2966296675904));
#48556=CARTESIAN_POINT('Ctrl Pts',(24.0981441517371,4.1871107392127,-49.1577797770064));
#48557=CARTESIAN_POINT('Ctrl Pts',(24.0796951632445,4.27687296827978,-50.3567072681302));
#48558=CARTESIAN_POINT('Ctrl Pts',(24.0548574625172,4.44322788604528,-51.7533392942329));
#48559=CARTESIAN_POINT('Ctrl Pts',(24.0376307905872,4.60874279082569,-52.6550105143473));
#48560=CARTESIAN_POINT('Ctrl Pts',(24.0269167212642,4.73426592858213,-53.212210232132));
#48561=CARTESIAN_POINT('Ctrl Pts',(24.022261688763,4.78802914663047,-53.4409847524117));
#48562=CARTESIAN_POINT('Ctrl Pts',(24.011937980585,4.90444432727691,-53.899996095257));
#48563=CARTESIAN_POINT('Ctrl Pts',(23.9917197269347,5.13175954459855,-54.7119534677432));
#48564=CARTESIAN_POINT('Ctrl Pts',(23.946881494816,5.67152647254202,-56.3614849702221));
#48565=CARTESIAN_POINT('Ctrl Pts',(23.9149861796843,6.25065906002568,-57.8060061410901));
#48566=CARTESIAN_POINT('Ctrl Pts',(23.9082889999673,6.68463357757772,-58.8311245098676));
#48567=CARTESIAN_POINT('Ctrl Pts',(23.9077683667265,6.73386259900167,-58.9460129438745));
#48568=CARTESIAN_POINT('Ctrl Pts',(23.9070918607004,6.83745355958267,-59.1824653739889));
#48569=CARTESIAN_POINT('Ctrl Pts',(23.9070829160766,7.02450015525985,-59.5961205690869));
#48570=CARTESIAN_POINT('Ctrl Pts',(23.9109487883727,7.42501547924234,-60.4353539082253));
#48571=CARTESIAN_POINT('Ctrl Pts',(23.9216909852029,7.92938628651344,-61.4108375088605));
#48572=CARTESIAN_POINT('Ctrl Pts',(23.9340640848195,8.45818729151285,-62.3980996785296));
#48573=CARTESIAN_POINT('Ctrl Pts',(23.9408211940191,8.76022657679104,-62.9567360326512));
#48574=CARTESIAN_POINT('Ctrl Pts',(23.9448860238444,8.96170365245728,-63.3303615884543));
#48575=CARTESIAN_POINT('Ctrl Pts',(23.9474573707423,9.09592765324216,-63.5797569212499));
#48576=CARTESIAN_POINT('Ctrl Pts',(23.9497770282467,9.22980515457034,-63.8295558129152));
#48577=CARTESIAN_POINT('Ctrl Pts',(23.9515308576229,9.34634785666618,-64.0485240946921));
#48578=CARTESIAN_POINT('Ctrl Pts',(23.9524438717482,9.41272428541754,-64.1737568833352));
#48579=CARTESIAN_POINT('Ctrl Pts',(23.9537200122451,9.51203994843218,-64.361702149246));
#48580=CARTESIAN_POINT('Ctrl Pts',(23.9545752284772,9.59425793624058,-64.5185625171711));
#48581=CARTESIAN_POINT('Ctrl Pts',(23.9556701773485,9.72925393134929,-64.7783107806095));
#48582=CARTESIAN_POINT('Ctrl Pts',(23.9567284557211,9.86106264889938,-65.0312747707878));
#48583=CARTESIAN_POINT('Ctrl Pts',(23.9584683822691,10.1283193737384,-65.5418186150697));
#48584=CARTESIAN_POINT('Ctrl Pts',(23.9606501935929,10.5924204836096,-66.4227026698923));
#48585=CARTESIAN_POINT('Ctrl Pts',(23.9623055482788,11.5187962468744,-68.1634283976708));
#48586=CARTESIAN_POINT('Ctrl Pts',(23.9614773124919,12.3120252077534,-69.641062233731));
#48587=CARTESIAN_POINT('Ctrl Pts',(23.9621246704273,12.9136059543534,-70.773334928149));
#48588=CARTESIAN_POINT('Ctrl Pts',(23.9622527599848,13.0467770048231,-71.0239630352363));
#48589=CARTESIAN_POINT('Ctrl Pts',(23.9624420290191,13.3135967940574,-71.5260295392633));
#48590=CARTESIAN_POINT('Ctrl Pts',(23.9625647757318,13.6468141449215,-72.1528836114454));
#48591=CARTESIAN_POINT('Ctrl Pts',(23.9625770445063,14.0467309375321,-72.9050342749593));
#48592=CARTESIAN_POINT('Ctrl Pts',(23.962409408479,14.8463966744232,-74.4087646262313));
#48593=CARTESIAN_POINT('Ctrl Pts',(23.9620320808063,15.512652456629,-75.6613100284921));
#48594=CARTESIAN_POINT('Ctrl Pts',(23.9620255452841,16.4825593234147,-77.4854317343623));
#48595=CARTESIAN_POINT('Ctrl Pts',(23.9620221622173,16.9189893457455,-78.3062332078354));
#48596=CARTESIAN_POINT('Ctrl Pts',(23.9620221622173,17.355510933135,-79.1272109099336));
#48597=CARTESIAN_POINT('Ctrl Pts',(25.844570784284,4.08057977943501,24.8306353590067));
#48598=CARTESIAN_POINT('Ctrl Pts',(25.844648185704,4.08057966651517,24.7817560666017));
#48599=CARTESIAN_POINT('Ctrl Pts',(25.8447293650715,4.08057954730243,24.7328778289554));
#48600=CARTESIAN_POINT('Ctrl Pts',(25.8456878994455,4.08057817374023,24.1822699652252));
#48601=CARTESIAN_POINT('Ctrl Pts',(25.8464233826524,4.08057784177856,23.1781352323388));
#48602=CARTESIAN_POINT('Ctrl Pts',(25.8481374319039,4.08057692917578,21.1695367649276));
#48603=CARTESIAN_POINT('Ctrl Pts',(25.8545155933218,4.08056815801389,19.6653829487358));
#48604=CARTESIAN_POINT('Ctrl Pts',(25.8680382452856,4.08054600320532,18.4143333506094));
#48605=CARTESIAN_POINT('Ctrl Pts',(25.8745244558723,4.0805353149668,17.9115175621618));
#48606=CARTESIAN_POINT('Ctrl Pts',(25.8908129421233,4.0805085448771,16.907528530086));
#48607=CARTESIAN_POINT('Ctrl Pts',(25.925750354669,4.08045059698757,15.1537187688109));
#48608=CARTESIAN_POINT('Ctrl Pts',(25.9589300071752,4.08039564964573,13.6519725049998));
#48609=CARTESIAN_POINT('Ctrl Pts',(25.9797127722873,4.08035898548116,12.3974923061763));
#48610=CARTESIAN_POINT('Ctrl Pts',(25.9882070772645,4.08034368966931,11.8965356241494));
#48611=CARTESIAN_POINT('Ctrl Pts',(26.005518572936,4.08031121874985,10.8946878428175));
#48612=CARTESIAN_POINT('Ctrl Pts',(26.0269097431622,4.08027143363959,9.64215699732804));
#48613=CARTESIAN_POINT('Ctrl Pts',(26.0494661062327,4.08022743379009,8.13766358558484));
#48614=CARTESIAN_POINT('Ctrl Pts',(26.0606095379075,4.08020777316334,7.13296163855839));
#48615=CARTESIAN_POINT('Ctrl Pts',(26.0657868554483,4.08019818971332,6.50498953783284));
#48616=CARTESIAN_POINT('Ctrl Pts',(26.0677293368991,4.08019860392813,6.254821542523));
#48617=CARTESIAN_POINT('Ctrl Pts',(26.0711518004003,4.08021363683779,5.75377060631554));
#48618=CARTESIAN_POINT('Ctrl Pts',(26.0759579026102,4.08027080938024,4.87544910775995));
#48619=CARTESIAN_POINT('Ctrl Pts',(26.081128793862,4.08043695841909,3.11515403116237));
#48620=CARTESIAN_POINT('Ctrl Pts',(26.0788518154024,4.08045581336314,1.60815971006337));
#48621=CARTESIAN_POINT('Ctrl Pts',(26.0749837526961,4.08017495077629,0.548307353526776));
#48622=CARTESIAN_POINT('Ctrl Pts',(26.0744793339419,4.08013714720592,0.422056861710988));
#48623=CARTESIAN_POINT('Ctrl Pts',(26.0732989455254,4.08005053177588,0.169779472383307));
#48624=CARTESIAN_POINT('Ctrl Pts',(26.0708087506696,4.07987008450307,-0.271193576271456));
#48625=CARTESIAN_POINT('Ctrl Pts',(26.0661614568501,4.07954941719884,-0.899809220006871));
#48626=CARTESIAN_POINT('Ctrl Pts',(26.0592820344404,4.07909382231187,-1.65246885411488));
#48627=CARTESIAN_POINT('Ctrl Pts',(26.0488932000221,4.07846206268153,-2.65438880624532));
#48628=CARTESIAN_POINT('Ctrl Pts',(26.0346923351045,4.07769375101536,-3.9048842466606));
#48629=CARTESIAN_POINT('Ctrl Pts',(26.024217932681,4.07729272551322,-4.90564261911502));
#48630=CARTESIAN_POINT('Ctrl Pts',(26.0186988348058,4.07714577043534,-5.53205833177433));
#48631=CARTESIAN_POINT('Ctrl Pts',(26.0164949451559,4.07709446937418,-5.78287146791138));
#48632=CARTESIAN_POINT('Ctrl Pts',(26.0120848108843,4.07702655552691,-6.28477858997372));
#48633=CARTESIAN_POINT('Ctrl Pts',(26.0043862149626,4.0769874486626,-7.16375641765298));
#48634=CARTESIAN_POINT('Ctrl Pts',(25.9935479321394,4.07709939533413,-8.4201770232055));
#48635=CARTESIAN_POINT('Ctrl Pts',(25.9832001785983,4.07725903384453,-9.67481503127917));
#48636=CARTESIAN_POINT('Ctrl Pts',(25.9763642186198,4.07730127796632,-10.5506640151661));
#48637=CARTESIAN_POINT('Ctrl Pts',(25.9725930924616,4.07729366717744,-11.050257032386));
#48638=CARTESIAN_POINT('Ctrl Pts',(25.9707563537227,4.07727728154854,-11.2997214865617));
#48639=CARTESIAN_POINT('Ctrl Pts',(25.9693926551822,4.07725920620956,-11.4874662439065));
#48640=CARTESIAN_POINT('Ctrl Pts',(25.9684619723602,4.07724603910095,-11.6135983416455));
#48641=CARTESIAN_POINT('Ctrl Pts',(25.9665527693782,4.07721311695757,-11.8655778154556));
#48642=CARTESIAN_POINT('Ctrl Pts',(25.9631025382659,4.07714069706844,-12.3058419391744));
#48643=CARTESIAN_POINT('Ctrl Pts',(25.9559122008311,4.07694519975544,-13.1839670337358));
#48644=CARTESIAN_POINT('Ctrl Pts',(25.9456061675272,4.07655137577511,-14.4337708179989));
#48645=CARTESIAN_POINT('Ctrl Pts',(25.9382627210243,4.07618719946379,-15.5583998491895));
#48646=CARTESIAN_POINT('Ctrl Pts',(25.9349787321692,4.07603124892372,-16.3103112660927));
#48647=CARTESIAN_POINT('Ctrl Pts',(25.9332708395799,4.07595705010926,-16.8123083898932));
#48648=CARTESIAN_POINT('Ctrl Pts',(25.9326014082205,4.07593777072971,-17.1897929762814));
#48649=CARTESIAN_POINT('Ctrl Pts',(25.9324422746817,4.07595254629577,-17.5043122449826));
#48650=CARTESIAN_POINT('Ctrl Pts',(25.9323909876488,4.0759529390079,-17.6290107968246));
#48651=CARTESIAN_POINT('Ctrl Pts',(25.9323335197263,4.07595072339627,-17.8784039971533));
#48652=CARTESIAN_POINT('Ctrl Pts',(25.9323539449517,4.0759394659283,-18.1279353152333));
#48653=CARTESIAN_POINT('Ctrl Pts',(25.9324598599516,4.07592737655612,-18.377562269577));
#48654=CARTESIAN_POINT('Ctrl Pts',(25.9325656989019,4.07591881813072,-18.5336303782332));
#48655=CARTESIAN_POINT('Ctrl Pts',(25.9326749957718,4.07591254453843,-18.6585121522346));
#48656=CARTESIAN_POINT('Ctrl Pts',(25.9327699231852,4.07590797996094,-18.7521884498438));
#48657=CARTESIAN_POINT('Ctrl Pts',(25.9328601637811,4.07590438461883,-18.8302641974303));
#48658=CARTESIAN_POINT('Ctrl Pts',(25.9329390907671,4.07590182294606,-18.8927321535059));
#48659=CARTESIAN_POINT('Ctrl Pts',(25.9336501455939,4.07588108238224,-19.4237516127014));
#48660=CARTESIAN_POINT('Ctrl Pts',(25.9363009371823,4.07583341441431,-20.4403475109291));
#48661=CARTESIAN_POINT('Ctrl Pts',(25.9453630178633,4.07641698035684,-21.9459502231633));
#48662=CARTESIAN_POINT('Ctrl Pts',(25.9558794513379,4.07731497584596,-22.9529656912019));
#48663=CARTESIAN_POINT('Ctrl Pts',(25.9642086520499,4.07805728208967,-23.5817432715613));
#48664=CARTESIAN_POINT('Ctrl Pts',(25.9678540602757,4.07839867495163,-23.8304233353386));
#48665=CARTESIAN_POINT('Ctrl Pts',(25.9764013443531,4.07915865200955,-24.3288588433319));
#48666=CARTESIAN_POINT('Ctrl Pts',(25.9942301597475,4.0806592216352,-25.2032646909985));
#48667=CARTESIAN_POINT('Ctrl Pts',(26.025221328115,4.082732631673,-26.4576901759554));
#48668=CARTESIAN_POINT('Ctrl Pts',(26.0630445990899,4.08449353718692,-27.967094636833));
#48669=CARTESIAN_POINT('Ctrl Pts',(26.0829726200033,4.08489425524181,-28.9734406960325));
#48670=CARTESIAN_POINT('Ctrl Pts',(26.0913002227101,4.08499781220332,-29.5386707502503));
#48671=CARTESIAN_POINT('Ctrl Pts',(26.0931251317467,4.08502743350306,-29.6641131002139));
#48672=CARTESIAN_POINT('Ctrl Pts',(26.0966334094344,4.08507488495586,-29.9151404576258));
#48673=CARTESIAN_POINT('Ctrl Pts',(26.1024148737267,4.08512341588005,-30.3545438582529));
#48674=CARTESIAN_POINT('Ctrl Pts',(26.1126395490258,4.08512931616553,-31.233781402742));
#48675=CARTESIAN_POINT('Ctrl Pts',(26.1238689000862,4.08484171664707,-32.4903335546092));
#48676=CARTESIAN_POINT('Ctrl Pts',(26.1318887243776,4.08432971989877,-33.7454848406989));
#48677=CARTESIAN_POINT('Ctrl Pts',(26.1372094940222,4.08391397588549,-34.7474837791314));
#48678=CARTESIAN_POINT('Ctrl Pts',(26.1396084872277,4.08363675797948,-35.247707527111));
#48679=CARTESIAN_POINT('Ctrl Pts',(26.141371220675,4.08344203936742,-35.623440510749));
#48680=CARTESIAN_POINT('Ctrl Pts',(26.1426337835212,4.08327341585163,-35.8753722067299));
#48681=CARTESIAN_POINT('Ctrl Pts',(26.1453549329869,4.08282791481109,-36.3783044765536));
#48682=CARTESIAN_POINT('Ctrl Pts',(26.1503980487191,4.08171475754224,-37.257313806696));
#48683=CARTESIAN_POINT('Ctrl Pts',(26.1593188077099,4.07897427874934,-39.01007237833));
#48684=CARTESIAN_POINT('Ctrl Pts',(26.1581117957454,4.07706675221868,-40.5130850563031));
#48685=CARTESIAN_POINT('Ctrl Pts',(26.1442318739232,4.07761140540693,-41.7694461876314));
#48686=CARTESIAN_POINT('Ctrl Pts',(26.1397782129226,4.07464958837052,-42.1647424202513));
#48687=CARTESIAN_POINT('Ctrl Pts',(26.1330493969374,4.06699950959388,-42.6753154763828));
#48688=CARTESIAN_POINT('Ctrl Pts',(26.1257350602188,4.05768397496789,-43.1849413640208));
#48689=CARTESIAN_POINT('Ctrl Pts',(26.115365164687,4.04442739625451,-43.8136832824334));
#48690=CARTESIAN_POINT('Ctrl Pts',(26.1005460918204,4.03055517689925,-44.5570878496065));
#48691=CARTESIAN_POINT('Ctrl Pts',(26.0858584399693,4.02434764341965,-45.1661285977057));
#48692=CARTESIAN_POINT('Ctrl Pts',(26.0724650863366,4.02463040301721,-45.646760157016));
#48693=CARTESIAN_POINT('Ctrl Pts',(26.0615494470953,4.02797252451459,-46.003952285481));
#48694=CARTESIAN_POINT('Ctrl Pts',(26.0497046656066,4.03492112593504,-46.3577693998032));
#48695=CARTESIAN_POINT('Ctrl Pts',(26.0325958430163,4.04959367855714,-46.8249245878478));
#48696=CARTESIAN_POINT('Ctrl Pts',(26.0182065832668,4.06739629210528,-47.1700518562479));
#48697=CARTESIAN_POINT('Ctrl Pts',(26.0026297402098,4.09061053940423,-47.5128689033931));
#48698=CARTESIAN_POINT('Ctrl Pts',(25.9912336674935,4.10813287081449,-47.7635943609639));
#48699=CARTESIAN_POINT('Ctrl Pts',(25.9649865045349,4.14438276814989,-48.2503889637481));
#48700=CARTESIAN_POINT('Ctrl Pts',(25.9113335131762,4.214496021023,-49.1021605184574));
#48701=CARTESIAN_POINT('Ctrl Pts',(25.8199243549994,4.33678677328201,-50.2966447803426));
#48702=CARTESIAN_POINT('Ctrl Pts',(25.7129189353006,4.53530999157483,-51.7027703341965));
#48703=CARTESIAN_POINT('Ctrl Pts',(25.6623982059248,4.71624948069983,-52.621419873122));
#48704=CARTESIAN_POINT('Ctrl Pts',(25.6428686247225,4.84960861203734,-53.1915163476384));
#48705=CARTESIAN_POINT('Ctrl Pts',(25.6354037440851,4.90561734273628,-53.4216810401192));
#48706=CARTESIAN_POINT('Ctrl Pts',(25.622450587021,5.02663649475412,-53.8855341814151));
#48707=CARTESIAN_POINT('Ctrl Pts',(25.6045455906359,5.26086402238474,-54.7045799538225));
#48708=CARTESIAN_POINT('Ctrl Pts',(25.5859152122443,5.8106038398779,-56.3677207273517));
#48709=CARTESIAN_POINT('Ctrl Pts',(25.5936609389522,6.38981330126379,-57.8204867428421));
#48710=CARTESIAN_POINT('Ctrl Pts',(25.6082771767271,6.81852440848565,-58.8514652972658));
#48711=CARTESIAN_POINT('Ctrl Pts',(25.6108235337001,6.86784699759766,-58.9686583326326));
#48712=CARTESIAN_POINT('Ctrl Pts',(25.6164812962558,6.97062005327531,-59.2083923499976));
#48713=CARTESIAN_POINT('Ctrl Pts',(25.628647620426,7.15515134191995,-59.627341287499));
#48714=CARTESIAN_POINT('Ctrl Pts',(25.6599824454046,7.54546138682434,-60.4734127225068));
#48715=CARTESIAN_POINT('Ctrl Pts',(25.7063620960752,8.02861820652914,-61.4508681824153));
#48716=CARTESIAN_POINT('Ctrl Pts',(25.7526341951128,8.53156286551664,-62.435681976523));
#48717=CARTESIAN_POINT('Ctrl Pts',(25.7767943793768,8.81850578713554,-62.9913328103881));
#48718=CARTESIAN_POINT('Ctrl Pts',(25.7913328807926,9.01016007811373,-63.3622459744139));
#48719=CARTESIAN_POINT('Ctrl Pts',(25.8005534938435,9.13793802959155,-63.6096298946428));
#48720=CARTESIAN_POINT('Ctrl Pts',(25.8089946376101,9.26556868353528,-63.8571080587124));
#48721=CARTESIAN_POINT('Ctrl Pts',(25.8155491309342,9.37691360542288,-64.0737428963701));
#48722=CARTESIAN_POINT('Ctrl Pts',(25.8190373561112,9.44040887490913,-64.1975514715952));
#48723=CARTESIAN_POINT('Ctrl Pts',(25.8240016713012,9.53549980173153,-64.383268720066));
#48724=CARTESIAN_POINT('Ctrl Pts',(25.8275621499168,9.61440570071669,-64.538068934009));
#48725=CARTESIAN_POINT('Ctrl Pts',(25.8325698248521,9.74429868510807,-64.7941471789633));
#48726=CARTESIAN_POINT('Ctrl Pts',(25.8372188246519,9.87232665433277,-65.0452157696068));
#48727=CARTESIAN_POINT('Ctrl Pts',(25.8444371392966,10.1327681425613,-65.5513457195204));
#48728=CARTESIAN_POINT('Ctrl Pts',(25.8522523448846,10.5886367494958,-66.4260858166688));
#48729=CARTESIAN_POINT('Ctrl Pts',(25.8529704258499,11.5096169214689,-68.1585107930789));
#48730=CARTESIAN_POINT('Ctrl Pts',(25.8427466506853,12.3095608914108,-69.6375099740252));
#48731=CARTESIAN_POINT('Ctrl Pts',(25.84405505498,12.9128106186317,-70.7746794958561));
#48732=CARTESIAN_POINT('Ctrl Pts',(25.844306964925,13.0455079725974,-71.024753629924));
#48733=CARTESIAN_POINT('Ctrl Pts',(25.8446814868113,13.3119932674773,-71.5266931920502));
#48734=CARTESIAN_POINT('Ctrl Pts',(25.8449316978369,13.6447800575678,-72.153072250218));
#48735=CARTESIAN_POINT('Ctrl Pts',(25.8449597858347,14.0445382927846,-72.9049624655928));
#48736=CARTESIAN_POINT('Ctrl Pts',(25.844637678253,14.8441994652986,-74.4082520428641));
#48737=CARTESIAN_POINT('Ctrl Pts',(25.8439279150842,15.511032583249,-75.6609274498486));
#48738=CARTESIAN_POINT('Ctrl Pts',(25.8439346315324,16.4812454805264,-77.4856308339518));
#48739=CARTESIAN_POINT('Ctrl Pts',(25.8439377293388,16.9175685704731,-78.306234354275));
#48740=CARTESIAN_POINT('Ctrl Pts',(25.843937729339,17.3540901578626,-79.1272120563734));
#48741=CARTESIAN_POINT('Ctrl Pts',(27.7252597652467,4.07604430203363,24.830629906652));
#48742=CARTESIAN_POINT('Ctrl Pts',(27.725342633422,4.07604398489538,24.7817504395661));
#48743=CARTESIAN_POINT('Ctrl Pts',(27.7254295486928,4.07604365338282,24.7328720248872));
#48744=CARTESIAN_POINT('Ctrl Pts',(27.7264557041567,4.07603969724442,24.1822620861588));
#48745=CARTESIAN_POINT('Ctrl Pts',(27.7272430738068,4.07603395588985,23.1781243249467));
#48746=CARTESIAN_POINT('Ctrl Pts',(27.7290798647343,4.07601957377584,21.1695223025744));
#48747=CARTESIAN_POINT('Ctrl Pts',(27.7359069292677,4.07599287934245,19.6653679592558));
#48748=CARTESIAN_POINT('Ctrl Pts',(27.7503810766268,4.07594970932461,18.4143185095723));
#48749=CARTESIAN_POINT('Ctrl Pts',(27.757323963104,4.07592802362061,17.9114919920945));
#48750=CARTESIAN_POINT('Ctrl Pts',(27.7747592655169,4.07587160380069,16.9074951083392));
#48751=CARTESIAN_POINT('Ctrl Pts',(27.8121566969761,4.07575137527824,15.1536852342599));
#48752=CARTESIAN_POINT('Ctrl Pts',(27.8476686036972,4.07565137525816,13.6519715739283));
#48753=CARTESIAN_POINT('Ctrl Pts',(27.8699096323763,4.07561802498269,12.3975366392587));
#48754=CARTESIAN_POINT('Ctrl Pts',(27.8789999249988,4.07560775093695,11.8965984778399));
#48755=CARTESIAN_POINT('Ctrl Pts',(27.8975261319994,4.07559790364118,10.8947777778399));
#48756=CARTESIAN_POINT('Ctrl Pts',(27.92041464346,4.07559964500799,9.64226446740739));
#48757=CARTESIAN_POINT('Ctrl Pts',(27.9445489060284,4.07561795275291,8.13776813910616));
#48758=CARTESIAN_POINT('Ctrl Pts',(27.956465467892,4.07563038589341,7.13304469504194));
#48759=CARTESIAN_POINT('Ctrl Pts',(27.9620013880069,4.07563792059547,6.50505993209809));
#48760=CARTESIAN_POINT('Ctrl Pts',(27.9640898945436,4.07565339079377,6.2549958595789));
#48761=CARTESIAN_POINT('Ctrl Pts',(27.9678091802326,4.07572482436653,5.75405417771761));
#48762=CARTESIAN_POINT('Ctrl Pts',(27.9731241294107,4.07592958460531,4.8758699093757));
#48763=CARTESIAN_POINT('Ctrl Pts',(27.9791216548069,4.07647638005503,3.11547842572566));
#48764=CARTESIAN_POINT('Ctrl Pts',(27.9766408448158,4.07649656028921,1.60780894281924));
#48765=CARTESIAN_POINT('Ctrl Pts',(27.9716927842217,4.07569812473195,0.547187709820962));
#48766=CARTESIAN_POINT('Ctrl Pts',(27.9710490981585,4.0755954385535,0.420807592805693));
#48767=CARTESIAN_POINT('Ctrl Pts',(27.969544237905,4.07535654929588,0.168308988144524));
#48768=CARTESIAN_POINT('Ctrl Pts',(27.9663754136284,4.07485760897021,-0.273024725269034));
#48769=CARTESIAN_POINT('Ctrl Pts',(27.9604721629123,4.07394173010837,-0.902038225881202));
#48770=CARTESIAN_POINT('Ctrl Pts',(27.951789048622,4.07262501270999,-1.65498593663574));
#48771=CARTESIAN_POINT('Ctrl Pts',(27.9387566627383,4.07070977393899,-2.65703120096997));
#48772=CARTESIAN_POINT('Ctrl Pts',(27.9212160850017,4.06827102583396,-3.90721016180692));
#48773=CARTESIAN_POINT('Ctrl Pts',(27.9087198935433,4.06683898836998,-4.90728724033103));
#48774=CARTESIAN_POINT('Ctrl Pts',(27.9023452962071,4.06627680295807,-5.53318228176463));
#48775=CARTESIAN_POINT('Ctrl Pts',(27.8998132638848,4.06605006258839,-5.78420215251212));
#48776=CARTESIAN_POINT('Ctrl Pts',(27.8948169833875,4.06559904063942,-6.28620637550023));
#48777=CARTESIAN_POINT('Ctrl Pts',(27.8862467391115,4.06484014153083,-7.16528954655609));
#48778=CARTESIAN_POINT('Ctrl Pts',(27.8745228455075,4.06397616282331,-8.42123471706821));
#48779=CARTESIAN_POINT('Ctrl Pts',(27.8635486779871,4.06376894206732,-9.67470205018876));
#48780=CARTESIAN_POINT('Ctrl Pts',(27.8562974748696,4.06415849215986,-10.5493253285242));
#48781=CARTESIAN_POINT('Ctrl Pts',(27.8522752578299,4.06456154596584,-11.0481047440172));
#48782=CARTESIAN_POINT('Ctrl Pts',(27.8503056619078,4.06482741062643,-11.2971266153811));
#48783=CARTESIAN_POINT('Ctrl Pts',(27.8488380948691,4.06505369206006,-11.4845136170205));
#48784=CARTESIAN_POINT('Ctrl Pts',(27.8478387225673,4.06522635783411,-11.6100666615064));
#48785=CARTESIAN_POINT('Ctrl Pts',(27.8457949913781,4.06565345729717,-11.8611571983129));
#48786=CARTESIAN_POINT('Ctrl Pts',(27.8421172256742,4.06659833553217,-12.2999491112108));
#48787=CARTESIAN_POINT('Ctrl Pts',(27.83450473203,4.06914670333787,-13.1759408515894));
#48788=CARTESIAN_POINT('Ctrl Pts',(27.8236949615891,4.07399139474701,-14.4248681628644));
#48789=CARTESIAN_POINT('Ctrl Pts',(27.8159716061492,4.07805125044414,-15.5513490835192));
#48790=CARTESIAN_POINT('Ctrl Pts',(27.8124463356609,4.07987178138328,-16.3055406475485));
#48791=CARTESIAN_POINT('Ctrl Pts',(27.8105826109813,4.08079914276608,-16.8093285996371));
#48792=CARTESIAN_POINT('Ctrl Pts',(27.809806805342,4.08110792252154,-17.188491092894));
#48793=CARTESIAN_POINT('Ctrl Pts',(27.8095628641991,4.08109372160537,-17.5045006498987));
#48794=CARTESIAN_POINT('Ctrl Pts',(27.8094599355081,4.08111817749354,-17.6283252589352));
#48795=CARTESIAN_POINT('Ctrl Pts',(27.8092512127343,4.08124060372734,-17.8769952578661));
#48796=CARTESIAN_POINT('Ctrl Pts',(27.8090537139309,4.08146137275893,-18.1257048811657));
#48797=CARTESIAN_POINT('Ctrl Pts',(27.8088922868064,4.08174129213902,-18.3749058438896));
#48798=CARTESIAN_POINT('Ctrl Pts',(27.8088138483126,4.08193318914977,-18.5307639459064));
#48799=CARTESIAN_POINT('Ctrl Pts',(27.8087675428498,4.08209203328318,-18.6555488900249));
#48800=CARTESIAN_POINT('Ctrl Pts',(27.8087421554227,4.08221266043367,-18.7491773194674));
#48801=CARTESIAN_POINT('Ctrl Pts',(27.8087295957166,4.08231343946583,-18.8272385283061));
#48802=CARTESIAN_POINT('Ctrl Pts',(27.8087249750729,4.08239359400097,-18.8897085260827));
#48803=CARTESIAN_POINT('Ctrl Pts',(27.808720773895,4.08307069487227,-19.4208291291356));
#48804=CARTESIAN_POINT('Ctrl Pts',(27.809766220267,4.08419888503665,-20.440153362845));
#48805=CARTESIAN_POINT('Ctrl Pts',(27.8182931588619,4.08046837024067,-21.9572999985565));
#48806=CARTESIAN_POINT('Ctrl Pts',(27.8311639841231,4.07136164873529,-22.9768965828833));
#48807=CARTESIAN_POINT('Ctrl Pts',(27.8421249121948,4.06268008158841,-23.6149629631284));
#48808=CARTESIAN_POINT('Ctrl Pts',(27.8470036316719,4.05875847852701,-23.8695454397219));
#48809=CARTESIAN_POINT('Ctrl Pts',(27.8585771754437,4.0492928372162,-24.3769158141936));
#48810=CARTESIAN_POINT('Ctrl Pts',(27.8829116671664,4.02899651239132,-25.2639735759599));
#48811=CARTESIAN_POINT('Ctrl Pts',(27.9251515127041,3.99244565770101,-26.5254803374876));
#48812=CARTESIAN_POINT('Ctrl Pts',(27.975597257599,3.94679410327626,-28.0273674093273));
#48813=CARTESIAN_POINT('Ctrl Pts',(28.001404566098,3.92264214621878,-29.0184171325543));
#48814=CARTESIAN_POINT('Ctrl Pts',(28.011633827728,3.9131270121333,-29.5724349601575));
#48815=CARTESIAN_POINT('Ctrl Pts',(28.0138570161614,3.91102844849041,-29.6977826106848));
#48816=CARTESIAN_POINT('Ctrl Pts',(28.018141578614,3.90693672684914,-29.9472368861018));
#48817=CARTESIAN_POINT('Ctrl Pts',(28.0252029585086,3.90004491183638,-30.3844944289742));
#48818=CARTESIAN_POINT('Ctrl Pts',(28.0376368063003,3.88743466921074,-31.2586216643811));
#48819=CARTESIAN_POINT('Ctrl Pts',(28.0508118216071,3.87324243377045,-32.5073230373447));
#48820=CARTESIAN_POINT('Ctrl Pts',(28.058464528192,3.86541237630078,-33.7532405839383));
#48821=CARTESIAN_POINT('Ctrl Pts',(28.061598007007,3.8636961549409,-34.7471057905053));
#48822=CARTESIAN_POINT('Ctrl Pts',(28.0622160983558,3.86446398961727,-35.24299923233));
#48823=CARTESIAN_POINT('Ctrl Pts',(28.0623363568929,3.86569332284622,-35.6153653883871));
#48824=CARTESIAN_POINT('Ctrl Pts',(28.0624084040805,3.86672772959505,-35.8648400903879));
#48825=CARTESIAN_POINT('Ctrl Pts',(28.0624249857157,3.86960165717128,-36.3632178233884));
#48826=CARTESIAN_POINT('Ctrl Pts',(28.0619088716433,3.87670634631738,-37.234748718342));
#48827=CARTESIAN_POINT('Ctrl Pts',(28.0565239559215,3.89862226927546,-38.974858080016));
#48828=CARTESIAN_POINT('Ctrl Pts',(28.0375516851198,3.9288465415769,-40.4707855447929));
#48829=CARTESIAN_POINT('Ctrl Pts',(28.0058950939431,3.95825344195036,-41.7230304683817));
#48830=CARTESIAN_POINT('Ctrl Pts',(27.9961949133861,3.96418821564324,-42.1192273100256));
#48831=CARTESIAN_POINT('Ctrl Pts',(27.9822576273785,3.96804481463516,-42.6287445473197));
#48832=CARTESIAN_POINT('Ctrl Pts',(27.96755666201,3.97036276216118,-43.1369109547469));
#48833=CARTESIAN_POINT('Ctrl Pts',(27.9474881920418,3.97195109531181,-43.7623681408787));
#48834=CARTESIAN_POINT('Ctrl Pts',(27.9199217600844,3.97701783601881,-44.4997356664036));
#48835=CARTESIAN_POINT('Ctrl Pts',(27.8933868124384,3.98789191040196,-45.1018732863831));
#48836=CARTESIAN_POINT('Ctrl Pts',(27.8696213174653,4.00280086222066,-45.5759985059116));
#48837=CARTESIAN_POINT('Ctrl Pts',(27.8504479695429,4.01761013346641,-45.927772180604));
#48838=CARTESIAN_POINT('Ctrl Pts',(27.8298393555229,4.03654503788735,-46.2756787441312));
#48839=CARTESIAN_POINT('Ctrl Pts',(27.8003406194524,4.06792328209229,-46.7343239196486));
#48840=CARTESIAN_POINT('Ctrl Pts',(27.7758603434497,4.0990316860175,-47.072428902339));
#48841=CARTESIAN_POINT('Ctrl Pts',(27.7496222602011,4.13616544021014,-47.4076655151877));
#48842=CARTESIAN_POINT('Ctrl Pts',(27.7300808308059,4.16404867107337,-47.6433623245972));
#48843=CARTESIAN_POINT('Ctrl Pts',(27.6850539923559,4.22426306029349,-48.1101929853665));
#48844=CARTESIAN_POINT('Ctrl Pts',(27.593116066249,4.34318408401633,-48.9343820357971));
#48845=CARTESIAN_POINT('Ctrl Pts',(27.4408114174443,4.54500317820541,-50.122975463761));
#48846=CARTESIAN_POINT('Ctrl Pts',(27.2755250705735,4.83476078856946,-51.5727845981512));
#48847=CARTESIAN_POINT('Ctrl Pts',(27.2061907388541,5.06456125557638,-52.5505534801801));
#48848=CARTESIAN_POINT('Ctrl Pts',(27.183551494855,5.22154654919903,-53.1641767504487));
#48849=CARTESIAN_POINT('Ctrl Pts',(27.1763563639251,5.28455046882595,-53.4037136252652));
#48850=CARTESIAN_POINT('Ctrl Pts',(27.1666283628491,5.4182927063964,-53.8883422138275));
#48851=CARTESIAN_POINT('Ctrl Pts',(27.161798484126,5.66792564631842,-54.7358199162023));
#48852=CARTESIAN_POINT('Ctrl Pts',(27.1916742338282,6.22480761952307,-56.4369091352207));
#48853=CARTESIAN_POINT('Ctrl Pts',(27.2592709585012,6.770416555555,-57.893854841528));
#48854=CARTESIAN_POINT('Ctrl Pts',(27.3024918086758,7.16866025819872,-58.9208359710296));
#48855=CARTESIAN_POINT('Ctrl Pts',(27.308267792042,7.21667437315079,-59.0431743753317));
#48856=CARTESIAN_POINT('Ctrl Pts',(27.3208610029625,7.31419109541403,-59.2892156770369));
#48857=CARTESIAN_POINT('Ctrl Pts',(27.3458092890061,7.48742213377067,-59.7190455675896));
#48858=CARTESIAN_POINT('Ctrl Pts',(27.4054139778381,7.84408431333284,-60.578846302573));
#48859=CARTESIAN_POINT('Ctrl Pts',(27.4882088196579,8.26968443491987,-61.5593398063424));
#48860=CARTESIAN_POINT('Ctrl Pts',(27.5695998286669,8.70647993816199,-62.5358329011113));
#48861=CARTESIAN_POINT('Ctrl Pts',(27.611788194642,8.95561345643034,-63.0827825152622));
#48862=CARTESIAN_POINT('Ctrl Pts',(27.6371741472353,9.12285524300534,-63.4461212682437));
#48863=CARTESIAN_POINT('Ctrl Pts',(27.6532879455544,9.23465279481759,-63.68797698079));
#48864=CARTESIAN_POINT('Ctrl Pts',(27.6680588741092,9.34685836197186,-63.9291967606));
#48865=CARTESIAN_POINT('Ctrl Pts',(27.6796050030846,9.44538682052386,-64.1396796035441));
#48866=CARTESIAN_POINT('Ctrl Pts',(27.6857786186791,9.50178161071815,-64.2597736386839));
#48867=CARTESIAN_POINT('Ctrl Pts',(27.694600528921,9.58646123109406,-64.4397203232055));
#48868=CARTESIAN_POINT('Ctrl Pts',(27.7010045164677,9.6572128452808,-64.589276980363));
#48869=CARTESIAN_POINT('Ctrl Pts',(27.7101987626557,9.77449673083689,-64.8361386585405));
#48870=CARTESIAN_POINT('Ctrl Pts',(27.7186300515028,9.89251261724371,-65.0813968670931));
#48871=CARTESIAN_POINT('Ctrl Pts',(27.7315080399507,10.135523604251,-65.5752676778135));
#48872=CARTESIAN_POINT('Ctrl Pts',(27.7447877706368,10.5706174643503,-66.4328510835051));
#48873=CARTESIAN_POINT('Ctrl Pts',(27.7435062478646,11.48013096566,-68.1432586929741));
#48874=CARTESIAN_POINT('Ctrl Pts',(27.7229022051548,12.3005800439645,-69.6263475279766));
#48875=CARTESIAN_POINT('Ctrl Pts',(27.7246885000752,12.9095176561353,-70.7774414900148));
#48876=CARTESIAN_POINT('Ctrl Pts',(27.7250295580969,13.0411787435169,-71.0261772935901));
#48877=CARTESIAN_POINT('Ctrl Pts',(27.7255384777638,13.3071441815651,-71.5280548752207));
#48878=CARTESIAN_POINT('Ctrl Pts',(27.7258701397283,13.6390881555502,-72.1534463363424));
#48879=CARTESIAN_POINT('Ctrl Pts',(27.7259037645158,14.038578087583,-72.9048957167522));
#48880=CARTESIAN_POINT('Ctrl Pts',(27.7254557241049,14.8382159491145,-74.4073405563225));
#48881=CARTESIAN_POINT('Ctrl Pts',(27.7244616541709,15.5061273143185,-75.6602517422099));
#48882=CARTESIAN_POINT('Ctrl Pts',(27.7244571580331,16.4769049386683,-77.4860026540351));
#48883=CARTESIAN_POINT('Ctrl Pts',(27.7244524507195,16.9130347404094,-78.3062352076152));
#48884=CARTESIAN_POINT('Ctrl Pts',(27.7244524507195,17.3495563277989,-79.1272129097137));
#48885=CARTESIAN_POINT('Ctrl Pts',(29.5993149956237,4.07429432543499,24.8306289799893));
#48886=CARTESIAN_POINT('Ctrl Pts',(29.5994030211458,4.07429420375214,24.7817494857571));
#48887=CARTESIAN_POINT('Ctrl Pts',(29.59949534349,4.07429407638746,24.7328710442847));
#48888=CARTESIAN_POINT('Ctrl Pts',(29.6005854466145,4.07429257198405,24.1822607664862));
#48889=CARTESIAN_POINT('Ctrl Pts',(29.6014191999821,4.07428801440418,23.1781214006778));
#48890=CARTESIAN_POINT('Ctrl Pts',(29.6033606044468,4.07427518556936,21.169519334596));
#48891=CARTESIAN_POINT('Ctrl Pts',(29.610614365,4.07426533445962,19.6653671077297));
#48892=CARTESIAN_POINT('Ctrl Pts',(29.6260068844141,4.07426137190018,18.4143195377649));
#48893=CARTESIAN_POINT('Ctrl Pts',(29.6333886063572,4.07425835334317,17.9114922155898));
#48894=CARTESIAN_POINT('Ctrl Pts',(29.6519236564938,4.074248997782,16.9074941482145));
#48895=CARTESIAN_POINT('Ctrl Pts',(29.6916804235764,4.07422988477827,15.1536809080577));
#48896=CARTESIAN_POINT('Ctrl Pts',(29.7294577809132,4.0742302222938,13.6519679097109));
#48897=CARTESIAN_POINT('Ctrl Pts',(29.7531561761526,4.07426282133815,12.397538380551));
#48898=CARTESIAN_POINT('Ctrl Pts',(29.7628464015737,4.07427993524369,11.8966022439376));
#48899=CARTESIAN_POINT('Ctrl Pts',(29.7826085546186,4.07432680774722,10.894784447323));
#48900=CARTESIAN_POINT('Ctrl Pts',(29.8070480979797,4.07440292614643,9.64227387939513));
#48901=CARTESIAN_POINT('Ctrl Pts',(29.8328361859105,4.07449964963566,8.13777685229673));
#48902=CARTESIAN_POINT('Ctrl Pts',(29.8455822861327,4.07455385603853,7.13305293157917));
#48903=CARTESIAN_POINT('Ctrl Pts',(29.8515040877241,4.07457966189139,6.50506371904686));
#48904=CARTESIAN_POINT('Ctrl Pts',(29.8537404124718,4.07459708884447,6.25493787721224));
#48905=CARTESIAN_POINT('Ctrl Pts',(29.8577314727171,4.07465518968221,5.75392922686311));
#48906=CARTESIAN_POINT('Ctrl Pts',(29.8634595996021,4.07480340043025,4.87566199267245));
#48907=CARTESIAN_POINT('Ctrl Pts',(29.8699965156647,4.07517020734333,3.11532288435605));
#48908=CARTESIAN_POINT('Ctrl Pts',(29.8674400947039,4.07520573399403,1.60804732713263));
#48909=CARTESIAN_POINT('Ctrl Pts',(29.8620878347049,4.07472089968938,0.547889031456945));
#48910=CARTESIAN_POINT('Ctrl Pts',(29.8613895600481,4.07465767536286,0.421591316014558));
#48911=CARTESIAN_POINT('Ctrl Pts',(29.8597571396638,4.07451115277002,0.169232318339714));
#48912=CARTESIAN_POINT('Ctrl Pts',(29.856317121489,4.07420506061204,-0.271871253606398));
#48913=CARTESIAN_POINT('Ctrl Pts',(29.8499161122282,4.07364689547312,-0.900625008197283));
#48914=CARTESIAN_POINT('Ctrl Pts',(29.8404860937258,4.07284305568233,-1.65337249707067));
#48915=CARTESIAN_POINT('Ctrl Pts',(29.8263547165861,4.07168110269093,-2.65530752368736));
#48916=CARTESIAN_POINT('Ctrl Pts',(29.807320426347,4.07020206040575,-3.90565497565007));
#48917=CARTESIAN_POINT('Ctrl Pts',(29.7938144989464,4.06932573664757,-4.90618427242206));
#48918=CARTESIAN_POINT('Ctrl Pts',(29.7869485492971,4.06896712283885,-5.53245729202235));
#48919=CARTESIAN_POINT('Ctrl Pts',(29.7841978202766,4.06880921526131,-5.78358305763091));
#48920=CARTESIAN_POINT('Ctrl Pts',(29.778691800741,4.06845493287361,-6.2857910547242));
#48921=CARTESIAN_POINT('Ctrl Pts',(29.7690983039301,4.0677711656481,-7.1651450030849));
#48922=CARTESIAN_POINT('Ctrl Pts',(29.7558289847445,4.06683005027031,-8.42127075077741));
#48923=CARTESIAN_POINT('Ctrl Pts',(29.7439734570452,4.06650837692734,-9.67464607355679));
#48924=CARTESIAN_POINT('Ctrl Pts',(29.7368599281075,4.06690769772748,-10.5490660751661));
#48925=CARTESIAN_POINT('Ctrl Pts',(29.7331933528798,4.06735782533445,-11.0476884332829));
#48926=CARTESIAN_POINT('Ctrl Pts',(29.7315036662616,4.06766424952826,-11.2966188177246));
#48927=CARTESIAN_POINT('Ctrl Pts',(29.7302888303135,4.06792828189808,-11.4839285689021));
#48928=CARTESIAN_POINT('Ctrl Pts',(29.7294870043292,4.06813502516679,-11.6093235894704));
#48929=CARTESIAN_POINT('Ctrl Pts',(29.7279421809126,4.06865423676777,-11.8601860900761));
#48930=CARTESIAN_POINT('Ctrl Pts',(29.725389826179,4.06981981355778,-12.2986108981964));
#48931=CARTESIAN_POINT('Ctrl Pts',(29.7208768841446,4.07300452507182,-13.1741417640586));
#48932=CARTESIAN_POINT('Ctrl Pts',(29.7159894535552,4.07896435358632,-14.4230614670945));
#48933=CARTESIAN_POINT('Ctrl Pts',(29.713271253966,4.08361336207818,-15.5504015677926));
#48934=CARTESIAN_POINT('Ctrl Pts',(29.7120630728298,4.08547635296668,-16.3055682087937));
#48935=CARTESIAN_POINT('Ctrl Pts',(29.7114079961759,4.08632655897303,-16.810110543954));
#48936=CARTESIAN_POINT('Ctrl Pts',(29.711085673268,4.08644238934912,-17.1899505619475));
#48937=CARTESIAN_POINT('Ctrl Pts',(29.7108944071852,4.08617666123501,-17.5065808020651));
#48938=CARTESIAN_POINT('Ctrl Pts',(29.7108576273923,4.08607793182161,-17.630606021894));
#48939=CARTESIAN_POINT('Ctrl Pts',(29.7109134653549,4.0859388067722,-17.8796884198289));
#48940=CARTESIAN_POINT('Ctrl Pts',(29.7111542199351,4.08585618358414,-18.1287794582781));
#48941=CARTESIAN_POINT('Ctrl Pts',(29.7115472674956,4.08580725212287,-18.3783404698916));
#48942=CARTESIAN_POINT('Ctrl Pts',(29.711851431493,4.08578080996527,-18.5344117625362));
#48943=CARTESIAN_POINT('Ctrl Pts',(29.7121258668272,4.08575951266777,-18.6593604015799));
#48944=CARTESIAN_POINT('Ctrl Pts',(29.7123464933354,4.08574189092715,-18.7531080428038));
#48945=CARTESIAN_POINT('Ctrl Pts',(29.7125419244913,4.0857249533818,-18.8312657442226));
#48946=CARTESIAN_POINT('Ctrl Pts',(29.712704719546,4.0857098145209,-18.8938109813415));
#48947=CARTESIAN_POINT('Ctrl Pts',(29.7141245567445,4.08556846233154,-19.4255598315393));
#48948=CARTESIAN_POINT('Ctrl Pts',(29.7179165159392,4.08477473745439,-20.4459195671905));
#48949=CARTESIAN_POINT('Ctrl Pts',(29.7227947595283,4.07813595568139,-21.9631847030267));
#48950=CARTESIAN_POINT('Ctrl Pts',(29.7228197405083,4.06656944330437,-22.9821417896511));
#48951=CARTESIAN_POINT('Ctrl Pts',(29.7212855264258,4.05610940139834,-23.6197858299393));
#48952=CARTESIAN_POINT('Ctrl Pts',(29.7206006154444,4.05132379121746,-23.8755233732632));
#48953=CARTESIAN_POINT('Ctrl Pts',(29.7189966927731,4.03971846009631,-24.384080615756));
#48954=CARTESIAN_POINT('Ctrl Pts',(29.7156823742808,4.01487967422658,-25.2728408188628));
#48955=CARTESIAN_POINT('Ctrl Pts',(29.7096529350652,3.97135847452742,-26.5344569657397));
#48956=CARTESIAN_POINT('Ctrl Pts',(29.7011660287891,3.92207482840445,-28.0330195389327));
#48957=CARTESIAN_POINT('Ctrl Pts',(29.6937877062663,3.90004084220167,-29.0183931840762));
#48958=CARTESIAN_POINT('Ctrl Pts',(29.6892079956831,3.89304817141064,-29.5681789460954));
#48959=CARTESIAN_POINT('Ctrl Pts',(29.6882027168309,3.89146670769311,-29.6935042542137));
#48960=CARTESIAN_POINT('Ctrl Pts',(29.6861323114497,3.88849456448362,-29.9423467419571));
#48961=CARTESIAN_POINT('Ctrl Pts',(29.6823614333076,3.88366439358369,-30.3786763102188));
#48962=CARTESIAN_POINT('Ctrl Pts',(29.6742460534377,3.87579628390308,-31.2502924258845));
#48963=CARTESIAN_POINT('Ctrl Pts',(29.6609144555033,3.87026071660242,-32.4942654758644));
#48964=CARTESIAN_POINT('Ctrl Pts',(29.6451304702306,3.87442122751028,-33.7338440750293));
#48965=CARTESIAN_POINT('Ctrl Pts',(29.6310400941273,3.88480360350046,-34.7218015165097));
#48966=CARTESIAN_POINT('Ctrl Pts',(29.6234327027725,3.89240511171261,-35.2144370370806));
#48967=CARTESIAN_POINT('Ctrl Pts',(29.6175189787847,3.8991544760285,-35.5842589899869));
#48968=CARTESIAN_POINT('Ctrl Pts',(29.6136224179486,3.90400477355977,-35.8322093983451));
#48969=CARTESIAN_POINT('Ctrl Pts',(29.6059853898096,3.91498514479027,-36.3275547496979));
#48970=CARTESIAN_POINT('Ctrl Pts',(29.5928447866597,3.9372613712976,-37.1940447974019));
#48971=CARTESIAN_POINT('Ctrl Pts',(29.5651743675474,3.99332949963186,-38.925059677524));
#48972=CARTESIAN_POINT('Ctrl Pts',(29.5330583057904,4.05686719182932,-40.414463461334));
#48973=CARTESIAN_POINT('Ctrl Pts',(29.4939991631395,4.11458157887276,-41.6622338145054));
#48974=CARTESIAN_POINT('Ctrl Pts',(29.481999865542,4.1296577793405,-42.0586700846136));
#48975=CARTESIAN_POINT('Ctrl Pts',(29.4654870958894,4.14506807273594,-42.5669781608281));
#48976=CARTESIAN_POINT('Ctrl Pts',(29.4485009083319,4.15895663671303,-43.0737203583354));
#48977=CARTESIAN_POINT('Ctrl Pts',(29.4262500169145,4.17491366446097,-43.6965311392603));
#48978=CARTESIAN_POINT('Ctrl Pts',(29.3974965002966,4.19753376495065,-44.4296641893549));
#48979=CARTESIAN_POINT('Ctrl Pts',(29.3715705382284,4.22356199850653,-45.0274643139234));
#48980=CARTESIAN_POINT('Ctrl Pts',(29.3494795130514,4.25108923091108,-45.4979018229268));
#48981=CARTESIAN_POINT('Ctrl Pts',(29.3322638627556,4.27568310557469,-45.846778881379));
#48982=CARTESIAN_POINT('Ctrl Pts',(29.314392778617,4.30479313323617,-46.1917374920439));
#48983=CARTESIAN_POINT('Ctrl Pts',(29.2896832385308,4.35032906285243,-46.6464347261138));
#48984=CARTESIAN_POINT('Ctrl Pts',(29.2702566246333,4.39295370510534,-46.9816704378597));
#48985=CARTESIAN_POINT('Ctrl Pts',(29.2501760994589,4.4422994607737,-47.3139071855016));
#48986=CARTESIAN_POINT('Ctrl Pts',(29.2351822739187,4.47751987988122,-47.5356590347669));
#48987=CARTESIAN_POINT('Ctrl Pts',(29.2002771765164,4.55768479882917,-47.9870237659329));
#48988=CARTESIAN_POINT('Ctrl Pts',(29.1288193456356,4.72142273984953,-48.7928463859593));
#48989=CARTESIAN_POINT('Ctrl Pts',(29.0117058666492,5.01407715242886,-49.9892916781006));
#48990=CARTESIAN_POINT('Ctrl Pts',(28.8869853863707,5.42531794347212,-51.4870056708363));
#48991=CARTESIAN_POINT('Ctrl Pts',(28.8383531646819,5.71474040591769,-52.5218188230081));
#48992=CARTESIAN_POINT('Ctrl Pts',(28.8272637315404,5.892048266746,-53.1805071735208));
#48993=CARTESIAN_POINT('Ctrl Pts',(28.825826739766,5.9609963501372,-53.4337737250127));
#48994=CARTESIAN_POINT('Ctrl Pts',(28.8288000690768,6.10127380632862,-53.9449231453492));
#48995=CARTESIAN_POINT('Ctrl Pts',(28.8502088233308,6.34808337843803,-54.8299403145687));
#48996=CARTESIAN_POINT('Ctrl Pts',(28.9443258702338,6.85206468914668,-56.5772621940024));
#48997=CARTESIAN_POINT('Ctrl Pts',(29.0743550579446,7.29956809649302,-58.0245962648194));
#48998=CARTESIAN_POINT('Ctrl Pts',(29.142362196496,7.63396361850681,-59.025759487261));
#48999=CARTESIAN_POINT('Ctrl Pts',(29.150368314908,7.67645094579754,-59.1530718934086));
#49000=CARTESIAN_POINT('Ctrl Pts',(29.1674383162613,7.76052935149197,-59.403928184714));
#49001=CARTESIAN_POINT('Ctrl Pts',(29.1991223274621,7.9085528314483,-59.8431987406454));
#49002=CARTESIAN_POINT('Ctrl Pts',(29.2690812034583,8.20600540902721,-60.7147381602923));
#49003=CARTESIAN_POINT('Ctrl Pts',(29.3577344780619,8.55148910181861,-61.6969370343437));
#49004=CARTESIAN_POINT('Ctrl Pts',(29.4418444288282,8.90699328456685,-62.6614155249426));
#49005=CARTESIAN_POINT('Ctrl Pts',(29.4848798671639,9.11213719381989,-63.1968645443645));
#49006=CARTESIAN_POINT('Ctrl Pts',(29.5107875800078,9.25161829540371,-63.5505543400145));
#49007=CARTESIAN_POINT('Ctrl Pts',(29.5272502284902,9.34538419914306,-63.7854673786848));
#49008=CARTESIAN_POINT('Ctrl Pts',(29.5424086917862,9.44035300080261,-64.0189839127288));
#49009=CARTESIAN_POINT('Ctrl Pts',(29.5543617511136,9.52464115379926,-64.2220783195799));
#49010=CARTESIAN_POINT('Ctrl Pts',(29.5607958107896,9.57315913640717,-64.3377676283452));
#49011=CARTESIAN_POINT('Ctrl Pts',(29.5700392154857,9.64629549385839,-64.5109277939624));
#49012=CARTESIAN_POINT('Ctrl Pts',(29.5768712110625,9.70800834440408,-64.6544478555143));
#49013=CARTESIAN_POINT('Ctrl Pts',(29.5869086511977,9.81123656178933,-64.8908706102067));
#49014=CARTESIAN_POINT('Ctrl Pts',(29.5960573924192,9.91696695876116,-65.1275057385619));
#49015=CARTESIAN_POINT('Ctrl Pts',(29.609872181182,10.1392905384201,-65.6052501796801));
#49016=CARTESIAN_POINT('Ctrl Pts',(29.6236975019776,10.5494798153022,-66.4401818001343));
#49017=CARTESIAN_POINT('Ctrl Pts',(29.6208255037327,11.4459753092593,-68.123924432973));
#49018=CARTESIAN_POINT('Ctrl Pts',(29.597720877929,12.2927174915538,-69.6119030654474));
#49019=CARTESIAN_POINT('Ctrl Pts',(29.5992865022612,12.9092073399133,-70.780618733348));
#49020=CARTESIAN_POINT('Ctrl Pts',(29.5995928254283,13.0396901616617,-71.0277553580473));
#49021=CARTESIAN_POINT('Ctrl Pts',(29.600045825416,13.305178885112,-71.5296772981996));
#49022=CARTESIAN_POINT('Ctrl Pts',(29.6003457225441,13.6362082664364,-72.1539563517124));
#49023=CARTESIAN_POINT('Ctrl Pts',(29.6003778189031,14.0354313024268,-72.9049693850447));
#49024=CARTESIAN_POINT('Ctrl Pts',(29.5999843874973,14.8350251245033,-74.4065089551867));
#49025=CARTESIAN_POINT('Ctrl Pts',(29.5991125426097,15.5040220823233,-75.6596150039117));
#49026=CARTESIAN_POINT('Ctrl Pts',(29.5991128528511,16.4753612997457,-77.4864029689));
#49027=CARTESIAN_POINT('Ctrl Pts',(29.5991129894343,16.9112819153692,-78.3062324169441));
#49028=CARTESIAN_POINT('Ctrl Pts',(29.5991129894343,17.3478035027587,-79.1272101190426));
#49029=CARTESIAN_POINT('Ctrl Pts',(31.4687069735213,4.07784582772364,24.830632914927));
#49030=CARTESIAN_POINT('Ctrl Pts',(31.4688000635425,4.07784624467808,24.7817535405126));
#49031=CARTESIAN_POINT('Ctrl Pts',(31.4688976979175,4.07784668242652,24.7328752241303));
#49032=CARTESIAN_POINT('Ctrl Pts',(31.4700505243162,4.07785183613015,24.1822662583626));
#49033=CARTESIAN_POINT('Ctrl Pts',(31.4709279702857,4.07785362025415,23.178126478299));
#49034=CARTESIAN_POINT('Ctrl Pts',(31.4729683211627,4.07785665699013,21.169527575308));
#49035=CARTESIAN_POINT('Ctrl Pts',(31.4806396876406,4.07789079203985,19.6653772917441));
#49036=CARTESIAN_POINT('Ctrl Pts',(31.4969397650137,4.07797400571134,18.4143316530787));
#49037=CARTESIAN_POINT('Ctrl Pts',(31.5047549575706,4.07801375969669,17.9115124513854));
#49038=CARTESIAN_POINT('Ctrl Pts',(31.5243755589964,4.07811333944882,16.9075189304788));
#49039=CARTESIAN_POINT('Ctrl Pts',(31.5664619580017,4.07832811607674,15.1537000124256));
#49040=CARTESIAN_POINT('Ctrl Pts',(31.6064806007486,4.07853723942291,13.6519540876285));
#49041=CARTESIAN_POINT('Ctrl Pts',(31.6316328890473,4.07867877911592,12.3974905146125));
#49042=CARTESIAN_POINT('Ctrl Pts',(31.6419227892459,4.07873805562588,11.8965403339566));
#49043=CARTESIAN_POINT('Ctrl Pts',(31.662924688753,4.07886351330506,10.8947024710264));
#49044=CARTESIAN_POINT('Ctrl Pts',(31.6889231294956,4.07902358553982,9.64217598858967));
#49045=CARTESIAN_POINT('Ctrl Pts',(31.7163820564252,4.07919813160548,8.13767926649671));
#49046=CARTESIAN_POINT('Ctrl Pts',(31.7299663429113,4.07928360551118,7.13296679681987));
#49047=CARTESIAN_POINT('Ctrl Pts',(31.7362807752421,4.07932315893059,6.50498407946279));
#49048=CARTESIAN_POINT('Ctrl Pts',(31.7386607704019,4.07933720918986,6.25474989933836));
#49049=CARTESIAN_POINT('Ctrl Pts',(31.7428928314146,4.07935913196592,5.75362660739471));
#49050=CARTESIAN_POINT('Ctrl Pts',(31.748931792919,4.07938196538265,4.8752133773194));
#49051=CARTESIAN_POINT('Ctrl Pts',(31.7557359412242,4.07938753101485,3.11496826331555));
#49052=CARTESIAN_POINT('Ctrl Pts',(31.7530991072807,4.07936570054024,1.60835609825969));
#49053=CARTESIAN_POINT('Ctrl Pts',(31.747831202818,4.07940105300397,0.548987428145391));
#49054=CARTESIAN_POINT('Ctrl Pts',(31.7471431370894,4.07940625482527,0.422828438854361));
#49055=CARTESIAN_POINT('Ctrl Pts',(31.7455308102498,4.07941788807958,0.170703857723262));
#49056=CARTESIAN_POINT('Ctrl Pts',(31.7421250519014,4.0794418507879,-0.27001683645575));
#49057=CARTESIAN_POINT('Ctrl Pts',(31.7357664534412,4.07948298217841,-0.898351856990242));
#49058=CARTESIAN_POINT('Ctrl Pts',(31.7263746716039,4.07954010204105,-1.65078035668601));
#49059=CARTESIAN_POINT('Ctrl Pts',(31.7122659162751,4.0796168459856,-2.65254930057485));
#49060=CARTESIAN_POINT('Ctrl Pts',(31.6932033012039,4.07969634396477,-3.90315909986217));
#49061=CARTESIAN_POINT('Ctrl Pts',(31.6795777768752,4.07971951734305,-4.90443422286743));
#49062=CARTESIAN_POINT('Ctrl Pts',(31.6725906366524,4.07970971933928,-5.5313148080553));
#49063=CARTESIAN_POINT('Ctrl Pts',(31.6697485046803,4.07969691159586,-5.78231976151824));
#49064=CARTESIAN_POINT('Ctrl Pts',(31.6639217657505,4.079640700228,-6.28454501781444));
#49065=CARTESIAN_POINT('Ctrl Pts',(31.6534779552804,4.07947905658651,-7.16394174025885));
#49066=CARTESIAN_POINT('Ctrl Pts',(31.6386066476219,4.07915577397756,-8.42056430436979));
#49067=CARTESIAN_POINT('Ctrl Pts',(31.6257945049036,4.07895378579147,-9.67488459875914));
#49068=CARTESIAN_POINT('Ctrl Pts',(31.618960078523,4.07900247231926,-10.5502342652491));
#49069=CARTESIAN_POINT('Ctrl Pts',(31.6158110476425,4.07910303501304,-11.0494586612985));
#49070=CARTESIAN_POINT('Ctrl Pts',(31.6145143722234,4.0791799694181,-11.2987140498463));
#49071=CARTESIAN_POINT('Ctrl Pts',(31.6136515985956,4.07924915509268,-11.4862856583363));
#49072=CARTESIAN_POINT('Ctrl Pts',(31.6131274815052,4.07930249851795,-11.6121482637079));
#49073=CARTESIAN_POINT('Ctrl Pts',(31.6122901367677,4.07944550038625,-11.8637173726598));
#49074=CARTESIAN_POINT('Ctrl Pts',(31.6113447622238,4.07978032212702,-12.3033175014865));
#49075=CARTESIAN_POINT('Ctrl Pts',(31.6112783421474,4.08071914839239,-13.1805656977755));
#49076=CARTESIAN_POINT('Ctrl Pts',(31.6148523621694,4.08257692351233,-14.4303175338137));
#49077=CARTESIAN_POINT('Ctrl Pts',(31.6187202822993,4.08401670864369,-15.5562589293961));
#49078=CARTESIAN_POINT('Ctrl Pts',(31.6199776863949,4.08441232747168,-16.3094955671417));
#49079=CARTESIAN_POINT('Ctrl Pts',(31.6203606822337,4.08449522846437,-16.8124947920013));
#49080=CARTESIAN_POINT('Ctrl Pts',(31.620050118909,4.08431569993787,-17.1908997106453));
#49081=CARTESIAN_POINT('Ctrl Pts',(31.619310512475,4.08400162739168,-17.5062483640748));
#49082=CARTESIAN_POINT('Ctrl Pts',(31.6190954350977,4.0838836770891,-17.6311496466164));
#49083=CARTESIAN_POINT('Ctrl Pts',(31.6189782372705,4.08356741764711,-17.8809905469006));
#49084=CARTESIAN_POINT('Ctrl Pts',(31.6192751513199,4.08316160710082,-18.1309141329983));
#49085=CARTESIAN_POINT('Ctrl Pts',(31.6198655894181,4.08266314623051,-18.3809095800197));
#49086=CARTESIAN_POINT('Ctrl Pts',(31.6203368834378,4.08231761180404,-18.5371934816371));
#49087=CARTESIAN_POINT('Ctrl Pts',(31.6207596883997,4.08202049119935,-18.6622410423212));
#49088=CARTESIAN_POINT('Ctrl Pts',(31.6210967681186,4.08178802013735,-18.7560379646719));
#49089=CARTESIAN_POINT('Ctrl Pts',(31.6213915535343,4.08158651687251,-18.8342116652941));
#49090=CARTESIAN_POINT('Ctrl Pts',(31.6216335004812,4.08142051212769,-18.8967560255184));
#49091=CARTESIAN_POINT('Ctrl Pts',(31.6237261069884,4.07998516218906,-19.4284203111848));
#49092=CARTESIAN_POINT('Ctrl Pts',(31.6285980996611,4.0765381756599,-20.4459114336292));
#49093=CARTESIAN_POINT('Ctrl Pts',(31.6245096349564,4.07053585147111,-21.9527148393062));
#49094=CARTESIAN_POINT('Ctrl Pts',(31.6054527654478,4.06783851514021,-22.9604284739142));
#49095=CARTESIAN_POINT('Ctrl Pts',(31.5851502219919,4.06703322930736,-23.5894247381428));
#49096=CARTESIAN_POINT('Ctrl Pts',(31.5761557495189,4.06655258278944,-23.8414590433909));
#49097=CARTESIAN_POINT('Ctrl Pts',(31.5544793458723,4.06506216304023,-24.3436418296724));
#49098=CARTESIAN_POINT('Ctrl Pts',(31.5078634265954,4.0612182643314,-25.2229432881163));
#49099=CARTESIAN_POINT('Ctrl Pts',(31.4220683331932,4.05296711392328,-26.4759183308666));
#49100=CARTESIAN_POINT('Ctrl Pts',(31.3083228675675,4.04194537238345,-27.9716356437027));
#49101=CARTESIAN_POINT('Ctrl Pts',(31.241208833653,4.03900947809416,-28.9617904982848));
#49102=CARTESIAN_POINT('Ctrl Pts',(31.2102909779811,4.04093054226757,-29.5163696380308));
#49103=CARTESIAN_POINT('Ctrl Pts',(31.2034300134135,4.04147801988664,-29.6416653102345));
#49104=CARTESIAN_POINT('Ctrl Pts',(31.189882917682,4.04255656273384,-29.8910246976545));
#49105=CARTESIAN_POINT('Ctrl Pts',(31.166602866815,4.0446452051083,-30.3278701302552));
#49106=CARTESIAN_POINT('Ctrl Pts',(31.1217485478009,4.04968077060979,-31.2004186275354));
#49107=CARTESIAN_POINT('Ctrl Pts',(31.0625616532806,4.06093324452965,-32.4447029374165));
#49108=CARTESIAN_POINT('Ctrl Pts',(31.0097944727872,4.08113968644785,-33.6836095292349));
#49109=CARTESIAN_POINT('Ctrl Pts',(30.9713218638268,4.10469684596768,-34.6704253479765));
#49110=CARTESIAN_POINT('Ctrl Pts',(30.9533849362174,4.11934855872571,-35.1623178497854));
#49111=CARTESIAN_POINT('Ctrl Pts',(30.9403650528998,4.13152953971904,-35.5315351808384));
#49112=CARTESIAN_POINT('Ctrl Pts',(30.931962014745,4.14013412429074,-35.7797086367032));
#49113=CARTESIAN_POINT('Ctrl Pts',(30.9163631552964,4.1588670841948,-36.2752055194683));
#49114=CARTESIAN_POINT('Ctrl Pts',(30.8918999880386,4.1956918462424,-37.1421567095371));
#49115=CARTESIAN_POINT('Ctrl Pts',(30.8520875761949,4.28367231496665,-38.8741422979402));
#49116=CARTESIAN_POINT('Ctrl Pts',(30.824585745144,4.37976812029803,-40.3635451829372));
#49117=CARTESIAN_POINT('Ctrl Pts',(30.795647337687,4.4659231753878,-41.6110017876324));
#49118=CARTESIAN_POINT('Ctrl Pts',(30.7861469487672,4.48985586971024,-42.0060413061234));
#49119=CARTESIAN_POINT('Ctrl Pts',(30.7739391456391,4.51690834540139,-42.5137074529757));
#49120=CARTESIAN_POINT('Ctrl Pts',(30.7616615007434,4.54256551313821,-43.0199495146523));
#49121=CARTESIAN_POINT('Ctrl Pts',(30.7464969580757,4.57345561727011,-43.6428716432487));
#49122=CARTESIAN_POINT('Ctrl Pts',(30.7287732714005,4.61477282839475,-44.377217515882));
#49123=CARTESIAN_POINT('Ctrl Pts',(30.7147709802563,4.65741603609451,-44.977016357536));
#49124=CARTESIAN_POINT('Ctrl Pts',(30.704346797177,4.69924303580619,-45.4497221191383));
#49125=CARTESIAN_POINT('Ctrl Pts',(30.6969679517773,4.73509707802723,-45.8005692897468));
#49126=CARTESIAN_POINT('Ctrl Pts',(30.690109753667,4.77608970526089,-46.1477696955023));
#49127=CARTESIAN_POINT('Ctrl Pts',(30.6817966335565,4.83845043678961,-46.6057570928931));
#49128=CARTESIAN_POINT('Ctrl Pts',(30.6765542601007,4.89475954321947,-46.9437642923097));
#49129=CARTESIAN_POINT('Ctrl Pts',(30.6722371976059,4.95880011563281,-47.2786017031431));
#49130=CARTESIAN_POINT('Ctrl Pts',(30.6697139007788,5.00309856561159,-47.4923421202682));
#49131=CARTESIAN_POINT('Ctrl Pts',(30.6614671304962,5.10626565674607,-47.9366598900565));
#49132=CARTESIAN_POINT('Ctrl Pts',(30.6411558365244,5.31864108263074,-48.7344018720708));
#49133=CARTESIAN_POINT('Ctrl Pts',(30.5988468763563,5.69851407103839,-49.9380115029223));
#49134=CARTESIAN_POINT('Ctrl Pts',(30.5487314548176,6.20918068978983,-51.4657504505471));
#49135=CARTESIAN_POINT('Ctrl Pts',(30.5360732835478,6.53535513791848,-52.5416398339894));
#49136=CARTESIAN_POINT('Ctrl Pts',(30.5436070090105,6.71763690250309,-53.2362337071639));
#49137=CARTESIAN_POINT('Ctrl Pts',(30.5499302831122,6.78717803372439,-53.5040512714113));
#49138=CARTESIAN_POINT('Ctrl Pts',(30.5696211270458,6.92150899013218,-54.0411043082594));
#49139=CARTESIAN_POINT('Ctrl Pts',(30.6230773435729,7.14154958243025,-54.9641411305007));
#49140=CARTESIAN_POINT('Ctrl Pts',(30.7912110839135,7.5404246546231,-56.7578792993563));
#49141=CARTESIAN_POINT('Ctrl Pts',(30.9860329592378,7.84676198898512,-58.1861024721125));
#49142=CARTESIAN_POINT('Ctrl Pts',(31.0752271371353,8.09892223662111,-59.1454725131373));
#49143=CARTESIAN_POINT('Ctrl Pts',(31.0853218009868,8.13314032704081,-59.2761377230917));
#49144=CARTESIAN_POINT('Ctrl Pts',(31.1058757443481,8.1990465314762,-59.5286092028247));
#49145=CARTESIAN_POINT('Ctrl Pts',(31.1414352880725,8.31446356687814,-59.9722776557029));
#49146=CARTESIAN_POINT('Ctrl Pts',(31.2113800066628,8.54226303971064,-60.8472925910589));
#49147=CARTESIAN_POINT('Ctrl Pts',(31.2857763710018,8.80550296428891,-61.8258299092601));
#49148=CARTESIAN_POINT('Ctrl Pts',(31.3507242714438,9.08534203953185,-62.7766992498672));
#49149=CARTESIAN_POINT('Ctrl Pts',(31.3830181518182,9.25156079466651,-63.3011287796442));
#49150=CARTESIAN_POINT('Ctrl Pts',(31.4025052137197,9.36699878875882,-63.6460583027522));
#49151=CARTESIAN_POINT('Ctrl Pts',(31.4149352565952,9.44526104167027,-63.8747808577239));
#49152=CARTESIAN_POINT('Ctrl Pts',(31.4264914430533,9.52554998192621,-64.1015753771454));
#49153=CARTESIAN_POINT('Ctrl Pts',(31.4357981005218,9.59776145502393,-64.2983655263945));
#49154=CARTESIAN_POINT('Ctrl Pts',(31.440879219036,9.63960551034226,-64.4103355604511));
#49155=CARTESIAN_POINT('Ctrl Pts',(31.44826118774,9.70296125674408,-64.5778027379595));
#49156=CARTESIAN_POINT('Ctrl Pts',(31.4539039935886,9.75701258305106,-64.7163456025992));
#49157=CARTESIAN_POINT('Ctrl Pts',(31.4625469125157,9.84823769697998,-64.9442418696047));
#49158=CARTESIAN_POINT('Ctrl Pts',(31.4704018060749,9.94247260813082,-65.1716937489053));
#49159=CARTESIAN_POINT('Ctrl Pts',(31.482138511333,10.1459603455991,-65.6337942490935));
#49160=CARTESIAN_POINT('Ctrl Pts',(31.4935293569103,10.5331942370106,-66.4464679478753));
#49161=CARTESIAN_POINT('Ctrl Pts',(31.489739600742,11.4180616192753,-68.1055723847549));
#49162=CARTESIAN_POINT('Ctrl Pts',(31.4689354929894,12.2901135094031,-69.5979852881751));
#49163=CARTESIAN_POINT('Ctrl Pts',(31.4697806871723,12.9140139982325,-70.7834972100309));
#49164=CARTESIAN_POINT('Ctrl Pts',(31.469989039785,13.0434440655494,-71.0291593677387));
#49165=CARTESIAN_POINT('Ctrl Pts',(31.470277045121,13.3085758311122,-71.5311884003762));
#49166=CARTESIAN_POINT('Ctrl Pts',(31.4704734126682,13.6388199643196,-72.1544788905691));
#49167=CARTESIAN_POINT('Ctrl Pts',(31.4704957141681,14.0378297615307,-72.9051396997616));
#49168=CARTESIAN_POINT('Ctrl Pts',(31.4702487463697,14.8373791344158,-74.4059019368014));
#49169=CARTESIAN_POINT('Ctrl Pts',(31.4696762369953,15.5072839216342,-75.6591361257847));
#49170=CARTESIAN_POINT('Ctrl Pts',(31.4696585255378,16.4790900577772,-77.4867586602277));
#49171=CARTESIAN_POINT('Ctrl Pts',(31.4696575427394,16.9148362784751,-78.3062378482243));
#49172=CARTESIAN_POINT('Ctrl Pts',(31.4696575427393,17.3513578658645,-79.1272155503226));
#49173=CARTESIAN_POINT('Ctrl Pts',(33.7970285977012,4.09821853641055,24.8306494002684));
#49174=CARTESIAN_POINT('Ctrl Pts',(33.7971282050739,4.09822036764379,24.781770541049));
#49175=CARTESIAN_POINT('Ctrl Pts',(33.7972326733307,4.09822228839506,24.7328927512991));
#49176=CARTESIAN_POINT('Ctrl Pts',(33.7984662721378,4.09824493829563,24.1822897741847));
#49177=CARTESIAN_POINT('Ctrl Pts',(33.7994033543667,4.09826758173109,23.1781553718533));
#49178=CARTESIAN_POINT('Ctrl Pts',(33.8015798097595,4.09832432028853,21.1695681394724));
#49179=CARTESIAN_POINT('Ctrl Pts',(33.809789540473,4.09847426299123,19.6654230517925));
#49180=CARTESIAN_POINT('Ctrl Pts',(33.8272430182452,4.09876605720855,18.4143804676529));
#49181=CARTESIAN_POINT('Ctrl Pts',(33.8356105809491,4.09890898968022,17.911592099575));
#49182=CARTESIAN_POINT('Ctrl Pts',(33.8566174432594,4.09927273294534,16.9076192478544));
#49183=CARTESIAN_POINT('Ctrl Pts',(33.9016781945664,4.10005254213659,15.1537923232443));
#49184=CARTESIAN_POINT('Ctrl Pts',(33.9445372161864,4.10075015715253,13.6519415878471));
#49185=CARTESIAN_POINT('Ctrl Pts',(33.9714908584138,4.10111414654576,12.3973491179456));
#49186=CARTESIAN_POINT('Ctrl Pts',(33.9825187974683,4.10125490028183,11.8963456467522));
#49187=CARTESIAN_POINT('Ctrl Pts',(34.0050307592515,4.10151625570471,10.8944298036317));
#49188=CARTESIAN_POINT('Ctrl Pts',(34.0329083871325,4.10179725385752,9.64184755920691));
#49189=CARTESIAN_POINT('Ctrl Pts',(34.0623629492985,4.10205582204821,8.13735768627829));
#49190=CARTESIAN_POINT('Ctrl Pts',(34.0769482549485,4.10216300191832,7.13269822728231));
#49191=CARTESIAN_POINT('Ctrl Pts',(34.0837323382561,4.10220971726014,6.50475899129787));
#49192=CARTESIAN_POINT('Ctrl Pts',(34.0862739652426,4.10221810797943,6.25443092752143));
#49193=CARTESIAN_POINT('Ctrl Pts',(34.0907407487412,4.1021998457707,5.75321624620991));
#49194=CARTESIAN_POINT('Ctrl Pts',(34.0969930980285,4.1020905575295,4.8746861490407));
#49195=CARTESIAN_POINT('Ctrl Pts',(34.103685094322,4.10170822554426,3.11454451952558));
#49196=CARTESIAN_POINT('Ctrl Pts',(34.1009489428922,4.1015395669589,1.60853147061917));
#49197=CARTESIAN_POINT('Ctrl Pts',(34.0964395095961,4.10194657169397,0.549856156660557));
#49198=CARTESIAN_POINT('Ctrl Pts',(34.0958477606116,4.10200085509198,0.423813583599584));
#49199=CARTESIAN_POINT('Ctrl Pts',(34.0944545982225,4.1021276108948,0.171887827235955));
#49200=CARTESIAN_POINT('Ctrl Pts',(34.0914952451723,4.10239545883754,-0.268508702835578));
#49201=CARTESIAN_POINT('Ctrl Pts',(34.0859339137065,4.10288703977165,-0.896487986774876));
#49202=CARTESIAN_POINT('Ctrl Pts',(34.0776481013222,4.10360530012229,-1.64864637123662));
#49203=CARTESIAN_POINT('Ctrl Pts',(34.0651183943709,4.10464258775604,-2.65027867683541));
#49204=CARTESIAN_POINT('Ctrl Pts',(34.0479680651029,4.10595923985949,-3.90110177373963));
#49205=CARTESIAN_POINT('Ctrl Pts',(34.0353734908973,4.10670070469566,-4.90298322940253));
#49206=CARTESIAN_POINT('Ctrl Pts',(34.0287148154635,4.10697788756576,-5.53030604893786));
#49207=CARTESIAN_POINT('Ctrl Pts',(34.0259683562906,4.10713807836924,-5.78050396910268));
#49208=CARTESIAN_POINT('Ctrl Pts',(34.020212265199,4.1076119846857,-6.28196993185703));
#49209=CARTESIAN_POINT('Ctrl Pts',(34.0096219631666,4.10873822584859,-7.16041794032691));
#49210=CARTESIAN_POINT('Ctrl Pts',(33.9940490444314,4.11055545053572,-8.41785751623567));
#49211=CARTESIAN_POINT('Ctrl Pts',(33.9805692707932,4.11102346648838,-9.67551174623761));
#49212=CARTESIAN_POINT('Ctrl Pts',(33.9736569921043,4.10977984028363,-10.5546102028952));
#49213=CARTESIAN_POINT('Ctrl Pts',(33.9706278463524,4.10849838473789,-11.0563763144717));
#49214=CARTESIAN_POINT('Ctrl Pts',(33.9694562894734,4.10764406600035,-11.3070255162176));
#49215=CARTESIAN_POINT('Ctrl Pts',(33.9687138816181,4.10691458550222,-11.4957406859376));
#49216=CARTESIAN_POINT('Ctrl Pts',(33.9683305005745,4.10635066232301,-11.623881277403));
#49217=CARTESIAN_POINT('Ctrl Pts',(33.9679941469379,4.10492260948579,-11.8788305489746));
#49218=CARTESIAN_POINT('Ctrl Pts',(33.9684435458204,4.1017019555296,-12.324027240282));
#49219=CARTESIAN_POINT('Ctrl Pts',(33.9728128464778,4.09283721169593,-13.2090959126564));
#49220=CARTESIAN_POINT('Ctrl Pts',(33.9847244786488,4.07593321409288,-14.4608181274448));
#49221=CARTESIAN_POINT('Ctrl Pts',(33.9926489282834,4.06270791099737,-15.5773441815626));
#49222=CARTESIAN_POINT('Ctrl Pts',(33.9926559322855,4.05823257350317,-16.3199250450109));
#49223=CARTESIAN_POINT('Ctrl Pts',(33.9909580318512,4.05665527841438,-16.8146719247331));
#49224=CARTESIAN_POINT('Ctrl Pts',(33.9875228023187,4.05725463110933,-17.1855451243572));
#49225=CARTESIAN_POINT('Ctrl Pts',(33.9830696704345,4.05905098401968,-17.4941735460199));
#49226=CARTESIAN_POINT('Ctrl Pts',(33.9814056436223,4.05963041847793,-17.6215761453741));
#49227=CARTESIAN_POINT('Ctrl Pts',(33.9783372416422,4.0605977981083,-17.8728790271971));
#49228=CARTESIAN_POINT('Ctrl Pts',(33.9756133255376,4.06127516748637,-18.1247044351465));
#49229=CARTESIAN_POINT('Ctrl Pts',(33.973037750308,4.06185452718477,-18.375286557969));
#49230=CARTESIAN_POINT('Ctrl Pts',(33.9714660496556,4.0621965310781,-18.5317727670195));
#49231=CARTESIAN_POINT('Ctrl Pts',(33.9702063188726,4.06248084755737,-18.6567506225113));
#49232=CARTESIAN_POINT('Ctrl Pts',(33.9692570300578,4.06270263149698,-18.7504177013163));
#49233=CARTESIAN_POINT('Ctrl Pts',(33.968457893804,4.06289856079581,-18.8284017384575));
#49234=CARTESIAN_POINT('Ctrl Pts',(33.9678105003257,4.06306458795975,-18.8907509910024));
#49235=CARTESIAN_POINT('Ctrl Pts',(33.9622595988739,4.06452886023594,-19.4204906348209));
#49236=CARTESIAN_POINT('Ctrl Pts',(33.9501447783641,4.06940351449382,-20.4259725248278));
#49237=CARTESIAN_POINT('Ctrl Pts',(33.9049300086482,4.09926664542524,-21.8905015715613));
#49238=CARTESIAN_POINT('Ctrl Pts',(33.8412587973299,4.14138642964727,-22.8524069521049));
#49239=CARTESIAN_POINT('Ctrl Pts',(33.7871591392881,4.17532867843808,-23.4478026640479));
#49240=CARTESIAN_POINT('Ctrl Pts',(33.7635278638142,4.18995873126553,-23.6803950602424));
#49241=CARTESIAN_POINT('Ctrl Pts',(33.7090682763451,4.22238043752065,-24.1517312196106));
#49242=CARTESIAN_POINT('Ctrl Pts',(33.5973815953313,4.28598348845388,-24.985690223896));
#49243=CARTESIAN_POINT('Ctrl Pts',(33.4076798001897,4.38631421939129,-26.2072358071185));
#49244=CARTESIAN_POINT('Ctrl Pts',(33.1821937759443,4.50076189696166,-27.7182987079329));
#49245=CARTESIAN_POINT('Ctrl Pts',(33.0624190729428,4.56821605762625,-28.7530471474503));
#49246=CARTESIAN_POINT('Ctrl Pts',(33.0096393889443,4.60295930013888,-29.3408905338608));
#49247=CARTESIAN_POINT('Ctrl Pts',(32.9980607975317,4.61041835741825,-29.4669949640881));
#49248=CARTESIAN_POINT('Ctrl Pts',(32.9754196679533,4.6252360792123,-29.7216007220453));
#49249=CARTESIAN_POINT('Ctrl Pts',(32.9371999997291,4.65065906069946,-30.1655944655998));
#49250=CARTESIAN_POINT('Ctrl Pts',(32.8660890777854,4.70016473201003,-31.0531853689413));
#49251=CARTESIAN_POINT('Ctrl Pts',(32.7790451317061,4.76997238849969,-32.3164739882917));
#49252=CARTESIAN_POINT('Ctrl Pts',(32.7095781231124,4.84516280801569,-33.5733152642523));
#49253=CARTESIAN_POINT('Ctrl Pts',(32.6637818788412,4.9118723010392,-34.5737015394328));
#49254=CARTESIAN_POINT('Ctrl Pts',(32.6442194323323,4.94810389547688,-35.0721798075551));
#49255=CARTESIAN_POINT('Ctrl Pts',(32.6306781266863,4.97656239475885,-35.4463068277234));
#49256=CARTESIAN_POINT('Ctrl Pts',(32.6221171787377,4.99614191803143,-35.6988034335822));
#49257=CARTESIAN_POINT('Ctrl Pts',(32.6071741780158,5.03671215964242,-36.202030201179));
#49258=CARTESIAN_POINT('Ctrl Pts',(32.5861604767153,5.11152796365657,-37.0819022504336));
#49259=CARTESIAN_POINT('Ctrl Pts',(32.5609699932313,5.27390711956672,-38.8361707540274));
#49260=CARTESIAN_POINT('Ctrl Pts',(32.554981900109,5.42853889027826,-40.3382427694044));
#49261=CARTESIAN_POINT('Ctrl Pts',(32.5459371475621,5.55790806072204,-41.5936066720029));
#49262=CARTESIAN_POINT('Ctrl Pts',(32.5420138658918,5.59421486056015,-41.984174813383));
#49263=CARTESIAN_POINT('Ctrl Pts',(32.5373730788485,5.6380683728732,-42.4923196178453));
#49264=CARTESIAN_POINT('Ctrl Pts',(32.5327641984067,5.68031193203146,-42.9997665311057));
#49265=CARTESIAN_POINT('Ctrl Pts',(32.5276504291001,5.7315365234597,-43.627710232422));
#49266=CARTESIAN_POINT('Ctrl Pts',(32.5232803629278,5.79608129494499,-44.3725340641912));
#49267=CARTESIAN_POINT('Ctrl Pts',(32.5219296485828,5.85686717131584,-44.9847842771367));
#49268=CARTESIAN_POINT('Ctrl Pts',(32.5228946316512,5.91237385605236,-45.4693743176206));
#49269=CARTESIAN_POINT('Ctrl Pts',(32.5247246540156,5.95805395638314,-45.8300154304055));
#49270=CARTESIAN_POINT('Ctrl Pts',(32.5278247101902,6.00842253105358,-46.1877882470674));
#49271=CARTESIAN_POINT('Ctrl Pts',(32.5339569753228,6.08265565062642,-46.6607371758016));
#49272=CARTESIAN_POINT('Ctrl Pts',(32.5408734284837,6.14715785201562,-47.0107614030028));
#49273=CARTESIAN_POINT('Ctrl Pts',(32.5500619378399,6.21885511206134,-47.3576960899547));
#49274=CARTESIAN_POINT('Ctrl Pts',(32.5581144745922,6.26895137514107,-47.575578936988));
#49275=CARTESIAN_POINT('Ctrl Pts',(32.5744820127434,6.38404756662234,-48.0281094073996));
#49276=CARTESIAN_POINT('Ctrl Pts',(32.6060226061346,6.61689911901625,-48.8347242072648));
#49277=CARTESIAN_POINT('Ctrl Pts',(32.6558408667422,7.01549898084816,-50.044478682879));
#49278=CARTESIAN_POINT('Ctrl Pts',(32.7274054405778,7.51367808139426,-51.5865810358887));
#49279=CARTESIAN_POINT('Ctrl Pts',(32.7906493652785,7.79578840821404,-52.6881528625075));
#49280=CARTESIAN_POINT('Ctrl Pts',(32.8386819868785,7.93232635462115,-53.4058345890841));
#49281=CARTESIAN_POINT('Ctrl Pts',(32.8597479739066,7.9842516044768,-53.6958302088392));
#49282=CARTESIAN_POINT('Ctrl Pts',(32.9108190532738,8.07144100511394,-54.2663327052882));
#49283=CARTESIAN_POINT('Ctrl Pts',(33.019547085727,8.18761287487766,-55.2415234092912));
#49284=CARTESIAN_POINT('Ctrl Pts',(33.2931164552012,8.31125407880594,-57.0871404591677));
#49285=CARTESIAN_POINT('Ctrl Pts',(33.5358997999199,8.36694047219133,-58.4509986593335));
#49286=CARTESIAN_POINT('Ctrl Pts',(33.629766996932,8.5000635463776,-59.318605589913));
#49287=CARTESIAN_POINT('Ctrl Pts',(33.640526434217,8.51993120779359,-59.4460956936651));
#49288=CARTESIAN_POINT('Ctrl Pts',(33.6605628283255,8.55836196716042,-59.6880631583425));
#49289=CARTESIAN_POINT('Ctrl Pts',(33.6915063919367,8.6285990716164,-60.1163445282915));
#49290=CARTESIAN_POINT('Ctrl Pts',(33.7386558114479,8.77755295787295,-60.9619250812387));
#49291=CARTESIAN_POINT('Ctrl Pts',(33.7653691776996,8.97465054982133,-61.9147245541562));
#49292=CARTESIAN_POINT('Ctrl Pts',(33.7783381708424,9.2056620343217,-62.8462653352938));
#49293=CARTESIAN_POINT('Ctrl Pts',(33.7829177528305,9.34955005789062,-63.3624432207782));
#49294=CARTESIAN_POINT('Ctrl Pts',(33.7858406170772,9.4517420062381,-63.702857887243));
#49295=CARTESIAN_POINT('Ctrl Pts',(33.7878203178101,9.52157568263138,-63.9288452877205));
#49296=CARTESIAN_POINT('Ctrl Pts',(33.7899354442175,9.59399559459775,-64.153275087536));
#49297=CARTESIAN_POINT('Ctrl Pts',(33.7920791446143,9.65972535332635,-64.3483419885931));
#49298=CARTESIAN_POINT('Ctrl Pts',(33.7934095898122,9.69797055378872,-64.4594218829255));
#49299=CARTESIAN_POINT('Ctrl Pts',(33.7955226256635,9.75602384276808,-64.6256403883808));
#49300=CARTESIAN_POINT('Ctrl Pts',(33.7975472234733,9.80585938053793,-64.7633453371639));
#49301=CARTESIAN_POINT('Ctrl Pts',(33.8013790957159,9.89023306448245,-64.9899273901492));
#49302=CARTESIAN_POINT('Ctrl Pts',(33.8049049794753,9.97508253817971,-65.2076712376803));
#49303=CARTESIAN_POINT('Ctrl Pts',(33.810078935351,10.164584800907,-65.6573965312079));
#49304=CARTESIAN_POINT('Ctrl Pts',(33.814875131772,10.5341174610181,-66.4507763384098));
#49305=CARTESIAN_POINT('Ctrl Pts',(33.8119694278541,11.4112563331564,-68.0910591200175));
#49306=CARTESIAN_POINT('Ctrl Pts',(33.8009691673892,12.3048066618138,-69.5863841076439));
#49307=CARTESIAN_POINT('Ctrl Pts',(33.8003410766881,12.9352837166494,-70.7856886607226));
#49308=CARTESIAN_POINT('Ctrl Pts',(33.8003831704564,13.0639995479544,-71.0302511003522));
#49309=CARTESIAN_POINT('Ctrl Pts',(33.8003672239512,13.3290522508635,-71.5325143948912));
#49310=CARTESIAN_POINT('Ctrl Pts',(33.8003895503051,13.658830490243,-72.1551409816205));
#49311=CARTESIAN_POINT('Ctrl Pts',(33.8004007241132,14.0577532219815,-72.9056498879106));
#49312=CARTESIAN_POINT('Ctrl Pts',(33.8004378474102,14.857255052155,-74.4059521057206));
#49313=CARTESIAN_POINT('Ctrl Pts',(33.8004407127823,15.5275910160368,-75.6591109780893));
#49314=CARTESIAN_POINT('Ctrl Pts',(33.8003969455338,16.4996040288826,-77.4870418399451));
#49315=CARTESIAN_POINT('Ctrl Pts',(33.8004049519044,16.9352520962529,-78.3062943979546));
#49316=CARTESIAN_POINT('Ctrl Pts',(33.8004049519044,17.3717736836423,-79.1272721000527));
#49317=CARTESIAN_POINT('Ctrl Pts',(36.1186449350266,4.15213573292229,24.8306479566142));
#49318=CARTESIAN_POINT('Ctrl Pts',(36.118751955118,4.15213910516501,24.7817690707861));
#49319=CARTESIAN_POINT('Ctrl Pts',(36.1188641989714,4.1521426412137,24.7328912549376));
#49320=CARTESIAN_POINT('Ctrl Pts',(36.1201895134702,4.15218440716461,24.1822879344031));
#49321=CARTESIAN_POINT('Ctrl Pts',(36.1212095746272,4.15222197704974,23.1781532987238));
#49322=CARTESIAN_POINT('Ctrl Pts',(36.1235891875911,4.15231267361934,21.1695652709454));
#49323=CARTESIAN_POINT('Ctrl Pts',(36.1324076246725,4.15259078195511,19.6654195537376));
#49324=CARTESIAN_POINT('Ctrl Pts',(36.1510886615449,4.15315263302483,18.4143757893904));
#49325=CARTESIAN_POINT('Ctrl Pts',(36.1600511061703,4.15342376468628,17.9115794728721));
#49326=CARTESIAN_POINT('Ctrl Pts',(36.1825617524411,4.15410772118649,16.9076013119465));
#49327=CARTESIAN_POINT('Ctrl Pts',(36.2308457613202,4.15557255720582,15.1537769141764));
#49328=CARTESIAN_POINT('Ctrl Pts',(36.2766768526778,4.15693796052261,13.6519512351655));
#49329=CARTESIAN_POINT('Ctrl Pts',(36.3053368834683,4.15774125966134,12.3973909479109));
#49330=CARTESIAN_POINT('Ctrl Pts',(36.3170450031152,4.15806369848647,11.8963997715426));
#49331=CARTESIAN_POINT('Ctrl Pts',(36.34088818551,4.1587014714145,10.894499728827));
#49332=CARTESIAN_POINT('Ctrl Pts',(36.3703244215625,4.15946462904555,9.64192212646858));
#49333=CARTESIAN_POINT('Ctrl Pts',(36.4013422084235,4.16024013195097,8.13742396783722));
#49334=CARTESIAN_POINT('Ctrl Pts',(36.416660456582,4.16061455607174,7.13274788009381));
#49335=CARTESIAN_POINT('Ctrl Pts',(36.4237783626832,4.16078504527602,6.5048016068737));
#49336=CARTESIAN_POINT('Ctrl Pts',(36.4264294595897,4.16084483231786,6.25454567739911));
#49337=CARTESIAN_POINT('Ctrl Pts',(36.4310320312793,4.16093593632228,5.75340726173014));
#49338=CARTESIAN_POINT('Ctrl Pts',(36.4373308648874,4.16102908765525,4.87497226920453));
#49339=CARTESIAN_POINT('Ctrl Pts',(36.4436051613166,4.16100828955505,3.11477173871754));
#49340=CARTESIAN_POINT('Ctrl Pts',(36.4404304587637,4.16085273295468,1.60829703065008));
#49341=CARTESIAN_POINT('Ctrl Pts',(36.4363722249507,4.16087269744914,0.54908913247953));
#49342=CARTESIAN_POINT('Ctrl Pts',(36.435841044003,4.16087513362729,0.422954290450214));
#49343=CARTESIAN_POINT('Ctrl Pts',(36.434589295354,4.16088144845133,0.170871541684232));
#49344=CARTESIAN_POINT('Ctrl Pts',(36.4319292680497,4.16089522631591,-0.26978215410378));
#49345=CARTESIAN_POINT('Ctrl Pts',(36.4269131718644,4.16092325537722,-0.898055013797758));
#49346=CARTESIAN_POINT('Ctrl Pts',(36.4194217572928,4.1609582606988,-1.65043323512625));
#49347=CARTESIAN_POINT('Ctrl Pts',(36.4080166493647,4.16100822936559,-2.6522040911542));
#49348=CARTESIAN_POINT('Ctrl Pts',(36.392266008259,4.16104373891537,-3.90286135663219));
#49349=CARTESIAN_POINT('Ctrl Pts',(36.3803636434912,4.16103146254835,-4.90429019119771));
#49350=CARTESIAN_POINT('Ctrl Pts',(36.3739116299766,4.1609871795194,-5.53120786050771));
#49351=CARTESIAN_POINT('Ctrl Pts',(36.3713606906984,4.16102356994971,-5.78138723335569));
#49352=CARTESIAN_POINT('Ctrl Pts',(36.366345718637,4.16127637656656,-6.28274353426383));
#49353=CARTESIAN_POINT('Ctrl Pts',(36.3577443463334,4.16207694741307,-7.16105813208124));
#49354=CARTESIAN_POINT('Ctrl Pts',(36.3456034160075,4.16363296143633,-8.41833001284824));
#49355=CARTESIAN_POINT('Ctrl Pts',(36.3328233994175,4.16400016903126,-9.67581570986639));
#49356=CARTESIAN_POINT('Ctrl Pts',(36.3230878338691,4.1627189089989,-10.5547256151369));
#49357=CARTESIAN_POINT('Ctrl Pts',(36.3172349488834,4.16141560307,-11.0563995665472));
#49358=CARTESIAN_POINT('Ctrl Pts',(36.3141976241003,4.1605546972218,-11.3069518728839));
#49359=CARTESIAN_POINT('Ctrl Pts',(36.311867463079,4.15981617321664,-11.4957297272532));
#49360=CARTESIAN_POINT('Ctrl Pts',(36.3104545978921,4.15901797692348,-11.628471241393));
#49361=CARTESIAN_POINT('Ctrl Pts',(36.3081772327842,4.15649951043857,-11.8892616158524));
#49362=CARTESIAN_POINT('Ctrl Pts',(36.3054764271753,4.14986400164058,-12.344182579232));
#49363=CARTESIAN_POINT('Ctrl Pts',(36.3039001418369,4.12976492006611,-13.2403168618754));
#49364=CARTESIAN_POINT('Ctrl Pts',(36.3055860448045,4.09306418891023,-14.4874973759583));
#49365=CARTESIAN_POINT('Ctrl Pts',(36.2942146040001,4.07651301036016,-15.5739312984285));
#49366=CARTESIAN_POINT('Ctrl Pts',(36.2740467355084,4.08175161671561,-16.2857592940339));
#49367=CARTESIAN_POINT('Ctrl Pts',(36.2567923498229,4.09007842869138,-16.7572189427173));
#49368=CARTESIAN_POINT('Ctrl Pts',(36.2389427433258,4.10244261181981,-17.1074548236883));
#49369=CARTESIAN_POINT('Ctrl Pts',(36.2208664629216,4.11665826718186,-17.3974452542242));
#49370=CARTESIAN_POINT('Ctrl Pts',(36.2133730769138,4.12288760773508,-17.5193584165972));
#49371=CARTESIAN_POINT('Ctrl Pts',(36.1972619311317,4.13573594543672,-17.7590957322682));
#49372=CARTESIAN_POINT('Ctrl Pts',(36.1794845836868,4.14963289799397,-18.0004187229686));
#49373=CARTESIAN_POINT('Ctrl Pts',(36.1602453247373,4.16435807034453,-18.2410234719111));
#49374=CARTESIAN_POINT('Ctrl Pts',(36.1476322300781,4.17393530170251,-18.3916144026914));
#49375=CARTESIAN_POINT('Ctrl Pts',(36.1372149370081,4.1818007370874,-18.5120405738868));
#49376=CARTESIAN_POINT('Ctrl Pts',(36.1292414811277,4.1878046265628,-18.6023874548805));
#49377=CARTESIAN_POINT('Ctrl Pts',(36.1224677615594,4.1928926133522,-18.677676965247));
#49378=CARTESIAN_POINT('Ctrl Pts',(36.1169744232355,4.19701302310448,-18.7379164308516));
#49379=CARTESIAN_POINT('Ctrl Pts',(36.0698644414276,4.23232318293373,-19.2499674852621));
#49380=CARTESIAN_POINT('Ctrl Pts',(35.9665612554792,4.30865010297181,-20.2294585309346));
#49381=CARTESIAN_POINT('Ctrl Pts',(35.8007022817384,4.44338771065726,-21.6777249613799));
#49382=CARTESIAN_POINT('Ctrl Pts',(35.6985474547797,4.55366109792194,-22.6436070310028));
#49383=CARTESIAN_POINT('Ctrl Pts',(35.6409616397526,4.63295243003527,-23.2440179530984));
#49384=CARTESIAN_POINT('Ctrl Pts',(35.6184001316968,4.66404898478509,-23.4651075012263));
#49385=CARTESIAN_POINT('Ctrl Pts',(35.5714930887105,4.73609875981253,-23.9253851652744));
#49386=CARTESIAN_POINT('Ctrl Pts',(35.4866210875483,4.88180845890605,-24.7451776075493));
#49387=CARTESIAN_POINT('Ctrl Pts',(35.3607305332135,5.13770232629307,-25.9708121318986));
#49388=CARTESIAN_POINT('Ctrl Pts',(35.2142276066228,5.47503752153702,-27.51013784333));
#49389=CARTESIAN_POINT('Ctrl Pts',(35.1287204298902,5.68300225352559,-28.579818117116));
#49390=CARTESIAN_POINT('Ctrl Pts',(35.0878448026781,5.78365285372853,-29.1926592172269));
#49391=CARTESIAN_POINT('Ctrl Pts',(35.0795921412154,5.804619458885,-29.3207592382003));
#49392=CARTESIAN_POINT('Ctrl Pts',(35.0630934440586,5.84649147906714,-29.5812104390111));
#49393=CARTESIAN_POINT('Ctrl Pts',(35.0354683041597,5.91754668256178,-30.0340522643875));
#49394=CARTESIAN_POINT('Ctrl Pts',(34.9841364638804,6.053064873335,-30.9387119821918));
#49395=CARTESIAN_POINT('Ctrl Pts',(34.9215988790561,6.23029214907037,-32.2219964317856));
#49396=CARTESIAN_POINT('Ctrl Pts',(34.8720796920368,6.39500510705853,-33.4942535933966));
#49397=CARTESIAN_POINT('Ctrl Pts',(34.8401758497231,6.52454157318325,-34.5043398338357));
#49398=CARTESIAN_POINT('Ctrl Pts',(34.8267142376718,6.589363786187,-35.0066684959514));
#49399=CARTESIAN_POINT('Ctrl Pts',(34.8175695011411,6.63850023499951,-35.3834627780651));
#49400=CARTESIAN_POINT('Ctrl Pts',(34.8116941048461,6.67171062801112,-35.6396028924226));
#49401=CARTESIAN_POINT('Ctrl Pts',(34.802022989597,6.73752943798291,-36.1488028995589));
#49402=CARTESIAN_POINT('Ctrl Pts',(34.7896756969634,6.85162363355519,-37.0388907733161));
#49403=CARTESIAN_POINT('Ctrl Pts',(34.780419785692,7.07415792333669,-38.8113317003373));
#49404=CARTESIAN_POINT('Ctrl Pts',(34.7885680474133,7.25240420099761,-40.3262000688208));
#49405=CARTESIAN_POINT('Ctrl Pts',(34.7922929384013,7.39024155720927,-41.591498175899));
#49406=CARTESIAN_POINT('Ctrl Pts',(34.7924068356153,7.42924402972164,-41.9789634900419));
#49407=CARTESIAN_POINT('Ctrl Pts',(34.7924493108881,7.47677005399358,-42.4886835116074));
#49408=CARTESIAN_POINT('Ctrl Pts',(34.7924820473252,7.52221413824149,-42.9983713480713));
#49409=CARTESIAN_POINT('Ctrl Pts',(34.7930507774722,7.57594601810967,-43.6322878904797));
#49410=CARTESIAN_POINT('Ctrl Pts',(34.7960381341315,7.63892333195803,-44.3884882496669));
#49411=CARTESIAN_POINT('Ctrl Pts',(34.8017725228489,7.69286318487468,-45.0139962663783));
#49412=CARTESIAN_POINT('Ctrl Pts',(34.8089999595259,7.73851263582959,-45.511382337068));
#49413=CARTESIAN_POINT('Ctrl Pts',(34.8160222362676,7.77439227005541,-45.882785120485));
#49414=CARTESIAN_POINT('Ctrl Pts',(34.824860917934,7.81230831042121,-46.2524957987966));
#49415=CARTESIAN_POINT('Ctrl Pts',(34.8393386173542,7.86608982182046,-46.742960460993));
#49416=CARTESIAN_POINT('Ctrl Pts',(34.8537455518391,7.91061328612196,-47.1080553302964));
#49417=CARTESIAN_POINT('Ctrl Pts',(34.8709410861411,7.95875254430267,-47.4714358673103));
#49418=CARTESIAN_POINT('Ctrl Pts',(34.8839834705516,7.99243680465684,-47.7022779156774));
#49419=CARTESIAN_POINT('Ctrl Pts',(34.9133572479211,8.06898230823606,-48.1772108814288));
#49420=CARTESIAN_POINT('Ctrl Pts',(34.9738217220953,8.22144382015883,-49.0185420321587));
#49421=CARTESIAN_POINT('Ctrl Pts',(35.0820820293093,8.47148089508071,-50.2647952395676));
#49422=CARTESIAN_POINT('Ctrl Pts',(35.2351526769321,8.75014012826034,-51.8333470205335));
#49423=CARTESIAN_POINT('Ctrl Pts',(35.3427326291523,8.86951422265271,-52.9349741093424));
#49424=CARTESIAN_POINT('Ctrl Pts',(35.4078923821326,8.90587288905447,-53.6436700502769));
#49425=CARTESIAN_POINT('Ctrl Pts',(35.4353624911882,8.91551702527776,-53.9526639891302));
#49426=CARTESIAN_POINT('Ctrl Pts',(35.4947913587344,8.91260207054687,-54.5419025239566));
#49427=CARTESIAN_POINT('Ctrl Pts',(35.6072519093414,8.86279590946284,-55.5418424448288));
#49428=CARTESIAN_POINT('Ctrl Pts',(35.8424450750142,8.65493143604865,-57.3800614358869));
#49429=CARTESIAN_POINT('Ctrl Pts',(36.0149308588584,8.5351779208891,-58.6759953288372));
#49430=CARTESIAN_POINT('Ctrl Pts',(36.0809952548126,8.60043152813387,-59.451695379221));
#49431=CARTESIAN_POINT('Ctrl Pts',(36.0885407153967,8.61075055262764,-59.5692306619767));
#49432=CARTESIAN_POINT('Ctrl Pts',(36.1020277936,8.63293407448938,-59.791773774123));
#49433=CARTESIAN_POINT('Ctrl Pts',(36.1215461055886,8.67887213429191,-60.189018935145));
#49434=CARTESIAN_POINT('Ctrl Pts',(36.1459574663463,8.79631439142916,-60.9828849793252));
#49435=CARTESIAN_POINT('Ctrl Pts',(36.1481729065539,8.98695572450133,-61.9000917036662));
#49436=CARTESIAN_POINT('Ctrl Pts',(36.1396454278851,9.22658847892513,-62.8181111290303));
#49437=CARTESIAN_POINT('Ctrl Pts',(36.1335264055312,9.37842901981253,-63.3346872065385));
#49438=CARTESIAN_POINT('Ctrl Pts',(36.1300114391582,9.48621884888992,-63.6785588611986));
#49439=CARTESIAN_POINT('Ctrl Pts',(36.127885752017,9.55979649333591,-63.9076897706352));
#49440=CARTESIAN_POINT('Ctrl Pts',(36.1262122462846,9.63586865333346,-64.1364782842017));
#49441=CARTESIAN_POINT('Ctrl Pts',(36.1253141932307,9.70455338622023,-64.3364143671117));
#49442=CARTESIAN_POINT('Ctrl Pts',(36.124991351822,9.74439272579184,-64.4505712574178));
#49443=CARTESIAN_POINT('Ctrl Pts',(36.1247099153703,9.80472639043459,-64.6216853401157));
#49444=CARTESIAN_POINT('Ctrl Pts',(36.124932073824,9.85621713484614,-64.7640878246856));
#49445=CARTESIAN_POINT('Ctrl Pts',(36.1260402834046,9.94277504210635,-64.9989547811454));
#49446=CARTESIAN_POINT('Ctrl Pts',(36.1273229909198,10.0254902169591,-65.2126141431759));
#49447=CARTESIAN_POINT('Ctrl Pts',(36.1291758847748,10.2137505174887,-65.6617087684228));
#49448=CARTESIAN_POINT('Ctrl Pts',(36.1311833869412,10.5810170945027,-66.4511101943034));
#49449=CARTESIAN_POINT('Ctrl Pts',(36.130738160053,11.4591355370609,-68.0894113511506));
#49450=CARTESIAN_POINT('Ctrl Pts',(36.126345375064,12.3572615261994,-69.5843476939743));
#49451=CARTESIAN_POINT('Ctrl Pts',(36.1249006423819,12.9894425233202,-70.7860628595763));
#49452=CARTESIAN_POINT('Ctrl Pts',(36.1249374217901,13.118205570479,-71.0305629313097));
#49453=CARTESIAN_POINT('Ctrl Pts',(36.1248379255275,13.3834907027566,-71.5330384800975));
#49454=CARTESIAN_POINT('Ctrl Pts',(36.1248501107365,13.7133832691705,-72.1557180082116));
#49455=CARTESIAN_POINT('Ctrl Pts',(36.1248713979155,14.1123888014151,-72.9063590020337));
#49456=CARTESIAN_POINT('Ctrl Pts',(36.1250136146553,14.911861549032,-74.4067848331667));
#49457=CARTESIAN_POINT('Ctrl Pts',(36.1252094628775,15.5818687416089,-75.6597056091058));
#49458=CARTESIAN_POINT('Ctrl Pts',(36.1251645924201,16.5536865502446,-77.4872413901607));
#49459=CARTESIAN_POINT('Ctrl Pts',(36.1251960907172,16.9893579083434,-78.306521149624));
#49460=CARTESIAN_POINT('Ctrl Pts',(36.1251960907173,17.4258794957329,-79.1274988517223));
#49461=CARTESIAN_POINT('Ctrl Pts',(37.9743793938247,4.21863409729416,24.8306267144035));
#49462=CARTESIAN_POINT('Ctrl Pts',(37.974492258943,4.21863841245639,24.78174714051));
#49463=CARTESIAN_POINT('Ctrl Pts',(37.9746106306985,4.21864293872577,24.7328686303977));
#49464=CARTESIAN_POINT('Ctrl Pts',(37.9760083865885,4.21869637434015,24.1822570212595));
#49465=CARTESIAN_POINT('Ctrl Pts',(37.9770915843225,4.21873200165046,23.178111074583));
#49466=CARTESIAN_POINT('Ctrl Pts',(37.9796217625982,4.21881175633108,21.1695081088091));
#49467=CARTESIAN_POINT('Ctrl Pts',(37.9889227535691,4.21916723227851,19.6653538966312));
#49468=CARTESIAN_POINT('Ctrl Pts',(38.0085894948983,4.21994781539465,18.4143063459505));
#49469=CARTESIAN_POINT('Ctrl Pts',(38.0180268333167,4.22031950377046,17.9114656680587));
#49470=CARTESIAN_POINT('Ctrl Pts',(38.0417338295989,4.22124783985785,16.9074551401735));
#49471=CARTESIAN_POINT('Ctrl Pts',(38.0925813872245,4.22323994665397,15.1536342494888));
#49472=CARTESIAN_POINT('Ctrl Pts',(38.1408117825693,4.22516867420997,13.6519382550817));
#49473=CARTESIAN_POINT('Ctrl Pts',(38.1709079604311,4.22644869451557,12.3975578235691));
#49474=CARTESIAN_POINT('Ctrl Pts',(38.1831964689025,4.22698016482334,11.8966405663243));
#49475=CARTESIAN_POINT('Ctrl Pts',(38.2082001178775,4.2280900923784,10.89484911608));
#49476=CARTESIAN_POINT('Ctrl Pts',(38.2390387632422,4.22949823370161,9.64233663567765));
#49477=CARTESIAN_POINT('Ctrl Pts',(38.2714937740577,4.23102035728818,8.13782020555378));
#49478=CARTESIAN_POINT('Ctrl Pts',(38.2875020804209,4.23178261123858,7.13305418257719));
#49479=CARTESIAN_POINT('Ctrl Pts',(38.2949304559688,4.23213921574379,6.50504097441828));
#49480=CARTESIAN_POINT('Ctrl Pts',(38.2976902518413,4.23227629394518,6.25486333187328));
#49481=CARTESIAN_POINT('Ctrl Pts',(38.3024566847348,4.23252931044664,5.75379505782952));
#49482=CARTESIAN_POINT('Ctrl Pts',(38.3089192082696,4.23291193377536,4.87544297152401));
#49483=CARTESIAN_POINT('Ctrl Pts',(38.3151336323395,4.23342810905955,3.11513770009187));
#49484=CARTESIAN_POINT('Ctrl Pts',(38.3116765402784,4.23335441307545,1.60808221958763));
#49485=CARTESIAN_POINT('Ctrl Pts',(38.3076705606032,4.23301392086635,0.548265115589204));
#49486=CARTESIAN_POINT('Ctrl Pts',(38.3071452992699,4.23296996296405,0.422036119001589));
#49487=CARTESIAN_POINT('Ctrl Pts',(38.3059091966356,4.23286482875268,0.169788232924755));
#49488=CARTESIAN_POINT('Ctrl Pts',(38.3032833893307,4.23263987593515,-0.271134839049098));
#49489=CARTESIAN_POINT('Ctrl Pts',(38.2983399003467,4.23220915338293,-0.899734170126479));
#49490=CARTESIAN_POINT('Ctrl Pts',(38.2909381042811,4.23157615514907,-1.65235304049793));
#49491=CARTESIAN_POINT('Ctrl Pts',(38.279665745071,4.23061740452919,-2.65432268665193));
#49492=CARTESIAN_POINT('Ctrl Pts',(38.2640282182585,4.22933803030512,-3.90490507972187));
#49493=CARTESIAN_POINT('Ctrl Pts',(38.2521329820479,4.22844215333868,-4.90599788327314));
#49494=CARTESIAN_POINT('Ctrl Pts',(38.2456115546156,4.22801160713605,-5.53266954474732));
#49495=CARTESIAN_POINT('Ctrl Pts',(38.2432139048281,4.22773560300612,-5.78506890425695));
#49496=CARTESIAN_POINT('Ctrl Pts',(38.2391023217651,4.22684064921901,-6.28876410275137));
#49497=CARTESIAN_POINT('Ctrl Pts',(38.2332760101616,4.22458816124566,-7.17007490241801));
#49498=CARTESIAN_POINT('Ctrl Pts',(38.226456056922,4.22056665615865,-8.42601796915756));
#49499=CARTESIAN_POINT('Ctrl Pts',(38.2151634607775,4.21878579347824,-9.67536092665477));
#49500=CARTESIAN_POINT('Ctrl Pts',(38.201510169486,4.22046816872256,-10.5446395981229));
#49501=CARTESIAN_POINT('Ctrl Pts',(38.1915776224637,4.22250384649015,-11.0397541416357));
#49502=CARTESIAN_POINT('Ctrl Pts',(38.1858209942656,4.22391321247,-11.2866020505556));
#49503=CARTESIAN_POINT('Ctrl Pts',(38.1811561945481,4.22513990252829,-11.4725955114208));
#49504=CARTESIAN_POINT('Ctrl Pts',(38.1781231817478,4.2256673507536,-11.6084095583563));
#49505=CARTESIAN_POINT('Ctrl Pts',(38.172416962679,4.22535403168541,-11.8719247327729));
#49506=CARTESIAN_POINT('Ctrl Pts',(38.1632101925206,4.22178743142648,-12.3315588082072));
#49507=CARTESIAN_POINT('Ctrl Pts',(38.1466521359241,4.20573495068469,-13.2300179665428));
#49508=CARTESIAN_POINT('Ctrl Pts',(38.1208998504696,4.17589084567263,-14.4631736218846));
#49509=CARTESIAN_POINT('Ctrl Pts',(38.0783845247824,4.17896862737656,-15.5157856111138));
#49510=CARTESIAN_POINT('Ctrl Pts',(38.0351280575023,4.20667903991865,-16.1974410314374));
#49511=CARTESIAN_POINT('Ctrl Pts',(38.0018870091212,4.23260587197108,-16.6468058390751));
#49512=CARTESIAN_POINT('Ctrl Pts',(37.9715402958889,4.26115653272591,-16.9784979407005));
#49513=CARTESIAN_POINT('Ctrl Pts',(37.9428822522154,4.29068437333013,-17.2519506004831));
#49514=CARTESIAN_POINT('Ctrl Pts',(37.9309121166235,4.30320748052913,-17.3618749444117));
#49515=CARTESIAN_POINT('Ctrl Pts',(37.9047576019355,4.33028450196241,-17.5826112593404));
#49516=CARTESIAN_POINT('Ctrl Pts',(37.8755045401449,4.3604750146577,-17.8060117972872));
#49517=CARTESIAN_POINT('Ctrl Pts',(37.843661785628,4.39334406374891,-18.031718943508));
#49518=CARTESIAN_POINT('Ctrl Pts',(37.8227909946016,4.41493560327634,-18.1738267243772));
#49519=CARTESIAN_POINT('Ctrl Pts',(37.8055778985813,4.43279175427115,-18.2881138433063));
#49520=CARTESIAN_POINT('Ctrl Pts',(37.7924268084728,4.44646428185898,-18.3741363191589));
#49521=CARTESIAN_POINT('Ctrl Pts',(37.7812809907889,4.45808321172109,-18.4460723317931));
#49522=CARTESIAN_POINT('Ctrl Pts',(37.7722595951433,4.46750766486995,-18.5037759979881));
#49523=CARTESIAN_POINT('Ctrl Pts',(37.695022708878,4.54835904189559,-18.9950878850114));
#49524=CARTESIAN_POINT('Ctrl Pts',(37.5305819780222,4.72434670681134,-19.9610964749048));
#49525=CARTESIAN_POINT('Ctrl Pts',(37.3051029479327,5.01823596921909,-21.4586235781379));
#49526=CARTESIAN_POINT('Ctrl Pts',(37.1955939026535,5.23122815130101,-22.4917581243808));
#49527=CARTESIAN_POINT('Ctrl Pts',(37.1455073222649,5.36711897314608,-23.1435640254773));
#49528=CARTESIAN_POINT('Ctrl Pts',(37.1296059114069,5.41770838498506,-23.3745708513876));
#49529=CARTESIAN_POINT('Ctrl Pts',(37.0991677184359,5.53041814804529,-23.8572987491716));
#49530=CARTESIAN_POINT('Ctrl Pts',(37.0535693526703,5.74525965546662,-24.7061348664269));
#49531=CARTESIAN_POINT('Ctrl Pts',(37.0012890967258,6.09156617222418,-25.9554051399712));
#49532=CARTESIAN_POINT('Ctrl Pts',(36.9473976697968,6.51348748988546,-27.499250671943));
#49533=CARTESIAN_POINT('Ctrl Pts',(36.9133313107658,6.76467422120613,-28.5625661281727));
#49534=CARTESIAN_POINT('Ctrl Pts',(36.8939524645289,6.88631594558857,-29.1702997742256));
#49535=CARTESIAN_POINT('Ctrl Pts',(36.8901953539948,6.91224581145836,-29.3008098254207));
#49536=CARTESIAN_POINT('Ctrl Pts',(36.8827996560842,6.96324100593501,-29.5639684519698));
#49537=CARTESIAN_POINT('Ctrl Pts',(36.8709931285117,7.04906085338863,-30.0222918894149));
#49538=CARTESIAN_POINT('Ctrl Pts',(36.851060722126,7.20889062551895,-30.9359618354406));
#49539=CARTESIAN_POINT('Ctrl Pts',(36.8328740793196,7.40877289976207,-32.2289515952689));
#49540=CARTESIAN_POINT('Ctrl Pts',(36.8263100628016,7.5850490148669,-33.5044476393165));
#49541=CARTESIAN_POINT('Ctrl Pts',(36.8265592325707,7.71975151448663,-34.5125815020699));
#49542=CARTESIAN_POINT('Ctrl Pts',(36.8284007726567,7.78649502690822,-35.0123003094323));
#49543=CARTESIAN_POINT('Ctrl Pts',(36.8302422030198,7.83687505870679,-35.3865350342881));
#49544=CARTESIAN_POINT('Ctrl Pts',(36.8315120391773,7.87101044252364,-35.6440496199976));
#49545=CARTESIAN_POINT('Ctrl Pts',(36.8358568082861,7.93751800985704,-36.1542445699149));
#49546=CARTESIAN_POINT('Ctrl Pts',(36.847237669633,8.05062893861643,-37.0470229512314));
#49547=CARTESIAN_POINT('Ctrl Pts',(36.8824480260088,8.26236414082339,-38.8243606250119));
#49548=CARTESIAN_POINT('Ctrl Pts',(36.9234642151751,8.41889131363091,-40.3443424816412));
#49549=CARTESIAN_POINT('Ctrl Pts',(36.9517860700139,8.53484591648929,-41.614030993031));
#49550=CARTESIAN_POINT('Ctrl Pts',(36.9592376200307,8.56764734381142,-41.9992090889243));
#49551=CARTESIAN_POINT('Ctrl Pts',(36.9683476045283,8.60760114210068,-42.50904350848));
#49552=CARTESIAN_POINT('Ctrl Pts',(36.9770403748266,8.6454975835139,-43.0191781457652));
#49553=CARTESIAN_POINT('Ctrl Pts',(36.9876403346379,8.68944332364214,-43.655405806571));
#49554=CARTESIAN_POINT('Ctrl Pts',(37.0013381840815,8.73840883574967,-44.4167461203277));
#49555=CARTESIAN_POINT('Ctrl Pts',(37.0147952319846,8.77741565667612,-45.0486963300423));
#49556=CARTESIAN_POINT('Ctrl Pts',(37.027632614232,8.80842154980143,-45.5525006513341));
#49557=CARTESIAN_POINT('Ctrl Pts',(37.038440488472,8.83172909652937,-45.929386688973));
#49558=CARTESIAN_POINT('Ctrl Pts',(37.0506250140234,8.85528687507259,-46.3052579784331));
#49559=CARTESIAN_POINT('Ctrl Pts',(37.0690074575453,8.88730474900626,-46.8048669254791));
#49560=CARTESIAN_POINT('Ctrl Pts',(37.0853542896548,8.91217988455291,-47.1779259422816));
#49561=CARTESIAN_POINT('Ctrl Pts',(37.1040005222447,8.93812390306473,-47.5500917536217));
#49562=CARTESIAN_POINT('Ctrl Pts',(37.1174893861852,8.95620812618262,-47.7877040574019));
#49563=CARTESIAN_POINT('Ctrl Pts',(37.1471749698849,8.99716486633686,-48.2747490401855));
#49564=CARTESIAN_POINT('Ctrl Pts',(37.2056971608678,9.07764006184513,-49.135329879993));
#49565=CARTESIAN_POINT('Ctrl Pts',(37.3028492188309,9.20328040460516,-50.4016484218929));
#49566=CARTESIAN_POINT('Ctrl Pts',(37.426850198214,9.32122267562777,-51.9762540942031));
#49567=CARTESIAN_POINT('Ctrl Pts',(37.5047710024866,9.34257078545175,-53.0651446979514));
#49568=CARTESIAN_POINT('Ctrl Pts',(37.5493822799248,9.32608751006771,-53.7605712583107));
#49569=CARTESIAN_POINT('Ctrl Pts',(37.5681824068605,9.3119219865871,-54.0737087055534));
#49570=CARTESIAN_POINT('Ctrl Pts',(37.6069862512297,9.26334418068316,-54.6630166434402));
#49571=CARTESIAN_POINT('Ctrl Pts',(37.6770765329605,9.13669869620959,-55.6608709574235));
#49572=CARTESIAN_POINT('Ctrl Pts',(37.8159387231878,8.79827935854848,-57.4834792507308));
#49573=CARTESIAN_POINT('Ctrl Pts',(37.913486645184,8.62006744396071,-58.7608746719867));
#49574=CARTESIAN_POINT('Ctrl Pts',(37.9535058005589,8.6630413573171,-59.5032113087664));
#49575=CARTESIAN_POINT('Ctrl Pts',(37.9580719704498,8.67021106909296,-59.6160263902128));
#49576=CARTESIAN_POINT('Ctrl Pts',(37.9662511317454,8.6870295365958,-59.8299975680421));
#49577=CARTESIAN_POINT('Ctrl Pts',(37.9781030159931,8.72491997924004,-60.2131778620392));
#49578=CARTESIAN_POINT('Ctrl Pts',(37.9929764021785,8.83200747034294,-60.9839274746279));
#49579=CARTESIAN_POINT('Ctrl Pts',(37.9943767493591,9.0221597655985,-61.8859344504134));
#49580=CARTESIAN_POINT('Ctrl Pts',(37.9893344013422,9.26865925501439,-62.7991904173723));
#49581=CARTESIAN_POINT('Ctrl Pts',(37.9857174720035,9.42598099805474,-63.3166639671887));
#49582=CARTESIAN_POINT('Ctrl Pts',(37.9836469546191,9.53759795275649,-63.6625454370981));
#49583=CARTESIAN_POINT('Ctrl Pts',(37.9824006145624,9.61372962915768,-63.8933931853993));
#49584=CARTESIAN_POINT('Ctrl Pts',(37.9814213750252,9.69231282634275,-64.1244361994236));
#49585=CARTESIAN_POINT('Ctrl Pts',(37.9809106222791,9.76304704436886,-64.326833963689));
#49586=CARTESIAN_POINT('Ctrl Pts',(37.9807337431088,9.80400196055581,-64.442535573146));
#49587=CARTESIAN_POINT('Ctrl Pts',(37.9805919097837,9.86594338959743,-64.6161004856718));
#49588=CARTESIAN_POINT('Ctrl Pts',(37.9807463369306,9.91863581785843,-64.7608413565679));
#49589=CARTESIAN_POINT('Ctrl Pts',(37.9814622524679,10.006859705651,-64.9998595182745));
#49590=CARTESIAN_POINT('Ctrl Pts',(37.9826301558853,10.0892520642219,-65.2123223473177));
#49591=CARTESIAN_POINT('Ctrl Pts',(37.984346930264,10.2780325969123,-65.6621174689531));
#49592=CARTESIAN_POINT('Ctrl Pts',(37.986642528923,10.6456486560468,-66.4511350626474));
#49593=CARTESIAN_POINT('Ctrl Pts',(37.9879108841636,11.524912009961,-68.0899328486106));
#49594=CARTESIAN_POINT('Ctrl Pts',(37.985066779144,12.4235874158634,-69.5844828536149));
#49595=CARTESIAN_POINT('Ctrl Pts',(37.9833104983342,13.056073118225,-70.7862662061612));
#49596=CARTESIAN_POINT('Ctrl Pts',(37.9834152527383,13.1849143669782,-71.0308187122585));
#49597=CARTESIAN_POINT('Ctrl Pts',(37.9833545435611,13.4503155154178,-71.5333720275582));
#49598=CARTESIAN_POINT('Ctrl Pts',(37.983414746917,13.7803064517032,-72.1561248389429));
#49599=CARTESIAN_POINT('Ctrl Pts',(37.9834440827621,14.1793606209594,-72.9068371922368));
#49600=CARTESIAN_POINT('Ctrl Pts',(37.983560394376,14.9788300444199,-74.4073549057964));
#49601=CARTESIAN_POINT('Ctrl Pts',(37.9836464209878,15.6486817082044,-75.6601782849562));
#49602=CARTESIAN_POINT('Ctrl Pts',(37.9835707570307,16.6204131422508,-77.487514078272));
#49603=CARTESIAN_POINT('Ctrl Pts',(37.9836041227838,17.0561121018744,-78.3068237760512));
#49604=CARTESIAN_POINT('Ctrl Pts',(37.9836041227839,17.4926336892639,-79.1278014781496));
#49605=CARTESIAN_POINT('Ctrl Pts',(39.8297890978139,4.30089180200322,24.8306033519864));
#49606=CARTESIAN_POINT('Ctrl Pts',(39.8299074020901,4.30089711404966,24.7817230525328));
#49607=CARTESIAN_POINT('Ctrl Pts',(39.830031479274,4.3009026866052,24.7328438116444));
#49608=CARTESIAN_POINT('Ctrl Pts',(39.8314965764819,4.30096848600841,24.1822234222506));
#49609=CARTESIAN_POINT('Ctrl Pts',(39.8326291542074,4.30100164232867,23.1780643674514));
#49610=CARTESIAN_POINT('Ctrl Pts',(39.8352733292624,4.30106760982009,21.1694460455231));
#49611=CARTESIAN_POINT('Ctrl Pts',(39.8450224013784,4.3015063259998,19.6652841373055));
#49612=CARTESIAN_POINT('Ctrl Pts',(39.8656503854775,4.30252264560954,18.4142343890651));
#49613=CARTESIAN_POINT('Ctrl Pts',(39.8755468785802,4.30300312909193,17.911351654955));
#49614=CARTESIAN_POINT('Ctrl Pts',(39.9004034153351,4.30419822099428,16.9073098440472));
#49615=CARTESIAN_POINT('Ctrl Pts',(39.953716293508,4.30676554786842,15.153489091752));
#49616=CARTESIAN_POINT('Ctrl Pts',(40.0043125451533,4.30931090977232,13.6519156262175));
#49617=CARTESIAN_POINT('Ctrl Pts',(40.0359355901385,4.31109503698416,12.3977077797573));
#49618=CARTESIAN_POINT('Ctrl Pts',(40.0488540424933,4.31184611138178,11.896861536915));
#49619=CARTESIAN_POINT('Ctrl Pts',(40.0751597988642,4.31344670334409,10.8951765808069));
#49620=CARTESIAN_POINT('Ctrl Pts',(40.1076330240833,4.31553018183121,9.64272890374985));
#49621=CARTESIAN_POINT('Ctrl Pts',(40.1418302072307,4.31782592199948,8.13819823380099));
#49622=CARTESIAN_POINT('Ctrl Pts',(40.158699490557,4.31899908471942,7.13334121701694));
#49623=CARTESIAN_POINT('Ctrl Pts',(40.1665241376599,4.31954936256452,6.5052603902337));
#49624=CARTESIAN_POINT('Ctrl Pts',(40.1694302788948,4.31976414814769,6.2551379681381));
#49625=CARTESIAN_POINT('Ctrl Pts',(40.174446373827,4.3201742172438,5.7541147994796));
#49626=CARTESIAN_POINT('Ctrl Pts',(40.1812395059384,4.32083073673609,4.87581090564104));
#49627=CARTESIAN_POINT('Ctrl Pts',(40.1877539016281,4.32182649441906,3.11541238522877));
#49628=CARTESIAN_POINT('Ctrl Pts',(40.1841301313211,4.32187206126619,1.60788760759156));
#49629=CARTESIAN_POINT('Ctrl Pts',(40.180007725456,4.3212798572179,0.547615075927073));
#49630=CARTESIAN_POINT('Ctrl Pts',(40.1794671788892,4.32120140318382,0.421323426395065));
#49631=CARTESIAN_POINT('Ctrl Pts',(40.1781932213731,4.32101446375644,0.168961732958732));
#49632=CARTESIAN_POINT('Ctrl Pts',(40.1754837625236,4.32061298834142,-0.272146661512237));
#49633=CARTESIAN_POINT('Ctrl Pts',(40.1703722396646,4.31985173574526,-0.900986822677657));
#49634=CARTESIAN_POINT('Ctrl Pts',(40.1627145970043,4.31872192159838,-1.65378076716345));
#49635=CARTESIAN_POINT('Ctrl Pts',(40.1510375361638,4.31703143200427,-2.65592708254926));
#49636=CARTESIAN_POINT('Ctrl Pts',(40.1348310495129,4.3147720923205,-3.90653507224137));
#49637=CARTESIAN_POINT('Ctrl Pts',(40.1224731624672,4.31322379578241,-4.90747430946853));
#49638=CARTESIAN_POINT('Ctrl Pts',(40.1156951883021,4.31246287247062,-5.53414030084685));
#49639=CARTESIAN_POINT('Ctrl Pts',(40.1134265827715,4.31174306157199,-5.79061969698076));
#49640=CARTESIAN_POINT('Ctrl Pts',(40.1103207508345,4.30897225982735,-6.29871002733814));
#49641=CARTESIAN_POINT('Ctrl Pts',(40.107764830051,4.30145627816816,-7.18564143430966));
#49642=CARTESIAN_POINT('Ctrl Pts',(40.1073129445978,4.28775474082735,-8.43927035199998));
#49643=CARTESIAN_POINT('Ctrl Pts',(40.0977448736392,4.28253710202282,-9.67381183084355));
#49644=CARTESIAN_POINT('Ctrl Pts',(40.0792095436937,4.28966756715249,-10.5256145598245));
#49645=CARTESIAN_POINT('Ctrl Pts',(40.0642320282913,4.29763772232685,-11.0088039007234));
#49646=CARTESIAN_POINT('Ctrl Pts',(40.0551153157523,4.30304169912288,-11.2489656079416));
#49647=CARTESIAN_POINT('Ctrl Pts',(40.0475753584296,4.30770081209947,-11.4298114982365));
#49648=CARTESIAN_POINT('Ctrl Pts',(40.0424649739259,4.31079842987331,-11.5667670080804));
#49649=CARTESIAN_POINT('Ctrl Pts',(40.0321283015705,4.31535000812646,-11.8295432782458));
#49650=CARTESIAN_POINT('Ctrl Pts',(40.0136236246797,4.32023439713232,-12.2882344186287));
#49651=CARTESIAN_POINT('Ctrl Pts',(39.9742697126271,4.32108683590219,-13.1798275768615));
#49652=CARTESIAN_POINT('Ctrl Pts',(39.9075680371124,4.32104910385571,-14.3935305465639));
#49653=CARTESIAN_POINT('Ctrl Pts',(39.8245515951701,4.36404624239605,-15.4144192264781));
#49654=CARTESIAN_POINT('Ctrl Pts',(39.7569601952596,4.42364867697426,-16.0701224672648));
#49655=CARTESIAN_POINT('Ctrl Pts',(39.7087610954069,4.4723153808393,-16.5012837962032));
#49656=CARTESIAN_POINT('Ctrl Pts',(39.6690529117656,4.51981795229302,-16.8187798291709));
#49657=CARTESIAN_POINT('Ctrl Pts',(39.6342883707279,4.56646918211518,-17.0802410219354));
#49658=CARTESIAN_POINT('Ctrl Pts',(39.6199984966607,4.58472515057873,-17.1762538452768));
#49659=CARTESIAN_POINT('Ctrl Pts',(39.5889265892873,4.62599416228208,-17.3771298804896));
#49660=CARTESIAN_POINT('Ctrl Pts',(39.554651239453,4.67288333425478,-17.5819569012756));
#49661=CARTESIAN_POINT('Ctrl Pts',(39.517836729212,4.72543655859869,-17.7935001323825));
#49662=CARTESIAN_POINT('Ctrl Pts',(39.4939152441966,4.76046599000218,-17.9278381161626));
#49663=CARTESIAN_POINT('Ctrl Pts',(39.4743069681511,4.78977534427916,-18.0367841617068));
#49664=CARTESIAN_POINT('Ctrl Pts',(39.4593852950562,4.81237727141882,-18.1191591592661));
#49665=CARTESIAN_POINT('Ctrl Pts',(39.4467851989995,4.83171899173353,-18.1883791438491));
#49666=CARTESIAN_POINT('Ctrl Pts',(39.4366168539807,4.84748950267596,-18.2440920040423));
#49667=CARTESIAN_POINT('Ctrl Pts',(39.3496791578271,4.98316553995294,-18.7195275406655));
#49668=CARTESIAN_POINT('Ctrl Pts',(39.1696125978185,5.29476671855043,-19.6872826769249));
#49669=CARTESIAN_POINT('Ctrl Pts',(38.9254391201082,5.8260446390497,-21.2538055525673));
#49670=CARTESIAN_POINT('Ctrl Pts',(38.8091730810157,6.16624702587357,-22.3689791879353));
#49671=CARTESIAN_POINT('Ctrl Pts',(38.7609438346582,6.35633355146274,-23.0827727912001));
#49672=CARTESIAN_POINT('Ctrl Pts',(38.7488279482753,6.42508837087025,-23.329659703437));
#49673=CARTESIAN_POINT('Ctrl Pts',(38.7278858800121,6.5693101036196,-23.8434439852938));
#49674=CARTESIAN_POINT('Ctrl Pts',(38.7073568571337,6.82482364374566,-24.7329543374407));
#49675=CARTESIAN_POINT('Ctrl Pts',(38.7112017822482,7.19631750331981,-26.0144237229354));
#49676=CARTESIAN_POINT('Ctrl Pts',(38.7502041664417,7.61697021007329,-27.5653952969295));
#49677=CARTESIAN_POINT('Ctrl Pts',(38.7794787848461,7.85707833808124,-28.6136653389407));
#49678=CARTESIAN_POINT('Ctrl Pts',(38.7890382182912,7.97473470366522,-29.2064710004707));
#49679=CARTESIAN_POINT('Ctrl Pts',(38.7909034054849,8.00090786122559,-29.3403315551717));
#49680=CARTESIAN_POINT('Ctrl Pts',(38.7953101761858,8.0511770518412,-29.606341355115));
#49681=CARTESIAN_POINT('Ctrl Pts',(38.8041101311858,8.13469272707989,-30.0712812851529));
#49682=CARTESIAN_POINT('Ctrl Pts',(38.8262952957626,8.28461802010922,-30.9955386075008));
#49683=CARTESIAN_POINT('Ctrl Pts',(38.8690901302992,8.45752449381605,-32.2998439063812));
#49684=CARTESIAN_POINT('Ctrl Pts',(38.9213026202173,8.59554440185858,-33.5769673036543));
#49685=CARTESIAN_POINT('Ctrl Pts',(38.9649646296608,8.69785473195649,-34.5798586006522));
#49686=CARTESIAN_POINT('Ctrl Pts',(38.9867947953882,8.74832837595039,-35.0744900763109));
#49687=CARTESIAN_POINT('Ctrl Pts',(39.0029788553092,8.7869259048607,-35.4441031748303));
#49688=CARTESIAN_POINT('Ctrl Pts',(39.0137851816264,8.81332284709096,-35.7023542144892));
#49689=CARTESIAN_POINT('Ctrl Pts',(39.0363669701529,8.86363270877695,-36.2118091976656));
#49690=CARTESIAN_POINT('Ctrl Pts',(39.0775623106058,8.94696765931663,-37.1041976637785));
#49691=CARTESIAN_POINT('Ctrl Pts',(39.1642231201606,9.09472486839895,-38.8796940426679));
#49692=CARTESIAN_POINT('Ctrl Pts',(39.2358830961913,9.19261049889707,-40.3979192073547));
#49693=CARTESIAN_POINT('Ctrl Pts',(39.2832491197789,9.26213510924688,-41.6660593258461));
#49694=CARTESIAN_POINT('Ctrl Pts',(39.2963609311839,9.28162753281898,-42.0486332010792));
#49695=CARTESIAN_POINT('Ctrl Pts',(39.3122407852406,9.30498530969422,-42.5567449806013));
#49696=CARTESIAN_POINT('Ctrl Pts',(39.3272012842619,9.32679323766449,-43.0652703573797));
#49697=CARTESIAN_POINT('Ctrl Pts',(39.3444391257118,9.3513141849052,-43.7003677520274));
#49698=CARTESIAN_POINT('Ctrl Pts',(39.3636542466282,9.37707891605137,-44.4615057370672));
#49699=CARTESIAN_POINT('Ctrl Pts',(39.3791663659872,9.39605873195574,-45.0943593321814));
#49700=CARTESIAN_POINT('Ctrl Pts',(39.3916724839035,9.41007620651285,-45.5995359708631));
#49701=CARTESIAN_POINT('Ctrl Pts',(39.4012261438507,9.42009333262994,-45.9777897987432));
#49702=CARTESIAN_POINT('Ctrl Pts',(39.4110598971786,9.42969807933419,-46.3553745961967));
#49703=CARTESIAN_POINT('Ctrl Pts',(39.4246721994116,9.4420605604787,-46.8577539520659));
#49704=CARTESIAN_POINT('Ctrl Pts',(39.4356599382094,9.45097650435408,-47.2334521355618));
#49705=CARTESIAN_POINT('Ctrl Pts',(39.4473515344133,9.45982361763867,-47.6087025243231));
#49706=CARTESIAN_POINT('Ctrl Pts',(39.455337067446,9.4663017968158,-47.8489229908066));
#49707=CARTESIAN_POINT('Ctrl Pts',(39.4718790872392,9.48214615291164,-48.3402938738331));
#49708=CARTESIAN_POINT('Ctrl Pts',(39.5020923450511,9.51513391225086,-49.2072285291987));
#49709=CARTESIAN_POINT('Ctrl Pts',(39.5475557172048,9.56722915901666,-50.4780205381822));
#49710=CARTESIAN_POINT('Ctrl Pts',(39.6016890568396,9.60042591580183,-52.0487581356094));
#49711=CARTESIAN_POINT('Ctrl Pts',(39.6347305365777,9.57525937165125,-53.1273923993307));
#49712=CARTESIAN_POINT('Ctrl Pts',(39.6535137749267,9.53479531567369,-53.8138129076782));
#49713=CARTESIAN_POINT('Ctrl Pts',(39.661169940129,9.51015686831468,-54.1263920717817));
#49714=CARTESIAN_POINT('Ctrl Pts',(39.6764625795126,9.44253409843686,-54.7125978515887));
#49715=CARTESIAN_POINT('Ctrl Pts',(39.7028639675253,9.28571205301212,-55.7058062339899));
#49716=CARTESIAN_POINT('Ctrl Pts',(39.7530011338049,8.89889291572278,-57.5194444827078));
#49717=CARTESIAN_POINT('Ctrl Pts',(39.7835032645467,8.69962611761777,-58.7903065084076));
#49718=CARTESIAN_POINT('Ctrl Pts',(39.8000150983343,8.73424237255801,-59.5232704936248));
#49719=CARTESIAN_POINT('Ctrl Pts',(39.8019222250902,8.74013864044067,-59.6338670314763));
#49720=CARTESIAN_POINT('Ctrl Pts',(39.8055094403312,8.75489037257384,-59.8442120746572));
#49721=CARTESIAN_POINT('Ctrl Pts',(39.8111544726665,8.78982528331435,-60.2212344718915));
#49722=CARTESIAN_POINT('Ctrl Pts',(39.8201591891876,8.89384559283988,-60.9820397452859));
#49723=CARTESIAN_POINT('Ctrl Pts',(39.8261140542061,9.08579366933095,-61.8776392676396));
#49724=CARTESIAN_POINT('Ctrl Pts',(39.829586958919,9.33715620879876,-62.7891644282645));
#49725=CARTESIAN_POINT('Ctrl Pts',(39.8310001436177,9.49778490900772,-63.3072282738974));
#49726=CARTESIAN_POINT('Ctrl Pts',(39.8318821730951,9.61161725883178,-63.6541416261478));
#49727=CARTESIAN_POINT('Ctrl Pts',(39.8324646653385,9.68921063017446,-63.8858427380399));
#49728=CARTESIAN_POINT('Ctrl Pts',(39.833062788756,9.76920095439907,-64.1179849789079));
#49729=CARTESIAN_POINT('Ctrl Pts',(39.8336228250072,9.84108231145926,-64.3215618361683));
#49730=CARTESIAN_POINT('Ctrl Pts',(39.8339584908655,9.88266127202547,-64.4379995134357));
#49731=CARTESIAN_POINT('Ctrl Pts',(39.8344801499524,9.94550363394761,-64.6127287338887));
#49732=CARTESIAN_POINT('Ctrl Pts',(39.8349578956891,9.99886501999364,-64.758571954533));
#49733=CARTESIAN_POINT('Ctrl Pts',(39.8358402435902,10.0880420096664,-64.9995450483702));
#49734=CARTESIAN_POINT('Ctrl Pts',(39.8373877044086,10.1705358382447,-65.2116971529894));
#49735=CARTESIAN_POINT('Ctrl Pts',(39.8397091263091,10.359927845254,-65.6621240062535));
#49736=CARTESIAN_POINT('Ctrl Pts',(39.8430289812638,10.7281424458995,-66.4514330159084));
#49737=CARTESIAN_POINT('Ctrl Pts',(39.8457928929032,11.6080654311873,-68.0909050412643));
#49738=CARTESIAN_POINT('Ctrl Pts',(39.8432888149172,12.5062750279481,-69.5851588058513));
#49739=CARTESIAN_POINT('Ctrl Pts',(39.841321185353,13.1386526418442,-70.7865926005885));
#49740=CARTESIAN_POINT('Ctrl Pts',(39.8415070828448,13.2675448732065,-71.0311925039694));
#49741=CARTESIAN_POINT('Ctrl Pts',(39.8415070337952,13.5329907597079,-71.5337671071248));
#49742=CARTESIAN_POINT('Ctrl Pts',(39.8416367901604,13.8630247881417,-72.1565594092134));
#49743=CARTESIAN_POINT('Ctrl Pts',(39.8416800538061,14.262096492683,-72.9073007263981));
#49744=CARTESIAN_POINT('Ctrl Pts',(39.8417621362322,15.0615590344823,-74.4078623733623));
#49745=CARTESIAN_POINT('Ctrl Pts',(39.841731405234,15.7313091343584,-75.6606358759336));
#49746=CARTESIAN_POINT('Ctrl Pts',(39.8416414731529,16.7029833477083,-77.4878768425244));
#49747=CARTESIAN_POINT('Ctrl Pts',(39.8416862517014,17.138686967236,-78.3071986448441));
#49748=CARTESIAN_POINT('Ctrl Pts',(39.8416862517014,17.5752085546255,-79.1281763469426));
#49749=CARTESIAN_POINT('Ctrl Pts',(42.1495473044919,4.43306139937208,24.8306020121279));
#49750=CARTESIAN_POINT('Ctrl Pts',(42.1496711288007,4.43306863677417,24.7817216606101));
#49751=CARTESIAN_POINT('Ctrl Pts',(42.1498009969792,4.43307622975196,24.7328423838449));
#49752=CARTESIAN_POINT('Ctrl Pts',(42.1513345113838,4.43316584953248,24.1822208256038));
#49753=CARTESIAN_POINT('Ctrl Pts',(42.1524899114227,4.43321285195566,23.1780525968573));
#49754=CARTESIAN_POINT('Ctrl Pts',(42.155167291499,4.43330892962013,21.1694346333917));
#49755=CARTESIAN_POINT('Ctrl Pts',(42.1653737847785,4.43390567942966,19.6652685471539));
#49756=CARTESIAN_POINT('Ctrl Pts',(42.1871192153285,4.43527922967145,18.4142216147178));
#49757=CARTESIAN_POINT('Ctrl Pts',(42.1975377622187,4.43593271204772,17.9113503761067));
#49758=CARTESIAN_POINT('Ctrl Pts',(42.2236822241422,4.43756527475675,16.9073116829106));
#49759=CARTESIAN_POINT('Ctrl Pts',(42.2797628188204,4.44107469922938,15.1534730382367));
#49760=CARTESIAN_POINT('Ctrl Pts',(42.3331943604571,4.44450509135218,13.651831009471));
#49761=CARTESIAN_POINT('Ctrl Pts',(42.3669550198508,4.44682915128521,12.3975686439851));
#49762=CARTESIAN_POINT('Ctrl Pts',(42.3807873604139,4.44779989493999,11.8967018737848));
#49763=CARTESIAN_POINT('Ctrl Pts',(42.4090840801753,4.44984468734248,10.8949964356632));
#49764=CARTESIAN_POINT('Ctrl Pts',(42.4442171196688,4.45246607212628,9.64252335981429));
#49765=CARTESIAN_POINT('Ctrl Pts',(42.4814072821943,4.45531901001824,8.13800024039924));
#49766=CARTESIAN_POINT('Ctrl Pts',(42.4998434201269,4.45675508843371,7.13312595518398));
#49767=CARTESIAN_POINT('Ctrl Pts',(42.5084122685094,4.45742537182735,6.50504551612233));
#49768=CARTESIAN_POINT('Ctrl Pts',(42.51160778917,4.45768189011103,6.2548761461837));
#49769=CARTESIAN_POINT('Ctrl Pts',(42.5171741324758,4.45815132839053,5.75380286805977));
#49770=CARTESIAN_POINT('Ctrl Pts',(42.5248501417164,4.45885435824313,4.87541295252293));
#49771=CARTESIAN_POINT('Ctrl Pts',(42.53273812315,4.45978601263875,3.11501628858445));
#49772=CARTESIAN_POINT('Ctrl Pts',(42.5294330916105,4.45970186585179,1.60755532665802));
#49773=CARTESIAN_POINT('Ctrl Pts',(42.5249151043497,4.45921098674461,0.547538475444217));
#49774=CARTESIAN_POINT('Ctrl Pts',(42.5243183972503,4.45914818259243,0.42131908384523));
#49775=CARTESIAN_POINT('Ctrl Pts',(42.5229020237262,4.45899935226643,0.169067490081134));
#49776=CARTESIAN_POINT('Ctrl Pts',(42.5198669424298,4.45868324002639,-0.271858993253347));
#49777=CARTESIAN_POINT('Ctrl Pts',(42.5141026079898,4.45807762005991,-0.9005622772302));
#49778=CARTESIAN_POINT('Ctrl Pts',(42.5054293061842,4.45717146798543,-1.65322810939649));
#49779=CARTESIAN_POINT('Ctrl Pts',(42.4922134460657,4.4557594557389,-2.65543993302332));
#49780=CARTESIAN_POINT('Ctrl Pts',(42.4739066559715,4.45377219520505,-3.90642746118527));
#49781=CARTESIAN_POINT('Ctrl Pts',(42.4601455997033,4.45218440214942,-4.90801081744749));
#49782=CARTESIAN_POINT('Ctrl Pts',(42.4526907229684,4.45130677983019,-5.53552450617664));
#49783=CARTESIAN_POINT('Ctrl Pts',(42.4505153709451,4.44981089037036,-5.80126348319439));
#49784=CARTESIAN_POINT('Ctrl Pts',(42.4487840037071,4.44317745383545,-6.31951543703047));
#49785=CARTESIAN_POINT('Ctrl Pts',(42.4510303132461,4.42430589539898,-7.21941478754799));
#49786=CARTESIAN_POINT('Ctrl Pts',(42.4602303355477,4.3893349439202,-8.46815781427861));
#49787=CARTESIAN_POINT('Ctrl Pts',(42.4532219858788,4.37685621361606,-9.66956937468799));
#49788=CARTESIAN_POINT('Ctrl Pts',(42.4271817651349,4.39590747938916,-10.4822054214672));
#49789=CARTESIAN_POINT('Ctrl Pts',(42.4044716210716,4.41668070021709,-10.9386148174557));
#49790=CARTESIAN_POINT('Ctrl Pts',(42.3902153921439,4.43063517945358,-11.1638416979877));
#49791=CARTESIAN_POINT('Ctrl Pts',(42.3782722056273,4.44263468939651,-11.3329536164645));
#49792=CARTESIAN_POINT('Ctrl Pts',(42.3697703806089,4.4519500151394,-11.4646692583993));
#49793=CARTESIAN_POINT('Ctrl Pts',(42.351321649476,4.46934048245381,-11.7159121980543));
#49794=CARTESIAN_POINT('Ctrl Pts',(42.3152439548395,4.49925129058086,-12.1560887373164));
#49795=CARTESIAN_POINT('Ctrl Pts',(42.2297056224542,4.55754971709465,-13.0140184699734));
#49796=CARTESIAN_POINT('Ctrl Pts',(42.0773240096532,4.64888468816603,-14.1882274322353));
#49797=CARTESIAN_POINT('Ctrl Pts',(41.9325191738719,4.77050106757277,-15.1912635102137));
#49798=CARTESIAN_POINT('Ctrl Pts',(41.8452918440761,4.88692134853426,-15.8482707091843));
#49799=CARTESIAN_POINT('Ctrl Pts',(41.7901431054233,4.97564273781242,-16.2835631550585));
#49800=CARTESIAN_POINT('Ctrl Pts',(41.7528864837405,5.05632896224043,-16.608048811206));
#49801=CARTESIAN_POINT('Ctrl Pts',(41.7246967815049,5.13293672777087,-16.8762028627259));
#49802=CARTESIAN_POINT('Ctrl Pts',(41.715396332616,5.15873444698128,-16.9612142112661));
#49803=CARTESIAN_POINT('Ctrl Pts',(41.6944040117279,5.22161590569571,-17.1514437495934));
#49804=CARTESIAN_POINT('Ctrl Pts',(41.672161523455,5.29428393728964,-17.3463288379007));
#49805=CARTESIAN_POINT('Ctrl Pts',(41.6479517267108,5.37832437641012,-17.552483703133));
#49806=CARTESIAN_POINT('Ctrl Pts',(41.6321781699855,5.43491908494667,-17.6841062705179));
#49807=CARTESIAN_POINT('Ctrl Pts',(41.6191255756403,5.48268422564165,-17.7915446933069));
#49808=CARTESIAN_POINT('Ctrl Pts',(41.6091394464926,5.51966990717561,-17.8729907465177));
#49809=CARTESIAN_POINT('Ctrl Pts',(41.600650421912,5.55144709136434,-17.9416361362078));
#49810=CARTESIAN_POINT('Ctrl Pts',(41.5937611144038,5.57742449020185,-17.996981410194));
#49811=CARTESIAN_POINT('Ctrl Pts',(41.5346675293466,5.80122879970189,-18.4699284319811));
#49812=CARTESIAN_POINT('Ctrl Pts',(41.4045373278031,6.32571973585028,-19.4466039091188));
#49813=CARTESIAN_POINT('Ctrl Pts',(41.1873260294732,7.19197459488153,-21.0465699183824));
#49814=CARTESIAN_POINT('Ctrl Pts',(41.0595608408375,7.70110568021989,-22.2372870473665));
#49815=CARTESIAN_POINT('Ctrl Pts',(41.0098926459178,7.95033509171429,-23.0367194728072));
#49816=CARTESIAN_POINT('Ctrl Pts',(40.9997427846034,8.03481830193072,-23.3111939636317));
#49817=CARTESIAN_POINT('Ctrl Pts',(40.9877047371297,8.1971669377381,-23.8792071216224));
#49818=CARTESIAN_POINT('Ctrl Pts',(40.9971528699687,8.44713220264407,-24.8513408873681));
#49819=CARTESIAN_POINT('Ctrl Pts',(41.0781879173059,8.72716793635427,-26.2183255071894));
#49820=CARTESIAN_POINT('Ctrl Pts',(41.232085897233,8.9607472408925,-27.7992151801498));
#49821=CARTESIAN_POINT('Ctrl Pts',(41.3275733968445,9.07279975647791,-28.8084262738872));
#49822=CARTESIAN_POINT('Ctrl Pts',(41.3663199668624,9.13284859687676,-29.3629560207209));
#49823=CARTESIAN_POINT('Ctrl Pts',(41.374418954637,9.14740642213019,-29.502410456033));
#49824=CARTESIAN_POINT('Ctrl Pts',(41.3910015401214,9.17309908398007,-29.7712916311122));
#49825=CARTESIAN_POINT('Ctrl Pts',(41.4200465535244,9.21262050656757,-30.2443705780784));
#49826=CARTESIAN_POINT('Ctrl Pts',(41.4785475784755,9.26973374039164,-31.178128557866));
#49827=CARTESIAN_POINT('Ctrl Pts',(41.5608973985288,9.30357052903612,-32.4869538878879));
#49828=CARTESIAN_POINT('Ctrl Pts',(41.6385333838955,9.30801153630281,-33.7540908153341));
#49829=CARTESIAN_POINT('Ctrl Pts',(41.6970645298839,9.31307806614043,-34.7421863638859));
#49830=CARTESIAN_POINT('Ctrl Pts',(41.725145340962,9.31904280747962,-35.2271388313623));
#49831=CARTESIAN_POINT('Ctrl Pts',(41.7457972589986,9.32585891497254,-35.5887587531886));
#49832=CARTESIAN_POINT('Ctrl Pts',(41.7596279291193,9.33040802484349,-35.8452562293953));
#49833=CARTESIAN_POINT('Ctrl Pts',(41.7870666252456,9.33854391595455,-36.3491403525278));
#49834=CARTESIAN_POINT('Ctrl Pts',(41.8343110804492,9.35083950840714,-37.2328678954738));
#49835=CARTESIAN_POINT('Ctrl Pts',(41.9242318227127,9.36875964061655,-38.9902018452413));
#49836=CARTESIAN_POINT('Ctrl Pts',(41.9877472130835,9.3773882204503,-40.4935747403769));
#49837=CARTESIAN_POINT('Ctrl Pts',(42.0272574366068,9.38538630372938,-41.7492890543106));
#49838=CARTESIAN_POINT('Ctrl Pts',(42.0381644075537,9.38721236589782,-42.1286435688507));
#49839=CARTESIAN_POINT('Ctrl Pts',(42.0511232360393,9.38880216746414,-42.6319389127963));
#49840=CARTESIAN_POINT('Ctrl Pts',(42.0630576969637,9.38997229832213,-43.1355830201978));
#49841=CARTESIAN_POINT('Ctrl Pts',(42.0761701660747,9.39088764188186,-43.7642917648869));
#49842=CARTESIAN_POINT('Ctrl Pts',(42.0893241462601,9.39189107665992,-44.5173903243411));
#49843=CARTESIAN_POINT('Ctrl Pts',(42.0983983816962,9.39329188039546,-45.1432207338739));
#49844=CARTESIAN_POINT('Ctrl Pts',(42.1047279826398,9.3951652624769,-45.6425970992607));
#49845=CARTESIAN_POINT('Ctrl Pts',(42.1090298863024,9.39702639675693,-46.0164087043907));
#49846=CARTESIAN_POINT('Ctrl Pts',(42.1129296314231,9.39943973181789,-46.3894634288434));
#49847=CARTESIAN_POINT('Ctrl Pts',(42.1176583956564,9.40352647135289,-46.8856896438178));
#49848=CARTESIAN_POINT('Ctrl Pts',(42.1206949411916,9.40767304516513,-47.2566448321986));
#49849=CARTESIAN_POINT('Ctrl Pts',(42.1235199090029,9.41276160489034,-47.6270477559909));
#49850=CARTESIAN_POINT('Ctrl Pts',(42.1250877992718,9.4172418231088,-47.8629849085641));
#49851=CARTESIAN_POINT('Ctrl Pts',(42.1270615745575,9.43060438525352,-48.3469638310146));
#49852=CARTESIAN_POINT('Ctrl Pts',(42.1277850714073,9.46312836091267,-49.2019780343514));
#49853=CARTESIAN_POINT('Ctrl Pts',(42.1229160656678,9.5238508496721,-50.4596868135424));
#49854=CARTESIAN_POINT('Ctrl Pts',(42.1133957123464,9.5772391955778,-52.0205213259128));
#49855=CARTESIAN_POINT('Ctrl Pts',(42.1084948227126,9.56874892174017,-53.0965359880168));
#49856=CARTESIAN_POINT('Ctrl Pts',(42.1073149193619,9.53893199127567,-53.7823908590073));
#49857=CARTESIAN_POINT('Ctrl Pts',(42.1068070481075,9.52000368930904,-54.0890497549449));
#49858=CARTESIAN_POINT('Ctrl Pts',(42.1057800418371,9.46508757911363,-54.6685113050492));
#49859=CARTESIAN_POINT('Ctrl Pts',(42.1038697439046,9.33357303918558,-55.6522294188415));
#49860=CARTESIAN_POINT('Ctrl Pts',(42.1014299978837,9.00154770075439,-57.4608506741487));
#49861=CARTESIAN_POINT('Ctrl Pts',(42.0981196164158,8.83054051958777,-58.7441892388778));
#49862=CARTESIAN_POINT('Ctrl Pts',(42.102473629823,8.87389154790522,-59.5018847710551));
#49863=CARTESIAN_POINT('Ctrl Pts',(42.1029927927764,8.88102566132885,-59.6144631853288));
#49864=CARTESIAN_POINT('Ctrl Pts',(42.1042902056847,8.89787525908731,-59.8290965989406));
#49865=CARTESIAN_POINT('Ctrl Pts',(42.1070771307108,8.93590705043286,-60.2127458185008));
#49866=CARTESIAN_POINT('Ctrl Pts',(42.1145055180033,9.04366772762629,-60.9845447964307));
#49867=CARTESIAN_POINT('Ctrl Pts',(42.1256720654178,9.23499438509171,-61.8869276390296));
#49868=CARTESIAN_POINT('Ctrl Pts',(42.1367429007561,9.48260508362316,-62.8003515442931));
#49869=CARTESIAN_POINT('Ctrl Pts',(42.14250105984,9.64046459144008,-63.3177835092151));
#49870=CARTESIAN_POINT('Ctrl Pts',(42.1459717192686,9.75238155687925,-63.6636132991502));
#49871=CARTESIAN_POINT('Ctrl Pts',(42.1481777795587,9.82869851579108,-63.8944172718737));
#49872=CARTESIAN_POINT('Ctrl Pts',(42.1502082497363,9.90743557445359,-64.1254062764649));
#49873=CARTESIAN_POINT('Ctrl Pts',(42.1518026560732,9.9782825312177,-64.3277498871866));
#49874=CARTESIAN_POINT('Ctrl Pts',(42.1526581514894,10.0192943221162,-64.4434190207101));
#49875=CARTESIAN_POINT('Ctrl Pts',(42.1538847500963,10.0813139802647,-64.616934095387));
#49876=CARTESIAN_POINT('Ctrl Pts',(42.1547828775597,10.1340519497849,-64.7616293724365));
#49877=CARTESIAN_POINT('Ctrl Pts',(42.1561038287678,10.2223350366598,-65.0005771275026));
#49878=CARTESIAN_POINT('Ctrl Pts',(42.1582105074284,10.3048934440516,-65.2131820487537));
#49879=CARTESIAN_POINT('Ctrl Pts',(42.1614148903209,10.4938853814907,-65.6631041403599));
#49880=CARTESIAN_POINT('Ctrl Pts',(42.1659317372334,10.8617557144184,-66.4523321841232));
#49881=CARTESIAN_POINT('Ctrl Pts',(42.1697446831104,11.7410172575913,-68.0912718937255));
#49882=CARTESIAN_POINT('Ctrl Pts',(42.1665941544893,12.6391474445693,-69.585738936787));
#49883=CARTESIAN_POINT('Ctrl Pts',(42.164216736395,13.2713485701069,-70.7872900881665));
#49884=CARTESIAN_POINT('Ctrl Pts',(42.1644755981786,13.4001883022114,-71.031839329675));
#49885=CARTESIAN_POINT('Ctrl Pts',(42.1645103319829,13.6655586906436,-71.5343623900713));
#49886=CARTESIAN_POINT('Ctrl Pts',(42.1646955444271,13.9955320466049,-72.1570933130439));
#49887=CARTESIAN_POINT('Ctrl Pts',(42.1647527808815,14.3945740389569,-72.9077835335904));
#49888=CARTESIAN_POINT('Ctrl Pts',(42.1648264840299,15.1940437661561,-74.4082770771058));
#49889=CARTESIAN_POINT('Ctrl Pts',(42.1647109721311,15.8639134512714,-75.6611090767548));
#49890=CARTESIAN_POINT('Ctrl Pts',(42.1645878003007,16.8356533223413,-77.4884825573361));
#49891=CARTESIAN_POINT('Ctrl Pts',(42.164642108565,17.2713436057313,-78.3077784929303));
#49892=CARTESIAN_POINT('Ctrl Pts',(42.1646421085649,17.7078651931207,-79.1287561950287));
#49893=CARTESIAN_POINT('Ctrl Pts',(44.9333669821193,4.63587816982636,24.8307041888048));
#49894=CARTESIAN_POINT('Ctrl Pts',(44.9334979023578,4.63589034715466,24.7818270640558));
#49895=CARTESIAN_POINT('Ctrl Pts',(44.9336352132025,4.63590311675132,24.7329510937676));
#49896=CARTESIAN_POINT('Ctrl Pts',(44.9352566680075,4.63605389014306,24.1823667254701));
#49897=CARTESIAN_POINT('Ctrl Pts',(44.9364556490902,4.63619612515483,23.1782347087865));
#49898=CARTESIAN_POINT('Ctrl Pts',(44.9392184572998,4.63654477111558,21.1696867815275));
#49899=CARTESIAN_POINT('Ctrl Pts',(44.9500110013522,4.63754679539249,19.6655321882608));
#49900=CARTESIAN_POINT('Ctrl Pts',(44.9731189460185,4.63953900490499,18.4144926058473));
#49901=CARTESIAN_POINT('Ctrl Pts',(44.984185233339,4.64050938219707,17.9118227013444));
#49902=CARTESIAN_POINT('Ctrl Pts',(45.0119472070561,4.64297264048472,16.9079214810503));
#49903=CARTESIAN_POINT('Ctrl Pts',(45.0715072955918,4.64825356183551,15.1540495788374));
#49904=CARTESIAN_POINT('Ctrl Pts',(45.1283478334055,4.65306438840288,13.6517227532813));
#49905=CARTESIAN_POINT('Ctrl Pts',(45.1644336381274,4.65570009337017,12.3966002597124));
#49906=CARTESIAN_POINT('Ctrl Pts',(45.1792335941515,4.65673530413848,11.895383592665));
#49907=CARTESIAN_POINT('Ctrl Pts',(45.2095615747859,4.6587103195502,10.8931727060101));
#49908=CARTESIAN_POINT('Ctrl Pts',(45.2472949754295,4.66094941471739,9.64032070536151));
#49909=CARTESIAN_POINT('Ctrl Pts',(45.2873515969718,4.66311480069243,8.13584259206917));
#49910=CARTESIAN_POINT('Ctrl Pts',(45.3072846050537,4.66410108210267,7.13126553200396));
#49911=CARTESIAN_POINT('Ctrl Pts',(45.3165865636776,4.66454211847491,6.50346922286369));
#49912=CARTESIAN_POINT('Ctrl Pts',(45.3200619051891,4.66468562275181,6.25304880874878));
#49913=CARTESIAN_POINT('Ctrl Pts',(45.3261392327148,4.66486046820295,5.75176838221114));
#49914=CARTESIAN_POINT('Ctrl Pts',(45.3345868607911,4.66490596131958,4.87307865335014));
#49915=CARTESIAN_POINT('Ctrl Pts',(45.343562651372,4.66426069244295,3.11300099070761));
#49916=CARTESIAN_POINT('Ctrl Pts',(45.3405430703049,4.66342578091586,1.60687954862173));
#49917=CARTESIAN_POINT('Ctrl Pts',(45.3360427857126,4.66366032599448,0.548605170266317));
#49918=CARTESIAN_POINT('Ctrl Pts',(45.3354519489155,4.66369145735315,0.422590875695751));
#49919=CARTESIAN_POINT('Ctrl Pts',(45.3340608597991,4.66376449726404,0.170728951294827));
#49920=CARTESIAN_POINT('Ctrl Pts',(45.3310991987033,4.66392039122531,-0.26956437068448));
#49921=CARTESIAN_POINT('Ctrl Pts',(45.325492148662,4.66421182722607,-0.897571164468606));
#49922=CARTESIAN_POINT('Ctrl Pts',(45.3169761097054,4.66466508037382,-1.64953651843115));
#49923=CARTESIAN_POINT('Ctrl Pts',(45.3037963714485,4.66535305212888,-2.65122580347224));
#49924=CARTESIAN_POINT('Ctrl Pts',(45.2849366378433,4.66632617957509,-3.90218803647896));
#49925=CARTESIAN_POINT('Ctrl Pts',(45.2695380422325,4.66700510860821,-4.90425811297242));
#49926=CARTESIAN_POINT('Ctrl Pts',(45.2605037636271,4.6673525618632,-5.53292392344991));
#49927=CARTESIAN_POINT('Ctrl Pts',(45.2579511424781,4.66497636398758,-5.81475951906011));
#49928=CARTESIAN_POINT('Ctrl Pts',(45.25626273268,4.65221408575269,-6.35050785645233));
#49929=CARTESIAN_POINT('Ctrl Pts',(45.2600538878317,4.61439141343846,-7.27242908556972));
#49930=CARTESIAN_POINT('Ctrl Pts',(45.2723247521635,4.54589500426883,-8.51158077669593));
#49931=CARTESIAN_POINT('Ctrl Pts',(45.2615711141445,4.52686668740426,-9.65381276654877));
#49932=CARTESIAN_POINT('Ctrl Pts',(45.225449036529,4.56656545267834,-10.3973910987338));
#49933=CARTESIAN_POINT('Ctrl Pts',(45.1944970405879,4.60700490521411,-10.8072424755639));
#49934=CARTESIAN_POINT('Ctrl Pts',(45.175294273951,4.63349787943198,-11.0070600284335));
#49935=CARTESIAN_POINT('Ctrl Pts',(45.1593270749882,4.65598440875296,-11.1560398985103));
#49936=CARTESIAN_POINT('Ctrl Pts',(45.1475104260899,4.67364615357786,-11.2648315375785));
#49937=CARTESIAN_POINT('Ctrl Pts',(45.1206604029663,4.7107868069394,-11.4784866796688));
#49938=CARTESIAN_POINT('Ctrl Pts',(45.0656450549295,4.78318112797988,-11.8572625762786));
#49939=CARTESIAN_POINT('Ctrl Pts',(44.9291075434275,4.95228012845482,-12.6240386706489));
#49940=CARTESIAN_POINT('Ctrl Pts',(44.6929466638584,5.24814367801828,-13.7657020756945));
#49941=CARTESIAN_POINT('Ctrl Pts',(44.5043923325839,5.57416245985198,-14.8524096422358));
#49942=CARTESIAN_POINT('Ctrl Pts',(44.4075739601456,5.82140209288632,-15.5941629233189));
#49943=CARTESIAN_POINT('Ctrl Pts',(44.3512027368814,5.99428860812313,-16.0922118718401));
#49944=CARTESIAN_POINT('Ctrl Pts',(44.3190745151794,6.13339619520395,-16.4694384969807));
#49945=CARTESIAN_POINT('Ctrl Pts',(44.299226354482,6.25379420494699,-16.7826337520401));
#49946=CARTESIAN_POINT('Ctrl Pts',(44.2969229064794,6.29291565417392,-16.8764705598309));
#49947=CARTESIAN_POINT('Ctrl Pts',(44.2902827333537,6.38480407787161,-17.0866420639222));
#49948=CARTESIAN_POINT('Ctrl Pts',(44.2860475637416,6.48497231549507,-17.2959799360825));
#49949=CARTESIAN_POINT('Ctrl Pts',(44.2820535485249,6.59558853274627,-17.5143805077403));
#49950=CARTESIAN_POINT('Ctrl Pts',(44.2799827571647,6.66801192718192,-17.6522587472907));
#49951=CARTESIAN_POINT('Ctrl Pts',(44.2784147873834,6.72802588610404,-17.7641449538538));
#49952=CARTESIAN_POINT('Ctrl Pts',(44.2773150161733,6.77395220332713,-17.8486085072498));
#49953=CARTESIAN_POINT('Ctrl Pts',(44.2764425517342,6.81298585885999,-17.919542477742));
#49954=CARTESIAN_POINT('Ctrl Pts',(44.2757697912063,6.84463869239768,-17.9765872337853));
#49955=CARTESIAN_POINT('Ctrl Pts',(44.2702372924635,7.11608657359585,-18.4632195255323));
#49956=CARTESIAN_POINT('Ctrl Pts',(44.2630045039821,7.7074245624471,-19.4457608820307));
#49957=CARTESIAN_POINT('Ctrl Pts',(44.2611419814737,8.6222707657364,-21.0521041695837));
#49958=CARTESIAN_POINT('Ctrl Pts',(44.2725461051462,9.13292987135093,-22.2730506947804));
#49959=CARTESIAN_POINT('Ctrl Pts',(44.2816142769132,9.35867008260939,-23.099799003702));
#49960=CARTESIAN_POINT('Ctrl Pts',(44.2876325887398,9.43432231200718,-23.4010860497399));
#49961=CARTESIAN_POINT('Ctrl Pts',(44.3058999069322,9.56020964037718,-24.0113613345034));
#49962=CARTESIAN_POINT('Ctrl Pts',(44.3525560292799,9.71031473239032,-25.0527674960325));
#49963=CARTESIAN_POINT('Ctrl Pts',(44.4443173329707,9.77268873266039,-26.4730277999505));
#49964=CARTESIAN_POINT('Ctrl Pts',(44.55190239764,9.73690379055372,-28.044254216766));
#49965=CARTESIAN_POINT('Ctrl Pts',(44.6030629052135,9.71526496697493,-29.0043367489214));
#49966=CARTESIAN_POINT('Ctrl Pts',(44.6217562968118,9.71971469691473,-29.5208988965381));
#49967=CARTESIAN_POINT('Ctrl Pts',(44.6257907026183,9.72052246806346,-29.6585948864942));
#49968=CARTESIAN_POINT('Ctrl Pts',(44.6330315310391,9.72062718334552,-29.9202917581488));
#49969=CARTESIAN_POINT('Ctrl Pts',(44.6437898559616,9.71741656585746,-30.3829589911478));
#49970=CARTESIAN_POINT('Ctrl Pts',(44.6583278615562,9.69897448965321,-31.2959284016156));
#49971=CARTESIAN_POINT('Ctrl Pts',(44.6639992263246,9.64838030429391,-32.5818848810449));
#49972=CARTESIAN_POINT('Ctrl Pts',(44.662053705329,9.58931415476959,-33.8363371428099));
#49973=CARTESIAN_POINT('Ctrl Pts',(44.6631620352193,9.54999353886839,-34.8212887515721));
#49974=CARTESIAN_POINT('Ctrl Pts',(44.665816383274,9.53502460744065,-35.3070035254001));
#49975=CARTESIAN_POINT('Ctrl Pts',(44.6690383588918,9.52628046901086,-35.6699624300507));
#49976=CARTESIAN_POINT('Ctrl Pts',(44.6712928845314,9.52019431481522,-35.9233658300565));
#49977=CARTESIAN_POINT('Ctrl Pts',(44.6760911582724,9.50849652247419,-36.4234977421827));
#49978=CARTESIAN_POINT('Ctrl Pts',(44.685147460511,9.48876679621087,-37.2999188157056));
#49979=CARTESIAN_POINT('Ctrl Pts',(44.7046283752818,9.45311685214669,-39.0448048665985));
#49980=CARTESIAN_POINT('Ctrl Pts',(44.7197705753507,9.43012322769321,-40.5386959198999));
#49981=CARTESIAN_POINT('Ctrl Pts',(44.7269699252603,9.41682046044001,-41.7869668791111));
#49982=CARTESIAN_POINT('Ctrl Pts',(44.7286300530116,9.41246364758171,-42.164811723922));
#49983=CARTESIAN_POINT('Ctrl Pts',(44.730085289389,9.40654236583585,-42.6653424239963));
#49984=CARTESIAN_POINT('Ctrl Pts',(44.7311163037048,9.40067534306281,-43.1661034760371));
#49985=CARTESIAN_POINT('Ctrl Pts',(44.7317465398154,9.39377152228866,-43.7907628656876));
#49986=CARTESIAN_POINT('Ctrl Pts',(44.7319011558653,9.38713394939372,-44.5384113611807));
#49987=CARTESIAN_POINT('Ctrl Pts',(44.7319043098671,9.38377476804963,-45.1591833277389));
#49988=CARTESIAN_POINT('Ctrl Pts',(44.7320495731726,9.38287360366303,-45.6542337605805));
#49989=CARTESIAN_POINT('Ctrl Pts',(44.7322894649879,9.38320418990688,-46.0246454874006));
#49990=CARTESIAN_POINT('Ctrl Pts',(44.7327160627022,9.38465971037982,-46.3941481905926));
#49991=CARTESIAN_POINT('Ctrl Pts',(44.7336068540788,9.3882586426597,-46.8854311103639));
#49992=CARTESIAN_POINT('Ctrl Pts',(44.734728483665,9.39299139524036,-47.2524296398557));
#49993=CARTESIAN_POINT('Ctrl Pts',(44.7362621756588,9.3993314064098,-47.6186566589199));
#49994=CARTESIAN_POINT('Ctrl Pts',(44.7372683747344,9.40488441682722,-47.8500549667319));
#49995=CARTESIAN_POINT('Ctrl Pts',(44.7391923515483,9.42160812051236,-48.3268142682009));
#49996=CARTESIAN_POINT('Ctrl Pts',(44.7424819869383,9.46295827084018,-49.1706486727884));
#49997=CARTESIAN_POINT('Ctrl Pts',(44.7476480509491,9.54397160623419,-50.4182362572702));
#49998=CARTESIAN_POINT('Ctrl Pts',(44.7572798693228,9.62975168477225,-51.9754036097172));
#49999=CARTESIAN_POINT('Ctrl Pts',(44.7679244366479,9.64388643626604,-53.0551856218759));
#50000=CARTESIAN_POINT('Ctrl Pts',(44.7766541899908,9.62670923029403,-53.7452837511029));
#50001=CARTESIAN_POINT('Ctrl Pts',(44.7806492307899,9.61386186366492,-54.0487471333629));
#50002=CARTESIAN_POINT('Ctrl Pts',(44.7899635506518,9.57141967994042,-54.6254954386526));
#50003=CARTESIAN_POINT('Ctrl Pts',(44.8090369070717,9.46305212497968,-55.6049996912444));
#50004=CARTESIAN_POINT('Ctrl Pts',(44.8535080186623,9.17796813642923,-57.4128116283892));
#50005=CARTESIAN_POINT('Ctrl Pts',(44.8871058615105,9.03482251140912,-58.7066364139985));
#50006=CARTESIAN_POINT('Ctrl Pts',(44.9025681610021,9.08815669291933,-59.4823187154555));
#50007=CARTESIAN_POINT('Ctrl Pts',(44.9043036643419,9.09661811168106,-59.5969035133632));
#50008=CARTESIAN_POINT('Ctrl Pts',(44.9076457910595,9.11571979425487,-59.8154200625901));
#50009=CARTESIAN_POINT('Ctrl Pts',(44.9130012877661,9.15698333644756,-60.2052869646091));
#50010=CARTESIAN_POINT('Ctrl Pts',(44.9220063838328,9.26828364727815,-60.987323531218));
#50011=CARTESIAN_POINT('Ctrl Pts',(44.9289888871208,9.45792877534444,-61.8962934745214));
#50012=CARTESIAN_POINT('Ctrl Pts',(44.9340057627777,9.70063939087671,-62.8116504337714));
#50013=CARTESIAN_POINT('Ctrl Pts',(44.9363590175526,9.85513792044804,-63.3285348517037));
#50014=CARTESIAN_POINT('Ctrl Pts',(44.9378449419104,9.96480529890248,-63.673351095806));
#50015=CARTESIAN_POINT('Ctrl Pts',(44.9388207088418,10.0396397863523,-63.9033067107434));
#50016=CARTESIAN_POINT('Ctrl Pts',(44.9397905035546,10.1169431330247,-64.1331971180868));
#50017=CARTESIAN_POINT('Ctrl Pts',(44.9406491940526,10.1866267537447,-64.3343557746241));
#50018=CARTESIAN_POINT('Ctrl Pts',(44.9411462012543,10.2270060089222,-64.4492842746316));
#50019=CARTESIAN_POINT('Ctrl Pts',(44.9419002284174,10.2881135621904,-64.6216269443045));
#50020=CARTESIAN_POINT('Ctrl Pts',(44.9425480773535,10.3401695449471,-64.7652089194153));
#50021=CARTESIAN_POINT('Ctrl Pts',(44.9436808820581,10.4274889561099,-65.002183647395));
#50022=CARTESIAN_POINT('Ctrl Pts',(44.9457296368594,10.5100058197732,-65.2151434701464));
#50023=CARTESIAN_POINT('Ctrl Pts',(44.9488563346992,10.6984555106575,-65.6644707635653));
#50024=CARTESIAN_POINT('Ctrl Pts',(44.9534691872529,11.0658192309505,-66.4534539136408));
#50025=CARTESIAN_POINT('Ctrl Pts',(44.9578122690832,11.9444667864977,-68.0917160342065));
#50026=CARTESIAN_POINT('Ctrl Pts',(44.9547060432961,12.842828120554,-69.5864114707208));
#50027=CARTESIAN_POINT('Ctrl Pts',(44.951532773924,13.4749122379537,-70.7882465589457));
#50028=CARTESIAN_POINT('Ctrl Pts',(44.9518124352172,13.6037024593924,-71.0327438068155));
#50029=CARTESIAN_POINT('Ctrl Pts',(44.9517934305402,13.8690078572436,-71.5352327466239));
#50030=CARTESIAN_POINT('Ctrl Pts',(44.9519840675579,14.1989254473966,-72.1579099499273));
#50031=CARTESIAN_POINT('Ctrl Pts',(44.9520529495098,14.597943036186,-72.9085592690338));
#50032=CARTESIAN_POINT('Ctrl Pts',(44.9522036988278,15.3974222066628,-74.4089927823421));
#50033=CARTESIAN_POINT('Ctrl Pts',(44.9521854715562,16.0673918589498,-75.6618676901378));
#50034=CARTESIAN_POINT('Ctrl Pts',(44.952029847549,17.0391786068487,-77.4893496207617));
#50035=CARTESIAN_POINT('Ctrl Pts',(44.9520993138037,17.4748560812393,-78.3086236045963));
#50036=CARTESIAN_POINT('Ctrl Pts',(44.9520993138036,17.9113776686288,-79.1296013066945));
#50037=CARTESIAN_POINT('Ctrl Pts',(47.7140540990422,4.88276541972323,24.8307163556754));
#50038=CARTESIAN_POINT('Ctrl Pts',(47.7141971173369,4.88278120060972,24.7818396449418));
#50039=CARTESIAN_POINT('Ctrl Pts',(47.7143471136432,4.88279775286369,24.7329641087686));
#50040=CARTESIAN_POINT('Ctrl Pts',(47.7161182130505,4.88299298383964,24.1823841333583));
#50041=CARTESIAN_POINT('Ctrl Pts',(47.7175115582471,4.8831861471748,23.1782641182978));
#50042=CARTESIAN_POINT('Ctrl Pts',(47.7207801503277,4.8836674491671,21.1697193937816));
#50043=CARTESIAN_POINT('Ctrl Pts',(47.7325651987108,4.88496318581718,19.6655383093397));
#50044=CARTESIAN_POINT('Ctrl Pts',(47.757378839843,4.88749314359155,18.4144737796136));
#50045=CARTESIAN_POINT('Ctrl Pts',(47.7693014564166,4.88871928109935,17.9117784514982));
#50046=CARTESIAN_POINT('Ctrl Pts',(47.7992812031425,4.89181749989893,16.9078631888763));
#50047=CARTESIAN_POINT('Ctrl Pts',(47.8635810010464,4.89844697175688,15.1540271445886));
#50048=CARTESIAN_POINT('Ctrl Pts',(47.9243824440423,4.90452675243611,13.6517624151243));
#50049=CARTESIAN_POINT('Ctrl Pts',(47.9619455787172,4.90795802124528,12.3967075962964));
#50050=CARTESIAN_POINT('Ctrl Pts',(47.9772376973858,4.90931662958083,11.8955151113586));
#50051=CARTESIAN_POINT('Ctrl Pts',(48.0082082808038,4.91194454293002,10.8933262319668));
#50052=CARTESIAN_POINT('Ctrl Pts',(48.046211838742,4.91498035507158,9.64042959022222));
#50053=CARTESIAN_POINT('Ctrl Pts',(48.0860185467446,4.91797824695313,8.13589047411817));
#50054=CARTESIAN_POINT('Ctrl Pts',(48.1056098351614,4.91937625239819,7.13124158256873));
#50055=CARTESIAN_POINT('Ctrl Pts',(48.1146981889812,4.92001433792512,6.50342636458933));
#50056=CARTESIAN_POINT('Ctrl Pts',(48.1180371737479,4.92023305876676,6.25306617747529));
#50057=CARTESIAN_POINT('Ctrl Pts',(48.1236727259873,4.92054064178157,5.75184956235704));
#50058=CARTESIAN_POINT('Ctrl Pts',(48.1309872142257,4.92077098009341,4.87322641890403));
#50059=CARTESIAN_POINT('Ctrl Pts',(48.1369265441169,4.92033171306085,3.11310955178566));
#50060=CARTESIAN_POINT('Ctrl Pts',(48.1322764461187,4.91940466989494,1.60646990766414));
#50061=CARTESIAN_POINT('Ctrl Pts',(48.129245719316,4.91953876976763,0.547621487047117));
#50062=CARTESIAN_POINT('Ctrl Pts',(48.1288783623415,4.9195368662062,0.420854514195474));
#50063=CARTESIAN_POINT('Ctrl Pts',(48.1281131888024,4.91945090085748,0.167995994665409));
#50064=CARTESIAN_POINT('Ctrl Pts',(48.126678129514,4.91911460500282,-0.273960982828218));
#50065=CARTESIAN_POINT('Ctrl Pts',(48.1242588428073,4.91820359136341,-0.903463341764215));
#50066=CARTESIAN_POINT('Ctrl Pts',(48.1204801725179,4.91687631511617,-1.65588634714346));
#50067=CARTESIAN_POINT('Ctrl Pts',(48.1138698310929,4.91526522898741,-2.65644975655062));
#50068=CARTESIAN_POINT('Ctrl Pts',(48.1019227893584,4.91469403605023,-3.90268697487727));
#50069=CARTESIAN_POINT('Ctrl Pts',(48.0868609972421,4.91793322355432,-4.89715028181298));
#50070=CARTESIAN_POINT('Ctrl Pts',(48.0752321103946,4.92190940017826,-5.52055922497928));
#50071=CARTESIAN_POINT('Ctrl Pts',(48.0712633898345,4.92005083458062,-5.81518377909426));
#50072=CARTESIAN_POINT('Ctrl Pts',(48.0655015626684,4.90450636863208,-6.36312763586707));
#50073=CARTESIAN_POINT('Ctrl Pts',(48.0592168020764,4.85552961531939,-7.29939475139431));
#50074=CARTESIAN_POINT('Ctrl Pts',(48.0511976567384,4.76958316060189,-8.52471463285954));
#50075=CARTESIAN_POINT('Ctrl Pts',(48.0199164246137,4.75932888021026,-9.61059960005426));
#50076=CARTESIAN_POINT('Ctrl Pts',(47.9752816089115,4.82181429860099,-10.2929408967411));
#50077=CARTESIAN_POINT('Ctrl Pts',(47.9424979225489,4.87987419509223,-10.6643694086282));
#50078=CARTESIAN_POINT('Ctrl Pts',(47.9236288796491,4.91691909256987,-10.8445900060882));
#50079=CARTESIAN_POINT('Ctrl Pts',(47.9084971204255,4.94799809250737,-10.9784412427892));
#50080=CARTESIAN_POINT('Ctrl Pts',(47.8976355795159,4.96884528601334,-11.0610698453323));
#50081=CARTESIAN_POINT('Ctrl Pts',(47.8727229773347,5.01818225658932,-11.2371677963152));
#50082=CARTESIAN_POINT('Ctrl Pts',(47.8218781901417,5.12167551518096,-11.5580728652217));
#50083=CARTESIAN_POINT('Ctrl Pts',(47.6967732133967,5.39744374854651,-12.2606177190604));
#50084=CARTESIAN_POINT('Ctrl Pts',(47.4805558259505,5.96971223774114,-13.4089363387501));
#50085=CARTESIAN_POINT('Ctrl Pts',(47.2864638625924,6.59347980095187,-14.5733310719199));
#50086=CARTESIAN_POINT('Ctrl Pts',(47.1773736182701,7.00141160295155,-15.4007988051126));
#50087=CARTESIAN_POINT('Ctrl Pts',(47.1122976380426,7.26794126587674,-15.9669900830333));
#50088=CARTESIAN_POINT('Ctrl Pts',(47.0741237010702,7.45793602346966,-16.4088688151826));
#50089=CARTESIAN_POINT('Ctrl Pts',(47.0518022747637,7.6058210314354,-16.7857958495628));
#50090=CARTESIAN_POINT('Ctrl Pts',(47.0489742060024,7.65345793122167,-16.9020873872941));
#50091=CARTESIAN_POINT('Ctrl Pts',(47.043384940024,7.7572671761431,-17.154408557878));
#50092=CARTESIAN_POINT('Ctrl Pts',(47.0433955158451,7.86100386175213,-17.4003654293072));
#50093=CARTESIAN_POINT('Ctrl Pts',(47.0469238435683,7.96774815158817,-17.6512767660494));
#50094=CARTESIAN_POINT('Ctrl Pts',(47.0509092928993,8.0347187919395,-17.8077901965876));
#50095=CARTESIAN_POINT('Ctrl Pts',(47.0549903822185,8.08864548775169,-17.9336983160115));
#50096=CARTESIAN_POINT('Ctrl Pts',(47.0585259276304,8.12915788199319,-18.0282424756206));
#50097=CARTESIAN_POINT('Ctrl Pts',(47.0618417665668,8.16298950947656,-18.1072348211177));
#50098=CARTESIAN_POINT('Ctrl Pts',(47.0647166611982,8.1900763342476,-18.1705263139997));
#50099=CARTESIAN_POINT('Ctrl Pts',(47.0903610767103,8.42040249669643,-18.7091546133712));
#50100=CARTESIAN_POINT('Ctrl Pts',(47.1782761053397,8.86342262799073,-19.7591085302407));
#50101=CARTESIAN_POINT('Ctrl Pts',(47.3622945182627,9.42369471265307,-21.4015509469075));
#50102=CARTESIAN_POINT('Ctrl Pts',(47.4614748893442,9.67809115965601,-22.556175004692));
#50103=CARTESIAN_POINT('Ctrl Pts',(47.4939758264104,9.79163368355877,-23.2884768894686));
#50104=CARTESIAN_POINT('Ctrl Pts',(47.5058241833002,9.83393921132415,-23.5903433667823));
#50105=CARTESIAN_POINT('Ctrl Pts',(47.527080293437,9.89432197909471,-24.1776719661128));
#50106=CARTESIAN_POINT('Ctrl Pts',(47.5570667969751,9.95034896451951,-25.1861886156599));
#50107=CARTESIAN_POINT('Ctrl Pts',(47.5813189919887,9.92692150286911,-26.5544701327999));
#50108=CARTESIAN_POINT('Ctrl Pts',(47.5907919954819,9.84487695116789,-28.0872067810766));
#50109=CARTESIAN_POINT('Ctrl Pts',(47.5895961217043,9.81034388656042,-29.0326355854953));
#50110=CARTESIAN_POINT('Ctrl Pts',(47.5878944989112,9.8094997328447,-29.543045756842));
#50111=CARTESIAN_POINT('Ctrl Pts',(47.5872811789768,9.80921610815855,-29.6731667034628));
#50112=CARTESIAN_POINT('Ctrl Pts',(47.5853766864156,9.80848681579351,-29.9239474618171));
#50113=CARTESIAN_POINT('Ctrl Pts',(47.5802903111877,9.80670231759085,-30.3674344249167));
#50114=CARTESIAN_POINT('Ctrl Pts',(47.5640056156477,9.80132977906479,-31.2501910378675));
#50115=CARTESIAN_POINT('Ctrl Pts',(47.5279973552059,9.78911979854965,-32.510888638707));
#50116=CARTESIAN_POINT('Ctrl Pts',(47.4878923241183,9.77377649988443,-33.7647088759262));
#50117=CARTESIAN_POINT('Ctrl Pts',(47.4612495425572,9.76236532583633,-34.7634274753251));
#50118=CARTESIAN_POINT('Ctrl Pts',(47.4510763748714,9.75745732390579,-35.2610383747428));
#50119=CARTESIAN_POINT('Ctrl Pts',(47.4451123721182,9.75431432208389,-35.6345701057286));
#50120=CARTESIAN_POINT('Ctrl Pts',(47.4413196822235,9.75228836524071,-35.8865342472504));
#50121=CARTESIAN_POINT('Ctrl Pts',(47.4344830515908,9.74825789205966,-36.388694212146));
#50122=CARTESIAN_POINT('Ctrl Pts',(47.4242868162918,9.74134624202967,-37.2664093733548));
#50123=CARTESIAN_POINT('Ctrl Pts',(47.4098208967714,9.72862251883125,-39.01646234273));
#50124=CARTESIAN_POINT('Ctrl Pts',(47.4029054140399,9.72041099201589,-40.5149166685421));
#50125=CARTESIAN_POINT('Ctrl Pts',(47.3954184588552,9.71639541728355,-41.7677554829351));
#50126=CARTESIAN_POINT('Ctrl Pts',(47.3928919742263,9.71475439976693,-42.1459791643895));
#50127=CARTESIAN_POINT('Ctrl Pts',(47.3892407582933,9.71214425217703,-42.6477286125353));
#50128=CARTESIAN_POINT('Ctrl Pts',(47.3854959843847,9.70939409226986,-43.1497036668692));
#50129=CARTESIAN_POINT('Ctrl Pts',(47.3808428311234,9.70599285160254,-43.7761834401676));
#50130=CARTESIAN_POINT('Ctrl Pts',(47.3759290165794,9.70289100421383,-44.5263946243753));
#50131=CARTESIAN_POINT('Ctrl Pts',(47.3729163064396,9.70188685186302,-45.1496679134366));
#50132=CARTESIAN_POINT('Ctrl Pts',(47.3714890385956,9.70250109054733,-45.6469583727039));
#50133=CARTESIAN_POINT('Ctrl Pts',(47.3709808369827,9.70377682246791,-46.0191617072633));
#50134=CARTESIAN_POINT('Ctrl Pts',(47.3711155244775,9.70598203671017,-46.3905676980616));
#50135=CARTESIAN_POINT('Ctrl Pts',(47.3722619960134,9.71030876625392,-46.8845459369719));
#50136=CARTESIAN_POINT('Ctrl Pts',(47.3743161765341,9.71528383058321,-47.2537195147694));
#50137=CARTESIAN_POINT('Ctrl Pts',(47.3773474890592,9.72163710347664,-47.6222653452682));
#50138=CARTESIAN_POINT('Ctrl Pts',(47.3796952654116,9.72714144142203,-47.8557565540428));
#50139=CARTESIAN_POINT('Ctrl Pts',(47.3853842139194,9.74340970086942,-48.335995883122));
#50140=CARTESIAN_POINT('Ctrl Pts',(47.3977916480236,9.78303804553009,-49.185160534592));
#50141=CARTESIAN_POINT('Ctrl Pts',(47.4212746322405,9.85897715801594,-50.4376674203479));
#50142=CARTESIAN_POINT('Ctrl Pts',(47.4556152568079,9.93497304216505,-51.9969760966932));
#50143=CARTESIAN_POINT('Ctrl Pts',(47.4811676044814,9.94145679742741,-53.0756574316043));
#50144=CARTESIAN_POINT('Ctrl Pts',(47.4976840347983,9.91961192914167,-53.7643743698396));
#50145=CARTESIAN_POINT('Ctrl Pts',(47.5049960739062,9.90437362808324,-54.069643578578));
#50146=CARTESIAN_POINT('Ctrl Pts',(47.5212002501635,9.85692668755594,-54.6481425932325));
#50147=CARTESIAN_POINT('Ctrl Pts',(47.5528019510802,9.73903591069576,-55.6302471286004));
#50148=CARTESIAN_POINT('Ctrl Pts',(47.6217691433342,9.43396909243672,-57.4389214989051));
#50149=CARTESIAN_POINT('Ctrl Pts',(47.6715736591803,9.27964416172965,-58.7268771422535));
#50150=CARTESIAN_POINT('Ctrl Pts',(47.6929289382822,9.32914414065638,-59.4924758815156));
#50151=CARTESIAN_POINT('Ctrl Pts',(47.6953084223224,9.33706414622836,-59.6060262207789));
#50152=CARTESIAN_POINT('Ctrl Pts',(47.6997399955762,9.35525736429222,-59.8224955049814));
#50153=CARTESIAN_POINT('Ctrl Pts',(47.7064814914924,9.39520989700813,-60.2091296542782));
#50154=CARTESIAN_POINT('Ctrl Pts',(47.7164083821879,9.50508439961949,-60.9858984347427));
#50155=CARTESIAN_POINT('Ctrl Pts',(47.7212347723481,9.69553200767656,-61.8916620069962));
#50156=CARTESIAN_POINT('Ctrl Pts',(47.7229811173075,9.94053973412928,-62.8062931149944));
#50157=CARTESIAN_POINT('Ctrl Pts',(47.7234538904886,10.0966356011433,-63.3236293982551));
#50158=CARTESIAN_POINT('Ctrl Pts',(47.7238251783761,10.2073953196583,-63.6690819228632));
#50159=CARTESIAN_POINT('Ctrl Pts',(47.7241044339201,10.2829556096916,-63.8995499207142));
#50160=CARTESIAN_POINT('Ctrl Pts',(47.7244634116366,10.3609734614794,-64.1300807060567));
#50161=CARTESIAN_POINT('Ctrl Pts',(47.7248880865451,10.4312491867597,-64.3319116549294));
#50162=CARTESIAN_POINT('Ctrl Pts',(47.7251694617457,10.471954805787,-64.4472559420996));
#50163=CARTESIAN_POINT('Ctrl Pts',(47.7256344500065,10.5335378042138,-64.6202526824162));
#50164=CARTESIAN_POINT('Ctrl Pts',(47.7261158818515,10.5859602740694,-64.7644468421099));
#50165=CARTESIAN_POINT('Ctrl Pts',(47.7270972701321,10.6738182258527,-65.0024966791782));
#50166=CARTESIAN_POINT('Ctrl Pts',(47.7292412577957,10.7564493085798,-65.2153400389283));
#50167=CARTESIAN_POINT('Ctrl Pts',(47.7324899373616,10.9453278605935,-65.6650772708215));
#50168=CARTESIAN_POINT('Ctrl Pts',(47.7374964661587,11.3131995151145,-66.4543190474403));
#50169=CARTESIAN_POINT('Ctrl Pts',(47.7426980816088,12.1924759235898,-68.0930375920078));
#50170=CARTESIAN_POINT('Ctrl Pts',(47.7397237287679,13.0906640581855,-69.587602268803));
#50171=CARTESIAN_POINT('Ctrl Pts',(47.7358536354079,13.7226246763649,-70.7892368292671));
#50172=CARTESIAN_POINT('Ctrl Pts',(47.7361736204316,13.8514600454724,-71.0337711059821));
#50173=CARTESIAN_POINT('Ctrl Pts',(47.7361291960693,14.1168018249454,-71.536283784416));
#50174=CARTESIAN_POINT('Ctrl Pts',(47.7363418421861,14.4467634673457,-72.158998942125));
#50175=CARTESIAN_POINT('Ctrl Pts',(47.7364213613972,14.8458003853794,-72.9096754717041));
#50176=CARTESIAN_POINT('Ctrl Pts',(47.7366172482031,15.6452858065704,-74.4101476191509));
#50177=CARTESIAN_POINT('Ctrl Pts',(47.7366332425202,16.315198688152,-75.662993732331));
#50178=CARTESIAN_POINT('Ctrl Pts',(47.7364484008569,17.2869467086366,-77.4904063862681));
#50179=CARTESIAN_POINT('Ctrl Pts',(47.7365301978728,17.7226365160067,-78.3096957673099));
#50180=CARTESIAN_POINT('Ctrl Pts',(47.7365301978729,18.1591581033962,-79.1306734694082));
#50181=CARTESIAN_POINT('Ctrl Pts',(50.4917922817391,5.17568235489026,24.8304882420805));
#50182=CARTESIAN_POINT('Ctrl Pts',(50.4919463673591,5.17569630217301,24.7816042480269));
#50183=CARTESIAN_POINT('Ctrl Pts',(50.4921079653614,5.17571093355396,24.7327213068017));
#50184=CARTESIAN_POINT('Ctrl Pts',(50.49401610954,5.17588375084432,24.1820554369562));
#50185=CARTESIAN_POINT('Ctrl Pts',(50.4955757902885,5.17595412085274,23.1778367254635));
#50186=CARTESIAN_POINT('Ctrl Pts',(50.4992711998872,5.17607766572335,21.1691325217455));
#50187=CARTESIAN_POINT('Ctrl Pts',(50.5119648081948,5.17722942219756,19.6648866682171));
#50188=CARTESIAN_POINT('Ctrl Pts',(50.5384011514674,5.17998292067282,18.413787630287));
#50189=CARTESIAN_POINT('Ctrl Pts',(50.5511164369398,5.18126936488514,17.910627519419));
#50190=CARTESIAN_POINT('Ctrl Pts',(50.5831063438728,5.18443886028894,16.9063830670091));
#50191=CARTESIAN_POINT('Ctrl Pts',(50.6516956130457,5.19124688005388,15.1526043614716));
#50192=CARTESIAN_POINT('Ctrl Pts',(50.7162903435254,5.19817646025032,13.6518036614801));
#50193=CARTESIAN_POINT('Ctrl Pts',(50.7557685599339,5.20338627675366,12.3986765425074));
#50194=CARTESIAN_POINT('Ctrl Pts',(50.7718008519029,5.20561383787571,11.8982690533153));
#50195=CARTESIAN_POINT('Ctrl Pts',(50.8041363870134,5.21047180505797,10.8972275154556));
#50196=CARTESIAN_POINT('Ctrl Pts',(50.8435837667984,5.21693603644432,9.64510071597907));
#50197=CARTESIAN_POINT('Ctrl Pts',(50.8846203402977,5.22422122892856,8.14041717856539));
#50198=CARTESIAN_POINT('Ctrl Pts',(50.9046159556434,5.22799629709726,7.13495554102581));
#50199=CARTESIAN_POINT('Ctrl Pts',(50.9138114954878,5.22978915534201,6.50646180185706));
#50200=CARTESIAN_POINT('Ctrl Pts',(50.9171497614407,5.23049291660771,6.25664748473695));
#50201=CARTESIAN_POINT('Ctrl Pts',(50.9226288259833,5.23185331422438,5.75587063687534));
#50202=CARTESIAN_POINT('Ctrl Pts',(50.9293284936965,5.23406903617317,4.87782255222184));
#50203=CARTESIAN_POINT('Ctrl Pts',(50.9331844612803,5.23762107699015,3.11689522340721));
#50204=CARTESIAN_POINT('Ctrl Pts',(50.9270757237267,5.23819298900028,1.60668800491269));
#50205=CARTESIAN_POINT('Ctrl Pts',(50.9248587722347,5.23662161216685,0.543497413880909));
#50206=CARTESIAN_POINT('Ctrl Pts',(50.9246333912762,5.23632273157213,0.414409441866805));
#50207=CARTESIAN_POINT('Ctrl Pts',(50.9243176736549,5.23531986251075,0.158287120738933));
#50208=CARTESIAN_POINT('Ctrl Pts',(50.9240633982016,5.23260278305952,-0.289084873984695));
#50209=CARTESIAN_POINT('Ctrl Pts',(50.924236551002,5.22653184322983,-0.923623408987164));
#50210=CARTESIAN_POINT('Ctrl Pts',(50.9242820186088,5.21760812954524,-1.6783329718768));
#50211=CARTESIAN_POINT('Ctrl Pts',(50.9227938318951,5.20583640270268,-2.67667968195561));
#50212=CARTESIAN_POINT('Ctrl Pts',(50.9155087270415,5.19591695372494,-3.91037106297294));
#50213=CARTESIAN_POINT('Ctrl Pts',(50.8985916819313,5.20214475796566,-4.8841803612588));
#50214=CARTESIAN_POINT('Ctrl Pts',(50.8828868788886,5.21330954430444,-5.49180684910913));
#50215=CARTESIAN_POINT('Ctrl Pts',(50.8764673354544,5.215033553012,-5.78755078053324));
#50216=CARTESIAN_POINT('Ctrl Pts',(50.8633859905258,5.20611621322098,-6.33245979971984));
#50217=CARTESIAN_POINT('Ctrl Pts',(50.8389770566919,5.16928155482403,-7.26301720700937));
#50218=CARTESIAN_POINT('Ctrl Pts',(50.7964827697425,5.10491128967598,-8.47107721615394));
#50219=CARTESIAN_POINT('Ctrl Pts',(50.7377218755804,5.12502850707293,-9.52925017206961));
#50220=CARTESIAN_POINT('Ctrl Pts',(50.6901697495722,5.2137233758942,-10.1916827055123));
#50221=CARTESIAN_POINT('Ctrl Pts',(50.662118172762,5.28912141861767,-10.5536869186764));
#50222=CARTESIAN_POINT('Ctrl Pts',(50.6478921279656,5.33596910600582,-10.7302411105224));
#50223=CARTESIAN_POINT('Ctrl Pts',(50.6371826404424,5.37485343867045,-10.8614554100438));
#50224=CARTESIAN_POINT('Ctrl Pts',(50.6307159721729,5.39705801614812,-10.9310818960025));
#50225=CARTESIAN_POINT('Ctrl Pts',(50.6154401332022,5.45490626609664,-11.0921354556276));
#50226=CARTESIAN_POINT('Ctrl Pts',(50.5846981114416,5.58090977361102,-11.3924344636096));
#50227=CARTESIAN_POINT('Ctrl Pts',(50.5066630577099,5.94058212465662,-12.0842817249592));
#50228=CARTESIAN_POINT('Ctrl Pts',(50.3578490121105,6.71358458556874,-13.2416724689023));
#50229=CARTESIAN_POINT('Ctrl Pts',(50.2065835518162,7.53232603473581,-14.4259820552415));
#50230=CARTESIAN_POINT('Ctrl Pts',(50.1139611608556,8.04584711163632,-15.2949612559555));
#50231=CARTESIAN_POINT('Ctrl Pts',(50.0564719102312,8.37311379279236,-15.900095054076));
#50232=CARTESIAN_POINT('Ctrl Pts',(50.0201438075105,8.59438581664167,-16.3873359291976));
#50233=CARTESIAN_POINT('Ctrl Pts',(49.9978240510594,8.75337087316149,-16.8152614588801));
#50234=CARTESIAN_POINT('Ctrl Pts',(49.9932719239137,8.80394733204392,-16.9530270287384));
#50235=CARTESIAN_POINT('Ctrl Pts',(49.9851495296652,8.90696100792097,-17.2462322364938));
#50236=CARTESIAN_POINT('Ctrl Pts',(49.9821302379449,9.00073505208439,-17.5314704398829));
#50237=CARTESIAN_POINT('Ctrl Pts',(49.9826393962094,9.08938550147516,-17.819049666724));
#50238=CARTESIAN_POINT('Ctrl Pts',(49.9845954418485,9.14189286236218,-17.9974335107659));
#50239=CARTESIAN_POINT('Ctrl Pts',(49.9869978917432,9.18249029971152,-18.1401049509871));
#50240=CARTESIAN_POINT('Ctrl Pts',(49.9892307552561,9.21215923530497,-18.2468571894993));
#50241=CARTESIAN_POINT('Ctrl Pts',(49.9914268319859,9.23627677705772,-18.3357024376677));
#50242=CARTESIAN_POINT('Ctrl Pts',(49.9933821403262,9.25520325252199,-18.4066777428617));
#50243=CARTESIAN_POINT('Ctrl Pts',(50.0110680129098,9.41401883658551,-19.0094610531942));
#50244=CARTESIAN_POINT('Ctrl Pts',(50.0792682289136,9.65255491121305,-20.1462575189252));
#50245=CARTESIAN_POINT('Ctrl Pts',(50.2091332895172,9.86433688529703,-21.7595264968037));
#50246=CARTESIAN_POINT('Ctrl Pts',(50.2674574528492,9.95568369829372,-22.7869865090925));
#50247=CARTESIAN_POINT('Ctrl Pts',(50.2825760832839,10.0117450467348,-23.4161246816041));
#50248=CARTESIAN_POINT('Ctrl Pts',(50.2875272443829,10.0339899843054,-23.705844706264));
#50249=CARTESIAN_POINT('Ctrl Pts',(50.2950269110892,10.0637741588356,-24.2559959869773));
#50250=CARTESIAN_POINT('Ctrl Pts',(50.3019274865117,10.0876891524349,-25.2161934049187));
#50251=CARTESIAN_POINT('Ctrl Pts',(50.297668864508,10.060160953794,-26.5368336469249));
#50252=CARTESIAN_POINT('Ctrl Pts',(50.2806400399388,9.99541428276367,-28.051138637435));
#50253=CARTESIAN_POINT('Ctrl Pts',(50.2704192293568,9.97068968221786,-29.0068078119763));
#50254=CARTESIAN_POINT('Ctrl Pts',(50.2680902577453,9.97170400042531,-29.5297903668874));
#50255=CARTESIAN_POINT('Ctrl Pts',(50.2675633128472,9.97203436851492,-29.6556098830141));
#50256=CARTESIAN_POINT('Ctrl Pts',(50.266354914397,9.97294138056059,-29.9020947112043));
#50257=CARTESIAN_POINT('Ctrl Pts',(50.2639105114052,9.9752324211205,-30.3367763830376));
#50258=CARTESIAN_POINT('Ctrl Pts',(50.2578839994032,9.98226236368177,-31.206406783758));
#50259=CARTESIAN_POINT('Ctrl Pts',(50.2473409278746,9.99796157371762,-32.4559954984309));
#50260=CARTESIAN_POINT('Ctrl Pts',(50.2376092948052,10.0167119816908,-33.7110935550376));
#50261=CARTESIAN_POINT('Ctrl Pts',(50.2322499145794,10.0303674776112,-34.7178088980314));
#50262=CARTESIAN_POINT('Ctrl Pts',(50.2306931834636,10.0362754548982,-35.2218816182731));
#50263=CARTESIAN_POINT('Ctrl Pts',(50.2300612982916,10.040109748401,-35.6010456515645));
#50264=CARTESIAN_POINT('Ctrl Pts',(50.2298010525293,10.042602014251,-35.8526947068551));
#50265=CARTESIAN_POINT('Ctrl Pts',(50.2298747170317,10.0474750052036,-36.356536925899));
#50266=CARTESIAN_POINT('Ctrl Pts',(50.2313887377468,10.0557642612372,-37.2361004289692));
#50267=CARTESIAN_POINT('Ctrl Pts',(50.2385455068631,10.0711028262601,-38.9908386578714));
#50268=CARTESIAN_POINT('Ctrl Pts',(50.2469303887032,10.0828908266136,-40.4936351840155));
#50269=CARTESIAN_POINT('Ctrl Pts',(50.2497861673699,10.0921244140975,-41.7505068669631));
#50270=CARTESIAN_POINT('Ctrl Pts',(50.2502702105738,10.0943027208078,-42.1293448835941));
#50271=CARTESIAN_POINT('Ctrl Pts',(50.2504294326418,10.0964052575757,-42.6323665495166));
#50272=CARTESIAN_POINT('Ctrl Pts',(50.250343076812,10.0981278236175,-43.1356412571861));
#50273=CARTESIAN_POINT('Ctrl Pts',(50.2499257473924,10.0997965195295,-43.7639609947201));
#50274=CARTESIAN_POINT('Ctrl Pts',(50.2494101467874,10.1017974964918,-44.5166494128688));
#50275=CARTESIAN_POINT('Ctrl Pts',(50.2493693574037,10.104099340921,-45.1422356819985));
#50276=CARTESIAN_POINT('Ctrl Pts',(50.249809185912,10.1066909341734,-45.6414808722959));
#50277=CARTESIAN_POINT('Ctrl Pts',(50.2504362280452,10.1091078188008,-46.0152243453922));
#50278=CARTESIAN_POINT('Ctrl Pts',(50.2514206232568,10.1120908343596,-46.3882409659662));
#50279=CARTESIAN_POINT('Ctrl Pts',(50.2532886632006,10.116950507721,-46.8844528098358));
#50280=CARTESIAN_POINT('Ctrl Pts',(50.25540923241,10.1217198984019,-47.2554383503514));
#50281=CARTESIAN_POINT('Ctrl Pts',(50.2581326010481,10.1274453409439,-47.6258728234225));
#50282=CARTESIAN_POINT('Ctrl Pts',(50.260107818025,10.1323681022638,-47.8613165863601));
#50283=CARTESIAN_POINT('Ctrl Pts',(50.2645300652927,10.1467153951326,-48.3447111522187));
#50284=CARTESIAN_POINT('Ctrl Pts',(50.2734586190813,10.1812210666923,-49.1988048899799));
#50285=CARTESIAN_POINT('Ctrl Pts',(50.289096735195,10.2454476087941,-50.4559708789396));
#50286=CARTESIAN_POINT('Ctrl Pts',(50.3113907758592,10.303771222499,-52.0172078681521));
#50287=CARTESIAN_POINT('Ctrl Pts',(50.3281951747258,10.2982140031211,-53.0944242249086));
#50288=CARTESIAN_POINT('Ctrl Pts',(50.3393348837964,10.2697154417897,-53.7813599592998));
#50289=CARTESIAN_POINT('Ctrl Pts',(50.3443475620727,10.2513279326554,-54.0881085257841));
#50290=CARTESIAN_POINT('Ctrl Pts',(50.3553654244131,10.1974224725376,-54.6678121480108));
#50291=CARTESIAN_POINT('Ctrl Pts',(50.3766105335714,10.0676138959923,-55.6516135370779));
#50292=CARTESIAN_POINT('Ctrl Pts',(50.422106002006,9.73901083306247,-57.4599799614481));
#50293=CARTESIAN_POINT('Ctrl Pts',(50.4518300690914,9.57152298929059,-58.7435487630709));
#50294=CARTESIAN_POINT('Ctrl Pts',(50.4673832424493,9.61678452934807,-59.5016760542654));
#50295=CARTESIAN_POINT('Ctrl Pts',(50.4691068208339,9.62413422649098,-59.6143692132953));
#50296=CARTESIAN_POINT('Ctrl Pts',(50.4724291890576,9.64137717775314,-59.8291956689248));
#50297=CARTESIAN_POINT('Ctrl Pts',(50.4777228802664,9.67998341820928,-60.2131942201998));
#50298=CARTESIAN_POINT('Ctrl Pts',(50.4865192303076,9.78848071124649,-60.9856468420894));
#50299=CARTESIAN_POINT('Ctrl Pts',(50.4930473652507,9.97985667703256,-61.8886735318654));
#50300=CARTESIAN_POINT('Ctrl Pts',(50.4975022393909,10.2272159581485,-62.8025747644526));
#50301=CARTESIAN_POINT('Ctrl Pts',(50.4995370799862,10.3849065774803,-63.3202082920092));
#50302=CARTESIAN_POINT('Ctrl Pts',(50.5008259755392,10.4967281288771,-63.6661400994148));
#50303=CARTESIAN_POINT('Ctrl Pts',(50.5016757912382,10.5729894359012,-63.8970034947931));
#50304=CARTESIAN_POINT('Ctrl Pts',(50.5025302150233,10.6516802926323,-64.1280375685076));
#50305=CARTESIAN_POINT('Ctrl Pts',(50.5032997606616,10.7225048544593,-64.3304078852364));
#50306=CARTESIAN_POINT('Ctrl Pts',(50.5037496849033,10.7635089449926,-64.4460882768762));
#50307=CARTESIAN_POINT('Ctrl Pts',(50.5044376473356,10.8255229325307,-64.6196163397289));
#50308=CARTESIAN_POINT('Ctrl Pts',(50.5050386966279,10.8782661361981,-64.7643128204007));
#50309=CARTESIAN_POINT('Ctrl Pts',(50.5061186304834,10.9665827412417,-65.0032530382309));
#50310=CARTESIAN_POINT('Ctrl Pts',(50.5086173349253,11.0493399786139,-65.2159941551862));
#50311=CARTESIAN_POINT('Ctrl Pts',(50.5123997427753,11.2386175512069,-65.6660613795346));
#50312=CARTESIAN_POINT('Ctrl Pts',(50.5183140141763,11.6069672647648,-66.4554986583973));
#50313=CARTESIAN_POINT('Ctrl Pts',(50.5247445762517,12.4868156446073,-68.0945711191323));
#50314=CARTESIAN_POINT('Ctrl Pts',(50.5217226319143,13.3848139405268,-69.5890289196084));
#50315=CARTESIAN_POINT('Ctrl Pts',(50.5172916352365,14.0166193126202,-70.7904864793872));
#50316=CARTESIAN_POINT('Ctrl Pts',(50.5176801339045,14.1454947301235,-71.0350483232966));
#50317=CARTESIAN_POINT('Ctrl Pts',(50.5176510909301,14.4108641406723,-71.5375759377691));
#50318=CARTESIAN_POINT('Ctrl Pts',(50.5179137443909,14.7408610844172,-72.1603179590527));
#50319=CARTESIAN_POINT('Ctrl Pts',(50.5180070923177,15.1399124031108,-72.9110139550441));
#50320=CARTESIAN_POINT('Ctrl Pts',(50.5182133876732,15.9394012467424,-74.4115156055686));
#50321=CARTESIAN_POINT('Ctrl Pts',(50.5181871982642,16.6092606723113,-75.6643418622959));
#50322=CARTESIAN_POINT('Ctrl Pts',(50.5179743581026,17.5809735969016,-77.4917026704339));
#50323=CARTESIAN_POINT('Ctrl Pts',(50.5180692026081,18.0166713543046,-78.3110028352501));
#50324=CARTESIAN_POINT('Ctrl Pts',(50.5180692026081,18.4531929416941,-79.1319805373485));
#50325=CARTESIAN_POINT('Ctrl Pts',(53.2695150563835,5.51412939726847,24.8304328418027));
#50326=CARTESIAN_POINT('Ctrl Pts',(53.2696688996589,5.51414443491013,24.7815471085002));
#50327=CARTESIAN_POINT('Ctrl Pts',(53.2698302575749,5.51416021237113,24.7326624174752));
#50328=CARTESIAN_POINT('Ctrl Pts',(53.2717355537201,5.51434666388,24.1819755549638));
#50329=CARTESIAN_POINT('Ctrl Pts',(53.2731190076681,5.51436686877321,23.1777004112197));
#50330=CARTESIAN_POINT('Ctrl Pts',(53.2762916814244,5.51433243053149,21.1689727072072));
#50331=CARTESIAN_POINT('Ctrl Pts',(53.2889745454163,5.51557857626836,19.6647602554609));
#50332=CARTESIAN_POINT('Ctrl Pts',(53.3162554220489,5.51883379753054,18.4137109770533));
#50333=CARTESIAN_POINT('Ctrl Pts',(53.3292888081772,5.52036031567856,17.9105682256386));
#50334=CARTESIAN_POINT('Ctrl Pts',(53.3619273956867,5.5241382069799,16.906316579728));
#50335=CARTESIAN_POINT('Ctrl Pts',(53.4319377194389,5.53228173032549,15.1524341677222));
#50336=CARTESIAN_POINT('Ctrl Pts',(53.4991258124589,5.54061652432534,13.6515381980859));
#50337=CARTESIAN_POINT('Ctrl Pts',(53.542473052396,5.54691456357747,12.3983966193952));
#50338=CARTESIAN_POINT('Ctrl Pts',(53.5603356607081,5.54961471051331,11.8979916029755));
#50339=CARTESIAN_POINT('Ctrl Pts',(53.5972024234654,5.55551879936049,10.897002135347));
#50340=CARTESIAN_POINT('Ctrl Pts',(53.6434512927629,5.56339708348542,9.64498895261323));
#50341=CARTESIAN_POINT('Ctrl Pts',(53.6928466346801,5.57224995798774,8.14041909589305));
#50342=CARTESIAN_POINT('Ctrl Pts',(53.7174864608606,5.57681098769189,7.13493855585078));
#50343=CARTESIAN_POINT('Ctrl Pts',(53.7289543784969,5.57895594316898,6.50639606605512));
#50344=CARTESIAN_POINT('Ctrl Pts',(53.7332399397066,5.57979684436249,6.25649768591037));
#50345=CARTESIAN_POINT('Ctrl Pts',(53.7407452387018,5.58140432867308,5.75560963473447));
#50346=CARTESIAN_POINT('Ctrl Pts',(53.7512130755125,5.58398764420394,4.87740710564012));
#50347=CARTESIAN_POINT('Ctrl Pts',(53.7625281946993,5.58799309354047,3.11630623138076));
#50348=CARTESIAN_POINT('Ctrl Pts',(53.7593283490689,5.58854306639946,1.60645823396047));
#50349=CARTESIAN_POINT('Ctrl Pts',(53.7543081104693,5.58680996580961,0.543452997857882));
#50350=CARTESIAN_POINT('Ctrl Pts',(53.7537151315514,5.58639943788977,0.412134805246649));
#50351=CARTESIAN_POINT('Ctrl Pts',(53.7525325840066,5.58484495007707,0.153207505278396));
#50352=CARTESIAN_POINT('Ctrl Pts',(53.7504298130056,5.58039238195928,-0.298852280230459));
#50353=CARTESIAN_POINT('Ctrl Pts',(53.7470896429771,5.57016836597694,-0.937114284333558));
#50354=CARTESIAN_POINT('Ctrl Pts',(53.7417739290271,5.55522922952095,-1.69238531231437));
#50355=CARTESIAN_POINT('Ctrl Pts',(53.7319395136192,5.53612531939417,-2.68582112449248));
#50356=CARTESIAN_POINT('Ctrl Pts',(53.7125866640681,5.52212017796381,-3.90307577254729));
#50357=CARTESIAN_POINT('Ctrl Pts',(53.6857013004841,5.53767860315604,-4.85280065205426));
#50358=CARTESIAN_POINT('Ctrl Pts',(53.6641830043257,5.56063240290011,-5.4420691309824));
#50359=CARTESIAN_POINT('Ctrl Pts',(53.6548139721549,5.56923331041967,-5.72862576373523));
#50360=CARTESIAN_POINT('Ctrl Pts',(53.6345170377436,5.57633161305388,-6.25852599704844));
#50361=CARTESIAN_POINT('Ctrl Pts',(53.5945971078396,5.57376225487845,-7.16757755734756));
#50362=CARTESIAN_POINT('Ctrl Pts',(53.5267535273497,5.56521492908129,-8.35957486081496));
#50363=CARTESIAN_POINT('Ctrl Pts',(53.4528066784746,5.63535903843469,-9.42461767107299));
#50364=CARTESIAN_POINT('Ctrl Pts',(53.4063264448625,5.75708558941193,-10.1070935533807));
#50365=CARTESIAN_POINT('Ctrl Pts',(53.3825855207646,5.85168431987466,-10.4839013761504));
#50366=CARTESIAN_POINT('Ctrl Pts',(53.3717711260772,5.9082780831659,-10.668762921667));
#50367=CARTESIAN_POINT('Ctrl Pts',(53.3641296138183,5.95448120662286,-10.8062514828049));
#50368=CARTESIAN_POINT('Ctrl Pts',(53.3609415101037,5.97947895554171,-10.8749525154684));
#50369=CARTESIAN_POINT('Ctrl Pts',(53.3525810895759,6.04538013200624,-11.037626473064));
#50370=CARTESIAN_POINT('Ctrl Pts',(53.3360567052155,6.18737340870044,-11.3401483424015));
#50371=CARTESIAN_POINT('Ctrl Pts',(53.2907506871901,6.5872514651254,-12.038539433205));
#50372=CARTESIAN_POINT('Ctrl Pts',(53.1925941608831,7.4250140432066,-13.204191553958));
#50373=CARTESIAN_POINT('Ctrl Pts',(53.0844762977564,8.2944695138769,-14.3991185169526));
#50374=CARTESIAN_POINT('Ctrl Pts',(53.0153923437052,8.83248777688499,-15.2830661152328));
#50375=CARTESIAN_POINT('Ctrl Pts',(52.9713518406644,9.17256455491026,-15.9017788862587));
#50376=CARTESIAN_POINT('Ctrl Pts',(52.9418943846209,9.3983203173646,-16.404501877126));
#50377=CARTESIAN_POINT('Ctrl Pts',(52.9220952320653,9.55509675497589,-16.8497512860891));
#50378=CARTESIAN_POINT('Ctrl Pts',(52.9170744783204,9.60547714751073,-16.9975381492885));
#50379=CARTESIAN_POINT('Ctrl Pts',(52.9076225110184,9.70397423114619,-17.3085087168662));
#50380=CARTESIAN_POINT('Ctrl Pts',(52.9014675276002,9.78896003877269,-17.6113587023661));
#50381=CARTESIAN_POINT('Ctrl Pts',(52.8975565743096,9.86463741111705,-17.9149028633213));
#50382=CARTESIAN_POINT('Ctrl Pts',(52.8961535288958,9.90755567793999,-18.1027394279948));
#50383=CARTESIAN_POINT('Ctrl Pts',(52.8955575391207,9.93964041294108,-18.2525370193699));
#50384=CARTESIAN_POINT('Ctrl Pts',(52.8953805694132,9.96253980574399,-18.3644296399647));
#50385=CARTESIAN_POINT('Ctrl Pts',(52.8954426432911,9.98071066858224,-18.4573752883049));
#50386=CARTESIAN_POINT('Ctrl Pts',(52.8956146345115,9.99470785692181,-18.5315144188974));
#50387=CARTESIAN_POINT('Ctrl Pts',(52.8977576515523,10.1107050642191,-19.1606209446941));
#50388=CARTESIAN_POINT('Ctrl Pts',(52.9225110046152,10.2395131612953,-20.3255595047088));
#50389=CARTESIAN_POINT('Ctrl Pts',(52.9776218232643,10.3008802158238,-21.9155284337944));
#50390=CARTESIAN_POINT('Ctrl Pts',(53.0035666335813,10.3301100096998,-22.889124084334));
#50391=CARTESIAN_POINT('Ctrl Pts',(53.0091514507972,10.3629588112806,-23.4703857380265));
#50392=CARTESIAN_POINT('Ctrl Pts',(53.0104509066303,10.376737772715,-23.7499115442637));
#50393=CARTESIAN_POINT('Ctrl Pts',(53.0116951558073,10.3951370917517,-24.2773902817673));
#50394=CARTESIAN_POINT('Ctrl Pts',(53.0098989792996,10.4107927229111,-25.2064856843808));
#50395=CARTESIAN_POINT('Ctrl Pts',(52.9996437044208,10.3962853899997,-26.5001577634974));
#50396=CARTESIAN_POINT('Ctrl Pts',(52.985573495527,10.3597651429066,-28.0151589056756));
#50397=CARTESIAN_POINT('Ctrl Pts',(52.9819354673514,10.3456237566901,-28.9932105392826));
#50398=CARTESIAN_POINT('Ctrl Pts',(52.9831672495963,10.3468226651521,-29.5345252208753));
#50399=CARTESIAN_POINT('Ctrl Pts',(52.9834618339309,10.3471246017814,-29.6607033909021));
#50400=CARTESIAN_POINT('Ctrl Pts',(52.984230858734,10.3478558390306,-29.9098655917076));
#50401=CARTESIAN_POINT('Ctrl Pts',(52.9859997430256,10.3494395327631,-30.3479071016356));
#50402=CARTESIAN_POINT('Ctrl Pts',(52.9910877275921,10.3536760394939,-31.2238536192905));
#50403=CARTESIAN_POINT('Ctrl Pts',(53.0018824045189,10.3617839853935,-32.4784261786044));
#50404=CARTESIAN_POINT('Ctrl Pts',(53.0150250933224,10.3703255534356,-33.7335695625717));
#50405=CARTESIAN_POINT('Ctrl Pts',(53.0255660425261,10.3763103895585,-34.7369580744697));
#50406=CARTESIAN_POINT('Ctrl Pts',(53.0306459750937,10.3788278479069,-35.2382903705776));
#50407=CARTESIAN_POINT('Ctrl Pts',(53.0343022880532,10.3804941335955,-35.6150223923661));
#50408=CARTESIAN_POINT('Ctrl Pts',(53.0368565578212,10.3816043729998,-35.8668683882239));
#50409=CARTESIAN_POINT('Ctrl Pts',(53.0423077317458,10.3837181513364,-36.3700419506216));
#50410=CARTESIAN_POINT('Ctrl Pts',(53.0526095271317,10.3872088831648,-37.2488784517629));
#50411=CARTESIAN_POINT('Ctrl Pts',(53.0749370713191,10.3934870690784,-39.0015781343972));
#50412=CARTESIAN_POINT('Ctrl Pts',(53.0927598271231,10.3985586653117,-40.5025012708411));
#50413=CARTESIAN_POINT('Ctrl Pts',(53.1020300932996,10.4033133844909,-41.7577923907435));
#50414=CARTESIAN_POINT('Ctrl Pts',(53.1043831419616,10.4041975940086,-42.1364495264179));
#50415=CARTESIAN_POINT('Ctrl Pts',(53.1068797929176,10.4046926600718,-42.6390036081494));
#50416=CARTESIAN_POINT('Ctrl Pts',(53.1090095338086,10.4048832049801,-43.1417926508615));
#50417=CARTESIAN_POINT('Ctrl Pts',(53.1110939742423,10.4048002178397,-43.7693855463974));
#50418=CARTESIAN_POINT('Ctrl Pts',(53.1130264615959,10.4050139698953,-44.5210345694311));
#50419=CARTESIAN_POINT('Ctrl Pts',(53.1144597922811,10.4061338634531,-45.1455962156924));
#50420=CARTESIAN_POINT('Ctrl Pts',(53.1156782935419,10.4079880616497,-45.6439451432393));
#50421=CARTESIAN_POINT('Ctrl Pts',(53.1166730225603,10.4099636011234,-46.0169683327606));
#50422=CARTESIAN_POINT('Ctrl Pts',(53.1177930906092,10.4126234963977,-46.3892183421306));
#50423=CARTESIAN_POINT('Ctrl Pts',(53.1195148227816,10.4172117803271,-46.884351859571));
#50424=CARTESIAN_POINT('Ctrl Pts',(53.1211258301745,10.4219833473072,-47.2544467632722));
#50425=CARTESIAN_POINT('Ctrl Pts',(53.1230500401165,10.4278371853805,-47.6239517433574));
#50426=CARTESIAN_POINT('Ctrl Pts',(53.12436166703,10.4328837420489,-47.8585839056701));
#50427=CARTESIAN_POINT('Ctrl Pts',(53.1269691023571,10.4477019749082,-48.3406195988866));
#50428=CARTESIAN_POINT('Ctrl Pts',(53.1315663929496,10.4835510487732,-49.1926272070234));
#50429=CARTESIAN_POINT('Ctrl Pts',(53.1383655351001,10.5511152764054,-50.4478347798509));
#50430=CARTESIAN_POINT('Ctrl Pts',(53.1479873645481,10.6147793240272,-52.0081718671275));
#50431=CARTESIAN_POINT('Ctrl Pts',(53.156447028726,10.6131912573835,-53.085717286359));
#50432=CARTESIAN_POINT('Ctrl Pts',(53.1629214165293,10.5870339863162,-53.7731140291621));
#50433=CARTESIAN_POINT('Ctrl Pts',(53.1659430409037,10.569810273764,-54.0790421421878));
#50434=CARTESIAN_POINT('Ctrl Pts',(53.1727564436081,10.5183244985191,-54.6579397162002));
#50435=CARTESIAN_POINT('Ctrl Pts',(53.1861233058401,10.3930525906094,-55.6406122873643));
#50436=CARTESIAN_POINT('Ctrl Pts',(53.2151846217902,10.0735258751026,-57.4487369102697));
#50437=CARTESIAN_POINT('Ctrl Pts',(53.2321543938323,9.91029533040072,-58.7350396653802));
#50438=CARTESIAN_POINT('Ctrl Pts',(53.243740090883,9.95716979747392,-59.4978810552022));
#50439=CARTESIAN_POINT('Ctrl Pts',(53.2449955793885,9.96473625601748,-59.6110245270641));
#50440=CARTESIAN_POINT('Ctrl Pts',(53.2475290643299,9.98235390960118,-59.8267667743487));
#50441=CARTESIAN_POINT('Ctrl Pts',(53.2517715992568,10.0215218737307,-60.2122127364834));
#50442=CARTESIAN_POINT('Ctrl Pts',(53.2596750196581,10.1307331248798,-60.9870643607676));
#50443=CARTESIAN_POINT('Ctrl Pts',(53.2672475158084,10.3220678340727,-61.8916255159988));
#50444=CARTESIAN_POINT('Ctrl Pts',(53.2735156455831,10.5687928930795,-62.8059939918394));
#50445=CARTESIAN_POINT('Ctrl Pts',(53.2766296476069,10.725990345077,-63.3235215809714));
#50446=CARTESIAN_POINT('Ctrl Pts',(53.2785685614647,10.8374653545796,-63.6692431125138));
#50447=CARTESIAN_POINT('Ctrl Pts',(53.2798277969375,10.9134935847789,-63.8999288216261));
#50448=CARTESIAN_POINT('Ctrl Pts',(53.2810447796835,10.9919538773434,-64.1307332047518));
#50449=CARTESIAN_POINT('Ctrl Pts',(53.2820765328361,11.0625855046011,-64.3328556288104));
#50450=CARTESIAN_POINT('Ctrl Pts',(53.2826580617144,11.103483121932,-64.4483814182979));
#50451=CARTESIAN_POINT('Ctrl Pts',(53.2835243590464,11.1653419503189,-64.6216651084278));
#50452=CARTESIAN_POINT('Ctrl Pts',(53.2842304329407,11.2179656495935,-64.7661305998104));
#50453=CARTESIAN_POINT('Ctrl Pts',(53.2854197490363,11.3061095226125,-65.0046642293767));
#50454=CARTESIAN_POINT('Ctrl Pts',(53.2882010693798,11.3889417772137,-65.2175224478048));
#50455=CARTESIAN_POINT('Ctrl Pts',(53.2924322715541,11.5782293927932,-65.6675133191105));
#50456=CARTESIAN_POINT('Ctrl Pts',(53.2991034786861,11.9466707796868,-66.4569647096837));
#50457=CARTESIAN_POINT('Ctrl Pts',(53.3065741614853,12.8266141431145,-68.0959329977427));
#50458=CARTESIAN_POINT('Ctrl Pts',(53.3034446514179,13.7246015455025,-69.5904384484924));
#50459=CARTESIAN_POINT('Ctrl Pts',(53.298454824434,14.3562318857571,-70.7919083359163));
#50460=CARTESIAN_POINT('Ctrl Pts',(53.2989019228725,14.4851096068852,-71.0364613092679));
#50461=CARTESIAN_POINT('Ctrl Pts',(53.2988790606072,14.7504636827547,-71.5389789626792));
#50462=CARTESIAN_POINT('Ctrl Pts',(53.2991825568548,15.0804570737878,-72.1617099472991));
#50463=CARTESIAN_POINT('Ctrl Pts',(53.2992890687305,15.4795056637326,-72.9123966172817));
#50464=CARTESIAN_POINT('Ctrl Pts',(53.2995141435576,16.2790023715052,-74.4128863212949));
#50465=CARTESIAN_POINT('Ctrl Pts',(53.2994612948345,16.9488827995346,-75.665724538253));
#50466=CARTESIAN_POINT('Ctrl Pts',(53.2992163810433,17.9206005062072,-77.4931099187158));
#50467=CARTESIAN_POINT('Ctrl Pts',(53.2993229371201,18.3562984860772,-78.312405584784));
#50468=CARTESIAN_POINT('Ctrl Pts',(53.29932293712,18.7928200734667,-79.1333832868824));
#50469=CARTESIAN_POINT('Ctrl Pts',(56.0538562954074,5.89165024012153,24.8309604003465));
#50470=CARTESIAN_POINT('Ctrl Pts',(56.0540116122581,5.89167990068842,24.7820913765585));
#50471=CARTESIAN_POINT('Ctrl Pts',(56.0541745295879,5.89171100104421,24.7332236978053));
#50472=CARTESIAN_POINT('Ctrl Pts',(56.0560981536171,5.89207817320162,24.1827331219404));
#50473=CARTESIAN_POINT('Ctrl Pts',(56.0573325828393,5.89247415459224,23.1786732167898));
#50474=CARTESIAN_POINT('Ctrl Pts',(56.0600534426369,5.89347092643402,21.1703130802733));
#50475=CARTESIAN_POINT('Ctrl Pts',(56.0728655050755,5.89590937649389,19.6662395446907));
#50476=CARTESIAN_POINT('Ctrl Pts',(56.1012316964193,5.90050969960956,18.4152728983411));
#50477=CARTESIAN_POINT('Ctrl Pts',(56.1147462351096,5.90279076485921,17.9132184233166));
#50478=CARTESIAN_POINT('Ctrl Pts',(56.1485361667684,5.90865570090384,16.9097331713725));
#50479=CARTESIAN_POINT('Ctrl Pts',(56.2210741679537,5.92123378561505,15.1557059965571));
#50480=CARTESIAN_POINT('Ctrl Pts',(56.2914134914659,5.93219694281183,13.6513343348583));
#50481=CARTESIAN_POINT('Ctrl Pts',(56.3380030057963,5.93721154809562,12.3936612477077));
#50482=CARTESIAN_POINT('Ctrl Pts',(56.3573126810151,5.93905485776692,11.8914244071032));
#50483=CARTESIAN_POINT('Ctrl Pts',(56.3975338417983,5.94215013443676,10.8877608718657));
#50484=CARTESIAN_POINT('Ctrl Pts',(56.4485948421275,5.94499428155967,9.63392266712354));
#50485=CARTESIAN_POINT('Ctrl Pts',(56.5038398846024,5.94702902649836,8.12966702503623));
#50486=CARTESIAN_POINT('Ctrl Pts',(56.5318786656771,5.9476348093116,7.12601654617415));
#50487=CARTESIAN_POINT('Ctrl Pts',(56.5451175184381,5.94783223170847,6.49903193976296));
#50488=CARTESIAN_POINT('Ctrl Pts',(56.5501450376796,5.94780846348296,6.24785780611247));
#50489=CARTESIAN_POINT('Ctrl Pts',(56.559241836301,5.94742736952047,5.74592863375821));
#50490=CARTESIAN_POINT('Ctrl Pts',(56.5726916525748,5.94601618318316,4.86637215456344));
#50491=CARTESIAN_POINT('Ctrl Pts',(56.5900048654683,5.94140601423123,3.10700589583077));
#50492=CARTESIAN_POINT('Ctrl Pts',(56.5895364791801,5.93821116463739,1.60556132597426));
#50493=CARTESIAN_POINT('Ctrl Pts',(56.5830907738242,5.94004214238158,0.551599771432738));
#50494=CARTESIAN_POINT('Ctrl Pts',(56.5823266484986,5.94002565977373,0.419000497013813));
#50495=CARTESIAN_POINT('Ctrl Pts',(56.580800409802,5.93910290897433,0.159135480437789));
#50496=CARTESIAN_POINT('Ctrl Pts',(56.5780725440921,5.93545041037213,-0.294580316420769));
#50497=CARTESIAN_POINT('Ctrl Pts',(56.5736645749159,5.9259217675061,-0.932794948601504));
#50498=CARTESIAN_POINT('Ctrl Pts',(56.5665312144104,5.91241497683955,-1.68514145248478));
#50499=CARTESIAN_POINT('Ctrl Pts',(56.5531776577419,5.8974933877812,-2.67026599152044));
#50500=CARTESIAN_POINT('Ctrl Pts',(56.5268416837315,5.8955788205326,-3.8692129523913));
#50501=CARTESIAN_POINT('Ctrl Pts',(56.4905108680574,5.93209099269583,-4.7958388535266));
#50502=CARTESIAN_POINT('Ctrl Pts',(56.4617001919105,5.9726109612883,-5.36829607916485));
#50503=CARTESIAN_POINT('Ctrl Pts',(56.4486050965068,5.99077468133528,-5.63962112151592));
#50504=CARTESIAN_POINT('Ctrl Pts',(56.4191070337447,6.02059082861141,-6.14825994930089));
#50505=CARTESIAN_POINT('Ctrl Pts',(56.3591906683692,6.06666028449872,-7.02774061874815));
#50506=CARTESIAN_POINT('Ctrl Pts',(56.258052074709,6.13755199903919,-8.20747819042182));
#50507=CARTESIAN_POINT('Ctrl Pts',(56.1585914012276,6.27717374595974,-9.30110347227688));
#50508=CARTESIAN_POINT('Ctrl Pts',(56.1031552157466,6.44038894773047,-10.0253563145223));
#50509=CARTESIAN_POINT('Ctrl Pts',(56.0772042357272,6.55677929476102,-10.4300198957996));
#50510=CARTESIAN_POINT('Ctrl Pts',(56.0663272930536,6.62350555199865,-10.6297806744373));
#50511=CARTESIAN_POINT('Ctrl Pts',(56.0590858017011,6.67694705514598,-10.7785470815969));
#50512=CARTESIAN_POINT('Ctrl Pts',(56.0572086293456,6.70556680595851,-10.8519969666275));
#50513=CARTESIAN_POINT('Ctrl Pts',(56.0515097738636,6.77914116439054,-11.0244233656895));
#50514=CARTESIAN_POINT('Ctrl Pts',(56.0411420905104,6.93302431413149,-11.3403871917385));
#50515=CARTESIAN_POINT('Ctrl Pts',(56.0119010310503,7.34960202239872,-12.0564238150741));
#50516=CARTESIAN_POINT('Ctrl Pts',(55.9423555314455,8.18633570232788,-13.2319459356605));
#50517=CARTESIAN_POINT('Ctrl Pts',(55.8606989766534,9.03446775281861,-14.4335826317914));
#50518=CARTESIAN_POINT('Ctrl Pts',(55.8078274105936,9.55305661363961,-15.323359668899));
#50519=CARTESIAN_POINT('Ctrl Pts',(55.773954709464,9.87868797757358,-15.9461193665655));
#50520=CARTESIAN_POINT('Ctrl Pts',(55.7512012634347,10.0918611128973,-16.4517402495332));
#50521=CARTESIAN_POINT('Ctrl Pts',(55.7358945084929,10.2373229525384,-16.8986727031992));
#50522=CARTESIAN_POINT('Ctrl Pts',(55.7320628041124,10.2851229032075,-17.0516780663757));
#50523=CARTESIAN_POINT('Ctrl Pts',(55.7251547347841,10.3759936592405,-17.3701166203036));
#50524=CARTESIAN_POINT('Ctrl Pts',(55.7211712881152,10.452196872169,-17.6808812380487));
#50525=CARTESIAN_POINT('Ctrl Pts',(55.7192131230406,10.5174898046456,-17.9910785587738));
#50526=CARTESIAN_POINT('Ctrl Pts',(55.7188977552019,10.5534715834494,-18.1828543478442));
#50527=CARTESIAN_POINT('Ctrl Pts',(55.7191039651392,10.5797214166711,-18.335541325308));
#50528=CARTESIAN_POINT('Ctrl Pts',(55.7194909678605,10.5981271124705,-18.4495004887757));
#50529=CARTESIAN_POINT('Ctrl Pts',(55.7199933559332,10.6124551659916,-18.5440686785368));
#50530=CARTESIAN_POINT('Ctrl Pts',(55.7204990192675,10.6233275116171,-18.6194481036827));
#50531=CARTESIAN_POINT('Ctrl Pts',(55.7253758088147,10.7124575844002,-19.2587758680929));
#50532=CARTESIAN_POINT('Ctrl Pts',(55.7522532141264,10.7815477183789,-20.4323773216303));
#50533=CARTESIAN_POINT('Ctrl Pts',(55.8031397938585,10.7627377228799,-22.0035158978069));
#50534=CARTESIAN_POINT('Ctrl Pts',(55.825737099881,10.7601510570931,-22.9452881163495));
#50535=CARTESIAN_POINT('Ctrl Pts',(55.8320950066742,10.782137854408,-23.5023779715933));
#50536=CARTESIAN_POINT('Ctrl Pts',(55.8340909980986,10.7915560371222,-23.7741616782038));
#50537=CARTESIAN_POINT('Ctrl Pts',(55.8372505969795,10.8051833217901,-24.2872868683742));
#50538=CARTESIAN_POINT('Ctrl Pts',(55.8404568442515,10.8197269207645,-25.1966898642464));
#50539=CARTESIAN_POINT('Ctrl Pts',(55.840087827842,10.8182318448034,-26.4760574343302));
#50540=CARTESIAN_POINT('Ctrl Pts',(55.8361433026693,10.8008785329893,-27.9945641694956));
#50541=CARTESIAN_POINT('Ctrl Pts',(55.834658027917,10.7916788201452,-28.9883692486796));
#50542=CARTESIAN_POINT('Ctrl Pts',(55.8352464030336,10.7906484334464,-29.5423588314564));
#50543=CARTESIAN_POINT('Ctrl Pts',(55.8353820157119,10.790377577361,-29.6692929526829));
#50544=CARTESIAN_POINT('Ctrl Pts',(55.8356247541215,10.7897068203214,-29.9209660665385));
#50545=CARTESIAN_POINT('Ctrl Pts',(55.8360007361368,10.7882119503876,-30.3624654127209));
#50546=CARTESIAN_POINT('Ctrl Pts',(55.8366037897902,10.7841005645739,-31.244305047108));
#50547=CARTESIAN_POINT('Ctrl Pts',(55.837392886965,10.7760252301369,-32.5030227351694));
#50548=CARTESIAN_POINT('Ctrl Pts',(55.8390037271353,10.7674769785333,-33.7573647708467));
#50549=CARTESIAN_POINT('Ctrl Pts',(55.8413101586343,10.7616974971422,-34.757077179787));
#50550=CARTESIAN_POINT('Ctrl Pts',(55.8428821540519,10.7594012798126,-35.255571422185));
#50551=CARTESIAN_POINT('Ctrl Pts',(55.8442554464811,10.7579659520475,-35.6298265937764));
#50552=CARTESIAN_POINT('Ctrl Pts',(55.8452792618007,10.7570014739844,-35.8817691950047));
#50553=CARTESIAN_POINT('Ctrl Pts',(55.8476951430184,10.7551262457876,-36.3841441827128));
#50554=CARTESIAN_POINT('Ctrl Pts',(55.8527414112041,10.7520089029467,-37.2620968637788));
#50555=CARTESIAN_POINT('Ctrl Pts',(55.8650741952096,10.7465773910564,-39.0126066758738));
#50556=CARTESIAN_POINT('Ctrl Pts',(55.8757055265642,10.744014883842,-40.5117095275918));
#50557=CARTESIAN_POINT('Ctrl Pts',(55.8804952904426,10.7437768053537,-41.7652712592726));
#50558=CARTESIAN_POINT('Ctrl Pts',(55.8815884039341,10.7432126106914,-42.1436772152057));
#50559=CARTESIAN_POINT('Ctrl Pts',(55.88255132219,10.7419325483112,-42.6456830734003));
#50560=CARTESIAN_POINT('Ctrl Pts',(55.8832415078542,10.7404472301093,-43.1479172097817));
#50561=CARTESIAN_POINT('Ctrl Pts',(55.883706560662,10.7384823465718,-43.7747209678689));
#50562=CARTESIAN_POINT('Ctrl Pts',(55.883986249836,10.736826384147,-44.5253077456604));
#50563=CARTESIAN_POINT('Ctrl Pts',(55.8842868961193,10.7367553253355,-45.1488783480515));
#50564=CARTESIAN_POINT('Ctrl Pts',(55.884752108554,10.7379140664082,-45.6463700676859));
#50565=CARTESIAN_POINT('Ctrl Pts',(55.8852567982933,10.7394977503655,-46.018718261597));
#50566=CARTESIAN_POINT('Ctrl Pts',(55.8859628356709,10.7419030693311,-46.3902611435584));
#50567=CARTESIAN_POINT('Ctrl Pts',(55.8872334971622,10.746345637622,-46.8844064295826));
#50568=CARTESIAN_POINT('Ctrl Pts',(55.888623767356,10.7512297242423,-47.2537105345762));
#50569=CARTESIAN_POINT('Ctrl Pts',(55.8904027456091,10.7573645699308,-47.6223775744809));
#50570=CARTESIAN_POINT('Ctrl Pts',(55.8916673641002,10.7626624185279,-47.8561843315716));
#50571=CARTESIAN_POINT('Ctrl Pts',(55.8943401260785,10.7782720818847,-48.3368618427273));
#50572=CARTESIAN_POINT('Ctrl Pts',(55.8994324357348,10.8161943746587,-49.1867388598945));
#50573=CARTESIAN_POINT('Ctrl Pts',(55.9078041596401,10.8884371599938,-50.4398661540837));
#50574=CARTESIAN_POINT('Ctrl Pts',(55.9200415336857,10.9593650678926,-51.9991864771287));
#50575=CARTESIAN_POINT('Ctrl Pts',(55.9304302925427,10.9627888364534,-53.077198113757));
#50576=CARTESIAN_POINT('Ctrl Pts',(55.9380573192689,10.9394594388728,-53.7652386011573));
#50577=CARTESIAN_POINT('Ctrl Pts',(55.9416089204399,10.9236075077244,-54.0703683356401));
#50578=CARTESIAN_POINT('Ctrl Pts',(55.9496284188782,10.8749406335218,-54.6485336841008));
#50579=CARTESIAN_POINT('Ctrl Pts',(55.9654007718481,10.7548844414289,-55.6301796463693));
#50580=CARTESIAN_POINT('Ctrl Pts',(55.9994801597755,10.4457295905618,-57.4383006955636));
#50581=CARTESIAN_POINT('Ctrl Pts',(56.0199751665574,10.2882719987063,-58.7271513010342));
#50582=CARTESIAN_POINT('Ctrl Pts',(56.0326904842793,10.337278922736,-59.4940543988374));
#50583=CARTESIAN_POINT('Ctrl Pts',(56.0340506213543,10.3451246445082,-59.6076251738527));
#50584=CARTESIAN_POINT('Ctrl Pts',(56.0367530445702,10.3632182368054,-59.8242094536169));
#50585=CARTESIAN_POINT('Ctrl Pts',(56.0411613373998,10.4030689516349,-60.210995835283));
#50586=CARTESIAN_POINT('Ctrl Pts',(56.0489566094561,10.5130336455672,-60.9880642774255));
#50587=CARTESIAN_POINT('Ctrl Pts',(56.0556887402585,10.7040394482772,-61.8940772156641));
#50588=CARTESIAN_POINT('Ctrl Pts',(56.0609545274981,10.9497688546937,-62.8089348476284));
#50589=CARTESIAN_POINT('Ctrl Pts',(56.063535498526,11.1062828232157,-63.3263977789393));
#50590=CARTESIAN_POINT('Ctrl Pts',(56.0651702598499,11.2173018665274,-63.6719400847196));
#50591=CARTESIAN_POINT('Ctrl Pts',(56.0662420948641,11.2930299821967,-63.9024701228049));
#50592=CARTESIAN_POINT('Ctrl Pts',(56.0673002598306,11.3712018859427,-64.133065809692));
#50593=CARTESIAN_POINT('Ctrl Pts',(56.0682223046878,11.4416005196807,-64.3349582563029));
#50594=CARTESIAN_POINT('Ctrl Pts',(56.0687505834134,11.4823719787838,-64.4503390882157));
#50595=CARTESIAN_POINT('Ctrl Pts',(56.0695468750535,11.5440494636025,-64.6233922442467));
#50596=CARTESIAN_POINT('Ctrl Pts',(56.07021642282,11.5965393493742,-64.7676365408963));
#50597=CARTESIAN_POINT('Ctrl Pts',(56.0713798269483,11.6844972675633,-65.0057761335482));
#50598=CARTESIAN_POINT('Ctrl Pts',(56.0742481638648,11.7673725945197,-65.2187440765607));
#50599=CARTESIAN_POINT('Ctrl Pts',(56.0786225888353,11.956626223471,-65.6686583942398));
#50600=CARTESIAN_POINT('Ctrl Pts',(56.0856207299876,12.325098293157,-66.4581217256169));
#50601=CARTESIAN_POINT('Ctrl Pts',(56.0937062273164,13.2050901989332,-68.0969928591841));
#50602=CARTESIAN_POINT('Ctrl Pts',(56.090624203504,14.1031075892701,-69.5915435266453));
#50603=CARTESIAN_POINT('Ctrl Pts',(56.0851893463343,14.7345980789755,-70.7930388880355));
#50604=CARTESIAN_POINT('Ctrl Pts',(56.0856673076515,14.8634752982914,-71.0375841108356));
#50605=CARTESIAN_POINT('Ctrl Pts',(56.0856335044423,15.1288146941014,-71.5400944851322));
#50606=CARTESIAN_POINT('Ctrl Pts',(56.0859568478666,15.4588035842588,-72.1628165081728));
#50607=CARTESIAN_POINT('Ctrl Pts',(56.0860723465189,15.8578497406362,-72.9134953028285));
#50608=CARTESIAN_POINT('Ctrl Pts',(56.0863258673364,16.657354734975,-74.4139738685058));
#50609=CARTESIAN_POINT('Ctrl Pts',(56.0862888584833,17.3272584591274,-75.6668214801239));
#50610=CARTESIAN_POINT('Ctrl Pts',(56.0860232991955,18.298981737646,-77.4942288106584));
#50611=CARTESIAN_POINT('Ctrl Pts',(56.0861395828494,18.7346801636112,-78.3135207979159));
#50612=CARTESIAN_POINT('Ctrl Pts',(56.0861395828494,19.1712017510007,-79.1344985000142));
#50613=CARTESIAN_POINT('Ctrl Pts',(58.8531048919552,6.29126117034768,24.8311270138471));
#50614=CARTESIAN_POINT('Ctrl Pts',(58.853288783423,6.29129935584637,24.7822631366728));
#50615=CARTESIAN_POINT('Ctrl Pts',(58.8534816497087,6.2913393689017,24.7334006343834));
#50616=CARTESIAN_POINT('Ctrl Pts',(58.8557584618987,6.29181245235756,24.1829722163064));
#50617=CARTESIAN_POINT('Ctrl Pts',(58.8576410777844,6.2924661188456,23.1790742508252));
#50618=CARTESIAN_POINT('Ctrl Pts',(58.8621221486529,6.29416752032691,21.1707865278706));
#50619=CARTESIAN_POINT('Ctrl Pts',(58.8772641083492,6.29730728170481,19.6666193118639));
#50620=CARTESIAN_POINT('Ctrl Pts',(58.9086867192454,6.30251976314054,18.4155160354777));
#50621=CARTESIAN_POINT('Ctrl Pts',(58.9238681411952,6.30510263301061,17.9134655130762));
#50622=CARTESIAN_POINT('Ctrl Pts',(58.9621931814769,6.31171912254366,16.9100353472743));
#50623=CARTESIAN_POINT('Ctrl Pts',(59.044403541375,6.32581484340266,15.1562873808193));
#50624=CARTESIAN_POINT('Ctrl Pts',(59.1211061781268,6.33775411577698,13.6520094580886));
#50625=CARTESIAN_POINT('Ctrl Pts',(59.1665661184318,6.3427083323814,12.3941538441954));
#50626=CARTESIAN_POINT('Ctrl Pts',(59.1848509216029,6.34443693178228,11.8918021760891));
#50627=CARTESIAN_POINT('Ctrl Pts',(59.2211705479974,6.347012855465,10.8878709549565));
#50628=CARTESIAN_POINT('Ctrl Pts',(59.2646739973078,6.34878292287888,9.63367636155125));
#50629=CARTESIAN_POINT('Ctrl Pts',(59.3092425919531,6.34933180168931,8.1292129060296));
#50630=CARTESIAN_POINT('Ctrl Pts',(59.3308039810503,6.34911032516135,7.12575148040342));
#50631=CARTESIAN_POINT('Ctrl Pts',(59.3407582844956,6.34895254139073,6.49900156323555));
#50632=CARTESIAN_POINT('Ctrl Pts',(59.3443009479904,6.3487870308239,6.2480976285954));
#50633=CARTESIAN_POINT('Ctrl Pts',(59.349863835633,6.34809587935646,5.74652248908033));
#50634=CARTESIAN_POINT('Ctrl Pts',(59.3559914845584,6.34610427421115,4.86750836522151));
#50635=CARTESIAN_POINT('Ctrl Pts',(59.3569458990738,6.34027728789477,3.10835172779085));
#50636=CARTESIAN_POINT('Ctrl Pts',(59.3490635616926,6.33670075767835,1.60628918930064));
#50637=CARTESIAN_POINT('Ctrl Pts',(59.3492784094883,6.33905879792391,0.550302612753713));
#50638=CARTESIAN_POINT('Ctrl Pts',(59.3495243001637,6.33896196490088,0.412614894001366));
#50639=CARTESIAN_POINT('Ctrl Pts',(59.3508389109231,6.33723377320785,0.146161885443116));
#50640=CARTESIAN_POINT('Ctrl Pts',(59.3550532176265,6.33072390632153,-0.318553477805038));
#50641=CARTESIAN_POINT('Ctrl Pts',(59.3652297576622,6.31399897839904,-0.965908052840755));
#50642=CARTESIAN_POINT('Ctrl Pts',(59.3798741113377,6.29000761912293,-1.72062652108147));
#50643=CARTESIAN_POINT('Ctrl Pts',(59.3971807795463,6.26259249771466,-2.69621161988787));
#50644=CARTESIAN_POINT('Ctrl Pts',(59.4043414085574,6.25497826476023,-3.85975006748727));
#50645=CARTESIAN_POINT('Ctrl Pts',(59.3733146100403,6.3105312327679,-4.73293165960504));
#50646=CARTESIAN_POINT('Ctrl Pts',(59.3363575784456,6.37295188297166,-5.26473353177676));
#50647=CARTESIAN_POINT('Ctrl Pts',(59.3183418149714,6.40289994227644,-5.50595486139798));
#50648=CARTESIAN_POINT('Ctrl Pts',(59.2730388009056,6.46480431714097,-5.97081755510265));
#50649=CARTESIAN_POINT('Ctrl Pts',(59.1724422888517,6.58535278710391,-6.78943021470857));
#50650=CARTESIAN_POINT('Ctrl Pts',(58.9912262531475,6.7868229657027,-7.94612904489456));
#50651=CARTESIAN_POINT('Ctrl Pts',(58.8223317891728,7.04771908873206,-9.10212973186673));
#50652=CARTESIAN_POINT('Ctrl Pts',(58.735697291889,7.28300208313501,-9.90635004105204));
#50653=CARTESIAN_POINT('Ctrl Pts',(58.6977351168525,7.43540237400419,-10.3634058429054));
#50654=CARTESIAN_POINT('Ctrl Pts',(58.6830346418896,7.51810068114256,-10.591111217551));
#50655=CARTESIAN_POINT('Ctrl Pts',(58.6738634777459,7.58260836432584,-10.761190612064));
#50656=CARTESIAN_POINT('Ctrl Pts',(58.6723346369094,7.6173239321139,-10.8453845146161));
#50657=CARTESIAN_POINT('Ctrl Pts',(58.6676689607852,7.70233593977603,-11.0379844018061));
#50658=CARTESIAN_POINT('Ctrl Pts',(58.6622876768978,7.87158105335511,-11.3815342433213));
#50659=CARTESIAN_POINT('Ctrl Pts',(58.6531725345026,8.29795340172989,-12.1307881868699));
#50660=CARTESIAN_POINT('Ctrl Pts',(58.6343507387422,9.0888204052782,-13.3224315637315));
#50661=CARTESIAN_POINT('Ctrl Pts',(58.6088503070498,9.85801911386535,-14.5331952917628));
#50662=CARTESIAN_POINT('Ctrl Pts',(58.5920713303508,10.3189685137634,-15.4243151261943));
#50663=CARTESIAN_POINT('Ctrl Pts',(58.5810899924814,10.6052359649885,-16.0452514748664));
#50664=CARTESIAN_POINT('Ctrl Pts',(58.5733938621257,10.7885227068715,-16.5448452975907));
#50665=CARTESIAN_POINT('Ctrl Pts',(58.5676247829872,10.911110806863,-16.9819314237086));
#50666=CARTESIAN_POINT('Ctrl Pts',(58.566515134249,10.9530822623337,-17.1389501191447));
#50667=CARTESIAN_POINT('Ctrl Pts',(58.5650823700106,11.0297845914177,-17.4602983187608));
#50668=CARTESIAN_POINT('Ctrl Pts',(58.5655994643091,11.0918640608194,-17.7749969970167));
#50669=CARTESIAN_POINT('Ctrl Pts',(58.567479755255,11.1421871122659,-18.0874443318188));
#50670=CARTESIAN_POINT('Ctrl Pts',(58.5692257607602,11.1687651072572,-18.2805138718139));
#50671=CARTESIAN_POINT('Ctrl Pts',(58.5709066006215,11.1874061276119,-18.4339668965554));
#50672=CARTESIAN_POINT('Ctrl Pts',(58.5723068416036,11.2000958147659,-18.5484262892516));
#50673=CARTESIAN_POINT('Ctrl Pts',(58.5735810792346,11.2096476662046,-18.6433263639815));
#50674=CARTESIAN_POINT('Ctrl Pts',(58.5746599324514,11.2166987397609,-18.7189271165951));
#50675=CARTESIAN_POINT('Ctrl Pts',(58.5841803354795,11.2733312266439,-19.3598937336237));
#50676=CARTESIAN_POINT('Ctrl Pts',(58.6120243623537,11.2811438472495,-20.5284346164844));
#50677=CARTESIAN_POINT('Ctrl Pts',(58.6548556526593,11.1940216759872,-22.0799936426061));
#50678=CARTESIAN_POINT('Ctrl Pts',(58.6749787296748,11.1632014021287,-23.0022998186139));
#50679=CARTESIAN_POINT('Ctrl Pts',(58.6826373505566,11.1724781990788,-23.5437147825256));
#50680=CARTESIAN_POINT('Ctrl Pts',(58.6852936633433,11.1764569534577,-23.8091597735434));
#50681=CARTESIAN_POINT('Ctrl Pts',(58.6897313102728,11.1821520504571,-24.3109583800983));
#50682=CARTESIAN_POINT('Ctrl Pts',(58.6951496568698,11.18811730114,-25.2033062990913));
#50683=CARTESIAN_POINT('Ctrl Pts',(58.6975113593674,11.1872479676171,-26.4667513104716));
#50684=CARTESIAN_POINT('Ctrl Pts',(58.6954851864191,11.1799618969185,-27.9801788785804));
#50685=CARTESIAN_POINT('Ctrl Pts',(58.6933663086165,11.1760448864423,-28.9802073808478));
#50686=CARTESIAN_POINT('Ctrl Pts',(58.6925291563035,11.1756400017411,-29.54013772036));
#50687=CARTESIAN_POINT('Ctrl Pts',(58.6922950590304,11.1755342273211,-29.6661205159246));
#50688=CARTESIAN_POINT('Ctrl Pts',(58.6916838214696,11.175261758783,-29.9172281844278));
#50689=CARTESIAN_POINT('Ctrl Pts',(58.6902528492363,11.1746278716065,-30.3572248042373));
#50690=CARTESIAN_POINT('Ctrl Pts',(58.686156011812,11.1728135218474,-31.237075055171));
#50691=CARTESIAN_POINT('Ctrl Pts',(58.6779244362639,11.1690434128148,-32.4940740070076));
#50692=CARTESIAN_POINT('Ctrl Pts',(58.6696380838126,11.1648456735736,-33.7486968816292));
#50693=CARTESIAN_POINT('Ctrl Pts',(58.6648548738614,11.162001808617,-34.7497098307469));
#50694=CARTESIAN_POINT('Ctrl Pts',(58.6633983437453,11.1608703557711,-35.2492405539033));
#50695=CARTESIAN_POINT('Ctrl Pts',(58.6627726971019,11.1601841652618,-35.6244027444587));
#50696=CARTESIAN_POINT('Ctrl Pts',(58.6624681048258,11.1597282059655,-35.8763034515194));
#50697=CARTESIAN_POINT('Ctrl Pts',(58.662267318025,11.1588190707973,-36.3789711970892));
#50698=CARTESIAN_POINT('Ctrl Pts',(58.6628639022804,11.1572820747005,-37.2572499766015));
#50699=CARTESIAN_POINT('Ctrl Pts',(58.6668824890188,11.1545806575703,-39.0086150002578));
#50700=CARTESIAN_POINT('Ctrl Pts',(58.6718031114793,11.1537637365605,-40.508386452936));
#50701=CARTESIAN_POINT('Ctrl Pts',(58.6730165686399,11.1546710008935,-41.7625412307252));
#50702=CARTESIAN_POINT('Ctrl Pts',(58.6731074510399,11.1544438395403,-42.1409999055361));
#50703=CARTESIAN_POINT('Ctrl Pts',(58.6728673574289,11.1535770440756,-42.6431794169131));
#50704=CARTESIAN_POINT('Ctrl Pts',(58.6724461101439,11.1524856555828,-43.1455918732114));
#50705=CARTESIAN_POINT('Ctrl Pts',(58.6716936934682,11.1509666828279,-43.7726690093924));
#50706=CARTESIAN_POINT('Ctrl Pts',(58.6707929708391,11.1497603315992,-44.52365118088));
#50707=CARTESIAN_POINT('Ctrl Pts',(58.6703480265652,11.1499817126121,-45.147614397289));
#50708=CARTESIAN_POINT('Ctrl Pts',(58.670359448683,11.1513089229432,-45.6454614270176));
#50709=CARTESIAN_POINT('Ctrl Pts',(58.6705970894054,11.152989107669,-46.018095499028));
#50710=CARTESIAN_POINT('Ctrl Pts',(58.6711096924726,11.1554586142605,-46.3899437030966));
#50711=CARTESIAN_POINT('Ctrl Pts',(58.6722217573552,11.1599390035811,-46.8845233225911));
#50712=CARTESIAN_POINT('Ctrl Pts',(58.6736050980711,11.1648026318779,-47.2541803983589));
#50713=CARTESIAN_POINT('Ctrl Pts',(58.6754544191834,11.1708724187996,-47.6232252559624));
#50714=CARTESIAN_POINT('Ctrl Pts',(58.6768261977709,11.1761194371953,-47.8573849835496));
#50715=CARTESIAN_POINT('Ctrl Pts',(58.6799052267683,11.1915668487932,-48.3386403067271));
#50716=CARTESIAN_POINT('Ctrl Pts',(58.6861582569438,11.2290588435075,-49.1893944317329));
#50717=CARTESIAN_POINT('Ctrl Pts',(58.6971032883846,11.3002628695192,-50.4432920806055));
#50718=CARTESIAN_POINT('Ctrl Pts',(58.7128620077876,11.3693893217062,-52.0028627018444));
#50719=CARTESIAN_POINT('Ctrl Pts',(58.7252444156214,11.3714512484384,-53.0805961140929));
#50720=CARTESIAN_POINT('Ctrl Pts',(58.7338153696161,11.347301218749,-53.76834192412));
#50721=CARTESIAN_POINT('Ctrl Pts',(58.7377766840328,11.3310354824593,-54.0737103110201));
#50722=CARTESIAN_POINT('Ctrl Pts',(58.7466284819545,11.2815142239099,-54.6520866627448));
#50723=CARTESIAN_POINT('Ctrl Pts',(58.7638687059199,11.1598471258297,-55.6340650974073));
#50724=CARTESIAN_POINT('Ctrl Pts',(58.800567281988,10.8473227536876,-57.4423158425765));
#50725=CARTESIAN_POINT('Ctrl Pts',(58.8224426358845,10.6879399518963,-58.7303538545682));
#50726=CARTESIAN_POINT('Ctrl Pts',(58.8355451088492,10.7362905625105,-59.4957112097895));
#50727=CARTESIAN_POINT('Ctrl Pts',(58.8369437008818,10.7440442698396,-59.6091146653755));
#50728=CARTESIAN_POINT('Ctrl Pts',(58.8396933622305,10.7619811815525,-59.8253728659405));
#50729=CARTESIAN_POINT('Ctrl Pts',(58.8441090309769,10.8015995672414,-60.2116412498697));
#50730=CARTESIAN_POINT('Ctrl Pts',(58.8516532452224,10.9112843858518,-60.9878681974567));
#50731=CARTESIAN_POINT('Ctrl Pts',(58.8576498131029,11.1023498914853,-61.8933793937477));
#50732=CARTESIAN_POINT('Ctrl Pts',(58.862065588882,11.348390653275,-62.8081425766873));
#50733=CARTESIAN_POINT('Ctrl Pts',(58.8641851331624,11.5051348146818,-63.3256911177079));
#50734=CARTESIAN_POINT('Ctrl Pts',(58.8655431183583,11.6163140515013,-63.6713440824319));
#50735=CARTESIAN_POINT('Ctrl Pts',(58.8664403305124,11.6921494967269,-63.9019619108394));
#50736=CARTESIAN_POINT('Ctrl Pts',(58.8673404322247,11.7704270793534,-64.1326656001653));
#50737=CARTESIAN_POINT('Ctrl Pts',(58.8681432316335,11.8409141347406,-64.3346702081786));
#50738=CARTESIAN_POINT('Ctrl Pts',(58.8686092840971,11.881734392604,-64.4501200906322));
#50739=CARTESIAN_POINT('Ctrl Pts',(58.869318507385,11.9434830759097,-64.6232815853475));
#50740=CARTESIAN_POINT('Ctrl Pts',(58.8699286517978,11.9960274978391,-64.7676265626046));
#50741=CARTESIAN_POINT('Ctrl Pts',(58.8710157569687,12.0840658209306,-65.0059424367529));
#50742=CARTESIAN_POINT('Ctrl Pts',(58.8738589421922,12.1669604684609,-65.2188979516415));
#50743=CARTESIAN_POINT('Ctrl Pts',(58.8781893104489,12.3562843388777,-65.6688870066509));
#50744=CARTESIAN_POINT('Ctrl Pts',(58.8851906494169,12.7248466273555,-66.4584035251456));
#50745=CARTESIAN_POINT('Ctrl Pts',(58.8934443763777,13.6049670574308,-68.0973570342353));
#50746=CARTESIAN_POINT('Ctrl Pts',(58.8905062211977,14.5029656194648,-69.5918838038918));
#50747=CARTESIAN_POINT('Ctrl Pts',(58.8849459593989,15.1344155593395,-70.7933399329592));
#50748=CARTESIAN_POINT('Ctrl Pts',(58.8854298430313,15.2633013275615,-71.0378917525492));
#50749=CARTESIAN_POINT('Ctrl Pts',(58.8853901310312,15.5286459532577,-71.540405931102));
#50750=CARTESIAN_POINT('Ctrl Pts',(58.8857159790617,15.8586422053525,-72.163134336603));
#50751=CARTESIAN_POINT('Ctrl Pts',(58.885832972894,16.2576915358115,-72.9138175400082));
#50752=CARTESIAN_POINT('Ctrl Pts',(58.8860950426403,17.0571981277039,-74.4143023315381));
#50753=CARTESIAN_POINT('Ctrl Pts',(58.8860657223544,17.7270914913872,-75.6671445469792));
#50754=CARTESIAN_POINT('Ctrl Pts',(58.8857948969183,18.6988067501922,-77.4945402056233));
#50755=CARTESIAN_POINT('Ctrl Pts',(58.8859129594251,19.1345069619474,-78.3138346232385));
#50756=CARTESIAN_POINT('Ctrl Pts',(58.8859129594252,19.5710285493368,-79.1348123253369));
#50757=CARTESIAN_POINT('Ctrl Pts',(61.1951430599348,6.62459351860839,24.8301566171112));
#50758=CARTESIAN_POINT('Ctrl Pts',(61.1953495829341,6.62461118340833,24.7812622509577));
#50759=CARTESIAN_POINT('Ctrl Pts',(61.1955661714496,6.62462972912612,24.7323686772253));
#50760=CARTESIAN_POINT('Ctrl Pts',(61.1981226275006,6.62484834924031,24.1815830296665));
#50761=CARTESIAN_POINT('Ctrl Pts',(61.200552546657,6.62487504513224,23.1773159143136));
#50762=CARTESIAN_POINT('Ctrl Pts',(61.2065289204206,6.62485044255725,21.1683500346935));
#50763=CARTESIAN_POINT('Ctrl Pts',(61.2235206228691,6.6263073739822,19.6639179088845));
#50764=CARTESIAN_POINT('Ctrl Pts',(61.2571976857159,6.63009622317173,18.4126432827115));
#50765=CARTESIAN_POINT('Ctrl Pts',(61.2735402762306,6.63178859409188,17.9085730154883));
#50766=CARTESIAN_POINT('Ctrl Pts',(61.3149072476585,6.63580631603488,16.9037326109381));
#50767=CARTESIAN_POINT('Ctrl Pts',(61.4035013072067,6.6443874466591,15.1503002603318));
#50768=CARTESIAN_POINT('Ctrl Pts',(61.4848249365008,6.65408168458786,13.6525508282425));
#50769=CARTESIAN_POINT('Ctrl Pts',(61.5305594648357,6.66308696916894,12.4031116832484));
#50770=CARTESIAN_POINT('Ctrl Pts',(61.5486814066148,6.66709153838059,11.9041991676416));
#50771=CARTESIAN_POINT('Ctrl Pts',(61.5837588738223,6.67629259873839,10.9052363266201));
#50772=CARTESIAN_POINT('Ctrl Pts',(61.6244364766192,6.68920666605379,9.65440342433843));
#50773=CARTESIAN_POINT('Ctrl Pts',(61.6644897802702,6.7043024031215,8.14923390352158));
#50774=CARTESIAN_POINT('Ctrl Pts',(61.6830749181458,6.71236791277641,7.14232597420164));
#50775=CARTESIAN_POINT('Ctrl Pts',(61.6913383718123,6.71624608706999,6.51262594167426));
#50776=CARTESIAN_POINT('Ctrl Pts',(61.69414610316,6.71780214827397,6.26370524403605));
#50777=CARTESIAN_POINT('Ctrl Pts',(61.6980214561424,6.72094132003559,5.76362531772536));
#50778=CARTESIAN_POINT('Ctrl Pts',(61.7007450863805,6.72636327795744,4.8866659505902));
#50779=CARTESIAN_POINT('Ctrl Pts',(61.6938174291058,6.73605603354009,3.12445746403));
#50780=CARTESIAN_POINT('Ctrl Pts',(61.6803461765711,6.73881989834997,1.61004654781063));
#50781=CARTESIAN_POINT('Ctrl Pts',(61.6804493960782,6.73532109511675,0.538275827822303));
#50782=CARTESIAN_POINT('Ctrl Pts',(61.6808101793117,6.73401731235922,0.391744046227261));
#50783=CARTESIAN_POINT('Ctrl Pts',(61.6827543160363,6.72849797514263,0.11292533490665));
#50784=CARTESIAN_POINT('Ctrl Pts',(61.6890248659479,6.71203304004211,-0.372274787302301));
#50785=CARTESIAN_POINT('Ctrl Pts',(61.7040904305426,6.67419733781364,-1.03825243668594));
#50786=CARTESIAN_POINT('Ctrl Pts',(61.7258780777276,6.62118416234288,-1.80127297542329));
#50787=CARTESIAN_POINT('Ctrl Pts',(61.7520928872156,6.55737622968081,-2.76765400835207));
#50788=CARTESIAN_POINT('Ctrl Pts',(61.7660952010983,6.52136939127453,-3.8821518154703));
#50789=CARTESIAN_POINT('Ctrl Pts',(61.729067495728,6.58516251664634,-4.67513771827723));
#50790=CARTESIAN_POINT('Ctrl Pts',(61.6839343104004,6.66311971581696,-5.14899657540951));
#50791=CARTESIAN_POINT('Ctrl Pts',(61.6617387075409,6.70034156427653,-5.35025911829331));
#50792=CARTESIAN_POINT('Ctrl Pts',(61.6046402242691,6.78918160908311,-5.75878526406458));
#50793=CARTESIAN_POINT('Ctrl Pts',(61.4765501720259,6.98331289136561,-6.50476976133261));
#50794=CARTESIAN_POINT('Ctrl Pts',(61.2474997672193,7.35403276894785,-7.64853950979505));
#50795=CARTESIAN_POINT('Ctrl Pts',(61.0315326652427,7.812434998521,-8.88214138951066));
#50796=CARTESIAN_POINT('Ctrl Pts',(60.9164087838436,8.15957649757144,-9.77875658120804));
#50797=CARTESIAN_POINT('Ctrl Pts',(60.8649434387047,8.36254780943143,-10.2990968288097));
#50798=CARTESIAN_POINT('Ctrl Pts',(60.8446861618763,8.46524558357949,-10.5620869355828));
#50799=CARTESIAN_POINT('Ctrl Pts',(60.8319717937481,8.54250760013033,-10.7601063274006));
#50800=CARTESIAN_POINT('Ctrl Pts',(60.8294620303259,8.5844566328175,-10.8601436322418));
#50801=CARTESIAN_POINT('Ctrl Pts',(60.8233921158387,8.68113683502462,-11.0820780579105));
#50802=CARTESIAN_POINT('Ctrl Pts',(60.8191540441179,8.86227482615309,-11.4680942275968));
#50803=CARTESIAN_POINT('Ctrl Pts',(60.8257513025041,9.27903522043605,-12.2748548396355));
#50804=CARTESIAN_POINT('Ctrl Pts',(60.8668397300883,9.97140776595471,-13.5004881682362));
#50805=CARTESIAN_POINT('Ctrl Pts',(60.91809750942,10.5941498479321,-14.7188381694371));
#50806=CARTESIAN_POINT('Ctrl Pts',(60.9479629679688,10.953166600623,-15.5959303525026));
#50807=CARTESIAN_POINT('Ctrl Pts',(60.9654273466163,11.1726390509724,-16.1995991182255));
#50808=CARTESIAN_POINT('Ctrl Pts',(60.9746817698278,11.3095967394032,-16.674774647252));
#50809=CARTESIAN_POINT('Ctrl Pts',(60.9784785963746,11.4012776811817,-17.082927036861));
#50810=CARTESIAN_POINT('Ctrl Pts',(60.9801506660244,11.4345556346319,-17.2394288135314));
#50811=CARTESIAN_POINT('Ctrl Pts',(60.9835902396351,11.493131799317,-17.5529833462735));
#50812=CARTESIAN_POINT('Ctrl Pts',(60.9872151786763,11.5395393577809,-17.8619373863565));
#50813=CARTESIAN_POINT('Ctrl Pts',(60.9908320118966,11.57551979552,-18.1673014652789));
#50814=CARTESIAN_POINT('Ctrl Pts',(60.9930796103776,11.5938996693051,-18.3562408564781));
#50815=CARTESIAN_POINT('Ctrl Pts',(60.9948531119313,11.6063443310479,-18.5063169153956));
#50816=CARTESIAN_POINT('Ctrl Pts',(60.9961699597551,11.6145865427258,-18.6182943335112));
#50817=CARTESIAN_POINT('Ctrl Pts',(60.9972543385166,11.6205841104154,-18.7111372183144));
#50818=CARTESIAN_POINT('Ctrl Pts',(60.9981121879651,11.6248839498187,-18.7851145838485));
#50819=CARTESIAN_POINT('Ctrl Pts',(61.0053617468449,11.6586247888096,-19.4123376454189));
#50820=CARTESIAN_POINT('Ctrl Pts',(61.0172652635169,11.638506103459,-20.5587287497834));
#50821=CARTESIAN_POINT('Ctrl Pts',(61.0268712384702,11.5302675454384,-22.0960102293423));
#50822=CARTESIAN_POINT('Ctrl Pts',(61.0305990851216,11.4890734836909,-23.0203699506435));
#50823=CARTESIAN_POINT('Ctrl Pts',(61.0339916227849,11.4918641686232,-23.5668462678014));
#50824=CARTESIAN_POINT('Ctrl Pts',(61.0351944413737,11.4929251983715,-23.8277092582862));
#50825=CARTESIAN_POINT('Ctrl Pts',(61.037153140714,11.4943502477889,-24.3247189869738));
#50826=CARTESIAN_POINT('Ctrl Pts',(61.0394974963756,11.4954093598254,-25.2082732613028));
#50827=CARTESIAN_POINT('Ctrl Pts',(61.040290778228,11.4936881528447,-26.4644309696059));
#50828=CARTESIAN_POINT('Ctrl Pts',(61.0387579071437,11.4898327101281,-27.9743589344223));
#50829=CARTESIAN_POINT('Ctrl Pts',(61.0372909646032,11.4884279010678,-28.9761098417619));
#50830=CARTESIAN_POINT('Ctrl Pts',(61.0367222294322,11.4886071465497,-29.5380249988527));
#50831=CARTESIAN_POINT('Ctrl Pts',(61.0365763771857,11.4886536420874,-29.6633057425343));
#50832=CARTESIAN_POINT('Ctrl Pts',(61.036197723935,11.4887692768465,-29.9137065824811));
#50833=CARTESIAN_POINT('Ctrl Pts',(61.0353289370354,11.4890318207177,-30.3522566304998));
#50834=CARTESIAN_POINT('Ctrl Pts',(61.0328937905285,11.4897738835658,-31.2299465515799));
#50835=CARTESIAN_POINT('Ctrl Pts',(61.0281756870949,11.4913506436747,-32.4851072083748));
#50836=CARTESIAN_POINT('Ctrl Pts',(61.0238079284518,11.493284065832,-33.7399112197011));
#50837=CARTESIAN_POINT('Ctrl Pts',(61.0217143885294,11.4948093702616,-34.7422387719057));
#50838=CARTESIAN_POINT('Ctrl Pts',(61.0213301291716,11.4955280787965,-35.2428220670568));
#50839=CARTESIAN_POINT('Ctrl Pts',(61.021365193341,11.4960345422261,-35.6189094102041));
#50840=CARTESIAN_POINT('Ctrl Pts',(61.0214880534992,11.4963594205114,-35.8707605975974));
#50841=CARTESIAN_POINT('Ctrl Pts',(61.022091923799,11.4969726153639,-36.3737127464358));
#50842=CARTESIAN_POINT('Ctrl Pts',(61.0239682927916,11.4979686662637,-37.2522956319764));
#50843=CARTESIAN_POINT('Ctrl Pts',(61.030118867598,11.4998855199777,-39.0044637620451));
#50844=CARTESIAN_POINT('Ctrl Pts',(61.0363540626141,11.5020954232287,-40.5049067899921));
#50845=CARTESIAN_POINT('Ctrl Pts',(61.038646816702,11.5050744859075,-41.7596996292913));
#50846=CARTESIAN_POINT('Ctrl Pts',(61.0390752697443,11.5054585796329,-42.1382540029348));
#50847=CARTESIAN_POINT('Ctrl Pts',(61.0392956115982,11.5053604416316,-42.6406423496876));
#50848=CARTESIAN_POINT('Ctrl Pts',(61.0393322346442,11.5049977022042,-43.1432669810382));
#50849=CARTESIAN_POINT('Ctrl Pts',(61.0391335617917,11.5043074977545,-43.7706467352822));
#50850=CARTESIAN_POINT('Ctrl Pts',(61.0388191356084,11.5039312905533,-44.5220374744878));
#50851=CARTESIAN_POINT('Ctrl Pts',(61.0387575897355,11.5046808017656,-45.1463820923632));
#50852=CARTESIAN_POINT('Ctrl Pts',(61.0389901580766,11.5063260376076,-45.644560991936));
#50853=CARTESIAN_POINT('Ctrl Pts',(61.0393440524272,11.5081845335494,-46.0174562444788));
#50854=CARTESIAN_POINT('Ctrl Pts',(61.0399174477217,11.5107693709555,-46.3895780162853));
#50855=CARTESIAN_POINT('Ctrl Pts',(61.0410285266999,11.5153152039897,-46.8845402270902));
#50856=CARTESIAN_POINT('Ctrl Pts',(61.042309730768,11.5201214408717,-47.2545020559948));
#50857=CARTESIAN_POINT('Ctrl Pts',(61.0439765688629,11.5260573269785,-47.6238702479814));
#50858=CARTESIAN_POINT('Ctrl Pts',(61.0451979805278,11.5311868441681,-47.8583439704282));
#50859=CARTESIAN_POINT('Ctrl Pts',(61.0478905014547,11.54627495127,-48.3401165469988));
#50860=CARTESIAN_POINT('Ctrl Pts',(61.0532534115344,11.5828352334387,-49.1916789368563));
#50861=CARTESIAN_POINT('Ctrl Pts',(61.062428503681,11.6519949668785,-50.4463578455976));
#50862=CARTESIAN_POINT('Ctrl Pts',(61.0755188185728,11.7179578989,-52.0063055054175));
#50863=CARTESIAN_POINT('Ctrl Pts',(61.0858830118634,11.7178472866256,-53.0838602731508));
#50864=CARTESIAN_POINT('Ctrl Pts',(61.0931433051171,11.692434627005,-53.7713622472881));
#50865=CARTESIAN_POINT('Ctrl Pts',(61.0965370029646,11.6755684209064,-54.0770339158701));
#50866=CARTESIAN_POINT('Ctrl Pts',(61.1041095778333,11.6247984603233,-54.6556827303067));
#50867=CARTESIAN_POINT('Ctrl Pts',(61.1188092586801,11.5008147164422,-55.6380313969055));
#50868=CARTESIAN_POINT('Ctrl Pts',(61.1497715914765,11.1836218272256,-57.4462290259746));
#50869=CARTESIAN_POINT('Ctrl Pts',(61.1670585779046,11.0216045517656,-58.733328081795));
#50870=CARTESIAN_POINT('Ctrl Pts',(61.1785128178043,11.0690131276586,-59.4972030211869));
#50871=CARTESIAN_POINT('Ctrl Pts',(61.1797256393047,11.0766416381124,-59.610448755841));
#50872=CARTESIAN_POINT('Ctrl Pts',(61.1821403331636,11.0943651818359,-59.8263975881668));
#50873=CARTESIAN_POINT('Ctrl Pts',(61.1860684267584,11.1336759262185,-60.2121735570825));
#50874=CARTESIAN_POINT('Ctrl Pts',(61.1929862876842,11.2430089381107,-60.9875889820288));
#50875=CARTESIAN_POINT('Ctrl Pts',(61.1988812462932,11.4341741250438,-61.8925738653455));
#50876=CARTESIAN_POINT('Ctrl Pts',(61.2034447566965,11.6805866699791,-62.8071682611196));
#50877=CARTESIAN_POINT('Ctrl Pts',(61.2056763108923,11.8375892467775,-63.3247484688506));
#50878=CARTESIAN_POINT('Ctrl Pts',(61.2070945659281,11.9489406644992,-63.6704733688684));
#50879=CARTESIAN_POINT('Ctrl Pts',(61.2080264110695,12.0248889722813,-63.9011526967969));
#50880=CARTESIAN_POINT('Ctrl Pts',(61.2089503354553,12.1032751394498,-64.1319376965954));
#50881=CARTESIAN_POINT('Ctrl Pts',(61.2097599890901,12.1738487662449,-64.3340311888907));
#50882=CARTESIAN_POINT('Ctrl Pts',(61.210225349747,12.2147156178177,-64.4495369264779));
#50883=CARTESIAN_POINT('Ctrl Pts',(61.2109285935608,12.2765309047319,-64.622787105303));
#50884=CARTESIAN_POINT('Ctrl Pts',(61.2115229163368,12.3291239896802,-64.7672168561216));
#50885=CARTESIAN_POINT('Ctrl Pts',(61.2125656045197,12.4172282475888,-65.0056835116515));
#50886=CARTESIAN_POINT('Ctrl Pts',(61.2153513922814,12.5001116560548,-65.2186040921951));
#50887=CARTESIAN_POINT('Ctrl Pts',(61.21959239646,12.6894555668514,-65.6686299937227));
#50888=CARTESIAN_POINT('Ctrl Pts',(61.2264764890157,13.0580265678792,-66.4581526677089));
#50889=CARTESIAN_POINT('Ctrl Pts',(61.2346640709762,13.9381721898705,-68.0971499643503));
#50890=CARTESIAN_POINT('Ctrl Pts',(61.2318777407206,14.8361818361123,-69.5916598166225));
#50891=CARTESIAN_POINT('Ctrl Pts',(61.2264107813354,15.46766355341,-70.7931005604253));
#50892=CARTESIAN_POINT('Ctrl Pts',(61.2268891177495,15.5965515817802,-71.0376558745414));
#50893=CARTESIAN_POINT('Ctrl Pts',(61.2268525774728,15.8619018084997,-71.5401728351865));
#50894=CARTESIAN_POINT('Ctrl Pts',(61.227175206126,16.1919015707836,-72.1629050847276));
#50895=CARTESIAN_POINT('Ctrl Pts',(61.2272904510929,16.5909525148039,-72.9135914650207));
#50896=CARTESIAN_POINT('Ctrl Pts',(61.227545933965,17.3904573528723,-74.4140808562323));
#50897=CARTESIAN_POINT('Ctrl Pts',(61.2275121731408,18.0603429850346,-75.6669195975717));
#50898=CARTESIAN_POINT('Ctrl Pts',(61.227246123972,19.032055779478,-77.4943066306203));
#50899=CARTESIAN_POINT('Ctrl Pts',(61.2273623803738,19.4677567453798,-78.3136026414037));
#50900=CARTESIAN_POINT('Ctrl Pts',(61.2273623803738,19.9042783327692,-79.134580343502));
#50901=CARTESIAN_POINT('Ctrl Pts',(62.8338034543076,6.85465958390862,24.8297410593479));
#50902=CARTESIAN_POINT('Ctrl Pts',(62.8339996969438,6.85466517832061,24.780833104738));
#50903=CARTESIAN_POINT('Ctrl Pts',(62.8342054937221,6.85467103851654,24.7319257482639));
#50904=CARTESIAN_POINT('Ctrl Pts',(62.8366359551373,6.85474201651055,24.1809791522283));
#50905=CARTESIAN_POINT('Ctrl Pts',(62.8386904201629,6.85437239286699,23.1764427006591));
#50906=CARTESIAN_POINT('Ctrl Pts',(62.8435952494902,6.8532127051144,21.1672198892287));
#50907=CARTESIAN_POINT('Ctrl Pts',(62.8597597964598,6.85370795725647,19.6628112443166));
#50908=CARTESIAN_POINT('Ctrl Pts',(62.8930919457468,6.85688911109818,18.4116365613619));
#50909=CARTESIAN_POINT('Ctrl Pts',(62.9090906942054,6.85822469673433,17.9070296332427));
#50910=CARTESIAN_POINT('Ctrl Pts',(62.9492589590369,6.86126039912779,16.9017582496074));
#50911=CARTESIAN_POINT('Ctrl Pts',(63.0353244769336,6.86788486987616,15.1481225567426));
#50912=CARTESIAN_POINT('Ctrl Pts',(63.1165131117359,6.87689795515155,13.6519556095856));
#50913=CARTESIAN_POINT('Ctrl Pts',(63.166621001802,6.88753276948555,12.4049165190744));
#50914=CARTESIAN_POINT('Ctrl Pts',(63.1870252331573,6.8924666149016,11.907114685837));
#50915=CARTESIAN_POINT('Ctrl Pts',(63.2283614260835,6.90441102490564,10.9098087803523));
#50916=CARTESIAN_POINT('Ctrl Pts',(63.2789666126022,6.92188378938289,9.66026453628725));
#50917=CARTESIAN_POINT('Ctrl Pts',(63.3318608211209,6.94290977387995,8.1549576700279));
#50918=CARTESIAN_POINT('Ctrl Pts',(63.3576559632414,6.95412499495758,7.14673713804403));
#50919=CARTESIAN_POINT('Ctrl Pts',(63.3695506483973,6.95942395216364,6.51574970029781));
#50920=CARTESIAN_POINT('Ctrl Pts',(63.37404243367,6.96148280299519,6.26569418550467));
#50921=CARTESIAN_POINT('Ctrl Pts',(63.3820460089262,6.9654124654468,5.76408603878877));
#50922=CARTESIAN_POINT('Ctrl Pts',(63.3934765388819,6.9717498345268,4.8851799884167));
#50923=CARTESIAN_POINT('Ctrl Pts',(63.4060594893532,6.98214664403403,3.12244904729691));
#50924=CARTESIAN_POINT('Ctrl Pts',(63.3991675704029,6.98667516443248,1.61406737086219));
#50925=CARTESIAN_POINT('Ctrl Pts',(63.3852972835858,6.98713243255313,0.549525775104275));
#50926=CARTESIAN_POINT('Ctrl Pts',(63.3837639990198,6.98625219299159,0.400255301022558));
#50927=CARTESIAN_POINT('Ctrl Pts',(63.3811412856108,6.98092701478105,0.118531957809457));
#50928=CARTESIAN_POINT('Ctrl Pts',(63.3774764614481,6.96352864269567,-0.371543466982117));
#50929=CARTESIAN_POINT('Ctrl Pts',(63.3737734202508,6.92182301979145,-1.04015416616342));
#50930=CARTESIAN_POINT('Ctrl Pts',(63.3679524464333,6.86362502470972,-1.80122588976293));
#50931=CARTESIAN_POINT('Ctrl Pts',(63.3543676733274,6.79529729582811,-2.75769703195224));
#50932=CARTESIAN_POINT('Ctrl Pts',(63.3183836510661,6.76331689501261,-3.84604778170242));
#50933=CARTESIAN_POINT('Ctrl Pts',(63.2579635548131,6.84096872539738,-4.60500935093061));
#50934=CARTESIAN_POINT('Ctrl Pts',(63.2096948711453,6.93185648904187,-5.05892091186654));
#50935=CARTESIAN_POINT('Ctrl Pts',(63.1875270883532,6.97241744695262,-5.23793787000871));
#50936=CARTESIAN_POINT('Ctrl Pts',(63.1325072151405,7.07773702786777,-5.62136260647696));
#50937=CARTESIAN_POINT('Ctrl Pts',(63.0132528713079,7.3211497909772,-6.34163824906952));
#50938=CARTESIAN_POINT('Ctrl Pts',(62.8029591903338,7.82115058001278,-7.49543786075017));
#50939=CARTESIAN_POINT('Ctrl Pts',(62.5936741996999,8.43186353143849,-8.76560234032894));
#50940=CARTESIAN_POINT('Ctrl Pts',(62.4749644958831,8.86097524178464,-9.71157013411916));
#50941=CARTESIAN_POINT('Ctrl Pts',(62.4201981206369,9.09857704453463,-10.2697527203838));
#50942=CARTESIAN_POINT('Ctrl Pts',(62.398078422383,9.21353125528222,-10.5555417660092));
#50943=CARTESIAN_POINT('Ctrl Pts',(62.3840104205132,9.29775257792002,-10.772463221046));
#50944=CARTESIAN_POINT('Ctrl Pts',(62.3807629530719,9.34383659535855,-10.8850870497912));
#50945=CARTESIAN_POINT('Ctrl Pts',(62.3738072198155,9.44544236662011,-11.1302215713694));
#50946=CARTESIAN_POINT('Ctrl Pts',(62.3697513233476,9.62729441691419,-11.5525904946933));
#50947=CARTESIAN_POINT('Ctrl Pts',(62.3837759970867,10.0163201736675,-12.4162142254667));
#50948=CARTESIAN_POINT('Ctrl Pts',(62.4573913421418,10.6023053239374,-13.6872790388798));
#50949=CARTESIAN_POINT('Ctrl Pts',(62.5511457032355,11.0856172382757,-14.9067331093471));
#50950=CARTESIAN_POINT('Ctrl Pts',(62.6046192000456,11.3545866340079,-15.7588167884263));
#50951=CARTESIAN_POINT('Ctrl Pts',(62.6359406541165,11.517469480017,-16.3378185226344));
#50952=CARTESIAN_POINT('Ctrl Pts',(62.6528314507055,11.6183761444237,-16.7844671295404));
#50953=CARTESIAN_POINT('Ctrl Pts',(62.6609105379355,11.6874797908918,-17.1630699070993));
#50954=CARTESIAN_POINT('Ctrl Pts',(62.6638768603096,11.7137656612047,-17.3163953547192));
#50955=CARTESIAN_POINT('Ctrl Pts',(62.6693846908667,11.7590723540921,-17.6187124890694));
#50956=CARTESIAN_POINT('Ctrl Pts',(62.6741202236337,11.7948578504016,-17.918557602196));
#50957=CARTESIAN_POINT('Ctrl Pts',(62.6780970886857,11.8220961938048,-18.2143292670326));
#50958=CARTESIAN_POINT('Ctrl Pts',(62.6802676343343,11.8358525159284,-18.3977339849119));
#50959=CARTESIAN_POINT('Ctrl Pts',(62.6818193623433,11.8450278385985,-18.5434605906301));
#50960=CARTESIAN_POINT('Ctrl Pts',(62.6828920339916,11.8510352847634,-18.6522820837644));
#50961=CARTESIAN_POINT('Ctrl Pts',(62.6837117248072,11.855339726448,-18.742558930143));
#50962=CARTESIAN_POINT('Ctrl Pts',(62.6843229408963,11.8583828851285,-18.8145327501737));
#50963=CARTESIAN_POINT('Ctrl Pts',(62.6892804465,11.8819918798033,-19.4249596018789));
#50964=CARTESIAN_POINT('Ctrl Pts',(62.6909212274186,11.8589387563064,-20.5480089229867));
#50965=CARTESIAN_POINT('Ctrl Pts',(62.6815549707715,11.7610077131498,-22.0779988678205));
#50966=CARTESIAN_POINT('Ctrl Pts',(62.6769765822225,11.7219942672605,-23.0149704733893));
#50967=CARTESIAN_POINT('Ctrl Pts',(62.678220056782,11.7226271915843,-23.5743284523991));
#50968=CARTESIAN_POINT('Ctrl Pts',(62.678644904202,11.7228532665709,-23.832451669843));
#50969=CARTESIAN_POINT('Ctrl Pts',(62.6792855094788,11.723026759193,-24.3286037118354));
#50970=CARTESIAN_POINT('Ctrl Pts',(62.6798847761189,11.7227673230976,-25.2088475010981));
#50971=CARTESIAN_POINT('Ctrl Pts',(62.6795926748682,11.7212741826651,-26.4629661695656));
#50972=CARTESIAN_POINT('Ctrl Pts',(62.6783812027991,11.7193132858567,-27.9721096910006));
#50973=CARTESIAN_POINT('Ctrl Pts',(62.6776646395247,11.7188580444735,-28.9752003144069));
#50974=CARTESIAN_POINT('Ctrl Pts',(62.6774328269539,11.7191365464673,-29.5382568196351));
#50975=CARTESIAN_POINT('Ctrl Pts',(62.6773678117679,11.7192072595742,-29.6634641511824));
#50976=CARTESIAN_POINT('Ctrl Pts',(62.6771988612175,11.7193791972438,-29.9139050923193));
#50977=CARTESIAN_POINT('Ctrl Pts',(62.6768085203825,11.7197566517483,-30.3524295416403));
#50978=CARTESIAN_POINT('Ctrl Pts',(62.6757232234573,11.720782501297,-31.2301444231918));
#50979=CARTESIAN_POINT('Ctrl Pts',(62.6737354365148,11.7228454679361,-32.485293390133));
#50980=CARTESIAN_POINT('Ctrl Pts',(62.6723159850072,11.7252030895258,-33.7400843530539));
#50981=CARTESIAN_POINT('Ctrl Pts',(62.6722120112137,11.7269777063412,-34.7424026860366));
#50982=CARTESIAN_POINT('Ctrl Pts',(62.6726265131155,11.7277869860697,-35.2429657135305));
#50983=CARTESIAN_POINT('Ctrl Pts',(62.6731547159542,11.7283441744651,-35.6190412398323));
#50984=CARTESIAN_POINT('Ctrl Pts',(62.6735967149658,11.7287044977291,-35.8708943236863));
#50985=CARTESIAN_POINT('Ctrl Pts',(62.6747899970285,11.729373041004,-36.3738452418783));
#50986=CARTESIAN_POINT('Ctrl Pts',(62.6775925742435,11.730465877738,-37.2524165673159));
#50987=CARTESIAN_POINT('Ctrl Pts',(62.6851862006745,11.7324561459671,-39.0045608875198));
#50988=CARTESIAN_POINT('Ctrl Pts',(62.6922451067709,11.7347616180926,-40.5049707060355));
#50989=CARTESIAN_POINT('Ctrl Pts',(62.6952068493182,11.737792854927,-41.7597519346065));
#50990=CARTESIAN_POINT('Ctrl Pts',(62.6958432636562,11.7381880744333,-42.1383085302216));
#50991=CARTESIAN_POINT('Ctrl Pts',(62.6963424790514,11.7380992974207,-42.6406967467138));
#50992=CARTESIAN_POINT('Ctrl Pts',(62.6966562218629,11.7377491377675,-43.143320636721));
#50993=CARTESIAN_POINT('Ctrl Pts',(62.6967883997396,11.7370747742033,-43.7706967073052));
#50994=CARTESIAN_POINT('Ctrl Pts',(62.6968136404172,11.7367166265468,-44.5220789304071));
#50995=CARTESIAN_POINT('Ctrl Pts',(62.696959820954,11.7374781356162,-45.1464126012592));
#50996=CARTESIAN_POINT('Ctrl Pts',(62.6972931105947,11.7391196339414,-45.644579362675));
#50997=CARTESIAN_POINT('Ctrl Pts',(62.6976873260218,11.7409726571807,-46.0174643891432));
#50998=CARTESIAN_POINT('Ctrl Pts',(62.6982612772622,11.7435478375997,-46.3895748088443));
#50999=CARTESIAN_POINT('Ctrl Pts',(62.699314289724,11.7480739682818,-46.8845197763614));
#51000=CARTESIAN_POINT('Ctrl Pts',(62.7004802564573,11.7528587259553,-47.2544685737077));
#51001=CARTESIAN_POINT('Ctrl Pts',(62.7019745326836,11.7587656435187,-47.6238213681755));
#51002=CARTESIAN_POINT('Ctrl Pts',(62.7030616556681,11.7638730493905,-47.8582806542546));
#51003=CARTESIAN_POINT('Ctrl Pts',(62.7054176541727,11.778908025164,-48.3400318385945));
#51004=CARTESIAN_POINT('Ctrl Pts',(62.7100281194328,11.8153601828062,-49.1915678567995));
#51005=CARTESIAN_POINT('Ctrl Pts',(62.7177314548789,11.8843055589473,-50.4462446983413));
#51006=CARTESIAN_POINT('Ctrl Pts',(62.7286617221578,11.9499950058551,-52.0062206589874));
#51007=CARTESIAN_POINT('Ctrl Pts',(62.7374616794921,11.9496729009723,-53.083802632839));
#51008=CARTESIAN_POINT('Ctrl Pts',(62.7437552022857,11.9241453339071,-53.7713206746562));
#51009=CARTESIAN_POINT('Ctrl Pts',(62.7467278641718,11.9072308339431,-54.0769989676418));
#51010=CARTESIAN_POINT('Ctrl Pts',(62.7533807248429,11.8563573736431,-54.6556561230826));
#51011=CARTESIAN_POINT('Ctrl Pts',(62.7662999686102,11.7321679192571,-55.6380097865569));
#51012=CARTESIAN_POINT('Ctrl Pts',(62.7933936148545,11.414547770685,-57.4461878152757));
#51013=CARTESIAN_POINT('Ctrl Pts',(62.8076998606852,11.2521153761541,-58.733261786034));
#51014=CARTESIAN_POINT('Ctrl Pts',(62.8180464901747,11.2993569627382,-59.4971585371426));
#51015=CARTESIAN_POINT('Ctrl Pts',(62.8191331598324,11.3069696756115,-59.6104073149356));
#51016=CARTESIAN_POINT('Ctrl Pts',(62.8213202536788,11.3246626827443,-59.8263616687962));
#51017=CARTESIAN_POINT('Ctrl Pts',(62.8249140045037,11.3639265488461,-60.212145946727));
#51018=CARTESIAN_POINT('Ctrl Pts',(62.8313936816921,11.4731898642321,-60.9875725235415));
#51019=CARTESIAN_POINT('Ctrl Pts',(62.8371959216708,11.6643173799114,-61.8925545557377));
#51020=CARTESIAN_POINT('Ctrl Pts',(62.8418437083872,11.9107138368155,-62.8071348176643));
#51021=CARTESIAN_POINT('Ctrl Pts',(62.8441472669097,12.0677119439638,-63.3247042909219));
#51022=CARTESIAN_POINT('Ctrl Pts',(62.8456061691458,12.1790595583554,-63.6704210493343));
#51023=CARTESIAN_POINT('Ctrl Pts',(62.8465622073511,12.2550054220157,-63.9010948539475));
#51024=CARTESIAN_POINT('Ctrl Pts',(62.8475036289829,12.3333877584247,-64.1318738609332));
#51025=CARTESIAN_POINT('Ctrl Pts',(62.8483203676067,12.4039577282718,-64.3339621228141));
#51026=CARTESIAN_POINT('Ctrl Pts',(62.8487869286133,12.4448221972824,-64.4494648452406));
#51027=CARTESIAN_POINT('Ctrl Pts',(62.8494889349193,12.5066336621532,-64.622710503327));
#51028=CARTESIAN_POINT('Ctrl Pts',(62.85007524664,12.5592225331623,-64.7671363855174));
#51029=CARTESIAN_POINT('Ctrl Pts',(62.8510932906693,12.6473190338681,-65.0055968429213));
#51030=CARTESIAN_POINT('Ctrl Pts',(62.8538434577762,12.7301919550291,-65.2185134295923));
#51031=CARTESIAN_POINT('Ctrl Pts',(62.8580322198517,12.9195194071033,-65.6685318447977));
#51032=CARTESIAN_POINT('Ctrl Pts',(62.8648496511971,13.2880665087214,-66.4580453122164));
#51033=CARTESIAN_POINT('Ctrl Pts',(62.8730120924218,14.1681922648577,-68.0970346604163));
#51034=CARTESIAN_POINT('Ctrl Pts',(62.8703191702332,15.0662143539911,-69.5915443941704));
#51035=CARTESIAN_POINT('Ctrl Pts',(62.8648969504777,15.6977083703332,-70.7929890769424));
#51036=CARTESIAN_POINT('Ctrl Pts',(62.8653727258091,15.8265950679221,-71.0375437867453));
#51037=CARTESIAN_POINT('Ctrl Pts',(62.8653378608801,16.091945143954,-71.540060490455));
#51038=CARTESIAN_POINT('Ctrl Pts',(62.8656588470002,16.4219435551466,-72.1627921140557));
#51039=CARTESIAN_POINT('Ctrl Pts',(62.8657732483579,16.8209939328041,-72.9134781847798));
#51040=CARTESIAN_POINT('Ctrl Pts',(62.8660253985644,17.6204977093811,-74.4139671461493));
#51041=CARTESIAN_POINT('Ctrl Pts',(62.8659882824124,18.2903821499167,-75.6668058494398));
#51042=CARTESIAN_POINT('Ctrl Pts',(62.8657236935421,19.2620949450523,-77.4941932451861));
#51043=CARTESIAN_POINT('Ctrl Pts',(62.865838847551,19.6977951217313,-78.3134889537359));
#51044=CARTESIAN_POINT('Ctrl Pts',(62.865838847551,20.1343167091208,-79.1344666558342));
#51045=CARTESIAN_POINT('Ctrl Pts',(63.7696816038415,6.98566143559185,24.8297767096392));
#51046=CARTESIAN_POINT('Ctrl Pts',(63.7698678921138,6.98566675201186,24.7808702678244));
#51047=CARTESIAN_POINT('Ctrl Pts',(63.770063285565,6.98567237256011,24.7319644955167));
#51048=CARTESIAN_POINT('Ctrl Pts',(63.7723701752329,6.98573834934271,24.1810344654839));
#51049=CARTESIAN_POINT('Ctrl Pts',(63.7740711730229,6.9853197046968,23.1764585729357));
#51050=CARTESIAN_POINT('Ctrl Pts',(63.7779926509635,6.98404916981452,21.1672937642235));
#51051=CARTESIAN_POINT('Ctrl Pts',(63.7933492509724,6.98450658438664,19.6629800249552));
#51052=CARTESIAN_POINT('Ctrl Pts',(63.8262474576607,6.98780920603375,18.4119113393576));
#51053=CARTESIAN_POINT('Ctrl Pts',(63.8419144473533,6.98923463277581,17.907607162241));
#51054=CARTESIAN_POINT('Ctrl Pts',(63.8810500167875,6.99255841021727,16.902518936812));
#51055=CARTESIAN_POINT('Ctrl Pts',(63.9649304744712,6.99982554504736,15.1486732817769));
#51056=CARTESIAN_POINT('Ctrl Pts',(64.045922706762,7.00927886130776,13.6515024814671));
#51057=CARTESIAN_POINT('Ctrl Pts',(64.0990790942045,7.01972854564653,12.4033154118975));
#51058=CARTESIAN_POINT('Ctrl Pts',(64.1210943657946,7.02454584913399,11.9050847032849));
#51059=CARTESIAN_POINT('Ctrl Pts',(64.1668633343807,7.0361092645071,10.9072098485462));
#51060=CARTESIAN_POINT('Ctrl Pts',(64.2248180717729,7.05293517703396,9.65737999202147));
#51061=CARTESIAN_POINT('Ctrl Pts',(64.2870324562887,7.07297879196909,8.15222145300158));
#51062=CARTESIAN_POINT('Ctrl Pts',(64.318132387073,7.08355383094343,7.14433253005041));
#51063=CARTESIAN_POINT('Ctrl Pts',(64.3325098039232,7.08845799507042,6.51352704158455));
#51064=CARTESIAN_POINT('Ctrl Pts',(64.3381594740021,7.09024700447211,6.26157340593109));
#51065=CARTESIAN_POINT('Ctrl Pts',(64.349002880189,7.09322958834607,5.7579425291834));
#51066=CARTESIAN_POINT('Ctrl Pts',(64.3664328329182,7.09708822036689,4.87642538977047));
#51067=CARTESIAN_POINT('Ctrl Pts',(64.3919649797897,7.10102666734999,3.11502263829812));
#51068=CARTESIAN_POINT('Ctrl Pts',(64.3878539994614,7.1036005456068,1.61837907716535));
#51069=CARTESIAN_POINT('Ctrl Pts',(64.3636805619995,7.11115149785545,0.566888086807873));
#51070=CARTESIAN_POINT('Ctrl Pts',(64.3607244710463,7.11131284275915,0.418190770104461));
#51071=CARTESIAN_POINT('Ctrl Pts',(64.354643323769,7.10805053627403,0.138129618760668));
#51072=CARTESIAN_POINT('Ctrl Pts',(64.3433926111677,7.09451685315122,-0.349389769171667));
#51073=CARTESIAN_POINT('Ctrl Pts',(64.3251138253951,7.05882182021602,-1.01427458036217));
#51074=CARTESIAN_POINT('Ctrl Pts',(64.2980337169301,7.00853937644289,-1.77080918208802));
#51075=CARTESIAN_POINT('Ctrl Pts',(64.2536264651652,6.95114469802438,-2.72065910584223));
#51076=CARTESIAN_POINT('Ctrl Pts',(64.1798526413958,6.93254514534883,-3.79979071287078));
#51077=CARTESIAN_POINT('Ctrl Pts',(64.1045827204883,7.02209746192965,-4.55524739849757));
#51078=CARTESIAN_POINT('Ctrl Pts',(64.0561043596687,7.12374897730917,-5.0093374304298));
#51079=CARTESIAN_POINT('Ctrl Pts',(64.0353415718871,7.16704405464195,-5.17985062820318));
#51080=CARTESIAN_POINT('Ctrl Pts',(63.98473363006,7.28357400055431,-5.55607874846997));
#51081=CARTESIAN_POINT('Ctrl Pts',(63.8771459519287,7.55714666286979,-6.27006582117503));
#51082=CARTESIAN_POINT('Ctrl Pts',(63.6862239458142,8.12629593123083,-7.43081918066162));
#51083=CARTESIAN_POINT('Ctrl Pts',(63.4899286215678,8.81070481486742,-8.71655424625204));
#51084=CARTESIAN_POINT('Ctrl Pts',(63.3753462052385,9.27819727404204,-9.68536073164948));
#51085=CARTESIAN_POINT('Ctrl Pts',(63.3216748507195,9.53128700469291,-10.2617919553927));
#51086=CARTESIAN_POINT('Ctrl Pts',(63.2997626278364,9.65129343395131,-10.5588427326214));
#51087=CARTESIAN_POINT('Ctrl Pts',(63.2857604236112,9.73807711029578,-10.7852247866449));
#51088=CARTESIAN_POINT('Ctrl Pts',(63.2823617213375,9.78586054723457,-10.9049831939649));
#51089=CARTESIAN_POINT('Ctrl Pts',(63.2754976620879,9.88870298656934,-11.1630548483794));
#51090=CARTESIAN_POINT('Ctrl Pts',(63.2722409143818,10.0681221358058,-11.6063711256514));
#51091=CARTESIAN_POINT('Ctrl Pts',(63.2907849195653,10.4351709496067,-12.5041502226328));
#51092=CARTESIAN_POINT('Ctrl Pts',(63.3791152909834,10.9518091655088,-13.8041091500526));
#51093=CARTESIAN_POINT('Ctrl Pts',(63.4895054865479,11.3517098296877,-15.0210931865357));
#51094=CARTESIAN_POINT('Ctrl Pts',(63.5517804011852,11.5697933201517,-15.8557317029522));
#51095=CARTESIAN_POINT('Ctrl Pts',(63.5882492340872,11.7013443654089,-16.4186590645639));
#51096=CARTESIAN_POINT('Ctrl Pts',(63.607999460131,11.7828835971173,-16.847875169099));
#51097=CARTESIAN_POINT('Ctrl Pts',(63.6178114872258,11.8399722925678,-17.2090989649054));
#51098=CARTESIAN_POINT('Ctrl Pts',(63.6213085239353,11.8623207145412,-17.3601083476327));
#51099=CARTESIAN_POINT('Ctrl Pts',(63.6276475672903,11.900407547536,-17.6552939990412));
#51100=CARTESIAN_POINT('Ctrl Pts',(63.6328094590008,11.9304891212912,-17.9492712973279));
#51101=CARTESIAN_POINT('Ctrl Pts',(63.6368975837894,11.9531961683379,-18.2390478308779));
#51102=CARTESIAN_POINT('Ctrl Pts',(63.6390109632988,11.9646113444201,-18.4189964736862));
#51103=CARTESIAN_POINT('Ctrl Pts',(63.6404502007218,11.9721732543855,-18.5620282108745));
#51104=CARTESIAN_POINT('Ctrl Pts',(63.6414060292637,11.9770986096451,-18.6688979579715));
#51105=CARTESIAN_POINT('Ctrl Pts',(63.6421027861453,11.980601906427,-18.7575928191368));
#51106=CARTESIAN_POINT('Ctrl Pts',(63.6426012395683,11.983062011924,-18.8283338164298));
#51107=CARTESIAN_POINT('Ctrl Pts',(63.6465169594665,12.0020384064807,-19.4284380820498));
#51108=CARTESIAN_POINT('Ctrl Pts',(63.6437665657216,11.9799130102247,-20.5374370938092));
#51109=CARTESIAN_POINT('Ctrl Pts',(63.6262331561345,11.8913092865018,-22.0636011055071));
#51110=CARTESIAN_POINT('Ctrl Pts',(63.6178550717916,11.8553688654383,-23.0089316838751));
#51111=CARTESIAN_POINT('Ctrl Pts',(63.6180369322824,11.8554514432705,-23.5768919709824));
#51112=CARTESIAN_POINT('Ctrl Pts',(63.6180901726606,11.8554515811078,-23.8335704323226));
#51113=CARTESIAN_POINT('Ctrl Pts',(63.6181298419009,11.8553460194198,-24.3296650889028));
#51114=CARTESIAN_POINT('Ctrl Pts',(63.6180477607667,11.8549170294627,-25.2086330940246));
#51115=CARTESIAN_POINT('Ctrl Pts',(63.617617569276,11.8538473380592,-26.4623745102019));
#51116=CARTESIAN_POINT('Ctrl Pts',(63.6169168962429,11.8526439793394,-27.9714303035608));
#51117=CARTESIAN_POINT('Ctrl Pts',(63.6165915435084,11.8524503148402,-28.9751490983386));
#51118=CARTESIAN_POINT('Ctrl Pts',(63.6165192995794,11.8526705637204,-29.5386893428186));
#51119=CARTESIAN_POINT('Ctrl Pts',(63.6164967601456,11.8527266046447,-29.6639149713298));
#51120=CARTESIAN_POINT('Ctrl Pts',(63.6164280037698,11.8528638342163,-29.9144380091037));
#51121=CARTESIAN_POINT('Ctrl Pts',(63.616253499369,11.8531672651109,-30.3530667865238));
#51122=CARTESIAN_POINT('Ctrl Pts',(63.6157408857792,11.8540022964339,-31.2309600714044));
#51123=CARTESIAN_POINT('Ctrl Pts',(63.6148560405522,11.8557046509276,-32.4862181294635));
#51124=CARTESIAN_POINT('Ctrl Pts',(63.6146079535709,11.8576964546748,-33.7409637565676));
#51125=CARTESIAN_POINT('Ctrl Pts',(63.6152919776485,11.8592251366319,-34.7431600757416));
#51126=CARTESIAN_POINT('Ctrl Pts',(63.6160131572755,11.8599271411013,-35.2436261487335));
#51127=CARTESIAN_POINT('Ctrl Pts',(63.6167289651422,11.8604163713172,-35.619620607901));
#51128=CARTESIAN_POINT('Ctrl Pts',(63.6172899438139,11.8607294551642,-35.8714754330862));
#51129=CARTESIAN_POINT('Ctrl Pts',(63.6186993626869,11.8613087578331,-36.37439912327));
#51130=CARTESIAN_POINT('Ctrl Pts',(63.6218187659422,11.8622303558402,-37.2529306311206));
#51131=CARTESIAN_POINT('Ctrl Pts',(63.6298724249999,11.8639299681856,-39.0049923904734));
#51132=CARTESIAN_POINT('Ctrl Pts',(63.6371218535708,11.8659593552387,-40.5053086477893));
#51133=CARTESIAN_POINT('Ctrl Pts',(63.6402975958026,11.8688422992738,-41.7600225880003));
#51134=CARTESIAN_POINT('Ctrl Pts',(63.6410071078334,11.869200696979,-42.1385723752223));
#51135=CARTESIAN_POINT('Ctrl Pts',(63.6416120930757,11.8690739021615,-42.6409445598202));
#51136=CARTESIAN_POINT('Ctrl Pts',(63.642032528753,11.8686874249504,-43.1435512139115));
#51137=CARTESIAN_POINT('Ctrl Pts',(63.6422952454253,11.867973795946,-43.7709012458352));
#51138=CARTESIAN_POINT('Ctrl Pts',(63.6424540668545,11.8675753333189,-44.5222449913211));
#51139=CARTESIAN_POINT('Ctrl Pts',(63.6426771430182,11.868307260696,-45.1465391900779));
#51140=CARTESIAN_POINT('Ctrl Pts',(63.6430445603417,11.8699329547278,-45.6446739195639));
#51141=CARTESIAN_POINT('Ctrl Pts',(63.6434473531315,11.8717750306657,-46.0175326399235));
#51142=CARTESIAN_POINT('Ctrl Pts',(63.6440108357314,11.8743406804985,-46.3896147721523));
#51143=CARTESIAN_POINT('Ctrl Pts',(63.6450217165968,11.878855847725,-46.8845205001939));
#51144=CARTESIAN_POINT('Ctrl Pts',(63.6461202649225,11.8836338117009,-47.2544343843313));
#51145=CARTESIAN_POINT('Ctrl Pts',(63.6475192687113,11.8895347153681,-47.6237524624304));
#51146=CARTESIAN_POINT('Ctrl Pts',(63.6485331967311,11.8946380812674,-47.8581793904239));
#51147=CARTESIAN_POINT('Ctrl Pts',(63.6507112577407,11.9096697449189,-48.3398776255269));
#51148=CARTESIAN_POINT('Ctrl Pts',(63.6549321968964,11.9461224149325,-49.1913321247398));
#51149=CARTESIAN_POINT('Ctrl Pts',(63.661899745935,12.0151105243108,-50.4459332494086));
#51150=CARTESIAN_POINT('Ctrl Pts',(63.6717662960858,12.0808653012226,-52.0058840819985));
#51151=CARTESIAN_POINT('Ctrl Pts',(63.6798092951177,12.0806078845269,-53.0834891683857));
#51152=CARTESIAN_POINT('Ctrl Pts',(63.685631755365,12.0551039347417,-53.7710339616749));
#51153=CARTESIAN_POINT('Ctrl Pts',(63.6884005575708,12.0382035085977,-54.0766930057463));
#51154=CARTESIAN_POINT('Ctrl Pts',(63.6946078413911,11.98735499784,-54.6553335456784));
#51155=CARTESIAN_POINT('Ctrl Pts',(63.7066671306212,11.8632143320451,-55.6376601087274));
#51156=CARTESIAN_POINT('Ctrl Pts',(63.7318747171782,11.5456729000009,-57.445823902878));
#51157=CARTESIAN_POINT('Ctrl Pts',(63.7447371065881,11.3832748414712,-58.7329708717663));
#51158=CARTESIAN_POINT('Ctrl Pts',(63.754538293205,11.430516675957,-59.4970034620545));
#51159=CARTESIAN_POINT('Ctrl Pts',(63.7555614946527,11.4381288101711,-59.6102669072837));
#51160=CARTESIAN_POINT('Ctrl Pts',(63.757633595964,11.4558204399389,-59.8262498407748));
#51161=CARTESIAN_POINT('Ctrl Pts',(63.7610559846096,11.4950820129313,-60.21207989842));
#51162=CARTESIAN_POINT('Ctrl Pts',(63.7673006995254,11.6043374957319,-60.9875811955258));
#51163=CARTESIAN_POINT('Ctrl Pts',(63.7730285030241,11.7954459457701,-61.892608993598));
#51164=CARTESIAN_POINT('Ctrl Pts',(63.7776894929842,12.0418091415548,-62.8071976481216));
#51165=CARTESIAN_POINT('Ctrl Pts',(63.7800137401256,12.1987840166583,-63.3247589036427));
#51166=CARTESIAN_POINT('Ctrl Pts',(63.7814841169113,12.3101155783141,-63.670465471561));
#51167=CARTESIAN_POINT('Ctrl Pts',(63.7824465908856,12.3860503841301,-63.9011311488922));
#51168=CARTESIAN_POINT('Ctrl Pts',(63.7833920679633,12.4644220752372,-64.1319003996215));
#51169=CARTESIAN_POINT('Ctrl Pts',(63.7842086917249,12.5349825047279,-64.3339784746905));
#51170=CARTESIAN_POINT('Ctrl Pts',(63.7846739751752,12.5758415864843,-64.4494749475913));
#51171=CARTESIAN_POINT('Ctrl Pts',(63.7853727382513,12.6376450105055,-64.6227108076007));
#51172=CARTESIAN_POINT('Ctrl Pts',(63.7859534955754,12.6902275539118,-64.7671276588133));
#51173=CARTESIAN_POINT('Ctrl Pts',(63.7869571977421,12.7783138276445,-65.0055722940027));
#51174=CARTESIAN_POINT('Ctrl Pts',(63.7896889391107,12.8611817533433,-65.2184894552572));
#51175=CARTESIAN_POINT('Ctrl Pts',(63.7938509211842,13.0504980009258,-65.6685005511499));
#51176=CARTESIAN_POINT('Ctrl Pts',(63.8006373935899,13.4190322005449,-66.4580084393605));
#51177=CARTESIAN_POINT('Ctrl Pts',(63.8087973635566,14.2991477292712,-68.0969899064714));
#51178=CARTESIAN_POINT('Ctrl Pts',(63.8061589029106,15.1971835373538,-69.5915021464135));
#51179=CARTESIAN_POINT('Ctrl Pts',(63.8007532551723,15.8286835484324,-70.79295089124));
#51180=CARTESIAN_POINT('Ctrl Pts',(63.8012281362553,15.9575693622819,-71.0375049654813));
#51181=CARTESIAN_POINT('Ctrl Pts',(63.80119393312,16.2229190548772,-71.5400213331366));
#51182=CARTESIAN_POINT('Ctrl Pts',(63.8015145278415,16.5529169158553,-72.1627523725029));
#51183=CARTESIAN_POINT('Ctrl Pts',(63.8016287284012,16.9519670659933,-72.9134380477093));
#51184=CARTESIAN_POINT('Ctrl Pts',(63.8018798688152,17.7514707684386,-74.4139264495771));
#51185=CARTESIAN_POINT('Ctrl Pts',(63.8018421662859,18.4213568004002,-75.6667657179307));
#51186=CARTESIAN_POINT('Ctrl Pts',(63.8015784260252,19.3930708108336,-77.4941542216223));
#51187=CARTESIAN_POINT('Ctrl Pts',(63.8016933902503,19.8287710106649,-78.3134497248231));
#51188=CARTESIAN_POINT('Ctrl Pts',(63.8016933902503,20.2652925980544,-79.1344274269214));
#51189=CARTESIAN_POINT('Ctrl Pts',(64.7051644480017,7.116408924445,24.8300078402108));
#51190=CARTESIAN_POINT('Ctrl Pts',(64.7053377316389,7.11641758404992,24.7811081862549));
#51191=CARTESIAN_POINT('Ctrl Pts',(64.7055194879703,7.11642663879709,24.7322093827696));
#51192=CARTESIAN_POINT('Ctrl Pts',(64.7076663238738,7.11653619539653,24.1813574002294));
#51193=CARTESIAN_POINT('Ctrl Pts',(64.7089333530155,7.11620394562584,23.1767995651906));
#51194=CARTESIAN_POINT('Ctrl Pts',(64.7116337977528,7.1151212164358,21.1678109264179));
#51195=CARTESIAN_POINT('Ctrl Pts',(64.7259372767009,7.11587257535556,19.6636235887676));
#51196=CARTESIAN_POINT('Ctrl Pts',(64.7581661701847,7.11956838042874,18.4126884759235));
#51197=CARTESIAN_POINT('Ctrl Pts',(64.7733686324166,7.12124444398637,17.9090536171669));
#51198=CARTESIAN_POINT('Ctrl Pts',(64.8110765201189,7.12531406955845,16.9043953209941));
#51199=CARTESIAN_POINT('Ctrl Pts',(64.8919838728444,7.13421361679888,15.1502768679816));
#51200=CARTESIAN_POINT('Ctrl Pts',(64.9721346453416,7.14443725626699,13.6507990842287));
#51201=CARTESIAN_POINT('Ctrl Pts',(65.0286064914778,7.15405321817069,12.3998864389711));
#51202=CARTESIAN_POINT('Ctrl Pts',(65.0524238497418,7.15838930231741,11.9005515076783));
#51203=CARTESIAN_POINT('Ctrl Pts',(65.1033124598707,7.16848098141989,10.9011803927829));
#51204=CARTESIAN_POINT('Ctrl Pts',(65.1695026290478,7.1826159281451,9.6504907924942));
#51205=CARTESIAN_POINT('Ctrl Pts',(65.2424382899957,7.19881941234379,8.14580949006214));
#51206=CARTESIAN_POINT('Ctrl Pts',(65.279415387021,7.20694536660956,7.13907151701641));
#51207=CARTESIAN_POINT('Ctrl Pts',(65.2966875219862,7.21061662674163,6.50907888376672));
#51208=CARTESIAN_POINT('Ctrl Pts',(65.3036787475355,7.21175047116428,6.25454693463909));
#51209=CARTESIAN_POINT('Ctrl Pts',(65.3178846915829,7.21280660662359,5.74832922553668));
#51210=CARTESIAN_POINT('Ctrl Pts',(65.3424912086468,7.21212906964805,4.86351419160469));
#51211=CARTESIAN_POINT('Ctrl Pts',(65.3844723448837,7.20489497920306,3.10426541017931));
#51212=CARTESIAN_POINT('Ctrl Pts',(65.3858137145825,7.20635092613468,1.62312142967191));
#51213=CARTESIAN_POINT('Ctrl Pts',(65.3481542401232,7.2251071791514,0.591055189956906));
#51214=CARTESIAN_POINT('Ctrl Pts',(65.3433461152336,7.22703081940691,0.44438325056417));
#51215=CARTESIAN_POINT('Ctrl Pts',(65.3327329810604,7.22742217338679,0.168378150486671));
#51216=CARTESIAN_POINT('Ctrl Pts',(65.3115151626867,7.22106840646313,-0.31248537606016));
#51217=CARTESIAN_POINT('Ctrl Pts',(65.2743678438677,7.19689004199902,-0.968906342622114));
#51218=CARTESIAN_POINT('Ctrl Pts',(65.2201659061355,7.16070318601945,-1.71729646420262));
#51219=CARTESIAN_POINT('Ctrl Pts',(65.138127961995,7.12149506286709,-2.65933294316632));
#51220=CARTESIAN_POINT('Ctrl Pts',(65.0212677514518,7.12265966426902,-3.7353594689389));
#51221=CARTESIAN_POINT('Ctrl Pts',(64.9316222306538,7.22839559664225,-4.49980537871026));
#51222=CARTESIAN_POINT('Ctrl Pts',(64.8840064123095,7.34336633938095,-4.9622184634216));
#51223=CARTESIAN_POINT('Ctrl Pts',(64.8654860744028,7.39011619218726,-5.12730050726085));
#51224=CARTESIAN_POINT('Ctrl Pts',(64.8212346614502,7.51900353960278,-5.50122851333676));
#51225=CARTESIAN_POINT('Ctrl Pts',(64.7296348616273,7.82305607592105,-6.21448621908583));
#51226=CARTESIAN_POINT('Ctrl Pts',(64.5653983284746,8.45591926839147,-7.38356887466015));
#51227=CARTESIAN_POINT('Ctrl Pts',(64.3894189549537,9.2044426119807,-8.68093399280264));
#51228=CARTESIAN_POINT('Ctrl Pts',(64.2833592573959,9.70429145696223,-9.66825308483886));
#51229=CARTESIAN_POINT('Ctrl Pts',(64.2329302649014,9.96981790534443,-10.260255099096));
#51230=CARTESIAN_POINT('Ctrl Pts',(64.2121358258074,10.0934659819557,-10.5671612632986));
#51231=CARTESIAN_POINT('Ctrl Pts',(64.1987940709705,10.1817853643353,-10.8019331896955));
#51232=CARTESIAN_POINT('Ctrl Pts',(64.1954277904282,10.2307787537786,-10.9286766181756));
#51233=CARTESIAN_POINT('Ctrl Pts',(64.1890543368135,10.333726963384,-11.1992781972767));
#51234=CARTESIAN_POINT('Ctrl Pts',(64.1870161213236,10.5087215932017,-11.6633744855384));
#51235=CARTESIAN_POINT('Ctrl Pts',(64.2100564700399,10.849714601789,-12.5959843412346));
#51236=CARTESIAN_POINT('Ctrl Pts',(64.3099262271591,11.2916795511846,-13.926060762851));
#51237=CARTESIAN_POINT('Ctrl Pts',(64.4314133690616,11.6068604287468,-15.1387472185044));
#51238=CARTESIAN_POINT('Ctrl Pts',(64.4991553033842,11.7749762761074,-15.9542459159056));
#51239=CARTESIAN_POINT('Ctrl Pts',(64.5387721490654,11.8761248705765,-16.5000309301001));
#51240=CARTESIAN_POINT('Ctrl Pts',(64.5602746005103,11.9393429310418,-16.9112726833083));
#51241=CARTESIAN_POINT('Ctrl Pts',(64.5712560875011,11.9851279878435,-17.2549405326659));
#51242=CARTESIAN_POINT('Ctrl Pts',(64.5751173799452,12.0036216300577,-17.4032968766163));
#51243=CARTESIAN_POINT('Ctrl Pts',(64.5819960563146,12.0348061971104,-17.6908970949841));
#51244=CARTESIAN_POINT('Ctrl Pts',(64.5874005454603,12.0595013591101,-17.9785789158532));
#51245=CARTESIAN_POINT('Ctrl Pts',(64.5914977476405,12.0780348571595,-18.2620220641703));
#51246=CARTESIAN_POINT('Ctrl Pts',(64.5935263039422,12.0873359651854,-18.4383221303805));
#51247=CARTESIAN_POINT('Ctrl Pts',(64.5948496094316,12.093471000405,-18.5785196944922));
#51248=CARTESIAN_POINT('Ctrl Pts',(64.5956954738538,12.0974554188175,-18.6833389389178));
#51249=CARTESIAN_POINT('Ctrl Pts',(64.5962825131139,12.1002766722583,-18.7703750310557));
#51250=CARTESIAN_POINT('Ctrl Pts',(64.5966829631923,12.1022495682262,-18.8398241225591));
#51251=CARTESIAN_POINT('Ctrl Pts',(64.5997081438088,12.1174140974332,-19.429125594599));
#51252=CARTESIAN_POINT('Ctrl Pts',(64.5935514726399,12.0978119383031,-20.523616605654));
#51253=CARTESIAN_POINT('Ctrl Pts',(64.5700582332538,12.0211834039782,-22.0464062828513));
#51254=CARTESIAN_POINT('Ctrl Pts',(64.5591540788071,11.9893996189005,-23.0012058052287));
#51255=CARTESIAN_POINT('Ctrl Pts',(64.5586478717312,11.9891742673814,-23.5785306049086));
#51256=CARTESIAN_POINT('Ctrl Pts',(64.5584554623995,11.9890788471195,-23.8338647853036));
#51257=CARTESIAN_POINT('Ctrl Pts',(64.5581062924057,11.9888665684243,-24.330175180966));
#51258=CARTESIAN_POINT('Ctrl Pts',(64.5575807630889,11.9884492160853,-25.2081942502245));
#51259=CARTESIAN_POINT('Ctrl Pts',(64.5570784245764,11.9878231887438,-26.4618175147749));
#51260=CARTESIAN_POINT('Ctrl Pts',(64.5568079816915,11.9873249387177,-27.9709194770668));
#51261=CARTESIAN_POINT('Ctrl Pts',(64.5568342751215,11.9873189576655,-28.9752550644233));
#51262=CARTESIAN_POINT('Ctrl Pts',(64.556881406146,11.9874619766805,-29.5392444787746));
#51263=CARTESIAN_POINT('Ctrl Pts',(64.5568870580478,11.9874981317671,-29.6645309762994));
#51264=CARTESIAN_POINT('Ctrl Pts',(64.5568864496663,11.9875848055615,-29.9151901610847));
#51265=CARTESIAN_POINT('Ctrl Pts',(64.5568586814735,11.9877733062284,-30.3540233528818));
#51266=CARTESIAN_POINT('Ctrl Pts',(64.5567348204472,11.9882812665427,-31.2322527065777));
#51267=CARTESIAN_POINT('Ctrl Pts',(64.5565930177403,11.9893111427986,-32.4877533171019));
#51268=CARTESIAN_POINT('Ctrl Pts',(64.5571102567688,11.9905299977796,-33.7424380807836));
#51269=CARTESIAN_POINT('Ctrl Pts',(64.5582850642549,11.9914937807235,-34.7444188305187));
#51270=CARTESIAN_POINT('Ctrl Pts',(64.5591916232676,11.9919571000629,-35.2447088874826));
#51271=CARTESIAN_POINT('Ctrl Pts',(64.560014903911,11.9922875235368,-35.6205538474929));
#51272=CARTESIAN_POINT('Ctrl Pts',(64.5606423843809,11.9924959468476,-35.8724151994287));
#51273=CARTESIAN_POINT('Ctrl Pts',(64.5621629227882,11.9928662115165,-36.375292038802));
#51274=CARTESIAN_POINT('Ctrl Pts',(64.5654294808747,11.9934431707212,-37.2537654623141));
#51275=CARTESIAN_POINT('Ctrl Pts',(64.5736110546591,11.9944766845492,-39.0056869199685));
#51276=CARTESIAN_POINT('Ctrl Pts',(64.5808488152006,11.9960885048588,-40.5058778756516));
#51277=CARTESIAN_POINT('Ctrl Pts',(64.5840919930745,11.998692499389,-41.7604850705067));
#51278=CARTESIAN_POINT('Ctrl Pts',(64.5848300484984,11.9989679793655,-42.1390216083991));
#51279=CARTESIAN_POINT('Ctrl Pts',(64.5854822617532,11.998737275502,-42.6413621623367));
#51280=CARTESIAN_POINT('Ctrl Pts',(64.5859544069295,11.9982544377607,-43.1439364206192));
#51281=CARTESIAN_POINT('Ctrl Pts',(64.5862845444706,11.9974332527632,-43.7712388965695));
#51282=CARTESIAN_POINT('Ctrl Pts',(64.5865132311935,11.996928669566,-44.5225165702291));
#51283=CARTESIAN_POINT('Ctrl Pts',(64.5867722507586,11.9975928091762,-45.1467473655363));
#51284=CARTESIAN_POINT('Ctrl Pts',(64.5871458137777,11.9991734720114,-45.6448259117841));
#51285=CARTESIAN_POINT('Ctrl Pts',(64.5875405637534,12.0009882992427,-46.017639988042));
#51286=CARTESIAN_POINT('Ctrl Pts',(64.5880812445665,12.0035329507914,-46.389674977256));
#51287=CARTESIAN_POINT('Ctrl Pts',(64.58903925609,12.0080285644188,-46.884514076738));
#51288=CARTESIAN_POINT('Ctrl Pts',(64.5900704047181,12.0128018055357,-47.2543749322652));
#51289=CARTESIAN_POINT('Ctrl Pts',(64.5913788092078,12.018704641493,-47.6236360390374));
#51290=CARTESIAN_POINT('Ctrl Pts',(64.5923259078638,12.0238118420256,-47.8580083019323));
#51291=CARTESIAN_POINT('Ctrl Pts',(64.5943469155263,12.0388642729446,-48.3396172101738));
#51292=CARTESIAN_POINT('Ctrl Pts',(64.598236438171,12.0753873612504,-49.1909349420587));
#51293=CARTESIAN_POINT('Ctrl Pts',(64.604589974817,12.1445490533975,-50.445413008557));
#51294=CARTESIAN_POINT('Ctrl Pts',(64.6135711070628,12.2106012572339,-52.005316948034));
#51295=CARTESIAN_POINT('Ctrl Pts',(64.6209720428472,12.2105364455327,-53.0829618288254));
#51296=CARTESIAN_POINT('Ctrl Pts',(64.6263938213671,12.1851433349393,-53.7705517051657));
#51297=CARTESIAN_POINT('Ctrl Pts',(64.6289890533431,12.168300433645,-54.0761677617449));
#51298=CARTESIAN_POINT('Ctrl Pts',(64.6348195106565,12.1175678410791,-54.6547705509414));
#51299=CARTESIAN_POINT('Ctrl Pts',(64.6461529446247,11.9936343662937,-55.6370418971346));
#51300=CARTESIAN_POINT('Ctrl Pts',(64.6697751752082,11.6764941201765,-57.4452006237545));
#51301=CARTESIAN_POINT('Ctrl Pts',(64.6814108650537,11.5142323582384,-58.7324797036675));
#51302=CARTESIAN_POINT('Ctrl Pts',(64.6907380805086,11.5615131816963,-59.4967522491422));
#51303=CARTESIAN_POINT('Ctrl Pts',(64.6917061998664,11.5691335623824,-59.6100417519035));
#51304=CARTESIAN_POINT('Ctrl Pts',(64.6936774844079,11.5868372471862,-59.8260754687692));
#51305=CARTESIAN_POINT('Ctrl Pts',(64.6969467821477,11.6261143248605,-60.2119861150514));
#51306=CARTESIAN_POINT('Ctrl Pts',(64.7029706707221,11.7353764924318,-60.9876187997222));
#51307=CARTESIAN_POINT('Ctrl Pts',(64.708601255582,11.9264435194088,-61.8927265572519));
#51308=CARTESIAN_POINT('Ctrl Pts',(64.7132409633046,12.1727368523407,-62.8073341711799));
#51309=CARTESIAN_POINT('Ctrl Pts',(64.7155668810181,12.3296674972552,-63.3248851479995));
#51310=CARTESIAN_POINT('Ctrl Pts',(64.7170377866538,12.4409692098032,-63.6705764933628));
#51311=CARTESIAN_POINT('Ctrl Pts',(64.7180000959491,12.516884389208,-63.9012298813615));
#51312=CARTESIAN_POINT('Ctrl Pts',(64.7189438441818,12.5952365311638,-64.1319835338068));
#51313=CARTESIAN_POINT('Ctrl Pts',(64.7197566706395,12.6657808414747,-64.3340452126826));
#51314=CARTESIAN_POINT('Ctrl Pts',(64.7202189568698,12.7066309878131,-64.4495315147314));
#51315=CARTESIAN_POINT('Ctrl Pts',(64.7209123254143,12.7684213551073,-64.6227513556222));
#51316=CARTESIAN_POINT('Ctrl Pts',(64.7214864980503,12.8209935770223,-64.76715311935));
#51317=CARTESIAN_POINT('Ctrl Pts',(64.7224757287238,12.9090644458765,-65.0055712328325));
#51318=CARTESIAN_POINT('Ctrl Pts',(64.7251908376815,12.9919278859981,-65.2184917956168));
#51319=CARTESIAN_POINT('Ctrl Pts',(64.7293290180449,13.1812312427184,-65.668493382022));
#51320=CARTESIAN_POINT('Ctrl Pts',(64.736090236661,13.5497510630374,-66.4579956692628));
#51321=CARTESIAN_POINT('Ctrl Pts',(64.7442571039241,14.4298545252654,-68.0969663258554));
#51322=CARTESIAN_POINT('Ctrl Pts',(64.7416692429259,15.3278999041524,-69.5914813224));
#51323=CARTESIAN_POINT('Ctrl Pts',(64.7362702143423,15.9594013041192,-70.792934567142));
#51324=CARTESIAN_POINT('Ctrl Pts',(64.7367447246466,16.0882861195186,-71.037487791828));
#51325=CARTESIAN_POINT('Ctrl Pts',(64.7367107895737,16.3536348916276,-71.5400036063225));
#51326=CARTESIAN_POINT('Ctrl Pts',(64.7370311378445,16.6836316372613,-72.1627337480955));
#51327=CARTESIAN_POINT('Ctrl Pts',(64.7371452341623,17.0826813009422,-72.9134187811415));
#51328=CARTESIAN_POINT('Ctrl Pts',(64.7373959106816,17.8821848341678,-74.4139062621009));
#51329=CARTESIAN_POINT('Ctrl Pts',(64.7373575913811,18.5520718028474,-75.6667460982806));
#51330=CARTESIAN_POINT('Ctrl Pts',(64.7370939145941,19.5237863885987,-77.4941361560859));
#51331=CARTESIAN_POINT('Ctrl Pts',(64.7372086991403,19.9594861833032,-78.3134312752707));
#51332=CARTESIAN_POINT('Ctrl Pts',(64.7372086991403,20.3960077706927,-79.134408977369));
#51333=CARTESIAN_POINT('Ctrl Pts',(65.8737924036832,7.27972362482747,24.830719708439));
#51334=CARTESIAN_POINT('Ctrl Pts',(65.8739508172382,7.27974807209772,24.7818433134185));
#51335=CARTESIAN_POINT('Ctrl Pts',(65.874117012026,7.27977377214088,24.7329682485245));
#51336=CARTESIAN_POINT('Ctrl Pts',(65.8760799171986,7.28007502125495,24.182387718394));
#51337=CARTESIAN_POINT('Ctrl Pts',(65.8768102200667,7.28016042533186,23.1780799047975));
#51338=CARTESIAN_POINT('Ctrl Pts',(65.8780004617329,7.28030066667095,21.169620222429));
#51339=CARTESIAN_POINT('Ctrl Pts',(65.8911077508792,7.28229576947915,19.665670039577));
#51340=CARTESIAN_POINT('Ctrl Pts',(65.9227618899891,7.28723028562115,18.4149091012139));
#51341=CARTESIAN_POINT('Ctrl Pts',(65.937553649303,7.28968195281574,17.9129514766427));
#51342=CARTESIAN_POINT('Ctrl Pts',(65.9740318210956,7.29600607013808,16.9094461468704));
#51343=CARTESIAN_POINT('Ctrl Pts',(66.052400367403,7.30966848395803,15.1549455903662));
#51344=CARTESIAN_POINT('Ctrl Pts',(66.1324413024313,7.32212732942626,13.6500845762898));
#51345=CARTESIAN_POINT('Ctrl Pts',(66.1926144093613,7.32878968779399,12.3922404302263));
#51346=CARTESIAN_POINT('Ctrl Pts',(66.2184460262715,7.33140049277579,11.889861993171));
#51347=CARTESIAN_POINT('Ctrl Pts',(66.2749869489222,7.33634110993353,10.8863037890924));
#51348=CARTESIAN_POINT('Ctrl Pts',(66.3506619970192,7.34181448430412,9.63295368880396));
#51349=CARTESIAN_POINT('Ctrl Pts',(66.4352056598121,7.34676377096916,8.12930385968051));
#51350=CARTESIAN_POINT('Ctrl Pts',(66.478136134215,7.34879358540089,7.12596809701373));
#51351=CARTESIAN_POINT('Ctrl Pts',(66.4976942337235,7.34962526288238,6.49871069230604));
#51352=CARTESIAN_POINT('Ctrl Pts',(66.5058488789386,7.3492667756571,6.23927695465185));
#51353=CARTESIAN_POINT('Ctrl Pts',(66.5229619736932,7.34631065962563,5.72839423002403));
#51354=CARTESIAN_POINT('Ctrl Pts',(66.5537894968395,7.33657879141901,4.83765269592994));
#51355=CARTESIAN_POINT('Ctrl Pts',(66.6076953182298,7.30860900780446,3.08462563305782));
#51356=CARTESIAN_POINT('Ctrl Pts',(66.6059773542651,7.30441857674907,1.63634923035219));
#51357=CARTESIAN_POINT('Ctrl Pts',(66.5525035252899,7.34205993182231,0.639509927514526));
#51358=CARTESIAN_POINT('Ctrl Pts',(66.5454972435413,7.34687556071208,0.498621633521989));
#51359=CARTESIAN_POINT('Ctrl Pts',(66.5295692371147,7.35384522301292,0.232470692643993));
#51360=CARTESIAN_POINT('Ctrl Pts',(66.4967140612984,7.36146043161841,-0.232522042960739));
#51361=CARTESIAN_POINT('Ctrl Pts',(66.4370554102342,7.36240274310148,-0.871660388794319));
#51362=CARTESIAN_POINT('Ctrl Pts',(66.3499379299258,7.35979327114988,-1.60636393970138));
#51363=CARTESIAN_POINT('Ctrl Pts',(66.2205880386724,7.36471254279015,-2.53912840525394));
#51364=CARTESIAN_POINT('Ctrl Pts',(66.0504853909669,7.41083991360725,-3.62275211870216));
#51365=CARTESIAN_POINT('Ctrl Pts',(65.9458978498926,7.54818163125836,-4.42265037276126));
#51366=CARTESIAN_POINT('Ctrl Pts',(65.9003376268575,7.68627547992059,-4.91125268444285));
#51367=CARTESIAN_POINT('Ctrl Pts',(65.8857974344671,7.7395375765202,-5.07593826553621));
#51368=CARTESIAN_POINT('Ctrl Pts',(65.851550679021,7.88692863191168,-5.45610951698722));
#51369=CARTESIAN_POINT('Ctrl Pts',(65.7838109216027,8.2291281944258,-6.1772119318308));
#51370=CARTESIAN_POINT('Ctrl Pts',(65.6592480872348,8.92455344306608,-7.35621915105546));
#51371=CARTESIAN_POINT('Ctrl Pts',(65.5197104055659,9.72490024945947,-8.66369594631866));
#51372=CARTESIAN_POINT('Ctrl Pts',(65.4332486345925,10.2469747370881,-9.66784137781621));
#51373=CARTESIAN_POINT('Ctrl Pts',(65.3915395824349,10.5189069855576,-10.2740459695132));
#51374=CARTESIAN_POINT('Ctrl Pts',(65.3741909497076,10.6431397110077,-10.5899292385663));
#51375=CARTESIAN_POINT('Ctrl Pts',(65.3630348686882,10.7306814906878,-10.8323698730741));
#51376=CARTESIAN_POINT('Ctrl Pts',(65.3602648479762,10.7799034008029,-10.9672831411013));
#51377=CARTESIAN_POINT('Ctrl Pts',(65.3555790293633,10.8802607991245,-11.2519472653632));
#51378=CARTESIAN_POINT('Ctrl Pts',(65.3562655432189,11.0454233414466,-11.740082914407));
#51379=CARTESIAN_POINT('Ctrl Pts',(65.3850343039264,11.3464970901329,-12.7135974761297));
#51380=CARTESIAN_POINT('Ctrl Pts',(65.4920620350658,11.6891954949238,-14.0786275442094));
#51381=CARTESIAN_POINT('Ctrl Pts',(65.6153815271947,11.9022605191301,-15.2820323810785));
#51382=CARTESIAN_POINT('Ctrl Pts',(65.6832508100979,12.0135101653315,-16.0726545200068));
#51383=CARTESIAN_POINT('Ctrl Pts',(65.7229408331874,12.0806916995302,-16.5970732688898));
#51384=CARTESIAN_POINT('Ctrl Pts',(65.7446229165371,12.1239928860792,-16.9868636471961));
#51385=CARTESIAN_POINT('Ctrl Pts',(65.7561104052002,12.1574777034339,-17.3100775064337));
#51386=CARTESIAN_POINT('Ctrl Pts',(65.7601334531901,12.1714935706227,-17.4547857382721));
#51387=CARTESIAN_POINT('Ctrl Pts',(65.7672145337002,12.1948950758284,-17.7328729709252));
#51388=CARTESIAN_POINT('Ctrl Pts',(65.7726548632663,12.2135323017902,-18.0125373060938));
#51389=CARTESIAN_POINT('Ctrl Pts',(65.7766652600269,12.2274898916777,-18.2880871043883));
#51390=CARTESIAN_POINT('Ctrl Pts',(65.7785927735464,12.234507621214,-18.4598334864742));
#51391=CARTESIAN_POINT('Ctrl Pts',(65.7798115376444,12.2391332042683,-18.5965121130943));
#51392=CARTESIAN_POINT('Ctrl Pts',(65.7805676453171,12.2421378889634,-18.698786873932));
#51393=CARTESIAN_POINT('Ctrl Pts',(65.7810710484178,12.2442641987468,-18.7837683048892));
#51394=CARTESIAN_POINT('Ctrl Pts',(65.7813998146423,12.2457504059072,-18.8516184625018));
#51395=CARTESIAN_POINT('Ctrl Pts',(65.7837868785876,12.2571684848512,-19.4275595821506));
#51396=CARTESIAN_POINT('Ctrl Pts',(65.775621119517,12.2421443708687,-20.5042456873665));
#51397=CARTESIAN_POINT('Ctrl Pts',(65.7489945935547,12.182244252697,-22.0232569275389));
#51398=CARTESIAN_POINT('Ctrl Pts',(65.7368006727203,12.1568935455233,-22.9902043797373));
#51399=CARTESIAN_POINT('Ctrl Pts',(65.735881815348,12.1567382779436,-23.5794953406884));
#51400=CARTESIAN_POINT('Ctrl Pts',(65.7355519854163,12.1566846906698,-23.8333229661963));
#51401=CARTESIAN_POINT('Ctrl Pts',(65.7350187722687,12.1566038370863,-24.3301850550868));
#51402=CARTESIAN_POINT('Ctrl Pts',(65.7343892144717,12.1565210061183,-25.2074750919231));
#51403=CARTESIAN_POINT('Ctrl Pts',(65.734204367445,12.1565279610149,-26.4614142145459));
#51404=CARTESIAN_POINT('Ctrl Pts',(65.7345785465822,12.1566258136834,-27.9707176947722));
#51405=CARTESIAN_POINT('Ctrl Pts',(65.7348957843501,12.1566692990628,-28.9756419058403));
#51406=CARTESIAN_POINT('Ctrl Pts',(65.73499335781,12.1566700253318,-29.5400152762751));
#51407=CARTESIAN_POINT('Ctrl Pts',(65.7350113611297,12.1566698453262,-29.6653982285895));
#51408=CARTESIAN_POINT('Ctrl Pts',(65.7350357450659,12.1566666612928,-29.9162329999839));
#51409=CARTESIAN_POINT('Ctrl Pts',(65.7350528642071,12.1566545758727,-30.3553462864775));
#51410=CARTESIAN_POINT('Ctrl Pts',(65.7350212283644,12.1566115529058,-31.2340211692203));
#51411=CARTESIAN_POINT('Ctrl Pts',(65.7350004144236,12.1565345212241,-32.4898442622548));
#51412=CARTESIAN_POINT('Ctrl Pts',(65.7355825509547,12.1565358623201,-33.7444453855406));
#51413=CARTESIAN_POINT('Ctrl Pts',(65.7367503236109,12.1566441564589,-34.7461353310499));
#51414=CARTESIAN_POINT('Ctrl Pts',(65.737626123592,12.1567431118176,-35.2461922563658));
#51415=CARTESIAN_POINT('Ctrl Pts',(65.7384156043536,12.1568380753438,-35.621838751668));
#51416=CARTESIAN_POINT('Ctrl Pts',(65.7390146685704,12.1568893906108,-35.8737074001352));
#51417=CARTESIAN_POINT('Ctrl Pts',(65.7404592386519,12.1569543472302,-36.376520769494));
#51418=CARTESIAN_POINT('Ctrl Pts',(65.7435442296114,12.1570041167726,-37.2549134713066));
#51419=CARTESIAN_POINT('Ctrl Pts',(65.7512391420775,12.157082948218,-39.0066502662914));
#51420=CARTESIAN_POINT('Ctrl Pts',(65.7580076945452,12.1580020051857,-40.5066591357687));
#51421=CARTESIAN_POINT('Ctrl Pts',(65.7610437102886,12.1601730856183,-41.7611157742616));
#51422=CARTESIAN_POINT('Ctrl Pts',(65.7617352350437,12.160327216616,-42.1396320632631));
#51423=CARTESIAN_POINT('Ctrl Pts',(65.7623464778483,12.1599518390054,-42.6419294274402));
#51424=CARTESIAN_POINT('Ctrl Pts',(65.7627881425271,12.1593327211339,-43.1444589945198));
#51425=CARTESIAN_POINT('Ctrl Pts',(65.7630951305003,12.1583595684145,-43.7716969484013));
#51426=CARTESIAN_POINT('Ctrl Pts',(65.7633030202572,12.1577030883427,-44.5228852355069));
#51427=CARTESIAN_POINT('Ctrl Pts',(65.7635365165661,12.158267411624,-45.1470299426665));
#51428=CARTESIAN_POINT('Ctrl Pts',(65.763877580132,12.1597882142212,-45.6450361333077));
#51429=CARTESIAN_POINT('Ctrl Pts',(65.7642392853216,12.1615669803864,-46.0177924223416));
#51430=CARTESIAN_POINT('Ctrl Pts',(65.7647362832457,12.1640849783657,-46.3897663728969));
#51431=CARTESIAN_POINT('Ctrl Pts',(65.7656192323513,12.1685577943658,-46.884520536456));
#51432=CARTESIAN_POINT('Ctrl Pts',(65.7665716015208,12.173328871499,-47.2543106941164));
#51433=CARTESIAN_POINT('Ctrl Pts',(65.7677823268629,12.1792395220295,-47.6234988671514));
#51434=CARTESIAN_POINT('Ctrl Pts',(65.768660862589,12.1843559187658,-47.8578016457596));
#51435=CARTESIAN_POINT('Ctrl Pts',(65.7705320125628,12.1994478294434,-48.3392960083222));
#51436=CARTESIAN_POINT('Ctrl Pts',(65.7741265585029,12.2360873515124,-49.1904350310024));
#51437=CARTESIAN_POINT('Ctrl Pts',(65.7799734947423,12.305546019183,-50.4447401645545));
#51438=CARTESIAN_POINT('Ctrl Pts',(65.7882309135466,12.3720591124559,-52.004565952058));
#51439=CARTESIAN_POINT('Ctrl Pts',(65.7950932312151,12.3723191345176,-53.0822510115124));
#51440=CARTESIAN_POINT('Ctrl Pts',(65.8001647624651,12.3470993371356,-53.7698948839355));
#51441=CARTESIAN_POINT('Ctrl Pts',(65.8026093112487,12.3303424812056,-54.0754504737583));
#51442=CARTESIAN_POINT('Ctrl Pts',(65.80811148906,12.2797835304874,-54.6539989744145));
#51443=CARTESIAN_POINT('Ctrl Pts',(65.8188108636188,12.1561703997236,-55.6361936231354));
#51444=CARTESIAN_POINT('Ctrl Pts',(65.8410155509584,11.8396438854787,-57.4443509994081));
#51445=CARTESIAN_POINT('Ctrl Pts',(65.8515345739574,11.6776885026692,-58.7318267365958));
#51446=CARTESIAN_POINT('Ctrl Pts',(65.8604129888326,11.7250675012197,-59.4964199594489));
#51447=CARTESIAN_POINT('Ctrl Pts',(65.861327518522,11.7327010985785,-59.6097436907726));
#51448=CARTESIAN_POINT('Ctrl Pts',(65.8631991793557,11.750426218956,-59.8258444305473));
#51449=CARTESIAN_POINT('Ctrl Pts',(65.8663119320418,11.7897326716554,-60.2118619231453));
#51450=CARTESIAN_POINT('Ctrl Pts',(65.8720888383968,11.8990178725946,-60.9876702353197));
#51451=CARTESIAN_POINT('Ctrl Pts',(65.8775618097942,12.0900399279052,-61.8928903527658));
#51452=CARTESIAN_POINT('Ctrl Pts',(65.8821141524937,12.3362439701848,-62.8075302866294));
#51453=CARTESIAN_POINT('Ctrl Pts',(65.8844065364392,12.4931153111574,-63.3250712383876));
#51454=CARTESIAN_POINT('Ctrl Pts',(65.8858572476094,12.6043773164143,-63.6707448858102));
#51455=CARTESIAN_POINT('Ctrl Pts',(65.8868063248849,12.6802661008852,-63.9013834884364));
#51456=CARTESIAN_POINT('Ctrl Pts',(65.8877368577102,12.7585927555402,-64.1321181809914));
#51457=CARTESIAN_POINT('Ctrl Pts',(65.88853723751,12.8291158174461,-64.3341594200084));
#51458=CARTESIAN_POINT('Ctrl Pts',(65.8889920597898,12.8699542671041,-64.4496329679656));
#51459=CARTESIAN_POINT('Ctrl Pts',(65.8896738172377,12.931727576733,-64.6228326327851));
#51460=CARTESIAN_POINT('Ctrl Pts',(65.8902373768405,12.9842867686261,-64.7672152994411));
#51461=CARTESIAN_POINT('Ctrl Pts',(65.8912070711975,13.072338288075,-65.0055995948209));
#51462=CARTESIAN_POINT('Ctrl Pts',(65.893904219689,13.1551982552599,-65.2185261014648));
#51463=CARTESIAN_POINT('Ctrl Pts',(65.8980167064991,13.3444882335856,-65.6685173087278));
#51464=CARTESIAN_POINT('Ctrl Pts',(65.9047560011375,13.712995741147,-66.4580151443174));
#51465=CARTESIAN_POINT('Ctrl Pts',(65.9129480637986,14.5930912526722,-68.0969738663711));
#51466=CARTESIAN_POINT('Ctrl Pts',(65.9104230697323,15.4911509741754,-69.5914929057301));
#51467=CARTESIAN_POINT('Ctrl Pts',(65.9050180119411,16.1226507856015,-70.7929510454671));
#51468=CARTESIAN_POINT('Ctrl Pts',(65.905492870021,16.2515347021751,-71.0375033190314));
#51469=CARTESIAN_POINT('Ctrl Pts',(65.9054587234462,16.5168823300383,-71.5400184758909));
#51470=CARTESIAN_POINT('Ctrl Pts',(65.9057793254249,16.8468781801207,-72.16274762481));
#51471=CARTESIAN_POINT('Ctrl Pts',(65.9058935864885,17.2459274490871,-72.9134318972112));
#51472=CARTESIAN_POINT('Ctrl Pts',(65.9061448213465,18.0454312362688,-74.4139182816276));
#51473=CARTESIAN_POINT('Ctrl Pts',(65.9061070245676,18.7153204568336,-75.6667589613612));
#51474=CARTESIAN_POINT('Ctrl Pts',(65.9058430512839,19.6870361875413,-77.4941510467294));
#51475=CARTESIAN_POINT('Ctrl Pts',(65.9059580210467,20.1227358835157,-78.3134457653799));
#51476=CARTESIAN_POINT('Ctrl Pts',(65.9059580210468,20.5592574709051,-79.1344234674783));
#51477=CARTESIAN_POINT('Ctrl Pts',(67.742805807408,7.54160808040336,24.8323707857055));
#51478=CARTESIAN_POINT('Ctrl Pts',(67.7429599438519,7.54167108069228,24.7835456054049));
#51479=CARTESIAN_POINT('Ctrl Pts',(67.7431216903204,7.54173699953244,24.7347227544535));
#51480=CARTESIAN_POINT('Ctrl Pts',(67.7450311299336,7.54251984739689,24.1847408960325));
#51481=CARTESIAN_POINT('Ctrl Pts',(67.7454542159906,7.5438074607775,23.1811252872465));
#51482=CARTESIAN_POINT('Ctrl Pts',(67.7457811718776,7.54716938456641,21.1737567515317));
#51483=CARTESIAN_POINT('Ctrl Pts',(67.7585271372276,7.5523488600553,19.670023507983));
#51484=CARTESIAN_POINT('Ctrl Pts',(67.7907393057243,7.55998007425724,18.4193411943366));
#51485=CARTESIAN_POINT('Ctrl Pts',(67.8058150390089,7.5640412743569,17.9206087648972));
#51486=CARTESIAN_POINT('Ctrl Pts',(67.8430415813513,7.57501016242088,16.9193609442862));
#51487=CARTESIAN_POINT('Ctrl Pts',(67.923184578734,7.59854283053069,15.164547126133));
#51488=CARTESIAN_POINT('Ctrl Pts',(68.0052074536955,7.61535646055261,13.6489946955723));
#51489=CARTESIAN_POINT('Ctrl Pts',(68.0672619893672,7.61551626660768,12.3772722079416));
#51490=CARTESIAN_POINT('Ctrl Pts',(68.0942310002145,7.61423207400124,11.8679018653112));
#51491=CARTESIAN_POINT('Ctrl Pts',(68.1540374999369,7.60738627849624,10.855276744513));
#51492=CARTESIAN_POINT('Ctrl Pts',(68.2343088168184,7.5927071823393,9.59654129740986));
#51493=CARTESIAN_POINT('Ctrl Pts',(68.3226710656602,7.57204229887091,8.09728674270897));
#51494=CARTESIAN_POINT('Ctrl Pts',(68.36488440954,7.56107248393117,7.10370740136219));
#51495=CARTESIAN_POINT('Ctrl Pts',(68.3825936563245,7.55677141971308,6.48416185059279));
#51496=CARTESIAN_POINT('Ctrl Pts',(68.3900676092246,7.55355227014377,6.21620475198307));
#51497=CARTESIAN_POINT('Ctrl Pts',(68.4062982498568,7.54294496556681,5.6981199796925));
#51498=CARTESIAN_POINT('Ctrl Pts',(68.4362371178003,7.51642570758137,4.79874139178095));
#51499=CARTESIAN_POINT('Ctrl Pts',(68.4899239058001,7.45236885152295,3.05968374041152));
#51500=CARTESIAN_POINT('Ctrl Pts',(68.4782603854943,7.45751053612557,1.66993124882464));
#51501=CARTESIAN_POINT('Ctrl Pts',(68.3952039810378,7.53749913627296,0.744765281110461));
#51502=CARTESIAN_POINT('Ctrl Pts',(68.3842008427377,7.54887409653413,0.618453143136928));
#51503=CARTESIAN_POINT('Ctrl Pts',(68.3588698517668,7.57060264433434,0.37648458626731));
#51504=CARTESIAN_POINT('Ctrl Pts',(68.3061409379183,7.60917219534973,-0.0481057361875789));
#51505=CARTESIAN_POINT('Ctrl Pts',(68.2107690363639,7.66390644809047,-0.641870471575015));
#51506=CARTESIAN_POINT('Ctrl Pts',(68.0771380246689,7.73110573139229,-1.34336822452881));
#51507=CARTESIAN_POINT('Ctrl Pts',(67.890924435506,7.82906293108064,-2.26476025149921));
#51508=CARTESIAN_POINT('Ctrl Pts',(67.6756317739727,7.98687869646959,-3.40211825486226));
#51509=CARTESIAN_POINT('Ctrl Pts',(67.5657544580734,8.21094517780775,-4.30266306393722));
#51510=CARTESIAN_POINT('Ctrl Pts',(67.5245233815194,8.39728418406289,-4.85788153652574));
#51511=CARTESIAN_POINT('Ctrl Pts',(67.5168291122563,8.46556549575842,-5.03399865888036));
#51512=CARTESIAN_POINT('Ctrl Pts',(67.498094458793,8.64557686408299,-5.4390138280413));
#51513=CARTESIAN_POINT('Ctrl Pts',(67.4675356717595,9.03871021017994,-6.18601230987185));
#51514=CARTESIAN_POINT('Ctrl Pts',(67.4119456645733,9.78056419203286,-7.38113321014756));
#51515=CARTESIAN_POINT('Ctrl Pts',(67.3463105795069,10.5913338716633,-8.698408224898));
#51516=CARTESIAN_POINT('Ctrl Pts',(67.3047874436322,11.1043449629669,-9.71620119923863));
#51517=CARTESIAN_POINT('Ctrl Pts',(67.2848402889429,11.3648155613531,-10.333193746664));
#51518=CARTESIAN_POINT('Ctrl Pts',(67.276616690386,11.4807774373825,-10.6554301435584));
#51519=CARTESIAN_POINT('Ctrl Pts',(67.2713943662642,11.5609909900776,-10.903179458728));
#51520=CARTESIAN_POINT('Ctrl Pts',(67.2706582747739,11.6075462300508,-11.0489379719184));
#51521=CARTESIAN_POINT('Ctrl Pts',(67.2706437082626,11.6978855799641,-11.3507195952246));
#51522=CARTESIAN_POINT('Ctrl Pts',(67.2777911266133,11.8389824143185,-11.8693793215723));
#51523=CARTESIAN_POINT('Ctrl Pts',(67.3152599975797,12.0652822944397,-12.8944649700296));
#51524=CARTESIAN_POINT('Ctrl Pts',(67.4178518526037,12.2508045803798,-14.297925846491));
#51525=CARTESIAN_POINT('Ctrl Pts',(67.5218179503882,12.3237687493651,-15.4806007042437));
#51526=CARTESIAN_POINT('Ctrl Pts',(67.5782051432208,12.3618802613975,-16.2356740428478));
#51527=CARTESIAN_POINT('Ctrl Pts',(67.6112804917142,12.3861954203215,-16.7307739218762));
#51528=CARTESIAN_POINT('Ctrl Pts',(67.629802139802,12.4050714788559,-17.0924204541062));
#51529=CARTESIAN_POINT('Ctrl Pts',(67.6403480227297,12.4232144522942,-17.3892704623789));
#51530=CARTESIAN_POINT('Ctrl Pts',(67.6440742945143,12.4311287307314,-17.528045321064));
#51531=CARTESIAN_POINT('Ctrl Pts',(67.6505780086127,12.4442497558684,-17.7923100213903));
#51532=CARTESIAN_POINT('Ctrl Pts',(67.6555479589858,12.4548337104085,-18.0600251419076));
#51533=CARTESIAN_POINT('Ctrl Pts',(67.6591812474422,12.4628105347589,-18.3240974338833));
#51534=CARTESIAN_POINT('Ctrl Pts',(67.6609177587551,12.4668616236941,-18.4891951551348));
#51535=CARTESIAN_POINT('Ctrl Pts',(67.6620086072592,12.4695517469555,-18.6207627473085));
#51536=CARTESIAN_POINT('Ctrl Pts',(67.6626817085544,12.4713118687434,-18.719341087396));
#51537=CARTESIAN_POINT('Ctrl Pts',(67.6631263749856,12.472568013926,-18.801342808996));
#51538=CARTESIAN_POINT('Ctrl Pts',(67.6634144201367,12.4734530469214,-18.8668744929406));
#51539=CARTESIAN_POINT('Ctrl Pts',(67.665489578405,12.4802979967182,-19.4234602240196));
#51540=CARTESIAN_POINT('Ctrl Pts',(67.6578561832691,12.4726640092777,-20.4744941719435));
#51541=CARTESIAN_POINT('Ctrl Pts',(67.6337655920693,12.4387833875839,-21.988465865762));
#51542=CARTESIAN_POINT('Ctrl Pts',(67.6230151758788,12.4240519376188,-22.9735202222548));
#51543=CARTESIAN_POINT('Ctrl Pts',(67.6222887352555,12.4242543566942,-23.5804071061423));
#51544=CARTESIAN_POINT('Ctrl Pts',(67.6220452785285,12.4243530616591,-23.8322273689017));
#51545=CARTESIAN_POINT('Ctrl Pts',(67.6217257596303,12.4245729199584,-24.3301491602105));
#51546=CARTESIAN_POINT('Ctrl Pts',(67.6215528040221,12.4250111840498,-25.2067512724399));
#51547=CARTESIAN_POINT('Ctrl Pts',(67.6221423903727,12.4256848711193,-26.4613493695427));
#51548=CARTESIAN_POINT('Ctrl Pts',(67.6232783878271,12.4262595156381,-27.9708139359673));
#51549=CARTESIAN_POINT('Ctrl Pts',(67.6237412574751,12.4262578976759,-28.9762328565498));
#51550=CARTESIAN_POINT('Ctrl Pts',(67.6237439413753,12.4260895555892,-29.540893931356));
#51551=CARTESIAN_POINT('Ctrl Pts',(67.6237363434596,12.4260461708279,-29.6663925140077));
#51552=CARTESIAN_POINT('Ctrl Pts',(67.6236936517162,12.4259353214926,-29.9174178590788));
#51553=CARTESIAN_POINT('Ctrl Pts',(67.6235533346394,12.4256827987944,-30.3568433047905));
#51554=CARTESIAN_POINT('Ctrl Pts',(67.6230619887266,12.4249722866822,-31.2360054690753));
#51555=CARTESIAN_POINT('Ctrl Pts',(67.6220605631816,12.4235542229819,-32.4921751234464));
#51556=CARTESIAN_POINT('Ctrl Pts',(67.6214659505391,12.4220626275935,-33.7466652722228));
#51557=CARTESIAN_POINT('Ctrl Pts',(67.6217163791426,12.4211031591343,-34.7480293774022));
#51558=CARTESIAN_POINT('Ctrl Pts',(67.6221665004297,12.4207523160916,-35.2478226594728));
#51559=CARTESIAN_POINT('Ctrl Pts',(67.6226566408131,12.4205516900217,-35.6232470890529));
#51560=CARTESIAN_POINT('Ctrl Pts',(67.6230489596044,12.4204066068882,-35.8751235864376));
#51561=CARTESIAN_POINT('Ctrl Pts',(67.6240585281982,12.4200847295307,-36.3778662665607));
#51562=CARTESIAN_POINT('Ctrl Pts',(67.6263390287901,12.4194853605145,-37.2561695027686));
#51563=CARTESIAN_POINT('Ctrl Pts',(67.632325278412,12.4183496428496,-39.0077021554759));
#51564=CARTESIAN_POINT('Ctrl Pts',(67.6377577403294,12.4184603549216,-40.5075168278314));
#51565=CARTESIAN_POINT('Ctrl Pts',(67.6400657259184,12.4201103103411,-41.7618072942457));
#51566=CARTESIAN_POINT('Ctrl Pts',(67.640566899813,12.4201140133972,-42.1402991098985));
#51567=CARTESIAN_POINT('Ctrl Pts',(67.6409671962261,12.4195546774867,-42.6425468132931));
#51568=CARTESIAN_POINT('Ctrl Pts',(67.6412235640905,12.4187641583059,-43.1450256319257));
#51569=CARTESIAN_POINT('Ctrl Pts',(67.6413400338377,12.4176004139746,-43.7721916062135));
#51570=CARTESIAN_POINT('Ctrl Pts',(67.6413641591375,12.4167556818269,-44.5232827606698));
#51571=CARTESIAN_POINT('Ctrl Pts',(67.6414643897262,12.4171989357511,-45.1473364014215));
#51572=CARTESIAN_POINT('Ctrl Pts',(67.6416994860161,12.4186434241101,-45.6452650445642));
#51573=CARTESIAN_POINT('Ctrl Pts',(67.6419797628929,12.4203764116758,-46.0179601430549));
#51574=CARTESIAN_POINT('Ctrl Pts',(67.6423906812054,12.4228601301659,-46.3898699970262));
#51575=CARTESIAN_POINT('Ctrl Pts',(67.6431490489485,12.4273028228971,-46.8845347673267));
#51576=CARTESIAN_POINT('Ctrl Pts',(67.6439933574302,12.4320694683604,-47.2542530416625));
#51577=CARTESIAN_POINT('Ctrl Pts',(67.6450803751829,12.4379880016587,-47.623365509274));
#51578=CARTESIAN_POINT('Ctrl Pts',(67.6458792333846,12.443115489082,-47.857596045839));
#51579=CARTESIAN_POINT('Ctrl Pts',(67.6475973396259,12.4582553810702,-48.338970501715));
#51580=CARTESIAN_POINT('Ctrl Pts',(67.6509363558493,12.4950414285458,-49.1899211168199));
#51581=CARTESIAN_POINT('Ctrl Pts',(67.656417817741,12.564853518565,-50.4440395966513));
#51582=CARTESIAN_POINT('Ctrl Pts',(67.6641480331354,12.6319236783931,-52.0037696390739));
#51583=CARTESIAN_POINT('Ctrl Pts',(67.6705503166098,12.6325474504813,-53.0814906845916));
#51584=CARTESIAN_POINT('Ctrl Pts',(67.6752859075517,12.6075250848195,-53.7691884355505));
#51585=CARTESIAN_POINT('Ctrl Pts',(67.6775870605467,12.5908672031517,-54.0746701819692));
#51586=CARTESIAN_POINT('Ctrl Pts',(67.6827720266418,12.5405076679727,-54.6531513588603));
#51587=CARTESIAN_POINT('Ctrl Pts',(67.6928452005905,12.4172535357334,-55.6352548638888));
#51588=CARTESIAN_POINT('Ctrl Pts',(67.7135779644103,12.1014009951142,-57.4434256620884));
#51589=CARTESIAN_POINT('Ctrl Pts',(67.722851809162,11.9397251962228,-58.7311281481815));
#51590=CARTESIAN_POINT('Ctrl Pts',(67.7312041788753,11.9871955958615,-59.4960738850571));
#51591=CARTESIAN_POINT('Ctrl Pts',(67.7320550014244,11.994843426241,-59.6094351306532));
#51592=CARTESIAN_POINT('Ctrl Pts',(67.7338048432822,12.0125903784316,-59.8256094334167));
#51593=CARTESIAN_POINT('Ctrl Pts',(67.7367168107863,12.0519246469009,-60.2117438069852));
#51594=CARTESIAN_POINT('Ctrl Pts',(67.7421406544915,12.1612221789839,-60.9877445387918));
#51595=CARTESIAN_POINT('Ctrl Pts',(67.7473099928523,12.3521746086762,-61.893089307246));
#51596=CARTESIAN_POINT('Ctrl Pts',(67.7516355763801,12.5982643565659,-62.8077700981422));
#51597=CARTESIAN_POINT('Ctrl Pts',(67.7538236438324,12.7550642190386,-63.3253043393395));
#51598=CARTESIAN_POINT('Ctrl Pts',(67.7552120031394,12.8662790790965,-63.670961444785));
#51599=CARTESIAN_POINT('Ctrl Pts',(67.7561212496728,12.9421369640812,-63.901585841944));
#51600=CARTESIAN_POINT('Ctrl Pts',(67.7570142538266,13.0204336258431,-64.1323015373684));
#51601=CARTESIAN_POINT('Ctrl Pts',(67.7577833567588,13.090932190376,-64.3343219676662));
#51602=CARTESIAN_POINT('Ctrl Pts',(67.7582206747438,13.1317572074132,-64.4497824107023));
#51603=CARTESIAN_POINT('Ctrl Pts',(67.7588765153974,13.1935110196122,-64.6229612480362));
#51604=CARTESIAN_POINT('Ctrl Pts',(67.7594190688071,13.2460552613512,-64.7673239208043));
#51605=CARTESIAN_POINT('Ctrl Pts',(67.7603545218044,13.3340849364679,-65.0056726218981));
#51606=CARTESIAN_POINT('Ctrl Pts',(67.7630264114336,13.4169425237236,-65.2186078123409));
#51607=CARTESIAN_POINT('Ctrl Pts',(67.7671022826528,13.606220231183,-65.6685908050389));
#51608=CARTESIAN_POINT('Ctrl Pts',(67.7738174709853,13.9747193655418,-66.4580877883408));
#51609=CARTESIAN_POINT('Ctrl Pts',(67.7820693092672,14.8548163287521,-68.0970364510266));
#51610=CARTESIAN_POINT('Ctrl Pts',(67.7796422117366,15.7528921082611,-69.5915590716733));
#51611=CARTESIAN_POINT('Ctrl Pts',(67.7742085967677,16.3843827046983,-70.7930204305104));
#51612=CARTESIAN_POINT('Ctrl Pts',(67.774684987654,16.513266189984,-71.0375719095944));
#51613=CARTESIAN_POINT('Ctrl Pts',(67.7746497020258,16.778612436894,-71.5400864033351));
#51614=CARTESIAN_POINT('Ctrl Pts',(67.7749711303553,17.1086075096059,-72.162814636667));
#51615=CARTESIAN_POINT('Ctrl Pts',(67.7750858845402,17.507656420601,-72.9134981492027));
#51616=CARTESIAN_POINT('Ctrl Pts',(67.7753392151518,18.3071607215725,-74.4139834265988));
#51617=CARTESIAN_POINT('Ctrl Pts',(67.7753030677253,18.9770518098338,-75.6668248107347));
#51618=CARTESIAN_POINT('Ctrl Pts',(67.7750376848129,19.9487680324284,-77.4942188650752));
#51619=CARTESIAN_POINT('Ctrl Pts',(67.7751531793561,20.3844675706249,-78.3135131806212));
#51620=CARTESIAN_POINT('Ctrl Pts',(67.7751531793563,20.8209891580143,-79.1344908827197));
#51621=CARTESIAN_POINT('Ctrl Pts',(70.0797409538656,7.87081603166709,24.8335816570491));
#51622=CARTESIAN_POINT('Ctrl Pts',(70.0799756448786,7.87092046555902,24.7847958004515));
#51623=CARTESIAN_POINT('Ctrl Pts',(70.0802217288107,7.87102995712953,24.7360128868017));
#51624=CARTESIAN_POINT('Ctrl Pts',(70.0831285733729,7.87231907386717,24.1864933048158));
#51625=CARTESIAN_POINT('Ctrl Pts',(70.0857084291293,7.87498063209253,23.1838567634182));
#51626=CARTESIAN_POINT('Ctrl Pts',(70.0919148806055,7.88234851674442,21.1771127206445));
#51627=CARTESIAN_POINT('Ctrl Pts',(70.1112363140131,7.89089667541493,19.6727038446357));
#51628=CARTESIAN_POINT('Ctrl Pts',(70.1504814375106,7.90058700585656,18.421108582133));
#51629=CARTESIAN_POINT('Ctrl Pts',(70.1697464384192,7.90583508389004,17.9235973663367));
#51630=CARTESIAN_POINT('Ctrl Pts',(70.2189478657357,7.92004955211645,16.9233181300777));
#51631=CARTESIAN_POINT('Ctrl Pts',(70.3246403871964,7.95017189341619,15.1692536305156));
#51632=CARTESIAN_POINT('Ctrl Pts',(70.419845264702,7.9691245051039,13.6496635406286));
#51633=CARTESIAN_POINT('Ctrl Pts',(70.4697508893646,7.96305756993818,12.3711740566263));
#51634=CARTESIAN_POINT('Ctrl Pts',(70.4903986876751,7.95739611684289,11.8535050431065));
#51635=CARTESIAN_POINT('Ctrl Pts',(70.5322522714481,7.93720517842765,10.8327471216722));
#51636=CARTESIAN_POINT('Ctrl Pts',(70.5814197965239,7.90173999531898,9.57080124372721));
#51637=CARTESIAN_POINT('Ctrl Pts',(70.6215548553232,7.86287760978718,8.08311707062897));
#51638=CARTESIAN_POINT('Ctrl Pts',(70.6265529441638,7.851025563103,7.10767909393591));
#51639=CARTESIAN_POINT('Ctrl Pts',(70.6200554158803,7.85109623620988,6.50259304499254));
#51640=CARTESIAN_POINT('Ctrl Pts',(70.6172821755683,7.84916354644725,6.22780779202129));
#51641=CARTESIAN_POINT('Ctrl Pts',(70.6099684248821,7.83998838688957,5.70611026729234));
#51642=CARTESIAN_POINT('Ctrl Pts',(70.5919833713834,7.81404214662331,4.80405814351667));
#51643=CARTESIAN_POINT('Ctrl Pts',(70.530876070008,7.75724957337001,3.09228082865713));
#51644=CARTESIAN_POINT('Ctrl Pts',(70.4229142961228,7.78796452061628,1.78279487855182));
#51645=CARTESIAN_POINT('Ctrl Pts',(70.3374929882626,7.91062380588921,0.920546111644628));
#51646=CARTESIAN_POINT('Ctrl Pts',(70.3261887650127,7.92655009675492,0.815573102355774));
#51647=CARTESIAN_POINT('Ctrl Pts',(70.3016919401967,7.96074643074563,0.604598130449329));
#51648=CARTESIAN_POINT('Ctrl Pts',(70.2535232133574,8.02788989730723,0.229523060001451));
#51649=CARTESIAN_POINT('Ctrl Pts',(70.1733985653285,8.14395394628861,-0.321339018131735));
#51650=CARTESIAN_POINT('Ctrl Pts',(70.0679296073265,8.3158125006749,-1.00743831078729));
#51651=CARTESIAN_POINT('Ctrl Pts',(69.924485576269,8.58574606963455,-1.95189023868025));
#51652=CARTESIAN_POINT('Ctrl Pts',(69.7543354654112,8.99387404858029,-3.18250609368043));
#51653=CARTESIAN_POINT('Ctrl Pts',(69.6556906939328,9.37193157308521,-4.20526479014222));
#51654=CARTESIAN_POINT('Ctrl Pts',(69.6176271763688,9.6167934094289,-4.85189132462664));
#51655=CARTESIAN_POINT('Ctrl Pts',(69.6150404011341,9.70387094654282,-5.05485554963878));
#51656=CARTESIAN_POINT('Ctrl Pts',(69.608351339168,9.91053595098722,-5.50475572282167));
#51657=CARTESIAN_POINT('Ctrl Pts',(69.6107081740475,10.318116215295,-6.30236350776975));
#51658=CARTESIAN_POINT('Ctrl Pts',(69.6343815288851,11.000254972414,-7.52661118182464));
#51659=CARTESIAN_POINT('Ctrl Pts',(69.6766224457615,11.6866786141997,-8.85980820136688));
#51660=CARTESIAN_POINT('Ctrl Pts',(69.7071296898245,12.096953840095,-9.87707362096165));
#51661=CARTESIAN_POINT('Ctrl Pts',(69.7227081692398,12.2973745110336,-10.4848255250078));
#51662=CARTESIAN_POINT('Ctrl Pts',(69.7293972812761,12.383871734745,-10.7982467733909));
#51663=CARTESIAN_POINT('Ctrl Pts',(69.7338313852413,12.4427638036451,-11.037717319835));
#51664=CARTESIAN_POINT('Ctrl Pts',(69.7372583324694,12.4792643931483,-11.1910809255586));
#51665=CARTESIAN_POINT('Ctrl Pts',(69.7450988986082,12.5453767274486,-11.4999472238591));
#51666=CARTESIAN_POINT('Ctrl Pts',(69.7613520093288,12.6419821016412,-12.0328588232142));
#51667=CARTESIAN_POINT('Ctrl Pts',(69.8016786896662,12.7677585020227,-13.0749199230374));
#51668=CARTESIAN_POINT('Ctrl Pts',(69.8691448168152,12.8029397807458,-14.4766219386973));
#51669=CARTESIAN_POINT('Ctrl Pts',(69.9235912109219,12.7682710815651,-15.6327397218786));
#51670=CARTESIAN_POINT('Ctrl Pts',(69.9528675113096,12.7526652494517,-16.362145317967));
#51671=CARTESIAN_POINT('Ctrl Pts',(69.9702913827983,12.7458820279233,-16.8377412914816));
#51672=CARTESIAN_POINT('Ctrl Pts',(69.9807618700987,12.7469619944152,-17.1822398002294));
#51673=CARTESIAN_POINT('Ctrl Pts',(69.9877367721392,12.7532498652985,-17.4633817754817));
#51674=CARTESIAN_POINT('Ctrl Pts',(69.9902724907931,12.7559041355279,-17.5957929350974));
#51675=CARTESIAN_POINT('Ctrl Pts',(69.9946923357774,12.7603733220597,-17.8480941322808));
#51676=CARTESIAN_POINT('Ctrl Pts',(69.9981362569232,12.7639894309032,-18.1046860591192));
#51677=CARTESIAN_POINT('Ctrl Pts',(70.0007143766111,12.7667555359829,-18.3585719929953));
#51678=CARTESIAN_POINT('Ctrl Pts',(70.0019843123243,12.7681708635531,-18.5176750764189));
#51679=CARTESIAN_POINT('Ctrl Pts',(70.0028084377921,12.7691206629677,-18.6446774706336));
#51680=CARTESIAN_POINT('Ctrl Pts',(70.0033337386207,12.7697465689295,-18.7399452824287));
#51681=CARTESIAN_POINT('Ctrl Pts',(70.0036969413586,12.7701976032863,-18.8192833935171));
#51682=CARTESIAN_POINT('Ctrl Pts',(70.0039442061729,12.7705181741567,-18.8827414859159));
#51683=CARTESIAN_POINT('Ctrl Pts',(70.0058065097664,12.7730150550074,-19.4220227073925));
#51684=CARTESIAN_POINT('Ctrl Pts',(70.0019467478389,12.7707690700143,-20.4500579544624));
#51685=CARTESIAN_POINT('Ctrl Pts',(69.9880028636105,12.759451471308,-21.9592536776598));
#51686=CARTESIAN_POINT('Ctrl Pts',(69.9819325942476,12.7544739985022,-22.9601843403765));
#51687=CARTESIAN_POINT('Ctrl Pts',(69.9818504352436,12.7546855124083,-23.5825598396711));
#51688=CARTESIAN_POINT('Ctrl Pts',(69.9818498694438,12.7547732795172,-23.8326459407025));
#51689=CARTESIAN_POINT('Ctrl Pts',(69.9819618693895,12.7549581583201,-24.331515238654));
#51690=CARTESIAN_POINT('Ctrl Pts',(69.9824089703596,12.7552944272569,-25.2074733334245));
#51691=CARTESIAN_POINT('Ctrl Pts',(69.9835134424833,12.7557536480768,-26.4623751878375));
#51692=CARTESIAN_POINT('Ctrl Pts',(69.9847399796544,12.756098892895,-27.9712796662369));
#51693=CARTESIAN_POINT('Ctrl Pts',(69.9849507476041,12.7560682675524,-28.9764144739503));
#51694=CARTESIAN_POINT('Ctrl Pts',(69.9847403411927,12.7559468487486,-29.5408469533237));
#51695=CARTESIAN_POINT('Ctrl Pts',(69.9846807995037,12.7559155593729,-29.6662922695801));
#51696=CARTESIAN_POINT('Ctrl Pts',(69.9845152198024,12.755835586929,-29.917220044137));
#51697=CARTESIAN_POINT('Ctrl Pts',(69.9841125650528,12.7556530022131,-30.356482175709));
#51698=CARTESIAN_POINT('Ctrl Pts',(69.9829269517545,12.7551400505817,-31.2353717708401));
#51699=CARTESIAN_POINT('Ctrl Pts',(69.9805586324968,12.7541171006627,-32.4912989215736));
#51700=CARTESIAN_POINT('Ctrl Pts',(69.9783895266914,12.7530531299486,-33.7457658728073));
#51701=CARTESIAN_POINT('Ctrl Pts',(69.9774310607184,12.7523853076487,-34.7472738759857));
#51702=CARTESIAN_POINT('Ctrl Pts',(69.9773215948423,12.7521475451418,-35.2471770527657));
#51703=CARTESIAN_POINT('Ctrl Pts',(69.977419139063,12.75201737046,-35.6227053059714));
#51704=CARTESIAN_POINT('Ctrl Pts',(69.977541730052,12.7519174157327,-35.8745739800902));
#51705=CARTESIAN_POINT('Ctrl Pts',(69.9779905683333,12.7516793667049,-36.3773483318021));
#51706=CARTESIAN_POINT('Ctrl Pts',(69.9792445246214,12.7512023133202,-37.2556757877539));
#51707=CARTESIAN_POINT('Ctrl Pts',(69.9830984509896,12.750259756629,-39.0072979426011));
#51708=CARTESIAN_POINT('Ctrl Pts',(69.9868932895405,12.7504494223442,-40.507159154037));
#51709=CARTESIAN_POINT('Ctrl Pts',(69.9883161118172,12.7521845202418,-41.7615060469929));
#51710=CARTESIAN_POINT('Ctrl Pts',(69.9885876280256,12.7522183251696,-42.1400024337612));
#51711=CARTESIAN_POINT('Ctrl Pts',(69.9887376000478,12.751702152804,-42.6422704841182));
#51712=CARTESIAN_POINT('Ctrl Pts',(69.9887763116878,12.7509546805858,-43.1447697673002));
#51713=CARTESIAN_POINT('Ctrl Pts',(69.9886741002939,12.7498432673778,-43.7719674815809));
#51714=CARTESIAN_POINT('Ctrl Pts',(69.9884953414307,12.7490527076822,-44.5231042257711));
#51715=CARTESIAN_POINT('Ctrl Pts',(69.9884545849398,12.7495288403564,-45.1472023879138));
#51716=CARTESIAN_POINT('Ctrl Pts',(69.9885812323078,12.7509907750599,-45.6451736508804));
#51717=CARTESIAN_POINT('Ctrl Pts',(69.988778939342,12.752731048271,-46.0179027182678));
#51718=CARTESIAN_POINT('Ctrl Pts',(69.9891028664157,12.7552157067239,-46.3898487461034));
#51719=CARTESIAN_POINT('Ctrl Pts',(69.9897351377018,12.7596501127633,-46.8845654751457));
#51720=CARTESIAN_POINT('Ctrl Pts',(69.9904684256117,12.7643991235181,-47.2543243694849));
#51721=CARTESIAN_POINT('Ctrl Pts',(69.9914269985218,12.7702904757354,-47.6234817042101));
#51722=CARTESIAN_POINT('Ctrl Pts',(69.9921449188023,12.7753983944061,-47.8577567510985));
#51723=CARTESIAN_POINT('Ctrl Pts',(69.9937153663376,12.7904898297555,-48.3392024846442));
#51724=CARTESIAN_POINT('Ctrl Pts',(69.9968245713006,12.8271665626957,-49.1902597011841));
#51725=CARTESIAN_POINT('Ctrl Pts',(70.0020056610302,12.8967595109998,-50.4444639950959));
#51726=CARTESIAN_POINT('Ctrl Pts',(70.0092629589438,12.9634701930194,-52.0042114998902));
#51727=CARTESIAN_POINT('Ctrl Pts',(70.0151774431333,12.963824528338,-53.0818878650222));
#51728=CARTESIAN_POINT('Ctrl Pts',(70.0195221116976,12.9386285707829,-53.769543617284));
#51729=CARTESIAN_POINT('Ctrl Pts',(70.0216564325669,12.9218892369982,-54.075048710684));
#51730=CARTESIAN_POINT('Ctrl Pts',(70.0264592121177,12.8713560782644,-54.6535485980993));
#51731=CARTESIAN_POINT('Ctrl Pts',(70.0357543986074,12.7477707333624,-55.6356845180778));
#51732=CARTESIAN_POINT('Ctrl Pts',(70.0545927477608,12.4311929338987,-57.4438736407867));
#51733=CARTESIAN_POINT('Ctrl Pts',(70.0622016950512,12.2690410492287,-58.7314980847868));
#51734=CARTESIAN_POINT('Ctrl Pts',(70.0698758147919,12.3163383864376,-59.4962722687201));
#51735=CARTESIAN_POINT('Ctrl Pts',(70.0706456017594,12.3239632483135,-59.6096143697204));
#51736=CARTESIAN_POINT('Ctrl Pts',(70.0722406933252,12.3416695007431,-59.8257516674088));
#51737=CARTESIAN_POINT('Ctrl Pts',(70.0748997350423,12.3809415586232,-60.2118271282564));
#51738=CARTESIAN_POINT('Ctrl Pts',(70.0798848449523,12.4901511750555,-60.9877325346741));
#51739=CARTESIAN_POINT('Ctrl Pts',(70.0846859736845,12.6810750279437,-61.8930224122099));
#51740=CARTESIAN_POINT('Ctrl Pts',(70.0887363756449,12.9271799879292,-62.8076960822796));
#51741=CARTESIAN_POINT('Ctrl Pts',(70.0907962690645,13.0839977672833,-63.3252423160145));
#51742=CARTESIAN_POINT('Ctrl Pts',(70.0921067372744,13.195225846899,-63.6709135692915));
#51743=CARTESIAN_POINT('Ctrl Pts',(70.0929658003375,13.2710925766303,-63.9015489775992));
#51744=CARTESIAN_POINT('Ctrl Pts',(70.0938109233596,13.3493980555299,-64.1322780048317));
#51745=CARTESIAN_POINT('Ctrl Pts',(70.0945394273088,13.4199035667187,-64.3343120637915));
#51746=CARTESIAN_POINT('Ctrl Pts',(70.0949538252675,13.4607322800446,-64.4497808485651));
#51747=CARTESIAN_POINT('Ctrl Pts',(70.0955755227905,13.5224913056746,-64.6229727263848));
#51748=CARTESIAN_POINT('Ctrl Pts',(70.0960900007352,13.5750392045839,-64.7673474251791));
#51749=CARTESIAN_POINT('Ctrl Pts',(70.0969790953196,13.6630733166992,-65.0057170674026));
#51750=CARTESIAN_POINT('Ctrl Pts',(70.0996177025827,13.7459300625678,-65.2186519130424));
#51751=CARTESIAN_POINT('Ctrl Pts',(70.1036433012842,13.9352112916688,-65.6686450143725));
#51752=CARTESIAN_POINT('Ctrl Pts',(70.1103217310111,14.3037186771198,-66.4581500926349));
#51753=CARTESIAN_POINT('Ctrl Pts',(70.1186392504916,15.1838405759538,-68.0971096194841));
#51754=CARTESIAN_POINT('Ctrl Pts',(70.1163397261599,16.0819302159619,-69.5916293629507));
#51755=CARTESIAN_POINT('Ctrl Pts',(70.1108790104758,16.7134126638863,-70.7930853094538));
#51756=CARTESIAN_POINT('Ctrl Pts',(70.1113567541731,16.8422974277222,-71.0376376506106));
#51757=CARTESIAN_POINT('Ctrl Pts',(70.1113202628326,17.1076442349163,-71.5401526000775));
#51758=CARTESIAN_POINT('Ctrl Pts',(70.1116423816177,17.4376404292802,-72.1628816489));
#51759=CARTESIAN_POINT('Ctrl Pts',(70.1117575330375,17.8366898205343,-72.9135656961683));
#51760=CARTESIAN_POINT('Ctrl Pts',(70.1120128139938,18.6361945871019,-74.4140517265804));
#51761=CARTESIAN_POINT('Ctrl Pts',(70.1119785342542,19.3060848488128,-75.6668924674932));
#51762=CARTESIAN_POINT('Ctrl Pts',(70.1117120950068,20.2778001540279,-77.4942851400854));
#51763=CARTESIAN_POINT('Ctrl Pts',(70.1118280829169,20.7135000717299,-78.3135797649147));
#51764=CARTESIAN_POINT('Ctrl Pts',(70.1118280829168,21.1500216591192,-79.1345574670135));
#51765=CARTESIAN_POINT('Ctrl Pts',(72.8865625591464,8.26574019266068,24.8276674291661));
#51766=CARTESIAN_POINT('Ctrl Pts',(72.8869359246848,8.26572049517288,24.7786937745789));
#51767=CARTESIAN_POINT('Ctrl Pts',(72.8873273851381,8.26569974190122,24.7297204267048));
#51768=CARTESIAN_POINT('Ctrl Pts',(72.8919447951196,8.26546070767614,24.17797013955));
#51769=CARTESIAN_POINT('Ctrl Pts',(72.8988873922156,8.26451654009221,23.1728032601338));
#51770=CARTESIAN_POINT('Ctrl Pts',(72.9173560080737,8.26165580699735,21.1618516897943));
#51771=CARTESIAN_POINT('Ctrl Pts',(72.9479727662523,8.25994157807903,19.6553564107176));
#51772=CARTESIAN_POINT('Ctrl Pts',(72.9958158327139,8.26031865031543,18.4025752947981));
#51773=CARTESIAN_POINT('Ctrl Pts',(73.0208253794137,8.25951792114091,17.8901989626081));
#51774=CARTESIAN_POINT('Ctrl Pts',(73.0873380218554,8.25553385745433,16.8798709913457));
#51775=CARTESIAN_POINT('Ctrl Pts',(73.2296748200099,8.24591178499764,15.1295740970655));
#51776=CARTESIAN_POINT('Ctrl Pts',(73.3371582268296,8.24853883578068,13.6575163179087));
#51777=CARTESIAN_POINT('Ctrl Pts',(73.3530585220882,8.2749226805994,12.4397384118938));
#51778=CARTESIAN_POINT('Ctrl Pts',(73.356533238332,8.2849822560771,11.9323304672573));
#51779=CARTESIAN_POINT('Ctrl Pts',(73.351918135292,8.30439994752229,10.9377185673971));
#51780=CARTESIAN_POINT('Ctrl Pts',(73.324432495624,8.33151574081882,9.70196617136291));
#51781=CARTESIAN_POINT('Ctrl Pts',(73.2565738047078,8.38018797690781,8.24482455372541));
#51782=CARTESIAN_POINT('Ctrl Pts',(73.188921906069,8.43134132223997,7.28751763953783));
#51783=CARTESIAN_POINT('Ctrl Pts',(73.139908835424,8.47204451181113,6.69392156609347));
#51784=CARTESIAN_POINT('Ctrl Pts',(73.1173372266464,8.49011925131763,6.44016523067723));
#51785=CARTESIAN_POINT('Ctrl Pts',(73.0653378607807,8.52148234509983,5.94599916456272));
#51786=CARTESIAN_POINT('Ctrl Pts',(72.9587586513335,8.57066940381603,5.08370778538657));
#51787=CARTESIAN_POINT('Ctrl Pts',(72.7116581638965,8.65615239472504,3.39681284085337));
#51788=CARTESIAN_POINT('Ctrl Pts',(72.5399901263606,8.79326075224883,1.99040804109539));
#51789=CARTESIAN_POINT('Ctrl Pts',(72.488100820693,9.02163723228497,1.02355785184261));
#51790=CARTESIAN_POINT('Ctrl Pts',(72.4833544360269,9.04789388573715,0.919138805898511));
#51791=CARTESIAN_POINT('Ctrl Pts',(72.4734944993745,9.10670425273688,0.701380761297459));
#51792=CARTESIAN_POINT('Ctrl Pts',(72.4573641049337,9.22167130677439,0.317256690956153));
#51793=CARTESIAN_POINT('Ctrl Pts',(72.4350064423105,9.41948780353124,-0.250089179012498));
#51794=CARTESIAN_POINT('Ctrl Pts',(72.4069158908792,9.69866948764853,-0.953704395888368));
#51795=CARTESIAN_POINT('Ctrl Pts',(72.367097095033,10.1105519747146,-1.9213359299363));
#51796=CARTESIAN_POINT('Ctrl Pts',(72.3145247685813,10.6685132376829,-3.18402347160584));
#51797=CARTESIAN_POINT('Ctrl Pts',(72.2842979906458,11.0951808963158,-4.26275861171817));
#51798=CARTESIAN_POINT('Ctrl Pts',(72.2768707776213,11.3322038028194,-4.96442639381475));
#51799=CARTESIAN_POINT('Ctrl Pts',(72.2817991873453,11.4180358849558,-5.2019584464972));
#51800=CARTESIAN_POINT('Ctrl Pts',(72.2957055330416,11.5998824492514,-5.70484469018419));
#51801=CARTESIAN_POINT('Ctrl Pts',(72.3400044590547,11.9223023270952,-6.58102264467085));
#51802=CARTESIAN_POINT('Ctrl Pts',(72.4485046707705,12.3824968693468,-7.8717536828968));
#51803=CARTESIAN_POINT('Ctrl Pts',(72.5868482248549,12.7732400063546,-9.21294999905228));
#51804=CARTESIAN_POINT('Ctrl Pts',(72.6694839019536,12.9825682881853,-10.1808033039262));
#51805=CARTESIAN_POINT('Ctrl Pts',(72.7079819980637,13.0811308336793,-10.7403201973301));
#51806=CARTESIAN_POINT('Ctrl Pts',(72.7235630104351,13.1230129893701,-11.0222398269303));
#51807=CARTESIAN_POINT('Ctrl Pts',(72.7336302268316,13.1516841759947,-11.235476861186));
#51808=CARTESIAN_POINT('Ctrl Pts',(72.7399593853654,13.1707010880872,-11.3844405524316));
#51809=CARTESIAN_POINT('Ctrl Pts',(72.7517498643427,13.2030198757993,-11.6767974705028));
#51810=CARTESIAN_POINT('Ctrl Pts',(72.7697996681693,13.2473586325557,-12.1844527718077));
#51811=CARTESIAN_POINT('Ctrl Pts',(72.7962782320539,13.2919511946022,-13.1752477705232));
#51812=CARTESIAN_POINT('Ctrl Pts',(72.8109024014116,13.2660096011693,-14.5238591316298));
#51813=CARTESIAN_POINT('Ctrl Pts',(72.8099755885965,13.2058906010588,-15.6607465153076));
#51814=CARTESIAN_POINT('Ctrl Pts',(72.8094437551831,13.1754828967126,-16.3890783692441));
#51815=CARTESIAN_POINT('Ctrl Pts',(72.809549987816,13.159168467406,-16.8669534234));
#51816=CARTESIAN_POINT('Ctrl Pts',(72.8106563092265,13.1530496688261,-17.2167613707435));
#51817=CARTESIAN_POINT('Ctrl Pts',(72.8127028755648,13.1530106002742,-17.5037664142363));
#51818=CARTESIAN_POINT('Ctrl Pts',(72.8134629462877,13.1529462455956,-17.631446044319));
#51819=CARTESIAN_POINT('Ctrl Pts',(72.8147612394063,13.1528359207374,-17.8787319632469));
#51820=CARTESIAN_POINT('Ctrl Pts',(72.8157545524651,13.1527002033884,-18.1292115146335));
#51821=CARTESIAN_POINT('Ctrl Pts',(72.8164679719332,13.1525607492633,-18.3782333876691));
#51822=CARTESIAN_POINT('Ctrl Pts',(72.8168062584366,13.1524676775119,-18.5342986085837));
#51823=CARTESIAN_POINT('Ctrl Pts',(72.8170154966428,13.1523917172578,-18.6590504455465));
#51824=CARTESIAN_POINT('Ctrl Pts',(72.81714308237,13.1523334865433,-18.752668411454));
#51825=CARTESIAN_POINT('Ctrl Pts',(72.8172257706092,13.1522841134498,-18.8306852443342));
#51826=CARTESIAN_POINT('Ctrl Pts',(72.817278168026,13.152244180255,-18.893112099867));
#51827=CARTESIAN_POINT('Ctrl Pts',(72.8176480539968,13.151901641012,-19.423789566149));
#51828=CARTESIAN_POINT('Ctrl Pts',(72.8160192886251,13.1511430274956,-20.4402588086319));
#51829=CARTESIAN_POINT('Ctrl Pts',(72.8110708994919,13.1500609857134,-21.946711243545));
#51830=CARTESIAN_POINT('Ctrl Pts',(72.8089031262298,13.1495061882381,-22.9551201162143));
#51831=CARTESIAN_POINT('Ctrl Pts',(72.8087715182586,13.1492717851851,-23.5849046078959));
#51832=CARTESIAN_POINT('Ctrl Pts',(72.8087370586053,13.1491837194568,-23.8341005320297));
#51833=CARTESIAN_POINT('Ctrl Pts',(72.8087323220412,13.1490219551124,-24.3333279217166));
#51834=CARTESIAN_POINT('Ctrl Pts',(72.8088662673866,13.1487767703018,-25.2087732822766));
#51835=CARTESIAN_POINT('Ctrl Pts',(72.8093266109851,13.1485371767267,-26.4634727764513));
#51836=CARTESIAN_POINT('Ctrl Pts',(72.8098422061217,13.1484307095398,-27.9716158872549));
#51837=CARTESIAN_POINT('Ctrl Pts',(72.8098636816209,13.1484791110874,-28.9762238937061));
#51838=CARTESIAN_POINT('Ctrl Pts',(72.809695974041,13.1485404445919,-29.5403115148885));
#51839=CARTESIAN_POINT('Ctrl Pts',(72.8096504359251,13.1485557179075,-29.6656275973256));
#51840=CARTESIAN_POINT('Ctrl Pts',(72.8095299300256,13.1485922645576,-29.9163418893078));
#51841=CARTESIAN_POINT('Ctrl Pts',(72.8092477764273,13.1486715934479,-30.3552440960804));
#51842=CARTESIAN_POINT('Ctrl Pts',(72.8084470491389,13.1488858874495,-31.2335561262111));
#51843=CARTESIAN_POINT('Ctrl Pts',(72.8069060771625,13.1493246110313,-32.4890162027479));
#51844=CARTESIAN_POINT('Ctrl Pts',(72.8055811662997,13.1498610648749,-33.7435174707489));
#51845=CARTESIAN_POINT('Ctrl Pts',(72.8050973616134,13.1503012894563,-34.7453688189319));
#51846=CARTESIAN_POINT('Ctrl Pts',(72.8051223743103,13.1505189541041,-35.2455401860808));
#51847=CARTESIAN_POINT('Ctrl Pts',(72.8052695179574,13.1506776609489,-35.6213073903767));
#51848=CARTESIAN_POINT('Ctrl Pts',(72.8054127632015,13.1507670975923,-35.8731634916129));
#51849=CARTESIAN_POINT('Ctrl Pts',(72.8058580763078,13.1508899756323,-36.3760126603184));
#51850=CARTESIAN_POINT('Ctrl Pts',(72.8070010659971,13.151001693871,-37.2544170873883));
#51851=CARTESIAN_POINT('Ctrl Pts',(72.8103276560061,13.1510724644046,-39.0062487185812));
#51852=CARTESIAN_POINT('Ctrl Pts',(72.8135232736315,13.1519042845439,-40.5062738671393));
#51853=CARTESIAN_POINT('Ctrl Pts',(72.8147874625334,13.1540974660561,-41.7607797533392));
#51854=CARTESIAN_POINT('Ctrl Pts',(72.8150437115558,13.1542686847748,-42.1392980320379));
#51855=CARTESIAN_POINT('Ctrl Pts',(72.8152170000764,13.1539277490992,-42.6416181546101));
#51856=CARTESIAN_POINT('Ctrl Pts',(72.8153010284797,13.1533492477975,-43.1441703083421));
#51857=CARTESIAN_POINT('Ctrl Pts',(72.8152838011158,13.1524330871771,-43.7714444955365));
#51858=CARTESIAN_POINT('Ctrl Pts',(72.8152106934443,13.1518401424435,-44.5226858579805));
#51859=CARTESIAN_POINT('Ctrl Pts',(72.8152263278303,13.1524409218818,-45.1468828510351));
#51860=CARTESIAN_POINT('Ctrl Pts',(72.815358309241,13.153972508572,-45.6449411346028));
#51861=CARTESIAN_POINT('Ctrl Pts',(72.8155348943229,13.1557487952531,-46.0177390087985));
#51862=CARTESIAN_POINT('Ctrl Pts',(72.8158073722611,13.1582518130966,-46.38975745001));
#51863=CARTESIAN_POINT('Ctrl Pts',(72.8163236379806,13.16268521408,-46.8845758652391));
#51864=CARTESIAN_POINT('Ctrl Pts',(72.8169088176789,13.1674030382691,-47.2544162259643));
#51865=CARTESIAN_POINT('Ctrl Pts',(72.8176675448834,13.1732397249461,-47.6236601496442));
#51866=CARTESIAN_POINT('Ctrl Pts',(72.8182420222224,13.1783039805414,-47.8580173951434));
#51867=CARTESIAN_POINT('Ctrl Pts',(72.8194910411997,13.1932756057432,-48.3395992515894));
#51868=CARTESIAN_POINT('Ctrl Pts',(72.8219486073975,13.2296643335382,-49.1908687776819));
#51869=CARTESIAN_POINT('Ctrl Pts',(72.8259596787755,13.2986484891989,-50.4452782120899));
#51870=CARTESIAN_POINT('Ctrl Pts',(72.8314631100544,13.3644210345925,-52.0051236883727));
#51871=CARTESIAN_POINT('Ctrl Pts',(72.8359915178612,13.3641025210508,-53.0827529928531));
#51872=CARTESIAN_POINT('Ctrl Pts',(72.8394034112851,13.3385039554964,-53.7703454551854));
#51873=CARTESIAN_POINT('Ctrl Pts',(72.8411346048377,13.3215759995062,-54.0759284754757));
#51874=CARTESIAN_POINT('Ctrl Pts',(72.8450369657781,13.2706456813332,-54.6544988397768));
#51875=CARTESIAN_POINT('Ctrl Pts',(72.8525511039821,13.1463106982952,-55.6367316934619));
#51876=CARTESIAN_POINT('Ctrl Pts',(72.8673326133932,12.8281734952145,-57.4449133974758));
#51877=CARTESIAN_POINT('Ctrl Pts',(72.8716417191591,12.6650265360812,-58.7322902670711));
#51878=CARTESIAN_POINT('Ctrl Pts',(72.8780571431512,12.7119587273811,-59.4966710357007));
#51879=CARTESIAN_POINT('Ctrl Pts',(72.878680938848,12.719537487613,-59.6099712697978));
#51880=CARTESIAN_POINT('Ctrl Pts',(72.8800066542427,12.7371627024027,-59.8260265119129));
#51881=CARTESIAN_POINT('Ctrl Pts',(72.882252534028,12.7763144747118,-60.2119714384574));
#51882=CARTESIAN_POINT('Ctrl Pts',(72.8866217314193,12.8853688503928,-60.9876622988252));
#51883=CARTESIAN_POINT('Ctrl Pts',(72.8911013820776,13.0762781429483,-61.8928145456306));
#51884=CARTESIAN_POINT('Ctrl Pts',(72.8950177095436,13.322458888845,-62.8074465123463));
#51885=CARTESIAN_POINT('Ctrl Pts',(72.8970367991066,13.4793367386658,-63.3250031405502));
#51886=CARTESIAN_POINT('Ctrl Pts',(72.8983197062041,13.5906053760081,-63.6706948039897));
#51887=CARTESIAN_POINT('Ctrl Pts',(72.8991593399374,13.6664987843523,-63.9013474223356));
#51888=CARTESIAN_POINT('Ctrl Pts',(72.8999819509068,13.7448296381239,-64.1320988669824));
#51889=CARTESIAN_POINT('Ctrl Pts',(72.9006855457522,13.815355017023,-64.3341572392981));
#51890=CARTESIAN_POINT('Ctrl Pts',(72.9010838538832,13.8561942287203,-64.4496412499583));
#51891=CARTESIAN_POINT('Ctrl Pts',(72.9016793794264,13.9179680385629,-64.6228572582028));
#51892=CARTESIAN_POINT('Ctrl Pts',(72.9021674144054,13.9705261148409,-64.767254909506));
#51893=CARTESIAN_POINT('Ctrl Pts',(72.9030045822634,14.0585728029474,-65.0056652986328));
#51894=CARTESIAN_POINT('Ctrl Pts',(72.9055939633252,14.1414228933973,-65.2185919113378));
#51895=CARTESIAN_POINT('Ctrl Pts',(72.9095453337735,14.3307041702797,-65.6685963244501));
#51896=CARTESIAN_POINT('Ctrl Pts',(72.916148601967,14.699210204333,-66.4581050158198));
#51897=CARTESIAN_POINT('Ctrl Pts',(72.9244920846649,15.5793474471033,-68.0970777158963));
#51898=CARTESIAN_POINT('Ctrl Pts',(72.9223525060322,16.4774546468999,-69.5915925940898));
#51899=CARTESIAN_POINT('Ctrl Pts',(72.916907887135,17.1089423094142,-70.793043389865));
#51900=CARTESIAN_POINT('Ctrl Pts',(72.917384567627,17.2378279180548,-71.0375967877744));
#51901=CARTESIAN_POINT('Ctrl Pts',(72.9173485145221,17.5031761663896,-71.5401125120657));
#51902=CARTESIAN_POINT('Ctrl Pts',(72.9176699512543,17.8331733766952,-72.1628426787913));
#51903=CARTESIAN_POINT('Ctrl Pts',(72.917784753143,18.2322232294136,-72.9135276172968));
#51904=CARTESIAN_POINT('Ctrl Pts',(72.9180388995489,19.0317276241097,-74.4140149343857));
#51905=CARTESIAN_POINT('Ctrl Pts',(72.9180039490813,19.7016155224588,-75.6668546533854));
#51906=CARTESIAN_POINT('Ctrl Pts',(72.9177383558073,20.6733298082105,-77.4942448926987));
#51907=CARTESIAN_POINT('Ctrl Pts',(72.9178539859473,21.1090298969448,-78.3135399675102));
#51908=CARTESIAN_POINT('Ctrl Pts',(72.9178539859467,21.5455514843342,-79.1345176696082));
#51909=CARTESIAN_POINT('Ctrl Pts',(75.6920843231871,8.65897692250244,24.8219643854307));
#51910=CARTESIAN_POINT('Ctrl Pts',(75.6923132292224,8.65879783026269,24.7728102144334));
#51911=CARTESIAN_POINT('Ctrl Pts',(75.6925532150177,8.6586101781166,24.7236580540939));
#51912=CARTESIAN_POINT('Ctrl Pts',(75.6953902922843,8.65640201617935,24.1696573197671));
#51913=CARTESIAN_POINT('Ctrl Pts',(75.6995064690153,8.64928079164444,23.1576519092927));
#51914=CARTESIAN_POINT('Ctrl Pts',(75.7103280108074,8.62912680918379,21.1444176786476));
#51915=CARTESIAN_POINT('Ctrl Pts',(75.7291509450652,8.61495252403147,19.6425276742755));
#51916=CARTESIAN_POINT('Ctrl Pts',(75.7594327416392,8.61193509309899,18.397120827803));
#51917=CARTESIAN_POINT('Ctrl Pts',(75.7767158149842,8.60615829648623,17.864843351189));
#51918=CARTESIAN_POINT('Ctrl Pts',(75.8250678816251,8.58547956144294,16.8429107530138));
#51919=CARTESIAN_POINT('Ctrl Pts',(75.9298815198313,8.54285802791338,15.0989495736632));
#51920=CARTESIAN_POINT('Ctrl Pts',(75.9978315522776,8.55572607586397,13.6999726172356));
#51921=CARTESIAN_POINT('Ctrl Pts',(75.983190075358,8.6425795941063,12.5772390575261));
#51922=CARTESIAN_POINT('Ctrl Pts',(75.9735243054875,8.68395341370793,12.0967435015462));
#51923=CARTESIAN_POINT('Ctrl Pts',(75.9417752207441,8.78149154793085,11.1511657014746));
#51924=CARTESIAN_POINT('Ctrl Pts',(75.8808350755608,8.93152341758648,9.95652328614932));
#51925=CARTESIAN_POINT('Ctrl Pts',(75.7827348239014,9.150895172005,8.52051663293493));
#51926=CARTESIAN_POINT('Ctrl Pts',(75.7040125639903,9.32420736540206,7.55808056960739));
#51927=CARTESIAN_POINT('Ctrl Pts',(75.6507853624626,9.44159633993459,6.95787391536139));
#51928=CARTESIAN_POINT('Ctrl Pts',(75.6279709087828,9.48720988729069,6.73800874146035));
#51929=CARTESIAN_POINT('Ctrl Pts',(75.5737377326004,9.58669194486765,6.27848372446474));
#51930=CARTESIAN_POINT('Ctrl Pts',(75.4618114014312,9.77627927411454,5.46037967472472));
#51931=CARTESIAN_POINT('Ctrl Pts',(75.2042613425529,10.2136783601429,3.74248125930447));
#51932=CARTESIAN_POINT('Ctrl Pts',(75.0088960863467,10.6627469527714,2.17071336334972));
#51933=CARTESIAN_POINT('Ctrl Pts',(74.944959962901,10.981253033238,1.03842468921417));
#51934=CARTESIAN_POINT('Ctrl Pts',(74.9402607665987,11.0169954680218,0.91882325276358));
#51935=CARTESIAN_POINT('Ctrl Pts',(74.9308100590913,11.0923951315099,0.670911402430064));
#51936=CARTESIAN_POINT('Ctrl Pts',(74.9185898285984,11.2290321678571,0.241146043059909));
#51937=CARTESIAN_POINT('Ctrl Pts',(74.9106916827709,11.4373076654428,-0.376998997526034));
#51938=CARTESIAN_POINT('Ctrl Pts',(74.916714958484,11.6983244017743,-1.12353421260398));
#51939=CARTESIAN_POINT('Ctrl Pts',(74.9434983842269,12.0509531026759,-2.13199781589735));
#51940=CARTESIAN_POINT('Ctrl Pts',(75.0080227454324,12.4805622284169,-3.4239925620957));
#51941=CARTESIAN_POINT('Ctrl Pts',(75.0746002971343,12.7666822976329,-4.50465271514652));
#51942=CARTESIAN_POINT('Ctrl Pts',(75.111308775638,12.9118512205026,-5.19568686901404));
#51943=CARTESIAN_POINT('Ctrl Pts',(75.1268413713536,12.9684034239111,-5.46586079559349));
#51944=CARTESIAN_POINT('Ctrl Pts',(75.1645636494145,13.0725467650836,-6.00799829553516));
#51945=CARTESIAN_POINT('Ctrl Pts',(75.244641386475,13.2327333351681,-6.95036646159278));
#51946=CARTESIAN_POINT('Ctrl Pts',(75.388561523126,13.398832966976,-8.28171045726725));
#51947=CARTESIAN_POINT('Ctrl Pts',(75.5307112116867,13.495115191397,-9.57979399837247));
#51948=CARTESIAN_POINT('Ctrl Pts',(75.6076903576886,13.5418896972981,-10.4684029145841));
#51949=CARTESIAN_POINT('Ctrl Pts',(75.6427125496599,13.5653831954232,-10.9705768831649));
#51950=CARTESIAN_POINT('Ctrl Pts',(75.6567949286975,13.5764163657282,-11.219687102322));
#51951=CARTESIAN_POINT('Ctrl Pts',(75.6659591397543,13.584614346601,-11.4068884650896));
#51952=CARTESIAN_POINT('Ctrl Pts',(75.6716655675417,13.5900814285709,-11.5428871613284));
#51953=CARTESIAN_POINT('Ctrl Pts',(75.6815054359044,13.5992084051951,-11.8080288277756));
#51954=CARTESIAN_POINT('Ctrl Pts',(75.694750288452,13.6113493218069,-12.2723888815295));
#51955=CARTESIAN_POINT('Ctrl Pts',(75.7071041132252,13.621656524442,-13.1891666318357));
#51956=CARTESIAN_POINT('Ctrl Pts',(75.6937196831686,13.606320519813,-14.4733937850652));
#51957=CARTESIAN_POINT('Ctrl Pts',(75.6670647741677,13.5781474141517,-15.6010295207835));
#51958=CARTESIAN_POINT('Ctrl Pts',(75.6527978341287,13.5628795901601,-16.343621465258));
#51959=CARTESIAN_POINT('Ctrl Pts',(75.644851449895,13.5543270872537,-16.8363600570689));
#51960=CARTESIAN_POINT('Ctrl Pts',(75.6413638372204,13.5504924104114,-17.2035737118605));
#51961=CARTESIAN_POINT('Ctrl Pts',(75.6406188912779,13.5495739023617,-17.5079155494171));
#51962=CARTESIAN_POINT('Ctrl Pts',(75.6403306860592,13.5492306750639,-17.6332689205196));
#51963=CARTESIAN_POINT('Ctrl Pts',(75.6397839187813,13.5486117359053,-17.8812884146137));
#51964=CARTESIAN_POINT('Ctrl Pts',(75.6392789801523,13.5480923740326,-18.1305446269046));
#51965=CARTESIAN_POINT('Ctrl Pts',(75.6388134337367,13.5476613064233,-18.3794207281482));
#51966=CARTESIAN_POINT('Ctrl Pts',(75.638538067035,13.5474270114781,-18.5351722177618));
#51967=CARTESIAN_POINT('Ctrl Pts',(75.6383268201157,13.5472593072431,-18.659770610816));
#51968=CARTESIAN_POINT('Ctrl Pts',(75.6381727881497,13.5471431295646,-18.7532550160439));
#51969=CARTESIAN_POINT('Ctrl Pts',(75.6380480220344,13.5470540416721,-18.8311735243319));
#51970=CARTESIAN_POINT('Ctrl Pts',(75.6379503208938,13.5469872704047,-18.8935211128262));
#51971=CARTESIAN_POINT('Ctrl Pts',(75.6371316346039,13.5464447006677,-19.423542940964));
#51972=CARTESIAN_POINT('Ctrl Pts',(75.6359351108233,13.5461755172403,-20.4390817726704));
#51973=CARTESIAN_POINT('Ctrl Pts',(75.634828360188,13.5467565616507,-21.9453949711133));
#51974=CARTESIAN_POINT('Ctrl Pts',(75.6342670266766,13.5469587534658,-22.9544223560489));
#51975=CARTESIAN_POINT('Ctrl Pts',(75.6338911420669,13.5467744906389,-23.5848356961732));
#51976=CARTESIAN_POINT('Ctrl Pts',(75.6337578246949,13.5467046700915,-23.8339636838752));
#51977=CARTESIAN_POINT('Ctrl Pts',(75.6335472035545,13.5465764365443,-24.333237735561));
#51978=CARTESIAN_POINT('Ctrl Pts',(75.6333112229087,13.5463810387052,-25.2086785091867));
#51979=CARTESIAN_POINT('Ctrl Pts',(75.633273505873,13.5461888092674,-26.4634348811356));
#51980=CARTESIAN_POINT('Ctrl Pts',(75.6334421176052,13.5460988580601,-27.9716593715141));
#51981=CARTESIAN_POINT('Ctrl Pts',(75.6335262374093,13.5461411274059,-28.9763405113967));
#51982=CARTESIAN_POINT('Ctrl Pts',(75.6335162580107,13.5461929051318,-29.5404813865156));
#51983=CARTESIAN_POINT('Ctrl Pts',(75.6335116717496,13.546205695701,-29.6658206594576));
#51984=CARTESIAN_POINT('Ctrl Pts',(75.6334941440586,13.5462364561623,-29.9165726274603));
#51985=CARTESIAN_POINT('Ctrl Pts',(75.6334441674742,13.5463038818912,-30.3555370725306));
#51986=CARTESIAN_POINT('Ctrl Pts',(75.6332866957545,13.5464864765899,-31.233946560225));
#51987=CARTESIAN_POINT('Ctrl Pts',(75.633012427691,13.5468616560165,-32.4894782454011));
#51988=CARTESIAN_POINT('Ctrl Pts',(75.6329779848593,13.5473140281086,-33.7439606386439));
#51989=CARTESIAN_POINT('Ctrl Pts',(75.6332773217597,13.547675246526,-34.7457481434029));
#51990=CARTESIAN_POINT('Ctrl Pts',(75.6335670343689,13.5478517301423,-35.2458674650133));
#51991=CARTESIAN_POINT('Ctrl Pts',(75.633848830281,13.5479780496411,-35.6215904838746));
#51992=CARTESIAN_POINT('Ctrl Pts',(75.6340681767887,13.5480441756403,-35.8734483901231));
#51993=CARTESIAN_POINT('Ctrl Pts',(75.6346144032638,13.5481148955266,-36.3762834856865));
#51994=CARTESIAN_POINT('Ctrl Pts',(75.6358149761765,13.5481248859595,-37.2546699759255));
#51995=CARTESIAN_POINT('Ctrl Pts',(75.6388918280923,13.5479599794559,-39.0064589139521));
#51996=CARTESIAN_POINT('Ctrl Pts',(75.64164937319,13.5485990819942,-40.5064445315137));
#51997=CARTESIAN_POINT('Ctrl Pts',(75.6428605986345,13.5506975221396,-41.7609180823806));
#51998=CARTESIAN_POINT('Ctrl Pts',(75.6431314381623,13.5508451721668,-42.1394333505526));
#51999=CARTESIAN_POINT('Ctrl Pts',(75.6433632198811,13.5504806601518,-42.6417446845613));
#52000=CARTESIAN_POINT('Ctrl Pts',(75.6435247248323,13.549883063377,-43.144287692992));
#52001=CARTESIAN_POINT('Ctrl Pts',(75.6436261736509,13.5489497761417,-43.7715478943923));
#52002=CARTESIAN_POINT('Ctrl Pts',(75.6436868543797,13.5483419216635,-44.5227689553694));
#52003=CARTESIAN_POINT('Ctrl Pts',(75.643770464559,13.5489307026378,-45.1469456734117));
#52004=CARTESIAN_POINT('Ctrl Pts',(75.6439086844781,13.5504500405917,-45.6449859955142));
#52005=CARTESIAN_POINT('Ctrl Pts',(75.6440605249743,13.5522152988932,-46.0177693785017));
#52006=CARTESIAN_POINT('Ctrl Pts',(75.6442733557844,13.5547047661443,-46.3897723471156));
#52007=CARTESIAN_POINT('Ctrl Pts',(75.644656281772,13.5591157996639,-46.8845688284039));
#52008=CARTESIAN_POINT('Ctrl Pts',(75.6450727331189,13.5638112097244,-47.2543912144994));
#52009=CARTESIAN_POINT('Ctrl Pts',(75.6456054473631,13.569620112677,-47.6236160183188));
#52010=CARTESIAN_POINT('Ctrl Pts',(75.6460158611401,13.5746647580007,-47.8579532218034));
#52011=CARTESIAN_POINT('Ctrl Pts',(75.6468902362759,13.5895954379087,-48.3395036708315));
#52012=CARTESIAN_POINT('Ctrl Pts',(75.6485756605151,13.6259076839064,-49.1907264409587));
#52013=CARTESIAN_POINT('Ctrl Pts',(75.6511845953537,13.6947708828899,-50.4450997762995));
#52014=CARTESIAN_POINT('Ctrl Pts',(75.6546283694998,13.760376303753,-52.0049425857155));
#52015=CARTESIAN_POINT('Ctrl Pts',(75.6575932745508,13.7599238349314,-53.0825947549811));
#52016=CARTESIAN_POINT('Ctrl Pts',(75.6599861051391,13.7342309340774,-53.7702079294383));
#52017=CARTESIAN_POINT('Ctrl Pts',(75.6612766328049,13.7172644585284,-54.0757846386637));
#52018=CARTESIAN_POINT('Ctrl Pts',(75.6642063201746,13.6662457593704,-54.6543510537387));
#52019=CARTESIAN_POINT('Ctrl Pts',(75.6698177772266,13.5417335286409,-55.6365739687886));
#52020=CARTESIAN_POINT('Ctrl Pts',(75.6803344558201,13.2231856481331,-57.4447430780544));
#52021=CARTESIAN_POINT('Ctrl Pts',(75.6812461445865,13.0596673289293,-58.7321420750093));
#52022=CARTESIAN_POINT('Ctrl Pts',(75.6863576792012,13.1064489388915,-59.4965882134124));
#52023=CARTESIAN_POINT('Ctrl Pts',(75.6868298303791,13.1140110602154,-59.6098960670077));
#52024=CARTESIAN_POINT('Ctrl Pts',(75.6878765509766,13.1316047602574,-59.8259658717656));
#52025=CARTESIAN_POINT('Ctrl Pts',(75.6896957250427,13.1707074094786,-60.2119341104625));
#52026=CARTESIAN_POINT('Ctrl Pts',(75.6934350108314,13.2796839737662,-60.9876625420266));
#52027=CARTESIAN_POINT('Ctrl Pts',(75.6976019424888,13.4705397296793,-61.8928354957714));
#52028=CARTESIAN_POINT('Ctrl Pts',(75.7014059645446,13.7166821115159,-62.8074682445014));
#52029=CARTESIAN_POINT('Ctrl Pts',(75.7033987287794,13.8735410785524,-63.3250187717106));
#52030=CARTESIAN_POINT('Ctrl Pts',(75.7046635121384,13.984796963924,-63.670703925322));
#52031=CARTESIAN_POINT('Ctrl Pts',(75.7054898861349,14.0606817798573,-63.9013515810976));
#52032=CARTESIAN_POINT('Ctrl Pts',(75.7062958025135,14.1390037284096,-64.1320971550734));
#52033=CARTESIAN_POINT('Ctrl Pts',(75.7069791147956,14.2095209049496,-64.3341496424494));
#52034=CARTESIAN_POINT('Ctrl Pts',(75.707363808776,14.2503552783613,-64.4496300809221));
#52035=CARTESIAN_POINT('Ctrl Pts',(75.7079366922177,14.3121216714576,-64.6228405330907));
#52036=CARTESIAN_POINT('Ctrl Pts',(75.7084008077015,14.3646731779577,-64.7672331121068));
#52037=CARTESIAN_POINT('Ctrl Pts',(75.7091894624142,14.4527084142938,-65.0056347430462));
#52038=CARTESIAN_POINT('Ctrl Pts',(75.7117295644385,14.5355494140757,-65.2185608369));
#52039=CARTESIAN_POINT('Ctrl Pts',(75.7156081698465,14.7248152544026,-65.6685602924904));
#52040=CARTESIAN_POINT('Ctrl Pts',(75.7221368537155,15.0933038646535,-66.4580645030462));
#52041=CARTESIAN_POINT('Ctrl Pts',(75.7305054466675,15.973436498,-68.0970319185886));
#52042=CARTESIAN_POINT('Ctrl Pts',(75.7285229169979,16.8715677772082,-69.5915478892842));
#52043=CARTESIAN_POINT('Ctrl Pts',(75.7230950724573,17.5030606903351,-70.79300135306));
#52044=CARTESIAN_POINT('Ctrl Pts',(75.7235707246569,17.6319456085467,-71.0375543406922));
#52045=CARTESIAN_POINT('Ctrl Pts',(75.7235352277703,17.897293641091,-71.5400698659183));
#52046=CARTESIAN_POINT('Ctrl Pts',(75.7238560437055,18.2272902790581,-72.1627996419));
#52047=CARTESIAN_POINT('Ctrl Pts',(75.7239705541676,18.6263398955066,-72.9134843431913));
#52048=CARTESIAN_POINT('Ctrl Pts',(75.7242235888834,19.4258440108923,-74.4139713263615));
#52049=CARTESIAN_POINT('Ctrl Pts',(75.7241877630892,20.0957322587687,-75.6668112765516));
#52050=CARTESIAN_POINT('Ctrl Pts',(75.7239228263678,21.0674470105801,-77.4942020668528));
#52051=CARTESIAN_POINT('Ctrl Pts',(75.7240381076587,21.5031469039378,-78.3134969859117));
#52052=CARTESIAN_POINT('Ctrl Pts',(75.7240381076589,21.9396684913276,-79.1344746880088));
#52053=CARTESIAN_POINT('Ctrl Pts',(77.5604728961388,8.92232863282295,24.831637685054));
#52054=CARTESIAN_POINT('Ctrl Pts',(77.5603493570431,8.9223354387487,24.7827883082522));
#52055=CARTESIAN_POINT('Ctrl Pts',(77.5602200765458,8.92234251567576,24.7339548685087));
#52056=CARTESIAN_POINT('Ctrl Pts',(77.5587043201865,8.92243143920465,24.1833245240063));
#52057=CARTESIAN_POINT('Ctrl Pts',(77.5541707126617,8.91819490443657,23.1672111498827));
#52058=CARTESIAN_POINT('Ctrl Pts',(77.5413564917759,8.90545159573916,21.1638460926666));
#52059=CARTESIAN_POINT('Ctrl Pts',(77.5316712108527,8.90605028564952,19.6764700508711));
#52060=CARTESIAN_POINT('Ctrl Pts',(77.5282133989158,8.92709808728221,18.448523681775));
#52061=CARTESIAN_POINT('Ctrl Pts',(77.5286669548489,8.93215210326381,17.9183992030719));
#52062=CARTESIAN_POINT('Ctrl Pts',(77.5346523607888,8.93339918176008,16.9032327124148));
#52063=CARTESIAN_POINT('Ctrl Pts',(77.5517074438493,8.93291389719877,15.1689361934228));
#52064=CARTESIAN_POINT('Ctrl Pts',(77.5545025014536,8.98867950575542,13.7837990376749));
#52065=CARTESIAN_POINT('Ctrl Pts',(77.5334676759905,9.12212002089865,12.6722367779447));
#52066=CARTESIAN_POINT('Ctrl Pts',(77.5228404246978,9.18526329919579,12.2029990094417));
#52067=CARTESIAN_POINT('Ctrl Pts',(77.4980025165873,9.33590048471274,11.2680893222593));
#52068=CARTESIAN_POINT('Ctrl Pts',(77.4599776567047,9.56976218287444,10.0770564394827));
#52069=CARTESIAN_POINT('Ctrl Pts',(77.4034435343428,9.90993885287635,8.62874999365388));
#52070=CARTESIAN_POINT('Ctrl Pts',(77.3556580024562,10.167949986372,7.65090706207837));
#52071=CARTESIAN_POINT('Ctrl Pts',(77.321538390164,10.3354614075502,7.03946341289537));
#52072=CARTESIAN_POINT('Ctrl Pts',(77.3107460750445,10.3972646607645,6.82714530720268));
#52073=CARTESIAN_POINT('Ctrl Pts',(77.2797603948243,10.5378416373698,6.37251376862689));
#52074=CARTESIAN_POINT('Ctrl Pts',(77.2107265384483,10.8110338890849,5.56040597038144));
#52075=CARTESIAN_POINT('Ctrl Pts',(77.0244884890886,11.4497714059702,3.83689517844971));
#52076=CARTESIAN_POINT('Ctrl Pts',(76.8477086808871,12.0394308712412,2.23618777764992));
#52077=CARTESIAN_POINT('Ctrl Pts',(76.8045266887848,12.3642912864388,1.02478882366062));
#52078=CARTESIAN_POINT('Ctrl Pts',(76.8018332405895,12.3998220875874,0.895053963897795));
#52079=CARTESIAN_POINT('Ctrl Pts',(76.7975599881676,12.4719209199013,0.627727535400199));
#52080=CARTESIAN_POINT('Ctrl Pts',(76.7961484035108,12.5954373158584,0.164847484187591));
#52081=CARTESIAN_POINT('Ctrl Pts',(76.8081210516562,12.7669303911879,-0.496937328452192));
#52082=CARTESIAN_POINT('Ctrl Pts',(76.8421695164869,12.9613919414899,-1.28751891755477));
#52083=CARTESIAN_POINT('Ctrl Pts',(76.907368785551,13.2023184560712,-2.34000853818552));
#52084=CARTESIAN_POINT('Ctrl Pts',(77.0165417606542,13.4604237900536,-3.65296048391174));
#52085=CARTESIAN_POINT('Ctrl Pts',(77.1017261429008,13.6092121570947,-4.70299436939395));
#52086=CARTESIAN_POINT('Ctrl Pts',(77.1431648681345,13.6839081189796,-5.36010504112367));
#52087=CARTESIAN_POINT('Ctrl Pts',(77.1600267658594,13.7126643979356,-5.64135389354874));
#52088=CARTESIAN_POINT('Ctrl Pts',(77.1964793930761,13.7580485585429,-6.18849990687238));
#52089=CARTESIAN_POINT('Ctrl Pts',(77.2650550752343,13.8119150283283,-7.13940043609606));
#52090=CARTESIAN_POINT('Ctrl Pts',(77.3689169294206,13.8308884985355,-8.45695460822024));
#52091=CARTESIAN_POINT('Ctrl Pts',(77.462013437121,13.816844559987,-9.72341652820403));
#52092=CARTESIAN_POINT('Ctrl Pts',(77.5127825171445,13.8093833979168,-10.5800335004951));
#52093=CARTESIAN_POINT('Ctrl Pts',(77.5362618868962,13.8084300066986,-11.0609219709444));
#52094=CARTESIAN_POINT('Ctrl Pts',(77.5459376584656,13.809491089976,-11.2982666676243));
#52095=CARTESIAN_POINT('Ctrl Pts',(77.5523645061952,13.8110319626543,-11.4761344552283));
#52096=CARTESIAN_POINT('Ctrl Pts',(77.5563684421625,13.8120414729932,-11.6047533692288));
#52097=CARTESIAN_POINT('Ctrl Pts',(77.563207858177,13.8137762526411,-11.8565333451865));
#52098=CARTESIAN_POINT('Ctrl Pts',(77.5722345549043,13.8162026642452,-12.2989412671837));
#52099=CARTESIAN_POINT('Ctrl Pts',(77.5797025409249,13.8189354435846,-13.1791858349696));
#52100=CARTESIAN_POINT('Ctrl Pts',(77.567442235306,13.8185734893195,-14.4318920297639));
#52101=CARTESIAN_POINT('Ctrl Pts',(77.5460838146306,13.8157763860591,-15.5573993650377));
#52102=CARTESIAN_POINT('Ctrl Pts',(77.5346131764236,13.8141983409583,-16.3094404958222));
#52103=CARTESIAN_POINT('Ctrl Pts',(77.5281856114487,13.8133451222479,-16.8112991818371));
#52104=CARTESIAN_POINT('Ctrl Pts',(77.5252183902111,13.8130219840261,-17.1885933255562));
#52105=CARTESIAN_POINT('Ctrl Pts',(77.5243996636297,13.8130791069995,-17.5028139971062));
#52106=CARTESIAN_POINT('Ctrl Pts',(77.5240871618263,13.8130991471089,-17.6275881030977));
#52107=CARTESIAN_POINT('Ctrl Pts',(77.5235038017461,13.8131319862885,-17.8770200759137));
#52108=CARTESIAN_POINT('Ctrl Pts',(77.5229737621476,13.8131503186923,-18.1266527225266));
#52109=CARTESIAN_POINT('Ctrl Pts',(77.5225027146661,13.8131612174878,-18.3763532857022));
#52110=CARTESIAN_POINT('Ctrl Pts',(77.5222286852055,13.8131635716777,-18.5324781127209));
#52111=CARTESIAN_POINT('Ctrl Pts',(77.5220225660326,13.8131636975449,-18.6574033620728));
#52112=CARTESIAN_POINT('Ctrl Pts',(77.5218738432195,13.813162692245,-18.751114001786));
#52113=CARTESIAN_POINT('Ctrl Pts',(77.521754696824,13.8131609973018,-18.8292191327213));
#52114=CARTESIAN_POINT('Ctrl Pts',(77.5216623650211,13.8131592229898,-18.8917108710437));
#52115=CARTESIAN_POINT('Ctrl Pts',(77.5208923228423,13.8131409579113,-19.4229383341762));
#52116=CARTESIAN_POINT('Ctrl Pts',(77.5198724781134,13.8130142665158,-20.4400567461457));
#52117=CARTESIAN_POINT('Ctrl Pts',(77.5191849299256,13.8127636053189,-21.9468185573054));
#52118=CARTESIAN_POINT('Ctrl Pts',(77.5188102789848,13.8126523539833,-22.9548510961017));
#52119=CARTESIAN_POINT('Ctrl Pts',(77.5184901432129,13.8126348355234,-23.5842786925733));
#52120=CARTESIAN_POINT('Ctrl Pts',(77.518378556833,13.8126299471196,-23.833530244898));
#52121=CARTESIAN_POINT('Ctrl Pts',(77.5182042363923,13.8126263820134,-24.3327687054052));
#52122=CARTESIAN_POINT('Ctrl Pts',(77.5180151513301,13.8126344714252,-25.208307411824));
#52123=CARTESIAN_POINT('Ctrl Pts',(77.5180051341375,13.8126742818782,-26.4631549208369));
#52124=CARTESIAN_POINT('Ctrl Pts',(77.5181998543373,13.8127276901683,-27.9716117860686));
#52125=CARTESIAN_POINT('Ctrl Pts',(77.5183118867057,13.8127381523655,-28.9764795533715));
#52126=CARTESIAN_POINT('Ctrl Pts',(77.5183308400025,13.8127295345326,-29.5407447854088));
#52127=CARTESIAN_POINT('Ctrl Pts',(77.5183339048034,13.812727087905,-29.666131624305));
#52128=CARTESIAN_POINT('Ctrl Pts',(77.5183347783658,13.8127200803141,-29.9169621574733));
#52129=CARTESIAN_POINT('Ctrl Pts',(77.5183243363575,13.8127027278597,-30.3560580092875));
#52130=CARTESIAN_POINT('Ctrl Pts',(77.518269227131,13.8126510859042,-31.2346771096834));
#52131=CARTESIAN_POINT('Ctrl Pts',(77.5181715016671,13.8125492224116,-32.4903732179553));
#52132=CARTESIAN_POINT('Ctrl Pts',(77.5182537665264,13.8124629578631,-33.7448337842219));
#52133=CARTESIAN_POINT('Ctrl Pts',(77.5185517121816,13.8124355035215,-34.7464923619268));
#52134=CARTESIAN_POINT('Ctrl Pts',(77.5187986221067,13.8124413142602,-35.2465094381523));
#52135=CARTESIAN_POINT('Ctrl Pts',(77.5190288078211,13.8124547826457,-35.6221430941577));
#52136=CARTESIAN_POINT('Ctrl Pts',(77.5192053564713,13.8124450077209,-35.8740052140173));
#52137=CARTESIAN_POINT('Ctrl Pts',(77.5196367643728,13.8123646406697,-36.3768122071899));
#52138=CARTESIAN_POINT('Ctrl Pts',(77.5205700476009,13.8121075927323,-37.2551664983108));
#52139=CARTESIAN_POINT('Ctrl Pts',(77.5229237682906,13.8114319945058,-39.0068748203133));
#52140=CARTESIAN_POINT('Ctrl Pts',(77.5250122180607,13.8116906843296,-40.5067882721922));
#52141=CARTESIAN_POINT('Ctrl Pts',(77.5259381954873,13.813562957597,-41.7611981469901));
#52142=CARTESIAN_POINT('Ctrl Pts',(77.5261466829081,13.8136486587969,-42.1397048423366));
#52143=CARTESIAN_POINT('Ctrl Pts',(77.5263276066643,13.8132122244767,-42.6419967409788));
#52144=CARTESIAN_POINT('Ctrl Pts',(77.5264555505707,13.8125484706242,-43.1445197670677));
#52145=CARTESIAN_POINT('Ctrl Pts',(77.5265392299621,13.8115434069221,-43.771750998851));
#52146=CARTESIAN_POINT('Ctrl Pts',(77.5265911327969,13.8108650239228,-44.5229319723421));
#52147=CARTESIAN_POINT('Ctrl Pts',(77.5266560653333,13.8114066209184,-45.1470702553536));
#52148=CARTESIAN_POINT('Ctrl Pts',(77.526759449157,13.8128950100562,-45.6450776120453));
#52149=CARTESIAN_POINT('Ctrl Pts',(77.5268719395928,13.8146399341467,-46.0178347404532));
#52150=CARTESIAN_POINT('Ctrl Pts',(77.527028916975,13.8171118245038,-46.3898099848536));
#52151=CARTESIAN_POINT('Ctrl Pts',(77.5273111040197,13.8215026578271,-46.8845677443817));
#52152=CARTESIAN_POINT('Ctrl Pts',(77.5276172544658,13.8261866864606,-47.2543582726095));
#52153=CARTESIAN_POINT('Ctrl Pts',(77.5280099686407,13.8319856870836,-47.6235498894623));
#52154=CARTESIAN_POINT('Ctrl Pts',(77.5283224254491,13.8370251439549,-47.8578555760083));
#52155=CARTESIAN_POINT('Ctrl Pts',(77.5289836202813,13.8519535520393,-48.339354009538));
#52156=CARTESIAN_POINT('Ctrl Pts',(77.5302513326552,13.8882797198523,-49.1904957378282));
#52157=CARTESIAN_POINT('Ctrl Pts',(77.5321365443416,13.9572103613029,-50.4447910137057));
#52158=CARTESIAN_POINT('Ctrl Pts',(77.5345196910022,14.0229255419454,-52.0045983515733));
#52159=CARTESIAN_POINT('Ctrl Pts',(77.5366551468569,14.0225402161045,-53.0822690254463));
#52160=CARTESIAN_POINT('Ctrl Pts',(77.5384933987961,13.9968718774403,-53.7699066660649));
#52161=CARTESIAN_POINT('Ctrl Pts',(77.539544778281,13.9799211159562,-54.0754555282557));
#52162=CARTESIAN_POINT('Ctrl Pts',(77.5419458309468,13.9289293555925,-54.6539969527055));
#52163=CARTESIAN_POINT('Ctrl Pts',(77.5465201665502,13.8044596468729,-55.6361849190021));
#52164=CARTESIAN_POINT('Ctrl Pts',(77.5546852113387,13.485954960897,-57.4443545537156));
#52165=CARTESIAN_POINT('Ctrl Pts',(77.5536961524377,13.322378317418,-58.7318441547698));
#52166=CARTESIAN_POINT('Ctrl Pts',(77.5580618267775,13.3691275726486,-59.4964367021951));
#52167=CARTESIAN_POINT('Ctrl Pts',(77.5584463406522,13.3766868573184,-59.6097601494794));
#52168=CARTESIAN_POINT('Ctrl Pts',(77.5593301880504,13.3942737779871,-59.825860501517));
#52169=CARTESIAN_POINT('Ctrl Pts',(77.5608951149712,13.4333639449777,-60.2118774121813));
#52170=CARTESIAN_POINT('Ctrl Pts',(77.5642389625225,13.5423107223386,-60.9876858226565));
#52171=CARTESIAN_POINT('Ctrl Pts',(77.5681638311065,13.7331210512987,-61.8929098456432));
#52172=CARTESIAN_POINT('Ctrl Pts',(77.571838979276,13.979209515868,-62.8075572239394));
#52173=CARTESIAN_POINT('Ctrl Pts',(77.573783286313,14.136036565878,-63.3251031269268));
#52174=CARTESIAN_POINT('Ctrl Pts',(77.5750180640539,14.2472713001593,-63.6707801762678));
#52175=CARTESIAN_POINT('Ctrl Pts',(77.5758245506604,14.3231420864373,-63.9014210705629));
#52176=CARTESIAN_POINT('Ctrl Pts',(77.5766099015153,14.4014502698545,-64.1321579673947));
#52177=CARTESIAN_POINT('Ctrl Pts',(77.5772733489536,14.4719557255358,-64.3342011137818));
#52178=CARTESIAN_POINT('Ctrl Pts',(77.5776459531678,14.5127835239758,-64.4496757244623));
#52179=CARTESIAN_POINT('Ctrl Pts',(77.5781998706167,14.5745401929167,-64.6228769593256));
#52180=CARTESIAN_POINT('Ctrl Pts',(77.5786462129329,14.6270838893925,-64.767260806259));
#52181=CARTESIAN_POINT('Ctrl Pts',(77.5794018194922,14.7151068641564,-65.0056469865528));
#52182=CARTESIAN_POINT('Ctrl Pts',(77.5819117301522,14.7979431048304,-65.2185757513146));
#52183=CARTESIAN_POINT('Ctrl Pts',(77.5857459671956,14.9871981458478,-65.6685704184725));
#52184=CARTESIAN_POINT('Ctrl Pts',(77.592233829575,15.3556765477811,-66.4580724905346));
#52185=CARTESIAN_POINT('Ctrl Pts',(77.6006340957855,16.2358080969961,-68.0970343525443));
#52186=CARTESIAN_POINT('Ctrl Pts',(77.5987537175233,17.1339558157083,-69.5915520005254));
#52187=CARTESIAN_POINT('Ctrl Pts',(77.5933231368364,17.7654478982166,-70.7930076564631));
#52188=CARTESIAN_POINT('Ctrl Pts',(77.5937988748601,17.8943323860493,-71.0375602056355));
#52189=CARTESIAN_POINT('Ctrl Pts',(77.5937632152446,18.1596798707538,-71.5400754235968));
#52190=CARTESIAN_POINT('Ctrl Pts',(77.5940840363107,18.4896760382719,-72.1628047274669));
#52191=CARTESIAN_POINT('Ctrl Pts',(77.5941985862454,18.8887254494592,-72.9134890727134));
#52192=CARTESIAN_POINT('Ctrl Pts',(77.5944518616113,19.6882296468342,-74.4139755411582));
#52193=CARTESIAN_POINT('Ctrl Pts',(77.5944162020427,20.3581187868093,-75.6668158277755));
#52194=CARTESIAN_POINT('Ctrl Pts',(77.5941510398116,21.3298339704383,-77.4942075157172));
#52195=CARTESIAN_POINT('Ctrl Pts',(77.5942663414283,21.7655337658572,-78.3135022343861));
#52196=CARTESIAN_POINT('Ctrl Pts',(77.5942663414295,22.2020553532467,-79.1344799364846));
#52197=CARTESIAN_POINT('Ctrl Pts',(78.4944431928074,9.05472319120301,24.8422120491812));
#52198=CARTESIAN_POINT('Ctrl Pts',(78.4941090996625,9.05495389158687,24.79369851169));
#52199=CARTESIAN_POINT('Ctrl Pts',(78.493759402762,9.05519524519429,24.7452129330012));
#52200=CARTESIAN_POINT('Ctrl Pts',(78.4896386357447,9.05804650036688,24.1983783588369));
#52201=CARTESIAN_POINT('Ctrl Pts',(78.4798996030533,9.05886922538468,23.181079865532));
#52202=CARTESIAN_POINT('Ctrl Pts',(78.4531620503516,9.05915179220653,21.1871854887968));
#52203=CARTESIAN_POINT('Ctrl Pts',(78.4266520106487,9.07673406666645,19.710806800959));
#52204=CARTESIAN_POINT('Ctrl Pts',(78.4037275756009,9.11889086547707,18.495513535801));
#52205=CARTESIAN_POINT('Ctrl Pts',(78.3942568697667,9.13425597018717,17.9735746968858));
#52206=CARTESIAN_POINT('Ctrl Pts',(78.3756192466889,9.15833365518852,16.9680112857039));
#52207=CARTESIAN_POINT('Ctrl Pts',(78.3429789670015,9.20099516530317,15.2406404115276));
#52208=CARTESIAN_POINT('Ctrl Pts',(78.3159389388634,9.29108207535428,13.8416153133473));
#52209=CARTESIAN_POINT('Ctrl Pts',(78.2930576982901,9.4564531271892,12.7110753825502));
#52210=CARTESIAN_POINT('Ctrl Pts',(78.2829059329715,9.5323412143847,12.243553384385));
#52211=CARTESIAN_POINT('Ctrl Pts',(78.2620281608176,9.71268002071975,11.304618676111));
#52212=CARTESIAN_POINT('Ctrl Pts',(78.2337441668383,9.98800839152576,10.1083439598779));
#52213=CARTESIAN_POINT('Ctrl Pts',(78.1943694058521,10.3776671196108,8.64933905863135));
#52214=CARTESIAN_POINT('Ctrl Pts',(78.1617028150339,10.6634373708522,7.66204859777137));
#52215=CARTESIAN_POINT('Ctrl Pts',(78.138675834175,10.8451931975712,7.04333807577186));
#52216=CARTESIAN_POINT('Ctrl Pts',(78.133284707382,10.91279587007,6.83011630244702));
#52217=CARTESIAN_POINT('Ctrl Pts',(78.1148497326943,11.0649203335883,6.3732471355136));
#52218=CARTESIAN_POINT('Ctrl Pts',(78.0724604624009,11.3579055907103,5.55881360490552));
#52219=CARTESIAN_POINT('Ctrl Pts',(77.9531033376769,12.0288023749603,3.83067103963575));
#52220=CARTESIAN_POINT('Ctrl Pts',(77.8409734441138,12.6322082264952,2.21796256708511));
#52221=CARTESIAN_POINT('Ctrl Pts',(77.8219828150867,12.9419384726309,0.991072244389946));
#52222=CARTESIAN_POINT('Ctrl Pts',(77.8215972792297,12.975935451507,0.857316122256786));
#52223=CARTESIAN_POINT('Ctrl Pts',(77.8219267219958,13.0435170228269,0.58349967768362));
#52224=CARTESIAN_POINT('Ctrl Pts',(77.8276567418555,13.1564000121974,0.109434330121606));
#52225=CARTESIAN_POINT('Ctrl Pts',(77.8480946596581,13.3048998846505,-0.565528789552421));
#52226=CARTESIAN_POINT('Ctrl Pts',(77.8890671108874,13.4621622433645,-1.36765415444729));
#52227=CARTESIAN_POINT('Ctrl Pts',(77.9598017899087,13.6450089607257,-2.42939005995793));
#52228=CARTESIAN_POINT('Ctrl Pts',(78.0673887569699,13.8241004616619,-3.74124171730161));
#52229=CARTESIAN_POINT('Ctrl Pts',(78.1457996681103,13.9209575761983,-4.77638478515412));
#52230=CARTESIAN_POINT('Ctrl Pts',(78.1830513985844,13.970442181397,-5.42026114022125));
#52231=CARTESIAN_POINT('Ctrl Pts',(78.1978295335833,13.9887362190921,-5.70206761049167));
#52232=CARTESIAN_POINT('Ctrl Pts',(78.2283353769435,14.0140207271012,-6.24661171807938));
#52233=CARTESIAN_POINT('Ctrl Pts',(78.2827028003512,14.0343205019205,-7.19391202090573));
#52234=CARTESIAN_POINT('Ctrl Pts',(78.359136378551,14.0116016943059,-8.50391706664852));
#52235=CARTESIAN_POINT('Ctrl Pts',(78.423976017323,13.9655408145372,-9.76132343244577));
#52236=CARTESIAN_POINT('Ctrl Pts',(78.4589425569872,13.9419477084446,-10.6099258168552));
#52237=CARTESIAN_POINT('Ctrl Pts',(78.4753458853024,13.9336425316214,-11.0859840763551));
#52238=CARTESIAN_POINT('Ctrl Pts',(78.4822600622728,13.9316444870457,-11.3208245121042));
#52239=CARTESIAN_POINT('Ctrl Pts',(78.4869465685096,13.9311036750484,-11.4967517629155));
#52240=CARTESIAN_POINT('Ctrl Pts',(78.4898770373256,13.9307321440272,-11.623045554729));
#52241=CARTESIAN_POINT('Ctrl Pts',(78.4948702825629,13.9301885643896,-11.8709732103692));
#52242=CARTESIAN_POINT('Ctrl Pts',(78.5014546892992,13.9296568401639,-12.3068657247852));
#52243=CARTESIAN_POINT('Ctrl Pts',(78.5069032837125,13.9302020950339,-13.1764570240478));
#52244=CARTESIAN_POINT('Ctrl Pts',(78.4978378653358,13.9344964994918,-14.4200848218227));
#52245=CARTESIAN_POINT('Ctrl Pts',(78.4820063937416,13.9395702721035,-15.5449319278543));
#52246=CARTESIAN_POINT('Ctrl Pts',(78.4734805308755,13.9422589450028,-16.2996340877095));
#52247=CARTESIAN_POINT('Ctrl Pts',(78.4686845731225,13.9437987418975,-16.8040935922028));
#52248=CARTESIAN_POINT('Ctrl Pts',(78.466476154674,13.9445889988638,-17.1842831031095));
#52249=CARTESIAN_POINT('Ctrl Pts',(78.4658437641202,13.9449513613105,-17.5013555911005));
#52250=CARTESIAN_POINT('Ctrl Pts',(78.4656010874182,13.9450851860882,-17.6259547666494));
#52251=CARTESIAN_POINT('Ctrl Pts',(78.4651447089073,13.9453221683621,-17.8757847301294));
#52252=CARTESIAN_POINT('Ctrl Pts',(78.4647301387349,13.9455144798975,-18.1255167174223));
#52253=CARTESIAN_POINT('Ctrl Pts',(78.4643542822628,13.9456664704443,-18.3754473313692));
#52254=CARTESIAN_POINT('Ctrl Pts',(78.464134732944,13.945745754614,-18.5316753566071));
#52255=CARTESIAN_POINT('Ctrl Pts',(78.4639679306339,13.9458002634768,-18.6566914677372));
#52256=CARTESIAN_POINT('Ctrl Pts',(78.4638471299424,13.9458368577808,-18.7504649012776));
#52257=CARTESIAN_POINT('Ctrl Pts',(78.4637499605465,13.9458639021429,-18.8286219308702));
#52258=CARTESIAN_POINT('Ctrl Pts',(78.4636742768409,13.9458835255714,-18.8911537046507));
#52259=CARTESIAN_POINT('Ctrl Pts',(78.463042393415,13.9460392519842,-19.4227165195588));
#52260=CARTESIAN_POINT('Ctrl Pts',(78.4621900746086,13.9459949146705,-20.440284171059));
#52261=CARTESIAN_POINT('Ctrl Pts',(78.4615280251198,13.9455267728767,-21.9471797075837));
#52262=CARTESIAN_POINT('Ctrl Pts',(78.4611999873932,13.9453399496592,-22.9549425208703));
#52263=CARTESIAN_POINT('Ctrl Pts',(78.4609431021595,13.9453828946249,-23.5841025152867));
#52264=CARTESIAN_POINT('Ctrl Pts',(78.4608535890108,13.9454010566074,-23.8333894477468));
#52265=CARTESIAN_POINT('Ctrl Pts',(78.4607184682495,13.9454414150757,-24.3326208669306));
#52266=CARTESIAN_POINT('Ctrl Pts',(78.4605860170337,13.9455196094341,-25.2081915966555));
#52267=CARTESIAN_POINT('Ctrl Pts',(78.4606293995287,13.9456374044057,-26.4630707237769));
#52268=CARTESIAN_POINT('Ctrl Pts',(78.4608481281189,13.9457336479593,-27.9715986041808));
#52269=CARTESIAN_POINT('Ctrl Pts',(78.4609673331931,13.9457344249985,-28.9765203813875));
#52270=CARTESIAN_POINT('Ctrl Pts',(78.4609884526296,13.9457063344184,-29.540821666395));
#52271=CARTESIAN_POINT('Ctrl Pts',(78.4609918239648,13.9456988577156,-29.6662231086672));
#52272=CARTESIAN_POINT('Ctrl Pts',(78.4609937810264,13.9456794893836,-29.9170775082585));
#52273=CARTESIAN_POINT('Ctrl Pts',(78.4609860880103,13.9456348791229,-30.3562133193338));
#52274=CARTESIAN_POINT('Ctrl Pts',(78.4609380217542,13.9455082933016,-31.2348958299418));
#52275=CARTESIAN_POINT('Ctrl Pts',(78.4608427072243,13.9452560614607,-32.4906412365538));
#52276=CARTESIAN_POINT('Ctrl Pts',(78.4608903888004,13.9449994336256,-33.7450945241474));
#52277=CARTESIAN_POINT('Ctrl Pts',(78.4611216241635,13.9448455174262,-34.7467138347845));
#52278=CARTESIAN_POINT('Ctrl Pts',(78.4613193079934,13.9447958246403,-35.2466997987045));
#52279=CARTESIAN_POINT('Ctrl Pts',(78.461505640177,13.9447715070098,-35.6223062745813));
#52280=CARTESIAN_POINT('Ctrl Pts',(78.4616488668374,13.9447361246778,-35.8741696747715));
#52281=CARTESIAN_POINT('Ctrl Pts',(78.4620000281453,13.944603781278,-36.3769680926777));
#52282=CARTESIAN_POINT('Ctrl Pts',(78.4627607934637,13.9442552423288,-37.2553128588882));
#52283=CARTESIAN_POINT('Ctrl Pts',(78.4646856170524,13.9433973484837,-39.0069967046669));
#52284=CARTESIAN_POINT('Ctrl Pts',(78.4663917055818,13.9435233444552,-40.5068899646765));
#52285=CARTESIAN_POINT('Ctrl Pts',(78.46714472153,13.9453184823223,-41.7612812521414));
#52286=CARTESIAN_POINT('Ctrl Pts',(78.4673136122907,13.9453830940369,-42.1397854037017));
#52287=CARTESIAN_POINT('Ctrl Pts',(78.4674590403002,13.944922388335,-42.6420714137411));
#52288=CARTESIAN_POINT('Ctrl Pts',(78.4675606952721,13.944236753947,-43.1445884497504));
#52289=CARTESIAN_POINT('Ctrl Pts',(78.4676249130845,13.9432084599653,-43.7718110240772));
#52290=CARTESIAN_POINT('Ctrl Pts',(78.4676621414338,13.9425076337916,-44.5229801532958));
#52291=CARTESIAN_POINT('Ctrl Pts',(78.4677114744421,13.9430341003948,-45.1471072349507));
#52292=CARTESIAN_POINT('Ctrl Pts',(78.4677941646448,13.9445118311423,-45.6451047487846));
#52293=CARTESIAN_POINT('Ctrl Pts',(78.4678853687203,13.9462493848491,-46.0178540917725));
#52294=CARTESIAN_POINT('Ctrl Pts',(78.4680137314505,13.9487143687068,-46.3898211431151));
#52295=CARTESIAN_POINT('Ctrl Pts',(78.468245817902,13.9530964035972,-46.8845673874747));
#52296=CARTESIAN_POINT('Ctrl Pts',(78.4684987565137,13.9577740969672,-47.2543487119385));
#52297=CARTESIAN_POINT('Ctrl Pts',(78.4688242791751,13.9635665868806,-47.6235305269572));
#52298=CARTESIAN_POINT('Ctrl Pts',(78.4690901755611,13.9686021051196,-47.8578271204967));
#52299=CARTESIAN_POINT('Ctrl Pts',(78.4696516956716,13.9835247681664,-48.3393103767143));
#52300=CARTESIAN_POINT('Ctrl Pts',(78.4707272102901,14.0198457808104,-49.1904283932384));
#52301=CARTESIAN_POINT('Ctrl Pts',(78.4722864807893,14.0887798041541,-50.4447004336901));
#52302=CARTESIAN_POINT('Ctrl Pts',(78.4741878925538,14.1545044719243,-52.0044960602158));
#52303=CARTESIAN_POINT('Ctrl Pts',(78.4759415582901,14.1541186517246,-53.0821713407886));
#52304=CARTESIAN_POINT('Ctrl Pts',(78.4775197830763,14.128444258846,-53.7698156277294));
#52305=CARTESIAN_POINT('Ctrl Pts',(78.4784589984044,14.1114926364803,-54.0753552618592));
#52306=CARTESIAN_POINT('Ctrl Pts',(78.4806112561439,14.0604964950487,-54.6538882235983));
#52307=CARTESIAN_POINT('Ctrl Pts',(78.484696308313,13.9360143457923,-55.6360647242936));
#52308=CARTESIAN_POINT('Ctrl Pts',(78.4917435111746,13.6174640782452,-57.4442357062244));
#52309=CARTESIAN_POINT('Ctrl Pts',(78.489846084057,13.4538183235814,-58.7317543181104));
#52310=CARTESIAN_POINT('Ctrl Pts',(78.493853653258,13.5005381781814,-59.4963920782044));
#52311=CARTESIAN_POINT('Ctrl Pts',(78.4941958612439,13.5080944186318,-59.6097203083738));
#52312=CARTESIAN_POINT('Ctrl Pts',(78.4950009250074,13.5256751424072,-59.8258300484725));
#52313=CARTESIAN_POINT('Ctrl Pts',(78.4964423261334,13.5647549519809,-60.2118618619371));
#52314=CARTESIAN_POINT('Ctrl Pts',(78.4995917413089,13.6736820495239,-60.9876947443874));
#52315=CARTESIAN_POINT('Ctrl Pts',(78.5033926265082,13.864471271119,-61.8929344557591));
#52316=CARTESIAN_POINT('Ctrl Pts',(78.506997430927,14.1105389952847,-62.8075866886342));
#52317=CARTESIAN_POINT('Ctrl Pts',(78.5089138128884,14.2673546408238,-63.3251314947716));
#52318=CARTESIAN_POINT('Ctrl Pts',(78.5101313622486,14.3785819038062,-63.670806272742));
#52319=CARTESIAN_POINT('Ctrl Pts',(78.5109264734954,14.4544477553733,-63.9014452443889));
#52320=CARTESIAN_POINT('Ctrl Pts',(78.5117003346679,14.5327510772896,-64.1321796173828));
#52321=CARTESIAN_POINT('Ctrl Pts',(78.5123529433146,14.6032523571431,-64.3342200198336));
#52322=CARTESIAN_POINT('Ctrl Pts',(78.512719049699,14.6440777935191,-64.4496929092764));
#52323=CARTESIAN_POINT('Ctrl Pts',(78.5132628684145,14.7058309470756,-64.6228914140419));
#52324=CARTESIAN_POINT('Ctrl Pts',(78.5136999945135,14.7583717665777,-64.767272657901));
#52325=CARTESIAN_POINT('Ctrl Pts',(78.5144387501633,14.8463901122126,-65.0056542121464));
#52326=CARTESIAN_POINT('Ctrl Pts',(78.5169338299697,14.9292242776233,-65.2185839652863));
#52327=CARTESIAN_POINT('Ctrl Pts',(78.5207461591452,15.1184751040468,-65.6685774074326));
#52328=CARTESIAN_POINT('Ctrl Pts',(78.5272145085589,15.4869498109295,-66.4580791539563));
#52329=CARTESIAN_POINT('Ctrl Pts',(78.5356322362024,16.3670826107093,-68.0970395727417));
#52330=CARTESIAN_POINT('Ctrl Pts',(78.5338034505173,17.2652381054602,-69.5915577683127));
#52331=CARTESIAN_POINT('Ctrl Pts',(78.5283703489949,17.8967293937733,-70.7930139710155));
#52332=CARTESIAN_POINT('Ctrl Pts',(78.5288462002196,18.0256137916774,-71.0375664036789));
#52333=CARTESIAN_POINT('Ctrl Pts',(78.5288104159599,18.2909610994936,-71.540081533252));
#52334=CARTESIAN_POINT('Ctrl Pts',(78.5291313145272,18.620957153872,-72.1628107124065));
#52335=CARTESIAN_POINT('Ctrl Pts',(78.5292459193545,19.0200065150567,-72.9134949563425));
#52336=CARTESIAN_POINT('Ctrl Pts',(78.52949943309,19.8195107725196,-74.4139812784567));
#52337=CARTESIAN_POINT('Ctrl Pts',(78.5294640739157,20.489400205506,-75.6668216809661));
#52338=CARTESIAN_POINT('Ctrl Pts',(78.5291988379399,21.461115499897,-77.494213646795));
#52339=CARTESIAN_POINT('Ctrl Pts',(78.5293142151722,21.8968152797781,-78.3135083149078));
#52340=CARTESIAN_POINT('Ctrl Pts',(78.5293142151733,22.3333368671674,-79.1344860170071));
#52341=CARTESIAN_POINT('',(-4.76125591968157E-15,2.14773017928896,-8.66962570190719));
#52342=CARTESIAN_POINT('',(-10.8669314563932,2.70458533911839,-5.6515925146482));
#52343=CARTESIAN_POINT('Ctrl Pts',(-4.42970115563661E-15,2.14773017928896,
-8.66962570190719));
#52344=CARTESIAN_POINT('Ctrl Pts',(-0.732788448239405,2.14811194208377,
-8.63073774781089));
#52345=CARTESIAN_POINT('Ctrl Pts',(-2.74012589153777,2.08364837443475,-8.55044425906516));
#52346=CARTESIAN_POINT('Ctrl Pts',(-4.65602395402778,1.93383212333491,-8.52049681196753));
#52347=CARTESIAN_POINT('Ctrl Pts',(-6.35178884646186,1.89995064476493,-8.21329860288647));
#52348=CARTESIAN_POINT('Ctrl Pts',(-7.78927254448508,1.96366399905155,-7.6984650995689));
#52349=CARTESIAN_POINT('Ctrl Pts',(-9.41546628484877,2.25717994847875,-6.74202902301025));
#52350=CARTESIAN_POINT('Ctrl Pts',(-10.402035668676,2.55608056709905,-6.0139438933557));
#52351=CARTESIAN_POINT('Ctrl Pts',(-10.8669314563932,2.70458533911839,-5.6515925146482));
#52352=CARTESIAN_POINT('',(10.8669314593876,2.70458534007494,-5.65159251231429));
#52353=CARTESIAN_POINT('Ctrl Pts',(10.8669314593876,2.70458534007494,-5.65159251231429));
#52354=CARTESIAN_POINT('Ctrl Pts',(9.84130490508928,2.37696258947676,-6.45099144354073));
#52355=CARTESIAN_POINT('Ctrl Pts',(8.64584176151521,2.09714053636285,-7.22243788779773));
#52356=CARTESIAN_POINT('Ctrl Pts',(7.56815391157874,1.97195531073023,-7.75084487345448));
#52357=CARTESIAN_POINT('Ctrl Pts',(7.09293395924904,1.93789858980489,-7.93919586996905));
#52358=CARTESIAN_POINT('Ctrl Pts',(6.68079083609235,1.92043728607192,-8.08002239814288));
#52359=CARTESIAN_POINT('Ctrl Pts',(6.2887344545226,1.91141535836306,-8.19558998704663));
#52360=CARTESIAN_POINT('Ctrl Pts',(5.19190123252587,1.91538845500566,-8.4485082380012));
#52361=CARTESIAN_POINT('Ctrl Pts',(3.54842407610298,2.01867949236351,-8.54807461885338));
#52362=CARTESIAN_POINT('Ctrl Pts',(1.33100482704111,2.14842359650083,-8.598991326133));
#52363=CARTESIAN_POINT('Ctrl Pts',(-4.42970115563661E-15,2.14773017928896,
-8.66962570190719));
#52364=CARTESIAN_POINT('',(16.6867771002228,4.07882260827389,0.570992448038681));
#52365=CARTESIAN_POINT('Ctrl Pts',(16.6867770992602,4.0788226180366,0.570992448535458));
#52366=CARTESIAN_POINT('Ctrl Pts',(16.6866006155042,4.07881770793486,0.570746939936513));
#52367=CARTESIAN_POINT('Ctrl Pts',(16.6864241325273,4.07881279553261,0.570501437345728));
#52368=CARTESIAN_POINT('Ctrl Pts',(16.6862476503278,4.07880788082875,0.570255940758842));
#52369=CARTESIAN_POINT('Ctrl Pts',(16.6516203780579,4.07784357514131,0.522087472883436));
#52370=CARTESIAN_POINT('Ctrl Pts',(16.6169978550456,4.07676173618344,0.473723921485881));
#52371=CARTESIAN_POINT('Ctrl Pts',(16.5823724030183,4.07556338852267,0.425511095989113));
#52372=CARTESIAN_POINT('Ctrl Pts',(16.5692484174572,4.07510918225312,0.407237127314825));
#52373=CARTESIAN_POINT('Ctrl Pts',(16.5561240069721,4.07463825977875,0.388985341062362));
#52374=CARTESIAN_POINT('Ctrl Pts',(16.5429987376474,4.07415075972573,0.370776534107786));
#52375=CARTESIAN_POINT('Ctrl Pts',(16.4944642419689,4.07234808668097,0.303444181483954));
#52376=CARTESIAN_POINT('Ctrl Pts',(16.4459179975801,4.07031893631195,0.236703222909966));
#52377=CARTESIAN_POINT('Ctrl Pts',(16.3973395991362,4.0680420516515,0.170323522116401));
#52378=CARTESIAN_POINT('Ctrl Pts',(16.304432925526,4.06368748693193,0.0433716794553504));
#52379=CARTESIAN_POINT('Ctrl Pts',(16.2114090994963,4.05842679877864,-0.0822720722562958));
#52380=CARTESIAN_POINT('Ctrl Pts',(16.1181189016894,4.05213093153233,-0.206993715717981));
#52381=CARTESIAN_POINT('Ctrl Pts',(16.111845521893,4.05170756051037,-0.215380730181117));
#52382=CARTESIAN_POINT('Ctrl Pts',(16.1055709354821,4.05127950565539,-0.223763555358829));
#52383=CARTESIAN_POINT('Ctrl Pts',(16.0992950962031,4.05084672649476,-0.232142299942472));
#52384=CARTESIAN_POINT('Ctrl Pts',(16.0121664484622,4.04483837265388,-0.348465974416771));
#52385=CARTESIAN_POINT('Ctrl Pts',(15.9247963048648,4.03792023437012,-0.464003684927603));
#52386=CARTESIAN_POINT('Ctrl Pts',(15.8370636993764,4.0299759162962,-0.579152551411837));
#52387=CARTESIAN_POINT('Ctrl Pts',(15.7187187913346,4.01925960863978,-0.73448000281174));
#52388=CARTESIAN_POINT('Ctrl Pts',(15.5997216093824,4.00671090090665,-0.888472620810391));
#52389=CARTESIAN_POINT('Ctrl Pts',(15.4793949306149,3.992065579383,-1.04164356221155));
#52390=CARTESIAN_POINT('Ctrl Pts',(15.3596494685553,3.97749099949079,-1.19407463851209));
#52391=CARTESIAN_POINT('Ctrl Pts',(15.2385873144689,3.96084067042942,-1.34569398391442));
#52392=CARTESIAN_POINT('Ctrl Pts',(15.115550686801,3.94182264816488,-1.4969645929773));
#52393=CARTESIAN_POINT('Ctrl Pts',(15.0637667141605,3.93381829398767,-1.56063175640255));
#52394=CARTESIAN_POINT('Ctrl Pts',(15.0116332052113,3.9253940638159,-1.62423685097789));
#52395=CARTESIAN_POINT('Ctrl Pts',(14.9591024156658,3.9165262015244,-1.68781278599852));
#52396=CARTESIAN_POINT('Ctrl Pts',(14.9133737464421,3.908806623255,-1.7431563840731));
#52397=CARTESIAN_POINT('Ctrl Pts',(14.8673492403764,3.90075028178363,-1.79848155516262));
#52398=CARTESIAN_POINT('Ctrl Pts',(14.821108096381,3.89236131247767,-1.85368816089058));
#52399=CARTESIAN_POINT('Ctrl Pts',(14.7421989228348,3.87804577921783,-1.9478966353333));
#52400=CARTESIAN_POINT('Ctrl Pts',(14.6626580969073,3.8627588588919,-2.04175953296958));
#52401=CARTESIAN_POINT('Ctrl Pts',(14.5828955564093,3.84655993363014,-2.13478415056217));
#52402=CARTESIAN_POINT('Ctrl Pts',(14.5025695248271,3.83024656931088,-2.22846595061526));
#52403=CARTESIAN_POINT('Ctrl Pts',(14.422019141762,3.81300816310403,-2.32129716270607));
#52404=CARTESIAN_POINT('Ctrl Pts',(14.3416751210386,3.79495689677215,-2.41278157909349));
#52405=CARTESIAN_POINT('Ctrl Pts',(14.2674756527927,3.77828615573967,-2.49726944748248));
#52406=CARTESIAN_POINT('Ctrl Pts',(14.1934526773196,3.76092283109034,-2.58060847594324));
#52407=CARTESIAN_POINT('Ctrl Pts',(14.11994836497,3.74299347675259,-2.66241771614859));
#52408=CARTESIAN_POINT('Ctrl Pts',(14.091758713591,3.73611738700936,-2.69379239182739));
#52409=CARTESIAN_POINT('Ctrl Pts',(14.0636453423154,3.72915841731571,-2.7249421892367));
#52410=CARTESIAN_POINT('Ctrl Pts',(14.0356273648762,3.72212505706484,-2.75584609692576));
#52411=CARTESIAN_POINT('Ctrl Pts',(14.0158271275187,3.71715459826958,-2.77768581425887));
#52412=CARTESIAN_POINT('Ctrl Pts',(13.9960728675733,3.71214686676995,-2.79940253671174));
#52413=CARTESIAN_POINT('Ctrl Pts',(13.9763646379192,3.70710306984621,-2.82099787017943));
#52414=CARTESIAN_POINT('Ctrl Pts',(13.8574048089802,3.67665846727242,-2.95134834915652));
#52415=CARTESIAN_POINT('Ctrl Pts',(13.7401260229588,3.64490042631668,-3.07727439623639));
#52416=CARTESIAN_POINT('Ctrl Pts',(13.6244886164948,3.61215382052082,-3.19910641675052));
#52417=CARTESIAN_POINT('Ctrl Pts',(13.5036610600527,3.57793744987508,-3.32640661990492));
#52418=CARTESIAN_POINT('Ctrl Pts',(13.3846249977527,3.54264299708048,-3.44923749763812));
#52419=CARTESIAN_POINT('Ctrl Pts',(13.2672861145932,3.50662094584695,-3.56799588009648));
#52420=CARTESIAN_POINT('Ctrl Pts',(13.2291660948582,3.4949184200776,-3.60657705422325));
#52421=CARTESIAN_POINT('Ctrl Pts',(13.1912248612021,3.48313887990425,-3.64472853208236));
#52422=CARTESIAN_POINT('Ctrl Pts',(13.1534582886814,3.47129366217228,-3.68246420730061));
#52423=CARTESIAN_POINT('Ctrl Pts',(13.0350852174139,3.43416678755334,-3.8007404360869));
#52424=CARTESIAN_POINT('Ctrl Pts',(12.9183376887957,3.39636362404428,-3.91503983158288));
#52425=CARTESIAN_POINT('Ctrl Pts',(12.8032900468155,3.35831030135525,-4.02541934004456));
#52426=CARTESIAN_POINT('Ctrl Pts',(12.728600000419,3.33360571473129,-4.09707878882871));
#52427=CARTESIAN_POINT('Ctrl Pts',(12.6546256074055,3.30879546598555,-4.1670867890684));
#52428=CARTESIAN_POINT('Ctrl Pts',(12.5813792188602,3.28399106130667,-4.23546594227292));
#52429=CARTESIAN_POINT('Ctrl Pts',(12.4713187082152,3.24671979784344,-4.33821291271917));
#52430=CARTESIAN_POINT('Ctrl Pts',(12.3629026011617,3.20946416281579,-4.43728130970139));
#52431=CARTESIAN_POINT('Ctrl Pts',(12.2561598418245,3.17256125137376,-4.5327698916291));
#52432=CARTESIAN_POINT('Ctrl Pts',(12.149762552496,3.13577777519101,-4.62794942738419));
#52433=CARTESIAN_POINT('Ctrl Pts',(12.0450276505195,3.09934499196931,-4.71957257257733));
#52434=CARTESIAN_POINT('Ctrl Pts',(11.9419638342286,3.06355324889592,-4.80775726087006));
#52435=CARTESIAN_POINT('Ctrl Pts',(11.8377523564963,3.02736294884177,-4.89692392489513));
#52436=CARTESIAN_POINT('Ctrl Pts',(11.7352492971318,2.99182818284969,-4.98257537944035));
#52437=CARTESIAN_POINT('Ctrl Pts',(11.6344449097747,2.95720154072858,-5.06485012041152));
#52438=CARTESIAN_POINT('Ctrl Pts',(11.5323329411863,2.92212574010822,-5.1481920858352));
#52439=CARTESIAN_POINT('Ctrl Pts',(11.431963904345,2.88798175631234,-5.22806941702913));
#52440=CARTESIAN_POINT('Ctrl Pts',(11.3333099431412,2.85498269623455,-5.30463916990859));
#52441=CARTESIAN_POINT('Ctrl Pts',(11.2317900216267,2.82102499247617,-5.38343332280276));
#52442=CARTESIAN_POINT('Ctrl Pts',(11.1320861988524,2.78827966370978,-5.45872516267022));
#52443=CARTESIAN_POINT('Ctrl Pts',(11.0341506839636,2.75692715602264,-5.53069595057747));
#52444=CARTESIAN_POINT('Ctrl Pts',(10.9928851789487,2.74371665659696,-5.56102111824196));
#52445=CARTESIAN_POINT('Ctrl Pts',(10.9519334162765,2.73075282403085,-5.59075676961424));
#52446=CARTESIAN_POINT('Ctrl Pts',(10.9112909871464,2.71804658071908,-5.61991682939025));
#52447=CARTESIAN_POINT('Ctrl Pts',(10.8964872733027,2.71341842255918,-5.63053817240124));
#52448=CARTESIAN_POINT('Ctrl Pts',(10.8817245953344,2.70882442578679,-5.64108315195563));
#52449=CARTESIAN_POINT('Ctrl Pts',(10.867002428818,2.70426484961688,-5.65155246189065));
#52450=CARTESIAN_POINT('',(21.1401475865982,4.08070793355491,6.62997524452016));
#52451=CARTESIAN_POINT('Ctrl Pts',(21.1401277912671,4.08070389027384,6.62994920882078));
#52452=CARTESIAN_POINT('Ctrl Pts',(21.0563644921349,4.08064024620979,6.51979585635074));
#52453=CARTESIAN_POINT('Ctrl Pts',(20.9712950286701,4.08056610843344,6.40796762284914));
#52454=CARTESIAN_POINT('Ctrl Pts',(20.8846961507685,4.08048805817888,6.29405879478709));
#52455=CARTESIAN_POINT('Ctrl Pts',(20.8746571610368,4.08047901018978,6.28085389441233));
#52456=CARTESIAN_POINT('Ctrl Pts',(20.8645975893816,4.08046991265708,6.26762099621871));
#52457=CARTESIAN_POINT('Ctrl Pts',(20.8545170605049,4.08046077832543,6.25435943227145));
#52458=CARTESIAN_POINT('Ctrl Pts',(20.761284055216,4.08037629652872,6.1317056036129));
#52459=CARTESIAN_POINT('Ctrl Pts',(20.6662576987441,4.08028827813828,6.00659886428616));
#52460=CARTESIAN_POINT('Ctrl Pts',(20.5690642470972,4.08020917541913,5.87840956843418));
#52461=CARTESIAN_POINT('Ctrl Pts',(20.4326379910561,4.08009814234401,5.69847578275955));
#52462=CARTESIAN_POINT('Ctrl Pts',(20.2919440715206,4.08000319764964,5.51247161641301));
#52463=CARTESIAN_POINT('Ctrl Pts',(20.1459857511765,4.07997954828105,5.31870077800298));
#52464=CARTESIAN_POINT('Ctrl Pts',(20.1362693355262,4.0799779739474,5.30580149276543));
#52465=CARTESIAN_POINT('Ctrl Pts',(20.1265295797202,4.07997671576694,5.2928677727711));
#52466=CARTESIAN_POINT('Ctrl Pts',(20.1167661849073,4.07997579012312,5.2798991102106));
#52467=CARTESIAN_POINT('Ctrl Pts',(20.0785787432934,4.07997216966425,5.22917494573398));
#52468=CARTESIAN_POINT('Ctrl Pts',(20.0400297848654,4.07997378208828,5.17791638188733));
#52469=CARTESIAN_POINT('Ctrl Pts',(20.0011014776089,4.07998188596764,5.12609307809296));
#52470=CARTESIAN_POINT('Ctrl Pts',(19.9977449105617,4.07998258471918,5.12162464866327));
#52471=CARTESIAN_POINT('Ctrl Pts',(19.9943855153735,4.07998333231857,5.11715201016286));
#52472=CARTESIAN_POINT('Ctrl Pts',(19.9910232903037,4.0799841289361,5.11267515602838));
#52473=CARTESIAN_POINT('Ctrl Pts',(19.9642901914985,4.07999046285325,5.07707962585797));
#52474=CARTESIAN_POINT('Ctrl Pts',(19.9373781731281,4.07999989586757,5.04121756185854));
#52475=CARTESIAN_POINT('Ctrl Pts',(19.9102821059269,4.08001286913029,5.00507829021745));
#52476=CARTESIAN_POINT('Ctrl Pts',(19.8234646575681,4.08005443625358,4.88928586447036));
#52477=CARTESIAN_POINT('Ctrl Pts',(19.7347628514344,4.08013214834245,4.7706540119105));
#52478=CARTESIAN_POINT('Ctrl Pts',(19.6439993917317,4.08026028155559,4.64882337427558));
#52479=CARTESIAN_POINT('Ctrl Pts',(19.5975888619335,4.08032580054666,4.58652711037373));
#52480=CARTESIAN_POINT('Ctrl Pts',(19.5506396858042,4.08040449335367,4.52339509780919));
#52481=CARTESIAN_POINT('Ctrl Pts',(19.5031310854659,4.08049818336552,4.45938387691135));
#52482=CARTESIAN_POINT('Ctrl Pts',(19.4447501728308,4.08061331427568,4.38072372973177));
#52483=CARTESIAN_POINT('Ctrl Pts',(19.3856534202294,4.08074934835936,4.30091019527115));
#52484=CARTESIAN_POINT('Ctrl Pts',(19.3255293965389,4.080913099628,4.21949508424769));
#52485=CARTESIAN_POINT('Ctrl Pts',(19.2688772893524,4.0810673949305,4.14278136295625));
#52486=CARTESIAN_POINT('Ctrl Pts',(19.2113117835773,4.08124630895807,4.06464383760304));
#52487=CARTESIAN_POINT('Ctrl Pts',(19.153024043681,4.08144838923387,3.98535013860247));
#52488=CARTESIAN_POINT('Ctrl Pts',(19.1013031567088,4.08162770260444,3.91498988015165));
#52489=CARTESIAN_POINT('Ctrl Pts',(19.0489158781451,4.08182661596193,3.84358652788689));
#52490=CARTESIAN_POINT('Ctrl Pts',(18.9958265893946,4.08204565924289,3.77109062298675));
#52491=CARTESIAN_POINT('Ctrl Pts',(18.9587689592859,4.0821985568438,3.72048669719649));
#52492=CARTESIAN_POINT('Ctrl Pts',(18.9219798015889,4.08235871849574,3.67018402584651));
#52493=CARTESIAN_POINT('Ctrl Pts',(18.885449910933,4.0825252126899,3.62017431206734));
#52494=CARTESIAN_POINT('Ctrl Pts',(18.7893760662606,4.08296309347907,3.4886484468794));
#52495=CARTESIAN_POINT('Ctrl Pts',(18.6948839522869,4.08344449533075,3.35886253084306));
#52496=CARTESIAN_POINT('Ctrl Pts',(18.602321754467,4.08394799909736,3.23132511241665));
#52497=CARTESIAN_POINT('Ctrl Pts',(18.5589985833635,4.08418366095874,3.17163200301858));
#52498=CARTESIAN_POINT('Ctrl Pts',(18.5160990740038,4.08442424751788,3.11243192432935));
#52499=CARTESIAN_POINT('Ctrl Pts',(18.4734425356514,4.08466551982131,3.05348729325027));
#52500=CARTESIAN_POINT('Ctrl Pts',(18.3914292931626,4.08512940003032,2.9401578832974));
#52501=CARTESIAN_POINT('Ctrl Pts',(18.3106734624825,4.0855993150209,2.82826791101076));
#52502=CARTESIAN_POINT('Ctrl Pts',(18.2310417730918,4.08604651058148,2.71772553516501));
#52503=CARTESIAN_POINT('Ctrl Pts',(18.1756290479738,4.08635769730703,2.64080321525077));
#52504=CARTESIAN_POINT('Ctrl Pts',(18.1207596302947,4.08665785079446,2.56453223458843));
#52505=CARTESIAN_POINT('Ctrl Pts',(18.066379339977,4.08693723904721,2.4888705876708));
#52506=CARTESIAN_POINT('Ctrl Pts',(18.0192713524714,4.08717926457232,2.42332720978834));
#52507=CARTESIAN_POINT('Ctrl Pts',(17.9725602422526,4.08740424180746,2.35828267344141));
#52508=CARTESIAN_POINT('Ctrl Pts',(17.9261657622048,4.08760622745652,2.2936473939049));
#52509=CARTESIAN_POINT('Ctrl Pts',(17.8410139049816,4.08797694942886,2.17501659797828));
#52510=CARTESIAN_POINT('Ctrl Pts',(17.7569288166908,4.08827013511229,2.05776474700644));
#52511=CARTESIAN_POINT('Ctrl Pts',(17.6738446859609,4.08842721492592,1.94189413170338));
#52512=CARTESIAN_POINT('Ctrl Pts',(17.564867849343,4.08863324778726,1.78991308548242));
#52513=CARTESIAN_POINT('Ctrl Pts',(17.4575265240186,4.08860949102722,1.64018729925338));
#52514=CARTESIAN_POINT('Ctrl Pts',(17.3514015519163,4.08820812095149,1.49234200613465));
#52515=CARTESIAN_POINT('Ctrl Pts',(17.3352343295005,4.08814697568891,1.46981905334015));
#52516=CARTESIAN_POINT('Ctrl Pts',(17.3190953908043,4.08807705423024,1.44733982362486));
#52517=CARTESIAN_POINT('Ctrl Pts',(17.3029833106586,4.08799781807257,1.4249030794789));
#52518=CARTESIAN_POINT('Ctrl Pts',(17.2996967352419,4.08798165531732,1.42032638602437));
#52519=CARTESIAN_POINT('Ctrl Pts',(17.2964112608272,4.08796510254446,1.4157514373454));
#52520=CARTESIAN_POINT('Ctrl Pts',(17.2931268880962,4.08794815631246,1.41117824074195));
#52521=CARTESIAN_POINT('Ctrl Pts',(17.2201023048574,4.08757137461583,1.30949801033402));
#52522=CARTESIAN_POINT('Ctrl Pts',(17.1476227548266,4.08700004957664,1.20868450230697));
#52523=CARTESIAN_POINT('Ctrl Pts',(17.0755476342745,4.08617659776486,1.10861146158045));
#52524=CARTESIAN_POINT('Ctrl Pts',(16.9597498463747,4.08485361838562,0.947831477366912));
#52525=CARTESIAN_POINT('Ctrl Pts',(16.8449967071095,4.08288234496673,0.788964410925807));
#52526=CARTESIAN_POINT('Ctrl Pts',(16.7307073558031,4.07998384329684,0.63148608409984));
#52527=CARTESIAN_POINT('Ctrl Pts',(16.7159333272004,4.07960915793826,0.611129075522529));
#52528=CARTESIAN_POINT('Ctrl Pts',(16.7011671087498,4.07921864284779,0.590795559364228));
#52529=CARTESIAN_POINT('Ctrl Pts',(16.6867771007016,4.0788225980919,0.570992447894296));
#52530=CARTESIAN_POINT('',(25.4568055127483,4.08055401005754,12.6479974296003));
#52531=CARTESIAN_POINT('Ctrl Pts',(25.4568055127483,4.08055401005754,12.6479974296003));
#52532=CARTESIAN_POINT('Ctrl Pts',(25.2812500090543,4.0807927703833,12.3850689542157));
#52533=CARTESIAN_POINT('Ctrl Pts',(25.0429611356646,4.08107710014979,12.0284743263647));
#52534=CARTESIAN_POINT('Ctrl Pts',(24.5376155259781,4.08153855678031,11.2800885455859));
#52535=CARTESIAN_POINT('Ctrl Pts',(23.7755577618618,4.08195087821486,10.1719836389024));
#52536=CARTESIAN_POINT('Ctrl Pts',(22.5853601008239,4.08176221127767,8.52809651334861));
#52537=CARTESIAN_POINT('Ctrl Pts',(21.7185595769906,4.08113204177903,7.3898603299135));
#52538=CARTESIAN_POINT('Ctrl Pts',(21.1401574799756,4.0807159798154,6.62998826233519));
#52539=CARTESIAN_POINT('',(30.3134449388696,4.07585023121522,18.6659931355559));
#52540=CARTESIAN_POINT('Ctrl Pts',(30.3134449229822,4.07585757700923,18.6659931355313));
#52541=CARTESIAN_POINT('Ctrl Pts',(28.1961718099026,4.07126384474955,16.7705691222953));
#52542=CARTESIAN_POINT('Ctrl Pts',(26.9909999267723,4.07846746334965,14.9457506743408));
#52543=CARTESIAN_POINT('Ctrl Pts',(25.4568055127483,4.08055401005754,12.6479974296003));
#52544=CARTESIAN_POINT('',(43.9982567711944,4.57019451624003,24.6840336607938));
#52545=CARTESIAN_POINT('Ctrl Pts',(43.9982567712356,4.57019451569775,24.6840336607913));
#52546=CARTESIAN_POINT('Ctrl Pts',(43.6563954192405,4.54439404820984,24.6501193006367));
#52547=CARTESIAN_POINT('Ctrl Pts',(43.307245667739,4.51904928549701,24.6083964604157));
#52548=CARTESIAN_POINT('Ctrl Pts',(42.9531363255538,4.49443707659921,24.5592450950212));
#52549=CARTESIAN_POINT('Ctrl Pts',(42.6880707668603,4.4760138154056,24.5224532553921));
#52550=CARTESIAN_POINT('Ctrl Pts',(42.4202264763677,4.45800003649193,24.4814991107356));
#52551=CARTESIAN_POINT('Ctrl Pts',(42.1505826287051,4.44049282217423,24.4365424344902));
#52552=CARTESIAN_POINT('Ctrl Pts',(41.9700544718839,4.42877163825239,24.4064436728469));
#52553=CARTESIAN_POINT('Ctrl Pts',(41.7887197355172,4.41727717030993,24.3745508395979));
#52554=CARTESIAN_POINT('Ctrl Pts',(41.6068694434254,4.40603746857656,24.3409115700462));
#52555=CARTESIAN_POINT('Ctrl Pts',(41.1987030733588,4.38080974854174,24.2654076025424));
#52556=CARTESIAN_POINT('Ctrl Pts',(40.7879492108107,4.3568639312022,24.1811059500155));
#52557=CARTESIAN_POINT('Ctrl Pts',(40.3744467654769,4.33428844255932,24.0823265719964));
#52558=CARTESIAN_POINT('Ctrl Pts',(40.0624031037516,4.31725217537188,24.0077841378032));
#52559=CARTESIAN_POINT('Ctrl Pts',(39.7487808519831,4.3010002904592,23.9249989010293));
#52560=CARTESIAN_POINT('Ctrl Pts',(39.4359132798453,4.2856784881585,23.8348004629979));
#52561=CARTESIAN_POINT('Ctrl Pts',(39.413276747975,4.28456992818944,23.8282744436882));
#52562=CARTESIAN_POINT('Ctrl Pts',(39.3906441679139,4.28346621432707,23.8217096183546));
#52563=CARTESIAN_POINT('Ctrl Pts',(39.3680164239544,4.28236739107164,23.815106301441));
#52564=CARTESIAN_POINT('Ctrl Pts',(39.0567379154496,4.26725143144832,23.7242677872822));
#52565=CARTESIAN_POINT('Ctrl Pts',(38.7463740872753,4.25306528550943,23.6261449516955));
#52566=CARTESIAN_POINT('Ctrl Pts',(38.4392040695246,4.23988360976955,23.5215568239253));
#52567=CARTESIAN_POINT('Ctrl Pts',(38.2841859690802,4.23323127322697,23.4687748075857));
#52568=CARTESIAN_POINT('Ctrl Pts',(38.1299813891894,4.22683393748975,23.4143461882941));
#52569=CARTESIAN_POINT('Ctrl Pts',(37.9768840192784,4.22069622128782,23.358376409543));
#52570=CARTESIAN_POINT('Ctrl Pts',(37.8169834657751,4.21428576356078,23.2999195032816));
#52571=CARTESIAN_POINT('Ctrl Pts',(37.6582906920349,4.20815851721116,23.2397814235049));
#52572=CARTESIAN_POINT('Ctrl Pts',(37.501140466546,4.20231456368994,23.1780824960211));
#52573=CARTESIAN_POINT('Ctrl Pts',(37.2372789042477,4.19250233019609,23.0744875100938));
#52574=CARTESIAN_POINT('Ctrl Pts',(36.9777656061434,4.18349013246665,22.9664921446601));
#52575=CARTESIAN_POINT('Ctrl Pts',(36.7241912711045,4.17525629897779,22.8546669878381));
#52576=CARTESIAN_POINT('Ctrl Pts',(36.6777761731309,4.17374915044075,22.8341981355427));
#52577=CARTESIAN_POINT('Ctrl Pts',(36.631560268027,4.1722680138333,22.8136008994392));
#52578=CARTESIAN_POINT('Ctrl Pts',(36.5855442937473,4.17081238439013,22.7928811810314));
#52579=CARTESIAN_POINT('Ctrl Pts',(36.1877852789154,4.15823002049714,22.6137813160287));
#52580=CARTESIAN_POINT('Ctrl Pts',(35.8049617339917,4.14754953335667,22.4255293822829));
#52581=CARTESIAN_POINT('Ctrl Pts',(35.4375616951524,4.13840101146235,22.2319430741017));
#52582=CARTESIAN_POINT('Ctrl Pts',(35.0903110062494,4.1297542226915,22.0489736354198));
#52583=CARTESIAN_POINT('Ctrl Pts',(34.7568397309836,4.12247648315498,21.8612392508755));
#52584=CARTESIAN_POINT('Ctrl Pts',(34.4375796112242,4.11629332984187,21.6719653816336));
#52585=CARTESIAN_POINT('Ctrl Pts',(34.2188688560817,4.11205752948168,21.5423023629583));
#52586=CARTESIAN_POINT('Ctrl Pts',(34.006827791327,4.1083361809388,21.4119169089772));
#52587=CARTESIAN_POINT('Ctrl Pts',(33.8015966607754,4.10505052539575,21.2818452639727));
#52588=CARTESIAN_POINT('Ctrl Pts',(33.5101520730079,4.10038463225022,21.0971331452181));
#52589=CARTESIAN_POINT('Ctrl Pts',(33.2324412026286,4.09659432928849,20.9130543381718));
#52590=CARTESIAN_POINT('Ctrl Pts',(32.9688572095313,4.0934483100564,20.732570880017));
#52591=CARTESIAN_POINT('Ctrl Pts',(32.9185685258695,4.09284808709105,20.6981367877694));
#52592=CARTESIAN_POINT('Ctrl Pts',(32.868794031995,4.09227146343527,20.6638335403719));
#52593=CARTESIAN_POINT('Ctrl Pts',(32.8195364096049,4.09171703638411,20.6296816684234));
#52594=CARTESIAN_POINT('Ctrl Pts',(32.5448903765516,4.08862571400945,20.4392608625282));
#52595=CARTESIAN_POINT('Ctrl Pts',(32.2863121035037,4.08622000587309,20.253550189542));
#52596=CARTESIAN_POINT('Ctrl Pts',(32.0443288798291,4.08429089599327,20.0741560370317));
#52597=CARTESIAN_POINT('Ctrl Pts',(31.8158602799689,4.0824695257903,19.9047809447226));
#52598=CARTESIAN_POINT('Ctrl Pts',(31.6021849429662,4.08107388003582,19.7410364759486));
#52599=CARTESIAN_POINT('Ctrl Pts',(31.4037380340014,4.07996894633293,19.5842664599639));
#52600=CARTESIAN_POINT('Ctrl Pts',(31.2690106400237,4.07921879688951,19.4778338840288));
#52601=CARTESIAN_POINT('Ctrl Pts',(31.1413043559806,4.0786025832564,19.3746189789883));
#52602=CARTESIAN_POINT('Ctrl Pts',(31.0185339853794,4.0780801427807,19.2732361504699));
#52603=CARTESIAN_POINT('Ctrl Pts',(30.8391071505753,4.07731660479943,19.1250668492333));
#52604=CARTESIAN_POINT('Ctrl Pts',(30.6702229751989,4.07675152626773,18.9808100222224));
#52605=CARTESIAN_POINT('Ctrl Pts',(30.5053789318961,4.07630814667192,18.8361514122018));
#52606=CARTESIAN_POINT('Ctrl Pts',(30.4409125747783,4.07613475206942,18.7795790700843));
#52607=CARTESIAN_POINT('Ctrl Pts',(30.3770641474424,4.07598054873336,18.7229454371387));
#52608=CARTESIAN_POINT('Ctrl Pts',(30.3134449547349,4.07584288616601,18.6659931355875));
#52609=CARTESIAN_POINT('',(48.9436857109461,5.01442544687573,24.6839747938942));
#52610=CARTESIAN_POINT('Ctrl Pts',(48.9436857109461,5.01442544687573,24.6839747938942));
#52611=CARTESIAN_POINT('Ctrl Pts',(48.562059296251,4.9745603086499,24.7263748666625));
#52612=CARTESIAN_POINT('Ctrl Pts',(48.1741509009344,4.93536251604839,24.7583003138797));
#52613=CARTESIAN_POINT('Ctrl Pts',(47.4017479491975,4.85999473704396,24.8018982028682));
#52614=CARTESIAN_POINT('Ctrl Pts',(47.0216137408318,4.82422047595138,24.8130651984859));
#52615=CARTESIAN_POINT('Ctrl Pts',(45.7588804631496,4.70971082580307,24.8171749588499));
#52616=CARTESIAN_POINT('Ctrl Pts',(44.8709429698041,4.63605663134738,24.7706071307739));
#52617=CARTESIAN_POINT('Ctrl Pts',(43.9982567712502,4.57019451569886,24.6840336607964));
#52618=CARTESIAN_POINT('',(60.9536795918051,6.58767285120455,18.6650422826153));
#52619=CARTESIAN_POINT('Ctrl Pts',(60.9536837037562,6.58764335981454,18.6650422970777));
#52620=CARTESIAN_POINT('Ctrl Pts',(60.8748932120277,6.57672320333976,18.8030200801626));
#52621=CARTESIAN_POINT('Ctrl Pts',(60.7989278472826,6.56617190512782,18.9327111752887));
#52622=CARTESIAN_POINT('Ctrl Pts',(60.7243765115728,6.5557970610253,19.0561356442329));
#52623=CARTESIAN_POINT('Ctrl Pts',(60.6409508535265,6.54418723286943,19.194252117166));
#52624=CARTESIAN_POINT('Ctrl Pts',(60.5592962133145,6.53279847920326,19.3245213816899));
#52625=CARTESIAN_POINT('Ctrl Pts',(60.4775049273693,6.52136765023818,19.449789902365));
#52626=CARTESIAN_POINT('Ctrl Pts',(60.395713641424,6.5099368212731,19.57505842304));
#52627=CARTESIAN_POINT('Ctrl Pts',(60.313786862902,6.49846407086503,19.6953265126474));
#52628=CARTESIAN_POINT('Ctrl Pts',(60.2298692144609,6.48669009469553,19.8134515963786));
#52629=CARTESIAN_POINT('Ctrl Pts',(60.0741012759495,6.46483524020335,20.0327153760616));
#52630=CARTESIAN_POINT('Ctrl Pts',(59.9113909123673,6.44192971076875,20.2445747818266));
#52631=CARTESIAN_POINT('Ctrl Pts',(59.7396908055897,6.41768204830029,20.4483176667295));
#52632=CARTESIAN_POINT('Ctrl Pts',(59.5728651506258,6.3941227608394,20.646276426663));
#52633=CARTESIAN_POINT('Ctrl Pts',(59.3975528519521,6.36929636809518,20.836573053325));
#52634=CARTESIAN_POINT('Ctrl Pts',(59.2119236140565,6.34294486051316,21.0185603920136));
#52635=CARTESIAN_POINT('Ctrl Pts',(59.100465832935,6.32712256550406,21.1278314593971));
#52636=CARTESIAN_POINT('Ctrl Pts',(58.9852895190672,6.31075062049767,21.2341069843407));
#52637=CARTESIAN_POINT('Ctrl Pts',(58.8660073159028,6.29377513369926,21.3372477590069));
#52638=CARTESIAN_POINT('Ctrl Pts',(58.7509346282163,6.27739871845157,21.4367486555033));
#52639=CARTESIAN_POINT('Ctrl Pts',(58.6320408505898,6.26046044518029,21.5333321072928));
#52640=CARTESIAN_POINT('Ctrl Pts',(58.508979876986,6.24292110566031,21.626876022722));
#52641=CARTESIAN_POINT('Ctrl Pts',(58.4887780107034,6.24004182247823,21.6422323263145));
#52642=CARTESIAN_POINT('Ctrl Pts',(58.4684635545249,6.23714630659417,21.6575066607819));
#52643=CARTESIAN_POINT('Ctrl Pts',(58.4480394154578,6.23423502388466,21.672698581597));
#52644=CARTESIAN_POINT('Ctrl Pts',(58.2005563901708,6.19895847929953,21.8567818622138));
#52645=CARTESIAN_POINT('Ctrl Pts',(57.9369665378702,6.16136281992631,22.0287628026985));
#52646=CARTESIAN_POINT('Ctrl Pts',(57.6624596166534,6.12230615533265,22.1878640684998));
#52647=CARTESIAN_POINT('Ctrl Pts',(57.5773728776958,6.11020006995563,22.2371794293332));
#52648=CARTESIAN_POINT('Ctrl Pts',(57.4912374652112,6.0979539425225,22.2852575101044));
#52649=CARTESIAN_POINT('Ctrl Pts',(57.4042083778879,6.0855940225361,22.3320755299395));
#52650=CARTESIAN_POINT('Ctrl Pts',(57.2087214193683,6.05783085461144,22.4372393617452));
#52651=CARTESIAN_POINT('Ctrl Pts',(57.008734261632,6.02949259342333,22.536044413206));
#52652=CARTESIAN_POINT('Ctrl Pts',(56.7999697583721,6.00003337925011,22.6310713355561));
#52653=CARTESIAN_POINT('Ctrl Pts',(56.6080942544555,5.97295740859317,22.7184106021788));
#52654=CARTESIAN_POINT('Ctrl Pts',(56.4088045308582,5.94493368525431,22.8025582988609));
#52655=CARTESIAN_POINT('Ctrl Pts',(56.1988074787868,5.91557352121889,22.8855191124983));
#52656=CARTESIAN_POINT('Ctrl Pts',(56.1803234096789,5.91298922160278,22.892821374113));
#52657=CARTESIAN_POINT('Ctrl Pts',(56.161756401499,5.91039459699341,22.9001144410366));
#52658=CARTESIAN_POINT('Ctrl Pts',(56.1431042186586,5.9077894003739,22.9073996808841));
#52659=CARTESIAN_POINT('Ctrl Pts',(56.1156742180694,5.9039581841876,22.918113393859));
#52660=CARTESIAN_POINT('Ctrl Pts',(56.0880595906354,5.90010405620253,22.9288101736885));
#52661=CARTESIAN_POINT('Ctrl Pts',(56.0604141437415,5.89624864805948,22.9394423898106));
#52662=CARTESIAN_POINT('Ctrl Pts',(55.9718745527707,5.88390099959056,22.9734940030897));
#52663=CARTESIAN_POINT('Ctrl Pts',(55.883019639351,5.87154145844787,23.0068833672292));
#52664=CARTESIAN_POINT('Ctrl Pts',(55.7988925218622,5.85986943633177,23.0380458796224));
#52665=CARTESIAN_POINT('Ctrl Pts',(55.7294946088525,5.85024098358503,23.0637523746121));
#52666=CARTESIAN_POINT('Ctrl Pts',(55.6633188405804,5.84107739387149,23.087943519035));
#52667=CARTESIAN_POINT('Ctrl Pts',(55.586943735967,5.8305287518237,23.1150152712605));
#52668=CARTESIAN_POINT('Ctrl Pts',(55.5418250424742,5.82429712766124,23.1310079444903));
#52669=CARTESIAN_POINT('Ctrl Pts',(55.4931472946897,5.81758269461732,23.1480059080949));
#52670=CARTESIAN_POINT('Ctrl Pts',(55.4381475647196,5.81001182026829,23.166915463685));
#52671=CARTESIAN_POINT('Ctrl Pts',(55.42725455157,5.80851236501854,23.1706606100304));
#52672=CARTESIAN_POINT('Ctrl Pts',(55.4161134782451,5.80697932863549,23.1744807518226));
#52673=CARTESIAN_POINT('Ctrl Pts',(55.4047258589144,5.80541300399653,23.1783744667056));
#52674=CARTESIAN_POINT('Ctrl Pts',(55.2889072779726,5.78948258941978,23.2179757669642));
#52675=CARTESIAN_POINT('Ctrl Pts',(55.1475857888739,5.77010467587343,23.2651873818611));
#52676=CARTESIAN_POINT('Ctrl Pts',(54.9823558303551,5.74761445563296,23.318513632426));
#52677=CARTESIAN_POINT('Ctrl Pts',(54.8248950225142,5.7261817307244,23.3693324704161));
#52678=CARTESIAN_POINT('Ctrl Pts',(54.6457219044543,5.70192243219709,23.4257044042999));
#52679=CARTESIAN_POINT('Ctrl Pts',(54.4462107368371,5.67517291439529,23.4863366809526));
#52680=CARTESIAN_POINT('Ctrl Pts',(54.3159317007704,5.65770571475885,23.5259290238333));
#52681=CARTESIAN_POINT('Ctrl Pts',(54.1769804185357,5.63917762942309,23.5673380043009));
#52682=CARTESIAN_POINT('Ctrl Pts',(54.0297364015009,5.61969401951032,23.610204179057));
#52683=CARTESIAN_POINT('Ctrl Pts',(53.7970966485848,5.58891068252112,23.6779310484032));
#52684=CARTESIAN_POINT('Ctrl Pts',(53.543745884538,5.55574006612116,23.7492900999149));
#52685=CARTESIAN_POINT('Ctrl Pts',(53.2732679872795,5.52091196649709,23.8221539563539));
#52686=CARTESIAN_POINT('Ctrl Pts',(52.9749987252396,5.48250531043235,23.9025045096144));
#52687=CARTESIAN_POINT('Ctrl Pts',(52.6559018189042,5.44208830841857,23.9846854993892));
#52688=CARTESIAN_POINT('Ctrl Pts',(52.3207576286579,5.40057964484992,24.0658311066893));
#52689=CARTESIAN_POINT('Ctrl Pts',(52.1333765429832,5.37737190719322,24.1112000924457));
#52690=CARTESIAN_POINT('Ctrl Pts',(51.9409784566618,5.35382241515805,24.1562453376084));
#52691=CARTESIAN_POINT('Ctrl Pts',(51.7443946064197,5.33008577804881,24.2004655968722));
#52692=CARTESIAN_POINT('Ctrl Pts',(51.3432051841192,5.28164391612837,24.2907105495789));
#52693=CARTESIAN_POINT('Ctrl Pts',(50.9246090760015,5.23242789976439,24.3775258737374));
#52694=CARTESIAN_POINT('Ctrl Pts',(50.4929870595525,5.1833823052378,24.4556071075138));
#52695=CARTESIAN_POINT('Ctrl Pts',(50.1455722059097,5.14390524569282,24.5184551073167));
#52696=CARTESIAN_POINT('Ctrl Pts',(49.7897170355193,5.10453958577619,24.5756445440186));
#52697=CARTESIAN_POINT('Ctrl Pts',(49.427729627481,5.06568535151103,24.624411660777));
#52698=CARTESIAN_POINT('Ctrl Pts',(49.2675194938438,5.04848905703845,24.645995246613));
#52699=CARTESIAN_POINT('Ctrl Pts',(49.1061080943944,5.03139228669694,24.6659290919299));
#52700=CARTESIAN_POINT('Ctrl Pts',(48.9436951551741,5.01442643343101,24.6839737446064));
#52701=CARTESIAN_POINT('Ctrl Pts',(48.9436920070984,5.01442610457919,24.6839740943688));
#52702=CARTESIAN_POINT('Ctrl Pts',(48.9436888590223,5.01442577572742,24.6839744441305));
#52703=CARTESIAN_POINT('Ctrl Pts',(48.9436857109458,5.01442544687569,24.6839747938914));
#52704=CARTESIAN_POINT('',(63.880064779209,6.9882076388047,12.6528714883835));
#52705=CARTESIAN_POINT('Ctrl Pts',(63.880064779209,6.9882076388047,12.6528714883835));
#52706=CARTESIAN_POINT('Ctrl Pts',(63.7740445264651,6.97254843494423,12.8870707048835));
#52707=CARTESIAN_POINT('Ctrl Pts',(63.6123361644209,6.94905832898685,13.2403034399106));
#52708=CARTESIAN_POINT('Ctrl Pts',(63.2900524331968,6.90311702623842,13.9391278664585));
#52709=CARTESIAN_POINT('Ctrl Pts',(62.4853443970193,6.79282876561949,15.6488004126113));
#52710=CARTESIAN_POINT('Ctrl Pts',(61.5478879227764,6.66996297123436,17.6228958620238));
#52711=CARTESIAN_POINT('Ctrl Pts',(60.9536795918051,6.58767285120455,18.6650422826153));
#52712=CARTESIAN_POINT('',(66.3006594538148,7.32609989629238,6.62697998093854));
#52713=CARTESIAN_POINT('Ctrl Pts',(66.300659446523,7.32609992703372,6.62697998211673));
#52714=CARTESIAN_POINT('Ctrl Pts',(66.2961516437242,7.32560197128319,6.63876773876303));
#52715=CARTESIAN_POINT('Ctrl Pts',(66.2911264841868,7.32504638436974,6.65192702458933));
#52716=CARTESIAN_POINT('Ctrl Pts',(66.2861021175671,7.32449011260781,6.66510631411833));
#52717=CARTESIAN_POINT('Ctrl Pts',(66.2265869187196,7.31790089907496,6.8212191331768));
#52718=CARTESIAN_POINT('Ctrl Pts',(66.1665664874988,7.31115403387545,6.98156417267042));
#52719=CARTESIAN_POINT('Ctrl Pts',(66.1052920653522,7.30410522937434,7.14672695293512));
#52720=CARTESIAN_POINT('Ctrl Pts',(66.0780532869344,7.30097177144541,7.22014800232068));
#52721=CARTESIAN_POINT('Ctrl Pts',(66.0505665836933,7.29777863650945,7.29452052682466));
#52722=CARTESIAN_POINT('Ctrl Pts',(66.0227663772338,7.29451325221887,7.36989242818266));
#52723=CARTESIAN_POINT('Ctrl Pts',(65.9666413110708,7.28792085839536,7.52205867042603));
#52724=CARTESIAN_POINT('Ctrl Pts',(65.909236835321,7.28103353146028,7.6783020694003));
#52725=CARTESIAN_POINT('Ctrl Pts',(65.8500061686631,7.27374086686791,7.83903564120958));
#52726=CARTESIAN_POINT('Ctrl Pts',(65.8311638865591,7.27142094627116,7.89016772319501));
#52727=CARTESIAN_POINT('Ctrl Pts',(65.8121369439297,7.26906003851291,7.94175385688256));
#52728=CARTESIAN_POINT('Ctrl Pts',(65.7929082290069,7.2666546952333,7.99380629067399));
#52729=CARTESIAN_POINT('Ctrl Pts',(65.7752908491144,7.26445091580764,8.04149681518978));
#52730=CARTESIAN_POINT('Ctrl Pts',(65.7575039285222,7.2622097550886,8.08957923853654));
#52731=CARTESIAN_POINT('Ctrl Pts',(65.7395342230684,7.25992847772148,8.13806342420129));
#52732=CARTESIAN_POINT('Ctrl Pts',(65.6805357302456,7.25243854269072,8.29724766276983));
#52733=CARTESIAN_POINT('Ctrl Pts',(65.6195662658539,7.24451574763741,8.46076214982886));
#52734=CARTESIAN_POINT('Ctrl Pts',(65.5561656976303,7.2360675884905,8.62895040123494));
#52735=CARTESIAN_POINT('Ctrl Pts',(65.5431387561496,7.2343317416691,8.66350811215447));
#52736=CARTESIAN_POINT('Ctrl Pts',(65.5300092729086,7.23257373433867,8.69826299491312));
#52737=CARTESIAN_POINT('Ctrl Pts',(65.5167734110897,7.23079279556236,8.73321779621613));
#52738=CARTESIAN_POINT('Ctrl Pts',(65.4837676855844,7.22635174161383,8.82038314991143));
#52739=CARTESIAN_POINT('Ctrl Pts',(65.4501686905856,7.2217789113791,8.90861216197532));
#52740=CARTESIAN_POINT('Ctrl Pts',(65.4157860386741,7.21704230591978,8.99829403032095));
#52741=CARTESIAN_POINT('Ctrl Pts',(65.3746164943489,7.21137072802897,9.10567846545784));
#52742=CARTESIAN_POINT('Ctrl Pts',(65.3323234237302,7.20546441961582,9.21514745632922));
#52743=CARTESIAN_POINT('Ctrl Pts',(65.2890065927822,7.19933679696803,9.32633307246552));
#52744=CARTESIAN_POINT('Ctrl Pts',(65.2609113571545,7.19536242953717,9.39844790670901));
#52745=CARTESIAN_POINT('Ctrl Pts',(65.2323499986339,7.19128946807759,9.47137580262029));
#52746=CARTESIAN_POINT('Ctrl Pts',(65.2032963048797,7.18711403038382,9.54513708528809));
#52747=CARTESIAN_POINT('Ctrl Pts',(65.1896601075941,7.18515431081674,9.57975655264426));
#52748=CARTESIAN_POINT('Ctrl Pts',(65.1760188101892,7.18318688194893,9.614296963272));
#52749=CARTESIAN_POINT('Ctrl Pts',(65.1623711062258,7.18121190329217,9.64875990838282));
#52750=CARTESIAN_POINT('Ctrl Pts',(65.1239051352521,7.17564543790808,9.74589351047838));
#52751=CARTESIAN_POINT('Ctrl Pts',(65.0853174690523,7.1700104476921,9.84259099567689));
#52752=CARTESIAN_POINT('Ctrl Pts',(65.0467091952298,7.16432647860304,9.93853650237319));
#52753=CARTESIAN_POINT('Ctrl Pts',(65.0032832899394,7.157933250445,10.0464543156895));
#52754=CARTESIAN_POINT('Ctrl Pts',(64.9598301710589,7.15147790800914,10.1534246055419));
#52755=CARTESIAN_POINT('Ctrl Pts',(64.9161906946988,7.14495370650557,10.259929264202));
#52756=CARTESIAN_POINT('Ctrl Pts',(64.9110320486335,7.14418247712284,10.2725192374135));
#52757=CARTESIAN_POINT('Ctrl Pts',(64.9058719259585,7.14341042276849,10.2850999251361));
#52758=CARTESIAN_POINT('Ctrl Pts',(64.9007103369394,7.14263756622216,10.2976714500119));
#52759=CARTESIAN_POINT('Ctrl Pts',(64.8220237704832,7.13085564639699,10.4893198210735));
#52760=CARTESIAN_POINT('Ctrl Pts',(64.7429951170709,7.11888689900363,10.6788439805008));
#52761=CARTESIAN_POINT('Ctrl Pts',(64.6636556105198,7.10681277214228,10.8666766704469));
#52762=CARTESIAN_POINT('Ctrl Pts',(64.6542323662028,7.10537871422744,10.8889857747636));
#52763=CARTESIAN_POINT('Ctrl Pts',(64.6448047349602,7.10394316921425,10.9112709982386));
#52764=CARTESIAN_POINT('Ctrl Pts',(64.635372092164,7.10250614545892,10.9335340503097));
#52765=CARTESIAN_POINT('Ctrl Pts',(64.6040882617547,7.09774018448415,11.0073705731617));
#52766=CARTESIAN_POINT('Ctrl Pts',(64.5727530941267,7.0929587717943,11.0809541181071));
#52767=CARTESIAN_POINT('Ctrl Pts',(64.5413598033906,7.08816550566459,11.154309716269));
#52768=CARTESIAN_POINT('Ctrl Pts',(64.5177330860973,7.08455807423252,11.2095174354665));
#52769=CARTESIAN_POINT('Ctrl Pts',(64.4940763830003,7.08094447718144,11.2645891973131));
#52770=CARTESIAN_POINT('Ctrl Pts',(64.470382570531,7.07732545714221,11.3195459712094));
#52771=CARTESIAN_POINT('Ctrl Pts',(64.4035641046536,7.06711952817599,11.4745285146928));
#52772=CARTESIAN_POINT('Ctrl Pts',(64.3364505075205,7.05687048265302,11.6285966092296));
#52773=CARTESIAN_POINT('Ctrl Pts',(64.2690337523511,7.04661896634741,11.7819573743463));
#52774=CARTESIAN_POINT('Ctrl Pts',(64.2510791342558,7.04388875395878,11.822800840656));
#52775=CARTESIAN_POINT('Ctrl Pts',(64.2331023996129,7.04115822385004,11.8635955499663));
#52776=CARTESIAN_POINT('Ctrl Pts',(64.2151029610433,7.03842800906183,11.9043463944726));
#52777=CARTESIAN_POINT('Ctrl Pts',(64.1803315818,7.03315377045434,11.9830690203668));
#52778=CARTESIAN_POINT('Ctrl Pts',(64.1454755177022,7.02788073298689,12.0616278828523));
#52779=CARTESIAN_POINT('Ctrl Pts',(64.1105266707577,7.02261257245995,12.1400667643143));
#52780=CARTESIAN_POINT('Ctrl Pts',(64.0341919105036,7.01110593330125,12.3113918217761));
#52781=CARTESIAN_POINT('Ctrl Pts',(63.9574150642832,6.99962279118902,12.482143738577));
#52782=CARTESIAN_POINT('Ctrl Pts',(63.8801064158733,6.98820114899864,12.6527834466791));
#52783=CARTESIAN_POINT('',(71.7123823850219,8.64377894688336,1.033152900074));
#52784=CARTESIAN_POINT('Ctrl Pts',(71.7123823116865,8.64377889138672,1.0331528409219));
#52785=CARTESIAN_POINT('Ctrl Pts',(71.7085363523106,8.64137100788826,1.03413021557008));
#52786=CARTESIAN_POINT('Ctrl Pts',(71.7046868561564,8.63896427541392,1.03511038928643));
#52787=CARTESIAN_POINT('Ctrl Pts',(71.7008338384512,8.63655872418921,1.03609341408942));
#52788=CARTESIAN_POINT('Ctrl Pts',(71.6209904060947,8.58671014284756,1.05646396007881));
#52789=CARTESIAN_POINT('Ctrl Pts',(71.5396217322624,8.53745717547068,1.07756846979329));
#52790=CARTESIAN_POINT('Ctrl Pts',(71.456859049088,8.48908067659746,1.09980595760576));
#52791=CARTESIAN_POINT('Ctrl Pts',(71.3807680272526,8.44460390166829,1.12025083814614));
#52792=CARTESIAN_POINT('Ctrl Pts',(71.3034986191992,8.40086816269192,1.14165286565924));
#52793=CARTESIAN_POINT('Ctrl Pts',(71.2251186384731,8.35808201230144,1.16434513180719));
#52794=CARTESIAN_POINT('Ctrl Pts',(71.1467386577471,8.31529586191095,1.18703739795513));
#52795=CARTESIAN_POINT('Ctrl Pts',(71.0672485802617,8.27345962988279,1.21101900311761));
#52796=CARTESIAN_POINT('Ctrl Pts',(70.9866768879313,8.2327678316685,1.23665789244156));
#52797=CARTESIAN_POINT('Ctrl Pts',(70.9225854914917,8.20039921564761,1.25705255181145));
#52798=CARTESIAN_POINT('Ctrl Pts',(70.8577935182715,8.1687475991007,1.27851198822847));
#52799=CARTESIAN_POINT('Ctrl Pts',(70.7925061661959,8.1379986244689,1.30115319693028));
#52800=CARTESIAN_POINT('Ctrl Pts',(70.7267525239182,8.10703003692366,1.32395611189601));
#52801=CARTESIAN_POINT('Ctrl Pts',(70.6604961163344,8.07697706982272,1.3479577397916));
#52802=CARTESIAN_POINT('Ctrl Pts',(70.5939313780561,8.04798541106798,1.37330331984324));
#52803=CARTESIAN_POINT('Ctrl Pts',(70.5257910186144,8.01830750502556,1.3992488426478));
#52804=CARTESIAN_POINT('Ctrl Pts',(70.4573271547263,7.98974176606292,1.4266027777622));
#52805=CARTESIAN_POINT('Ctrl Pts',(70.3887376769203,7.96239790239819,1.45554731412904));
#52806=CARTESIAN_POINT('Ctrl Pts',(70.3778897660787,7.9580732770389,1.4601250971929));
#52807=CARTESIAN_POINT('Ctrl Pts',(70.3670386998171,7.95377912294994,1.46474271725));
#52808=CARTESIAN_POINT('Ctrl Pts',(70.3561852489274,7.94951577156251,1.46940094995523));
#52809=CARTESIAN_POINT('Ctrl Pts',(70.3065003382005,7.9299990081631,1.49072540044166));
#52810=CARTESIAN_POINT('Ctrl Pts',(70.2567653163896,7.91112852120851,1.51290089381212));
#52811=CARTESIAN_POINT('Ctrl Pts',(70.2070623135176,7.89291853271043,1.53600529080569));
#52812=CARTESIAN_POINT('Ctrl Pts',(70.159209965595,7.87538657981169,1.55824941248034));
#52813=CARTESIAN_POINT('Ctrl Pts',(70.1113957992755,7.85847545200609,1.5813364086832));
#52814=CARTESIAN_POINT('Ctrl Pts',(70.0640678103716,7.84231378742065,1.60505474719515));
#52815=CARTESIAN_POINT('Ctrl Pts',(70.0464012568961,7.83628097431651,1.61390830943973));
#52816=CARTESIAN_POINT('Ctrl Pts',(70.0288026585101,7.83035211896612,1.62284973799107));
#52817=CARTESIAN_POINT('Ctrl Pts',(70.0112961471453,7.82453231586902,1.63186758920309));
#52818=CARTESIAN_POINT('Ctrl Pts',(69.9525478479664,7.80500223780914,1.66212966769005));
#52819=CARTESIAN_POINT('Ctrl Pts',(69.8948362221269,7.78669457785894,1.69325323137175));
#52820=CARTESIAN_POINT('Ctrl Pts',(69.8377704723018,7.7693827643488,1.72543337981226));
#52821=CARTESIAN_POINT('Ctrl Pts',(69.8322750469301,7.76771563863002,1.72853232453389));
#52822=CARTESIAN_POINT('Ctrl Pts',(69.8267856033749,7.76605778674206,1.73164106526536));
#52823=CARTESIAN_POINT('Ctrl Pts',(69.8213017872758,7.76440903040879,1.73475977511561));
#52824=CARTESIAN_POINT('Ctrl Pts',(69.7467647250881,7.7419988235152,1.77714986731706));
#52825=CARTESIAN_POINT('Ctrl Pts',(69.6732726250391,7.72127062399585,1.82137723267184));
#52826=CARTESIAN_POINT('Ctrl Pts',(69.6008174128332,7.70204255404898,1.86742873080328));
#52827=CARTESIAN_POINT('Ctrl Pts',(69.5519019344798,7.68906142804534,1.89851871027355));
#52828=CARTESIAN_POINT('Ctrl Pts',(69.5034597369955,7.67676431036926,1.93043932883238));
#52829=CARTESIAN_POINT('Ctrl Pts',(69.4554974352252,7.66509865519602,1.96317722051819));
#52830=CARTESIAN_POINT('Ctrl Pts',(69.3814453687939,7.64708730378109,2.01372334613052));
#52831=CARTESIAN_POINT('Ctrl Pts',(69.3085341262881,7.63057938939238,2.06622116555943));
#52832=CARTESIAN_POINT('Ctrl Pts',(69.2367320173285,7.61537862467897,2.12062321961406));
#52833=CARTESIAN_POINT('Ctrl Pts',(69.1931442909367,7.60615094623228,2.15364818060257));
#52834=CARTESIAN_POINT('Ctrl Pts',(69.1499659753585,7.59740542792075,2.18737417453181));
#52835=CARTESIAN_POINT('Ctrl Pts',(69.1071959837192,7.58910201458796,2.22178463376911));
#52836=CARTESIAN_POINT('Ctrl Pts',(69.050583461092,7.57811119702716,2.26733205679904));
#52837=CARTESIAN_POINT('Ctrl Pts',(68.9946823019327,7.56789262939594,2.31408266864305));
#52838=CARTESIAN_POINT('Ctrl Pts',(68.9392638713717,7.5583260135376,2.36208160192688));
#52839=CARTESIAN_POINT('Ctrl Pts',(68.9115546560912,7.55354270560842,2.38608106856881));
#52840=CARTESIAN_POINT('Ctrl Pts',(68.883965998737,7.54892353081008,2.41039260184554));
#52841=CARTESIAN_POINT('Ctrl Pts',(68.8567731667949,7.54449996075162,2.43489503258616));
#52842=CARTESIAN_POINT('Ctrl Pts',(68.8295803348527,7.54007639069317,2.45939746332675));
#52843=CARTESIAN_POINT('Ctrl Pts',(68.8027835039613,7.53584644002574,2.48409084385879));
#52844=CARTESIAN_POINT('Ctrl Pts',(68.7758795221472,7.53172516776694,2.50914205840402));
#52845=CARTESIAN_POINT('Ctrl Pts',(68.7301518127084,7.52472039272396,2.55172068738643));
#52846=CARTESIAN_POINT('Ctrl Pts',(68.6840624656445,7.51802262568023,2.59538653605302));
#52847=CARTESIAN_POINT('Ctrl Pts',(68.6372644191002,7.51157227596553,2.64100742771448));
#52848=CARTESIAN_POINT('Ctrl Pts',(68.5897557349075,7.50502397640697,2.68732108169315));
#52849=CARTESIAN_POINT('Ctrl Pts',(68.5415167591615,7.49873099597664,2.73564949180677));
#52850=CARTESIAN_POINT('Ctrl Pts',(68.4921482382404,7.49265420489694,2.78693336440043));
#52851=CARTESIAN_POINT('Ctrl Pts',(68.4421098073691,7.48649495433225,2.83891313745651));
#52852=CARTESIAN_POINT('Ctrl Pts',(68.3909109596423,7.48055824363085,2.89392903813864));
#52853=CARTESIAN_POINT('Ctrl Pts',(68.3380983558102,7.47482122749588,2.95299557340639));
#52854=CARTESIAN_POINT('Ctrl Pts',(68.2828747081629,7.46882230044824,3.01475866203846));
#52855=CARTESIAN_POINT('Ctrl Pts',(68.2258865060699,7.46304247477419,3.08095050350886));
#52856=CARTESIAN_POINT('Ctrl Pts',(68.1665747574627,7.45746619752795,3.15277143207088));
#52857=CARTESIAN_POINT('Ctrl Pts',(68.1342306780551,7.45442532353104,3.19193705896753));
#52858=CARTESIAN_POINT('Ctrl Pts',(68.1011949235458,7.45144510807664,3.23277736689701));
#52859=CARTESIAN_POINT('Ctrl Pts',(68.067372593208,7.44852266268155,3.27549181431079));
#52860=CARTESIAN_POINT('Ctrl Pts',(68.0393618341962,7.44610237073628,3.31086678939027));
#52861=CARTESIAN_POINT('Ctrl Pts',(68.0108461331695,7.44372514058797,3.34750216611316));
#52862=CARTESIAN_POINT('Ctrl Pts',(67.9818717403097,7.44139632116286,3.38541042745233));
#52863=CARTESIAN_POINT('Ctrl Pts',(67.9352181391225,7.4376465337826,3.44644904575164));
#52864=CARTESIAN_POINT('Ctrl Pts',(67.8873742724675,7.43402312749421,3.51078829405039));
#52865=CARTESIAN_POINT('Ctrl Pts',(67.8385661574121,7.4305321130176,3.57847174093336));
#52866=CARTESIAN_POINT('Ctrl Pts',(67.7799537039465,7.42633984041443,3.65975111171679));
#52867=CARTESIAN_POINT('Ctrl Pts',(67.7199498519168,7.42233929637198,3.74585372531127));
#52868=CARTESIAN_POINT('Ctrl Pts',(67.658984107429,7.41850083566823,3.83683942029884));
#52869=CARTESIAN_POINT('Ctrl Pts',(67.5959003797892,7.41452902475006,3.93098600786092));
#52870=CARTESIAN_POINT('Ctrl Pts',(67.5317869521182,7.41073023073603,4.03036110899213));
#52871=CARTESIAN_POINT('Ctrl Pts',(67.4671609034974,7.40703976043349,4.13500568014468));
#52872=CARTESIAN_POINT('Ctrl Pts',(67.3976824709064,7.40307219475965,4.24750738708804));
#52873=CARTESIAN_POINT('Ctrl Pts',(67.327611744913,7.39922890666538,4.3660999664496));
#52874=CARTESIAN_POINT('Ctrl Pts',(67.2576354760908,7.39540446226772,4.49079996308749));
#52875=CARTESIAN_POINT('Ctrl Pts',(67.2253998664584,7.39364267503987,4.5482448723464));
#52876=CARTESIAN_POINT('Ctrl Pts',(67.1931848694007,7.3918846469134,4.60698535420133));
#52877=CARTESIAN_POINT('Ctrl Pts',(67.1610601855551,7.39011941651789,4.66702057018075));
#52878=CARTESIAN_POINT('Ctrl Pts',(67.1027034504911,7.38691275204104,4.77607873897899));
#52879=CARTESIAN_POINT('Ctrl Pts',(67.0445967951296,7.38367598971354,4.88940658137533));
#52880=CARTESIAN_POINT('Ctrl Pts',(66.987257923219,7.3803305620751,5.00568290057736));
#52881=CARTESIAN_POINT('Ctrl Pts',(66.9741040662662,7.37956310231986,5.03235733658942));
#52882=CARTESIAN_POINT('Ctrl Pts',(66.9609906888157,7.37879001909429,5.05918675937889));
#52883=CARTESIAN_POINT('Ctrl Pts',(66.9479241477424,7.37801056057405,5.08615491125607));
#52884=CARTESIAN_POINT('Ctrl Pts',(66.8875144375256,7.37440693945733,5.21083505658684));
#52885=CARTESIAN_POINT('Ctrl Pts',(66.8281056642597,7.37066314832943,5.33848162552259));
#52886=CARTESIAN_POINT('Ctrl Pts',(66.7703316269961,7.36673766393218,5.46737610691827));
#52887=CARTESIAN_POINT('Ctrl Pts',(66.7485076159051,7.36525482113496,5.51606570392032));
#52888=CARTESIAN_POINT('Ctrl Pts',(66.7269168694435,7.36374656641509,5.56493325569604));
#52889=CARTESIAN_POINT('Ctrl Pts',(66.7055933079143,7.36221263535037,5.61388618348348));
#52890=CARTESIAN_POINT('Ctrl Pts',(66.6705404894961,7.35969107688538,5.69435764161353));
#52891=CARTESIAN_POINT('Ctrl Pts',(66.6362070137045,7.35709334765865,5.77457740473056));
#52892=CARTESIAN_POINT('Ctrl Pts',(66.6024276407753,7.35440345015614,5.85511097730033));
#52893=CARTESIAN_POINT('Ctrl Pts',(66.5697369835203,7.35180024856651,5.93304893736597));
#52894=CARTESIAN_POINT('Ctrl Pts',(66.5375651271738,7.34911077725039,6.01128296840618));
#52895=CARTESIAN_POINT('Ctrl Pts',(66.5057598873521,7.346313564451,6.09054288218826));
#52896=CARTESIAN_POINT('Ctrl Pts',(66.4858044278963,7.34455851820955,6.14027267529217));
#52897=CARTESIAN_POINT('Ctrl Pts',(66.465993265484,7.34276095254317,6.19040585962652));
#52898=CARTESIAN_POINT('Ctrl Pts',(66.4462888775018,7.34091441397408,6.24112139183781));
#52899=CARTESIAN_POINT('Ctrl Pts',(66.4177191712417,7.33823708826549,6.31465465049112));
#52900=CARTESIAN_POINT('Ctrl Pts',(66.3893738107666,7.33545693498657,6.38941296128914));
#52901=CARTESIAN_POINT('Ctrl Pts',(66.3611415770503,7.33254927110616,6.46471849632842));
#52902=CARTESIAN_POINT('Ctrl Pts',(66.3411307769353,7.3304883402816,6.51809450703888));
#52903=CARTESIAN_POINT('Ctrl Pts',(66.3211768417519,7.32836327159669,6.57174617528332));
#52904=CARTESIAN_POINT('Ctrl Pts',(66.3012408988535,7.32616401149819,6.62541455568106));
#52905=CARTESIAN_POINT('Ctrl Pts',(66.3010470943458,7.32614263169574,6.62593628540793));
#52906=CARTESIAN_POINT('Ctrl Pts',(66.3008532829922,7.32612125012428,6.62645809298242));
#52907=CARTESIAN_POINT('Ctrl Pts',(66.300659464751,7.32609986677702,6.62697997853453));
#52908=CARTESIAN_POINT('',(77.889681615155,13.4545721695848,-1.3438880610302));
#52909=CARTESIAN_POINT('Ctrl Pts',(77.8897369876382,13.454578052485,-1.34376136630412));
#52910=CARTESIAN_POINT('Ctrl Pts',(77.7696649432831,13.3860274200672,-1.26444509700194));
#52911=CARTESIAN_POINT('Ctrl Pts',(77.6507591912599,13.3147757364772,-1.18781988562592));
#52912=CARTESIAN_POINT('Ctrl Pts',(77.5329174622466,13.2411051793034,-1.11382860288741));
#52913=CARTESIAN_POINT('Ctrl Pts',(77.4085913534954,13.1633808130739,-1.03576586279179));
#52914=CARTESIAN_POINT('Ctrl Pts',(77.2854492624687,13.0829643495867,-0.960634817073859));
#52915=CARTESIAN_POINT('Ctrl Pts',(77.1633377242301,13.0001610172308,-0.888327978216956));
#52916=CARTESIAN_POINT('Ctrl Pts',(77.0305214521826,12.9100988488619,-0.809682463476546));
#52917=CARTESIAN_POINT('Ctrl Pts',(76.8989239464047,12.8172131254906,-0.734377989221384));
#52918=CARTESIAN_POINT('Ctrl Pts',(76.7683148872926,12.7218623074812,-0.662230278878765));
#52919=CARTESIAN_POINT('Ctrl Pts',(76.6491405067779,12.6348593480762,-0.59639902074026));
#52920=CARTESIAN_POINT('Ctrl Pts',(76.5307882492475,12.545803177586,-0.533195049924176));
#52921=CARTESIAN_POINT('Ctrl Pts',(76.4130672370339,12.4549458820906,-0.472450897944697));
#52922=CARTESIAN_POINT('Ctrl Pts',(76.2762974708588,12.3493867229691,-0.401877571173899));
#52923=CARTESIAN_POINT('Ctrl Pts',(76.1403792450269,12.2413957409076,-0.334625199413047));
#52924=CARTESIAN_POINT('Ctrl Pts',(76.004996467159,12.1313534640472,-0.270409688323707));
#52925=CARTESIAN_POINT('Ctrl Pts',(75.8959215084883,12.0426947957172,-0.218672648144735));
#52926=CARTESIAN_POINT('Ctrl Pts',(75.7872165562079,11.9527241237791,-0.168939362331957));
#52927=CARTESIAN_POINT('Ctrl Pts',(75.6791301262885,11.8620082672792,-0.121234670160239));
#52928=CARTESIAN_POINT('Ctrl Pts',(75.5617280619492,11.7634738922486,-0.0694184584137104));
#52929=CARTESIAN_POINT('Ctrl Pts',(75.4450556136026,11.6640617599789,-0.019995805029085));
#52930=CARTESIAN_POINT('Ctrl Pts',(75.3293856079521,11.5645181097544,0.0270406542219756));
#52931=CARTESIAN_POINT('Ctrl Pts',(75.2545888435804,11.5001492795753,0.0574562744140373));
#52932=CARTESIAN_POINT('Ctrl Pts',(75.1802103035331,11.4357258127535,0.0868749546023082));
#52933=CARTESIAN_POINT('Ctrl Pts',(75.1063155860452,11.3714486085643,0.115306615285322));
#52934=CARTESIAN_POINT('Ctrl Pts',(75.0634481505555,11.334160436991,0.131800248682));
#52935=CARTESIAN_POINT('Ctrl Pts',(75.0207456102727,11.2969243424609,0.147958040871395));
#52936=CARTESIAN_POINT('Ctrl Pts',(74.9781991372383,11.2597586237108,0.163796713837524));
#52937=CARTESIAN_POINT('Ctrl Pts',(74.8570163150392,11.1539015134508,0.208909150968764));
#52938=CARTESIAN_POINT('Ctrl Pts',(74.7370964572705,11.0486184760316,0.251433430739692));
#52939=CARTESIAN_POINT('Ctrl Pts',(74.6182988652355,10.9443033407062,0.29167327561244));
#52940=CARTESIAN_POINT('Ctrl Pts',(74.53257013101,10.8690256826425,0.320711835294296));
#52941=CARTESIAN_POINT('Ctrl Pts',(74.447426725528,10.7942510487121,0.348560587500119));
#52942=CARTESIAN_POINT('Ctrl Pts',(74.362827427958,10.7201158474377,0.375331231937685));
#52943=CARTESIAN_POINT('Ctrl Pts',(74.3241300435651,10.6862049467191,0.387576651793423));
#52944=CARTESIAN_POINT('Ctrl Pts',(74.2855466310907,10.652427718942,0.399596480972964));
#52945=CARTESIAN_POINT('Ctrl Pts',(74.2470739624078,10.6187965603701,0.411402002610675));
#52946=CARTESIAN_POINT('Ctrl Pts',(74.1152717740108,10.503580734438,0.451846131918322));
#52947=CARTESIAN_POINT('Ctrl Pts',(73.9847620349683,10.390081163806,0.489768074617004));
#52948=CARTESIAN_POINT('Ctrl Pts',(73.855569922101,10.2788762885707,0.525598948152581));
#52949=CARTESIAN_POINT('Ctrl Pts',(73.7181119302229,10.160556381127,0.563722327468323));
#52950=CARTESIAN_POINT('Ctrl Pts',(73.5821457405882,10.0448340625995,0.599478074205453));
#52951=CARTESIAN_POINT('Ctrl Pts',(73.4477337028793,9.93236292982832,0.633364489974651));
#52952=CARTESIAN_POINT('Ctrl Pts',(73.4400508513117,9.925934197451,0.635301402076798));
#52953=CARTESIAN_POINT('Ctrl Pts',(73.4323730851476,9.91951607647723,0.637232202501358));
#52954=CARTESIAN_POINT('Ctrl Pts',(73.4247004187787,9.91310868515717,0.639156982847771));
#52955=CARTESIAN_POINT('Ctrl Pts',(73.3484071455047,9.84939669333381,0.658296065130513));
#52956=CARTESIAN_POINT('Ctrl Pts',(73.2726503620905,9.78677844675524,0.676809304159524));
#52957=CARTESIAN_POINT('Ctrl Pts',(73.1970992174034,9.72507933887715,0.694899701214236));
#52958=CARTESIAN_POINT('Ctrl Pts',(73.1320183483839,9.67193081842693,0.710483035736911));
#52959=CARTESIAN_POINT('Ctrl Pts',(73.0670904212155,9.61946453509583,0.725752353116069));
#52960=CARTESIAN_POINT('Ctrl Pts',(73.0021168694563,9.56759598842738,0.740829004151231));
#52961=CARTESIAN_POINT('Ctrl Pts',(72.932838096084,9.51229057272347,0.756904651272255));
#52962=CARTESIAN_POINT('Ctrl Pts',(72.8635071947699,9.45766382673869,0.772761034710399));
#52963=CARTESIAN_POINT('Ctrl Pts',(72.7938955857395,9.40365790551125,0.788511490263578));
#52964=CARTESIAN_POINT('Ctrl Pts',(72.7382855472508,9.36051465110428,0.801093923735916));
#52965=CARTESIAN_POINT('Ctrl Pts',(72.6824966686878,9.31776823977093,0.813608634719925));
#52966=CARTESIAN_POINT('Ctrl Pts',(72.6264202454239,9.27541176713065,0.826110541299093));
#52967=CARTESIAN_POINT('Ctrl Pts',(72.5945374139565,9.25132955574594,0.833218629819788));
#52968=CARTESIAN_POINT('Ctrl Pts',(72.5625640095599,9.22737353904165,0.840326021588078));
#52969=CARTESIAN_POINT('Ctrl Pts',(72.5303081355092,9.20341764626573,0.847487344676562));
#52970=CARTESIAN_POINT('Ctrl Pts',(72.487572237045,9.1716784163914,0.856975401825411));
#52971=CARTESIAN_POINT('Ctrl Pts',(72.4443402247944,9.13993774890631,0.866558533369955));
#52972=CARTESIAN_POINT('Ctrl Pts',(72.4001654819828,9.10791760692907,0.876355253944482));
#52973=CARTESIAN_POINT('Ctrl Pts',(72.3718124277847,9.08736584447092,0.882643167166719));
#52974=CARTESIAN_POINT('Ctrl Pts',(72.3430712691142,9.06669988959138,0.889018841982827));
#52975=CARTESIAN_POINT('Ctrl Pts',(72.313826406605,9.04585705470419,0.895511213136602));
#52976=CARTESIAN_POINT('Ctrl Pts',(72.2782005556,9.02046648465175,0.903420166284219));
#52977=CARTESIAN_POINT('Ctrl Pts',(72.2418271176384,8.99481287323038,0.911501910042503));
#52978=CARTESIAN_POINT('Ctrl Pts',(72.2045037278336,8.9687958769127,0.919834021587207));
#52979=CARTESIAN_POINT('Ctrl Pts',(72.1538128961915,8.93346084472328,0.931150294459102));
#52980=CARTESIAN_POINT('Ctrl Pts',(72.1013168125388,8.89743020840457,0.942915182554698));
#52981=CARTESIAN_POINT('Ctrl Pts',(72.0474557803843,8.86112788084346,0.955113998180602));
#52982=CARTESIAN_POINT('Ctrl Pts',(71.9937786728343,8.82494951843807,0.967271157301807));
#52983=CARTESIAN_POINT('Ctrl Pts',(71.9387461380037,8.78850141025257,0.979861167387469));
#52984=CARTESIAN_POINT('Ctrl Pts',(71.8827684068436,8.75215890578048,0.992874181303956));
#52985=CARTESIAN_POINT('Ctrl Pts',(71.8301767728057,8.71801476210752,1.00510003704056));
#52986=CARTESIAN_POINT('Ctrl Pts',(71.7767506298625,8.68396339190662,1.01770080297037));
#52987=CARTESIAN_POINT('Ctrl Pts',(71.7228079848105,8.65028033847831,1.03064780199761));
#52988=CARTESIAN_POINT('Ctrl Pts',(71.7193349032355,8.648111664841,1.03148139077935));
#52989=CARTESIAN_POINT('Ctrl Pts',(71.7158596731749,8.64594450634418,1.03231640289029));
#52990=CARTESIAN_POINT('Ctrl Pts',(71.7123823764776,8.64377893173703,1.03315282533716));
#52991=CARTESIAN_POINT('',(76.015201080752,13.203464720596,-5.13235367185313));
#52992=CARTESIAN_POINT('Ctrl Pts',(76.0153669751839,13.2030576234056,-5.13241323346553));
#52993=CARTESIAN_POINT('Ctrl Pts',(76.421418629627,13.284909104379,-4.56170310137939));
#52994=CARTESIAN_POINT('Ctrl Pts',(76.7911800730128,13.3487897444448,-3.96280879484323));
#52995=CARTESIAN_POINT('Ctrl Pts',(77.4282530545409,13.4417516204142,-2.69007218753358));
#52996=CARTESIAN_POINT('Ctrl Pts',(77.6871091804814,13.4682801109617,-2.03089402659865));
#52997=CARTESIAN_POINT('Ctrl Pts',(77.8897919794669,13.4547521623004,-1.34470326831834));
#52998=CARTESIAN_POINT('',(69.6237422477963,12.3291004120382,-10.9554808154403));
#52999=CARTESIAN_POINT('Ctrl Pts',(69.6237422477963,12.3291004120382,-10.9554808154403));
#53000=CARTESIAN_POINT('Ctrl Pts',(70.0827581319187,12.3750434414314,-10.6014370912123));
#53001=CARTESIAN_POINT('Ctrl Pts',(70.9196713183267,12.4282942768532,-9.96905190676241));
#53002=CARTESIAN_POINT('Ctrl Pts',(71.9983599818921,12.4985273335172,-9.148643524566));
#53003=CARTESIAN_POINT('Ctrl Pts',(72.8711908196415,12.5908103550809,-8.44939111030075));
#53004=CARTESIAN_POINT('Ctrl Pts',(73.8194076466462,12.7307073058631,-7.63287520525915));
#53005=CARTESIAN_POINT('Ctrl Pts',(74.8903772207131,12.9478927784384,-6.5947327339628));
#53006=CARTESIAN_POINT('Ctrl Pts',(75.636641075592,13.1281023785155,-5.67240251279549));
#53007=CARTESIAN_POINT('Ctrl Pts',(76.015201080752,13.203464720596,-5.13235367185313));
#53008=CARTESIAN_POINT('',(56.9472987453407,10.4971210955841,-16.8490842893539));
#53009=CARTESIAN_POINT('Ctrl Pts',(56.9472987452418,10.4971210960185,-16.8490842892186));
#53010=CARTESIAN_POINT('Ctrl Pts',(57.5279764227459,10.5627663098217,-16.6356348664524));
#53011=CARTESIAN_POINT('Ctrl Pts',(59.2489796005507,10.727653207555,-16.0034819097119));
#53012=CARTESIAN_POINT('Ctrl Pts',(61.3469127090617,10.8548490654473,-15.2216988808759));
#53013=CARTESIAN_POINT('Ctrl Pts',(63.6263802921922,11.1482588003824,-14.3361986078586));
#53014=CARTESIAN_POINT('Ctrl Pts',(65.6200127215301,11.5559853879963,-13.4649812857152));
#53015=CARTESIAN_POINT('Ctrl Pts',(67.2665644790765,11.9454658004384,-12.5548298006343));
#53016=CARTESIAN_POINT('Ctrl Pts',(68.6272491818126,12.2018297485735,-11.6733467842871));
#53017=CARTESIAN_POINT('Ctrl Pts',(69.3091557765954,12.295115398284,-11.1879566051838));
#53018=CARTESIAN_POINT('Ctrl Pts',(69.6237422477963,12.3291004120382,-10.9554808154403));
#53019=CARTESIAN_POINT('',(43.6350103091031,8.95468725191293,-22.9398456748034));
#53020=CARTESIAN_POINT('Ctrl Pts',(43.6350103091031,8.95468725191292,-22.9398456748034));
#53021=CARTESIAN_POINT('Ctrl Pts',(43.9816241860284,8.96228593705789,-22.557621122663));
#53022=CARTESIAN_POINT('Ctrl Pts',(45.0665104587698,8.90088112468958,-21.464400433797));
#53023=CARTESIAN_POINT('Ctrl Pts',(46.5058625028201,8.76988624042247,-20.3242063737796));
#53024=CARTESIAN_POINT('Ctrl Pts',(48.0929903702374,8.97675586023584,-19.5751405126828));
#53025=CARTESIAN_POINT('Ctrl Pts',(48.9363712410941,9.12178060695302,-19.2461729821237));
#53026=CARTESIAN_POINT('Ctrl Pts',(49.8971073949701,9.31033141838707,-18.924603413807));
#53027=CARTESIAN_POINT('Ctrl Pts',(51.3205749059214,9.59771447476012,-18.4933476791936));
#53028=CARTESIAN_POINT('Ctrl Pts',(53.704075386902,10.0351563165077,-17.8376971923096));
#53029=CARTESIAN_POINT('Ctrl Pts',(55.8717928719535,10.3637905543193,-17.2067231078532));
#53030=CARTESIAN_POINT('Ctrl Pts',(56.9472987452418,10.4971210960185,-16.8490842892186));
#53031=CARTESIAN_POINT('',(39.8379457614118,8.40789306792086,-29.2047706348498));
#53032=CARTESIAN_POINT('Ctrl Pts',(39.8379458507108,8.40789307202619,-29.2047705582436));
#53033=CARTESIAN_POINT('Ctrl Pts',(39.8654457076855,8.40364510819277,-29.0955685679339));
#53034=CARTESIAN_POINT('Ctrl Pts',(39.8944208207261,8.39988236979115,-28.9853680288274));
#53035=CARTESIAN_POINT('Ctrl Pts',(39.9245087456163,8.39664864008142,-28.8750526458601));
#53036=CARTESIAN_POINT('Ctrl Pts',(39.9491018028661,8.39400547674688,-28.7848838310032));
#53037=CARTESIAN_POINT('Ctrl Pts',(39.974439446193,8.39171630686269,-28.6946375080915));
#53038=CARTESIAN_POINT('Ctrl Pts',(40.0003463528771,8.38980515356937,-28.6047839467515));
#53039=CARTESIAN_POINT('Ctrl Pts',(40.036943271421,8.38710539777634,-28.4778539544787));
#53040=CARTESIAN_POINT('Ctrl Pts',(40.0746628015218,8.38514479988263,-28.351668786224));
#53041=CARTESIAN_POINT('Ctrl Pts',(40.1151217116781,8.38440583150625,-28.2241319360277));
#53042=CARTESIAN_POINT('Ctrl Pts',(40.1509951639247,8.38375061497522,-28.111049623936));
#53043=CARTESIAN_POINT('Ctrl Pts',(40.1890192933759,8.38405564745187,-27.9969067272385));
#53044=CARTESIAN_POINT('Ctrl Pts',(40.230302310591,8.3856577702999,-27.8802179261844));
#53045=CARTESIAN_POINT('Ctrl Pts',(40.2509085167103,8.38645746169511,-27.8219733101525));
#53046=CARTESIAN_POINT('Ctrl Pts',(40.2723265910565,8.38758035193068,-27.7630938340167));
#53047=CARTESIAN_POINT('Ctrl Pts',(40.294695712765,8.38906805768105,-27.703389664616));
#53048=CARTESIAN_POINT('Ctrl Pts',(40.3301636319506,8.39142692666185,-27.6087242288008));
#53049=CARTESIAN_POINT('Ctrl Pts',(40.3680208790409,8.39470347103164,-27.5119877200577));
#53050=CARTESIAN_POINT('Ctrl Pts',(40.4088318964747,8.39906594238233,-27.4123919238348));
#53051=CARTESIAN_POINT('Ctrl Pts',(40.4156338083733,8.39979302902838,-27.3957924398233));
#53052=CARTESIAN_POINT('Ctrl Pts',(40.4225178367521,8.40055025887844,-27.3791134347866));
#53053=CARTESIAN_POINT('Ctrl Pts',(40.4294866832965,8.40133837812109,-27.3623511375053));
#53054=CARTESIAN_POINT('Ctrl Pts',(40.4660898787361,8.40547789855459,-27.2743087850876));
#53055=CARTESIAN_POINT('Ctrl Pts',(40.5050731911368,8.41048451571273,-27.1839285580151));
#53056=CARTESIAN_POINT('Ctrl Pts',(40.5468152791266,8.41653147821018,-27.0912433138878));
#53057=CARTESIAN_POINT('Ctrl Pts',(40.5863426940439,8.42225761236248,-27.0034755888465));
#53058=CARTESIAN_POINT('Ctrl Pts',(40.6283436920716,8.42891728279138,-26.9136409650853));
#53059=CARTESIAN_POINT('Ctrl Pts',(40.6731712777039,8.43663873332445,-26.8217452228992));
#53060=CARTESIAN_POINT('Ctrl Pts',(40.7158607183075,8.44399189319812,-26.7342326394656));
#53061=CARTESIAN_POINT('Ctrl Pts',(40.7611133986222,8.4523085787623,-26.6448508348228));
#53062=CARTESIAN_POINT('Ctrl Pts',(40.8092660707817,8.4616729323727,-26.5535842941883));
#53063=CARTESIAN_POINT('Ctrl Pts',(40.8546173937697,8.47049250159107,-26.4676273124322));
#53064=CARTESIAN_POINT('Ctrl Pts',(40.9025411427559,8.48024183005811,-26.3799983939024));
#53065=CARTESIAN_POINT('Ctrl Pts',(40.9533481888092,8.49095967199949,-26.2906670701268));
#53066=CARTESIAN_POINT('Ctrl Pts',(40.9708435866532,8.49465035908641,-26.2599058436672));
#53067=CARTESIAN_POINT('Ctrl Pts',(40.9886811427199,8.49845557165255,-26.2289425997796));
#53068=CARTESIAN_POINT('Ctrl Pts',(41.006874407862,8.50237580188874,-26.1977756141706));
#53069=CARTESIAN_POINT('Ctrl Pts',(41.0543714794208,8.51261032848971,-26.1164081117363));
#53070=CARTESIAN_POINT('Ctrl Pts',(41.1042913860663,8.5236312272845,-26.0336524923972));
#53071=CARTESIAN_POINT('Ctrl Pts',(41.156883062279,8.53543041516824,-25.9494837002749));
#53072=CARTESIAN_POINT('Ctrl Pts',(41.182392510285,8.54115357882281,-25.9086578589823));
#53073=CARTESIAN_POINT('Ctrl Pts',(41.2085309627192,8.5470592965295,-25.8674994260819));
#53074=CARTESIAN_POINT('Ctrl Pts',(41.2353251982349,8.5531467156204,-25.8260048651385));
#53075=CARTESIAN_POINT('Ctrl Pts',(41.29696834527,8.56715150668316,-25.7305419690284));
#53076=CARTESIAN_POINT('Ctrl Pts',(41.3620507458278,8.58211304497296,-25.6333500282192));
#53077=CARTESIAN_POINT('Ctrl Pts',(41.4303930158195,8.59780001240496,-25.5346447309645));
#53078=CARTESIAN_POINT('Ctrl Pts',(41.4648092332714,8.60569975121032,-25.4849381149217));
#53079=CARTESIAN_POINT('Ctrl Pts',(41.5000518250078,8.61378278089177,-25.4348478483315));
#53080=CARTESIAN_POINT('Ctrl Pts',(41.5360953172835,8.62201528938143,-25.384402666044));
#53081=CARTESIAN_POINT('Ctrl Pts',(41.559761387381,8.62742073460035,-25.3512804810191));
#53082=CARTESIAN_POINT('Ctrl Pts',(41.5837751341606,8.63289296667882,-25.3179985849375));
#53083=CARTESIAN_POINT('Ctrl Pts',(41.6093083635431,8.63869517343395,-25.2830281569375));
#53084=CARTESIAN_POINT('Ctrl Pts',(41.6273155224164,8.64278714540074,-25.2583654696045));
#53085=CARTESIAN_POINT('Ctrl Pts',(41.646078875468,8.64704290198039,-25.2328624102245));
#53086=CARTESIAN_POINT('Ctrl Pts',(41.6660177860212,8.65154646109351,-25.2059722122501));
#53087=CARTESIAN_POINT('Ctrl Pts',(41.7061938401206,8.66062094056852,-25.1517896105636));
#53088=CARTESIAN_POINT('Ctrl Pts',(41.7511315850727,8.67069915813332,-25.0919867008814));
#53089=CARTESIAN_POINT('Ctrl Pts',(41.8008463390065,8.68169374062394,-25.0271020172724));
#53090=CARTESIAN_POINT('Ctrl Pts',(41.8505610929402,8.69268832311456,-24.9622173336634));
#53091=CARTESIAN_POINT('Ctrl Pts',(41.9050537586142,8.704600084385,-24.8922502534608));
#53092=CARTESIAN_POINT('Ctrl Pts',(41.9643405116155,8.7172845050543,-24.8177290368986));
#53093=CARTESIAN_POINT('Ctrl Pts',(42.0110422922183,8.72727636666222,-24.7590266568565));
#53094=CARTESIAN_POINT('Ctrl Pts',(42.0606925307826,8.73773282487033,-24.6974848315058));
#53095=CARTESIAN_POINT('Ctrl Pts',(42.1132268093581,8.74852068902431,-24.6333316508617));
#53096=CARTESIAN_POINT('Ctrl Pts',(42.1717469346412,8.76053774110816,-24.5618687456805));
#53097=CARTESIAN_POINT('Ctrl Pts',(42.2338464229499,8.7729672300637,-24.4871659557205));
#53098=CARTESIAN_POINT('Ctrl Pts',(42.2994250245914,8.78556845114903,-24.4094937624744));
#53099=CARTESIAN_POINT('Ctrl Pts',(42.3634124541936,8.79786392142312,-24.3337061751673));
#53100=CARTESIAN_POINT('Ctrl Pts',(42.4307126950835,8.81032240727235,-24.2550903585965));
#53101=CARTESIAN_POINT('Ctrl Pts',(42.501209777579,8.8226782550421,-24.1739053400292));
#53102=CARTESIAN_POINT('Ctrl Pts',(42.5570843250992,8.83247124758767,-24.1095597527043));
#53103=CARTESIAN_POINT('Ctrl Pts',(42.6149667148955,8.84219877627966,-24.0436001241147));
#53104=CARTESIAN_POINT('Ctrl Pts',(42.6747857552258,8.85171312383745,-23.9761668200724));
#53105=CARTESIAN_POINT('Ctrl Pts',(42.7238451349108,8.85951612413157,-23.9208627555447));
#53106=CARTESIAN_POINT('Ctrl Pts',(42.7742443970811,8.8670794989284,-23.8640393593037));
#53107=CARTESIAN_POINT('Ctrl Pts',(42.8258983427455,8.8743404967404,-23.806024202641));
#53108=CARTESIAN_POINT('Ctrl Pts',(42.8935600993232,8.8838517133599,-23.7300298646009));
#53109=CARTESIAN_POINT('Ctrl Pts',(42.9633750842634,8.89284222249282,-23.6519886341592));
#53110=CARTESIAN_POINT('Ctrl Pts',(43.0350811932542,8.90130616648017,-23.5731341011721));
#53111=CARTESIAN_POINT('Ctrl Pts',(43.0937059954034,8.90822603772467,-23.5086649581661));
#53112=CARTESIAN_POINT('Ctrl Pts',(43.1535941612811,8.91479461164248,-23.4436558523941));
#53113=CARTESIAN_POINT('Ctrl Pts',(43.2145942946101,8.92102322071077,-23.3787767103528));
#53114=CARTESIAN_POINT('Ctrl Pts',(43.2511690823933,8.92475780361125,-23.3398761256784));
#53115=CARTESIAN_POINT('Ctrl Pts',(43.288144220567,8.92836938755794,-23.3010181242117));
#53116=CARTESIAN_POINT('Ctrl Pts',(43.3255173890699,8.93177350374001,-23.2619819456453));
#53117=CARTESIAN_POINT('Ctrl Pts',(43.3607688402983,8.93498436437547,-23.2251618953257));
#53118=CARTESIAN_POINT('Ctrl Pts',(43.3963743880188,8.93801049201531,-23.1881827163246));
#53119=CARTESIAN_POINT('Ctrl Pts',(43.4323243751605,8.94079491063417,-23.1508996625381));
#53120=CARTESIAN_POINT('Ctrl Pts',(43.4663601170789,8.94343106605561,-23.1156018363774));
#53121=CARTESIAN_POINT('Ctrl Pts',(43.5007045420071,8.94585052166189,-23.0800314125403));
#53122=CARTESIAN_POINT('Ctrl Pts',(43.5353428904246,8.94801909874426,-23.0441085446635));
#53123=CARTESIAN_POINT('Ctrl Pts',(43.56843184955,8.95009067437406,-23.0097925232266));
#53124=CARTESIAN_POINT('Ctrl Pts',(43.6017889679761,8.95193331677229,-22.9751548483822));
#53125=CARTESIAN_POINT('Ctrl Pts',(43.6353959980847,8.95353081601041,-22.9401679958081));
#53126=CARTESIAN_POINT('',(38.9090196509257,8.64412049687874,-35.3258758917141));
#53127=CARTESIAN_POINT('Ctrl Pts',(38.9087434864013,8.64500019882641,-35.3257985374456));
#53128=CARTESIAN_POINT('Ctrl Pts',(38.9479517964268,8.6357301980531,-35.0802394942275));
#53129=CARTESIAN_POINT('Ctrl Pts',(38.9841706465803,8.62691819966679,-34.8358387398463));
#53130=CARTESIAN_POINT('Ctrl Pts',(39.0183707678307,8.61831927471614,-34.592222979301));
#53131=CARTESIAN_POINT('Ctrl Pts',(39.0533216837988,8.60953157770287,-34.3432591258404));
#53132=CARTESIAN_POINT('Ctrl Pts',(39.0861634603905,8.60096397289051,-34.0951162517341));
#53133=CARTESIAN_POINT('Ctrl Pts',(39.1178679600129,8.59241082953619,-33.847691734173));
#53134=CARTESIAN_POINT('Ctrl Pts',(39.1483258371988,8.58419399618631,-33.6099959604378));
#53135=CARTESIAN_POINT('Ctrl Pts',(39.177733914408,8.57599040915156,-33.3729645385711));
#53136=CARTESIAN_POINT('Ctrl Pts',(39.2069267841172,8.56763119233727,-33.1364750675382));
#53137=CARTESIAN_POINT('Ctrl Pts',(39.2209380749374,8.5636191366887,-33.0229705444275));
#53138=CARTESIAN_POINT('Ctrl Pts',(39.2348992662765,8.55957176304503,-32.9095908069147));
#53139=CARTESIAN_POINT('Ctrl Pts',(39.2488997523204,8.55547356312888,-32.7963217176363));
#53140=CARTESIAN_POINT('Ctrl Pts',(39.26811319789,8.54984943402538,-32.6408778655624));
#53141=CARTESIAN_POINT('Ctrl Pts',(39.287411692567,8.54413100777768,-32.4856347486376));
#53142=CARTESIAN_POINT('Ctrl Pts',(39.3068613012534,8.53834397345013,-32.3318970469014));
#53143=CARTESIAN_POINT('Ctrl Pts',(39.3222504300968,8.53376509382722,-32.2102550468871));
#53144=CARTESIAN_POINT('Ctrl Pts',(39.3377340677726,8.52914351924649,-32.0895562304329));
#53145=CARTESIAN_POINT('Ctrl Pts',(39.3533417882143,8.52450910313885,-31.9704683767878));
#53146=CARTESIAN_POINT('Ctrl Pts',(39.3684284241685,8.52002941317148,-31.8553564293885));
#53147=CARTESIAN_POINT('Ctrl Pts',(39.3836241066648,8.51553644644276,-31.7417266115632));
#53148=CARTESIAN_POINT('Ctrl Pts',(39.3993540901875,8.51096525102908,-31.6274715263285));
#53149=CARTESIAN_POINT('Ctrl Pts',(39.4141691946333,8.50665992309289,-31.5198616856205));
#53150=CARTESIAN_POINT('Ctrl Pts',(39.4294581565008,8.50228588894945,-31.4116967681536));
#53151=CARTESIAN_POINT('Ctrl Pts',(39.4455740757653,8.49775799379722,-31.3011828176225));
#53152=CARTESIAN_POINT('Ctrl Pts',(39.4524220787895,8.49583399311276,-31.254223047284));
#53153=CARTESIAN_POINT('Ctrl Pts',(39.4594193759509,8.49388175815388,-31.2068387470179));
#53154=CARTESIAN_POINT('Ctrl Pts',(39.4665929841818,8.49189240305858,-31.1588905269845));
#53155=CARTESIAN_POINT('Ctrl Pts',(39.4847506007671,8.48685700860855,-31.0375254667118));
#53156=CARTESIAN_POINT('Ctrl Pts',(39.5040385640118,8.48158512359671,-30.912541647874));
#53157=CARTESIAN_POINT('Ctrl Pts',(39.524965953692,8.47609349451604,-30.7832819655347));
#53158=CARTESIAN_POINT('Ctrl Pts',(39.5439349368359,8.47111577770303,-30.6661185365096));
#53159=CARTESIAN_POINT('Ctrl Pts',(39.5642507061145,8.46595797996059,-30.5454436942775));
#53160=CARTESIAN_POINT('Ctrl Pts',(39.5862904148607,8.46059797969943,-30.4207161971419));
#53161=CARTESIAN_POINT('Ctrl Pts',(39.5961523203423,8.45819958974947,-30.3649055327691));
#53162=CARTESIAN_POINT('Ctrl Pts',(39.6063593530292,8.45576024361895,-30.3082830308203));
#53163=CARTESIAN_POINT('Ctrl Pts',(39.6169450976819,8.45327533083215,-30.2507978882589));
#53164=CARTESIAN_POINT('Ctrl Pts',(39.632271772875,8.44967752525343,-30.1675674555055));
#53165=CARTESIAN_POINT('Ctrl Pts',(39.6483434234174,8.44608466718477,-30.0835384063042));
#53166=CARTESIAN_POINT('Ctrl Pts',(39.6652506185106,8.44244734684986,-29.9982286935872));
#53167=CARTESIAN_POINT('Ctrl Pts',(39.682240834708,8.43879216581432,-29.9125000759897));
#53168=CARTESIAN_POINT('Ctrl Pts',(39.7000749896951,8.43509186361522,-29.8254738199901));
#53169=CARTESIAN_POINT('Ctrl Pts',(39.7188369052445,8.43129884492167,-29.7368106658926));
#53170=CARTESIAN_POINT('Ctrl Pts',(39.7281696213245,8.42941208839834,-29.6927070645427));
#53171=CARTESIAN_POINT('Ctrl Pts',(39.7377318669302,8.42750219560164,-29.6481990543948));
#53172=CARTESIAN_POINT('Ctrl Pts',(39.7475337255395,8.42556209647708,-29.6032497837854));
#53173=CARTESIAN_POINT('Ctrl Pts',(39.757461449336,8.42359708463452,-29.5577233217899));
#53174=CARTESIAN_POINT('Ctrl Pts',(39.7676348147295,8.42160156843537,-29.5117485114425));
#53175=CARTESIAN_POINT('Ctrl Pts',(39.7780765752702,8.41953687256901,-29.4650397996942));
#53176=CARTESIAN_POINT('Ctrl Pts',(39.7825055440345,8.41866111282865,-29.4452278700344));
#53177=CARTESIAN_POINT('Ctrl Pts',(39.7869828223184,8.41777282382613,-29.425283308357));
#53178=CARTESIAN_POINT('Ctrl Pts',(39.7915102532766,8.41686865746927,-29.4051814390361));
#53179=CARTESIAN_POINT('Ctrl Pts',(39.7979316406918,8.41558625194641,-29.3766703713094));
#53180=CARTESIAN_POINT('Ctrl Pts',(39.8044540915392,8.4142714260871,-29.3478383316315));
#53181=CARTESIAN_POINT('Ctrl Pts',(39.8110618301717,8.41296548896544,-29.3190355764946));
#53182=CARTESIAN_POINT('Ctrl Pts',(39.8174072319651,8.41171139944787,-29.2913763326495));
#53183=CARTESIAN_POINT('Ctrl Pts',(39.8238312870333,8.41046549363018,-29.263743939833));
#53184=CARTESIAN_POINT('Ctrl Pts',(39.8303182042911,8.40926931741567,-29.2364965182498));
#53185=CARTESIAN_POINT('Ctrl Pts',(39.8325491549127,8.40885793401687,-29.2271257108693));
#53186=CARTESIAN_POINT('Ctrl Pts',(39.8347875241813,8.40845247797901,-29.2178008778995));
#53187=CARTESIAN_POINT('Ctrl Pts',(39.8370326159301,8.4080547876622,-29.208538029524));
#53188=CARTESIAN_POINT('Ctrl Pts',(39.837336887212,8.40800088975689,-29.2072826604502));
#53189=CARTESIAN_POINT('Ctrl Pts',(39.837641291277,8.40794698587253,-29.2060268678952));
#53190=CARTESIAN_POINT('Ctrl Pts',(39.8379458282931,8.40789307599463,-29.2047706507169));
#53191=CARTESIAN_POINT('',(37.4911183000542,8.66292929398162,-41.3743318420141));
#53192=CARTESIAN_POINT('Ctrl Pts',(37.4911898651196,8.66293555381076,-41.3740674147214));
#53193=CARTESIAN_POINT('Ctrl Pts',(37.6801716473364,8.68001236440291,-40.6833502317314));
#53194=CARTESIAN_POINT('Ctrl Pts',(38.0233165576779,8.70919148388572,-39.5173351893382));
#53195=CARTESIAN_POINT('Ctrl Pts',(38.4518695777218,8.70933987554425,-37.8053909622071));
#53196=CARTESIAN_POINT('Ctrl Pts',(38.6892091015529,8.68608245062232,-36.6248757859991));
#53197=CARTESIAN_POINT('Ctrl Pts',(38.818728329062,8.66459053329314,-35.8932912681495));
#53198=CARTESIAN_POINT('Ctrl Pts',(38.8824625141317,8.65036952003038,-35.4979095277334));
#53199=CARTESIAN_POINT('Ctrl Pts',(38.9091460645523,8.64371781549238,-35.3259113004388));
#53200=CARTESIAN_POINT('',(36.4975121937785,8.64395853169441,-47.4046427887098));
#53201=CARTESIAN_POINT('Ctrl Pts',(36.4974760183619,8.64411817641805,-47.4042708861961));
#53202=CARTESIAN_POINT('Ctrl Pts',(36.5017609841129,8.64268775187304,-47.3573097347399));
#53203=CARTESIAN_POINT('Ctrl Pts',(36.5059335353835,8.64129768267962,-47.3111892821043));
#53204=CARTESIAN_POINT('Ctrl Pts',(36.5099914476731,8.6399524796883,-47.2660110824115));
#53205=CARTESIAN_POINT('Ctrl Pts',(36.5144484058799,8.63847499247709,-47.2163901607351));
#53206=CARTESIAN_POINT('Ctrl Pts',(36.518767198879,8.63705162890043,-47.1679050560211));
#53207=CARTESIAN_POINT('Ctrl Pts',(36.5229530172055,8.63568534639452,-47.1206225324743));
#53208=CARTESIAN_POINT('Ctrl Pts',(36.5274144350992,8.63422910612218,-47.0702268678377));
#53209=CARTESIAN_POINT('Ctrl Pts',(36.5317261160483,8.63283736585082,-47.0211834002847));
#53210=CARTESIAN_POINT('Ctrl Pts',(36.5358915607992,8.631513263941,-46.9736167749596));
#53211=CARTESIAN_POINT('Ctrl Pts',(36.537647500156,8.63095509001365,-46.9535651083383));
#53212=CARTESIAN_POINT('Ctrl Pts',(36.5393775323541,8.63040888592338,-46.9337750226926));
#53213=CARTESIAN_POINT('Ctrl Pts',(36.5410820584912,8.62987472195882,-46.9142539481906));
#53214=CARTESIAN_POINT('Ctrl Pts',(36.5414176071999,8.62976956779039,-46.9104110787865));
#53215=CARTESIAN_POINT('Ctrl Pts',(36.5417522008652,8.62966486911207,-46.9065782521653));
#53216=CARTESIAN_POINT('Ctrl Pts',(36.5420870513848,8.62956024964645,-46.9027416653917));
#53217=CARTESIAN_POINT('Ctrl Pts',(36.5460702365561,8.62831575791135,-46.8571038818039));
#53218=CARTESIAN_POINT('Ctrl Pts',(36.5500453677753,8.62709642970009,-46.8114405783938));
#53219=CARTESIAN_POINT('Ctrl Pts',(36.5540243986474,8.62590470392077,-46.7657539407575));
#53220=CARTESIAN_POINT('Ctrl Pts',(36.556385723778,8.62519748346384,-46.7386415586093));
#53221=CARTESIAN_POINT('Ctrl Pts',(36.5587485687228,8.62449993284698,-46.7115197533868));
#53222=CARTESIAN_POINT('Ctrl Pts',(36.5611163443151,8.62381217719835,-46.6843811764931));
#53223=CARTESIAN_POINT('Ctrl Pts',(36.562423756438,8.62343241989551,-46.66939609744));
#53224=CARTESIAN_POINT('Ctrl Pts',(36.5637327734946,8.62305562005744,-46.6544047768329));
#53225=CARTESIAN_POINT('Ctrl Pts',(36.5650426602007,8.62268214977037,-46.6394210330265));
#53226=CARTESIAN_POINT('Ctrl Pts',(36.5684349148007,8.62171496207895,-46.6006171627238));
#53227=CARTESIAN_POINT('Ctrl Pts',(36.5718357059482,8.62076932915961,-46.5618331423751));
#53228=CARTESIAN_POINT('Ctrl Pts',(36.5752641319001,8.61984224913339,-46.5229435211988));
#53229=CARTESIAN_POINT('Ctrl Pts',(36.5814415558131,8.61817181307802,-46.4528712258681));
#53230=CARTESIAN_POINT('Ctrl Pts',(36.5877090791056,8.61656174374666,-46.3824547510109));
#53231=CARTESIAN_POINT('Ctrl Pts',(36.594089463791,8.61503000670491,-46.3119630026283));
#53232=CARTESIAN_POINT('Ctrl Pts',(36.595834692974,8.61461103005729,-46.2926813664097));
#53233=CARTESIAN_POINT('Ctrl Pts',(36.5975882890355,8.61419790459739,-46.2733946228975));
#53234=CARTESIAN_POINT('Ctrl Pts',(36.5993525794991,8.61379052995912,-46.2540873946039));
#53235=CARTESIAN_POINT('Ctrl Pts',(36.6123492664835,8.61078959515377,-46.1118602455913));
#53236=CARTESIAN_POINT('Ctrl Pts',(36.6259089518447,8.60810497287949,-45.9687191069632));
#53237=CARTESIAN_POINT('Ctrl Pts',(36.6404465288085,8.60582064395813,-45.8241744715311));
#53238=CARTESIAN_POINT('Ctrl Pts',(36.6574427818986,8.60314997658452,-45.6551836408901));
#53239=CARTESIAN_POINT('Ctrl Pts',(36.6757747741864,8.60102579619041,-45.4842673506916));
#53240=CARTESIAN_POINT('Ctrl Pts',(36.6961137047484,8.59958744575822,-45.3106010637092));
#53241=CARTESIAN_POINT('Ctrl Pts',(36.7014364382353,8.59921102694957,-45.2651522944906));
#53242=CARTESIAN_POINT('Ctrl Pts',(36.7068966967673,8.59888163230131,-45.2195153674192));
#53243=CARTESIAN_POINT('Ctrl Pts',(36.7125067718823,8.59860188028545,-45.1736754567841));
#53244=CARTESIAN_POINT('Ctrl Pts',(36.716359917578,8.5984097393152,-45.142191412322));
#53245=CARTESIAN_POINT('Ctrl Pts',(36.7202825680454,8.59824107383479,-45.1106211484891));
#53246=CARTESIAN_POINT('Ctrl Pts',(36.7242791266398,8.59809669301701,-45.0789560892659));
#53247=CARTESIAN_POINT('Ctrl Pts',(36.7366984669174,8.59764802838137,-44.9805566448154));
#53248=CARTESIAN_POINT('Ctrl Pts',(36.7498311650086,8.59743340908391,-44.8812354332942));
#53249=CARTESIAN_POINT('Ctrl Pts',(36.7638292859017,8.59748007452552,-44.7806458610636));
#53250=CARTESIAN_POINT('Ctrl Pts',(36.7691763788146,8.59749790009325,-44.7422220045413));
#53251=CARTESIAN_POINT('Ctrl Pts',(36.7746499508775,8.59755391226604,-44.7036127882181));
#53252=CARTESIAN_POINT('Ctrl Pts',(36.7802459639653,8.59764698565104,-44.664850828662));
#53253=CARTESIAN_POINT('Ctrl Pts',(36.7831524683006,8.59769532688841,-44.6447183161522));
#53254=CARTESIAN_POINT('Ctrl Pts',(36.7860916992519,8.59775366030292,-44.6245466950945));
#53255=CARTESIAN_POINT('Ctrl Pts',(36.7890641096592,8.59782186120053,-44.6043338411012));
#53256=CARTESIAN_POINT('Ctrl Pts',(36.7982395704418,8.5980323888786,-44.5419392778655));
#53257=CARTESIAN_POINT('Ctrl Pts',(36.8077393750307,8.59833696666467,-44.4790921606058));
#53258=CARTESIAN_POINT('Ctrl Pts',(36.8175796728728,8.59873406400653,-44.415757223244));
#53259=CARTESIAN_POINT('Ctrl Pts',(36.8188383897378,8.59878485851797,-44.407655765841));
#53260=CARTESIAN_POINT('Ctrl Pts',(36.8201026882879,8.59883717004869,-44.399546329321));
#53261=CARTESIAN_POINT('Ctrl Pts',(36.821372612154,8.59889099821599,-44.391428839473));
#53262=CARTESIAN_POINT('Ctrl Pts',(36.8223610381664,8.59893289455495,-44.3851107141618));
#53263=CARTESIAN_POINT('Ctrl Pts',(36.8233528898425,8.59897571162432,-44.3787876223995));
#53264=CARTESIAN_POINT('Ctrl Pts',(36.8243458969836,8.59901934535582,-44.3724740243719));
#53265=CARTESIAN_POINT('Ctrl Pts',(36.838789710824,8.59965402104843,-44.2806394032497));
#53266=CARTESIAN_POINT('Ctrl Pts',(36.8535934776877,8.60046538228348,-44.1900559875258));
#53267=CARTESIAN_POINT('Ctrl Pts',(36.8687566014926,8.60143265418725,-44.1006242196692));
#53268=CARTESIAN_POINT('Ctrl Pts',(36.8826235674842,8.60231724279622,-44.0188371618449));
#53269=CARTESIAN_POINT('Ctrl Pts',(36.8967918685694,8.6033324784733,-43.9380103420868));
#53270=CARTESIAN_POINT('Ctrl Pts',(36.9112857225907,8.60447070040713,-43.8580679367849));
#53271=CARTESIAN_POINT('Ctrl Pts',(36.9384153257078,8.60660122478518,-43.7084317030483));
#53272=CARTESIAN_POINT('Ctrl Pts',(36.9666925269518,8.60916555894038,-43.5619136599842));
#53273=CARTESIAN_POINT('Ctrl Pts',(36.9959471215658,8.61202820481559,-43.4179272462726));
#53274=CARTESIAN_POINT('Ctrl Pts',(37.0180880069539,8.61419475386768,-43.3089533662543));
#53275=CARTESIAN_POINT('Ctrl Pts',(37.0407868905128,8.61653172315501,-43.2014336937385));
#53276=CARTESIAN_POINT('Ctrl Pts',(37.0639612478015,8.61897702647482,-43.0950922117049));
#53277=CARTESIAN_POINT('Ctrl Pts',(37.071407004209,8.61976268506439,-43.0609254487882));
#53278=CARTESIAN_POINT('Ctrl Pts',(37.0789018371853,8.62055951697033,-43.0268800101056));
#53279=CARTESIAN_POINT('Ctrl Pts',(37.0864429363177,8.62136543706961,-42.9929462645575));
#53280=CARTESIAN_POINT('Ctrl Pts',(37.1086169465024,8.62373518187414,-42.8931667488425));
#53281=CARTESIAN_POINT('Ctrl Pts',(37.1311886149013,8.62618323438476,-42.7943634428842));
#53282=CARTESIAN_POINT('Ctrl Pts',(37.1541236014169,8.62867697054841,-42.696357845321));
#53283=CARTESIAN_POINT('Ctrl Pts',(37.1694195627341,8.63034011047957,-42.6309952680123));
#53284=CARTESIAN_POINT('Ctrl Pts',(37.1848765769503,8.63202351303894,-42.5659898511523));
#53285=CARTESIAN_POINT('Ctrl Pts',(37.2004833982249,8.63371744373424,-42.5012925931775));
#53286=CARTESIAN_POINT('Ctrl Pts',(37.2234845648212,8.63621394071077,-42.405942464998));
#53287=CARTESIAN_POINT('Ctrl Pts',(37.2468132737793,8.63873357086562,-42.3112505507811));
#53288=CARTESIAN_POINT('Ctrl Pts',(37.2704802586746,8.6412502632337,-42.2168802808142));
#53289=CARTESIAN_POINT('Ctrl Pts',(37.2806197694381,8.6423284753282,-42.1764497666481));
#53290=CARTESIAN_POINT('Ctrl Pts',(37.2908220477617,8.64340621535967,-42.1360759299403));
#53291=CARTESIAN_POINT('Ctrl Pts',(37.3010859637758,8.644481192736,-42.0957411959757));
#53292=CARTESIAN_POINT('Ctrl Pts',(37.3309930243853,8.647613468322,-41.9782136040035));
#53293=CARTESIAN_POINT('Ctrl Pts',(37.3614146919285,8.65072108931857,-41.8610575206228));
#53294=CARTESIAN_POINT('Ctrl Pts',(37.3921802979378,8.65373381794591,-41.7443617179619));
#53295=CARTESIAN_POINT('Ctrl Pts',(37.4247914593669,8.65692727298719,-41.6206656120724));
#53296=CARTESIAN_POINT('Ctrl Pts',(37.4577901536412,8.66001389139707,-41.4974790863762));
#53297=CARTESIAN_POINT('Ctrl Pts',(37.4909751693545,8.66291677591587,-41.3748606964831));
#53298=CARTESIAN_POINT('',(34.9058155546954,8.66668722396345,-53.4453943172971));
#53299=CARTESIAN_POINT('Ctrl Pts',(34.9063163914155,8.66722257324602,-53.4437571318374));
#53300=CARTESIAN_POINT('Ctrl Pts',(35.1934727320302,8.72417720600899,-52.7556732998408));
#53301=CARTESIAN_POINT('Ctrl Pts',(35.6781869696737,8.77551394752499,-51.5893141420722));
#53302=CARTESIAN_POINT('Ctrl Pts',(36.1004243200409,8.76372397778573,-50.1832810022625));
#53303=CARTESIAN_POINT('Ctrl Pts',(36.3808701953256,8.69787452481665,-48.6485604468675));
#53304=CARTESIAN_POINT('Ctrl Pts',(36.4554561965542,8.65716158483284,-47.8501354265767));
#53305=CARTESIAN_POINT('Ctrl Pts',(36.4974177553681,8.64413762617975,-47.4049093964135));
#53306=CARTESIAN_POINT('',(32.8153450360175,8.33795397633509,-59.2035503428015));
#53307=CARTESIAN_POINT('Ctrl Pts',(32.8153447698313,8.33795299861922,-59.2035496355344));
#53308=CARTESIAN_POINT('Ctrl Pts',(32.8259142758667,8.33379969528807,-59.1737918941683));
#53309=CARTESIAN_POINT('Ctrl Pts',(32.836888046712,8.32960496057437,-59.1426558331879));
#53310=CARTESIAN_POINT('Ctrl Pts',(32.84820294588,8.32543107112663,-59.1103062534762));
#53311=CARTESIAN_POINT('Ctrl Pts',(32.8590619641319,8.32142534902326,-59.0792600487053));
#53312=CARTESIAN_POINT('Ctrl Pts',(32.8702352647792,8.31743909897791,-59.047095978524));
#53313=CARTESIAN_POINT('Ctrl Pts',(32.8816554232607,8.31352701533988,-59.0140069035606));
#53314=CARTESIAN_POINT('Ctrl Pts',(32.8847282162794,8.31247440093782,-59.0051037102549));
#53315=CARTESIAN_POINT('Ctrl Pts',(32.887818809973,8.31142714143201,-58.9961338291535));
#53316=CARTESIAN_POINT('Ctrl Pts',(32.8909257279932,8.31038625917849,-58.9871016512053));
#53317=CARTESIAN_POINT('Ctrl Pts',(32.9166461377401,8.30176938616025,-58.9123293797061));
#53318=CARTESIAN_POINT('Ctrl Pts',(32.9434850606827,8.29359020115758,-58.8332884311441));
#53319=CARTESIAN_POINT('Ctrl Pts',(32.9715704512017,8.286120681936,-58.7496650526602));
#53320=CARTESIAN_POINT('Ctrl Pts',(32.9994388641737,8.27870886951243,-58.6666877180873));
#53321=CARTESIAN_POINT('Ctrl Pts',(33.028543782772,8.27192349048084,-58.5792095859131));
#53322=CARTESIAN_POINT('Ctrl Pts',(33.0590264471052,8.26603260100496,-58.4868732050853));
#53323=CARTESIAN_POINT('Ctrl Pts',(33.0827962253682,8.2614390019979,-58.414871123053));
#53324=CARTESIAN_POINT('Ctrl Pts',(33.1073972028525,8.25743539344415,-58.3399095066768));
#53325=CARTESIAN_POINT('Ctrl Pts',(33.1329039327878,8.25415052960207,-58.2617933242852));
#53326=CARTESIAN_POINT('Ctrl Pts',(33.1444908198075,8.25265832161187,-58.2263076551273));
#53327=CARTESIAN_POINT('Ctrl Pts',(33.1562652731685,8.25131438810635,-58.1901689837327));
#53328=CARTESIAN_POINT('Ctrl Pts',(33.1682348793725,8.25013104739556,-58.153357072047));
#53329=CARTESIAN_POINT('Ctrl Pts',(33.172888612169,8.24967096947977,-58.13904475485));
#53330=CARTESIAN_POINT('Ctrl Pts',(33.1775716886937,8.24923518581891,-58.1246311479278));
#53331=CARTESIAN_POINT('Ctrl Pts',(33.1822843164442,8.24882444181012,-58.1101157969434));
#53332=CARTESIAN_POINT('Ctrl Pts',(33.1977570970947,8.24747586256983,-58.0624581304058));
#53333=CARTESIAN_POINT('Ctrl Pts',(33.2135484995211,8.24639726237193,-58.0137034575228));
#53334=CARTESIAN_POINT('Ctrl Pts',(33.2297106092063,8.24563674393401,-57.9637961640372));
#53335=CARTESIAN_POINT('Ctrl Pts',(33.2471482039732,8.24481620672745,-57.9099502753097));
#53336=CARTESIAN_POINT('Ctrl Pts',(33.2650142543286,8.24436619688766,-57.8547722516667));
#53337=CARTESIAN_POINT('Ctrl Pts',(33.2833684711262,8.24434526101578,-57.7982094792638));
#53338=CARTESIAN_POINT('Ctrl Pts',(33.3063215665668,8.24431907939927,-57.7274741965948));
#53339=CARTESIAN_POINT('Ctrl Pts',(33.3300375594471,8.24496406860893,-57.6545752851795));
#53340=CARTESIAN_POINT('Ctrl Pts',(33.3546344753326,8.24638956625908,-57.5794018081793));
#53341=CARTESIAN_POINT('Ctrl Pts',(33.3614229390721,8.24678298709094,-57.558654799686));
#53342=CARTESIAN_POINT('Ctrl Pts',(33.3682785492559,8.24723583050548,-57.5377343596278));
#53343=CARTESIAN_POINT('Ctrl Pts',(33.3752037881199,8.24775032850502,-57.516638067781));
#53344=CARTESIAN_POINT('Ctrl Pts',(33.3821513819785,8.24826648732813,-57.4954736761183));
#53345=CARTESIAN_POINT('Ctrl Pts',(33.389166411806,8.24884449413713,-57.474140342021));
#53346=CARTESIAN_POINT('Ctrl Pts',(33.3962529902172,8.2494866177797,-57.4526306323922));
#53347=CARTESIAN_POINT('Ctrl Pts',(33.4076971023218,8.25052358294455,-57.417894612547));
#53348=CARTESIAN_POINT('Ctrl Pts',(33.4193286235789,8.25172775605007,-57.3826960849223));
#53349=CARTESIAN_POINT('Ctrl Pts',(33.4311705155945,8.25310999857074,-57.3469870633452));
#53350=CARTESIAN_POINT('Ctrl Pts',(33.4429082771928,8.25448008648889,-57.3115920452495));
#53351=CARTESIAN_POINT('Ctrl Pts',(33.4548527326506,8.25602512572448,-57.2756954318753));
#53352=CARTESIAN_POINT('Ctrl Pts',(33.4669948717588,8.25773922660508,-57.2393361990404));
#53353=CARTESIAN_POINT('Ctrl Pts',(33.4748222932729,8.25884422054318,-57.2158972449326));
#53354=CARTESIAN_POINT('Ctrl Pts',(33.4827312053234,8.26001935464201,-57.1922679924709));
#53355=CARTESIAN_POINT('Ctrl Pts',(33.4907291824969,8.26126493817209,-57.1684294560724));
#53356=CARTESIAN_POINT('Ctrl Pts',(33.5104238457025,8.26433213223717,-57.1097281200348));
#53357=CARTESIAN_POINT('Ctrl Pts',(33.530650114247,8.26782441812749,-57.0497816457331));
#53358=CARTESIAN_POINT('Ctrl Pts',(33.5514510113948,8.27174678432962,-56.9885302069414));
#53359=CARTESIAN_POINT('Ctrl Pts',(33.5536522114834,8.27216185838965,-56.9820484349517));
#53360=CARTESIAN_POINT('Ctrl Pts',(33.5558598550761,8.27258176223285,-56.9755520437706));
#53361=CARTESIAN_POINT('Ctrl Pts',(33.5580739984412,8.27300651115138,-56.9690409614721));
#53362=CARTESIAN_POINT('Ctrl Pts',(33.5598274302077,8.27334287972545,-56.9638846835561));
#53363=CARTESIAN_POINT('Ctrl Pts',(33.5615847458961,8.27368225369376,-56.958719762588));
#53364=CARTESIAN_POINT('Ctrl Pts',(33.5633416033356,8.27402377918612,-56.9535589856994));
#53365=CARTESIAN_POINT('Ctrl Pts',(33.5837469887939,8.2779904979185,-56.8936180711393));
#53366=CARTESIAN_POINT('Ctrl Pts',(33.6042412054578,8.28227489925269,-56.8337918778109));
#53367=CARTESIAN_POINT('Ctrl Pts',(33.6248563320432,8.28685556871978,-56.7740171494789));
#53368=CARTESIAN_POINT('Ctrl Pts',(33.6443100297644,8.29117816935014,-56.7176100499874));
#53369=CARTESIAN_POINT('Ctrl Pts',(33.663873298769,8.29576527135127,-56.6612431340435));
#53370=CARTESIAN_POINT('Ctrl Pts',(33.6835833024292,8.30061282476209,-56.6048470285847));
#53371=CARTESIAN_POINT('Ctrl Pts',(33.6893816449354,8.30203889121431,-56.5882562688313));
#53372=CARTESIAN_POINT('Ctrl Pts',(33.6951926237817,8.30348754214602,-56.5716632461933));
#53373=CARTESIAN_POINT('Ctrl Pts',(33.7010204123138,8.30495966895789,-56.5550572898264));
#53374=CARTESIAN_POINT('Ctrl Pts',(33.715002721784,8.30849166613824,-56.5152154836775));
#53375=CARTESIAN_POINT('Ctrl Pts',(33.7290746865241,8.31215704388324,-56.4753195088408));
#53376=CARTESIAN_POINT('Ctrl Pts',(33.74322157891,8.31595074092791,-56.4354301621671));
#53377=CARTESIAN_POINT('Ctrl Pts',(33.7581621889465,8.31995728502219,-56.3933028060662));
#53378=CARTESIAN_POINT('Ctrl Pts',(33.773186237498,8.32410693444565,-56.3511832323761));
#53379=CARTESIAN_POINT('Ctrl Pts',(33.7883319940688,8.32840148291067,-56.3089714939313));
#53380=CARTESIAN_POINT('Ctrl Pts',(33.7954479669976,8.33041920255878,-56.2891390354705));
#53381=CARTESIAN_POINT('Ctrl Pts',(33.802591452665,8.33246909818501,-56.2692844582634));
#53382=CARTESIAN_POINT('Ctrl Pts',(33.8097645416245,8.33455082052943,-56.2494026966234));
#53383=CARTESIAN_POINT('Ctrl Pts',(33.8462246713151,8.34513201742883,-56.1483455911049));
#53384=CARTESIAN_POINT('Ctrl Pts',(33.8833759461346,8.35651669070866,-56.0467964423657));
#53385=CARTESIAN_POINT('Ctrl Pts',(33.9213794241352,8.36859834249817,-55.944346058535));
#53386=CARTESIAN_POINT('Ctrl Pts',(33.9236399780667,8.36931699318198,-55.9382520210905));
#53387=CARTESIAN_POINT('Ctrl Pts',(33.9259035368344,8.370038098574,-55.9321548016935));
#53388=CARTESIAN_POINT('Ctrl Pts',(33.9281701296812,8.37076163202236,-55.9260543186707));
#53389=CARTESIAN_POINT('Ctrl Pts',(33.9573143269606,8.38006493569585,-55.8476133754845));
#53390=CARTESIAN_POINT('Ctrl Pts',(33.9869603922587,8.38976832201774,-55.7686344037265));
#53391=CARTESIAN_POINT('Ctrl Pts',(34.0171999918353,8.39974841800064,-55.6889038557678));
#53392=CARTESIAN_POINT('Ctrl Pts',(34.0281218179651,8.40335299195699,-55.6601070729322));
#53393=CARTESIAN_POINT('Ctrl Pts',(34.0391208754096,8.40699358016688,-55.6312126412986));
#53394=CARTESIAN_POINT('Ctrl Pts',(34.0502007239699,8.41066410234706,-55.6022121085287));
#53395=CARTESIAN_POINT('Ctrl Pts',(34.0643034591948,8.41533604367935,-55.565299434785));
#53396=CARTESIAN_POINT('Ctrl Pts',(34.0785184752553,8.42007191091369,-55.5282494150646));
#53397=CARTESIAN_POINT('Ctrl Pts',(34.092875808014,8.42487556703544,-55.4909786487536));
#53398=CARTESIAN_POINT('Ctrl Pts',(34.1181955193908,8.43334700031626,-55.4252502114704));
#53399=CARTESIAN_POINT('Ctrl Pts',(34.1439565202898,8.44202869183888,-55.3588378159729));
#53400=CARTESIAN_POINT('Ctrl Pts',(34.1701229500259,8.45086466932254,-55.2917559898774));
#53401=CARTESIAN_POINT('Ctrl Pts',(34.1951835073361,8.45932721168519,-55.2275092445516));
#53402=CARTESIAN_POINT('Ctrl Pts',(34.2206382490956,8.46793947463191,-55.1625911095839));
#53403=CARTESIAN_POINT('Ctrl Pts',(34.2465119704947,8.47666674763625,-55.096886514898));
#53404=CARTESIAN_POINT('Ctrl Pts',(34.2810334275061,8.48831092418124,-55.0092215707671));
#53405=CARTESIAN_POINT('Ctrl Pts',(34.316300310326,8.50016098260613,-54.9201579067433));
#53406=CARTESIAN_POINT('Ctrl Pts',(34.3523754032991,8.51211590055436,-54.8294370320581));
#53407=CARTESIAN_POINT('Ctrl Pts',(34.3580566585003,8.51399861059544,-54.8151499326029));
#53408=CARTESIAN_POINT('Ctrl Pts',(34.3637579344201,8.51588386178967,-54.8008218174869));
#53409=CARTESIAN_POINT('Ctrl Pts',(34.3694794325271,8.5177711795535,-54.7864518076394));
#53410=CARTESIAN_POINT('Ctrl Pts',(34.4062918113315,8.52991426780531,-54.6939945113097));
#53411=CARTESIAN_POINT('Ctrl Pts',(34.4429234458461,8.54180511233091,-54.6023582808303));
#53412=CARTESIAN_POINT('Ctrl Pts',(34.4793139250894,8.55331711614767,-54.5115448246281));
#53413=CARTESIAN_POINT('Ctrl Pts',(34.4859936988634,8.55543023976629,-54.4948752628174));
#53414=CARTESIAN_POINT('Ctrl Pts',(34.492665423656,8.55753061500944,-54.4782333035134));
#53415=CARTESIAN_POINT('Ctrl Pts',(34.4993288064946,8.55961746400979,-54.4616188411806));
#53416=CARTESIAN_POINT('Ctrl Pts',(34.508307513822,8.56242943007335,-54.4392313544787));
#53417=CARTESIAN_POINT('Ctrl Pts',(34.5172710772812,8.56521684015726,-54.4168937849649));
#53418=CARTESIAN_POINT('Ctrl Pts',(34.5262216330844,8.56797891631761,-54.3945976038152));
#53419=CARTESIAN_POINT('Ctrl Pts',(34.5399062564537,8.5722018911588,-54.360508677014));
#53420=CARTESIAN_POINT('Ctrl Pts',(34.5535550570989,8.57636392293325,-54.3265300154006));
#53421=CARTESIAN_POINT('Ctrl Pts',(34.5671649038471,8.5804587094149,-54.2926582644767));
#53422=CARTESIAN_POINT('Ctrl Pts',(34.6093466406989,8.59314990344738,-54.1876777080735));
#53423=CARTESIAN_POINT('Ctrl Pts',(34.6511540459079,8.60519202444507,-54.083728340169));
#53424=CARTESIAN_POINT('Ctrl Pts',(34.6927510226543,8.6164196351585,-53.9801080854673));
#53425=CARTESIAN_POINT('Ctrl Pts',(34.7070257878526,8.6202725956188,-53.9445488953207));
#53426=CARTESIAN_POINT('Ctrl Pts',(34.7212757582281,8.62402996101889,-53.9090280240373));
#53427=CARTESIAN_POINT('Ctrl Pts',(34.7355072873544,8.62768595039805,-53.8735157136822));
#53428=CARTESIAN_POINT('Ctrl Pts',(34.7609434211676,8.63422033150661,-53.810044257439));
#53429=CARTESIAN_POINT('Ctrl Pts',(34.7863201703147,8.64043513357872,-53.7465942195638));
#53430=CARTESIAN_POINT('Ctrl Pts',(34.8112855448272,8.64622252443879,-53.6839604325147));
#53431=CARTESIAN_POINT('Ctrl Pts',(34.8178852864895,8.6477524548052,-53.6674028273544));
#53432=CARTESIAN_POINT('Ctrl Pts',(34.8244563799806,8.64925272860502,-53.6509021159995));
#53433=CARTESIAN_POINT('Ctrl Pts',(34.8309925582067,8.650721840173,-53.6344726598005));
#53434=CARTESIAN_POINT('Ctrl Pts',(34.8541971497883,8.65593744671606,-53.5761451773154));
#53435=CARTESIAN_POINT('Ctrl Pts',(34.8769595552522,8.66075536322111,-53.5187196936103));
#53436=CARTESIAN_POINT('Ctrl Pts',(34.8990072868524,8.6650774614646,-53.4628834086385));
#53437=CARTESIAN_POINT('Ctrl Pts',(34.9011747086567,8.66550234916474,-53.4573943731354));
#53438=CARTESIAN_POINT('Ctrl Pts',(34.9033352418631,8.6659224793078,-53.4519206795066));
#53439=CARTESIAN_POINT('Ctrl Pts',(34.9054886396442,8.66633778125862,-53.4464629701074));
#53440=CARTESIAN_POINT('',(30.3373688833396,9.77553124130065,-64.7925772570577));
#53441=CARTESIAN_POINT('Ctrl Pts',(30.3373684825906,9.77557092417984,-64.7925605023553));
#53442=CARTESIAN_POINT('Ctrl Pts',(30.3375463229291,9.77544705826916,-64.7922628769377));
#53443=CARTESIAN_POINT('Ctrl Pts',(30.3377241674401,9.77532319428866,-64.7919652277452));
#53444=CARTESIAN_POINT('Ctrl Pts',(30.3379020161204,9.77519933220178,-64.7916675546795));
#53445=CARTESIAN_POINT('Ctrl Pts',(30.4036061558056,9.72943991559357,-64.6816956805759));
#53446=CARTESIAN_POINT('Ctrl Pts',(30.4698883800189,9.68484787112186,-64.5713024429491));
#53447=CARTESIAN_POINT('Ctrl Pts',(30.5367348270984,9.64110666805661,-64.4594875830257));
#53448=CARTESIAN_POINT('Ctrl Pts',(30.5532694353223,9.6302871901708,-64.4318299440156));
#53449=CARTESIAN_POINT('Ctrl Pts',(30.5698384647393,9.61951997556837,-64.4040851911615));
#53450=CARTESIAN_POINT('Ctrl Pts',(30.5864416055175,9.60880010688694,-64.376236554061));
#53451=CARTESIAN_POINT('Ctrl Pts',(30.6029407158524,9.59814740577976,-64.3485624084078));
#53452=CARTESIAN_POINT('Ctrl Pts',(30.6194735127258,9.58754145673769,-64.3207856723907));
#53453=CARTESIAN_POINT('Ctrl Pts',(30.6360396182955,9.57697783103276,-64.2928904738032));
#53454=CARTESIAN_POINT('Ctrl Pts',(30.6688000900593,9.55608762481185,-64.2377260380931));
#53455=CARTESIAN_POINT('Ctrl Pts',(30.7016908435539,9.53536279863202,-64.1820984392842));
#53456=CARTESIAN_POINT('Ctrl Pts',(30.7347086744899,9.51477022684478,-64.1258818683911));
#53457=CARTESIAN_POINT('Ctrl Pts',(30.7989006919381,9.47473492803825,-64.0165877386031));
#53458=CARTESIAN_POINT('Ctrl Pts',(30.8635734637805,9.43519782370463,-63.9050699203138));
#53459=CARTESIAN_POINT('Ctrl Pts',(30.9286992633925,9.39592330007792,-63.7903478022949));
#53460=CARTESIAN_POINT('Ctrl Pts',(30.9322875485719,9.39375936210095,-63.7840268714457));
#53461=CARTESIAN_POINT('Ctrl Pts',(30.9358772074505,9.39159622837222,-63.7776962036545));
#53462=CARTESIAN_POINT('Ctrl Pts',(30.9394682353198,9.38943386640271,-63.7713556428843));
#53463=CARTESIAN_POINT('Ctrl Pts',(30.9673747151068,9.37262978890998,-63.7220820818283));
#53464=CARTESIAN_POINT('Ctrl Pts',(30.9953638849514,9.35587219743963,-63.6722110687769));
#53465=CARTESIAN_POINT('Ctrl Pts',(31.0234333085263,9.33914738700648,-63.6216701776393));
#53466=CARTESIAN_POINT('Ctrl Pts',(31.0543134478064,9.32074784722863,-63.5660684032211));
#53467=CARTESIAN_POINT('Ctrl Pts',(31.0852907474618,9.30238796850476,-63.5096560444589));
#53468=CARTESIAN_POINT('Ctrl Pts',(31.1163613946637,9.28404855304618,-63.4523275077404));
#53469=CARTESIAN_POINT('Ctrl Pts',(31.1829819817661,9.24472582452293,-63.3294056790099));
#53470=CARTESIAN_POINT('Ctrl Pts',(31.2500330279944,9.20549427976786,-63.2022717921672));
#53471=CARTESIAN_POINT('Ctrl Pts',(31.3174662640762,9.16620743702038,-63.0699186138175));
#53472=CARTESIAN_POINT('Ctrl Pts',(31.356885099242,9.14324188370522,-62.9925501168538));
#53473=CARTESIAN_POINT('Ctrl Pts',(31.3964342454244,9.12025823995894,-62.9133979272066));
#53474=CARTESIAN_POINT('Ctrl Pts',(31.436099984031,9.09723452561081,-62.8322600716));
#53475=CARTESIAN_POINT('Ctrl Pts',(31.4465581059631,9.09116417824198,-62.8108675646896));
#53476=CARTESIAN_POINT('Ctrl Pts',(31.4570222813784,9.08509167798631,-62.7893392930934));
#53477=CARTESIAN_POINT('Ctrl Pts',(31.4674908820943,9.07901874264532,-62.7676786570229));
#53478=CARTESIAN_POINT('Ctrl Pts',(31.5209901089275,9.047983329779,-62.6569831291357));
#53479=CARTESIAN_POINT('Ctrl Pts',(31.574607074813,9.01693952807107,-62.5428290251401));
#53480=CARTESIAN_POINT('Ctrl Pts',(31.6281106237607,8.98608871872255,-62.4256639577479));
#53481=CARTESIAN_POINT('Ctrl Pts',(31.6807944160655,8.95571059121297,-62.3102940393545));
#53482=CARTESIAN_POINT('Ctrl Pts',(31.7333686664999,8.92551918584558,-62.1920045938983));
#53483=CARTESIAN_POINT('Ctrl Pts',(31.7855822717626,8.89567426032026,-62.071244707503));
#53484=CARTESIAN_POINT('Ctrl Pts',(31.8368240386367,8.86638483070797,-61.9527324937746));
#53485=CARTESIAN_POINT('Ctrl Pts',(31.8877185600007,8.83742885512422,-61.8318400901663));
#53486=CARTESIAN_POINT('Ctrl Pts',(31.9379950259541,8.80893211037967,-61.7090524023681));
#53487=CARTESIAN_POINT('Ctrl Pts',(31.9905182826746,8.779161882669,-61.5807774903181));
#53488=CARTESIAN_POINT('Ctrl Pts',(32.0423671155747,8.74989268183046,-61.4504342096747));
#53489=CARTESIAN_POINT('Ctrl Pts',(32.0931938750543,8.72124186168149,-61.3186103997138));
#53490=CARTESIAN_POINT('Ctrl Pts',(32.1224075483681,8.70477424288037,-61.2428420887175));
#53491=CARTESIAN_POINT('Ctrl Pts',(32.1512828341325,8.68851045659444,-61.166585309833));
#53492=CARTESIAN_POINT('Ctrl Pts',(32.1797484643676,8.67246943556838,-61.0899561252136));
#53493=CARTESIAN_POINT('Ctrl Pts',(32.2341117036637,8.64183453104005,-60.9436108426356));
#53494=CARTESIAN_POINT('Ctrl Pts',(32.2870749287235,8.61198816189768,-60.7957628561251));
#53495=CARTESIAN_POINT('Ctrl Pts',(32.3387992780698,8.58324303503906,-60.6478476683524));
#53496=CARTESIAN_POINT('Ctrl Pts',(32.3944398342923,8.55232152771585,-60.4887333744958));
#53497=CARTESIAN_POINT('Ctrl Pts',(32.4486449703774,8.52267390784803,-60.3295428623252));
#53498=CARTESIAN_POINT('Ctrl Pts',(32.501630510655,8.49457301465818,-60.1718098794048));
#53499=CARTESIAN_POINT('Ctrl Pts',(32.5046546997238,8.49296913530613,-60.1628071522412));
#53500=CARTESIAN_POINT('Ctrl Pts',(32.5076749214702,8.49137028732541,-60.1538091845707));
#53501=CARTESIAN_POINT('Ctrl Pts',(32.5106912185181,8.48977651907442,-60.1448162661682));
#53502=CARTESIAN_POINT('Ctrl Pts',(32.5352852545509,8.47678138193424,-60.0714905440266));
#53503=CARTESIAN_POINT('Ctrl Pts',(32.5596149213573,8.46414266611182,-59.998591329611));
#53504=CARTESIAN_POINT('Ctrl Pts',(32.5835883165298,8.45183872019133,-59.9261096446501));
#53505=CARTESIAN_POINT('Ctrl Pts',(32.6107857864825,8.43788007157003,-59.8438802217977));
#53506=CARTESIAN_POINT('Ctrl Pts',(32.6375244536277,8.42435304402482,-59.762189720735));
#53507=CARTESIAN_POINT('Ctrl Pts',(32.6636616266459,8.41129914680092,-59.6814250560713));
#53508=CARTESIAN_POINT('Ctrl Pts',(32.6766561521125,8.40480918708737,-59.6412715746278));
#53509=CARTESIAN_POINT('Ctrl Pts',(32.6894507451753,8.39870830073878,-59.6027697852629));
#53510=CARTESIAN_POINT('Ctrl Pts',(32.7022892380683,8.39268048839557,-59.5642015698746));
#53511=CARTESIAN_POINT('Ctrl Pts',(32.7118904854834,8.38817259808776,-59.5353583885611));
#53512=CARTESIAN_POINT('Ctrl Pts',(32.7215159782231,8.38370675703068,-59.5064820798043));
#53513=CARTESIAN_POINT('Ctrl Pts',(32.731266476481,8.37912370098253,-59.4766551710175));
#53514=CARTESIAN_POINT('Ctrl Pts',(32.738674467287,8.37564170076368,-59.4539940248668));
#53515=CARTESIAN_POINT('Ctrl Pts',(32.7461545082956,8.37209237863037,-59.430785169056));
#53516=CARTESIAN_POINT('Ctrl Pts',(32.753749108309,8.3684033190236,-59.4065921797029));
#53517=CARTESIAN_POINT('Ctrl Pts',(32.7561506241305,8.36723678819956,-59.3989420274109));
#53518=CARTESIAN_POINT('Ctrl Pts',(32.7585635847051,8.36605624554138,-59.3911931144473));
#53519=CARTESIAN_POINT('Ctrl Pts',(32.7609893066747,8.36485926220333,-59.3833304692864));
#53520=CARTESIAN_POINT('Ctrl Pts',(32.7654154513653,8.36267516134063,-59.3689837281638));
#53521=CARTESIAN_POINT('Ctrl Pts',(32.7698841725407,8.36043567928045,-59.3542547618505));
#53522=CARTESIAN_POINT('Ctrl Pts',(32.7743993505077,8.35815864159974,-59.3392303200884));
#53523=CARTESIAN_POINT('Ctrl Pts',(32.7786170436054,8.35603162774136,-59.3251957715548));
#53524=CARTESIAN_POINT('Ctrl Pts',(32.7828752838157,8.3538717471765,-59.3109028270378));
#53525=CARTESIAN_POINT('Ctrl Pts',(32.7871761742764,8.35170090050936,-59.2964627260597));
#53526=CARTESIAN_POINT('Ctrl Pts',(32.7912324851766,8.34965350379485,-59.282843793066));
#53527=CARTESIAN_POINT('Ctrl Pts',(32.7953267422896,8.34759626861694,-59.2690934580539));
#53528=CARTESIAN_POINT('Ctrl Pts',(32.7994596002972,8.34555561824614,-59.2553498996653));
#53529=CARTESIAN_POINT('Ctrl Pts',(32.8033041258697,8.34365733562412,-59.2425651725866));
#53530=CARTESIAN_POINT('Ctrl Pts',(32.8071820576321,8.34177336230744,-59.229786038189));
#53531=CARTESIAN_POINT('Ctrl Pts',(32.8110928545661,8.33993297119414,-59.217168835316));
#53532=CARTESIAN_POINT('Ctrl Pts',(32.8121810991747,8.33942085160815,-59.2136578877435));
#53533=CARTESIAN_POINT('Ctrl Pts',(32.8132718816812,8.33891215942377,-59.2101597778347));
#53534=CARTESIAN_POINT('Ctrl Pts',(32.8143651736023,8.33840765419576,-59.206678606258));
#53535=CARTESIAN_POINT('Ctrl Pts',(32.8146919155016,8.33825687745151,-59.2056382211691));
#53536=CARTESIAN_POINT('Ctrl Pts',(32.8150189113244,8.33810590712252,-59.2045955534805));
#53537=CARTESIAN_POINT('Ctrl Pts',(32.8153461624519,8.33795474232361,-59.2035505847575));
#53538=CARTESIAN_POINT('',(27.8093579489698,12.8426393692443,-70.6502216958336));
#53539=CARTESIAN_POINT('Ctrl Pts',(27.8093579489706,12.8426393697467,-70.6502216955679));
#53540=CARTESIAN_POINT('Ctrl Pts',(28.1531837700217,12.2318062816667,-69.496432085362));
#53541=CARTESIAN_POINT('Ctrl Pts',(28.9080975096274,11.0141698218073,-67.3154640104755));
#53542=CARTESIAN_POINT('Ctrl Pts',(29.7727535124309,10.1579126475408,-65.7117945504243));
#53543=CARTESIAN_POINT('Ctrl Pts',(30.3373688833396,9.77553124130065,-64.7925772570577));
#53544=CARTESIAN_POINT('',(25.9580275654173,16.0437450369841,-76.6642789908813));
#53545=CARTESIAN_POINT('Ctrl Pts',(25.9580275654173,16.0437450369841,-76.6642789908813));
#53546=CARTESIAN_POINT('Ctrl Pts',(26.6559762479054,14.9591966918103,-74.6266658726109));
#53547=CARTESIAN_POINT('Ctrl Pts',(27.2836007288677,13.7527661001403,-72.3692972947473));
#53548=CARTESIAN_POINT('Ctrl Pts',(27.8093579489706,12.8426393697467,-70.6502216955679));
#53549=CARTESIAN_POINT('',(25.7066762097982,16.4237782457055,-77.3782777057259));
#53550=CARTESIAN_POINT('Ctrl Pts',(25.7066762161377,16.4237824971517,-77.3782754451113));
#53551=CARTESIAN_POINT('Ctrl Pts',(25.7493317432104,16.361108340562,-77.2605263204144));
#53552=CARTESIAN_POINT('Ctrl Pts',(25.7914521798399,16.2982559066625,-77.1424435089061));
#53553=CARTESIAN_POINT('Ctrl Pts',(25.8751675367156,16.1716233431714,-76.9045368904255));
#53554=CARTESIAN_POINT('Ctrl Pts',(25.9168664608344,16.1076591547755,-76.7843673153015));
#53555=CARTESIAN_POINT('Ctrl Pts',(25.9580275563336,16.0437394275245,-76.6642819734839));
#53556=CARTESIAN_POINT('',(20.8066780834701,16.2071460528291,-76.9702782129913));
#53557=CARTESIAN_POINT('Ctrl Pts',(20.8066780834701,16.2071460528291,-76.9702782129913));
#53558=CARTESIAN_POINT('Ctrl Pts',(20.7814199439412,16.2902997214971,-77.1267023814477));
#53559=CARTESIAN_POINT('Ctrl Pts',(20.7510970195006,16.462201386336,-77.4500437795191));
#53560=CARTESIAN_POINT('Ctrl Pts',(20.8055482815057,16.7173317962075,-77.9297992830641));
#53561=CARTESIAN_POINT('Ctrl Pts',(21.0009366844085,16.9521786769222,-78.3712110483715));
#53562=CARTESIAN_POINT('Ctrl Pts',(21.2717280412466,17.0949090521466,-78.6392688130115));
#53563=CARTESIAN_POINT('Ctrl Pts',(21.4878400853508,17.1684263103318,-78.777240406493));
#53564=CARTESIAN_POINT('Ctrl Pts',(21.6407851560214,17.2127260997074,-78.8603513323804));
#53565=CARTESIAN_POINT('Ctrl Pts',(21.9258991389736,17.2758277200359,-78.9786607564294));
#53566=CARTESIAN_POINT('Ctrl Pts',(22.3594194342618,17.3310653318226,-79.0820453922927));
#53567=CARTESIAN_POINT('Ctrl Pts',(22.9124146240747,17.3542009086611,-79.1251165545024));
#53568=CARTESIAN_POINT('Ctrl Pts',(23.5418771977656,17.3391957004687,-79.0966974225329));
#53569=CARTESIAN_POINT('Ctrl Pts',(24.2749365963644,17.2629716950359,-78.9536848243009));
#53570=CARTESIAN_POINT('Ctrl Pts',(24.9206297891638,17.1086649231884,-78.6644707327587));
#53571=CARTESIAN_POINT('Ctrl Pts',(25.3704424188049,16.8998240213439,-78.2726976801559));
#53572=CARTESIAN_POINT('Ctrl Pts',(25.6207437197086,16.674198124308,-77.8490131748246));
#53573=CARTESIAN_POINT('Ctrl Pts',(25.6912026729945,16.5078943516558,-77.5364389821151));
#53574=CARTESIAN_POINT('Ctrl Pts',(25.7066762066284,16.4237761199824,-77.3782788360332));
#53575=CARTESIAN_POINT('',(21.0403876071431,16.0446209665478,-76.6642753537542));
#53576=CARTESIAN_POINT('Ctrl Pts',(21.0403876071431,16.0446209665478,-76.6642753537542));
#53577=CARTESIAN_POINT('Ctrl Pts',(21.00240573693,16.0723625448958,-76.7165035747521));
#53578=CARTESIAN_POINT('Ctrl Pts',(20.9637701717481,16.0999221085431,-76.7683905060148));
#53579=CARTESIAN_POINT('Ctrl Pts',(20.8858789219625,16.1540987363042,-76.8703926297541));
#53580=CARTESIAN_POINT('Ctrl Pts',(20.8466178752764,16.1807440064858,-76.9205608786289));
#53581=CARTESIAN_POINT('Ctrl Pts',(20.8066780817163,16.2071484214984,-76.9702769535722));
#53582=CARTESIAN_POINT('',(23.6739538950181,12.8462304042226,-70.6468064576015));
#53583=CARTESIAN_POINT('Ctrl Pts',(23.6739538950114,12.8462304034107,-70.6468064580614));
#53584=CARTESIAN_POINT('Ctrl Pts',(23.6310070416931,12.9226146262459,-70.7905530926008));
#53585=CARTESIAN_POINT('Ctrl Pts',(23.5868595342126,12.9994632040654,-70.9351540957691));
#53586=CARTESIAN_POINT('Ctrl Pts',(23.4968949910939,13.1529431996464,-71.2239148776459));
#53587=CARTESIAN_POINT('Ctrl Pts',(23.4510453066928,13.2296432218887,-71.368204417614));
#53588=CARTESIAN_POINT('Ctrl Pts',(23.3130966014547,13.4560967906469,-71.7941829319882));
#53589=CARTESIAN_POINT('Ctrl Pts',(23.2147099938374,13.6120649244949,-72.0875323254961));
#53590=CARTESIAN_POINT('Ctrl Pts',(22.9103990595176,14.0734231098319,-72.9552509912363));
#53591=CARTESIAN_POINT('Ctrl Pts',(22.6919329352605,14.3771016959961,-73.5263966705118));
#53592=CARTESIAN_POINT('Ctrl Pts',(22.0400659372768,15.1823811459668,-75.0412727227511));
#53593=CARTESIAN_POINT('Ctrl Pts',(21.5785607485871,15.6515432869189,-75.9242400324668));
#53594=CARTESIAN_POINT('Ctrl Pts',(21.0403876071432,16.0446209665478,-76.6642753537542));
#53595=CARTESIAN_POINT('',(24.8344045918158,9.66888145222939,-64.6543282396439));
#53596=CARTESIAN_POINT('Ctrl Pts',(24.8344045929607,9.66888120903035,-64.6543283644958));
#53597=CARTESIAN_POINT('Ctrl Pts',(24.8303501358965,9.70941951662452,-64.73332914588));
#53598=CARTESIAN_POINT('Ctrl Pts',(24.8258802785889,9.74917832575716,-64.8106105339471));
#53599=CARTESIAN_POINT('Ctrl Pts',(24.8209763204938,9.78866534954903,-64.8871863689394));
#53600=CARTESIAN_POINT('Ctrl Pts',(24.8199646022781,9.79681177749121,-64.9029844580829));
#53601=CARTESIAN_POINT('Ctrl Pts',(24.8189342458198,9.80494663665857,-64.918752444668));
#53602=CARTESIAN_POINT('Ctrl Pts',(24.8178848358697,9.81307438905661,-64.9344991318275));
#53603=CARTESIAN_POINT('Ctrl Pts',(24.8155682503962,9.83101650322885,-64.9692601389317));
#53604=CARTESIAN_POINT('Ctrl Pts',(24.8131590265581,9.84892467935145,-65.0039180758427));
#53605=CARTESIAN_POINT('Ctrl Pts',(24.810645719863,9.8668831345148,-65.0386377886802));
#53606=CARTESIAN_POINT('Ctrl Pts',(24.8028781675356,9.92238501197181,-65.1459415199712));
#53607=CARTESIAN_POINT('Ctrl Pts',(24.7941090477931,9.97836864578574,-65.2538384783798));
#53608=CARTESIAN_POINT('Ctrl Pts',(24.7843654791308,10.0345257433411,-65.3617487507159));
#53609=CARTESIAN_POINT('Ctrl Pts',(24.7826546343078,10.0443862044268,-65.3806964009229));
#53610=CARTESIAN_POINT('Ctrl Pts',(24.7809138740523,10.0542519990379,-65.3996444807811));
#53611=CARTESIAN_POINT('Ctrl Pts',(24.7791435094063,10.0641214352372,-65.4185898648104));
#53612=CARTESIAN_POINT('Ctrl Pts',(24.7584167318918,10.1796691608203,-65.6403954462719));
#53613=CARTESIAN_POINT('Ctrl Pts',(24.7336388591999,10.2957131317301,-65.8618169276568));
#53614=CARTESIAN_POINT('Ctrl Pts',(24.7046949084052,10.4130044997939,-66.0845375417376));
#53615=CARTESIAN_POINT('Ctrl Pts',(24.7008996526852,10.4283842500809,-66.1137416296845));
#53616=CARTESIAN_POINT('Ctrl Pts',(24.6970326774042,10.4437854596428,-66.1429681011285));
#53617=CARTESIAN_POINT('Ctrl Pts',(24.6930936396352,10.4592098397787,-66.1722208064147));
#53618=CARTESIAN_POINT('Ctrl Pts',(24.6625714917577,10.5787276608925,-66.3988892084302));
#53619=CARTESIAN_POINT('Ctrl Pts',(24.6277268042723,10.6996122801159,-66.627083756415));
#53620=CARTESIAN_POINT('Ctrl Pts',(24.5885038182621,10.822311194009,-66.8579348550256));
#53621=CARTESIAN_POINT('Ctrl Pts',(24.5727743595823,10.8715167158845,-66.9505122741914));
#53622=CARTESIAN_POINT('Ctrl Pts',(24.5563411231441,10.9210138128591,-67.0435165697199));
#53623=CARTESIAN_POINT('Ctrl Pts',(24.539201945762,10.9708303881966,-67.137018880739));
#53624=CARTESIAN_POINT('Ctrl Pts',(24.5319183453243,10.9920008342364,-67.1767543626868));
#53625=CARTESIAN_POINT('Ctrl Pts',(24.5245072651196,11.0132289672869,-67.2165797658144));
#53626=CARTESIAN_POINT('Ctrl Pts',(24.5169724822948,11.0345099947928,-67.2564873906126));
#53627=CARTESIAN_POINT('Ctrl Pts',(24.4946558110608,11.0975405698481,-67.3746865959579));
#53628=CARTESIAN_POINT('Ctrl Pts',(24.4712375373057,11.1610700850315,-67.4937103111689));
#53629=CARTESIAN_POINT('Ctrl Pts',(24.4467384852227,11.2251548137537,-67.6136954338559));
#53630=CARTESIAN_POINT('Ctrl Pts',(24.400804523427,11.3453090740422,-67.8386589150087));
#53631=CARTESIAN_POINT('Ctrl Pts',(24.3512314195594,11.4670167961932,-68.0661686704969));
#53632=CARTESIAN_POINT('Ctrl Pts',(24.2986050952819,11.5895147520019,-68.2950168825741));
#53633=CARTESIAN_POINT('Ctrl Pts',(24.2194550792226,11.773751734208,-68.639204699408));
#53634=CARTESIAN_POINT('Ctrl Pts',(24.1333995603996,11.9597735798187,-68.986415264212));
#53635=CARTESIAN_POINT('Ctrl Pts',(24.0424408348367,12.1450384042839,-69.3326474110774));
#53636=CARTESIAN_POINT('Ctrl Pts',(23.9740416340358,12.2843539658368,-69.5930072829929));
#53637=CARTESIAN_POINT('Ctrl Pts',(23.9028690387089,12.423244236739,-69.8528192706222));
#53638=CARTESIAN_POINT('Ctrl Pts',(23.8297837772451,12.5606256545873,-70.1103770138851));
#53639=CARTESIAN_POINT('Ctrl Pts',(23.8169956343545,12.5846640607826,-70.1554433536292));
#53640=CARTESIAN_POINT('Ctrl Pts',(23.8041489695695,12.6086562304002,-70.200440596941));
#53641=CARTESIAN_POINT('Ctrl Pts',(23.7912484243222,12.6325963398636,-70.245359562372));
#53642=CARTESIAN_POINT('Ctrl Pts',(23.7525659360645,12.7043811354252,-70.3800497882137));
#53643=CARTESIAN_POINT('Ctrl Pts',(23.7133985611913,12.7756821419663,-70.5140424729259));
#53644=CARTESIAN_POINT('Ctrl Pts',(23.6739538950215,12.8462304046968,-70.6468064573353));
#53645=CARTESIAN_POINT('',(24.4986797976544,6.71047053280757,-58.7794556342451));
#53646=CARTESIAN_POINT('Ctrl Pts',(24.4986797976544,6.71047053280757,-58.7794556342451));
#53647=CARTESIAN_POINT('Ctrl Pts',(24.6381921878201,7.28402736458032,-60.1192331620747));
#53648=CARTESIAN_POINT('Ctrl Pts',(24.8491604058793,8.33135979595778,-62.1002014923607));
#53649=CARTESIAN_POINT('Ctrl Pts',(24.8726304141327,9.27135230412159,-63.8796298265301));
#53650=CARTESIAN_POINT('Ctrl Pts',(24.8344045906688,9.66888169588101,-64.6543281145597));
#53651=CARTESIAN_POINT('',(23.8104975525172,4.71983210132197,-53.1013215771875));
#53652=CARTESIAN_POINT('Ctrl Pts',(23.8104975547445,4.71983210069848,-53.1013215768221));
#53653=CARTESIAN_POINT('Ctrl Pts',(23.9337205829163,4.84404524606257,-53.6404826359787));
#53654=CARTESIAN_POINT('Ctrl Pts',(24.0199474940819,4.99885485594887,-54.1957970613934));
#53655=CARTESIAN_POINT('Ctrl Pts',(24.1600565300499,5.3462915437671,-55.3009470158922));
#53656=CARTESIAN_POINT('Ctrl Pts',(24.2146562929896,5.54550925178696,-55.8683918927849));
#53657=CARTESIAN_POINT('Ctrl Pts',(24.2888535333137,5.82844014520507,-56.6195254124793));
#53658=CARTESIAN_POINT('Ctrl Pts',(24.3080077308712,5.9038243509016,-56.8149835325362));
#53659=CARTESIAN_POINT('Ctrl Pts',(24.3413690767299,6.03831715020874,-57.1570027496823));
#53660=CARTESIAN_POINT('Ctrl Pts',(24.3556625645275,6.09700551911714,-57.304102153857));
#53661=CARTESIAN_POINT('Ctrl Pts',(24.3913918117882,6.24581854559107,-57.672515111601));
#53662=CARTESIAN_POINT('Ctrl Pts',(24.4128016567203,6.33691449783787,-57.8939185828946));
#53663=CARTESIAN_POINT('Ctrl Pts',(24.4449941284588,6.4753019929398,-58.2255323486235));
#53664=CARTESIAN_POINT('Ctrl Pts',(24.4557841965576,6.52189313240607,-58.3363874846924));
#53665=CARTESIAN_POINT('Ctrl Pts',(24.471911122741,6.59208959264157,-58.5024114063079));
#53666=CARTESIAN_POINT('Ctrl Pts',(24.4772911301109,6.61560292274562,-58.5578573126726));
#53667=CARTESIAN_POINT('Ctrl Pts',(24.4893061751536,6.66838686278425,-58.6819862965278));
#53668=CARTESIAN_POINT('Ctrl Pts',(24.4949961722313,6.69358513202795,-58.7410135943171));
#53669=CARTESIAN_POINT('Ctrl Pts',(24.4987083708446,6.71008931346543,-58.7796158705648));
#53670=CARTESIAN_POINT('',(18.0802312907388,4.08541520334038,-47.3815173795873));
#53671=CARTESIAN_POINT('Ctrl Pts',(18.0802313198441,4.08541519315892,-47.3815173754911));
#53672=CARTESIAN_POINT('Ctrl Pts',(18.0818954942396,4.08545546640632,-47.3820362045046));
#53673=CARTESIAN_POINT('Ctrl Pts',(18.0835590772247,4.08549575181441,-47.3825548949369));
#53674=CARTESIAN_POINT('Ctrl Pts',(18.0852220694125,4.08553604937883,-47.3830734479269));
#53675=CARTESIAN_POINT('Ctrl Pts',(18.1678282741835,4.0875377598395,-47.4088316534028));
#53676=CARTESIAN_POINT('Ctrl Pts',(18.248970713161,4.08957534677303,-47.4347714589022));
#53677=CARTESIAN_POINT('Ctrl Pts',(18.3287266556004,4.09163932528598,-47.4608648300448));
#53678=CARTESIAN_POINT('Ctrl Pts',(18.4252175502284,4.09413638227154,-47.4924332956463));
#53679=CARTESIAN_POINT('Ctrl Pts',(18.5196790922603,4.09667205963219,-47.5242270828985));
#53680=CARTESIAN_POINT('Ctrl Pts',(18.6122436622419,4.09923712348749,-47.5562764970958));
#53681=CARTESIAN_POINT('Ctrl Pts',(18.7731727968583,4.10369664300506,-47.6119963528975));
#53682=CARTESIAN_POINT('Ctrl Pts',(18.9283690860628,4.10824464966644,-47.6684960624441));
#53683=CARTESIAN_POINT('Ctrl Pts',(19.0785058320582,4.1128615144897,-47.7261539453444));
#53684=CARTESIAN_POINT('Ctrl Pts',(19.0996497598848,4.113511712787,-47.7342739702364));
#53685=CARTESIAN_POINT('Ctrl Pts',(19.1206933073599,4.11416329813255,-47.7424169078168));
#53686=CARTESIAN_POINT('Ctrl Pts',(19.1416383266119,4.11481622511397,-47.7505835985577));
#53687=CARTESIAN_POINT('Ctrl Pts',(19.2054083250036,4.11680415131512,-47.7754482142997));
#53688=CARTESIAN_POINT('Ctrl Pts',(19.2682650139487,4.11880450099507,-47.8005329842545));
#53689=CARTESIAN_POINT('Ctrl Pts',(19.3302603531123,4.12082313687603,-47.8259594010279));
#53690=CARTESIAN_POINT('Ctrl Pts',(19.476568492363,4.12558708951427,-47.8859653914153));
#53691=CARTESIAN_POINT('Ctrl Pts',(19.618073824103,4.13041529144838,-47.9473890021447));
#53692=CARTESIAN_POINT('Ctrl Pts',(19.7546645730943,4.1352530499461,-48.0100920493126));
#53693=CARTESIAN_POINT('Ctrl Pts',(19.7902338162518,4.13651283810608,-48.0264203874168));
#53694=CARTESIAN_POINT('Ctrl Pts',(19.8254696213882,4.13777331865906,-48.0428356976964));
#53695=CARTESIAN_POINT('Ctrl Pts',(19.8603696738727,4.13903362990627,-48.0593360018436));
#53696=CARTESIAN_POINT('Ctrl Pts',(19.907297533467,4.14072828951404,-48.0815229013225));
#53697=CARTESIAN_POINT('Ctrl Pts',(19.9536183372731,4.14242260338841,-48.1038634250931));
#53698=CARTESIAN_POINT('Ctrl Pts',(19.9993252666987,4.14411462066421,-48.1263504155863));
#53699=CARTESIAN_POINT('Ctrl Pts',(20.1283290996858,4.14889019226356,-48.1898179904686));
#53700=CARTESIAN_POINT('Ctrl Pts',(20.2524434881266,4.15364525445708,-48.2544528349789));
#53701=CARTESIAN_POINT('Ctrl Pts',(20.3715073556093,4.15834181382186,-48.319863761312));
#53702=CARTESIAN_POINT('Ctrl Pts',(20.5478383713987,4.1652973167886,-48.4167359302404));
#53703=CARTESIAN_POINT('Ctrl Pts',(20.7131238675307,4.17214241143718,-48.5155240818662));
#53704=CARTESIAN_POINT('Ctrl Pts',(20.8716066057245,4.17909356110718,-48.6185955718901));
#53705=CARTESIAN_POINT('Ctrl Pts',(20.9945301288674,4.18448506189186,-48.6985406235325));
#53706=CARTESIAN_POINT('Ctrl Pts',(21.1133631600208,4.18994138765124,-48.7810661753323));
#53707=CARTESIAN_POINT('Ctrl Pts',(21.2300788101569,4.19557937729348,-48.8672621022061));
#53708=CARTESIAN_POINT('Ctrl Pts',(21.2355169545766,4.19584206873096,-48.8712782379872));
#53709=CARTESIAN_POINT('Ctrl Pts',(21.2409504287901,4.19610515370641,-48.8753022806401));
#53710=CARTESIAN_POINT('Ctrl Pts',(21.2463793779124,4.19636866023458,-48.8793345271448));
#53711=CARTESIAN_POINT('Ctrl Pts',(21.3426159920706,4.20103972557494,-48.9508124029394));
#53712=CARTESIAN_POINT('Ctrl Pts',(21.4374324925893,4.20584148619805,-49.0248706969702));
#53713=CARTESIAN_POINT('Ctrl Pts',(21.5316270036835,4.21094199052955,-49.1031856542045));
#53714=CARTESIAN_POINT('Ctrl Pts',(21.6124142391004,4.21531650916537,-49.1703535689083));
#53715=CARTESIAN_POINT('Ctrl Pts',(21.6927443752873,4.21991037614473,-49.2406526714573));
#53716=CARTESIAN_POINT('Ctrl Pts',(21.7731004780744,4.22484894017138,-49.3151172586566));
#53717=CARTESIAN_POINT('Ctrl Pts',(21.8478383719207,4.22944221760988,-49.3843755504401));
#53718=CARTESIAN_POINT('Ctrl Pts',(21.9225992369863,4.23433303916604,-49.457237390789));
#53719=CARTESIAN_POINT('Ctrl Pts',(21.9977460885454,4.2396476973278,-49.5345114605038));
#53720=CARTESIAN_POINT('Ctrl Pts',(22.0033950397209,4.24004721166336,-49.5403203192636));
#53721=CARTESIAN_POINT('Ctrl Pts',(22.0090461570274,4.24044913664175,-49.5461540984415));
#53722=CARTESIAN_POINT('Ctrl Pts',(22.0146995869572,4.24085353401629,-49.5520131353011));
#53723=CARTESIAN_POINT('Ctrl Pts',(22.0940464373028,4.24652931992959,-49.6342457138667));
#53724=CARTESIAN_POINT('Ctrl Pts',(22.1738759302386,4.25269005891086,-49.721482999791));
#53725=CARTESIAN_POINT('Ctrl Pts',(22.2532325274327,4.25945526922204,-49.8134791920094));
#53726=CARTESIAN_POINT('Ctrl Pts',(22.3314807570317,4.26612599035213,-49.9041904803643));
#53727=CARTESIAN_POINT('Ctrl Pts',(22.4092680991043,4.27338434916336,-49.9995279779554));
#53728=CARTESIAN_POINT('Ctrl Pts',(22.4856729607389,4.28139444099833,-50.0992589162882));
#53729=CARTESIAN_POINT('Ctrl Pts',(22.5459313021454,4.28771177262047,-50.1779138709897));
#53730=CARTESIAN_POINT('Ctrl Pts',(22.6053293198368,4.29449772547797,-50.2593015052972));
#53731=CARTESIAN_POINT('Ctrl Pts',(22.663420454943,4.30185445637358,-50.3433131260172));
#53732=CARTESIAN_POINT('Ctrl Pts',(22.6811953577698,4.30410549134739,-50.3690192581471));
#53733=CARTESIAN_POINT('Ctrl Pts',(22.6988479689518,4.30641009737276,-50.3949711131632));
#53734=CARTESIAN_POINT('Ctrl Pts',(22.7163656995239,4.3087714756635,-50.4211654372162));
#53735=CARTESIAN_POINT('Ctrl Pts',(22.7378417722252,4.31166643580909,-50.4532786841583));
#53736=CARTESIAN_POINT('Ctrl Pts',(22.7591151053141,4.31464672184621,-50.4857563551764));
#53737=CARTESIAN_POINT('Ctrl Pts',(22.7801631127034,4.3177186863129,-50.5185925879126));
#53738=CARTESIAN_POINT('Ctrl Pts',(22.8488611872628,4.32774519571459,-50.6257659617633));
#53739=CARTESIAN_POINT('Ctrl Pts',(22.9151916406563,4.33874940122539,-50.7367729700415));
#53740=CARTESIAN_POINT('Ctrl Pts',(22.9788702095239,4.35089642274516,-50.8509037331451));
#53741=CARTESIAN_POINT('Ctrl Pts',(23.039777833928,4.36251487205255,-50.9600681471023));
#53742=CARTESIAN_POINT('Ctrl Pts',(23.098259047567,4.37517975057679,-51.0720902612061));
#53743=CARTESIAN_POINT('Ctrl Pts',(23.1541059170705,4.38902878270128,-51.1863693014867));
#53744=CARTESIAN_POINT('Ctrl Pts',(23.2079534667054,4.40238201899452,-51.2965571481546));
#53745=CARTESIAN_POINT('Ctrl Pts',(23.2593519356011,4.41683676555948,-51.4088432548648));
#53746=CARTESIAN_POINT('Ctrl Pts',(23.3081556564332,4.43249913743182,-51.5227089775153));
#53747=CARTESIAN_POINT('Ctrl Pts',(23.3388595793072,4.44235281763886,-51.5943454082353));
#53748=CARTESIAN_POINT('Ctrl Pts',(23.3685373195835,4.45268409619484,-51.6666074631411));
#53749=CARTESIAN_POINT('Ctrl Pts',(23.3971609632618,4.46351416843441,-51.7393700251083));
#53750=CARTESIAN_POINT('Ctrl Pts',(23.3979634190634,4.46381778646427,-51.7414099030724));
#53751=CARTESIAN_POINT('Ctrl Pts',(23.3987650360467,4.46412179584896,-51.7434501719335));
#53752=CARTESIAN_POINT('Ctrl Pts',(23.3995658157371,4.46442619750041,-51.7454908323607));
#53753=CARTESIAN_POINT('Ctrl Pts',(23.456663235734,4.4861307301565,-51.8909945793684));
#53754=CARTESIAN_POINT('Ctrl Pts',(23.5095017668692,4.5098262849802,-52.0384892149187));
#53755=CARTESIAN_POINT('Ctrl Pts',(23.5586490724152,4.53585951374875,-52.1882628922863));
#53756=CARTESIAN_POINT('Ctrl Pts',(23.6069335827223,4.5614357216169,-52.3354072491998));
#53757=CARTESIAN_POINT('Ctrl Pts',(23.6516553829564,4.58926716144762,-52.4847514954688));
#53758=CARTESIAN_POINT('Ctrl Pts',(23.6933757118896,4.61973038249599,-52.6365651937523));
#53759=CARTESIAN_POINT('Ctrl Pts',(23.7308930784603,4.64712469745508,-52.7730849747459));
#53760=CARTESIAN_POINT('Ctrl Pts',(23.7659833400795,4.67664726218901,-52.9116016648842));
#53761=CARTESIAN_POINT('Ctrl Pts',(23.7990721375966,4.70861665137786,-53.0523078155129));
#53762=CARTESIAN_POINT('Ctrl Pts',(23.8027789801418,4.71219808983686,-53.068070719718));
#53763=CARTESIAN_POINT('Ctrl Pts',(23.8064607237595,4.71581028662781,-53.0838610985039));
#53764=CARTESIAN_POINT('Ctrl Pts',(23.8101179823112,4.7194537290064,-53.0996792201637));
#53765=CARTESIAN_POINT('Ctrl Pts',(23.8102445371179,4.71957980572192,-53.100226586258));
#53766=CARTESIAN_POINT('Ctrl Pts',(23.8103710590392,4.71970592969668,-53.1007740390327));
#53767=CARTESIAN_POINT('Ctrl Pts',(23.810497548099,4.71983210089637,-53.1013215783063));
#53768=CARTESIAN_POINT('',(1.31624832366244E-14,4.0543744617278,-45.4831027428904));
#53769=CARTESIAN_POINT('Ctrl Pts',(3.43297346105942E-9,4.05427777602882,
-45.4831012288709));
#53770=CARTESIAN_POINT('Ctrl Pts',(6.05186862449095E-5,4.05427775975267,
-45.4831024054858));
#53771=CARTESIAN_POINT('Ctrl Pts',(0.000121034596136508,4.05427774347302,
-45.4831035821241));
#53772=CARTESIAN_POINT('Ctrl Pts',(0.000181551162595994,4.05427772718987,
-45.483104758786));
#53773=CARTESIAN_POINT('Ctrl Pts',(0.404036195742715,4.05416906235028,-45.4909571599143));
#53774=CARTESIAN_POINT('Ctrl Pts',(0.83713307952267,4.0539012467317,-45.4998582098889));
#53775=CARTESIAN_POINT('Ctrl Pts',(1.28696595037213,4.05344844944743,-45.5098531479376));
#53776=CARTESIAN_POINT('Ctrl Pts',(1.48640695053461,4.05324769412451,-45.5142845725181));
#53777=CARTESIAN_POINT('Ctrl Pts',(1.68913754270891,4.05301114478449,-45.5189306432058));
#53778=CARTESIAN_POINT('Ctrl Pts',(1.89406691812013,4.05273924500278,-45.5237937603419));
#53779=CARTESIAN_POINT('Ctrl Pts',(2.40207554685425,4.05206522042732,-45.5358491597334));
#53780=CARTESIAN_POINT('Ctrl Pts',(2.92359528397998,4.0511695350036,-45.5492383085822));
#53781=CARTESIAN_POINT('Ctrl Pts',(3.44183098945343,4.05031895343455,-45.5640819003926));
#53782=CARTESIAN_POINT('Ctrl Pts',(3.55707650285137,4.05012980068306,-45.5673828257067));
#53783=CARTESIAN_POINT('Ctrl Pts',(3.67215975304471,4.04994301706739,-45.5707556451171));
#53784=CARTESIAN_POINT('Ctrl Pts',(3.7868964873834,4.04976156559607,-45.5742015989867));
#53785=CARTESIAN_POINT('Ctrl Pts',(4.22095109987234,4.04907512590854,-45.5872378090565));
#53786=CARTESIAN_POINT('Ctrl Pts',(4.65004621640487,4.04846758781903,-45.6013200772451));
#53787=CARTESIAN_POINT('Ctrl Pts',(5.06447649274192,4.04800401280653,-45.616441724763));
#53788=CARTESIAN_POINT('Ctrl Pts',(5.44484785101927,4.04757853554959,-45.6303206374153));
#53789=CARTESIAN_POINT('Ctrl Pts',(5.81286752503525,4.04727488700343,-45.6450742828859));
#53790=CARTESIAN_POINT('Ctrl Pts',(6.16101928401631,4.04710852121872,-45.6607119137277));
#53791=CARTESIAN_POINT('Ctrl Pts',(6.19219321962801,4.04709362462226,-45.6621121263776));
#53792=CARTESIAN_POINT('Ctrl Pts',(6.2232078440126,4.04707980157761,-45.6635194407835));
#53793=CARTESIAN_POINT('Ctrl Pts',(6.25405774996299,4.04706704679936,-45.6649338724781));
#53794=CARTESIAN_POINT('Ctrl Pts',(6.39369015341136,4.04700931630432,-45.671335853001));
#53795=CARTESIAN_POINT('Ctrl Pts',(6.52992501973367,4.04697334440262,-45.6778867910422));
#53796=CARTESIAN_POINT('Ctrl Pts',(6.66370228859331,4.04695855294085,-45.6846379325746));
#53797=CARTESIAN_POINT('Ctrl Pts',(6.97370603308844,4.04692427650082,-45.7002824375976));
#53798=CARTESIAN_POINT('Ctrl Pts',(7.27051360118711,4.04700094253711,-45.7170033860239));
#53799=CARTESIAN_POINT('Ctrl Pts',(7.56580390759954,4.04720606586608,-45.7354275474617));
#53800=CARTESIAN_POINT('Ctrl Pts',(7.57251673859061,4.04721072893226,-45.7358463837025));
#53801=CARTESIAN_POINT('Ctrl Pts',(7.57922878490261,4.04721546021916,-45.736266099256));
#53802=CARTESIAN_POINT('Ctrl Pts',(7.58594018431063,4.04722025876168,-45.7366867010865));
#53803=CARTESIAN_POINT('Ctrl Pts',(7.95978215304528,4.04748754975046,-45.7601152897915));
#53804=CARTESIAN_POINT('Ctrl Pts',(8.33161933763295,4.04795972550633,-45.7862993479164));
#53805=CARTESIAN_POINT('Ctrl Pts',(8.70240386159958,4.04846734504311,-45.8158868079574));
#53806=CARTESIAN_POINT('Ctrl Pts',(8.75744748111489,4.04854270206272,-45.8202791188217));
#53807=CARTESIAN_POINT('Ctrl Pts',(8.81246786886126,4.04861892343029,-45.8247464065533));
#53808=CARTESIAN_POINT('Ctrl Pts',(8.86746810593587,4.04869554438674,-45.8292907621443));
#53809=CARTESIAN_POINT('Ctrl Pts',(9.21325287644122,4.04917725794381,-45.8578609836323));
#53810=CARTESIAN_POINT('Ctrl Pts',(9.55824383302655,4.04967203846346,-45.8894772374749));
#53811=CARTESIAN_POINT('Ctrl Pts',(9.90713893817511,4.05009215387646,-45.9248188740961));
#53812=CARTESIAN_POINT('Ctrl Pts',(9.98756366758387,4.05018899578657,-45.9329655678163));
#53813=CARTESIAN_POINT('Ctrl Pts',(10.0681959253425,4.0502820013443,-45.9413100595536));
#53814=CARTESIAN_POINT('Ctrl Pts',(10.1490934332731,4.05037031202927,-45.9498603773688));
#53815=CARTESIAN_POINT('Ctrl Pts',(10.4017415872042,4.05064611201496,-45.9765635733855));
#53816=CARTESIAN_POINT('Ctrl Pts',(10.6569707728277,4.05087496421816,-46.0052806388128));
#53817=CARTESIAN_POINT('Ctrl Pts',(10.9122399706433,4.05103425693971,-46.0356784115238));
#53818=CARTESIAN_POINT('Ctrl Pts',(11.0578538286592,4.05112512269216,-46.0530182903554));
#53819=CARTESIAN_POINT('Ctrl Pts',(11.2034804477291,4.05119360068566,-46.07090537708));
#53820=CARTESIAN_POINT('Ctrl Pts',(11.3486452763677,4.05123805153778,-46.0892809134502));
#53821=CARTESIAN_POINT('Ctrl Pts',(11.383976601352,4.05124887032575,-46.0937532918724));
#53822=CARTESIAN_POINT('Ctrl Pts',(11.4192805580855,4.05125827662745,-46.0982546159133));
#53823=CARTESIAN_POINT('Ctrl Pts',(11.4545498895211,4.05126637489147,-46.1027841806848));
#53824=CARTESIAN_POINT('Ctrl Pts',(11.7742497637354,4.05133978183977,-46.1438425514774));
#53825=CARTESIAN_POINT('Ctrl Pts',(12.0911755578599,4.05130574615934,-46.1872009234999));
#53826=CARTESIAN_POINT('Ctrl Pts',(12.4042033751243,4.05124265326174,-46.2324848587249));
#53827=CARTESIAN_POINT('Ctrl Pts',(12.694496373003,4.05118414272248,-46.2744798782957));
#53828=CARTESIAN_POINT('Ctrl Pts',(12.9814371435597,4.05110083046585,-46.3181318940072));
#53829=CARTESIAN_POINT('Ctrl Pts',(13.2641790028529,4.05105226727443,-46.3631417277007));
#53830=CARTESIAN_POINT('Ctrl Pts',(13.2863224412092,4.05104846396055,-46.3666667539572));
#53831=CARTESIAN_POINT('Ctrl Pts',(13.3084401516756,4.05104487157467,-46.3702001039138));
#53832=CARTESIAN_POINT('Ctrl Pts',(13.3305317410286,4.05104151756354,-46.3737416311182));
#53833=CARTESIAN_POINT('Ctrl Pts',(13.5484374371254,4.05100843446944,-46.4086743350719));
#53834=CARTESIAN_POINT('Ctrl Pts',(13.7638001579389,4.05099865212725,-46.4444031545213));
#53835=CARTESIAN_POINT('Ctrl Pts',(13.9762533895905,4.05103765329587,-46.4807836800727));
#53836=CARTESIAN_POINT('Ctrl Pts',(14.0502765809521,4.05105124212643,-46.4934594232647));
#53837=CARTESIAN_POINT('Ctrl Pts',(14.123945972003,4.05107078300246,-46.506215870132));
#53838=CARTESIAN_POINT('Ctrl Pts',(14.1972362791489,4.05109736515344,-46.5190461735337));
#53839=CARTESIAN_POINT('Ctrl Pts',(14.4152033436357,4.05117642108377,-46.5572037918853));
#53840=CARTESIAN_POINT('Ctrl Pts',(14.6298152039408,4.05132110559856,-46.5960153776103));
#53841=CARTESIAN_POINT('Ctrl Pts',(14.8403666086119,4.05164841295011,-46.63537629821));
#53842=CARTESIAN_POINT('Ctrl Pts',(14.9669073543126,4.05184512366027,-46.6590320902573));
#53843=CARTESIAN_POINT('Ctrl Pts',(15.0919820464878,4.05210702155462,-46.6828861270287));
#53844=CARTESIAN_POINT('Ctrl Pts',(15.2154428418291,4.05245235788283,-46.7069136265541));
#53845=CARTESIAN_POINT('Ctrl Pts',(15.4204518451068,4.05302579543639,-46.7468117473734));
#53846=CARTESIAN_POINT('Ctrl Pts',(15.6210091637685,4.05383142766662,-46.7871891841816));
#53847=CARTESIAN_POINT('Ctrl Pts',(15.8164619842098,4.05491944656549,-46.8279226001094));
#53848=CARTESIAN_POINT('Ctrl Pts',(15.9582682497402,4.05570883346984,-46.8574757863053));
#53849=CARTESIAN_POINT('Ctrl Pts',(16.0973882435089,4.05664596943625,-46.8872160234026));
#53850=CARTESIAN_POINT('Ctrl Pts',(16.2335823643503,4.0577373193662,-46.9170900353023));
#53851=CARTESIAN_POINT('Ctrl Pts',(16.4490700936387,4.05946406437406,-46.9643570021083));
#53852=CARTESIAN_POINT('Ctrl Pts',(16.6572464582291,4.06157688937563,-47.011941479225));
#53853=CARTESIAN_POINT('Ctrl Pts',(16.8582463821327,4.06407456508433,-47.0599168052684));
#53854=CARTESIAN_POINT('Ctrl Pts',(16.9176596804606,4.06481284970218,-47.0740977676451));
#53855=CARTESIAN_POINT('Ctrl Pts',(16.976446152718,4.06558452834257,-47.088312692545));
#53856=CARTESIAN_POINT('Ctrl Pts',(17.0346097395913,4.06638904300838,-47.1025630232352));
#53857=CARTESIAN_POINT('Ctrl Pts',(17.2060465166445,4.06876034451871,-47.1445657761052));
#53858=CARTESIAN_POINT('Ctrl Pts',(17.372076387095,4.07141599648714,-47.1868760786687));
#53859=CARTESIAN_POINT('Ctrl Pts',(17.5328887073449,4.07430357677168,-47.2294920695148));
#53860=CARTESIAN_POINT('Ctrl Pts',(17.70411692991,4.07737818721738,-47.2748683214965));
#53861=CARTESIAN_POINT('Ctrl Pts',(17.8694294628641,4.0807156401366,-47.3205910960604));
#53862=CARTESIAN_POINT('Ctrl Pts',(18.0289977932907,4.08426414519071,-47.3666573201107));
#53863=CARTESIAN_POINT('Ctrl Pts',(18.0461419230271,4.08464539898246,-47.3716067064925));
#53864=CARTESIAN_POINT('Ctrl Pts',(18.0632196968548,4.08502910018635,-47.3765600571397));
#53865=CARTESIAN_POINT('Ctrl Pts',(18.0802312943422,4.08541519258013,-47.3815173680596));
#53866=CARTESIAN_POINT('',(-18.0802309774523,4.08571015955263,-47.3814955774373));
#53867=CARTESIAN_POINT('Ctrl Pts',(-18.0802309774513,4.0857101605419,-47.3814955773641));
#53868=CARTESIAN_POINT('Ctrl Pts',(-17.5067139301086,4.0727934681898,-47.2143630626668));
#53869=CARTESIAN_POINT('Ctrl Pts',(-16.1440950398105,4.05188108130506,-46.8717506694211));
#53870=CARTESIAN_POINT('Ctrl Pts',(-14.1201831359268,4.05068380667564,-46.4964790979153));
#53871=CARTESIAN_POINT('Ctrl Pts',(-12.8049882654227,4.05125213987811,-46.2906560258708));
#53872=CARTESIAN_POINT('Ctrl Pts',(-11.4702101265463,4.0515968823569,-46.0956364270593));
#53873=CARTESIAN_POINT('Ctrl Pts',(-9.97768282702567,4.05009813281506,-45.9211073625856));
#53874=CARTESIAN_POINT('Ctrl Pts',(-8.13525028131847,4.04739085834718,-45.7662068083777));
#53875=CARTESIAN_POINT('Ctrl Pts',(-6.8682519065081,4.04686778354698,-45.692032173767));
#53876=CARTESIAN_POINT('Ctrl Pts',(-5.13414802380493,4.04767124663689,-45.6143613687216));
#53877=CARTESIAN_POINT('Ctrl Pts',(-2.82998160019649,4.05178951295812,-45.5424604326639));
#53878=CARTESIAN_POINT('Ctrl Pts',(-0.829721113891657,4.05412214869547,
-45.4992347614638));
#53879=CARTESIAN_POINT('Ctrl Pts',(1.31624832385343E-14,4.0543744617278,
-45.4831027428904));
#53880=CARTESIAN_POINT('',(-23.8104968601155,4.71986549956444,-53.1013140443576));
#53881=CARTESIAN_POINT('Ctrl Pts',(-23.8104968601155,4.71986549956443,-53.1013140443576));
#53882=CARTESIAN_POINT('Ctrl Pts',(-23.7477724747327,4.65732912739002,-52.8297917254588));
#53883=CARTESIAN_POINT('Ctrl Pts',(-23.5151124729736,4.47941158193885,-51.9618739110486));
#53884=CARTESIAN_POINT('Ctrl Pts',(-22.9893961882904,4.32328459465657,-50.7078659748253));
#53885=CARTESIAN_POINT('Ctrl Pts',(-21.9700525412669,4.23238141610583,-49.4407645829627));
#53886=CARTESIAN_POINT('Ctrl Pts',(-20.9139224437741,4.17982285241228,-48.6001017036111));
#53887=CARTESIAN_POINT('Ctrl Pts',(-19.7542941715404,4.1339665963394,-47.9759241951474));
#53888=CARTESIAN_POINT('Ctrl Pts',(-18.7286389805631,4.10128995312838,-47.5836512241988));
#53889=CARTESIAN_POINT('Ctrl Pts',(-18.0802309774513,4.0857101605419,-47.3814955773641));
#53890=CARTESIAN_POINT('',(-24.4986968589845,6.71024380605157,-58.7795509549468));
#53891=CARTESIAN_POINT('Ctrl Pts',(-24.4986797976549,6.71047053280741,-58.7794556342435));
#53892=CARTESIAN_POINT('Ctrl Pts',(-24.4252551199817,6.38406893036685,-58.0159461404066));
#53893=CARTESIAN_POINT('Ctrl Pts',(-24.2995445048026,5.84530779207223,-56.7153263194681));
#53894=CARTESIAN_POINT('Ctrl Pts',(-24.1427524316995,5.29535697555521,-55.1551273288394));
#53895=CARTESIAN_POINT('Ctrl Pts',(-24.0157643032102,4.99438929412664,-54.1765791490832));
#53896=CARTESIAN_POINT('Ctrl Pts',(-23.8948201762871,4.80482491391012,-53.4702756145878));
#53897=CARTESIAN_POINT('Ctrl Pts',(-23.8104968601155,4.71986549956443,-53.1013140443576));
#53898=CARTESIAN_POINT('',(-24.8344040968691,9.66898708497287,-64.6542740052741));
#53899=CARTESIAN_POINT('Ctrl Pts',(-24.8344040968691,9.66898708497287,-64.6542740052741));
#53900=CARTESIAN_POINT('Ctrl Pts',(-24.8344224440182,9.66879626623666,-64.653902178655));
#53901=CARTESIAN_POINT('Ctrl Pts',(-24.8344407806158,9.66860542911226,-64.6535303121725));
#53902=CARTESIAN_POINT('Ctrl Pts',(-24.8344591066652,9.668414573522,-64.6531584056758));
#53903=CARTESIAN_POINT('Ctrl Pts',(-24.8406922382788,9.60349998185404,-64.5266640318661));
#53904=CARTESIAN_POINT('Ctrl Pts',(-24.845543748124,9.53913720233528,-64.4020695812121));
#53905=CARTESIAN_POINT('Ctrl Pts',(-24.8491870326249,9.47559685187425,-64.2796392143731));
#53906=CARTESIAN_POINT('Ctrl Pts',(-24.8501169863959,9.45937808320314,-64.248388681701));
#53907=CARTESIAN_POINT('Ctrl Pts',(-24.8509682174295,9.44321271503155,-64.2172790189038));
#53908=CARTESIAN_POINT('Ctrl Pts',(-24.8517436631487,9.42710337089091,-64.1863110121561));
#53909=CARTESIAN_POINT('Ctrl Pts',(-24.8525260595257,9.41084963168299,-64.155065425677));
#53910=CARTESIAN_POINT('Ctrl Pts',(-24.8532313056664,9.39465292971663,-64.1239640567786));
#53911=CARTESIAN_POINT('Ctrl Pts',(-24.853862327618,9.37851683625275,-64.0930100676953));
#53912=CARTESIAN_POINT('Ctrl Pts',(-24.8551422263563,9.34578807679707,-64.0302262430248));
#53913=CARTESIAN_POINT('Ctrl Pts',(-24.8561167908272,9.31330875463947,-63.9680487208868));
#53914=CARTESIAN_POINT('Ctrl Pts',(-24.8568104559153,9.28110504994544,-63.9064976883872));
#53915=CARTESIAN_POINT('Ctrl Pts',(-24.8582409926514,9.21469175715154,-63.7795617727215));
#53916=CARTESIAN_POINT('Ctrl Pts',(-24.8584773379802,9.14945187681934,-63.6552897653036));
#53917=CARTESIAN_POINT('Ctrl Pts',(-24.8577256710445,9.08557210499735,-63.5338319601283));
#53918=CARTESIAN_POINT('Ctrl Pts',(-24.8573369025111,9.05253294360197,-63.4710129500809));
#53919=CARTESIAN_POINT('Ctrl Pts',(-24.8566837216044,9.01985732795747,-63.4089469492897));
#53920=CARTESIAN_POINT('Ctrl Pts',(-24.8557940882076,8.98757346065118,-63.3476620540359));
#53921=CARTESIAN_POINT('Ctrl Pts',(-24.8548818089494,8.95446779867432,-63.2848171350145));
#53922=CARTESIAN_POINT('Ctrl Pts',(-24.8537208873905,8.9217740456132,-63.2227935470531));
#53923=CARTESIAN_POINT('Ctrl Pts',(-24.8523401728298,8.88951735436266,-63.161617164268));
#53924=CARTESIAN_POINT('Ctrl Pts',(-24.8491493068904,8.81497133278947,-63.0202370110637));
#53925=CARTESIAN_POINT('Ctrl Pts',(-24.8447863435392,8.74276273534532,-62.8833818467826));
#53926=CARTESIAN_POINT('Ctrl Pts',(-24.8395922216543,8.67316848592726,-62.7513690700857));
#53927=CARTESIAN_POINT('Ctrl Pts',(-24.8350852872875,8.61278162528261,-62.6368217157227));
#53928=CARTESIAN_POINT('Ctrl Pts',(-24.8299522037595,8.55436225020739,-62.525920199597));
#53929=CARTESIAN_POINT('Ctrl Pts',(-24.8243995161682,8.49806401214277,-62.4188696888623));
#53930=CARTESIAN_POINT('Ctrl Pts',(-24.8179231259384,8.43240042978602,-62.2940110739286));
#53931=CARTESIAN_POINT('Ctrl Pts',(-24.8108764077816,8.36962333665799,-62.1743920867275));
#53932=CARTESIAN_POINT('Ctrl Pts',(-24.8035602182169,8.30994192047519,-62.0603472077105));
#53933=CARTESIAN_POINT('Ctrl Pts',(-24.795963710439,8.24797382380193,-61.9419327239393));
#53934=CARTESIAN_POINT('Ctrl Pts',(-24.7880766366637,8.18934299086503,-61.8295276615945));
#53935=CARTESIAN_POINT('Ctrl Pts',(-24.7802072266692,8.13423747464485,-61.723492436022));
#53936=CARTESIAN_POINT('Ctrl Pts',(-24.7790968967969,8.12646239356123,-61.7085314569205));
#53937=CARTESIAN_POINT('Ctrl Pts',(-24.7779868750224,8.11875742404929,-61.6936972647197));
#53938=CARTESIAN_POINT('Ctrl Pts',(-24.7768779853736,8.11112302824542,-61.6789908511765));
#53939=CARTESIAN_POINT('Ctrl Pts',(-24.7726019398298,8.08168364787585,-61.6222807049786));
#53940=CARTESIAN_POINT('Ctrl Pts',(-24.7683428924224,8.05329390958756,-61.567470659123));
#53941=CARTESIAN_POINT('Ctrl Pts',(-24.7641470319276,8.02597767604251,-61.514616177431));
#53942=CARTESIAN_POINT('Ctrl Pts',(-24.7535979342429,7.95730007906331,-61.3817311372514));
#53943=CARTESIAN_POINT('Ctrl Pts',(-24.7437087555778,7.89555086323448,-61.2614546023172));
#53944=CARTESIAN_POINT('Ctrl Pts',(-24.734591378146,7.84043481895105,-61.1535048428839));
#53945=CARTESIAN_POINT('Ctrl Pts',(-24.7236433235866,7.77425203070551,-61.023879864121));
#53946=CARTESIAN_POINT('Ctrl Pts',(-24.7138064905812,7.71762815366309,-60.9120270608297));
#53947=CARTESIAN_POINT('Ctrl Pts',(-24.7052248674143,7.67001622988454,-60.8174730315066));
#53948=CARTESIAN_POINT('Ctrl Pts',(-24.7014023754499,7.64880856409547,-60.7753560554688));
#53949=CARTESIAN_POINT('Ctrl Pts',(-24.6978285223653,7.62938908047058,-60.7366716068643));
#53950=CARTESIAN_POINT('Ctrl Pts',(-24.6945151438418,7.61171250297287,-60.7013800383922));
#53951=CARTESIAN_POINT('Ctrl Pts',(-24.6911719711583,7.59387697630155,-60.6657711253638));
#53952=CARTESIAN_POINT('Ctrl Pts',(-24.688096864724,7.57781359951931,-60.6336175901605));
#53953=CARTESIAN_POINT('Ctrl Pts',(-24.68499470864,7.56169084505966,-60.6012688132271));
#53954=CARTESIAN_POINT('Ctrl Pts',(-24.684165593198,7.5573817051171,-60.5926229328271));
#53955=CARTESIAN_POINT('Ctrl Pts',(-24.6833346094936,7.55306858444141,-60.5839632025695));
#53956=CARTESIAN_POINT('Ctrl Pts',(-24.6824962645542,7.54871708623057,-60.5752201349814));
#53957=CARTESIAN_POINT('Ctrl Pts',(-24.6785212311363,7.52808434904397,-60.5337646621742));
#53958=CARTESIAN_POINT('Ctrl Pts',(-24.6743778519337,7.50658795121024,-60.4904274495276));
#53959=CARTESIAN_POINT('Ctrl Pts',(-24.670260456794,7.48553430446318,-60.4478289601855));
#53960=CARTESIAN_POINT('Ctrl Pts',(-24.6632384283214,7.44962827604104,-60.3751791913624));
#53961=CARTESIAN_POINT('Ctrl Pts',(-24.6562928707284,7.41500093872425,-60.3046841856839));
#53962=CARTESIAN_POINT('Ctrl Pts',(-24.6493275032303,7.38086146759743,-60.2347361217812));
#53963=CARTESIAN_POINT('Ctrl Pts',(-24.648618581765,7.3773868190735,-60.2276169448002));
#53964=CARTESIAN_POINT('Ctrl Pts',(-24.6479094647092,7.37391726536273,-60.2205034482435));
#53965=CARTESIAN_POINT('Ctrl Pts',(-24.6472000572969,7.37045200118949,-60.2133939471382));
#53966=CARTESIAN_POINT('Ctrl Pts',(-24.6467056641082,7.36803702359793,-60.2084392640324));
#53967=CARTESIAN_POINT('Ctrl Pts',(-24.6462111299257,7.3656241294789,-60.2034865214929));
#53968=CARTESIAN_POINT('Ctrl Pts',(-24.6457164231681,7.36321304982242,-60.1985351552348));
#53969=CARTESIAN_POINT('Ctrl Pts',(-24.633104532769,7.30174578279113,-60.0723066620617));
#53970=CARTESIAN_POINT('Ctrl Pts',(-24.6203743116398,7.2414509890623,-59.9469538919258));
#53971=CARTESIAN_POINT('Ctrl Pts',(-24.6076554397387,7.18271338071539,-59.8231292097387));
#53972=CARTESIAN_POINT('Ctrl Pts',(-24.6038772972698,7.16526536690217,-59.7863470726034));
#53973=CARTESIAN_POINT('Ctrl Pts',(-24.6001000414851,7.14795446886728,-59.7496996349988));
#53974=CARTESIAN_POINT('Ctrl Pts',(-24.5963267699639,7.13078998746342,-59.713203608095));
#53975=CARTESIAN_POINT('Ctrl Pts',(-24.5886731810201,7.09597407655986,-59.6391761795279));
#53976=CARTESIAN_POINT('Ctrl Pts',(-24.58105329827,7.06139276976336,-59.5649721004123));
#53977=CARTESIAN_POINT('Ctrl Pts',(-24.5734606104834,7.02728461174253,-59.4910568103805));
#53978=CARTESIAN_POINT('Ctrl Pts',(-24.5636741126434,6.98332133757985,-59.3957846423995));
#53979=CARTESIAN_POINT('Ctrl Pts',(-24.5539335820194,6.94014571561547,-59.3009912537256));
#53980=CARTESIAN_POINT('Ctrl Pts',(-24.5442226032045,6.89808037257437,-59.2073294929134));
#53981=CARTESIAN_POINT('Ctrl Pts',(-24.5416644851313,6.88699929451397,-59.1826566100174));
#53982=CARTESIAN_POINT('Ctrl Pts',(-24.5391083193834,6.87599500118245,-59.1580622963691));
#53983=CARTESIAN_POINT('Ctrl Pts',(-24.5365535829411,6.86507286998188,-59.1335587093582));
#53984=CARTESIAN_POINT('Ctrl Pts',(-24.531532367751,6.84360593108926,-59.0853980532233));
#53985=CARTESIAN_POINT('Ctrl Pts',(-24.5265166119427,6.82245811143022,-59.0375914462527));
#53986=CARTESIAN_POINT('Ctrl Pts',(-24.5214880208954,6.8018476240916,-58.9906631794842));
#53987=CARTESIAN_POINT('Ctrl Pts',(-24.5202367873599,6.79671924266268,-58.9789863060638));
#53988=CARTESIAN_POINT('Ctrl Pts',(-24.5189847612876,6.79162401850022,-58.967363593278));
#53989=CARTESIAN_POINT('Ctrl Pts',(-24.5177316660908,6.78656507652644,-58.9558026410564));
#53990=CARTESIAN_POINT('Ctrl Pts',(-24.5145490120368,6.77371620261572,-58.9264397390598));
#53991=CARTESIAN_POINT('Ctrl Pts',(-24.5113596688225,6.7610994594533,-58.8974704883638));
#53992=CARTESIAN_POINT('Ctrl Pts',(-24.508181636039,6.74846010516535,-58.8682875733842));
#53993=CARTESIAN_POINT('Ctrl Pts',(-24.5052694035877,6.73687786538744,-58.8415454225581));
#53994=CARTESIAN_POINT('Ctrl Pts',(-24.5023666549417,6.72527668001029,-58.8146239786376));
#53995=CARTESIAN_POINT('Ctrl Pts',(-24.4994852743528,6.71347910466107,-58.7871019844863));
#53996=CARTESIAN_POINT('Ctrl Pts',(-24.4992222898793,6.71240233640863,-58.7845900437977));
#53997=CARTESIAN_POINT('Ctrl Pts',(-24.4989594820256,6.71132394573296,-58.7820731338583));
#53998=CARTESIAN_POINT('Ctrl Pts',(-24.4986968589845,6.71024380605157,-58.7795509549467));
#53999=CARTESIAN_POINT('',(-23.6739538968997,12.846244756358,-70.6467988317471));
#54000=CARTESIAN_POINT('Ctrl Pts',(-23.6739538968997,12.846244756358,-70.6467988317471));
#54001=CARTESIAN_POINT('Ctrl Pts',(-23.7652621574204,12.6829373366643,-70.3394704142904));
#54002=CARTESIAN_POINT('Ctrl Pts',(-24.0270822733915,12.1921901977266,-69.4189320572497));
#54003=CARTESIAN_POINT('Ctrl Pts',(-24.3752871742381,11.4464620234297,-68.0281725531546));
#54004=CARTESIAN_POINT('Ctrl Pts',(-24.6927334369296,10.5534106262424,-66.3568311811825));
#54005=CARTESIAN_POINT('Ctrl Pts',(-24.8064000890597,9.94888081636442,-65.1999953822759));
#54006=CARTESIAN_POINT('Ctrl Pts',(-24.834404590668,9.66888169588114,-64.6543281145607));
#54007=CARTESIAN_POINT('',(-21.0403876111779,16.0446155815448,-76.6642782169352));
#54008=CARTESIAN_POINT('Ctrl Pts',(-21.0403876111779,16.0446155815448,-76.6642782169352));
#54009=CARTESIAN_POINT('Ctrl Pts',(-21.1157744386118,15.9895528116427,-76.5606151308124));
#54010=CARTESIAN_POINT('Ctrl Pts',(-21.1894544949622,15.9330326908327,-76.4542145604713));
#54011=CARTESIAN_POINT('Ctrl Pts',(-21.2615519837989,15.8752394470457,-76.3454234075435));
#54012=CARTESIAN_POINT('Ctrl Pts',(-21.3425035537031,15.8103487845565,-76.2232719323215));
#54013=CARTESIAN_POINT('Ctrl Pts',(-21.4214605193681,15.7438528570669,-76.0981061976719));
#54014=CARTESIAN_POINT('Ctrl Pts',(-21.4985706912578,15.6759811894835,-75.9703585271215));
#54015=CARTESIAN_POINT('Ctrl Pts',(-21.5673831294008,15.615413111203,-75.8563576312315));
#54016=CARTESIAN_POINT('Ctrl Pts',(-21.6347244735916,15.5537485428601,-75.740298881361));
#54017=CARTESIAN_POINT('Ctrl Pts',(-21.7006795254284,15.491137347613,-75.6224646500583));
#54018=CARTESIAN_POINT('Ctrl Pts',(-21.7660650693083,15.4290667868266,-75.5056478924814));
#54019=CARTESIAN_POINT('Ctrl Pts',(-21.8302672176974,15.3658891486313,-75.3867550339643));
#54020=CARTESIAN_POINT('Ctrl Pts',(-21.8931017751448,15.301979237563,-75.2664911270759));
#54021=CARTESIAN_POINT('Ctrl Pts',(-21.9140608170538,15.2806615016086,-75.2263759998752));
#54022=CARTESIAN_POINT('Ctrl Pts',(-21.9348679110239,15.2592624788604,-75.1861086789179));
#54023=CARTESIAN_POINT('Ctrl Pts',(-21.9555168651605,15.2377965702097,-75.1457162520817));
#54024=CARTESIAN_POINT('Ctrl Pts',(-22.0271530207548,15.1633262042088,-75.0055852723458));
#54025=CARTESIAN_POINT('Ctrl Pts',(-22.096882122716,15.0880497994365,-74.863946650444));
#54026=CARTESIAN_POINT('Ctrl Pts',(-22.1648447318524,15.0120088428319,-74.720877921363));
#54027=CARTESIAN_POINT('Ctrl Pts',(-22.2328073409888,14.9359678862273,-74.5778091922819));
#54028=CARTESIAN_POINT('Ctrl Pts',(-22.2990048300633,14.8591617040834,-74.4333090900849));
#54029=CARTESIAN_POINT('Ctrl Pts',(-22.363614314154,14.7816525062363,-74.2874939422127));
#54030=CARTESIAN_POINT('Ctrl Pts',(-22.4167826773859,14.7178687252177,-74.1674999064158));
#54031=CARTESIAN_POINT('Ctrl Pts',(-22.4687952306308,14.6537059438917,-74.0467978231759));
#54032=CARTESIAN_POINT('Ctrl Pts',(-22.5197134187718,14.5892908679778,-73.9256254181383));
#54033=CARTESIAN_POINT('Ctrl Pts',(-22.5315313738241,14.5743403267345,-73.8975016751578));
#54034=CARTESIAN_POINT('Ctrl Pts',(-22.5432903955293,14.5593762976717,-73.8693527895989));
#54035=CARTESIAN_POINT('Ctrl Pts',(-22.5549912688892,14.5444005592069,-73.8411820979184));
#54036=CARTESIAN_POINT('Ctrl Pts',(-22.5802750736682,14.5120402698404,-73.7803095248174));
#54037=CARTESIAN_POINT('Ctrl Pts',(-22.6054781494533,14.4793808052658,-73.7188752021463));
#54038=CARTESIAN_POINT('Ctrl Pts',(-22.6305925092312,14.4464447355768,-73.656921526668));
#54039=CARTESIAN_POINT('Ctrl Pts',(-22.6570055251894,14.4118055513813,-73.5917642447962));
#54040=CARTESIAN_POINT('Ctrl Pts',(-22.6833051765735,14.3768807447599,-73.5260705381479));
#54041=CARTESIAN_POINT('Ctrl Pts',(-22.7095089054492,14.3416661164437,-73.4598327530951));
#54042=CARTESIAN_POINT('Ctrl Pts',(-22.7708723054029,14.2592011614813,-73.3047183525638));
#54043=CARTESIAN_POINT('Ctrl Pts',(-22.8317093809367,14.1751448480743,-73.1466165290608));
#54044=CARTESIAN_POINT('Ctrl Pts',(-22.8917965026637,14.0899135670005,-72.9863073813454));
#54045=CARTESIAN_POINT('Ctrl Pts',(-22.9019397255509,14.0755257937799,-72.959245818578));
#54046=CARTESIAN_POINT('Ctrl Pts',(-22.9120615982471,14.0611045940741,-72.9321214595726));
#54047=CARTESIAN_POINT('Ctrl Pts',(-22.9221610720533,14.0466520342293,-72.9049381755185));
#54048=CARTESIAN_POINT('Ctrl Pts',(-23.0008434107626,13.9340559494477,-72.6931603736021));
#54049=CARTESIAN_POINT('Ctrl Pts',(-23.0782166637999,13.8194803232158,-72.4776639036223));
#54050=CARTESIAN_POINT('Ctrl Pts',(-23.153934413458,13.7037037360802,-72.2599027125882));
#54051=CARTESIAN_POINT('Ctrl Pts',(-23.1663291103867,13.6847515654799,-72.2242560646371));
#54052=CARTESIAN_POINT('Ctrl Pts',(-23.1786794750302,13.6657672647917,-72.1885488265631));
#54053=CARTESIAN_POINT('Ctrl Pts',(-23.1909840247367,13.6467543026212,-72.1527874762431));
#54054=CARTESIAN_POINT('Ctrl Pts',(-23.2766051125639,13.5144527927993,-71.9039424725987));
#54055=CARTESIAN_POINT('Ctrl Pts',(-23.360006842537,13.3807628703025,-71.6524754466928));
#54056=CARTESIAN_POINT('Ctrl Pts',(-23.4407760922421,13.2467437015264,-71.4003541575491));
#54057=CARTESIAN_POINT('Ctrl Pts',(-23.4810080390131,13.1799874535214,-71.274770097753));
#54058=CARTESIAN_POINT('Ctrl Pts',(-23.5205870372981,13.1131486974205,-71.14902216018));
#54059=CARTESIAN_POINT('Ctrl Pts',(-23.5594144433799,13.0464455753219,-71.023518316434));
#54060=CARTESIAN_POINT('Ctrl Pts',(-23.5982418494616,12.9797424532234,-70.898014472688));
#54061=CARTESIAN_POINT('Ctrl Pts',(-23.6363197141491,12.9131779257759,-70.7727603664136));
#54062=CARTESIAN_POINT('Ctrl Pts',(-23.6738690325247,12.8463956913735,-70.6470828763833));
#54063=CARTESIAN_POINT('',(-20.8066780834711,16.2071460528287,-76.9702782129914));
#54064=CARTESIAN_POINT('Ctrl Pts',(-20.806678083471,16.2071460528287,-76.9702782129914));
#54065=CARTESIAN_POINT('Ctrl Pts',(-20.8862783237883,16.1545206907567,-76.8711944318144));
#54066=CARTESIAN_POINT('Ctrl Pts',(-20.964160252313,16.1002920803761,-76.7690967308679));
#54067=CARTESIAN_POINT('Ctrl Pts',(-21.040387611155,16.0446155815615,-76.6642782169667));
#54068=CARTESIAN_POINT('',(-25.7066762066276,16.4237761199824,-77.3782788360333));
#54069=CARTESIAN_POINT('Ctrl Pts',(-25.7066762066276,16.4237761199824,-77.3782788360333));
#54070=CARTESIAN_POINT('Ctrl Pts',(-25.6911863733062,16.507982961079,-77.5366055866555));
#54071=CARTESIAN_POINT('Ctrl Pts',(-25.6219414370306,16.672353368847,-77.845549521693));
#54072=CARTESIAN_POINT('Ctrl Pts',(-25.2871445035823,16.9752951011235,-78.4144172197497));
#54073=CARTESIAN_POINT('Ctrl Pts',(-24.6881842909862,17.1791668341045,-78.7966009790571));
#54074=CARTESIAN_POINT('Ctrl Pts',(-24.0052836532123,17.2918079376106,-79.007776150789));
#54075=CARTESIAN_POINT('Ctrl Pts',(-23.4548404136072,17.3408644644138,-79.0998653586004));
#54076=CARTESIAN_POINT('Ctrl Pts',(-22.915385779096,17.3537835256363,-79.1243293554279));
#54077=CARTESIAN_POINT('Ctrl Pts',(-22.453183479509,17.3348149207234,-79.0890214085024));
#54078=CARTESIAN_POINT('Ctrl Pts',(-22.1409244224793,17.3017278860839,-79.0271274374767));
#54079=CARTESIAN_POINT('Ctrl Pts',(-21.9683332638225,17.2768673638735,-78.980572195562));
#54080=CARTESIAN_POINT('Ctrl Pts',(-21.842286688042,17.2550204029918,-78.9396380523261));
#54081=CARTESIAN_POINT('Ctrl Pts',(-21.7192769440428,17.2296451041489,-78.8920701039884));
#54082=CARTESIAN_POINT('Ctrl Pts',(-21.6202901990439,17.2054366649431,-78.8466701327192));
#54083=CARTESIAN_POINT('Ctrl Pts',(-21.5578972221677,17.1881137776076,-78.8141735369845));
#54084=CARTESIAN_POINT('Ctrl Pts',(-21.5200612514553,17.1770416352821,-78.7934005178304));
#54085=CARTESIAN_POINT('Ctrl Pts',(-21.4920163013668,17.1684848139744,-78.7773452063036));
#54086=CARTESIAN_POINT('Ctrl Pts',(-21.4598148077115,17.1581297618176,-78.7579137361204));
#54087=CARTESIAN_POINT('Ctrl Pts',(-21.4325806776235,17.1489958995923,-78.7407724150982));
#54088=CARTESIAN_POINT('Ctrl Pts',(-21.410197465255,17.1411647504829,-78.726074667103));
#54089=CARTESIAN_POINT('Ctrl Pts',(-21.392491440011,17.1347699480245,-78.7140719746968));
#54090=CARTESIAN_POINT('Ctrl Pts',(-21.2430108509951,17.0796173710175,-78.6105496138558));
#54091=CARTESIAN_POINT('Ctrl Pts',(-21.0013130164285,16.9524612526866,-78.3717421247602));
#54092=CARTESIAN_POINT('Ctrl Pts',(-20.7388418587697,16.6352545775742,-77.7755268245789));
#54093=CARTESIAN_POINT('Ctrl Pts',(-20.7560657229672,16.3737697050196,-77.2837215842416));
#54094=CARTESIAN_POINT('Ctrl Pts',(-20.8066780834711,16.2071460528287,-76.9702782129914));
#54095=CARTESIAN_POINT('',(-25.9580275654167,16.0437450369841,-76.6642789908811));
#54096=CARTESIAN_POINT('Ctrl Pts',(-25.9580171294882,16.0437528221483,-76.6643138637023));
#54097=CARTESIAN_POINT('Ctrl Pts',(-25.8750885959483,16.1725292612534,-76.9062552995085));
#54098=CARTESIAN_POINT('Ctrl Pts',(-25.7912591348258,16.2994925070891,-77.1447932578045));
#54099=CARTESIAN_POINT('Ctrl Pts',(-25.7066761933522,16.4237671850429,-77.3782835868249));
#54100=CARTESIAN_POINT('',(-27.8093579489709,12.8426393697465,-70.6502216955646));
#54101=CARTESIAN_POINT('Ctrl Pts',(-27.8093579489709,12.8426393697465,-70.6502216955646));
#54102=CARTESIAN_POINT('Ctrl Pts',(-27.6629613805351,13.0960632412153,-71.1288965648361));
#54103=CARTESIAN_POINT('Ctrl Pts',(-27.3589056055191,13.6404286392169,-72.1540324778666));
#54104=CARTESIAN_POINT('Ctrl Pts',(-26.7510733868799,14.7393369280985,-74.2160146070454));
#54105=CARTESIAN_POINT('Ctrl Pts',(-26.2631471674262,15.5696171136249,-75.7735033231351));
#54106=CARTESIAN_POINT('Ctrl Pts',(-25.9580275654167,16.0437450369841,-76.6642789908811));
#54107=CARTESIAN_POINT('',(-30.33736888334,9.77553124130067,-64.7925772570574));
#54108=CARTESIAN_POINT('Ctrl Pts',(-30.3373681408964,9.77560492643774,-64.7925461433589));
#54109=CARTESIAN_POINT('Ctrl Pts',(-30.1852567493822,9.8786370639834,-65.0401821262795));
#54110=CARTESIAN_POINT('Ctrl Pts',(-30.0522518687011,9.97792805405255,-65.2605477273785));
#54111=CARTESIAN_POINT('Ctrl Pts',(-29.5847277881304,10.3617001491574,-66.0727023311734));
#54112=CARTESIAN_POINT('Ctrl Pts',(-29.2973751005394,10.6626910528547,-66.6432962914613));
#54113=CARTESIAN_POINT('Ctrl Pts',(-28.7957862062539,11.271428069297,-67.7691626336424));
#54114=CARTESIAN_POINT('Ctrl Pts',(-28.575739044809,11.5846998083453,-68.3335909516651));
#54115=CARTESIAN_POINT('Ctrl Pts',(-28.2728671785687,12.0549538215514,-69.1894896819946));
#54116=CARTESIAN_POINT('Ctrl Pts',(-28.1756180623507,12.2132686880608,-69.4789022400814));
#54117=CARTESIAN_POINT('Ctrl Pts',(-28.0350849141614,12.4495248094586,-69.9150228417591));
#54118=CARTESIAN_POINT('Ctrl Pts',(-27.9889555168352,12.5283881508439,-70.061304788306));
#54119=CARTESIAN_POINT('Ctrl Pts',(-27.9208881500455,12.646344253899,-70.281369857301));
#54120=CARTESIAN_POINT('Ctrl Pts',(-27.8983536215529,12.6856658373485,-70.3549429927763));
#54121=CARTESIAN_POINT('Ctrl Pts',(-27.8529729253694,12.7653429953578,-70.5044861836174));
#54122=CARTESIAN_POINT('Ctrl Pts',(-27.8307788796621,12.8045663382374,-70.5783475852013));
#54123=CARTESIAN_POINT('Ctrl Pts',(-27.8093579217479,12.8426234408141,-70.6502301207803));
#54124=CARTESIAN_POINT('',(-32.81521999432,8.33900374689714,-59.2033586636525));
#54125=CARTESIAN_POINT('Ctrl Pts',(-32.815219994237,8.33900374759826,-59.2033586635242));
#54126=CARTESIAN_POINT('Ctrl Pts',(-32.6923181777297,8.39620454756814,-59.5955480932275));
#54127=CARTESIAN_POINT('Ctrl Pts',(-32.3170499076978,8.58960686180279,-60.7566922032304));
#54128=CARTESIAN_POINT('Ctrl Pts',(-31.4950115977029,9.06913125042783,-62.8815100017806));
#54129=CARTESIAN_POINT('Ctrl Pts',(-30.825979501774,9.43523105888426,-63.9748521677351));
#54130=CARTESIAN_POINT('Ctrl Pts',(-30.33736888334,9.77553124130067,-64.7925772570574));
#54131=CARTESIAN_POINT('',(-34.9063163914144,8.66722257324563,-53.4437571318393));
#54132=CARTESIAN_POINT('Ctrl Pts',(-34.9063163914144,8.66722257324563,-53.4437571318393));
#54133=CARTESIAN_POINT('Ctrl Pts',(-34.5724735540937,8.60352804275007,-54.2895979904455));
#54134=CARTESIAN_POINT('Ctrl Pts',(-34.0106677638488,8.38266385056441,-55.6375787991562));
#54135=CARTESIAN_POINT('Ctrl Pts',(-33.3555720402961,8.20876541621131,-57.5526773984119));
#54136=CARTESIAN_POINT('Ctrl Pts',(-32.9982863465608,8.26644533317311,-58.6882956274082));
#54137=CARTESIAN_POINT('Ctrl Pts',(-32.815219994237,8.33900374759826,-59.2033586635242));
#54138=CARTESIAN_POINT('',(-36.4974177553682,8.64413762617978,-47.4049093964133));
#54139=CARTESIAN_POINT('Ctrl Pts',(-36.4973970222996,8.64418876114758,-47.4049059587411));
#54140=CARTESIAN_POINT('Ctrl Pts',(-36.4930289916103,8.64553623909837,-47.4512937213671));
#54141=CARTESIAN_POINT('Ctrl Pts',(-36.4886315292324,8.64694889881603,-47.4972561440451));
#54142=CARTESIAN_POINT('Ctrl Pts',(-36.484192549884,8.64843677203915,-47.5430220976373));
#54143=CARTESIAN_POINT('Ctrl Pts',(-36.4787175260311,8.65027191042287,-47.5994696879291));
#54144=CARTESIAN_POINT('Ctrl Pts',(-36.4731794617622,8.65222167439011,-47.6556192569373));
#54145=CARTESIAN_POINT('Ctrl Pts',(-36.4675493926941,8.65430341847232,-47.7119871384523));
#54146=CARTESIAN_POINT('Ctrl Pts',(-36.4658463631896,8.6549331215097,-47.7290377579324));
#54147=CARTESIAN_POINT('Ctrl Pts',(-36.4641348729266,8.65557487828422,-47.7461087665885));
#54148=CARTESIAN_POINT('Ctrl Pts',(-36.4624140181909,8.65622909617189,-47.7632151944437));
#54149=CARTESIAN_POINT('Ctrl Pts',(-36.4536224220762,8.65957140003995,-47.8506094419356));
#54150=CARTESIAN_POINT('Ctrl Pts',(-36.4445877356492,8.66324213430238,-47.9389321062188));
#54151=CARTESIAN_POINT('Ctrl Pts',(-36.4352616615615,8.66706716925153,-48.0267057038783));
#54152=CARTESIAN_POINT('Ctrl Pts',(-36.4318722169841,8.66845733019651,-48.0586059163179));
#54153=CARTESIAN_POINT('Ctrl Pts',(-36.4284441225271,8.66986751298689,-48.0904332878203));
#54154=CARTESIAN_POINT('Ctrl Pts',(-36.4249745171483,8.67128828565653,-48.1221167741548));
#54155=CARTESIAN_POINT('Ctrl Pts',(-36.4163577663833,8.67481676876961,-48.2008025828584));
#54156=CARTESIAN_POINT('Ctrl Pts',(-36.407485592542,8.67841162841733,-48.2786028353604));
#54157=CARTESIAN_POINT('Ctrl Pts',(-36.3982992396125,8.68193730465335,-48.3547699804819));
#54158=CARTESIAN_POINT('Ctrl Pts',(-36.3832550118477,8.68771120390653,-48.4795067381686));
#54159=CARTESIAN_POINT('Ctrl Pts',(-36.3674213410786,8.69348144139046,-48.6016400496475));
#54160=CARTESIAN_POINT('Ctrl Pts',(-36.3506717255914,8.69909693977363,-48.7215796362339));
#54161=CARTESIAN_POINT('Ctrl Pts',(-36.3447399773247,8.70108562559313,-48.7640553238337));
#54162=CARTESIAN_POINT('Ctrl Pts',(-36.3386935379683,8.70305534242297,-48.80625573984));
#54163=CARTESIAN_POINT('Ctrl Pts',(-36.3325273598475,8.7050007255993,-48.8481986924699));
#54164=CARTESIAN_POINT('Ctrl Pts',(-36.3139269188474,8.71086902591192,-48.974720729375));
#54165=CARTESIAN_POINT('Ctrl Pts',(-36.2942355210381,8.71651232896629,-49.0988978177763));
#54166=CARTESIAN_POINT('Ctrl Pts',(-36.273332807523,8.72179936887609,-49.2210928935335));
#54167=CARTESIAN_POINT('Ctrl Pts',(-36.2514155037859,8.72734303474937,-49.3492191575517));
#54168=CARTESIAN_POINT('Ctrl Pts',(-36.2281665678998,8.73249563709191,-49.4751662784035));
#54169=CARTESIAN_POINT('Ctrl Pts',(-36.2034673290701,8.73715372561922,-49.5993803218675));
#54170=CARTESIAN_POINT('Ctrl Pts',(-36.1770276647907,8.74214004514491,-49.7323470756462));
#54171=CARTESIAN_POINT('Ctrl Pts',(-36.1489261982809,8.74656032064097,-49.863327691379));
#54172=CARTESIAN_POINT('Ctrl Pts',(-36.1190381533995,8.75033147847292,-49.9929025197663));
#54173=CARTESIAN_POINT('Ctrl Pts',(-36.1146844987613,8.75088080576588,-50.0117770916841));
#54174=CARTESIAN_POINT('Ctrl Pts',(-36.1102929679145,8.75141642102278,-50.0306218921998));
#54175=CARTESIAN_POINT('Ctrl Pts',(-36.1058632068143,8.751938125806,-50.0494387730954));
#54176=CARTESIAN_POINT('Ctrl Pts',(-36.0835767301713,8.75456286361976,-50.144107981453));
#54177=CARTESIAN_POINT('Ctrl Pts',(-36.0602596436235,8.75682996775874,-50.2382269535845));
#54178=CARTESIAN_POINT('Ctrl Pts',(-36.0358615729958,8.75871909889858,-50.3320618854742));
#54179=CARTESIAN_POINT('Ctrl Pts',(-35.9999440738256,8.76150017397549,-50.4702005169957));
#54180=CARTESIAN_POINT('Ctrl Pts',(-35.9616833399972,8.76346229475952,-50.6077212978283));
#54181=CARTESIAN_POINT('Ctrl Pts',(-35.9209301557936,8.76454314369576,-50.7455436566489));
#54182=CARTESIAN_POINT('Ctrl Pts',(-35.8822140489112,8.76556996561794,-50.8764768654072));
#54183=CARTESIAN_POINT('Ctrl Pts',(-35.8412488566998,8.76580268314493,-51.0076821423615));
#54184=CARTESIAN_POINT('Ctrl Pts',(-35.7979164514549,8.76518430437887,-51.1399924693141));
#54185=CARTESIAN_POINT('Ctrl Pts',(-35.7818028154709,8.76495435336922,-51.1891935333535));
#54186=CARTESIAN_POINT('Ctrl Pts',(-35.7653619105376,8.76460658281126,-51.2385478748913));
#54187=CARTESIAN_POINT('Ctrl Pts',(-35.7485878674312,8.76413739810438,-51.2881000964566));
#54188=CARTESIAN_POINT('Ctrl Pts',(-35.7079903302002,8.76300184935893,-51.4080293315912));
#54189=CARTESIAN_POINT('Ctrl Pts',(-35.6654412007548,8.76115656530288,-51.529114700737));
#54190=CARTESIAN_POINT('Ctrl Pts',(-35.620851257772,8.75854559565368,-51.6520184108547));
#54191=CARTESIAN_POINT('Ctrl Pts',(-35.5961416953814,8.75709872415909,-51.7201256271918));
#54192=CARTESIAN_POINT('Ctrl Pts',(-35.5708054769911,8.75541638233675,-51.7887919529377));
#54193=CARTESIAN_POINT('Ctrl Pts',(-35.5448277903592,8.75348544289058,-51.8581361380061));
#54194=CARTESIAN_POINT('Ctrl Pts',(-35.5034267713903,8.75040807646563,-51.9686509795348));
#54195=CARTESIAN_POINT('Ctrl Pts',(-35.4603963380976,8.74670139246173,-52.0808858519023));
#54196=CARTESIAN_POINT('Ctrl Pts',(-35.4156751384311,8.74227587473622,-52.1953420239112));
#54197=CARTESIAN_POINT('Ctrl Pts',(-35.373287056294,8.73808123751165,-52.3038269853255));
#54198=CARTESIAN_POINT('Ctrl Pts',(-35.329379885665,8.73324135910154,-52.414307454948));
#54199=CARTESIAN_POINT('Ctrl Pts',(-35.2839046009633,8.72764503042221,-52.5272398205582));
#54200=CARTESIAN_POINT('Ctrl Pts',(-35.2414710308672,8.72242302451609,-52.6326184560888));
#54201=CARTESIAN_POINT('Ctrl Pts',(-35.197671958818,8.71654270599691,-52.7401319985077));
#54202=CARTESIAN_POINT('Ctrl Pts',(-35.1524723942141,8.70987655801072,-52.8501776988826));
#54203=CARTESIAN_POINT('Ctrl Pts',(-35.1380366349633,8.70774753512516,-52.8853239055136));
#54204=CARTESIAN_POINT('Ctrl Pts',(-35.1234580703044,8.70553803581093,-52.9207286095553));
#54205=CARTESIAN_POINT('Ctrl Pts',(-35.1087357173717,8.70324293979444,-52.9564053679361));
#54206=CARTESIAN_POINT('Ctrl Pts',(-35.0659132069259,8.69656725598293,-53.0601773917032));
#54207=CARTESIAN_POINT('Ctrl Pts',(-35.0218735461726,8.68917045117481,-53.166249305713));
#54208=CARTESIAN_POINT('Ctrl Pts',(-34.9765945533639,8.68090166712676,-53.2749698162118));
#54209=CARTESIAN_POINT('Ctrl Pts',(-34.9534600464532,8.67667687700144,-53.3305186534418));
#54210=CARTESIAN_POINT('Ctrl Pts',(-34.9300021434374,8.67222379725344,-53.3867592998611));
#54211=CARTESIAN_POINT('Ctrl Pts',(-34.9062189727919,8.66751773911485,-53.4437408417599));
#54212=CARTESIAN_POINT('',(-37.4912550961874,8.66275191199404,-41.3740808902194));
#54213=CARTESIAN_POINT('Ctrl Pts',(-37.491189835617,8.6629355512308,-41.3740675237284));
#54214=CARTESIAN_POINT('Ctrl Pts',(-37.356700123897,8.65117444483456,-41.870984084739));
#54215=CARTESIAN_POINT('Ctrl Pts',(-37.1655465363814,8.62975442365193,-42.611977051936));
#54216=CARTESIAN_POINT('Ctrl Pts',(-36.88503216533,8.59955674721597,-43.9209841884754));
#54217=CARTESIAN_POINT('Ctrl Pts',(-36.6512741057588,8.59103223488232,-45.4978226844016));
#54218=CARTESIAN_POINT('Ctrl Pts',(-36.5532891736331,8.62548607044055,-46.792631727622));
#54219=CARTESIAN_POINT('Ctrl Pts',(-36.4974177553682,8.64413762617978,-47.4049093964133));
#54220=CARTESIAN_POINT('',(-38.9091460669097,8.64371781494149,-35.3259112856609));
#54221=CARTESIAN_POINT('Ctrl Pts',(-38.9090921504208,8.64388899039054,-35.3258962859625));
#54222=CARTESIAN_POINT('Ctrl Pts',(-38.9089923803477,8.64391395683976,-35.3265391752867));
#54223=CARTESIAN_POINT('Ctrl Pts',(-38.9088925687444,8.64393892778801,-35.3271821637191));
#54224=CARTESIAN_POINT('Ctrl Pts',(-38.9087927155238,8.64396390325458,-35.3278252515927));
#54225=CARTESIAN_POINT('Ctrl Pts',(-38.9010416619146,8.64590261068036,-35.377744608754));
#54226=CARTESIAN_POINT('Ctrl Pts',(-38.893040948649,8.6478815213966,-35.4291730896422));
#54227=CARTESIAN_POINT('Ctrl Pts',(-38.8847602428943,8.64987340469648,-35.4819038201963));
#54228=CARTESIAN_POINT('Ctrl Pts',(-38.8774468694352,8.65163260094019,-35.5284746725773));
#54229=CARTESIAN_POINT('Ctrl Pts',(-38.8699150880467,8.65340194442179,-35.5760616904033));
#54230=CARTESIAN_POINT('Ctrl Pts',(-38.8621452295201,8.65515861579911,-35.6244816485022));
#54231=CARTESIAN_POINT('Ctrl Pts',(-38.8578352844873,8.65613304243134,-35.6513402273532));
#54232=CARTESIAN_POINT('Ctrl Pts',(-38.8534521080782,8.65710349341095,-35.6784543186067));
#54233=CARTESIAN_POINT('Ctrl Pts',(-38.8489925569198,8.65806538151594,-35.7057855665315));
#54234=CARTESIAN_POINT('Ctrl Pts',(-38.837160129509,8.66061753772527,-35.7783029557562));
#54235=CARTESIAN_POINT('Ctrl Pts',(-38.8247903422569,8.66310890245544,-35.8523421507106));
#54236=CARTESIAN_POINT('Ctrl Pts',(-38.8117921403903,8.66555150832271,-35.9284109044899));
#54237=CARTESIAN_POINT('Ctrl Pts',(-38.8030160035092,8.66720070900891,-35.9797710697189));
#54238=CARTESIAN_POINT('Ctrl Pts',(-38.7939533509191,8.66882771198339,-36.0320571416344));
#54239=CARTESIAN_POINT('Ctrl Pts',(-38.7845753678349,8.67043697660535,-36.0854391578441));
#54240=CARTESIAN_POINT('Ctrl Pts',(-38.7626357657024,8.6742018187057,-36.2103253072602));
#54241=CARTESIAN_POINT('Ctrl Pts',(-38.7389709088127,8.67787156150978,-36.3412193387587));
#54242=CARTESIAN_POINT('Ctrl Pts',(-38.7132264474225,8.68142472654518,-36.4794520117829));
#54243=CARTESIAN_POINT('Ctrl Pts',(-38.7083652398284,8.6820956542679,-36.5055538482001));
#54244=CARTESIAN_POINT('Ctrl Pts',(-38.7034298482699,8.68276236529588,-36.5319172136502));
#54245=CARTESIAN_POINT('Ctrl Pts',(-38.6984178331563,8.68342462471417,-36.558550866477));
#54246=CARTESIAN_POINT('Ctrl Pts',(-38.6811269220411,8.68570934821904,-36.6504340937338));
#54247=CARTESIAN_POINT('Ctrl Pts',(-38.6629336867529,8.68791838048242,-36.7452218008698));
#54248=CARTESIAN_POINT('Ctrl Pts',(-38.6436861704223,8.690012614542,-36.8431203416096));
#54249=CARTESIAN_POINT('Ctrl Pts',(-38.6125355094802,8.6934019752264,-37.0015617839719));
#54250=CARTESIAN_POINT('Ctrl Pts',(-38.5786256817257,8.69649257073304,-37.1681471984866));
#54251=CARTESIAN_POINT('Ctrl Pts',(-38.5412800152023,8.6991051969997,-37.3439169337678));
#54252=CARTESIAN_POINT('Ctrl Pts',(-38.5374413725623,8.69937374056909,-37.3619837474971));
#54253=CARTESIAN_POINT('Ctrl Pts',(-38.5335664272518,8.69963719321634,-37.3801474087064));
#54254=CARTESIAN_POINT('Ctrl Pts',(-38.5296547036981,8.69989534537905,-37.3984080931803));
#54255=CARTESIAN_POINT('Ctrl Pts',(-38.4929974502891,8.70231452176423,-37.5695312640755));
#54256=CARTESIAN_POINT('Ctrl Pts',(-38.4531125120698,8.70427049130661,-37.7491723002855));
#54257=CARTESIAN_POINT('Ctrl Pts',(-38.4096004714822,8.70558653496202,-37.9374917606443));
#54258=CARTESIAN_POINT('Ctrl Pts',(-38.3846707945306,8.70634054563908,-38.0453870293346));
#54259=CARTESIAN_POINT('Ctrl Pts',(-38.3585500110649,8.70688401621914,-38.1561316054534));
#54260=CARTESIAN_POINT('Ctrl Pts',(-38.3311593377478,8.70717887644011,-38.2697606369798));
#54261=CARTESIAN_POINT('Ctrl Pts',(-38.3244562750184,8.70725103481807,-38.2975680047425));
#54262=CARTESIAN_POINT('Ctrl Pts',(-38.3176771765432,8.70730828039793,-38.3255479458308));
#54263=CARTESIAN_POINT('Ctrl Pts',(-38.3108174593195,8.70734996070891,-38.3537140754484));
#54264=CARTESIAN_POINT('Ctrl Pts',(-38.2765890091585,8.70755793611093,-38.4942567439596));
#54265=CARTESIAN_POINT('Ctrl Pts',(-38.2403549331725,8.70738074668867,-38.6394344676793));
#54266=CARTESIAN_POINT('Ctrl Pts',(-38.2015342101401,8.70671971787683,-38.7909302440284));
#54267=CARTESIAN_POINT('Ctrl Pts',(-38.1708049037257,8.706196467527,-38.910849703747));
#54268=CARTESIAN_POINT('Ctrl Pts',(-38.1384610683968,8.70536846681098,-39.0347278181911));
#54269=CARTESIAN_POINT('Ctrl Pts',(-38.1057102218041,8.70427431951171,-39.1582853361838));
#54270=CARTESIAN_POINT('Ctrl Pts',(-38.0887946401576,8.7037092001362,-39.2221019241832));
#54271=CARTESIAN_POINT('Ctrl Pts',(-38.0717710110007,8.70307368167698,-39.2858329237427));
#54272=CARTESIAN_POINT('Ctrl Pts',(-38.0548093062264,8.70237725162869,-39.3488880213126));
#54273=CARTESIAN_POINT('Ctrl Pts',(-37.9738109041856,8.6990515410474,-39.6499993902266));
#54274=CARTESIAN_POINT('Ctrl Pts',(-37.8941771573195,8.69432620811437,-39.9357008070417));
#54275=CARTESIAN_POINT('Ctrl Pts',(-37.8166126392952,8.68890321160458,-40.211615336106));
#54276=CARTESIAN_POINT('Ctrl Pts',(-37.7987960992563,8.68765755138637,-40.2749927975999));
#54277=CARTESIAN_POINT('Ctrl Pts',(-37.7810885840085,8.6863750335467,-40.3378537397244));
#54278=CARTESIAN_POINT('Ctrl Pts',(-37.763498260598,8.68506409032027,-40.4002661241927));
#54279=CARTESIAN_POINT('Ctrl Pts',(-37.7002374816639,8.68034949311207,-40.6247222620632));
#54280=CARTESIAN_POINT('Ctrl Pts',(-37.6384910072925,8.67526723033651,-40.8433800677456));
#54281=CARTESIAN_POINT('Ctrl Pts',(-37.5783484419992,8.67010156626611,-41.0592716010482));
#54282=CARTESIAN_POINT('Ctrl Pts',(-37.5489627761302,8.66757762207411,-41.1647562346124));
#54283=CARTESIAN_POINT('Ctrl Pts',(-37.5199593500415,8.66503352278262,-41.2695805547653));
#54284=CARTESIAN_POINT('Ctrl Pts',(-37.4913443196371,8.66250084268668,-41.3740991647216));
#54285=CARTESIAN_POINT('',(-39.8378651641511,8.40808204040271,-29.2047428884228));
#54286=CARTESIAN_POINT('Ctrl Pts',(-39.8378651639228,8.40808204093907,-29.204742888344));
#54287=CARTESIAN_POINT('Ctrl Pts',(-39.7403557200732,8.42558824320743,-29.6064705490188));
#54288=CARTESIAN_POINT('Ctrl Pts',(-39.5863221729383,8.46001992220811,-30.3835625396964));
#54289=CARTESIAN_POINT('Ctrl Pts',(-39.4599526712302,8.4939877818819,-31.1842583062903));
#54290=CARTESIAN_POINT('Ctrl Pts',(-39.3117522083446,8.53693747852479,-32.2573499658343));
#54291=CARTESIAN_POINT('Ctrl Pts',(-39.1834328367189,8.5752710622992,-33.3490981603829));
#54292=CARTESIAN_POINT('Ctrl Pts',(-39.0384531936711,8.61284501735072,-34.4653792758384));
#54293=CARTESIAN_POINT('Ctrl Pts',(-38.959857971873,8.63186531179917,-35.008020879665));
#54294=CARTESIAN_POINT('Ctrl Pts',(-38.9091460669097,8.64371781494149,-35.3259112856608));
#54295=CARTESIAN_POINT('',(-43.6350081753485,8.95468720513522,-22.9398480277775));
#54296=CARTESIAN_POINT('Ctrl Pts',(-43.6350081753485,8.95468720513522,-22.9398480277775));
#54297=CARTESIAN_POINT('Ctrl Pts',(-43.4741574413301,8.94820825817609,-23.1065847254121));
#54298=CARTESIAN_POINT('Ctrl Pts',(-43.1335328486735,8.92374576231794,-23.4666708399978));
#54299=CARTESIAN_POINT('Ctrl Pts',(-42.181557989294,8.79178703405004,-24.5033719122517));
#54300=CARTESIAN_POINT('Ctrl Pts',(-41.0217226392209,8.48128348309427,-26.0202735195218));
#54301=CARTESIAN_POINT('Ctrl Pts',(-40.2577289267292,8.36214502734256,-27.6878442174315));
#54302=CARTESIAN_POINT('Ctrl Pts',(-39.9631870435311,8.38841260911053,-28.7076954825739));
#54303=CARTESIAN_POINT('Ctrl Pts',(-39.8378651639228,8.4080820409391,-29.204742888344));
#54304=CARTESIAN_POINT('',(-56.9472987453291,10.4971210956015,-16.8490842893495));
#54305=CARTESIAN_POINT('Ctrl Pts',(-56.9472987452347,10.4971210960165,-16.8490842892202));
#54306=CARTESIAN_POINT('Ctrl Pts',(-56.2481469214632,10.4104471933364,-17.0815737981202));
#54307=CARTESIAN_POINT('Ctrl Pts',(-54.1344740653502,10.1093354912827,-17.7283592068575));
#54308=CARTESIAN_POINT('Ctrl Pts',(-51.3563456833993,9.61325730669952,-18.4697257428994));
#54309=CARTESIAN_POINT('Ctrl Pts',(-48.9121891096784,9.10710294010294,-19.2319251368394));
#54310=CARTESIAN_POINT('Ctrl Pts',(-47.2414265358552,8.840217651377,-19.9343653479424));
#54311=CARTESIAN_POINT('Ctrl Pts',(-46.0257479434454,8.82194194637927,-20.7196929414398));
#54312=CARTESIAN_POINT('Ctrl Pts',(-44.8748647635386,8.90526226846306,-21.6754872735224));
#54313=CARTESIAN_POINT('Ctrl Pts',(-44.0874700808914,8.96460650876973,-22.4409005690892));
#54314=CARTESIAN_POINT('Ctrl Pts',(-43.6350081753485,8.95468720513522,-22.9398480277775));
#54315=CARTESIAN_POINT('',(-69.6237422477832,12.3291004120271,-10.9554808154416));
#54316=CARTESIAN_POINT('Ctrl Pts',(-69.6237422477832,12.3291004120271,-10.9554808154416));
#54317=CARTESIAN_POINT('Ctrl Pts',(-69.0619467479908,12.2684092204603,-11.3706412385527));
#54318=CARTESIAN_POINT('Ctrl Pts',(-67.3257727339187,11.9872729690017,-12.5677786432507));
#54319=CARTESIAN_POINT('Ctrl Pts',(-65.1428673887983,11.4234020038613,-13.7075202041218));
#54320=CARTESIAN_POINT('Ctrl Pts',(-62.7668261595333,11.0221069854903,-14.6746180957437));
#54321=CARTESIAN_POINT('Ctrl Pts',(-61.0303852735734,10.8460095502133,-15.3378639972945));
#54322=CARTESIAN_POINT('Ctrl Pts',(-59.1522514841506,10.7106003736308,-16.0390772817491));
#54323=CARTESIAN_POINT('Ctrl Pts',(-57.6974034262523,10.5819199165458,-16.5733557441422));
#54324=CARTESIAN_POINT('Ctrl Pts',(-56.9472987452347,10.4971210960165,-16.8490842892202));
#54325=CARTESIAN_POINT('',(-76.0152010859362,13.203464721645,-5.1323536644963));
#54326=CARTESIAN_POINT('Ctrl Pts',(-76.0152010859361,13.203464721645,-5.1323536644963));
#54327=CARTESIAN_POINT('Ctrl Pts',(-75.6055079654791,13.12190451308,-5.716816608525));
#54328=CARTESIAN_POINT('Ctrl Pts',(-74.9215487758576,12.957479513477,-6.54678203039554));
#54329=CARTESIAN_POINT('Ctrl Pts',(-73.5802384751692,12.6798652978959,-7.873047892913));
#54330=CARTESIAN_POINT('Ctrl Pts',(-71.872722792672,12.4627641836395,-9.26669786648776));
#54331=CARTESIAN_POINT('Ctrl Pts',(-70.451678034269,12.4119687385728,-10.3168853345243));
#54332=CARTESIAN_POINT('Ctrl Pts',(-69.6237422477832,12.3291004120271,-10.9554808154415));
#54333=CARTESIAN_POINT('',(-77.8900123568112,13.4547375618153,-1.34395683259202));
#54334=CARTESIAN_POINT('Ctrl Pts',(-77.8897919792404,13.4547521615023,-1.34470326410749));
#54335=CARTESIAN_POINT('Ctrl Pts',(-77.687905838974,13.4682199621307,-2.0282002152612));
#54336=CARTESIAN_POINT('Ctrl Pts',(-77.4243415558115,13.4409012933351,-2.69552577166936));
#54337=CARTESIAN_POINT('Ctrl Pts',(-76.9525567732676,13.3724546737323,-3.64049244562797));
#54338=CARTESIAN_POINT('Ctrl Pts',(-76.7857287407807,13.3453290176752,-3.94159347054734));
#54339=CARTESIAN_POINT('Ctrl Pts',(-76.4200308904728,13.2814819277456,-4.54406678801877));
#54340=CARTESIAN_POINT('Ctrl Pts',(-76.2223690395977,13.2448574973167,-4.84142100893202));
#54341=CARTESIAN_POINT('Ctrl Pts',(-76.0153375294591,13.2031298898674,-5.13240265603379));
#54342=CARTESIAN_POINT('',(-71.7129439767344,8.64375557957816,1.03298829038523));
#54343=CARTESIAN_POINT('Ctrl Pts',(-71.7139042075071,8.64435208932012,1.03275752880096));
#54344=CARTESIAN_POINT('Ctrl Pts',(-71.7747188119592,8.68227215256098,1.01813579272073));
#54345=CARTESIAN_POINT('Ctrl Pts',(-71.8355664916663,8.72108772894506,1.00379664885951));
#54346=CARTESIAN_POINT('Ctrl Pts',(-71.8965306070675,8.76083117390857,0.989646569940123));
#54347=CARTESIAN_POINT('Ctrl Pts',(-71.966691596487,8.80657020256874,0.973361850137095));
#54348=CARTESIAN_POINT('Ctrl Pts',(-72.0370070497349,8.85353814249846,0.957327521923361));
#54349=CARTESIAN_POINT('Ctrl Pts',(-72.1076057540138,8.90179697013866,0.941404592495416));
#54350=CARTESIAN_POINT('Ctrl Pts',(-72.177854073707,8.94981628701864,0.925560689291656));
#54351=CARTESIAN_POINT('Ctrl Pts',(-72.2483828085012,8.99911375717801,0.909827250443446));
#54352=CARTESIAN_POINT('Ctrl Pts',(-72.319318686479,9.04976146747853,0.894069297918034));
#54353=CARTESIAN_POINT('Ctrl Pts',(-72.3888099009981,9.09937769838638,0.878632268159006));
#54354=CARTESIAN_POINT('Ctrl Pts',(-72.4586921083569,9.15028999732531,0.863171759399451));
#54355=CARTESIAN_POINT('Ctrl Pts',(-72.5290521981716,9.20255582626718,0.847568109351788));
#54356=CARTESIAN_POINT('Ctrl Pts',(-72.6359128789326,9.28193551546284,0.823869778794765));
#54357=CARTESIAN_POINT('Ctrl Pts',(-72.7438735159213,9.3644356615039,0.799841815292893));
#54358=CARTESIAN_POINT('Ctrl Pts',(-72.8530365481291,9.44985698853578,0.775079198820834));
#54359=CARTESIAN_POINT('Ctrl Pts',(-72.9033286761307,9.48921115657477,0.763670898299317));
#54360=CARTESIAN_POINT('Ctrl Pts',(-72.9538763340886,9.52918586174015,0.75210656838282));
#54361=CARTESIAN_POINT('Ctrl Pts',(-73.0046912038893,9.56976373539415,0.740346307564975));
#54362=CARTESIAN_POINT('Ctrl Pts',(-73.1234537853114,9.66460079869218,0.712860673174829));
#54363=CARTESIAN_POINT('Ctrl Pts',(-73.2436726461032,9.76273123797388,0.684305087434254));
#54364=CARTESIAN_POINT('Ctrl Pts',(-73.3655479475731,9.86396463519217,0.654162545478233));
#54365=CARTESIAN_POINT('Ctrl Pts',(-73.4834530575551,9.96190026849052,0.625001922434837));
#54366=CARTESIAN_POINT('Ctrl Pts',(-73.6029476879116,10.0626889841494,0.594338940577086));
#54367=CARTESIAN_POINT('Ctrl Pts',(-73.7243030596086,10.1661070351483,0.561682029959349));
#54368=CARTESIAN_POINT('Ctrl Pts',(-73.7942839346597,10.2257441620739,0.542850072629904));
#54369=CARTESIAN_POINT('Ctrl Pts',(-73.8648429610062,10.286308900022,0.523372952508207));
#54370=CARTESIAN_POINT('Ctrl Pts',(-73.9360196572315,10.3477822481166,0.503164180801907));
#54371=CARTESIAN_POINT('Ctrl Pts',(-73.9704193189414,10.3774922865248,0.493397291537105));
#54372=CARTESIAN_POINT('Ctrl Pts',(-74.0049632394888,10.4074145442767,0.483459525796313));
#54373=CARTESIAN_POINT('Ctrl Pts',(-74.0396557889533,10.4375468077449,0.473341248310394));
#54374=CARTESIAN_POINT('Ctrl Pts',(-74.0616239408447,10.4566272774976,0.466934113057424));
#54375=CARTESIAN_POINT('Ctrl Pts',(-74.0836491924182,10.4757897854284,0.460455326897042));
#54376=CARTESIAN_POINT('Ctrl Pts',(-74.1057326637109,10.4950337600684,0.453902493490168));
#54377=CARTESIAN_POINT('Ctrl Pts',(-74.1209340570077,10.5082805555209,0.449391780635923));
#54378=CARTESIAN_POINT('Ctrl Pts',(-74.1361639292525,10.5215667293953,0.444845719375119));
#54379=CARTESIAN_POINT('Ctrl Pts',(-74.15142479311,10.5348939807602,0.440262869550269));
#54380=CARTESIAN_POINT('Ctrl Pts',(-74.2209214739893,10.5955851541924,0.419392959775233));
#54381=CARTESIAN_POINT('Ctrl Pts',(-74.2910599577422,10.6571271073302,0.397761489779669));
#54382=CARTESIAN_POINT('Ctrl Pts',(-74.3618601395729,10.7194002313636,0.375310769785536));
#54383=CARTESIAN_POINT('Ctrl Pts',(-74.4443416020322,10.7919477617423,0.34915591861849));
#54384=CARTESIAN_POINT('Ctrl Pts',(-74.5278728361943,10.8653701096654,0.321829534180452));
#54385=CARTESIAN_POINT('Ctrl Pts',(-74.6124874497988,10.9396747980141,0.29321819202761));
#54386=CARTESIAN_POINT('Ctrl Pts',(-74.6981797801607,11.0149258879875,0.264242433829161));
#54387=CARTESIAN_POINT('Ctrl Pts',(-74.7836188958127,11.0899283290314,0.234411023652205));
#54388=CARTESIAN_POINT('Ctrl Pts',(-74.8688498737947,11.164552430703,0.203648851738809));
#54389=CARTESIAN_POINT('Ctrl Pts',(-74.905368038679,11.1965259609111,0.190468455447126));
#54390=CARTESIAN_POINT('Ctrl Pts',(-74.9418483580553,11.2284304875774,0.177116693959281));
#54391=CARTESIAN_POINT('Ctrl Pts',(-74.9782954785082,11.2602569521105,0.163585454925456));
#54392=CARTESIAN_POINT('Ctrl Pts',(-75.0074345983226,11.2857019022679,0.15276736036695));
#54393=CARTESIAN_POINT('Ctrl Pts',(-75.0365610563992,11.3111070185523,0.141831372080102));
#54394=CARTESIAN_POINT('Ctrl Pts',(-75.0656646015123,11.3364528632712,0.130777364319412));
#54395=CARTESIAN_POINT('Ctrl Pts',(-75.1693891430163,11.4267850242597,0.0913810680159116));
#54396=CARTESIAN_POINT('Ctrl Pts',(-75.2728226806968,11.5163646344423,0.0504861477426313));
#54397=CARTESIAN_POINT('Ctrl Pts',(-75.3762211738556,11.6050891055634,0.00797700848348162));
#54398=CARTESIAN_POINT('Ctrl Pts',(-75.5209764363984,11.7293011101946,-0.0515347061067087));
#54399=CARTESIAN_POINT('Ctrl Pts',(-75.6656005855099,11.8517654908376,-0.114186880414224));
#54400=CARTESIAN_POINT('Ctrl Pts',(-75.8105815039629,11.9720103355759,-0.180199616753054));
#54401=CARTESIAN_POINT('Ctrl Pts',(-75.8688769667546,12.0203596559357,-0.206742716742249));
#54402=CARTESIAN_POINT('Ctrl Pts',(-75.9272301710115,12.0683429779132,-0.233828803928773));
#54403=CARTESIAN_POINT('Ctrl Pts',(-75.9856730522913,12.1159454171049,-0.261471969112078));
#54404=CARTESIAN_POINT('Ctrl Pts',(-76.0738442188497,12.1877619070289,-0.303176451646275));
#54405=CARTESIAN_POINT('Ctrl Pts',(-76.1622194677579,12.2587114608792,-0.346148840494859));
#54406=CARTESIAN_POINT('Ctrl Pts',(-76.2508921194158,12.3286689947587,-0.390466393683425));
#54407=CARTESIAN_POINT('Ctrl Pts',(-76.3045126820762,12.3709724813333,-0.417265323153464));
#54408=CARTESIAN_POINT('Ctrl Pts',(-76.3582418720366,12.412917464529,-0.444556260698553));
#54409=CARTESIAN_POINT('Ctrl Pts',(-76.4120993155164,12.4544814707452,-0.472356374618462));
#54410=CARTESIAN_POINT('Ctrl Pts',(-76.4246540554797,12.4641704804003,-0.478836875337829));
#54411=CARTESIAN_POINT('Ctrl Pts',(-76.4372157038024,12.4738388656321,-0.485345020926855));
#54412=CARTESIAN_POINT('Ctrl Pts',(-76.4497845907488,12.4834862511291,-0.491881065292419));
#54413=CARTESIAN_POINT('Ctrl Pts',(-76.5663072516948,12.5729244833353,-0.552474917777949));
#54414=CARTESIAN_POINT('Ctrl Pts',(-76.6834519541958,12.6605584945839,-0.615466015597185));
#54415=CARTESIAN_POINT('Ctrl Pts',(-76.8014105707122,12.7461545044742,-0.681003990962555));
#54416=CARTESIAN_POINT('Ctrl Pts',(-76.9250297873023,12.8358580971271,-0.749687003792275));
#54417=CARTESIAN_POINT('Ctrl Pts',(-77.0495441480684,12.9233233001143,-0.821168132964172));
#54418=CARTESIAN_POINT('Ctrl Pts',(-77.1751446629466,13.0082520782237,-0.895608320462843));
#54419=CARTESIAN_POINT('Ctrl Pts',(-77.2934431354488,13.0882433484153,-0.965720775673853));
#54420=CARTESIAN_POINT('Ctrl Pts',(-77.4127053358055,13.1659845002992,-1.03845878994031));
#54421=CARTESIAN_POINT('Ctrl Pts',(-77.5330572832168,13.2411990194525,-1.11393705810681));
#54422=CARTESIAN_POINT('Ctrl Pts',(-77.6092830790908,13.288836691356,-1.16174177739831));
#54423=CARTESIAN_POINT('Ctrl Pts',(-77.6859470912346,13.3354581966371,-1.21064851708965));
#54424=CARTESIAN_POINT('Ctrl Pts',(-77.7627810117474,13.3808245309148,-1.26048464802789));
#54425=CARTESIAN_POINT('Ctrl Pts',(-77.805172502908,13.4058544466824,-1.28798067959899));
#54426=CARTESIAN_POINT('Ctrl Pts',(-77.8476154631687,13.4305028627614,-1.31575900541072));
#54427=CARTESIAN_POINT('Ctrl Pts',(-77.8900628058563,13.4547342196409,-1.34378595877275));
#54428=CARTESIAN_POINT('',(-66.3007096452781,7.3256579779933,6.6269806053999));
#54429=CARTESIAN_POINT('Ctrl Pts',(-66.3007095462964,7.32565791266264,6.62698056598248));
#54430=CARTESIAN_POINT('Ctrl Pts',(-66.3009135695284,7.3256802261172,6.62643125788398));
#54431=CARTESIAN_POINT('Ctrl Pts',(-66.3011176225372,7.32570254169686,6.62588191975181));
#54432=CARTESIAN_POINT('Ctrl Pts',(-66.3013217053874,7.32572485941033,6.62533255152024));
#54433=CARTESIAN_POINT('Ctrl Pts',(-66.3194179281466,7.32770379254521,6.57661954164251));
#54434=CARTESIAN_POINT('Ctrl Pts',(-66.3378230918283,7.32965372278552,6.52699894618457));
#54435=CARTESIAN_POINT('Ctrl Pts',(-66.3565849496956,7.33157745912018,6.47668360260689));
#54436=CARTESIAN_POINT('Ctrl Pts',(-66.374078920144,7.33337119334559,6.42976846553077));
#54437=CARTESIAN_POINT('Ctrl Pts',(-66.3918830071351,7.33514214755358,6.38224911349161));
#54438=CARTESIAN_POINT('Ctrl Pts',(-66.410035606402,7.3368925923503,6.3343426080647));
#54439=CARTESIAN_POINT('Ctrl Pts',(-66.4217701751073,7.33802415011952,6.30337392026969));
#54440=CARTESIAN_POINT('Ctrl Pts',(-66.4336503754913,7.33914713718827,6.27224433285713));
#54441=CARTESIAN_POINT('Ctrl Pts',(-66.4456864922457,7.34026218757265,6.24102425000606));
#54442=CARTESIAN_POINT('Ctrl Pts',(-66.4747433527868,7.34295407434778,6.16565462606573));
#54443=CARTESIAN_POINT('Ctrl Pts',(-66.5047091948074,7.34559978471336,6.08976624501636));
#54444=CARTESIAN_POINT('Ctrl Pts',(-66.5357273196607,7.34820719314405,6.01308254286435));
#54445=CARTESIAN_POINT('Ctrl Pts',(-66.5568756309281,7.3499849371358,5.96079921465153));
#54446=CARTESIAN_POINT('Ctrl Pts',(-66.578513037914,7.35174485098548,5.90814543700593));
#54447=CARTESIAN_POINT('Ctrl Pts',(-66.6006836819377,7.35348934292209,5.85501943010007));
#54448=CARTESIAN_POINT('Ctrl Pts',(-66.6428593479286,7.35680792533058,5.75395674918312));
#54449=CARTESIAN_POINT('Ctrl Pts',(-66.686966030636,7.36007054666283,5.65117826481152));
#54450=CARTESIAN_POINT('Ctrl Pts',(-66.7332927314322,7.3632907199729,5.54643924423697));
#54451=CARTESIAN_POINT('Ctrl Pts',(-66.7810584598513,7.36661092022778,5.43844675770848));
#54452=CARTESIAN_POINT('Ctrl Pts',(-66.8310605834434,7.36988089902069,5.32897366717206));
#54453=CARTESIAN_POINT('Ctrl Pts',(-66.883383161277,7.37312728448175,5.21861412315586));
#54454=CARTESIAN_POINT('Ctrl Pts',(-66.9042716248249,7.3744233216262,5.17455587129235));
#54455=CARTESIAN_POINT('Ctrl Pts',(-66.9255296182242,7.37571585460846,5.13035673764271));
#54456=CARTESIAN_POINT('Ctrl Pts',(-66.9471612143753,7.37700769457503,5.08605616894808));
#54457=CARTESIAN_POINT('Ctrl Pts',(-67.0020202838865,7.38028388085499,4.97370717905229));
#54458=CARTESIAN_POINT('Ctrl Pts',(-67.0592848107264,7.3835531223658,4.86070546692605));
#54459=CARTESIAN_POINT('Ctrl Pts',(-67.1189977790173,7.38688847113522,4.74763793427717));
#54460=CARTESIAN_POINT('Ctrl Pts',(-67.1763135110444,7.39008991902428,4.63910960973153));
#54461=CARTESIAN_POINT('Ctrl Pts',(-67.2358851065306,7.39335216145908,4.53052082135333));
#54462=CARTESIAN_POINT('Ctrl Pts',(-67.297716666954,7.39677274401974,4.42239841323215));
#54463=CARTESIAN_POINT('Ctrl Pts',(-67.3585623242391,7.40013878545192,4.31600001499786));
#54464=CARTESIAN_POINT('Ctrl Pts',(-67.4215966129306,7.40365803772726,4.21005340898495));
#54465=CARTESIAN_POINT('Ctrl Pts',(-67.4867880504236,7.40745792272589,4.10506590900433));
#54466=CARTESIAN_POINT('Ctrl Pts',(-67.5511198678568,7.41120770210489,4.00146278348265));
#54467=CARTESIAN_POINT('Ctrl Pts',(-67.6175524583477,7.41523077998971,3.89879381993956));
#54468=CARTESIAN_POINT('Ctrl Pts',(-67.6860185912183,7.41968423904816,3.79754912249489));
#54469=CARTESIAN_POINT('Ctrl Pts',(-67.7359642288322,7.42293301100205,3.72369171655007));
#54470=CARTESIAN_POINT('Ctrl Pts',(-67.7869912854423,7.42641156134627,3.65059231891243));
#54471=CARTESIAN_POINT('Ctrl Pts',(-67.8390603750945,7.43019232082122,3.57844119038534));
#54472=CARTESIAN_POINT('Ctrl Pts',(-67.8857580036338,7.43358305614492,3.51373319143344));
#54473=CARTESIAN_POINT('Ctrl Pts',(-67.9332935903729,7.43721706882084,3.44978792357554));
#54474=CARTESIAN_POINT('Ctrl Pts',(-67.9816311052487,7.44114802956374,3.3867439779933));
#54475=CARTESIAN_POINT('Ctrl Pts',(-68.0194296228557,7.44422192546497,3.33744546330498));
#54476=CARTESIAN_POINT('Ctrl Pts',(-68.0577180817216,7.44747752520659,3.28869812900676));
#54477=CARTESIAN_POINT('Ctrl Pts',(-68.0964849977637,7.45094195228621,3.24056752849838));
#54478=CARTESIAN_POINT('Ctrl Pts',(-68.167468735921,7.45728545364744,3.15243851818121));
#54479=CARTESIAN_POINT('Ctrl Pts',(-68.240236923429,7.46434767010371,3.06631689289534));
#54480=CARTESIAN_POINT('Ctrl Pts',(-68.3143503194014,7.47226730576452,2.98259175686538));
#54481=CARTESIAN_POINT('Ctrl Pts',(-68.3809814871828,7.47938740282066,2.90731921654876));
#54482=CARTESIAN_POINT('Ctrl Pts',(-68.4486998362414,7.48720099887561,2.83398386620116));
#54483=CARTESIAN_POINT('Ctrl Pts',(-68.5172226611057,7.49581109283069,2.76284316012924));
#54484=CARTESIAN_POINT('Ctrl Pts',(-68.5837159569218,7.50416617050726,2.69380952027606));
#54485=CARTESIAN_POINT('Ctrl Pts',(-68.6509665695429,7.51327156880274,2.62684268767755));
#54486=CARTESIAN_POINT('Ctrl Pts',(-68.7187552419876,7.5232183054159,2.56214960643483));
#54487=CARTESIAN_POINT('Ctrl Pts',(-68.7852864741979,7.53298053588124,2.4986565440199));
#54488=CARTESIAN_POINT('Ctrl Pts',(-68.8523359727839,7.54355343171551,2.43735377662181));
#54489=CARTESIAN_POINT('Ctrl Pts',(-68.9197363662121,7.55501595279508,2.37840660705263));
#54490=CARTESIAN_POINT('Ctrl Pts',(-68.949043521386,7.56000010595616,2.3527750972386));
#54491=CARTESIAN_POINT('Ctrl Pts',(-68.9784175370779,7.56515234688882,2.32758855806634));
#54492=CARTESIAN_POINT('Ctrl Pts',(-69.0078470239477,7.57047856294424,2.30285869971681));
#54493=CARTESIAN_POINT('Ctrl Pts',(-69.0811794028085,7.58375042512104,2.24123685256458));
#54494=CARTESIAN_POINT('Ctrl Pts',(-69.154831024795,7.59809903352262,2.18246657147294));
#54495=CARTESIAN_POINT('Ctrl Pts',(-69.2286605473917,7.6136124418366,2.1264662081964));
#54496=CARTESIAN_POINT('Ctrl Pts',(-69.3059090789679,7.62984426848056,2.06787249556368));
#54497=CARTESIAN_POINT('Ctrl Pts',(-69.3833525322979,7.64735154983253,2.0123112110714));
#54498=CARTESIAN_POINT('Ctrl Pts',(-69.4608738698136,7.66622374537447,1.95965407767665));
#54499=CARTESIAN_POINT('Ctrl Pts',(-69.5449564724437,7.68669324924739,1.90254014021424));
#54500=CARTESIAN_POINT('Ctrl Pts',(-69.629130994274,7.70876903418113,1.8488426881589));
#54501=CARTESIAN_POINT('Ctrl Pts',(-69.7132966457926,7.73254554360505,1.79835787559971));
#54502=CARTESIAN_POINT('Ctrl Pts',(-69.7971367364602,7.75623008319924,1.74806834316057));
#54503=CARTESIAN_POINT('Ctrl Pts',(-69.880969193409,7.78160254817844,1.70096571478774));
#54504=CARTESIAN_POINT('Ctrl Pts',(-69.9647281914062,7.80873119754363,1.65681886174829));
#54505=CARTESIAN_POINT('Ctrl Pts',(-70.0380592877499,7.83248236037801,1.61816824257998));
#54506=CARTESIAN_POINT('Ctrl Pts',(-70.1112816378291,7.85755983506915,1.58186156351898));
#54507=CARTESIAN_POINT('Ctrl Pts',(-70.1841143970553,7.8839044258334,1.54766345052146));
#54508=CARTESIAN_POINT('Ctrl Pts',(-70.241950136846,7.9048243925149,1.52050708317151));
#54509=CARTESIAN_POINT('Ctrl Pts',(-70.2995407757624,7.9265426198367,1.49468000367399));
#54510=CARTESIAN_POINT('Ctrl Pts',(-70.3567496590864,7.94900631970774,1.47006601912511));
#54511=CARTESIAN_POINT('Ctrl Pts',(-70.4224156098662,7.97479078051802,1.44181340162984));
#54512=CARTESIAN_POINT('Ctrl Pts',(-70.4875795354592,8.00155856095457,1.41515741744729));
#54513=CARTESIAN_POINT('Ctrl Pts',(-70.5520542732033,8.02916527010112,1.38994245160169));
#54514=CARTESIAN_POINT('Ctrl Pts',(-70.6158157737203,8.05646658626165,1.36500642062193));
#54515=CARTESIAN_POINT('Ctrl Pts',(-70.6789036055966,8.08458833367319,1.34147963066587));
#54516=CARTESIAN_POINT('Ctrl Pts',(-70.7411232251305,8.11334882868581,1.31923720824191));
#54517=CARTESIAN_POINT('Ctrl Pts',(-70.7928520977186,8.1372600642932,1.30074504380507));
#54518=CARTESIAN_POINT('Ctrl Pts',(-70.8439806675348,8.16161202433244,1.28314112432323));
#54519=CARTESIAN_POINT('Ctrl Pts',(-70.8943876832028,8.18627849626928,1.26636748743511));
#54520=CARTESIAN_POINT('Ctrl Pts',(-70.9685642174178,8.22257648724013,1.24168421202093));
#54521=CARTESIAN_POINT('Ctrl Pts',(-71.0412299653039,8.25958269162281,1.21873568845334));
#54522=CARTESIAN_POINT('Ctrl Pts',(-71.1125632075137,8.29718424520714,1.19715207673234));
#54523=CARTESIAN_POINT('Ctrl Pts',(-71.1877147737129,8.33679853380312,1.17441313798763));
#54524=CARTESIAN_POINT('Ctrl Pts',(-71.2613866892902,8.37707311139465,1.153190021763));
#54525=CARTESIAN_POINT('Ctrl Pts',(-71.3337438157902,8.41790617984398,1.13308174347315));
#54526=CARTESIAN_POINT('Ctrl Pts',(-71.4105556377512,8.46125315249983,1.11173549098008));
#54527=CARTESIAN_POINT('Ctrl Pts',(-71.4858851171286,8.50522892886088,1.09164653976952));
#54528=CARTESIAN_POINT('Ctrl Pts',(-71.5598924747369,8.54975360065063,1.07235492453254));
#54529=CARTESIAN_POINT('Ctrl Pts',(-71.6070899451594,8.57814877577616,1.06005188509195));
#54530=CARTESIAN_POINT('Ctrl Pts',(-71.6537489985828,8.60676808056893,1.04807346027955));
#54531=CARTESIAN_POINT('Ctrl Pts',(-71.6999058441912,8.63560026715401,1.03630157777965));
#54532=CARTESIAN_POINT('Ctrl Pts',(-71.704120708006,8.63823311041569,1.03522661520525));
#54533=CARTESIAN_POINT('Ctrl Pts',(-71.708331426215,8.64086748855088,1.03415473800599));
#54534=CARTESIAN_POINT('Ctrl Pts',(-71.7125380276667,8.6435033979355,1.03308584761069));
#54535=CARTESIAN_POINT('',(-63.8800558890744,6.98826998322039,12.652871638431));
#54536=CARTESIAN_POINT('Ctrl Pts',(-63.8800459600055,6.98833961342996,12.652871806017));
#54537=CARTESIAN_POINT('Ctrl Pts',(-63.8800561878002,6.98834112621968,12.6528492302221));
#54538=CARTESIAN_POINT('Ctrl Pts',(-63.8800664155777,6.98834263900889,12.6528266544218));
#54539=CARTESIAN_POINT('Ctrl Pts',(-63.880076643338,6.98834415179758,12.6528040786163));
#54540=CARTESIAN_POINT('Ctrl Pts',(-63.9572793151289,6.99976320410498,12.4823940898988));
#54541=CARTESIAN_POINT('Ctrl Pts',(-64.0340116487795,7.01124392269474,12.3117675918103));
#54542=CARTESIAN_POINT('Ctrl Pts',(-64.1102406561908,7.02272416958815,12.1407419422998));
#54543=CARTESIAN_POINT('Ctrl Pts',(-64.1453347460234,7.02800941243021,12.0620056487097));
#54544=CARTESIAN_POINT('Ctrl Pts',(-64.1803219866163,7.03329450837554,11.9831849600398));
#54545=CARTESIAN_POINT('Ctrl Pts',(-64.2151980126629,7.03857457831673,11.904262701183));
#54546=CARTESIAN_POINT('Ctrl Pts',(-64.3118605224935,7.05320883773364,11.6855215059444));
#54547=CARTESIAN_POINT('Ctrl Pts',(-64.4076718527601,7.0678064597728,11.4660006269974));
#54548=CARTESIAN_POINT('Ctrl Pts',(-64.5025055426427,7.08225064094446,11.2455495972412));
#54549=CARTESIAN_POINT('Ctrl Pts',(-64.5155997988649,7.08424503565182,11.2151106016516));
#54550=CARTESIAN_POINT('Ctrl Pts',(-64.5286753465173,7.0862364629838,11.1846538725359));
#54551=CARTESIAN_POINT('Ctrl Pts',(-64.5417317838301,7.0882245749091,11.1541790127706));
#54552=CARTESIAN_POINT('Ctrl Pts',(-64.6301515191858,7.1016883036492,10.9477996635737));
#54553=CARTESIAN_POINT('Ctrl Pts',(-64.7176988502198,7.11500064672635,10.740587896499));
#54554=CARTESIAN_POINT('Ctrl Pts',(-64.8042231407219,7.12804626582424,10.5324087104427));
#54555=CARTESIAN_POINT('Ctrl Pts',(-64.8363675374695,7.13289280722514,10.4550686442905));
#54556=CARTESIAN_POINT('Ctrl Pts',(-64.8683702418261,7.13770246224527,10.3775951715722));
#54557=CARTESIAN_POINT('Ctrl Pts',(-64.9002217457112,7.14246913199823,10.299981827171));
#54558=CARTESIAN_POINT('Ctrl Pts',(-64.9478661518172,7.1495992552823,10.1838855287595));
#54559=CARTESIAN_POINT('Ctrl Pts',(-64.9951724628551,7.15663301464725,10.0674761822453));
#54560=CARTESIAN_POINT('Ctrl Pts',(-65.0421056966384,7.16354976945968,9.95073637091178));
#54561=CARTESIAN_POINT('Ctrl Pts',(-65.0825059421805,7.16950372937786,9.85024644805254));
#54562=CARTESIAN_POINT('Ctrl Pts',(-65.1226458394789,7.17537320271517,9.7495018816085));
#54563=CARTESIAN_POINT('Ctrl Pts',(-65.1624544957306,7.18113925044134,9.64878744287005));
#54564=CARTESIAN_POINT('Ctrl Pts',(-65.2419384276758,7.19265202651099,9.44769601330832));
#54565=CARTESIAN_POINT('Ctrl Pts',(-65.3201024156781,7.20374940290162,9.24672378317048));
#54566=CARTESIAN_POINT('Ctrl Pts',(-65.3963637810109,7.2143106093483,9.04815217590113));
#54567=CARTESIAN_POINT('Ctrl Pts',(-65.468296331599,7.2242723312986,8.86085206498778));
#54568=CARTESIAN_POINT('Ctrl Pts',(-65.5385340583308,7.23375700647539,8.67568850949559));
#54569=CARTESIAN_POINT('Ctrl Pts',(-65.6065923143366,7.24270648257226,8.49458419430487));
#54570=CARTESIAN_POINT('Ctrl Pts',(-65.6502509006398,7.24844746827295,8.37840786480911));
#54571=CARTESIAN_POINT('Ctrl Pts',(-65.6930128012289,7.25396914188262,8.26390206970707));
#54572=CARTESIAN_POINT('Ctrl Pts',(-65.7347567854724,7.25926556663905,8.15157432823398));
#54573=CARTESIAN_POINT('Ctrl Pts',(-65.7364420781083,7.25947939447078,8.14703942053546));
#54574=CARTESIAN_POINT('Ctrl Pts',(-65.7381257216343,7.25969285723204,8.14250805592864));
#54575=CARTESIAN_POINT('Ctrl Pts',(-65.739807721741,7.25990595645158,8.13798023872227));
#54576=CARTESIAN_POINT('Ctrl Pts',(-65.8100377537922,7.26880367587444,7.94892629855544));
#54577=CARTESIAN_POINT('Ctrl Pts',(-65.8773985543478,7.27706623739923,7.76605796002971));
#54578=CARTESIAN_POINT('Ctrl Pts',(-65.9423265821899,7.28481922328194,7.58967481592044));
#54579=CARTESIAN_POINT('Ctrl Pts',(-66.0095897680272,7.29285104786611,7.40694799369743));
#54580=CARTESIAN_POINT('Ctrl Pts',(-66.0742418673935,7.30033681706775,7.23118091907675));
#54581=CARTESIAN_POINT('Ctrl Pts',(-66.1368236734351,7.30742582948383,7.06269520960938));
#54582=CARTESIAN_POINT('Ctrl Pts',(-66.1929759980861,7.31378653640203,6.91151925519911));
#54583=CARTESIAN_POINT('Ctrl Pts',(-66.2474625884719,7.31982822145605,6.76620507781348));
#54584=CARTESIAN_POINT('Ctrl Pts',(-66.3007095158743,7.32565790933545,6.62698064789046));
#54585=CARTESIAN_POINT('',(-60.9536795918073,6.58767285120433,18.6650422826135));
#54586=CARTESIAN_POINT('Ctrl Pts',(-60.9536795918073,6.58767285120433,18.6650422826135));
#54587=CARTESIAN_POINT('Ctrl Pts',(-61.1064136681965,6.60882453290174,18.397171129156));
#54588=CARTESIAN_POINT('Ctrl Pts',(-61.4026533876799,6.64953999991258,17.8502351016645));
#54589=CARTESIAN_POINT('Ctrl Pts',(-61.8813511258638,6.71394676359331,16.8972049262099));
#54590=CARTESIAN_POINT('Ctrl Pts',(-62.313674056402,6.7713543457067,16.0028732107663));
#54591=CARTESIAN_POINT('Ctrl Pts',(-62.7048717197328,6.82345654645031,15.1819379428255));
#54592=CARTESIAN_POINT('Ctrl Pts',(-63.2386855526803,6.89569253577236,14.0502307887768));
#54593=CARTESIAN_POINT('Ctrl Pts',(-63.6251462417326,6.95055614069076,13.2159876874408));
#54594=CARTESIAN_POINT('Ctrl Pts',(-63.88006477921,6.98820763880422,12.6528714883805));
#54595=CARTESIAN_POINT('',(-48.943686428043,5.01441858224854,24.6839747939812));
#54596=CARTESIAN_POINT('Ctrl Pts',(-48.943686427953,5.01441858311083,24.6839747939811));
#54597=CARTESIAN_POINT('Ctrl Pts',(-48.9436933030855,5.01441930127938,24.6839740301331));
#54598=CARTESIAN_POINT('Ctrl Pts',(-48.9437001782249,5.01442001944909,24.6839732662801));
#54599=CARTESIAN_POINT('Ctrl Pts',(-48.9437070533713,5.01442073761994,24.6839725024221));
#54600=CARTESIAN_POINT('Ctrl Pts',(-49.2104058457392,5.04227982433237,24.6543411359102));
#54601=CARTESIAN_POINT('Ctrl Pts',(-49.4876048491357,5.0718742454339,24.6172984586111));
#54602=CARTESIAN_POINT('Ctrl Pts',(-49.7724012808886,5.10302368190886,24.5737464914054));
#54603=CARTESIAN_POINT('Ctrl Pts',(-50.0079486615118,5.12878653337579,24.5377258441904));
#54604=CARTESIAN_POINT('Ctrl Pts',(-50.2486931821281,5.15561239316509,24.4972525288513));
#54605=CARTESIAN_POINT('Ctrl Pts',(-50.4929944974496,5.18337221375705,24.4528377619485));
#54606=CARTESIAN_POINT('Ctrl Pts',(-50.7766538286848,5.21560426348613,24.4012675808382));
#54607=CARTESIAN_POINT('Ctrl Pts',(-51.0651079819501,5.24909696850875,24.3443836308993));
#54608=CARTESIAN_POINT('Ctrl Pts',(-51.3558112857037,5.28357192459843,24.2829878673439));
#54609=CARTESIAN_POINT('Ctrl Pts',(-51.6520246136125,5.31870032300662,24.220428401361));
#54610=CARTESIAN_POINT('Ctrl Pts',(-51.9505734679519,5.35484840513919,24.1531844876066));
#54611=CARTESIAN_POINT('Ctrl Pts',(-52.2487678361982,5.39166710815415,24.0821063528286));
#54612=CARTESIAN_POINT('Ctrl Pts',(-52.55816891618,5.42986952808365,24.0083569665047));
#54613=CARTESIAN_POINT('Ctrl Pts',(-52.867188802127,5.46879371681604,23.9304798136703));
#54614=CARTESIAN_POINT('Ctrl Pts',(-53.172820278291,5.50799417252183,23.8494259008386));
#54615=CARTESIAN_POINT('Ctrl Pts',(-53.2063458833143,5.51229418445523,23.8405348615343));
#54616=CARTESIAN_POINT('Ctrl Pts',(-53.2398307108533,5.51659746965907,23.8316055983123));
#54617=CARTESIAN_POINT('Ctrl Pts',(-53.273270786351,5.52090340344408,23.822639366649));
#54618=CARTESIAN_POINT('Ctrl Pts',(-53.4433076524457,5.54279831472997,23.7770476653738));
#54619=CARTESIAN_POINT('Ctrl Pts',(-53.6121875240046,5.56476198960391,23.7305001411357));
#54620=CARTESIAN_POINT('Ctrl Pts',(-53.7793893479847,5.58669844287257,23.6831595754526));
#54621=CARTESIAN_POINT('Ctrl Pts',(-54.093173328354,5.62786610156178,23.5943165785321));
#54622=CARTESIAN_POINT('Ctrl Pts',(-54.4010372363093,5.6689398394008,23.5026837491855));
#54623=CARTESIAN_POINT('Ctrl Pts',(-54.6974294149276,5.70897076501432,23.4097505788098));
#54624=CARTESIAN_POINT('Ctrl Pts',(-54.9414822833493,5.74193270843367,23.3332282936825));
#54625=CARTESIAN_POINT('Ctrl Pts',(-55.1777570043168,5.77418559781669,23.2558242895775));
#54626=CARTESIAN_POINT('Ctrl Pts',(-55.4031331947367,5.80518387641173,23.1783707257999));
#54627=CARTESIAN_POINT('Ctrl Pts',(-55.6070057675119,5.83322454387087,23.1083071698912));
#54628=CARTESIAN_POINT('Ctrl Pts',(-55.8019601413752,5.86023797808104,23.0382030434586));
#54629=CARTESIAN_POINT('Ctrl Pts',(-55.9856699657615,5.88582111046705,22.9686751793201));
#54630=CARTESIAN_POINT('Ctrl Pts',(-56.0107942755779,5.88931988113044,22.9591664902485));
#54631=CARTESIAN_POINT('Ctrl Pts',(-56.0357087956219,5.89279198396761,22.949668578276));
#54632=CARTESIAN_POINT('Ctrl Pts',(-56.0604194770111,5.89623806282833,22.9401792214321));
#54633=CARTESIAN_POINT('Ctrl Pts',(-56.2634514356021,5.92455230190299,22.8622112093225));
#54634=CARTESIAN_POINT('Ctrl Pts',(-56.4527203540863,5.95110528147132,22.7848206242314));
#54635=CARTESIAN_POINT('Ctrl Pts',(-56.6315152700827,5.97627685995714,22.706775556212));
#54636=CARTESIAN_POINT('Ctrl Pts',(-56.8341077358789,6.00479876800473,22.6183427130007));
#54637=CARTESIAN_POINT('Ctrl Pts',(-57.0232522057511,6.03154794669356,22.529069618797));
#54638=CARTESIAN_POINT('Ctrl Pts',(-57.2037695117562,6.0571386150431,22.4371655163732));
#54639=CARTESIAN_POINT('Ctrl Pts',(-57.3334050691406,6.07551613589554,22.3711660850317));
#54640=CARTESIAN_POINT('Ctrl Pts',(-57.4585922263825,6.09329753291716,22.3038098301435));
#54641=CARTESIAN_POINT('Ctrl Pts',(-57.5811269320388,6.11072246502127,22.2344337090417));
#54642=CARTESIAN_POINT('Ctrl Pts',(-57.7960199612812,6.14128112531378,22.1127665883611));
#54643=CARTESIAN_POINT('Ctrl Pts',(-58.002734874994,6.17074052332906,21.9848890384924));
#54644=CARTESIAN_POINT('Ctrl Pts',(-58.2027480597424,6.19925187141741,21.8478966424791));
#54645=CARTESIAN_POINT('Ctrl Pts',(-58.2856305930849,6.21106655634201,21.7911290006634));
#54646=CARTESIAN_POINT('Ctrl Pts',(-58.3673628401942,6.22271872520401,21.7327962746785));
#54647=CARTESIAN_POINT('Ctrl Pts',(-58.4480523143857,6.23422017683554,21.6726921818843));
#54648=CARTESIAN_POINT('Ctrl Pts',(-58.5904224605179,6.25451357155549,21.5666433005403));
#54649=CARTESIAN_POINT('Ctrl Pts',(-58.7295450374508,6.27433754426476,21.4550796143134));
#54650=CARTESIAN_POINT('Ctrl Pts',(-58.866025069094,6.29376041498173,21.3368706761723));
#54651=CARTESIAN_POINT('Ctrl Pts',(-58.8669089202096,6.29388619840766,21.3361051495191));
#54652=CARTESIAN_POINT('Ctrl Pts',(-58.8677926605737,6.29401196502538,21.335339344183));
#54653=CARTESIAN_POINT('Ctrl Pts',(-58.8686762903519,6.29413771485699,21.3345732598584));
#54654=CARTESIAN_POINT('Ctrl Pts',(-59.0693160286427,6.32269086451823,21.1606237595298));
#54655=CARTESIAN_POINT('Ctrl Pts',(-59.2642396750474,6.35037577232071,20.9722889479987));
#54656=CARTESIAN_POINT('Ctrl Pts',(-59.4520298320428,6.37697681306191,20.7716602375005));
#54657=CARTESIAN_POINT('Ctrl Pts',(-59.6398199890382,6.40357785380311,20.5710315270023));
#54658=CARTESIAN_POINT('Ctrl Pts',(-59.8204767928905,6.42909479775789,20.3581090997196));
#54659=CARTESIAN_POINT('Ctrl Pts',(-59.9926310538925,6.45333012417932,20.134997670789));
#54660=CARTESIAN_POINT('Ctrl Pts',(-60.1295309743094,6.47260245725467,19.9575757662313));
#54661=CARTESIAN_POINT('Ctrl Pts',(-60.2610708473564,6.49106748603937,19.773713601681));
#54662=CARTESIAN_POINT('Ctrl Pts',(-60.3891143826253,6.50898792976107,19.5828383420744));
#54663=CARTESIAN_POINT('Ctrl Pts',(-60.5104434499889,6.52596864431983,19.4019723797108));
#54664=CARTESIAN_POINT('Ctrl Pts',(-60.6286331300441,6.54246035334563,19.2148094425513));
#54665=CARTESIAN_POINT('Ctrl Pts',(-60.7453139889917,6.55869185993184,19.020871129382));
#54666=CARTESIAN_POINT('Ctrl Pts',(-60.8151920342546,6.56841261415106,18.9047249992618));
#54667=CARTESIAN_POINT('Ctrl Pts',(-60.8845297938964,6.57804014476984,18.7861489951842));
#54668=CARTESIAN_POINT('Ctrl Pts',(-60.9536863008776,6.58762473125413,18.665042306171));
#54669=CARTESIAN_POINT('',(-43.998256547978,4.57019747403691,24.6840336608423));
#54670=CARTESIAN_POINT('Ctrl Pts',(-43.9982565479099,4.57019747493893,24.6840336608423));
#54671=CARTESIAN_POINT('Ctrl Pts',(-44.7983004349469,4.63056911424585,24.7634007046597));
#54672=CARTESIAN_POINT('Ctrl Pts',(-45.6065458290174,4.69707310585867,24.8079761534353));
#54673=CARTESIAN_POINT('Ctrl Pts',(-47.2553606707774,4.84445121892603,24.8169837372541));
#54674=CARTESIAN_POINT('Ctrl Pts',(-48.1045754985842,4.92676600513598,24.7772030223014));
#54675=CARTESIAN_POINT('Ctrl Pts',(-48.943686427953,5.01441858311083,24.6839747939812));
#54676=CARTESIAN_POINT('',(-30.3134449265951,4.07585591331178,18.6659931355377));
#54677=CARTESIAN_POINT('Ctrl Pts',(-30.3134449302137,4.07585425011609,18.665993135544));
#54678=CARTESIAN_POINT('Ctrl Pts',(-30.5181570460434,4.07629984775709,18.8492527201676));
#54679=CARTESIAN_POINT('Ctrl Pts',(-30.7306280520902,4.07692382601424,19.032878104075));
#54680=CARTESIAN_POINT('Ctrl Pts',(-30.9534488453249,4.07782080148265,19.2181909065929));
#54681=CARTESIAN_POINT('Ctrl Pts',(-31.1681448217793,4.07868507012316,19.396746563399));
#54682=CARTESIAN_POINT('Ctrl Pts',(-31.3924496744848,4.07980188235618,19.5768689665312));
#54683=CARTESIAN_POINT('Ctrl Pts',(-31.6286796916658,4.08130139885299,19.7597442125536));
#54684=CARTESIAN_POINT('Ctrl Pts',(-31.7324682166588,4.08196021692897,19.8400911230304));
#54685=CARTESIAN_POINT('Ctrl Pts',(-31.8385587306746,4.08269424598024,19.920968736235));
#54686=CARTESIAN_POINT('Ctrl Pts',(-31.945633483405,4.08350482910259,20.0014046313493));
#54687=CARTESIAN_POINT('Ctrl Pts',(-32.0868798312397,4.08457409989452,20.1075106566261));
#54688=CARTESIAN_POINT('Ctrl Pts',(-32.2298388402814,4.08577749941939,20.2128481180817));
#54689=CARTESIAN_POINT('Ctrl Pts',(-32.3714856621259,4.08709818275659,20.31518127585));
#54690=CARTESIAN_POINT('Ctrl Pts',(-32.6205108244127,4.08942003776253,20.4950902274858));
#54691=CARTESIAN_POINT('Ctrl Pts',(-32.8654802639302,4.09209932738748,20.6657155719101));
#54692=CARTESIAN_POINT('Ctrl Pts',(-33.1064729800666,4.0951370942871,20.8281355915901));
#54693=CARTESIAN_POINT('Ctrl Pts',(-33.3420167258229,4.09810617570061,20.9868832103339));
#54694=CARTESIAN_POINT('Ctrl Pts',(-33.5737828997118,4.10141821376346,21.1378098526377));
#54695=CARTESIAN_POINT('Ctrl Pts',(-33.801596834306,4.10506508715158,21.2813307553833));
#54696=CARTESIAN_POINT('Ctrl Pts',(-34.0187745948657,4.10854169536209,21.4181509560761));
#54697=CARTESIAN_POINT('Ctrl Pts',(-34.2323606929839,4.11232238479546,21.5482409335746));
#54698=CARTESIAN_POINT('Ctrl Pts',(-34.4422091994987,4.11638534088304,21.6719655411268));
#54699=CARTESIAN_POINT('Ctrl Pts',(-34.6983862296924,4.12134528099226,21.8230049888265));
#54700=CARTESIAN_POINT('Ctrl Pts',(-34.9489931041619,4.12672608777494,21.9645581634061));
#54701=CARTESIAN_POINT('Ctrl Pts',(-35.1937750867211,4.13247990804728,22.0972961327151));
#54702=CARTESIAN_POINT('Ctrl Pts',(-35.4313178144435,4.13806356313507,22.2261084700136));
#54703=CARTESIAN_POINT('Ctrl Pts',(-35.6633753700192,4.14399822754493,22.3466194588185));
#54704=CARTESIAN_POINT('Ctrl Pts',(-35.8897221244981,4.15022593205858,22.4594474749716));
#54705=CARTESIAN_POINT('Ctrl Pts',(-36.1280821148351,4.15678416873891,22.5782637791943));
#54706=CARTESIAN_POINT('Ctrl Pts',(-36.3601091602886,4.16366732082402,22.688560022379));
#54707=CARTESIAN_POINT('Ctrl Pts',(-36.5855452007813,4.17080074833602,22.7910624884676));
#54708=CARTESIAN_POINT('Ctrl Pts',(-36.9014638915004,4.18079730024053,22.9347060904907));
#54709=CARTESIAN_POINT('Ctrl Pts',(-37.2044390322616,4.19128489538215,23.0630439489659));
#54710=CARTESIAN_POINT('Ctrl Pts',(-37.4937605320397,4.20203012125431,23.1780823421347));
#54711=CARTESIAN_POINT('Ctrl Pts',(-37.6593150137322,4.20817871477847,23.2439091872548));
#54712=CARTESIAN_POINT('Ctrl Pts',(-37.8203989701946,4.21441160013928,23.3053814950684));
#54713=CARTESIAN_POINT('Ctrl Pts',(-37.9768795174009,4.22068493286446,23.362875825288));
#54714=CARTESIAN_POINT('Ctrl Pts',(-37.9980459759114,4.22153349991782,23.370652838961));
#54715=CARTESIAN_POINT('Ctrl Pts',(-38.0191282062722,4.22238280724491,23.3783570687426));
#54716=CARTESIAN_POINT('Ctrl Pts',(-38.0401258778123,4.22323274137395,23.385989447289));
#54717=CARTESIAN_POINT('Ctrl Pts',(-38.4250493867617,4.23881349882616,23.5259041004981));
#54718=CARTESIAN_POINT('Ctrl Pts',(-38.7814993652197,4.25460815954868,23.6416161168415));
#54719=CARTESIAN_POINT('Ctrl Pts',(-39.1025011525761,4.26968007837109,23.7382724472324));
#54720=CARTESIAN_POINT('Ctrl Pts',(-39.1939361781236,4.2739732048796,23.7658043002834));
#54721=CARTESIAN_POINT('Ctrl Pts',(-39.2824949682192,4.27820734981913,23.7917900658136));
#54722=CARTESIAN_POINT('Ctrl Pts',(-39.3680159669074,4.28236034493513,23.81634868312));
#54723=CARTESIAN_POINT('Ctrl Pts',(-39.5018516789771,4.28885955643987,23.8547815836366));
#54724=CARTESIAN_POINT('Ctrl Pts',(-39.6282476293091,4.29515990196685,23.8897193222904));
#54725=CARTESIAN_POINT('Ctrl Pts',(-39.7465823943656,4.30117637238633,23.92161762482));
#54726=CARTESIAN_POINT('Ctrl Pts',(-39.8741179109594,4.30766063474704,23.9559960806325));
#54727=CARTESIAN_POINT('Ctrl Pts',(-39.9922928698564,4.31381067584175,23.98684415462));
#54728=CARTESIAN_POINT('Ctrl Pts',(-40.1070321775967,4.31989179764076,24.0158116417197));
#54729=CARTESIAN_POINT('Ctrl Pts',(-40.1989532767345,4.32476356661657,24.0390183640358));
#54730=CARTESIAN_POINT('Ctrl Pts',(-40.2886693510511,4.32959237034955,24.0610181045133));
#54731=CARTESIAN_POINT('Ctrl Pts',(-40.3792268216836,4.3345384269169,24.0826590548447));
#54732=CARTESIAN_POINT('Ctrl Pts',(-40.5550100507714,4.34413933326496,24.124666810839));
#54733=CARTESIAN_POINT('Ctrl Pts',(-40.7339621950764,4.35418390708394,24.1653227568943));
#54734=CARTESIAN_POINT('Ctrl Pts',(-40.9199894723898,4.36493764138614,24.2052754880848));
#54735=CARTESIAN_POINT('Ctrl Pts',(-40.9494216450215,4.3666390357676,24.2115965808756));
#54736=CARTESIAN_POINT('Ctrl Pts',(-40.9790309204839,4.3683582876528,24.2179000708525));
#54737=CARTESIAN_POINT('Ctrl Pts',(-41.0088327685384,4.37009657042689,24.224188526569));
#54738=CARTESIAN_POINT('Ctrl Pts',(-41.2587538625024,4.38467397286592,24.2769241062269));
#54739=CARTESIAN_POINT('Ctrl Pts',(-41.522215837609,4.4005938813599,24.3286024290861));
#54740=CARTESIAN_POINT('Ctrl Pts',(-41.7959610673191,4.41781281081743,24.3778619523168));
#54741=CARTESIAN_POINT('Ctrl Pts',(-41.9123878923407,4.42513620888773,24.3988125635764));
#54742=CARTESIAN_POINT('Ctrl Pts',(-42.030674852438,4.43269397282911,24.4193256463625));
#54743=CARTESIAN_POINT('Ctrl Pts',(-42.1505713508101,4.44047982652793,24.439296481844));
#54744=CARTESIAN_POINT('Ctrl Pts',(-42.2409398060512,4.44634818449541,24.4543489110379));
#54745=CARTESIAN_POINT('Ctrl Pts',(-42.3322226369957,4.45234608023781,24.4690932928778));
#54746=CARTESIAN_POINT('Ctrl Pts',(-42.42431198011,4.45847033217187,24.4834847584958));
#54747=CARTESIAN_POINT('Ctrl Pts',(-42.784797503065,4.48244383536452,24.5398204302896));
#54748=CARTESIAN_POINT('Ctrl Pts',(-43.1576489772132,4.5083540926368,24.590748313527));
#54749=CARTESIAN_POINT('Ctrl Pts',(-43.5419429082308,4.5363561170648,24.635085509321));
#54750=CARTESIAN_POINT('Ctrl Pts',(-43.6923106007685,4.54731283394157,24.6524339014944));
#54751=CARTESIAN_POINT('Ctrl Pts',(-43.8444299906764,4.55858966891662,24.6687732511125));
#54752=CARTESIAN_POINT('Ctrl Pts',(-43.9982463104202,4.57019670241406,24.6840326452309));
#54753=CARTESIAN_POINT('Ctrl Pts',(-43.9982497229159,4.57019695992218,24.6840329837686));
#54754=CARTESIAN_POINT('Ctrl Pts',(-43.9982531354125,4.57019721743047,24.6840333223057));
#54755=CARTESIAN_POINT('Ctrl Pts',(-43.9982565479099,4.57019747493892,24.6840336608423));
#54756=CARTESIAN_POINT('',(-25.4568055127478,4.0805540095759,12.6479974296003));
#54757=CARTESIAN_POINT('Ctrl Pts',(-25.4568055127484,4.08055401005756,12.6479974296003));
#54758=CARTESIAN_POINT('Ctrl Pts',(-27.0327363192644,4.07841070070495,15.0082590047032));
#54759=CARTESIAN_POINT('Ctrl Pts',(-28.2185108053635,4.07131231245263,16.7905674249077));
#54760=CARTESIAN_POINT('Ctrl Pts',(-30.3134449229829,4.07585757700934,18.6659931355318));
#54761=CARTESIAN_POINT('',(-21.1401509099359,4.08071597508933,6.62997962237056));
#54762=CARTESIAN_POINT('Ctrl Pts',(-21.1401574799756,4.08071597981543,6.62998826233523));
#54763=CARTESIAN_POINT('Ctrl Pts',(-21.4692458061929,4.08095270291158,7.06232595293004));
#54764=CARTESIAN_POINT('Ctrl Pts',(-21.7882670410954,4.08118452196195,7.48072007481999));
#54765=CARTESIAN_POINT('Ctrl Pts',(-22.1061108542803,4.08137642561277,7.90235762953136));
#54766=CARTESIAN_POINT('Ctrl Pts',(-22.284711446525,4.08148425878198,8.13928128152719));
#54767=CARTESIAN_POINT('Ctrl Pts',(-22.4629415192341,4.0815794918012,8.37723040795624));
#54768=CARTESIAN_POINT('Ctrl Pts',(-22.6423690871753,4.08165601858648,8.61922908722337));
#54769=CARTESIAN_POINT('Ctrl Pts',(-22.7822570470729,4.08171568152453,8.80789965735382));
#54770=CARTESIAN_POINT('Ctrl Pts',(-22.9228728197913,4.0817639754497,8.99903144132748));
#54771=CARTESIAN_POINT('Ctrl Pts',(-23.0649499739826,4.08179806827018,9.19403707854816));
#54772=CARTESIAN_POINT('Ctrl Pts',(-23.089242443057,4.08180389748876,9.22737930333079));
#54773=CARTESIAN_POINT('Ctrl Pts',(-23.1135776064206,4.0818093117026,9.26083472002905));
#54774=CARTESIAN_POINT('Ctrl Pts',(-23.1379446185742,4.08181430925493,9.29438788392053));
#54775=CARTESIAN_POINT('Ctrl Pts',(-23.2474269721439,4.08183676353811,9.44514413295864));
#54776=CARTESIAN_POINT('Ctrl Pts',(-23.3579353512576,4.08184894949124,9.59840224218975));
#54777=CARTESIAN_POINT('Ctrl Pts',(-23.4683481026768,4.08185062199027,9.75258737280672));
#54778=CARTESIAN_POINT('Ctrl Pts',(-23.6195577047054,4.08185291246768,9.96374298608199));
#54779=CARTESIAN_POINT('Ctrl Pts',(-23.7705834817783,4.08183546777614,10.1766325430206));
#54780=CARTESIAN_POINT('Ctrl Pts',(-23.9185172660665,4.08179797831881,10.3871359698167));
#54781=CARTESIAN_POINT('Ctrl Pts',(-24.0197941038079,4.08177231268939,10.5312485638547));
#54782=CARTESIAN_POINT('Ctrl Pts',(-24.1196208989452,4.08173725990457,10.6742407070177));
#54783=CARTESIAN_POINT('Ctrl Pts',(-24.2170854846451,4.08169283385564,10.8148087558425));
#54784=CARTESIAN_POINT('Ctrl Pts',(-24.2619861753325,4.08167236734191,10.8795666618601));
#54785=CARTESIAN_POINT('Ctrl Pts',(-24.3063859262931,4.08164991286656,10.9438105322975));
#54786=CARTESIAN_POINT('Ctrl Pts',(-24.3501981466148,4.08162547894153,11.0074159299064));
#54787=CARTESIAN_POINT('Ctrl Pts',(-24.3825541098732,4.08160743413177,11.0543894430712));
#54788=CARTESIAN_POINT('Ctrl Pts',(-24.4145897119851,4.08158830987438,11.1010148268432));
#54789=CARTESIAN_POINT('Ctrl Pts',(-24.4463194375088,4.08156817329577,11.147301956624));
#54790=CARTESIAN_POINT('Ctrl Pts',(-24.5269242714908,4.08151701919503,11.2648877960821));
#54791=CARTESIAN_POINT('Ctrl Pts',(-24.6061395773467,4.08145979701039,11.3811447622533));
#54792=CARTESIAN_POINT('Ctrl Pts',(-24.6840716542324,4.08139685593094,11.4960646524234));
#54793=CARTESIAN_POINT('Ctrl Pts',(-24.7705692911081,4.08132699696077,11.6236154546984));
#54794=CARTESIAN_POINT('Ctrl Pts',(-24.8554863518349,4.08125009280203,11.7495191699868));
#54795=CARTESIAN_POINT('Ctrl Pts',(-24.939014259396,4.08116678926922,11.8738119545452));
#54796=CARTESIAN_POINT('Ctrl Pts',(-25.033126716636,4.08107292961922,12.013854961889));
#54797=CARTESIAN_POINT('Ctrl Pts',(-25.1254766313393,4.08097094742442,12.1518534862534));
#54798=CARTESIAN_POINT('Ctrl Pts',(-25.2163841921841,4.08086196114674,12.2879118774981));
#54799=CARTESIAN_POINT('Ctrl Pts',(-25.2975937607871,4.08076460149357,12.4094555990007));
#54800=CARTESIAN_POINT('Ctrl Pts',(-25.3776540492092,4.08066165823048,12.5294527346467));
#54801=CARTESIAN_POINT('Ctrl Pts',(-25.4568055127484,4.08055401005756,12.6479974296003));
#54802=CARTESIAN_POINT('',(-16.686777128013,4.07896401785927,0.570989604234123));
#54803=CARTESIAN_POINT('Ctrl Pts',(-16.6867771273137,4.07896172090824,0.570989650428049));
#54804=CARTESIAN_POINT('Ctrl Pts',(-16.7841459689088,4.08162687912007,0.704986248288088));
#54805=CARTESIAN_POINT('Ctrl Pts',(-16.880846010462,4.08355025119849,0.838584067301125));
#54806=CARTESIAN_POINT('Ctrl Pts',(-16.9766362404799,4.08495392785334,0.971294459765536));
#54807=CARTESIAN_POINT('Ctrl Pts',(-17.0096954643441,4.08543836620115,1.01709560851285));
#54808=CARTESIAN_POINT('Ctrl Pts',(-17.0426464502949,4.08586064648245,1.0627911508977));
#54809=CARTESIAN_POINT('Ctrl Pts',(-17.0754929950314,4.08622882894667,1.10837987529852));
#54810=CARTESIAN_POINT('Ctrl Pts',(-17.1731007695106,4.08732293096634,1.24385269187051));
#54811=CARTESIAN_POINT('Ctrl Pts',(-17.2697875086632,4.08794300664813,1.37838378599298));
#54812=CARTESIAN_POINT('Ctrl Pts',(-17.3656435015793,4.08826316038151,1.51193079495319));
#54813=CARTESIAN_POINT('Ctrl Pts',(-17.4642655981198,4.08859255274855,1.6493315521692));
#54814=CARTESIAN_POINT('Ctrl Pts',(-17.5620082347372,4.0886040867082,1.7856907594135));
#54815=CARTESIAN_POINT('Ctrl Pts',(-17.6589529261752,4.08843757506459,1.92093947295767));
#54816=CARTESIAN_POINT('Ctrl Pts',(-17.7610551734985,4.0882622048327,2.06338355520294));
#54817=CARTESIAN_POINT('Ctrl Pts',(-17.8622722619584,4.08788904084334,2.20459606314489));
#54818=CARTESIAN_POINT('Ctrl Pts',(-17.9626819456571,4.08743203252299,2.34446843489057));
#54819=CARTESIAN_POINT('Ctrl Pts',(-17.9857716705684,4.08732694110143,2.37663280855774));
#54820=CARTESIAN_POINT('Ctrl Pts',(-18.0088224426463,4.08721631990852,2.40873151016149));
#54821=CARTESIAN_POINT('Ctrl Pts',(-18.0318289356247,4.08710273253635,2.440754419878));
#54822=CARTESIAN_POINT('Ctrl Pts',(-18.0826477931075,4.08685183030264,2.51148956784678));
#54823=CARTESIAN_POINT('Ctrl Pts',(-18.1332504270625,4.08658646050215,2.58185461834398));
#54824=CARTESIAN_POINT('Ctrl Pts',(-18.1836567657045,4.08631176891754,2.65186612027432));
#54825=CARTESIAN_POINT('Ctrl Pts',(-18.2770994146918,4.08580254904538,2.78165257920393));
#54826=CARTESIAN_POINT('Ctrl Pts',(-18.3694162091785,4.08527202707044,2.90959746665377));
#54827=CARTESIAN_POINT('Ctrl Pts',(-18.4612811429612,4.08475867356178,3.03657594574594));
#54828=CARTESIAN_POINT('Ctrl Pts',(-18.4688691213433,4.08471627092602,3.04706427806888));
#54829=CARTESIAN_POINT('Ctrl Pts',(-18.4764540006169,4.08467398512724,3.05754599355073));
#54830=CARTESIAN_POINT('Ctrl Pts',(-18.4840361525888,4.08463183770619,3.06802157368569));
#54831=CARTESIAN_POINT('Ctrl Pts',(-18.5451231850346,4.08429226908686,3.15242005395425));
#54832=CARTESIAN_POINT('Ctrl Pts',(-18.6060211115761,4.08396170556085,3.23640371253096));
#54833=CARTESIAN_POINT('Ctrl Pts',(-18.6669509110043,4.08364541281635,3.32026056370214));
#54834=CARTESIAN_POINT('Ctrl Pts',(-18.7190814341725,4.0833747980039,3.39200709107969));
#54835=CARTESIAN_POINT('Ctrl Pts',(-18.7712351265386,4.08311462674048,3.46366056109551));
#54836=CARTESIAN_POINT('Ctrl Pts',(-18.8235118219749,4.08286882610003,3.53534797170876));
#54837=CARTESIAN_POINT('Ctrl Pts',(-18.8441314456826,4.08277187435756,3.56362381085831));
#54838=CARTESIAN_POINT('Ctrl Pts',(-18.8647718882406,4.08267706144966,3.59190722809431));
#54839=CARTESIAN_POINT('Ctrl Pts',(-18.8854405400068,4.08258452488808,3.62020769046226));
#54840=CARTESIAN_POINT('Ctrl Pts',(-18.9139413939724,4.08245692241754,3.6592323619423));
#54841=CARTESIAN_POINT('Ctrl Pts',(-18.94249588657,4.08233365051722,3.69828944962005));
#54842=CARTESIAN_POINT('Ctrl Pts',(-18.9711233744466,4.08221500263331,3.73740362574907));
#54843=CARTESIAN_POINT('Ctrl Pts',(-19.0606946304323,4.08184377061924,3.8597862077566));
#54844=CARTESIAN_POINT('Ctrl Pts',(-19.1509291277118,4.08151777088175,3.98265901523723));
#54845=CARTESIAN_POINT('Ctrl Pts',(-19.242528424724,4.08124251797849,4.10691573705344));
#54846=CARTESIAN_POINT('Ctrl Pts',(-19.2635485518487,4.08117935318131,4.1354300616593));
#54847=CARTESIAN_POINT('Ctrl Pts',(-19.2846407111546,4.08111887286734,4.16401739825223));
#54848=CARTESIAN_POINT('Ctrl Pts',(-19.3058137050309,4.08106116769549,4.19268882867069));
#54849=CARTESIAN_POINT('Ctrl Pts',(-19.3322323911041,4.0809891658412,4.2284637183211));
#54850=CARTESIAN_POINT('Ctrl Pts',(-19.3587769939038,4.08092148536531,4.26436962064455));
#54851=CARTESIAN_POINT('Ctrl Pts',(-19.3854337817106,4.08085764253541,4.30038893000356));
#54852=CARTESIAN_POINT('Ctrl Pts',(-19.39842995467,4.08082651678742,4.31794967954701));
#54853=CARTESIAN_POINT('Ctrl Pts',(-19.4114573113798,4.08079638090457,4.33554349027692));
#54854=CARTESIAN_POINT('Ctrl Pts',(-19.4245173432076,4.08076723479642,4.35317245358558));
#54855=CARTESIAN_POINT('Ctrl Pts',(-19.489472938666,4.08062227321939,4.44085216402782));
#54856=CARTESIAN_POINT('Ctrl Pts',(-19.5537417608887,4.08050583169764,4.52738438607107));
#54857=CARTESIAN_POINT('Ctrl Pts',(-19.6173542232542,4.08041287513929,4.61284247073614));
#54858=CARTESIAN_POINT('Ctrl Pts',(-19.6961025636338,4.08029780060161,4.7186343563062));
#54859=CARTESIAN_POINT('Ctrl Pts',(-19.7738497167904,4.08021869702705,4.82278679314521));
#54860=CARTESIAN_POINT('Ctrl Pts',(-19.8506921953251,4.08016901437943,4.92546814305012));
#54861=CARTESIAN_POINT('Ctrl Pts',(-19.885211075738,4.08014669613301,4.97159426112431));
#54862=CARTESIAN_POINT('Ctrl Pts',(-19.919553701739,4.08013009809011,5.01743162922105));
#54863=CARTESIAN_POINT('Ctrl Pts',(-19.9537115876116,4.08011650017662,5.06297116675175));
#54864=CARTESIAN_POINT('Ctrl Pts',(-19.9695992615268,4.08011017545218,5.08415272714558));
#54865=CARTESIAN_POINT('Ctrl Pts',(-19.9854469188514,4.08010450048555,5.1052697797261));
#54866=CARTESIAN_POINT('Ctrl Pts',(-20.0012608379634,4.08009922299098,5.1263311055391));
#54867=CARTESIAN_POINT('Ctrl Pts',(-20.0876094687218,4.08007040632468,5.24133211401896));
#54868=CARTESIAN_POINT('Ctrl Pts',(-20.1728585866075,4.08007004066717,5.35454628879534));
#54869=CARTESIAN_POINT('Ctrl Pts',(-20.2571125809195,4.08009030729853,5.46618501499764));
#54870=CARTESIAN_POINT('Ctrl Pts',(-20.3344593924838,4.08010891246175,5.56867154503511));
#54871=CARTESIAN_POINT('Ctrl Pts',(-20.4109698888398,4.08014488839819,5.66983361846497));
#54872=CARTESIAN_POINT('Ctrl Pts',(-20.4867385357516,4.08019174670546,5.76985765191063));
#54873=CARTESIAN_POINT('Ctrl Pts',(-20.5985299989913,4.08026088293725,5.91743628124831));
#54874=CARTESIAN_POINT('Ctrl Pts',(-20.7086941885613,4.08035370311237,6.06252104066088));
#54875=CARTESIAN_POINT('Ctrl Pts',(-20.8175153853736,4.08044838230245,6.20569714733634));
#54876=CARTESIAN_POINT('Ctrl Pts',(-20.8837484074139,4.08050600792197,6.29283996975399));
#54877=CARTESIAN_POINT('Ctrl Pts',(-20.9494899802706,4.08056430624765,6.37928395918526));
#54878=CARTESIAN_POINT('Ctrl Pts',(-21.0147749929071,4.08061833242126,6.46512326211024));
#54879=CARTESIAN_POINT('Ctrl Pts',(-21.056753592743,4.08065307152953,6.52031837661131));
#54880=CARTESIAN_POINT('Ctrl Pts',(-21.0985432473107,4.08068604483045,6.57526325140479));
#54881=CARTESIAN_POINT('Ctrl Pts',(-21.1401509099359,4.08071597508933,6.62997962237056));
#54882=CARTESIAN_POINT('Ctrl Pts',(-10.8670147648799,2.7042092247722,-5.65154550519047));
#54883=CARTESIAN_POINT('Ctrl Pts',(-10.8825819667526,2.70903278193244,-5.64047515756788));
#54884=CARTESIAN_POINT('Ctrl Pts',(-10.8981033350986,2.71386799061846,-5.62937871312437));
#54885=CARTESIAN_POINT('Ctrl Pts',(-10.9135792074401,2.71871360214693,-5.61825800418583));
#54886=CARTESIAN_POINT('Ctrl Pts',(-11.0107587992363,2.74914126011334,-5.54842633775175));
#54887=CARTESIAN_POINT('Ctrl Pts',(-11.1061434441261,2.77997495059204,-5.477637425274));
#54888=CARTESIAN_POINT('Ctrl Pts',(-11.1997509871659,2.81085934490754,-5.40635622923117));
#54889=CARTESIAN_POINT('Ctrl Pts',(-11.2928171879274,2.84156513151862,-5.33548725985091));
#54890=CARTESIAN_POINT('Ctrl Pts',(-11.3841265997849,2.87232103418462,-5.26413206407766));
#54891=CARTESIAN_POINT('Ctrl Pts',(-11.4737096205386,2.90282774713705,-5.19274952618222));
#54892=CARTESIAN_POINT('Ctrl Pts',(-11.5164512601376,2.91738303807718,-5.15869165804243));
#54893=CARTESIAN_POINT('Ctrl Pts',(-11.5588001080816,2.93188233724435,-5.12462755866404));
#54894=CARTESIAN_POINT('Ctrl Pts',(-11.6007606569768,2.94629714755178,-5.09060688784509));
#54895=CARTESIAN_POINT('Ctrl Pts',(-11.6698696768522,2.97003833870074,-5.03457484637507));
#54896=CARTESIAN_POINT('Ctrl Pts',(-11.737965114793,2.99357278208341,-4.97856686204584));
#54897=CARTESIAN_POINT('Ctrl Pts',(-11.8054490598404,3.01696025884261,-4.92223728584462));
#54898=CARTESIAN_POINT('Ctrl Pts',(-11.8794776799778,3.04261588155053,-4.86044479881427));
#54899=CARTESIAN_POINT('Ctrl Pts',(-11.952770434535,3.06809557782894,-4.7982654510355));
#54900=CARTESIAN_POINT('Ctrl Pts',(-12.0258886104834,3.09350467545653,-4.73519326240181));
#54901=CARTESIAN_POINT('Ctrl Pts',(-12.102122512934,3.11999651069141,-4.66943342890923));
#54902=CARTESIAN_POINT('Ctrl Pts',(-12.1781669364099,3.14641306799247,-4.60270275829058));
#54903=CARTESIAN_POINT('Ctrl Pts',(-12.2546871001548,3.17288172182397,-4.53437800091278));
#54904=CARTESIAN_POINT('Ctrl Pts',(-12.3317459488349,3.19953670909201,-4.46557225243795));
#54905=CARTESIAN_POINT('Ctrl Pts',(-12.4092877338435,3.22624611123961,-4.39514937721361));
#54906=CARTESIAN_POINT('Ctrl Pts',(-12.4880146031307,3.25312461003796,-4.32242993472665));
#54907=CARTESIAN_POINT('Ctrl Pts',(-12.5192375769084,3.26378458763852,-4.29358949859024));
#54908=CARTESIAN_POINT('Ctrl Pts',(-12.5506471645991,3.27447086295421,-4.26438740435322));
#54909=CARTESIAN_POINT('Ctrl Pts',(-12.5822878884511,3.28518907137685,-4.23477968801371));
#54910=CARTESIAN_POINT('Ctrl Pts',(-12.6568047736437,3.31043146185554,-4.16505072702003));
#54911=CARTESIAN_POINT('Ctrl Pts',(-12.7326033668085,3.33585402022417,-4.09307337513168));
#54912=CARTESIAN_POINT('Ctrl Pts',(-12.8102719529775,3.36149876026795,-4.01825763687434));
#54913=CARTESIAN_POINT('Ctrl Pts',(-12.8439067468809,3.37260435119765,-3.98585828391655));
#54914=CARTESIAN_POINT('Ctrl Pts',(-12.8778922944557,3.38375105078127,-3.95292636620954));
#54915=CARTESIAN_POINT('Ctrl Pts',(-12.9122764856802,3.3949393291939,-3.91941291420406));
#54916=CARTESIAN_POINT('Ctrl Pts',(-12.9370845594558,3.40301163295904,-3.89523307573123));
#54917=CARTESIAN_POINT('Ctrl Pts',(-12.9621001530937,3.41110553892594,-3.87075050495877));
#54918=CARTESIAN_POINT('Ctrl Pts',(-12.9873408891014,3.41922107952233,-3.84594638986787));
#54919=CARTESIAN_POINT('Ctrl Pts',(-13.0760628982132,3.44774746902704,-3.75875911749837));
#54920=CARTESIAN_POINT('Ctrl Pts',(-13.1675146048207,3.47651397214489,-3.66771261218589));
#54921=CARTESIAN_POINT('Ctrl Pts',(-13.2613154033226,3.50517803164381,-3.57289531261814));
#54922=CARTESIAN_POINT('Ctrl Pts',(-13.3558400529778,3.53406328875359,-3.47734631766253));
#54923=CARTESIAN_POINT('Ctrl Pts',(-13.4527501050739,3.56284323316075,-3.3779680079072));
#54924=CARTESIAN_POINT('Ctrl Pts',(-13.5516154260481,3.591163592317,-3.27488416648269));
#54925=CARTESIAN_POINT('Ctrl Pts',(-13.6339391159868,3.61474553635114,-3.18904777698334));
#54926=CARTESIAN_POINT('Ctrl Pts',(-13.7176176631479,3.63800835248907,-3.10064273411202));
#54927=CARTESIAN_POINT('Ctrl Pts',(-13.8023830403473,3.66075569667637,-3.00975812175573));
#54928=CARTESIAN_POINT('Ctrl Pts',(-13.8961548674793,3.68591998069561,-2.90921688144739));
#54929=CARTESIAN_POINT('Ctrl Pts',(-13.9912484919101,3.71045810812311,-2.8056379406839));
#54930=CARTESIAN_POINT('Ctrl Pts',(-14.0880081563311,3.73427239190452,-2.69847830019729));
#54931=CARTESIAN_POINT('Ctrl Pts',(-14.0986567235059,3.73689319471615,-2.68668519780301));
#54932=CARTESIAN_POINT('Ctrl Pts',(-14.1093254421708,3.73950518591304,-2.67484873235818));
#54933=CARTESIAN_POINT('Ctrl Pts',(-14.1200147504619,3.74210820192807,-2.66296818424889));
#54934=CARTESIAN_POINT('Ctrl Pts',(-14.215122794505,3.76526851829853,-2.55726109244567));
#54935=CARTESIAN_POINT('Ctrl Pts',(-14.3118634807218,3.78772128016114,-2.44806304643595));
#54936=CARTESIAN_POINT('Ctrl Pts',(-14.4105259337003,3.80933210165384,-2.33487331767942));
#54937=CARTESIAN_POINT('Ctrl Pts',(-14.5090268780975,3.83090754663789,-2.22186887838165));
#54938=CARTESIAN_POINT('Ctrl Pts',(-14.6094437433893,3.85164325824876,-2.10488521430534));
#54939=CARTESIAN_POINT('Ctrl Pts',(-14.712027927971,3.87137351965582,-1.98344311485669));
#54940=CARTESIAN_POINT('Ctrl Pts',(-14.7480030930743,3.87829270914438,-1.94085468277071));
#54941=CARTESIAN_POINT('Ctrl Pts',(-14.784252937188,3.88508861678897,-1.89771585291644));
#54942=CARTESIAN_POINT('Ctrl Pts',(-14.8207338105388,3.89174386471088,-1.85407313434892));
#54943=CARTESIAN_POINT('Ctrl Pts',(-14.8955878522407,3.90539957412038,-1.76452391100031));
#54944=CARTESIAN_POINT('Ctrl Pts',(-14.971414188907,3.91846034565269,-1.67285267325724));
#54945=CARTESIAN_POINT('Ctrl Pts',(-15.0478385606804,3.93080581904371,-1.57947261102481));
#54946=CARTESIAN_POINT('Ctrl Pts',(-15.1270962517208,3.9436089823942,-1.4826306226641));
#54947=CARTESIAN_POINT('Ctrl Pts',(-15.2069966171596,3.95564252009211,-1.38395112278974));
#54948=CARTESIAN_POINT('Ctrl Pts',(-15.2871330839331,3.96682523634334,-1.2838979026888));
#54949=CARTESIAN_POINT('Ctrl Pts',(-15.3511514963117,3.97575874401229,-1.20396864498479));
#54950=CARTESIAN_POINT('Ctrl Pts',(-15.4153207078596,3.98415025880874,-1.12316291197415));
#54951=CARTESIAN_POINT('Ctrl Pts',(-15.4794409402304,3.99198113393681,-1.04171785846541));
#54952=CARTESIAN_POINT('Ctrl Pts',(-15.5573651090663,4.00149785608596,-0.94273914510455));
#54953=CARTESIAN_POINT('Ctrl Pts',(-15.6352162293308,4.01018564820184,-0.842816346832298));
#54954=CARTESIAN_POINT('Ctrl Pts',(-15.7126525047195,4.01805069496177,-0.742364156738377));
#54955=CARTESIAN_POINT('Ctrl Pts',(-15.8133014664812,4.02827340759379,-0.611799914219101));
#54956=CARTESIAN_POINT('Ctrl Pts',(-15.9132436882516,4.03708677559505,-0.480700346086931));
#54957=CARTESIAN_POINT('Ctrl Pts',(-16.0122412921091,4.04463271570221,-0.349301786997184));
#54958=CARTESIAN_POINT('Ctrl Pts',(-16.0416708873646,4.04687594134125,-0.310240170750923));
#54959=CARTESIAN_POINT('Ctrl Pts',(-16.0710172335301,4.04900741347074,-0.271152030394429));
#54960=CARTESIAN_POINT('Ctrl Pts',(-16.100274661319,4.05103144399587,-0.232043298691982));
#54961=CARTESIAN_POINT('Ctrl Pts',(-16.1836574145965,4.05679986762905,-0.120584637661964));
#54962=CARTESIAN_POINT('Ctrl Pts',(-16.2663166502409,4.06169446575746,-0.00896259225158377));
#54963=CARTESIAN_POINT('Ctrl Pts',(-16.3481339461205,4.06582084985792,0.102612874254018));
#54964=CARTESIAN_POINT('Ctrl Pts',(-16.3647111828591,4.06665690836331,0.125219499205496));
#54965=CARTESIAN_POINT('Ctrl Pts',(-16.3812539136449,4.06746147727406,0.147824366621108));
#54966=CARTESIAN_POINT('Ctrl Pts',(-16.3977612396738,4.06823550038658,0.170425963319117));
#54967=CARTESIAN_POINT('Ctrl Pts',(-16.4465477097304,4.07052308199341,0.237223706249112));
#54968=CARTESIAN_POINT('Ctrl Pts',(-16.4950247902217,4.07254398783715,0.30399644028247));
#54969=CARTESIAN_POINT('Ctrl Pts',(-16.5431702873596,4.07432687884092,0.370874939270894));
#54970=CARTESIAN_POINT('Ctrl Pts',(-16.5745169579264,4.07548768722953,0.41441833170452));
#54971=CARTESIAN_POINT('Ctrl Pts',(-16.6057230998384,4.07654732854821,0.458000668758363));
#54972=CARTESIAN_POINT('Ctrl Pts',(-16.6367834831488,4.07750677533081,0.501329112044902));
#54973=CARTESIAN_POINT('Ctrl Pts',(-16.6533361456736,4.07801808256884,0.524419654498255));
#54974=CARTESIAN_POINT('Ctrl Pts',(-16.6698474196488,4.07850097957143,0.547438993526175));
#54975=CARTESIAN_POINT('Ctrl Pts',(-16.6863165610272,4.07895589513591,0.570348816731394));
#54976=CARTESIAN_POINT('Ctrl Pts',(-16.6864700870274,4.07896013587715,0.570562383027311));
#54977=CARTESIAN_POINT('Ctrl Pts',(-16.6866236098607,4.07896437475301,0.570775948118517));
#54978=CARTESIAN_POINT('Ctrl Pts',(-16.6867771295269,4.07896861176448,0.57098951200485));
#54979=CARTESIAN_POINT('',(-34.5094710129489,4.11696067448647,0.612674457278041));
#54980=CARTESIAN_POINT('',(-35.0820169555422,4.13115532855471,-2.69386316078375));
#54981=CARTESIAN_POINT('Origin',(-42.4365979192343,4.31984058958519,0.26838881652106));
#54982=CARTESIAN_POINT('',(-35.2886576356463,4.13442741082932,6.62929523481876));
#54983=CARTESIAN_POINT('Ctrl Pts',(-35.2883365499271,4.13441961266498,6.62833239954248));
#54984=CARTESIAN_POINT('Ctrl Pts',(-34.6423025074559,4.11873027055746,4.6907194393648));
#54985=CARTESIAN_POINT('Ctrl Pts',(-34.3775118580705,4.11384875218964,2.64941339379631));
#54986=CARTESIAN_POINT('Ctrl Pts',(-34.5094662196082,4.1169605614472,0.612748436480715));
#54987=CARTESIAN_POINT('',(-38.96547857039,4.2626731672903,12.6510864480354));
#54988=CARTESIAN_POINT('Ctrl Pts',(-38.9640138900455,4.26260658610796,12.6495838748125));
#54989=CARTESIAN_POINT('Ctrl Pts',(-37.3069065807585,4.18728739522815,10.9493640627874));
#54990=CARTESIAN_POINT('Ctrl Pts',(-36.0425989591165,4.1527392094223,8.88970910721889));
#54991=CARTESIAN_POINT('Ctrl Pts',(-35.2888843457993,4.13443291690738,6.6299750673985));
#54992=CARTESIAN_POINT('',(-61.2151481505771,6.62152250824553,12.6564237477171));
#54993=CARTESIAN_POINT('Ctrl Pts',(-61.2151481505771,6.62152250824553,12.6564237477171));
#54994=CARTESIAN_POINT('Ctrl Pts',(-58.2965417115554,6.22483785549351,15.6153467534928));
#54995=CARTESIAN_POINT('Ctrl Pts',(-50.1081788357534,4.96418169793774,19.0244081704428));
#54996=CARTESIAN_POINT('Ctrl Pts',(-41.8770097886242,4.39504138626396,15.6375182081803));
#54997=CARTESIAN_POINT('Ctrl Pts',(-38.96547857039,4.2626731672903,12.6510864480354));
#54998=CARTESIAN_POINT('',(-64.9284491122907,7.16443381643712,6.63636663678025));
#54999=CARTESIAN_POINT('Ctrl Pts',(-64.9279798115614,7.16341862632849,6.63807904463546));
#55000=CARTESIAN_POINT('Ctrl Pts',(-64.8508885627514,7.15299985198849,6.86358669794533));
#55001=CARTESIAN_POINT('Ctrl Pts',(-64.7684102394653,7.14156243532073,7.08720349281578));
#55002=CARTESIAN_POINT('Ctrl Pts',(-64.6809064278057,7.12914354033835,7.30871875086926));
#55003=CARTESIAN_POINT('Ctrl Pts',(-64.5974607138085,7.11730058699488,7.51996096442497));
#55004=CARTESIAN_POINT('Ctrl Pts',(-64.5094459744822,7.1045662353132,7.72929139412695));
#55005=CARTESIAN_POINT('Ctrl Pts',(-64.4171380221575,7.09100102588375,7.93652647044922));
#55006=CARTESIAN_POINT('Ctrl Pts',(-64.3852592526469,7.08631624874512,8.00809559386943));
#55007=CARTESIAN_POINT('Ctrl Pts',(-64.3528680238246,7.08153255014063,8.07941484428056));
#55008=CARTESIAN_POINT('Ctrl Pts',(-64.3199742825305,7.07665281288929,8.1504768514447));
#55009=CARTESIAN_POINT('Ctrl Pts',(-64.3071410638109,7.07474902411438,8.17820110063947));
#55010=CARTESIAN_POINT('Ctrl Pts',(-64.2942313488762,7.07283061818773,8.2058861961849));
#55011=CARTESIAN_POINT('Ctrl Pts',(-64.2812457042831,7.0708977660961,8.23353171912382));
#55012=CARTESIAN_POINT('Ctrl Pts',(-64.1910552011233,7.05747333410678,8.42554094947833));
#55013=CARTESIAN_POINT('Ctrl Pts',(-64.0972054525586,7.04334975225786,8.6156411800766));
#55014=CARTESIAN_POINT('Ctrl Pts',(-63.9998442582977,7.0285858672386,8.80367434032654));
#55015=CARTESIAN_POINT('Ctrl Pts',(-63.9029115746634,7.01388696171829,8.99087992026658));
#55016=CARTESIAN_POINT('Ctrl Pts',(-63.8024983496159,6.99855324463019,9.1760363662355));
#55017=CARTESIAN_POINT('Ctrl Pts',(-63.6987070211235,6.98267230296273,9.35899039531681));
#55018=CARTESIAN_POINT('Ctrl Pts',(-63.6417591017022,6.97395879481566,9.45937307137728));
#55019=CARTESIAN_POINT('Ctrl Pts',(-63.5837934413672,6.9650810994762,9.5590927750825));
#55020=CARTESIAN_POINT('Ctrl Pts',(-63.5248214191519,6.95605724044794,9.65812507941458));
#55021=CARTESIAN_POINT('Ctrl Pts',(-63.5210198925743,6.95547553341739,9.6645090208637));
#55022=CARTESIAN_POINT('Ctrl Pts',(-63.5172141827313,6.95489321973694,9.67089010615184));
#55023=CARTESIAN_POINT('Ctrl Pts',(-63.5134042920641,6.95431030451018,9.67726832887461));
#55024=CARTESIAN_POINT('Ctrl Pts',(-63.4053691505814,6.93778087243555,9.85813236263684));
#55025=CARTESIAN_POINT('Ctrl Pts',(-63.2939758134642,6.92076945837511,10.0366929411969));
#55026=CARTESIAN_POINT('Ctrl Pts',(-63.179268520996,6.90337495979145,10.2128406339241));
#55027=CARTESIAN_POINT('Ctrl Pts',(-63.0644443776627,6.88596274165252,10.3891677660735));
#55028=CARTESIAN_POINT('Ctrl Pts',(-62.9462992983965,6.86816729533639,10.5630773346187));
#55029=CARTESIAN_POINT('Ctrl Pts',(-62.8248362353091,6.85006129639097,10.7344780991604));
#55030=CARTESIAN_POINT('Ctrl Pts',(-62.7237908235596,6.83499887270372,10.8770668038006));
#55031=CARTESIAN_POINT('Ctrl Pts',(-62.6204482553076,6.81972118356617,11.0179197159958));
#55032=CARTESIAN_POINT('Ctrl Pts',(-62.514791071203,6.80425173418117,11.1569917197539));
#55033=CARTESIAN_POINT('Ctrl Pts',(-62.3870909877244,6.78555494612483,11.3250778431912));
#55034=CARTESIAN_POINT('Ctrl Pts',(-62.256009986916,6.76657955576061,11.4905618395803));
#55035=CARTESIAN_POINT('Ctrl Pts',(-62.1214919444444,6.74732763669793,11.6533667143777));
#55036=CARTESIAN_POINT('Ctrl Pts',(-62.0878954759279,6.74251938584335,11.6940279427896));
#55037=CARTESIAN_POINT('Ctrl Pts',(-62.0540845042587,6.73769366259078,11.7345221212631));
#55038=CARTESIAN_POINT('Ctrl Pts',(-62.0200579664813,6.73285005326746,11.7748481636997));
#55039=CARTESIAN_POINT('Ctrl Pts',(-61.9835559126172,6.7276540592003,11.8181080270094));
#55040=CARTESIAN_POINT('Ctrl Pts',(-61.9468057712324,6.72243747786662,11.8611743977494));
#55041=CARTESIAN_POINT('Ctrl Pts',(-61.9098067959039,6.71720001308234,11.9040458787038));
#55042=CARTESIAN_POINT('Ctrl Pts',(-61.7985120786369,6.70144546428232,12.0330053785082));
#55043=CARTESIAN_POINT('Ctrl Pts',(-61.6849649179537,6.68550281059298,12.1602033116016));
#55044=CARTESIAN_POINT('Ctrl Pts',(-61.5691520865945,6.66935638985563,12.2856216372723));
#55045=CARTESIAN_POINT('Ctrl Pts',(-61.4549290846619,6.65343162033362,12.4093182733649));
#55046=CARTESIAN_POINT('Ctrl Pts',(-61.3386809921953,6.63733318178291,12.5311923351786));
#55047=CARTESIAN_POINT('Ctrl Pts',(-61.2204712761571,6.62104377694539,12.6511854446751));
#55048=CARTESIAN_POINT('Ctrl Pts',(-61.2199200988289,6.62096782421546,12.6517449374453));
#55049=CARTESIAN_POINT('Ctrl Pts',(-61.2193688737375,6.62089186653554,12.6523043884547));
#55050=CARTESIAN_POINT('Ctrl Pts',(-61.2188176008955,6.62081590390381,12.652863797695));
#55051=CARTESIAN_POINT('',(-65.7394232394244,7.26094188381232,0.668649941455471));
#55052=CARTESIAN_POINT('Ctrl Pts',(-65.7395827156737,7.26124220258481,0.671033071149472));
#55053=CARTESIAN_POINT('Ctrl Pts',(-65.9020867768559,7.22064705772462,2.65598726978187));
#55054=CARTESIAN_POINT('Ctrl Pts',(-65.5865610442786,7.25403397826185,4.71036142108621));
#55055=CARTESIAN_POINT('Ctrl Pts',(-64.9284491122907,7.16443381643712,6.63636663678025));
#55056=CARTESIAN_POINT('',(-64.0795635270123,7.11304235593188,-4.92051130426413));
#55057=CARTESIAN_POINT('Ctrl Pts',(-64.0835337535963,7.11077786349443,-4.91454011088298));
#55058=CARTESIAN_POINT('Ctrl Pts',(-64.1323411238627,7.10143308976583,-4.82718197003987));
#55059=CARTESIAN_POINT('Ctrl Pts',(-64.1802005667353,7.09364154317148,-4.73875740081963));
#55060=CARTESIAN_POINT('Ctrl Pts',(-64.2272039770873,7.0873437062873,-4.64918122502579));
#55061=CARTESIAN_POINT('Ctrl Pts',(-64.2731661376042,7.08118538314411,-4.56158939840107));
#55062=CARTESIAN_POINT('Ctrl Pts',(-64.3183102368122,7.07645513160571,-4.47289638639061));
#55063=CARTESIAN_POINT('Ctrl Pts',(-64.362691913154,7.07305727552395,-4.38303080249611));
#55064=CARTESIAN_POINT('Ctrl Pts',(-64.407348532143,7.06963836986447,-4.29260850503057));
#55065=CARTESIAN_POINT('Ctrl Pts',(-64.4512334822151,7.06756810463911,-4.20099882935125));
#55066=CARTESIAN_POINT('Ctrl Pts',(-64.4943671378015,7.0667116387588,-4.10813965798429));
#55067=CARTESIAN_POINT('Ctrl Pts',(-64.538733872391,7.06583068874702,-4.0126258844766));
#55068=CARTESIAN_POINT('Ctrl Pts',(-64.5823058216986,7.06623345912329,-3.91578975174785));
#55069=CARTESIAN_POINT('Ctrl Pts',(-64.625064292327,7.06773963749489,-3.81757984118512));
#55070=CARTESIAN_POINT('Ctrl Pts',(-64.6366297318445,7.06814703314313,-3.79101572970186));
#55071=CARTESIAN_POINT('Ctrl Pts',(-64.6481354299698,7.06863499482074,-3.76435122011603));
#55072=CARTESIAN_POINT('Ctrl Pts',(-64.6595805256827,7.06919962896058,-3.73758555155824));
#55073=CARTESIAN_POINT('Ctrl Pts',(-64.7044712102175,7.07141427300421,-3.63260353884933));
#55074=CARTESIAN_POINT('Ctrl Pts',(-64.7484339464594,7.07480847542174,-3.52606497812548));
#55075=CARTESIAN_POINT('Ctrl Pts',(-64.791404704864,7.07913848472074,-3.41808155276295));
#55076=CARTESIAN_POINT('Ctrl Pts',(-64.8142018012916,7.0814356664133,-3.3607935585087));
#55077=CARTESIAN_POINT('Ctrl Pts',(-64.8367187512787,7.08399620397509,-3.30309898433251));
#55078=CARTESIAN_POINT('Ctrl Pts',(-64.858940198642,7.08678381264196,-3.24501532835008));
#55079=CARTESIAN_POINT('Ctrl Pts',(-64.9045049237743,7.09249975997003,-3.12591571362922));
#55080=CARTESIAN_POINT('Ctrl Pts',(-64.9488302632029,7.09916995637793,-3.00517924810612));
#55081=CARTESIAN_POINT('Ctrl Pts',(-64.9917455430339,7.10648781659526,-2.88297777630594));
#55082=CARTESIAN_POINT('Ctrl Pts',(-65.0375600701317,7.11430005285572,-2.75252068355919));
#55083=CARTESIAN_POINT('Ctrl Pts',(-65.0817671166487,7.12284975587435,-2.62039419187577));
#55084=CARTESIAN_POINT('Ctrl Pts',(-65.1241037097651,7.13177696281216,-2.48682213043831));
#55085=CARTESIAN_POINT('Ctrl Pts',(-65.1318590972489,7.1334122845009,-2.46235386274833));
#55086=CARTESIAN_POINT('Ctrl Pts',(-65.1395515909995,7.13506032430707,-2.43783711801167));
#55087=CARTESIAN_POINT('Ctrl Pts',(-65.147179412765,7.13671894382896,-2.41327330962486));
#55088=CARTESIAN_POINT('Ctrl Pts',(-65.1548093866202,7.13837803130856,-2.38870257088207));
#55089=CARTESIAN_POINT('Ctrl Pts',(-65.162374652527,7.14004770064065,-2.36408474166654));
#55090=CARTESIAN_POINT('Ctrl Pts',(-65.1698737946742,7.14172531456448,-2.33942154267057));
#55091=CARTESIAN_POINT('Ctrl Pts',(-65.2102039449649,7.15074746941242,-2.20678363520819));
#55092=CARTESIAN_POINT('Ctrl Pts',(-65.2488912851349,7.16005021608417,-2.07258936172927));
#55093=CARTESIAN_POINT('Ctrl Pts',(-65.2858205099729,7.16927502780963,-1.93704689908791));
#55094=CARTESIAN_POINT('Ctrl Pts',(-65.3077327593675,7.17474864324654,-1.8566217004009));
#55095=CARTESIAN_POINT('Ctrl Pts',(-65.3290254015679,7.18019570057733,-1.77572190701815));
#55096=CARTESIAN_POINT('Ctrl Pts',(-65.3496700473213,7.18554871571595,-1.69439082134555));
#55097=CARTESIAN_POINT('Ctrl Pts',(-65.385357852192,7.19480231890289,-1.55379611460786));
#55098=CARTESIAN_POINT('Ctrl Pts',(-65.4191095339481,7.20377199941432,-1.4119135129394));
#55099=CARTESIAN_POINT('Ctrl Pts',(-65.4507698563869,7.21212018115951,-1.26909214155907));
#55100=CARTESIAN_POINT('Ctrl Pts',(-65.4750302946932,7.21851716427901,-1.15965203475376));
#55101=CARTESIAN_POINT('Ctrl Pts',(-65.498062302265,7.22455029649033,-1.04966052491815));
#55102=CARTESIAN_POINT('Ctrl Pts',(-65.5197944063732,7.23008731297395,-0.939268302285297));
#55103=CARTESIAN_POINT('Ctrl Pts',(-65.524236410554,7.23121906948712,-0.916704324493633));
#55104=CARTESIAN_POINT('Ctrl Pts',(-65.5286241098133,7.23233015301656,-0.894123582617326));
#55105=CARTESIAN_POINT('Ctrl Pts',(-65.5329569904809,7.2334191756638,-0.871526032417236));
#55106=CARTESIAN_POINT('Ctrl Pts',(-65.5570702056107,7.23947977123251,-0.745766836359672));
#55107=CARTESIAN_POINT('Ctrl Pts',(-65.5794867225205,7.24485641788753,-0.619490657946675));
#55108=CARTESIAN_POINT('Ctrl Pts',(-65.6001882638281,7.24934156066612,-0.492123250458605));
#55109=CARTESIAN_POINT('Ctrl Pts',(-65.6185807063574,7.25332642003314,-0.378962704220613));
#55110=CARTESIAN_POINT('Ctrl Pts',(-65.6356193472249,7.25660864722147,-0.264940523657192));
#55111=CARTESIAN_POINT('Ctrl Pts',(-65.6512872325861,7.25903990662824,-0.149619654441558));
#55112=CARTESIAN_POINT('Ctrl Pts',(-65.6531503494619,7.25932901523006,-0.135906491968494));
#55113=CARTESIAN_POINT('Ctrl Pts',(-65.6549940787113,7.25960607744851,-0.122174923828413));
#55114=CARTESIAN_POINT('Ctrl Pts',(-65.6568183790756,7.25987084800059,-0.10842604919408));
#55115=CARTESIAN_POINT('Ctrl Pts',(-65.6645280546458,7.26098979480182,-0.0503219316038178));
#55116=CARTESIAN_POINT('Ctrl Pts',(-65.6718710057134,7.26188323443358,0.00675034893310512));
#55117=CARTESIAN_POINT('Ctrl Pts',(-65.6788643662617,7.26255350370653,0.0633737642326929));
#55118=CARTESIAN_POINT('Ctrl Pts',(-65.686925212884,7.26332608475218,0.128640335691545));
#55119=CARTESIAN_POINT('Ctrl Pts',(-65.6945220442716,7.26380328978071,0.193312839132918));
#55120=CARTESIAN_POINT('Ctrl Pts',(-65.7016657796718,7.26396077863301,0.258338263786383));
#55121=CARTESIAN_POINT('Ctrl Pts',(-65.7058603841224,7.2640532517446,0.296519400176069));
#55122=CARTESIAN_POINT('Ctrl Pts',(-65.7098984505169,7.26403499039114,0.334820379179476));
#55123=CARTESIAN_POINT('Ctrl Pts',(-65.713780714574,7.26388377792568,0.37383220486236));
#55124=CARTESIAN_POINT('Ctrl Pts',(-65.7167673931564,7.26376744811778,0.403844533367242));
#55125=CARTESIAN_POINT('Ctrl Pts',(-65.7196618187443,7.2635723487753,0.434277416501284));
#55126=CARTESIAN_POINT('Ctrl Pts',(-65.7224634125073,7.2632854179205,0.46542151022431));
#55127=CARTESIAN_POINT('Ctrl Pts',(-65.7245218275605,7.26307460120662,0.488304010957459));
#55128=CARTESIAN_POINT('Ctrl Pts',(-65.7265301305615,7.26281402466057,0.511575469365943));
#55129=CARTESIAN_POINT('Ctrl Pts',(-65.7284858187154,7.26251260512385,0.534798711637291));
#55130=CARTESIAN_POINT('Ctrl Pts',(-65.7303609092576,7.26222360765695,0.557064880123483));
#55131=CARTESIAN_POINT('Ctrl Pts',(-65.7321876345632,7.26189704344469,0.579287553385808));
#55132=CARTESIAN_POINT('Ctrl Pts',(-65.7339633481816,7.26154152718023,0.601031873391619));
#55133=CARTESIAN_POINT('Ctrl Pts',(-65.7355811316233,7.26121763017347,0.620842275525464));
#55134=CARTESIAN_POINT('Ctrl Pts',(-65.7371565718029,7.26086969558048,0.640255744443095));
#55135=CARTESIAN_POINT('Ctrl Pts',(-65.7386872986922,7.26050504824662,0.658895929602836));
#55136=CARTESIAN_POINT('Ctrl Pts',(-65.7388367302922,7.26046945088766,0.660715609333391));
#55137=CARTESIAN_POINT('Ctrl Pts',(-65.7389857354748,7.26043369499359,0.662527878289384));
#55138=CARTESIAN_POINT('Ctrl Pts',(-65.7391343118341,7.26039778787535,0.664332358598316));
#55139=CARTESIAN_POINT('',(-59.0504798555313,7.75485996799304,-10.7041909447736));
#55140=CARTESIAN_POINT('Ctrl Pts',(-59.0504798555313,7.75485996799304,-10.7041909447736));
#55141=CARTESIAN_POINT('Ctrl Pts',(-60.0796098167125,7.87873199265082,-9.96197480208937));
#55142=CARTESIAN_POINT('Ctrl Pts',(-62.0660466287397,7.97403730548955,-8.03642045404962));
#55143=CARTESIAN_POINT('Ctrl Pts',(-63.5230316254146,7.22290795330965,-5.91353180077074));
#55144=CARTESIAN_POINT('Ctrl Pts',(-64.0795059534616,7.11307519407537,-4.92059789448709));
#55145=CARTESIAN_POINT('',(-41.3402244866054,4.38233490926977,-11.3195856097259));
#55146=CARTESIAN_POINT('Ctrl Pts',(-41.3402244866054,4.38233490926977,-11.3195856097259));
#55147=CARTESIAN_POINT('Ctrl Pts',(-41.9985023915937,4.44701923023704,-11.7653170427634));
#55148=CARTESIAN_POINT('Ctrl Pts',(-43.3908039796773,4.61571635395792,-12.5174764940247));
#55149=CARTESIAN_POINT('Ctrl Pts',(-46.1914722110254,5.3927514423487,-13.3156545423547));
#55150=CARTESIAN_POINT('Ctrl Pts',(-49.9948035131066,7.02745080169609,-13.706606972641));
#55151=CARTESIAN_POINT('Ctrl Pts',(-54.1289712559167,7.53905427079786,-13.0742974757744));
#55152=CARTESIAN_POINT('Ctrl Pts',(-56.7102378337881,7.56456386339554,-12.0170276546053));
#55153=CARTESIAN_POINT('Ctrl Pts',(-57.9084119982073,7.63003527898566,-11.4010944726287));
#55154=CARTESIAN_POINT('Ctrl Pts',(-58.5678160077699,7.69080724613176,-11.0134367986666));
#55155=CARTESIAN_POINT('Ctrl Pts',(-58.8883897060344,7.73532762094072,-10.8209468457134));
#55156=CARTESIAN_POINT('Ctrl Pts',(-59.0486785764031,7.75464303119201,-10.7054892315628));
#55157=CARTESIAN_POINT('',(-36.1360059330621,4.15901206247279,-5.40582646581216));
#55158=CARTESIAN_POINT('Ctrl Pts',(-36.1360059330621,4.15901206247279,-5.40582646581216));
#55159=CARTESIAN_POINT('Ctrl Pts',(-36.735234866715,4.17590258588924,-6.60510917508678));
#55160=CARTESIAN_POINT('Ctrl Pts',(-37.85694008542,4.21051024093903,-8.27236172411371));
#55161=CARTESIAN_POINT('Ctrl Pts',(-39.7542446236388,4.26982122872605,-10.1775780089158));
#55162=CARTESIAN_POINT('Ctrl Pts',(-40.8013703910201,4.32944548953245,-10.9546239517306));
#55163=CARTESIAN_POINT('Ctrl Pts',(-41.3379913976662,4.38211560392107,-11.3180733508353));
#55164=CARTESIAN_POINT('Ctrl Pts',(-35.0820169555422,4.1311553285547,-2.69386316078375));
#55165=CARTESIAN_POINT('Ctrl Pts',(-35.3472499758451,4.13782412394816,-3.62262376308943));
#55166=CARTESIAN_POINT('Ctrl Pts',(-35.7008401684657,4.14674629646921,-4.53483852841008));
#55167=CARTESIAN_POINT('Ctrl Pts',(-36.135822819044,4.15900690108209,-5.40545997363959));
#55168=CARTESIAN_POINT('',(3.02589869591714,2.03453539417915,-29.481040542818));
#55169=CARTESIAN_POINT('',(1.7019170311789,1.9841758627661,-32.7826729204701));
#55170=CARTESIAN_POINT('Ctrl Pts',(3.02620767763066,2.03445931614535,-29.482369472598));
#55171=CARTESIAN_POINT('Ctrl Pts',(3.20555263301232,2.02375902210562,-30.2475171721583));
#55172=CARTESIAN_POINT('Ctrl Pts',(3.02661590274896,1.96081108314947,-31.598486221152));
#55173=CARTESIAN_POINT('Ctrl Pts',(2.12920577407486,1.97332831724216,-32.5206340925411));
#55174=CARTESIAN_POINT('Ctrl Pts',(1.7019170311789,1.9841758627661,-32.7826729204701));
#55175=CARTESIAN_POINT('',(-3.02596826212615,2.03432873875274,-29.4800060173015));
#55176=CARTESIAN_POINT('Ctrl Pts',(-3.0255268228659,2.03435552877844,-29.4781858978988));
#55177=CARTESIAN_POINT('Ctrl Pts',(-2.89748980529269,2.04212655242135,-28.9515397139976));
#55178=CARTESIAN_POINT('Ctrl Pts',(-2.34728642075398,2.07624236465954,-27.9637381387751));
#55179=CARTESIAN_POINT('Ctrl Pts',(-0.86527131205636,2.14132533286026,-27.1055607008419));
#55180=CARTESIAN_POINT('Ctrl Pts',(0.863471086326564,2.14121820993117,-27.1043323065609));
#55181=CARTESIAN_POINT('Ctrl Pts',(2.10137698734444,2.08724640507052,-27.8170592929481));
#55182=CARTESIAN_POINT('Ctrl Pts',(2.75995282450495,2.0506331663776,-28.6996503464524));
#55183=CARTESIAN_POINT('Ctrl Pts',(2.9604184742133,2.03838594914446,-29.2034367727384));
#55184=CARTESIAN_POINT('Ctrl Pts',(3.02523930059986,2.0345171033467,-29.4782510284727));
#55185=CARTESIAN_POINT('Ctrl Pts',(1.7019170311789,1.9841758627661,-32.7826729204701));
#55186=CARTESIAN_POINT('Ctrl Pts',(1.28857863702931,1.99466925188967,-33.036156566229));
#55187=CARTESIAN_POINT('Ctrl Pts',(0.321543600862733,2.02241016559728,-33.3511773448253));
#55188=CARTESIAN_POINT('Ctrl Pts',(-1.19853457360234,2.00220690733558,-33.1534394779125));
#55189=CARTESIAN_POINT('Ctrl Pts',(-2.44599217953573,1.95940735428246,-32.3264040160697));
#55190=CARTESIAN_POINT('Ctrl Pts',(-3.02438609187982,1.98457308078909,-31.2166546642125));
#55191=CARTESIAN_POINT('Ctrl Pts',(-3.14100419297298,2.01861532274412,-30.2293427451567));
#55192=CARTESIAN_POINT('Ctrl Pts',(-3.08328115399646,2.03085086602267,-29.7168832273726));
#55193=CARTESIAN_POINT('Ctrl Pts',(-3.02628868373051,2.03430929303555,-29.4813271629984));
#55194=CARTESIAN_POINT('',(2.75100840866463,2.05012843941995,-23.4599303049991));
#55195=CARTESIAN_POINT('',(1.61567592638144,2.10484535966067,-24.6418414854819));
#55196=CARTESIAN_POINT('Ctrl Pts',(2.75100552264243,2.05012860052275,-23.459935693484));
#55197=CARTESIAN_POINT('Ctrl Pts',(2.4917371536323,2.06460141183357,-23.9440137803207));
#55198=CARTESIAN_POINT('Ctrl Pts',(2.09220096563961,2.08654257832164,-24.3598140131154));
#55199=CARTESIAN_POINT('Ctrl Pts',(1.61567592638144,2.10484535966067,-24.6418414854819));
#55200=CARTESIAN_POINT('',(-2.75095635228815,2.0500785577562,-23.4601289752605));
#55201=CARTESIAN_POINT('Ctrl Pts',(-2.75104415575314,2.04996283861984,-23.459954551535));
#55202=CARTESIAN_POINT('Ctrl Pts',(-3.14697228957638,2.02797021966844,-22.7225859102412));
#55203=CARTESIAN_POINT('Ctrl Pts',(-3.28470830566268,2.01818671464134,-20.9006764566282));
#55204=CARTESIAN_POINT('Ctrl Pts',(-1.71693918475569,2.11168339882122,-19.2349389943924));
#55205=CARTESIAN_POINT('Ctrl Pts',(-5.68372511193975E-5,2.14348108036939,
-18.8971771498333));
#55206=CARTESIAN_POINT('Ctrl Pts',(1.71728341750388,2.11146607039885,-19.2336854760647));
#55207=CARTESIAN_POINT('Ctrl Pts',(3.28527599025147,2.01819903914408,-20.9040176508014));
#55208=CARTESIAN_POINT('Ctrl Pts',(3.14638608131475,2.02805776491796,-22.7217197351585));
#55209=CARTESIAN_POINT('Ctrl Pts',(2.75100840866463,2.05012843941995,-23.4599303049991));
#55210=CARTESIAN_POINT('Ctrl Pts',(1.61567592638144,2.10484535966067,-24.6418414854819));
#55211=CARTESIAN_POINT('Ctrl Pts',(1.04038344114352,2.12694168555298,-24.9823236681931));
#55212=CARTESIAN_POINT('Ctrl Pts',(-0.182315527702726,2.1513398143738,-25.2447478054221));
#55213=CARTESIAN_POINT('Ctrl Pts',(-1.8215791399191,2.10154489826223,-24.6600514792354));
#55214=CARTESIAN_POINT('Ctrl Pts',(-2.51542689144179,2.06305029395261,-23.8984874041331));
#55215=CARTESIAN_POINT('Ctrl Pts',(-2.75069164890588,2.04998241903505,-23.4606108465542));
#55216=CARTESIAN_POINT('Ctrl Pts',(-36.0549975098271,1.0528127756878,-2.38156518037249));
#55217=CARTESIAN_POINT('Ctrl Pts',(-36.3055439100197,1.05947580029909,-3.26356670979119));
#55218=CARTESIAN_POINT('Ctrl Pts',(-36.6408912827729,1.0685194404478,-4.1293438871194));
#55219=CARTESIAN_POINT('Ctrl Pts',(-37.6383467540235,1.09756433969661,-6.1123912328036));
#55220=CARTESIAN_POINT('Ctrl Pts',(-39.0798375037675,1.14868878793061,-8.2395365565181));
#55221=CARTESIAN_POINT('Ctrl Pts',(-41.0527618672285,1.2073272187152,-9.94414705234827));
#55222=CARTESIAN_POINT('Ctrl Pts',(-42.7057446504772,1.37815356390123,-11.0289708344873));
#55223=CARTESIAN_POINT('Ctrl Pts',(-43.9254694159358,1.53436264077785,-11.7104906826344));
#55224=CARTESIAN_POINT('Ctrl Pts',(-46.4982294500662,2.17389001321762,-12.6997150872518));
#55225=CARTESIAN_POINT('Ctrl Pts',(-49.146908121031,3.18680258560818,-13.126588408564));
#55226=CARTESIAN_POINT('Ctrl Pts',(-52.2274475031305,3.91643241459121,-12.9928561969852));
#55227=CARTESIAN_POINT('Ctrl Pts',(-54.304794246108,4.12355684923066,-12.5232019348578));
#55228=CARTESIAN_POINT('Ctrl Pts',(-56.2616035231788,4.24838602596462,-11.771250103581));
#55229=CARTESIAN_POINT('Ctrl Pts',(-57.2017281607085,4.31931888732918,-11.2901555467756));
#55230=CARTESIAN_POINT('Ctrl Pts',(-58.0855152875449,4.42766154699302,-10.7543378595292));
#55231=CARTESIAN_POINT('Ctrl Pts',(-58.6455973785906,4.50104299766934,-10.3873810885685));
#55232=CARTESIAN_POINT('Ctrl Pts',(-59.7051812089351,4.62670775817537,-9.58743591765393));
#55233=CARTESIAN_POINT('Ctrl Pts',(-61.3073010844994,4.69820828480475,-8.09568859876704));
#55234=CARTESIAN_POINT('Ctrl Pts',(-62.4948759707816,4.24202197752351,-6.47656645464623));
#55235=CARTESIAN_POINT('Ctrl Pts',(-63.1244186765201,4.05382187176954,-5.31872941631596));
#55236=CARTESIAN_POINT('Ctrl Pts',(-63.553812419201,3.95238147285607,-4.49832460967661));
#55237=CARTESIAN_POINT('Ctrl Pts',(-64.1594826858112,3.94362994185027,-3.07561996126338));
#55238=CARTESIAN_POINT('Ctrl Pts',(-64.6533034252321,4.13724389424319,-1.12169408361937));
#55239=CARTESIAN_POINT('Ctrl Pts',(-64.8054164174362,4.18825541443859,0.14378394163381));
#55240=CARTESIAN_POINT('Ctrl Pts',(-64.8433184824513,4.17721322512098,0.712263787109276));
#55241=CARTESIAN_POINT('Ctrl Pts',(-64.8578491520905,4.17264647741419,0.9518443795634));
#55242=CARTESIAN_POINT('Ctrl Pts',(-64.8752061422976,4.16523924168687,1.43110149180136));
#55243=CARTESIAN_POINT('Ctrl Pts',(-64.8689819333809,4.15580967855481,2.33145574074262));
#55244=CARTESIAN_POINT('Ctrl Pts',(-64.735236304878,4.14969563886838,3.99635849634215));
#55245=CARTESIAN_POINT('Ctrl Pts',(-64.4136362028236,4.12346149799371,5.39715323956259));
#55246=CARTESIAN_POINT('Ctrl Pts',(-63.8396954291777,4.03789832143775,7.10460988677013));
#55247=CARTESIAN_POINT('Ctrl Pts',(-62.9522024951476,3.89240808333474,9.15158202965359));
#55248=CARTESIAN_POINT('Ctrl Pts',(-61.6207408360306,3.67379600611113,10.9504902331086));
#55249=CARTESIAN_POINT('Ctrl Pts',(-58.7632410796701,3.26700669501724,13.8580023828708));
#55250=CARTESIAN_POINT('Ctrl Pts',(-55.2909382628842,2.70208941668797,15.8250391551239));
#55251=CARTESIAN_POINT('Ctrl Pts',(-48.0383621414291,1.75314527999541,16.7544202746464));
#55252=CARTESIAN_POINT('Ctrl Pts',(-42.9494969015026,1.3477622455303,14.9599652046533));
#55253=CARTESIAN_POINT('Ctrl Pts',(-40.0709952890308,1.20105054797173,12.2933217048773));
#55254=CARTESIAN_POINT('Ctrl Pts',(-39.1374904320878,1.1557136830438,11.3477424017553));
#55255=CARTESIAN_POINT('Ctrl Pts',(-37.7188277175619,1.09649931876771,9.64176435135193));
#55256=CARTESIAN_POINT('Ctrl Pts',(-36.7050062286424,1.06766764201769,7.63136101756027));
#55257=CARTESIAN_POINT('Ctrl Pts',(-35.6516839503182,1.04076735648636,4.50019397537972));
#55258=CARTESIAN_POINT('Ctrl Pts',(-35.4031603226107,1.03589678751514,2.5790344470455));
#55259=CARTESIAN_POINT('Ctrl Pts',(-35.5943183545488,1.04064036797772,-0.357304714959154));
#55260=CARTESIAN_POINT('Ctrl Pts',(-35.7726531517491,1.04530411699111,-1.38762491439351));
#55261=CARTESIAN_POINT('Ctrl Pts',(-36.0549975098271,1.0528127756878,-2.3815651803725));
#55262=CARTESIAN_POINT('Ctrl Pts',(-36.0555939497443,0.904484667441714,
-2.38244503347954));
#55263=CARTESIAN_POINT('Ctrl Pts',(-36.3062567268876,0.911222945188725,
-3.26462769997687));
#55264=CARTESIAN_POINT('Ctrl Pts',(-36.6417190294816,0.920392628576229,
-4.13054503564706));
#55265=CARTESIAN_POINT('Ctrl Pts',(-37.6400317392652,0.949603777841035,
-6.11448651724083));
#55266=CARTESIAN_POINT('Ctrl Pts',(-39.0812931660259,1.00146080909335,-8.24071227119904));
#55267=CARTESIAN_POINT('Ctrl Pts',(-41.0571520775041,1.058676413563,-9.94781725293408));
#55268=CARTESIAN_POINT('Ctrl Pts',(-42.7190199509979,1.22650923997694,-11.0365782464944));
#55269=CARTESIAN_POINT('Ctrl Pts',(-43.9458025053604,1.38117579517859,-11.7205907593239));
#55270=CARTESIAN_POINT('Ctrl Pts',(-46.5493430056267,2.00732942103926,-12.7149357794429));
#55271=CARTESIAN_POINT('Ctrl Pts',(-49.2086162954305,2.99676762410914,-13.1287136767877));
#55272=CARTESIAN_POINT('Ctrl Pts',(-52.2577461319444,3.70830093718569,-12.9861164884077));
#55273=CARTESIAN_POINT('Ctrl Pts',(-54.3176790478885,3.91571550975409,-12.5183560303513));
#55274=CARTESIAN_POINT('Ctrl Pts',(-56.2712243588391,4.04550672280604,-11.766236506535));
#55275=CARTESIAN_POINT('Ctrl Pts',(-57.2153673507245,4.12163827308303,-11.2822410862027));
#55276=CARTESIAN_POINT('Ctrl Pts',(-58.102252377271,4.23385380952422,-10.7429529768583));
#55277=CARTESIAN_POINT('Ctrl Pts',(-58.6604423297125,4.30678598655203,-10.37617396621));
#55278=CARTESIAN_POINT('Ctrl Pts',(-59.7153301961589,4.43155309898789,-9.57750241559074));
#55279=CARTESIAN_POINT('Ctrl Pts',(-61.2908741299189,4.50077347501871,-8.10847394371011));
#55280=CARTESIAN_POINT('Ctrl Pts',(-62.4722805388144,4.0598548345074,-6.51133116997329));
#55281=CARTESIAN_POINT('Ctrl Pts',(-63.1141505984817,3.87574923768064,-5.33689586275052));
#55282=CARTESIAN_POINT('Ctrl Pts',(-63.5512241737457,3.77783013568088,-4.50433690621057));
#55283=CARTESIAN_POINT('Ctrl Pts',(-64.1634629023857,3.77430690726006,-3.06490045526055));
#55284=CARTESIAN_POINT('Ctrl Pts',(-64.6550498983541,3.97353574719654,-1.10801283943642));
#55285=CARTESIAN_POINT('Ctrl Pts',(-64.8051375979326,4.02693314861109,0.147101311648772));
#55286=CARTESIAN_POINT('Ctrl Pts',(-64.8427246461288,4.01690539467727,0.709043311905127));
#55287=CARTESIAN_POINT('Ctrl Pts',(-64.8573586797898,4.01277167274026,0.949436098755388));
#55288=CARTESIAN_POINT('Ctrl Pts',(-64.8747862570427,4.00596589881556,1.42891266008647));
#55289=CARTESIAN_POINT('Ctrl Pts',(-64.8686835673502,3.99696796876503,2.3306272191874));
#55290=CARTESIAN_POINT('Ctrl Pts',(-64.7348567544036,3.98971137788843,3.99538790298088));
#55291=CARTESIAN_POINT('Ctrl Pts',(-64.4142860107865,3.96181921816279,5.39245691306954));
#55292=CARTESIAN_POINT('Ctrl Pts',(-63.8425047226651,3.8763093951887,7.09608474134876));
#55293=CARTESIAN_POINT('Ctrl Pts',(-62.958566432785,3.7311154604734,9.13944093727611));
#55294=CARTESIAN_POINT('Ctrl Pts',(-61.6293277697593,3.51429001249069,10.9391823544689));
#55295=CARTESIAN_POINT('Ctrl Pts',(-58.7777794785863,3.10978159513787,13.8465999095765));
#55296=CARTESIAN_POINT('Ctrl Pts',(-55.3120622199062,2.54885112777169,15.8174374982029));
#55297=CARTESIAN_POINT('Ctrl Pts',(-48.0528651919166,1.60552999596159,16.7577861953313));
#55298=CARTESIAN_POINT('Ctrl Pts',(-42.956881702099,1.20109260351356,14.9644289431498));
#55299=CARTESIAN_POINT('Ctrl Pts',(-40.0748747688297,1.0539287969232,12.296583589382));
#55300=CARTESIAN_POINT('Ctrl Pts',(-39.1403720142934,1.00843546237801,11.350577888442));
#55301=CARTESIAN_POINT('Ctrl Pts',(-37.7203617502752,0.948875201418379,
9.64381909341719));
#55302=CARTESIAN_POINT('Ctrl Pts',(-36.705921936741,0.919660734901868,7.63269341173704));
#55303=CARTESIAN_POINT('Ctrl Pts',(-35.6520519680447,0.892335839803674,
4.50068627822135));
#55304=CARTESIAN_POINT('Ctrl Pts',(-35.4034621866083,0.887355587669725,
2.57923003175189));
#55305=CARTESIAN_POINT('Ctrl Pts',(-35.5946982044237,0.892169363420933,
-0.357746184990163));
#55306=CARTESIAN_POINT('Ctrl Pts',(-35.7731184447994,0.896891204899179,
-1.38830064150969));
#55307=CARTESIAN_POINT('Ctrl Pts',(-36.0555939497443,0.904484667441719,
-2.38244503347954));
#55308=CARTESIAN_POINT('Ctrl Pts',(-35.9922681759013,0.608882116610321,
-2.40252489470072));
#55309=CARTESIAN_POINT('Ctrl Pts',(-36.2443785607268,0.615769948902191,
-3.28909825742476));
#55310=CARTESIAN_POINT('Ctrl Pts',(-36.5816919949173,0.625189340318007,
-4.15917917294117));
#55311=CARTESIAN_POINT('Ctrl Pts',(-37.5863972856988,0.654732027487002,
-6.1538645640023));
#55312=CARTESIAN_POINT('Ctrl Pts',(-39.0342187194187,0.708039659060072,
-8.28751826776375));
#55313=CARTESIAN_POINT('Ctrl Pts',(-41.0238977934904,0.762443843619788,
-10.0080550546168));
#55314=CARTESIAN_POINT('Ctrl Pts',(-42.7093426314559,0.924341288012181,
-11.1127801661199));
#55315=CARTESIAN_POINT('Ctrl Pts',(-43.9550916538701,1.07596757220897,-11.8065547998463));
#55316=CARTESIAN_POINT('Ctrl Pts',(-46.6258628903611,1.67564312080215,-12.8347074267587));
#55317=CARTESIAN_POINT('Ctrl Pts',(-49.3209792563777,2.61889807843932,-13.2552065788425));
#55318=CARTESIAN_POINT('Ctrl Pts',(-52.3365683940236,3.29462450617091,-13.1079278924267));
#55319=CARTESIAN_POINT('Ctrl Pts',(-54.3811675813475,3.50259527469106,-12.6377569789553));
#55320=CARTESIAN_POINT('Ctrl Pts',(-56.3432172769078,3.64215593963216,-11.8721821586535));
#55321=CARTESIAN_POINT('Ctrl Pts',(-57.3004435327768,3.72851730538224,-11.3729256118978));
#55322=CARTESIAN_POINT('Ctrl Pts',(-58.1983366806673,3.84837683953258,-10.8187721359246));
#55323=CARTESIAN_POINT('Ctrl Pts',(-58.7575257930806,3.92041942928577,-10.4498241116935));
#55324=CARTESIAN_POINT('Ctrl Pts',(-59.8115950408937,4.04339107950324,-9.64752989021953));
#55325=CARTESIAN_POINT('Ctrl Pts',(-61.3488447008931,4.10808603220261,-8.21282218706084));
#55326=CARTESIAN_POINT('Ctrl Pts',(-62.5172938429767,3.69736142138752,-6.63867657150117));
#55327=CARTESIAN_POINT('Ctrl Pts',(-63.180538680225,3.52130030141665,-5.41964915825797));
#55328=CARTESIAN_POINT('Ctrl Pts',(-63.6308402479908,3.43032212436478,-4.55486496656474));
#55329=CARTESIAN_POINT('Ctrl Pts',(-64.2552005173933,3.43711541496265,-3.07145772521243));
#55330=CARTESIAN_POINT('Ctrl Pts',(-64.7398338150334,3.64746919653615,-1.09596732690597));
#55331=CARTESIAN_POINT('Ctrl Pts',(-64.883657444038,3.70557613317877,0.145685389858161));
#55332=CARTESIAN_POINT('Ctrl Pts',(-64.9199369800284,3.69755989799623,0.697703834262555));
#55333=CARTESIAN_POINT('Ctrl Pts',(-64.9344053541345,3.69428520684122,0.941028798737093));
#55334=CARTESIAN_POINT('Ctrl Pts',(-64.9514652230736,3.68867191422421,1.42351021989472));
#55335=CARTESIAN_POINT('Ctrl Pts',(-64.9451323226112,3.68052822707428,2.33266296731874));
#55336=CARTESIAN_POINT('Ctrl Pts',(-64.8115806130686,3.67100337684105,4.00597005240495));
#55337=CARTESIAN_POINT('Ctrl Pts',(-64.4930085401915,3.6398247492517,5.40357234851391));
#55338=CARTESIAN_POINT('Ctrl Pts',(-63.9225371750656,3.55442398498814,7.10889226910018));
#55339=CARTESIAN_POINT('Ctrl Pts',(-63.0407763459327,3.40982158427969,9.15635693290283));
#55340=CARTESIAN_POINT('Ctrl Pts',(-61.7073917428413,3.19653576750585,10.9664076276178));
#55341=CARTESIAN_POINT('Ctrl Pts',(-58.8512171752399,2.79654951543426,13.8877565738267));
#55342=CARTESIAN_POINT('Ctrl Pts',(-55.3788151857701,2.24352248023264,15.8731131092571));
#55343=CARTESIAN_POINT('Ctrl Pts',(-48.0711268741737,1.31134848387323,16.8333529503183));
#55344=CARTESIAN_POINT('Ctrl Pts',(-42.9393497504966,0.908782583618137,
15.0329488636439));
#55345=CARTESIAN_POINT('Ctrl Pts',(-40.037135888014,0.76072091085068,12.3510345169592));
#55346=CARTESIAN_POINT('Ctrl Pts',(-39.0963650953478,0.714916638110273,
11.3999947936465));
#55347=CARTESIAN_POINT('Ctrl Pts',(-37.6670519522153,0.654669347149692,
9.68416817237497));
#55348=CARTESIAN_POINT('Ctrl Pts',(-36.6464607599348,0.624695100829358,
7.66263154429121));
#55349=CARTESIAN_POINT('Ctrl Pts',(-35.586343168216,0.59652792171092,4.51480593811151));
#55350=CARTESIAN_POINT('Ctrl Pts',(-35.3363720722281,0.591329963871329,
2.58396879028904));
#55351=CARTESIAN_POINT('Ctrl Pts',(-35.5287065927405,0.596283167752303,
-0.367726615960636));
#55352=CARTESIAN_POINT('Ctrl Pts',(-35.7081613409452,0.601120118890534,
-1.40343256371961));
#55353=CARTESIAN_POINT('Ctrl Pts',(-35.9922681759013,0.608882116610323,
-2.40252489470072));
#55354=CARTESIAN_POINT('Ctrl Pts',(-35.6788452868189,0.190821093669241,
-2.49451532637507));
#55355=CARTESIAN_POINT('Ctrl Pts',(-35.9371748016095,0.197823785522891,
-3.40120776118929));
#55356=CARTESIAN_POINT('Ctrl Pts',(-36.282732356387,0.207442112280784,-4.29073825142866));
#55357=CARTESIAN_POINT('Ctrl Pts',(-37.3127391006884,0.237223038563802,
-6.33180135183161));
#55358=CARTESIAN_POINT('Ctrl Pts',(-38.7939215560336,0.291757553947807,
-8.50810321664163));
#55359=CARTESIAN_POINT('Ctrl Pts',(-40.831367727429,0.343809372406078,-10.2771054693631));
#55360=CARTESIAN_POINT('Ctrl Pts',(-42.5704878635999,0.502424780495082,
-11.4310756317738));
#55361=CARTESIAN_POINT('Ctrl Pts',(-43.8601407661417,0.65251648547724,-12.1548977466516));
#55362=CARTESIAN_POINT('Ctrl Pts',(-46.6405321830093,1.24431899385572,-13.3013571802195));
#55363=CARTESIAN_POINT('Ctrl Pts',(-49.4150466416309,2.17965774129795,-13.8276699904443));
#55364=CARTESIAN_POINT('Ctrl Pts',(-52.487289380987,2.84182050128404,-13.7124729474502));
#55365=CARTESIAN_POINT('Ctrl Pts',(-54.5834122822819,3.04709747487405,-13.2191083636475));
#55366=CARTESIAN_POINT('Ctrl Pts',(-56.6086890147239,3.18486064563698,-12.396446266628));
#55367=CARTESIAN_POINT('Ctrl Pts',(-57.6010557122091,3.27180967339437,-11.848924443058));
#55368=CARTESIAN_POINT('Ctrl Pts',(-58.5304988833242,3.39304237564432,-11.251201716693));
#55369=CARTESIAN_POINT('Ctrl Pts',(-59.1071788251335,3.46491928745013,-10.8706615658623));
#55370=CARTESIAN_POINT('Ctrl Pts',(-60.1895627849156,3.5861844069988,-10.0428303353042));
#55371=CARTESIAN_POINT('Ctrl Pts',(-61.7323526812202,3.64882218416258,-8.60872134074377));
#55372=CARTESIAN_POINT('Ctrl Pts',(-62.8852363599739,3.25177729002768,-6.99767453874843));
#55373=CARTESIAN_POINT('Ctrl Pts',(-63.5663559032184,3.07268589980912,-5.68650329864844));
#55374=CARTESIAN_POINT('Ctrl Pts',(-64.0280889424921,2.98137593833669,-4.7548806456604));
#55375=CARTESIAN_POINT('Ctrl Pts',(-64.6668361058713,2.99356768937731,-3.17739735347249));
#55376=CARTESIAN_POINT('Ctrl Pts',(-65.1359228942973,3.2101415043566,-1.13275347647021));
#55377=CARTESIAN_POINT('Ctrl Pts',(-65.2645995616865,3.2700027911371,0.11596751667424));
#55378=CARTESIAN_POINT('Ctrl Pts',(-65.2970672831498,3.26337755333429,0.665229271993136));
#55379=CARTESIAN_POINT('Ctrl Pts',(-65.3101975596581,3.2605905741402,0.917050306601995));
#55380=CARTESIAN_POINT('Ctrl Pts',(-65.3252187606999,3.2556972790431,1.41248776916539));
#55381=CARTESIAN_POINT('Ctrl Pts',(-65.3170768123695,3.24806453671255,2.34819404964879));
#55382=CARTESIAN_POINT('Ctrl Pts',(-65.1849806435554,3.23714367305903,4.06366048664381));
#55383=CARTESIAN_POINT('Ctrl Pts',(-64.8682585802219,3.20411847574444,5.48964402016827));
#55384=CARTESIAN_POINT('Ctrl Pts',(-64.2891191680327,3.11906713455525,7.22967412462136));
#55385=CARTESIAN_POINT('Ctrl Pts',(-63.3933532975505,2.97528454618844,9.32178548398929));
#55386=CARTESIAN_POINT('Ctrl Pts',(-62.0251967524475,2.76420001016156,11.176124232464));
#55387=CARTESIAN_POINT('Ctrl Pts',(-59.1061532670881,2.36758918865814,14.1656659960127));
#55388=CARTESIAN_POINT('Ctrl Pts',(-55.5571056026393,1.82037527149572,16.1958610845329));
#55389=CARTESIAN_POINT('Ctrl Pts',(-48.0605713766001,0.895007067307973,
17.1791038904439));
#55390=CARTESIAN_POINT('Ctrl Pts',(-42.8024300701058,0.493573724953808,
15.3372352360987));
#55391=CARTESIAN_POINT('Ctrl Pts',(-39.8257879925702,0.344597652056968,
12.594654996906));
#55392=CARTESIAN_POINT('Ctrl Pts',(-38.8613094672086,0.298515741742694,
11.6219453892284));
#55393=CARTESIAN_POINT('Ctrl Pts',(-37.3959267257012,0.237691755664316,
9.86716981758532));
#55394=CARTESIAN_POINT('Ctrl Pts',(-36.34967000299,0.207126063084511,7.79970934891721));
#55395=CARTESIAN_POINT('Ctrl Pts',(-35.2628987004346,0.178306255067115,
4.58036202846229));
#55396=CARTESIAN_POINT('Ctrl Pts',(-35.0066880334485,0.172944297082686,
2.60569473777376));
#55397=CARTESIAN_POINT('Ctrl Pts',(-35.2038137596613,0.178003560438737,
-0.413421569693999));
#55398=CARTESIAN_POINT('Ctrl Pts',(-35.387730024456,0.182929659049877,-1.47275052239072));
#55399=CARTESIAN_POINT('Ctrl Pts',(-35.6788452868189,0.19082109366924,-2.49451532637507));
#55400=CARTESIAN_POINT('Ctrl Pts',(-35.3280864353835,0.0555127849838203,
-2.59511145651185));
#55401=CARTESIAN_POINT('Ctrl Pts',(-35.5930227147958,0.0623741059613249,
-3.52382056888469));
#55402=CARTESIAN_POINT('Ctrl Pts',(-35.9474295279237,0.0717571238130431,
-4.43479293536763));
#55403=CARTESIAN_POINT('Ctrl Pts',(-37.0036313064953,0.101206985431967,
-6.52566825268797));
#55404=CARTESIAN_POINT('Ctrl Pts',(-38.5220700933842,0.154518393969504,
-8.75194826360237));
#55405=CARTESIAN_POINT('Ctrl Pts',(-40.6072512998611,0.209107862145042,
-10.5688352699363));
#55406=CARTESIAN_POINT('Ctrl Pts',(-42.3874676158688,0.376237052150697,
-11.7654874351406));
#55407=CARTESIAN_POINT('Ctrl Pts',(-43.7107791876456,0.531145971673501,
-12.515371429476));
#55408=CARTESIAN_POINT('Ctrl Pts',(-46.5430769526905,1.17496549761945,-13.7574803436035));
#55409=CARTESIAN_POINT('Ctrl Pts',(-49.3605442991523,2.20753320357867,-14.3726106319492));
#55410=CARTESIAN_POINT('Ctrl Pts',(-52.5532731257945,2.9243401122523,-14.2847163631391));
#55411=CARTESIAN_POINT('Ctrl Pts',(-54.7393178368275,3.12348754878638,-13.7687183927178));
#55412=CARTESIAN_POINT('Ctrl Pts',(-56.8359906168391,3.23569223062666,-12.9035548079215));
#55413=CARTESIAN_POINT('Ctrl Pts',(-57.8576327536343,3.29986469632328,-12.3254963884192));
#55414=CARTESIAN_POINT('Ctrl Pts',(-58.8145013408182,3.40586009857496,-11.6988424821367));
#55415=CARTESIAN_POINT('Ctrl Pts',(-59.4122362997243,3.47946714478885,-11.3058944870703));
#55416=CARTESIAN_POINT('Ctrl Pts',(-60.532919917232,3.60139924350621,-10.4502770318816));
#55417=CARTESIAN_POINT('Ctrl Pts',(-62.1418004651168,3.67048433387294,-8.96072780586377));
#55418=CARTESIAN_POINT('Ctrl Pts',(-63.3061607182308,3.22908091298505,-7.27825424542751));
#55419=CARTESIAN_POINT('Ctrl Pts',(-63.9855192119155,3.0237769607437,-5.91821784636985));
#55420=CARTESIAN_POINT('Ctrl Pts',(-64.4473654457923,2.91464681574267,-4.94982855292355));
#55421=CARTESIAN_POINT('Ctrl Pts',(-65.0922321521348,2.91163642890028,-3.31422240884912));
#55422=CARTESIAN_POINT('Ctrl Pts',(-65.5562709582115,3.11313222367988,-1.20317387586483));
#55423=CARTESIAN_POINT('Ctrl Pts',(-65.6765118300283,3.16440593553937,0.0764583233013215));
#55424=CARTESIAN_POINT('Ctrl Pts',(-65.7065113328794,3.15556766719144,0.637330258957667));
#55425=CARTESIAN_POINT('Ctrl Pts',(-65.7184356601194,3.1516252764093,0.896477679082247));
#55426=CARTESIAN_POINT('Ctrl Pts',(-65.7317238609617,3.14520008550437,1.40543165819501));
#55427=CARTESIAN_POINT('Ctrl Pts',(-65.7218096180503,3.13643053510135,2.36692751924055));
#55428=CARTESIAN_POINT('Ctrl Pts',(-65.5903053362458,3.12832565018766,4.12841315210705));
#55429=CARTESIAN_POINT('Ctrl Pts',(-65.2714249136872,3.09979578088586,5.59308771296452));
#55430=CARTESIAN_POINT('Ctrl Pts',(-64.6778956707148,3.01523526234882,7.37918415885639));
#55431=CARTESIAN_POINT('Ctrl Pts',(-63.7590738429973,2.87171165703166,9.52742689805567));
#55432=CARTESIAN_POINT('Ctrl Pts',(-62.3499639442105,2.65618062577662,11.4286796347776));
#55433=CARTESIAN_POINT('Ctrl Pts',(-59.3509400735407,2.2550704713425,14.4935263716135));
#55434=CARTESIAN_POINT('Ctrl Pts',(-55.7061987517473,1.6997474464948,16.5669811264171));
#55435=CARTESIAN_POINT('Ctrl Pts',(-48.0174632092897,0.759785836285453,
17.5572025721814));
#55436=CARTESIAN_POINT('Ctrl Pts',(-42.6326410688909,0.35574578981809,15.6677377197388));
#55437=CARTESIAN_POINT('Ctrl Pts',(-39.5809054933731,0.207174781350006,
12.8596900461973));
#55438=CARTESIAN_POINT('Ctrl Pts',(-38.592216719327,0.16130623594675,11.8636454473681));
#55439=CARTESIAN_POINT('Ctrl Pts',(-37.0897327714284,0.101038920786803,
10.0669225154591));
#55440=CARTESIAN_POINT('Ctrl Pts',(-36.0165024752287,0.0711941104908416,
7.9496729397282));
#55441=CARTESIAN_POINT('Ctrl Pts',(-34.9015558309501,0.0431888394733598,
4.6523117895337));
#55442=CARTESIAN_POINT('Ctrl Pts',(-34.6386449346511,0.0380442549261144,
2.62945113732801));
#55443=CARTESIAN_POINT('Ctrl Pts',(-34.8408722523068,0.042968270696446,
-0.463365540987003));
#55444=CARTESIAN_POINT('Ctrl Pts',(-35.029525914519,0.0477806632471993,
-1.54853574050673));
#55445=CARTESIAN_POINT('Ctrl Pts',(-35.3280864353835,0.0555127849838172,
-2.59511145651185));
#55446=CARTESIAN_POINT('Ctrl Pts',(-35.11517701784,0.0508510909662703,-2.65562493453964));
#55447=CARTESIAN_POINT('Ctrl Pts',(-35.3840062951942,0.0575422421921914,
-3.5976188055133));
#55448=CARTESIAN_POINT('Ctrl Pts',(-35.7436259783105,0.0666559496806185,
-4.521538758328));
#55449=CARTESIAN_POINT('Ctrl Pts',(-36.8151557983613,0.095692551513825,
-6.64222332188911));
#55450=CARTESIAN_POINT('Ctrl Pts',(-38.3559078896116,0.147573716864128,
-8.89963534126349));
#55451=CARTESIAN_POINT('Ctrl Pts',(-40.469472385245,0.204977053081564,-10.7437628031316));
#55452=CARTESIAN_POINT('Ctrl Pts',(-42.2712014812638,0.381060117365087,
-11.9612747311747));
#55453=CARTESIAN_POINT('Ctrl Pts',(-43.6118086922819,0.540518683561826,
-12.724156531761));
#55454=CARTESIAN_POINT('Ctrl Pts',(-46.4621628306032,1.23462273661855,-14.0012119190018));
#55455=CARTESIAN_POINT('Ctrl Pts',(-49.295584910841,2.34465836914774,-14.632672959566));
#55456=CARTESIAN_POINT('Ctrl Pts',(-52.5620566289039,3.10483667886162,-14.5433464527275));
#55457=CARTESIAN_POINT('Ctrl Pts',(-54.8001566067438,3.30035269345341,-14.0186136905654));
#55458=CARTESIAN_POINT('Ctrl Pts',(-56.9350672575427,3.39429553816601,-13.1429311762582));
#55459=CARTESIAN_POINT('Ctrl Pts',(-57.9716624173195,3.44148099145208,-12.5594172014826));
#55460=CARTESIAN_POINT('Ctrl Pts',(-58.9428583166749,3.53537179799872,-11.9255218957174));
#55461=CARTESIAN_POINT('Ctrl Pts',(-59.5517785065692,3.61039741065779,-11.5258146157856));
#55462=CARTESIAN_POINT('Ctrl Pts',(-60.6939165981419,3.73345458801685,-10.6556781858428));
#55463=CARTESIAN_POINT('Ctrl Pts',(-62.3504191551611,3.80834832178581,-9.12254403970273));
#55464=CARTESIAN_POINT('Ctrl Pts',(-63.5361674281905,3.32898348528657,-7.40198206074098));
#55465=CARTESIAN_POINT('Ctrl Pts',(-64.2149763686856,3.10273760294942,-6.03098199576973));
#55466=CARTESIAN_POINT('Ctrl Pts',(-64.6776127435176,2.97884271655914,-5.05337165230659));
#55467=CARTESIAN_POINT('Ctrl Pts',(-65.3270688519725,2.96185205497302,-3.39714199807037));
#55468=CARTESIAN_POINT('Ctrl Pts',(-65.7950910047088,3.14840094628669,-1.25128635775172));
#55469=CARTESIAN_POINT('Ctrl Pts',(-65.9145204535827,3.19168477671591,0.0517785197280895));
#55470=CARTESIAN_POINT('Ctrl Pts',(-65.9441051213068,3.18047187028911,0.622955634058679));
#55471=CARTESIAN_POINT('Ctrl Pts',(-65.9557016612563,3.17533523586427,0.88586519906267));
#55472=CARTESIAN_POINT('Ctrl Pts',(-65.9685107144033,3.16731893908496,1.40252832323383));
#55473=CARTESIAN_POINT('Ctrl Pts',(-65.9579083168253,3.15739901945015,2.37829097111894));
#55474=CARTESIAN_POINT('Ctrl Pts',(-65.8257155275689,3.15229864335318,4.16664556351419));
#55475=CARTESIAN_POINT('Ctrl Pts',(-65.5034203203996,3.12833741358611,5.65528760646102));
#55476=CARTESIAN_POINT('Ctrl Pts',(-64.9002921012009,3.04408997663893,7.4699894353198));
#55477=CARTESIAN_POINT('Ctrl Pts',(-63.9662479404238,2.90055300510061,9.65247467963668));
#55478=CARTESIAN_POINT('Ctrl Pts',(-62.5336778099795,2.68044822146662,11.5812656319969));
#55479=CARTESIAN_POINT('Ctrl Pts',(-59.4862509442383,2.27438763852615,14.691094912035));
#55480=CARTESIAN_POINT('Ctrl Pts',(-55.783918038216,1.71016553075871,16.7906541149307));
#55481=CARTESIAN_POINT('Ctrl Pts',(-47.9845453946372,0.754692999391247,
17.7848020910906));
#55482=CARTESIAN_POINT('Ctrl Pts',(-42.5252504170977,0.347888964974057,
15.8667796976236));
#55483=CARTESIAN_POINT('Ctrl Pts',(-39.4298897457784,0.19996339908082,13.0192697191585));
#55484=CARTESIAN_POINT('Ctrl Pts',(-38.4270467968691,0.154379143867951,
12.0091830811851));
#55485=CARTESIAN_POINT('Ctrl Pts',(-36.9028760126082,0.0948092812359606,
10.1871843261409));
#55486=CARTESIAN_POINT('Ctrl Pts',(-35.8138531895274,0.0658148084159087,
8.03995386779416));
#55487=CARTESIAN_POINT('Ctrl Pts',(-34.682418296982,0.0387556318332189,
4.69562286008841));
#55488=CARTESIAN_POINT('Ctrl Pts',(-34.4155737946825,0.0338633837576097,
2.64375559367379));
#55489=CARTESIAN_POINT('Ctrl Pts',(-34.6207976535155,0.038627270703424,
-0.493388346484037));
#55490=CARTESIAN_POINT('Ctrl Pts',(-34.8122294213517,0.043310735981189,
-1.59407843213931));
#55491=CARTESIAN_POINT('Ctrl Pts',(-35.11517701784,0.0508510909662663,-2.65562493453964));
#55492=CARTESIAN_POINT('',(-36.055003997507,1.05060622379088,-2.38157894671781));
#55493=CARTESIAN_POINT('Ctrl Pts',(-35.11517701784,0.0508510909662703,-2.65562493453964));
#55494=CARTESIAN_POINT('Ctrl Pts',(-35.3280864353835,0.0555127849838203,
-2.59511145651185));
#55495=CARTESIAN_POINT('Ctrl Pts',(-35.6788452868189,0.190821093669241,
-2.49451532637507));
#55496=CARTESIAN_POINT('Ctrl Pts',(-35.9918225445504,0.608287708528165,
-2.40265568865918));
#55497=CARTESIAN_POINT('Ctrl Pts',(-36.0552784362427,0.903015554155871,
-2.38254505299135));
#55498=CARTESIAN_POINT('Ctrl Pts',(-36.055003997507,1.05060622379088,-2.38157894671781));
#55499=CARTESIAN_POINT('',(-64.8720027515639,4.16096914635678,1.63199606547109));
#55500=CARTESIAN_POINT('Ctrl Pts',(-36.055003997507,1.05060622379089,-2.38157894671782));
#55501=CARTESIAN_POINT('Ctrl Pts',(-36.1322935555675,1.05266199109914,-2.65366126311645));
#55502=CARTESIAN_POINT('Ctrl Pts',(-36.2176393940941,1.05494437214152,-2.92418923910143));
#55503=CARTESIAN_POINT('Ctrl Pts',(-36.3109765306706,1.05747450348401,-3.19257913391778));
#55504=CARTESIAN_POINT('Ctrl Pts',(-36.4042248382911,1.06000222690042,-3.46071360206248));
#55505=CARTESIAN_POINT('Ctrl Pts',(-36.5054492155598,1.0627772292734,-3.72671372010584));
#55506=CARTESIAN_POINT('Ctrl Pts',(-36.6145331160612,1.0658205868793,-3.99000253341186));
#55507=CARTESIAN_POINT('Ctrl Pts',(-36.7235075599445,1.06886089072907,-4.2530271582997));
#55508=CARTESIAN_POINT('Ctrl Pts',(-36.8403257011726,1.07216901153767,-4.51334558411149));
#55509=CARTESIAN_POINT('Ctrl Pts',(-36.9648203194525,1.07576596220024,-4.7703927225219));
#55510=CARTESIAN_POINT('Ctrl Pts',(-36.9953298241032,1.07664745558915,-4.83338645649311));
#55511=CARTESIAN_POINT('Ctrl Pts',(-37.026300123263,1.07754629545318,-4.89618378526105));
#55512=CARTESIAN_POINT('Ctrl Pts',(-37.0577282953327,1.07846279106366,-4.95877651989893));
#55513=CARTESIAN_POINT('Ctrl Pts',(-37.191989322685,1.0823780567035,-5.22617243585101));
#55514=CARTESIAN_POINT('Ctrl Pts',(-37.3339878357898,1.0867584845706,-5.48861222280936));
#55515=CARTESIAN_POINT('Ctrl Pts',(-37.4834941556401,1.09151956863047,-5.74597365794833));
#55516=CARTESIAN_POINT('Ctrl Pts',(-37.6350344703111,1.0963454260078,-6.00683642886125));
#55517=CARTESIAN_POINT('Ctrl Pts',(-37.7942884884527,1.10156236749132,-6.26248241688958));
#55518=CARTESIAN_POINT('Ctrl Pts',(-37.9610686654377,1.10708239086208,-6.51277093542689));
#55519=CARTESIAN_POINT('Ctrl Pts',(-38.1283425215666,1.11261875382703,-6.76380032271606));
#55520=CARTESIAN_POINT('Ctrl Pts',(-38.3031875375309,1.11845999561527,-7.00944112260689));
#55521=CARTESIAN_POINT('Ctrl Pts',(-38.4854614009836,1.12451733021712,-7.24952794553518));
#55522=CARTESIAN_POINT('Ctrl Pts',(-38.6673538937057,1.13056199108684,-7.48911243595516));
#55523=CARTESIAN_POINT('Ctrl Pts',(-38.8566446481855,1.13682184145623,-7.72316674673868));
#55524=CARTESIAN_POINT('Ctrl Pts',(-39.0532324665159,1.14320865145002,-7.95149404526017));
#55525=CARTESIAN_POINT('Ctrl Pts',(-39.1059157316391,1.1449202427737,-8.01268312454808));
#55526=CARTESIAN_POINT('Ctrl Pts',(-39.1591232574712,1.1466409520596,-8.0734606948525));
#55527=CARTESIAN_POINT('Ctrl Pts',(-39.2128535191938,1.14836908120523,-8.13382248951383));
#55528=CARTESIAN_POINT('Ctrl Pts',(-39.377032041595,1.15364956338699,-8.31826436526975));
#55529=CARTESIAN_POINT('Ctrl Pts',(-39.5461034134596,1.15899932279134,-8.49883113714326));
#55530=CARTESIAN_POINT('Ctrl Pts',(-39.7197596703417,1.16498249252869,-8.67513434098695));
#55531=CARTESIAN_POINT('Ctrl Pts',(-39.9019313933737,1.17125905497346,-8.86008280755486));
#55532=CARTESIAN_POINT('Ctrl Pts',(-40.0891487598253,1.17823267106649,-9.04033867429534));
#55533=CARTESIAN_POINT('Ctrl Pts',(-40.2810101475514,1.18655459897303,-9.21549445643098));
#55534=CARTESIAN_POINT('Ctrl Pts',(-40.4638745846345,1.19448628694898,-9.38243666341536));
#55535=CARTESIAN_POINT('Ctrl Pts',(-40.6509571307088,1.20364279891409,-9.54474595128902));
#55536=CARTESIAN_POINT('Ctrl Pts',(-40.8418740647712,1.21458800384062,-9.70210900822495));
#55537=CARTESIAN_POINT('Ctrl Pts',(-41.0328375236401,1.22553587601896,-9.85951041317748));
#55538=CARTESIAN_POINT('Ctrl Pts',(-41.2276369488457,1.23827331304294,-10.011962966512));
#55539=CARTESIAN_POINT('Ctrl Pts',(-41.425857428129,1.25336459621525,-10.1591951341152));
#55540=CARTESIAN_POINT('Ctrl Pts',(-41.6242463092005,1.26846870045974,-10.3065523854654));
#55541=CARTESIAN_POINT('Ctrl Pts',(-41.8260617492356,1.2859306520565,-10.4486801988254));
#55542=CARTESIAN_POINT('Ctrl Pts',(-42.0308613301175,1.30631617171648,-10.5853513426465));
#55543=CARTESIAN_POINT('Ctrl Pts',(-42.0607832486186,1.30929456578956,-10.6053194637201));
#55544=CARTESIAN_POINT('Ctrl Pts',(-42.0907688260537,1.31233536695569,-10.625171186479));
#55545=CARTESIAN_POINT('Ctrl Pts',(-42.120816641723,1.31544033955858,-10.644905885882));
#55546=CARTESIAN_POINT('Ctrl Pts',(-42.3559034005757,1.33973288559832,-10.7993053460842));
#55547=CARTESIAN_POINT('Ctrl Pts',(-42.5950137384494,1.36687278436907,-10.9466772342795));
#55548=CARTESIAN_POINT('Ctrl Pts',(-42.8376128379884,1.39836730966744,-11.086802603462));
#55549=CARTESIAN_POINT('Ctrl Pts',(-43.0805446382786,1.42990502660273,-11.2271201407756));
#55550=CARTESIAN_POINT('Ctrl Pts',(-43.3269744463138,1.46580932213761,-11.3601711739332));
#55551=CARTESIAN_POINT('Ctrl Pts',(-43.5763500708487,1.50759367980925,-11.4857858807722));
#55552=CARTESIAN_POINT('Ctrl Pts',(-43.6977164532822,1.52792933347377,-11.5469201739812));
#55553=CARTESIAN_POINT('Ctrl Pts',(-43.819780379753,1.54965772931728,-11.6062938729776));
#55554=CARTESIAN_POINT('Ctrl Pts',(-43.9424772606944,1.57295333338661,-11.6638917675623));
#55555=CARTESIAN_POINT('Ctrl Pts',(-44.1747498761995,1.6170533206515,-11.7729280651448));
#55556=CARTESIAN_POINT('Ctrl Pts',(-44.4093065880691,1.66676967748696,-11.8756041239089));
#55557=CARTESIAN_POINT('Ctrl Pts',(-44.6456367997568,1.72160486396264,-11.9718184735828));
#55558=CARTESIAN_POINT('Ctrl Pts',(-44.8824535709107,1.77655294577602,-12.0682309105104));
#55559=CARTESIAN_POINT('Ctrl Pts',(-45.1210507987122,1.83664095634219,-12.1581549600952));
#55560=CARTESIAN_POINT('Ctrl Pts',(-45.3609076348146,1.9013682763762,-12.2415404290646));
#55561=CARTESIAN_POINT('Ctrl Pts',(-45.5273868230638,1.94629404072762,-12.2994163912901));
#55562=CARTESIAN_POINT('Ctrl Pts',(-45.6944726686526,1.99345476140644,-12.3541435226089));
#55563=CARTESIAN_POINT('Ctrl Pts',(-45.8619903777366,2.042683047791,-12.4057197872398));
#55564=CARTESIAN_POINT('Ctrl Pts',(-46.0944304045427,2.11099000034794,-12.4772846886398));
#55565=CARTESIAN_POINT('Ctrl Pts',(-46.3276914891466,2.18327765523928,-12.5427863991036));
#55566=CARTESIAN_POINT('Ctrl Pts',(-46.5617698195259,2.25813907221755,-12.6023525500692));
#55567=CARTESIAN_POINT('Ctrl Pts',(-46.7972329711181,2.33344337375536,-12.6622710978983));
#55568=CARTESIAN_POINT('Ctrl Pts',(-47.0335235344732,2.41135198051783,-12.7161838131883));
#55569=CARTESIAN_POINT('Ctrl Pts',(-47.2706600841618,2.49043283361392,-12.7641729127843));
#55570=CARTESIAN_POINT('Ctrl Pts',(-47.5087361286878,2.56982699165316,-12.8123521370631));
#55571=CARTESIAN_POINT('Ctrl Pts',(-47.7476653612993,2.65040270290849,-12.8545608454763));
#55572=CARTESIAN_POINT('Ctrl Pts',(-47.9874819513711,2.73071082024241,-12.890832108857));
#55573=CARTESIAN_POINT('Ctrl Pts',(-48.227129692856,2.81096239473197,-12.92707783459));
#55574=CARTESIAN_POINT('Ctrl Pts',(-48.4676640406405,2.89094675197924,-12.9573945421757));
#55575=CARTESIAN_POINT('Ctrl Pts',(-48.7091270187202,2.96921780361185,-12.9817638440304));
#55576=CARTESIAN_POINT('Ctrl Pts',(-48.9494154580997,3.04710812450067,-13.0060146072655));
#55577=CARTESIAN_POINT('Ctrl Pts',(-49.1906240098808,3.12330176716413,-13.0243756948092));
#55578=CARTESIAN_POINT('Ctrl Pts',(-49.4327945273407,3.19637364319789,-13.036777533859));
#55579=CARTESIAN_POINT('Ctrl Pts',(-49.5681239803724,3.23720758582381,-13.0437079154463));
#55580=CARTESIAN_POINT('Ctrl Pts',(-49.7037538009874,3.27706666778437,-13.0487764279543));
#55581=CARTESIAN_POINT('Ctrl Pts',(-49.8396904754171,3.31570220099547,-13.0519638705386));
#55582=CARTESIAN_POINT('Ctrl Pts',(-50.1782233791656,3.41191905565005,-13.0599017886765));
#55583=CARTESIAN_POINT('Ctrl Pts',(-50.518582222015,3.50054751812004,-13.056172132156));
#55584=CARTESIAN_POINT('Ctrl Pts',(-50.8602747909478,3.5807299233009,-13.0404229903288));
#55585=CARTESIAN_POINT('Ctrl Pts',(-51.1751659120314,3.65462303586533,-13.0259091689087));
#55586=CARTESIAN_POINT('Ctrl Pts',(-51.4911898131278,3.72134309963386,-13.0011868511954));
#55587=CARTESIAN_POINT('Ctrl Pts',(-51.8079187282795,3.78021885210975,-12.9659530059506));
#55588=CARTESIAN_POINT('Ctrl Pts',(-51.8348765969948,3.78522996644075,-12.9629541342689));
#55589=CARTESIAN_POINT('Ctrl Pts',(-51.8618395452152,3.79018425432501,-12.9598790993903));
#55590=CARTESIAN_POINT('Ctrl Pts',(-51.8888072932649,3.79508130187158,-12.9567277064462));
#55591=CARTESIAN_POINT('Ctrl Pts',(-52.099829761794,3.83340066987668,-12.9320680753509));
#55592=CARTESIAN_POINT('Ctrl Pts',(-52.3111643310852,3.86821518154434,-12.9027265467538));
#55593=CARTESIAN_POINT('Ctrl Pts',(-52.5223516668009,3.89997784147055,-12.8686708631832));
#55594=CARTESIAN_POINT('Ctrl Pts',(-52.7330469211624,3.93166649216386,-12.8346945317519));
#55595=CARTESIAN_POINT('Ctrl Pts',(-52.9435952878337,3.9603174966052,-12.7960259885999));
#55596=CARTESIAN_POINT('Ctrl Pts',(-53.15354205119,3.9863807001654,-12.7526850506438));
#55597=CARTESIAN_POINT('Ctrl Pts',(-53.3633141711024,4.01242222314546,-12.7093801656877));
#55598=CARTESIAN_POINT('Ctrl Pts',(-53.5724853493314,4.03588024875905,-12.6614106889577));
#55599=CARTESIAN_POINT('Ctrl Pts',(-53.780608504578,4.05720350070397,-12.6088479826448));
#55600=CARTESIAN_POINT('Ctrl Pts',(-53.9887349759261,4.07852709239997,-12.5562844388312));
#55601=CARTESIAN_POINT('Ctrl Pts',(-54.1958130568032,4.09771584239852,-12.4991275895464));
#55602=CARTESIAN_POINT('Ctrl Pts',(-54.4014072013379,4.11521849584678,-12.4374996534384));
#55603=CARTESIAN_POINT('Ctrl Pts',(-54.5862926290981,4.13095817353576,-12.3820792651044));
#55604=CARTESIAN_POINT('Ctrl Pts',(-54.7699779948038,4.14533431612562,-12.3230438550149));
#55605=CARTESIAN_POINT('Ctrl Pts',(-54.9521578365331,4.15867326758291,-12.2605165051515));
#55606=CARTESIAN_POINT('Ctrl Pts',(-55.1517001248123,4.17328347292599,-12.192030055974));
#55607=CARTESIAN_POINT('Ctrl Pts',(-55.3494514939048,4.1866493698181,-12.1193573255133));
#55608=CARTESIAN_POINT('Ctrl Pts',(-55.5455657376014,4.19972898490674,-12.0424636765534));
#55609=CARTESIAN_POINT('Ctrl Pts',(-55.6748708970455,4.20835284456439,-11.9917649340675));
#55610=CARTESIAN_POINT('Ctrl Pts',(-55.8034640727799,4.21685225070397,-11.9392302238067));
#55611=CARTESIAN_POINT('Ctrl Pts',(-55.9313849198071,4.22550180155907,-11.8848380394075));
#55612=CARTESIAN_POINT('Ctrl Pts',(-56.1506171346802,4.24032550102394,-11.7916200899119));
#55613=CARTESIAN_POINT('Ctrl Pts',(-56.3678647316653,4.25559019800313,-11.6929433272729));
#55614=CARTESIAN_POINT('Ctrl Pts',(-56.5826783791045,4.2721750813338,-11.5889779895733));
#55615=CARTESIAN_POINT('Ctrl Pts',(-56.7974907879464,4.28875986903743,-11.4850132513289));
#55616=CARTESIAN_POINT('Ctrl Pts',(-57.0098689485361,4.30666482786843,-11.3757601408548));
#55617=CARTESIAN_POINT('Ctrl Pts',(-57.2193847947822,4.32676913145603,-11.2614365003806));
#55618=CARTESIAN_POINT('Ctrl Pts',(-57.415690155682,4.34560580964584,-11.1543212443999));
#55619=CARTESIAN_POINT('Ctrl Pts',(-57.6094827608094,4.36637322822266,-11.0427552658619));
#55620=CARTESIAN_POINT('Ctrl Pts',(-57.8004311760719,4.38979452405874,-10.9269537836621));
#55621=CARTESIAN_POINT('Ctrl Pts',(-57.9483123118011,4.40793328590039,-10.8372706371259));
#55622=CARTESIAN_POINT('Ctrl Pts',(-58.0948414911701,4.42652998500644,-10.7448297287611));
#55623=CARTESIAN_POINT('Ctrl Pts',(-58.2396322283765,4.44497959030501,-10.6498619680056));
#55624=CARTESIAN_POINT('Ctrl Pts',(-58.3740970612243,4.4621134425144,-10.5616669334177));
#55625=CARTESIAN_POINT('Ctrl Pts',(-58.5070626671158,4.47912043310067,-10.4712931632196));
#55626=CARTESIAN_POINT('Ctrl Pts',(-58.6382418504244,4.49551596420629,-10.3789591096853));
#55627=CARTESIAN_POINT('Ctrl Pts',(-58.7793571620321,4.5131533699485,-10.2796312406754));
#55628=CARTESIAN_POINT('Ctrl Pts',(-58.918404907508,4.5300831784743,-10.1780449583785));
#55629=CARTESIAN_POINT('Ctrl Pts',(-59.0556314028655,4.54572602503811,-10.0740454574417));
#55630=CARTESIAN_POINT('Ctrl Pts',(-59.1833292612958,4.5602826746177,-9.97726740074885));
#55631=CARTESIAN_POINT('Ctrl Pts',(-59.3094499076329,4.57372488341918,-9.87839907259325));
#55632=CARTESIAN_POINT('Ctrl Pts',(-59.4341673742325,4.58558578894325,-9.77728339330231));
#55633=CARTESIAN_POINT('Ctrl Pts',(-59.5962054154582,4.60099596324107,-9.64590976091361));
#55634=CARTESIAN_POINT('Ctrl Pts',(-59.7558736542354,4.613736854791,-9.51073085320083));
#55635=CARTESIAN_POINT('Ctrl Pts',(-59.9127949926263,4.6227019676806,-9.37199436529526));
#55636=CARTESIAN_POINT('Ctrl Pts',(-60.0695888566196,4.63165979779797,-9.23337057939951));
#55637=CARTESIAN_POINT('Ctrl Pts',(-60.2236400109866,4.63684798123959,-9.09119519083188));
#55638=CARTESIAN_POINT('Ctrl Pts',(-60.374604228999,4.63716271647514,-8.94575635226619));
#55639=CARTESIAN_POINT('Ctrl Pts',(-60.5255583550716,4.63747743067068,-8.80032723626937));
#55640=CARTESIAN_POINT('Ctrl Pts',(-60.6734257119601,4.63291934821723,-8.65163533700792));
#55641=CARTESIAN_POINT('Ctrl Pts',(-60.8178979821347,4.62238488893667,-8.50000659817944));
#55642=CARTESIAN_POINT('Ctrl Pts',(-60.8461349302844,4.6203259403223,-8.47037092601109));
#55643=CARTESIAN_POINT('Ctrl Pts',(-60.8742423012993,4.61803869245437,-8.44062317532011));
#55644=CARTESIAN_POINT('Ctrl Pts',(-60.9022179651097,4.61551490577955,-8.41076593635432));
#55645=CARTESIAN_POINT('Ctrl Pts',(-61.1259061652568,4.59533517733165,-8.17203301152134));
#55646=CARTESIAN_POINT('Ctrl Pts',(-61.341181112213,4.56003280409024,-7.92628709053869));
#55647=CARTESIAN_POINT('Ctrl Pts',(-61.5476559471016,4.51576670901703,-7.67416287821696));
#55648=CARTESIAN_POINT('Ctrl Pts',(-61.7546563946079,4.47138792796869,-7.42139684594989));
#55649=CARTESIAN_POINT('Ctrl Pts',(-61.9528118061257,4.41799973000764,-7.1622202527666));
#55650=CARTESIAN_POINT('Ctrl Pts',(-62.1417816318185,4.3618081933155,-6.89729085245331));
#55651=CARTESIAN_POINT('Ctrl Pts',(-62.3315145775604,4.30538973738861,-6.63129158325373));
#55652=CARTESIAN_POINT('Ctrl Pts',(-62.5119875421368,4.24614525547315,-6.35949319617911));
#55653=CARTESIAN_POINT('Ctrl Pts',(-62.6829063613797,4.19035631611767,-6.0825760589589));
#55654=CARTESIAN_POINT('Ctrl Pts',(-62.7797254131915,4.158753990324,-5.92571296585504));
#55655=CARTESIAN_POINT('Ctrl Pts',(-62.8734796582814,4.12826047706972,-5.76720761562995));
#55656=CARTESIAN_POINT('Ctrl Pts',(-62.9641228638388,4.10001755239961,-5.60718528462863));
#55657=CARTESIAN_POINT('Ctrl Pts',(-63.0152047876007,4.08410126925475,-5.51700479661378));
#55658=CARTESIAN_POINT('Ctrl Pts',(-63.0653027666178,4.06889974586153,-5.42634434508404));
#55659=CARTESIAN_POINT('Ctrl Pts',(-63.114690027439,4.05526150059234,-5.33467778889543));
#55660=CARTESIAN_POINT('Ctrl Pts',(-63.1438918413464,4.04719744735773,-5.2804769753488));
#55661=CARTESIAN_POINT('Ctrl Pts',(-63.1728443241659,4.03967993925421,-5.22592394033852));
#55662=CARTESIAN_POINT('Ctrl Pts',(-63.2015963121648,4.0328843828772,-5.17090601533745));
#55663=CARTESIAN_POINT('Ctrl Pts',(-63.2894948262794,4.01210949565389,-5.00270916378545));
#55664=CARTESIAN_POINT('Ctrl Pts',(-63.3744719191724,3.99625727530115,-4.83215125581444));
#55665=CARTESIAN_POINT('Ctrl Pts',(-63.4562599252191,3.98469841004765,-4.65961827175044));
#55666=CARTESIAN_POINT('Ctrl Pts',(-63.5366571757962,3.97333609629173,-4.49001910650485));
#55667=CARTESIAN_POINT('Ctrl Pts',(-63.6139728247038,3.96612236725379,-4.31851180304446));
#55668=CARTESIAN_POINT('Ctrl Pts',(-63.6879982711723,3.962459471557,-4.14548861462962));
#55669=CARTESIAN_POINT('Ctrl Pts',(-63.7639445164335,3.9587015317103,-3.96797585205806));
#55670=CARTESIAN_POINT('Ctrl Pts',(-63.8364272308132,3.95868108869533,-3.78886772818592));
#55671=CARTESIAN_POINT('Ctrl Pts',(-63.9052732336969,3.96175264228226,-3.60861111381425));
#55672=CARTESIAN_POINT('Ctrl Pts',(-63.9741192365805,3.9648241958692,-3.42835449944258));
#55673=CARTESIAN_POINT('Ctrl Pts',(-64.0393284286319,3.97098774605804,-3.24694973670777));
#55674=CARTESIAN_POINT('Ctrl Pts',(-64.1007822541809,3.97959779261897,-3.06486232390459));
#55675=CARTESIAN_POINT('Ctrl Pts',(-64.1702270221536,3.98932741775323,-2.85909778410764));
#55676=CARTESIAN_POINT('Ctrl Pts',(-64.2348845570762,4.00218114911087,-2.652469780862));
#55677=CARTESIAN_POINT('Ctrl Pts',(-64.2948630613201,4.01668597766837,-2.44487228947275));
#55678=CARTESIAN_POINT('Ctrl Pts',(-64.3549604873855,4.03121956553977,-2.23686318608836));
#55679=CARTESIAN_POINT('Ctrl Pts',(-64.4103604314521,4.04741080449716,-2.02788033843582));
#55680=CARTESIAN_POINT('Ctrl Pts',(-64.4611227734419,4.06377790634833,-1.81779844513638));
#55681=CARTESIAN_POINT('Ctrl Pts',(-64.5118609248486,4.08013720852512,-1.60781666549011));
#55682=CARTESIAN_POINT('Ctrl Pts',(-64.5579659879566,4.09667220602219,-1.39673647437591));
#55683=CARTESIAN_POINT('Ctrl Pts',(-64.5994472931465,4.11190322805798,-1.18442030572762));
#55684=CARTESIAN_POINT('Ctrl Pts',(-64.6204216122818,4.11960453628521,-1.07706623240652));
#55685=CARTESIAN_POINT('Ctrl Pts',(-64.6402129899606,4.12697246390265,-0.969396004279037));
#55686=CARTESIAN_POINT('Ctrl Pts',(-64.6588176023091,4.13381573006831,-0.861391140572027));
#55687=CARTESIAN_POINT('Ctrl Pts',(-64.6983751695293,4.14836604459698,-0.631748642454824));
#55688=CARTESIAN_POINT('Ctrl Pts',(-64.732559846353,4.16054445540993,-0.400605174382738));
#55689=CARTESIAN_POINT('Ctrl Pts',(-64.7612370512181,4.16849178751679,-0.168417716141251));
#55690=CARTESIAN_POINT('Ctrl Pts',(-64.7898878583897,4.17643180401403,0.063556010903203));
#55691=CARTESIAN_POINT('Ctrl Pts',(-64.8130412472295,4.18014852773221,0.296571463029256));
#55692=CARTESIAN_POINT('Ctrl Pts',(-64.8306138183485,4.17778791313152,0.530161692369568));
#55693=CARTESIAN_POINT('Ctrl Pts',(-64.8336767293851,4.17737645640931,0.570876627402885));
#55694=CARTESIAN_POINT('Ctrl Pts',(-64.8365702175283,4.17678036573755,0.611609004456205));
#55695=CARTESIAN_POINT('Ctrl Pts',(-64.839294001694,4.17598982323856,0.652356328090951));
#55696=CARTESIAN_POINT('Ctrl Pts',(-64.8432954133527,4.17482846617806,0.712216730359264));
#55697=CARTESIAN_POINT('Ctrl Pts',(-64.8469308150517,4.17368838965138,0.772114743988323));
#55698=CARTESIAN_POINT('Ctrl Pts',(-64.8501981550959,4.1726021357397,0.832015202980184));
#55699=CARTESIAN_POINT('Ctrl Pts',(-64.8600001752284,4.16934337400467,1.01171657995577));
#55700=CARTESIAN_POINT('Ctrl Pts',(-64.8664934873315,4.16656901580476,1.19143948170663));
#55701=CARTESIAN_POINT('Ctrl Pts',(-64.8696864375022,4.1641759703485,1.37131271729487));
#55702=CARTESIAN_POINT('Ctrl Pts',(-64.8712285716237,4.16302017496955,1.45818806433278));
#55703=CARTESIAN_POINT('Ctrl Pts',(-64.8719999767219,4.16195332864408,1.54509863601051));
#55704=CARTESIAN_POINT('Ctrl Pts',(-64.8719999999995,4.16096914635678,1.63199606547182));
#55705=CARTESIAN_POINT('Ctrl Pts',(-64.8720055031283,4.16096914635646,1.63199606549839));
#55706=CARTESIAN_POINT('Ctrl Pts',(-64.8719930365275,4.15923636219392,1.78499063561214));
#55707=CARTESIAN_POINT('Ctrl Pts',(-64.8620592180002,4.15312946060718,2.41759877960346));
#55708=CARTESIAN_POINT('Ctrl Pts',(-64.7352335229478,4.14731569311366,3.99634452035672));
#55709=CARTESIAN_POINT('Ctrl Pts',(-64.4136487318254,4.12105688799969,5.39708413320686));
#55710=CARTESIAN_POINT('Ctrl Pts',(-63.8397399723428,4.03549450524408,7.10448416695828));
#55711=CARTESIAN_POINT('Ctrl Pts',(-62.9522997363556,3.89000867503392,9.15140293674327));
#55712=CARTESIAN_POINT('Ctrl Pts',(-61.6208708298335,3.67142317516158,10.9503238549484));
#55713=CARTESIAN_POINT('Ctrl Pts',(-58.7634589988956,3.26466779407872,13.8578351195001));
#55714=CARTESIAN_POINT('Ctrl Pts',(-55.2912534175913,2.6998098225271,15.8249286900159));
#55715=CARTESIAN_POINT('Ctrl Pts',(-48.0385774976576,1.75094933219347,16.7544728922648));
#55716=CARTESIAN_POINT('Ctrl Pts',(-42.9496055667091,1.34558036473629,14.9600338121896));
#55717=CARTESIAN_POINT('Ctrl Pts',(-40.071051319765,1.19886194165591,12.29337200187));
#55718=CARTESIAN_POINT('Ctrl Pts',(-39.1375314597392,1.15352274909741,11.3477862008985));
#55719=CARTESIAN_POINT('Ctrl Pts',(-37.7188484542204,1.09430323930076,9.64179625830726));
#55720=CARTESIAN_POINT('Ctrl Pts',(-36.7050175851536,1.06546586823309,7.63138184708971));
#55721=CARTESIAN_POINT('Ctrl Pts',(-35.6516869686853,1.03855926629819,4.50020178467594));
#55722=CARTESIAN_POINT('Ctrl Pts',(-35.4031623106733,1.03368706569832,2.57903751737137));
#55723=CARTESIAN_POINT('Ctrl Pts',(-35.594321537606,1.03843169037817,-0.357311618779464));
#55724=CARTESIAN_POINT('Ctrl Pts',(-35.7726576378221,1.04309630355831,-1.3876354762478));
#55725=CARTESIAN_POINT('Ctrl Pts',(-36.055003997507,1.05060622379088,-2.38157894671782));
#55726=CARTESIAN_POINT('Origin',(-50.184,-32.64,1.632));
#55727=CARTESIAN_POINT('',(-64.8718846268333,6.25079236928354,1.6329527449831));
#55728=CARTESIAN_POINT('',(-64.872,-32.64,1.632));
#55729=CARTESIAN_POINT('',(-36.065644266864,3.13140677366842,-2.41884872497431));
#55730=CARTESIAN_POINT('Ctrl Pts',(-36.065644266864,3.13140677366842,-2.41884872497431));
#55731=CARTESIAN_POINT('Ctrl Pts',(-35.7780846374424,3.12368828933858,-1.4166219279989));
#55732=CARTESIAN_POINT('Ctrl Pts',(-35.5953745209546,3.11887456876326,-0.372879642437447));
#55733=CARTESIAN_POINT('Ctrl Pts',(-35.4027861848181,3.11402573771371,2.58487032700104));
#55734=CARTESIAN_POINT('Ctrl Pts',(-35.6521037255763,3.11894001012135,4.4959742368839));
#55735=CARTESIAN_POINT('Ctrl Pts',(-36.9698692287106,3.1530828253069,8.42617802922758));
#55736=CARTESIAN_POINT('Ctrl Pts',(-38.1616212543277,3.1879695783913,10.3549179060355));
#55737=CARTESIAN_POINT('Ctrl Pts',(-42.4613671667828,3.39627919561991,14.7446124362785));
#55738=CARTESIAN_POINT('Ctrl Pts',(-50.2262334512378,3.97083149861718,17.9144169067269));
#55739=CARTESIAN_POINT('Ctrl Pts',(-57.9134779272454,5.23514997311662,14.7265287262636));
#55740=CARTESIAN_POINT('Ctrl Pts',(-62.2002402570179,5.85744949443928,10.3661404754207));
#55741=CARTESIAN_POINT('Ctrl Pts',(-63.3943845893009,6.06869311513403,8.42892326864068));
#55742=CARTESIAN_POINT('Ctrl Pts',(-64.6118270133895,6.24609538226257,4.81359831624348));
#55743=CARTESIAN_POINT('Ctrl Pts',(-64.8712207656872,6.23100612702719,3.22312584190541));
#55744=CARTESIAN_POINT('Ctrl Pts',(-64.8718846268333,6.25079236928354,1.6329527449831));
#55745=CARTESIAN_POINT('Ctrl Pts',(-64.8718846268333,6.25079236928354,1.6329527449831));
#55746=CARTESIAN_POINT('Ctrl Pts',(-64.8720137299782,6.25464026144678,1.32370682963648));
#55747=CARTESIAN_POINT('Ctrl Pts',(-64.8623577223499,6.2598071376853,1.01447223668158));
#55748=CARTESIAN_POINT('Ctrl Pts',(-64.8279255683366,6.27285046627563,0.470282225806653));
#55749=CARTESIAN_POINT('Ctrl Pts',(-64.7869366759734,6.27297083982397,0.00182753649455431));
#55750=CARTESIAN_POINT('Ctrl Pts',(-64.6604441900832,6.24060155475075,-0.928432328896818));
#55751=CARTESIAN_POINT('Ctrl Pts',(-64.3201724720767,6.12732012565137,-2.54924414126407));
#55752=CARTESIAN_POINT('Ctrl Pts',(-63.8282831273652,6.05945295552752,-3.88543452904561));
#55753=CARTESIAN_POINT('Ctrl Pts',(-62.9004728688998,6.33137887468648,-5.81565625714699));
#55754=CARTESIAN_POINT('Ctrl Pts',(-61.6122544655027,7.13811360863407,-7.83110990015508));
#55755=CARTESIAN_POINT('Ctrl Pts',(-59.8048511793193,7.01369953657289,-9.53478552281347));
#55756=CARTESIAN_POINT('Ctrl Pts',(-58.6631333960574,6.8704405564795,-10.363121955978));
#55757=CARTESIAN_POINT('Ctrl Pts',(-58.3493696503069,6.83776391263835,-10.5817734230167));
#55758=CARTESIAN_POINT('Ctrl Pts',(-57.7047601394273,6.7930417097451,-10.9951030826806));
#55759=CARTESIAN_POINT('Ctrl Pts',(-56.5377248070284,6.7584186916988,-11.6470045461552));
#55760=CARTESIAN_POINT('Ctrl Pts',(-54.0569552148524,6.75345765423783,-12.6904602333806));
#55761=CARTESIAN_POINT('Ctrl Pts',(-50.2178417525627,6.25049709636969,-13.2722316651482));
#55762=CARTESIAN_POINT('Ctrl Pts',(-46.7178274773985,4.51449035845978,-12.7648792404124));
#55763=CARTESIAN_POINT('Ctrl Pts',(-43.9411365965136,3.61830280145254,-11.7305732722043));
#55764=CARTESIAN_POINT('Ctrl Pts',(-42.5911117010961,3.45233648724814,-10.9642662180381));
#55765=CARTESIAN_POINT('Ctrl Pts',(-41.4467701567403,3.33147776885485,-10.1910309575598));
#55766=CARTESIAN_POINT('Ctrl Pts',(-40.4532021950847,3.27050850699576,-9.42430687806686));
#55767=CARTESIAN_POINT('Ctrl Pts',(-38.6732274933371,3.21130715662269,-7.64161528907957));
#55768=CARTESIAN_POINT('Ctrl Pts',(-37.6213539969012,3.17638521197561,-6.08089500182063));
#55769=CARTESIAN_POINT('Ctrl Pts',(-36.6477529660739,3.14707541849258,-4.14218022621547));
#55770=CARTESIAN_POINT('Ctrl Pts',(-36.3151556718838,3.13810399286304,-3.28846667783078));
#55771=CARTESIAN_POINT('Ctrl Pts',(-36.065644266864,3.13140677366842,-2.41884872497431));
#55772=CARTESIAN_POINT('Ctrl Pts',(-36.065644266864,3.13140677366842,-2.41884872497431));
#55773=CARTESIAN_POINT('Ctrl Pts',(-35.7780846374424,3.12368828933858,-1.4166219279989));
#55774=CARTESIAN_POINT('Ctrl Pts',(-35.5953745209546,3.11887456876326,-0.372879642437447));
#55775=CARTESIAN_POINT('Ctrl Pts',(-35.4027861848181,3.11402573771371,2.58487032700104));
#55776=CARTESIAN_POINT('Ctrl Pts',(-35.6521037255763,3.11894001012135,4.4959742368839));
#55777=CARTESIAN_POINT('Ctrl Pts',(-36.9698692287106,3.1530828253069,8.42617802922758));
#55778=CARTESIAN_POINT('Ctrl Pts',(-38.1616212543277,3.1879695783913,10.3549179060355));
#55779=CARTESIAN_POINT('Ctrl Pts',(-42.4613671667828,3.39627919561991,14.7446124362785));
#55780=CARTESIAN_POINT('Ctrl Pts',(-50.2262334512378,3.97083149861718,17.9144169067269));
#55781=CARTESIAN_POINT('Ctrl Pts',(-57.9134779272454,5.23514997311662,14.7265287262636));
#55782=CARTESIAN_POINT('Ctrl Pts',(-62.2002402570179,5.85744949443928,10.3661404754207));
#55783=CARTESIAN_POINT('Ctrl Pts',(-63.3943845893009,6.06869311513403,8.42892326864068));
#55784=CARTESIAN_POINT('Ctrl Pts',(-64.7103648856598,6.26045404234611,4.52097960892216));
#55785=CARTESIAN_POINT('Ctrl Pts',(-64.9627582385739,6.22177417224124,2.60127270216699));
#55786=CARTESIAN_POINT('Ctrl Pts',(-64.8279255683366,6.27285046627563,0.470282225806653));
#55787=CARTESIAN_POINT('Ctrl Pts',(-64.7869366759734,6.27297083982397,0.00182753649455431));
#55788=CARTESIAN_POINT('Ctrl Pts',(-64.6604441900832,6.24060155475075,-0.928432328896818));
#55789=CARTESIAN_POINT('Ctrl Pts',(-64.3201724720767,6.12732012565137,-2.54924414126407));
#55790=CARTESIAN_POINT('Ctrl Pts',(-63.8282831273652,6.05945295552752,-3.88543452904561));
#55791=CARTESIAN_POINT('Ctrl Pts',(-62.9004728688998,6.33137887468648,-5.81565625714699));
#55792=CARTESIAN_POINT('Ctrl Pts',(-61.6122544655027,7.13811360863407,-7.83110990015508));
#55793=CARTESIAN_POINT('Ctrl Pts',(-59.8048511793193,7.01369953657289,-9.53478552281347));
#55794=CARTESIAN_POINT('Ctrl Pts',(-58.6631333960574,6.8704405564795,-10.363121955978));
#55795=CARTESIAN_POINT('Ctrl Pts',(-58.3493696503069,6.83776391263835,-10.5817734230167));
#55796=CARTESIAN_POINT('Ctrl Pts',(-57.7047601394273,6.7930417097451,-10.9951030826806));
#55797=CARTESIAN_POINT('Ctrl Pts',(-56.5377248070284,6.7584186916988,-11.6470045461552));
#55798=CARTESIAN_POINT('Ctrl Pts',(-54.0569552148524,6.75345765423783,-12.6904602333806));
#55799=CARTESIAN_POINT('Ctrl Pts',(-50.2178417525627,6.25049709636969,-13.2722316651482));
#55800=CARTESIAN_POINT('Ctrl Pts',(-46.7178274773985,4.51449035845978,-12.7648792404124));
#55801=CARTESIAN_POINT('Ctrl Pts',(-43.9411365965136,3.61830280145254,-11.7305732722043));
#55802=CARTESIAN_POINT('Ctrl Pts',(-42.5911117010961,3.45233648724814,-10.9642662180381));
#55803=CARTESIAN_POINT('Ctrl Pts',(-41.4467701567403,3.33147776885485,-10.1910309575598));
#55804=CARTESIAN_POINT('Ctrl Pts',(-40.4532021950847,3.27050850699576,-9.42430687806686));
#55805=CARTESIAN_POINT('Ctrl Pts',(-38.6732274933371,3.21130715662269,-7.64161528907957));
#55806=CARTESIAN_POINT('Ctrl Pts',(-37.6213539969012,3.17638521197561,-6.08089500182063));
#55807=CARTESIAN_POINT('Ctrl Pts',(-36.6477529660739,3.14707541849258,-4.14218022621547));
#55808=CARTESIAN_POINT('Ctrl Pts',(-36.3151556718838,3.13810399286304,-3.28846667783078));
#55809=CARTESIAN_POINT('Ctrl Pts',(-36.065644266864,3.13140677366842,-2.41884872497431));
#55810=CARTESIAN_POINT('Ctrl Pts',(-36.0650646070859,3.4346612700204,-2.41682844638411));
#55811=CARTESIAN_POINT('Ctrl Pts',(-35.7778621348589,3.42677312832869,-1.41532929226861));
#55812=CARTESIAN_POINT('Ctrl Pts',(-35.5953276311515,3.42184355033732,-0.371937396594396));
#55813=CARTESIAN_POINT('Ctrl Pts',(-35.4029663176075,3.41686295257622,2.58412733083116));
#55814=CARTESIAN_POINT('Ctrl Pts',(-35.6520686551882,3.42197511366452,4.49482638811762));
#55815=CARTESIAN_POINT('Ctrl Pts',(-36.968521585772,3.4572178918651,8.42244597254387));
#55816=CARTESIAN_POINT('Ctrl Pts',(-38.1580037490657,3.49281635955522,10.3496423448272));
#55817=CARTESIAN_POINT('Ctrl Pts',(-42.4498664685835,3.70275922439794,14.7330424895737));
#55818=CARTESIAN_POINT('Ctrl Pts',(-50.1810892659201,4.27080024554784,17.9103274086348));
#55819=CARTESIAN_POINT('Ctrl Pts',(-57.8815423520458,5.51753858629548,14.7469836103004));
#55820=CARTESIAN_POINT('Ctrl Pts',(-62.1866799556937,6.13507517348564,10.3858739129262));
#55821=CARTESIAN_POINT('Ctrl Pts',(-63.3857030057778,6.34398363305886,8.44800531621039));
#55822=CARTESIAN_POINT('Ctrl Pts',(-64.7107997545463,6.53780208228581,4.52413466314126));
#55823=CARTESIAN_POINT('Ctrl Pts',(-64.9616943271868,6.50914304046526,2.5989830365699));
#55824=CARTESIAN_POINT('Ctrl Pts',(-64.8281749317427,6.55133949313081,0.475090785410251));
#55825=CARTESIAN_POINT('Ctrl Pts',(-64.7863724086547,6.54981290757855,-0.00354337177167986));
#55826=CARTESIAN_POINT('Ctrl Pts',(-64.6582750072647,6.51215776525242,-0.94161213829145));
#55827=CARTESIAN_POINT('Ctrl Pts',(-64.3145441725083,6.38690347009193,-2.568589975368));
#55828=CARTESIAN_POINT('Ctrl Pts',(-63.8287571100992,6.3086096976912,-3.88066143217033));
#55829=CARTESIAN_POINT('Ctrl Pts',(-62.9289673976073,6.54418319192483,-5.76366911909594));
#55830=CARTESIAN_POINT('Ctrl Pts',(-61.6371827042111,7.32609606241457,-7.81260292844509));
#55831=CARTESIAN_POINT('Ctrl Pts',(-59.7926587181835,7.21283514873646,-9.54588742378878));
#55832=CARTESIAN_POINT('Ctrl Pts',(-58.6482498454689,7.07001126275249,-10.3736593014408));
#55833=CARTESIAN_POINT('Ctrl Pts',(-58.3385085297827,7.03254425950593,-10.5890602215478));
#55834=CARTESIAN_POINT('Ctrl Pts',(-57.6985348409166,6.98190728715686,-10.998859774944));
#55835=CARTESIAN_POINT('Ctrl Pts',(-56.5373250194885,6.93691002365351,-11.6473031199624));
#55836=CARTESIAN_POINT('Ctrl Pts',(-54.0509279624105,6.92531201937256,-12.6932902933945));
#55837=CARTESIAN_POINT('Ctrl Pts',(-50.1679811065434,6.42171268884258,-13.2814410926045));
#55838=CARTESIAN_POINT('Ctrl Pts',(-46.6184476459557,4.72761566928903,-12.740305567001));
#55839=CARTESIAN_POINT('Ctrl Pts',(-43.8944244000067,3.90614836057661,-11.7049493454516));
#55840=CARTESIAN_POINT('Ctrl Pts',(-42.5674858734948,3.74857859214072,-10.9494179972056));
#55841=CARTESIAN_POINT('Ctrl Pts',(-41.4315976471264,3.62970738952218,-10.1792648565723));
#55842=CARTESIAN_POINT('Ctrl Pts',(-40.4473443265289,3.57455025905753,-9.41841100374971));
#55843=CARTESIAN_POINT('Ctrl Pts',(-38.6696727269255,3.51502557823487,-7.63715913873979));
#55844=CARTESIAN_POINT('Ctrl Pts',(-37.6188008298502,3.48053370900519,-6.076262128612));
#55845=CARTESIAN_POINT('Ctrl Pts',(-36.6466007134482,3.45067784482792,-4.13925470645933));
#55846=CARTESIAN_POINT('Ctrl Pts',(-36.3142661118821,3.44150569849757,-3.28581503386884));
#55847=CARTESIAN_POINT('Ctrl Pts',(-36.0650646070859,3.4346612700204,-2.41682844638411));
#55848=CARTESIAN_POINT('Ctrl Pts',(-35.8155534753675,3.95922815415782,-2.48463600652939));
#55849=CARTESIAN_POINT('Ctrl Pts',(-35.5240223169276,3.95107190238858,-1.46597111396737));
#55850=CARTESIAN_POINT('Ctrl Pts',(-35.3388157069111,3.94595107338873,-0.40527320525134));
#55851=CARTESIAN_POINT('Ctrl Pts',(-35.1436102274987,3.94076100294377,2.60032378867928));
#55852=CARTESIAN_POINT('Ctrl Pts',(-35.3963491893894,3.94620086831573,4.54302230566112));
#55853=CARTESIAN_POINT('Ctrl Pts',(-36.731867402577,3.98322862837942,8.53671442736042));
#55854=CARTESIAN_POINT('Ctrl Pts',(-37.9377019443431,4.01999998102908,10.495940394407));
#55855=CARTESIAN_POINT('Ctrl Pts',(-42.2899491029564,4.2324854098098,14.9509728434312));
#55856=CARTESIAN_POINT('Ctrl Pts',(-50.1129881046017,4.78982733568662,18.1867023470396));
#55857=CARTESIAN_POINT('Ctrl Pts',(-57.9483290593166,6.00736287403418,14.9823983499893));
#55858=CARTESIAN_POINT('Ctrl Pts',(-62.3399356821522,6.61691276101214,10.5486133037616));
#55859=CARTESIAN_POINT('Ctrl Pts',(-63.5613060337253,6.82198967979261,8.57896237194291));
#55860=CARTESIAN_POINT('Ctrl Pts',(-64.9230450981126,7.0192762223136,4.5726621091647));
#55861=CARTESIAN_POINT('Ctrl Pts',(-65.192622059577,7.00684276405108,2.60965408956806));
#55862=CARTESIAN_POINT('Ctrl Pts',(-65.0446288523742,7.03437779670717,0.466431163727447));
#55863=CARTESIAN_POINT('Ctrl Pts',(-64.9980055512648,7.03014036934465,-0.0365399369319378));
#55864=CARTESIAN_POINT('Ctrl Pts',(-64.8571340870366,6.98374035596922,-1.00071940981554));
#55865=CARTESIAN_POINT('Ctrl Pts',(-64.4848024323001,6.83851971166886,-2.65718050680847));
#55866=CARTESIAN_POINT('Ctrl Pts',(-63.9862452561701,6.74259812652883,-3.93751639334648));
#55867=CARTESIAN_POINT('Ctrl Pts',(-63.0899327077538,6.91582060101885,-5.74134045894053));
#55868=CARTESIAN_POINT('Ctrl Pts',(-61.7532719631801,7.65468816352199,-7.84153086863482));
#55869=CARTESIAN_POINT('Ctrl Pts',(-59.8421629477594,7.56060613887443,-9.64672021837555));
#55870=CARTESIAN_POINT('Ctrl Pts',(-58.6851925837328,7.41843354268482,-10.4808914644111));
#55871=CARTESIAN_POINT('Ctrl Pts',(-58.3767589854455,7.37274010456707,-10.687376889481));
#55872=CARTESIAN_POINT('Ctrl Pts',(-57.7367797264508,7.31190480666232,-11.0881951675255));
#55873=CARTESIAN_POINT('Ctrl Pts',(-56.5732669821134,7.24895695789893,-11.7252028912417));
#55874=CARTESIAN_POINT('Ctrl Pts',(-54.0603724547201,7.22580025282231,-12.7753953588624));
#55875=CARTESIAN_POINT('Ctrl Pts',(-50.0841495080587,6.72117303445737,-13.3797286087254));
#55876=CARTESIAN_POINT('Ctrl Pts',(-46.4191811247196,5.10039243267267,-12.8412071463471));
#55877=CARTESIAN_POINT('Ctrl Pts',(-43.7167587333486,4.40484600132639,-11.8767330810714));
#55878=CARTESIAN_POINT('Ctrl Pts',(-42.3981754693853,4.26102412055946,-11.1378753168652));
#55879=CARTESIAN_POINT('Ctrl Pts',(-41.2564486598985,4.14573262965561,-10.3613182181735));
#55880=CARTESIAN_POINT('Ctrl Pts',(-40.2650697587731,4.10017673244414,-9.60492248587169));
#55881=CARTESIAN_POINT('Ctrl Pts',(-38.4589390717363,4.04017090207336,-7.79283393642232));
#55882=CARTESIAN_POINT('Ctrl Pts',(-37.3917532046939,4.00650035743647,-6.20548621434273));
#55883=CARTESIAN_POINT('Ctrl Pts',(-36.4057350142359,3.97579715932729,-4.23644501702129));
#55884=CARTESIAN_POINT('Ctrl Pts',(-36.068510919692,3.96630521794014,-3.36851706138635));
#55885=CARTESIAN_POINT('Ctrl Pts',(-35.8155534753675,3.95922815415782,-2.48463600652939));
#55886=CARTESIAN_POINT('Ctrl Pts',(-35.300583251693,4.13600582362742,-2.63111698861473));
#55887=CARTESIAN_POINT('Ctrl Pts',(-34.9991934800771,4.12811190259441,-1.57610435146056));
#55888=CARTESIAN_POINT('Ctrl Pts',(-34.8077644827284,4.12317489235507,-0.477647028350931));
#55889=CARTESIAN_POINT('Ctrl Pts',(-34.6060333124814,4.11818868004728,2.6346991492121));
#55890=CARTESIAN_POINT('Ctrl Pts',(-34.8671273680138,4.12331427351438,4.64644201761164));
#55891=CARTESIAN_POINT('Ctrl Pts',(-36.2471277637543,4.1586388019116,8.78323323890242));
#55892=CARTESIAN_POINT('Ctrl Pts',(-37.4935827303532,4.19414050837293,10.81320828298));
#55893=CARTESIAN_POINT('Ctrl Pts',(-41.9963149144722,4.40389550232149,15.4313894678807));
#55894=CARTESIAN_POINT('Ctrl Pts',(-50.1022225688271,4.9674647626258,18.7736207894476));
#55895=CARTESIAN_POINT('Ctrl Pts',(-58.1850741698473,6.2085491891343,15.4255183205296));
#55896=CARTESIAN_POINT('Ctrl Pts',(-62.712974569855,6.82560512914881,10.841656335752));
#55897=CARTESIAN_POINT('Ctrl Pts',(-63.969610611664,7.03376995866941,8.80641509887463));
#55898=CARTESIAN_POINT('Ctrl Pts',(-65.3827943906313,7.23025660308972,4.66801890208108));
#55899=CARTESIAN_POINT('Ctrl Pts',(-65.6866084443025,7.20685314020845,2.63859554445347));
#55900=CARTESIAN_POINT('Ctrl Pts',(-65.5116379537911,7.24390206311906,0.433244296697788));
#55901=CARTESIAN_POINT('Ctrl Pts',(-65.4585912453259,7.24146200832042,-0.0918947338236302));
#55902=CARTESIAN_POINT('Ctrl Pts',(-65.2992289363671,7.19990543690473,-1.08988473989177));
#55903=CARTESIAN_POINT('Ctrl Pts',(-64.8836246369305,7.06430956710991,-2.79529312832537));
#55904=CARTESIAN_POINT('Ctrl Pts',(-64.3446567263413,6.97888693816536,-4.0813056792627));
#55905=CARTESIAN_POINT('Ctrl Pts',(-63.3883510078546,7.15506110909943,-5.84612212194586));
#55906=CARTESIAN_POINT('Ctrl Pts',(-61.9668081348504,7.89578816450023,-7.96758783776226));
#55907=CARTESIAN_POINT('Ctrl Pts',(-59.999382965377,7.80389026779883,-9.85943516852207));
#55908=CARTESIAN_POINT('Ctrl Pts',(-58.8198661566153,7.6612085250852,-10.7098022926259));
#55909=CARTESIAN_POINT('Ctrl Pts',(-58.5032990808582,7.6148790028951,-10.9062394845128));
#55910=CARTESIAN_POINT('Ctrl Pts',(-57.8503744210902,7.5524633917664,-11.2975303524532));
#55911=CARTESIAN_POINT('Ctrl Pts',(-56.664326473605,7.48518113024164,-11.9193059799705));
#55912=CARTESIAN_POINT('Ctrl Pts',(-54.1048100395427,7.45888940763357,-12.9741605614099));
#55913=CARTESIAN_POINT('Ctrl Pts',(-50.018244533416,6.94967066206464,-13.5982483167349));
#55914=CARTESIAN_POINT('Ctrl Pts',(-46.2497967424538,5.33227973346929,-13.1575362520759));
#55915=CARTESIAN_POINT('Ctrl Pts',(-43.4813240908299,4.60340874785693,-12.3181482587086));
#55916=CARTESIAN_POINT('Ctrl Pts',(-42.1142395829665,4.4453022212816,-11.574327561683));
#55917=CARTESIAN_POINT('Ctrl Pts',(-40.9360947918748,4.32903411911999,-10.7753888548978));
#55918=CARTESIAN_POINT('Ctrl Pts',(-39.9057722307278,4.27570940455937,-10.0065317563462));
#55919=CARTESIAN_POINT('Ctrl Pts',(-38.0354999795452,4.21604903461122,-8.12865768725083));
#55920=CARTESIAN_POINT('Ctrl Pts',(-36.9302316463433,4.18186405058577,-6.48531537837426));
#55921=CARTESIAN_POINT('Ctrl Pts',(-35.9107301048361,4.15202804468452,-4.44559361297825));
#55922=CARTESIAN_POINT('Ctrl Pts',(-35.5620948746067,4.14285526675692,-3.54653646505307));
#55923=CARTESIAN_POINT('Ctrl Pts',(-35.300583251693,4.13600582362742,-2.63111698861472));
#55924=CARTESIAN_POINT('Ctrl Pts',(-35.0820169555422,4.1311553285547,-2.69386316078375));
#55925=CARTESIAN_POINT('Ctrl Pts',(-34.7762954146415,4.123468523943,-1.62332480119136));
#55926=CARTESIAN_POINT('Ctrl Pts',(-34.5821230489298,4.11867398866152,-0.50868185551124));
#55927=CARTESIAN_POINT('Ctrl Pts',(-34.3775118580705,4.11384875218964,2.64941339379631));
#55928=CARTESIAN_POINT('Ctrl Pts',(-34.6423025074559,4.11873027055746,4.6907194393648));
#55929=CARTESIAN_POINT('Ctrl Pts',(-36.04198628679,4.1527224694396,8.88871095791407));
#55930=CARTESIAN_POINT('Ctrl Pts',(-37.3065050558491,4.18726914503329,10.9489520915154));
#55931=CARTESIAN_POINT('Ctrl Pts',(-41.8756295459123,4.39494595491279,15.6369502302462));
#55932=CARTESIAN_POINT('Ctrl Pts',(-50.1074923035213,4.9640760014635,19.0246939944322));
#55933=CARTESIAN_POINT('Ctrl Pts',(-58.2965417115554,6.22483785549351,15.6153467534928));
#55934=CARTESIAN_POINT('Ctrl Pts',(-62.8818624102576,6.84805526665328,10.9666861040641));
#55935=CARTESIAN_POINT('Ctrl Pts',(-64.1536744099658,7.05889697316184,8.903002529081));
#55936=CARTESIAN_POINT('Ctrl Pts',(-65.587111358284,7.2541543028841,4.709423159478));
#55937=CARTESIAN_POINT('Ctrl Pts',(-65.9028420963167,7.22055997092229,2.65197203401351));
#55938=CARTESIAN_POINT('Ctrl Pts',(-65.7186730629668,7.26645282243596,0.417296843035803));
#55939=CARTESIAN_POINT('Ctrl Pts',(-65.6635658897677,7.26567899418896,-0.115119959858279));
#55940=CARTESIAN_POINT('Ctrl Pts',(-65.4980339395569,7.22894983406278,-1.12644210521919));
#55941=CARTESIAN_POINT('Ctrl Pts',(-65.0673144851431,7.10361635805402,-2.85325522762648));
#55942=CARTESIAN_POINT('Ctrl Pts',(-64.5112907294815,7.02863116832091,-4.14935247202906));
#55943=CARTESIAN_POINT('Ctrl Pts',(-63.5261863279776,7.22128027561666,-5.90893413005372));
#55944=CARTESIAN_POINT('Ctrl Pts',(-62.068197594767,7.97414050458901,-8.03433541315561));
#55945=CARTESIAN_POINT('Ctrl Pts',(-60.0796098167125,7.87873199265082,-9.96197480208937));
#55946=CARTESIAN_POINT('Ctrl Pts',(-58.8895882593918,7.73549412644146,-10.8202271543694));
#55947=CARTESIAN_POINT('Ctrl Pts',(-58.5684317890665,7.6908639977441,-11.0130747863924));
#55948=CARTESIAN_POINT('Ctrl Pts',(-57.9084119982073,7.63003527898566,-11.4010944726287));
#55949=CARTESIAN_POINT('Ctrl Pts',(-56.7102378337881,7.56456386339554,-12.0170276546053));
#55950=CARTESIAN_POINT('Ctrl Pts',(-54.1289712559167,7.53905427079786,-13.0742974757744));
#55951=CARTESIAN_POINT('Ctrl Pts',(-49.9948035131066,7.02745080169609,-13.706606972641));
#55952=CARTESIAN_POINT('Ctrl Pts',(-46.1914722110254,5.3927514423487,-13.3156545423547));
#55953=CARTESIAN_POINT('Ctrl Pts',(-43.3908039796773,4.61571635395792,-12.5174764940247));
#55954=CARTESIAN_POINT('Ctrl Pts',(-41.9985023915937,4.44701923023704,-11.7653170427634));
#55955=CARTESIAN_POINT('Ctrl Pts',(-40.8028218808128,4.32952815033359,-10.9557009467549));
#55956=CARTESIAN_POINT('Ctrl Pts',(-39.754901868991,4.26984177464805,-10.1782379949765));
#55957=CARTESIAN_POINT('Ctrl Pts',(-37.85694008542,4.21051024093903,-8.27236172411371));
#55958=CARTESIAN_POINT('Ctrl Pts',(-36.735234866715,4.17590258588924,-6.60510917508678));
#55959=CARTESIAN_POINT('Ctrl Pts',(-35.7009394011684,4.14674880041722,-4.5350945305174));
#55960=CARTESIAN_POINT('Ctrl Pts',(-35.3472871931217,4.13782505970798,-3.62275408600405));
#55961=CARTESIAN_POINT('Ctrl Pts',(-35.0820169555422,4.1311553285547,-2.69386316078375));
#55962=CARTESIAN_POINT('Ctrl Pts',(-35.0820169555422,4.1311553285547,-2.69386316078375));
#55963=CARTESIAN_POINT('Ctrl Pts',(-35.300583251693,4.13600582362742,-2.63111698861473));
#55964=CARTESIAN_POINT('Ctrl Pts',(-35.8155534753675,3.95922815415782,-2.48463600652939));
#55965=CARTESIAN_POINT('Ctrl Pts',(-36.0650646070859,3.4346612700204,-2.41682844638411));
#55966=CARTESIAN_POINT('Ctrl Pts',(-36.065644266864,3.13140677366842,-2.41884872497431));
#55967=CARTESIAN_POINT('Ctrl Pts',(1.34046462259684,-0.994431239233107,
-23.5830172776492));
#55968=CARTESIAN_POINT('Ctrl Pts',(1.15566339708668,-0.981222287792037,
-23.7427314913969));
#55969=CARTESIAN_POINT('Ctrl Pts',(0.510597376526876,-0.937346932838556,
-24.1271727076141));
#55970=CARTESIAN_POINT('Ctrl Pts',(-0.795414560778026,-0.941634478778648,
-24.119095744646));
#55971=CARTESIAN_POINT('Ctrl Pts',(-1.58219675349064,-1.01297453127524,
-23.4267441649288));
#55972=CARTESIAN_POINT('Ctrl Pts',(-2.00978422295716,-1.0483911567391,-22.6184046246051));
#55973=CARTESIAN_POINT('Ctrl Pts',(-2.11303381784703,-1.05826233623046,
-22.0402329203993));
#55974=CARTESIAN_POINT('Ctrl Pts',(-1.91580205826814,-1.04028492443336,
-21.212120769873));
#55975=CARTESIAN_POINT('Ctrl Pts',(-1.54497027776593,-1.00976017368561,
-20.5983257098217));
#55976=CARTESIAN_POINT('Ctrl Pts',(-0.607145822015571,-0.940669573101927,
-19.9292256569487));
#55977=CARTESIAN_POINT('Ctrl Pts',(0.606887110287569,-0.939423264837247,
-19.9262432814847));
#55978=CARTESIAN_POINT('Ctrl Pts',(1.54458406111778,-1.00903316772747,-20.5984241362299));
#55979=CARTESIAN_POINT('Ctrl Pts',(2.14134596539594,-1.05914052353263,-21.578464777093));
#55980=CARTESIAN_POINT('Ctrl Pts',(2.07601143327058,-1.05435985255611,-22.4957984055296));
#55981=CARTESIAN_POINT('Ctrl Pts',(1.69261614119323,-1.02145958385162,-23.2155194332715));
#55982=CARTESIAN_POINT('Ctrl Pts',(1.53141254982529,-1.00807953562059,-23.4179907851037));
#55983=CARTESIAN_POINT('Ctrl Pts',(1.34046462259684,-0.994431239233105,
-23.5830172776492));
#55984=CARTESIAN_POINT('Ctrl Pts',(1.33240415293763,-1.28753222554999,-23.5899835278486));
#55985=CARTESIAN_POINT('Ctrl Pts',(1.1469157030279,-1.27577525109937,-23.7485337176985));
#55986=CARTESIAN_POINT('Ctrl Pts',(0.501623816284161,-1.23758746220324,
-24.1249425674433));
#55987=CARTESIAN_POINT('Ctrl Pts',(-0.780574636333104,-1.2409583285191,
-24.1189164938403));
#55988=CARTESIAN_POINT('Ctrl Pts',(-1.57425541223237,-1.3038793604076,-23.435400280391));
#55989=CARTESIAN_POINT('Ctrl Pts',(-2.00781896637476,-1.33644887563698,
-22.6230530338899));
#55990=CARTESIAN_POINT('Ctrl Pts',(-2.11303497262538,-1.34561536136995,
-22.0396719347269));
#55991=CARTESIAN_POINT('Ctrl Pts',(-1.91258908442446,-1.32903543096936,
-21.2060259117698));
#55992=CARTESIAN_POINT('Ctrl Pts',(-1.53633055206404,-1.30096043919022,
-20.5893234525047));
#55993=CARTESIAN_POINT('Ctrl Pts',(-0.596251688256806,-1.24026580005628,
-19.9304047255554));
#55994=CARTESIAN_POINT('Ctrl Pts',(0.595626544455079,-1.23930620689027,
-19.9281869876753));
#55995=CARTESIAN_POINT('Ctrl Pts',(1.53605999452011,-1.30033581584115,-20.5900175249093));
#55996=CARTESIAN_POINT('Ctrl Pts',(2.14157620787691,-1.34648816973293,-21.5740783667172));
#55997=CARTESIAN_POINT('Ctrl Pts',(2.07534233636514,-1.34187841054564,-22.5011424018098));
#55998=CARTESIAN_POINT('Ctrl Pts',(1.68697288849109,-1.31176837112141,-23.2237452080945));
#55999=CARTESIAN_POINT('Ctrl Pts',(1.52406216244111,-1.29968025051912,-23.4261597759772));
#56000=CARTESIAN_POINT('Ctrl Pts',(1.33240415293763,-1.28753222554998,-23.5899835278486));
#56001=CARTESIAN_POINT('Ctrl Pts',(1.4758309169534,-1.79544747755601,-23.7841728091566));
#56002=CARTESIAN_POINT('Ctrl Pts',(1.26838865034841,-1.78601872806586,-23.9621689855623));
#56003=CARTESIAN_POINT('Ctrl Pts',(0.551030494946323,-1.75703447393435,
-24.3824714148802));
#56004=CARTESIAN_POINT('Ctrl Pts',(-0.858786621919096,-1.75892874024821,
-24.3770422952472));
#56005=CARTESIAN_POINT('Ctrl Pts',(-1.74729745582464,-1.80824551117858,
-23.6127100620137));
#56006=CARTESIAN_POINT('Ctrl Pts',(-2.23527843187923,-1.8361855302437,-22.6984081072173));
#56007=CARTESIAN_POINT('Ctrl Pts',(-2.35403929323783,-1.84418965457546,
-22.0410059801487));
#56008=CARTESIAN_POINT('Ctrl Pts',(-2.12796028967623,-1.82989818874935,
-21.1014645536594));
#56009=CARTESIAN_POINT('Ctrl Pts',(-1.70448676238135,-1.80582090614153,
-20.4074451781338));
#56010=CARTESIAN_POINT('Ctrl Pts',(-0.655240694168969,-1.75868262352979,
-19.6708937823934));
#56011=CARTESIAN_POINT('Ctrl Pts',(0.655193324216905,-1.7581595208231,-19.6684797661189));
#56012=CARTESIAN_POINT('Ctrl Pts',(1.70386306074689,-1.80534861734831,-20.4079383197073));
#56013=CARTESIAN_POINT('Ctrl Pts',(2.38615076333066,-1.84508770821069,-21.5157914644901));
#56014=CARTESIAN_POINT('Ctrl Pts',(2.31069308799246,-1.8407737494664,-22.5596482740071));
#56015=CARTESIAN_POINT('Ctrl Pts',(1.87321043198864,-1.81518150600845,-23.3728871164866));
#56016=CARTESIAN_POINT('Ctrl Pts',(1.69017295239418,-1.80518983811954,-23.6002562748075));
#56017=CARTESIAN_POINT('Ctrl Pts',(1.4758309169534,-1.79544747755601,-23.7841728091566));
#56018=CARTESIAN_POINT('Ctrl Pts',(1.80304354213939,-1.98648318031429,-24.1734013935208));
#56019=CARTESIAN_POINT('Ctrl Pts',(1.55183159751857,-1.97512642852453,-24.3932594536731));
#56020=CARTESIAN_POINT('Ctrl Pts',(0.679721866652848,-1.93861163401404,
-24.9201620196685));
#56021=CARTESIAN_POINT('Ctrl Pts',(-1.05900238101113,-1.94168634007152,
-24.910084768943));
#56022=CARTESIAN_POINT('Ctrl Pts',(-2.13145659008938,-2.00220229591781,
-23.9590865594632));
#56023=CARTESIAN_POINT('Ctrl Pts',(-2.71931215681635,-2.03407334807429,
-22.8426999176217));
#56024=CARTESIAN_POINT('Ctrl Pts',(-2.86228855524459,-2.04307423559703,
-22.043277402193));
#56025=CARTESIAN_POINT('Ctrl Pts',(-2.59014207056062,-2.02683577645921,
-20.8988502028586));
#56026=CARTESIAN_POINT('Ctrl Pts',(-2.08038729224802,-1.99936686297598,
-20.051300417594));
#56027=CARTESIAN_POINT('Ctrl Pts',(-0.80844853421373,-1.94110132490594,
-19.1332915718003));
#56028=CARTESIAN_POINT('Ctrl Pts',(0.808258885423883,-1.94022830439346,
-19.1294522906829));
#56029=CARTESIAN_POINT('Ctrl Pts',(2.07969237177025,-1.99876909577637,-20.0515337319994));
#56030=CARTESIAN_POINT('Ctrl Pts',(2.90085466420141,-2.04396331371082,-21.404748876263));
#56031=CARTESIAN_POINT('Ctrl Pts',(2.81033956030822,-2.03937236813819,-22.6732842137794));
#56032=CARTESIAN_POINT('Ctrl Pts',(2.28328462136404,-2.00996084831922,-23.6670462324578));
#56033=CARTESIAN_POINT('Ctrl Pts',(2.06261108552529,-1.99821767075566,-23.946230600932));
#56034=CARTESIAN_POINT('Ctrl Pts',(1.80304354213939,-1.98648318031429,-24.1734013935208));
#56035=CARTESIAN_POINT('Ctrl Pts',(1.94662784270136,-1.99329185033283,-24.3399175880524));
#56036=CARTESIAN_POINT('Ctrl Pts',(1.67638127074653,-1.98030748769492,-24.5776542418215));
#56037=CARTESIAN_POINT('Ctrl Pts',(0.736629093141336,-1.93751000700026,
-25.1500576569261));
#56038=CARTESIAN_POINT('Ctrl Pts',(-1.14750345414621,-1.94155549971475,
-25.1379865951392));
#56039=CARTESIAN_POINT('Ctrl Pts',(-2.29979798593773,-2.01146084484187,
-24.1072334392769));
#56040=CARTESIAN_POINT('Ctrl Pts',(-2.93067378779831,-2.04663627148226,
-22.9044123516052));
#56041=CARTESIAN_POINT('Ctrl Pts',(-3.08401460891383,-2.05645871391943,
-22.0442241048096));
#56042=CARTESIAN_POINT('Ctrl Pts',(-2.79208955112528,-2.03860098114137,
-20.8121763806738));
#56043=CARTESIAN_POINT('Ctrl Pts',(-2.24515915919612,-2.00827757256358,
-19.898951478238));
#56044=CARTESIAN_POINT('Ctrl Pts',(-0.876173007874418,-1.94068884397439,
-18.9033970954646));
#56045=CARTESIAN_POINT('Ctrl Pts',(0.875895764425228,-1.93951554837252,
-18.8989606653587));
#56046=CARTESIAN_POINT('Ctrl Pts',(2.2444503085602,-2.00757360901504,-19.8990971193787));
#56047=CARTESIAN_POINT('Ctrl Pts',(3.12537961073622,-2.05736838288602,-21.3572403317401));
#56048=CARTESIAN_POINT('Ctrl Pts',(3.02843680266979,-2.05254349855045,-22.721972135133));
#56049=CARTESIAN_POINT('Ctrl Pts',(2.46280778521956,-2.01992324553137,-23.7929340812186));
#56050=CARTESIAN_POINT('Ctrl Pts',(2.22586312706117,-2.00670808783477,-24.0942735392203));
#56051=CARTESIAN_POINT('Ctrl Pts',(1.94662784270136,-1.99329185033284,-24.3399175880524));
#56052=CARTESIAN_POINT('',(1.34046462259684,-0.994431239233107,-23.5830172776492));
#56053=CARTESIAN_POINT('Ctrl Pts',(1.94661322350961,-1.99329115684075,-24.3399006340105));
#56054=CARTESIAN_POINT('Ctrl Pts',(1.80303402327035,-1.9864776228478,-24.1733900705544));
#56055=CARTESIAN_POINT('Ctrl Pts',(1.47582883074698,-1.79544008970153,-23.7841699845866));
#56056=CARTESIAN_POINT('Ctrl Pts',(1.33240415293763,-1.28753222554999,-23.5899835278486));
#56057=CARTESIAN_POINT('Ctrl Pts',(1.34046462259684,-0.994431239233107,
-23.5830172776492));
#56058=CARTESIAN_POINT('',(-2.04965785769565,-1.05238869753535,-22.0330650649484));
#56059=CARTESIAN_POINT('Ctrl Pts',(1.34046462259684,-0.994431239233107,
-23.5830172776492));
#56060=CARTESIAN_POINT('Ctrl Pts',(1.15566339708668,-0.981222287792037,
-23.7427314913969));
#56061=CARTESIAN_POINT('Ctrl Pts',(0.510597376526876,-0.937346932838556,
-24.1271727076141));
#56062=CARTESIAN_POINT('Ctrl Pts',(-0.795414560778026,-0.941634478778648,
-24.119095744646));
#56063=CARTESIAN_POINT('Ctrl Pts',(-1.58219675349064,-1.01297453127524,
-23.4267441649288));
#56064=CARTESIAN_POINT('Ctrl Pts',(-1.96798801478004,-1.04492922027809,
-22.6974189318937));
#56065=CARTESIAN_POINT('Ctrl Pts',(-2.04906955950107,-1.05226003620114,
-22.3656080815114));
#56066=CARTESIAN_POINT('Ctrl Pts',(-2.04965785769565,-1.05238869753535,
-22.0330650649484));
#56067=CARTESIAN_POINT('Ctrl Pts',(-2.04965785769565,-1.05238869753535,
-22.0330650649484));
#56068=CARTESIAN_POINT('Ctrl Pts',(-2.04981577269251,-1.05242323368449,
-21.9438016099532));
#56069=CARTESIAN_POINT('Ctrl Pts',(-2.0352872104395,-1.05117583667188,-21.7138001471288));
#56070=CARTESIAN_POINT('Ctrl Pts',(-1.91580205826814,-1.04028492443336,
-21.212120769873));
#56071=CARTESIAN_POINT('Ctrl Pts',(-1.54497027776593,-1.00976017368561,
-20.5983257098217));
#56072=CARTESIAN_POINT('Ctrl Pts',(-0.607145822015571,-0.940669573101927,
-19.9292256569487));
#56073=CARTESIAN_POINT('Ctrl Pts',(0.606887110287569,-0.939423264837247,
-19.9262432814847));
#56074=CARTESIAN_POINT('Ctrl Pts',(1.54458406111778,-1.00903316772747,-20.5984241362299));
#56075=CARTESIAN_POINT('Ctrl Pts',(2.14134596539594,-1.05914052353263,-21.578464777093));
#56076=CARTESIAN_POINT('Ctrl Pts',(2.07601143327058,-1.05435985255611,-22.4957984055296));
#56077=CARTESIAN_POINT('Ctrl Pts',(1.69261614119323,-1.02145958385162,-23.2155194332715));
#56078=CARTESIAN_POINT('Ctrl Pts',(1.53141254982529,-1.00807953562059,-23.4179907851037));
#56079=CARTESIAN_POINT('Ctrl Pts',(1.34046462259684,-0.994431239233105,
-23.5830172776492));
#56080=CARTESIAN_POINT('Origin',(0.,-32.64,-22.032));
#56081=CARTESIAN_POINT('',(-2.04798719608651,1.031471238741,-22.0314998033837));
#56082=CARTESIAN_POINT('',(-2.05,-32.64,-22.032));
#56083=CARTESIAN_POINT('',(1.06033811196866,1.10557153022754,-23.7864751603562));
#56084=CARTESIAN_POINT('Ctrl Pts',(1.06033811196866,1.10557153022754,-23.7864751603562));
#56085=CARTESIAN_POINT('Ctrl Pts',(1.3741706509286,1.08763482658183,-23.5968067003208));
#56086=CARTESIAN_POINT('Ctrl Pts',(1.6389112117965,1.06602766214671,-23.3172136393184));
#56087=CARTESIAN_POINT('Ctrl Pts',(2.07504458979883,1.02978963073027,-22.4955454402302));
#56088=CARTESIAN_POINT('Ctrl Pts',(2.16671526713221,1.02015496747681,-21.2738800000443));
#56089=CARTESIAN_POINT('Ctrl Pts',(1.12497802521023,1.11222339267956,-20.1511354024741));
#56090=CARTESIAN_POINT('Ctrl Pts',(-2.22411254650599E-5,1.14324344009484,
-19.9249469059644));
#56091=CARTESIAN_POINT('Ctrl Pts',(-1.12483654553001,1.11241940027572,-20.1519785870164));
#56092=CARTESIAN_POINT('Ctrl Pts',(-1.92005960293299,1.04196266266284,-21.0068804220012));
#56093=CARTESIAN_POINT('Ctrl Pts',(-2.04846270330842,1.03133303488674,-21.8009775414312));
#56094=CARTESIAN_POINT('Ctrl Pts',(-2.04798719608651,1.031471238741,-22.0314998033837));
#56095=CARTESIAN_POINT('Ctrl Pts',(-2.04798719608651,1.031471238741,-22.0314998033837));
#56096=CARTESIAN_POINT('Ctrl Pts',(-2.0472990346369,1.0316712495091,-22.3651152074008));
#56097=CARTESIAN_POINT('Ctrl Pts',(-1.96760078125492,1.03861898694433,-22.6990725582984));
#56098=CARTESIAN_POINT('Ctrl Pts',(-1.65476826134601,1.06448801082077,-23.2866051421743));
#56099=CARTESIAN_POINT('Ctrl Pts',(-1.19459273103418,1.10242309331756,-23.7986869773671));
#56100=CARTESIAN_POINT('Ctrl Pts',(-0.11883654419667,1.1509767800617,-24.1919960917867));
#56101=CARTESIAN_POINT('Ctrl Pts',(0.681458753251526,1.12722590296183,-24.0154554462922));
#56102=CARTESIAN_POINT('Ctrl Pts',(1.06033811196866,1.10557153022754,-23.7864751603562));
#56103=CARTESIAN_POINT('Ctrl Pts',(1.06033811196866,1.10557153022754,-23.7864751603562));
#56104=CARTESIAN_POINT('Ctrl Pts',(1.3741706509286,1.08763482658183,-23.5968067003208));
#56105=CARTESIAN_POINT('Ctrl Pts',(1.6389112117965,1.06602766214671,-23.3172136393184));
#56106=CARTESIAN_POINT('Ctrl Pts',(2.07504458979883,1.02978963073027,-22.4955454402302));
#56107=CARTESIAN_POINT('Ctrl Pts',(2.16671526713221,1.02015496747681,-21.2738800000443));
#56108=CARTESIAN_POINT('Ctrl Pts',(1.12497802521023,1.11222339267956,-20.1511354024741));
#56109=CARTESIAN_POINT('Ctrl Pts',(-2.22411254650599E-5,1.14324344009484,
-19.9249469059644));
#56110=CARTESIAN_POINT('Ctrl Pts',(-1.12483654553001,1.11241940027572,-20.1519785870164));
#56111=CARTESIAN_POINT('Ctrl Pts',(-2.16645281839403,1.02013223160363,-21.2717646077205));
#56112=CARTESIAN_POINT('Ctrl Pts',(-2.07546536871258,1.02969935292042,-22.4964914462192));
#56113=CARTESIAN_POINT('Ctrl Pts',(-1.65476826134601,1.06448801082077,-23.2866051421743));
#56114=CARTESIAN_POINT('Ctrl Pts',(-1.19459273103418,1.10242309331756,-23.7986869773671));
#56115=CARTESIAN_POINT('Ctrl Pts',(-0.11883654419667,1.1509767800617,-24.1919960917867));
#56116=CARTESIAN_POINT('Ctrl Pts',(0.681458753251526,1.12722590296183,-24.0154554462922));
#56117=CARTESIAN_POINT('Ctrl Pts',(1.06033811196866,1.10557153022754,-23.7864751603562));
#56118=CARTESIAN_POINT('Ctrl Pts',(1.06885567305814,1.40828367652872,-23.7813274701248));
#56119=CARTESIAN_POINT('Ctrl Pts',(1.38248586686808,1.39243884639632,-23.5895875529348));
#56120=CARTESIAN_POINT('Ctrl Pts',(1.64436283152676,1.3732095635864,-23.3087243380774));
#56121=CARTESIAN_POINT('Ctrl Pts',(2.07314889996122,1.34044977214445,-22.4906135360011));
#56122=CARTESIAN_POINT('Ctrl Pts',(2.16411028206747,1.33196913158902,-21.2847252513266));
#56123=CARTESIAN_POINT('Ctrl Pts',(1.13744447201766,1.4143568387895,-20.1592143027524));
#56124=CARTESIAN_POINT('Ctrl Pts',(-0.000256227932920122,1.44137426575786,
-19.92387643395));
#56125=CARTESIAN_POINT('Ctrl Pts',(-1.13694778952218,1.41450806520655,-20.1595508202468));
#56126=CARTESIAN_POINT('Ctrl Pts',(-2.16383403896832,1.33195045856082,-21.2825688856218));
#56127=CARTESIAN_POINT('Ctrl Pts',(-2.07325337832862,1.34033815950352,-22.4907608848192));
#56128=CARTESIAN_POINT('Ctrl Pts',(-1.6592835139715,1.37180588493616,-23.2775613318082));
#56129=CARTESIAN_POINT('Ctrl Pts',(-1.20487142745969,1.40556608560269,-23.7910434905851));
#56130=CARTESIAN_POINT('Ctrl Pts',(-0.122112202043455,1.4482379067298,-24.1940212246999));
#56131=CARTESIAN_POINT('Ctrl Pts',(0.690220598763919,1.42741260146251,-24.0128085558852));
#56132=CARTESIAN_POINT('Ctrl Pts',(1.06885567305814,1.40828367652872,-23.7813274701248));
#56133=CARTESIAN_POINT('Ctrl Pts',(1.21687788573647,1.93213443184209,-23.992953261104));
#56134=CARTESIAN_POINT('Ctrl Pts',(1.57324186146248,1.91959724479566,-23.7763501693715));
#56135=CARTESIAN_POINT('Ctrl Pts',(1.8683540783032,1.9042141351763,-23.4608590636703));
#56136=CARTESIAN_POINT('Ctrl Pts',(2.34973256394823,1.87701976965164,-22.5436171337775));
#56137=CARTESIAN_POINT('Ctrl Pts',(2.45226711834097,1.87047554852946,-21.1978834357668));
#56138=CARTESIAN_POINT('Ctrl Pts',(1.29873523523315,1.93739606097254,-19.9306130867953));
#56139=CARTESIAN_POINT('Ctrl Pts',(-2.48986141743091E-5,1.95795842159875,
-19.6634199435529));
#56140=CARTESIAN_POINT('Ctrl Pts',(-1.29846053070403,1.93745323324118,-19.9312506887653));
#56141=CARTESIAN_POINT('Ctrl Pts',(-2.45198106316624,1.87046011766442,-21.1955379468141));
#56142=CARTESIAN_POINT('Ctrl Pts',(-2.35021929528818,1.87691821348825,-22.5445287638371));
#56143=CARTESIAN_POINT('Ctrl Pts',(-1.88580976045264,1.90305993699306,-23.4266020673305));
#56144=CARTESIAN_POINT('Ctrl Pts',(-1.37432153671418,1.93016224431321,-24.003984576668));
#56145=CARTESIAN_POINT('Ctrl Pts',(-0.13951160354739,1.96345677777968,-24.4611199386481));
#56146=CARTESIAN_POINT('Ctrl Pts',(0.786651768838543,1.94727015168814,-24.2544508125171));
#56147=CARTESIAN_POINT('Ctrl Pts',(1.21687788573647,1.93213443184209,-23.992953261104));
#56148=CARTESIAN_POINT('Ctrl Pts',(1.49832696166209,2.10922709805227,-24.4473929779526));
#56149=CARTESIAN_POINT('Ctrl Pts',(1.93946239340197,2.09347121942612,-24.184968765879));
#56150=CARTESIAN_POINT('Ctrl Pts',(2.30810979033992,2.07439966898151,-23.79924586829));
#56151=CARTESIAN_POINT('Ctrl Pts',(2.91131182915358,2.04195622182916,-22.6683467986794));
#56152=CARTESIAN_POINT('Ctrl Pts',(3.03948394883541,2.03353491233303,-20.9920377381179));
#56153=CARTESIAN_POINT('Ctrl Pts',(1.59432559617741,2.11523562113408,-19.4424175335459));
#56154=CARTESIAN_POINT('Ctrl Pts',(-3.29269739570931E-5,2.14220011170132,
-19.126726079993));
#56155=CARTESIAN_POINT('Ctrl Pts',(-1.59401433946836,2.11538707819239,-19.4435006465808));
#56156=CARTESIAN_POINT('Ctrl Pts',(-3.03913212305212,2.03351582365801,-20.989134884764));
#56157=CARTESIAN_POINT('Ctrl Pts',(-2.91185846141516,2.04185422508344,-22.6696329552038));
#56158=CARTESIAN_POINT('Ctrl Pts',(-2.32998889963734,2.07301540754862,-23.757123907291));
#56159=CARTESIAN_POINT('Ctrl Pts',(-1.69011408984992,2.10650576808936,-24.4634914741773));
#56160=CARTESIAN_POINT('Ctrl Pts',(-0.169731804772517,2.14900999872136,
-25.0099387468857));
#56161=CARTESIAN_POINT('Ctrl Pts',(0.965759146868535,2.12824863485557,-24.764208810727));
#56162=CARTESIAN_POINT('Ctrl Pts',(1.49832696166209,2.10922709805227,-24.4473929779526));
#56163=CARTESIAN_POINT('Ctrl Pts',(1.61567592638144,2.10484535966067,-24.6418414854819));
#56164=CARTESIAN_POINT('Ctrl Pts',(2.09220096563961,2.08654257832164,-24.3598140131154));
#56165=CARTESIAN_POINT('Ctrl Pts',(2.4917371536323,2.06460141183357,-23.9440137803207));
#56166=CARTESIAN_POINT('Ctrl Pts',(3.14638574337583,2.02805778890562,-22.7217241578602));
#56167=CARTESIAN_POINT('Ctrl Pts',(3.28527751630146,2.01819894837187,-20.9040192764535));
#56168=CARTESIAN_POINT('Ctrl Pts',(1.71728341750388,2.11146607039885,-19.2336854760647));
#56169=CARTESIAN_POINT('Ctrl Pts',(-5.68372511193975E-5,2.14348108036939,
-18.8971771498333));
#56170=CARTESIAN_POINT('Ctrl Pts',(-1.71693918475569,2.11168339882122,-19.2349389943924));
#56171=CARTESIAN_POINT('Ctrl Pts',(-3.2848943379376,2.01817562027762,-20.9008741138759));
#56172=CARTESIAN_POINT('Ctrl Pts',(-3.14693139817671,2.02797312390453,-22.7231264087792));
#56173=CARTESIAN_POINT('Ctrl Pts',(-2.51542689144179,2.06305029395261,-23.8984874041331));
#56174=CARTESIAN_POINT('Ctrl Pts',(-1.8215791399191,2.10154489826223,-24.6600514792354));
#56175=CARTESIAN_POINT('Ctrl Pts',(-0.182315527702726,2.1513398143738,-25.2447478054221));
#56176=CARTESIAN_POINT('Ctrl Pts',(1.04038344114352,2.12694168555298,-24.9823236681931));
#56177=CARTESIAN_POINT('Ctrl Pts',(1.61567592638144,2.10484535966067,-24.6418414854819));
#56178=CARTESIAN_POINT('Ctrl Pts',(1.61567592638144,2.10484535966067,-24.6418414854819));
#56179=CARTESIAN_POINT('Ctrl Pts',(1.49832696166209,2.10922709805227,-24.4473929779526));
#56180=CARTESIAN_POINT('Ctrl Pts',(1.21687788573647,1.93213443184209,-23.992953261104));
#56181=CARTESIAN_POINT('Ctrl Pts',(1.06885567305814,1.40828367652872,-23.7813274701248));
#56182=CARTESIAN_POINT('Ctrl Pts',(1.06033811196866,1.10557153022754,-23.7864751603562));
#56183=CARTESIAN_POINT('Ctrl Pts',(1.32735269144094,-1.10555525796307,-31.754253126905));
#56184=CARTESIAN_POINT('Ctrl Pts',(1.06710073148761,-1.09683487190185,-31.975373592947));
#56185=CARTESIAN_POINT('Ctrl Pts',(0.428155187551756,-1.06165436373511,
-32.2864496159946));
#56186=CARTESIAN_POINT('Ctrl Pts',(-0.630282194184733,-1.0692102615866,
-32.2353219180946));
#56187=CARTESIAN_POINT('Ctrl Pts',(-1.53618081272622,-1.12324621261658,
-31.6799876467057));
#56188=CARTESIAN_POINT('Ctrl Pts',(-2.06354935994887,-1.09811456220838,
-30.7530725805608));
#56189=CARTESIAN_POINT('Ctrl Pts',(-2.07369689301627,-1.05472770793943,
-30.0461163773485));
#56190=CARTESIAN_POINT('Ctrl Pts',(-1.95022898432517,-1.04370742396877,
-29.5338952679768));
#56191=CARTESIAN_POINT('Ctrl Pts',(-1.81664117243763,-1.0312338635184,-29.1901382103174));
#56192=CARTESIAN_POINT('Ctrl Pts',(-1.37870319165073,-0.994208730015135,
-28.5976563596733));
#56193=CARTESIAN_POINT('Ctrl Pts',(-0.565632139754401,-0.938431810497882,
-28.1175164175936));
#56194=CARTESIAN_POINT('Ctrl Pts',(0.566051291595285,-0.938787274998903,
-28.1186849695365));
#56195=CARTESIAN_POINT('Ctrl Pts',(1.29716483238625,-0.988597635068523,
-28.5489950966502));
#56196=CARTESIAN_POINT('Ctrl Pts',(1.65332946690085,-1.01745671260863,-28.9696512040306));
#56197=CARTESIAN_POINT('Ctrl Pts',(1.80035161541673,-1.0302070446804,-29.1988189274931));
#56198=CARTESIAN_POINT('Ctrl Pts',(1.89755296929512,-1.0389008897144,-29.406736531242));
#56199=CARTESIAN_POINT('Ctrl Pts',(1.95792514729417,-1.04441107544017,-29.5794738833423));
#56200=CARTESIAN_POINT('Ctrl Pts',(1.98223924757779,-1.04664413680767,-29.6674728551243));
#56201=CARTESIAN_POINT('Ctrl Pts',(2.02810945191073,-1.0508832347292,-29.8577107402739));
#56202=CARTESIAN_POINT('Ctrl Pts',(2.06564184504211,-1.0616449129841,-30.159982754614));
#56203=CARTESIAN_POINT('Ctrl Pts',(1.99588940266396,-1.10355864373223,-30.9150513968238));
#56204=CARTESIAN_POINT('Ctrl Pts',(1.67008090765068,-1.11703921512503,-31.4630575374169));
#56205=CARTESIAN_POINT('Ctrl Pts',(1.32735269144094,-1.10555525796307,-31.754253126905));
#56206=CARTESIAN_POINT('Ctrl Pts',(1.32359268837332,-1.3930284764443,-31.7574477757783));
#56207=CARTESIAN_POINT('Ctrl Pts',(1.06075990223367,-1.38701669149454,-31.9795472988009));
#56208=CARTESIAN_POINT('Ctrl Pts',(0.419725709553912,-1.3602190366849,-32.2844089798952));
#56209=CARTESIAN_POINT('Ctrl Pts',(-0.618485714611421,-1.36594619964849,
-32.2352048569959));
#56210=CARTESIAN_POINT('Ctrl Pts',(-1.53434167017165,-1.40706476564176,
-31.6853452283511));
#56211=CARTESIAN_POINT('Ctrl Pts',(-2.06756518656419,-1.38208136621911,
-30.7392367955497));
#56212=CARTESIAN_POINT('Ctrl Pts',(-2.07107027760732,-1.34300067689607,
-30.0368863357017));
#56213=CARTESIAN_POINT('Ctrl Pts',(-1.94807632133963,-1.33142265611008,
-29.5305662158123));
#56214=CARTESIAN_POINT('Ctrl Pts',(-1.81175633221395,-1.32042474667762,
-29.1822460250395));
#56215=CARTESIAN_POINT('Ctrl Pts',(-1.3687168401187,-1.28652020920908,-28.5906178404563));
#56216=CARTESIAN_POINT('Ctrl Pts',(-0.555659683581034,-1.23798415259695,
-28.1189521130734));
#56217=CARTESIAN_POINT('Ctrl Pts',(0.556795084374633,-1.23819678242899,
-28.1201472467162));
#56218=CARTESIAN_POINT('Ctrl Pts',(1.28744457447514,-1.28184563228667,-28.5417785542487));
#56219=CARTESIAN_POINT('Ctrl Pts',(1.64696260849818,-1.30788994439935,-28.9617938965102));
#56220=CARTESIAN_POINT('Ctrl Pts',(1.79566840873594,-1.31945564515493,-29.1912135128309));
#56221=CARTESIAN_POINT('Ctrl Pts',(1.89426584711195,-1.32742070284596,-29.400029974807));
#56222=CARTESIAN_POINT('Ctrl Pts',(1.95553864001657,-1.33248283811966,-29.5737054711291));
#56223=CARTESIAN_POINT('Ctrl Pts',(1.98023234041262,-1.33453601106632,-29.6622637213054));
#56224=CARTESIAN_POINT('Ctrl Pts',(2.02679416400233,-1.33848243383651,-29.8536245299278));
#56225=CARTESIAN_POINT('Ctrl Pts',(2.06442657207142,-1.34907719838766,-30.1508642304607));
#56226=CARTESIAN_POINT('Ctrl Pts',(2.00034510775818,-1.38695750726818,-30.9054053055921));
#56227=CARTESIAN_POINT('Ctrl Pts',(1.6697196184884,-1.40094545171871,-31.4649628570855));
#56228=CARTESIAN_POINT('Ctrl Pts',(1.32359268837332,-1.3930284764443,-31.7574477757783));
#56229=CARTESIAN_POINT('Ctrl Pts',(1.46653971754463,-1.8915537217059,-31.9389064298716));
#56230=CARTESIAN_POINT('Ctrl Pts',(1.17208250986832,-1.88990990750113,-32.1922127295594));
#56231=CARTESIAN_POINT('Ctrl Pts',(0.460648793220428,-1.87680187973207,
-32.5388567043923));
#56232=CARTESIAN_POINT('Ctrl Pts',(-0.679806548016544,-1.87951434725149,
-32.4836938552306));
#56233=CARTESIAN_POINT('Ctrl Pts',(-1.70258640950013,-1.89979282381933,
-31.8577659411165));
#56234=CARTESIAN_POINT('Ctrl Pts',(-2.30312627589108,-1.87494954073869,
-30.7804042928418));
#56235=CARTESIAN_POINT('Ctrl Pts',(-2.3047574810545,-1.84291420533356,-30.0049321102413));
#56236=CARTESIAN_POINT('Ctrl Pts',(-2.16713537988374,-1.83047398511645,
-29.450084851244));
#56237=CARTESIAN_POINT('Ctrl Pts',(-2.01322265024838,-1.82185288488754,
-29.0528943526148));
#56238=CARTESIAN_POINT('Ctrl Pts',(-1.51600088272362,-1.79307985743714,
-28.3908970609083));
#56239=CARTESIAN_POINT('Ctrl Pts',(-0.612040482336112,-1.75621723925646,
-27.8627033356224));
#56240=CARTESIAN_POINT('Ctrl Pts',(0.612324780435475,-1.75625510817756,
-27.8650485172928));
#56241=CARTESIAN_POINT('Ctrl Pts',(1.42455024203057,-1.78983816998982,-28.3335961136323));
#56242=CARTESIAN_POINT('Ctrl Pts',(1.82755327624387,-1.81131968108437,-28.8054906524833));
#56243=CARTESIAN_POINT('Ctrl Pts',(1.99464262300472,-1.82096843430477,-29.0635047207685));
#56244=CARTESIAN_POINT('Ctrl Pts',(2.10562099039111,-1.82774616567129,-29.2985549129538));
#56245=CARTESIAN_POINT('Ctrl Pts',(2.1746649507395,-1.83208104982681,-29.4941944943251));
#56246=CARTESIAN_POINT('Ctrl Pts',(2.2025166171187,-1.83384404888901,-29.594055594785));
#56247=CARTESIAN_POINT('Ctrl Pts',(2.25497054882611,-1.83730258309225,-29.8091760872681));
#56248=CARTESIAN_POINT('Ctrl Pts',(2.29712794695441,-1.84758569353084,-30.1318884172415));
#56249=CARTESIAN_POINT('Ctrl Pts',(2.22692569402416,-1.87892699693054,-30.9729351466869));
#56250=CARTESIAN_POINT('Ctrl Pts',(1.85431314124951,-1.89371847585523,-31.6053250179881));
#56251=CARTESIAN_POINT('Ctrl Pts',(1.46653971754463,-1.8915537217059,-31.9389064298717));
#56252=CARTESIAN_POINT('Ctrl Pts',(1.78295981235903,-2.09034202746774,-32.3165923940998));
#56253=CARTESIAN_POINT('Ctrl Pts',(1.42887704568795,-2.08528185371715,-32.6294992152107));
#56254=CARTESIAN_POINT('Ctrl Pts',(0.5682747633569,-2.06094872479154,-33.0717163335162));
#56255=CARTESIAN_POINT('Ctrl Pts',(-0.837377841698829,-2.06620701234019,
-32.9989619534493));
#56256=CARTESIAN_POINT('Ctrl Pts',(-2.0651652506236,-2.10333070270456,-32.2093337878777));
#56257=CARTESIAN_POINT('Ctrl Pts',(-2.79217267385067,-2.07752992562671,
-30.9061146080709));
#56258=CARTESIAN_POINT('Ctrl Pts',(-2.80438461577025,-2.04051125226246,
-29.9635496597121));
#56259=CARTESIAN_POINT('Ctrl Pts',(-2.63548264699564,-2.02890333097792,
-29.2894223532697));
#56260=CARTESIAN_POINT('Ctrl Pts',(-2.45137426614447,-2.01824716085344,
-28.8045713252895));
#56261=CARTESIAN_POINT('Ctrl Pts',(-1.85198515728335,-1.98522456653967,
-27.9937075036918));
#56262=CARTESIAN_POINT('Ctrl Pts',(-0.753821627316684,-1.93883646088754,
-27.3319251834597));
#56263=CARTESIAN_POINT('Ctrl Pts',(0.754378094218889,-1.93902779172867,
-27.3349745231335));
#56264=CARTESIAN_POINT('Ctrl Pts',(1.74159121964216,-1.98078805737154,-27.921968319788));
#56265=CARTESIAN_POINT('Ctrl Pts',(2.22779548254146,-2.00605371647797,-28.5013840066074));
#56266=CARTESIAN_POINT('Ctrl Pts',(2.42910284089573,-2.01729978469252,-28.8172792473517));
#56267=CARTESIAN_POINT('Ctrl Pts',(2.56263060668496,-2.02507503169194,-29.1041603431301));
#56268=CARTESIAN_POINT('Ctrl Pts',(2.64567276448555,-2.03002288631674,-29.3426222472456));
#56269=CARTESIAN_POINT('Ctrl Pts',(2.67915108961055,-2.03203164657226,-29.4642451627364));
#56270=CARTESIAN_POINT('Ctrl Pts',(2.74228969748,-2.03589942781969,-29.7261453244971));
#56271=CARTESIAN_POINT('Ctrl Pts',(2.79358493531193,-2.0461853708987,-30.118560451381));
#56272=CARTESIAN_POINT('Ctrl Pts',(2.69905012072682,-2.08239625976544,-31.139014614668));
#56273=CARTESIAN_POINT('Ctrl Pts',(2.24925468688582,-2.09700581714128,-31.9045225036042));
#56274=CARTESIAN_POINT('Ctrl Pts',(1.78295981235902,-2.09034202746774,-32.3165923940998));
#56275=CARTESIAN_POINT('Ctrl Pts',(1.92217361622795,-2.10353486590704,-32.4807924448345));
#56276=CARTESIAN_POINT('Ctrl Pts',(1.54214210494487,-2.09550639469273,-32.8185779932545));
#56277=CARTESIAN_POINT('Ctrl Pts',(0.61600518091511,-2.06181102885638,-33.3002465007061));
#56278=CARTESIAN_POINT('Ctrl Pts',(-0.907207782595835,-2.0691118392714,
-33.2202856317455));
#56279=CARTESIAN_POINT('Ctrl Pts',(-2.22461176780362,-2.1206214736028,-32.3628055449923));
#56280=CARTESIAN_POINT('Ctrl Pts',(-3.00594215374136,-2.09423195572766,
-30.9643085677682));
#56281=CARTESIAN_POINT('Ctrl Pts',(-3.02268599780788,-2.05274388500329,
-29.9478114914885));
#56282=CARTESIAN_POINT('Ctrl Pts',(-2.84029263744146,-2.04183273360025,
-29.22012928383));
#56283=CARTESIAN_POINT('Ctrl Pts',(-2.64319201568411,-2.02946358499133,
-28.6985450532409));
#56284=CARTESIAN_POINT('Ctrl Pts',(-1.99960374430712,-1.99287484878532,
-27.8235216602912));
#56285=CARTESIAN_POINT('Ctrl Pts',(-0.816457589247531,-1.93849257916689,
-27.1049559716654));
#56286=CARTESIAN_POINT('Ctrl Pts',(0.817160570345912,-1.93883495609753,
-27.1081768085736));
#56287=CARTESIAN_POINT('Ctrl Pts',(1.88095619521476,-1.98740065419004,-27.7460109726621));
#56288=CARTESIAN_POINT('Ctrl Pts',(2.40323538999901,-2.01585893888295,-28.3714302885281));
#56289=CARTESIAN_POINT('Ctrl Pts',(2.61933802028281,-2.02845220565332,-28.7120950601187));
#56290=CARTESIAN_POINT('Ctrl Pts',(2.76258855495401,-2.0370663728381,-29.0211619117701));
#56291=CARTESIAN_POINT('Ctrl Pts',(2.85165863890266,-2.04253049221437,-29.2779504603529));
#56292=CARTESIAN_POINT('Ctrl Pts',(2.88755751178509,-2.04474699586185,-29.4088777844149));
#56293=CARTESIAN_POINT('Ctrl Pts',(2.95529437562388,-2.04895478990619,-29.690865199318));
#56294=CARTESIAN_POINT('Ctrl Pts',(3.01054093596492,-2.05929030439916,-30.1150007456908));
#56295=CARTESIAN_POINT('Ctrl Pts',(2.90557514872957,-2.09980733494611,-31.2138156516044));
#56296=CARTESIAN_POINT('Ctrl Pts',(2.42264063284103,-2.11410763399941,-32.0359595279482));
#56297=CARTESIAN_POINT('Ctrl Pts',(1.92217361622794,-2.10353486590704,-32.4807924448345));
#56298=CARTESIAN_POINT('',(1.32735269144094,-1.10555525796307,-31.754253126905));
#56299=CARTESIAN_POINT('Ctrl Pts',(1.92209690203547,-2.10352758862968,-32.4807019617002));
#56300=CARTESIAN_POINT('Ctrl Pts',(1.78290998961342,-2.09031072420672,-32.3165329245109));
#56301=CARTESIAN_POINT('Ctrl Pts',(1.46652846325438,-1.89151447256697,-31.9388921435421));
#56302=CARTESIAN_POINT('Ctrl Pts',(1.32359268837332,-1.3930284764443,-31.7574477757783));
#56303=CARTESIAN_POINT('Ctrl Pts',(1.32735269144094,-1.10555525796307,-31.754253126905));
#56304=CARTESIAN_POINT('',(-2.04999522160878,-1.06512573620563,-30.1923376809671));
#56305=CARTESIAN_POINT('Ctrl Pts',(1.32735269144094,-1.10555525796307,-31.754253126905));
#56306=CARTESIAN_POINT('Ctrl Pts',(1.06710073148761,-1.09683487190185,-31.975373592947));
#56307=CARTESIAN_POINT('Ctrl Pts',(0.428155187551756,-1.06165436373511,
-32.2864496159946));
#56308=CARTESIAN_POINT('Ctrl Pts',(-0.630282194184733,-1.0692102615866,
-32.2353219180946));
#56309=CARTESIAN_POINT('Ctrl Pts',(-1.53618081272622,-1.12324621261658,
-31.6799876467057));
#56310=CARTESIAN_POINT('Ctrl Pts',(-1.98079487593783,-1.10205821181136,
-30.8985237615705));
#56311=CARTESIAN_POINT('Ctrl Pts',(-2.05000335389775,-1.07367692784301,
-30.3739907004343));
#56312=CARTESIAN_POINT('Ctrl Pts',(-2.04999522160878,-1.06512573620563,
-30.1923376809671));
#56313=CARTESIAN_POINT('Ctrl Pts',(-2.04999522160878,-1.06512573620563,
-30.1923376809671));
#56314=CARTESIAN_POINT('Ctrl Pts',(-2.04998798795319,-1.05751946748649,
-30.0307576651865));
#56315=CARTESIAN_POINT('Ctrl Pts',(-2.03102354673217,-1.05091884457554,
-29.8690809921543));
#56316=CARTESIAN_POINT('Ctrl Pts',(-1.95022898432517,-1.04370742396877,
-29.5338952679768));
#56317=CARTESIAN_POINT('Ctrl Pts',(-1.81664117243763,-1.0312338635184,-29.1901382103174));
#56318=CARTESIAN_POINT('Ctrl Pts',(-1.37870319165073,-0.994208730015135,
-28.5976563596733));
#56319=CARTESIAN_POINT('Ctrl Pts',(-0.565632139754401,-0.938431810497882,
-28.1175164175936));
#56320=CARTESIAN_POINT('Ctrl Pts',(0.566051291595285,-0.938787274998903,
-28.1186849695365));
#56321=CARTESIAN_POINT('Ctrl Pts',(1.29716483238625,-0.988597635068523,
-28.5489950966502));
#56322=CARTESIAN_POINT('Ctrl Pts',(1.65332946690085,-1.01745671260863,-28.9696512040306));
#56323=CARTESIAN_POINT('Ctrl Pts',(1.80035161541673,-1.0302070446804,-29.1988189274931));
#56324=CARTESIAN_POINT('Ctrl Pts',(1.89755296929512,-1.0389008897144,-29.406736531242));
#56325=CARTESIAN_POINT('Ctrl Pts',(1.95792514729417,-1.04441107544017,-29.5794738833423));
#56326=CARTESIAN_POINT('Ctrl Pts',(1.98223924757779,-1.04664413680767,-29.6674728551243));
#56327=CARTESIAN_POINT('Ctrl Pts',(2.02810945191073,-1.0508832347292,-29.8577107402739));
#56328=CARTESIAN_POINT('Ctrl Pts',(2.06564184504211,-1.0616449129841,-30.159982754614));
#56329=CARTESIAN_POINT('Ctrl Pts',(1.99588940266396,-1.10355864373223,-30.9150513968238));
#56330=CARTESIAN_POINT('Ctrl Pts',(1.67008090765068,-1.11703921512503,-31.4630575374169));
#56331=CARTESIAN_POINT('Ctrl Pts',(1.32735269144094,-1.10555525796307,-31.754253126905));
#56332=CARTESIAN_POINT('Origin',(0.,-32.64,-30.192));
#56333=CARTESIAN_POINT('',(-2.04996075587217,1.01995056002153,-30.1919211569379));
#56334=CARTESIAN_POINT('',(-2.05,-32.64,-30.192));
#56335=CARTESIAN_POINT('',(1.11427248149542,0.985616400927087,-31.9127256716229));
#56336=CARTESIAN_POINT('Ctrl Pts',(1.11427248149542,0.985616400927087,-31.9127256716229));
#56337=CARTESIAN_POINT('Ctrl Pts',(1.39531085079306,0.975440411623561,-31.7307365688176));
#56338=CARTESIAN_POINT('Ctrl Pts',(1.99044683757195,0.965060884489212,-31.0938116474192));
#56339=CARTESIAN_POINT('Ctrl Pts',(2.11292571169222,1.02591892089202,-30.2033470929722));
#56340=CARTESIAN_POINT('Ctrl Pts',(1.94993402071046,1.04016458736943,-29.5342274298653));
#56341=CARTESIAN_POINT('Ctrl Pts',(1.81641479649524,1.0523146735164,-29.1904822889767));
#56342=CARTESIAN_POINT('Ctrl Pts',(1.37906269670218,1.08848337424274,-28.5984740900847));
#56343=CARTESIAN_POINT('Ctrl Pts',(0.564594594180929,1.14119196261678,-28.1173646277202));
#56344=CARTESIAN_POINT('Ctrl Pts',(-0.565690606478501,1.14128987332371,
-28.118282602635));
#56345=CARTESIAN_POINT('Ctrl Pts',(-1.54155256487553,1.0776718216566,-28.6932848560635));
#56346=CARTESIAN_POINT('Ctrl Pts',(-1.90806784508456,1.04384068155644,-29.3576617301976));
#56347=CARTESIAN_POINT('Ctrl Pts',(-2.03072544333898,1.03276938773931,-29.8679570181404));
#56348=CARTESIAN_POINT('Ctrl Pts',(-2.04987917115497,1.02693726153892,-30.0302127515688));
#56349=CARTESIAN_POINT('Ctrl Pts',(-2.04996075587217,1.01995056002153,-30.1919211569379));
#56350=CARTESIAN_POINT('Ctrl Pts',(-2.04999999848379,1.019950560016,-30.1919211555564));
#56351=CARTESIAN_POINT('Ctrl Pts',(-2.05000005380476,1.01988841535769,-30.1933595318955));
#56352=CARTESIAN_POINT('Ctrl Pts',(-2.0499985952739,1.01982617935423,-30.1947978635202));
#56353=CARTESIAN_POINT('Ctrl Pts',(-2.04999562318249,1.0197638529079,-30.1962361459661));
#56354=CARTESIAN_POINT('Ctrl Pts',(-2.04975068589453,1.01462737874599,-30.3147685035087));
#56355=CARTESIAN_POINT('Ctrl Pts',(-2.03922196734261,1.00887663384279,-30.4329535298336));
#56356=CARTESIAN_POINT('Ctrl Pts',(-2.01860478544297,1.00335286719046,-30.5493999443016));
#56357=CARTESIAN_POINT('Ctrl Pts',(-2.01084599258605,1.0012741271641,-30.593221821277));
#56358=CARTESIAN_POINT('Ctrl Pts',(-2.00165893224459,0.999227532176541,
-30.6367977614767));
#56359=CARTESIAN_POINT('Ctrl Pts',(-1.99105581950972,0.997257917428783,
-30.6800540170888));
#56360=CARTESIAN_POINT('Ctrl Pts',(-1.97431541280555,0.994148250225161,
-30.748347859619));
#56361=CARTESIAN_POINT('Ctrl Pts',(-1.9540381171472,0.991230469561293,-30.8158565688041));
#56362=CARTESIAN_POINT('Ctrl Pts',(-1.93032221771434,0.988582488966841,
-30.8821855806943));
#56363=CARTESIAN_POINT('Ctrl Pts',(-1.90661593400946,0.985935582009134,
-30.9484876991607));
#56364=CARTESIAN_POINT('Ctrl Pts',(-1.87947397032055,0.983558256381658,
-31.0136105978385));
#56365=CARTESIAN_POINT('Ctrl Pts',(-1.84904444368859,0.981528330881211,
-31.0771749235402));
#56366=CARTESIAN_POINT('Ctrl Pts',(-1.81862281036336,0.979498931935937,
-31.1407227608908));
#56367=CARTESIAN_POINT('Ctrl Pts',(-1.78491552685566,0.977816752912453,
-31.20271238098));
#56368=CARTESIAN_POINT('Ctrl Pts',(-1.74811795368169,0.976559552065531,
-31.2627864493053));
#56369=CARTESIAN_POINT('Ctrl Pts',(-1.71130007460099,0.975301657460817,
-31.3228936681435));
#56370=CARTESIAN_POINT('Ctrl Pts',(-1.67138876382225,0.974469210191225,
-31.3810828009535));
#56371=CARTESIAN_POINT('Ctrl Pts',(-1.62862354828288,0.974140097309977,
-31.4370242318841));
#56372=CARTESIAN_POINT('Ctrl Pts',(-1.6015032683714,0.973931384847071,-31.4725004301529));
#56373=CARTESIAN_POINT('Ctrl Pts',(-1.57323611092066,0.973925097132324,
-31.5070732670964));
#56374=CARTESIAN_POINT('Ctrl Pts',(-1.54389146947895,0.974141098580752,
-31.5406656852127));
#56375=CARTESIAN_POINT('Ctrl Pts',(-1.49368685948395,0.974510647089232,
-31.5981376517272));
#56376=CARTESIAN_POINT('Ctrl Pts',(-1.44029009238857,0.975530846253287,
-31.6527802833411));
#56377=CARTESIAN_POINT('Ctrl Pts',(-1.38403878501658,0.977004899514149,
-31.7042620942052));
#56378=CARTESIAN_POINT('Ctrl Pts',(-1.32772589645034,0.978480566496798,
-31.7558002648508));
#56379=CARTESIAN_POINT('Ctrl Pts',(-1.26855250415855,0.980411081834956,
-31.8041704474619));
#56380=CARTESIAN_POINT('Ctrl Pts',(-1.20689100633097,0.982599001932101,
-31.8490799916834));
#56381=CARTESIAN_POINT('Ctrl Pts',(-1.14520292035325,0.984787865450183,
-31.8940089006908));
#56382=CARTESIAN_POINT('Ctrl Pts',(-1.08102489983426,0.987234355758579,
-31.9354739805255));
#56383=CARTESIAN_POINT('Ctrl Pts',(-1.01475894042778,0.98974077374038,-31.9732255030798));
#56384=CARTESIAN_POINT('Ctrl Pts',(-0.948445088105803,0.992249003205265,
-32.0110043100874));
#56385=CARTESIAN_POINT('Ctrl Pts',(-0.880040613676623,0.994817246998847,
-32.0450640170226));
#56386=CARTESIAN_POINT('Ctrl Pts',(-0.809972632927784,0.997247377040431,
-32.0752005559441));
#56387=CARTESIAN_POINT('Ctrl Pts',(-0.791398111670701,0.997891587157983,
-32.083189537171));
#56388=CARTESIAN_POINT('Ctrl Pts',(-0.772706805174443,0.998526091438893,
-32.0909030798375));
#56389=CARTESIAN_POINT('Ctrl Pts',(-0.753906908629067,0.999147198916575,
-32.0983379482981));
#56390=CARTESIAN_POINT('Ctrl Pts',(-0.67836183054658,1.00164304312433,-32.128214055171));
#56391=CARTESIAN_POINT('Ctrl Pts',(-0.601050728001295,1.00392256437619,
-32.1535899336801));
#56392=CARTESIAN_POINT('Ctrl Pts',(-0.522511154750602,1.00588453382231,
-32.1742921311354));
#56393=CARTESIAN_POINT('Ctrl Pts',(-0.447881594202448,1.0077488286168,-32.1939636907648));
#56394=CARTESIAN_POINT('Ctrl Pts',(-0.372143322601374,1.00932640255769,
-32.209415691935));
#56395=CARTESIAN_POINT('Ctrl Pts',(-0.295771013314592,1.01053040534075,
-32.2205510857957));
#56396=CARTESIAN_POINT('Ctrl Pts',(-0.219414607426094,1.01173415740812,
-32.2316841608761));
#56397=CARTESIAN_POINT('Ctrl Pts',(-0.142424777405172,1.01256449388275,
-32.2385023728595));
#56398=CARTESIAN_POINT('Ctrl Pts',(-0.0652837489749921,1.012934618705,-32.2409602319518));
#56399=CARTESIAN_POINT('Ctrl Pts',(0.0118274848913055,1.01330460057211,
-32.2434171417328));
#56400=CARTESIAN_POINT('Ctrl Pts',(0.0890894474301462,1.01321472621786,
-32.241517046982));
#56401=CARTESIAN_POINT('Ctrl Pts',(0.16601789719275,1.0125783001148,-32.2352665165885));
#56402=CARTESIAN_POINT('Ctrl Pts',(0.178178240097014,1.01247769806614,-32.2342784738923));
#56403=CARTESIAN_POINT('Ctrl Pts',(0.190330250549795,1.01236343921683,-32.2331818318135));
#56404=CARTESIAN_POINT('Ctrl Pts',(0.202472019062823,1.01223518113576,-32.2319767355283));
#56405=CARTESIAN_POINT('Ctrl Pts',(0.27220735997383,1.01149854042331,-32.2250553549908));
#56406=CARTESIAN_POINT('Ctrl Pts',(0.341638885368904,1.0103001079684,-32.2145487493329));
#56407=CARTESIAN_POINT('Ctrl Pts',(0.410365860739164,1.00877460508166,-32.2005068733614));
#56408=CARTESIAN_POINT('Ctrl Pts',(0.479101969682676,1.00724889946096,-32.1864631312739));
#56409=CARTESIAN_POINT('Ctrl Pts',(0.547132845704916,1.00539603646965,-32.1688832655349));
#56410=CARTESIAN_POINT('Ctrl Pts',(0.614066975647822,1.00335079113749,-32.1478685409349));
#56411=CARTESIAN_POINT('Ctrl Pts',(0.68100394653689,1.00130545899712,-32.1268529243878));
#56412=CARTESIAN_POINT('Ctrl Pts',(0.746843602335305,0.999067728184644,
-32.1024023210015));
#56413=CARTESIAN_POINT('Ctrl Pts',(0.811211060810975,0.996772390891678,
-32.0746674201297));
#56414=CARTESIAN_POINT('Ctrl Pts',(0.875645346513367,0.994474670546324,
-32.0469037244826));
#56415=CARTESIAN_POINT('Ctrl Pts',(0.938603927258259,0.992119224042631,
-32.0158491368998));
#56416=CARTESIAN_POINT('Ctrl Pts',(0.999734427064827,0.989841263837853,
-31.9817013927863));
#56417=CARTESIAN_POINT('Ctrl Pts',(1.0386837119197,0.98838986198142,-31.9599441649404));
#56418=CARTESIAN_POINT('Ctrl Pts',(1.07689136950961,0.986969916451226,-31.9369321707182));
#56419=CARTESIAN_POINT('Ctrl Pts',(1.11427248149541,0.985616400927093,-31.9127256716229));
#56420=CARTESIAN_POINT('Ctrl Pts',(1.11427248149542,0.985616400927087,-31.9127256716229));
#56421=CARTESIAN_POINT('Ctrl Pts',(1.39531085079306,0.975440411623561,-31.7307365688176));
#56422=CARTESIAN_POINT('Ctrl Pts',(1.99044683757195,0.965060884489212,-31.0938116474192));
#56423=CARTESIAN_POINT('Ctrl Pts',(2.11292571169222,1.02591892089202,-30.2033470929722));
#56424=CARTESIAN_POINT('Ctrl Pts',(1.94993402071046,1.04016458736943,-29.5342274298653));
#56425=CARTESIAN_POINT('Ctrl Pts',(1.81641479649524,1.0523146735164,-29.1904822889767));
#56426=CARTESIAN_POINT('Ctrl Pts',(1.37906269670218,1.08848337424274,-28.5984740900847));
#56427=CARTESIAN_POINT('Ctrl Pts',(0.564594594180929,1.14119196261678,-28.1173646277202));
#56428=CARTESIAN_POINT('Ctrl Pts',(-0.565690606478501,1.14128987332371,
-28.118282602635));
#56429=CARTESIAN_POINT('Ctrl Pts',(-1.54155256487553,1.0776718216566,-28.6932848560635));
#56430=CARTESIAN_POINT('Ctrl Pts',(-1.90806784508456,1.04384068155644,-29.3576617301976));
#56431=CARTESIAN_POINT('Ctrl Pts',(-2.03106003574106,1.0327391868317,-29.8693490307722));
#56432=CARTESIAN_POINT('Ctrl Pts',(-2.06937685224897,1.02092745047005,-30.1968502518399));
#56433=CARTESIAN_POINT('Ctrl Pts',(-1.99066291316253,0.987995197249567,
-30.8469392317313));
#56434=CARTESIAN_POINT('Ctrl Pts',(-1.60389855123596,0.962274733835357,
-31.594329399779));
#56435=CARTESIAN_POINT('Ctrl Pts',(-0.782446503162938,1.00260836621067,
-32.1715806038486));
#56436=CARTESIAN_POINT('Ctrl Pts',(0.209646108503345,1.02217499482138,-32.310885465022));
#56437=CARTESIAN_POINT('Ctrl Pts',(0.842409601437768,0.995460159152721,
-32.0887730979989));
#56438=CARTESIAN_POINT('Ctrl Pts',(1.11427248149542,0.985616400927087,-31.9127256716229));
#56439=CARTESIAN_POINT('Ctrl Pts',(1.11956381130215,1.29420809400475,-31.9092992200441));
#56440=CARTESIAN_POINT('Ctrl Pts',(1.39818435418416,1.28711878983686,-31.7274836751049));
#56441=CARTESIAN_POINT('Ctrl Pts',(1.98135604782,1.28207482701826,-31.1022476003622));
#56442=CARTESIAN_POINT('Ctrl Pts',(2.1128795676757,1.33532002180968,-30.2176795236496));
#56443=CARTESIAN_POINT('Ctrl Pts',(1.94985285160701,1.35063254955861,-29.5389616589331));
#56444=CARTESIAN_POINT('Ctrl Pts',(1.81913793522182,1.3612658092768,-29.1996370764735));
#56445=CARTESIAN_POINT('Ctrl Pts',(1.38765007217341,1.3937566224756,-28.6077703469072));
#56446=CARTESIAN_POINT('Ctrl Pts',(0.573031934016957,1.4401444299264,-28.1188124687556));
#56447=CARTESIAN_POINT('Ctrl Pts',(-0.57399177348583,1.44023865387881,-28.1195341194796));
#56448=CARTESIAN_POINT('Ctrl Pts',(-1.55039175852058,1.38391592875038,-28.7058296242747));
#56449=CARTESIAN_POINT('Ctrl Pts',(-1.9095164692758,1.35344936800592,-29.3666716185023));
#56450=CARTESIAN_POINT('Ctrl Pts',(-2.03050637137044,1.34331472964374,-29.8743021354302));
#56451=CARTESIAN_POINT('Ctrl Pts',(-2.06837339171471,1.3316298126124,-30.2064485213252));
#56452=CARTESIAN_POINT('Ctrl Pts',(-1.98506648137687,1.30187139856525,-30.8552545286718));
#56453=CARTESIAN_POINT('Ctrl Pts',(-1.60212643522416,1.27750805182646,-31.5889934734217));
#56454=CARTESIAN_POINT('Ctrl Pts',(-0.792039056601329,1.30634155677681,
-32.1675382972107));
#56455=CARTESIAN_POINT('Ctrl Pts',(0.213298425973278,1.32138237766697,-32.3124702863081));
#56456=CARTESIAN_POINT('Ctrl Pts',(0.850039819185237,1.3010659428227,-32.085178754963));
#56457=CARTESIAN_POINT('Ctrl Pts',(1.11956381130215,1.29420809400475,-31.9092992200441));
#56458=CARTESIAN_POINT('Ctrl Pts',(1.27454163485273,1.8276996776529,-32.1285752398414));
#56459=CARTESIAN_POINT('Ctrl Pts',(1.59048771051817,1.82546583320247,-31.9272465850611));
#56460=CARTESIAN_POINT('Ctrl Pts',(2.24506867253542,1.82887441364011,-31.2405221593139));
#56461=CARTESIAN_POINT('Ctrl Pts',(2.39580868742134,1.87009241788133,-30.2391853142947));
#56462=CARTESIAN_POINT('Ctrl Pts',(2.21207475359764,1.88703580700542,-29.456927089891));
#56463=CARTESIAN_POINT('Ctrl Pts',(2.06558631312181,1.89524681774927,-29.0798299199868));
#56464=CARTESIAN_POINT('Ctrl Pts',(1.57974170165877,1.92187683611202,-28.4135771845243));
#56465=CARTESIAN_POINT('Ctrl Pts',(0.655063819144604,1.95814863714053,-27.8622104435215));
#56466=CARTESIAN_POINT('Ctrl Pts',(-0.65717394110681,1.95823512688616,-27.8629454348409));
#56467=CARTESIAN_POINT('Ctrl Pts',(-1.76474453532705,1.91360863385461,-28.527769477946));
#56468=CARTESIAN_POINT('Ctrl Pts',(-2.16726287994011,1.88851922966795,-29.2691704704899));
#56469=CARTESIAN_POINT('Ctrl Pts',(-2.30281338888132,1.87995898954312,-29.8386330483677));
#56470=CARTESIAN_POINT('Ctrl Pts',(-2.34544045465379,1.86847127655649,-30.2231880710558));
#56471=CARTESIAN_POINT('Ctrl Pts',(-2.25007163104386,1.84369961096044,-30.9597522307304));
#56472=CARTESIAN_POINT('Ctrl Pts',(-1.82100012358539,1.82146628356056,-31.7765943544781));
#56473=CARTESIAN_POINT('Ctrl Pts',(-0.906777259631241,1.83213318063528,
-32.4148810720433));
#56474=CARTESIAN_POINT('Ctrl Pts',(0.244785644071488,1.8398977864338,-32.5765442393965));
#56475=CARTESIAN_POINT('Ctrl Pts',(0.968910733677276,1.82986059036888,-32.3233308102765));
#56476=CARTESIAN_POINT('Ctrl Pts',(1.27454163485273,1.8276996776529,-32.1285752398414));
#56477=CARTESIAN_POINT('Ctrl Pts',(1.57644208397091,1.99566187679991,-32.5884753902851));
#56478=CARTESIAN_POINT('Ctrl Pts',(1.97100507309382,1.9885807024151,-32.345177614523));
#56479=CARTESIAN_POINT('Ctrl Pts',(2.79658360538242,1.98287648602251,-31.4952486579893));
#56480=CARTESIAN_POINT('Ctrl Pts',(2.96667415068578,2.03643433013976,-30.2472423249499));
#56481=CARTESIAN_POINT('Ctrl Pts',(2.74056010357048,2.05208677514991,-29.2806260191735));
#56482=CARTESIAN_POINT('Ctrl Pts',(2.55597801423823,2.06256996690073,-28.8141728220434));
#56483=CARTESIAN_POINT('Ctrl Pts',(1.94794652960207,2.09483464954365,-27.9954419169136));
#56484=CARTESIAN_POINT('Ctrl Pts',(0.802279448537956,2.14101584746524,-27.3312746370507));
#56485=CARTESIAN_POINT('Ctrl Pts',(-0.80422250876151,2.14111565459134,-27.3323492148327));
#56486=CARTESIAN_POINT('Ctrl Pts',(-2.17661844051394,2.08500434760299,-28.1331664227393));
#56487=CARTESIAN_POINT('Ctrl Pts',(-2.68307713098919,2.05482231865599,-29.0481824505078));
#56488=CARTESIAN_POINT('Ctrl Pts',(-2.85317444361622,2.04476692737883,-29.7536088239151));
#56489=CARTESIAN_POINT('Ctrl Pts',(-2.90642449768279,2.03282840777432,-30.22927942631));
#56490=CARTESIAN_POINT('Ctrl Pts',(-2.79629611681264,2.00277800636097,-31.1428048397418));
#56491=CARTESIAN_POINT('Ctrl Pts',(-2.26248035166364,1.97897801598921,-32.1646758668128));
#56492=CARTESIAN_POINT('Ctrl Pts',(-1.11307220412048,2.00775834857362,-32.9330684865351));
#56493=CARTESIAN_POINT('Ctrl Pts',(0.299068585902303,2.02244161902527,-33.1194515816353));
#56494=CARTESIAN_POINT('Ctrl Pts',(1.19476099588608,2.00251186126023,-32.823829851655));
#56495=CARTESIAN_POINT('Ctrl Pts',(1.57644208397091,1.99566187679991,-32.5884753902851));
#56496=CARTESIAN_POINT('Ctrl Pts',(1.7019170311789,1.9841758627661,-32.7826729204701));
#56497=CARTESIAN_POINT('Ctrl Pts',(2.12920577407486,1.97332831724216,-32.5206340925411));
#56498=CARTESIAN_POINT('Ctrl Pts',(3.02661590274896,1.96081108314947,-31.598486221152));
#56499=CARTESIAN_POINT('Ctrl Pts',(3.20555263301232,2.02375902210562,-30.2475171721583));
#56500=CARTESIAN_POINT('Ctrl Pts',(2.96141616799977,2.03832498497809,-29.2059464506088));
#56501=CARTESIAN_POINT('Ctrl Pts',(2.76077187221957,2.05058763177432,-28.7007479940497));
#56502=CARTESIAN_POINT('Ctrl Pts',(2.10137698734444,2.08724640507052,-27.8170592929481));
#56503=CARTESIAN_POINT('Ctrl Pts',(0.863471086326564,2.14121820993117,-27.1043323065609));
#56504=CARTESIAN_POINT('Ctrl Pts',(-0.86527131205636,2.14132533286026,-27.1055607008419));
#56505=CARTESIAN_POINT('Ctrl Pts',(-2.34826718848484,2.07619929406285,-27.9643060633081));
#56506=CARTESIAN_POINT('Ctrl Pts',(-2.89858207601554,2.04205880766061,-28.953501894721));
#56507=CARTESIAN_POINT('Ctrl Pts',(-3.08328115399646,2.03085086602267,-29.7168832273726));
#56508=CARTESIAN_POINT('Ctrl Pts',(-3.14100419297298,2.01861532274412,-30.2293427451567));
#56509=CARTESIAN_POINT('Ctrl Pts',(-3.02438609187982,1.98457308078909,-31.2166546642125));
#56510=CARTESIAN_POINT('Ctrl Pts',(-2.44599217953573,1.95940735428246,-32.3264040160697));
#56511=CARTESIAN_POINT('Ctrl Pts',(-1.19853457360234,2.00220690733558,-33.1534394779125));
#56512=CARTESIAN_POINT('Ctrl Pts',(0.321543600862733,2.02241016559728,-33.3511773448253));
#56513=CARTESIAN_POINT('Ctrl Pts',(1.28857863702931,1.99466925188967,-33.036156566229));
#56514=CARTESIAN_POINT('Ctrl Pts',(1.7019170311789,1.9841758627661,-32.7826729204701));
#56515=CARTESIAN_POINT('Ctrl Pts',(1.7019170311789,1.9841758627661,-32.7826729204701));
#56516=CARTESIAN_POINT('Ctrl Pts',(1.57644208397091,1.99566187679991,-32.5884753902851));
#56517=CARTESIAN_POINT('Ctrl Pts',(1.27454163485273,1.8276996776529,-32.1285752398414));
#56518=CARTESIAN_POINT('Ctrl Pts',(1.11956381130215,1.29420809400475,-31.9092992200441));
#56519=CARTESIAN_POINT('Ctrl Pts',(1.11427248149542,0.985616400927087,-31.9127256716229));
#56520=CARTESIAN_POINT('Ctrl Pts',(-2.6112,-1.7952,-17.9847266586119));
#56521=CARTESIAN_POINT('Ctrl Pts',(-2.6112,-1.7952,-17.8038186312799));
#56522=CARTESIAN_POINT('Ctrl Pts',(-2.6112,-1.7952,-17.6229797056178));
#56523=CARTESIAN_POINT('Ctrl Pts',(-2.61120000000001,-1.7952,-15.4299462974754));
#56524=CARTESIAN_POINT('Ctrl Pts',(-2.61119999999997,-1.79520000000006,
-13.4283436818382));
#56525=CARTESIAN_POINT('Ctrl Pts',(-2.6112,-1.7952,-11.3982797880253));
#56526=CARTESIAN_POINT('Ctrl Pts',(-2.6112,-1.7952,-11.3949488097292));
#56527=CARTESIAN_POINT('Ctrl Pts',(-2.6112,-1.7952,-11.3916190672592));
#56528=CARTESIAN_POINT('Ctrl Pts',(-2.77989728120026,-1.95404468986484,
-17.9847305491976));
#56529=CARTESIAN_POINT('Ctrl Pts',(-2.77989657069797,-1.95404498366009,
-17.8038217156034));
#56530=CARTESIAN_POINT('Ctrl Pts',(-2.77989885548672,-1.95404480761269,
-17.6228745058655));
#56531=CARTESIAN_POINT('Ctrl Pts',(-2.77986360351872,-1.95404717491004,
-15.4319102613121));
#56532=CARTESIAN_POINT('Ctrl Pts',(-2.78490918456105,-1.9809296830024,-13.4264720521715));
#56533=CARTESIAN_POINT('Ctrl Pts',(-2.77977307325551,-1.95384830245126,
-11.3904949845565));
#56534=CARTESIAN_POINT('Ctrl Pts',(-2.77976473793328,-1.95380467400608,
-11.3872330515971));
#56535=CARTESIAN_POINT('Ctrl Pts',(-2.77975642964883,-1.95376115846772,
-11.3839397041863));
#56536=CARTESIAN_POINT('Ctrl Pts',(-3.00527959091536,-2.05140295765447,
-17.9847344249878));
#56537=CARTESIAN_POINT('Ctrl Pts',(-3.00527820077576,-2.0514038959004,-17.80382478864));
#56538=CARTESIAN_POINT('Ctrl Pts',(-3.00528063959888,-2.05140328438882,
-17.6227699131191));
#56539=CARTESIAN_POINT('Ctrl Pts',(-3.00524011522215,-2.05141620495531,
-15.433862968178));
#56540=CARTESIAN_POINT('Ctrl Pts',(-3.03079562252321,-2.09655587208129,
-13.4246144926598));
#56541=CARTESIAN_POINT('Ctrl Pts',(-3.00496931991195,-2.05104808335724,
-11.3827398048443));
#56542=CARTESIAN_POINT('Ctrl Pts',(-3.00492672599342,-2.05097607451537,
-11.3795465922533));
#56543=CARTESIAN_POINT('Ctrl Pts',(-3.00488462572301,-2.05090371235558,
-11.376289460898));
#56544=CARTESIAN_POINT('Ctrl Pts',(-3.2365718826939,-2.06534153551084,-17.9847374128284));
#56545=CARTESIAN_POINT('Ctrl Pts',(-3.23657012621139,-2.06534337873604,
-17.8038271587737));
#56546=CARTESIAN_POINT('Ctrl Pts',(-3.23657277689822,-2.06534385547269,
-17.6226933437992));
#56547=CARTESIAN_POINT('Ctrl Pts',(-3.23652783128775,-2.06535065050216,
-15.4352998782646));
#56548=CARTESIAN_POINT('Ctrl Pts',(-3.28422590292882,-2.11198472512398,
-13.4234076931397));
#56549=CARTESIAN_POINT('Ctrl Pts',(-3.2360940577226,-2.06491840819467,-11.3767602403348));
#56550=CARTESIAN_POINT('Ctrl Pts',(-3.23601450622251,-2.06484630497268,
-11.3736192543818));
#56551=CARTESIAN_POINT('Ctrl Pts',(-3.23593596401738,-2.06477283942456,
-11.3703894647525));
#56552=CARTESIAN_POINT('',(-2.6112,-1.7952,-12.0768));
#56553=CARTESIAN_POINT('Ctrl Pts',(-3.23593596335381,-2.06477283939948,
-11.3703894654624));
#56554=CARTESIAN_POINT('Ctrl Pts',(-3.23474911227318,-2.06472795379312,
-11.3716587203814));
#56555=CARTESIAN_POINT('Ctrl Pts',(-3.23356208451618,-2.06468080653982,
-11.3729279078231));
#56556=CARTESIAN_POINT('Ctrl Pts',(-3.21770668024123,-2.06402110482042,
-11.3898827330855));
#56557=CARTESIAN_POINT('Ctrl Pts',(-3.20326350624142,-2.06308054430746,
-11.4057713990633));
#56558=CARTESIAN_POINT('Ctrl Pts',(-3.17469796288973,-2.0605365195,-11.4371598604922));
#56559=CARTESIAN_POINT('Ctrl Pts',(-3.16053710931684,-2.05894031541534,
-11.4527727770445));
#56560=CARTESIAN_POINT('Ctrl Pts',(-3.11874262004929,-2.05324512177431,
-11.4989707101412));
#56561=CARTESIAN_POINT('Ctrl Pts',(-3.09119467476536,-2.04821009397366,
-11.5295815571663));
#56562=CARTESIAN_POINT('Ctrl Pts',(-3.01139845824404,-2.02988905583392,
-11.6185972772731));
#56563=CARTESIAN_POINT('Ctrl Pts',(-2.95944916080578,-2.01321064940806,
-11.6770218573854));
#56564=CARTESIAN_POINT('Ctrl Pts',(-2.80388238880711,-1.94794876530532,
-11.8532974877227));
#56565=CARTESIAN_POINT('Ctrl Pts',(-2.7010964672983,-1.88292076974793,-11.9716088406924));
#56566=CARTESIAN_POINT('Ctrl Pts',(-2.61119999999998,-1.79520000000001,
-12.0768));
#56567=CARTESIAN_POINT('',(-2.6112,-1.7952,-17.2992));
#56568=CARTESIAN_POINT('Ctrl Pts',(-2.6112,-1.7952,-17.2992));
#56569=CARTESIAN_POINT('Ctrl Pts',(-2.70186167676372,-1.88058822619405,
-17.4015213914483));
#56570=CARTESIAN_POINT('Ctrl Pts',(-2.80486101159827,-1.94451507288388,
-17.5160105710852));
#56571=CARTESIAN_POINT('Ctrl Pts',(-3.01370491385484,-2.03227186506088,
-17.7451334738264));
#56572=CARTESIAN_POINT('Ctrl Pts',(-3.12339555017824,-2.05811702770554,
-17.8639679791454));
#56573=CARTESIAN_POINT('Ctrl Pts',(-3.23424858100826,-2.06519943732415,
-17.9822588144596));
#56574=CARTESIAN_POINT('Ctrl Pts',(-3.23541015404723,-2.06527153855177,
-17.983498128713));
#56575=CARTESIAN_POINT('Ctrl Pts',(-3.23657188269389,-2.06534153551084,
-17.9847374128283));
#56576=CARTESIAN_POINT('',(-2.6112,-1.7952,-17.2992));
#56577=CARTESIAN_POINT('Ctrl Pts',(3.29672665861269,-1.7952,-17.2992));
#56578=CARTESIAN_POINT('Ctrl Pts',(2.35555773128068,-1.7952,-17.2992));
#56579=CARTESIAN_POINT('Ctrl Pts',(0.157077029037056,-1.7952,-17.2992));
#56580=CARTESIAN_POINT('Ctrl Pts',(-2.04159461806908,-1.7952,-17.2992));
#56581=CARTESIAN_POINT('Ctrl Pts',(-3.29672665861176,-1.7952,-17.2992));
#56582=CARTESIAN_POINT('Ctrl Pts',(3.27462222013899,-1.9675756217075,-17.4822674903391));
#56583=CARTESIAN_POINT('Ctrl Pts',(2.33444703225756,-1.93319533298188,-17.4767078287549));
#56584=CARTESIAN_POINT('Ctrl Pts',(0.154267744829852,-1.85615680163965,
-17.4367287277564));
#56585=CARTESIAN_POINT('Ctrl Pts',(-2.0208154190802,-1.92172646467574,-17.4748531896899));
#56586=CARTESIAN_POINT('Ctrl Pts',(-3.27462222013808,-1.96757562170745,
-17.4822674903391));
#56587=CARTESIAN_POINT('Ctrl Pts',(3.25263565790317,-2.06631231538414,-17.7328313194308));
#56588=CARTESIAN_POINT('Ctrl Pts',(2.31339000270371,-2.00929176274259,-17.7003376499762));
#56589=CARTESIAN_POINT('Ctrl Pts',(0.151449899736544,-1.88860291849517,
-17.5858308525659));
#56590=CARTESIAN_POINT('Ctrl Pts',(-2.00006847092217,-1.99027036317821,
-17.6894981361277));
#56591=CARTESIAN_POINT('Ctrl Pts',(-3.25263565790227,-2.06631231538406,
-17.7328313194307));
#56592=CARTESIAN_POINT('Ctrl Pts',(3.2365718826948,-2.06534153551092,-17.9847374128284));
#56593=CARTESIAN_POINT('Ctrl Pts',(2.29676905143962,-2.00870599133178,-17.924480085149));
#56594=CARTESIAN_POINT('Ctrl Pts',(0.14883959757836,-1.89016258129227,-17.7348933106489));
#56595=CARTESIAN_POINT('Ctrl Pts',(-1.98326165214378,-1.9898130261557,-17.9043789347151));
#56596=CARTESIAN_POINT('Ctrl Pts',(-3.23657188269391,-2.06534153551084,
-17.9847374128283));
#56597=CARTESIAN_POINT('',(2.6112,-1.7952,-17.2992));
#56598=CARTESIAN_POINT('Ctrl Pts',(2.6112,-1.7952,-17.2992));
#56599=CARTESIAN_POINT('Ctrl Pts',(2.70179483356098,-1.88052135230686,-17.4014820850961));
#56600=CARTESIAN_POINT('Ctrl Pts',(2.80470828086409,-1.94441882305696,-17.5159947338438));
#56601=CARTESIAN_POINT('Ctrl Pts',(3.01348181545287,-2.03220905700659,-17.7451259671429));
#56602=CARTESIAN_POINT('Ctrl Pts',(3.12325136755414,-2.05810707767854,-17.8640229733036));
#56603=CARTESIAN_POINT('Ctrl Pts',(3.23424428254041,-2.06519917044408,-17.9822585773976));
#56604=CARTESIAN_POINT('Ctrl Pts',(3.23540799956588,-2.06527140871556,-17.9834980150053));
#56605=CARTESIAN_POINT('Ctrl Pts',(3.23657188269388,-2.06534153551087,-17.9847374128284));
#56606=CARTESIAN_POINT('',(2.6112,-1.7952,-17.2992));
#56607=CARTESIAN_POINT('Ctrl Pts',(2.6112,-1.7952,-11.3916190672592));
#56608=CARTESIAN_POINT('Ctrl Pts',(2.6112,-1.7952,-11.3949488317952));
#56609=CARTESIAN_POINT('Ctrl Pts',(2.6112,-1.7952,-11.3982785791877));
#56610=CARTESIAN_POINT('Ctrl Pts',(2.61119999999999,-1.7952,-11.602832033445));
#56611=CARTESIAN_POINT('Ctrl Pts',(2.6112,-1.7952,-12.0053665520704));
#56612=CARTESIAN_POINT('Ctrl Pts',(2.6112,-1.7952,-12.6092595592021));
#56613=CARTESIAN_POINT('Ctrl Pts',(2.6112,-1.7952,-13.2132104845282));
#56614=CARTESIAN_POINT('Ctrl Pts',(2.6112,-1.7952,-13.817202001388));
#56615=CARTESIAN_POINT('Ctrl Pts',(2.6112,-1.7952,-14.4211425787327));
#56616=CARTESIAN_POINT('Ctrl Pts',(2.6112,-1.7952,-15.0251107188001));
#56617=CARTESIAN_POINT('Ctrl Pts',(2.6112,-1.7952,-15.6291801268932));
#56618=CARTESIAN_POINT('Ctrl Pts',(2.6112,-1.7952,-16.2333316263011));
#56619=CARTESIAN_POINT('Ctrl Pts',(2.6112,-1.7952,-16.8375946102639));
#56620=CARTESIAN_POINT('Ctrl Pts',(2.6112,-1.7952,-17.2405176643803));
#56621=CARTESIAN_POINT('Ctrl Pts',(2.6112,-1.7952,-17.6229032948673));
#56622=CARTESIAN_POINT('Ctrl Pts',(2.6112,-1.7952,-17.8038125599604));
#56623=CARTESIAN_POINT('Ctrl Pts',(2.6112,-1.7952,-17.9847266586118));
#56624=CARTESIAN_POINT('Ctrl Pts',(2.77975642964883,-1.95376115846772,-11.3839397041863));
#56625=CARTESIAN_POINT('Ctrl Pts',(2.77976473798834,-1.95380467429445,-11.387233073422));
#56626=CARTESIAN_POINT('Ctrl Pts',(2.77977307189872,-1.95384850217605,-11.3905252176229));
#56627=CARTESIAN_POINT('Ctrl Pts',(2.78029059422271,-1.95655831630512,-11.5929254382172));
#56628=CARTESIAN_POINT('Ctrl Pts',(2.78108092408054,-1.96087507413405,-11.9996813082198));
#56629=CARTESIAN_POINT('Ctrl Pts',(2.78166904335597,-1.96461218616667,-12.6052412508096));
#56630=CARTESIAN_POINT('Ctrl Pts',(2.78190434852498,-1.96611094161964,-13.2119111458807));
#56631=CARTESIAN_POINT('Ctrl Pts',(2.78187541204246,-1.96583132347523,-13.817493293962));
#56632=CARTESIAN_POINT('Ctrl Pts',(2.78165383672433,-1.96424923733261,-14.4226530410535));
#56633=CARTESIAN_POINT('Ctrl Pts',(2.78128602574335,-1.96184656545489,-15.02729567872));
#56634=CARTESIAN_POINT('Ctrl Pts',(2.78083334812767,-1.95910495087451,-15.6315963053697));
#56635=CARTESIAN_POINT('Ctrl Pts',(2.78037226762904,-1.95651735366381,-16.2354433429288));
#56636=CARTESIAN_POINT('Ctrl Pts',(2.78000529832649,-1.9545750332871,-16.8389564677654));
#56637=CARTESIAN_POINT('Ctrl Pts',(2.77989762673263,-1.95404171479014,-17.2410103818547));
#56638=CARTESIAN_POINT('Ctrl Pts',(2.77989674977132,-1.95404389310532,-17.6226204503694));
#56639=CARTESIAN_POINT('Ctrl Pts',(2.77989657067412,-1.95404498366996,-17.8038156442568));
#56640=CARTESIAN_POINT('Ctrl Pts',(2.77989728120025,-1.95404468986484,-17.9847305491976));
#56641=CARTESIAN_POINT('Ctrl Pts',(3.00488462572301,-2.05090371235558,-11.376289460898));
#56642=CARTESIAN_POINT('Ctrl Pts',(3.00492672627241,-2.05097607499491,-11.3795466138381));
#56643=CARTESIAN_POINT('Ctrl Pts',(3.00496909004423,-2.05104893207522,-11.3828013386179));
#56644=CARTESIAN_POINT('Ctrl Pts',(3.00759032329905,-2.05555770794966,-11.583059109221));
#56645=CARTESIAN_POINT('Ctrl Pts',(3.01162939612273,-2.06287948227701,-11.994019831593));
#56646=CARTESIAN_POINT('Ctrl Pts',(3.01502559244183,-2.06919068355675,-12.6012395611528));
#56647=CARTESIAN_POINT('Ctrl Pts',(3.01638025343442,-2.07174063869622,-13.210615927018));
#56648=CARTESIAN_POINT('Ctrl Pts',(3.01615487636255,-2.07126503359285,-13.8177813034702));
#56649=CARTESIAN_POINT('Ctrl Pts',(3.01476443826533,-2.0685876908235,-14.4241546208859));
#56650=CARTESIAN_POINT('Ctrl Pts',(3.01260262607997,-2.06452689158505,-15.0294692549031));
#56651=CARTESIAN_POINT('Ctrl Pts',(3.01008433904802,-2.05990604728973,-15.6340008239812));
#56652=CARTESIAN_POINT('Ctrl Pts',(3.00765552944531,-2.05555450697557,-16.2375454125361));
#56653=CARTESIAN_POINT('Ctrl Pts',(3.00579999024632,-2.05229554923455,-16.8403123323523));
#56654=CARTESIAN_POINT('Ctrl Pts',(3.00527820611931,-2.051400250927,-17.2415009376399));
#56655=CARTESIAN_POINT('Ctrl Pts',(3.00527780370662,-2.05140286172455,-17.6223388317464));
#56656=CARTESIAN_POINT('Ctrl Pts',(3.0052782007291,-2.05140389593189,-17.8038187172666));
#56657=CARTESIAN_POINT('Ctrl Pts',(3.00527959091535,-2.05140295765448,-17.9847344249877));
#56658=CARTESIAN_POINT('Ctrl Pts',(3.23593596401738,-2.06477283942456,-11.3703894647525));
#56659=CARTESIAN_POINT('Ctrl Pts',(3.23601450674301,-2.06484630545954,-11.3736192757854));
#56660=CARTESIAN_POINT('Ctrl Pts',(3.2360935773066,-2.06492021722567,-11.3768457420933));
#56661=CARTESIAN_POINT('Ctrl Pts',(3.24098309020377,-2.06950210825037,-11.5754888699177));
#56662=CARTESIAN_POINT('Ctrl Pts',(3.24852404096208,-2.07718177263222,-11.9897144106618));
#56663=CARTESIAN_POINT('Ctrl Pts',(3.25495835163609,-2.0836979792605,-12.5981980422748));
#56664=CARTESIAN_POINT('Ctrl Pts',(3.25752083357516,-2.08636008311531,-13.2096246578577));
#56665=CARTESIAN_POINT('Ctrl Pts',(3.25707692954116,-2.08586417392827,-13.8179806012891));
#56666=CARTESIAN_POINT('Ctrl Pts',(3.25441336551011,-2.08309603063915,-14.42527398279));
#56667=CARTESIAN_POINT('Ctrl Pts',(3.25030484001515,-2.07889552730337,-15.0311078760445));
#56668=CARTESIAN_POINT('Ctrl Pts',(3.24554996678201,-2.07412283442935,-15.6358291186907));
#56669=CARTESIAN_POINT('Ctrl Pts',(3.24099557149147,-2.06963003990913,-16.2391544763694));
#56670=CARTESIAN_POINT('Ctrl Pts',(3.23753474759444,-2.0662687333896,-16.8413552372142));
#56671=CARTESIAN_POINT('Ctrl Pts',(3.23656829394497,-2.06534293239529,-17.2418783823923));
#56672=CARTESIAN_POINT('Ctrl Pts',(3.23656896082705,-2.06534377018181,-17.6221221200761));
#56673=CARTESIAN_POINT('Ctrl Pts',(3.23657012615242,-2.06534337879792,-17.8038210873795));
#56674=CARTESIAN_POINT('Ctrl Pts',(3.23657188269388,-2.06534153551086,-17.9847374128284));
#56675=CARTESIAN_POINT('',(2.6112,-1.7952,-12.0768));
#56676=CARTESIAN_POINT('Ctrl Pts',(2.6112,-1.7952,-12.0768));
#56677=CARTESIAN_POINT('Ctrl Pts',(2.70108906248718,-1.88293102006866,-11.97158933628));
#56678=CARTESIAN_POINT('Ctrl Pts',(2.80383287136991,-1.94791497263524,-11.8532683416248));
#56679=CARTESIAN_POINT('Ctrl Pts',(2.95935587549655,-2.0131643150658,-11.6768902688329));
#56680=CARTESIAN_POINT('Ctrl Pts',(3.01128269850091,-2.02984330840291,-11.6183900264733));
#56681=CARTESIAN_POINT('Ctrl Pts',(3.09123953787233,-2.04821304173687,-11.529435637509));
#56682=CARTESIAN_POINT('Ctrl Pts',(3.11894944687461,-2.05328114880983,-11.4988527223898));
#56683=CARTESIAN_POINT('Ctrl Pts',(3.17524764513357,-2.06093594854933,-11.4367604756888));
#56684=CARTESIAN_POINT('Ctrl Pts',(3.20350843291098,-2.06343538786481,-11.4052693925845));
#56685=CARTESIAN_POINT('Ctrl Pts',(3.23357666665279,-2.06468169900353,-11.3729269299378));
#56686=CARTESIAN_POINT('Ctrl Pts',(3.23475628359345,-2.06472837703521,-11.3716581976009));
#56687=CARTESIAN_POINT('Ctrl Pts',(3.2359359640172,-2.06477283942451,-11.3703894647503));
#56688=CARTESIAN_POINT('',(2.6112,-1.7952,-12.0768));
#56689=CARTESIAN_POINT('Ctrl Pts',(-3.29642266651177,-1.79519748712059,
-12.0768026712547));
#56690=CARTESIAN_POINT('Ctrl Pts',(-3.24358001593308,-1.7951975141813,-12.0768026674452));
#56691=CARTESIAN_POINT('Ctrl Pts',(-3.19073147951111,-1.79519754134527,
-12.0768026631509));
#56692=CARTESIAN_POINT('Ctrl Pts',(-2.30200704699003,-1.79519799153053,
-12.0768025940069));
#56693=CARTESIAN_POINT('Ctrl Pts',(-0.210367141271462,-1.7951990085787,
-12.0768020751207));
#56694=CARTESIAN_POINT('Ctrl Pts',(1.88431933586522,-1.79519823108613,-12.0768025301754));
#56695=CARTESIAN_POINT('Ctrl Pts',(3.1907250856176,-1.79519754057334,-12.0768026640128));
#56696=CARTESIAN_POINT('Ctrl Pts',(3.24358391077697,-1.79519751417976,-12.076802667445));
#56697=CARTESIAN_POINT('Ctrl Pts',(3.29642845573587,-1.79519748711763,-12.0768026712551));
#56698=CARTESIAN_POINT('Ctrl Pts',(-3.27408831410364,-1.9722276015856,-11.888615889407));
#56699=CARTESIAN_POINT('Ctrl Pts',(-3.22130116681679,-1.97032122721793,
-11.8888842560883));
#56700=CARTESIAN_POINT('Ctrl Pts',(-3.16852989305899,-1.96840757721836,
-11.889186770879));
#56701=CARTESIAN_POINT('Ctrl Pts',(-2.28147119761913,-1.93669289133901,
-11.8940577302633));
#56702=CARTESIAN_POINT('Ctrl Pts',(-0.206758859811364,-1.86504377040126,
-11.9306120492651));
#56703=CARTESIAN_POINT('Ctrl Pts',(1.86459196778903,-1.91981665684861,-11.8985544808556));
#56704=CARTESIAN_POINT('Ctrl Pts',(3.16852276150168,-1.96846195848408,-11.8891260506951));
#56705=CARTESIAN_POINT('Ctrl Pts',(3.22130505642342,-1.97032133571503,-11.8888842700037));
#56706=CARTESIAN_POINT('Ctrl Pts',(3.27409409724692,-1.97222781045467,-11.8886158599898));
#56707=CARTESIAN_POINT('Ctrl Pts',(-3.25188642042027,-2.07124454663285,
-11.6291452762124));
#56708=CARTESIAN_POINT('Ctrl Pts',(-3.19915094357724,-2.06808131163795,
-11.6308935276775));
#56709=CARTESIAN_POINT('Ctrl Pts',(-3.1464530232335,-2.06491642594862,-11.6326958363931));
#56710=CARTESIAN_POINT('Ctrl Pts',(-2.26099539435471,-2.01245733351299,
-11.66238937861));
#56711=CARTESIAN_POINT('Ctrl Pts',(-0.203136696371867,-1.90101534660559,
-11.7690581356509));
#56712=CARTESIAN_POINT('Ctrl Pts',(1.84488996298587,-1.98523478906184,-11.6813986289955));
#56713=CARTESIAN_POINT('Ctrl Pts',(3.1464452756991,-2.06498681864732,-11.6325557398156));
#56714=CARTESIAN_POINT('Ctrl Pts',(3.19915482816189,-2.06808150272424,-11.6308934784624));
#56715=CARTESIAN_POINT('Ctrl Pts',(3.25189219790266,-2.07124489320274,-11.6291450846441));
#56716=CARTESIAN_POINT('Ctrl Pts',(-3.23597709627681,-2.0647751983077,-11.3703832379468));
#56717=CARTESIAN_POINT('Ctrl Pts',(-3.18320926520253,-2.06164839985804,
-11.3736415239251));
#56718=CARTESIAN_POINT('Ctrl Pts',(-3.13049942170299,-2.05852190907284,
-11.3769735809423));
#56719=CARTESIAN_POINT('Ctrl Pts',(-2.24493355632026,-2.00672158959924,
-11.4319074741996));
#56720=CARTESIAN_POINT('Ctrl Pts',(-0.199619045096931,-1.89967482673457,
-11.6080442665278));
#56721=CARTESIAN_POINT('Ctrl Pts',(1.82862748588428,-1.98056379950097,-11.4653731295733));
#56722=CARTESIAN_POINT('Ctrl Pts',(3.13049602407356,-2.0585699244099,-11.3767617538477));
#56723=CARTESIAN_POINT('Ctrl Pts',(3.18321314808538,-2.06164860144816,-11.3736414048196));
#56724=CARTESIAN_POINT('Ctrl Pts',(3.23598287730504,-2.0647755408798,-11.370382880926));
#56725=CARTESIAN_POINT('',(-2.6112,-1.7952,-12.0768));
#56726=CARTESIAN_POINT('Origin',(0.,-1.7952,-14.688));
#56727=CARTESIAN_POINT('Ctrl Pts',(-27.803209900382,9.23603435870819,-72.5577790171547));
#56728=CARTESIAN_POINT('Ctrl Pts',(-27.8052592499116,10.4382360290543,-71.9219265766247));
#56729=CARTESIAN_POINT('Ctrl Pts',(-27.8073085994413,11.6404376994003,-71.2860741360946));
#56730=CARTESIAN_POINT('Ctrl Pts',(-27.8093579489709,12.8426393697465,-70.6502216955646));
#56731=CARTESIAN_POINT('Ctrl Pts',(-27.6551378439486,9.49096672380132,-73.0393005844633));
#56732=CARTESIAN_POINT('Ctrl Pts',(-27.6577399757294,10.6926691697792,-72.4025060111301));
#56733=CARTESIAN_POINT('Ctrl Pts',(-27.6603592487415,11.8943607952455,-71.7656911381846));
#56734=CARTESIAN_POINT('Ctrl Pts',(-27.6629613805351,13.0960632412153,-71.1288965648361));
#56735=CARTESIAN_POINT('Ctrl Pts',(-27.3490633632825,10.0377474084797,-74.0689767319683));
#56736=CARTESIAN_POINT('Ctrl Pts',(-27.3523402607163,11.2386401731222,-73.4306601269834));
#56737=CARTESIAN_POINT('Ctrl Pts',(-27.3556287080767,12.4395358745722,-72.7923490828472));
#56738=CARTESIAN_POINT('Ctrl Pts',(-27.3589056055191,13.6404286392169,-72.1540324778666));
#56739=CARTESIAN_POINT('Ctrl Pts',(-26.7423192852016,11.1383815330078,-76.1342058942393));
#56740=CARTESIAN_POINT('Ctrl Pts',(-26.7452350312789,12.3387016520456,-75.4948119055702));
#56741=CARTESIAN_POINT('Ctrl Pts',(-26.7481576407974,13.5390168090643,-74.8554085957215));
#56742=CARTESIAN_POINT('Ctrl Pts',(-26.7510733868799,14.7393369280985,-74.2160146070454));
#56743=CARTESIAN_POINT('Ctrl Pts',(-26.2567727580936,11.9678276411624,-77.6901374866193));
#56744=CARTESIAN_POINT('Ctrl Pts',(-26.2588779851847,13.1684233865823,-77.0512578239776));
#56745=CARTESIAN_POINT('Ctrl Pts',(-26.2610419402911,14.3690213682034,-76.4123829857732));
#56746=CARTESIAN_POINT('Ctrl Pts',(-26.2631471674262,15.5696171136249,-75.7735033231351));
#56747=CARTESIAN_POINT('Ctrl Pts',(-25.9521939343629,12.4413211944637,-78.5797217247913));
#56748=CARTESIAN_POINT('Ctrl Pts',(-25.9541384780474,13.6421291419706,-77.941240813488));
#56749=CARTESIAN_POINT('Ctrl Pts',(-25.9560830217321,14.8429370894773,-77.3027599021845));
#56750=CARTESIAN_POINT('Ctrl Pts',(-25.9580275654167,16.0437450369841,-76.6642789908811));
#56751=CARTESIAN_POINT('',(-25.9551107509796,14.2425337887163,-77.6219999999998));
#56752=CARTESIAN_POINT('',(-27.806283925825,11.0393375380009,-71.6039999999963));
#56753=CARTESIAN_POINT('Ctrl Pts',(-30.3753540341099,6.01695723880277,-66.3794227429406));
#56754=CARTESIAN_POINT('Ctrl Pts',(-30.362690827324,7.26996265932069,-65.8504120080144));
#56755=CARTESIAN_POINT('Ctrl Pts',(-30.350027620538,8.52296807983859,-65.3214012730881));
#56756=CARTESIAN_POINT('Ctrl Pts',(-30.3373644137521,9.7759735003565,-64.7923905381619));
#56757=CARTESIAN_POINT('Ctrl Pts',(-30.1088133612586,6.21732189962616,-66.8603832394881));
#56758=CARTESIAN_POINT('Ctrl Pts',(-30.106912725349,7.45664743997982,-66.2989301326288));
#56759=CARTESIAN_POINT('Ctrl Pts',(-30.104370068785,8.69572635844707,-65.7362566384473));
#56760=CARTESIAN_POINT('Ctrl Pts',(-30.1024695839643,9.93505195683909,-65.1748038187859));
#56761=CARTESIAN_POINT('Ctrl Pts',(-29.7096580135423,6.55735136704459,-67.5873569901587));
#56762=CARTESIAN_POINT('Ctrl Pts',(-29.7189274177172,7.7778112690182,-66.9861296374917));
#56763=CARTESIAN_POINT('Ctrl Pts',(-29.7274740067858,8.99846080978516,-66.3850583054978));
#56764=CARTESIAN_POINT('Ctrl Pts',(-29.7367435810634,10.2189206671305,-65.783830916114));
#56765=CARTESIAN_POINT('Ctrl Pts',(-28.7821722057447,7.57574471691707,-69.5467552476757));
#56766=CARTESIAN_POINT('Ctrl Pts',(-28.8019189087709,8.76527728138276,-68.8866094926591));
#56767=CARTESIAN_POINT('Ctrl Pts',(-28.821609300456,9.95439323841018,-68.2252261249033));
#56768=CARTESIAN_POINT('Ctrl Pts',(-28.8413560167341,11.1439259009176,-67.5650806611384));
#56769=CARTESIAN_POINT('Ctrl Pts',(-28.2846186462697,8.42885715791647,-71.0332031632364));
#56770=CARTESIAN_POINT('Ctrl Pts',(-28.2867169655075,9.61827756684128,-70.3734598241401));
#56771=CARTESIAN_POINT('Ctrl Pts',(-28.2831472841818,10.8081867183063,-69.7127753471578));
#56772=CARTESIAN_POINT('Ctrl Pts',(-28.2852469372896,11.9976070122136,-69.0530322295429));
#56773=CARTESIAN_POINT('Ctrl Pts',(-27.8032099026791,9.23603570625527,-72.5577783044281));
#56774=CARTESIAN_POINT('Ctrl Pts',(-27.8052594925831,10.4383783864874,-71.9218512828337));
#56775=CARTESIAN_POINT('Ctrl Pts',(-27.8073090824873,11.6407210667195,-71.2859242612392));
#56776=CARTESIAN_POINT('Ctrl Pts',(-27.8093586723913,12.8430637469518,-70.6499972396448));
#56777=CARTESIAN_POINT('',(-30.356361458725,7.89624424005172,-65.585999999999));
#56778=CARTESIAN_POINT('Ctrl Pts',(-33.2870419060249,4.35253527707242,-59.9326413364709));
#56779=CARTESIAN_POINT('Ctrl Pts',(-33.1297679354289,5.68135810058103,-59.6895471121553));
#56780=CARTESIAN_POINT('Ctrl Pts',(-32.972493964833,7.01018092408964,-59.4464528878397));
#56781=CARTESIAN_POINT('Ctrl Pts',(-32.815219994237,8.33900374759826,-59.2033586635242));
#56782=CARTESIAN_POINT('Ctrl Pts',(-33.1236843979303,4.41327697339383,-60.3703598245789));
#56783=CARTESIAN_POINT('Ctrl Pts',(-32.9800384987428,5.74096812205601,-60.1121164371264));
#56784=CARTESIAN_POINT('Ctrl Pts',(-32.8359640769173,7.06851339890597,-59.8537914806801));
#56785=CARTESIAN_POINT('Ctrl Pts',(-32.6923181777297,8.39620454756814,-59.5955480932275));
#56786=CARTESIAN_POINT('Ctrl Pts',(-32.6598069524929,4.6233160195265,-61.6572795724073));
#56787=CARTESIAN_POINT('Ctrl Pts',(-32.5452155833611,5.94541733829744,-61.3571538338168));
#56788=CARTESIAN_POINT('Ctrl Pts',(-32.4316412768296,7.26750554303185,-61.056817941821));
#56789=CARTESIAN_POINT('Ctrl Pts',(-32.3170499076978,8.58960686180279,-60.7566922032304));
#56790=CARTESIAN_POINT('Ctrl Pts',(-31.725539611122,5.1629429740609,-64.061279077029));
#56791=CARTESIAN_POINT('Ctrl Pts',(-31.6492324422371,6.46500946226312,-63.6680054128815));
#56792=CARTESIAN_POINT('Ctrl Pts',(-31.5713187665878,7.7670647622256,-63.2747836659281));
#56793=CARTESIAN_POINT('Ctrl Pts',(-31.4950115977029,9.06913125042783,-62.8815100017806));
#56794=CARTESIAN_POINT('Ctrl Pts',(-30.929578969617,5.6097190919677,-65.4015789370632));
#56795=CARTESIAN_POINT('Ctrl Pts',(-30.8937893171137,6.88505174727525,-64.926143571465));
#56796=CARTESIAN_POINT('Ctrl Pts',(-30.8617691542772,8.15989840357671,-64.4502875333333));
#56797=CARTESIAN_POINT('Ctrl Pts',(-30.825979501774,9.43523105888426,-63.9748521677351));
#56798=CARTESIAN_POINT('Ctrl Pts',(-30.3753540341099,6.01695723880277,-66.3794227429406));
#56799=CARTESIAN_POINT('Ctrl Pts',(-30.3626923171866,7.26981523963541,-65.8504742476462));
#56800=CARTESIAN_POINT('Ctrl Pts',(-30.3500306002633,8.52267324046804,-65.3215257523518));
#56801=CARTESIAN_POINT('Ctrl Pts',(-30.33736888334,9.77553124130067,-64.7925772570574));
#56802=CARTESIAN_POINT('',(-33.051130950131,6.34576951233522,-59.5679999999976));
#56803=CARTESIAN_POINT('',(-33.0511309501309,6.34576951233534,-59.5679999999975));
#56804=CARTESIAN_POINT('',(-33.0511309501309,6.34576951233534,-59.5679999999975));
#56805=CARTESIAN_POINT('Ctrl Pts',(-36.1829138277439,4.79791400485575,-53.6562428681641));
#56806=CARTESIAN_POINT('Ctrl Pts',(-35.7573813489674,6.08768352765237,-53.5854142893892));
#56807=CARTESIAN_POINT('Ctrl Pts',(-35.3318488701909,7.377453050449,-53.5145857106142));
#56808=CARTESIAN_POINT('Ctrl Pts',(-34.9063163914144,8.66722257324563,-53.4437571318393));
#56809=CARTESIAN_POINT('Ctrl Pts',(-35.8221894292354,4.71279832802143,-54.2735126527001));
#56810=CARTESIAN_POINT('Ctrl Pts',(-35.4055710113178,6.0086770499647,-54.27897609436));
#56811=CARTESIAN_POINT('Ctrl Pts',(-34.9890919720113,7.30764932080681,-54.2841345487856));
#56812=CARTESIAN_POINT('Ctrl Pts',(-34.5724735540937,8.60352804275007,-54.2895979904455));
#56813=CARTESIAN_POINT('Ctrl Pts',(-35.1345762789437,4.46191327643785,-55.4630423598499));
#56814=CARTESIAN_POINT('Ctrl Pts',(-34.7604641920181,5.76926615742872,-55.5213765022354));
#56815=CARTESIAN_POINT('Ctrl Pts',(-34.3847798507744,7.07531096957354,-55.5792446567707));
#56816=CARTESIAN_POINT('Ctrl Pts',(-34.0106677638488,8.38266385056441,-55.6375787991562));
#56817=CARTESIAN_POINT('Ctrl Pts',(-34.1112888063175,4.18758073788383,-57.6561452037581));
#56818=CARTESIAN_POINT('Ctrl Pts',(-33.8593807355069,5.52781101585105,-57.6216091426396));
#56819=CARTESIAN_POINT('Ctrl Pts',(-33.6074801111067,6.86853513824409,-57.5872134595304));
#56820=CARTESIAN_POINT('Ctrl Pts',(-33.3555720402961,8.20876541621131,-57.5526773984119));
#56821=CARTESIAN_POINT('Ctrl Pts',(-33.5340571648804,4.24789457701618,-59.2008344761412));
#56822=CARTESIAN_POINT('Ctrl Pts',(-33.3563722159371,5.58810392677528,-59.0303155049847));
#56823=CARTESIAN_POINT('Ctrl Pts',(-33.1759712955042,6.92623598341401,-58.8588145985647));
#56824=CARTESIAN_POINT('Ctrl Pts',(-32.9982863465608,8.26644533317311,-58.6882956274082));
#56825=CARTESIAN_POINT('Ctrl Pts',(-33.2870419060249,4.35253527707242,-59.9326413364709));
#56826=CARTESIAN_POINT('Ctrl Pts',(-33.1297679354289,5.68135810058103,-59.6895471121553));
#56827=CARTESIAN_POINT('Ctrl Pts',(-32.972493964833,7.01018092408964,-59.4464528878397));
#56828=CARTESIAN_POINT('Ctrl Pts',(-32.815219994237,8.33900374759826,-59.2033586635242));
#56829=CARTESIAN_POINT('',(-35.5446151095792,6.73256828905069,-53.5500000000017));
#56830=CARTESIAN_POINT('',(-35.5446151095792,6.73256828905069,-53.5500000000017));
#56831=CARTESIAN_POINT('',(-35.5446151095792,6.73256828905069,-53.5500000000017));
#56832=CARTESIAN_POINT('Ctrl Pts',(-38.0224713055506,4.8684211641347,-47.6590291921613));
#56833=CARTESIAN_POINT('Ctrl Pts',(-37.5141101402729,6.12702180277212,-47.5743024240645));
#56834=CARTESIAN_POINT('Ctrl Pts',(-37.0057489009982,7.38562239684713,-47.4895759845357));
#56835=CARTESIAN_POINT('Ctrl Pts',(-36.4973877357239,8.6442230354866,-47.4048492164237));
#56836=CARTESIAN_POINT('Ctrl Pts',(-37.9812710970613,4.87622981994569,-48.0222296824199));
#56837=CARTESIAN_POINT('Ctrl Pts',(-37.4764043002191,6.13527223994773,-47.9241769029098));
#56838=CARTESIAN_POINT('Ctrl Pts',(-36.9719750983327,7.39457818133208,-47.8241811391747));
#56839=CARTESIAN_POINT('Ctrl Pts',(-36.4671082813248,8.65362058919022,-47.7261284492034));
#56840=CARTESIAN_POINT('Ctrl Pts',(-37.8390117177081,4.91385054480188,-49.0952025625359));
#56841=CARTESIAN_POINT('Ctrl Pts',(-37.3492889481593,6.17608455138244,-48.9616650119934));
#56842=CARTESIAN_POINT('Ctrl Pts',(-36.8594199960831,7.43860904700498,-48.8252249030439));
#56843=CARTESIAN_POINT('Ctrl Pts',(-36.3696972332709,8.7008430401989,-48.6916874862603));
#56844=CARTESIAN_POINT('Ctrl Pts',(-37.4172803943982,4.97200440485067,-51.0816419245504));
#56845=CARTESIAN_POINT('Ctrl Pts',(-36.9598775494223,6.2431156660951,-50.9280798398504));
#56846=CARTESIAN_POINT('Ctrl Pts',(-36.5027094328069,7.51388912919058,-50.7775833348501));
#56847=CARTESIAN_POINT('Ctrl Pts',(-36.0453065770139,8.78500040600178,-50.6240211088788));
#56848=CARTESIAN_POINT('Ctrl Pts',(-36.8017946572527,4.93958146881401,-52.5177513156359));
#56849=CARTESIAN_POINT('Ctrl Pts',(-36.3599669126062,6.21923512189812,-52.3770542244419));
#56850=CARTESIAN_POINT('Ctrl Pts',(-35.9183025240337,7.50075084985685,-52.2181590441769));
#56851=CARTESIAN_POINT('Ctrl Pts',(-35.4764747718593,8.78040441713075,-52.0774627916075));
#56852=CARTESIAN_POINT('Ctrl Pts',(-36.1828876819812,4.79790801989533,-53.6562909659612));
#56853=CARTESIAN_POINT('Ctrl Pts',(-35.7573460862841,6.08770768960492,-53.5854637068186));
#56854=CARTESIAN_POINT('Ctrl Pts',(-35.3318044836858,7.37750728064934,-53.5146372164721));
#56855=CARTESIAN_POINT('Ctrl Pts',(-34.906262887989,8.66730695036257,-53.4438099572941));
#56856=CARTESIAN_POINT('',(-37.2599410472769,6.75628005534009,-47.5319999999999));
#56857=CARTESIAN_POINT('Ctrl Pts',(-38.8604541099244,4.82976572790842,-41.6539325852781));
#56858=CARTESIAN_POINT('Ctrl Pts',(-38.4040326949895,6.10748900320921,-41.5606441950923));
#56859=CARTESIAN_POINT('Ctrl Pts',(-37.9476112800546,7.38521227851001,-41.4673558049066));
#56860=CARTESIAN_POINT('Ctrl Pts',(-37.4911898651198,8.66293555381081,-41.3740674147208));
#56861=CARTESIAN_POINT('Ctrl Pts',(-38.7579547565586,4.82831575431509,-42.1355598788231));
#56862=CARTESIAN_POINT('Ctrl Pts',(-38.2908397454192,6.10259351827304,-42.0473364200289));
#56863=CARTESIAN_POINT('Ctrl Pts',(-37.8238151536734,7.37689668296498,-41.9592074712887));
#56864=CARTESIAN_POINT('Ctrl Pts',(-37.3567001425339,8.65117444692294,-41.8709840124945));
#56865=CARTESIAN_POINT('Ctrl Pts',(-38.6165637640568,4.82401373724133,-42.8556343306891));
#56866=CARTESIAN_POINT('Ctrl Pts',(-38.1329344749416,6.09261012024952,-42.7744054967877));
#56867=CARTESIAN_POINT('Ctrl Pts',(-37.6491758337013,7.36115804152699,-42.6932058475502));
#56868=CARTESIAN_POINT('Ctrl Pts',(-37.1655465445862,8.62975442453518,-42.6119770136488));
#56869=CARTESIAN_POINT('Ctrl Pts',(-38.4070763697413,4.82011917504479,-44.1382125964065));
#56870=CARTESIAN_POINT('Ctrl Pts',(-37.8997443650628,6.07993325028302,-44.0657708065558));
#56871=CARTESIAN_POINT('Ctrl Pts',(-37.3923641700085,7.33974267197774,-43.993425978326));
#56872=CARTESIAN_POINT('Ctrl Pts',(-36.88503216533,8.59955674721597,-43.9209841884754));
#56873=CARTESIAN_POINT('Ctrl Pts',(-38.2178923694507,4.82934361138434,-45.7021852706702));
#56874=CARTESIAN_POINT('Ctrl Pts',(-37.6956752256365,6.08323545488938,-45.6340690461451));
#56875=CARTESIAN_POINT('Ctrl Pts',(-37.173491249573,7.33714039137729,-45.5659389089267));
#56876=CARTESIAN_POINT('Ctrl Pts',(-36.6512741057588,8.59103223488232,-45.4978226844016));
#56877=CARTESIAN_POINT('Ctrl Pts',(-38.0970582995982,4.85566739849337,-47.0220693317479));
#56878=CARTESIAN_POINT('Ctrl Pts',(-37.5826091437923,6.11231335186017,-46.9455012979541));
#56879=CARTESIAN_POINT('Ctrl Pts',(-37.0677383294391,7.36884011707376,-46.8691997614158));
#56880=CARTESIAN_POINT('Ctrl Pts',(-36.5532891736331,8.62548607044055,-46.792631727622));
#56881=CARTESIAN_POINT('Ctrl Pts',(-38.0224643391855,4.8684224845004,-47.6590906035864));
#56882=CARTESIAN_POINT('Ctrl Pts',(-37.5141154779131,6.12699419839353,-47.5743635345287));
#56883=CARTESIAN_POINT('Ctrl Pts',(-37.0057666166406,7.38556591228666,-47.489636465471));
#56884=CARTESIAN_POINT('Ctrl Pts',(-36.4974177553682,8.64413762617978,-47.4049093964133));
#56885=CARTESIAN_POINT('',(-38.1758219875221,6.74635064085961,-41.5139999999995));
#56886=CARTESIAN_POINT('Ctrl Pts',(-40.1355634406229,4.76730425857361,-35.6660853079992));
#56887=CARTESIAN_POINT('Ctrl Pts',(-39.7267565272628,6.05944617662692,-35.5526924624031));
#56888=CARTESIAN_POINT('Ctrl Pts',(-39.3179496117989,7.35158809405154,-35.4392996166302));
#56889=CARTESIAN_POINT('Ctrl Pts',(-38.9091426984386,8.64373001210486,-35.3259067710341));
#56890=CARTESIAN_POINT('Ctrl Pts',(-40.069789899138,4.77667325925527,-36.0099761177602));
#56891=CARTESIAN_POINT('Ctrl Pts',(-39.6647601607778,6.07017700486549,-35.8984639074028));
#56892=CARTESIAN_POINT('Ctrl Pts',(-39.2599437298742,7.36374449671887,-35.7869696292885));
#56893=CARTESIAN_POINT('Ctrl Pts',(-38.854913990157,8.65724824192357,-35.6754574188171));
#56894=CARTESIAN_POINT('Ctrl Pts',(-39.9548410579829,4.79179797702963,-36.6038794519936));
#56895=CARTESIAN_POINT('Ctrl Pts',(-39.5552706371814,6.08724978139326,-36.4953741367376));
#56896=CARTESIAN_POINT('Ctrl Pts',(-39.1556935142984,7.382699722788,-36.3868668179017));
#56897=CARTESIAN_POINT('Ctrl Pts',(-38.7561230935397,8.67815152716346,-36.2783615026586));
#56898=CARTESIAN_POINT('Ctrl Pts',(-39.7443037262004,4.81133016772462,-37.6330866698068));
#56899=CARTESIAN_POINT('Ctrl Pts',(-39.3462971338669,6.10759749935179,-37.5287105189401));
#56900=CARTESIAN_POINT('Ctrl Pts',(-38.9483293158955,7.40387558580187,-37.4243359249927));
#56901=CARTESIAN_POINT('Ctrl Pts',(-38.5503227233153,8.70014291736062,-37.3199597741161));
#56902=CARTESIAN_POINT('Ctrl Pts',(-39.5813565519597,4.82173156565819,-38.3962454196463));
#56903=CARTESIAN_POINT('Ctrl Pts',(-39.1798326777781,6.11712296255223,-38.2944317819117));
#56904=CARTESIAN_POINT('Ctrl Pts',(-38.7782569657644,7.41249976037084,-38.1926219386844));
#56905=CARTESIAN_POINT('Ctrl Pts',(-38.3767330919126,8.70789115735774,-38.0908083009255));
#56906=CARTESIAN_POINT('Ctrl Pts',(-39.4305411403599,4.82773783061676,-39.0811836979273));
#56907=CARTESIAN_POINT('Ctrl Pts',(-39.0220576798717,6.12110969421629,-38.9813878108934));
#56908=CARTESIAN_POINT('Ctrl Pts',(-38.6136027152855,7.41449063362709,-38.8815873335481));
#56909=CARTESIAN_POINT('Ctrl Pts',(-38.205119254616,8.70786249716888,-38.7817914465434));
#56910=CARTESIAN_POINT('Ctrl Pts',(-39.2609912818215,4.83170251246378,-39.8388585382037));
#56911=CARTESIAN_POINT('Ctrl Pts',(-38.8419292709767,6.12186145082356,-39.7411109024355));
#56912=CARTESIAN_POINT('Ctrl Pts',(-38.4227884822824,7.41199667487817,-39.6433661601837));
#56913=CARTESIAN_POINT('Ctrl Pts',(-38.0037264719387,8.7021556133888,-39.5456185243971));
#56914=CARTESIAN_POINT('Ctrl Pts',(-39.0664816974284,4.83206157495894,-40.6998863785975));
#56915=CARTESIAN_POINT('Ctrl Pts',(-38.6309073172999,6.11693937633135,-40.6042764850154));
#56916=CARTESIAN_POINT('Ctrl Pts',(-38.1954185995026,7.40184291372179,-40.5086663461849));
#56917=CARTESIAN_POINT('Ctrl Pts',(-37.7598442188292,8.68672071493048,-40.4130564526044));
#56918=CARTESIAN_POINT('Ctrl Pts',(-38.9270107680783,4.83045995066367,-41.3378067172326));
#56919=CARTESIAN_POINT('Ctrl Pts',(-38.477464005224,6.11058667135808,-41.2437467144136));
#56920=CARTESIAN_POINT('Ctrl Pts',(-38.0278583234486,7.39069394777282,-41.1496860831278));
#56921=CARTESIAN_POINT('Ctrl Pts',(-37.5783115609693,8.67082066859093,-41.055626080313));
#56922=CARTESIAN_POINT('Ctrl Pts',(-38.8604527970962,4.82976571421489,-41.6539388208502));
#56923=CARTESIAN_POINT('Ctrl Pts',(-38.4040297947643,6.10749300631662,-41.5606501491508));
#56924=CARTESIAN_POINT('Ctrl Pts',(-37.9476067935945,7.3852202988019,-41.4673614774639));
#56925=CARTESIAN_POINT('Ctrl Pts',(-37.4911837912626,8.66294759090364,-41.3740728057645));
#56926=CARTESIAN_POINT('',(-39.5223544282476,6.70551108323309,-35.4960000000003));
#56927=CARTESIAN_POINT('Ctrl Pts',(-41.4215456143025,4.68791021227309,-29.7512571116587));
#56928=CARTESIAN_POINT('Ctrl Pts',(-40.8936521308426,5.92796748849508,-29.5690857038871));
#56929=CARTESIAN_POINT('Ctrl Pts',(-40.3657586473827,7.16802476471708,-29.3869142961156));
#56930=CARTESIAN_POINT('Ctrl Pts',(-39.8378651639228,8.40808204093907,-29.204742888344));
#56931=CARTESIAN_POINT('Ctrl Pts',(-41.3092811227302,4.69284109397027,-30.1101403746882));
#56932=CARTESIAN_POINT('Ctrl Pts',(-40.7860870227411,5.9370021984995,-29.9421436309555));
#56933=CARTESIAN_POINT('Ctrl Pts',(-40.2635498200622,7.18142713867819,-29.7744672927514));
#56934=CARTESIAN_POINT('Ctrl Pts',(-39.7403557200732,8.42558824320743,-29.6064705490188));
#56935=CARTESIAN_POINT('Ctrl Pts',(-41.1168122255416,4.70227545160565,-30.8154015426932));
#56936=CARTESIAN_POINT('Ctrl Pts',(-40.6066654279172,5.95485537606158,-30.6714196014921));
#56937=CARTESIAN_POINT('Ctrl Pts',(-40.0964689705627,7.20743999775218,-30.5275444808975));
#56938=CARTESIAN_POINT('Ctrl Pts',(-39.5863221729383,8.46001992220811,-30.3835625396964));
#56939=CARTESIAN_POINT('Ctrl Pts',(-40.9411342639833,4.71057860533754,-31.5583878958659));
#56940=CARTESIAN_POINT('Ctrl Pts',(-40.4474171521444,5.97172751091908,-31.43372866912));
#56941=CARTESIAN_POINT('Ctrl Pts',(-39.9536697830691,7.23283887630036,-31.3089175330362));
#56942=CARTESIAN_POINT('Ctrl Pts',(-39.4599526712302,8.4939877818819,-31.1842583062903));
#56943=CARTESIAN_POINT('Ctrl Pts',(-40.72104027405,4.72052127144792,-32.5727429381947));
#56944=CARTESIAN_POINT('Ctrl Pts',(-40.2513012525973,5.99266951177614,-32.4676364806858));
#56945=CARTESIAN_POINT('Ctrl Pts',(-39.7814912297972,7.26478923819657,-32.3624564233432));
#56946=CARTESIAN_POINT('Ctrl Pts',(-39.3117522083446,8.53693747852479,-32.2573499658343));
#56947=CARTESIAN_POINT('Ctrl Pts',(-40.5142429668683,4.72897579183149,-33.638548551572));
#56948=CARTESIAN_POINT('Ctrl Pts',(-40.0706647764219,6.01107660461561,-33.5420022229916));
#56949=CARTESIAN_POINT('Ctrl Pts',(-39.6270110271653,7.29317024951508,-33.4456444889633));
#56950=CARTESIAN_POINT('Ctrl Pts',(-39.1834328367189,8.5752710622992,-33.3490981603829));
#56951=CARTESIAN_POINT('Ctrl Pts',(-40.3021090297733,4.74530128710119,-34.7695223916763));
#56952=CARTESIAN_POINT('Ctrl Pts',(-39.8808239070379,6.0344697149634,-34.668233741174));
#56953=CARTESIAN_POINT('Ctrl Pts',(-39.4597383158449,7.32367658963407,-34.5666679306649));
#56954=CARTESIAN_POINT('Ctrl Pts',(-39.0384531931095,8.61284501749628,-34.4653792801627));
#56955=CARTESIAN_POINT('Ctrl Pts',(-40.197670469322,4.75763956421394,-35.3320435682359));
#56956=CARTESIAN_POINT('Ctrl Pts',(-39.7850494778165,6.0490278260316,-35.2239026652054));
#56957=CARTESIAN_POINT('Ctrl Pts',(-39.3724789621606,7.34047705027623,-35.116161791104));
#56958=CARTESIAN_POINT('Ctrl Pts',(-38.9598579706551,8.6318653120939,-35.0080208880735));
#56959=CARTESIAN_POINT('Ctrl Pts',(-40.1355627919428,4.76730435097372,-35.6660886995623));
#56960=CARTESIAN_POINT('Ctrl Pts',(-39.726757216146,6.05944217247997,-35.5526962331876));
#56961=CARTESIAN_POINT('Ctrl Pts',(-39.3179516403492,7.35157999398622,-35.439303766813));
#56962=CARTESIAN_POINT('Ctrl Pts',(-38.9091460645523,8.64371781549247,-35.3259113004384));
#56963=CARTESIAN_POINT('',(-40.6297053891126,6.54799612660609,-29.4780000000013));
#56964=CARTESIAN_POINT('Ctrl Pts',(-44.8643748763769,5.20597739807172,-23.9801519722228));
#56965=CARTESIAN_POINT('Ctrl Pts',(-44.4545859760341,6.45554733375955,-23.633383990741));
#56966=CARTESIAN_POINT('Ctrl Pts',(-44.0447970756913,7.70511726944739,-23.2866160092593));
#56967=CARTESIAN_POINT('Ctrl Pts',(-43.6350081753485,8.95468720513522,-22.9398480277775));
#56968=CARTESIAN_POINT('Ctrl Pts',(-44.74295142856,5.19893273360771,-24.0982573983942));
#56969=CARTESIAN_POINT('Ctrl Pts',(-44.3193209089096,6.44821626255224,-23.7681532567383));
#56970=CARTESIAN_POINT('Ctrl Pts',(-43.8977879609805,7.69892472923156,-23.436688867068));
#56971=CARTESIAN_POINT('Ctrl Pts',(-43.4741574413301,8.94820825817609,-23.1065847254121));
#56972=CARTESIAN_POINT('Ctrl Pts',(-44.4866987396665,5.17768472779144,-24.3599634571171));
#56973=CARTESIAN_POINT('Ctrl Pts',(-44.0364884211506,6.42690120872934,-24.0616242521564));
#56974=CARTESIAN_POINT('Ctrl Pts',(-43.5837431671894,7.67452928138004,-23.7650100449585));
#56975=CARTESIAN_POINT('Ctrl Pts',(-43.1335328486735,8.92374576231794,-23.4666708399978));
#56976=CARTESIAN_POINT('Ctrl Pts',(-43.7774989443756,5.08577719072335,-25.1469769549528));
#56977=CARTESIAN_POINT('Ctrl Pts',(-43.2443604259601,6.32042239432471,-24.933270807941));
#56978=CARTESIAN_POINT('Ctrl Pts',(-42.7146965077096,7.55714183044868,-24.7170780592635));
#56979=CARTESIAN_POINT('Ctrl Pts',(-42.181557989294,8.79178703405004,-24.5033719122517));
#56980=CARTESIAN_POINT('Ctrl Pts',(-42.7956488003254,4.84372654876611,-26.5306371507459));
#56981=CARTESIAN_POINT('Ctrl Pts',(-42.2045420756648,6.05642918637459,-26.3604342415932));
#56982=CARTESIAN_POINT('Ctrl Pts',(-41.6128293638815,7.2685808454858,-26.1904764286745));
#56983=CARTESIAN_POINT('Ctrl Pts',(-41.0217226392209,8.48128348309427,-26.0202735195218));
#56984=CARTESIAN_POINT('Ctrl Pts',(-41.9333999007591,4.68167633313014,-28.2389876838209));
#56985=CARTESIAN_POINT('Ctrl Pts',(-41.3748325386295,5.90841244052776,-28.0551638450349));
#56986=CARTESIAN_POINT('Ctrl Pts',(-40.8162962888588,7.13540891994494,-27.8716680562176));
#56987=CARTESIAN_POINT('Ctrl Pts',(-40.2577289267292,8.36214502734256,-27.6878442174315));
#56988=CARTESIAN_POINT('Ctrl Pts',(-41.5686373679341,4.67844271843895,-29.2605708183325));
#56989=CARTESIAN_POINT('Ctrl Pts',(-41.0326449179321,5.91472734108893,-29.0769717489468));
#56990=CARTESIAN_POINT('Ctrl Pts',(-40.4991794935331,7.15212798646055,-28.8912945519595));
#56991=CARTESIAN_POINT('Ctrl Pts',(-39.9631870435311,8.38841260911053,-28.7076954825739));
#56992=CARTESIAN_POINT('Ctrl Pts',(-41.4215456143024,4.68791021227308,-29.7512571116587));
#56993=CARTESIAN_POINT('Ctrl Pts',(-40.8936521308426,5.92796748849509,-29.5690857038871));
#56994=CARTESIAN_POINT('Ctrl Pts',(-40.3657586473827,7.16802476471709,-29.3869142961156));
#56995=CARTESIAN_POINT('Ctrl Pts',(-39.8378651639228,8.4080820409391,-29.204742888344));
#56996=CARTESIAN_POINT('',(-44.2496915258627,7.08033230160341,-23.4600000000002));
#56997=CARTESIAN_POINT('',(-44.2496915258627,7.08033230160347,-23.4600000000001));
#56998=CARTESIAN_POINT('',(-44.2496915258627,7.08033230160347,-23.4600000000001));
#56999=CARTESIAN_POINT('Ctrl Pts',(-57.8135230790975,6.69056632259502,-18.0349157107833));
#57000=CARTESIAN_POINT('Ctrl Pts',(-57.5247816344766,7.95941791373551,-17.6396385702623));
#57001=CARTESIAN_POINT('Ctrl Pts',(-57.2360401898557,9.22826950487599,-17.2443614297412));
#57002=CARTESIAN_POINT('Ctrl Pts',(-56.9472987452347,10.4971210960165,-16.8490842892202));
#57003=CARTESIAN_POINT('Ctrl Pts',(-57.1239745403965,6.58412560248485,-18.1969381440623));
#57004=CARTESIAN_POINT('Ctrl Pts',(-56.8293558324884,7.85914040842569,-17.8258953952808));
#57005=CARTESIAN_POINT('Ctrl Pts',(-56.5427656293713,9.13543238739557,-17.4526165469018));
#57006=CARTESIAN_POINT('Ctrl Pts',(-56.2481469214632,10.4104471933364,-17.0815737981202));
#57007=CARTESIAN_POINT('Ctrl Pts',(-55.0066008221098,6.23208146801642,-18.6635552175992));
#57008=CARTESIAN_POINT('Ctrl Pts',(-54.7175706740941,7.52475833001072,-18.3513974459225));
#57009=CARTESIAN_POINT('Ctrl Pts',(-54.423504213366,8.81665862928835,-18.0405169785343));
#57010=CARTESIAN_POINT('Ctrl Pts',(-54.1344740653502,10.1093354912827,-17.7283592068575));
#57011=CARTESIAN_POINT('Ctrl Pts',(-52.3438248091449,5.73435620824511,-19.2638310488358));
#57012=CARTESIAN_POINT('Ctrl Pts',(-52.0143059097852,7.02728121608903,-18.9991095830863));
#57013=CARTESIAN_POINT('Ctrl Pts',(-51.685864582759,8.32033229885559,-18.7344472086489));
#57014=CARTESIAN_POINT('Ctrl Pts',(-51.3563456833993,9.61325730669952,-18.4697257428994));
#57015=CARTESIAN_POINT('Ctrl Pts',(-50.0095424054025,5.30085549787886,-20.220604371564));
#57016=CARTESIAN_POINT('Ctrl Pts',(-49.643613283696,6.56955609994842,-19.8911383329522));
#57017=CARTESIAN_POINT('Ctrl Pts',(-49.2781182313849,7.83840233803338,-19.5613911754511));
#57018=CARTESIAN_POINT('Ctrl Pts',(-48.9121891096784,9.10710294010294,-19.2319251368394));
#57019=CARTESIAN_POINT('Ctrl Pts',(-48.2669654993335,5.10361702097977,-21.2264548583875));
#57020=CARTESIAN_POINT('Ctrl Pts',(-47.9253792124948,6.3492056772126,-20.7955041080243));
#57021=CARTESIAN_POINT('Ctrl Pts',(-47.5830128226939,7.59462899514417,-20.3653160983057));
#57022=CARTESIAN_POINT('Ctrl Pts',(-47.2414265358552,8.840217651377,-19.9343653479424));
#57023=CARTESIAN_POINT('Ctrl Pts',(-46.9594441235353,5.13430758608674,-22.1958151860038));
#57024=CARTESIAN_POINT('Ctrl Pts',(-46.648112214713,6.36337591783102,-21.7041817066266));
#57025=CARTESIAN_POINT('Ctrl Pts',(-46.3370798522678,7.59287361463498,-21.2113264208171));
#57026=CARTESIAN_POINT('Ctrl Pts',(-46.0257479434454,8.82194194637927,-20.7196929414398));
#57027=CARTESIAN_POINT('Ctrl Pts',(-45.8504881283735,5.21184561373662,-23.1088853518396));
#57028=CARTESIAN_POINT('Ctrl Pts',(-45.5253385580089,6.44309869251224,-22.6308162647746));
#57029=CARTESIAN_POINT('Ctrl Pts',(-45.2000143339031,7.67400918968744,-22.1535563605875));
#57030=CARTESIAN_POINT('Ctrl Pts',(-44.8748647635386,8.90526226846306,-21.6754872735224));
#57031=CARTESIAN_POINT('Ctrl Pts',(-45.2012130342128,5.23387305606066,-23.6826188427425));
#57032=CARTESIAN_POINT('Ctrl Pts',(-44.8305825688381,6.47688655683838,-23.2691414457344));
#57033=CARTESIAN_POINT('Ctrl Pts',(-44.458100546266,7.72159300799202,-22.8543779660973));
#57034=CARTESIAN_POINT('Ctrl Pts',(-44.0874700808914,8.96460650876973,-22.4409005690892));
#57035=CARTESIAN_POINT('Ctrl Pts',(-44.8643748763769,5.20597739807172,-23.9801519722228));
#57036=CARTESIAN_POINT('Ctrl Pts',(-44.4545859760341,6.45554733375955,-23.633383990741));
#57037=CARTESIAN_POINT('Ctrl Pts',(-44.0447970756913,7.70511726944739,-23.2866160092593));
#57038=CARTESIAN_POINT('Ctrl Pts',(-43.6350081753485,8.95468720513522,-22.9398480277775));
#57039=CARTESIAN_POINT('',(-57.3804109121661,8.59384370930575,-17.4420000000018));
#57040=CARTESIAN_POINT('',(-57.3804109121661,8.59384370930575,-17.4420000000018));
#57041=CARTESIAN_POINT('',(-57.3804109121661,8.59384370930575,-17.4420000000018));
#57042=CARTESIAN_POINT('Ctrl Pts',(-70.7282577522101,8.51486331985853,-11.892519184563));
#57043=CARTESIAN_POINT('Ctrl Pts',(-70.3600859174011,9.78627568391473,-11.5801730615225));
#57044=CARTESIAN_POINT('Ctrl Pts',(-69.9919140825922,11.0576880479709,-11.267826938482));
#57045=CARTESIAN_POINT('Ctrl Pts',(-69.6237422477832,12.3291004120271,-10.9554808154416));
#57046=CARTESIAN_POINT('Ctrl Pts',(-70.1991067619348,8.44172633189886,-12.218539623772));
#57047=CARTESIAN_POINT('Ctrl Pts',(-69.8208712427477,9.71815881129524,-11.9344438903904));
#57048=CARTESIAN_POINT('Ctrl Pts',(-69.4401822671779,10.9919767410639,-11.6547369719342));
#57049=CARTESIAN_POINT('Ctrl Pts',(-69.0619467479908,12.2684092204603,-11.3706412385527));
#57050=CARTESIAN_POINT('Ctrl Pts',(-68.595429397507,8.158930957405,-13.1757731414385));
#57051=CARTESIAN_POINT('Ctrl Pts',(-68.1715348548732,9.43443402361281,-12.9743515055776));
#57052=CARTESIAN_POINT('Ctrl Pts',(-67.7496672765525,10.7117699027939,-12.7692002791116));
#57053=CARTESIAN_POINT('Ctrl Pts',(-67.3257727339187,11.9872729690017,-12.5677786432507));
#57054=CARTESIAN_POINT('Ctrl Pts',(-66.4080850486133,7.61830551402404,-14.5220628619485));
#57055=CARTESIAN_POINT('Ctrl Pts',(-65.9863449158698,8.88672644030649,-14.2505530903174));
#57056=CARTESIAN_POINT('Ctrl Pts',(-65.5646075215418,10.1549810775789,-13.9790299757529));
#57057=CARTESIAN_POINT('Ctrl Pts',(-65.1428673887983,11.4234020038613,-13.7075202041218));
#57058=CARTESIAN_POINT('Ctrl Pts',(-63.7670026279933,7.28205441226018,-15.9847718406443));
#57059=CARTESIAN_POINT('Ctrl Pts',(-63.433848092195,8.52888773018001,-15.5476019176397));
#57060=CARTESIAN_POINT('Ctrl Pts',(-63.0999806953316,9.77527366757043,-15.1117880187483));
#57061=CARTESIAN_POINT('Ctrl Pts',(-62.7668261595333,11.0221069854903,-14.6746180957437));
#57062=CARTESIAN_POINT('Ctrl Pts',(-61.8892806965024,7.15471518367529,-16.8453028714865));
#57063=CARTESIAN_POINT('Ctrl Pts',(-61.6026532538942,8.38492602600039,-16.3432643430782));
#57064=CARTESIAN_POINT('Ctrl Pts',(-61.3170127161816,9.61579870788819,-15.8399025257027));
#57065=CARTESIAN_POINT('Ctrl Pts',(-61.0303852735734,10.8460095502133,-15.3378639972945));
#57066=CARTESIAN_POINT('Ctrl Pts',(-59.9765401917668,7.00460230079879,-17.5365065043827));
#57067=CARTESIAN_POINT('Ctrl Pts',(-59.7021139192336,8.24020918624605,-17.0371230534497));
#57068=CARTESIAN_POINT('Ctrl Pts',(-59.4266777566838,9.47499348818355,-16.5384607326821));
#57069=CARTESIAN_POINT('Ctrl Pts',(-59.1522514841506,10.7106003736308,-16.0390772817491));
#57070=CARTESIAN_POINT('Ctrl Pts',(-58.5497235666632,6.81245518627654,-17.8884040415039));
#57071=CARTESIAN_POINT('Ctrl Pts',(-58.2653553289422,8.06852593330302,-17.4497909528517));
#57072=CARTESIAN_POINT('Ctrl Pts',(-57.9817716639733,9.32584916951929,-17.0119688327944));
#57073=CARTESIAN_POINT('Ctrl Pts',(-57.6974034262523,10.5819199165458,-16.5733557441422));
#57074=CARTESIAN_POINT('Ctrl Pts',(-57.8135230790975,6.69056632259502,-18.0349157107833));
#57075=CARTESIAN_POINT('Ctrl Pts',(-57.5247816344766,7.95941791373551,-17.6396385702623));
#57076=CARTESIAN_POINT('Ctrl Pts',(-57.2360401898557,9.22826950487599,-17.2443614297412));
#57077=CARTESIAN_POINT('Ctrl Pts',(-56.9472987452347,10.4971210960165,-16.8490842892202));
#57078=CARTESIAN_POINT('',(-70.1759999999962,10.4219818659442,-11.4240000000019));
#57079=CARTESIAN_POINT('',(-70.1759999999966,10.4219818659428,-11.4240000000023));
#57080=CARTESIAN_POINT('',(-70.1759999999966,10.4219818659428,-11.4240000000023));
#57081=CARTESIAN_POINT('Ctrl Pts',(-77.5415210531587,9.45904311830585,-5.6796370336054));
#57082=CARTESIAN_POINT('Ctrl Pts',(-77.0327642242293,10.707186890519,-5.4971857604248));
#57083=CARTESIAN_POINT('Ctrl Pts',(-76.5240071582721,11.95533075251,-5.31473468722646));
#57084=CARTESIAN_POINT('Ctrl Pts',(-76.0152503292933,13.2034745247418,-5.13228341408748));
#57085=CARTESIAN_POINT('Ctrl Pts',(-77.1255245937012,9.37017154437904,-6.23165809536591));
#57086=CARTESIAN_POINT('Ctrl Pts',(-76.6182066545349,10.6210013196209,-6.06058457490718));
#57087=CARTESIAN_POINT('Ctrl Pts',(-76.1128620314122,11.8710836770426,-5.8878461381967));
#57088=CARTESIAN_POINT('Ctrl Pts',(-75.6055445028749,13.1219132967538,-5.71677227128412));
#57089=CARTESIAN_POINT('Ctrl Pts',(-76.405465217238,9.19639822407867,-7.09347041402827));
#57090=CARTESIAN_POINT('Ctrl Pts',(-75.9110410562668,10.4500649957193,-6.91088111986312));
#57091=CARTESIAN_POINT('Ctrl Pts',(-75.4159945623941,11.7038171731561,-6.72934984943679));
#57092=CARTESIAN_POINT('Ctrl Pts',(-74.9215702719211,12.9574839625689,-6.54676077543671));
#57093=CARTESIAN_POINT('Ctrl Pts',(-74.9141341563532,8.89641968768657,-8.65752098839668));
#57094=CARTESIAN_POINT('Ctrl Pts',(-74.4693520068755,10.1574090917317,-8.39661857717499));
#57095=CARTESIAN_POINT('Ctrl Pts',(-74.0250205308659,11.4188757945292,-8.13395067151794));
#57096=CARTESIAN_POINT('Ctrl Pts',(-73.5802384751692,12.6798652978959,-7.873047892913));
#57097=CARTESIAN_POINT('Ctrl Pts',(-72.9631668562262,8.69637264444927,-10.4087281112213));
#57098=CARTESIAN_POINT('Ctrl Pts',(-72.599764363485,9.95227518704734,-10.0271076573509));
#57099=CARTESIAN_POINT('Ctrl Pts',(-72.236097993674,11.2068584385996,-9.64834004665345));
#57100=CARTESIAN_POINT('Ctrl Pts',(-71.8726954460223,12.4627607066652,-9.2667201864336));
#57101=CARTESIAN_POINT('Ctrl Pts',(-71.5045506975364,8.62838606863837,-11.4414060938779));
#57102=CARTESIAN_POINT('Ctrl Pts',(-71.1537252528359,9.88821257086177,-11.0687855431255));
#57103=CARTESIAN_POINT('Ctrl Pts',(-70.8024466765253,11.1521393493876,-10.6895493100031));
#57104=CARTESIAN_POINT('Ctrl Pts',(-70.4516211375321,12.411966704841,-10.3169273825877));
#57105=CARTESIAN_POINT('Ctrl Pts',(-70.7282794573195,8.51445269903683,-11.8926709016604));
#57106=CARTESIAN_POINT('Ctrl Pts',(-70.3600672197069,9.78599878287807,-11.5802995099963));
#57107=CARTESIAN_POINT('Ctrl Pts',(-69.9918550365244,11.057544374204,-11.2679289129904));
#57108=CARTESIAN_POINT('Ctrl Pts',(-69.623642798923,12.3290904579427,-10.9555575214917));
#57109=CARTESIAN_POINT('',(-76.7782566939679,11.3314434017562,-5.40599999999698));
#57110=CARTESIAN_POINT('Ctrl Pts',(-79.5980561168786,9.7948810259695,-1.92025417907612));
#57111=CARTESIAN_POINT('Ctrl Pts',(-79.0286226813552,11.015051365124,-1.72806356741562));
#57112=CARTESIAN_POINT('Ctrl Pts',(-78.4591892458318,12.2352217042785,-1.53587295575512));
#57113=CARTESIAN_POINT('Ctrl Pts',(-77.8897558103085,13.455392043433,-1.34368234409463));
#57114=CARTESIAN_POINT('Ctrl Pts',(-79.3926541200977,9.78652201900712,-2.47576181499884));
#57115=CARTESIAN_POINT('Ctrl Pts',(-78.8328950227455,11.0133203526859,-2.29743332344463));
#57116=CARTESIAN_POINT('Ctrl Pts',(-78.273415546693,12.240356547761,-2.11844736719906));
#57117=CARTESIAN_POINT('Ctrl Pts',(-77.713656387765,13.46715482906,-1.94011902042602));
#57118=CARTESIAN_POINT('Ctrl Pts',(-78.8071962567564,9.7034726253451,-3.78882461998114));
#57119=CARTESIAN_POINT('Ctrl Pts',(-78.2719624773854,10.9425576600723,-3.61894133239815));
#57120=CARTESIAN_POINT('Ctrl Pts',(-77.7366705145668,12.1816470179848,-3.44939658013833));
#57121=CARTESIAN_POINT('Ctrl Pts',(-77.2014367480084,13.4207320517599,-3.27951321800603));
#57122=CARTESIAN_POINT('Ctrl Pts',(-78.0251745283461,9.56134461172776,-5.02766395488251));
#57123=CARTESIAN_POINT('Ctrl Pts',(-77.5136242019621,10.8076044886706,-4.83982958167015));
#57124=CARTESIAN_POINT('Ctrl Pts',(-77.0020491726152,12.0537106468992,-4.65168259079091));
#57125=CARTESIAN_POINT('Ctrl Pts',(-76.4904988516711,13.2999705576926,-4.46384828642048));
#57126=CARTESIAN_POINT('Ctrl Pts',(-77.5413122691002,9.45942207531784,-5.67964638243143));
#57127=CARTESIAN_POINT('Ctrl Pts',(-77.0325525411905,10.7075737063638,-5.4971953741327));
#57128=CARTESIAN_POINT('Ctrl Pts',(-76.5237928132806,11.9557253374098,-5.31474436583398));
#57129=CARTESIAN_POINT('Ctrl Pts',(-76.0150330853708,13.2038769684557,-5.13229335753524));
#57130=CARTESIAN_POINT('',(-78.744,11.6249350354095,-1.632));
#57131=CARTESIAN_POINT('Ctrl Pts',(-23.8932545728999,0.740547902948747,
-53.9987504226491));
#57132=CARTESIAN_POINT('Ctrl Pts',(-23.86567132551,2.06698974342288,-53.6996164276723));
#57133=CARTESIAN_POINT('Ctrl Pts',(-23.8380880426163,3.39343157051117,-53.4004823892113));
#57134=CARTESIAN_POINT('Ctrl Pts',(-23.8105047952247,4.71987341098465,-53.1013483942324));
#57135=CARTESIAN_POINT('Ctrl Pts',(-23.8111491297826,0.66280895354329,-53.6616057058667));
#57136=CARTESIAN_POINT('Ctrl Pts',(-23.7899322073168,1.99428207452091,-53.3842279343313));
#57137=CARTESIAN_POINT('Ctrl Pts',(-23.7689959243087,3.32586100308869,-53.107193880104));
#57138=CARTESIAN_POINT('Ctrl Pts',(-23.7477790154882,4.65733412921086,-52.8298161252807));
#57139=CARTESIAN_POINT('Ctrl Pts',(-23.5120480269356,0.444631858653941,
-52.5958478954493));
#57140=CARTESIAN_POINT('Ctrl Pts',(-23.5131370234285,1.78958247655091,-52.3846028150775));
#57141=CARTESIAN_POINT('Ctrl Pts',(-23.5140290283712,3.13446261342227,-52.1731322226411));
#57142=CARTESIAN_POINT('Ctrl Pts',(-23.5151180152861,4.47941322789233,-51.9618871313045));
#57143=CARTESIAN_POINT('Ctrl Pts',(-22.9082077797905,0.265131218620393,
-51.1308970104399));
#57144=CARTESIAN_POINT('Ctrl Pts',(-22.9352266775722,1.61785129599896,-50.9898559415293));
#57145=CARTESIAN_POINT('Ctrl Pts',(-22.9623772841048,2.97056451761134,-50.8489070392546));
#57146=CARTESIAN_POINT('Ctrl Pts',(-22.9893961882904,4.32328459465657,-50.7078659748253));
#57147=CARTESIAN_POINT('Ctrl Pts',(-21.9019816170089,0.165924669481705,
-49.7679496219043));
#57148=CARTESIAN_POINT('Ctrl Pts',(-21.9246701219479,1.52140639652562,-49.6589009921318));
#57149=CARTESIAN_POINT('Ctrl Pts',(-21.947364036065,2.87689968849961,-49.5498132146386));
#57150=CARTESIAN_POINT('Ctrl Pts',(-21.9700525412669,4.23238141610583,-49.4407645829627));
#57151=CARTESIAN_POINT('Ctrl Pts',(-20.8891826568043,0.111651161782249,
-48.9120914269852));
#57152=CARTESIAN_POINT('Ctrl Pts',(-20.8974190589084,1.46770925485864,-48.8080765082637));
#57153=CARTESIAN_POINT('Ctrl Pts',(-20.9056860401831,2.82376475946175,-48.7041166196569));
#57154=CARTESIAN_POINT('Ctrl Pts',(-20.9139224437741,4.17982285241228,-48.6001017036111));
#57155=CARTESIAN_POINT('Ctrl Pts',(-19.7609227539775,0.06610415987474,-48.291627810693));
#57156=CARTESIAN_POINT('Ctrl Pts',(-19.7587290709853,1.42205329907346,-48.1863874960513));
#57157=CARTESIAN_POINT('Ctrl Pts',(-19.7564713684224,2.77801680439355,-48.081155633946));
#57158=CARTESIAN_POINT('Ctrl Pts',(-19.7542776823175,4.13396594429077,-47.9759153197152));
#57159=CARTESIAN_POINT('Ctrl Pts',(-18.7367225861336,0.0329100024412727,
-47.8927011046375));
#57160=CARTESIAN_POINT('Ctrl Pts',(-18.7339401998428,1.3890343296589,-47.7896347298988));
#57161=CARTESIAN_POINT('Ctrl Pts',(-18.7313776034358,2.74516423171156,-47.6867008588423));
#57162=CARTESIAN_POINT('Ctrl Pts',(-18.7285952278316,4.10128855920025,-47.5836344905461));
#57163=CARTESIAN_POINT('Ctrl Pts',(-18.0840673956984,0.0167299223542211,
-47.6824848396237));
#57164=CARTESIAN_POINT('Ctrl Pts',(-18.0827609388197,1.37305600404991,-47.5821464675806));
#57165=CARTESIAN_POINT('Ctrl Pts',(-18.081454453813,2.7293820850321,-47.4818080785799));
#57166=CARTESIAN_POINT('Ctrl Pts',(-18.0801479969329,4.08570816672776,-47.3814697065359));
#57167=CARTESIAN_POINT('',(-18.0821908984155,2.05127053807155,-47.5319999999985));
#57168=CARTESIAN_POINT('',(-18.0821908984155,2.05127053807155,-47.5319999999985));
#57169=CARTESIAN_POINT('',(-23.8518695172951,2.73025015572333,-53.5499999999992));
#57170=CARTESIAN_POINT('',(-18.0821908984155,2.05127053807155,-47.5319999999985));
#57171=CARTESIAN_POINT('Ctrl Pts',(-24.7799130650367,2.95812473554076,-60.3565443657526));
#57172=CARTESIAN_POINT('Ctrl Pts',(-24.6861686425761,4.20890666796298,-59.8308481219162));
#57173=CARTESIAN_POINT('Ctrl Pts',(-24.5924242201155,5.45968860038519,-59.3051518780799));
#57174=CARTESIAN_POINT('Ctrl Pts',(-24.4986797976549,6.71047053280741,-58.7794556342435));
#57175=CARTESIAN_POINT('Ctrl Pts',(-24.7093254167293,2.61894304809241,-59.562121477931));
#57176=CARTESIAN_POINT('Ctrl Pts',(-24.6146095582202,3.8738857913977,-59.0466983423777));
#57177=CARTESIAN_POINT('Ctrl Pts',(-24.5199709784907,5.12912618706156,-58.5313692759599));
#57178=CARTESIAN_POINT('Ctrl Pts',(-24.4252551199817,6.38406893036685,-58.0159461404066));
#57179=CARTESIAN_POINT('Ctrl Pts',(-24.5694830832048,2.04316650995158,-58.1763047923767));
#57180=CARTESIAN_POINT('Ctrl Pts',(-24.4795102446963,3.31055333878821,-57.6893014217856));
#57181=CARTESIAN_POINT('Ctrl Pts',(-24.3895173433111,4.5779209632356,-57.2023296900593));
#57182=CARTESIAN_POINT('Ctrl Pts',(-24.2995445048026,5.84530779207223,-56.7153263194681));
#57183=CARTESIAN_POINT('Ctrl Pts',(-24.3518230181499,1.42202438632593,-56.4243962709067));
#57184=CARTESIAN_POINT('Ctrl Pts',(-24.2821550992614,2.71319822602082,-56.0014370835227));
#57185=CARTESIAN_POINT('Ctrl Pts',(-24.212420350588,4.00418313586032,-55.5780865162234));
#57186=CARTESIAN_POINT('Ctrl Pts',(-24.1427524316995,5.29535697555521,-55.1551273288394));
#57187=CARTESIAN_POINT('Ctrl Pts',(-24.1714172775178,1.07110956737089,-55.2893749713734));
#57188=CARTESIAN_POINT('Ctrl Pts',(-24.1195415474074,2.37885367803318,-54.9184414382784));
#57189=CARTESIAN_POINT('Ctrl Pts',(-24.0676400333205,3.68664518346435,-54.5475126821782));
#57190=CARTESIAN_POINT('Ctrl Pts',(-24.0157643032102,4.99438929412664,-54.1765791490832));
#57191=CARTESIAN_POINT('Ctrl Pts',(-24.0036588764749,0.844289079598309,
-54.4481403827476));
#57192=CARTESIAN_POINT('Ctrl Pts',(-23.9673653219391,2.16453830185569,-54.1222935195884));
#57193=CARTESIAN_POINT('Ctrl Pts',(-23.9311137308229,3.48457569165273,-53.7961224777469));
#57194=CARTESIAN_POINT('Ctrl Pts',(-23.8948201762871,4.80482491391012,-53.4702756145878));
#57195=CARTESIAN_POINT('Ctrl Pts',(-23.8932421744747,0.740634811882228,
-53.9986859556407));
#57196=CARTESIAN_POINT('Ctrl Pts',(-23.8656604030216,2.06704504110963,-53.699561985213));
#57197=CARTESIAN_POINT('Ctrl Pts',(-23.8380786315686,3.39345527033703,-53.4004380147853));
#57198=CARTESIAN_POINT('Ctrl Pts',(-23.8104968601155,4.71986549956443,-53.1013140443576));
#57199=CARTESIAN_POINT('',(-24.6392964313458,4.83429763417409,-59.5679999999981));
#57200=CARTESIAN_POINT('Ctrl Pts',(-24.8514816439886,6.03933586362476,-66.5177940910004));
#57201=CARTESIAN_POINT('Ctrl Pts',(-24.8457871534356,7.24924543830288,-65.8966616404837));
#57202=CARTESIAN_POINT('Ctrl Pts',(-24.8400921747285,8.45915509270137,-65.275529378494));
#57203=CARTESIAN_POINT('Ctrl Pts',(-24.8343976842069,9.66906466737436,-64.6543969279651));
#57204=CARTESIAN_POINT('Ctrl Pts',(-24.9519005131634,5.40013434801617,-65.2717689951452));
#57205=CARTESIAN_POINT('Ctrl Pts',(-24.9326786072616,6.59873041285434,-64.6288206915467));
#57206=CARTESIAN_POINT('Ctrl Pts',(-24.9184337609038,7.79651367564351,-63.9839502278183));
#57207=CARTESIAN_POINT('Ctrl Pts',(-24.8992115344816,8.99510979282575,-63.341002048006));
#57208=CARTESIAN_POINT('Ctrl Pts',(-24.955193873487,4.48978712507474,-63.5721497671119));
#57209=CARTESIAN_POINT('Ctrl Pts',(-24.8978913410139,5.69561205548002,-62.9450648497406));
#57210=CARTESIAN_POINT('Ctrl Pts',(-24.840394330803,6.90143304615417,-62.318020459864));
#57211=CARTESIAN_POINT('Ctrl Pts',(-24.7830918108543,8.10725797681316,-61.6909355398828));
#57212=CARTESIAN_POINT('Ctrl Pts',(-24.9193282160013,4.02246798717194,-62.6314379535427));
#57213=CARTESIAN_POINT('Ctrl Pts',(-24.8479165191087,5.2381550017438,-62.0258687577014));
#57214=CARTESIAN_POINT('Ctrl Pts',(-24.7768538140445,6.45354203486205,-61.4196009992347));
#57215=CARTESIAN_POINT('Ctrl Pts',(-24.7054420946769,7.66922906875258,-60.8140318483805));
#57216=CARTESIAN_POINT('Ctrl Pts',(-24.9088241241943,3.89449030749864,-62.3747837256354));
#57217=CARTESIAN_POINT('Ctrl Pts',(-24.8333191742452,5.11298267792579,-61.7753555460744));
#57218=CARTESIAN_POINT('Ctrl Pts',(-24.7581355545957,6.33163360070118,-61.1762619544598));
#57219=CARTESIAN_POINT('Ctrl Pts',(-24.682630583953,7.55012596091763,-60.5768337533516));
#57220=CARTESIAN_POINT('Ctrl Pts',(-24.9003852832803,3.80179791434547,-62.1865158010774));
#57221=CARTESIAN_POINT('Ctrl Pts',(-24.8221913397055,5.02260346864682,-61.592168571107));
#57222=CARTESIAN_POINT('Ctrl Pts',(-24.7442452372017,6.24340817620379,-60.9977988992182));
#57223=CARTESIAN_POINT('Ctrl Pts',(-24.666051277666,7.46421373055968,-60.403451670693));
#57224=CARTESIAN_POINT('Ctrl Pts',(-24.8848681816847,3.64819007810987,-61.8717738157264));
#57225=CARTESIAN_POINT('Ctrl Pts',(-24.802362419227,4.87306103722246,-61.2863881627958));
#57226=CARTESIAN_POINT('Ctrl Pts',(-24.7201086021799,6.09797862128327,-60.7010879047467));
#57227=CARTESIAN_POINT('Ctrl Pts',(-24.637602823497,7.32284957739323,-60.1157022463168));
#57228=CARTESIAN_POINT('Ctrl Pts',(-24.8483417886798,3.34833875688338,-61.2421817255175));
#57229=CARTESIAN_POINT('Ctrl Pts',(-24.758735472489,4.58246016741107,-60.6774045777714));
#57230=CARTESIAN_POINT('Ctrl Pts',(-24.6692623550833,5.81657910544939,-60.112615896231));
#57231=CARTESIAN_POINT('Ctrl Pts',(-24.5796560303146,7.05070051613632,-59.5478387492278));
#57232=CARTESIAN_POINT('Ctrl Pts',(-24.8095494386071,3.11146053772572,-60.716090603378));
#57233=CARTESIAN_POINT('Ctrl Pts',(-24.7166187762756,4.35508116577155,-60.173124017711));
#57234=CARTESIAN_POINT('Ctrl Pts',(-24.6236575971476,5.59875733363374,-59.6302142613489));
#57235=CARTESIAN_POINT('Ctrl Pts',(-24.5307269367814,6.84237795810284,-59.0872476720221));
#57236=CARTESIAN_POINT('Ctrl Pts',(-24.779910160927,2.95810970987412,-60.3565091331962));
#57237=CARTESIAN_POINT('Ctrl Pts',(-24.6861626398759,4.20893262287472,-59.8307976527483));
#57238=CARTESIAN_POINT('Ctrl Pts',(-24.5924151218147,5.45975553043318,-59.3050861667321));
#57239=CARTESIAN_POINT('Ctrl Pts',(-24.4986676007634,6.71057844343413,-58.7793746862846));
#57240=CARTESIAN_POINT('',(-24.8429480415422,7.85407743444482,-65.5860000000009));
#57241=CARTESIAN_POINT('Ctrl Pts',(-23.6734819284749,9.24326495191836,-72.5612011682599));
#57242=CARTESIAN_POINT('Ctrl Pts',(-23.6736392512832,10.4442582200649,-71.9230670560889));
#57243=CARTESIAN_POINT('Ctrl Pts',(-23.6737965740915,11.6452514882115,-71.284932943918));
#57244=CARTESIAN_POINT('Ctrl Pts',(-23.6739538968997,12.846244756358,-70.6467988317471));
#57245=CARTESIAN_POINT('Ctrl Pts',(-23.7649042668809,9.0816244028814,-72.257009894464));
#57246=CARTESIAN_POINT('Ctrl Pts',(-23.7650247809087,10.2820560268017,-71.6178191935096));
#57247=CARTESIAN_POINT('Ctrl Pts',(-23.7651416433926,11.482505712744,-70.9786611152447));
#57248=CARTESIAN_POINT('Ctrl Pts',(-23.7652621574204,12.6829373366643,-70.3394704142904));
#57249=CARTESIAN_POINT('Ctrl Pts',(-24.026191926212,8.5949110125477,-71.3440354252429));
#57250=CARTESIAN_POINT('Ctrl Pts',(-24.026490117635,9.79400808195901,-70.7023415912864));
#57251=CARTESIAN_POINT('Ctrl Pts',(-24.0267840819686,10.9930931283153,-70.0606258912063));
#57252=CARTESIAN_POINT('Ctrl Pts',(-24.0270822733915,12.1921901977266,-69.4189320572497));
#57253=CARTESIAN_POINT('Ctrl Pts',(-24.3676733444401,7.85042242107576,-69.9555629639005));
#57254=CARTESIAN_POINT('Ctrl Pts',(-24.3702647663561,9.04908783302253,-69.3130728922147));
#57255=CARTESIAN_POINT('Ctrl Pts',(-24.3726957523222,10.2477966114829,-68.6706626248404));
#57256=CARTESIAN_POINT('Ctrl Pts',(-24.3752871742381,11.4464620234297,-68.0281725531546));
#57257=CARTESIAN_POINT('Ctrl Pts',(-24.6786062061593,6.94797749971677,-68.2666525661597));
#57258=CARTESIAN_POINT('Ctrl Pts',(-24.6833099022124,8.14979165663938,-67.6300522330398));
#57259=CARTESIAN_POINT('Ctrl Pts',(-24.6880297408764,9.35159646931981,-66.9934315143023));
#57260=CARTESIAN_POINT('Ctrl Pts',(-24.6927334369296,10.5534106262424,-66.3568311811825));
#57261=CARTESIAN_POINT('Ctrl Pts',(-24.8079585801581,6.32785027214234,-67.080190599109));
#57262=CARTESIAN_POINT('Ctrl Pts',(-24.8075961665432,7.53482759926113,-66.4533978140702));
#57263=CARTESIAN_POINT('Ctrl Pts',(-24.8067625026745,8.74190348924563,-65.8267881673147));
#57264=CARTESIAN_POINT('Ctrl Pts',(-24.8064000890597,9.94888081636442,-65.1999953822759));
#57265=CARTESIAN_POINT('Ctrl Pts',(-24.8514914924163,6.0392731730085,-66.5176718854411));
#57266=CARTESIAN_POINT('Ctrl Pts',(-24.8457958585002,7.24914268063271,-65.8965572951477));
#57267=CARTESIAN_POINT('Ctrl Pts',(-24.8401002245841,8.45901218825693,-65.2754427048542));
#57268=CARTESIAN_POINT('Ctrl Pts',(-24.834404590668,9.66888169588114,-64.6543281145607));
#57269=CARTESIAN_POINT('',(-23.6737179126873,11.0447548541382,-71.6040000000035));
#57270=CARTESIAN_POINT('Ctrl Pts',(-21.0430574415816,12.4421901739772,-78.5797217830362));
#57271=CARTESIAN_POINT('Ctrl Pts',(-21.042167498106,13.642998643172,-77.9412405943464));
#57272=CARTESIAN_POINT('Ctrl Pts',(-21.0412775546305,14.8438071123667,-77.3027594056566));
#57273=CARTESIAN_POINT('Ctrl Pts',(-21.040387611155,16.0446155815615,-76.6642782169667));
#57274=CARTESIAN_POINT('Ctrl Pts',(-21.3778021402842,12.1976961752275,-78.1194288669213));
#57275=CARTESIAN_POINT('Ctrl Pts',(-21.3769081685314,13.3985041597138,-77.4809467730066));
#57276=CARTESIAN_POINT('Ctrl Pts',(-21.3760224274111,14.5993118579,-76.8424641268745));
#57277=CARTESIAN_POINT('Ctrl Pts',(-21.3751284556584,15.8001198423863,-76.2039820329599));
#57278=CARTESIAN_POINT('Ctrl Pts',(-21.9881636463861,11.644899047288,-77.0789580092169));
#57279=CARTESIAN_POINT('Ctrl Pts',(-21.9873817766374,12.8457004437947,-76.4404633549307));
#57280=CARTESIAN_POINT('Ctrl Pts',(-21.986615227335,14.0465025180761,-75.8019699506747));
#57281=CARTESIAN_POINT('Ctrl Pts',(-21.9858333575863,15.2473039145829,-75.1634752963886));
#57282=CARTESIAN_POINT('Ctrl Pts',(-22.84310382117,10.6110321918245,-75.1338794942987));
#57283=CARTESIAN_POINT('Ctrl Pts',(-22.8428530090605,11.811809075809,-74.4953382081582));
#57284=CARTESIAN_POINT('Ctrl Pts',(-22.8426022779187,13.0125856498721,-73.8567963290241));
#57285=CARTESIAN_POINT('Ctrl Pts',(-22.8423514658093,14.2133625338566,-73.2182550428836));
#57286=CARTESIAN_POINT('Ctrl Pts',(-23.3878046917012,9.75120273870573,-73.5170894484657));
#57287=CARTESIAN_POINT('Ctrl Pts',(-23.3880652364971,10.9520370262507,-72.8786561872709));
#57288=CARTESIAN_POINT('Ctrl Pts',(-23.3883718428281,12.1528739545353,-72.2402278077585));
#57289=CARTESIAN_POINT('Ctrl Pts',(-23.3886323876239,13.3537082420802,-71.6017945465636));
#57290=CARTESIAN_POINT('Ctrl Pts',(-23.6734819284749,9.24326495191836,-72.5612011682599));
#57291=CARTESIAN_POINT('Ctrl Pts',(-23.6736392512832,10.4442582200649,-71.9230670560889));
#57292=CARTESIAN_POINT('Ctrl Pts',(-23.6737965740915,11.6452514882115,-71.284932943918));
#57293=CARTESIAN_POINT('Ctrl Pts',(-23.6739538968997,12.846244756358,-70.6467988317471));
#57294=CARTESIAN_POINT('',(-21.0417225263683,14.2434028777694,-77.6220000000015));
#57295=CARTESIAN_POINT('Ctrl Pts',(-20.809321916529,12.6047206302969,-78.8857217870086));
#57296=CARTESIAN_POINT('Ctrl Pts',(-20.808440638843,13.8055291044742,-78.2472405956695));
#57297=CARTESIAN_POINT('Ctrl Pts',(-20.807559361157,15.0063375786514,-77.6087594043305));
#57298=CARTESIAN_POINT('Ctrl Pts',(-20.806678083471,16.2071460528287,-76.9702782129914));
#57299=CARTESIAN_POINT('Ctrl Pts',(-20.8889387648524,12.5520952777272,-78.7866380007792));
#57300=CARTESIAN_POINT('Ctrl Pts',(-20.8880519500474,13.7529037487349,-78.1481568111254));
#57301=CARTESIAN_POINT('Ctrl Pts',(-20.8871651385933,14.953712219749,-77.5096756214682));
#57302=CARTESIAN_POINT('Ctrl Pts',(-20.8862783237883,16.1545206907567,-76.8711944318144));
#57303=CARTESIAN_POINT('Ctrl Pts',(-20.966829204766,12.4978666722846,-78.6845402972071));
#57304=CARTESIAN_POINT('Ctrl Pts',(-20.965939552898,13.6986751416463,-78.0460591084285));
#57305=CARTESIAN_POINT('Ctrl Pts',(-20.965049904181,14.8994836110143,-77.4075779196465));
#57306=CARTESIAN_POINT('Ctrl Pts',(-20.964160252313,16.1002920803761,-76.7690967308679));
#57307=CARTESIAN_POINT('Ctrl Pts',(-21.0430574415815,12.4421901739772,-78.5797217830362));
#57308=CARTESIAN_POINT('Ctrl Pts',(-21.042167498106,13.642998643172,-77.9412405943464));
#57309=CARTESIAN_POINT('Ctrl Pts',(-21.0412775546305,14.8438071123667,-77.3027594056565));
#57310=CARTESIAN_POINT('Ctrl Pts',(-21.040387611155,16.0446155815615,-76.6642782169667));
#57311=CARTESIAN_POINT('',(-20.808,14.4059333415628,-77.928));
#57312=CARTESIAN_POINT('Ctrl Pts',(23.6734819284753,9.2432649519181,-72.5612011682563));
#57313=CARTESIAN_POINT('Ctrl Pts',(23.6736392516143,10.4442607414065,-71.9230657163991));
#57314=CARTESIAN_POINT('Ctrl Pts',(23.6737965747534,11.6452565308947,-71.2849302645419));
#57315=CARTESIAN_POINT('Ctrl Pts',(23.6739538978923,12.8462523203831,-70.6467948126847));
#57316=CARTESIAN_POINT('Ctrl Pts',(23.5615106118548,9.44235138733137,-72.9358619934788));
#57317=CARTESIAN_POINT('Ctrl Pts',(23.5617208320191,10.6432845725721,-72.2976087481736));
#57318=CARTESIAN_POINT('Ctrl Pts',(23.5619117889063,11.8442196676616,-71.6593590410948));
#57319=CARTESIAN_POINT('Ctrl Pts',(23.5621220091515,13.0451528528943,-71.0211057957747));
#57320=CARTESIAN_POINT('Ctrl Pts',(23.2106747185919,10.0332017364569,-74.0473320232884));
#57321=CARTESIAN_POINT('Ctrl Pts',(23.2107881218931,11.2340121859773,-73.4088478072317));
#57322=CARTESIAN_POINT('Ctrl Pts',(23.2109141600603,12.4348203100041,-72.7703592264185));
#57323=CARTESIAN_POINT('Ctrl Pts',(23.2110275633084,13.6356307595342,-72.1318750103799));
#57324=CARTESIAN_POINT('Ctrl Pts',(22.4162563803382,11.1958361188247,-76.2337986537702));
#57325=CARTESIAN_POINT('Ctrl Pts',(22.4156559127772,12.396613745026,-75.5952528536972));
#57326=CARTESIAN_POINT('Ctrl Pts',(22.4150306235993,13.5973972303885,-74.9567180648474));
#57327=CARTESIAN_POINT('Ctrl Pts',(22.4144301561425,14.7981748565652,-74.3181722647281));
#57328=CARTESIAN_POINT('Ctrl Pts',(21.6377011779931,12.0078686581778,-77.7620529729162));
#57329=CARTESIAN_POINT('Ctrl Pts',(21.6367967414816,13.208683760128,-77.1235782253732));
#57330=CARTESIAN_POINT('Ctrl Pts',(21.6359289318972,14.4094834349257,-76.4850743279567));
#57331=CARTESIAN_POINT('Ctrl Pts',(21.6350244952319,15.6102985369408,-75.8465995805361));
#57332=CARTESIAN_POINT('Ctrl Pts',(21.0430574415837,12.442190173977,-78.5797217830346));
#57333=CARTESIAN_POINT('Ctrl Pts',(21.0421674962392,13.6430011641255,-77.9412392539299));
#57334=CARTESIAN_POINT('Ctrl Pts',(21.0412775508946,14.843812154274,-77.3027567248251));
#57335=CARTESIAN_POINT('Ctrl Pts',(21.0403876055502,16.0446231444226,-76.6642741957204));
#57336=CARTESIAN_POINT('',(21.0417225263694,14.2434028777691,-77.6219999999999));
#57337=CARTESIAN_POINT('',(23.6737179126884,11.0447548541379,-71.6039999999999));
#57338=CARTESIAN_POINT('Ctrl Pts',(24.8514914924156,6.03927317300853,-66.5176718854405));
#57339=CARTESIAN_POINT('Ctrl Pts',(24.8457958585,7.24914268063269,-65.8965572951469));
#57340=CARTESIAN_POINT('Ctrl Pts',(24.8401002245844,8.45901218825685,-65.2754427048533));
#57341=CARTESIAN_POINT('Ctrl Pts',(24.8344045906688,9.66888169588101,-64.6543281145597));
#57342=CARTESIAN_POINT('Ctrl Pts',(24.7857582030557,6.47501525815644,-67.3670569474013));
#57343=CARTESIAN_POINT('Ctrl Pts',(24.7880943840847,7.68057023012441,-66.73749583644));
#57344=CARTESIAN_POINT('Ctrl Pts',(24.7897825180673,8.88611633876867,-66.1078291491835));
#57345=CARTESIAN_POINT('Ctrl Pts',(24.7921186990963,10.0916713107366,-65.4782680382222));
#57346=CARTESIAN_POINT('Ctrl Pts',(24.550338270654,7.4900405053709,-69.2911770386706));
#57347=CARTESIAN_POINT('Ctrl Pts',(24.5559989571534,8.68780867473477,-68.6470021875378));
#57348=CARTESIAN_POINT('Ctrl Pts',(24.5610779768368,9.88549730957243,-68.0027096389216));
#57349=CARTESIAN_POINT('Ctrl Pts',(24.5667386633363,11.0832654789363,-67.3585347877888));
#57350=CARTESIAN_POINT('Ctrl Pts',(24.0160972599616,8.6374991045811,-71.4212107028606));
#57351=CARTESIAN_POINT('Ctrl Pts',(24.0154309216262,9.83632107354304,-70.7789993845374));
#57352=CARTESIAN_POINT('Ctrl Pts',(24.0168080472231,11.0354101577888,-70.1372628915936));
#57353=CARTESIAN_POINT('Ctrl Pts',(24.0161417088878,12.2342321267508,-69.4950515732704));
#57354=CARTESIAN_POINT('Ctrl Pts',(23.6734819284753,9.2432649519181,-72.5612011682563));
#57355=CARTESIAN_POINT('Ctrl Pts',(23.673639251284,10.4442582200647,-71.9230670560853));
#57356=CARTESIAN_POINT('Ctrl Pts',(23.6737965740928,11.6452514882112,-71.2849329439144));
#57357=CARTESIAN_POINT('Ctrl Pts',(23.6739538969015,12.8462447563578,-70.6467988317435));
#57358=CARTESIAN_POINT('',(24.8429480415422,7.85407743444477,-65.5860000000001));
#57359=CARTESIAN_POINT('Ctrl Pts',(24.7799191277205,2.95792794530187,-60.3565375266123));
#57360=CARTESIAN_POINT('Ctrl Pts',(24.6861703694341,4.20876617277843,-59.8308217469595));
#57361=CARTESIAN_POINT('Ctrl Pts',(24.5924217855773,5.45960447146532,-59.3051063962421));
#57362=CARTESIAN_POINT('Ctrl Pts',(24.4986730273061,6.71044269894815,-58.7793906166268));
#57363=CARTESIAN_POINT('Ctrl Pts',(24.9089035260939,3.62528183199708,-61.9213719956554));
#57364=CARTESIAN_POINT('Ctrl Pts',(24.8198633370479,4.8453463929819,-61.3235933669262));
#57365=CARTESIAN_POINT('Ctrl Pts',(24.7272287916051,6.06394357005601,-60.7169759429534));
#57366=CARTESIAN_POINT('Ctrl Pts',(24.6381882876209,7.28400800246834,-60.1191965397671));
#57367=CARTESIAN_POINT('Ctrl Pts',(24.9834159830366,4.731838028036,-64.0136175321612));
#57368=CARTESIAN_POINT('Ctrl Pts',(24.9383372996939,5.93153728641096,-63.3748948329307));
#57369=CARTESIAN_POINT('Ctrl Pts',(24.8942407363303,7.13166149255805,-62.7389258132719));
#57370=CARTESIAN_POINT('Ctrl Pts',(24.8491621390411,8.33136078816702,-62.1002033553194));
#57371=CARTESIAN_POINT('Ctrl Pts',(24.9107202843689,5.66209961304811,-65.7828228049932));
#57372=CARTESIAN_POINT('Ctrl Pts',(24.8976557677923,6.8651069265034,-65.1478601922165));
#57373=CARTESIAN_POINT('Ctrl Pts',(24.8856952678506,8.06836234662063,-64.5146251843238));
#57374=CARTESIAN_POINT('Ctrl Pts',(24.8726308480082,9.27136968181508,-63.8796627229203));
#57375=CARTESIAN_POINT('Ctrl Pts',(24.8514884085996,6.03913854124118,-66.5178010814603));
#57376=CARTESIAN_POINT('Ctrl Pts',(24.8457930019507,7.24906150548085,-65.8966601719787));
#57377=CARTESIAN_POINT('Ctrl Pts',(24.8400975238651,8.45898445366638,-65.2755191507098));
#57378=CARTESIAN_POINT('Ctrl Pts',(24.8344021172099,9.66890741790464,-64.6543782412184));
#57379=CARTESIAN_POINT('',(24.639296431346,4.83429763417431,-59.5679999999998));
#57380=CARTESIAN_POINT('Ctrl Pts',(23.8932421744751,0.740634811882458,-53.9986859556419));
#57381=CARTESIAN_POINT('Ctrl Pts',(23.8656593284557,2.06709671711524,-53.6995503315557));
#57382=CARTESIAN_POINT('Ctrl Pts',(23.8380764824361,3.39355862234801,-53.4004147074695));
#57383=CARTESIAN_POINT('Ctrl Pts',(23.8104936364166,4.7200205275808,-53.1012790833832));
#57384=CARTESIAN_POINT('Ctrl Pts',(24.1789074622363,1.00880462386192,-55.1614948960392));
#57385=CARTESIAN_POINT('Ctrl Pts',(24.1277458282354,2.31879778942141,-54.7919563810276));
#57386=CARTESIAN_POINT('Ctrl Pts',(24.0798103811834,3.62982881878404,-54.4253709231687));
#57387=CARTESIAN_POINT('Ctrl Pts',(24.0286484958026,4.93982190347465,-54.0558321780592));
#57388=CARTESIAN_POINT('Ctrl Pts',(24.4015168304308,1.52786212045763,-56.7701588656369));
#57389=CARTESIAN_POINT('Ctrl Pts',(24.3255448890141,2.81314050207022,-56.3301388554163));
#57390=CARTESIAN_POINT('Ctrl Pts',(24.2496983734156,4.09850722836944,-55.8901826689679));
#57391=CARTESIAN_POINT('Ctrl Pts',(24.173726422226,5.38378560309834,-55.4501626537743));
#57392=CARTESIAN_POINT('Ctrl Pts',(24.6106655417996,2.23012064092564,-58.6108222610336));
#57393=CARTESIAN_POINT('Ctrl Pts',(24.5199407290614,3.49401760823125,-58.1162740526191));
#57394=CARTESIAN_POINT('Ctrl Pts',(24.4296363415329,4.75814275026669,-57.6224267085783));
#57395=CARTESIAN_POINT('Ctrl Pts',(24.3389114960358,6.02203969979325,-57.1278784455535));
#57396=CARTESIAN_POINT('Ctrl Pts',(24.6996147992407,2.59058304170841,-59.488342199932));
#57397=CARTESIAN_POINT('Ctrl Pts',(24.6057756690561,3.84681036908307,-58.9756997363143));
#57398=CARTESIAN_POINT('Ctrl Pts',(24.5118615880014,5.10287355736105,-58.4625429317005));
#57399=CARTESIAN_POINT('Ctrl Pts',(24.418022463657,6.35910089752518,-57.9499005081595));
#57400=CARTESIAN_POINT('Ctrl Pts',(24.7614059735443,2.86919605364059,-60.1482578252368));
#57401=CARTESIAN_POINT('Ctrl Pts',(24.667356476118,4.12105401998294,-59.6249836943641));
#57402=CARTESIAN_POINT('Ctrl Pts',(24.5734673948942,5.37318097339444,-59.1024871867851));
#57403=CARTESIAN_POINT('Ctrl Pts',(24.4794178849684,6.6250389187777,-58.5792129953211));
#57404=CARTESIAN_POINT('Ctrl Pts',(24.7799130650375,2.95812473554106,-60.3565443657544));
#57405=CARTESIAN_POINT('Ctrl Pts',(24.68616499036,4.2089553975436,-59.8308276411638));
#57406=CARTESIAN_POINT('Ctrl Pts',(24.5924169156826,5.45978605954612,-59.305110916573));
#57407=CARTESIAN_POINT('Ctrl Pts',(24.498668841005,6.71061672154866,-58.7793941919824));
#57408=CARTESIAN_POINT('',(23.8518695172954,2.73025015572356,-53.5500000000004));
#57409=CARTESIAN_POINT('Ctrl Pts',(18.0841396805929,0.0168146404897664,
-47.6825020134366));
#57410=CARTESIAN_POINT('Ctrl Pts',(18.0828330780895,1.3731194054854,-47.5821649137338));
#57411=CARTESIAN_POINT('Ctrl Pts',(18.081526479321,2.72942417022187,-47.4818278133018));
#57412=CARTESIAN_POINT('Ctrl Pts',(18.0802198768176,4.08572893521751,-47.3814907135991));
#57413=CARTESIAN_POINT('Ctrl Pts',(18.5443648070833,0.0282243501846493,
-47.8307394400169));
#57414=CARTESIAN_POINT('Ctrl Pts',(18.5421205699259,1.38438459857093,-47.7284998708658));
#57415=CARTESIAN_POINT('Ctrl Pts',(18.5397222302431,2.74055553971965,-47.6262903896664));
#57416=CARTESIAN_POINT('Ctrl Pts',(18.5374779933162,4.09671578808994,-47.5240508204702));
#57417=CARTESIAN_POINT('Ctrl Pts',(19.3713825374723,0.0528487038591615,
-48.1299992700489));
#57418=CARTESIAN_POINT('Ctrl Pts',(19.3683888317819,1.40882529369436,-48.0252908017089));
#57419=CARTESIAN_POINT('Ctrl Pts',(19.365563708298,2.76479677687121,-47.920635084255));
#57420=CARTESIAN_POINT('Ctrl Pts',(19.3625700023554,4.12077336671404,-47.8159266158361));
#57421=CARTESIAN_POINT('Ctrl Pts',(20.3970287176425,0.0913850843528481,
-48.6274441293917));
#57422=CARTESIAN_POINT('Ctrl Pts',(20.4001722793646,1.44737071048997,-48.5228840106449));
#57423=CARTESIAN_POINT('Ctrl Pts',(20.4031843891888,2.80336002413669,-48.4183208296279));
#57424=CARTESIAN_POINT('Ctrl Pts',(20.4063279511075,4.1593456502683,-48.3137607108857));
#57425=CARTESIAN_POINT('Ctrl Pts',(21.2030623279049,0.127765179000182,-49.1632061443352));
#57426=CARTESIAN_POINT('Ctrl Pts',(21.2157420402905,1.48366970427005,-49.0580958545386));
#57427=CARTESIAN_POINT('Ctrl Pts',(21.2284906751219,2.83956742651729,-48.9530453801162));
#57428=CARTESIAN_POINT('Ctrl Pts',(21.2411703874045,4.19547195179733,-48.8479350902301));
#57429=CARTESIAN_POINT('Ctrl Pts',(21.9415244226505,0.170818208138083,-49.8301345883609));
#57430=CARTESIAN_POINT('Ctrl Pts',(21.9642269284021,1.52612482082818,-49.7193172627231));
#57431=CARTESIAN_POINT('Ctrl Pts',(21.9868032115003,2.88143737386752,-49.6085370939327));
#57432=CARTESIAN_POINT('Ctrl Pts',(22.0095057174407,4.23674398654873,-49.4977197682393));
#57433=CARTESIAN_POINT('Ctrl Pts',(22.7299618914328,0.246693032010643,-50.877466594607));
#57434=CARTESIAN_POINT('Ctrl Pts',(22.7563638685511,1.59993105501455,-50.7426800809163));
#57435=CARTESIAN_POINT('Ctrl Pts',(22.7826599837655,2.95314572641759,-50.6077394381178));
#57436=CARTESIAN_POINT('Ctrl Pts',(22.8090619610422,4.30638374945642,-50.4729529246576));
#57437=CARTESIAN_POINT('Ctrl Pts',(23.4121500524248,0.405565211479381,-52.3094090691719));
#57438=CARTESIAN_POINT('Ctrl Pts',(23.4198394420821,1.75224322857291,-52.1135550169374));
#57439=CARTESIAN_POINT('Ctrl Pts',(23.427563745456,3.09892933740634,-51.9177173826107));
#57440=CARTESIAN_POINT('Ctrl Pts',(23.4352531350609,4.44560735448777,-51.7218633303516));
#57441=CARTESIAN_POINT('Ctrl Pts',(23.7490678075399,0.604114032031964,-53.4066787177267));
#57442=CARTESIAN_POINT('Ctrl Pts',(23.7328855382795,1.93947127745986,-53.1461836033946));
#57443=CARTESIAN_POINT('Ctrl Pts',(23.7165336536041,3.27471109737415,-52.8850050076064));
#57444=CARTESIAN_POINT('Ctrl Pts',(23.7003513845974,4.61006834297765,-52.6245098942964));
#57445=CARTESIAN_POINT('Ctrl Pts',(23.8932460088521,0.740622488142717,-53.9987038928088));
#57446=CARTESIAN_POINT('Ctrl Pts',(23.8656637224211,2.06704392239731,-53.6995764062096));
#57447=CARTESIAN_POINT('Ctrl Pts',(23.8380814401183,3.39346535950986,-53.4004489362454));
#57448=CARTESIAN_POINT('Ctrl Pts',(23.8104991536872,4.71988679376446,-53.1013214496463));
#57449=CARTESIAN_POINT('',(18.0821908984197,2.05127053807158,-47.5319999999999));
#57450=CARTESIAN_POINT('',(18.0821908984197,2.05127053807158,-47.5319999999999));
#57451=CARTESIAN_POINT('',(18.0821908984197,2.05127053807158,-47.5319999999999));
#57452=CARTESIAN_POINT('Ctrl Pts',(-3.2690524243696E-5,-0.0251265829928964,
-45.4192965823161));
#57453=CARTESIAN_POINT('Ctrl Pts',(-3.27354186043915E-5,1.33471801276171,
-45.4405652637787));
#57454=CARTESIAN_POINT('Ctrl Pts',(-3.27175351009904E-5,2.69456260844022,
-45.4618339363921));
#57455=CARTESIAN_POINT('Ctrl Pts',(-3.27624304691016E-5,4.05440720419482,
-45.4831026178549));
#57456=CARTESIAN_POINT('Ctrl Pts',(1.8682027887804,-0.0257296837108507,
-45.4578603912295));
#57457=CARTESIAN_POINT('Ctrl Pts',(1.87076844273175,1.33412472643363,-45.4782403258505));
#57458=CARTESIAN_POINT('Ctrl Pts',(1.86974641330836,2.69398348477606,-45.4991259855145));
#57459=CARTESIAN_POINT('Ctrl Pts',(1.87231212483236,4.05383789485077,-45.51950591202));
#57460=CARTESIAN_POINT('Ctrl Pts',(4.99153621662472,-0.0330411951959642,
-45.534798185463));
#57461=CARTESIAN_POINT('Ctrl Pts',(4.9932336251418,1.32683289940186,-45.5543492662237));
#57462=CARTESIAN_POINT('Ctrl Pts',(4.99497908362866,2.68670867600787,-45.5738691487411));
#57463=CARTESIAN_POINT('Ctrl Pts',(4.99667649137468,4.0465827705787,-45.5934202300024));
#57464=CARTESIAN_POINT('Ctrl Pts',(7.59438888123013,-0.0326758765092276,
-45.6867097257879));
#57465=CARTESIAN_POINT('Ctrl Pts',(7.59249880785721,1.32724755035341,-45.7021384549768));
#57466=CARTESIAN_POINT('Ctrl Pts',(7.59047347647672,2.68717345156613,-45.7176245959044));
#57467=CARTESIAN_POINT('Ctrl Pts',(7.58858340527433,4.04709687838906,-45.733053324172));
#57468=CARTESIAN_POINT('Ctrl Pts',(8.87729659300802,-0.0314509584309369,
-45.7887336658147));
#57469=CARTESIAN_POINT('Ctrl Pts',(8.87441777432724,1.3285062657543,-45.8007152975604));
#57470=CARTESIAN_POINT('Ctrl Pts',(8.87155087449128,2.68846580175383,-45.8126919130268));
#57471=CARTESIAN_POINT('Ctrl Pts',(8.86867205561924,4.04842302590197,-45.8246735448531));
#57472=CARTESIAN_POINT('Ctrl Pts',(10.1490597186576,-0.0297979816701636,
-45.9251950972821));
#57473=CARTESIAN_POINT('Ctrl Pts',(10.1465580226243,1.33020253676551,-45.9314329040811));
#57474=CARTESIAN_POINT('Ctrl Pts',(10.1440412110529,2.69020835929771,-45.9377490875431));
#57475=CARTESIAN_POINT('Ctrl Pts',(10.1415395152622,4.05020887764826,-45.9439868930844));
#57476=CARTESIAN_POINT('Ctrl Pts',(11.8978630897578,-0.0280707333736627,
-46.1680533783691));
#57477=CARTESIAN_POINT('Ctrl Pts',(11.8982432356438,1.33196096673256,-46.1620867040576));
#57478=CARTESIAN_POINT('Ctrl Pts',(11.898750185013,2.69199259656723,-46.1560178387715));
#57479=CARTESIAN_POINT('Ctrl Pts',(11.8991303288642,4.05202429667458,-46.1500511660999));
#57480=CARTESIAN_POINT('Ctrl Pts',(13.9971210552705,-0.0295760205187906,
-46.5641348045042));
#57481=CARTESIAN_POINT('Ctrl Pts',(14.0040786793423,1.33022743179417,-46.5331292464512));
#57482=CARTESIAN_POINT('Ctrl Pts',(14.0114201033648,2.69005785826174,-46.5023729377843));
#57483=CARTESIAN_POINT('Ctrl Pts',(14.0183777212778,4.04986131014184,-46.4713673757315));
#57484=CARTESIAN_POINT('Ctrl Pts',(16.2942313977893,-0.0209121707010144,
-47.1212911897684));
#57485=CARTESIAN_POINT('Ctrl Pts',(16.2992203099862,1.33750106368331,-47.0520421334878));
#57486=CARTESIAN_POINT('Ctrl Pts',(16.3037485306264,2.69589336048563,-46.9826958057665));
#57487=CARTESIAN_POINT('Ctrl Pts',(16.3087374502163,4.05430659520594,-46.9134467510469));
#57488=CARTESIAN_POINT('Ctrl Pts',(17.5354503382007,0.00240667102759995,
-47.4946713071985));
#57489=CARTESIAN_POINT('Ctrl Pts',(17.5350963620415,1.35941127856638,-47.4038531728718));
#57490=CARTESIAN_POINT('Ctrl Pts',(17.5354201549704,2.71645997318391,-47.3134407766488));
#57491=CARTESIAN_POINT('Ctrl Pts',(17.5350661679349,4.07346458001521,-47.222622635811));
#57492=CARTESIAN_POINT('Ctrl Pts',(18.0841700243305,0.0168314204591895,
-47.6825109969299));
#57493=CARTESIAN_POINT('Ctrl Pts',(18.0828633665264,1.37313536000937,-47.5821735769392));
#57494=CARTESIAN_POINT('Ctrl Pts',(18.0815566850005,2.72943929801651,-47.4818361427477));
#57495=CARTESIAN_POINT('Ctrl Pts',(18.0802500271968,4.08574323756672,-47.3814987227573));
#57496=CARTESIAN_POINT('',(0.,2.01462393409065,-45.4512));
#57497=CARTESIAN_POINT('Ctrl Pts',(70.7282577522084,8.51486331986405,-11.8925191845565));
#57498=CARTESIAN_POINT('Ctrl Pts',(70.3600859174044,9.78627568392211,-11.5801730615178));
#57499=CARTESIAN_POINT('Ctrl Pts',(69.9919140826003,11.0576880479802,-11.267826938479));
#57500=CARTESIAN_POINT('Ctrl Pts',(69.6237422477963,12.3291004120382,-10.9554808154403));
#57501=CARTESIAN_POINT('Ctrl Pts',(71.1586139886749,8.57802101438411,-11.6423301611079));
#57502=CARTESIAN_POINT('Ctrl Pts',(70.8002393926315,9.84354972351229,-11.2952769038158));
#57503=CARTESIAN_POINT('Ctrl Pts',(70.4411327279621,11.1095147323032,-10.9484903485044));
#57504=CARTESIAN_POINT('Ctrl Pts',(70.0827581319187,12.3750434414314,-10.6014370912123));
#57505=CARTESIAN_POINT('Ctrl Pts',(71.9827018728919,8.65468599963629,-11.0972577103214));
#57506=CARTESIAN_POINT('Ctrl Pts',(71.6283269336556,9.91255505994493,-10.7211921629858));
#57507=CARTESIAN_POINT('Ctrl Pts',(71.274046257563,11.1704252165446,-10.345117454098));
#57508=CARTESIAN_POINT('Ctrl Pts',(70.9196713183267,12.4282942768532,-9.96905190676241));
#57509=CARTESIAN_POINT('Ctrl Pts',(73.1303575054126,8.72650011278445,-10.21988802762));
#57510=CARTESIAN_POINT('Ctrl Pts',(72.7531257555003,9.98379326247583,-9.86275653492437));
#57511=CARTESIAN_POINT('Ctrl Pts',(72.3755917318045,11.2412341838258,-9.50577501726162));
#57512=CARTESIAN_POINT('Ctrl Pts',(71.9983599818921,12.4985273335172,-9.148643524566));
#57513=CARTESIAN_POINT('Ctrl Pts',(74.1065736572356,8.81331425878696,-9.37805983947955));
#57514=CARTESIAN_POINT('Ctrl Pts',(73.6947438271767,10.0724325673801,-9.06858889521421));
#57515=CARTESIAN_POINT('Ctrl Pts',(73.2830206497004,11.3316920464878,-8.7588620545661));
#57516=CARTESIAN_POINT('Ctrl Pts',(72.8711908196415,12.5908103550809,-8.44939111030075));
#57517=CARTESIAN_POINT('Ctrl Pts',(75.1777989853639,8.95359154800345,-8.37681652932542));
#57518=CARTESIAN_POINT('Ctrl Pts',(74.7248971875948,10.2125650956128,-8.12906705485955));
#57519=CARTESIAN_POINT('Ctrl Pts',(74.2723094444152,11.4717337582538,-7.88062467972502));
#57520=CARTESIAN_POINT('Ctrl Pts',(73.8194076466462,12.7307073058631,-7.63287520525915));
#57521=CARTESIAN_POINT('Ctrl Pts',(76.3760621018627,9.18465108771821,-7.13733271471052));
#57522=CARTESIAN_POINT('Ctrl Pts',(75.8808429490457,10.4390507692653,-6.95644970672696));
#57523=CARTESIAN_POINT('Ctrl Pts',(75.3855963914733,11.6934931005301,-6.77561572455319));
#57524=CARTESIAN_POINT('Ctrl Pts',(74.8903772386563,12.9478927820772,-6.59473271656963));
#57525=CARTESIAN_POINT('Ctrl Pts',(77.1569389883271,9.37730603443782,-6.18970317121555));
#57526=CARTESIAN_POINT('Ctrl Pts',(76.6501763150819,10.6273118023276,-6.01732352238457));
#57527=CARTESIAN_POINT('Ctrl Pts',(76.1434037774154,11.8780966175269,-5.8447821263057));
#57528=CARTESIAN_POINT('Ctrl Pts',(75.6366411041703,13.1281023854167,-5.67240247747472));
#57529=CARTESIAN_POINT('Ctrl Pts',(77.5413122691233,9.45942207531684,-5.67964638243731));
#57530=CARTESIAN_POINT('Ctrl Pts',(77.0326085523511,10.7074362929352,-5.49721546081316));
#57531=CARTESIAN_POINT('Ctrl Pts',(76.5239048355788,11.9554505105535,-5.314784539189));
#57532=CARTESIAN_POINT('Ctrl Pts',(76.0152011188066,13.2034647281718,-5.13235361756485));
#57533=CARTESIAN_POINT('',(76.778256693965,11.3314434017443,-5.40600000000103));
#57534=CARTESIAN_POINT('',(70.1760000000024,10.4219818659511,-11.4239999999984));
#57535=CARTESIAN_POINT('',(70.1760000000024,10.4219818659511,-11.4239999999984));
#57536=CARTESIAN_POINT('',(70.1760000000024,10.4219818659511,-11.4239999999984));
#57537=CARTESIAN_POINT('Ctrl Pts',(57.8135230791049,6.6905663225968,-18.0349157107808));
#57538=CARTESIAN_POINT('Ctrl Pts',(57.5247816344839,7.95941791373735,-17.6396385702601));
#57539=CARTESIAN_POINT('Ctrl Pts',(57.2360401898628,9.22826950487791,-17.2443614297393));
#57540=CARTESIAN_POINT('Ctrl Pts',(56.9472987452418,10.4971210960185,-16.8490842892186));
#57541=CARTESIAN_POINT('Ctrl Pts',(58.3834371192583,6.78492400902022,-17.921496800064));
#57542=CARTESIAN_POINT('Ctrl Pts',(58.0977762359506,8.04459708605881,-17.4923487139126));
#57543=CARTESIAN_POINT('Ctrl Pts',(57.8136373060536,9.30309323278309,-17.0647829526039));
#57544=CARTESIAN_POINT('Ctrl Pts',(57.5279764227459,10.5627663098217,-16.6356348664524));
#57545=CARTESIAN_POINT('Ctrl Pts',(60.069006328368,7.0315326697423,-17.5237672087188));
#57546=CARTESIAN_POINT('Ctrl Pts',(59.7958287466441,8.26340634490229,-17.0172277477915));
#57547=CARTESIAN_POINT('Ctrl Pts',(59.5221571822746,9.49577953239501,-16.5100213706393));
#57548=CARTESIAN_POINT('Ctrl Pts',(59.2489796005507,10.727653207555,-16.0034819097119));
#57549=CARTESIAN_POINT('Ctrl Pts',(62.2034160825709,7.1647901104433,-16.747451663188));
#57550=CARTESIAN_POINT('Ctrl Pts',(61.9177268933279,8.39487645389337,-16.2388750355847));
#57551=CARTESIAN_POINT('Ctrl Pts',(61.6326018983047,9.62476272199721,-15.7302755084792));
#57552=CARTESIAN_POINT('Ctrl Pts',(61.3469127090617,10.8548490654473,-15.2216988808759));
#57553=CARTESIAN_POINT('Ctrl Pts',(64.7264374328703,7.37946418630416,-15.4764719489058));
#57554=CARTESIAN_POINT('Ctrl Pts',(64.3595954246239,8.63587598557369,-15.0963863265111));
#57555=CARTESIAN_POINT('Ctrl Pts',(63.9932223004386,9.89184700111287,-14.7162842302533));
#57556=CARTESIAN_POINT('Ctrl Pts',(63.6263802921922,11.1482588003824,-14.3361986078586));
#57557=CARTESIAN_POINT('Ctrl Pts',(66.8940351574184,7.74903378142021,-14.2111203469359));
#57558=CARTESIAN_POINT('Ctrl Pts',(66.4695339814581,9.01812242902804,-13.9619266203826));
#57559=CARTESIAN_POINT('Ctrl Pts',(66.0445138974904,10.2868967403885,-13.7141750122686));
#57560=CARTESIAN_POINT('Ctrl Pts',(65.6200127215301,11.5559853879963,-13.4649812857152));
#57561=CARTESIAN_POINT('Ctrl Pts',(68.5152601688859,8.12096232366399,-13.2306538995856));
#57562=CARTESIAN_POINT('Ctrl Pts',(68.0991834125406,9.39567311929895,-13.0053211729385));
#57563=CARTESIAN_POINT('Ctrl Pts',(67.6826412354218,10.6707550048034,-12.7801625272814));
#57564=CARTESIAN_POINT('Ctrl Pts',(67.2665644790765,11.9454658004384,-12.5548298006343));
#57565=CARTESIAN_POINT('Ctrl Pts',(69.7958454230149,8.37193054851245,-12.4618050355517));
#57566=CARTESIAN_POINT('Ctrl Pts',(69.4062810684438,9.6486674313224,-12.1988738548688));
#57567=CARTESIAN_POINT('Ctrl Pts',(69.0168135363837,10.9250928657635,-11.93627796497));
#57568=CARTESIAN_POINT('Ctrl Pts',(68.6272491818126,12.2018297485735,-11.6733467842871));
#57569=CARTESIAN_POINT('Ctrl Pts',(70.4319511017933,8.47390908124125,-12.0750795994181));
#57570=CARTESIAN_POINT('Ctrl Pts',(70.0578486510975,9.74756100248359,-11.7792662482282));
#57571=CARTESIAN_POINT('Ctrl Pts',(69.6832582272912,11.0214634770417,-11.4837699563737));
#57572=CARTESIAN_POINT('Ctrl Pts',(69.3091557765954,12.295115398284,-11.1879566051838));
#57573=CARTESIAN_POINT('Ctrl Pts',(70.7282577522084,8.51486331986406,-11.8925191845565));
#57574=CARTESIAN_POINT('Ctrl Pts',(70.3600859174044,9.78627568392211,-11.5801730615178));
#57575=CARTESIAN_POINT('Ctrl Pts',(69.9919140826003,11.0576880479802,-11.267826938479));
#57576=CARTESIAN_POINT('Ctrl Pts',(69.6237422477963,12.3291004120382,-10.9554808154403));
#57577=CARTESIAN_POINT('',(57.3804109121731,8.59384370930882,-17.4419999999993));
#57578=CARTESIAN_POINT('',(57.3804109121734,8.59384370930763,-17.4419999999997));
#57579=CARTESIAN_POINT('',(57.3804109121734,8.59384370930763,-17.4419999999997));
#57580=CARTESIAN_POINT('Ctrl Pts',(44.864374876377,5.20597739807143,-23.9801519722225));
#57581=CARTESIAN_POINT('Ctrl Pts',(44.4545859760344,6.45554733375931,-23.6333839907407));
#57582=CARTESIAN_POINT('Ctrl Pts',(44.0447970756917,7.7051172694472,-23.286616009259));
#57583=CARTESIAN_POINT('Ctrl Pts',(43.635008175349,8.95468720513508,-22.9398480277772));
#57584=CARTESIAN_POINT('Ctrl Pts',(45.1224142763232,5.22734724195968,-23.7522227177446));
#57585=CARTESIAN_POINT('Ctrl Pts',(44.740324729997,6.47318492815149,-23.3556198386977));
#57586=CARTESIAN_POINT('Ctrl Pts',(44.3637122482329,7.7164483348677,-22.9542254972333));
#57587=CARTESIAN_POINT('Ctrl Pts',(43.9816227019066,8.96228602105951,-22.5576226181864));
#57588=CARTESIAN_POINT('Ctrl Pts',(45.9649684987856,5.22804284539893,-23.0069752550256));
#57589=CARTESIAN_POINT('Ctrl Pts',(45.6662512806454,6.45193039127154,-22.4921612743428));
#57590=CARTESIAN_POINT('Ctrl Pts',(45.36522683304,7.67699365561725,-21.9792150829581));
#57591=CARTESIAN_POINT('Ctrl Pts',(45.0665096148998,8.90088120148987,-21.4644011022753));
#57592=CARTESIAN_POINT('Ctrl Pts',(47.4758616466553,5.06915938849053,-21.7520512140078));
#57593=CARTESIAN_POINT('Ctrl Pts',(47.1533462028712,6.3023705311178,-21.2750662029529));
#57594=CARTESIAN_POINT('Ctrl Pts',(46.8283779466042,7.53667509779519,-20.8011913848345));
#57595=CARTESIAN_POINT('Ctrl Pts',(46.5058625028201,8.76988624042247,-20.3242063737796));
#57596=CARTESIAN_POINT('Ctrl Pts',(49.1569256056527,5.20366478491719,-20.7106555371184));
#57597=CARTESIAN_POINT('Ctrl Pts',(48.8012788734978,6.46168428440042,-20.3329464870476));
#57598=CARTESIAN_POINT('Ctrl Pts',(48.4486371023923,7.71873636075261,-19.9528495627537));
#57599=CARTESIAN_POINT('Ctrl Pts',(48.0929903702374,8.97675586023584,-19.5751405126828));
#57600=CARTESIAN_POINT('Ctrl Pts',(50.0106311017377,5.31735504507218,-20.255161743136));
#57601=CARTESIAN_POINT('Ctrl Pts',(49.6529273423844,6.58525639569541,-19.918243070567));
#57602=CARTESIAN_POINT('Ctrl Pts',(49.2940750004474,7.8538792563298,-19.5830916546927));
#57603=CARTESIAN_POINT('Ctrl Pts',(48.9363712410941,9.12178060695302,-19.2461729821237));
#57604=CARTESIAN_POINT('Ctrl Pts',(50.9536821648416,5.47540829520537,-19.8330327894735));
#57605=CARTESIAN_POINT('Ctrl Pts',(50.6007520305354,6.75386029493047,-19.5306366791759));
#57606=CARTESIAN_POINT('Ctrl Pts',(50.2500375292763,8.03187941866197,-19.2269995241046));
#57607=CARTESIAN_POINT('Ctrl Pts',(49.8971073949701,9.31033141838707,-18.924603413807));
#57608=CARTESIAN_POINT('Ctrl Pts',(52.3106429243915,5.72884656211269,-19.3291250816917));
#57609=CARTESIAN_POINT('Ctrl Pts',(51.980515160004,7.01824730214814,-19.0500355888166));
#57610=CARTESIAN_POINT('Ctrl Pts',(51.650702670309,8.30831373472467,-18.7724371720687));
#57611=CARTESIAN_POINT('Ctrl Pts',(51.3205749059214,9.59771447476012,-18.4933476791936));
#57612=CARTESIAN_POINT('Ctrl Pts',(54.584459674483,6.15313027810468,-18.7389663173459));
#57613=CARTESIAN_POINT('Ctrl Pts',(54.2914742766135,7.44767092452855,-18.4397413559177));
#57614=CARTESIAN_POINT('Ctrl Pts',(53.9970607847715,8.74061567008386,-18.1369221537377));
#57615=CARTESIAN_POINT('Ctrl Pts',(53.704075386902,10.0351563165077,-17.8376971923096));
#57616=CARTESIAN_POINT('Ctrl Pts',(56.7527899477957,6.52682846803759,-18.2841549642181));
#57617=CARTESIAN_POINT('Ctrl Pts',(56.4580200210017,7.80528056919744,-17.9241761601542));
#57618=CARTESIAN_POINT('Ctrl Pts',(56.1665627987475,9.08533845315947,-17.5667019119172));
#57619=CARTESIAN_POINT('Ctrl Pts',(55.8717928719535,10.3637905543193,-17.2067231078532));
#57620=CARTESIAN_POINT('Ctrl Pts',(57.8135230791049,6.69056632259679,-18.0349157107808));
#57621=CARTESIAN_POINT('Ctrl Pts',(57.5247816344839,7.95941791373734,-17.6396385702601));
#57622=CARTESIAN_POINT('Ctrl Pts',(57.2360401898628,9.2282695048779,-17.2443614297393));
#57623=CARTESIAN_POINT('Ctrl Pts',(56.9472987452418,10.4971210960185,-16.8490842892186));
#57624=CARTESIAN_POINT('',(44.249691525863,7.08033230160326,-23.4599999999998));
#57625=CARTESIAN_POINT('',(44.249691525863,7.08033230160326,-23.4599999999998));
#57626=CARTESIAN_POINT('',(44.249691525863,7.08033230160326,-23.4599999999998));
#57627=CARTESIAN_POINT('Ctrl Pts',(41.4215425945231,4.68791040664211,-29.7512671854166));
#57628=CARTESIAN_POINT('Ctrl Pts',(40.8936377463565,5.92799480013269,-29.5690918542356));
#57629=CARTESIAN_POINT('Ctrl Pts',(40.3657328989121,7.1680791888473,-29.3869165043121));
#57630=CARTESIAN_POINT('Ctrl Pts',(39.8378280507455,8.40816358233807,-29.2047411731319));
#57631=CARTESIAN_POINT('Ctrl Pts',(41.4802683438712,4.68413044508663,-29.5553621466157));
#57632=CARTESIAN_POINT('Ctrl Pts',(40.9494709539923,5.92282615948956,-29.3722187306946));
#57633=CARTESIAN_POINT('Ctrl Pts',(40.4186595175311,7.16161474998382,-29.1894397906751));
#57634=CARTESIAN_POINT('Ctrl Pts',(39.8878621282648,8.40031046033545,-29.0062963588554));
#57635=CARTESIAN_POINT('Ctrl Pts',(41.6778807320694,4.68063487456826,-28.9529176330051));
#57636=CARTESIAN_POINT('Ctrl Pts',(41.1360096258359,5.91450409764293,-28.768958382227));
#57637=CARTESIAN_POINT('Ctrl Pts',(40.5940809445236,7.14834387762203,-28.5849862352923));
#57638=CARTESIAN_POINT('Ctrl Pts',(40.0522098408016,8.38221310198101,-28.4010269850767));
#57639=CARTESIAN_POINT('Ctrl Pts',(42.0667678924717,4.70419304693246,-27.964824273678));
#57640=CARTESIAN_POINT('Ctrl Pts',(41.5010972238371,5.92783482634179,-27.7841784792369));
#57641=CARTESIAN_POINT('Ctrl Pts',(40.9357028569913,7.1514823641546,-27.6030152424684));
#57642=CARTESIAN_POINT('Ctrl Pts',(40.3700321763043,8.37512414331273,-27.4223694705982));
#57643=CARTESIAN_POINT('Ctrl Pts',(42.6729216974824,4.823611553925,-26.7992794766923));
#57644=CARTESIAN_POINT('Ctrl Pts',(42.0918120029199,6.04066662955073,-26.6236449949611));
#57645=CARTESIAN_POINT('Ctrl Pts',(41.5102646021906,7.25771063739046,-26.4488728648612));
#57646=CARTESIAN_POINT('Ctrl Pts',(40.929154926721,8.47476571349897,-26.2732383455139));
#57647=CARTESIAN_POINT('Ctrl Pts',(43.1602150679141,4.93691815783542,-26.0485095188922));
#57648=CARTESIAN_POINT('Ctrl Pts',(42.5955457707243,6.15965834108405,-25.8592274909061));
#57649=CARTESIAN_POINT('Ctrl Pts',(42.0312832814734,7.38237091318394,-25.6691749339123));
#57650=CARTESIAN_POINT('Ctrl Pts',(41.4666139665385,8.60511109763698,-25.4798929395369));
#57651=CARTESIAN_POINT('Ctrl Pts',(43.3508405942975,4.97964296442833,-25.7696090237298));
#57652=CARTESIAN_POINT('Ctrl Pts',(42.7960855748333,6.20551740122266,-25.5716146485843));
#57653=CARTESIAN_POINT('Ctrl Pts',(42.24110371321,7.43134209790289,-25.373966918556));
#57654=CARTESIAN_POINT('Ctrl Pts',(41.6863487036408,8.6572165368669,-25.1759725282897));
#57655=CARTESIAN_POINT('Ctrl Pts',(43.6185109451061,5.03817773651984,-25.3933166689187));
#57656=CARTESIAN_POINT('Ctrl Pts',(43.0800759415707,6.26907713023514,-25.1812823216724));
#57657=CARTESIAN_POINT('Ctrl Pts',(42.5417926904819,7.49987935633806,-24.9689147600707));
#57658=CARTESIAN_POINT('Ctrl Pts',(42.003357680327,8.73077875429183,-24.7568804273593));
#57659=CARTESIAN_POINT('Ctrl Pts',(44.1126628332362,5.13439778509021,-24.7624098976365));
#57660=CARTESIAN_POINT('Ctrl Pts',(43.61806572663,6.37718213105814,-24.5106662229177));
#57661=CARTESIAN_POINT('Ctrl Pts',(43.1231679405891,7.62001857940251,-24.2593794372098));
#57662=CARTESIAN_POINT('Ctrl Pts',(42.6285708470986,8.86280292309772,-24.0076357425614));
#57663=CARTESIAN_POINT('Ctrl Pts',(44.5974345578285,5.19049120521572,-24.2397960938373));
#57664=CARTESIAN_POINT('Ctrl Pts',(44.1586022338354,6.44060862595914,-23.9289029933399));
#57665=CARTESIAN_POINT('Ctrl Pts',(43.7201939318932,7.69040988955953,-23.6172776091317));
#57666=CARTESIAN_POINT('Ctrl Pts',(43.2813615894041,8.94052732409383,-23.3063845405767));
#57667=CARTESIAN_POINT('Ctrl Pts',(44.8644027152632,5.20597901315863,-23.9801248941554));
#57668=CARTESIAN_POINT('Ctrl Pts',(44.4546079053322,6.45557614794012,-23.6333456074787));
#57669=CARTESIAN_POINT('Ctrl Pts',(44.0448130511831,7.70517331569156,-23.2865663971665));
#57670=CARTESIAN_POINT('Ctrl Pts',(43.635018241254,8.9547704504716,-22.9397871104864));
#57671=CARTESIAN_POINT('',(40.6297053891129,6.5479961266057,-29.4780000000001));
#57672=CARTESIAN_POINT('Ctrl Pts',(40.1355624239865,4.76730440823259,-35.6660906786094));
#57673=CARTESIAN_POINT('Ctrl Pts',(39.7267542314648,6.05945057763009,-35.5526974481249));
#57674=CARTESIAN_POINT('Ctrl Pts',(39.3179460376291,7.35159674641259,-35.439304217727));
#57675=CARTESIAN_POINT('Ctrl Pts',(38.9091378451075,8.6437429158101,-35.3259109872425));
#57676=CARTESIAN_POINT('Ctrl Pts',(40.3022852108888,4.74136008557223,-34.7693748964185));
#57677=CARTESIAN_POINT('Ctrl Pts',(39.8830814907514,6.03145578103333,-34.6704501714334));
#57678=CARTESIAN_POINT('Ctrl Pts',(39.464473218501,7.3218301400057,-34.5714862261209));
#57679=CARTESIAN_POINT('Ctrl Pts',(39.0452694906739,8.61192583186812,-34.4725615016423));
#57680=CARTESIAN_POINT('Ctrl Pts',(40.5112835949553,4.72982185272993,-33.6344144304767));
#57681=CARTESIAN_POINT('Ctrl Pts',(40.0672938950195,6.01213072428518,-33.5400173560715));
#57682=CARTESIAN_POINT('Ctrl Pts',(39.6231973650581,7.29439145612538,-33.4457381236464));
#57683=CARTESIAN_POINT('Ctrl Pts',(39.1792076665018,8.57670032830231,-33.3513410477193));
#57684=CARTESIAN_POINT('Ctrl Pts',(40.7814488661554,4.71765074492916,-32.2936083574543));
#57685=CARTESIAN_POINT('Ctrl Pts',(40.30513540374,5.98679527850069,-32.1831482629611));
#57686=CARTESIAN_POINT('Ctrl Pts',(39.82883397811,7.25594573394774,-32.0726643871796));
#57687=CARTESIAN_POINT('Ctrl Pts',(39.3525205155391,8.52509026744278,-31.9622042929936));
#57688=CARTESIAN_POINT('Ctrl Pts',(40.942076978619,4.71061953663584,-31.5521512150188));
#57689=CARTESIAN_POINT('Ctrl Pts',(40.4480662906984,5.97166384408667,-31.427374520508));
#57690=CARTESIAN_POINT('Ctrl Pts',(39.9542499180149,7.23280392932176,-31.3028020868362));
#57691=CARTESIAN_POINT('Ctrl Pts',(39.460239227585,8.49384823553572,-31.1780253896876));
#57692=CARTESIAN_POINT('Ctrl Pts',(41.1407904972541,4.7010692865962,-30.7187856331133));
#57693=CARTESIAN_POINT('Ctrl Pts',(40.6287473002004,5.95259800346332,-30.5721760653661));
#57694=CARTESIAN_POINT('Ctrl Pts',(40.11632906848,7.20394181697493,-30.4251866697367));
#57695=CARTESIAN_POINT('Ctrl Pts',(39.6042858762695,8.45547053622989,-30.2785771068945));
#57696=CARTESIAN_POINT('Ctrl Pts',(41.3201731760795,4.69236269068941,-30.0753208265298));
#57697=CARTESIAN_POINT('Ctrl Pts',(40.7965442941259,5.936128776676,-29.9058793753165));
#57698=CARTESIAN_POINT('Ctrl Pts',(40.2734349337518,7.18014776732202,-29.7369323570816));
#57699=CARTESIAN_POINT('Ctrl Pts',(39.7498060450891,8.42391385004259,-29.5674908994831));
#57700=CARTESIAN_POINT('Ctrl Pts',(41.4215465127793,4.68791017280978,-29.7512542394393));
#57701=CARTESIAN_POINT('Ctrl Pts',(40.8936495828703,5.92797542331161,-29.5690815425449));
#57702=CARTESIAN_POINT('Ctrl Pts',(40.3657526483566,7.16804067157194,-29.3869088412683));
#57703=CARTESIAN_POINT('Ctrl Pts',(39.8378557184476,8.4081059220738,-29.204736144374));
#57704=CARTESIAN_POINT('',(39.5223544282475,6.70551108323301,-35.4960000000008));
#57705=CARTESIAN_POINT('Ctrl Pts',(38.8604541099242,4.82976572790836,-41.6539325852788));
#57706=CARTESIAN_POINT('Ctrl Pts',(38.4040326949894,6.10748900320916,-41.560644195093));
#57707=CARTESIAN_POINT('Ctrl Pts',(37.9476112800545,7.38521227850996,-41.4673558049072));
#57708=CARTESIAN_POINT('Ctrl Pts',(37.4911898651196,8.66293555381076,-41.3740674147214));
#57709=CARTESIAN_POINT('Ctrl Pts',(39.0048197292983,4.83127154325761,-40.9682358462176));
#57710=CARTESIAN_POINT('Ctrl Pts',(38.5631614180215,6.11417338749171,-40.8732587077797));
#57711=CARTESIAN_POINT('Ctrl Pts',(38.1218299586132,7.39711052016881,-40.7783273701692));
#57712=CARTESIAN_POINT('Ctrl Pts',(37.6801716473364,8.68001236440291,-40.6833502317314));
#57713=CARTESIAN_POINT('Ctrl Pts',(39.2693233059464,4.83474737532154,-39.8104175938772));
#57714=CARTESIAN_POINT('Ctrl Pts',(38.8540548662111,6.12623786385084,-39.7127351491205));
#57715=CARTESIAN_POINT('Ctrl Pts',(38.4385849974131,7.41770099535643,-39.6150176340949));
#57716=CARTESIAN_POINT('Ctrl Pts',(38.0233165576779,8.70919148388572,-39.5173351893382));
#57717=CARTESIAN_POINT('Ctrl Pts',(39.6452981730948,4.8199494242592,-38.1129891991618));
#57718=CARTESIAN_POINT('Ctrl Pts',(39.2474592055531,6.1164069836728,-38.0104489972814));
#57719=CARTESIAN_POINT('Ctrl Pts',(38.8497085452635,7.41288231613064,-37.9079311640875));
#57720=CARTESIAN_POINT('Ctrl Pts',(38.4518695777218,8.70933987554425,-37.8053909622071));
#57721=CARTESIAN_POINT('Ctrl Pts',(39.8853277117453,4.79858865457864,-36.9461294764195));
#57722=CARTESIAN_POINT('Ctrl Pts',(39.4866283556263,6.09442229132186,-36.839046741644));
#57723=CARTESIAN_POINT('Ctrl Pts',(39.0879084576719,7.39024881387909,-36.7319585207745));
#57724=CARTESIAN_POINT('Ctrl Pts',(38.6892091015529,8.68608245062232,-36.6248757859991));
#57725=CARTESIAN_POINT('Ctrl Pts',(40.0280907705529,4.78204396051868,-36.2245904908727));
#57726=CARTESIAN_POINT('Ctrl Pts',(39.6249516837898,6.0762191111159,-36.1141481442971));
#57727=CARTESIAN_POINT('Ctrl Pts',(39.2218674158251,7.37041538269592,-36.0037336147251));
#57728=CARTESIAN_POINT('Ctrl Pts',(38.818728329062,8.66459053329314,-35.8932912681495));
#57729=CARTESIAN_POINT('Ctrl Pts',(40.1031985714104,4.7719144148413,-35.8353019842399));
#57730=CARTESIAN_POINT('Ctrl Pts',(39.6962798859278,6.06473085465749,-35.722829449568));
#57731=CARTESIAN_POINT('Ctrl Pts',(39.2893811996143,7.35755308021419,-35.6103820624053));
#57732=CARTESIAN_POINT('Ctrl Pts',(38.8824625141317,8.65036952003038,-35.4979095277334));
#57733=CARTESIAN_POINT('Ctrl Pts',(40.1355627919427,4.76730435097364,-35.6660886995628));
#57734=CARTESIAN_POINT('Ctrl Pts',(39.7267572161459,6.05944217247988,-35.5526962331881));
#57735=CARTESIAN_POINT('Ctrl Pts',(39.3179516403491,7.35157999398613,-35.4393037668135));
#57736=CARTESIAN_POINT('Ctrl Pts',(38.9091460645523,8.64371781549238,-35.3259113004388));
#57737=CARTESIAN_POINT('',(38.1758219875219,6.74635064085956,-41.5140000000001));
#57738=CARTESIAN_POINT('Ctrl Pts',(38.0224643391856,4.86842248450045,-47.6590906035866));
#57739=CARTESIAN_POINT('Ctrl Pts',(37.5141154779131,6.12699419839355,-47.5743635345289));
#57740=CARTESIAN_POINT('Ctrl Pts',(37.0057666166406,7.38556591228665,-47.4896364654712));
#57741=CARTESIAN_POINT('Ctrl Pts',(36.497417755368,8.64413762617975,-47.4049093964135));
#57742=CARTESIAN_POINT('Ctrl Pts',(38.0629003858012,4.86150818139181,-47.3137728097505));
#57743=CARTESIAN_POINT('Ctrl Pts',(37.5511999079971,6.1190243894845,-47.2334402336884));
#57744=CARTESIAN_POINT('Ctrl Pts',(37.0394051258501,7.3765107446069,-47.1533372415835));
#57745=CARTESIAN_POINT('Ctrl Pts',(36.527704648046,8.63402695269959,-47.0730046655214));
#57746=CARTESIAN_POINT('Ctrl Pts',(38.1507053914965,4.8450084544398,-46.4729294774833));
#57747=CARTESIAN_POINT('Ctrl Pts',(37.6327442277917,6.10042701332241,-46.400485455692));
#57748=CARTESIAN_POINT('Ctrl Pts',(37.1149509225975,7.35590056277829,-46.3277870171961));
#57749=CARTESIAN_POINT('Ctrl Pts',(36.5969897588927,8.6113191216609,-46.2553429954049));
#57750=CARTESIAN_POINT('Ctrl Pts',(38.2620837951133,4.82664388150297,-45.3133943758124));
#57751=CARTESIAN_POINT('Ctrl Pts',(37.7433647107974,6.08193783777536,-45.2441132294512));
#57752=CARTESIAN_POINT('Ctrl Pts',(37.2245219104796,7.33719426285198,-45.1749682106718));
#57753=CARTESIAN_POINT('Ctrl Pts',(36.7058028261638,8.59248821912437,-45.1056870643106));
#57754=CARTESIAN_POINT('Ctrl Pts',(38.4228858295138,4.82107508008706,-44.0628313203019));
#57755=CARTESIAN_POINT('Ctrl Pts',(37.9176015720814,6.08163116257953,-43.9896189803569));
#57756=CARTESIAN_POINT('Ctrl Pts',(37.4123697296278,7.34219997720122,-43.9163618117411));
#57757=CARTESIAN_POINT('Ctrl Pts',(36.9070854721954,8.60275605969368,-43.8431494717961));
#57758=CARTESIAN_POINT('Ctrl Pts',(38.5993784816469,4.82325654371877,-42.9411023467542));
#57759=CARTESIAN_POINT('Ctrl Pts',(38.1135891457311,6.09108424087921,-42.8607129324259));
#57760=CARTESIAN_POINT('Ctrl Pts',(37.6277594573051,7.35891332881017,-42.7803490135197));
#57761=CARTESIAN_POINT('Ctrl Pts',(37.1419701213893,8.6267410259706,-42.6999595991915));
#57762=CARTESIAN_POINT('Ctrl Pts',(38.7504700253912,4.82820987401249,-42.170729376939));
#57763=CARTESIAN_POINT('Ctrl Pts',(38.2826040468472,6.10225649008106,-42.0828980653399));
#57764=CARTESIAN_POINT('Ctrl Pts',(37.8147453818706,7.37626900862381,-41.9951012812711));
#57765=CARTESIAN_POINT('Ctrl Pts',(37.3468794033266,8.65031562469239,-41.9072699696721));
#57766=CARTESIAN_POINT('Ctrl Pts',(38.8604541099242,4.82976572790836,-41.6539325852788));
#57767=CARTESIAN_POINT('Ctrl Pts',(38.4040326949894,6.10748900320916,-41.560644195093));
#57768=CARTESIAN_POINT('Ctrl Pts',(37.9476112800545,7.38521227850996,-41.4673558049072));
#57769=CARTESIAN_POINT('Ctrl Pts',(37.4911898651196,8.66293555381076,-41.3740674147214));
#57770=CARTESIAN_POINT('',(37.2599410472768,6.7562800553401,-47.532));
#57771=CARTESIAN_POINT('Ctrl Pts',(36.1829187178027,4.79789635062137,-53.6562454252777));
#57772=CARTESIAN_POINT('Ctrl Pts',(35.7573843424341,6.08767170594883,-53.5854166319681));
#57773=CARTESIAN_POINT('Ctrl Pts',(35.331849966191,7.37744705912874,-53.514587843528));
#57774=CARTESIAN_POINT('Ctrl Pts',(34.9063155908223,8.66722241445618,-53.4437590502184));
#57775=CARTESIAN_POINT('Ctrl Pts',(36.4945975641142,4.8692415372667,-53.0828797714532));
#57776=CARTESIAN_POINT('Ctrl Pts',(36.0607845903544,6.15396331395307,-52.9743935222565));
#57777=CARTESIAN_POINT('Ctrl Pts',(35.6272852524983,7.4394553746638,-52.8641606487343));
#57778=CARTESIAN_POINT('Ctrl Pts',(35.1934722815684,8.72417715829996,-52.7556743837789));
#57779=CARTESIAN_POINT('Ctrl Pts',(37.0196238186211,4.94621406635564,-52.0172199352926));
#57780=CARTESIAN_POINT('Ctrl Pts',(36.5725094960081,6.22274211276401,-51.8743508628265));
#57781=CARTESIAN_POINT('Ctrl Pts',(36.1253011361753,7.49898590806397,-51.7321837308753));
#57782=CARTESIAN_POINT('Ctrl Pts',(35.6781868127138,8.77551395190772,-51.5893146647424));
#57783=CARTESIAN_POINT('Ctrl Pts',(37.4961264547335,4.95593012911406,-50.632199053437));
#57784=CARTESIAN_POINT('Ctrl Pts',(37.0309089823822,6.22517924195192,-50.4826709817263));
#57785=CARTESIAN_POINT('Ctrl Pts',(36.5656417928408,7.49447486452825,-50.3328090769852));
#57786=CARTESIAN_POINT('Ctrl Pts',(36.1004243200409,8.76372397778573,-50.1832810022625));
#57787=CARTESIAN_POINT('Ctrl Pts',(37.8514088449462,4.91190498255859,-49.0406523578434));
#57788=CARTESIAN_POINT('Ctrl Pts',(37.3611948698808,6.17388941863381,-48.9098613797906));
#57789=CARTESIAN_POINT('Ctrl Pts',(36.8710842666241,7.43589006578039,-48.7793508906566));
#57790=CARTESIAN_POINT('Ctrl Pts',(36.3808702924914,8.69787450200186,-48.6485599151345));
#57791=CARTESIAN_POINT('Ctrl Pts',(37.9653755874324,4.87922727833883,-48.1624087409971));
#57792=CARTESIAN_POINT('Ctrl Pts',(37.4620517032201,6.13855052559459,-48.0582635515641));
#57793=CARTESIAN_POINT('Ctrl Pts',(36.9587801664333,7.39783829087798,-47.9542796924559));
#57794=CARTESIAN_POINT('Ctrl Pts',(36.4554562826933,8.65716153781361,-47.8501345044785));
#57795=CARTESIAN_POINT('Ctrl Pts',(38.0224713673792,4.86840542327654,-47.6590904423752));
#57796=CARTESIAN_POINT('Ctrl Pts',(37.5141201997668,6.12698281293256,-47.574363041552));
#57797=CARTESIAN_POINT('Ctrl Pts',(37.0057690320183,7.38556020268079,-47.4896356403095));
#57798=CARTESIAN_POINT('Ctrl Pts',(36.4974178644059,8.6441375923368,-47.4049082394863));
#57799=CARTESIAN_POINT('',(35.5446151095801,6.73256828905091,-53.5499999999998));
#57800=CARTESIAN_POINT('',(35.5446151095801,6.732568289051,-53.5499999999998));
#57801=CARTESIAN_POINT('',(35.5446151095801,6.732568289051,-53.5499999999998));
#57802=CARTESIAN_POINT('Ctrl Pts',(33.2870419060244,4.35253527707261,-59.9326413364725));
#57803=CARTESIAN_POINT('Ctrl Pts',(33.1297679354284,5.68135810058122,-59.6895471121569));
#57804=CARTESIAN_POINT('Ctrl Pts',(32.9724939648324,7.01018092408982,-59.4464528878414));
#57805=CARTESIAN_POINT('Ctrl Pts',(32.8152199942364,8.33900374759843,-59.2033586635258));
#57806=CARTESIAN_POINT('Ctrl Pts',(33.4229509461086,4.29496143663751,-59.5299975144865));
#57807=CARTESIAN_POINT('Ctrl Pts',(33.2540721505405,5.629703551151,-59.3266294513922));
#57808=CARTESIAN_POINT('Ctrl Pts',(33.0848228192888,6.96433962786048,-59.1233364488466));
#57809=CARTESIAN_POINT('Ctrl Pts',(32.9159440237207,8.29908174237397,-58.9199683857523));
#57810=CARTESIAN_POINT('Ctrl Pts',(33.6851862294326,4.2187977606422,-58.7810965318263));
#57811=CARTESIAN_POINT('Ctrl Pts',(33.4882387352318,5.56019112234171,-58.6494224775955));
#57812=CARTESIAN_POINT('Ctrl Pts',(33.2911863744521,6.90158317509347,-58.518229027166));
#57813=CARTESIAN_POINT('Ctrl Pts',(33.0942388802513,8.24297653679298,-58.3865549729352));
#57814=CARTESIAN_POINT('Ctrl Pts',(34.2073884246238,4.23730640106381,-57.4829997732066));
#57815=CARTESIAN_POINT('Ctrl Pts',(33.9441936148297,5.57213375970279,-57.4484139032383));
#57816=CARTESIAN_POINT('Ctrl Pts',(33.6810016174677,6.90699115801177,-57.4140188439892));
#57817=CARTESIAN_POINT('Ctrl Pts',(33.4178068076735,8.24181851665074,-57.3794329740209));
#57818=CARTESIAN_POINT('Ctrl Pts',(34.7098314415821,4.34420708527133,-56.3714098124856));
#57819=CARTESIAN_POINT('Ctrl Pts',(34.3867318358801,5.66571066712957,-56.3909712140127));
#57820=CARTESIAN_POINT('Ctrl Pts',(34.063764606468,6.98719531120586,-56.409854609254));
#57821=CARTESIAN_POINT('Ctrl Pts',(33.7406650007661,8.3086988930641,-56.4294160107811));
#57822=CARTESIAN_POINT('Ctrl Pts',(35.1927431574716,4.49494117626302,-55.4098063298174));
#57823=CARTESIAN_POINT('Ctrl Pts',(34.8214509904975,5.80298260475985,-55.4445840814943));
#57824=CARTESIAN_POINT('Ctrl Pts',(34.4501548296962,7.11104892816353,-55.4807062041802));
#57825=CARTESIAN_POINT('Ctrl Pts',(34.0788626627221,8.41909035666035,-55.5154839558572));
#57826=CARTESIAN_POINT('Ctrl Pts',(35.7305102690663,4.67496655037645,-54.4301029015604));
#57827=CARTESIAN_POINT('Ctrl Pts',(35.3205130214595,5.97210422303575,-54.4388227939225));
#57828=CARTESIAN_POINT('Ctrl Pts',(34.9105277929706,7.26920952621076,-54.445846095379));
#57829=CARTESIAN_POINT('Ctrl Pts',(34.5005305453637,8.56634719887006,-54.4545659877411));
#57830=CARTESIAN_POINT('Ctrl Pts',(36.0414358248271,4.76453118953972,-53.8983393183568));
#57831=CARTESIAN_POINT('Ctrl Pts',(35.6194610289143,6.05709958470143,-53.8565986935583));
#57832=CARTESIAN_POINT('Ctrl Pts',(35.1973562738383,7.34967284882424,-53.8172409820912));
#57833=CARTESIAN_POINT('Ctrl Pts',(34.7753814779255,8.64224124398597,-53.7755003572928));
#57834=CARTESIAN_POINT('Ctrl Pts',(36.1829138277446,4.79791400485598,-53.6562428681622));
#57835=CARTESIAN_POINT('Ctrl Pts',(35.7573813489682,6.08768352765266,-53.5854142893873));
#57836=CARTESIAN_POINT('Ctrl Pts',(35.3318488701919,7.37745305044934,-53.5145857106124));
#57837=CARTESIAN_POINT('Ctrl Pts',(34.9063163914155,8.66722257324602,-53.4437571318374));
#57838=CARTESIAN_POINT('',(33.0511309501304,6.3457695123354,-59.5679999999992));
#57839=CARTESIAN_POINT('',(33.0511309501304,6.34576951233552,-59.5679999999991));
#57840=CARTESIAN_POINT('',(33.0511309501304,6.34576951233552,-59.5679999999991));
#57841=CARTESIAN_POINT('Ctrl Pts',(30.375352617956,6.01695827937672,-66.3794252415248));
#57842=CARTESIAN_POINT('Ctrl Pts',(30.3626907742229,7.26983436695969,-65.8504689498228));
#57843=CARTESIAN_POINT('Ctrl Pts',(30.3500289284736,8.52271045531506,-65.321512657339));
#57844=CARTESIAN_POINT('Ctrl Pts',(30.3373670847405,9.77558654289799,-64.7925563656371));
#57845=CARTESIAN_POINT('Ctrl Pts',(30.7734080472794,5.72447156348205,-65.6771181764558));
#57846=CARTESIAN_POINT('Ctrl Pts',(30.7448485850692,6.99344565155228,-65.1864226761427));
#57847=CARTESIAN_POINT('Ctrl Pts',(30.7168558233171,8.26220262947483,-64.6959469190092));
#57848=CARTESIAN_POINT('Ctrl Pts',(30.6882963446928,9.53117672383348,-64.2052514123314));
#57849=CARTESIAN_POINT('Ctrl Pts',(31.4978212248027,5.28838709683457,-64.4647878013927));
#57850=CARTESIAN_POINT('Ctrl Pts',(31.4326417736021,6.58333296740239,-64.0472546764288));
#57851=CARTESIAN_POINT('Ctrl Pts',(31.3670636236145,7.87843336812688,-63.6295773598725));
#57852=CARTESIAN_POINT('Ctrl Pts',(31.3018841839619,9.17337923421885,-63.212044239085));
#57853=CARTESIAN_POINT('Ctrl Pts',(32.3856289559011,4.77997444759906,-62.3963211915439));
#57854=CARTESIAN_POINT('Ctrl Pts',(32.2825028323417,6.09671440776364,-62.0695151547111));
#57855=CARTESIAN_POINT('Ctrl Pts',(32.1795677235084,7.4133780774859,-61.7427677520746));
#57856=CARTESIAN_POINT('Ctrl Pts',(32.0764415944165,8.73011803986018,-61.4159617135434));
#57857=CARTESIAN_POINT('Ctrl Pts',(32.8375602373923,4.5442896682234,-61.1512919674956));
#57858=CARTESIAN_POINT('Ctrl Pts',(32.7118681225965,5.86835965228387,-60.8667666847735));
#57859=CARTESIAN_POINT('Ctrl Pts',(32.5860717505013,7.19248099999695,-60.5822170975346));
#57860=CARTESIAN_POINT('Ctrl Pts',(32.4603796387252,8.5165509825697,-60.2976918155163));
#57861=CARTESIAN_POINT('Ctrl Pts',(33.092150020816,4.4293908705056,-60.4613447566517));
#57862=CARTESIAN_POINT('Ctrl Pts',(32.9499790526618,5.75660571904382,-60.2002657624891));
#57863=CARTESIAN_POINT('Ctrl Pts',(32.8078113847281,7.08377427021025,-59.9392806852867));
#57864=CARTESIAN_POINT('Ctrl Pts',(32.6656404164781,8.41098912008943,-59.6782016884039));
#57865=CARTESIAN_POINT('Ctrl Pts',(33.2133454585014,4.37993800979747,-60.1301118440788));
#57866=CARTESIAN_POINT('Ctrl Pts',(33.0621641363232,5.70821979358271,-59.8801414619397));
#57867=CARTESIAN_POINT('Ctrl Pts',(32.9109493382996,7.03658498637352,-59.6302488962229));
#57868=CARTESIAN_POINT('Ctrl Pts',(32.7597680170911,8.36486676774288,-59.3802785118299));
#57869=CARTESIAN_POINT('Ctrl Pts',(33.287043479682,4.35253469193526,-59.9326371198377));
#57870=CARTESIAN_POINT('Ctrl Pts',(33.1297671012815,5.68137677156017,-59.6895395217589));
#57871=CARTESIAN_POINT('Ctrl Pts',(32.9724907235957,7.01021884940405,-59.4464419220186));
#57872=CARTESIAN_POINT('Ctrl Pts',(32.8152143451951,8.339060929029,-59.2033443239399));
#57873=CARTESIAN_POINT('',(30.3563614587248,7.89624424005165,-65.5859999999992));
#57874=CARTESIAN_POINT('Ctrl Pts',(27.8032099026773,9.23603570625547,-72.5577783044314));
#57875=CARTESIAN_POINT('Ctrl Pts',(27.8052592514418,10.4382369274192,-71.9219261014769));
#57876=CARTESIAN_POINT('Ctrl Pts',(27.8073086002062,11.6404381485829,-71.2860738985224));
#57877=CARTESIAN_POINT('Ctrl Pts',(27.8093579489706,12.8426393697467,-70.6502216955679));
#57878=CARTESIAN_POINT('Ctrl Pts',(28.1510242423018,8.65285503600956,-71.4562837782078));
#57879=CARTESIAN_POINT('Ctrl Pts',(28.1527242375236,9.84564349530056,-70.802192004818));
#57880=CARTESIAN_POINT('Ctrl Pts',(28.1514837747999,11.0390178223757,-70.1505238587518));
#57881=CARTESIAN_POINT('Ctrl Pts',(28.1531837700217,12.2318062816667,-69.496432085362));
#57882=CARTESIAN_POINT('Ctrl Pts',(28.8443112604251,7.45365732155485,-69.2995688107867));
#57883=CARTESIAN_POINT('Ctrl Pts',(28.8647942312408,8.64083812394836,-68.6377099178768));
#57884=CARTESIAN_POINT('Ctrl Pts',(28.8876145388117,9.82698901941381,-67.9773229033855));
#57885=CARTESIAN_POINT('Ctrl Pts',(28.9080975096274,11.0141698218073,-67.3154640104755));
#57886=CARTESIAN_POINT('Ctrl Pts',(29.7346820906896,6.49856484963839,-67.5354860661677));
#57887=CARTESIAN_POINT('Ctrl Pts',(29.7474671388954,7.71803436653537,-66.9293044052007));
#57888=CARTESIAN_POINT('Ctrl Pts',(29.7599684642251,8.93844313064385,-66.3179762113913));
#57889=CARTESIAN_POINT('Ctrl Pts',(29.7727535124309,10.1579126475408,-65.7117945504243));
#57890=CARTESIAN_POINT('Ctrl Pts',(30.3753540341101,6.01695723880264,-66.3794227429407));
#57891=CARTESIAN_POINT('Ctrl Pts',(30.3626923171866,7.26981523963531,-65.8504742476464));
#57892=CARTESIAN_POINT('Ctrl Pts',(30.3500306002631,8.52267324046798,-65.321525752352));
#57893=CARTESIAN_POINT('Ctrl Pts',(30.3373688833396,9.77553124130065,-64.7925772570577));
#57894=CARTESIAN_POINT('',(27.806283925824,11.0393375380011,-71.6039999999996));
#57895=CARTESIAN_POINT('Ctrl Pts',(25.9521939365417,12.4413225404487,-78.5797210091187));
#57896=CARTESIAN_POINT('Ctrl Pts',(25.9541384795002,13.6421300392938,-77.9412403363729));
#57897=CARTESIAN_POINT('Ctrl Pts',(25.9560830224588,14.842937538139,-77.3027596636271));
#57898=CARTESIAN_POINT('Ctrl Pts',(25.9580275654173,16.0437450369841,-76.6642789908813));
#57899=CARTESIAN_POINT('Ctrl Pts',(26.6489056111189,11.3582252904424,-76.5448332365292));
#57900=CARTESIAN_POINT('Ctrl Pts',(26.6512972678507,12.5584545103135,-75.9052703277155));
#57901=CARTESIAN_POINT('Ctrl Pts',(26.6535845911736,13.7589674719392,-75.2662287814246));
#57902=CARTESIAN_POINT('Ctrl Pts',(26.6559762479054,14.9591966918103,-74.6266658726109));
#57903=CARTESIAN_POINT('Ctrl Pts',(27.2714354678562,10.1515799210123,-74.2870773091685));
#57904=CARTESIAN_POINT('Ctrl Pts',(27.2756644534002,11.3518792281848,-73.6476429472785));
#57905=CARTESIAN_POINT('Ctrl Pts',(27.2793717433237,12.5524667929678,-73.0087316566374));
#57906=CARTESIAN_POINT('Ctrl Pts',(27.2836007288677,13.7527661001403,-72.3692972947473));
#57907=CARTESIAN_POINT('Ctrl Pts',(27.8032099026773,9.23603570625547,-72.5577783044313));
#57908=CARTESIAN_POINT('Ctrl Pts',(27.8052592514418,10.4382369274192,-71.9219261014769));
#57909=CARTESIAN_POINT('Ctrl Pts',(27.8073086002062,11.6404381485829,-71.2860738985224));
#57910=CARTESIAN_POINT('Ctrl Pts',(27.8093579489706,12.8426393697467,-70.6502216955679));
#57911=CARTESIAN_POINT('',(25.9551107509795,14.2425337887164,-77.622));
#57912=CARTESIAN_POINT('Ctrl Pts',(25.7013237933716,12.8213530409933,-79.2937211639668));
#57913=CARTESIAN_POINT('Ctrl Pts',(25.703107932115,14.0221614010657,-78.6552400332983));
#57914=CARTESIAN_POINT('Ctrl Pts',(25.7048920708584,15.222969761138,-78.0167589026299));
#57915=CARTESIAN_POINT('Ctrl Pts',(25.7066762096018,16.4237781212104,-77.3782777719614));
#57916=CARTESIAN_POINT('Ctrl Pts',(25.7858423841264,12.6969189363309,-79.0599308245275));
#57917=CARTESIAN_POINT('Ctrl Pts',(25.7876841876523,13.8977272296109,-78.4214497293732));
#57918=CARTESIAN_POINT('Ctrl Pts',(25.7895259902168,15.098535522888,-77.7829686342204));
#57919=CARTESIAN_POINT('Ctrl Pts',(25.7913677937427,16.299343816168,-77.1444875390661));
#57920=CARTESIAN_POINT('Ctrl Pts',(25.8694745378322,12.5700031119249,-78.8214820370544));
#57921=CARTESIAN_POINT('Ctrl Pts',(25.8713700338312,13.7708113397676,-78.1830009766937));
#57922=CARTESIAN_POINT('Ctrl Pts',(25.8732655270703,14.9716195676109,-77.5445199163328));
#57923=CARTESIAN_POINT('Ctrl Pts',(25.8751610230693,16.1724277954536,-76.9060388559721));
#57924=CARTESIAN_POINT('Ctrl Pts',(25.9521939365416,12.4413225404487,-78.5797210091187));
#57925=CARTESIAN_POINT('Ctrl Pts',(25.9541384805804,13.6421307063697,-77.9412399816823));
#57926=CARTESIAN_POINT('Ctrl Pts',(25.9560830246193,14.8429388722908,-77.302758954246));
#57927=CARTESIAN_POINT('Ctrl Pts',(25.9580275686581,16.0437470382118,-76.6642779268097));
#57928=CARTESIAN_POINT('',(25.704,14.6225645804879,-78.336));
#57929=CARTESIAN_POINT('Ctrl Pts',(16.6868359538665,-0.000191536951231605,
0.654121073022559));
#57930=CARTESIAN_POINT('Ctrl Pts',(16.6871130009561,1.35958001992956,0.626822611164732));
#57931=CARTESIAN_POINT('Ctrl Pts',(16.6873900829518,2.71935102913423,0.599523466282213));
#57932=CARTESIAN_POINT('Ctrl Pts',(16.6876671300389,4.07912258605159,0.572225004469986));
#57933=CARTESIAN_POINT('Ctrl Pts',(16.4198213451363,-0.0072139952602401,
0.301563721594622));
#57934=CARTESIAN_POINT('Ctrl Pts',(16.4149483564531,1.35222993480795,0.260719814132208));
#57935=CARTESIAN_POINT('Ctrl Pts',(16.4100641886526,2.71184728945692,0.220092277311395));
#57936=CARTESIAN_POINT('Ctrl Pts',(16.4051912007158,4.07129120794696,0.179248355403675));
#57937=CARTESIAN_POINT('Ctrl Pts',(15.9097730333143,-0.035107207618914,
-0.369838110396843));
#57938=CARTESIAN_POINT('Ctrl Pts',(15.8868427712196,1.32341742242539,-0.442089514816164));
#57939=CARTESIAN_POINT('Ctrl Pts',(15.8641357832454,2.68219337959501,-0.514193315526313));
#57940=CARTESIAN_POINT('Ctrl Pts',(15.8412055062445,4.04071799286026,-0.586444729799931));
#57941=CARTESIAN_POINT('Ctrl Pts',(15.1895782981127,-0.127632624932323,
-1.30811589893802));
#57942=CARTESIAN_POINT('Ctrl Pts',(15.1168866283587,1.22525531384823,-1.4352518979635));
#57943=CARTESIAN_POINT('Ctrl Pts',(15.0450007447708,2.57878997793115,-1.56159595966525));
#57944=CARTESIAN_POINT('Ctrl Pts',(14.972309021221,3.93167787353513,-1.68873201156193));
#57945=CARTESIAN_POINT('Ctrl Pts',(14.4478451522131,-0.294302251982803,
-2.24397964816492));
#57946=CARTESIAN_POINT('Ctrl Pts',(14.3065594477978,1.04741687112848,-2.42449959114297));
#57947=CARTESIAN_POINT('Ctrl Pts',(14.1657723022977,2.38986935560785,-2.60458130729388));
#57948=CARTESIAN_POINT('Ctrl Pts',(14.0244865645977,3.73158842975856,-2.78510127952877));
#57949=CARTESIAN_POINT('Ctrl Pts',(13.3090122220842,-0.649992640739952,
-3.60728200843994));
#57950=CARTESIAN_POINT('Ctrl Pts',(13.0576846605298,0.667403037119348,-3.84500082344613));
#57951=CARTESIAN_POINT('Ctrl Pts',(12.8072569661008,1.98553821670635,-4.08237633541932));
#57952=CARTESIAN_POINT('Ctrl Pts',(12.5559293444697,3.30293384519514,-4.32009517334507));
#57953=CARTESIAN_POINT('Ctrl Pts',(12.4227603814739,-1.01957344555764,-4.524504549358));
#57954=CARTESIAN_POINT('Ctrl Pts',(12.127008354679,0.290201594277321,-4.74199275926332));
#57955=CARTESIAN_POINT('Ctrl Pts',(11.8349318621356,1.60395062323898,-4.95610715005898));
#57956=CARTESIAN_POINT('Ctrl Pts',(11.5391795899552,2.91372539776307,-5.17359558520671));
#57957=CARTESIAN_POINT('Ctrl Pts',(11.7462901651811,-1.24921324929923,-5.16107659537416));
#57958=CARTESIAN_POINT('Ctrl Pts',(11.4529263608345,0.0686917034324408,
-5.32475380701892));
#57959=CARTESIAN_POINT('Ctrl Pts',(11.159558691757,1.38659247768001,-5.48843456601537));
#57960=CARTESIAN_POINT('Ctrl Pts',(10.8661948876683,2.70449743069063,-5.65211177742331));
#57961=CARTESIAN_POINT('',(11.3069663320366,0.727806741256165,-5.40599999999995));
#57962=CARTESIAN_POINT('',(11.3069663320366,0.727806741256156,-5.40599999999995));
#57963=CARTESIAN_POINT('',(16.6863859277573,2.03937401791753,0.612000000000006));
#57964=CARTESIAN_POINT('',(11.3069663320366,0.727806741256156,-5.40599999999995));
#57965=CARTESIAN_POINT('Ctrl Pts',(21.143061504949,0.000717013383189635,
6.63001173766479));
#57966=CARTESIAN_POINT('Ctrl Pts',(21.1420934966245,1.36071666886059,6.63000391255492));
#57967=CARTESIAN_POINT('Ctrl Pts',(21.1411254883,2.72071632433799,6.62999608744506));
#57968=CARTESIAN_POINT('Ctrl Pts',(21.1401574799756,4.0807159798154,6.62998826233519));
#57969=CARTESIAN_POINT('Ctrl Pts',(20.7896206018235,0.000462775210329253,
6.1661088491225));
#57970=CARTESIAN_POINT('Ctrl Pts',(20.7886536144186,1.36046223337728,6.16578937691944));
#57971=CARTESIAN_POINT('Ctrl Pts',(20.7876658550932,2.72046226560781,6.16549015689824));
#57972=CARTESIAN_POINT('Ctrl Pts',(20.7866988676883,4.08046172377477,6.16517068469518));
#57973=CARTESIAN_POINT('Ctrl Pts',(20.2242344700564,-0.000331798776586382,
5.42457815226979));
#57974=CARTESIAN_POINT('Ctrl Pts',(20.2234969692448,1.359668566771,5.42428041199225));
#57975=CARTESIAN_POINT('Ctrl Pts',(20.2227569926779,2.71966965367535,5.42402726122232));
#57976=CARTESIAN_POINT('Ctrl Pts',(20.2220194918663,4.07967001922293,5.42372952094477));
#57977=CARTESIAN_POINT('Ctrl Pts',(19.3349512314561,0.000515684789920872,
4.24013268454022));
#57978=CARTESIAN_POINT('Ctrl Pts',(19.3369098147026,1.36051510559572,4.24122795422388));
#57979=CARTESIAN_POINT('Ctrl Pts',(19.3388458619514,2.7205156633834,4.24232412204579));
#57980=CARTESIAN_POINT('Ctrl Pts',(19.3408044451979,4.08051508418919,4.24341939172945));
#57981=CARTESIAN_POINT('Ctrl Pts',(18.5712915581816,0.00384555894097715,
3.20912559098008));
#57982=CARTESIAN_POINT('Ctrl Pts',(18.5769308819044,1.36383440276467,3.21096269832565));
#57983=CARTESIAN_POINT('Ctrl Pts',(18.5826039971431,2.72382355018078,3.21280405416297));
#57984=CARTESIAN_POINT('Ctrl Pts',(18.5882433208659,4.08381239400447,3.21464116150854));
#57985=CARTESIAN_POINT('Ctrl Pts',(17.8944576250494,0.00817944857551684,
2.2875691909004));
#57986=CARTESIAN_POINT('Ctrl Pts',(17.9030245260052,1.36815405871329,2.28703275437041));
#57987=CARTESIAN_POINT('Ctrl Pts',(17.911586634633,2.7281306172685,2.28650324952679));
#57988=CARTESIAN_POINT('Ctrl Pts',(17.9201535355888,4.08810522740628,2.28596681299679));
#57989=CARTESIAN_POINT('Ctrl Pts',(17.2634879094926,0.00962372236703112,
1.42927972685571));
#57990=CARTESIAN_POINT('Ctrl Pts',(17.2717012892452,1.36958819872823,1.42064856538643));
#57991=CARTESIAN_POINT('Ctrl Pts',(17.2799243919317,2.72955178630459,1.41200698847874));
#57992=CARTESIAN_POINT('Ctrl Pts',(17.2881377716844,4.08951626266578,1.40337582700946));
#57993=CARTESIAN_POINT('Ctrl Pts',(16.875007029906,0.0048281666224073,0.905562213293497));
#57994=CARTESIAN_POINT('Ctrl Pts',(16.8789212630212,1.36470105924659,0.885765429291508));
#57995=CARTESIAN_POINT('Ctrl Pts',(16.882837602917,2.72458396387897,0.865986258071026));
#57996=CARTESIAN_POINT('Ctrl Pts',(16.8867518360321,4.08445685650315,0.846189474069038));
#57997=CARTESIAN_POINT('Ctrl Pts',(16.6859947282585,-0.000213685071588643,
0.653010349651272));
#57998=CARTESIAN_POINT('Ctrl Pts',(16.6862555279244,1.35951145025449,0.625670116550428));
#57999=CARTESIAN_POINT('Ctrl Pts',(16.6865163275903,2.71923658558057,0.598329883449584));
#58000=CARTESIAN_POINT('Ctrl Pts',(16.6867771272561,4.07896172090665,0.57098965034874));
#58001=CARTESIAN_POINT('',(21.1416094924623,2.04071649659929,6.62999999999999));
#58002=CARTESIAN_POINT('Ctrl Pts',(25.4512489060474,0.000557793871117651,
12.6480025703997));
#58003=CARTESIAN_POINT('Ctrl Pts',(25.453101108281,1.36055653259993,12.6480008567999));
#58004=CARTESIAN_POINT('Ctrl Pts',(25.4549533105147,2.72055527132873,12.6479991432001));
#58005=CARTESIAN_POINT('Ctrl Pts',(25.4568055127483,4.08055401005754,12.6479974296003));
#58006=CARTESIAN_POINT('Ctrl Pts',(25.2761532109731,0.000795927984841995,
12.3850804994989));
#58007=CARTESIAN_POINT('Ctrl Pts',(25.277851623458,1.36079487814099,12.3850766366272));
#58008=CARTESIAN_POINT('Ctrl Pts',(25.2795515965695,2.72079382022715,12.3850728170873));
#58009=CARTESIAN_POINT('Ctrl Pts',(25.2812500090543,4.0807927703833,12.3850689542157));
#58010=CARTESIAN_POINT('Ctrl Pts',(25.0385405727546,0.00107944402204348,
12.0284981506081));
#58011=CARTESIAN_POINT('Ctrl Pts',(25.040013789292,1.36107866148558,12.0284901984931));
#58012=CARTESIAN_POINT('Ctrl Pts',(25.0414879191271,2.72107788268626,12.0284822784796));
#58013=CARTESIAN_POINT('Ctrl Pts',(25.0429611356646,4.08107710014979,12.0284743263647));
#58014=CARTESIAN_POINT('Ctrl Pts',(24.5346770904967,0.00153952329737014,
11.2801401659155));
#58015=CARTESIAN_POINT('Ctrl Pts',(24.5356564959609,1.36153920365418,11.2801229600891));
#58016=CARTESIAN_POINT('Ctrl Pts',(24.5366361205139,2.72153887642349,11.2801057514123));
#58017=CARTESIAN_POINT('Ctrl Pts',(24.5376155259781,4.08153855678031,11.2800885455859));
#58018=CARTESIAN_POINT('Ctrl Pts',(23.7748717062593,0.00195060306715209,
10.1720733370841));
#58019=CARTESIAN_POINT('Ctrl Pts',(23.7751011060668,1.36195069280139,10.1720434504722));
#58020=CARTESIAN_POINT('Ctrl Pts',(23.7753283620544,2.72195078848062,10.1720135255144));
#58021=CARTESIAN_POINT('Ctrl Pts',(23.7755577618618,4.08195087821486,10.1719836389024));
#58022=CARTESIAN_POINT('Ctrl Pts',(22.5874547933106,0.00176250665503241,
8.52818644438044));
#58023=CARTESIAN_POINT('Ctrl Pts',(22.5867557909889,1.36176241103452,8.52815645805608));
#58024=CARTESIAN_POINT('Ctrl Pts',(22.5860591031456,2.72176230689818,8.52812649967298));
#58025=CARTESIAN_POINT('Ctrl Pts',(22.5853601008239,4.08176221127767,8.52809651334861));
#58026=CARTESIAN_POINT('Ctrl Pts',(21.7214346225638,0.00113305483753488,
7.38990420970681));
#58027=CARTESIAN_POINT('Ctrl Pts',(21.7204825968315,1.36113270990459,7.38988970735517));
#58028=CARTESIAN_POINT('Ctrl Pts',(21.7195116027229,2.72113238671198,7.38987483226514));
#58029=CARTESIAN_POINT('Ctrl Pts',(21.7185595769906,4.08113204177903,7.3898603299135));
#58030=CARTESIAN_POINT('Ctrl Pts',(21.143061504949,0.000717013383189635,
6.63001173766479));
#58031=CARTESIAN_POINT('Ctrl Pts',(21.1420934966245,1.36071666886059,6.63000391255492));
#58032=CARTESIAN_POINT('Ctrl Pts',(21.1411254883,2.72071632433799,6.62999608744506));
#58033=CARTESIAN_POINT('Ctrl Pts',(21.1401574799756,4.0807159798154,6.62998826233519));
#58034=CARTESIAN_POINT('',(25.4540272093978,2.04055590196433,12.648));
#58035=CARTESIAN_POINT('Ctrl Pts',(30.3222847700924,-0.00413483878088493,
18.6660068644751));
#58036=CARTESIAN_POINT('Ctrl Pts',(30.319338154389,1.35586263314915,18.6660022881605));
#58037=CARTESIAN_POINT('Ctrl Pts',(30.3163915386857,2.71586010507919,18.6659977118459));
#58038=CARTESIAN_POINT('Ctrl Pts',(30.3134449229822,4.07585757700923,18.6659931355313));
#58039=CARTESIAN_POINT('Ctrl Pts',(28.1822868666683,-0.00877780704942276,
16.7706615754742));
#58040=CARTESIAN_POINT('Ctrl Pts',(28.1864353099662,1.35122688309983,16.7706138302738));
#58041=CARTESIAN_POINT('Ctrl Pts',(28.1920233651988,2.71125915457337,16.7706168674462));
#58042=CARTESIAN_POINT('Ctrl Pts',(28.1961718099026,4.07126384474955,16.7705691222953));
#58043=CARTESIAN_POINT('Ctrl Pts',(26.9814250093985,-0.0015252724597002,
14.9457017822533));
#58044=CARTESIAN_POINT('Ctrl Pts',(26.9842959290968,1.35846869411807,14.9457149724762));
#58045=CARTESIAN_POINT('Ctrl Pts',(26.9881290061344,2.71847349676129,14.9457374841088));
#58046=CARTESIAN_POINT('Ctrl Pts',(26.9909999267723,4.07846746334965,14.9457506743408));
#58047=CARTESIAN_POINT('Ctrl Pts',(25.4512489033343,0.000555801717781314,
12.6480025704022));
#58048=CARTESIAN_POINT('Ctrl Pts',(25.4531011064722,1.36055520449771,12.6480008568016));
#58049=CARTESIAN_POINT('Ctrl Pts',(25.4549533096103,2.72055460727762,12.6479991432009));
#58050=CARTESIAN_POINT('Ctrl Pts',(25.4568055127483,4.08055401005754,12.6479974296003));
#58051=CARTESIAN_POINT('',(30.3178648443792,2.03586236518943,18.6659999999999));
#58052=CARTESIAN_POINT('Ctrl Pts',(44.3060709912999,0.501825342747216,24.6840442872876));
#58053=CARTESIAN_POINT('Ctrl Pts',(44.2037274807061,1.85798098503677,24.684066745284));
#58054=CARTESIAN_POINT('Ctrl Pts',(44.1013837137367,3.21413663472216,24.684089198907));
#58055=CARTESIAN_POINT('Ctrl Pts',(43.9990402031475,4.5702922770116,24.6841116569036));
#58056=CARTESIAN_POINT('Ctrl Pts',(43.5190253308226,0.442431104389339,24.6077945998755));
#58057=CARTESIAN_POINT('Ctrl Pts',(43.4225063663672,1.79903503321773,24.6078001904995));
#58058=CARTESIAN_POINT('Ctrl Pts',(43.3262381461302,3.15563172830434,24.6078100586932));
#58059=CARTESIAN_POINT('Ctrl Pts',(43.2297191772901,4.51223565725923,24.6078156492424));
#58060=CARTESIAN_POINT('Ctrl Pts',(42.281953252035,0.357580859065014,24.4341272831452));
#58061=CARTESIAN_POINT('Ctrl Pts',(42.1948238660848,1.71481412833685,24.434108345902));
#58062=CARTESIAN_POINT('Ctrl Pts',(42.1075870938005,3.0720521269536,24.434087295295));
#58063=CARTESIAN_POINT('Ctrl Pts',(42.0204577097281,4.42928539614273,24.4340683580887));
#58064=CARTESIAN_POINT('Ctrl Pts',(39.7590447329804,0.209255798855571,23.9283169242352));
#58065=CARTESIAN_POINT('Ctrl Pts',(39.6912109919964,1.5676408818353,23.9282776137135));
#58066=CARTESIAN_POINT('Ctrl Pts',(39.6235574611987,2.92602127280361,23.9282403159865));
#58067=CARTESIAN_POINT('Ctrl Pts',(39.5557237170632,4.2844063558654,23.9282010054296));
#58068=CARTESIAN_POINT('Ctrl Pts',(36.2988021098604,0.0624334299665293,
22.7904348263529));
#58069=CARTESIAN_POINT('Ctrl Pts',(36.259739607807,1.42202689650176,22.7904573128975));
#58070=CARTESIAN_POINT('Ctrl Pts',(36.2205336224352,2.78162409564511,22.7904779882549));
#58071=CARTESIAN_POINT('Ctrl Pts',(36.1814711228908,4.14121756211507,22.7905004748311));
#58072=CARTESIAN_POINT('Ctrl Pts',(33.2830669754168,0.0134785075079505,
20.9642163836828));
#58073=CARTESIAN_POINT('Ctrl Pts',(33.266042022136,1.3733999950468,20.9642333108646));
#58074=CARTESIAN_POINT('Ctrl Pts',(33.2490275122761,2.73332557982227,20.964248077881));
#58075=CARTESIAN_POINT('Ctrl Pts',(33.2320025588127,4.09324706728946,20.9642650051006));
#58076=CARTESIAN_POINT('Ctrl Pts',(31.3600228082259,-0.00140329014482304,
19.5545670903082));
#58077=CARTESIAN_POINT('Ctrl Pts',(31.3529985429648,1.3585971916633,19.5545657430667));
#58078=CARTESIAN_POINT('Ctrl Pts',(31.3460228944958,2.71859422757804,19.554566141491));
#58079=CARTESIAN_POINT('Ctrl Pts',(31.3389986283846,4.07859470944643,19.5545647942189));
#58080=CARTESIAN_POINT('Ctrl Pts',(30.6632779300613,-0.00339318635361294,
18.9680312409348));
#58081=CARTESIAN_POINT('Ctrl Pts',(30.6591100208208,1.35661121146251,18.9680286797402));
#58082=CARTESIAN_POINT('Ctrl Pts',(30.6549852558424,2.71662066980922,18.968023788134));
#58083=CARTESIAN_POINT('Ctrl Pts',(30.6508173458474,4.07662506753684,18.9680212269803));
#58084=CARTESIAN_POINT('Ctrl Pts',(30.321935879594,-0.00413360349513863,
18.6656978544223));
#58085=CARTESIAN_POINT('Ctrl Pts',(30.318990489166,1.35587510023538,18.6656932760086));
#58086=CARTESIAN_POINT('Ctrl Pts',(30.3160450546095,2.71588379879152,18.6656886999778));
#58087=CARTESIAN_POINT('Ctrl Pts',(30.3130996641822,4.07589250252213,18.6656841215641));
#58088=CARTESIAN_POINT('',(44.1517615497858,2.53598100128542,24.684));
#58089=CARTESIAN_POINT('Ctrl Pts',(49.367596314931,0.956500241803234,24.6840252060176));
#58090=CARTESIAN_POINT('Ctrl Pts',(49.2262927990192,2.30914179729203,24.6840084019793));
#58091=CARTESIAN_POINT('Ctrl Pts',(49.0849892831073,3.66178335278082,24.6839915979409));
#58092=CARTESIAN_POINT('Ctrl Pts',(48.9436857671955,5.01442490826962,24.6839747939026));
#58093=CARTESIAN_POINT('Ctrl Pts',(48.9249563174813,0.91026051062961,24.7319912218939));
#58094=CARTESIAN_POINT('Ctrl Pts',(48.7870744516188,2.26326030531412,24.7319949786716));
#58095=CARTESIAN_POINT('Ctrl Pts',(48.6493002916307,3.61626896125776,24.7319975111381));
#58096=CARTESIAN_POINT('Ctrl Pts',(48.5114184254269,4.96926875591419,24.7320012679197));
#58097=CARTESIAN_POINT('Ctrl Pts',(48.2454451876077,0.842024097628023,24.7841312821754));
#58098=CARTESIAN_POINT('Ctrl Pts',(48.1129276720479,2.19556213273895,24.7841582385071));
#58099=CARTESIAN_POINT('Ctrl Pts',(47.9803793431562,3.54909669207479,24.7841839725438));
#58100=CARTESIAN_POINT('Ctrl Pts',(47.8478618276941,4.90263472719673,24.7842109288793));
#58101=CARTESIAN_POINT('Ctrl Pts',(46.6888479202391,0.694486082024801,24.8361224907741));
#58102=CARTESIAN_POINT('Ctrl Pts',(46.5684234944341,2.04917028244214,24.8361780798375));
#58103=CARTESIAN_POINT('Ctrl Pts',(46.4481124839905,3.40386435489333,24.8362331625796));
#58104=CARTESIAN_POINT('Ctrl Pts',(46.3276880578261,4.75854855527939,24.8362887516446));
#58105=CARTESIAN_POINT('Ctrl Pts',(45.4053646426555,0.584777912483909,24.7905806974873));
#58106=CARTESIAN_POINT('Ctrl Pts',(45.2947746656324,1.94030222186044,24.7906247929504));
#58107=CARTESIAN_POINT('Ctrl Pts',(45.1841696299648,3.29582325494898,24.7906652802213));
#58108=CARTESIAN_POINT('Ctrl Pts',(45.0735796529894,4.65134756433589,24.7907093756959));
#58109=CARTESIAN_POINT('Ctrl Pts',(44.3052665433902,0.501764637226404,24.6839663391593));
#58110=CARTESIAN_POINT('Ctrl Pts',(44.202929718831,1.85791102879411,24.6839887797553));
#58111=CARTESIAN_POINT('Ctrl Pts',(44.1005928942718,3.21405742036182,24.6840112203513));
#58112=CARTESIAN_POINT('Ctrl Pts',(43.9982560697126,4.57020381192954,24.6840336609473));
#58113=CARTESIAN_POINT('',(49.1556413769138,2.98545936007418,24.684));
#58114=CARTESIAN_POINT('Ctrl Pts',(61.5167105273182,2.54668955743568,18.6668749079439));
#58115=CARTESIAN_POINT('Ctrl Pts',(61.3290483861646,3.89369298763947,18.6662363925884));
#58116=CARTESIAN_POINT('Ctrl Pts',(61.1413862320074,5.24069641592315,18.6655978761149));
#58117=CARTESIAN_POINT('Ctrl Pts',(60.9537240908538,6.58769984612695,18.6649593607594));
#58118=CARTESIAN_POINT('Ctrl Pts',(61.263103455342,2.51156902512523,19.1131892935311));
#58119=CARTESIAN_POINT('Ctrl Pts',(61.0749027843424,3.85849731336309,19.1127174727806));
#58120=CARTESIAN_POINT('Ctrl Pts',(60.8867721832384,5.20543594818961,19.1122516770937));
#58121=CARTESIAN_POINT('Ctrl Pts',(60.6985715121748,6.55236423641801,19.1117798563378));
#58122=CARTESIAN_POINT('Ctrl Pts',(60.590040319334,2.41777554679417,20.1912494551796));
#58123=CARTESIAN_POINT('Ctrl Pts',(60.4003560171827,3.76449700545968,20.191255703466));
#58124=CARTESIAN_POINT('Ctrl Pts',(60.2106481477568,5.1112145815907,20.1912513624428));
#58125=CARTESIAN_POINT('Ctrl Pts',(60.0209638456271,6.45793604025974,20.1912576107388));
#58126=CARTESIAN_POINT('Ctrl Pts',(59.4895781905362,2.26151401138549,21.4128488549465));
#58127=CARTESIAN_POINT('Ctrl Pts',(59.2977245032483,3.60792694709506,21.4133840492524));
#58128=CARTESIAN_POINT('Ctrl Pts',(59.1058315470634,4.9543338671036,21.413920162527));
#58129=CARTESIAN_POINT('Ctrl Pts',(58.9139778598114,6.30074680281867,21.414455356832));
#58130=CARTESIAN_POINT('Ctrl Pts',(57.9960406900284,2.04849564503984,22.3558602231261));
#58131=CARTESIAN_POINT('Ctrl Pts',(57.8047660818527,3.39499098804245,22.3564123469393));
#58132=CARTESIAN_POINT('Ctrl Pts',(57.6135147306327,4.74148873290627,22.3569599420449));
#58133=CARTESIAN_POINT('Ctrl Pts',(57.4222401224356,6.08798407590668,22.3575120658621));
#58134=CARTESIAN_POINT('Ctrl Pts',(57.0698741394985,1.91749687991536,22.7723218917253));
#58135=CARTESIAN_POINT('Ctrl Pts',(56.8805882431121,3.2642740689222,22.7727214343706));
#58136=CARTESIAN_POINT('Ctrl Pts',(56.6912424961737,4.61104196764428,22.7731176132384));
#58137=CARTESIAN_POINT('Ctrl Pts',(56.501956599842,5.95781915665962,22.7735171558868));
#58138=CARTESIAN_POINT('Ctrl Pts',(56.3512933832801,1.81739755300788,23.0411120395903));
#58139=CARTESIAN_POINT('Ctrl Pts',(56.1644223104387,3.16451153197724,23.041370704679));
#58140=CARTESIAN_POINT('Ctrl Pts',(55.9776124637286,4.51163236434906,23.0416218085428));
#58141=CARTESIAN_POINT('Ctrl Pts',(55.7907413908312,5.85874634331215,23.0418804736386));
#58142=CARTESIAN_POINT('Ctrl Pts',(55.9375938125836,1.76021042751909,23.1895737845226));
#58143=CARTESIAN_POINT('Ctrl Pts',(55.7523080868053,3.10754254014476,23.1897559420741));
#58144=CARTESIAN_POINT('Ctrl Pts',(55.5670201212181,4.45487370505996,23.189930543941));
#58145=CARTESIAN_POINT('Ctrl Pts',(55.3817343954418,5.8022058176865,23.1901127014995));
#58146=CARTESIAN_POINT('Ctrl Pts',(54.7224264440694,1.59337924540381,23.5835239931621));
#58147=CARTESIAN_POINT('Ctrl Pts',(54.5425349310206,2.94145569457832,23.5834560816272));
#58148=CARTESIAN_POINT('Ctrl Pts',(54.362649133093,4.28952928057054,23.5833833295269));
#58149=CARTESIAN_POINT('Ctrl Pts',(54.182757620039,5.63760572974766,23.5833154179965));
#58150=CARTESIAN_POINT('Ctrl Pts',(52.3183753604669,1.28300286500095,24.2171514519698));
#58151=CARTESIAN_POINT('Ctrl Pts',(52.1541392715394,2.63311089716375,24.2169378345412));
#58152=CARTESIAN_POINT('Ctrl Pts',(51.9899010441846,3.98322045499549,24.2167309505167));
#58153=CARTESIAN_POINT('Ctrl Pts',(51.825664955259,5.3333284871569,24.2165173330819));
#58154=CARTESIAN_POINT('Ctrl Pts',(50.3762919306573,1.06185100093138,24.574737313459));
#58155=CARTESIAN_POINT('Ctrl Pts',(50.2270882512909,2.41367972324444,24.574684778323));
#58156=CARTESIAN_POINT('Ctrl Pts',(50.0779440671583,3.76551046496078,24.5746027634213));
#58157=CARTESIAN_POINT('Ctrl Pts',(49.9287403877375,5.11733918727201,24.5745502283122));
#58158=CARTESIAN_POINT('Ctrl Pts',(49.3672237994714,0.956442455724845,24.6840657814739));
#58159=CARTESIAN_POINT('Ctrl Pts',(49.2259220751389,2.30909523778757,24.6840489905667));
#58160=CARTESIAN_POINT('Ctrl Pts',(49.0846203287234,3.66174801910072,24.6840322106014));
#58161=CARTESIAN_POINT('Ctrl Pts',(48.943318604391,5.01440080116346,24.6840154196942));
#58162=CARTESIAN_POINT('',(61.2351702347366,4.56718724108023,18.6660000000004));
#58163=CARTESIAN_POINT('Ctrl Pts',(64.4551411469049,2.94895124118378,12.643128511618));
#58164=CARTESIAN_POINT('Ctrl Pts',(64.2634490243396,4.29537004039075,12.6463761705398));
#58165=CARTESIAN_POINT('Ctrl Pts',(64.0717569017743,5.64178883959772,12.6496238294616));
#58166=CARTESIAN_POINT('Ctrl Pts',(63.880064779209,6.9882076388047,12.6528714883835));
#58167=CARTESIAN_POINT('Ctrl Pts',(64.3479516013103,2.93312045091166,12.879447083032));
#58168=CARTESIAN_POINT('Ctrl Pts',(64.1565846949601,4.27958819113799,12.8820318362782));
#58169=CARTESIAN_POINT('Ctrl Pts',(63.9654114328152,5.6260806947179,12.8844859516373));
#58170=CARTESIAN_POINT('Ctrl Pts',(63.7740445264651,6.97254843494423,12.8870707048835));
#58171=CARTESIAN_POINT('Ctrl Pts',(64.1837627981494,2.90927418572721,13.2358935474039));
#58172=CARTESIAN_POINT('Ctrl Pts',(63.9933586114422,4.25587812903196,13.2373129480525));
#58173=CARTESIAN_POINT('Ctrl Pts',(63.8027403511282,5.60245438568209,13.2388840392621));
#58174=CARTESIAN_POINT('Ctrl Pts',(63.6123361644209,6.94905832898685,13.2403034399106));
#58175=CARTESIAN_POINT('Ctrl Pts',(63.8565165085826,2.86262631538198,13.9401757025571));
#58176=CARTESIAN_POINT('Ctrl Pts',(63.6676797875646,4.2094547640839,13.9398268183957));
#58177=CARTESIAN_POINT('Ctrl Pts',(63.4788891542148,5.5562885775365,13.9394767506199));
#58178=CARTESIAN_POINT('Ctrl Pts',(63.2900524331968,6.90311702623842,13.9391278664585));
#58179=CARTESIAN_POINT('Ctrl Pts',(63.0373241745919,2.7503468228343,15.6623359995965));
#58180=CARTESIAN_POINT('Ctrl Pts',(62.853358990902,4.09784400417783,15.6578276836229));
#58181=CARTESIAN_POINT('Ctrl Pts',(62.6693095807093,5.44533158427596,15.6533087285849));
#58182=CARTESIAN_POINT('Ctrl Pts',(62.4853443970193,6.79282876561949,15.6488004126113));
#58183=CARTESIAN_POINT('Ctrl Pts',(62.1072697672375,2.62849234465526,17.6291609829972));
#58184=CARTESIAN_POINT('Ctrl Pts',(61.9211507613171,3.97569482112501,17.6267449384719));
#58185=CARTESIAN_POINT('Ctrl Pts',(61.7340069286968,5.3227604947646,17.625311906549));
#58186=CARTESIAN_POINT('Ctrl Pts',(61.5478879227764,6.66996297123436,17.6228958620238));
#58187=CARTESIAN_POINT('Ctrl Pts',(61.5166608776681,2.54670163095592,18.6669577173854));
#58188=CARTESIAN_POINT('Ctrl Pts',(61.3290004490471,3.89369203770546,18.6663192391287));
#58189=CARTESIAN_POINT('Ctrl Pts',(61.1413400204261,5.240682444455,18.665680760872));
#58190=CARTESIAN_POINT('Ctrl Pts',(60.9536795918051,6.58767285120455,18.6650422826153));
#58191=CARTESIAN_POINT('',(64.167602963057,4.96857943999424,12.6480000000007));
#58192=CARTESIAN_POINT('Ctrl Pts',(66.7631910634513,3.27249821468361,6.63302015235614));
#58193=CARTESIAN_POINT('Ctrl Pts',(66.6090104253407,4.6237288674264,6.63100671745196));
#58194=CARTESIAN_POINT('Ctrl Pts',(66.4548297872301,5.97495952016919,6.62899328254778));
#58195=CARTESIAN_POINT('Ctrl Pts',(66.3006491491196,7.32619017291198,6.62697984764361));
#58196=CARTESIAN_POINT('Ctrl Pts',(66.5144891466017,3.24514897378173,7.32332685183486));
#58197=CARTESIAN_POINT('Ctrl Pts',(66.3551290019871,4.59580056453943,7.32187855047366));
#58198=CARTESIAN_POINT('Ctrl Pts',(66.1953212237692,5.94636797561221,7.32055770621773));
#58199=CARTESIAN_POINT('Ctrl Pts',(66.0359610791546,7.29701956636991,7.31910940485653));
#58200=CARTESIAN_POINT('Ctrl Pts',(66.1915309888886,3.20756373571229,8.33471690257991));
#58201=CARTESIAN_POINT('Ctrl Pts',(66.0196634412346,4.55670888345873,8.33655180786372));
#58202=CARTESIAN_POINT('Ctrl Pts',(65.8477742059612,5.90585017783967,8.33839439268998));
#58203=CARTESIAN_POINT('Ctrl Pts',(65.6759066583072,7.25499532558611,8.34022929797379));
#58204=CARTESIAN_POINT('Ctrl Pts',(65.6053523490308,3.12335915915328,9.92777824589967));
#58205=CARTESIAN_POINT('Ctrl Pts',(65.4195611156543,4.47060257180804,9.93331106670633));
#58206=CARTESIAN_POINT('Ctrl Pts',(65.2336127473442,5.81781667090629,9.93888534635652));
#58207=CARTESIAN_POINT('Ctrl Pts',(65.0478215139677,7.16506008356105,9.94441816716317));
#58208=CARTESIAN_POINT('Ctrl Pts',(65.2980709440698,3.07680103779862,10.698179922846));
#58209=CARTESIAN_POINT('Ctrl Pts',(65.1081306893196,4.42345821365678,10.7044812911298));
#58210=CARTESIAN_POINT('Ctrl Pts',(64.9181117320464,5.77010091702523,10.7108042261835));
#58211=CARTESIAN_POINT('Ctrl Pts',(64.7281714772961,7.11675809288339,10.7171055944672));
#58212=CARTESIAN_POINT('Ctrl Pts',(64.9198814657602,3.01893190960619,11.6037177274062));
#58213=CARTESIAN_POINT('Ctrl Pts',(64.7272386716612,4.3652056163787,11.6098061088883));
#58214=CARTESIAN_POINT('Ctrl Pts',(64.5345650233203,5.71147224923531,11.6158943535898));
#58215=CARTESIAN_POINT('Ctrl Pts',(64.3419222292212,7.05774595600782,11.6219827350719));
#58216=CARTESIAN_POINT('Ctrl Pts',(64.6569638176777,2.97875922081063,12.1978206672481));
#58217=CARTESIAN_POINT('Ctrl Pts',(64.4645407384521,4.3250695329532,12.2026347082501));
#58218=CARTESIAN_POINT('Ctrl Pts',(64.2721091536059,5.67138056268601,12.2074466881067));
#58219=CARTESIAN_POINT('Ctrl Pts',(64.0796860743802,7.01769087482858,12.2122607291087));
#58220=CARTESIAN_POINT('Ctrl Pts',(64.4551411469049,2.94895124118378,12.643128511618));
#58221=CARTESIAN_POINT('Ctrl Pts',(64.2634490243396,4.29537004039075,12.6463761705398));
#58222=CARTESIAN_POINT('Ctrl Pts',(64.0717569017743,5.64178883959772,12.6496238294616));
#58223=CARTESIAN_POINT('Ctrl Pts',(63.880064779209,6.9882076388047,12.6528714883835));
#58224=CARTESIAN_POINT('',(66.5319201062854,5.2993441937978,6.62999999999987));
#58225=CARTESIAN_POINT('Ctrl Pts',(73.6772000252932,5.16855773887608,0.190556358283422));
#58226=CARTESIAN_POINT('Ctrl Pts',(73.0223213239028,6.32715830579005,0.471418061534128));
#58227=CARTESIAN_POINT('Ctrl Pts',(72.3674437003221,7.48575858003024,0.752278931816456));
#58228=CARTESIAN_POINT('Ctrl Pts',(71.7125649990545,8.64435914691087,1.03314063497225));
#58229=CARTESIAN_POINT('Ctrl Pts',(73.3568906352367,4.96394356197773,0.287771904083843));
#58230=CARTESIAN_POINT('Ctrl Pts',(72.7322924584517,6.14260682030999,0.555547261873308));
#58231=CARTESIAN_POINT('Ctrl Pts',(72.1070367739604,7.32144864826471,0.823830761013211));
#58232=CARTESIAN_POINT('Ctrl Pts',(71.4824385222558,8.500111926944,1.09160617670262));
#58233=CARTESIAN_POINT('Ctrl Pts',(72.6506490423299,4.5449564025123,0.519060452703995));
#58234=CARTESIAN_POINT('Ctrl Pts',(72.0995945512668,5.77032628529454,0.752863921322597));
#58235=CARTESIAN_POINT('Ctrl Pts',(71.5484722850479,6.99561665985264,0.986731326285281));
#58236=CARTESIAN_POINT('Ctrl Pts',(70.9974177862621,8.22098653357535,1.22053480218908));
#58237=CARTESIAN_POINT('Ctrl Pts',(71.7208328945397,4.12810236418734,0.920670038259505));
#58238=CARTESIAN_POINT('Ctrl Pts',(71.2816558446986,5.40575802043638,1.09320539300391));
#58239=CARTESIAN_POINT('Ctrl Pts',(70.8428390686283,6.68358189489245,1.26556719727816));
#58240=CARTESIAN_POINT('Ctrl Pts',(70.4036620598385,7.96123757030904,1.43810253224744));
#58241=CARTESIAN_POINT('Ctrl Pts',(71.1121435558323,3.91335904361009,1.24156644857775));
#58242=CARTESIAN_POINT('Ctrl Pts',(70.7451023181714,5.21686775824389,1.37107739155829));
#58243=CARTESIAN_POINT('Ctrl Pts',(70.3769195816328,6.52017282873975,1.50138101937032));
#58244=CARTESIAN_POINT('Ctrl Pts',(70.0098782139044,7.82368152016941,1.63089205267299));
#58245=CARTESIAN_POINT('Ctrl Pts',(70.7268083932345,3.79039665573098,1.45971612003484));
#58246=CARTESIAN_POINT('Ctrl Pts',(70.4038475319979,5.10816401749319,1.56223160793066));
#58247=CARTESIAN_POINT('Ctrl Pts',(70.0802934739855,6.42586804043829,1.66518735010833));
#58248=CARTESIAN_POINT('Ctrl Pts',(69.7573325451574,7.74363539498338,1.76770288816874));
#58249=CARTESIAN_POINT('Ctrl Pts',(70.2740603998417,3.66820000092256,1.74447590965103));
#58250=CARTESIAN_POINT('Ctrl Pts',(70.0004869733914,4.99923228800803,1.81550491446754));
#58251=CARTESIAN_POINT('Ctrl Pts',(69.7261539195068,6.33012671143447,1.88708998584075));
#58252=CARTESIAN_POINT('Ctrl Pts',(69.452580406501,7.66115898281112,1.95811905401802));
#58253=CARTESIAN_POINT('Ctrl Pts',(69.8645442359654,3.58028617064753,2.03975339886061));
#58254=CARTESIAN_POINT('Ctrl Pts',(69.6308079493548,4.91966896788311,2.08422343244304));
#58255=CARTESIAN_POINT('Ctrl Pts',(69.3961593101812,6.25895087375893,2.12935401774862));
#58256=CARTESIAN_POINT('Ctrl Pts',(69.162422919613,7.59833365949849,2.17382412659732));
#58257=CARTESIAN_POINT('Ctrl Pts',(69.6001682821458,3.53233689289179,2.25060622748988));
#58258=CARTESIAN_POINT('Ctrl Pts',(69.3891578707081,4.87579662728807,2.27944637857042));
#58259=CARTESIAN_POINT('Ctrl Pts',(69.177764953627,6.21917813634206,2.30861486850998));
#58260=CARTESIAN_POINT('Ctrl Pts',(68.9667544986049,7.56263786182499,2.33745505700294));
#58261=CARTESIAN_POINT('Ctrl Pts',(69.4542644409521,3.50811556510099,2.37266587496734));
#58262=CARTESIAN_POINT('Ctrl Pts',(69.2554779909857,4.85353840156605,2.39299440880989));
#58263=CARTESIAN_POINT('Ctrl Pts',(69.0551783441871,6.19878494315157,2.41437407306302));
#58264=CARTESIAN_POINT('Ctrl Pts',(68.8563917218001,7.54420775952879,2.43470272667616));
#58265=CARTESIAN_POINT('Ctrl Pts',(69.1063126801324,3.45392517384496,2.67613303504415));
#58266=CARTESIAN_POINT('Ctrl Pts',(68.9327041121834,4.80332717113759,2.67855721319536));
#58267=CARTESIAN_POINT('Ctrl Pts',(68.7619611221849,6.15298634546019,2.67921927385303));
#58268=CARTESIAN_POINT('Ctrl Pts',(68.5883528807529,7.50238837205674,2.68164325122055));
#58269=CARTESIAN_POINT('Ctrl Pts',(68.5226423483623,3.38434890663629,3.23347205056578));
#58270=CARTESIAN_POINT('Ctrl Pts',(68.3870872529164,4.73769746898268,3.20779650773751));
#58271=CARTESIAN_POINT('Ctrl Pts',(68.2523866052647,6.09104928826278,3.18180222884627));
#58272=CARTESIAN_POINT('Ctrl Pts',(68.1168316071785,7.44439785098028,3.15612664969976));
#58273=CARTESIAN_POINT('Ctrl Pts',(67.694496492102,3.33750087776864,4.42270985506997));
#58274=CARTESIAN_POINT('Ctrl Pts',(67.5680466748002,4.69126331549113,4.38548802714617));
#58275=CARTESIAN_POINT('Ctrl Pts',(67.4410408793703,6.04506547121618,4.34835845428985));
#58276=CARTESIAN_POINT('Ctrl Pts',(67.3145909987177,7.39882791346432,4.31113663687802));
#58277=CARTESIAN_POINT('Ctrl Pts',(67.1258634544533,3.30676257207483,5.67411595656781));
#58278=CARTESIAN_POINT('Ctrl Pts',(66.9814730735797,4.65918845340503,5.65288869680402));
#58279=CARTESIAN_POINT('Ctrl Pts',(66.83772386963,6.01163361516273,5.63136136659782));
#58280=CARTESIAN_POINT('Ctrl Pts',(66.693333561815,7.36405949868983,5.61013407264264));
#58281=CARTESIAN_POINT('Ctrl Pts',(66.8856192780979,3.28558579390195,6.3034280330774));
#58282=CARTESIAN_POINT('Ctrl Pts',(66.734365096802,4.63730028384587,6.29421068413704));
#58283=CARTESIAN_POINT('Ctrl Pts',(66.58213266316,5.9889814423923,6.28545083230468));
#58284=CARTESIAN_POINT('Ctrl Pts',(66.4308783703976,7.3406959285383,6.27623353549363));
#58285=CARTESIAN_POINT('Ctrl Pts',(66.7628337599032,3.27206241735065,6.63410327899077));
#58286=CARTESIAN_POINT('Ctrl Pts',(66.6086224407573,4.62347610990505,6.6321132270148));
#58287=CARTESIAN_POINT('Ctrl Pts',(66.4544143284188,5.97488991172763,6.63012167531874));
#58288=CARTESIAN_POINT('Ctrl Pts',(66.3002030096383,7.32630360429448,6.62813162317191));
#58289=CARTESIAN_POINT('',(72.6943757632035,6.90627177260518,0.612000000000049));
#58290=CARTESIAN_POINT('Ctrl Pts',(79.5980561168973,9.79488102600527,-1.92025417906537));
#58291=CARTESIAN_POINT('Ctrl Pts',(79.0286742320677,11.0149409033542,-1.72808096639347));
#58292=CARTESIAN_POINT('Ctrl Pts',(78.4592923472381,12.2350007807032,-1.53590775372157));
#58293=CARTESIAN_POINT('Ctrl Pts',(77.8899104624086,13.4550606580522,-1.34373454104967));
#58294=CARTESIAN_POINT('Ctrl Pts',(79.1741566879662,9.55093781207194,-1.62747314540123));
#58295=CARTESIAN_POINT('Ctrl Pts',(78.5266575000171,10.7270377262137,-1.38765912524391));
#58296=CARTESIAN_POINT('Ctrl Pts',(77.8806952279844,11.9041863724067,-1.14995078261078));
#58297=CARTESIAN_POINT('Ctrl Pts',(77.2331959798932,13.0802862455097,-0.910136680054649));
#58298=CARTESIAN_POINT('Ctrl Pts',(78.5111339416338,9.08098342033927,-1.27556034622203));
#58299=CARTESIAN_POINT('Ctrl Pts',(77.7749706051526,10.187565205955,-0.978114370073764));
#58300=CARTESIAN_POINT('Ctrl Pts',(77.0384203562647,11.2937880799109,-0.680365554578324));
#58301=CARTESIAN_POINT('Ctrl Pts',(76.3022570349242,12.4003698795714,-0.382919590280686));
#58302=CARTESIAN_POINT('Ctrl Pts',(77.4831763160976,8.21812193305731,-0.881741433435836));
#58303=CARTESIAN_POINT('Ctrl Pts',(76.6879687540478,9.26872864098366,-0.543920625490695));
#58304=CARTESIAN_POINT('Ctrl Pts',(75.8930514554952,10.3194801010249,-0.206524782939603));
#58305=CARTESIAN_POINT('Ctrl Pts',(75.0978438820867,11.3700868032869,0.131296041635168));
#58306=CARTESIAN_POINT('Ctrl Pts',(76.6699028312841,7.50475073429994,-0.627389809719394));
#58307=CARTESIAN_POINT('Ctrl Pts',(75.8605684319178,8.54015089006858,-0.277402530357528));
#58308=CARTESIAN_POINT('Ctrl Pts',(75.0508678458463,9.57527060317076,0.0726661668725478));
#58309=CARTESIAN_POINT('Ctrl Pts',(74.2415334608095,10.6106707699136,0.422653443048392));
#58310=CARTESIAN_POINT('Ctrl Pts',(75.80573025497,6.75707546613834,-0.393749096424453));
#58311=CARTESIAN_POINT('Ctrl Pts',(75.0101325640915,7.80439560667266,-0.0470408174776192));
#58312=CARTESIAN_POINT('Ctrl Pts',(74.2147230665259,8.85183366407264,0.299507495459954));
#58313=CARTESIAN_POINT('Ctrl Pts',(73.4191253682831,9.89915379999267,0.646215780666534));
#58314=CARTESIAN_POINT('Ctrl Pts',(75.0458066034774,6.13922536294966,-0.198996877529824));
#58315=CARTESIAN_POINT('Ctrl Pts',(74.2854803652574,7.21759061042868,0.132625058966034));
#58316=CARTESIAN_POINT('Ctrl Pts',(73.5239941762248,8.29496715825229,0.464731466750703));
#58317=CARTESIAN_POINT('Ctrl Pts',(72.7636679833957,9.37333244442084,0.796353384288361));
#58318=CARTESIAN_POINT('Ctrl Pts',(74.3631103004922,5.62958316749681,-0.0144852711055081));
#58319=CARTESIAN_POINT('Ctrl Pts',(73.6484856916462,6.74484315518654,0.295796529234268));
#58320=CARTESIAN_POINT('Ctrl Pts',(72.934428597165,7.86059742247381,0.60581285019285));
#58321=CARTESIAN_POINT('Ctrl Pts',(72.2198039661113,8.97585739082152,0.916094660921293));
#58322=CARTESIAN_POINT('Ctrl Pts',(73.9160929284303,5.32217497724758,0.115709478461592));
#58323=CARTESIAN_POINT('Ctrl Pts',(73.2392816264558,6.46557061287508,0.407584897130259));
#58324=CARTESIAN_POINT('Ctrl Pts',(72.5615875732502,7.60823306211348,0.699849561231062));
#58325=CARTESIAN_POINT('Ctrl Pts',(71.8847763058192,8.75162872643185,0.991724964667882));
#58326=CARTESIAN_POINT('Ctrl Pts',(73.6763794821108,5.16849021502026,0.190830237853467));
#58327=CARTESIAN_POINT('Ctrl Pts',(73.0216365149966,6.32699523020028,0.471632851257021));
#58328=CARTESIAN_POINT('Ctrl Pts',(72.3668939389581,7.48550057019518,0.752435292217885));
#58329=CARTESIAN_POINT('Ctrl Pts',(71.7121509718286,8.6440055853625,1.03323790562819));
#58330=CARTESIAN_POINT('',(78.744,11.6249350354382,-1.632));
#58331=CARTESIAN_POINT('Ctrl Pts',(-66.7631905323708,3.2722402959031,6.63310021356383));
#58332=CARTESIAN_POINT('Ctrl Pts',(-66.6089890872461,4.62364551905875,6.63108830419267));
#58333=CARTESIAN_POINT('Ctrl Pts',(-66.454788368593,5.97505083079199,6.62907615047543));
#58334=CARTESIAN_POINT('Ctrl Pts',(-66.3005869234631,7.32645605394699,6.62706424110603));
#58335=CARTESIAN_POINT('Ctrl Pts',(-66.8801520480825,3.28511688844106,6.31812745992113));
#58336=CARTESIAN_POINT('Ctrl Pts',(-66.7294154291688,4.63691492746342,6.30905636882779));
#58337=CARTESIAN_POINT('Ctrl Pts',(-66.5758074951115,5.98836287185121,6.30095103402918));
#58338=CARTESIAN_POINT('Ctrl Pts',(-66.425070897001,7.34016091341009,6.29187993593875));
#58339=CARTESIAN_POINT('Ctrl Pts',(-67.2656923328878,3.32461709132614,5.28712579307929));
#58340=CARTESIAN_POINT('Ctrl Pts',(-67.1240316027416,4.67718487149427,5.25864400138529));
#58341=CARTESIAN_POINT('Ctrl Pts',(-66.983738489829,6.02990026804461,5.22971048647717));
#58342=CARTESIAN_POINT('Ctrl Pts',(-66.8420777497741,7.38246804714321,5.201228698056));
#58343=CARTESIAN_POINT('Ctrl Pts',(-68.0947647618052,3.34327433626794,3.65883664280228));
#58344=CARTESIAN_POINT('Ctrl Pts',(-67.9826229514963,4.698415843162,3.61464625653939));
#58345=CARTESIAN_POINT('Ctrl Pts',(-67.8693904320237,6.05332680022653,3.57118515922622));
#58346=CARTESIAN_POINT('Ctrl Pts',(-67.7572486296174,7.40846830879098,3.52699476767946));
#58347=CARTESIAN_POINT('Ctrl Pts',(-69.6077567772536,3.50670424092515,2.17712360811833));
#58348=CARTESIAN_POINT('Ctrl Pts',(-69.4065126173048,4.85388456367134,2.20093078770444));
#58349=CARTESIAN_POINT('Ctrl Pts',(-69.2043637928767,6.20103120513092,2.22527031105748));
#58350=CARTESIAN_POINT('Ctrl Pts',(-69.0031196394824,7.54821152812113,2.24907748678665));
#58351=CARTESIAN_POINT('Ctrl Pts',(-71.0306840271174,3.84389883696231,1.23932043725278));
#58352=CARTESIAN_POINT('Ctrl Pts',(-70.6764707998785,5.15752311784233,1.3634613121629));
#58353=CARTESIAN_POINT('Ctrl Pts',(-70.320394059464,6.47117910808559,1.48914321767995));
#58354=CARTESIAN_POINT('Ctrl Pts',(-69.9661808457267,7.78480338873587,1.61328408142497));
#58355=CARTESIAN_POINT('Ctrl Pts',(-72.5341132600611,4.47318246023834,0.554474346147679));
#58356=CARTESIAN_POINT('Ctrl Pts',(-71.9943868391019,5.7067749223203,0.783587502056807));
#58357=CARTESIAN_POINT('Ctrl Pts',(-71.4576484705403,6.9409738913966,1.01048513921957));
#58358=CARTESIAN_POINT('Ctrl Pts',(-70.917922027932,8.17456634908429,1.23959831118061));
#58359=CARTESIAN_POINT('Ctrl Pts',(-73.321583078895,4.94156553523102,0.298504751819751));
#58360=CARTESIAN_POINT('Ctrl Pts',(-72.7013339116048,6.1223415340885,0.56395096502215));
#58361=CARTESIAN_POINT('Ctrl Pts',(-72.0773277659962,7.30357890889758,0.832614564183271));
#58362=CARTESIAN_POINT('Ctrl Pts',(-71.4570786259261,8.4843549044123,1.09806075407501));
#58363=CARTESIAN_POINT('Ctrl Pts',(-73.676698823977,5.16839729396267,0.190716795481847));
#58364=CARTESIAN_POINT('Ctrl Pts',(-73.0218655138857,6.32701710217377,0.471559009605434));
#58365=CARTESIAN_POINT('Ctrl Pts',(-72.367033153576,7.48563679373651,0.75240041035525));
#58366=CARTESIAN_POINT('Ctrl Pts',(-71.7121998434778,8.64425660194844,1.03324262448473));
#58367=CARTESIAN_POINT('',(-72.6943757632042,6.90627177261614,0.611999999999845));
#58368=CARTESIAN_POINT('',(-66.5319201062853,5.29934419379849,6.63000000000032));
#58369=CARTESIAN_POINT('Ctrl Pts',(-64.4551381252455,2.94895079490255,12.6431351787018));
#58370=CARTESIAN_POINT('Ctrl Pts',(-64.2634452441834,4.29537501555654,12.6463828262949));
#58371=CARTESIAN_POINT('Ctrl Pts',(-64.0717523568639,5.64179923490367,12.6496304767655));
#58372=CARTESIAN_POINT('Ctrl Pts',(-63.8800594758019,6.98822345555767,12.6528781243586));
#58373=CARTESIAN_POINT('Ctrl Pts',(-64.8619779760282,3.00903854327299,11.7454712505408));
#58374=CARTESIAN_POINT('Ctrl Pts',(-64.6685250414154,4.35518589975374,11.7520042315012));
#58375=CARTESIAN_POINT('Ctrl Pts',(-64.4759146079884,5.70150921150542,11.7581498076534));
#58376=CARTESIAN_POINT('Ctrl Pts',(-64.2824616665933,7.04765656656971,11.7646827917324));
#58377=CARTESIAN_POINT('Ctrl Pts',(-65.5054391943955,3.11095638268489,10.2498035257975));
#58378=CARTESIAN_POINT('Ctrl Pts',(-65.3148558476391,4.45757013432088,10.256832933587));
#58379=CARTESIAN_POINT('Ctrl Pts',(-65.1241323613641,5.80417075067127,10.2638960513912));
#58380=CARTESIAN_POINT('Ctrl Pts',(-64.9335490157358,7.150784502413,10.2709254589092));
#58381=CARTESIAN_POINT('Ctrl Pts',(-66.2655547628832,3.21663712022031,8.09409275195383));
#58382=CARTESIAN_POINT('Ctrl Pts',(-66.0972008564802,4.5662428952645,8.09485849997599));
#58383=CARTESIAN_POINT('Ctrl Pts',(-65.9290633872416,5.91588626629592,8.09554030404865));
#58384=CARTESIAN_POINT('Ctrl Pts',(-65.7607094790964,7.26549204103747,8.09630605274657));
#58385=CARTESIAN_POINT('Ctrl Pts',(-66.6023005642846,3.25480541981896,7.07959378173536));
#58386=CARTESIAN_POINT('Ctrl Pts',(-66.4447225077453,4.6056467360467,7.07797597725202));
#58387=CARTESIAN_POINT('Ctrl Pts',(-66.286993061246,5.95649409802222,7.07635049023918));
#58388=CARTESIAN_POINT('Ctrl Pts',(-66.1294150059254,7.30733541420128,7.07473268581768));
#58389=CARTESIAN_POINT('Ctrl Pts',(-66.7631928097984,3.27249840672654,6.63301530513675));
#58390=CARTESIAN_POINT('Ctrl Pts',(-66.6090115879722,4.62373450251277,6.63100185783403));
#58391=CARTESIAN_POINT('Ctrl Pts',(-66.4548303677893,5.97497059823337,6.62898841061472));
#58392=CARTESIAN_POINT('Ctrl Pts',(-66.3006491459632,7.32620669401961,6.626974963312));
#58393=CARTESIAN_POINT('',(-64.1676029630583,4.96857943999383,12.6479999999978));
#58394=CARTESIAN_POINT('Ctrl Pts',(-61.5166608776679,2.54670163095537,18.6669577173835));
#58395=CARTESIAN_POINT('Ctrl Pts',(-61.3290004490477,3.89369203770503,18.6663192391269));
#58396=CARTESIAN_POINT('Ctrl Pts',(-61.1413400204275,5.24068244445468,18.6656807608702));
#58397=CARTESIAN_POINT('Ctrl Pts',(-60.9536795918073,6.58767285120433,18.6650422826135));
#58398=CARTESIAN_POINT('Ctrl Pts',(-61.6684697611081,2.56772494628588,18.4002045982419));
#58399=CARTESIAN_POINT('Ctrl Pts',(-61.481119730636,3.91475839918527,18.3991907381346));
#58400=CARTESIAN_POINT('Ctrl Pts',(-61.2937636986685,5.26179108000234,18.3981849892633));
#58401=CARTESIAN_POINT('Ctrl Pts',(-61.1064136681965,6.60882453290174,18.397171129156));
#58402=CARTESIAN_POINT('Ctrl Pts',(-61.9625499390985,2.60814245928146,17.8557473383311));
#58403=CARTESIAN_POINT('Ctrl Pts',(-61.7759183873088,3.95527510074787,17.8539100263603));
#58404=CARTESIAN_POINT('Ctrl Pts',(-61.5892849394696,5.30240735844617,17.8520724136354));
#58405=CARTESIAN_POINT('Ctrl Pts',(-61.4026533876799,6.64953999991258,17.8502351016645));
#58406=CARTESIAN_POINT('Ctrl Pts',(-62.4381571638254,2.67212888504903,16.9059398732426));
#58407=CARTESIAN_POINT('Ctrl Pts',(-62.2525608544797,4.01940233987682,16.9030239595655));
#58408=CARTESIAN_POINT('Ctrl Pts',(-62.0669474352095,5.36667330876553,16.900120839887));
#58409=CARTESIAN_POINT('Ctrl Pts',(-61.8813511258638,6.71394676359331,16.8972049262099));
#58410=CARTESIAN_POINT('Ctrl Pts',(-62.869845927729,2.72945153992658,16.0124392072496));
#58411=CARTESIAN_POINT('Ctrl Pts',(-62.684458435686,4.07675300841687,16.0092492045648));
#58412=CARTESIAN_POINT('Ctrl Pts',(-62.499061548445,5.4240528772164,16.006063213451));
#58413=CARTESIAN_POINT('Ctrl Pts',(-62.313674056402,6.7713543457067,16.0028732107663));
#58414=CARTESIAN_POINT('Ctrl Pts',(-63.2631611554505,2.78184209774869,15.1899665862504));
#58415=CARTESIAN_POINT('Ctrl Pts',(-63.0770761206611,4.12904873315006,15.1872846774923));
#58416=CARTESIAN_POINT('Ctrl Pts',(-62.8909567545222,5.47624991104894,15.1846198515837));
#58417=CARTESIAN_POINT('Ctrl Pts',(-62.7048717197328,6.82345654645031,15.1819379428255));
#58418=CARTESIAN_POINT('Ctrl Pts',(-63.8033258621819,2.85494775855224,14.0529811384669));
#58419=CARTESIAN_POINT('Ctrl Pts',(-63.6151133268446,4.20186286915551,14.0520637506875));
#58420=CARTESIAN_POINT('Ctrl Pts',(-63.4268980880177,5.5487774251691,14.0511481765562));
#58421=CARTESIAN_POINT('Ctrl Pts',(-63.2386855526803,6.89569253577236,14.0502307887768));
#58422=CARTESIAN_POINT('Ctrl Pts',(-64.1974111237398,2.91088717513149,13.2113405564316));
#58423=CARTESIAN_POINT('Ctrl Pts',(-64.0067045174499,4.25745129117103,13.2128652412228));
#58424=CARTESIAN_POINT('Ctrl Pts',(-63.8158528480224,5.60399202465122,13.2144630026497));
#58425=CARTESIAN_POINT('Ctrl Pts',(-63.6251462417326,6.95055614069076,13.2159876874408));
#58426=CARTESIAN_POINT('Ctrl Pts',(-64.4551411469067,2.94895124118343,12.643128511615));
#58427=CARTESIAN_POINT('Ctrl Pts',(-64.2634490243411,4.29537004039036,12.6463761705368));
#58428=CARTESIAN_POINT('Ctrl Pts',(-64.0717569017755,5.64178883959729,12.6496238294587));
#58429=CARTESIAN_POINT('Ctrl Pts',(-63.88006477921,6.98820763880422,12.6528714883805));
#58430=CARTESIAN_POINT('',(-61.2351702347376,4.56718724107985,18.6659999999985));
#58431=CARTESIAN_POINT('Ctrl Pts',(-49.3675859352765,0.95649915750836,24.6840263307957));
#58432=CARTESIAN_POINT('Ctrl Pts',(-49.2262718634984,2.30924252806422,24.6840095259536));
#58433=CARTESIAN_POINT('Ctrl Pts',(-49.0849577968025,3.66198589988169,24.6839927211353));
#58434=CARTESIAN_POINT('Ctrl Pts',(-48.9436437250236,5.01472927043735,24.6839759162932));
#58435=CARTESIAN_POINT('Ctrl Pts',(-50.8584017018464,1.11223489879812,24.5224763946979));
#58436=CARTESIAN_POINT('Ctrl Pts',(-50.7056849804841,2.46382207459278,24.5223933820322));
#58437=CARTESIAN_POINT('Ctrl Pts',(-50.5522383262356,3.8152280469866,24.5223069484186));
#58438=CARTESIAN_POINT('Ctrl Pts',(-50.3995217170639,5.16681525063223,24.5222239362787));
#58439=CARTESIAN_POINT('Ctrl Pts',(-53.5751416624051,1.4341043041265,23.9491058552266));
#58440=CARTESIAN_POINT('Ctrl Pts',(-53.4005789255763,2.78302562289254,23.9487852654754));
#58441=CARTESIAN_POINT('Ctrl Pts',(-53.2260564170108,4.13196065521127,23.9484657624716));
#58442=CARTESIAN_POINT('Ctrl Pts',(-53.0514936739988,5.48088197186954,23.9481451725534));
#58443=CARTESIAN_POINT('Ctrl Pts',(-56.685826170517,1.86305916206279,22.9608139368193));
#58444=CARTESIAN_POINT('Ctrl Pts',(-56.4969209650842,3.2099809398552,22.9611535371675));
#58445=CARTESIAN_POINT('Ctrl Pts',(-56.3079639218489,4.55688980206708,22.9614916488461));
#58446=CARTESIAN_POINT('Ctrl Pts',(-56.1190587243836,5.90381158184462,22.9618312494231));
#58447=CARTESIAN_POINT('Ctrl Pts',(-58.1934501574325,2.0765014749507,22.2614053479118));
#58448=CARTESIAN_POINT('Ctrl Pts',(-58.0019534508983,3.42305945926425,22.2619900909815));
#58449=CARTESIAN_POINT('Ctrl Pts',(-57.8104611513907,4.76961709641986,22.2625761875077));
#58450=CARTESIAN_POINT('Ctrl Pts',(-57.6189644441791,6.11617508078676,22.2631609303694));
#58451=CARTESIAN_POINT('Ctrl Pts',(-59.4665491367357,2.25831996402558,21.3906391167669));
#58452=CARTESIAN_POINT('Ctrl Pts',(-59.2748532413305,3.60484625129877,21.3911333943376));
#58453=CARTESIAN_POINT('Ctrl Pts',(-59.083244425966,4.95138635507911,21.3916338266604));
#58454=CARTESIAN_POINT('Ctrl Pts',(-58.8915485171766,6.29791264022871,21.3921281032851));
#58455=CARTESIAN_POINT('Ctrl Pts',(-60.5958537618148,2.41846851546986,20.1757409355903));
#58456=CARTESIAN_POINT('Ctrl Pts',(-60.4061290637618,3.76527728555233,20.1757511768844));
#58457=CARTESIAN_POINT('Ctrl Pts',(-60.2163577444682,5.11207779893297,20.1757546912248));
#58458=CARTESIAN_POINT('Ctrl Pts',(-60.0266330535809,6.4588865702845,20.1757649335528));
#58459=CARTESIAN_POINT('Ctrl Pts',(-61.2120167280186,2.50451325219275,19.2030857378747));
#58460=CARTESIAN_POINT('Ctrl Pts',(-61.023694343456,3.85151637169761,19.2026480404633));
#58461=CARTESIAN_POINT('Ctrl Pts',(-60.8354578933919,5.19853352201533,19.2022158597943));
#58462=CARTESIAN_POINT('Ctrl Pts',(-60.6471354956212,6.54553663936365,19.201778161535));
#58463=CARTESIAN_POINT('Ctrl Pts',(-61.5166651210464,2.54670221859596,18.6669502496772));
#58464=CARTESIAN_POINT('Ctrl Pts',(-61.3289902797436,3.89379614280972,18.6663117195562));
#58465=CARTESIAN_POINT('Ctrl Pts',(-61.1413154372439,5.24089006682804,18.6656731893582));
#58466=CARTESIAN_POINT('Ctrl Pts',(-60.9536405959413,6.58798399104182,18.6650346592371));
#58467=CARTESIAN_POINT('',(-49.1556413769138,2.98545936007412,24.684));
#58468=CARTESIAN_POINT('Ctrl Pts',(-44.3052665433893,0.501764637226471,
24.6839663391592));
#58469=CARTESIAN_POINT('Ctrl Pts',(-44.2029297843719,1.85791016024482,24.6839887797408));
#58470=CARTESIAN_POINT('Ctrl Pts',(-44.1005930253547,3.21405568326316,24.6840112203225));
#58471=CARTESIAN_POINT('Ctrl Pts',(-43.9982562663373,4.57020120628151,24.6840336609041));
#58472=CARTESIAN_POINT('Ctrl Pts',(-45.8824543200059,0.620779044324047,
24.8368171284471));
#58473=CARTESIAN_POINT('Ctrl Pts',(-45.7683449707959,1.9760391843988,24.8368709823476));
#58474=CARTESIAN_POINT('Ctrl Pts',(-45.6540347061159,3.33127517894173,24.8369185616456));
#58475=CARTESIAN_POINT('Ctrl Pts',(-45.5399253572853,4.68653531906208,24.8369724155581));
#58476=CARTESIAN_POINT('Ctrl Pts',(-47.6223636079185,0.774187094160568,
24.8731447167143));
#58477=CARTESIAN_POINT('Ctrl Pts',(-47.4947624703292,2.12826193920829,24.8732119796069));
#58478=CARTESIAN_POINT('Ctrl Pts',(-47.3669515564575,3.48230662826334,24.8732654147927));
#58479=CARTESIAN_POINT('Ctrl Pts',(-47.2393504192644,4.836381473368,24.8733326777113));
#58480=CARTESIAN_POINT('Ctrl Pts',(-49.3675963149307,0.956500241803143,
24.6840252060176));
#58481=CARTESIAN_POINT('Ctrl Pts',(-49.2262928895174,2.30914093098729,24.68400840199));
#58482=CARTESIAN_POINT('Ctrl Pts',(-49.0849894641042,3.66178162017143,24.6839915979625));
#58483=CARTESIAN_POINT('Ctrl Pts',(-48.9436860386909,5.01442230935558,24.6839747939349));
#58484=CARTESIAN_POINT('',(-44.1517615497847,2.53598100128547,24.6839999999998));
#58485=CARTESIAN_POINT('Ctrl Pts',(-30.3222847657765,-0.00413284663027091,
18.6660068644689));
#58486=CARTESIAN_POINT('Ctrl Pts',(-30.3193380428039,1.35591413499973,18.6660022879877));
#58487=CARTESIAN_POINT('Ctrl Pts',(-30.3163913198313,2.71596111662972,18.6659977115065));
#58488=CARTESIAN_POINT('Ctrl Pts',(-30.3134445968586,4.07600809825972,18.6659931350253));
#58489=CARTESIAN_POINT('Ctrl Pts',(-30.7285587386581,-0.00325138912786291,
19.0258393291216));
#58490=CARTESIAN_POINT('Ctrl Pts',(-30.7242038094781,1.35678904299654,19.0258352491989));
#58491=CARTESIAN_POINT('Ctrl Pts',(-30.7197590861058,2.71683977628968,19.0258341061951));
#58492=CARTESIAN_POINT('Ctrl Pts',(-30.7154041635513,4.07688020765401,19.0258300260557));
#58493=CARTESIAN_POINT('Ctrl Pts',(-31.3846390634535,-0.00108090020159251,
19.5676919050105));
#58494=CARTESIAN_POINT('Ctrl Pts',(-31.3774453264759,1.35895950731376,19.5676938356344));
#58495=CARTESIAN_POINT('Ctrl Pts',(-31.3704111723482,2.7189902139802,19.5676927166136));
#58496=CARTESIAN_POINT('Ctrl Pts',(-31.3632174235957,4.07903062221134,19.5676946474626));
#58497=CARTESIAN_POINT('Ctrl Pts',(-32.4133598840372,0.00689348995379523,
20.3244421620242));
#58498=CARTESIAN_POINT('Ctrl Pts',(-32.4008153837116,1.36688359155885,20.3244484473944));
#58499=CARTESIAN_POINT('Ctrl Pts',(-32.3880844526511,2.72688562198433,20.3244585987986));
#58500=CARTESIAN_POINT('Ctrl Pts',(-32.3755399660813,4.08687572270922,20.3244648838835));
#58501=CARTESIAN_POINT('Ctrl Pts',(-34.9086113550027,0.0335760566375183,
22.0306340145341));
#58502=CARTESIAN_POINT('Ctrl Pts',(-34.8807089306754,1.39342690355597,22.0306646909123));
#58503=CARTESIAN_POINT('Ctrl Pts',(-34.8531425913375,2.75325176630356,22.0306876482546));
#58504=CARTESIAN_POINT('Ctrl Pts',(-34.8252401422121,4.11310261513926,22.0307183252023));
#58505=CARTESIAN_POINT('Ctrl Pts',(-37.6978937468501,0.11693363945437,23.2888479293169));
#58506=CARTESIAN_POINT('Ctrl Pts',(-37.6467464569746,1.4761094188233,23.288839788297));
#58507=CARTESIAN_POINT('Ctrl Pts',(-37.5956678603332,2.83529753697036,23.2888329740954));
#58508=CARTESIAN_POINT('Ctrl Pts',(-37.5445205653891,4.19447331542888,23.2888248329776));
#58509=CARTESIAN_POINT('Ctrl Pts',(-39.7806058664349,0.216865324193402,
23.8826917702588));
#58510=CARTESIAN_POINT('Ctrl Pts',(-39.7130039220979,1.57523767019141,23.88266191101));
#58511=CARTESIAN_POINT('Ctrl Pts',(-39.6451963213448,2.93360250982931,23.8826327869049));
#58512=CARTESIAN_POINT('Ctrl Pts',(-39.5775943921822,4.29197485638117,23.8826029276017));
#58513=CARTESIAN_POINT('Ctrl Pts',(-40.597421702395,0.259993271724183,24.084560939485));
#58514=CARTESIAN_POINT('Ctrl Pts',(-40.5232228932742,1.6180231184918,24.0845316720413));
#58515=CARTESIAN_POINT('Ctrl Pts',(-40.4491669163617,2.97605728903849,24.0845017165109));
#58516=CARTESIAN_POINT('Ctrl Pts',(-40.3749680967022,4.33408713548708,24.084472449118));
#58517=CARTESIAN_POINT('Ctrl Pts',(-41.4486629431555,0.307991395735675,
24.2719159198737));
#58518=CARTESIAN_POINT('Ctrl Pts',(-41.3679223481086,1.66564807615995,24.2718886820322));
#58519=CARTESIAN_POINT('Ctrl Pts',(-41.2870893775298,3.02330276774818,24.2718620297276));
#58520=CARTESIAN_POINT('Ctrl Pts',(-41.2063487892987,4.38095944831921,24.2718347918428));
#58521=CARTESIAN_POINT('Ctrl Pts',(-42.6707056826778,0.383592726711738,
24.4939878032503));
#58522=CARTESIAN_POINT('Ctrl Pts',(-42.5805406284222,1.7406702197844,24.4939762987861));
#58523=CARTESIAN_POINT('Ctrl Pts',(-42.4905339901398,3.09775247806375,24.493963982215));
#58524=CARTESIAN_POINT('Ctrl Pts',(-42.4003689241955,4.45482997078481,24.4939524778108));
#58525=CARTESIAN_POINT('Ctrl Pts',(-43.7457382365382,0.459542695930701,
24.6297413546134));
#58526=CARTESIAN_POINT('Ctrl Pts',(-43.6476399272098,1.81605527587309,24.6297525178164));
#58527=CARTESIAN_POINT('Ctrl Pts',(-43.5494164060833,3.17256384303449,24.6297645822975));
#58528=CARTESIAN_POINT('Ctrl Pts',(-43.4513181059938,4.52907642327296,24.629775745434));
#58529=CARTESIAN_POINT('Ctrl Pts',(-44.3052665433893,0.501764637226471,
24.6839663391592));
#58530=CARTESIAN_POINT('Ctrl Pts',(-44.2029261055258,1.85795891155164,24.6839887805475));
#58531=CARTESIAN_POINT('Ctrl Pts',(-44.1005856676623,3.21415318587681,24.6840112219359));
#58532=CARTESIAN_POINT('Ctrl Pts',(-43.9982452297988,4.57034746020199,24.6840336633242));
#58533=CARTESIAN_POINT('',(-30.3178648443797,2.03586236518953,18.6660000000004));
#58534=CARTESIAN_POINT('Ctrl Pts',(-25.4512489060473,0.000557793871136247,
12.6480025703997));
#58535=CARTESIAN_POINT('Ctrl Pts',(-25.453101108281,1.36055653259994,12.6480008567999));
#58536=CARTESIAN_POINT('Ctrl Pts',(-25.4549533105147,2.72055527132875,12.6479991432001));
#58537=CARTESIAN_POINT('Ctrl Pts',(-25.4568055127484,4.08055401005756,12.6479974296003));
#58538=CARTESIAN_POINT('Ctrl Pts',(-27.0230520916476,-0.00157989408392619,
15.008208642719));
#58539=CARTESIAN_POINT('Ctrl Pts',(-27.025967107362,1.35841338001428,15.0082212028861));
#58540=CARTESIAN_POINT('Ctrl Pts',(-27.0298213035499,2.71841742660675,15.0082464445362));
#58541=CARTESIAN_POINT('Ctrl Pts',(-27.0327363192644,4.07841070070495,15.0082590047032));
#58542=CARTESIAN_POINT('Ctrl Pts',(-28.204865633569,-0.00872682770445543,
16.7906590474112));
#58543=CARTESIAN_POINT('Ctrl Pts',(-28.2089295504538,1.35127726481958,16.7906114791363));
#58544=CARTESIAN_POINT('Ctrl Pts',(-28.2144468884787,2.71130821992859,16.7906149931826));
#58545=CARTESIAN_POINT('Ctrl Pts',(-28.2185108053635,4.07131231245263,16.7905674249077));
#58546=CARTESIAN_POINT('Ctrl Pts',(-30.3222847657765,-0.00413284663027091,
18.6660068644689));
#58547=CARTESIAN_POINT('Ctrl Pts',(-30.319338151512,1.3558639612496,18.6660022881565));
#58548=CARTESIAN_POINT('Ctrl Pts',(-30.3163915372475,2.71586076912947,18.6659977118442));
#58549=CARTESIAN_POINT('Ctrl Pts',(-30.3134449229829,4.07585757700934,18.6659931355318));
#58550=CARTESIAN_POINT('',(-25.4540272093979,2.04055590196435,12.648));
#58551=CARTESIAN_POINT('Ctrl Pts',(-21.1430615049491,0.000717013383229603,
6.63001173766484));
#58552=CARTESIAN_POINT('Ctrl Pts',(-21.1420934966246,1.36071666886063,6.63000391255497));
#58553=CARTESIAN_POINT('Ctrl Pts',(-21.1411254883001,2.72071632433803,6.6299960874451));
#58554=CARTESIAN_POINT('Ctrl Pts',(-21.1401574799756,4.08071597981543,6.62998826233523));
#58555=CARTESIAN_POINT('Ctrl Pts',(-21.8005099855675,0.00118993616216897,
7.49379695859226));
#58556=CARTESIAN_POINT('Ctrl Pts',(-21.7995582366668,1.3611895530325,7.493782020727));
#58557=CARTESIAN_POINT('Ctrl Pts',(-21.7985906509679,2.72118930903738,7.4937652269592));
#58558=CARTESIAN_POINT('Ctrl Pts',(-21.7976389020672,4.08118892590771,7.49375028909394));
#58559=CARTESIAN_POINT('Ctrl Pts',(-22.8275445640793,0.00197688629320044,
8.83972141456318));
#58560=CARTESIAN_POINT('Ctrl Pts',(-22.8269415478554,1.36197695395413,8.83968617050489));
#58561=CARTESIAN_POINT('Ctrl Pts',(-22.8263393218972,2.72197703099325,8.83965028373617));
#58562=CARTESIAN_POINT('Ctrl Pts',(-22.8257363056734,4.08197709865418,8.83961503967788));
#58563=CARTESIAN_POINT('Ctrl Pts',(-24.3932856767672,0.00180919175862648,
11.05541899507));
#58564=CARTESIAN_POINT('Ctrl Pts',(-24.3940975319706,1.36180915945558,11.0553960222686));
#58565=CARTESIAN_POINT('Ctrl Pts',(-24.3949048701553,2.72180914970329,11.0553728965359));
#58566=CARTESIAN_POINT('Ctrl Pts',(-24.3957167253587,4.08180911740025,11.0553499237346));
#58567=CARTESIAN_POINT('Ctrl Pts',(-25.1061238118938,0.0010271718212213,
12.1297659316509));
#58568=CARTESIAN_POINT('Ctrl Pts',(-25.1076729687202,1.36102630813001,12.12976051533));
#58569=CARTESIAN_POINT('Ctrl Pts',(-25.1092249488343,2.72102548600383,12.1297535835151));
#58570=CARTESIAN_POINT('Ctrl Pts',(-25.1107741056607,4.08102462231262,12.1297481671942));
#58571=CARTESIAN_POINT('Ctrl Pts',(-25.4512489060473,0.000557793871136247,
12.6480025703997));
#58572=CARTESIAN_POINT('Ctrl Pts',(-25.453101108281,1.36055653259994,12.6480008567999));
#58573=CARTESIAN_POINT('Ctrl Pts',(-25.4549533105147,2.72055527132875,12.6479991432001));
#58574=CARTESIAN_POINT('Ctrl Pts',(-25.4568055127484,4.08055401005756,12.6479974296003));
#58575=CARTESIAN_POINT('',(-21.1416094924623,2.04071649659933,6.63000000000004));
#58576=CARTESIAN_POINT('Ctrl Pts',(-16.6859947282585,-0.000213685071575598,
0.653010349651237));
#58577=CARTESIAN_POINT('Ctrl Pts',(-16.6862555279244,1.3595114502545,0.625670116550412));
#58578=CARTESIAN_POINT('Ctrl Pts',(-16.6865163275903,2.71923658558058,0.598329883449587));
#58579=CARTESIAN_POINT('Ctrl Pts',(-16.6867771272561,4.07896172090666,0.570989650348762));
#58580=CARTESIAN_POINT('Ctrl Pts',(-17.1283146873041,0.0115850794287345,
1.24402336313977));
#58581=CARTESIAN_POINT('Ctrl Pts',(-17.1369212648133,1.37157656223025,1.23410219696274));
#58582=CARTESIAN_POINT('Ctrl Pts',(-17.1461443494675,2.73182976169598,1.22492379185217));
#58583=CARTESIAN_POINT('Ctrl Pts',(-17.1547509269767,4.09182124449749,1.21500262567514));
#58584=CARTESIAN_POINT('Ctrl Pts',(-17.7995093414147,0.00861285405854421,
2.15897284032503));
#58585=CARTESIAN_POINT('Ctrl Pts',(-17.8086067249379,1.36857803218947,2.1586056624823));
#58586=CARTESIAN_POINT('Ctrl Pts',(-17.817701749899,2.72852490191836,2.15820377353535));
#58587=CARTESIAN_POINT('Ctrl Pts',(-17.8267991334222,4.08849008004929,2.15783659569263));
#58588=CARTESIAN_POINT('Ctrl Pts',(-18.6500576004548,0.00359926355307256,
3.31551610923036));
#58589=CARTESIAN_POINT('Ctrl Pts',(-18.6553153931928,1.36359151605813,3.31726183535392));
#58590=CARTESIAN_POINT('Ctrl Pts',(-18.6606491109907,2.72362743141132,3.31912211797675));
#58591=CARTESIAN_POINT('Ctrl Pts',(-18.6659069037288,4.08361968391638,3.32086784410031));
#58592=CARTESIAN_POINT('Ctrl Pts',(-19.2949742331925,0.000749258977111304,
4.18600514145956));
#58593=CARTESIAN_POINT('Ctrl Pts',(-19.2971395770759,1.36074705522213,4.18714822626292));
#58594=CARTESIAN_POINT('Ctrl Pts',(-19.2993388889085,2.72076348791444,4.18835516320786));
#58595=CARTESIAN_POINT('Ctrl Pts',(-19.3015042327919,4.08076128415945,4.18949824801122));
#58596=CARTESIAN_POINT('Ctrl Pts',(-20.1855381343016,-0.000360669926822324,
5.37385984414699));
#58597=CARTESIAN_POINT('Ctrl Pts',(-20.1848339213132,1.35964105651181,5.37362227555459));
#58598=CARTESIAN_POINT('Ctrl Pts',(-20.1841478714708,2.71966507969474,5.37343458389977));
#58599=CARTESIAN_POINT('Ctrl Pts',(-20.1834436584824,4.07966680613337,5.37319701530737));
#58600=CARTESIAN_POINT('Ctrl Pts',(-20.7645962878633,0.000444774645616996,
6.13326360844075));
#58601=CARTESIAN_POINT('Ctrl Pts',(-20.7636457870061,1.3604434450274,6.13291231871182));
#58602=CARTESIAN_POINT('Ctrl Pts',(-20.7626238007416,2.7204450515632,6.13261197194776));
#58603=CARTESIAN_POINT('Ctrl Pts',(-20.7616732998844,4.08044372194498,6.13226068221884));
#58604=CARTESIAN_POINT('Ctrl Pts',(-21.1430615049491,0.000717013383229603,
6.63001173766484));
#58605=CARTESIAN_POINT('Ctrl Pts',(-21.1420934966246,1.36071666886063,6.63000391255497));
#58606=CARTESIAN_POINT('Ctrl Pts',(-21.1411254883001,2.72071632433803,6.6299960874451));
#58607=CARTESIAN_POINT('Ctrl Pts',(-21.1401574799756,4.08071597981543,6.62998826233523));
#58608=CARTESIAN_POINT('',(-16.6863859277573,2.03937401791754,0.611999999999999));
#58609=CARTESIAN_POINT('Ctrl Pts',(-11.7469519845649,-1.24898856655025,
-5.1604537901259));
#58610=CARTESIAN_POINT('Ctrl Pts',(-11.4535903397776,0.0688879795759836,
-5.3241809848708));
#58611=CARTESIAN_POINT('Ctrl Pts',(-11.1602285866567,1.38676445662711,-5.4879087785922));
#58612=CARTESIAN_POINT('Ctrl Pts',(-10.8668669418732,2.70464100275581,-5.65163597331566));
#58613=CARTESIAN_POINT('Ctrl Pts',(-12.0050933687692,-1.16134492936906,
-4.91752211089309));
#58614=CARTESIAN_POINT('Ctrl Pts',(-11.711107008775,0.153817187963984,-5.10239435840529));
#58615=CARTESIAN_POINT('Ctrl Pts',(-11.4176900288694,1.46934235066558,-5.2841184918417));
#58616=CARTESIAN_POINT('Ctrl Pts',(-11.1237036484762,2.78450445499191,-5.4689908521404));
#58617=CARTESIAN_POINT('Ctrl Pts',(-12.7010765381262,-0.905927472950019,
-4.23328860522664));
#58618=CARTESIAN_POINT('Ctrl Pts',(-12.4199418855767,0.406194899132227,
-4.45475204341524));
#58619=CARTESIAN_POINT('Ctrl Pts',(-12.1385802960752,1.71818448859926,-4.67783714572155));
#58620=CARTESIAN_POINT('Ctrl Pts',(-11.8574456516561,3.03030686543866,-4.89930052581131));
#58621=CARTESIAN_POINT('Ctrl Pts',(-13.4034560583173,-0.630382964431516,
-3.47895409086386));
#58622=CARTESIAN_POINT('Ctrl Pts',(-13.1657297111913,0.690309717783447,
-3.70499001167999));
#58623=CARTESIAN_POINT('Ctrl Pts',(-12.9282670445964,2.01114267174908,-3.93059648835147));
#58624=CARTESIAN_POINT('Ctrl Pts',(-12.6905406880236,3.33183534893858,-4.15663242455316));
#58625=CARTESIAN_POINT('Ctrl Pts',(-14.2693062595799,-0.346358717812154,
-2.463047534852));
#58626=CARTESIAN_POINT('Ctrl Pts',(-14.1094732202099,0.991288087753195,
-2.65490390307943));
#58627=CARTESIAN_POINT('Ctrl Pts',(-13.9495030479015,2.3289080887949,-2.8465979544352));
#58628=CARTESIAN_POINT('Ctrl Pts',(-13.7896700134444,3.66655489532056,-3.03845432847791));
#58629=CARTESIAN_POINT('Ctrl Pts',(-14.9655514589865,-0.169147364522696,
-1.59527625944176));
#58630=CARTESIAN_POINT('Ctrl Pts',(-14.8738731361902,1.18114798058698,-1.7391436974675));
#58631=CARTESIAN_POINT('Ctrl Pts',(-14.7820906943996,2.53150537188668,-1.88363575390914));
#58632=CARTESIAN_POINT('Ctrl Pts',(-14.6904123753336,3.88180071477345,-2.02750316955686));
#58633=CARTESIAN_POINT('Ctrl Pts',(-15.8024771762679,-0.039623100750617,
-0.512730537069246));
#58634=CARTESIAN_POINT('Ctrl Pts',(-15.7752096756165,1.31866535626611,-0.59285342408472));
#58635=CARTESIAN_POINT('Ctrl Pts',(-15.7480885002328,2.67691275138139,-0.672116635479013));
#58636=CARTESIAN_POINT('Ctrl Pts',(-15.7208209943389,4.03520120986923,-0.752239553293818));
#58637=CARTESIAN_POINT('Ctrl Pts',(-16.3914419547385,-0.00797615819818137,
0.264094830899975));
#58638=CARTESIAN_POINT('Ctrl Pts',(-16.3862014526881,1.35143079639208,0.222423946339894));
#58639=CARTESIAN_POINT('Ctrl Pts',(-16.3803829115459,2.71097183412246,0.179138036275036));
#58640=CARTESIAN_POINT('Ctrl Pts',(-16.3751424302047,4.07037878390896,0.137467209575971));
#58641=CARTESIAN_POINT('Ctrl Pts',(-16.6860507767434,-0.000212207904980436,
0.653084353789295));
#58642=CARTESIAN_POINT('Ctrl Pts',(-16.6863126279545,1.35953734982766,0.625746357783578));
#58643=CARTESIAN_POINT('Ctrl Pts',(-16.6865745891456,2.71928688204919,0.598408669055888));
#58644=CARTESIAN_POINT('Ctrl Pts',(-16.6868364403527,4.07903643978274,0.571070673039161));
#58645=CARTESIAN_POINT('',(-11.3069663320367,0.727806741256162,-5.40599999999988));
#58646=CARTESIAN_POINT('',(-11.3069663320367,0.727806741256166,-5.40599999999988));
#58647=CARTESIAN_POINT('',(-11.3069663320367,0.727806741256166,-5.40599999999988));
#58648=CARTESIAN_POINT('Ctrl Pts',(6.41902973990636E-15,-1.93207323326078,
-8.62957429809281));
#58649=CARTESIAN_POINT('Ctrl Pts',(2.80278610805871E-15,-0.572138762410863,
-8.64292476603094));
#58650=CARTESIAN_POINT('Ctrl Pts',(-8.13457523788951E-16,0.78779570843905,
-8.65627523396906));
#58651=CARTESIAN_POINT('Ctrl Pts',(-4.42970115563661E-15,2.14773017928896,
-8.66962570190719));
#58652=CARTESIAN_POINT('Ctrl Pts',(-0.658062683030888,-1.93165972294369,
-8.58745240866785));
#58653=CARTESIAN_POINT('Ctrl Pts',(-0.682573404813958,-0.571376327075844,
-8.60175832749374));
#58654=CARTESIAN_POINT('Ctrl Pts',(-0.708277726456336,0.78782854621592,
-8.61643182898499));
#58655=CARTESIAN_POINT('Ctrl Pts',(-0.732788448239405,2.14811194208377,
-8.63073774781089));
#58656=CARTESIAN_POINT('Ctrl Pts',(-2.46516391286739,-1.98743098295203,
-8.49849688064982));
#58657=CARTESIAN_POINT('Ctrl Pts',(-2.55711848213956,-0.630595668642713,
-8.51587687470825));
#58658=CARTESIAN_POINT('Ctrl Pts',(-2.6481713222656,0.726813060125434,-8.53306426500673));
#58659=CARTESIAN_POINT('Ctrl Pts',(-2.74012589153777,2.08364837443475,-8.55044425906516));
#58660=CARTESIAN_POINT('Ctrl Pts',(-4.39676963179061,-2.13852225314529,
-8.46329578588585));
#58661=CARTESIAN_POINT('Ctrl Pts',(-4.48313054872813,-0.781026877589576,
-8.48236683893671));
#58662=CARTESIAN_POINT('Ctrl Pts',(-4.56966303709027,0.576336747779195,
-8.50142575891667));
#58663=CARTESIAN_POINT('Ctrl Pts',(-4.65602395402778,1.93383212333491,-8.52049681196753));
#58664=CARTESIAN_POINT('Ctrl Pts',(-6.35409454450772,-2.18205385875907,
-8.11784826271868));
#58665=CARTESIAN_POINT('Ctrl Pts',(-6.35325914215375,-0.821354211984902,
-8.1496301634349));
#58666=CARTESIAN_POINT('Ctrl Pts',(-6.35262424881583,0.539250997990761,
-8.18151670217025));
#58667=CARTESIAN_POINT('Ctrl Pts',(-6.35178884646186,1.89995064476493,-8.21329860288647));
#58668=CARTESIAN_POINT('Ctrl Pts',(-8.15537660210863,-2.1050270665009,-7.52858105609529));
#58669=CARTESIAN_POINT('Ctrl Pts',(-8.03377897269566,-0.748914208094495,
-7.58528703948586));
#58670=CARTESIAN_POINT('Ctrl Pts',(-7.91087017389806,0.607551140645141,
-7.64175911617833));
#58671=CARTESIAN_POINT('Ctrl Pts',(-7.78927254448508,1.96366399905155,-7.6984650995689));
#58672=CARTESIAN_POINT('Ctrl Pts',(-10.2097165609597,-1.7375710793364,-6.40958181990177));
#58673=CARTESIAN_POINT('Ctrl Pts',(-9.94448455848953,-0.405812797944965,
-6.52029409947421));
#58674=CARTESIAN_POINT('Ctrl Pts',(-9.68069833114861,0.925421674998247,
-6.63131671765967));
#58675=CARTESIAN_POINT('Ctrl Pts',(-9.41546632867843,2.25717995638968,-6.7420289972321));
#58676=CARTESIAN_POINT('Ctrl Pts',(-11.2781006865412,-1.40420632664524,
-5.56975094644535));
#58677=CARTESIAN_POINT('Ctrl Pts',(-10.9870984387785,-0.0845518570703568,
-5.71805524906024));
#58678=CARTESIAN_POINT('Ctrl Pts',(-10.6930379962096,1.23642612169233,-5.86563953187011));
#58679=CARTESIAN_POINT('Ctrl Pts',(-10.4020357484469,2.55608059126722,-6.013943834485));
#58680=CARTESIAN_POINT('Ctrl Pts',(-11.7470010949101,-1.24897189262896,
-5.16040757324739));
#58681=CARTESIAN_POINT('Ctrl Pts',(-11.4536445863279,0.0688805299611238,
-5.32413585774905));
#58682=CARTESIAN_POINT('Ctrl Pts',(-11.1602880777456,1.38673295255121,-5.48786414225071));
#58683=CARTESIAN_POINT('Ctrl Pts',(-10.8669315691633,2.70458537514129,-5.65159242675238));
#58684=CARTESIAN_POINT('',(0.,0.107828473014093,-8.6496));
#58685=CARTESIAN_POINT('Ctrl Pts',(-73.6764856602474,5.168558288494,0.190796964362639));
#58686=CARTESIAN_POINT('Ctrl Pts',(-73.0217457288853,6.32703394457543,0.471598988120776));
#58687=CARTESIAN_POINT('Ctrl Pts',(-72.3670057975232,7.48550960065686,0.752401011878913));
#58688=CARTESIAN_POINT('Ctrl Pts',(-71.7122658661611,8.64398525673828,1.03320303563705));
#58689=CARTESIAN_POINT('Ctrl Pts',(-74.7404207630834,5.85068057265868,-0.142609694242852));
#58690=CARTESIAN_POINT('Ctrl Pts',(-73.9872728090383,6.93979153504156,0.186818345160544));
#58691=CARTESIAN_POINT('Ctrl Pts',(-73.2316019247904,8.03256413589653,0.519523811415036));
#58692=CARTESIAN_POINT('Ctrl Pts',(-72.4784539707453,9.12167509827942,0.848951850818431));
#58693=CARTESIAN_POINT('Ctrl Pts',(-75.9741648812485,6.89428690872944,-0.412567225194581));
#58694=CARTESIAN_POINT('Ctrl Pts',(-75.1564827140154,7.91936761120769,-0.0547049712921969));
#58695=CARTESIAN_POINT('Ctrl Pts',(-74.3386463722817,8.94330795351427,0.302963615183627));
#58696=CARTESIAN_POINT('Ctrl Pts',(-73.5209642050486,9.96838865599251,0.66082586908601));
#58697=CARTESIAN_POINT('Ctrl Pts',(-77.4581499404949,8.19662250468364,-0.873282366765809));
#58698=CARTESIAN_POINT('Ctrl Pts',(-76.6611237143454,9.24570529771174,-0.534158754431353));
#58699=CARTESIAN_POINT('Ctrl Pts',(-75.8638070483209,10.2958056899081,-0.194566350790663));
#58700=CARTESIAN_POINT('Ctrl Pts',(-75.0667808221714,11.3448884829362,0.144557261543794));
#58701=CARTESIAN_POINT('Ctrl Pts',(-78.1080385927614,8.74315679055215,-1.12050093759123));
#58702=CARTESIAN_POINT('Ctrl Pts',(-77.3487456616466,9.82768503189974,-0.807299633395332));
#58703=CARTESIAN_POINT('Ctrl Pts',(-76.5890175462894,10.9122676252282,-0.493818169521655));
#58704=CARTESIAN_POINT('Ctrl Pts',(-75.8297246151746,11.9967958665758,-0.180616865325761));
#58705=CARTESIAN_POINT('Ctrl Pts',(-78.8357086373011,9.31133939639374,-1.44888811728152));
#58706=CARTESIAN_POINT('Ctrl Pts',(-78.1426077220294,10.4518303214309,-1.17933446484409));
#58707=CARTESIAN_POINT('Ctrl Pts',(-77.450171149787,11.592893117714,-0.910220255034814));
#58708=CARTESIAN_POINT('Ctrl Pts',(-76.7570702345152,12.7333840427512,-0.640666602597381));
#58709=CARTESIAN_POINT('Ctrl Pts',(-79.2776917908501,9.61051959968398,-1.69898330179011));
#58710=CARTESIAN_POINT('Ctrl Pts',(-78.6499410387911,10.7976671952425,-1.47139959830661));
#58711=CARTESIAN_POINT('Ctrl Pts',(-78.0213825166128,11.9846055748152,-1.24363766834935));
#58712=CARTESIAN_POINT('Ctrl Pts',(-77.3936317645538,13.1717531703737,-1.01605396486585));
#58713=CARTESIAN_POINT('Ctrl Pts',(-79.5980561168787,9.79488102596951,-1.92025417907613));
#58714=CARTESIAN_POINT('Ctrl Pts',(-79.0286853722929,11.0149170322628,-1.72808472635871));
#58715=CARTESIAN_POINT('Ctrl Pts',(-78.4593146277071,12.2349530385561,-1.53591527364129));
#58716=CARTESIAN_POINT('Ctrl Pts',(-77.8899438831213,13.4549890448494,-1.34374582092387));
#58717=CARTESIAN_POINT('Ctrl Pts',(11.7470010949101,-1.24897189262897,-5.16040757324743));
#58718=CARTESIAN_POINT('Ctrl Pts',(11.4536445863278,0.068880529961115,-5.32413585774911));
#58719=CARTESIAN_POINT('Ctrl Pts',(11.1602880777455,1.3867329525512,-5.48786414225079));
#58720=CARTESIAN_POINT('Ctrl Pts',(10.8669315691632,2.70458537514128,-5.65159242675248));
#58721=CARTESIAN_POINT('Ctrl Pts',(10.7125397951466,-1.59144123476306,-6.0634775436082));
#58722=CARTESIAN_POINT('Ctrl Pts',(10.4228755853451,-0.267776435549922,
-6.19166121896685));
#58723=CARTESIAN_POINT('Ctrl Pts',(10.1309691717591,1.05329780357478,-6.32280773148431));
#58724=CARTESIAN_POINT('Ctrl Pts',(9.84130496195755,2.37696260278792,-6.45099140684296));
#58725=CARTESIAN_POINT('Ctrl Pts',(9.24118021009056,-1.93913982160653,-6.97487125430323));
#58726=CARTESIAN_POINT('Ctrl Pts',(9.04250186351073,-0.593814054742301,
-7.05753687418105));
#58727=CARTESIAN_POINT('Ctrl Pts',(8.84452012731969,0.751814771731771,-7.13977225849378));
#58728=CARTESIAN_POINT('Ctrl Pts',(8.64584178073985,2.097140538596,-7.22243787837159));
#58729=CARTESIAN_POINT('Ctrl Pts',(7.87873760695008,-2.09354224390961,-7.58570787305198));
#58730=CARTESIAN_POINT('Ctrl Pts',(7.77530583020013,-0.738307891227118,
-7.64064961915395));
#58731=CARTESIAN_POINT('Ctrl Pts',(7.67158568832869,0.616720958047741,-7.69590312735252));
#58732=CARTESIAN_POINT('Ctrl Pts',(7.56815391157874,1.97195531073023,-7.75084487345448));
#58733=CARTESIAN_POINT('Ctrl Pts',(7.28211573159564,-2.13599647613335,-7.80368259116433));
#58734=CARTESIAN_POINT('Ctrl Pts',(7.21917418428538,-0.777984989202499,
-7.84880269620889));
#58735=CARTESIAN_POINT('Ctrl Pts',(7.15587550655931,0.579887102874036,-7.89407576492449));
#58736=CARTESIAN_POINT('Ctrl Pts',(7.09293395924904,1.93789858980489,-7.93919586996905));
#58737=CARTESIAN_POINT('Ctrl Pts',(6.7745203245172,-2.15695778989224,-7.96476246664597));
#58738=CARTESIAN_POINT('Ctrl Pts',(6.74319842093572,-0.797829234317486,
-8.00316656823017));
#58739=CARTESIAN_POINT('Ctrl Pts',(6.71211273967383,0.561308730497167,-8.04161829655868));
#58740=CARTESIAN_POINT('Ctrl Pts',(6.68079083609235,1.92043728607192,-8.08002239814288));
#58741=CARTESIAN_POINT('Ctrl Pts',(6.29786588949097,-2.16773371799523,-8.09674109067091));
#58742=CARTESIAN_POINT('Ctrl Pts',(6.29530177097099,-0.807935606154201,
-8.12958458865204));
#58743=CARTESIAN_POINT('Ctrl Pts',(6.29129857304258,0.551617246522031,-8.1627464890655));
#58744=CARTESIAN_POINT('Ctrl Pts',(6.2887344545226,1.91141535836306,-8.19558998704663));
#58745=CARTESIAN_POINT('Ctrl Pts',(5.00815621212858,-2.16216752644387,-8.38292053232245));
#58746=CARTESIAN_POINT('Ctrl Pts',(5.06969455888082,-0.803042657470201,
-8.40482373966323));
#58747=CARTESIAN_POINT('Ctrl Pts',(5.13036288577363,0.556263586031991,-8.42660503066042));
#58748=CARTESIAN_POINT('Ctrl Pts',(5.19190123252587,1.91538845500566,-8.4485082380012));
#58749=CARTESIAN_POINT('Ctrl Pts',(3.22852047111695,-2.04767166606362,-8.49451211875645));
#58750=CARTESIAN_POINT('Ctrl Pts',(3.33405646482314,-0.692138611224734,
-8.51233430927317));
#58751=CARTESIAN_POINT('Ctrl Pts',(3.44288808239679,0.663146437524625,-8.53025242833666));
#58752=CARTESIAN_POINT('Ctrl Pts',(3.54842407610298,2.01867949236351,-8.54807461885338));
#58753=CARTESIAN_POINT('Ctrl Pts',(1.19527622155365,-1.93132215124059,-8.55306594389669));
#58754=CARTESIAN_POINT('Ctrl Pts',(1.24356632046841,-0.571512548852095,
-8.56835748664852));
#58755=CARTESIAN_POINT('Ctrl Pts',(1.28271472812635,0.788613994112341,-8.58369978338118));
#58756=CARTESIAN_POINT('Ctrl Pts',(1.33100482704111,2.14842359650083,-8.598991326133));
#58757=CARTESIAN_POINT('Ctrl Pts',(6.41902973990636E-15,-1.93207323326078,
-8.62957429809281));
#58758=CARTESIAN_POINT('Ctrl Pts',(2.80278610805871E-15,-0.572138762410868,
-8.64292476603094));
#58759=CARTESIAN_POINT('Ctrl Pts',(-8.13457523788951E-16,0.787795708439045,
-8.65627523396906));
#58760=CARTESIAN_POINT('Ctrl Pts',(-4.42970115563661E-15,2.14773017928896,
-8.66962570190719));
#58761=CARTESIAN_POINT('Ctrl Pts',(77.5413122691233,9.45942207531684,-5.67964638243731));
#58762=CARTESIAN_POINT('Ctrl Pts',(77.0326085523511,10.7074362929352,-5.49721546081316));
#58763=CARTESIAN_POINT('Ctrl Pts',(76.5239048355788,11.9554505105535,-5.314784539189));
#58764=CARTESIAN_POINT('Ctrl Pts',(76.0152011188066,13.2034647281718,-5.13235361756485));
#58765=CARTESIAN_POINT('Ctrl Pts',(78.375913647818,9.63522559747283,-4.55505891458532));
#58766=CARTESIAN_POINT('Ctrl Pts',(77.8612559061973,10.8797481339151,-4.36483973542567));
#58767=CARTESIAN_POINT('Ctrl Pts',(77.3499789374201,12.1246925927886,-4.16959241162605));
#58768=CARTESIAN_POINT('Ctrl Pts',(76.8353211957994,13.3692151292309,-3.97937323246641));
#58769=CARTESIAN_POINT('Ctrl Pts',(79.119383339007,9.77540103482857,-3.21481989604027));
#58770=CARTESIAN_POINT('Ctrl Pts',(78.5708662074078,11.0105688473922,-3.05739091744627));
#58771=CARTESIAN_POINT('Ctrl Pts',(78.028068075148,12.247228353462,-2.89111167264609));
#58772=CARTESIAN_POINT('Ctrl Pts',(77.4795509435488,13.4823961660256,-2.73368269405209));
#58773=CARTESIAN_POINT('Ctrl Pts',(79.5980561168973,9.79488102600527,-1.92025417906537));
#58774=CARTESIAN_POINT('Ctrl Pts',(79.0286853722991,11.0149170322939,-1.72808472635512));
#58775=CARTESIAN_POINT('Ctrl Pts',(78.4593146277009,12.2349530385826,-1.53591527364488));
#58776=CARTESIAN_POINT('Ctrl Pts',(77.8899438831027,13.4549890448712,-1.34374582093463));
#58777=CARTESIAN_POINT('Ctrl Pts',(20.8093219165299,12.6047206302974,-78.8857217870086));
#58778=CARTESIAN_POINT('Ctrl Pts',(20.8084406388433,13.8055291044746,-78.2472405956695));
#58779=CARTESIAN_POINT('Ctrl Pts',(20.8075593611567,15.0063375786519,-77.6087594043304));
#58780=CARTESIAN_POINT('Ctrl Pts',(20.8066780834701,16.2071460528291,-76.9702782129913));
#58781=CARTESIAN_POINT('Ctrl Pts',(20.7840585070756,12.6878742959502,-79.0421459570682));
#58782=CARTESIAN_POINT('Ctrl Pts',(20.7831790034045,13.8886827711699,-78.4036647651749));
#58783=CARTESIAN_POINT('Ctrl Pts',(20.7822994476123,15.0894912462774,-77.7651835733411));
#58784=CARTESIAN_POINT('Ctrl Pts',(20.7814199439412,16.2902997214971,-77.1267023814477));
#58785=CARTESIAN_POINT('Ctrl Pts',(20.7537282342997,12.8597759562963,-79.3654873575285));
#58786=CARTESIAN_POINT('Ctrl Pts',(20.7528512698888,14.0605844328848,-78.7270061649073));
#58787=CARTESIAN_POINT('Ctrl Pts',(20.7519739839115,15.2613929097475,-78.0885249721403));
#58788=CARTESIAN_POINT('Ctrl Pts',(20.7510970195006,16.462201386336,-77.4500437795191));
#58789=CARTESIAN_POINT('Ctrl Pts',(20.8081933777383,13.1149063735043,-79.8452428571726));
#58790=CARTESIAN_POINT('Ctrl Pts',(20.8073117469505,14.3157148475504,-79.2067616659032));
#58791=CARTESIAN_POINT('Ctrl Pts',(20.8064299122934,15.5165233221614,-78.5682804743334));
#58792=CARTESIAN_POINT('Ctrl Pts',(20.8055482815057,16.7173317962075,-77.9297992830641));
#58793=CARTESIAN_POINT('Ctrl Pts',(21.0036168912534,13.3497532744261,-80.2866546117358));
#58794=CARTESIAN_POINT('Ctrl Pts',(21.0027239008197,14.5505617417736,-79.6481734240281));
#58795=CARTESIAN_POINT('Ctrl Pts',(21.0018296748422,15.7513702095747,-79.0096922360792));
#58796=CARTESIAN_POINT('Ctrl Pts',(21.0009366844085,16.9521786769222,-78.3712110483715));
#58797=CARTESIAN_POINT('Ctrl Pts',(21.2743902926592,13.4924836387241,-80.5547123821854));
#58798=CARTESIAN_POINT('Ctrl Pts',(21.273503030042,14.6932921096191,-79.9162311925915));
#58799=CARTESIAN_POINT('Ctrl Pts',(21.2726153038638,15.8941005812516,-79.2777500026055));
#58800=CARTESIAN_POINT('Ctrl Pts',(21.2717280412466,17.0949090521466,-78.6392688130115));
#58801=CARTESIAN_POINT('Ctrl Pts',(21.4904278237746,13.5660008548253,-80.6926839980435));
#58802=CARTESIAN_POINT('Ctrl Pts',(21.4895656787975,14.7668093397565,-80.0542028009863));
#58803=CARTESIAN_POINT('Ctrl Pts',(21.488702230328,15.9676178254005,-79.4157216035502));
#58804=CARTESIAN_POINT('Ctrl Pts',(21.4878400853508,17.1684263103318,-78.777240406493));
#58805=CARTESIAN_POINT('Ctrl Pts',(21.6433045087496,13.6103006059301,-80.7757949442799));
#58806=CARTESIAN_POINT('Ctrl Pts',(21.6424648381891,14.8111091037285,-80.1373137403811));
#58807=CARTESIAN_POINT('Ctrl Pts',(21.6416248265819,16.011917601909,-79.4988325362792));
#58808=CARTESIAN_POINT('Ctrl Pts',(21.6407851560214,17.2127260997074,-78.8603513323804));
#58809=CARTESIAN_POINT('Ctrl Pts',(21.928242214773,13.6734021326948,-80.8941044180776));
#58810=CARTESIAN_POINT('Ctrl Pts',(21.9274618395652,14.8742106613855,-80.2556231977532));
#58811=CARTESIAN_POINT('Ctrl Pts',(21.9266795141814,16.0750191913452,-79.6171419767539));
#58812=CARTESIAN_POINT('Ctrl Pts',(21.9258991389736,17.2758277200359,-78.9786607564294));
#58813=CARTESIAN_POINT('Ctrl Pts',(22.3613428584683,13.7286395353824,-80.997489165121));
#58814=CARTESIAN_POINT('Ctrl Pts',(22.3607015893129,14.9294481342844,-80.3590079074645));
#58815=CARTESIAN_POINT('Ctrl Pts',(22.3600607034172,16.1302567329206,-79.7205266499492));
#58816=CARTESIAN_POINT('Ctrl Pts',(22.3594194342618,17.3310653318226,-79.0820453922927));
#58817=CARTESIAN_POINT('Ctrl Pts',(22.9135127166986,13.7517748296916,-81.0405604775543));
#58818=CARTESIAN_POINT('Ctrl Pts',(22.9131468583814,14.9525835222783,-80.4020791700847));
#58819=CARTESIAN_POINT('Ctrl Pts',(22.9127804823919,16.1533922160744,-79.763597861972));
#58820=CARTESIAN_POINT('Ctrl Pts',(22.9124146240747,17.3542009086611,-79.1251165545024));
#58821=CARTESIAN_POINT('Ctrl Pts',(23.5417513911928,13.736769442166,-81.0121414409379));
#58822=CARTESIAN_POINT('Ctrl Pts',(23.5417933622192,14.9375781946617,-80.3736601016141));
#58823=CARTESIAN_POINT('Ctrl Pts',(23.5418352267392,16.138386947973,-79.7351787618567));
#58824=CARTESIAN_POINT('Ctrl Pts',(23.5418771977656,17.3391957004687,-79.0966974225329));
#58825=CARTESIAN_POINT('Ctrl Pts',(24.2730525164329,13.660545753115,-80.8691286744826));
#58826=CARTESIAN_POINT('Ctrl Pts',(24.273680519978,14.8613544010243,-80.2306473907684));
#58827=CARTESIAN_POINT('Ctrl Pts',(24.2743085928193,16.0621630471265,-79.5921661080151));
#58828=CARTESIAN_POINT('Ctrl Pts',(24.2749365963644,17.2629716950359,-78.9536848243009));
#58829=CARTESIAN_POINT('Ctrl Pts',(24.9170787624367,13.5062400436736,-80.579914018049));
#58830=CARTESIAN_POINT('Ctrl Pts',(24.9182622477484,14.7070483369479,-79.9414329228976));
#58831=CARTESIAN_POINT('Ctrl Pts',(24.9194463038521,15.9078566299141,-79.3029518279101));
#58832=CARTESIAN_POINT('Ctrl Pts',(24.9206297891638,17.1086649231884,-78.6644707327587));
#58833=CARTESIAN_POINT('Ctrl Pts',(25.3658123504925,13.2974001437394,-80.1881404327209));
#58834=CARTESIAN_POINT('Ctrl Pts',(25.3673554971624,14.4982081031418,-79.5496595150923));
#58835=CARTESIAN_POINT('Ctrl Pts',(25.368899272135,15.6990160619414,-78.9111785977844));
#58836=CARTESIAN_POINT('Ctrl Pts',(25.3704424188049,16.8998240213439,-78.2726976801559));
#58837=CARTESIAN_POINT('Ctrl Pts',(25.6155655213289,13.0717748423381,-79.7644556106849));
#58838=CARTESIAN_POINT('Ctrl Pts',(25.6172915372986,14.2725826029869,-79.1259747987356));
#58839=CARTESIAN_POINT('Ctrl Pts',(25.6190177037389,15.4733903636591,-78.4874939867739));
#58840=CARTESIAN_POINT('Ctrl Pts',(25.6207437197086,16.674198124308,-77.8490131748246));
#58841=CARTESIAN_POINT('Ctrl Pts',(25.6858818663905,12.9054712360564,-79.4518813295147));
#58842=CARTESIAN_POINT('Ctrl Pts',(25.687655531541,14.1062789411321,-78.8134005471141));
#58843=CARTESIAN_POINT('Ctrl Pts',(25.6894290078439,15.3070866465801,-78.1749197645157));
#58844=CARTESIAN_POINT('Ctrl Pts',(25.6912026729945,16.5078943516558,-77.5364389821151));
#58845=CARTESIAN_POINT('Ctrl Pts',(25.7013237933716,12.8213530409933,-79.2937211639668));
#58846=CARTESIAN_POINT('Ctrl Pts',(25.7031079311239,14.0221607339897,-78.6552403879889));
#58847=CARTESIAN_POINT('Ctrl Pts',(25.7048920688761,15.222968426986,-78.0167596120111));
#58848=CARTESIAN_POINT('Ctrl Pts',(25.7066762066284,16.4237761199824,-77.3782788360332));
#58849=CARTESIAN_POINT('',(20.808,14.4059333415632,-77.928));
#58850=CARTESIAN_POINT('Ctrl Pts',(21.0430574415837,12.442190173977,-78.5797217830346));
#58851=CARTESIAN_POINT('Ctrl Pts',(21.0421674979575,13.6429988456018,-77.9412404867108));
#58852=CARTESIAN_POINT('Ctrl Pts',(21.0412775543313,14.8438075172267,-77.3027591903869));
#58853=CARTESIAN_POINT('Ctrl Pts',(21.0403876107051,16.0446161888516,-76.664277894063));
#58854=CARTESIAN_POINT('Ctrl Pts',(20.9663933429453,12.4981850222955,-78.6851396340205));
#58855=CARTESIAN_POINT('Ctrl Pts',(20.9655036927131,13.6989936940884,-78.0466583376072));
#58856=CARTESIAN_POINT('Ctrl Pts',(20.9646140452926,14.8998023658873,-77.4081770411908));
#58857=CARTESIAN_POINT('Ctrl Pts',(20.9637243950605,16.1006110376802,-76.7696957447776));
#58858=CARTESIAN_POINT('Ctrl Pts',(20.8885043097157,12.5523824450204,-78.7871786835729));
#58859=CARTESIAN_POINT('Ctrl Pts',(20.887617525105,13.7531911184756,-78.1486973862758));
#58860=CARTESIAN_POINT('Ctrl Pts',(20.8867307434391,14.953999791937,-77.5102160889755));
#58861=CARTESIAN_POINT('Ctrl Pts',(20.8858439588284,16.1548084653921,-76.8717347916784));
#58862=CARTESIAN_POINT('Ctrl Pts',(20.8093219165299,12.6047206302974,-78.8857217870086));
#58863=CARTESIAN_POINT('Ctrl Pts',(20.8084406386947,13.8055293069047,-78.2472404880355));
#58864=CARTESIAN_POINT('Ctrl Pts',(20.8075593608596,15.0063379835122,-77.6087591890624));
#58865=CARTESIAN_POINT('Ctrl Pts',(20.8066780830244,16.2071466601195,-76.9702778900892));
#58866=CARTESIAN_POINT('Ctrl Pts',(-18.084171536322,0.0168069507424406,
-47.6825133195673));
#58867=CARTESIAN_POINT('Ctrl Pts',(-18.0828648825787,1.37310817598614,-47.5821760815471));
#58868=CARTESIAN_POINT('Ctrl Pts',(-18.0815581911822,2.72940939835026,-47.4818388069225));
#58869=CARTESIAN_POINT('Ctrl Pts',(-18.0802515374385,4.08571062359393,-47.3815015689019));
#58870=CARTESIAN_POINT('Ctrl Pts',(-17.506930629517,0.00163240881209737,
-47.4849099125784));
#58871=CARTESIAN_POINT('Ctrl Pts',(-17.5065137114848,1.35865940324804,-47.3943886329251));
#58872=CARTESIAN_POINT('Ctrl Pts',(-17.5071471183302,2.71576672268321,-47.3048884241277));
#58873=CARTESIAN_POINT('Ctrl Pts',(-17.506730212951,4.07279371808681,-47.2143671567752));
#58874=CARTESIAN_POINT('Ctrl Pts',(-16.1265953574943,-0.0239511115510788,
-47.0702290864536));
#58875=CARTESIAN_POINT('Ctrl Pts',(-16.132609651975,1.33467278918204,-47.0042231917552));
#58876=CARTESIAN_POINT('Ctrl Pts',(-16.1380915006763,2.69325718740651,-46.9377585627012));
#58877=CARTESIAN_POINT('Ctrl Pts',(-16.1441057887425,4.05188108766375,-46.8717526624765));
#58878=CARTESIAN_POINT('Ctrl Pts',(-14.10127225119,-0.0283229642908482,
-46.5960988598152));
#58879=CARTESIAN_POINT('Ctrl Pts',(-14.1075627501349,1.3313449215142,-46.5628949517334));
#58880=CARTESIAN_POINT('Ctrl Pts',(-14.1138926365074,2.69101592083309,-46.5296830060939));
#58881=CARTESIAN_POINT('Ctrl Pts',(-14.1201831359268,4.05068380667564,-46.4964790979153));
#58882=CARTESIAN_POINT('Ctrl Pts',(-12.7955484756759,-0.0284838878760417,
-46.3416616237862));
#58883=CARTESIAN_POINT('Ctrl Pts',(-12.7985366234782,1.33141633282946,-46.3244926843625));
#58884=CARTESIAN_POINT('Ctrl Pts',(-12.802000111894,2.69135191874657,-46.3078249592564));
#58885=CARTESIAN_POINT('Ctrl Pts',(-12.8049882654227,4.05125213987811,-46.2906560258708));
#58886=CARTESIAN_POINT('Ctrl Pts',(-11.470436949813,-0.0285771185290155,
-46.1028837411342));
#58887=CARTESIAN_POINT('Ctrl Pts',(-11.4702745894939,1.33147515866783,-46.1004393686973));
#58888=CARTESIAN_POINT('Ctrl Pts',(-11.4703724837302,2.69154460495323,-46.0980807984626));
#58889=CARTESIAN_POINT('Ctrl Pts',(-11.4702101265463,4.0515968823569,-46.0956364270593));
#58890=CARTESIAN_POINT('Ctrl Pts',(-9.98689553497245,-0.0298699386781541,
-45.8979097929726));
#58891=CARTESIAN_POINT('Ctrl Pts',(-9.98372271526217,1.3301121906159,-45.9055403357692));
#58892=CARTESIAN_POINT('Ctrl Pts',(-9.98085564305265,2.69011600325979,-45.9134768161035));
#58893=CARTESIAN_POINT('Ctrl Pts',(-9.97768282702567,4.05009813281506,-45.9211073625856));
#58894=CARTESIAN_POINT('Ctrl Pts',(-8.14237944721806,-0.0324247744844724,
-45.7230625805931));
#58895=CARTESIAN_POINT('Ctrl Pts',(-8.13997400378338,1.32751302340312,-45.7374232436365));
#58896=CARTESIAN_POINT('Ctrl Pts',(-8.1376557237031,2.68745306043262,-45.7518461445845));
#58897=CARTESIAN_POINT('Ctrl Pts',(-8.13525028131847,4.04739085834718,-45.7662068083777));
#58898=CARTESIAN_POINT('Ctrl Pts',(-6.87097468423606,-0.0328533238228722,
-45.6419015366938));
#58899=CARTESIAN_POINT('Ctrl Pts',(-6.87002039103409,1.32705155847938,-45.658581401155));
#58900=CARTESIAN_POINT('Ctrl Pts',(-6.86920619802231,2.6869629011669,-45.6753523082089));
#58901=CARTESIAN_POINT('Ctrl Pts',(-6.8682519065081,4.04686778354698,-45.692032173767));
#58902=CARTESIAN_POINT('Ctrl Pts',(-5.13083769090565,-0.0319736651072693,
-45.5581580996358));
#58903=CARTESIAN_POINT('Ctrl Pts',(-5.1319190187102,1.32790705483533,-45.5768752722455));
#58904=CARTESIAN_POINT('Ctrl Pts',(-5.1330666952011,2.68779052666114,-45.5956441954884));
#58905=CARTESIAN_POINT('Ctrl Pts',(-5.13414802380493,4.04767124663689,-45.6143613687216));
#58906=CARTESIAN_POINT('Ctrl Pts',(-2.82311055870927,-0.0277859137287846,
-45.4820465344085));
#58907=CARTESIAN_POINT('Ctrl Pts',(-2.82542111997424,1.33207058630606,-45.5021622318001));
#58908=CARTESIAN_POINT('Ctrl Pts',(-2.82765880245458,2.69193303472359,-45.5223443526086));
#58909=CARTESIAN_POINT('Ctrl Pts',(-2.8299693628416,4.0517895348301,-45.5424600508003));
#58910=CARTESIAN_POINT('Ctrl Pts',(-0.827876248095319,-0.0254184256084418,
-45.4363857618409));
#58911=CARTESIAN_POINT('Ctrl Pts',(-0.828401955565921,1.33442934851277,
-45.4573391307405));
#58912=CARTESIAN_POINT('Ctrl Pts',(-0.829171501015099,2.69427440248123,
-45.4782808761721));
#58913=CARTESIAN_POINT('Ctrl Pts',(-0.829697211423176,4.05412217656967,
-45.4992342449317));
#58914=CARTESIAN_POINT('Ctrl Pts',(2.96793475906394E-5,-0.0251511567891935,
-45.4192962601408));
#58915=CARTESIAN_POINT('Ctrl Pts',(2.96981943129004E-5,1.33469071903223,
-45.4405648948134));
#58916=CARTESIAN_POINT('Ctrl Pts',(2.97257824282988E-5,2.69453259495117,
-45.4618335299028));
#58917=CARTESIAN_POINT('Ctrl Pts',(2.97446292558659E-5,4.05437447077259,
-45.4831021645754));
#58918=CARTESIAN_POINT('Ctrl Pts',(-25.7013237899579,12.8213507429086,-79.29372238588));
#58919=CARTESIAN_POINT('Ctrl Pts',(-25.7020884215611,13.3359833773638,-79.0200873602994));
#58920=CARTESIAN_POINT('Ctrl Pts',(-25.703872560451,14.5367918363885,-78.3816061770171));
#58921=CARTESIAN_POINT('Ctrl Pts',(-25.7056566993409,15.737600295413,-77.7431249937349));
#58922=CARTESIAN_POINT('Ctrl Pts',(-25.7066762066276,16.4237761199824,-77.3782788360333));
#58923=CARTESIAN_POINT('Ctrl Pts',(-25.6858655966018,12.9055575473563,-79.4520491559888));
#58924=CARTESIAN_POINT('Ctrl Pts',(-25.6866261120234,13.4201901873017,-79.178414127489));
#58925=CARTESIAN_POINT('Ctrl Pts',(-25.6883996507926,14.620998658509,-78.5399329377291));
#58926=CARTESIAN_POINT('Ctrl Pts',(-25.6901723542552,15.8218071291893,-77.9014517482493));
#58927=CARTESIAN_POINT('Ctrl Pts',(-25.6911863733062,16.507982961079,-77.5366055866555));
#58928=CARTESIAN_POINT('Ctrl Pts',(-25.6167632558673,13.0699277926588,-79.7609931774108));
#58929=CARTESIAN_POINT('Ctrl Pts',(-25.6175025156277,13.5845604555093,-79.4873581367321));
#58930=CARTESIAN_POINT('Ctrl Pts',(-25.6192286397047,14.7853689809119,-78.8488769181561));
#58931=CARTESIAN_POINT('Ctrl Pts',(-25.6209557588151,15.9861775064173,-78.2103956995253));
#58932=CARTESIAN_POINT('Ctrl Pts',(-25.6219414370306,16.672353368847,-77.845549521693));
#58933=CARTESIAN_POINT('Ctrl Pts',(-25.2826927947797,13.3728687263107,-80.3298613001038));
#58934=CARTESIAN_POINT('Ctrl Pts',(-25.283329806226,13.887501503606,-80.0562261985736));
#58935=CARTESIAN_POINT('Ctrl Pts',(-25.2848135698082,15.0883102951698,-79.4177448384771));
#58936=CARTESIAN_POINT('Ctrl Pts',(-25.2862951562559,16.2891190861009,-78.7792634787171));
#58937=CARTESIAN_POINT('Ctrl Pts',(-25.2871445035823,16.9752951011235,-78.4144172197497));
#58938=CARTESIAN_POINT('Ctrl Pts',(-24.6852313330219,13.5767391583647,-80.7120457511261));
#58939=CARTESIAN_POINT('Ctrl Pts',(-24.6856528650133,14.0913721211625,-80.4384105509626));
#58940=CARTESIAN_POINT('Ctrl Pts',(-24.6866372266374,15.2921813464143,-79.7999289602702));
#58941=CARTESIAN_POINT('Ctrl Pts',(-24.6876222491661,16.4929905717456,-79.1614473695355));
#58942=CARTESIAN_POINT('Ctrl Pts',(-24.6881842909862,17.1791668341045,-78.7966009790571));
#58943=CARTESIAN_POINT('Ctrl Pts',(-24.0040551378999,13.6893795635206,-80.9232212941775));
#58944=CARTESIAN_POINT('Ctrl Pts',(-24.004230358018,14.2040126262127,-80.6495860408992));
#58945=CARTESIAN_POINT('Ctrl Pts',(-24.004639900488,15.4048220842307,-80.0111043264428));
#58946=CARTESIAN_POINT('Ctrl Pts',(-24.0050500267346,16.6056315420595,-79.372622612087));
#58947=CARTESIAN_POINT('Ctrl Pts',(-24.0052836532123,17.2918079376106,-79.007776150789));
#58948=CARTESIAN_POINT('Ctrl Pts',(-23.4548778566481,13.7384359365402,-81.0153105837569));
#58949=CARTESIAN_POINT('Ctrl Pts',(-23.4548724406338,14.253069021085,-80.7416753188595));
#58950=CARTESIAN_POINT('Ctrl Pts',(-23.4548599684916,15.4538785303795,-80.1031935771389));
#58951=CARTESIAN_POINT('Ctrl Pts',(-23.4548476349486,16.654688039726,-79.4647118353906));
#58952=CARTESIAN_POINT('Ctrl Pts',(-23.4548404136072,17.3408644644138,-79.0998653586004));
#58953=CARTESIAN_POINT('Ctrl Pts',(-22.9164771617764,13.7513551462076,-81.0397745016549));
#58954=CARTESIAN_POINT('Ctrl Pts',(-22.9163209973395,14.2659882094511,-80.7661392480834));
#58955=CARTESIAN_POINT('Ctrl Pts',(-22.9159572365429,15.4667976692766,-80.127657532666));
#58956=CARTESIAN_POINT('Ctrl Pts',(-22.9155939980342,16.6676071293499,-79.4891758171168));
#58957=CARTESIAN_POINT('Ctrl Pts',(-22.915385779096,17.3537835256363,-79.1243293554279));
#58958=CARTESIAN_POINT('Ctrl Pts',(-22.4549655367611,13.7323867778409,-81.0044664289556));
#58959=CARTESIAN_POINT('Ctrl Pts',(-22.4547109103277,14.2470198074144,-80.7308311932868));
#58960=CARTESIAN_POINT('Ctrl Pts',(-22.4541168974148,15.447829188375,-80.0923495198026));
#58961=CARTESIAN_POINT('Ctrl Pts',(-22.4535229809148,16.6486385693303,-79.4538678463211));
#58962=CARTESIAN_POINT('Ctrl Pts',(-22.453183479509,17.3348149207234,-79.0890214085024));
#58963=CARTESIAN_POINT('Ctrl Pts',(-22.1430512368791,13.6992998972659,-80.9425723760123));
#58964=CARTESIAN_POINT('Ctrl Pts',(-22.1427473388653,14.2139329047488,-80.6689371520894));
#58965=CARTESIAN_POINT('Ctrl Pts',(-22.1420384096197,15.4147422343653,-80.0304555059053));
#58966=CARTESIAN_POINT('Ctrl Pts',(-22.1413296192275,16.6155515641451,-79.3919738596343));
#58967=CARTESIAN_POINT('Ctrl Pts',(-22.1409244224793,17.3017278860839,-79.0271274374767));
#58968=CARTESIAN_POINT('Ctrl Pts',(-21.9706189386793,13.6744394516519,-80.8960170933706));
#58969=CARTESIAN_POINT('Ctrl Pts',(-21.9702923495131,14.1890724482461,-80.6223818752372));
#58970=CARTESIAN_POINT('Ctrl Pts',(-21.9695304663557,15.3898817523233,-79.9839002426326));
#58971=CARTESIAN_POINT('Ctrl Pts',(-21.9687687153957,16.5906910564529,-79.3454186100002));
#58972=CARTESIAN_POINT('Ctrl Pts',(-21.9683332638225,17.2768673638735,-78.980572195562));
#58973=CARTESIAN_POINT('Ctrl Pts',(-21.8446726909401,13.6525925417021,-80.8550829230538));
#58974=CARTESIAN_POINT('Ctrl Pts',(-21.844331772734,14.1672255309889,-80.5814477088058));
#58975=CARTESIAN_POINT('Ctrl Pts',(-21.8435364464263,15.3680348180929,-79.942966085226));
#58976=CARTESIAN_POINT('Ctrl Pts',(-21.8427412449731,16.5688441053144,-79.3044844615836));
#58977=CARTESIAN_POINT('Ctrl Pts',(-21.842286688042,17.2550204029918,-78.9396380523261));
#58978=CARTESIAN_POINT('Ctrl Pts',(-21.721746177194,13.6272172866624,-80.8075149514255));
#58979=CARTESIAN_POINT('Ctrl Pts',(-21.7213933708601,14.1418502697189,-80.5338797404902));
#58980=CARTESIAN_POINT('Ctrl Pts',(-21.7205703008806,15.3426595422183,-79.8953981246758));
#58981=CARTESIAN_POINT('Ctrl Pts',(-21.7197473517875,16.5434688147785,-79.2569165088291));
#58982=CARTESIAN_POINT('Ctrl Pts',(-21.7192769440428,17.2296451041489,-78.8920701039884));
#58983=CARTESIAN_POINT('Ctrl Pts',(-21.6228148027256,13.6030088775296,-80.7621149641663));
#58984=CARTESIAN_POINT('Ctrl Pts',(-21.6224540937013,14.1176418562761,-80.4884797555227));
#58985=CARTESIAN_POINT('Ctrl Pts',(-21.6216125658996,15.318451118753,-79.8499981450373));
#58986=CARTESIAN_POINT('Ctrl Pts',(-21.6207711436935,16.5192603813193,-79.2115165345044));
#58987=CARTESIAN_POINT('Ctrl Pts',(-21.6202901990439,17.2054366649431,-78.8466701327192));
#58988=CARTESIAN_POINT('Ctrl Pts',(-21.5604515982842,13.5856860066143,-80.7296183597009));
#58989=CARTESIAN_POINT('Ctrl Pts',(-21.5600866332627,14.1003189830252,-80.4559831522991));
#58990=CARTESIAN_POINT('Ctrl Pts',(-21.5592351816853,15.3011282400274,-79.8175015447247));
#58991=CARTESIAN_POINT('Ctrl Pts',(-21.5583838414717,16.501937497098,-79.1790199371138));
#58992=CARTESIAN_POINT('Ctrl Pts',(-21.5578972221677,17.1881137776076,-78.8141735369845));
#58993=CARTESIAN_POINT('Ctrl Pts',(-21.5226324038841,13.574613873599,-80.7088453355964));
#58994=CARTESIAN_POINT('Ctrl Pts',(-21.5222650446281,14.0892468486761,-80.4352101289038));
#58995=CARTESIAN_POINT('Ctrl Pts',(-21.521408000631,15.2900561025754,-79.7967285229793));
#58996=CARTESIAN_POINT('Ctrl Pts',(-21.5205510630675,16.4908653565509,-79.1582469170141));
#58997=CARTESIAN_POINT('Ctrl Pts',(-21.5200612514553,17.1770416352821,-78.7934005178304));
#58998=CARTESIAN_POINT('Ctrl Pts',(-21.4945991349715,13.5660570588058,-80.6927900206057));
#58999=CARTESIAN_POINT('Ctrl Pts',(-21.4942301067783,14.0806900329552,-80.4191548144064));
#59000=CARTESIAN_POINT('Ctrl Pts',(-21.4933691690818,15.2814992846826,-79.7806732096367));
#59001=CARTESIAN_POINT('Ctrl Pts',(-21.4925083382252,16.4823085364802,-79.1421916048296));
#59002=CARTESIAN_POINT('Ctrl Pts',(-21.4920163013668,17.1684848139744,-78.7773452063036));
#59003=CARTESIAN_POINT('Ctrl Pts',(-21.4624099987218,13.5557020135771,-80.6733585467387));
#59004=CARTESIAN_POINT('Ctrl Pts',(-21.4620392051584,14.0703349867346,-80.3997233410669));
#59005=CARTESIAN_POINT('Ctrl Pts',(-21.4611741483302,15.271144236153,-79.7612417375249));
#59006=CARTESIAN_POINT('Ctrl Pts',(-21.4603091983932,16.4719534856458,-79.1227601339433));
#59007=CARTESIAN_POINT('Ctrl Pts',(-21.4598148077115,17.1581297618176,-78.7579137361204));
#59008=CARTESIAN_POINT('Ctrl Pts',(-21.435185616044,13.5465681568376,-80.6562172227997));
#59009=CARTESIAN_POINT('Ctrl Pts',(-21.4348134318159,14.0612011292143,-80.3825820175431));
#59010=CARTESIAN_POINT('Ctrl Pts',(-21.4339451256095,15.2620103768036,-79.7441004149736));
#59011=CARTESIAN_POINT('Ctrl Pts',(-21.4330769225221,16.4628196244617,-79.1056188123675));
#59012=CARTESIAN_POINT('Ctrl Pts',(-21.4325806776235,17.1489958995923,-78.7407724150982));
#59013=CARTESIAN_POINT('Ctrl Pts',(-21.412809848635,13.5387370119342,-80.6415194725682));
#59014=CARTESIAN_POINT('Ctrl Pts',(-21.4124365976858,14.0533699837061,-80.367884267633));
#59015=CARTESIAN_POINT('Ctrl Pts',(-21.4115658102438,15.254179229894,-79.7294026658087));
#59016=CARTESIAN_POINT('Ctrl Pts',(-21.4106951324464,16.4549884761586,-79.0909210639435));
#59017=CARTESIAN_POINT('Ctrl Pts',(-21.410197465255,17.1411647504829,-78.726074667103));
#59018=CARTESIAN_POINT('Ctrl Pts',(-21.3951093791352,13.5323422126205,-80.6295167784899));
#59019=CARTESIAN_POINT('Ctrl Pts',(-21.3947353396864,14.0469751839487,-80.3558815737907));
#59020=CARTESIAN_POINT('Ctrl Pts',(-21.393862699644,15.2477844290876,-79.7173999725242));
#59021=CARTESIAN_POINT('Ctrl Pts',(-21.3929901585335,16.4485936742919,-79.0789183712227));
#59022=CARTESIAN_POINT('Ctrl Pts',(-21.392491440011,17.1347699480245,-78.7140719746968));
#59023=CARTESIAN_POINT('Ctrl Pts',(-21.2456739047379,13.4771896612147,-80.5259944040367));
#59024=CARTESIAN_POINT('Ctrl Pts',(-21.2452933752653,13.9918226288365,-80.2523592013081));
#59025=CARTESIAN_POINT('Ctrl Pts',(-21.2444057029843,15.1926318654482,-79.6138776045755));
#59026=CARTESIAN_POINT('Ctrl Pts',(-21.2435182228696,16.3934411022267,-78.9753960077542));
#59027=CARTESIAN_POINT('Ctrl Pts',(-21.2430108509951,17.0796173710175,-78.6105496138558));
#59028=CARTESIAN_POINT('Ctrl Pts',(-21.0039921951822,13.3500335523429,-80.2871869099115));
#59029=CARTESIAN_POINT('Ctrl Pts',(-21.0036094681115,13.8646665186922,-80.0135517078596));
#59030=CARTESIAN_POINT('Ctrl Pts',(-21.0027164067956,15.0654757521404,-79.3750701128091));
#59031=CARTESIAN_POINT('Ctrl Pts',(-21.0018233184298,16.2662849855924,-78.7365885177565));
#59032=CARTESIAN_POINT('Ctrl Pts',(-21.0013130164285,16.9524612526866,-78.3717421247602));
#59033=CARTESIAN_POINT('Ctrl Pts',(-20.7414740910803,13.032826850117,-79.6909716241468));
#59034=CARTESIAN_POINT('Ctrl Pts',(-20.7410979762074,13.5474598202787,-79.4173364200678));
#59035=CARTESIAN_POINT('Ctrl Pts',(-20.7402205762101,14.7482690627728,-78.7788548202075));
#59036=CARTESIAN_POINT('Ctrl Pts',(-20.7393433445201,15.9490783053969,-78.140373220278));
#59037=CARTESIAN_POINT('Ctrl Pts',(-20.7388418587697,16.6352545775742,-77.7755268245789));
#59038=CARTESIAN_POINT('Ctrl Pts',(-20.7586989978057,12.7713419783598,-79.1991663833854));
#59039=CARTESIAN_POINT('Ctrl Pts',(-20.7583231666064,13.2859749486613,-78.9255311792321));
#59040=CARTESIAN_POINT('Ctrl Pts',(-20.7574453618225,14.4867841908561,-78.2870495795309));
#59041=CARTESIAN_POINT('Ctrl Pts',(-20.7565668304884,15.6875934326558,-77.6485679800397));
#59042=CARTESIAN_POINT('Ctrl Pts',(-20.7560657229672,16.3737697050196,-77.2837215842416));
#59043=CARTESIAN_POINT('Ctrl Pts',(-20.8093219182155,12.6047183322107,-78.8857230089227));
#59044=CARTESIAN_POINT('Ctrl Pts',(-20.8089442272165,13.1193513014583,-78.6120878053298));
#59045=CARTESIAN_POINT('Ctrl Pts',(-20.8080629489683,14.3201605416643,-77.9736062066861));
#59046=CARTESIAN_POINT('Ctrl Pts',(-20.8071816707202,15.5209697818703,-77.3351246080423));
#59047=CARTESIAN_POINT('Ctrl Pts',(-20.8066780834711,16.2071460528287,-76.9702782129914));
#59048=CARTESIAN_POINT('',(-25.704,14.6225645804878,-78.336));
#59049=CARTESIAN_POINT('Ctrl Pts',(-25.9521939365424,12.4413225404486,-78.5797210091185));
#59050=CARTESIAN_POINT('Ctrl Pts',(-25.9541384795005,13.6421300392938,-77.9412403363727));
#59051=CARTESIAN_POINT('Ctrl Pts',(-25.9560830224586,14.8429375381389,-77.3027596636269));
#59052=CARTESIAN_POINT('Ctrl Pts',(-25.9580275654167,16.0437450369841,-76.6642789908811));
#59053=CARTESIAN_POINT('Ctrl Pts',(-25.8694498071432,12.5700415836659,-78.8215543165566));
#59054=CARTESIAN_POINT('Ctrl Pts',(-25.8713452879931,13.7708491444509,-78.1830736108767));
#59055=CARTESIAN_POINT('Ctrl Pts',(-25.8732407643774,14.9716567052373,-77.5445929051962));
#59056=CARTESIAN_POINT('Ctrl Pts',(-25.8751362452272,16.1724642660223,-76.9061121995164));
#59057=CARTESIAN_POINT('Ctrl Pts',(-25.7857936084007,12.6969907473229,-79.0600657450643));
#59058=CARTESIAN_POINT('Ctrl Pts',(-25.7876353781899,13.8977983735652,-78.4215850045802));
#59059=CARTESIAN_POINT('Ctrl Pts',(-25.7894771453224,15.0986059998054,-77.7831042640973));
#59060=CARTESIAN_POINT('Ctrl Pts',(-25.7913189151116,16.2994136260477,-77.1446235236132));
#59061=CARTESIAN_POINT('Ctrl Pts',(-25.7013237933724,12.8213530409933,-79.2937211639668));
#59062=CARTESIAN_POINT('Ctrl Pts',(-25.7031079311241,14.0221607339896,-78.6552403879889));
#59063=CARTESIAN_POINT('Ctrl Pts',(-25.7048920688759,15.222968426986,-78.0167596120111));
#59064=CARTESIAN_POINT('Ctrl Pts',(-25.7066762066276,16.4237761199824,-77.3782788360333));
#59065=CARTESIAN_POINT('',(0.,0.,0.));
#59066=CARTESIAN_POINT('Origin',(-29.376,24.6394718625761,38.352));
#59067=CARTESIAN_POINT('',(-33.2237359312881,25.0637359312881,38.352));
#59068=CARTESIAN_POINT('',(-29.376,25.0637359312881,42.1997359312881));
#59069=CARTESIAN_POINT('Origin',(-29.376,25.0637359312881,38.352));
#59070=CARTESIAN_POINT('',(-29.376,24.6394718625761,42.024));
#59071=CARTESIAN_POINT('Origin',(-29.376,24.6394718625761,42.624));
#59072=CARTESIAN_POINT('',(-33.048,24.6394718625761,38.352));
#59073=CARTESIAN_POINT('Origin',(-29.376,24.6394718625761,38.352));
#59074=CARTESIAN_POINT('Origin',(-29.376,24.6394718625761,38.352));
#59075=CARTESIAN_POINT('Origin',(-29.376,25.0637359312881,38.352));
#59076=CARTESIAN_POINT('Origin',(-29.376,22.44,38.352));
#59077=CARTESIAN_POINT('',(-29.376,23.04,34.68));
#59078=CARTESIAN_POINT('',(-33.048,23.04,38.352));
#59079=CARTESIAN_POINT('Origin',(-29.376,23.04,38.352));
#59080=CARTESIAN_POINT('Origin',(-29.376,23.04,38.352));
#59081=CARTESIAN_POINT('',(-33.048,22.44,38.352));
#59082=CARTESIAN_POINT('Origin',(-29.376,25.296,38.352));
#59083=CARTESIAN_POINT('',(-33.6882640687119,25.5282640687119,38.352));
#59084=CARTESIAN_POINT('',(-33.456,25.296,38.352));
#59085=CARTESIAN_POINT('',(-29.376,25.5282640687119,34.0397359312881));
#59086=CARTESIAN_POINT('Origin',(-29.376,25.5282640687119,38.352));
#59087=CARTESIAN_POINT('Origin',(-29.376,25.5282640687119,38.352));
#59088=CARTESIAN_POINT('Origin',(-17.352,22.44,6.82615721505037));
#59089=CARTESIAN_POINT('',(-17.952,23.04,6.82615721505037));
#59090=CARTESIAN_POINT('',(-17.5132903225806,23.04,7.40407194218736));
#59091=CARTESIAN_POINT('Origin',(-17.352,23.04,6.82615721505037));
#59092=CARTESIAN_POINT('',(-17.5132903225806,25.104,7.40407194218736));
#59093=CARTESIAN_POINT('',(-17.5132903225806,22.44,7.40407194218736));
#59094=CARTESIAN_POINT('',(-17.952,25.104,6.82615721505037));
#59095=CARTESIAN_POINT('Origin',(-17.352,25.104,6.82615721505037));
#59096=CARTESIAN_POINT('',(-17.952,22.44,6.82615721505037));
#59097=CARTESIAN_POINT('Origin',(-17.352,25.104,6.82615721505037));
#59098=CARTESIAN_POINT('',(-17.352,25.704,6.82615721505037));
#59099=CARTESIAN_POINT('Origin',(-17.352,25.104,6.82615721505037));
#59100=CARTESIAN_POINT('Origin',(-17.352,25.104,6.82615721505037));
#59101=CARTESIAN_POINT('Origin',(-17.352,23.04,6.82615721505037));
#59102=CARTESIAN_POINT('',(-17.352,22.44,6.82615721505037));
#59103=CARTESIAN_POINT('Origin',(-17.352,23.04,6.82615721505037));
#59104=CARTESIAN_POINT('Origin',(-17.352,23.04,6.82615721505037));
#59105=CARTESIAN_POINT('Origin',(-17.352,25.104,5.1));
#59106=CARTESIAN_POINT('',(-17.352,25.704,-32.9381572150504));
#59107=CARTESIAN_POINT('',(-17.352,25.704,5.1));
#59108=CARTESIAN_POINT('',(-17.952,25.104,-32.9381572150504));
#59109=CARTESIAN_POINT('Origin',(-17.352,25.104,-32.9381572150504));
#59110=CARTESIAN_POINT('',(-17.952,25.104,5.1));
#59111=CARTESIAN_POINT('Origin',(-17.952,25.104,8.976));
#59112=CARTESIAN_POINT('',(-19.5239280578126,25.104,9.41470967741935));
#59113=CARTESIAN_POINT('Origin',(-17.952,25.104,8.976));
#59114=CARTESIAN_POINT('',(-20.1018427849496,25.704,9.576));
#59115=CARTESIAN_POINT('Origin',(-20.1018427849496,25.104,9.576));
#59116=CARTESIAN_POINT('Origin',(-17.952,25.704,8.976));
#59117=CARTESIAN_POINT('Origin',(-17.952,22.44,8.976));
#59118=CARTESIAN_POINT('',(-19.5239280578126,23.04,9.41470967741935));
#59119=CARTESIAN_POINT('Origin',(-17.952,23.04,8.976));
#59120=CARTESIAN_POINT('',(-19.5239280578126,22.44,9.41470967741935));
#59121=CARTESIAN_POINT('Origin',(-17.352,22.44,-32.9381572150504));
#59122=CARTESIAN_POINT('',(-17.5132903225806,25.104,-33.5160719421874));
#59123=CARTESIAN_POINT('Origin',(-17.352,25.104,-32.9381572150504));
#59124=CARTESIAN_POINT('',(-17.5132903225806,23.04,-33.5160719421874));
#59125=CARTESIAN_POINT('',(-17.5132903225806,22.44,-33.5160719421874));
#59126=CARTESIAN_POINT('',(-17.952,23.04,-32.9381572150504));
#59127=CARTESIAN_POINT('Origin',(-17.352,23.04,-32.9381572150504));
#59128=CARTESIAN_POINT('',(-17.952,22.44,-32.9381572150504));
#59129=CARTESIAN_POINT('Origin',(-17.352,23.04,-32.9381572150504));
#59130=CARTESIAN_POINT('',(-17.352,22.44,-32.9381572150504));
#59131=CARTESIAN_POINT('Origin',(-17.352,23.04,-32.9381572150504));
#59132=CARTESIAN_POINT('Origin',(-17.352,23.04,-32.9381572150504));
#59133=CARTESIAN_POINT('Origin',(-17.352,25.104,-32.9381572150504));
#59134=CARTESIAN_POINT('Origin',(-17.352,25.104,-32.9381572150504));
#59135=CARTESIAN_POINT('Origin',(-17.952,25.104,-35.088));
#59136=CARTESIAN_POINT('',(-20.1018427849496,25.704,-35.688));
#59137=CARTESIAN_POINT('Origin',(-17.952,25.704,-35.088));
#59138=CARTESIAN_POINT('',(-19.5239280578126,25.104,-35.5267096774194));
#59139=CARTESIAN_POINT('Origin',(-20.1018427849496,25.104,-35.688));
#59140=CARTESIAN_POINT('Origin',(-17.952,25.104,-35.088));
#59141=CARTESIAN_POINT('Origin',(-17.952,22.44,8.976));
#59142=CARTESIAN_POINT('',(-17.952,23.04,5.1));
#59143=CARTESIAN_POINT('Origin',(-20.1018427849496,22.44,-35.688));
#59144=CARTESIAN_POINT('',(-20.1018427849496,23.04,-35.088));
#59145=CARTESIAN_POINT('',(-19.5239280578126,23.04,-35.5267096774194));
#59146=CARTESIAN_POINT('Origin',(-20.1018427849496,23.04,-35.688));
#59147=CARTESIAN_POINT('',(-19.5239280578126,22.44,-35.5267096774194));
#59148=CARTESIAN_POINT('',(-20.1018427849496,25.104,-35.088));
#59149=CARTESIAN_POINT('Origin',(-20.1018427849496,25.104,-35.688));
#59150=CARTESIAN_POINT('',(-20.1018427849496,22.44,-35.088));
#59151=CARTESIAN_POINT('Origin',(-20.1018427849496,25.104,-35.688));
#59152=CARTESIAN_POINT('Origin',(-20.1018427849496,25.104,-35.688));
#59153=CARTESIAN_POINT('Origin',(-20.1018427849496,23.04,-35.688));
#59154=CARTESIAN_POINT('',(-20.1018427849496,22.44,-35.688));
#59155=CARTESIAN_POINT('Origin',(-20.1018427849496,23.04,-35.688));
#59156=CARTESIAN_POINT('Origin',(-20.1018427849496,23.04,-35.688));
#59157=CARTESIAN_POINT('Origin',(-8.976,25.104,-35.688));
#59158=CARTESIAN_POINT('',(-26.4101572150504,25.704,-35.688));
#59159=CARTESIAN_POINT('',(-8.976,25.704,-35.688));
#59160=CARTESIAN_POINT('',(-26.4101572150504,25.104,-35.088));
#59161=CARTESIAN_POINT('Origin',(-26.4101572150504,25.104,-35.688));
#59162=CARTESIAN_POINT('',(-8.976,25.104,-35.088));
#59163=CARTESIAN_POINT('Origin',(-17.952,22.44,-35.088));
#59164=CARTESIAN_POINT('Origin',(-17.952,23.04,-35.088));
#59165=CARTESIAN_POINT('Origin',(-26.4101572150504,22.44,-35.688));
#59166=CARTESIAN_POINT('',(-26.9880719421874,25.104,-35.5267096774194));
#59167=CARTESIAN_POINT('Origin',(-26.4101572150504,25.104,-35.688));
#59168=CARTESIAN_POINT('',(-26.9880719421874,23.04,-35.5267096774194));
#59169=CARTESIAN_POINT('',(-26.9880719421874,22.44,-35.5267096774194));
#59170=CARTESIAN_POINT('',(-26.4101572150504,23.04,-35.088));
#59171=CARTESIAN_POINT('Origin',(-26.4101572150504,23.04,-35.688));
#59172=CARTESIAN_POINT('',(-26.4101572150504,22.44,-35.088));
#59173=CARTESIAN_POINT('Origin',(-26.4101572150504,23.04,-35.688));
#59174=CARTESIAN_POINT('',(-26.4101572150504,22.44,-35.688));
#59175=CARTESIAN_POINT('Origin',(-26.4101572150504,23.04,-35.688));
#59176=CARTESIAN_POINT('Origin',(-26.4101572150504,23.04,-35.688));
#59177=CARTESIAN_POINT('Origin',(-26.4101572150504,25.104,-35.688));
#59178=CARTESIAN_POINT('Origin',(-26.4101572150504,25.104,-35.688));
#59179=CARTESIAN_POINT('Origin',(-28.56,25.104,-35.088));
#59180=CARTESIAN_POINT('',(-29.16,25.704,-32.9381572150504));
#59181=CARTESIAN_POINT('Origin',(-28.56,25.704,-35.088));
#59182=CARTESIAN_POINT('',(-28.9987096774194,25.104,-33.5160719421874));
#59183=CARTESIAN_POINT('Origin',(-29.16,25.104,-32.9381572150504));
#59184=CARTESIAN_POINT('Origin',(-28.56,25.104,-35.088));
#59185=CARTESIAN_POINT('Origin',(-17.952,22.44,-35.088));
#59186=CARTESIAN_POINT('',(-8.976,23.04,-35.088));
#59187=CARTESIAN_POINT('Origin',(26.4101572150504,22.44,9.576));
#59188=CARTESIAN_POINT('',(26.4101572150504,25.104,8.976));
#59189=CARTESIAN_POINT('',(26.9880719421874,25.104,9.41470967741935));
#59190=CARTESIAN_POINT('Origin',(26.4101572150504,25.104,9.576));
#59191=CARTESIAN_POINT('',(26.9880719421874,23.04,9.41470967741935));
#59192=CARTESIAN_POINT('',(26.9880719421874,22.44,9.41470967741935));
#59193=CARTESIAN_POINT('',(26.4101572150504,23.04,8.976));
#59194=CARTESIAN_POINT('Origin',(26.4101572150504,23.04,9.576));
#59195=CARTESIAN_POINT('',(26.4101572150504,22.44,8.976));
#59196=CARTESIAN_POINT('Origin',(26.4101572150504,23.04,9.576));
#59197=CARTESIAN_POINT('',(26.4101572150504,22.44,9.576));
#59198=CARTESIAN_POINT('Origin',(26.4101572150504,23.04,9.576));
#59199=CARTESIAN_POINT('Origin',(26.4101572150504,23.04,9.576));
#59200=CARTESIAN_POINT('Origin',(26.4101572150504,25.104,9.576));
#59201=CARTESIAN_POINT('',(26.4101572150504,25.704,9.576));
#59202=CARTESIAN_POINT('Origin',(26.4101572150504,25.104,9.576));
#59203=CARTESIAN_POINT('Origin',(26.4101572150504,25.104,9.576));
#59204=CARTESIAN_POINT('Origin',(28.56,25.104,8.976));
#59205=CARTESIAN_POINT('',(29.16,25.704,6.82615721505037));
#59206=CARTESIAN_POINT('Origin',(28.56,25.704,8.976));
#59207=CARTESIAN_POINT('',(28.9987096774193,25.104,7.40407194218736));
#59208=CARTESIAN_POINT('Origin',(29.16,25.104,6.82615721505037));
#59209=CARTESIAN_POINT('Origin',(28.56,25.104,8.976));
#59210=CARTESIAN_POINT('Origin',(8.976,25.104,9.576));
#59211=CARTESIAN_POINT('',(20.1018427849496,25.104,8.976));
#59212=CARTESIAN_POINT('',(8.976,25.104,8.976));
#59213=CARTESIAN_POINT('',(20.1018427849496,25.704,9.576));
#59214=CARTESIAN_POINT('Origin',(20.1018427849496,25.104,9.576));
#59215=CARTESIAN_POINT('',(8.976,25.704,9.576));
#59216=CARTESIAN_POINT('Origin',(17.952,22.44,8.976));
#59217=CARTESIAN_POINT('',(20.1018427849496,23.04,8.976));
#59218=CARTESIAN_POINT('',(8.976,23.04,8.976));
#59219=CARTESIAN_POINT('',(20.1018427849496,22.44,8.976));
#59220=CARTESIAN_POINT('Origin',(29.16,22.44,6.82615721505037));
#59221=CARTESIAN_POINT('',(28.56,23.04,6.82615721505037));
#59222=CARTESIAN_POINT('',(28.9987096774193,23.04,7.40407194218736));
#59223=CARTESIAN_POINT('Origin',(29.16,23.04,6.82615721505037));
#59224=CARTESIAN_POINT('',(28.9987096774193,22.44,7.40407194218736));
#59225=CARTESIAN_POINT('',(28.56,25.104,6.82615721505037));
#59226=CARTESIAN_POINT('Origin',(29.16,25.104,6.82615721505037));
#59227=CARTESIAN_POINT('',(28.56,22.44,6.82615721505037));
#59228=CARTESIAN_POINT('Origin',(29.16,25.104,6.82615721505037));
#59229=CARTESIAN_POINT('Origin',(29.16,25.104,6.82615721505037));
#59230=CARTESIAN_POINT('Origin',(29.16,23.04,6.82615721505037));
#59231=CARTESIAN_POINT('',(29.16,22.44,6.82615721505037));
#59232=CARTESIAN_POINT('Origin',(29.16,23.04,6.82615721505037));
#59233=CARTESIAN_POINT('Origin',(29.16,23.04,6.82615721505037));
#59234=CARTESIAN_POINT('Origin',(29.16,25.104,5.1));
#59235=CARTESIAN_POINT('',(29.16,25.704,-32.9381572150504));
#59236=CARTESIAN_POINT('',(29.16,25.704,5.1));
#59237=CARTESIAN_POINT('',(28.56,25.104,-32.9381572150504));
#59238=CARTESIAN_POINT('Origin',(29.16,25.104,-32.9381572150504));
#59239=CARTESIAN_POINT('',(28.56,25.104,5.1));
#59240=CARTESIAN_POINT('Origin',(28.56,22.44,8.976));
#59241=CARTESIAN_POINT('Origin',(28.56,23.04,8.976));
#59242=CARTESIAN_POINT('Origin',(-28.152,23.04,28.56));
#59243=CARTESIAN_POINT('',(-28.152,22.44,25.46));
#59244=CARTESIAN_POINT('Origin',(-28.152,22.44,28.56));
#59245=CARTESIAN_POINT('',(-28.152,23.04,26.06));
#59246=CARTESIAN_POINT('Origin',(-28.152,23.04,25.46));
#59247=CARTESIAN_POINT('',(-30.652,23.04,28.56));
#59248=CARTESIAN_POINT('Origin',(-28.152,23.04,28.56));
#59249=CARTESIAN_POINT('Origin',(-28.152,23.04,28.56));
#59250=CARTESIAN_POINT('Origin',(0.,22.44,1.224));
#59251=CARTESIAN_POINT('',(-14.472,22.44,12.8074718625761));
#59252=CARTESIAN_POINT('',(-8.1888,22.44,6.52427186257614));
#59253=CARTESIAN_POINT('',(-7.87026406871193,22.44,6.20573593128807));
#59254=CARTESIAN_POINT('',(-14.472,22.44,32.448));
#59255=CARTESIAN_POINT('',(-14.472,22.44,17.136));
#59256=CARTESIAN_POINT('',(-17.328,22.44,32.448));
#59257=CARTESIAN_POINT('',(-8.364,22.44,32.448));
#59258=CARTESIAN_POINT('',(-17.328,22.44,39.768));
#59259=CARTESIAN_POINT('',(-17.328,22.44,20.196));
#59260=CARTESIAN_POINT('',(-14.472,22.44,39.768));
#59261=CARTESIAN_POINT('',(-6.936,22.44,39.768));
#59262=CARTESIAN_POINT('',(-14.472,22.44,47.952));
#59263=CARTESIAN_POINT('',(-14.472,22.44,24.888));
#59264=CARTESIAN_POINT('',(-32.3914718625761,22.44,47.952));
#59265=CARTESIAN_POINT('',(-16.32,22.44,47.952));
#59266=CARTESIAN_POINT('',(-35.712,22.44,44.6314718625761));
#59267=CARTESIAN_POINT('',(-37.7237359312881,22.44,42.619735931288));
#59268=CARTESIAN_POINT('',(-35.712,22.44,-42.2038804065906));
#59269=CARTESIAN_POINT('',(-35.712,22.44,-20.604));
#59270=CARTESIAN_POINT('',(-32.7785603614138,22.44,-45.504));
#59271=CARTESIAN_POINT('',(-37.0566026846519,22.44,-40.6912023863572));
#59272=CARTESIAN_POINT('',(32.7785603614138,22.44,-45.504));
#59273=CARTESIAN_POINT('',(16.524,22.44,-45.504));
#59274=CARTESIAN_POINT('',(35.712,22.44,-42.2038804065906));
#59275=CARTESIAN_POINT('',(38.6886026846519,22.44,-38.8552023863572));
#59276=CARTESIAN_POINT('',(35.712,22.44,44.6314718625761));
#59277=CARTESIAN_POINT('',(35.712,22.44,23.052));
#59278=CARTESIAN_POINT('',(32.3914718625761,22.44,47.952));
#59279=CARTESIAN_POINT('',(35.8877359312881,22.44,44.455735931288));
#59280=CARTESIAN_POINT('',(14.472,22.44,47.952));
#59281=CARTESIAN_POINT('',(6.936,22.44,47.952));
#59282=CARTESIAN_POINT('',(14.472,22.44,39.768));
#59283=CARTESIAN_POINT('',(14.472,22.44,20.196));
#59284=CARTESIAN_POINT('',(17.328,22.44,39.768));
#59285=CARTESIAN_POINT('',(8.364,22.44,39.768));
#59286=CARTESIAN_POINT('',(17.328,22.44,32.448));
#59287=CARTESIAN_POINT('',(17.328,22.44,17.136));
#59288=CARTESIAN_POINT('',(14.472,22.44,32.448));
#59289=CARTESIAN_POINT('',(6.936,22.44,32.448));
#59290=CARTESIAN_POINT('',(14.472,22.44,12.8074718625761));
#59291=CARTESIAN_POINT('',(14.472,22.44,7.14));
#59292=CARTESIAN_POINT('',(8.1888,22.44,6.52427186257615));
#59293=CARTESIAN_POINT('',(4.72866406871193,22.44,3.06413593128807));
#59294=CARTESIAN_POINT('',(8.1888,22.44,-21.7872));
#59295=CARTESIAN_POINT('',(8.1888,22.44,-10.2816));
#59296=CARTESIAN_POINT('',(-8.1888,22.44,-21.7872));
#59297=CARTESIAN_POINT('Origin',(0.,22.44,-21.7872));
#59298=CARTESIAN_POINT('',(-8.1888,22.44,3.9984));
#59299=CARTESIAN_POINT('',(29.376,22.44,34.08));
#59300=CARTESIAN_POINT('Origin',(29.376,22.44,38.352));
#59301=CARTESIAN_POINT('',(3.456,22.44,-37.944));
#59302=CARTESIAN_POINT('',(3.456,22.44,-35.496));
#59303=CARTESIAN_POINT('',(3.456,22.44,-17.136));
#59304=CARTESIAN_POINT('',(-3.456,22.44,-37.944));
#59305=CARTESIAN_POINT('Origin',(0.,22.44,-37.944));
#59306=CARTESIAN_POINT('',(-3.456,22.44,-35.496));
#59307=CARTESIAN_POINT('',(-3.456,22.44,-18.36));
#59308=CARTESIAN_POINT('Origin',(0.,22.44,-35.496));
#59309=CARTESIAN_POINT('',(29.16,22.44,-32.9381572150504));
#59310=CARTESIAN_POINT('',(29.16,22.44,5.1));
#59311=CARTESIAN_POINT('',(26.4101572150504,22.44,-35.688));
#59312=CARTESIAN_POINT('Origin',(28.56,22.44,-35.088));
#59313=CARTESIAN_POINT('',(20.1018427849496,22.44,-35.688));
#59314=CARTESIAN_POINT('',(14.28,22.44,-35.688));
#59315=CARTESIAN_POINT('',(17.352,22.44,-32.9381572150504));
#59316=CARTESIAN_POINT('Origin',(17.952,22.44,-35.088));
#59317=CARTESIAN_POINT('',(17.352,22.44,6.82615721505036));
#59318=CARTESIAN_POINT('',(17.352,22.44,-16.932));
#59319=CARTESIAN_POINT('',(20.1018427849496,22.44,9.576));
#59320=CARTESIAN_POINT('Origin',(17.952,22.44,8.976));
#59321=CARTESIAN_POINT('',(8.976,22.44,9.576));
#59322=CARTESIAN_POINT('Origin',(28.56,22.44,8.976));
#59323=CARTESIAN_POINT('',(28.152,22.44,25.46));
#59324=CARTESIAN_POINT('Origin',(28.152,22.44,28.56));
#59325=CARTESIAN_POINT('',(-26.4101572150504,22.44,9.576));
#59326=CARTESIAN_POINT('',(-29.16,22.44,6.82615721505037));
#59327=CARTESIAN_POINT('Origin',(-28.56,22.44,8.976));
#59328=CARTESIAN_POINT('',(-20.1018427849496,22.44,9.576));
#59329=CARTESIAN_POINT('',(-14.28,22.44,9.576));
#59330=CARTESIAN_POINT('Origin',(-17.952,22.44,8.976));
#59331=CARTESIAN_POINT('',(-17.352,22.44,5.1));
#59332=CARTESIAN_POINT('Origin',(-17.952,22.44,-35.088));
#59333=CARTESIAN_POINT('',(-8.976,22.44,-35.688));
#59334=CARTESIAN_POINT('',(-29.16,22.44,-32.9381572150504));
#59335=CARTESIAN_POINT('Origin',(-28.56,22.44,-35.088));
#59336=CARTESIAN_POINT('',(-29.16,22.44,-16.932));
#59337=CARTESIAN_POINT('',(-29.376,22.44,34.08));
#59338=CARTESIAN_POINT('Origin',(-29.376,22.44,38.352));
#59339=CARTESIAN_POINT('Origin',(-28.152,22.44,28.56));
#59340=CARTESIAN_POINT('',(-30.652,25.104,28.56));
#59341=CARTESIAN_POINT('',(-30.652,22.44,28.56));
#59342=CARTESIAN_POINT('',(-28.152,25.104,31.06));
#59343=CARTESIAN_POINT('Origin',(-28.152,25.104,28.56));
#59344=CARTESIAN_POINT('Origin',(-28.152,25.104,28.56));
#59345=CARTESIAN_POINT('Origin',(29.376,23.04,38.352));
#59346=CARTESIAN_POINT('',(29.376,23.04,34.68));
#59347=CARTESIAN_POINT('Origin',(29.376,23.04,34.08));
#59348=CARTESIAN_POINT('',(25.704,23.04,38.352));
#59349=CARTESIAN_POINT('Origin',(29.376,23.04,38.352));
#59350=CARTESIAN_POINT('Origin',(29.376,23.04,38.352));
#59351=CARTESIAN_POINT('Origin',(29.376,22.44,38.352));
#59352=CARTESIAN_POINT('',(25.704,24.6394718625761,38.352));
#59353=CARTESIAN_POINT('',(25.704,22.44,38.352));
#59354=CARTESIAN_POINT('',(29.376,24.6394718625761,42.024));
#59355=CARTESIAN_POINT('Origin',(29.376,24.6394718625761,38.352));
#59356=CARTESIAN_POINT('Origin',(29.376,24.6394718625761,38.352));
#59357=CARTESIAN_POINT('Origin',(-29.376,23.04,38.352));
#59358=CARTESIAN_POINT('Origin',(-29.376,23.04,34.08));
#59359=CARTESIAN_POINT('Origin',(3.456,23.04,-17.136));
#59360=CARTESIAN_POINT('',(2.856,23.04,-35.496));
#59361=CARTESIAN_POINT('Origin',(3.456,23.04,-35.496));
#59362=CARTESIAN_POINT('',(2.856,23.04,-37.944));
#59363=CARTESIAN_POINT('',(2.856,23.04,-17.136));
#59364=CARTESIAN_POINT('Origin',(3.456,23.04,-37.944));
#59365=CARTESIAN_POINT('Origin',(0.,23.04,-37.944));
#59366=CARTESIAN_POINT('',(-2.856,23.04,-37.944));
#59367=CARTESIAN_POINT('Origin',(-3.456,23.04,-37.944));
#59368=CARTESIAN_POINT('Origin',(0.,23.04,-37.944));
#59369=CARTESIAN_POINT('Origin',(-3.456,23.04,-18.36));
#59370=CARTESIAN_POINT('',(-2.856,23.04,-35.496));
#59371=CARTESIAN_POINT('Origin',(-3.456,23.04,-35.496));
#59372=CARTESIAN_POINT('',(-2.856,23.04,-18.36));
#59373=CARTESIAN_POINT('Origin',(0.,23.04,-35.496));
#59374=CARTESIAN_POINT('Origin',(0.,23.04,-35.496));
#59375=CARTESIAN_POINT('Origin',(0.,22.44,-37.944));
#59376=CARTESIAN_POINT('',(2.856,25.104,-37.944));
#59377=CARTESIAN_POINT('',(2.856,22.44,-37.944));
#59378=CARTESIAN_POINT('',(-2.856,25.104,-37.944));
#59379=CARTESIAN_POINT('Origin',(0.,25.104,-37.944));
#59380=CARTESIAN_POINT('',(-2.856,22.44,-37.944));
#59381=CARTESIAN_POINT('Origin',(2.856,22.44,-35.496));
#59382=CARTESIAN_POINT('',(2.856,25.104,-35.496));
#59383=CARTESIAN_POINT('',(2.856,22.44,-35.496));
#59384=CARTESIAN_POINT('',(2.856,25.104,-17.136));
#59385=CARTESIAN_POINT('Origin',(29.16,23.04,5.1));
#59386=CARTESIAN_POINT('',(28.56,23.04,-32.9381572150504));
#59387=CARTESIAN_POINT('',(28.56,23.04,5.1));
#59388=CARTESIAN_POINT('Origin',(29.16,23.04,-32.9381572150504));
#59389=CARTESIAN_POINT('Origin',(28.56,23.04,8.976));
#59390=CARTESIAN_POINT('Origin',(20.1018427849496,23.04,9.576));
#59391=CARTESIAN_POINT('Origin',(20.1018427849496,23.04,9.576));
#59392=CARTESIAN_POINT('',(19.5239280578126,23.04,9.41470967741935));
#59393=CARTESIAN_POINT('Origin',(20.1018427849496,23.04,9.576));
#59394=CARTESIAN_POINT('Origin',(20.1018427849496,23.04,9.576));
#59395=CARTESIAN_POINT('Origin',(8.976,23.04,9.576));
#59396=CARTESIAN_POINT('Origin',(29.16,23.04,-32.9381572150504));
#59397=CARTESIAN_POINT('',(28.9987096774193,23.04,-33.5160719421874));
#59398=CARTESIAN_POINT('Origin',(29.16,23.04,-32.9381572150504));
#59399=CARTESIAN_POINT('Origin',(29.16,23.04,-32.9381572150504));
#59400=CARTESIAN_POINT('Origin',(28.56,22.44,8.976));
#59401=CARTESIAN_POINT('',(28.56,22.44,-32.9381572150504));
#59402=CARTESIAN_POINT('Origin',(20.1018427849496,22.44,9.576));
#59403=CARTESIAN_POINT('',(19.5239280578126,25.104,9.41470967741935));
#59404=CARTESIAN_POINT('',(19.5239280578126,22.44,9.41470967741935));
#59405=CARTESIAN_POINT('Origin',(20.1018427849496,25.104,9.576));
#59406=CARTESIAN_POINT('Origin',(17.952,23.04,8.976));
#59407=CARTESIAN_POINT('',(17.5132903225806,23.04,7.40407194218736));
#59408=CARTESIAN_POINT('Origin',(17.352,23.04,6.82615721505037));
#59409=CARTESIAN_POINT('Origin',(17.952,23.04,8.976));
#59410=CARTESIAN_POINT('Origin',(-7.87026406871193,23.04,6.20573593128807));
#59411=CARTESIAN_POINT('',(-13.872,23.04,13.056));
#59412=CARTESIAN_POINT('Origin',(-14.472,23.04,12.8074718625761));
#59413=CARTESIAN_POINT('',(-7.76453593128807,23.04,6.94853593128807));
#59414=CARTESIAN_POINT('Origin',(-8.1888,23.04,6.52427186257614));
#59415=CARTESIAN_POINT('',(-7.446,23.04,6.63));
#59416=CARTESIAN_POINT('Origin',(-8.1888,23.04,6.52427186257615));
#59417=CARTESIAN_POINT('',(-7.5888,23.04,6.52427186257615));
#59418=CARTESIAN_POINT('Origin',(-8.1888,23.04,6.52427186257615));
#59419=CARTESIAN_POINT('Origin',(-8.1888,23.04,6.52427186257615));
#59420=CARTESIAN_POINT('Origin',(-8.1888,23.04,3.9984));
#59421=CARTESIAN_POINT('',(-7.5888,23.04,-21.7872));
#59422=CARTESIAN_POINT('Origin',(-8.1888,23.04,-21.7872));
#59423=CARTESIAN_POINT('',(-7.5888,23.04,3.9984));
#59424=CARTESIAN_POINT('Origin',(35.712,23.04,-42.2038804065906));
#59425=CARTESIAN_POINT('',(36.312,23.04,-42.2038804065906));
#59426=CARTESIAN_POINT('',(36.1604455912102,23.04,-42.6024987098885));
#59427=CARTESIAN_POINT('Origin',(35.712,23.04,-42.2038804065906));
#59428=CARTESIAN_POINT('Origin',(35.712,23.04,-42.2038804065906));
#59429=CARTESIAN_POINT('Origin',(35.712,23.04,-42.2038804065906));
#59430=CARTESIAN_POINT('Origin',(35.712,23.04,44.6314718625761));
#59431=CARTESIAN_POINT('',(36.312,23.04,44.6314718625761));
#59432=CARTESIAN_POINT('Origin',(35.712,23.04,44.6314718625761));
#59433=CARTESIAN_POINT('',(36.1362640687119,23.04,45.0557359312881));
#59434=CARTESIAN_POINT('Origin',(35.712,23.04,44.6314718625761));
#59435=CARTESIAN_POINT('Origin',(35.712,23.04,44.6314718625761));
#59436=CARTESIAN_POINT('Origin',(35.712,23.04,23.052));
#59437=CARTESIAN_POINT('',(36.312,23.04,23.052));
#59438=CARTESIAN_POINT('Origin',(32.7785603614138,23.04,-45.504));
#59439=CARTESIAN_POINT('',(33.227005952624,23.04,-45.902618303298));
#59440=CARTESIAN_POINT('',(32.7785603614138,23.04,-46.104));
#59441=CARTESIAN_POINT('Origin',(32.7785603614138,23.04,-45.504));
#59442=CARTESIAN_POINT('Origin',(32.7785603614138,23.04,-45.504));
#59443=CARTESIAN_POINT('Origin',(32.7785603614138,23.04,-45.504));
#59444=CARTESIAN_POINT('Origin',(38.6886026846519,23.04,-38.8552023863572));
#59445=CARTESIAN_POINT('',(39.1370482758621,23.04,-39.2538206896552));
#59446=CARTESIAN_POINT('Origin',(-32.7785603614138,23.04,-45.504));
#59447=CARTESIAN_POINT('',(-32.7785603614138,23.04,-46.104));
#59448=CARTESIAN_POINT('',(-33.227005952624,23.04,-45.902618303298));
#59449=CARTESIAN_POINT('Origin',(-32.7785603614138,23.04,-45.504));
#59450=CARTESIAN_POINT('Origin',(-32.7785603614138,23.04,-45.504));
#59451=CARTESIAN_POINT('Origin',(-32.7785603614138,23.04,-45.504));
#59452=CARTESIAN_POINT('Origin',(16.524,23.04,-45.504));
#59453=CARTESIAN_POINT('',(16.524,23.04,-46.104));
#59454=CARTESIAN_POINT('Origin',(-37.0566026846519,23.04,-40.6912023863572));
#59455=CARTESIAN_POINT('',(-36.1604455912102,23.04,-42.6024987098885));
#59456=CARTESIAN_POINT('Origin',(-35.712,23.04,-42.2038804065906));
#59457=CARTESIAN_POINT('',(-37.5050482758621,23.04,-41.0898206896552));
#59458=CARTESIAN_POINT('Origin',(-35.712,23.04,-42.2038804065906));
#59459=CARTESIAN_POINT('',(-36.312,23.04,-42.2038804065906));
#59460=CARTESIAN_POINT('Origin',(-35.712,23.04,-42.2038804065906));
#59461=CARTESIAN_POINT('Origin',(-35.712,23.04,-42.2038804065906));
#59462=CARTESIAN_POINT('Origin',(-32.7785603614138,22.44,-45.504));
#59463=CARTESIAN_POINT('',(-33.227005952624,25.104,-45.902618303298));
#59464=CARTESIAN_POINT('',(-32.7785603614138,25.104,-46.104));
#59465=CARTESIAN_POINT('Origin',(-32.7785603614138,25.104,-45.504));
#59466=CARTESIAN_POINT('',(-32.7785603614138,22.44,-46.104));
#59467=CARTESIAN_POINT('',(-33.227005952624,22.44,-45.902618303298));
#59468=CARTESIAN_POINT('Origin',(-32.7785603614138,25.104,-45.504));
#59469=CARTESIAN_POINT('',(-32.7785603614138,25.704,-45.504));
#59470=CARTESIAN_POINT('Origin',(-32.7785603614138,25.104,-45.504));
#59471=CARTESIAN_POINT('Origin',(-32.7785603614138,25.104,-45.504));
#59472=CARTESIAN_POINT('Origin',(32.7785603614138,22.44,-45.504));
#59473=CARTESIAN_POINT('',(32.7785603614138,25.104,-46.104));
#59474=CARTESIAN_POINT('',(33.227005952624,25.104,-45.902618303298));
#59475=CARTESIAN_POINT('Origin',(32.7785603614138,25.104,-45.504));
#59476=CARTESIAN_POINT('',(33.227005952624,22.44,-45.902618303298));
#59477=CARTESIAN_POINT('',(32.7785603614138,22.44,-46.104));
#59478=CARTESIAN_POINT('Origin',(32.7785603614138,25.104,-45.504));
#59479=CARTESIAN_POINT('',(32.7785603614138,25.704,-45.504));
#59480=CARTESIAN_POINT('Origin',(32.7785603614138,25.104,-45.504));
#59481=CARTESIAN_POINT('Origin',(32.7785603614138,25.104,-45.504));
#59482=CARTESIAN_POINT('Origin',(35.712,22.44,-42.2038804065906));
#59483=CARTESIAN_POINT('',(36.1604455912102,25.104,-42.6024987098885));
#59484=CARTESIAN_POINT('',(36.312,25.104,-42.2038804065906));
#59485=CARTESIAN_POINT('Origin',(35.712,25.104,-42.2038804065906));
#59486=CARTESIAN_POINT('',(36.312,22.44,-42.2038804065906));
#59487=CARTESIAN_POINT('',(36.1604455912102,22.44,-42.6024987098885));
#59488=CARTESIAN_POINT('Origin',(35.712,25.104,-42.2038804065906));
#59489=CARTESIAN_POINT('',(35.712,25.704,-42.2038804065906));
#59490=CARTESIAN_POINT('Origin',(35.712,25.104,-42.2038804065906));
#59491=CARTESIAN_POINT('Origin',(35.712,25.104,-42.2038804065906));
#59492=CARTESIAN_POINT('Origin',(36.312,22.44,-42.432));
#59493=CARTESIAN_POINT('',(39.1370482758621,25.104,-39.2538206896552));
#59494=CARTESIAN_POINT('Origin',(33.048,22.44,-46.104));
#59495=CARTESIAN_POINT('',(16.524,25.104,-46.104));
#59496=CARTESIAN_POINT('Origin',(16.524,25.104,-45.504));
#59497=CARTESIAN_POINT('',(16.524,25.704,-45.504));
#59498=CARTESIAN_POINT('Origin',(-37.0566026846519,25.104,-40.6912023863572));
#59499=CARTESIAN_POINT('',(-36.1604455912102,25.104,-42.6024987098885));
#59500=CARTESIAN_POINT('',(-37.5050482758621,25.104,-41.0898206896552));
#59501=CARTESIAN_POINT('',(-35.712,25.704,-42.2038804065906));
#59502=CARTESIAN_POINT('Origin',(-35.712,25.104,-42.2038804065906));
#59503=CARTESIAN_POINT('',(-37.0566026846519,25.704,-40.6912023863572));
#59504=CARTESIAN_POINT('Origin',(-33.048,22.44,-46.104));
#59505=CARTESIAN_POINT('',(-36.1604455912102,22.44,-42.6024987098885));
#59506=CARTESIAN_POINT('Origin',(-29.16,23.04,6.82615721505037));
#59507=CARTESIAN_POINT('',(-28.56,23.04,6.82615721505037));
#59508=CARTESIAN_POINT('Origin',(-29.16,23.04,6.82615721505037));
#59509=CARTESIAN_POINT('',(-28.9987096774194,23.04,7.40407194218737));
#59510=CARTESIAN_POINT('Origin',(-29.16,23.04,6.82615721505037));
#59511=CARTESIAN_POINT('Origin',(-29.16,23.04,6.82615721505037));
#59512=CARTESIAN_POINT('Origin',(-29.16,25.104,6.82615721505037));
#59513=CARTESIAN_POINT('',(-28.9987096774194,25.104,7.40407194218737));
#59514=CARTESIAN_POINT('',(-28.56,25.104,6.82615721505037));
#59515=CARTESIAN_POINT('Origin',(-29.16,25.104,6.82615721505037));
#59516=CARTESIAN_POINT('',(-29.16,25.704,6.82615721505037));
#59517=CARTESIAN_POINT('Origin',(-29.16,25.104,6.82615721505037));
#59518=CARTESIAN_POINT('Origin',(-29.16,25.104,6.82615721505037));
#59519=CARTESIAN_POINT('Origin',(-29.16,22.44,6.82615721505037));
#59520=CARTESIAN_POINT('',(-28.9987096774194,22.44,7.40407194218737));
#59521=CARTESIAN_POINT('',(-28.56,22.44,6.82615721505037));
#59522=CARTESIAN_POINT('Origin',(-28.56,23.04,8.976));
#59523=CARTESIAN_POINT('',(-26.9880719421874,23.04,9.41470967741935));
#59524=CARTESIAN_POINT('Origin',(-26.4101572150504,23.04,9.576));
#59525=CARTESIAN_POINT('Origin',(-28.56,23.04,8.976));
#59526=CARTESIAN_POINT('Origin',(-26.4101572150504,23.04,9.576));
#59527=CARTESIAN_POINT('',(-26.4101572150504,23.04,8.976));
#59528=CARTESIAN_POINT('Origin',(-26.4101572150504,23.04,9.576));
#59529=CARTESIAN_POINT('Origin',(-26.4101572150504,23.04,9.576));
#59530=CARTESIAN_POINT('Origin',(-29.16,23.04,-16.932));
#59531=CARTESIAN_POINT('',(-28.56,23.04,-32.9381572150504));
#59532=CARTESIAN_POINT('Origin',(-29.16,23.04,-32.9381572150504));
#59533=CARTESIAN_POINT('',(-28.56,23.04,-16.932));
#59534=CARTESIAN_POINT('Origin',(-28.56,23.04,-35.088));
#59535=CARTESIAN_POINT('',(-28.9987096774194,23.04,-33.5160719421874));
#59536=CARTESIAN_POINT('Origin',(-28.56,23.04,-35.088));
#59537=CARTESIAN_POINT('Origin',(-29.16,23.04,-32.9381572150504));
#59538=CARTESIAN_POINT('Origin',(-8.976,23.04,-35.688));
#59539=CARTESIAN_POINT('Origin',(-17.952,23.04,-35.088));
#59540=CARTESIAN_POINT('Origin',(-17.352,23.04,5.1));
#59541=CARTESIAN_POINT('Origin',(-20.1018427849496,23.04,9.576));
#59542=CARTESIAN_POINT('Origin',(-20.1018427849496,23.04,9.576));
#59543=CARTESIAN_POINT('',(-20.1018427849496,23.04,8.976));
#59544=CARTESIAN_POINT('Origin',(-20.1018427849496,23.04,9.576));
#59545=CARTESIAN_POINT('Origin',(-20.1018427849496,23.04,9.576));
#59546=CARTESIAN_POINT('Origin',(-17.952,23.04,8.976));
#59547=CARTESIAN_POINT('Origin',(-29.16,23.04,-32.9381572150504));
#59548=CARTESIAN_POINT('Origin',(-29.16,23.04,-32.9381572150504));
#59549=CARTESIAN_POINT('Origin',(-28.56,25.104,8.976));
#59550=CARTESIAN_POINT('',(-26.4101572150504,25.704,9.576));
#59551=CARTESIAN_POINT('Origin',(-28.56,25.704,8.976));
#59552=CARTESIAN_POINT('',(-26.9880719421874,25.104,9.41470967741935));
#59553=CARTESIAN_POINT('Origin',(-26.4101572150504,25.104,9.576));
#59554=CARTESIAN_POINT('Origin',(-28.56,25.104,8.976));
#59555=CARTESIAN_POINT('Origin',(-29.16,25.104,-16.932));
#59556=CARTESIAN_POINT('',(-28.56,25.104,-32.9381572150504));
#59557=CARTESIAN_POINT('',(-28.56,25.104,-16.932));
#59558=CARTESIAN_POINT('Origin',(-29.16,25.104,-32.9381572150504));
#59559=CARTESIAN_POINT('',(-29.16,25.704,-16.932));
#59560=CARTESIAN_POINT('Origin',(-28.56,22.44,-35.088));
#59561=CARTESIAN_POINT('',(-28.56,22.44,-32.9381572150504));
#59562=CARTESIAN_POINT('Origin',(-29.16,22.44,-32.9381572150504));
#59563=CARTESIAN_POINT('',(-28.9987096774194,22.44,-33.5160719421874));
#59564=CARTESIAN_POINT('Origin',(-29.16,25.104,-32.9381572150504));
#59565=CARTESIAN_POINT('Origin',(-28.56,22.44,-35.088));
#59566=CARTESIAN_POINT('Origin',(-20.1018427849496,22.44,9.576));
#59567=CARTESIAN_POINT('',(-20.1018427849496,25.104,8.976));
#59568=CARTESIAN_POINT('',(-20.1018427849496,22.44,8.976));
#59569=CARTESIAN_POINT('Origin',(-20.1018427849496,25.104,9.576));
#59570=CARTESIAN_POINT('Origin',(28.152,23.04,28.56));
#59571=CARTESIAN_POINT('',(28.152,23.04,26.06));
#59572=CARTESIAN_POINT('Origin',(28.152,23.04,25.46));
#59573=CARTESIAN_POINT('',(25.652,23.04,28.56));
#59574=CARTESIAN_POINT('Origin',(28.152,23.04,28.56));
#59575=CARTESIAN_POINT('Origin',(28.152,23.04,28.56));
#59576=CARTESIAN_POINT('Origin',(28.152,22.44,28.56));
#59577=CARTESIAN_POINT('',(25.652,25.104,28.56));
#59578=CARTESIAN_POINT('',(25.652,22.44,28.56));
#59579=CARTESIAN_POINT('',(28.152,25.104,31.06));
#59580=CARTESIAN_POINT('Origin',(28.152,25.104,28.56));
#59581=CARTESIAN_POINT('Origin',(28.152,25.104,28.56));
#59582=CARTESIAN_POINT('Origin',(-35.712,23.04,44.6314718625761));
#59583=CARTESIAN_POINT('',(-36.312,23.04,44.6314718625761));
#59584=CARTESIAN_POINT('',(-36.1362640687119,23.04,45.0557359312881));
#59585=CARTESIAN_POINT('Origin',(-35.712,23.04,44.6314718625761));
#59586=CARTESIAN_POINT('Origin',(-35.712,23.04,44.6314718625761));
#59587=CARTESIAN_POINT('Origin',(-35.712,23.04,44.6314718625761));
#59588=CARTESIAN_POINT('Origin',(-35.712,23.04,-20.604));
#59589=CARTESIAN_POINT('',(-36.312,23.04,-20.604));
#59590=CARTESIAN_POINT('Origin',(-32.3914718625761,23.04,47.952));
#59591=CARTESIAN_POINT('',(-32.8157359312881,23.04,48.3762640687119));
#59592=CARTESIAN_POINT('',(-32.3914718625761,23.04,48.552));
#59593=CARTESIAN_POINT('Origin',(-32.3914718625761,23.04,47.952));
#59594=CARTESIAN_POINT('Origin',(-32.3914718625761,23.04,47.952));
#59595=CARTESIAN_POINT('Origin',(-32.3914718625761,23.04,47.952));
#59596=CARTESIAN_POINT('Origin',(-37.7237359312881,23.04,42.619735931288));
#59597=CARTESIAN_POINT('',(-38.148,23.04,43.044));
#59598=CARTESIAN_POINT('Origin',(-14.472,23.04,47.952));
#59599=CARTESIAN_POINT('',(-14.472,23.04,48.552));
#59600=CARTESIAN_POINT('',(-13.872,23.04,47.952));
#59601=CARTESIAN_POINT('Origin',(-14.472,23.04,47.952));
#59602=CARTESIAN_POINT('Origin',(-14.472,23.04,47.952));
#59603=CARTESIAN_POINT('Origin',(-14.472,23.04,47.952));
#59604=CARTESIAN_POINT('Origin',(-16.32,23.04,47.952));
#59605=CARTESIAN_POINT('',(-16.32,23.04,48.552));
#59606=CARTESIAN_POINT('Origin',(-14.472,23.04,39.768));
#59607=CARTESIAN_POINT('',(-13.872,23.04,39.768));
#59608=CARTESIAN_POINT('',(-14.472,23.04,39.168));
#59609=CARTESIAN_POINT('Origin',(-14.472,23.04,39.768));
#59610=CARTESIAN_POINT('Origin',(-14.472,23.04,39.768));
#59611=CARTESIAN_POINT('Origin',(-14.472,23.04,39.768));
#59612=CARTESIAN_POINT('Origin',(-14.472,23.04,24.888));
#59613=CARTESIAN_POINT('',(-13.872,23.04,24.888));
#59614=CARTESIAN_POINT('Origin',(-6.936,23.04,39.768));
#59615=CARTESIAN_POINT('',(-16.728,23.04,39.168));
#59616=CARTESIAN_POINT('',(-6.936,23.04,39.168));
#59617=CARTESIAN_POINT('Origin',(-17.328,23.04,39.768));
#59618=CARTESIAN_POINT('Origin',(-17.328,23.04,20.196));
#59619=CARTESIAN_POINT('',(-16.728,23.04,33.048));
#59620=CARTESIAN_POINT('Origin',(-17.328,23.04,32.448));
#59621=CARTESIAN_POINT('',(-16.728,23.04,20.196));
#59622=CARTESIAN_POINT('Origin',(-14.472,23.04,32.448));
#59623=CARTESIAN_POINT('',(-14.472,23.04,33.048));
#59624=CARTESIAN_POINT('',(-13.872,23.04,32.448));
#59625=CARTESIAN_POINT('Origin',(-14.472,23.04,32.448));
#59626=CARTESIAN_POINT('Origin',(-14.472,23.04,32.448));
#59627=CARTESIAN_POINT('Origin',(-14.472,23.04,32.448));
#59628=CARTESIAN_POINT('Origin',(-8.364,23.04,32.448));
#59629=CARTESIAN_POINT('',(-8.364,23.04,33.048));
#59630=CARTESIAN_POINT('Origin',(-14.472,23.04,17.136));
#59631=CARTESIAN_POINT('',(-13.872,23.04,17.136));
#59632=CARTESIAN_POINT('Origin',(-14.472,22.44,32.448));
#59633=CARTESIAN_POINT('',(-13.872,25.104,32.448));
#59634=CARTESIAN_POINT('',(-14.472,25.104,33.048));
#59635=CARTESIAN_POINT('Origin',(-14.472,25.104,32.448));
#59636=CARTESIAN_POINT('',(-14.472,22.44,33.048));
#59637=CARTESIAN_POINT('',(-13.872,22.44,32.448));
#59638=CARTESIAN_POINT('Origin',(-14.472,25.104,32.448));
#59639=CARTESIAN_POINT('',(-14.472,25.704,32.448));
#59640=CARTESIAN_POINT('Origin',(-14.472,25.104,32.448));
#59641=CARTESIAN_POINT('Origin',(-14.472,25.104,32.448));
#59642=CARTESIAN_POINT('Origin',(-14.472,22.44,39.768));
#59643=CARTESIAN_POINT('',(-14.472,25.104,39.168));
#59644=CARTESIAN_POINT('',(-13.872,25.104,39.768));
#59645=CARTESIAN_POINT('Origin',(-14.472,25.104,39.768));
#59646=CARTESIAN_POINT('',(-13.872,22.44,39.768));
#59647=CARTESIAN_POINT('',(-14.472,22.44,39.168));
#59648=CARTESIAN_POINT('Origin',(-14.472,25.104,39.768));
#59649=CARTESIAN_POINT('',(-14.472,25.704,39.768));
#59650=CARTESIAN_POINT('Origin',(-14.472,25.104,39.768));
#59651=CARTESIAN_POINT('Origin',(-14.472,25.104,39.768));
#59652=CARTESIAN_POINT('Origin',(-14.472,22.44,47.952));
#59653=CARTESIAN_POINT('',(-13.872,25.104,47.952));
#59654=CARTESIAN_POINT('',(-14.472,25.104,48.552));
#59655=CARTESIAN_POINT('Origin',(-14.472,25.104,47.952));
#59656=CARTESIAN_POINT('',(-14.472,22.44,48.552));
#59657=CARTESIAN_POINT('',(-13.872,22.44,47.952));
#59658=CARTESIAN_POINT('Origin',(-14.472,25.104,47.952));
#59659=CARTESIAN_POINT('',(-14.472,25.704,47.952));
#59660=CARTESIAN_POINT('Origin',(-14.472,25.104,47.952));
#59661=CARTESIAN_POINT('Origin',(-14.472,25.104,47.952));
#59662=CARTESIAN_POINT('Origin',(-32.3914718625761,22.44,47.952));
#59663=CARTESIAN_POINT('',(-32.3914718625761,25.104,48.552));
#59664=CARTESIAN_POINT('',(-32.8157359312881,25.104,48.3762640687119));
#59665=CARTESIAN_POINT('Origin',(-32.3914718625761,25.104,47.952));
#59666=CARTESIAN_POINT('',(-32.8157359312881,22.44,48.3762640687119));
#59667=CARTESIAN_POINT('',(-32.3914718625761,22.44,48.552));
#59668=CARTESIAN_POINT('Origin',(-32.3914718625761,25.104,47.952));
#59669=CARTESIAN_POINT('',(-32.3914718625761,25.704,47.952));
#59670=CARTESIAN_POINT('Origin',(-32.3914718625761,25.104,47.952));
#59671=CARTESIAN_POINT('Origin',(-32.3914718625761,25.104,47.952));
#59672=CARTESIAN_POINT('Origin',(-35.712,22.44,44.6314718625761));
#59673=CARTESIAN_POINT('',(-36.1362640687119,25.104,45.0557359312881));
#59674=CARTESIAN_POINT('',(-36.312,25.104,44.6314718625761));
#59675=CARTESIAN_POINT('Origin',(-35.712,25.104,44.6314718625761));
#59676=CARTESIAN_POINT('',(-36.312,22.44,44.6314718625761));
#59677=CARTESIAN_POINT('',(-36.1362640687119,22.44,45.0557359312881));
#59678=CARTESIAN_POINT('Origin',(-35.712,25.104,44.6314718625761));
#59679=CARTESIAN_POINT('',(-35.712,25.704,44.6314718625761));
#59680=CARTESIAN_POINT('Origin',(-35.712,25.104,44.6314718625761));
#59681=CARTESIAN_POINT('Origin',(-35.712,25.104,44.6314718625761));
#59682=CARTESIAN_POINT('Origin',(-35.712,22.44,-42.2038804065906));
#59683=CARTESIAN_POINT('',(-36.312,25.104,-42.2038804065906));
#59684=CARTESIAN_POINT('',(-36.312,22.44,-42.2038804065906));
#59685=CARTESIAN_POINT('Origin',(-35.712,25.104,-42.2038804065906));
#59686=CARTESIAN_POINT('Origin',(-35.712,25.104,-42.2038804065906));
#59687=CARTESIAN_POINT('Origin',(-35.712,25.104,-42.2038804065906));
#59688=CARTESIAN_POINT('Origin',(-32.64,22.44,48.552));
#59689=CARTESIAN_POINT('',(-16.32,25.104,48.552));
#59690=CARTESIAN_POINT('Origin',(-37.7237359312881,25.104,42.619735931288));
#59691=CARTESIAN_POINT('',(-37.7237359312881,25.704,42.619735931288));
#59692=CARTESIAN_POINT('',(-38.148,25.104,43.044));
#59693=CARTESIAN_POINT('Origin',(-16.32,25.104,47.952));
#59694=CARTESIAN_POINT('',(-16.32,25.704,47.952));
#59695=CARTESIAN_POINT('Origin',(-13.872,22.44,48.552));
#59696=CARTESIAN_POINT('',(-13.872,25.104,24.888));
#59697=CARTESIAN_POINT('Origin',(-14.472,25.104,24.888));
#59698=CARTESIAN_POINT('',(-14.472,25.704,24.888));
#59699=CARTESIAN_POINT('Origin',(-6.936,25.104,39.768));
#59700=CARTESIAN_POINT('',(-16.728,25.104,39.168));
#59701=CARTESIAN_POINT('',(-6.936,25.104,39.168));
#59702=CARTESIAN_POINT('',(-17.328,25.704,39.768));
#59703=CARTESIAN_POINT('Origin',(-17.328,25.104,39.768));
#59704=CARTESIAN_POINT('',(-6.936,25.704,39.768));
#59705=CARTESIAN_POINT('Origin',(-13.872,22.44,39.168));
#59706=CARTESIAN_POINT('',(-16.728,22.44,39.168));
#59707=CARTESIAN_POINT('Origin',(-16.728,22.44,39.168));
#59708=CARTESIAN_POINT('',(-16.728,25.104,33.048));
#59709=CARTESIAN_POINT('',(-16.728,22.44,33.048));
#59710=CARTESIAN_POINT('',(-16.728,25.104,20.196));
#59711=CARTESIAN_POINT('Origin',(-16.728,22.44,33.048));
#59712=CARTESIAN_POINT('',(-8.364,25.104,33.048));
#59713=CARTESIAN_POINT('Origin',(-8.364,25.104,32.448));
#59714=CARTESIAN_POINT('',(-17.328,25.704,32.448));
#59715=CARTESIAN_POINT('',(-8.364,25.704,32.448));
#59716=CARTESIAN_POINT('Origin',(-17.328,25.104,32.448));
#59717=CARTESIAN_POINT('Origin',(-14.472,25.104,17.136));
#59718=CARTESIAN_POINT('',(-13.872,25.104,13.056));
#59719=CARTESIAN_POINT('',(-13.872,25.104,17.136));
#59720=CARTESIAN_POINT('',(-14.472,25.704,12.8074718625761));
#59721=CARTESIAN_POINT('Origin',(-14.472,25.104,12.8074718625761));
#59722=CARTESIAN_POINT('',(-14.472,25.704,17.136));
#59723=CARTESIAN_POINT('Origin',(-13.872,22.44,33.048));
#59724=CARTESIAN_POINT('',(-13.872,22.44,13.056));
#59725=CARTESIAN_POINT('Origin',(28.152,25.104,28.56));
#59726=CARTESIAN_POINT('',(28.152,25.704,31.66));
#59727=CARTESIAN_POINT('Origin',(28.152,25.704,28.56));
#59728=CARTESIAN_POINT('Origin',(28.152,25.104,31.66));
#59729=CARTESIAN_POINT('Origin',(0.,25.704,1.224));
#59730=CARTESIAN_POINT('',(-8.1888,25.704,6.52427186257614));
#59731=CARTESIAN_POINT('',(-7.87026406871193,25.704,6.20573593128807));
#59732=CARTESIAN_POINT('',(-8.1888,25.704,-21.7872));
#59733=CARTESIAN_POINT('',(-8.1888,25.704,3.9984));
#59734=CARTESIAN_POINT('',(8.1888,25.704,-21.7872));
#59735=CARTESIAN_POINT('Origin',(0.,25.704,-21.7872));
#59736=CARTESIAN_POINT('',(8.1888,25.704,6.52427186257614));
#59737=CARTESIAN_POINT('',(8.1888,25.704,-10.2816));
#59738=CARTESIAN_POINT('',(14.472,25.704,12.8074718625761));
#59739=CARTESIAN_POINT('',(4.72866406871193,25.704,3.06413593128807));
#59740=CARTESIAN_POINT('',(14.472,25.704,32.448));
#59741=CARTESIAN_POINT('',(14.472,25.704,7.14));
#59742=CARTESIAN_POINT('',(17.328,25.704,32.448));
#59743=CARTESIAN_POINT('',(6.936,25.704,32.448));
#59744=CARTESIAN_POINT('',(17.328,25.704,39.768));
#59745=CARTESIAN_POINT('',(17.328,25.704,17.136));
#59746=CARTESIAN_POINT('',(14.472,25.704,39.768));
#59747=CARTESIAN_POINT('',(8.364,25.704,39.768));
#59748=CARTESIAN_POINT('',(14.472,25.704,47.952));
#59749=CARTESIAN_POINT('',(14.472,25.704,20.196));
#59750=CARTESIAN_POINT('',(32.3914718625761,25.704,47.952));
#59751=CARTESIAN_POINT('',(6.936,25.704,47.952));
#59752=CARTESIAN_POINT('',(35.712,25.704,44.6314718625761));
#59753=CARTESIAN_POINT('',(35.8877359312881,25.704,44.455735931288));
#59754=CARTESIAN_POINT('',(35.712,25.704,23.052));
#59755=CARTESIAN_POINT('',(38.6886026846519,25.704,-38.8552023863572));
#59756=CARTESIAN_POINT('',(-35.712,25.704,-20.604));
#59757=CARTESIAN_POINT('',(-17.328,25.704,20.196));
#59758=CARTESIAN_POINT('',(17.352,25.704,6.82615721505037));
#59759=CARTESIAN_POINT('Origin',(17.952,25.704,8.976));
#59760=CARTESIAN_POINT('',(17.352,25.704,-32.9381572150504));
#59761=CARTESIAN_POINT('',(17.352,25.704,-16.932));
#59762=CARTESIAN_POINT('',(20.1018427849496,25.704,-35.688));
#59763=CARTESIAN_POINT('Origin',(17.952,25.704,-35.088));
#59764=CARTESIAN_POINT('',(26.4101572150504,25.704,-35.688));
#59765=CARTESIAN_POINT('',(14.28,25.704,-35.688));
#59766=CARTESIAN_POINT('Origin',(28.56,25.704,-35.088));
#59767=CARTESIAN_POINT('',(3.456,25.704,-35.496));
#59768=CARTESIAN_POINT('',(3.456,25.704,-37.944));
#59769=CARTESIAN_POINT('',(3.456,25.704,-17.136));
#59770=CARTESIAN_POINT('',(-3.456,25.704,-35.496));
#59771=CARTESIAN_POINT('Origin',(0.,25.704,-35.496));
#59772=CARTESIAN_POINT('',(-3.456,25.704,-37.944));
#59773=CARTESIAN_POINT('',(-3.456,25.704,-18.36));
#59774=CARTESIAN_POINT('Origin',(0.,25.704,-37.944));
#59775=CARTESIAN_POINT('',(29.376,25.704,33.6154718625761));
#59776=CARTESIAN_POINT('Origin',(29.376,25.704,38.352));
#59777=CARTESIAN_POINT('',(-14.28,25.704,9.576));
#59778=CARTESIAN_POINT('',(-29.376,25.704,33.6154718625761));
#59779=CARTESIAN_POINT('Origin',(-29.376,25.704,38.352));
#59780=CARTESIAN_POINT('',(-28.152,25.704,31.66));
#59781=CARTESIAN_POINT('Origin',(-28.152,25.704,28.56));
#59782=CARTESIAN_POINT('Origin',(-20.1018427849496,25.104,9.576));
#59783=CARTESIAN_POINT('Origin',(-20.1018427849496,25.104,9.576));
#59784=CARTESIAN_POINT('Origin',(-14.28,25.104,9.576));
#59785=CARTESIAN_POINT('',(-26.4101572150504,25.104,8.976));
#59786=CARTESIAN_POINT('Origin',(-26.4101572150504,25.104,9.576));
#59787=CARTESIAN_POINT('',(-14.28,25.104,8.976));
#59788=CARTESIAN_POINT('Origin',(-14.28,23.04,9.576));
#59789=CARTESIAN_POINT('',(-14.28,23.04,8.976));
#59790=CARTESIAN_POINT('Origin',(-26.4101572150504,22.44,9.576));
#59791=CARTESIAN_POINT('',(-26.9880719421874,22.44,9.41470967741935));
#59792=CARTESIAN_POINT('Origin',(-26.4101572150504,25.104,9.576));
#59793=CARTESIAN_POINT('',(-26.4101572150504,22.44,8.976));
#59794=CARTESIAN_POINT('Origin',(-26.4101572150504,25.104,9.576));
#59795=CARTESIAN_POINT('Origin',(-29.16,25.104,-32.9381572150504));
#59796=CARTESIAN_POINT('Origin',(-28.56,22.44,8.976));
#59797=CARTESIAN_POINT('Origin',(-28.56,22.44,8.976));
#59798=CARTESIAN_POINT('Origin',(-17.328,25.104,20.196));
#59799=CARTESIAN_POINT('Origin',(-35.712,25.104,-20.604));
#59800=CARTESIAN_POINT('',(-36.312,25.104,-20.604));
#59801=CARTESIAN_POINT('Origin',(38.6886026846519,25.104,-38.8552023863572));
#59802=CARTESIAN_POINT('Origin',(35.712,25.104,44.6314718625761));
#59803=CARTESIAN_POINT('',(36.312,25.104,44.6314718625761));
#59804=CARTESIAN_POINT('Origin',(35.712,25.104,44.6314718625761));
#59805=CARTESIAN_POINT('',(36.1362640687119,25.104,45.0557359312881));
#59806=CARTESIAN_POINT('Origin',(35.712,25.104,44.6314718625761));
#59807=CARTESIAN_POINT('Origin',(35.712,25.104,44.6314718625761));
#59808=CARTESIAN_POINT('Origin',(35.712,25.104,23.052));
#59809=CARTESIAN_POINT('',(36.312,25.104,23.052));
#59810=CARTESIAN_POINT('Origin',(-36.312,22.44,44.88));
#59811=CARTESIAN_POINT('Origin',(-36.312,22.44,-42.432));
#59812=CARTESIAN_POINT('Origin',(36.312,22.44,44.88));
#59813=CARTESIAN_POINT('',(36.312,22.44,44.6314718625761));
#59814=CARTESIAN_POINT('Origin',(35.712,22.44,44.6314718625761));
#59815=CARTESIAN_POINT('',(36.1362640687119,22.44,45.0557359312881));
#59816=CARTESIAN_POINT('Origin',(17.352,23.04,6.82615721505037));
#59817=CARTESIAN_POINT('',(17.952,23.04,6.82615721505037));
#59818=CARTESIAN_POINT('Origin',(17.352,23.04,6.82615721505037));
#59819=CARTESIAN_POINT('Origin',(17.352,23.04,6.82615721505036));
#59820=CARTESIAN_POINT('Origin',(17.352,23.04,-32.9381572150504));
#59821=CARTESIAN_POINT('',(17.952,23.04,-32.9381572150504));
#59822=CARTESIAN_POINT('',(17.5132903225806,23.04,-33.5160719421874));
#59823=CARTESIAN_POINT('Origin',(17.352,23.04,-32.9381572150504));
#59824=CARTESIAN_POINT('Origin',(17.352,23.04,-32.9381572150504));
#59825=CARTESIAN_POINT('Origin',(17.352,23.04,-32.9381572150504));
#59826=CARTESIAN_POINT('Origin',(17.352,23.04,-16.932));
#59827=CARTESIAN_POINT('',(17.952,23.04,-16.932));
#59828=CARTESIAN_POINT('Origin',(20.1018427849496,23.04,-35.688));
#59829=CARTESIAN_POINT('',(19.5239280578126,23.04,-35.5267096774194));
#59830=CARTESIAN_POINT('Origin',(20.1018427849496,23.04,-35.688));
#59831=CARTESIAN_POINT('',(20.1018427849496,23.04,-35.088));
#59832=CARTESIAN_POINT('Origin',(20.1018427849496,23.04,-35.688));
#59833=CARTESIAN_POINT('Origin',(20.1018427849496,23.04,-35.688));
#59834=CARTESIAN_POINT('Origin',(17.952,23.04,-35.088));
#59835=CARTESIAN_POINT('Origin',(17.952,23.04,-35.088));
#59836=CARTESIAN_POINT('Origin',(17.352,22.44,-32.9381572150504));
#59837=CARTESIAN_POINT('',(17.5132903225806,25.104,-33.5160719421874));
#59838=CARTESIAN_POINT('',(17.952,25.104,-32.9381572150504));
#59839=CARTESIAN_POINT('Origin',(17.352,25.104,-32.9381572150504));
#59840=CARTESIAN_POINT('',(17.952,22.44,-32.9381572150504));
#59841=CARTESIAN_POINT('',(17.5132903225806,22.44,-33.5160719421874));
#59842=CARTESIAN_POINT('Origin',(17.352,25.104,-32.9381572150504));
#59843=CARTESIAN_POINT('Origin',(17.352,25.104,-32.9381572150504));
#59844=CARTESIAN_POINT('Origin',(17.352,25.104,-32.9381572150504));
#59845=CARTESIAN_POINT('Origin',(17.352,25.104,6.82615721505037));
#59846=CARTESIAN_POINT('',(17.5132903225806,25.104,7.40407194218736));
#59847=CARTESIAN_POINT('',(17.952,25.104,6.82615721505036));
#59848=CARTESIAN_POINT('Origin',(17.352,25.104,6.82615721505037));
#59849=CARTESIAN_POINT('Origin',(17.352,25.104,6.82615721505036));
#59850=CARTESIAN_POINT('Origin',(17.352,25.104,6.82615721505037));
#59851=CARTESIAN_POINT('Origin',(17.352,22.44,6.82615721505037));
#59852=CARTESIAN_POINT('',(17.5132903225806,22.44,7.40407194218736));
#59853=CARTESIAN_POINT('',(17.952,22.44,6.82615721505037));
#59854=CARTESIAN_POINT('Origin',(20.1018427849496,25.104,9.576));
#59855=CARTESIAN_POINT('Origin',(20.1018427849496,25.104,9.576));
#59856=CARTESIAN_POINT('Origin',(17.952,22.44,8.976));
#59857=CARTESIAN_POINT('Origin',(17.952,25.104,8.976));
#59858=CARTESIAN_POINT('Origin',(17.952,25.104,8.976));
#59859=CARTESIAN_POINT('Origin',(29.16,25.104,-32.9381572150504));
#59860=CARTESIAN_POINT('',(28.9987096774194,25.104,-33.5160719421874));
#59861=CARTESIAN_POINT('Origin',(29.16,25.104,-32.9381572150504));
#59862=CARTESIAN_POINT('Origin',(29.16,25.104,-32.9381572150504));
#59863=CARTESIAN_POINT('Origin',(29.16,22.44,-32.9381572150504));
#59864=CARTESIAN_POINT('',(28.9987096774193,22.44,-33.5160719421874));
#59865=CARTESIAN_POINT('Origin',(28.56,23.04,-35.088));
#59866=CARTESIAN_POINT('',(26.9880719421874,23.04,-35.5267096774194));
#59867=CARTESIAN_POINT('Origin',(28.56,23.04,-35.088));
#59868=CARTESIAN_POINT('Origin',(26.4101572150504,23.04,-35.688));
#59869=CARTESIAN_POINT('Origin',(26.4101572150504,23.04,-35.688));
#59870=CARTESIAN_POINT('',(26.4101572150504,23.04,-35.088));
#59871=CARTESIAN_POINT('Origin',(26.4101572150504,23.04,-35.688));
#59872=CARTESIAN_POINT('Origin',(26.4101572150504,23.04,-35.688));
#59873=CARTESIAN_POINT('Origin',(28.56,25.104,-35.088));
#59874=CARTESIAN_POINT('',(26.9880719421874,25.104,-35.5267096774194));
#59875=CARTESIAN_POINT('Origin',(26.4101572150504,25.104,-35.688));
#59876=CARTESIAN_POINT('Origin',(28.56,25.104,-35.088));
#59877=CARTESIAN_POINT('Origin',(20.1018427849496,25.104,-35.688));
#59878=CARTESIAN_POINT('',(19.5239280578126,25.104,-35.5267096774194));
#59879=CARTESIAN_POINT('',(20.1018427849496,25.104,-35.088));
#59880=CARTESIAN_POINT('Origin',(20.1018427849496,25.104,-35.688));
#59881=CARTESIAN_POINT('Origin',(20.1018427849496,25.104,-35.688));
#59882=CARTESIAN_POINT('Origin',(20.1018427849496,25.104,-35.688));
#59883=CARTESIAN_POINT('Origin',(20.1018427849496,22.44,-35.688));
#59884=CARTESIAN_POINT('',(20.1018427849496,22.44,-35.088));
#59885=CARTESIAN_POINT('',(19.5239280578126,22.44,-35.5267096774194));
#59886=CARTESIAN_POINT('Origin',(14.28,23.04,-35.688));
#59887=CARTESIAN_POINT('',(14.28,23.04,-35.088));
#59888=CARTESIAN_POINT('Origin',(26.4101572150504,22.44,-35.688));
#59889=CARTESIAN_POINT('',(26.9880719421874,22.44,-35.5267096774194));
#59890=CARTESIAN_POINT('',(26.4101572150504,25.104,-35.088));
#59891=CARTESIAN_POINT('Origin',(26.4101572150504,25.104,-35.688));
#59892=CARTESIAN_POINT('',(26.4101572150504,22.44,-35.088));
#59893=CARTESIAN_POINT('Origin',(26.4101572150504,25.104,-35.688));
#59894=CARTESIAN_POINT('Origin',(26.4101572150504,25.104,-35.688));
#59895=CARTESIAN_POINT('Origin',(28.56,22.44,-35.088));
#59896=CARTESIAN_POINT('',(14.28,25.104,-35.088));
#59897=CARTESIAN_POINT('Origin',(28.56,22.44,-35.088));
#59898=CARTESIAN_POINT('Origin',(-7.87026406871193,25.104,6.20573593128807));
#59899=CARTESIAN_POINT('',(-7.76453593128807,25.104,6.94853593128807));
#59900=CARTESIAN_POINT('Origin',(-8.1888,25.104,6.52427186257614));
#59901=CARTESIAN_POINT('',(-7.446,25.104,6.63));
#59902=CARTESIAN_POINT('Origin',(8.1888,23.04,6.52427186257615));
#59903=CARTESIAN_POINT('',(7.5888,23.04,6.52427186257614));
#59904=CARTESIAN_POINT('',(7.76453593128807,23.04,6.94853593128807));
#59905=CARTESIAN_POINT('Origin',(8.1888,23.04,6.52427186257614));
#59906=CARTESIAN_POINT('Origin',(8.1888,23.04,6.52427186257615));
#59907=CARTESIAN_POINT('Origin',(8.1888,23.04,6.52427186257614));
#59908=CARTESIAN_POINT('Origin',(0.,23.04,-21.7872));
#59909=CARTESIAN_POINT('',(7.5888,23.04,-21.7872));
#59910=CARTESIAN_POINT('Origin',(8.1888,23.04,-21.7872));
#59911=CARTESIAN_POINT('Origin',(0.,23.04,-21.7872));
#59912=CARTESIAN_POINT('Origin',(8.1888,23.04,-10.2816));
#59913=CARTESIAN_POINT('',(7.5888,23.04,-10.2816));
#59914=CARTESIAN_POINT('Origin',(4.72866406871193,23.04,3.06413593128807));
#59915=CARTESIAN_POINT('',(13.872,23.04,13.056));
#59916=CARTESIAN_POINT('',(4.3044,23.04,3.4884));
#59917=CARTESIAN_POINT('Origin',(14.472,23.04,12.8074718625761));
#59918=CARTESIAN_POINT('Origin',(14.472,23.04,32.448));
#59919=CARTESIAN_POINT('',(13.872,23.04,32.448));
#59920=CARTESIAN_POINT('',(14.472,23.04,33.048));
#59921=CARTESIAN_POINT('Origin',(14.472,23.04,32.448));
#59922=CARTESIAN_POINT('Origin',(14.472,23.04,32.448));
#59923=CARTESIAN_POINT('Origin',(14.472,23.04,32.448));
#59924=CARTESIAN_POINT('Origin',(14.472,23.04,7.14));
#59925=CARTESIAN_POINT('',(13.872,23.04,7.14));
#59926=CARTESIAN_POINT('Origin',(6.936,23.04,32.448));
#59927=CARTESIAN_POINT('',(16.728,23.04,33.048));
#59928=CARTESIAN_POINT('',(6.936,23.04,33.048));
#59929=CARTESIAN_POINT('Origin',(17.328,23.04,32.448));
#59930=CARTESIAN_POINT('Origin',(17.328,23.04,17.136));
#59931=CARTESIAN_POINT('',(16.728,23.04,39.168));
#59932=CARTESIAN_POINT('Origin',(17.328,23.04,39.768));
#59933=CARTESIAN_POINT('',(16.728,23.04,17.136));
#59934=CARTESIAN_POINT('Origin',(14.472,23.04,39.768));
#59935=CARTESIAN_POINT('',(14.472,23.04,39.168));
#59936=CARTESIAN_POINT('',(13.872,23.04,39.768));
#59937=CARTESIAN_POINT('Origin',(14.472,23.04,39.768));
#59938=CARTESIAN_POINT('Origin',(14.472,23.04,39.768));
#59939=CARTESIAN_POINT('Origin',(14.472,23.04,39.768));
#59940=CARTESIAN_POINT('Origin',(8.364,23.04,39.768));
#59941=CARTESIAN_POINT('',(8.364,23.04,39.168));
#59942=CARTESIAN_POINT('Origin',(14.472,23.04,47.952));
#59943=CARTESIAN_POINT('',(13.872,23.04,47.952));
#59944=CARTESIAN_POINT('',(14.472,23.04,48.552));
#59945=CARTESIAN_POINT('Origin',(14.472,23.04,47.952));
#59946=CARTESIAN_POINT('Origin',(14.472,23.04,47.952));
#59947=CARTESIAN_POINT('Origin',(14.472,23.04,47.952));
#59948=CARTESIAN_POINT('Origin',(14.472,23.04,20.196));
#59949=CARTESIAN_POINT('',(13.872,23.04,20.196));
#59950=CARTESIAN_POINT('Origin',(32.3914718625761,23.04,47.952));
#59951=CARTESIAN_POINT('',(32.3914718625761,23.04,48.552));
#59952=CARTESIAN_POINT('',(32.8157359312881,23.04,48.3762640687119));
#59953=CARTESIAN_POINT('Origin',(32.3914718625761,23.04,47.952));
#59954=CARTESIAN_POINT('Origin',(32.3914718625761,23.04,47.952));
#59955=CARTESIAN_POINT('Origin',(32.3914718625761,23.04,47.952));
#59956=CARTESIAN_POINT('Origin',(6.936,23.04,47.952));
#59957=CARTESIAN_POINT('',(6.936,23.04,48.552));
#59958=CARTESIAN_POINT('Origin',(35.8877359312881,23.04,44.455735931288));
#59959=CARTESIAN_POINT('',(36.312,23.04,44.88));
#59960=CARTESIAN_POINT('Origin',(32.3914718625761,22.44,47.952));
#59961=CARTESIAN_POINT('',(32.8157359312881,25.104,48.3762640687119));
#59962=CARTESIAN_POINT('',(32.3914718625761,25.104,48.552));
#59963=CARTESIAN_POINT('Origin',(32.3914718625761,25.104,47.952));
#59964=CARTESIAN_POINT('',(32.3914718625761,22.44,48.552));
#59965=CARTESIAN_POINT('',(32.8157359312881,22.44,48.3762640687119));
#59966=CARTESIAN_POINT('Origin',(35.8877359312881,25.104,44.455735931288));
#59967=CARTESIAN_POINT('Origin',(32.3914718625761,25.104,47.952));
#59968=CARTESIAN_POINT('',(36.312,25.104,44.88));
#59969=CARTESIAN_POINT('Origin',(14.472,22.44,47.952));
#59970=CARTESIAN_POINT('',(14.472,25.104,48.552));
#59971=CARTESIAN_POINT('',(13.872,25.104,47.952));
#59972=CARTESIAN_POINT('Origin',(14.472,25.104,47.952));
#59973=CARTESIAN_POINT('',(13.872,22.44,47.952));
#59974=CARTESIAN_POINT('',(14.472,22.44,48.552));
#59975=CARTESIAN_POINT('Origin',(14.472,25.104,47.952));
#59976=CARTESIAN_POINT('Origin',(14.472,25.104,47.952));
#59977=CARTESIAN_POINT('Origin',(14.472,25.104,47.952));
#59978=CARTESIAN_POINT('Origin',(14.472,22.44,39.768));
#59979=CARTESIAN_POINT('',(13.872,25.104,39.768));
#59980=CARTESIAN_POINT('',(14.472,25.104,39.168));
#59981=CARTESIAN_POINT('Origin',(14.472,25.104,39.768));
#59982=CARTESIAN_POINT('',(14.472,22.44,39.168));
#59983=CARTESIAN_POINT('',(13.872,22.44,39.768));
#59984=CARTESIAN_POINT('Origin',(14.472,25.104,39.768));
#59985=CARTESIAN_POINT('Origin',(14.472,25.104,39.768));
#59986=CARTESIAN_POINT('Origin',(14.472,25.104,39.768));
#59987=CARTESIAN_POINT('Origin',(14.472,22.44,32.448));
#59988=CARTESIAN_POINT('',(14.472,25.104,33.048));
#59989=CARTESIAN_POINT('',(13.872,25.104,32.448));
#59990=CARTESIAN_POINT('Origin',(14.472,25.104,32.448));
#59991=CARTESIAN_POINT('',(13.872,22.44,32.448));
#59992=CARTESIAN_POINT('',(14.472,22.44,33.048));
#59993=CARTESIAN_POINT('Origin',(14.472,25.104,32.448));
#59994=CARTESIAN_POINT('Origin',(14.472,25.104,32.448));
#59995=CARTESIAN_POINT('Origin',(14.472,25.104,32.448));
#59996=CARTESIAN_POINT('Origin',(8.1888,22.44,6.52427186257614));
#59997=CARTESIAN_POINT('',(7.76453593128807,25.104,6.94853593128807));
#59998=CARTESIAN_POINT('',(7.5888,25.104,6.52427186257614));
#59999=CARTESIAN_POINT('Origin',(8.1888,25.104,6.52427186257614));
#60000=CARTESIAN_POINT('',(7.5888,22.44,6.52427186257614));
#60001=CARTESIAN_POINT('',(7.76453593128807,22.44,6.94853593128807));
#60002=CARTESIAN_POINT('Origin',(8.1888,25.104,6.52427186257614));
#60003=CARTESIAN_POINT('Origin',(8.1888,25.104,6.52427186257615));
#60004=CARTESIAN_POINT('Origin',(8.1888,25.104,6.52427186257614));
#60005=CARTESIAN_POINT('Origin',(-8.1888,22.44,6.52427186257615));
#60006=CARTESIAN_POINT('',(-7.5888,25.104,6.52427186257615));
#60007=CARTESIAN_POINT('',(-7.5888,22.44,6.52427186257615));
#60008=CARTESIAN_POINT('Origin',(-8.1888,25.104,6.52427186257615));
#60009=CARTESIAN_POINT('',(-7.76453593128807,22.44,6.94853593128807));
#60010=CARTESIAN_POINT('Origin',(32.3914718625761,25.104,47.952));
#60011=CARTESIAN_POINT('Origin',(32.3914718625761,25.104,47.952));
#60012=CARTESIAN_POINT('Origin',(-8.1888,25.104,6.52427186257615));
#60013=CARTESIAN_POINT('Origin',(-8.1888,25.104,6.52427186257615));
#60014=CARTESIAN_POINT('Origin',(8.1888,25.104,-10.2816));
#60015=CARTESIAN_POINT('',(7.5888,25.104,-21.7872));
#60016=CARTESIAN_POINT('Origin',(8.1888,25.104,-21.7872));
#60017=CARTESIAN_POINT('',(7.5888,25.104,-10.2816));
#60018=CARTESIAN_POINT('Origin',(4.72866406871193,25.104,3.06413593128807));
#60019=CARTESIAN_POINT('',(13.872,25.104,13.056));
#60020=CARTESIAN_POINT('',(4.3044,25.104,3.4884));
#60021=CARTESIAN_POINT('Origin',(14.472,25.104,12.8074718625761));
#60022=CARTESIAN_POINT('Origin',(7.5888,22.44,6.7728));
#60023=CARTESIAN_POINT('',(13.872,22.44,13.056));
#60024=CARTESIAN_POINT('Origin',(13.872,22.44,13.056));
#60025=CARTESIAN_POINT('',(13.872,25.104,7.14));
#60026=CARTESIAN_POINT('Origin',(14.472,25.104,7.14));
#60027=CARTESIAN_POINT('Origin',(6.936,25.104,32.448));
#60028=CARTESIAN_POINT('',(16.728,25.104,33.048));
#60029=CARTESIAN_POINT('',(6.936,25.104,33.048));
#60030=CARTESIAN_POINT('Origin',(17.328,25.104,32.448));
#60031=CARTESIAN_POINT('Origin',(13.872,22.44,33.048));
#60032=CARTESIAN_POINT('',(16.728,22.44,33.048));
#60033=CARTESIAN_POINT('Origin',(16.728,22.44,33.048));
#60034=CARTESIAN_POINT('',(16.728,25.104,39.168));
#60035=CARTESIAN_POINT('',(16.728,22.44,39.168));
#60036=CARTESIAN_POINT('',(16.728,25.104,17.136));
#60037=CARTESIAN_POINT('Origin',(16.728,22.44,39.168));
#60038=CARTESIAN_POINT('',(8.364,25.104,39.168));
#60039=CARTESIAN_POINT('Origin',(8.364,25.104,39.768));
#60040=CARTESIAN_POINT('Origin',(17.328,25.104,39.768));
#60041=CARTESIAN_POINT('Origin',(13.872,22.44,39.168));
#60042=CARTESIAN_POINT('',(13.872,25.104,20.196));
#60043=CARTESIAN_POINT('Origin',(14.472,25.104,20.196));
#60044=CARTESIAN_POINT('Origin',(13.872,22.44,48.552));
#60045=CARTESIAN_POINT('',(6.936,25.104,48.552));
#60046=CARTESIAN_POINT('Origin',(6.936,25.104,47.952));
#60047=CARTESIAN_POINT('Origin',(32.64,22.44,48.552));
#60048=CARTESIAN_POINT('Origin',(17.328,25.104,17.136));
#60049=CARTESIAN_POINT('Origin',(-8.1888,25.104,3.9984));
#60050=CARTESIAN_POINT('',(-7.5888,25.104,-21.7872));
#60051=CARTESIAN_POINT('',(-7.5888,25.104,3.9984));
#60052=CARTESIAN_POINT('Origin',(-8.1888,25.104,-21.7872));
#60053=CARTESIAN_POINT('Origin',(0.,25.104,-21.7872));
#60054=CARTESIAN_POINT('Origin',(0.,25.104,-21.7872));
#60055=CARTESIAN_POINT('Origin',(7.5888,22.44,-21.7872));
#60056=CARTESIAN_POINT('',(7.5888,22.44,-21.7872));
#60057=CARTESIAN_POINT('Origin',(0.,22.44,-21.7872));
#60058=CARTESIAN_POINT('',(-7.5888,22.44,-21.7872));
#60059=CARTESIAN_POINT('Origin',(-7.5888,22.44,6.7728));
#60060=CARTESIAN_POINT('Origin',(14.28,25.104,-35.688));
#60061=CARTESIAN_POINT('Origin',(17.952,25.104,-35.088));
#60062=CARTESIAN_POINT('Origin',(17.952,25.104,-35.088));
#60063=CARTESIAN_POINT('Origin',(17.352,25.104,-16.932));
#60064=CARTESIAN_POINT('',(17.952,25.104,-16.932));
#60065=CARTESIAN_POINT('Origin',(17.952,22.44,-35.088));
#60066=CARTESIAN_POINT('Origin',(17.952,22.44,-35.088));
#60067=CARTESIAN_POINT('Origin',(-28.152,25.104,28.56));
#60068=CARTESIAN_POINT('Origin',(-28.152,25.104,31.66));
#60069=CARTESIAN_POINT('Origin',(3.456,25.104,-17.136));
#60070=CARTESIAN_POINT('Origin',(3.456,25.104,-37.944));
#60071=CARTESIAN_POINT('Origin',(3.456,25.104,-35.496));
#60072=CARTESIAN_POINT('Origin',(0.,25.104,-35.496));
#60073=CARTESIAN_POINT('',(-2.856,25.104,-35.496));
#60074=CARTESIAN_POINT('Origin',(-3.456,25.104,-35.496));
#60075=CARTESIAN_POINT('Origin',(0.,25.104,-35.496));
#60076=CARTESIAN_POINT('Origin',(-3.456,25.104,-18.36));
#60077=CARTESIAN_POINT('Origin',(-3.456,25.104,-37.944));
#60078=CARTESIAN_POINT('',(-2.856,25.104,-18.36));
#60079=CARTESIAN_POINT('Origin',(0.,25.104,-37.944));
#60080=CARTESIAN_POINT('Origin',(0.,22.44,-35.496));
#60081=CARTESIAN_POINT('',(-2.856,22.44,-35.496));
#60082=CARTESIAN_POINT('Origin',(-29.376,25.104,38.352));
#60083=CARTESIAN_POINT('Origin',(-29.376,25.104,33.6154718625761));
#60084=CARTESIAN_POINT('Origin',(29.376,25.104,38.352));
#60085=CARTESIAN_POINT('',(25.0637359312881,25.5282640687119,38.352));
#60086=CARTESIAN_POINT('',(29.376,25.5282640687119,34.0397359312881));
#60087=CARTESIAN_POINT('Origin',(29.376,25.5282640687119,38.352));
#60088=CARTESIAN_POINT('Origin',(29.376,25.104,33.6154718625761));
#60089=CARTESIAN_POINT('Origin',(29.376,25.5282640687119,38.352));
#60090=CARTESIAN_POINT('Origin',(29.376,25.296,38.352));
#60091=CARTESIAN_POINT('',(29.376,25.0637359312881,42.1997359312881));
#60092=CARTESIAN_POINT('',(25.5282640687119,25.0637359312881,38.352));
#60093=CARTESIAN_POINT('Origin',(29.376,25.0637359312881,38.352));
#60094=CARTESIAN_POINT('Origin',(29.376,25.0637359312881,38.352));
#60095=CARTESIAN_POINT('',(25.296,25.296,38.352));
#60096=CARTESIAN_POINT('Origin',(29.376,24.6394718625761,38.352));
#60097=CARTESIAN_POINT('Origin',(29.376,24.6394718625761,42.624));
#60098=CARTESIAN_POINT('Origin',(-2.856,22.44,-37.944));
#60099=CARTESIAN_POINT('Origin',(-13.872,22.44,13.056));
#60100=CARTESIAN_POINT('',(0.,0.,0.));
#60101=CARTESIAN_POINT('Origin',(-18.368,7.548,38.36));
#60102=CARTESIAN_POINT('',(-18.768,14.272,38.36));
#60103=CARTESIAN_POINT('',(-18.768,8.576,38.36));
#60104=CARTESIAN_POINT('',(-18.768,7.548,38.36));
#60105=CARTESIAN_POINT('',(-18.368,8.976,38.76));
#60106=CARTESIAN_POINT('Origin',(-18.368,8.576,38.36));
#60107=CARTESIAN_POINT('',(-18.368,13.872,38.76));
#60108=CARTESIAN_POINT('',(-18.368,7.548,38.76));
#60109=CARTESIAN_POINT('Origin',(-18.368,14.272,38.36));
#60110=CARTESIAN_POINT('Origin',(-18.368,8.576,37.332));
#60111=CARTESIAN_POINT('',(-18.368,8.976,41.616));
#60112=CARTESIAN_POINT('',(-18.368,8.976,37.332));
#60113=CARTESIAN_POINT('',(-18.768,8.576,42.016));
#60114=CARTESIAN_POINT('',(-18.768,8.576,37.332));
#60115=CARTESIAN_POINT('Origin',(-18.368,8.576,42.016));
#60116=CARTESIAN_POINT('Origin',(-18.368,14.272,38.76));
#60117=CARTESIAN_POINT('',(-18.768,14.272,42.016));
#60118=CARTESIAN_POINT('',(-18.768,14.272,38.76));
#60119=CARTESIAN_POINT('',(-18.368,13.872,41.616));
#60120=CARTESIAN_POINT('',(-18.368,13.872,38.76));
#60121=CARTESIAN_POINT('Origin',(-18.368,14.272,42.016));
#60122=CARTESIAN_POINT('Origin',(-18.368,5.1,42.016));
#60123=CARTESIAN_POINT('',(-18.768,5.1,42.016));
#60124=CARTESIAN_POINT('',(-18.368,5.1,41.616));
#60125=CARTESIAN_POINT('Origin',(-17.544,13.872,41.616));
#60126=CARTESIAN_POINT('',(-17.944,13.872,38.76));
#60127=CARTESIAN_POINT('',(-17.544,13.872,38.76));
#60128=CARTESIAN_POINT('',(-17.944,13.872,41.616));
#60129=CARTESIAN_POINT('',(-17.944,13.872,40.392));
#60130=CARTESIAN_POINT('',(-17.544,13.872,41.616));
#60131=CARTESIAN_POINT('Origin',(-17.544,13.872,38.76));
#60132=CARTESIAN_POINT('',(-17.944,8.976,38.76));
#60133=CARTESIAN_POINT('',(-17.544,8.976,38.76));
#60134=CARTESIAN_POINT('',(-17.944,12.852,38.76));
#60135=CARTESIAN_POINT('Origin',(-18.768,1.224,35.904));
#60136=CARTESIAN_POINT('',(-18.768,2.4322958752602,36.3127352401262));
#60137=CARTESIAN_POINT('',(-18.768,21.216,33.0460040879975));
#60138=CARTESIAN_POINT('',(-18.768,11.3065034423776,34.769394793671));
#60139=CARTESIAN_POINT('',(-18.768,2.048,35.904));
#60140=CARTESIAN_POINT('Origin',(-18.768,2.048,36.4696854249492));
#60141=CARTESIAN_POINT('',(-18.768,1.624,35.904));
#60142=CARTESIAN_POINT('',(-18.768,1.224,35.904));
#60143=CARTESIAN_POINT('',(-18.768,1.624,45.296));
#60144=CARTESIAN_POINT('',(-18.768,1.624,37.74));
#60145=CARTESIAN_POINT('',(-18.768,21.216,45.296));
#60146=CARTESIAN_POINT('',(-18.768,1.224,45.296));
#60147=CARTESIAN_POINT('',(-18.768,21.216,32.64));
#60148=CARTESIAN_POINT('Origin',(-18.368,11.3065034423776,34.769394793671));
#60149=CARTESIAN_POINT('',(-18.368,2.43108893861255,35.9069410541543));
#60150=CARTESIAN_POINT('Ctrl Pts',(-18.768,2.43229587526021,36.3127352401262));
#60151=CARTESIAN_POINT('Ctrl Pts',(-18.768,2.43163865325589,36.3095167959342));
#60152=CARTESIAN_POINT('Ctrl Pts',(-18.7679595430623,2.43096733281414,36.3062986618292));
#60153=CARTESIAN_POINT('Ctrl Pts',(-18.7670365475227,2.42318946934172,36.2696281280777));
#60154=CARTESIAN_POINT('Ctrl Pts',(-18.7617623197712,2.41476971759224,36.2363087583245));
#60155=CARTESIAN_POINT('Ctrl Pts',(-18.7426520469775,2.39907273991872,36.1720724010591));
#60156=CARTESIAN_POINT('Ctrl Pts',(-18.7287849670363,2.3918106985706,36.1410603177669));
#60157=CARTESIAN_POINT('Ctrl Pts',(-18.6936954523635,2.38175700469627,36.0832890660283));
#60158=CARTESIAN_POINT('Ctrl Pts',(-18.672468995915,2.37899329807783,36.0565274804843));
#60159=CARTESIAN_POINT('Ctrl Pts',(-18.6001051985816,2.37899329807783,35.9841636831509));
#60160=CARTESIAN_POINT('Ctrl Pts',(-18.5389719289432,2.39142035091093,35.9463799403922));
#60161=CARTESIAN_POINT('Ctrl Pts',(-18.4407068959515,2.41470336343454,35.9150691173314));
#60162=CARTESIAN_POINT('Ctrl Pts',(-18.4068151443652,2.42301155359813,35.9087870732679));
#60163=CARTESIAN_POINT('Ctrl Pts',(-18.3711843766952,2.43043368046293,35.9070646745485));
#60164=CARTESIAN_POINT('Ctrl Pts',(-18.3695923051444,2.43076276515015,35.9069977799739));
#60165=CARTESIAN_POINT('Ctrl Pts',(-18.368,2.43108893861256,35.9069410541544));
#60166=CARTESIAN_POINT('',(-18.368,21.216,32.64));
#60167=CARTESIAN_POINT('Origin',(-18.368,21.216,33.0460040879975));
#60168=CARTESIAN_POINT('',(-18.368,11.2379669724771,34.3753100917431));
#60169=CARTESIAN_POINT('Origin',(-17.944,10.404,42.016));
#60170=CARTESIAN_POINT('',(-17.544,14.272,42.016));
#60171=CARTESIAN_POINT('',(-17.544,8.576,42.016));
#60172=CARTESIAN_POINT('',(-17.544,10.404,42.016));
#60173=CARTESIAN_POINT('',(-17.944,8.976,41.616));
#60174=CARTESIAN_POINT('Origin',(-17.944,8.576,42.016));
#60175=CARTESIAN_POINT('',(-17.944,10.404,41.616));
#60176=CARTESIAN_POINT('Origin',(-17.944,14.272,42.016));
#60177=CARTESIAN_POINT('Origin',(-17.944,12.852,38.36));
#60178=CARTESIAN_POINT('',(-17.544,8.576,38.36));
#60179=CARTESIAN_POINT('',(-17.544,14.272,38.36));
#60180=CARTESIAN_POINT('',(-17.544,12.852,38.36));
#60181=CARTESIAN_POINT('Origin',(-17.944,14.272,38.36));
#60182=CARTESIAN_POINT('Origin',(-17.944,8.576,38.36));
#60183=CARTESIAN_POINT('Origin',(-17.944,14.272,40.392));
#60184=CARTESIAN_POINT('',(-17.544,14.272,40.392));
#60185=CARTESIAN_POINT('Origin',(-17.944,8.576,38.964));
#60186=CARTESIAN_POINT('',(-17.544,8.576,38.964));
#60187=CARTESIAN_POINT('',(-17.944,8.976,38.964));
#60188=CARTESIAN_POINT('Origin',(-17.544,8.976,38.76));
#60189=CARTESIAN_POINT('',(-17.544,8.976,41.616));
#60190=CARTESIAN_POINT('Origin',(-17.544,11.832,39.168));
#60191=CARTESIAN_POINT('',(-17.544,21.616,32.9764388706062));
#60192=CARTESIAN_POINT('',(-17.544,2.448,36.3100040879975));
#60193=CARTESIAN_POINT('',(-17.544,16.179296102928,33.9219525918361));
#60194=CARTESIAN_POINT('',(-17.544,21.616,21.216));
#60195=CARTESIAN_POINT('',(-17.544,21.616,36.312));
#60196=CARTESIAN_POINT('',(-17.544,22.04,21.216));
#60197=CARTESIAN_POINT('',(-17.544,21.216,21.216));
#60198=CARTESIAN_POINT('',(-17.544,22.04,45.296));
#60199=CARTESIAN_POINT('',(-17.544,22.04,36.312));
#60200=CARTESIAN_POINT('',(-17.544,2.448,45.296));
#60201=CARTESIAN_POINT('',(-17.544,6.528,45.296));
#60202=CARTESIAN_POINT('',(-17.544,2.448,39.372));
#60203=CARTESIAN_POINT('Origin',(-17.944,16.179296102928,33.9219525918361));
#60204=CARTESIAN_POINT('',(-17.944,21.216,32.64));
#60205=CARTESIAN_POINT('Origin',(-17.944,21.616,32.9764388706062));
#60206=CARTESIAN_POINT('',(-17.944,2.448,35.904));
#60207=CARTESIAN_POINT('Origin',(-17.944,2.448,36.3100040879975));
#60208=CARTESIAN_POINT('',(-17.944,16.1107596330275,33.5278678899083));
#60209=CARTESIAN_POINT('Origin',(18.368,1.09602270843261,36.5451305734875));
#60210=CARTESIAN_POINT('',(18.768,2.4322958752602,36.3127352401262));
#60211=CARTESIAN_POINT('',(18.368,2.43108893861254,35.9069410541543));
#60212=CARTESIAN_POINT('Ctrl Pts',(18.368,2.43108893861255,35.9069410541543));
#60213=CARTESIAN_POINT('Ctrl Pts',(18.3695923051444,2.43076276515014,35.9069977799739));
#60214=CARTESIAN_POINT('Ctrl Pts',(18.3711843766952,2.43043368046293,35.9070646745484));
#60215=CARTESIAN_POINT('Ctrl Pts',(18.4068151443652,2.42301155359813,35.9087870732679));
#60216=CARTESIAN_POINT('Ctrl Pts',(18.4407068959515,2.41470336343453,35.9150691173314));
#60217=CARTESIAN_POINT('Ctrl Pts',(18.5389719289432,2.39142035091092,35.9463799403922));
#60218=CARTESIAN_POINT('Ctrl Pts',(18.6001051985816,2.37899329807782,35.9841636831509));
#60219=CARTESIAN_POINT('Ctrl Pts',(18.672468995915,2.37899329807782,36.0565274804843));
#60220=CARTESIAN_POINT('Ctrl Pts',(18.6936954523635,2.38175700469626,36.0832890660283));
#60221=CARTESIAN_POINT('Ctrl Pts',(18.7287849670363,2.3918106985706,36.1410603177669));
#60222=CARTESIAN_POINT('Ctrl Pts',(18.7426520469775,2.39907273991871,36.1720724010591));
#60223=CARTESIAN_POINT('Ctrl Pts',(18.7617623197712,2.41476971759224,36.2363087583245));
#60224=CARTESIAN_POINT('Ctrl Pts',(18.7670365475227,2.42318946934172,36.2696281280776));
#60225=CARTESIAN_POINT('Ctrl Pts',(18.7679595430623,2.43096733281413,36.3062986618292));
#60226=CARTESIAN_POINT('Ctrl Pts',(18.768,2.4316386532559,36.3095167959342));
#60227=CARTESIAN_POINT('Ctrl Pts',(18.768,2.43229587526021,36.3127352401262));
#60228=CARTESIAN_POINT('',(18.368,21.216,32.64));
#60229=CARTESIAN_POINT('',(18.368,1.02748623853211,36.1510458715596));
#60230=CARTESIAN_POINT('',(18.768,21.216,33.0460040879975));
#60231=CARTESIAN_POINT('Origin',(18.368,21.216,33.0460040879975));
#60232=CARTESIAN_POINT('',(18.768,1.09602270843261,36.5451305734875));
#60233=CARTESIAN_POINT('Origin',(17.544,2.448,35.904));
#60234=CARTESIAN_POINT('',(18.2023145750508,2.448,35.904));
#60235=CARTESIAN_POINT('Origin',(18.2718797924421,2.048,35.9735652173913));
#60236=CARTESIAN_POINT('',(17.944,2.448,35.904));
#60237=CARTESIAN_POINT('',(8.772,2.448,35.904));
#60238=CARTESIAN_POINT('',(17.944,21.216,32.64));
#60239=CARTESIAN_POINT('',(17.944,6.72675963302752,35.1598678899083));
#60240=CARTESIAN_POINT('',(17.544,21.216,32.64));
#60241=CARTESIAN_POINT('Origin',(18.368,7.548,42.016));
#60242=CARTESIAN_POINT('',(18.768,14.272,42.016));
#60243=CARTESIAN_POINT('',(18.768,8.576,42.016));
#60244=CARTESIAN_POINT('',(18.768,7.548,42.016));
#60245=CARTESIAN_POINT('',(18.368,8.976,41.616));
#60246=CARTESIAN_POINT('Origin',(18.368,8.576,42.016));
#60247=CARTESIAN_POINT('',(18.368,13.872,41.616));
#60248=CARTESIAN_POINT('',(18.368,7.548,41.616));
#60249=CARTESIAN_POINT('Origin',(18.368,14.272,42.016));
#60250=CARTESIAN_POINT('Origin',(18.368,8.576,43.656));
#60251=CARTESIAN_POINT('',(18.368,8.976,38.76));
#60252=CARTESIAN_POINT('',(18.368,8.976,43.656));
#60253=CARTESIAN_POINT('',(18.768,8.576,38.36));
#60254=CARTESIAN_POINT('',(18.768,8.576,43.656));
#60255=CARTESIAN_POINT('Origin',(18.368,8.576,38.36));
#60256=CARTESIAN_POINT('Origin',(18.368,14.272,42.228));
#60257=CARTESIAN_POINT('',(18.768,14.272,38.36));
#60258=CARTESIAN_POINT('',(18.768,14.272,42.228));
#60259=CARTESIAN_POINT('',(18.368,13.872,38.76));
#60260=CARTESIAN_POINT('',(18.368,13.872,42.228));
#60261=CARTESIAN_POINT('Origin',(18.368,14.272,38.36));
#60262=CARTESIAN_POINT('Origin',(18.368,5.1,38.36));
#60263=CARTESIAN_POINT('',(18.768,5.1,38.36));
#60264=CARTESIAN_POINT('',(18.368,5.1,38.76));
#60265=CARTESIAN_POINT('Origin',(17.544,13.872,38.76));
#60266=CARTESIAN_POINT('',(17.944,13.872,41.616));
#60267=CARTESIAN_POINT('',(17.544,13.872,41.616));
#60268=CARTESIAN_POINT('',(17.944,13.872,38.76));
#60269=CARTESIAN_POINT('',(17.944,13.872,38.964));
#60270=CARTESIAN_POINT('',(17.544,13.872,38.76));
#60271=CARTESIAN_POINT('Origin',(17.544,13.872,41.616));
#60272=CARTESIAN_POINT('',(17.944,8.976,41.616));
#60273=CARTESIAN_POINT('',(17.544,8.976,41.616));
#60274=CARTESIAN_POINT('',(17.944,12.852,41.616));
#60275=CARTESIAN_POINT('Origin',(18.768,1.224,45.696));
#60276=CARTESIAN_POINT('',(18.768,21.216,45.296));
#60277=CARTESIAN_POINT('',(18.768,21.216,32.64));
#60278=CARTESIAN_POINT('',(18.768,1.624,45.296));
#60279=CARTESIAN_POINT('',(18.768,1.224,45.296));
#60280=CARTESIAN_POINT('',(18.768,1.624,35.904));
#60281=CARTESIAN_POINT('',(18.768,1.624,42.636));
#60282=CARTESIAN_POINT('',(18.768,2.048,35.904));
#60283=CARTESIAN_POINT('',(18.768,1.224,35.904));
#60284=CARTESIAN_POINT('Origin',(18.768,2.048,36.4696854249492));
#60285=CARTESIAN_POINT('Origin',(-17.944,22.04,45.296));
#60286=CARTESIAN_POINT('',(-17.944,22.04,45.696));
#60287=CARTESIAN_POINT('Origin',(-17.944,22.04,45.296));
#60288=CARTESIAN_POINT('',(-17.944,22.44,45.296));
#60289=CARTESIAN_POINT('Origin',(-17.944,22.04,45.296));
#60290=CARTESIAN_POINT('Origin',(-17.944,22.04,45.296));
#60291=CARTESIAN_POINT('Origin',(-17.944,6.528,45.296));
#60292=CARTESIAN_POINT('',(-17.944,2.048,45.696));
#60293=CARTESIAN_POINT('Origin',(-17.944,2.048,45.296));
#60294=CARTESIAN_POINT('',(-17.944,6.528,45.696));
#60295=CARTESIAN_POINT('Origin',(-18.768,1.224,45.696));
#60296=CARTESIAN_POINT('',(17.944,2.048,45.696));
#60297=CARTESIAN_POINT('',(-9.384,2.048,45.696));
#60298=CARTESIAN_POINT('',(-32.64,22.04,45.696));
#60299=CARTESIAN_POINT('',(-26.316,22.04,45.696));
#60300=CARTESIAN_POINT('',(-32.64,21.616,45.696));
#60301=CARTESIAN_POINT('',(-32.64,21.216,45.696));
#60302=CARTESIAN_POINT('',(-18.368,21.616,45.696));
#60303=CARTESIAN_POINT('',(-26.316,21.616,45.696));
#60304=CARTESIAN_POINT('',(-18.368,1.624,45.696));
#60305=CARTESIAN_POINT('',(-18.368,1.224,45.696));
#60306=CARTESIAN_POINT('',(18.368,1.624,45.696));
#60307=CARTESIAN_POINT('',(-9.384,1.624,45.696));
#60308=CARTESIAN_POINT('',(18.368,21.616,45.696));
#60309=CARTESIAN_POINT('',(18.368,1.224,45.696));
#60310=CARTESIAN_POINT('',(32.64,21.616,45.696));
#60311=CARTESIAN_POINT('',(7.548,21.616,45.696));
#60312=CARTESIAN_POINT('',(32.64,22.04,45.696));
#60313=CARTESIAN_POINT('',(32.64,21.216,45.696));
#60314=CARTESIAN_POINT('',(17.944,22.04,45.696));
#60315=CARTESIAN_POINT('',(7.548,22.04,45.696));
#60316=CARTESIAN_POINT('',(17.944,6.528,45.696));
#60317=CARTESIAN_POINT('Origin',(-26.316,22.04,45.296));
#60318=CARTESIAN_POINT('',(-32.5750889359327,22.44,45.296));
#60319=CARTESIAN_POINT('',(-26.316,22.44,45.296));
#60320=CARTESIAN_POINT('Origin',(-32.5750889359327,22.04,45.296));
#60321=CARTESIAN_POINT('Origin',(-17.944,22.04,36.312));
#60322=CARTESIAN_POINT('',(-17.944,22.44,21.616));
#60323=CARTESIAN_POINT('Origin',(-17.944,22.04,21.616));
#60324=CARTESIAN_POINT('',(-17.944,22.44,36.312));
#60325=CARTESIAN_POINT('Origin',(7.548,21.616,45.296));
#60326=CARTESIAN_POINT('Origin',(18.368,21.616,45.296));
#60327=CARTESIAN_POINT('',(32.5750889359327,21.216,45.296));
#60328=CARTESIAN_POINT('',(7.548,21.216,45.296));
#60329=CARTESIAN_POINT('Origin',(32.5750889359326,21.616,45.296));
#60330=CARTESIAN_POINT('Origin',(18.368,1.624,45.296));
#60331=CARTESIAN_POINT('Origin',(18.368,1.624,45.296));
#60332=CARTESIAN_POINT('',(18.368,1.224,45.296));
#60333=CARTESIAN_POINT('Origin',(18.368,1.624,45.296));
#60334=CARTESIAN_POINT('Origin',(18.368,1.624,45.296));
#60335=CARTESIAN_POINT('Origin',(18.368,1.224,45.296));
#60336=CARTESIAN_POINT('Origin',(34.9003088935933,21.616,44.5209266807798));
#60337=CARTESIAN_POINT('',(37.4710889359326,21.216,43.664));
#60338=CARTESIAN_POINT('',(34.9003088935933,21.216,44.5209266807798));
#60339=CARTESIAN_POINT('',(37.536,21.616,44.064));
#60340=CARTESIAN_POINT('Origin',(37.4710889359326,21.616,43.664));
#60341=CARTESIAN_POINT('',(35.0268,21.616,44.9004));
#60342=CARTESIAN_POINT('Origin',(32.64,21.216,45.696));
#60343=CARTESIAN_POINT('',(37.536,22.04,44.064));
#60344=CARTESIAN_POINT('',(37.536,21.216,44.064));
#60345=CARTESIAN_POINT('',(35.0268,22.04,44.9004));
#60346=CARTESIAN_POINT('Origin',(-17.944,21.616,36.312));
#60347=CARTESIAN_POINT('',(-17.944,21.216,21.616));
#60348=CARTESIAN_POINT('',(-17.944,21.216,36.312));
#60349=CARTESIAN_POINT('Origin',(-17.944,21.616,21.616));
#60350=CARTESIAN_POINT('Origin',(-25.704,21.616,21.616));
#60351=CARTESIAN_POINT('',(-24.4189556308608,21.216,21.616));
#60352=CARTESIAN_POINT('',(-25.704,21.216,21.616));
#60353=CARTESIAN_POINT('',(-24.48,21.616,21.216));
#60354=CARTESIAN_POINT('Origin',(-24.4189556308608,21.616,21.616));
#60355=CARTESIAN_POINT('',(-25.704,21.616,21.216));
#60356=CARTESIAN_POINT('Origin',(-30.3776010347741,21.616,23.4780766887229));
#60357=CARTESIAN_POINT('',(-37.3227504587735,21.216,25.6484358837227));
#60358=CARTESIAN_POINT('',(-30.3776010347741,21.216,23.4780766887229));
#60359=CARTESIAN_POINT('',(-37.536,21.616,25.296));
#60360=CARTESIAN_POINT('Origin',(-37.3227504587735,21.616,25.6484358837227));
#60361=CARTESIAN_POINT('',(-30.4969110320285,21.616,23.0962846975089));
#60362=CARTESIAN_POINT('Origin',(-38.964,21.616,43.664));
#60363=CARTESIAN_POINT('',(-37.536,21.616,44.064));
#60364=CARTESIAN_POINT('',(-44.064,21.616,44.064));
#60365=CARTESIAN_POINT('',(-38.964,21.616,44.064));
#60366=CARTESIAN_POINT('',(-44.064,21.216,43.664));
#60367=CARTESIAN_POINT('Origin',(-44.064,21.616,43.664));
#60368=CARTESIAN_POINT('',(-37.4710889359326,21.216,43.664));
#60369=CARTESIAN_POINT('',(-38.964,21.216,43.664));
#60370=CARTESIAN_POINT('Origin',(-37.4710889359326,21.616,43.664));
#60371=CARTESIAN_POINT('Origin',(-37.3483088935933,21.616,43.7049266807798));
#60372=CARTESIAN_POINT('',(-32.5750889359327,21.216,45.296));
#60373=CARTESIAN_POINT('',(-37.3483088935933,21.216,43.7049266807798));
#60374=CARTESIAN_POINT('Origin',(-32.5750889359327,21.616,45.296));
#60375=CARTESIAN_POINT('',(-37.4748,21.616,44.0844));
#60376=CARTESIAN_POINT('Origin',(-18.368,1.624,45.296));
#60377=CARTESIAN_POINT('Origin',(-18.368,1.624,45.296));
#60378=CARTESIAN_POINT('',(-18.368,1.224,45.296));
#60379=CARTESIAN_POINT('Origin',(-18.368,1.624,45.296));
#60380=CARTESIAN_POINT('Origin',(-18.368,1.624,45.296));
#60381=CARTESIAN_POINT('Origin',(-18.368,1.224,45.296));
#60382=CARTESIAN_POINT('Origin',(-18.368,21.616,45.296));
#60383=CARTESIAN_POINT('Origin',(-26.316,21.616,45.296));
#60384=CARTESIAN_POINT('',(-26.316,21.216,45.296));
#60385=CARTESIAN_POINT('Origin',(-44.064,21.616,37.944));
#60386=CARTESIAN_POINT('',(-43.9006475697477,21.216,32.226332994697));
#60387=CARTESIAN_POINT('Origin',(-44.064,21.216,37.944));
#60388=CARTESIAN_POINT('',(-44.064,21.616,31.824));
#60389=CARTESIAN_POINT('Origin',(-44.064,21.616,37.944));
#60390=CARTESIAN_POINT('Ctrl Pts',(-44.064,21.616,31.824));
#60391=CARTESIAN_POINT('Ctrl Pts',(-44.064,21.5840682080023,31.824));
#60392=CARTESIAN_POINT('Ctrl Pts',(-44.0624149120547,21.5524184382745,31.8278216249186));
#60393=CARTESIAN_POINT('Ctrl Pts',(-44.0593318094221,21.5217063486302,31.8352741901928));
#60394=CARTESIAN_POINT('Ctrl Pts',(-44.0577471400151,21.5059207862653,31.8391046991316));
#60395=CARTESIAN_POINT('Ctrl Pts',(-44.0557666149525,21.4903819028471,31.843894541907));
#60396=CARTESIAN_POINT('Ctrl Pts',(-44.0534015865836,21.475175853192,31.8496182972997));
#60397=CARTESIAN_POINT('Ctrl Pts',(-44.0495756131013,21.4505765953079,31.8588777787669));
#60398=CARTESIAN_POINT('Ctrl Pts',(-44.0447927695183,21.4271697387686,31.8704588320918));
#60399=CARTESIAN_POINT('Ctrl Pts',(-44.0391810250039,21.4052271621859,31.8840862281474));
#60400=CARTESIAN_POINT('Ctrl Pts',(-44.0341776804514,21.3856635005241,31.8962362035505));
#60401=CARTESIAN_POINT('Ctrl Pts',(-44.0285149435481,21.3672620257947,31.9100133437439));
#60402=CARTESIAN_POINT('Ctrl Pts',(-44.0222720478219,21.3501947099065,31.9252340460289));
#60403=CARTESIAN_POINT('Ctrl Pts',(-44.0152384316176,21.3309656606226,31.9423825910193));
#60404=CARTESIAN_POINT('Ctrl Pts',(-44.0075357743028,21.3136149870718,31.9611976208913));
#60405=CARTESIAN_POINT('Ctrl Pts',(-43.9993191486927,21.2982764025804,31.9813427758152));
#60406=CARTESIAN_POINT('Ctrl Pts',(-43.990799466837,21.2823720805162,32.0022309504784));
#60407=CARTESIAN_POINT('Ctrl Pts',(-43.9817264778667,21.2686293158374,32.0245499043989));
#60408=CARTESIAN_POINT('Ctrl Pts',(-43.9722455966321,21.2571751454754,32.0479521273707));
#60409=CARTESIAN_POINT('Ctrl Pts',(-43.9611780430457,21.2438040630693,32.0752708280667));
#60410=CARTESIAN_POINT('Ctrl Pts',(-43.9496295400104,21.233637777512,32.1038928160359));
#60411=CARTESIAN_POINT('Ctrl Pts',(-43.9378427069995,21.2267529507217,32.1332458643287));
#60412=CARTESIAN_POINT('Ctrl Pts',(-43.9259526178902,21.2198078108386,32.1628560538942));
#60413=CARTESIAN_POINT('Ctrl Pts',(-43.9138558645576,21.2162224659953,32.1931211104425));
#60414=CARTESIAN_POINT('Ctrl Pts',(-43.9017875351294,21.21601003407,32.2234661770043));
#60415=CARTESIAN_POINT('Ctrl Pts',(-43.9014075008992,21.216003344544,32.2244217495283));
#60416=CARTESIAN_POINT('Ctrl Pts',(-43.9010275100446,21.216,32.2253773614068));
#60417=CARTESIAN_POINT('Ctrl Pts',(-43.9006475697477,21.216,32.226332994697));
#60418=CARTESIAN_POINT('Origin',(-38.3751572875254,21.616,26.7008427124746));
#60419=CARTESIAN_POINT('',(-38.3751572875254,21.216,26.7008427124746));
#60420=CARTESIAN_POINT('',(-38.658,21.616,26.418));
#60421=CARTESIAN_POINT('Origin',(-17.544,21.216,21.216));
#60422=CARTESIAN_POINT('',(-24.48,22.04,21.216));
#60423=CARTESIAN_POINT('',(-24.48,21.216,21.216));
#60424=CARTESIAN_POINT('',(-25.704,22.04,21.216));
#60425=CARTESIAN_POINT('Origin',(-24.48,21.216,21.216));
#60426=CARTESIAN_POINT('',(-37.536,22.04,25.296));
#60427=CARTESIAN_POINT('',(-37.536,21.216,25.296));
#60428=CARTESIAN_POINT('',(-30.4969110320285,22.04,23.0962846975089));
#60429=CARTESIAN_POINT('Origin',(-37.536,21.216,25.296));
#60430=CARTESIAN_POINT('',(-44.064,22.04,31.824));
#60431=CARTESIAN_POINT('',(-44.064,21.216,31.824));
#60432=CARTESIAN_POINT('',(-38.658,22.04,26.418));
#60433=CARTESIAN_POINT('Origin',(-44.064,21.216,37.944));
#60434=CARTESIAN_POINT('',(-44.064,22.04,44.064));
#60435=CARTESIAN_POINT('',(-44.064,21.216,44.064));
#60436=CARTESIAN_POINT('Origin',(-44.064,22.04,37.944));
#60437=CARTESIAN_POINT('Origin',(-44.064,21.216,44.064));
#60438=CARTESIAN_POINT('',(-37.536,22.04,44.064));
#60439=CARTESIAN_POINT('',(-37.536,21.216,44.064));
#60440=CARTESIAN_POINT('',(-38.964,22.04,44.064));
#60441=CARTESIAN_POINT('Origin',(-37.536,21.216,44.064));
#60442=CARTESIAN_POINT('',(-37.4748,22.04,44.0844));
#60443=CARTESIAN_POINT('Origin',(-9.384,1.624,45.296));
#60444=CARTESIAN_POINT('',(-9.384,1.224,45.296));
#60445=CARTESIAN_POINT('Origin',(-18.368,1.624,37.74));
#60446=CARTESIAN_POINT('',(-18.368,1.224,36.0696854249492));
#60447=CARTESIAN_POINT('Origin',(-18.368,1.624,36.0696854249492));
#60448=CARTESIAN_POINT('',(-18.368,1.224,37.74));
#60449=CARTESIAN_POINT('Origin',(17.944,6.528,45.296));
#60450=CARTESIAN_POINT('',(17.544,2.448,45.296));
#60451=CARTESIAN_POINT('Origin',(17.944,2.048,45.296));
#60452=CARTESIAN_POINT('',(17.544,22.04,45.296));
#60453=CARTESIAN_POINT('Origin',(17.944,22.04,45.296));
#60454=CARTESIAN_POINT('',(17.544,6.528,45.296));
#60455=CARTESIAN_POINT('Origin',(17.944,22.04,45.296));
#60456=CARTESIAN_POINT('',(17.944,22.44,45.296));
#60457=CARTESIAN_POINT('Origin',(17.944,22.04,45.296));
#60458=CARTESIAN_POINT('Origin',(17.944,22.04,45.296));
#60459=CARTESIAN_POINT('Origin',(7.548,22.04,45.296));
#60460=CARTESIAN_POINT('',(32.5750889359327,22.44,45.296));
#60461=CARTESIAN_POINT('Origin',(32.5750889359327,22.04,45.296));
#60462=CARTESIAN_POINT('',(7.548,22.44,45.296));
#60463=CARTESIAN_POINT('Origin',(17.944,6.79529610292802,35.5539525918361));
#60464=CARTESIAN_POINT('',(17.544,21.616,32.9764388706062));
#60465=CARTESIAN_POINT('Origin',(17.944,21.616,32.9764388706062));
#60466=CARTESIAN_POINT('',(17.544,2.448,36.3100040879975));
#60467=CARTESIAN_POINT('Origin',(17.944,2.448,36.3100040879975));
#60468=CARTESIAN_POINT('',(17.544,6.79529610292802,35.5539525918361));
#60469=CARTESIAN_POINT('Origin',(17.944,10.404,38.36));
#60470=CARTESIAN_POINT('',(17.544,14.272,38.36));
#60471=CARTESIAN_POINT('',(17.544,8.576,38.36));
#60472=CARTESIAN_POINT('',(17.544,10.404,38.36));
#60473=CARTESIAN_POINT('',(17.944,8.976,38.76));
#60474=CARTESIAN_POINT('Origin',(17.944,8.576,38.36));
#60475=CARTESIAN_POINT('',(17.944,10.404,38.76));
#60476=CARTESIAN_POINT('Origin',(17.944,14.272,38.36));
#60477=CARTESIAN_POINT('Origin',(17.944,12.852,42.016));
#60478=CARTESIAN_POINT('',(17.544,8.576,42.016));
#60479=CARTESIAN_POINT('',(17.544,14.272,42.016));
#60480=CARTESIAN_POINT('',(17.544,12.852,42.016));
#60481=CARTESIAN_POINT('Origin',(17.944,14.272,42.016));
#60482=CARTESIAN_POINT('Origin',(17.944,8.576,42.016));
#60483=CARTESIAN_POINT('Origin',(17.944,14.272,38.964));
#60484=CARTESIAN_POINT('',(17.544,14.272,38.964));
#60485=CARTESIAN_POINT('Origin',(17.944,8.576,40.392));
#60486=CARTESIAN_POINT('',(17.544,8.576,40.392));
#60487=CARTESIAN_POINT('',(17.944,8.976,40.392));
#60488=CARTESIAN_POINT('Origin',(17.544,8.976,41.616));
#60489=CARTESIAN_POINT('',(17.544,8.976,38.76));
#60490=CARTESIAN_POINT('Origin',(17.544,11.832,39.168));
#60491=CARTESIAN_POINT('',(17.544,22.04,21.216));
#60492=CARTESIAN_POINT('',(17.544,22.04,36.312));
#60493=CARTESIAN_POINT('',(17.544,21.616,21.216));
#60494=CARTESIAN_POINT('',(17.544,21.216,21.216));
#60495=CARTESIAN_POINT('',(17.544,21.616,36.312));
#60496=CARTESIAN_POINT('',(17.544,2.448,39.372));
#60497=CARTESIAN_POINT('Origin',(35.7,21.616,43.664));
#60498=CARTESIAN_POINT('',(44.064,21.216,43.664));
#60499=CARTESIAN_POINT('',(44.064,21.616,44.064));
#60500=CARTESIAN_POINT('Origin',(44.064,21.616,43.664));
#60501=CARTESIAN_POINT('',(35.7,21.616,44.064));
#60502=CARTESIAN_POINT('',(35.7,21.216,43.664));
#60503=CARTESIAN_POINT('Origin',(44.064,21.616,37.944));
#60504=CARTESIAN_POINT('',(44.064,21.616,31.824));
#60505=CARTESIAN_POINT('Origin',(44.064,21.616,37.944));
#60506=CARTESIAN_POINT('',(43.9006475697477,21.216,32.226332994697));
#60507=CARTESIAN_POINT('Origin',(44.064,21.216,37.944));
#60508=CARTESIAN_POINT('Ctrl Pts',(43.9006475697477,21.216,32.226332994697));
#60509=CARTESIAN_POINT('Ctrl Pts',(43.9010275100447,21.216,32.2253773614065));
#60510=CARTESIAN_POINT('Ctrl Pts',(43.901407500899,21.216003344544,32.2244217495286));
#60511=CARTESIAN_POINT('Ctrl Pts',(43.9017875351293,21.21601003407,32.2234661770043));
#60512=CARTESIAN_POINT('Ctrl Pts',(43.9138558645572,21.2162224659953,32.193121110443));
#60513=CARTESIAN_POINT('Ctrl Pts',(43.9259526178902,21.2198078108386,32.1628560538943));
#60514=CARTESIAN_POINT('Ctrl Pts',(43.9378427069995,21.2267529507217,32.1332458643287));
#60515=CARTESIAN_POINT('Ctrl Pts',(43.9496295400104,21.233637777512,32.1038928160359));
#60516=CARTESIAN_POINT('Ctrl Pts',(43.9611780430457,21.2438040630693,32.0752708280668));
#60517=CARTESIAN_POINT('Ctrl Pts',(43.9722455966321,21.2571751454754,32.0479521273707));
#60518=CARTESIAN_POINT('Ctrl Pts',(43.9820721961623,21.2690469896968,32.0236965473702));
#60519=CARTESIAN_POINT('Ctrl Pts',(43.9914607629778,21.2833774561247,32.0006045298454));
#60520=CARTESIAN_POINT('Ctrl Pts',(44.0002489315777,21.300024857828,31.9790634597097));
#60521=CARTESIAN_POINT('Ctrl Pts',(44.0081171229227,21.3149295493471,31.9597773866584));
#60522=CARTESIAN_POINT('Ctrl Pts',(44.0155043707225,21.3316927057167,31.9417342092235));
#60523=CARTESIAN_POINT('Ctrl Pts',(44.0222720478219,21.3501947099065,31.9252340460289));
#60524=CARTESIAN_POINT('Ctrl Pts',(44.029760827937,21.3706681218367,31.9069757733286));
#60525=CARTESIAN_POINT('Ctrl Pts',(44.0364152831142,21.393062029884,31.8907942319792));
#60526=CARTESIAN_POINT('Ctrl Pts',(44.0420970014355,21.4170773367871,31.8770079892748));
#60527=CARTESIAN_POINT('Ctrl Pts',(44.0464641694145,21.4355363439712,31.8664113996019));
#60528=CARTESIAN_POINT('Ctrl Pts',(44.0502563764082,21.4549535917043,31.8572302202428));
#60529=CARTESIAN_POINT('Ctrl Pts',(44.0534015865836,21.475175853192,31.8496182972998));
#60530=CARTESIAN_POINT('Ctrl Pts',(44.0584453970152,21.5076052451096,31.8374114512694));
#60531=CARTESIAN_POINT('Ctrl Pts',(44.0617407660415,21.5415499503757,31.8294519002684));
#60532=CARTESIAN_POINT('Ctrl Pts',(44.0631761028331,21.57616875624,31.8259877017421));
#60533=CARTESIAN_POINT('Ctrl Pts',(44.0637232166716,21.5893645635749,31.824667237469));
#60534=CARTESIAN_POINT('Ctrl Pts',(44.064,21.6026580205647,31.824));
#60535=CARTESIAN_POINT('Ctrl Pts',(44.064,21.616,31.824));
#60536=CARTESIAN_POINT('Origin',(41.6391572875254,21.616,29.9648427124746));
#60537=CARTESIAN_POINT('',(37.3227504587735,21.216,25.6484358837227));
#60538=CARTESIAN_POINT('',(41.6391572875254,21.216,29.9648427124746));
#60539=CARTESIAN_POINT('',(37.536,21.616,25.296));
#60540=CARTESIAN_POINT('Origin',(37.3227504587735,21.616,25.6484358837227));
#60541=CARTESIAN_POINT('',(41.922,21.616,29.682));
#60542=CARTESIAN_POINT('Origin',(36.9056010347741,21.616,25.5180766887229));
#60543=CARTESIAN_POINT('',(24.4189556308608,21.216,21.616));
#60544=CARTESIAN_POINT('',(36.9056010347741,21.216,25.5180766887229));
#60545=CARTESIAN_POINT('',(24.48,21.616,21.216));
#60546=CARTESIAN_POINT('Origin',(24.4189556308608,21.616,21.616));
#60547=CARTESIAN_POINT('',(37.0249110320285,21.616,25.1362846975089));
#60548=CARTESIAN_POINT('Origin',(17.944,21.616,36.312));
#60549=CARTESIAN_POINT('',(17.944,21.216,21.616));
#60550=CARTESIAN_POINT('',(17.944,21.216,36.312));
#60551=CARTESIAN_POINT('Origin',(17.944,21.616,21.616));
#60552=CARTESIAN_POINT('Origin',(29.172,21.616,21.616));
#60553=CARTESIAN_POINT('',(29.172,21.216,21.616));
#60554=CARTESIAN_POINT('',(29.172,21.616,21.216));
#60555=CARTESIAN_POINT('Origin',(37.536,21.216,44.064));
#60556=CARTESIAN_POINT('',(44.064,22.04,44.064));
#60557=CARTESIAN_POINT('',(44.064,21.216,44.064));
#60558=CARTESIAN_POINT('',(35.7,22.04,44.064));
#60559=CARTESIAN_POINT('Origin',(44.064,21.216,37.944));
#60560=CARTESIAN_POINT('',(44.064,22.04,31.824));
#60561=CARTESIAN_POINT('',(44.064,21.216,31.824));
#60562=CARTESIAN_POINT('Origin',(44.064,22.04,37.944));
#60563=CARTESIAN_POINT('Origin',(44.064,21.216,31.824));
#60564=CARTESIAN_POINT('',(37.536,22.04,25.296));
#60565=CARTESIAN_POINT('',(37.536,21.216,25.296));
#60566=CARTESIAN_POINT('',(41.922,22.04,29.682));
#60567=CARTESIAN_POINT('Origin',(37.536,21.216,25.296));
#60568=CARTESIAN_POINT('',(24.48,22.04,21.216));
#60569=CARTESIAN_POINT('',(24.48,21.216,21.216));
#60570=CARTESIAN_POINT('',(37.0249110320285,22.04,25.1362846975089));
#60571=CARTESIAN_POINT('Origin',(24.48,21.216,21.216));
#60572=CARTESIAN_POINT('',(29.172,22.04,21.216));
#60573=CARTESIAN_POINT('Origin',(-37.3483088935933,22.04,43.7049266807798));
#60574=CARTESIAN_POINT('',(-37.4710889359326,22.44,43.664));
#60575=CARTESIAN_POINT('',(-37.3483088935933,22.44,43.7049266807798));
#60576=CARTESIAN_POINT('Origin',(-37.4710889359326,22.04,43.664));
#60577=CARTESIAN_POINT('Origin',(-44.064,22.04,37.944));
#60578=CARTESIAN_POINT('',(-44.064,22.44,43.664));
#60579=CARTESIAN_POINT('Origin',(-44.064,22.04,43.664));
#60580=CARTESIAN_POINT('',(-43.9006475697477,22.44,32.226332994697));
#60581=CARTESIAN_POINT('Origin',(-44.064,22.44,37.944));
#60582=CARTESIAN_POINT('Ctrl Pts',(-43.9006475697477,22.44,32.226332994697));
#60583=CARTESIAN_POINT('Ctrl Pts',(-43.901027510044,22.44,32.2253773614083));
#60584=CARTESIAN_POINT('Ctrl Pts',(-43.9014075009006,22.439996655456,32.2244217495276));
#60585=CARTESIAN_POINT('Ctrl Pts',(-43.90178753513,22.43998996593,32.223466177005));
#60586=CARTESIAN_POINT('Ctrl Pts',(-43.9138558645418,22.4397775340048,32.1931211104619));
#60587=CARTESIAN_POINT('Ctrl Pts',(-43.9259526178886,22.4361921891623,32.1628560538983));
#60588=CARTESIAN_POINT('Ctrl Pts',(-43.9378427069994,22.4292470492784,32.133245864329));
#60589=CARTESIAN_POINT('Ctrl Pts',(-43.9496295400103,22.4223622224881,32.1038928160361));
#60590=CARTESIAN_POINT('Ctrl Pts',(-43.9611780430457,22.4121959369308,32.0752708280669));
#60591=CARTESIAN_POINT('Ctrl Pts',(-43.9722455966321,22.3988248545246,32.0479521273707));
#60592=CARTESIAN_POINT('Ctrl Pts',(-43.9820721961623,22.3869530103033,32.0236965473703));
#60593=CARTESIAN_POINT('Ctrl Pts',(-43.9914607629777,22.3726225438754,32.0006045298457));
#60594=CARTESIAN_POINT('Ctrl Pts',(-44.0002489315775,22.3559751421723,31.9790634597102));
#60595=CARTESIAN_POINT('Ctrl Pts',(-44.0081171229226,22.3410704506531,31.9597773866587));
#60596=CARTESIAN_POINT('Ctrl Pts',(-44.0155043707224,22.3243072942834,31.9417342092236));
#60597=CARTESIAN_POINT('Ctrl Pts',(-44.0222720478219,22.3058052900935,31.9252340460289));
#60598=CARTESIAN_POINT('Ctrl Pts',(-44.0297608279369,22.2853318781636,31.9069757733289));
#60599=CARTESIAN_POINT('Ctrl Pts',(-44.036415283114,22.2629379701166,31.8907942319796));
#60600=CARTESIAN_POINT('Ctrl Pts',(-44.0420970014353,22.238922663214,31.8770079892754));
#60601=CARTESIAN_POINT('Ctrl Pts',(-44.0464641694143,22.2204636560296,31.8664113996022));
#60602=CARTESIAN_POINT('Ctrl Pts',(-44.0502563764081,22.2010464082961,31.8572302202429));
#60603=CARTESIAN_POINT('Ctrl Pts',(-44.0534015865836,22.180824146808,31.8496182972997));
#60604=CARTESIAN_POINT('Ctrl Pts',(-44.0584453970151,22.1483947548905,31.8374114512694));
#60605=CARTESIAN_POINT('Ctrl Pts',(-44.0617407660415,22.1144500496243,31.8294519002684));
#60606=CARTESIAN_POINT('Ctrl Pts',(-44.063176102833,22.0798312437601,31.8259877017421));
#60607=CARTESIAN_POINT('Ctrl Pts',(-44.0637232166716,22.0666354364251,31.824667237469));
#60608=CARTESIAN_POINT('Ctrl Pts',(-44.064,22.0533419794354,31.824));
#60609=CARTESIAN_POINT('Ctrl Pts',(-44.064,22.04,31.824));
#60610=CARTESIAN_POINT('Origin',(-38.964,22.04,43.664));
#60611=CARTESIAN_POINT('',(-38.964,22.44,43.664));
#60612=CARTESIAN_POINT('Origin',(-38.3751572875254,22.04,26.7008427124746));
#60613=CARTESIAN_POINT('',(-37.3227504587735,22.44,25.6484358837227));
#60614=CARTESIAN_POINT('',(-38.3751572875254,22.44,26.7008427124746));
#60615=CARTESIAN_POINT('Origin',(-37.3227504587735,22.04,25.6484358837227));
#60616=CARTESIAN_POINT('Origin',(-30.3776010347741,22.04,23.4780766887229));
#60617=CARTESIAN_POINT('',(-24.4189556308608,22.44,21.616));
#60618=CARTESIAN_POINT('',(-30.3776010347741,22.44,23.4780766887229));
#60619=CARTESIAN_POINT('Origin',(-24.4189556308608,22.04,21.616));
#60620=CARTESIAN_POINT('Origin',(-25.704,22.04,21.616));
#60621=CARTESIAN_POINT('',(-25.704,22.44,21.616));
#60622=CARTESIAN_POINT('Origin',(-33.864,22.44,33.456));
#60623=CARTESIAN_POINT('',(-29.376,22.44,42.424));
#60624=CARTESIAN_POINT('Origin',(-29.376,22.44,38.352));
#60625=CARTESIAN_POINT('',(-44.064,22.44,40.792));
#60626=CARTESIAN_POINT('Origin',(-44.064,22.44,37.944));
#60627=CARTESIAN_POINT('',(-28.152,22.44,31.46));
#60628=CARTESIAN_POINT('Origin',(-28.152,22.44,28.56));
#60629=CARTESIAN_POINT('Origin',(-29.376,21.1264,38.352));
#60630=CARTESIAN_POINT('',(-29.376,20.7264,44.072));
#60631=CARTESIAN_POINT('Origin',(-29.376,20.7264,38.352));
#60632=CARTESIAN_POINT('',(-29.376,21.1264,44.472));
#60633=CARTESIAN_POINT('Origin',(-29.376,21.1264,44.072));
#60634=CARTESIAN_POINT('',(-35.496,21.1264,38.352));
#60635=CARTESIAN_POINT('Origin',(-29.376,21.1264,38.352));
#60636=CARTESIAN_POINT('Origin',(-29.376,21.1264,38.352));
#60637=CARTESIAN_POINT('Origin',(-29.376,20.7264,38.352));
#60638=CARTESIAN_POINT('',(-29.376,20.7264,34.28));
#60639=CARTESIAN_POINT('Origin',(-29.376,20.7264,38.352));
#60640=CARTESIAN_POINT('Origin',(-29.376,21.216,38.352));
#60641=CARTESIAN_POINT('',(-35.496,21.216,38.352));
#60642=CARTESIAN_POINT('',(-35.496,21.216,38.352));
#60643=CARTESIAN_POINT('Origin',(-29.376,21.216,38.352));
#60644=CARTESIAN_POINT('Origin',(35.7,22.04,43.664));
#60645=CARTESIAN_POINT('',(44.064,22.44,43.664));
#60646=CARTESIAN_POINT('Origin',(44.064,22.04,43.664));
#60647=CARTESIAN_POINT('',(37.4710889359326,22.44,43.664));
#60648=CARTESIAN_POINT('',(35.7,22.44,43.664));
#60649=CARTESIAN_POINT('Origin',(37.4710889359326,22.04,43.664));
#60650=CARTESIAN_POINT('Origin',(34.9003088935933,22.04,44.5209266807798));
#60651=CARTESIAN_POINT('',(34.9003088935933,22.44,44.5209266807798));
#60652=CARTESIAN_POINT('Origin',(17.944,22.04,36.312));
#60653=CARTESIAN_POINT('',(17.944,22.44,21.616));
#60654=CARTESIAN_POINT('',(17.944,22.44,36.312));
#60655=CARTESIAN_POINT('Origin',(17.944,22.04,21.616));
#60656=CARTESIAN_POINT('Origin',(29.172,22.04,21.616));
#60657=CARTESIAN_POINT('',(24.4189556308608,22.44,21.616));
#60658=CARTESIAN_POINT('',(29.172,22.44,21.616));
#60659=CARTESIAN_POINT('Origin',(24.4189556308608,22.04,21.616));
#60660=CARTESIAN_POINT('Origin',(36.9056010347741,22.04,25.5180766887229));
#60661=CARTESIAN_POINT('',(37.3227504587735,22.44,25.6484358837227));
#60662=CARTESIAN_POINT('',(36.9056010347741,22.44,25.5180766887229));
#60663=CARTESIAN_POINT('Origin',(37.3227504587735,22.04,25.6484358837227));
#60664=CARTESIAN_POINT('Origin',(41.6391572875254,22.04,29.9648427124746));
#60665=CARTESIAN_POINT('',(43.9006475697477,22.44,32.226332994697));
#60666=CARTESIAN_POINT('',(41.6391572875254,22.44,29.9648427124746));
#60667=CARTESIAN_POINT('Ctrl Pts',(43.9006475697477,22.44,32.226332994697));
#60668=CARTESIAN_POINT('Ctrl Pts',(43.9010275100447,22.44,32.2253773614065));
#60669=CARTESIAN_POINT('Ctrl Pts',(43.901407500899,22.439996655456,32.2244217495286));
#60670=CARTESIAN_POINT('Ctrl Pts',(43.9017875351293,22.43998996593,32.2234661770043));
#60671=CARTESIAN_POINT('Ctrl Pts',(43.9138558645572,22.4397775340047,32.193121110443));
#60672=CARTESIAN_POINT('Ctrl Pts',(43.9259526178902,22.4361921891614,32.1628560538943));
#60673=CARTESIAN_POINT('Ctrl Pts',(43.9378427069995,22.4292470492783,32.1332458643287));
#60674=CARTESIAN_POINT('Ctrl Pts',(43.9496295400103,22.422362222488,32.103892816036));
#60675=CARTESIAN_POINT('Ctrl Pts',(43.9611780430457,22.4121959369307,32.0752708280668));
#60676=CARTESIAN_POINT('Ctrl Pts',(43.9722455966321,22.3988248545246,32.0479521273707));
#60677=CARTESIAN_POINT('Ctrl Pts',(43.9820721961622,22.3869530103033,32.0236965473703));
#60678=CARTESIAN_POINT('Ctrl Pts',(43.9914607629777,22.3726225438755,32.0006045298457));
#60679=CARTESIAN_POINT('Ctrl Pts',(44.0002489315775,22.3559751421724,31.9790634597103));
#60680=CARTESIAN_POINT('Ctrl Pts',(44.0081171229226,22.3410704506532,31.9597773866587));
#60681=CARTESIAN_POINT('Ctrl Pts',(44.0155043707224,22.3243072942834,31.9417342092237));
#60682=CARTESIAN_POINT('Ctrl Pts',(44.0222720478219,22.3058052900935,31.9252340460289));
#60683=CARTESIAN_POINT('Ctrl Pts',(44.029760827937,22.2853318781633,31.9069757733286));
#60684=CARTESIAN_POINT('Ctrl Pts',(44.0364152831142,22.262937970116,31.8907942319792));
#60685=CARTESIAN_POINT('Ctrl Pts',(44.0420970014355,22.2389226632129,31.8770079892748));
#60686=CARTESIAN_POINT('Ctrl Pts',(44.0464641694145,22.2204636560288,31.8664113996019));
#60687=CARTESIAN_POINT('Ctrl Pts',(44.0502563764082,22.2010464082957,31.8572302202428));
#60688=CARTESIAN_POINT('Ctrl Pts',(44.0534015865836,22.180824146808,31.8496182972998));
#60689=CARTESIAN_POINT('Ctrl Pts',(44.0584453970152,22.1483947548904,31.8374114512694));
#60690=CARTESIAN_POINT('Ctrl Pts',(44.0617407660415,22.1144500496243,31.8294519002684));
#60691=CARTESIAN_POINT('Ctrl Pts',(44.0631761028331,22.07983124376,31.8259877017421));
#60692=CARTESIAN_POINT('Ctrl Pts',(44.0637232166716,22.0666354364251,31.824667237469));
#60693=CARTESIAN_POINT('Ctrl Pts',(44.064,22.0533419794353,31.824));
#60694=CARTESIAN_POINT('Ctrl Pts',(44.064,22.04,31.824));
#60695=CARTESIAN_POINT('Origin',(44.064,22.04,37.944));
#60696=CARTESIAN_POINT('Origin',(44.064,22.44,37.944));
#60697=CARTESIAN_POINT('Origin',(33.864,22.44,33.456));
#60698=CARTESIAN_POINT('',(29.376,22.44,42.424));
#60699=CARTESIAN_POINT('Origin',(29.376,22.44,38.352));
#60700=CARTESIAN_POINT('',(28.152,22.44,31.46));
#60701=CARTESIAN_POINT('Origin',(28.152,22.44,28.56));
#60702=CARTESIAN_POINT('',(44.064,22.44,40.792));
#60703=CARTESIAN_POINT('Origin',(44.064,22.44,37.944));
#60704=CARTESIAN_POINT('Origin',(29.376,21.1264,38.352));
#60705=CARTESIAN_POINT('',(29.376,20.7264,44.072));
#60706=CARTESIAN_POINT('Origin',(29.376,20.7264,38.352));
#60707=CARTESIAN_POINT('',(29.376,21.1264,44.472));
#60708=CARTESIAN_POINT('Origin',(29.376,21.1264,44.072));
#60709=CARTESIAN_POINT('',(23.256,21.1264,38.352));
#60710=CARTESIAN_POINT('Origin',(29.376,21.1264,38.352));
#60711=CARTESIAN_POINT('Origin',(29.376,21.1264,38.352));
#60712=CARTESIAN_POINT('Origin',(29.376,20.7264,38.352));
#60713=CARTESIAN_POINT('',(29.376,20.7264,34.28));
#60714=CARTESIAN_POINT('Origin',(29.376,20.7264,38.352));
#60715=CARTESIAN_POINT('Origin',(29.376,21.216,38.352));
#60716=CARTESIAN_POINT('',(23.256,21.216,38.352));
#60717=CARTESIAN_POINT('',(23.256,21.216,38.352));
#60718=CARTESIAN_POINT('Origin',(29.376,21.216,38.352));
#60719=CARTESIAN_POINT('Origin',(29.376,21.1264,38.352));
#60720=CARTESIAN_POINT('',(29.376,21.1264,34.68));
#60721=CARTESIAN_POINT('Origin',(29.376,21.1264,34.28));
#60722=CARTESIAN_POINT('',(25.704,21.1264,38.352));
#60723=CARTESIAN_POINT('Origin',(29.376,21.1264,38.352));
#60724=CARTESIAN_POINT('Origin',(29.376,21.1264,38.352));
#60725=CARTESIAN_POINT('Origin',(29.376,20.7264,38.352));
#60726=CARTESIAN_POINT('',(25.704,22.04,38.352));
#60727=CARTESIAN_POINT('',(25.704,20.7264,38.352));
#60728=CARTESIAN_POINT('',(29.376,22.04,42.024));
#60729=CARTESIAN_POINT('Origin',(29.376,22.04,38.352));
#60730=CARTESIAN_POINT('Origin',(29.376,22.04,38.352));
#60731=CARTESIAN_POINT('Origin',(29.376,22.04,38.352));
#60732=CARTESIAN_POINT('Origin',(29.376,22.04,42.424));
#60733=CARTESIAN_POINT('Origin',(-29.376,21.1264,38.352));
#60734=CARTESIAN_POINT('',(-29.376,21.1264,34.68));
#60735=CARTESIAN_POINT('Origin',(-29.376,21.1264,34.28));
#60736=CARTESIAN_POINT('',(-33.048,21.1264,38.352));
#60737=CARTESIAN_POINT('Origin',(-29.376,21.1264,38.352));
#60738=CARTESIAN_POINT('Origin',(-29.376,21.1264,38.352));
#60739=CARTESIAN_POINT('Origin',(-29.376,20.7264,38.352));
#60740=CARTESIAN_POINT('',(-33.048,22.04,38.352));
#60741=CARTESIAN_POINT('',(-33.048,20.7264,38.352));
#60742=CARTESIAN_POINT('',(-29.376,22.04,42.024));
#60743=CARTESIAN_POINT('Origin',(-29.376,22.04,38.352));
#60744=CARTESIAN_POINT('Origin',(-29.376,22.04,38.352));
#60745=CARTESIAN_POINT('Origin',(-29.376,22.04,38.352));
#60746=CARTESIAN_POINT('Origin',(-29.376,22.04,42.424));
#60747=CARTESIAN_POINT('Origin',(44.064,22.04,37.944));
#60748=CARTESIAN_POINT('',(44.064,22.04,40.392));
#60749=CARTESIAN_POINT('Origin',(44.064,22.04,40.792));
#60750=CARTESIAN_POINT('',(41.616,22.04,37.944));
#60751=CARTESIAN_POINT('Origin',(44.064,22.04,37.944));
#60752=CARTESIAN_POINT('Origin',(44.064,22.04,37.944));
#60753=CARTESIAN_POINT('Origin',(44.064,20.7264,37.944));
#60754=CARTESIAN_POINT('',(44.064,21.616,35.496));
#60755=CARTESIAN_POINT('',(41.616,21.616,37.944));
#60756=CARTESIAN_POINT('Origin',(44.064,21.616,37.944));
#60757=CARTESIAN_POINT('Origin',(44.064,21.616,37.944));
#60758=CARTESIAN_POINT('',(41.616,20.7264,37.944));
#60759=CARTESIAN_POINT('Origin',(44.064,21.616,37.944));
#60760=CARTESIAN_POINT('',(44.064,21.216,35.096));
#60761=CARTESIAN_POINT('Origin',(44.064,21.216,37.944));
#60762=CARTESIAN_POINT('Origin',(44.064,21.616,35.096));
#60763=CARTESIAN_POINT('Origin',(33.864,21.216,33.456));
#60764=CARTESIAN_POINT('',(28.152,21.216,25.66));
#60765=CARTESIAN_POINT('Origin',(28.152,21.216,28.56));
#60766=CARTESIAN_POINT('Origin',(-28.152,22.04,28.56));
#60767=CARTESIAN_POINT('',(-28.152,22.04,31.06));
#60768=CARTESIAN_POINT('Origin',(-28.152,22.04,31.46));
#60769=CARTESIAN_POINT('',(-30.652,22.04,28.56));
#60770=CARTESIAN_POINT('Origin',(-28.152,22.04,28.56));
#60771=CARTESIAN_POINT('Origin',(-28.152,22.04,28.56));
#60772=CARTESIAN_POINT('Origin',(-28.152,20.7264,28.56));
#60773=CARTESIAN_POINT('',(-28.152,21.616,26.06));
#60774=CARTESIAN_POINT('',(-30.652,21.616,28.56));
#60775=CARTESIAN_POINT('Origin',(-28.152,21.616,28.56));
#60776=CARTESIAN_POINT('Origin',(-28.152,21.616,28.56));
#60777=CARTESIAN_POINT('',(-30.652,20.7264,28.56));
#60778=CARTESIAN_POINT('Origin',(-28.152,21.616,28.56));
#60779=CARTESIAN_POINT('',(-28.152,21.216,25.66));
#60780=CARTESIAN_POINT('Origin',(-28.152,21.216,28.56));
#60781=CARTESIAN_POINT('Origin',(-28.152,21.616,25.66));
#60782=CARTESIAN_POINT('Origin',(-33.864,21.216,33.456));
#60783=CARTESIAN_POINT('',(-17.544,21.216,32.64));
#60784=CARTESIAN_POINT('',(-44.064,21.216,35.096));
#60785=CARTESIAN_POINT('Origin',(-44.064,21.216,37.944));
#60786=CARTESIAN_POINT('Origin',(28.152,22.04,28.56));
#60787=CARTESIAN_POINT('',(28.152,22.04,31.06));
#60788=CARTESIAN_POINT('Origin',(28.152,22.04,31.46));
#60789=CARTESIAN_POINT('',(25.652,22.04,28.56));
#60790=CARTESIAN_POINT('Origin',(28.152,22.04,28.56));
#60791=CARTESIAN_POINT('Origin',(28.152,22.04,28.56));
#60792=CARTESIAN_POINT('Origin',(28.152,20.7264,28.56));
#60793=CARTESIAN_POINT('',(28.152,21.616,26.06));
#60794=CARTESIAN_POINT('',(25.652,21.616,28.56));
#60795=CARTESIAN_POINT('Origin',(28.152,21.616,28.56));
#60796=CARTESIAN_POINT('Origin',(28.152,21.616,28.56));
#60797=CARTESIAN_POINT('',(25.652,20.7264,28.56));
#60798=CARTESIAN_POINT('Origin',(28.152,21.616,28.56));
#60799=CARTESIAN_POINT('Origin',(28.152,21.616,25.66));
#60800=CARTESIAN_POINT('Origin',(-44.064,22.04,37.944));
#60801=CARTESIAN_POINT('',(-44.064,22.04,40.392));
#60802=CARTESIAN_POINT('Origin',(-44.064,22.04,40.792));
#60803=CARTESIAN_POINT('',(-46.512,22.04,37.944));
#60804=CARTESIAN_POINT('Origin',(-44.064,22.04,37.944));
#60805=CARTESIAN_POINT('Origin',(-44.064,22.04,37.944));
#60806=CARTESIAN_POINT('Origin',(-44.064,20.7264,37.944));
#60807=CARTESIAN_POINT('',(-44.064,21.616,35.496));
#60808=CARTESIAN_POINT('',(-46.512,21.616,37.944));
#60809=CARTESIAN_POINT('Origin',(-44.064,21.616,37.944));
#60810=CARTESIAN_POINT('Origin',(-44.064,21.616,37.944));
#60811=CARTESIAN_POINT('',(-46.512,20.7264,37.944));
#60812=CARTESIAN_POINT('Origin',(-44.064,21.616,37.944));
#60813=CARTESIAN_POINT('Origin',(-44.064,21.616,35.096));
#60814=CARTESIAN_POINT('Origin',(6.528,2.048,42.432));
#60815=CARTESIAN_POINT('',(6.528,2.448,44.132));
#60816=CARTESIAN_POINT('Origin',(6.528,2.448,42.432));
#60817=CARTESIAN_POINT('',(6.528,2.048,43.732));
#60818=CARTESIAN_POINT('Origin',(6.528,2.048,44.132));
#60819=CARTESIAN_POINT('',(5.228,2.048,42.432));
#60820=CARTESIAN_POINT('Origin',(6.528,2.048,42.432));
#60821=CARTESIAN_POINT('Origin',(6.528,2.048,42.432));
#60822=CARTESIAN_POINT('Origin',(6.528,1.224,42.432));
#60823=CARTESIAN_POINT('',(6.528,1.624,41.132));
#60824=CARTESIAN_POINT('',(5.228,1.624,42.432));
#60825=CARTESIAN_POINT('Origin',(6.528,1.624,42.432));
#60826=CARTESIAN_POINT('Origin',(6.528,1.624,42.432));
#60827=CARTESIAN_POINT('',(5.228,1.224,42.432));
#60828=CARTESIAN_POINT('Origin',(0.,2.448,39.576));
#60829=CARTESIAN_POINT('',(-18.2023145750508,2.448,35.904));
#60830=CARTESIAN_POINT('',(-16.1543145750508,2.448,33.856));
#60831=CARTESIAN_POINT('',(-13.4871572875254,2.448,31.1888427124746));
#60832=CARTESIAN_POINT('',(-8.772,2.448,35.904));
#60833=CARTESIAN_POINT('',(-9.384,2.448,45.296));
#60834=CARTESIAN_POINT('',(16.1543145750508,2.448,33.856));
#60835=CARTESIAN_POINT('',(14.7111572875254,2.448,32.4128427124746));
#60836=CARTESIAN_POINT('',(8.16,2.448,33.856));
#60837=CARTESIAN_POINT('',(-6.528,2.448,44.132));
#60838=CARTESIAN_POINT('Origin',(-6.528,2.448,42.432));
#60839=CARTESIAN_POINT('',(-15.904,2.448,35.504));
#60840=CARTESIAN_POINT('',(-15.904,2.448,41.608));
#60841=CARTESIAN_POINT('',(-15.904,2.448,37.74));
#60842=CARTESIAN_POINT('',(-12.656,2.448,35.504));
#60843=CARTESIAN_POINT('',(-6.528,2.448,35.504));
#60844=CARTESIAN_POINT('',(-12.656,2.448,41.608));
#60845=CARTESIAN_POINT('',(-12.656,2.448,40.392));
#60846=CARTESIAN_POINT('',(-7.752,2.448,41.608));
#60847=CARTESIAN_POINT('',(12.656,2.448,35.504));
#60848=CARTESIAN_POINT('',(12.656,2.448,41.608));
#60849=CARTESIAN_POINT('',(12.656,2.448,37.74));
#60850=CARTESIAN_POINT('',(15.904,2.448,35.504));
#60851=CARTESIAN_POINT('',(7.752,2.448,35.504));
#60852=CARTESIAN_POINT('',(15.904,2.448,41.608));
#60853=CARTESIAN_POINT('',(15.904,2.448,40.392));
#60854=CARTESIAN_POINT('',(6.528,2.448,41.608));
#60855=CARTESIAN_POINT('Origin',(-13.4871572875254,2.048,31.1888427124746));
#60856=CARTESIAN_POINT('',(-16.32,2.048,33.456));
#60857=CARTESIAN_POINT('',(-13.77,2.048,30.906));
#60858=CARTESIAN_POINT('Origin',(-18.2718797924421,2.048,35.9735652173913));
#60859=CARTESIAN_POINT('Origin',(-16.1543145750508,2.048,33.856));
#60860=CARTESIAN_POINT('Origin',(8.16,2.048,33.856));
#60861=CARTESIAN_POINT('',(16.32,2.048,33.456));
#60862=CARTESIAN_POINT('Origin',(16.1543145750508,2.048,33.856));
#60863=CARTESIAN_POINT('',(8.16,2.048,33.456));
#60864=CARTESIAN_POINT('Origin',(14.7111572875254,2.048,32.4128427124746));
#60865=CARTESIAN_POINT('',(14.994,2.048,32.13));
#60866=CARTESIAN_POINT('Origin',(-16.32,1.224,33.456));
#60867=CARTESIAN_POINT('',(-16.32,1.624,33.456));
#60868=CARTESIAN_POINT('',(-16.32,1.224,33.456));
#60869=CARTESIAN_POINT('',(-13.77,1.624,30.906));
#60870=CARTESIAN_POINT('Origin',(16.32,1.224,33.456));
#60871=CARTESIAN_POINT('',(16.32,1.624,33.456));
#60872=CARTESIAN_POINT('',(16.32,1.224,33.456));
#60873=CARTESIAN_POINT('',(8.16,1.624,33.456));
#60874=CARTESIAN_POINT('Origin',(18.768,1.224,35.904));
#60875=CARTESIAN_POINT('',(14.994,1.624,32.13));
#60876=CARTESIAN_POINT('Origin',(-9.384,2.048,45.296));
#60877=CARTESIAN_POINT('Origin',(6.528,1.624,42.432));
#60878=CARTESIAN_POINT('',(6.528,1.224,40.732));
#60879=CARTESIAN_POINT('Origin',(6.528,1.224,42.432));
#60880=CARTESIAN_POINT('Origin',(6.528,1.624,40.732));
#60881=CARTESIAN_POINT('Origin',(0.,1.224,39.576));
#60882=CARTESIAN_POINT('',(-16.1543145750508,1.224,33.856));
#60883=CARTESIAN_POINT('',(-13.4871572875254,1.224,31.1888427124746));
#60884=CARTESIAN_POINT('',(16.1543145750508,1.224,33.856));
#60885=CARTESIAN_POINT('',(8.16,1.224,33.856));
#60886=CARTESIAN_POINT('',(18.368,1.224,36.0696854249492));
#60887=CARTESIAN_POINT('',(14.7111572875254,1.224,32.4128427124746));
#60888=CARTESIAN_POINT('',(18.368,1.224,42.636));
#60889=CARTESIAN_POINT('',(-15.904,1.224,41.208));
#60890=CARTESIAN_POINT('',(-14.8512,1.224,41.208));
#60891=CARTESIAN_POINT('',(-7.752,1.224,41.208));
#60892=CARTESIAN_POINT('',(-14.8512,1.224,42.432));
#60893=CARTESIAN_POINT('',(-14.8512,1.224,41.004));
#60894=CARTESIAN_POINT('',(-13.7088,1.224,42.432));
#60895=CARTESIAN_POINT('',(-6.8544,1.224,42.432));
#60896=CARTESIAN_POINT('',(-13.7088,1.224,41.208));
#60897=CARTESIAN_POINT('',(-13.7088,1.224,38.2296));
#60898=CARTESIAN_POINT('',(-12.656,1.224,41.208));
#60899=CARTESIAN_POINT('',(-7.752,1.224,41.208));
#60900=CARTESIAN_POINT('',(-12.656,1.224,35.504));
#60901=CARTESIAN_POINT('',(-12.656,1.224,40.392));
#60902=CARTESIAN_POINT('',(-15.904,1.224,35.504));
#60903=CARTESIAN_POINT('',(-6.528,1.224,35.504));
#60904=CARTESIAN_POINT('',(-15.904,1.224,37.74));
#60905=CARTESIAN_POINT('',(12.656,1.224,41.208));
#60906=CARTESIAN_POINT('',(13.7088,1.224,41.208));
#60907=CARTESIAN_POINT('',(6.528,1.224,41.208));
#60908=CARTESIAN_POINT('',(13.7088,1.224,42.432));
#60909=CARTESIAN_POINT('',(13.7088,1.224,41.004));
#60910=CARTESIAN_POINT('',(14.8512,1.224,42.432));
#60911=CARTESIAN_POINT('',(7.4256,1.224,42.432));
#60912=CARTESIAN_POINT('',(14.8512,1.224,41.208));
#60913=CARTESIAN_POINT('',(14.8512,1.224,38.2296));
#60914=CARTESIAN_POINT('',(15.904,1.224,41.208));
#60915=CARTESIAN_POINT('',(6.528,1.224,41.208));
#60916=CARTESIAN_POINT('',(15.904,1.224,35.504));
#60917=CARTESIAN_POINT('',(15.904,1.224,40.392));
#60918=CARTESIAN_POINT('',(12.656,1.224,35.504));
#60919=CARTESIAN_POINT('',(7.752,1.224,35.504));
#60920=CARTESIAN_POINT('',(12.656,1.224,37.74));
#60921=CARTESIAN_POINT('',(-6.528,1.224,40.732));
#60922=CARTESIAN_POINT('Origin',(-6.528,1.224,42.432));
#60923=CARTESIAN_POINT('Origin',(8.16,1.624,33.856));
#60924=CARTESIAN_POINT('Origin',(-16.1543145750508,1.624,33.856));
#60925=CARTESIAN_POINT('Origin',(16.1543145750508,1.624,33.856));
#60926=CARTESIAN_POINT('Origin',(-13.4871572875254,1.624,31.1888427124746));
#60927=CARTESIAN_POINT('Origin',(18.368,1.624,42.636));
#60928=CARTESIAN_POINT('Origin',(18.368,1.624,36.0696854249492));
#60929=CARTESIAN_POINT('Origin',(14.7111572875254,1.624,32.4128427124746));
#60930=CARTESIAN_POINT('Origin',(-6.528,1.624,42.432));
#60931=CARTESIAN_POINT('',(-6.528,1.624,41.132));
#60932=CARTESIAN_POINT('Origin',(-6.528,1.624,40.732));
#60933=CARTESIAN_POINT('',(-7.828,1.624,42.432));
#60934=CARTESIAN_POINT('Origin',(-6.528,1.624,42.432));
#60935=CARTESIAN_POINT('Origin',(-6.528,1.624,42.432));
#60936=CARTESIAN_POINT('Origin',(-6.528,1.224,42.432));
#60937=CARTESIAN_POINT('',(-7.828,2.048,42.432));
#60938=CARTESIAN_POINT('',(-7.828,1.224,42.432));
#60939=CARTESIAN_POINT('',(-6.528,2.048,43.732));
#60940=CARTESIAN_POINT('Origin',(-6.528,2.048,42.432));
#60941=CARTESIAN_POINT('Origin',(-6.528,2.048,42.432));
#60942=CARTESIAN_POINT('Origin',(-6.528,2.048,42.432));
#60943=CARTESIAN_POINT('Origin',(-6.528,2.048,44.132));
#60944=CARTESIAN_POINT('Origin',(12.656,2.048,37.74));
#60945=CARTESIAN_POINT('',(13.056,2.048,41.208));
#60946=CARTESIAN_POINT('Origin',(12.656,2.048,41.608));
#60947=CARTESIAN_POINT('',(13.056,2.048,35.904));
#60948=CARTESIAN_POINT('',(13.056,2.048,37.74));
#60949=CARTESIAN_POINT('Origin',(12.656,2.048,35.504));
#60950=CARTESIAN_POINT('Origin',(6.528,2.048,41.608));
#60951=CARTESIAN_POINT('',(15.504,2.048,41.208));
#60952=CARTESIAN_POINT('',(6.528,2.048,41.208));
#60953=CARTESIAN_POINT('Origin',(15.904,2.048,41.608));
#60954=CARTESIAN_POINT('Origin',(7.752,2.048,35.504));
#60955=CARTESIAN_POINT('',(15.504,2.048,35.904));
#60956=CARTESIAN_POINT('',(7.752,2.048,35.904));
#60957=CARTESIAN_POINT('Origin',(15.904,2.048,35.504));
#60958=CARTESIAN_POINT('Origin',(15.904,2.048,40.392));
#60959=CARTESIAN_POINT('',(15.504,2.048,40.392));
#60960=CARTESIAN_POINT('Origin',(15.504,1.224,35.904));
#60961=CARTESIAN_POINT('',(13.056,1.624,35.904));
#60962=CARTESIAN_POINT('',(13.056,1.224,35.904));
#60963=CARTESIAN_POINT('',(15.504,1.624,35.904));
#60964=CARTESIAN_POINT('',(7.752,1.624,35.904));
#60965=CARTESIAN_POINT('',(15.504,1.224,35.904));
#60966=CARTESIAN_POINT('Origin',(13.056,1.224,35.904));
#60967=CARTESIAN_POINT('',(13.056,1.624,41.208));
#60968=CARTESIAN_POINT('',(13.056,1.224,41.208));
#60969=CARTESIAN_POINT('',(13.056,1.624,37.74));
#60970=CARTESIAN_POINT('Origin',(12.656,1.624,37.74));
#60971=CARTESIAN_POINT('Origin',(12.656,1.624,41.208));
#60972=CARTESIAN_POINT('Origin',(12.656,1.624,35.504));
#60973=CARTESIAN_POINT('Origin',(7.752,1.624,35.504));
#60974=CARTESIAN_POINT('Origin',(15.904,1.624,35.504));
#60975=CARTESIAN_POINT('Origin',(15.904,1.624,40.392));
#60976=CARTESIAN_POINT('',(15.504,1.624,41.208));
#60977=CARTESIAN_POINT('Origin',(15.904,1.624,41.208));
#60978=CARTESIAN_POINT('',(15.504,1.624,40.392));
#60979=CARTESIAN_POINT('Origin',(15.504,1.224,41.208));
#60980=CARTESIAN_POINT('',(15.504,1.224,41.208));
#60981=CARTESIAN_POINT('Origin',(-15.904,2.048,37.74));
#60982=CARTESIAN_POINT('',(-15.504,2.048,41.208));
#60983=CARTESIAN_POINT('Origin',(-15.904,2.048,41.608));
#60984=CARTESIAN_POINT('',(-15.504,2.048,35.904));
#60985=CARTESIAN_POINT('',(-15.504,2.048,37.74));
#60986=CARTESIAN_POINT('Origin',(-15.904,2.048,35.504));
#60987=CARTESIAN_POINT('Origin',(-7.752,2.048,41.608));
#60988=CARTESIAN_POINT('',(-13.056,2.048,41.208));
#60989=CARTESIAN_POINT('',(-7.752,2.048,41.208));
#60990=CARTESIAN_POINT('Origin',(-12.656,2.048,41.608));
#60991=CARTESIAN_POINT('Origin',(-6.528,2.048,35.504));
#60992=CARTESIAN_POINT('',(-13.056,2.048,35.904));
#60993=CARTESIAN_POINT('',(-6.528,2.048,35.904));
#60994=CARTESIAN_POINT('Origin',(-12.656,2.048,35.504));
#60995=CARTESIAN_POINT('Origin',(-12.656,2.048,40.392));
#60996=CARTESIAN_POINT('',(-13.056,2.048,40.392));
#60997=CARTESIAN_POINT('Origin',(-13.056,1.224,35.904));
#60998=CARTESIAN_POINT('',(-15.504,1.624,35.904));
#60999=CARTESIAN_POINT('',(-15.504,1.224,35.904));
#61000=CARTESIAN_POINT('',(-13.056,1.624,35.904));
#61001=CARTESIAN_POINT('',(-6.528,1.624,35.904));
#61002=CARTESIAN_POINT('',(-13.056,1.224,35.904));
#61003=CARTESIAN_POINT('Origin',(-15.504,1.224,35.904));
#61004=CARTESIAN_POINT('',(-15.504,1.624,41.208));
#61005=CARTESIAN_POINT('',(-15.504,1.224,41.208));
#61006=CARTESIAN_POINT('',(-15.504,1.624,37.74));
#61007=CARTESIAN_POINT('Origin',(-15.904,1.624,37.74));
#61008=CARTESIAN_POINT('Origin',(-15.904,1.624,41.208));
#61009=CARTESIAN_POINT('Origin',(-15.904,1.624,35.504));
#61010=CARTESIAN_POINT('Origin',(-6.528,1.624,35.504));
#61011=CARTESIAN_POINT('Origin',(-12.656,1.624,35.504));
#61012=CARTESIAN_POINT('Origin',(-12.656,1.624,40.392));
#61013=CARTESIAN_POINT('',(-13.056,1.624,41.208));
#61014=CARTESIAN_POINT('Origin',(-12.656,1.624,41.208));
#61015=CARTESIAN_POINT('',(-13.056,1.624,40.392));
#61016=CARTESIAN_POINT('Origin',(-13.056,1.224,41.208));
#61017=CARTESIAN_POINT('',(-13.056,1.224,41.208));
#61018=CARTESIAN_POINT('Origin',(14.1088,0.8896,41.0448));
#61019=CARTESIAN_POINT('',(13.7101470682411,0.8568,36.8832));
#61020=CARTESIAN_POINT('',(14.1088,0.4896,36.8832));
#61021=CARTESIAN_POINT('Origin',(14.1088,0.8896,36.8832));
#61022=CARTESIAN_POINT('',(14.1088,0.4896,42.432));
#61023=CARTESIAN_POINT('',(14.1088,0.4896,41.0448));
#61024=CARTESIAN_POINT('',(13.7088,0.8896,42.432));
#61025=CARTESIAN_POINT('Origin',(14.1088,0.8896,42.432));
#61026=CARTESIAN_POINT('',(13.7088,0.8896,41.208));
#61027=CARTESIAN_POINT('',(13.7088,0.8896,41.0448));
#61028=CARTESIAN_POINT('',(13.7101470682411,0.8568,41.208));
#61029=CARTESIAN_POINT('Origin',(14.1088,0.8896,41.208));
#61030=CARTESIAN_POINT('',(13.7101470682411,0.8568,41.0448));
#61031=CARTESIAN_POINT('Origin',(14.1088,0.824,41.0448));
#61032=CARTESIAN_POINT('',(14.1088,1.224,41.208));
#61033=CARTESIAN_POINT('Origin',(14.1088,0.824,41.208));
#61034=CARTESIAN_POINT('',(14.1088,1.224,36.8832));
#61035=CARTESIAN_POINT('',(14.1088,1.224,41.0448));
#61036=CARTESIAN_POINT('Origin',(14.1088,0.824,36.8832));
#61037=CARTESIAN_POINT('Origin',(13.056,1.224,41.208));
#61038=CARTESIAN_POINT('',(14.8512,0.8896,41.208));
#61039=CARTESIAN_POINT('',(14.8512,1.224,41.208));
#61040=CARTESIAN_POINT('',(14.8498529317589,0.8568,41.208));
#61041=CARTESIAN_POINT('Origin',(14.4512,0.8896,41.208));
#61042=CARTESIAN_POINT('',(14.4512,1.224,41.208));
#61043=CARTESIAN_POINT('Origin',(14.4512,0.824,41.208));
#61044=CARTESIAN_POINT('',(6.528,1.224,41.208));
#61045=CARTESIAN_POINT('',(13.7088,1.224,41.208));
#61046=CARTESIAN_POINT('Origin',(13.7088,1.224,42.432));
#61047=CARTESIAN_POINT('',(13.7088,1.224,42.432));
#61048=CARTESIAN_POINT('Origin',(13.7088,1.224,36.8832));
#61049=CARTESIAN_POINT('',(14.4512,1.224,36.8832));
#61050=CARTESIAN_POINT('',(13.7088,1.224,36.8832));
#61051=CARTESIAN_POINT('',(14.8498529317589,0.8568,36.8832));
#61052=CARTESIAN_POINT('Origin',(14.4512,0.824,36.8832));
#61053=CARTESIAN_POINT('',(14.4512,0.4896,36.8832));
#61054=CARTESIAN_POINT('Origin',(14.4512,0.8896,36.8832));
#61055=CARTESIAN_POINT('',(13.7088,0.4896,36.8832));
#61056=CARTESIAN_POINT('Origin',(14.4512,0.8896,38.2704));
#61057=CARTESIAN_POINT('',(14.8512,0.8896,42.432));
#61058=CARTESIAN_POINT('',(14.4512,0.4896,42.432));
#61059=CARTESIAN_POINT('Origin',(14.4512,0.8896,42.432));
#61060=CARTESIAN_POINT('',(14.4512,0.4896,38.2704));
#61061=CARTESIAN_POINT('',(14.8498529317589,0.8568,38.2704));
#61062=CARTESIAN_POINT('',(14.8512,0.8896,38.2704));
#61063=CARTESIAN_POINT('Origin',(14.28,0.4896,39.6576));
#61064=CARTESIAN_POINT('',(14.8512,0.4896,42.432));
#61065=CARTESIAN_POINT('Origin',(14.8512,1.224,42.432));
#61066=CARTESIAN_POINT('',(14.8512,1.224,42.432));
#61067=CARTESIAN_POINT('Origin',(14.8512,1.224,36.8832));
#61068=CARTESIAN_POINT('Origin',(14.4512,0.824,38.2704));
#61069=CARTESIAN_POINT('',(14.4512,1.224,38.2704));
#61070=CARTESIAN_POINT('Origin',(-14.4512,0.8896,41.0448));
#61071=CARTESIAN_POINT('',(-14.8498529317589,0.8568,36.8832));
#61072=CARTESIAN_POINT('',(-14.4512,0.4896,36.8832));
#61073=CARTESIAN_POINT('Origin',(-14.4512,0.8896,36.8832));
#61074=CARTESIAN_POINT('',(-14.4512,0.4896,42.432));
#61075=CARTESIAN_POINT('',(-14.4512,0.4896,41.0448));
#61076=CARTESIAN_POINT('',(-14.8512,0.8896,42.432));
#61077=CARTESIAN_POINT('Origin',(-14.4512,0.8896,42.432));
#61078=CARTESIAN_POINT('',(-14.8512,0.8896,41.208));
#61079=CARTESIAN_POINT('',(-14.8512,0.8896,41.0448));
#61080=CARTESIAN_POINT('',(-14.8498529317589,0.8568,41.208));
#61081=CARTESIAN_POINT('Origin',(-14.4512,0.8896,41.208));
#61082=CARTESIAN_POINT('',(-14.8498529317589,0.8568,41.0448));
#61083=CARTESIAN_POINT('Origin',(-14.4512,0.824,41.0448));
#61084=CARTESIAN_POINT('',(-14.4512,1.224,41.208));
#61085=CARTESIAN_POINT('Origin',(-14.4512,0.824,41.208));
#61086=CARTESIAN_POINT('',(-14.4512,1.224,36.8832));
#61087=CARTESIAN_POINT('',(-14.4512,1.224,41.0448));
#61088=CARTESIAN_POINT('Origin',(-14.4512,0.824,36.8832));
#61089=CARTESIAN_POINT('Origin',(-15.504,1.224,41.208));
#61090=CARTESIAN_POINT('',(-13.7088,0.8896,41.208));
#61091=CARTESIAN_POINT('',(-13.7088,1.224,41.208));
#61092=CARTESIAN_POINT('',(-13.7101470682411,0.8568,41.208));
#61093=CARTESIAN_POINT('Origin',(-14.1088,0.8896,41.208));
#61094=CARTESIAN_POINT('',(-14.1088,1.224,41.208));
#61095=CARTESIAN_POINT('Origin',(-14.1088,0.824,41.208));
#61096=CARTESIAN_POINT('',(-7.752,1.224,41.208));
#61097=CARTESIAN_POINT('',(-14.8512,1.224,41.208));
#61098=CARTESIAN_POINT('Origin',(-14.8512,1.224,42.432));
#61099=CARTESIAN_POINT('',(-14.8512,1.224,42.432));
#61100=CARTESIAN_POINT('Origin',(-14.8512,1.224,36.8832));
#61101=CARTESIAN_POINT('',(-14.1088,1.224,36.8832));
#61102=CARTESIAN_POINT('',(-14.8512,1.224,36.8832));
#61103=CARTESIAN_POINT('',(-13.7101470682411,0.8568,36.8832));
#61104=CARTESIAN_POINT('Origin',(-14.1088,0.824,36.8832));
#61105=CARTESIAN_POINT('',(-14.1088,0.4896,36.8832));
#61106=CARTESIAN_POINT('Origin',(-14.1088,0.8896,36.8832));
#61107=CARTESIAN_POINT('',(-14.8512,0.4896,36.8832));
#61108=CARTESIAN_POINT('Origin',(-14.1088,0.8896,38.2704));
#61109=CARTESIAN_POINT('',(-13.7088,0.8896,42.432));
#61110=CARTESIAN_POINT('',(-14.1088,0.4896,42.432));
#61111=CARTESIAN_POINT('Origin',(-14.1088,0.8896,42.432));
#61112=CARTESIAN_POINT('',(-14.1088,0.4896,38.2704));
#61113=CARTESIAN_POINT('',(-13.7101470682411,0.8568,38.2704));
#61114=CARTESIAN_POINT('',(-13.7088,0.8896,38.2704));
#61115=CARTESIAN_POINT('Origin',(-14.28,0.4896,39.6576));
#61116=CARTESIAN_POINT('',(-13.7088,0.4896,42.432));
#61117=CARTESIAN_POINT('Origin',(-13.7088,1.224,42.432));
#61118=CARTESIAN_POINT('',(-13.7088,1.224,42.432));
#61119=CARTESIAN_POINT('Origin',(-13.7088,1.224,36.8832));
#61120=CARTESIAN_POINT('Origin',(-14.1088,0.824,38.2704));
#61121=CARTESIAN_POINT('',(-14.1088,1.224,38.2704));
#61122=CARTESIAN_POINT('Origin',(-14.28,1.224,39.6576));
#61123=CARTESIAN_POINT('Origin',(14.28,1.224,39.6576));
#61124=CARTESIAN_POINT('Origin',(-17.544,8.976,41.616));
#61125=CARTESIAN_POINT('Origin',(-17.544,21.216,32.64));
#61126=CARTESIAN_POINT('Origin',(17.544,8.976,38.76));
#61127=CARTESIAN_POINT('',(0.,0.,0.));
#61128=CARTESIAN_POINT('Origin',(16.744,21.232,44.896));
#61129=CARTESIAN_POINT('',(16.744,21.232,45.696));
#61130=CARTESIAN_POINT('',(16.744,22.032,44.896));
#61131=CARTESIAN_POINT('Origin',(16.744,21.232,44.896));
#61132=CARTESIAN_POINT('',(17.544,21.232,44.896));
#61133=CARTESIAN_POINT('Origin',(16.744,21.232,44.896));
#61134=CARTESIAN_POINT('Origin',(16.744,21.232,44.896));
#61135=CARTESIAN_POINT('Origin',(16.744,3.248,44.896));
#61136=CARTESIAN_POINT('',(16.744,3.248,45.696));
#61137=CARTESIAN_POINT('',(17.544,3.248,44.896));
#61138=CARTESIAN_POINT('Origin',(16.744,3.248,44.896));
#61139=CARTESIAN_POINT('',(16.744,2.448,44.896));
#61140=CARTESIAN_POINT('Origin',(16.744,3.248,44.896));
#61141=CARTESIAN_POINT('Origin',(16.744,3.248,44.896));
#61142=CARTESIAN_POINT('Origin',(-8.772,3.248,44.896));
#61143=CARTESIAN_POINT('',(4.35247056279534,3.248,45.696));
#61144=CARTESIAN_POINT('',(4.35247056279534,2.448,44.896));
#61145=CARTESIAN_POINT('Origin',(4.35247056279534,3.248,44.896));
#61146=CARTESIAN_POINT('',(-8.772,2.448,44.896));
#61147=CARTESIAN_POINT('',(-8.772,3.248,45.696));
#61148=CARTESIAN_POINT('Origin',(16.744,3.248,44.064));
#61149=CARTESIAN_POINT('',(16.744,2.448,39.968));
#61150=CARTESIAN_POINT('',(17.544,3.248,39.968));
#61151=CARTESIAN_POINT('Origin',(16.744,3.248,39.968));
#61152=CARTESIAN_POINT('',(17.544,3.248,44.064));
#61153=CARTESIAN_POINT('',(16.744,2.448,44.064));
#61154=CARTESIAN_POINT('Origin',(16.744,2.448,44.896));
#61155=CARTESIAN_POINT('',(16.744,2.448,45.696));
#61156=CARTESIAN_POINT('',(17.544,2.448,44.896));
#61157=CARTESIAN_POINT('Origin',(16.744,21.232,39.968));
#61158=CARTESIAN_POINT('',(17.544,21.232,39.968));
#61159=CARTESIAN_POINT('',(16.744,22.032,39.968));
#61160=CARTESIAN_POINT('Origin',(16.744,21.232,39.968));
#61161=CARTESIAN_POINT('',(16.744,21.232,39.168));
#61162=CARTESIAN_POINT('Origin',(16.744,21.232,39.968));
#61163=CARTESIAN_POINT('Origin',(16.744,21.232,39.968));
#61164=CARTESIAN_POINT('Origin',(16.744,2.448,39.968));
#61165=CARTESIAN_POINT('',(16.744,3.248,39.168));
#61166=CARTESIAN_POINT('Origin',(16.744,3.248,39.968));
#61167=CARTESIAN_POINT('',(16.744,2.448,39.168));
#61168=CARTESIAN_POINT('',(17.544,2.448,39.968));
#61169=CARTESIAN_POINT('Origin',(8.772,21.232,39.968));
#61170=CARTESIAN_POINT('',(13.056,22.032,39.968));
#61171=CARTESIAN_POINT('',(8.772,22.032,39.968));
#61172=CARTESIAN_POINT('',(12.256,21.232,39.168));
#61173=CARTESIAN_POINT('',(8.772,21.232,39.168));
#61174=CARTESIAN_POINT('Origin',(12.256,21.232,39.968));
#61175=CARTESIAN_POINT('Origin',(-8.772,21.232,44.896));
#61176=CARTESIAN_POINT('',(12.256,21.232,45.696));
#61177=CARTESIAN_POINT('',(-8.772,21.232,45.696));
#61178=CARTESIAN_POINT('',(13.056,22.032,44.896));
#61179=CARTESIAN_POINT('',(-8.772,22.032,44.896));
#61180=CARTESIAN_POINT('Origin',(12.256,21.232,44.896));
#61181=CARTESIAN_POINT('Origin',(12.256,29.392,39.968));
#61182=CARTESIAN_POINT('',(13.056,29.392,39.968));
#61183=CARTESIAN_POINT('',(12.256,30.192,39.968));
#61184=CARTESIAN_POINT('Origin',(12.256,29.392,39.968));
#61185=CARTESIAN_POINT('',(12.256,29.392,39.168));
#61186=CARTESIAN_POINT('Origin',(12.256,29.392,39.968));
#61187=CARTESIAN_POINT('Origin',(12.256,29.392,39.968));
#61188=CARTESIAN_POINT('Origin',(12.256,12.24,39.968));
#61189=CARTESIAN_POINT('',(12.256,12.24,39.168));
#61190=CARTESIAN_POINT('',(13.056,12.24,39.968));
#61191=CARTESIAN_POINT('Origin',(8.772,29.392,39.968));
#61192=CARTESIAN_POINT('',(-12.256,29.392,39.168));
#61193=CARTESIAN_POINT('',(-12.256,30.192,39.968));
#61194=CARTESIAN_POINT('Origin',(-12.256,29.392,39.968));
#61195=CARTESIAN_POINT('',(8.772,30.192,39.968));
#61196=CARTESIAN_POINT('',(8.772,29.392,39.168));
#61197=CARTESIAN_POINT('Origin',(12.256,29.392,44.896));
#61198=CARTESIAN_POINT('',(12.256,29.392,45.696));
#61199=CARTESIAN_POINT('',(12.256,30.192,44.896));
#61200=CARTESIAN_POINT('Origin',(12.256,29.392,44.896));
#61201=CARTESIAN_POINT('',(13.056,29.392,44.896));
#61202=CARTESIAN_POINT('Origin',(12.256,29.392,44.896));
#61203=CARTESIAN_POINT('Origin',(12.256,29.392,44.896));
#61204=CARTESIAN_POINT('Origin',(12.256,12.24,44.896));
#61205=CARTESIAN_POINT('',(13.056,12.24,44.896));
#61206=CARTESIAN_POINT('',(12.256,12.24,45.696));
#61207=CARTESIAN_POINT('Origin',(12.256,29.392,44.064));
#61208=CARTESIAN_POINT('',(12.256,30.192,44.064));
#61209=CARTESIAN_POINT('',(13.056,29.392,44.064));
#61210=CARTESIAN_POINT('Origin',(-12.256,29.392,44.896));
#61211=CARTESIAN_POINT('',(-13.056,29.392,44.896));
#61212=CARTESIAN_POINT('',(-12.256,30.192,44.896));
#61213=CARTESIAN_POINT('Origin',(-12.256,29.392,44.896));
#61214=CARTESIAN_POINT('',(-12.256,29.392,45.696));
#61215=CARTESIAN_POINT('Origin',(-12.256,29.392,44.896));
#61216=CARTESIAN_POINT('Origin',(-12.256,29.392,44.896));
#61217=CARTESIAN_POINT('Origin',(-16.744,3.248,44.896));
#61218=CARTESIAN_POINT('',(-16.744,2.448,44.896));
#61219=CARTESIAN_POINT('',(-17.544,3.248,44.896));
#61220=CARTESIAN_POINT('Origin',(-16.744,3.248,44.896));
#61221=CARTESIAN_POINT('',(-16.744,3.248,45.696));
#61222=CARTESIAN_POINT('Origin',(-16.744,3.248,44.896));
#61223=CARTESIAN_POINT('Origin',(-16.744,3.248,44.896));
#61224=CARTESIAN_POINT('Origin',(-8.772,3.248,44.896));
#61225=CARTESIAN_POINT('',(-4.35247056279534,2.448,44.896));
#61226=CARTESIAN_POINT('',(-4.35247056279534,3.248,45.696));
#61227=CARTESIAN_POINT('Origin',(-4.35247056279534,3.248,44.896));
#61228=CARTESIAN_POINT('',(-8.772,3.248,45.696));
#61229=CARTESIAN_POINT('',(-8.772,2.448,44.896));
#61230=CARTESIAN_POINT('Origin',(-16.744,21.232,44.896));
#61231=CARTESIAN_POINT('',(-17.544,21.232,44.896));
#61232=CARTESIAN_POINT('',(-16.744,22.032,44.896));
#61233=CARTESIAN_POINT('Origin',(-16.744,21.232,44.896));
#61234=CARTESIAN_POINT('',(-16.744,21.232,45.696));
#61235=CARTESIAN_POINT('Origin',(-16.744,21.232,44.896));
#61236=CARTESIAN_POINT('Origin',(-16.744,21.232,44.896));
#61237=CARTESIAN_POINT('Origin',(-16.744,2.448,44.896));
#61238=CARTESIAN_POINT('',(-17.544,2.448,44.896));
#61239=CARTESIAN_POINT('',(-16.744,2.448,45.696));
#61240=CARTESIAN_POINT('Origin',(-8.772,21.232,44.896));
#61241=CARTESIAN_POINT('',(-13.056,22.032,44.896));
#61242=CARTESIAN_POINT('',(-8.772,22.032,44.896));
#61243=CARTESIAN_POINT('',(-12.256,21.232,45.696));
#61244=CARTESIAN_POINT('',(-8.772,21.232,45.696));
#61245=CARTESIAN_POINT('Origin',(-12.256,21.232,44.896));
#61246=CARTESIAN_POINT('Origin',(-16.744,21.232,39.968));
#61247=CARTESIAN_POINT('',(-17.544,21.232,39.968));
#61248=CARTESIAN_POINT('',(-16.744,22.032,39.968));
#61249=CARTESIAN_POINT('Origin',(-16.744,21.232,39.968));
#61250=CARTESIAN_POINT('',(-16.744,21.232,39.168));
#61251=CARTESIAN_POINT('Origin',(-16.744,21.232,39.968));
#61252=CARTESIAN_POINT('Origin',(-16.744,21.232,39.968));
#61253=CARTESIAN_POINT('Origin',(-16.744,21.232,40.8));
#61254=CARTESIAN_POINT('',(-17.544,21.232,40.8));
#61255=CARTESIAN_POINT('',(-16.744,22.032,40.8));
#61256=CARTESIAN_POINT('Origin',(-12.256,12.24,44.896));
#61257=CARTESIAN_POINT('',(-12.256,12.24,45.696));
#61258=CARTESIAN_POINT('',(-13.056,12.24,44.896));
#61259=CARTESIAN_POINT('Origin',(-16.744,3.248,40.8));
#61260=CARTESIAN_POINT('',(-17.544,3.248,39.968));
#61261=CARTESIAN_POINT('',(-16.744,2.448,39.968));
#61262=CARTESIAN_POINT('Origin',(-16.744,3.248,39.968));
#61263=CARTESIAN_POINT('',(-16.744,2.448,40.8));
#61264=CARTESIAN_POINT('',(-17.544,3.248,40.8));
#61265=CARTESIAN_POINT('Origin',(-16.744,3.248,39.968));
#61266=CARTESIAN_POINT('',(-16.744,3.248,39.168));
#61267=CARTESIAN_POINT('Origin',(-16.744,3.248,39.968));
#61268=CARTESIAN_POINT('Origin',(-16.744,3.248,39.968));
#61269=CARTESIAN_POINT('Origin',(-8.772,29.392,44.896));
#61270=CARTESIAN_POINT('',(-8.772,30.192,44.896));
#61271=CARTESIAN_POINT('',(-8.772,29.392,45.696));
#61272=CARTESIAN_POINT('Origin',(-12.256,29.392,40.8));
#61273=CARTESIAN_POINT('',(-13.056,29.392,39.968));
#61274=CARTESIAN_POINT('Origin',(-12.256,29.392,39.968));
#61275=CARTESIAN_POINT('',(-13.056,29.392,40.8));
#61276=CARTESIAN_POINT('',(-12.256,30.192,40.8));
#61277=CARTESIAN_POINT('Origin',(16.744,21.232,44.064));
#61278=CARTESIAN_POINT('',(16.744,22.032,44.064));
#61279=CARTESIAN_POINT('',(17.544,21.232,44.064));
#61280=CARTESIAN_POINT('Ctrl Pts',(7.4948384107818E-16,2.448,45.696));
#61281=CARTESIAN_POINT('Ctrl Pts',(-0.0042297694102402,2.448,45.6960019265802));
#61282=CARTESIAN_POINT('Ctrl Pts',(-0.00845818449221337,2.44800353095933,
45.6960038547636));
#61283=CARTESIAN_POINT('Ctrl Pts',(-0.926069758734644,2.44858567321808,
45.6964214479009));
#61284=CARTESIAN_POINT('Ctrl Pts',(-2.15780484233224,2.59294255969351,45.6969841667508));
#61285=CARTESIAN_POINT('Ctrl Pts',(-3.5684103856049,2.97124337151832,45.6966752349463));
#61286=CARTESIAN_POINT('Ctrl Pts',(-4.10516581642087,3.15568217900954,45.6962732015741));
#61287=CARTESIAN_POINT('Ctrl Pts',(-4.36651858547018,3.25568165343709,45.6959807918452));
#61288=CARTESIAN_POINT('Ctrl Pts',(7.4948384107818E-16,2.448,45.696));
#61289=CARTESIAN_POINT('Ctrl Pts',(-0.00416276422045042,2.448,45.6958022200772));
#61290=CARTESIAN_POINT('Ctrl Pts',(-0.00836699352100908,2.44798339666368,
45.6956042979429));
#61291=CARTESIAN_POINT('Ctrl Pts',(-0.913504058614908,2.4498415415713,45.6527356961232));
#61292=CARTESIAN_POINT('Ctrl Pts',(-2.13405707884003,2.53374268898235,45.5949753639831));
#61293=CARTESIAN_POINT('Ctrl Pts',(-3.56166897255153,2.79399285615006,45.6268807116574));
#61294=CARTESIAN_POINT('Ctrl Pts',(-4.10497083294057,2.93362393613479,45.6682659881586));
#61295=CARTESIAN_POINT('Ctrl Pts',(-4.36653277992524,3.01450371964943,45.6983471985849));
#61296=CARTESIAN_POINT('Ctrl Pts',(7.4948384107818E-16,2.448,45.696));
#61297=CARTESIAN_POINT('Ctrl Pts',(-0.00407497810370066,2.448,45.6954571286858));
#61298=CARTESIAN_POINT('Ctrl Pts',(-0.00817838886308814,2.44799413269538,
45.6949016819103));
#61299=CARTESIAN_POINT('Ctrl Pts',(-0.893431977013438,2.44860632854555,
45.5767431370729));
#61300=CARTESIAN_POINT('Ctrl Pts',(-2.08821913676147,2.46675784665521,45.4140811184592));
#61301=CARTESIAN_POINT('Ctrl Pts',(-3.534931299702,2.53273348711954,45.3978866963668));
#61302=CARTESIAN_POINT('Ctrl Pts',(-4.09594086592657,2.57158546220149,45.4499925192889));
#61303=CARTESIAN_POINT('Ctrl Pts',(-4.36704474249966,2.59586901950321,45.4983996515835));
#61304=CARTESIAN_POINT('Ctrl Pts',(7.4948384107818E-16,2.448,45.696));
#61305=CARTESIAN_POINT('Ctrl Pts',(-0.00398896174508187,2.448,45.6951045051365));
#61306=CARTESIAN_POINT('Ctrl Pts',(-0.0079872843945144,2.448,45.6942070450307));
#61307=CARTESIAN_POINT('Ctrl Pts',(-0.87369611876912,2.44800000000002,45.5001223087092));
#61308=CARTESIAN_POINT('Ctrl Pts',(-2.03938167211534,2.448,45.2359122100003));
#61309=CARTESIAN_POINT('Ctrl Pts',(-3.49454117469163,2.448,45.0734599399993));
#61310=CARTESIAN_POINT('Ctrl Pts',(-4.07699986556522,2.448,45.0613017312264));
#61311=CARTESIAN_POINT('Ctrl Pts',(-4.36811063334064,2.448,45.0763052280038));
#61312=CARTESIAN_POINT('Ctrl Pts',(7.4948384107818E-16,2.448,45.696));
#61313=CARTESIAN_POINT('Ctrl Pts',(-0.00395271020241197,2.448,45.6949547336815));
#61314=CARTESIAN_POINT('Ctrl Pts',(-0.0079050097320282,2.448,45.6939088542388));
#61315=CARTESIAN_POINT('Ctrl Pts',(-0.865284652416804,2.44800000000002,
45.4674065150327));
#61316=CARTESIAN_POINT('Ctrl Pts',(-2.01851098765155,2.448,45.1596990578109));
#61317=CARTESIAN_POINT('Ctrl Pts',(-3.47727706236774,2.448,44.9347642209047));
#61318=CARTESIAN_POINT('Ctrl Pts',(-4.06894992871341,2.448,44.8952825142091));
#61319=CARTESIAN_POINT('Ctrl Pts',(-4.36856368751371,2.448,44.8960197795982));
#61320=CARTESIAN_POINT('',(0.,2.448,45.696));
#61321=CARTESIAN_POINT('Ctrl Pts',(-4.35247056279534,2.448,44.896));
#61322=CARTESIAN_POINT('Ctrl Pts',(-4.05826044258909,2.448,44.896));
#61323=CARTESIAN_POINT('Ctrl Pts',(-3.47197716194173,2.448,44.9355814405115));
#61324=CARTESIAN_POINT('Ctrl Pts',(-2.01851098765155,2.448,45.1596990578109));
#61325=CARTESIAN_POINT('Ctrl Pts',(-0.865284652416804,2.44800000000002,
45.4674065150327));
#61326=CARTESIAN_POINT('Ctrl Pts',(-0.0079050097320282,2.448,45.6939088542388));
#61327=CARTESIAN_POINT('Ctrl Pts',(-0.00395271020241197,2.448,45.6949547336815));
#61328=CARTESIAN_POINT('Ctrl Pts',(7.4948384107818E-16,2.448,45.696));
#61329=CARTESIAN_POINT('',(-0.0438084974115087,2.44807801344885,45.6958602367687));
#61330=CARTESIAN_POINT('Ctrl Pts',(7.4948384107818E-16,2.448,45.696));
#61331=CARTESIAN_POINT('Ctrl Pts',(-0.0146028459483958,2.448,45.6959524518301));
#61332=CARTESIAN_POINT('Ctrl Pts',(-0.029205702201559,2.4480259973895,45.6959058635638));
#61333=CARTESIAN_POINT('Ctrl Pts',(-0.0438084974115087,2.44807801344885,
45.6958602367687));
#61334=CARTESIAN_POINT('Ctrl Pts',(-0.0438084974115087,2.44807801344885,
45.6958602367687));
#61335=CARTESIAN_POINT('Ctrl Pts',(-0.215221081627298,2.44868859567132,
45.6953246539055));
#61336=CARTESIAN_POINT('Ctrl Pts',(-0.572631506599956,2.45743734647924,
45.6944841070415));
#61337=CARTESIAN_POINT('Ctrl Pts',(-0.929503603080839,2.48192374326381,
45.6942306077308));
#61338=CARTESIAN_POINT('Ctrl Pts',(-1.48294296488667,2.53254694014243,45.6943635436273));
#61339=CARTESIAN_POINT('Ctrl Pts',(-1.84923144734727,2.58285611046353,45.6951271660723));
#61340=CARTESIAN_POINT('Ctrl Pts',(-2.58528683030832,2.71814578051949,45.6960725289316));
#61341=CARTESIAN_POINT('Ctrl Pts',(-2.95437944818565,2.80386392547483,45.695959587621));
#61342=CARTESIAN_POINT('Ctrl Pts',(-3.66834194740326,3.00499350179398,45.695870963165));
#61343=CARTESIAN_POINT('Ctrl Pts',(-4.01319449081232,3.11891878356932,45.696));
#61344=CARTESIAN_POINT('Ctrl Pts',(-4.35247056279534,3.248,45.696));
#61345=CARTESIAN_POINT('Origin',(-12.256,29.392,39.968));
#61346=CARTESIAN_POINT('Origin',(-12.256,29.392,39.968));
#61347=CARTESIAN_POINT('Ctrl Pts',(4.39516096358101,3.27057537586253,45.695842677698));
#61348=CARTESIAN_POINT('Ctrl Pts',(3.10136038026502,2.76989103636905,45.6999183484526));
#61349=CARTESIAN_POINT('Ctrl Pts',(1.55459125658799,2.44759664360609,45.6978772609464));
#61350=CARTESIAN_POINT('Ctrl Pts',(0.00845534674966224,2.44800610805417,
45.696010238955));
#61351=CARTESIAN_POINT('Ctrl Pts',(0.00423047718001614,2.448,45.6960051189726));
#61352=CARTESIAN_POINT('Ctrl Pts',(7.47837257143373E-16,2.448,45.696));
#61353=CARTESIAN_POINT('Ctrl Pts',(4.39511536874253,3.02604293559063,45.7030390251783));
#61354=CARTESIAN_POINT('Ctrl Pts',(3.10299573355848,2.61832690373019,45.5463077383758));
#61355=CARTESIAN_POINT('Ctrl Pts',(1.53064193566912,2.45080363107014,45.6242176396158));
#61356=CARTESIAN_POINT('Ctrl Pts',(0.00835778454095319,2.4479978870276,
45.6956086270239));
#61357=CARTESIAN_POINT('Ctrl Pts',(0.00417737580197284,2.448,45.695804314302));
#61358=CARTESIAN_POINT('Ctrl Pts',(7.47837257143373E-16,2.448,45.696));
#61359=CARTESIAN_POINT('Ctrl Pts',(4.39671743528037,2.59903454561625,45.5050418831425));
#61360=CARTESIAN_POINT('Ctrl Pts',(3.05527533000142,2.47592075525703,45.2585583869767));
#61361=CARTESIAN_POINT('Ctrl Pts',(1.49436708678789,2.44969437712917,45.4997611979407));
#61362=CARTESIAN_POINT('Ctrl Pts',(0.00817708117964293,2.44799748268289,
45.6949007347785));
#61363=CARTESIAN_POINT('Ctrl Pts',(0.00408478680943832,2.448,45.6954541858716));
#61364=CARTESIAN_POINT('Ctrl Pts',(7.47837257143373E-16,2.448,45.696));
#61365=CARTESIAN_POINT('Ctrl Pts',(4.4000397197984,2.44795709552943,45.0779870733328));
#61366=CARTESIAN_POINT('Ctrl Pts',(2.95581829667796,2.4492887212198,44.9980915455101));
#61367=CARTESIAN_POINT('Ctrl Pts',(1.46391650084949,2.4480041008596,45.3714533842438));
#61368=CARTESIAN_POINT('Ctrl Pts',(0.00798512064170265,2.44799999699524,
45.6942002504552));
#61369=CARTESIAN_POINT('Ctrl Pts',(0.00399219781690372,2.448,45.6951040574412));
#61370=CARTESIAN_POINT('Ctrl Pts',(7.47837257143373E-16,2.448,45.696));
#61371=CARTESIAN_POINT('Ctrl Pts',(4.40145261138498,2.448,44.8961576078484));
#61372=CARTESIAN_POINT('Ctrl Pts',(2.91352207632623,2.448,44.8865642443111));
#61373=CARTESIAN_POINT('Ctrl Pts',(1.45091428114908,2.44799999999988,45.3167261493743));
#61374=CARTESIAN_POINT('Ctrl Pts',(0.00790328288195149,2.448,45.6939015162397));
#61375=CARTESIAN_POINT('Ctrl Pts',(0.00395271020241243,2.448,45.6949547336815));
#61376=CARTESIAN_POINT('Ctrl Pts',(7.47837257143373E-16,2.448,45.696));
#61377=CARTESIAN_POINT('',(0.113153243773417,2.44852303636207,45.696));
#61378=CARTESIAN_POINT('Origin',(0.,14.688,45.696));
#61379=CARTESIAN_POINT('Origin',(0.,14.688,45.696));
#61380=CARTESIAN_POINT('Ctrl Pts',(7.46282150093834E-16,2.448,45.696));
#61381=CARTESIAN_POINT('Ctrl Pts',(0.00395271020241243,2.448,45.6949547336815));
#61382=CARTESIAN_POINT('Ctrl Pts',(0.00790328288195149,2.448,45.6939015162397));
#61383=CARTESIAN_POINT('Ctrl Pts',(1.43512030035333,2.44799999999988,45.320854392685));
#61384=CARTESIAN_POINT('Ctrl Pts',(2.88141996176407,2.448,44.896));
#61385=CARTESIAN_POINT('Ctrl Pts',(4.35247056279534,2.448,44.896));
#61386=CARTESIAN_POINT('Origin',(16.744,3.248,39.968));
#61387=CARTESIAN_POINT('Origin',(16.744,3.248,39.968));
#61388=CARTESIAN_POINT('Origin',(13.056,22.032,45.696));
#61389=CARTESIAN_POINT('',(13.056,22.032,44.064));
#61390=CARTESIAN_POINT('Origin',(0.,2.448,42.432));
#61391=CARTESIAN_POINT('',(8.772,2.448,39.968));
#61392=CARTESIAN_POINT('',(-6.528,2.448,40.332));
#61393=CARTESIAN_POINT('Origin',(-6.528,2.448,42.432));
#61394=CARTESIAN_POINT('',(6.528,2.448,40.332));
#61395=CARTESIAN_POINT('Origin',(6.528,2.448,42.432));
#61396=CARTESIAN_POINT('Origin',(-17.544,2.448,39.168));
#61397=CARTESIAN_POINT('',(-17.544,2.448,39.968));
#61398=CARTESIAN_POINT('Origin',(-16.744,2.448,39.968));
#61399=CARTESIAN_POINT('',(-16.744,2.448,39.168));
#61400=CARTESIAN_POINT('Origin',(17.544,2.448,45.696));
#61401=CARTESIAN_POINT('Origin',(0.,30.192,42.432));
#61402=CARTESIAN_POINT('Origin',(8.772,3.248,39.968));
#61403=CARTESIAN_POINT('',(8.772,3.248,39.168));
#61404=CARTESIAN_POINT('Origin',(8.772,21.232,39.968));
#61405=CARTESIAN_POINT('',(-13.056,22.032,39.968));
#61406=CARTESIAN_POINT('',(8.772,22.032,39.968));
#61407=CARTESIAN_POINT('',(-12.256,21.232,39.168));
#61408=CARTESIAN_POINT('Origin',(-12.256,21.232,39.968));
#61409=CARTESIAN_POINT('',(8.772,21.232,39.168));
#61410=CARTESIAN_POINT('Origin',(-12.256,12.24,39.968));
#61411=CARTESIAN_POINT('',(-12.256,12.24,39.168));
#61412=CARTESIAN_POINT('',(-13.056,12.24,39.968));
#61413=CARTESIAN_POINT('Origin',(0.,22.032,42.432));
#61414=CARTESIAN_POINT('',(-13.056,22.032,40.8));
#61415=CARTESIAN_POINT('Origin',(0.,14.688,46.3872037037125));
#61416=CARTESIAN_POINT('',(-5.7528,14.688,46.3872037037125));
#61417=CARTESIAN_POINT('Origin',(0.,14.688,46.3872037037125));
#61418=CARTESIAN_POINT('',(-6.3648,14.688,47.1648));
#61419=CARTESIAN_POINT('Origin',(-6.5528,14.688,46.3872037037125));
#61420=CARTESIAN_POINT('Origin',(0.,14.688,47.1648));
#61421=CARTESIAN_POINT('Origin',(0.,14.688,40.7184));
#61422=CARTESIAN_POINT('',(-5.7528,14.688,40.7184));
#61423=CARTESIAN_POINT('Origin',(0.,14.688,40.7184));
#61424=CARTESIAN_POINT('',(-5.7528,14.688,40.7184));
#61425=CARTESIAN_POINT('Origin',(0.,14.688,46.6912));
#61426=CARTESIAN_POINT('',(-11.44,14.688,47.4912));
#61427=CARTESIAN_POINT('Origin',(0.,14.688,47.4912));
#61428=CARTESIAN_POINT('',(-12.24,14.688,46.6912));
#61429=CARTESIAN_POINT('Origin',(-11.44,14.688,46.6912));
#61430=CARTESIAN_POINT('Origin',(0.,14.688,46.6912));
#61431=CARTESIAN_POINT('Origin',(0.,14.688,47.4912));
#61432=CARTESIAN_POINT('',(11.3943409947345,14.688,47.4912));
#61433=CARTESIAN_POINT('Origin',(0.,14.688,47.4912));
#61434=CARTESIAN_POINT('Origin',(0.,14.688,45.696));
#61435=CARTESIAN_POINT('',(-12.24,14.688,45.696));
#61436=CARTESIAN_POINT('',(-12.24,14.688,45.696));
#61437=CARTESIAN_POINT('',(-4.59359814877846,3.34267250153002,45.696));
#61438=CARTESIAN_POINT('Origin',(0.,14.688,45.696));
#61439=CARTESIAN_POINT('Origin',(0.,14.688,45.696));
#61440=CARTESIAN_POINT('',(4.59359814877845,3.34267250153002,45.696));
#61441=CARTESIAN_POINT('Origin',(0.,14.688,45.696));
#61442=CARTESIAN_POINT('',(10.4030656451586,21.13732749847,45.696));
#61443=CARTESIAN_POINT('Origin',(0.,14.688,45.696));
#61444=CARTESIAN_POINT('',(-10.4030656451586,21.13732749847,45.696));
#61445=CARTESIAN_POINT('Origin',(0.,14.688,45.696));
#61446=CARTESIAN_POINT('Origin',(0.,14.688,45.696));
#61447=CARTESIAN_POINT('Origin',(0.,14.688,46.6912));
#61448=CARTESIAN_POINT('',(10.608,14.688,46.8384));
#61449=CARTESIAN_POINT('Origin',(0.,14.688,46.8384));
#61450=CARTESIAN_POINT('Origin',(11.3943409947345,14.688,46.6912));
#61451=CARTESIAN_POINT('Origin',(6.528,3.248,42.432));
#61452=CARTESIAN_POINT('',(6.528,3.248,41.132));
#61453=CARTESIAN_POINT('Origin',(6.528,3.248,40.332));
#61454=CARTESIAN_POINT('',(5.228,3.248,42.432));
#61455=CARTESIAN_POINT('Origin',(6.528,3.248,42.432));
#61456=CARTESIAN_POINT('Origin',(6.528,3.248,42.432));
#61457=CARTESIAN_POINT('Origin',(6.528,2.448,42.432));
#61458=CARTESIAN_POINT('',(5.228,6.12,42.432));
#61459=CARTESIAN_POINT('',(5.228,2.448,42.432));
#61460=CARTESIAN_POINT('Origin',(6.528,6.12,42.432));
#61461=CARTESIAN_POINT('Origin',(-6.528,3.248,42.432));
#61462=CARTESIAN_POINT('',(-6.528,3.248,41.132));
#61463=CARTESIAN_POINT('Origin',(-6.528,3.248,40.332));
#61464=CARTESIAN_POINT('',(-7.828,3.248,42.432));
#61465=CARTESIAN_POINT('Origin',(-6.528,3.248,42.432));
#61466=CARTESIAN_POINT('Origin',(-6.528,3.248,42.432));
#61467=CARTESIAN_POINT('Origin',(-6.528,2.448,42.432));
#61468=CARTESIAN_POINT('',(-7.828,6.12,42.432));
#61469=CARTESIAN_POINT('',(-7.828,2.448,42.432));
#61470=CARTESIAN_POINT('Origin',(-6.528,6.12,42.432));
#61471=CARTESIAN_POINT('Origin',(-16.64932749847,20.4,44.896));
#61472=CARTESIAN_POINT('',(-16.64932749847,21.13732749847,45.696));
#61473=CARTESIAN_POINT('',(-16.64932749847,3.34267250153002,45.696));
#61474=CARTESIAN_POINT('',(-16.64932749847,20.4,45.696));
#61475=CARTESIAN_POINT('',(-15.912,4.08,45.2064));
#61476=CARTESIAN_POINT('Origin',(-16.64932749847,3.34267250153002,44.896));
#61477=CARTESIAN_POINT('',(-15.912,20.4,45.2064));
#61478=CARTESIAN_POINT('',(-15.912,20.4,45.2064));
#61479=CARTESIAN_POINT('Origin',(-16.64932749847,21.13732749847,44.896));
#61480=CARTESIAN_POINT('Origin',(-15.912,3.34267250153002,44.896));
#61481=CARTESIAN_POINT('',(-6.88783275058274,4.08000000000001,45.2064));
#61482=CARTESIAN_POINT('Ctrl Pts',(-6.88783275058276,4.08,45.2064));
#61483=CARTESIAN_POINT('Ctrl Pts',(-6.83096980964154,4.0598235620632,45.2543273276803));
#61484=CARTESIAN_POINT('Ctrl Pts',(-6.7651197403416,4.03741502983645,45.2945582388546));
#61485=CARTESIAN_POINT('Ctrl Pts',(-6.39957290725477,3.9155905586413,45.4848436925738));
#61486=CARTESIAN_POINT('Ctrl Pts',(-5.98530408411679,3.7896019396787,45.564325669844));
#61487=CARTESIAN_POINT('Ctrl Pts',(-5.5447169847327,3.65682068790766,45.635102112391));
#61488=CARTESIAN_POINT('Ctrl Pts',(-5.32942559902382,3.59265625235564,45.6587020324601));
#61489=CARTESIAN_POINT('Ctrl Pts',(-5.01397139988192,3.49312899095025,45.6826190067178));
#61490=CARTESIAN_POINT('Ctrl Pts',(-4.89575271613861,3.45453624015517,45.6891574202889));
#61491=CARTESIAN_POINT('Ctrl Pts',(-4.74288425804082,3.40004644173792,45.694072800358));
#61492=CARTESIAN_POINT('Ctrl Pts',(-4.70238437966304,3.38513990705534,45.6950176500099));
#61493=CARTESIAN_POINT('Ctrl Pts',(-4.63941311517471,3.36096086412175,45.6958408853381));
#61494=CARTESIAN_POINT('Ctrl Pts',(-4.61634398319733,3.35188203936778,45.696));
#61495=CARTESIAN_POINT('Ctrl Pts',(-4.59359814877846,3.34267250153002,45.696));
#61496=CARTESIAN_POINT('',(-15.912,4.08,45.2064));
#61497=CARTESIAN_POINT('',(-15.912,3.34267250153002,45.696));
#61498=CARTESIAN_POINT('Origin',(15.912,21.13732749847,44.896));
#61499=CARTESIAN_POINT('',(-11.2847224157265,20.4,45.2064));
#61500=CARTESIAN_POINT('Ctrl Pts',(-10.4030656451586,21.13732749847,45.696));
#61501=CARTESIAN_POINT('Ctrl Pts',(-10.4051770230818,21.1339217475383,45.696));
#61502=CARTESIAN_POINT('Ctrl Pts',(-10.4073411793795,21.1305091350682,45.6959782528326));
#61503=CARTESIAN_POINT('Ctrl Pts',(-10.412554449671,21.1224696164265,45.6958753597619));
#61504=CARTESIAN_POINT('Ctrl Pts',(-10.4156410384128,21.1178470255194,45.6957761688512));
#61505=CARTESIAN_POINT('Ctrl Pts',(-10.4269111127494,21.101439194627,45.6952815482675));
#61506=CARTESIAN_POINT('Ctrl Pts',(-10.4354731270868,21.0898118955789,45.6946703826387));
#61507=CARTESIAN_POINT('Ctrl Pts',(-10.5276360945525,20.9718731085772,45.6859518637731));
#61508=CARTESIAN_POINT('Ctrl Pts',(-10.6546192820411,20.8677270702112,45.6569089689747));
#61509=CARTESIAN_POINT('Ctrl Pts',(-10.8999196049235,20.6799375325347,45.5604011294049));
#61510=CARTESIAN_POINT('Ctrl Pts',(-11.0271541759068,20.5894785071695,45.4916387532884));
#61511=CARTESIAN_POINT('Ctrl Pts',(-11.189723388502,20.4714505593328,45.3443731595757));
#61512=CARTESIAN_POINT('Ctrl Pts',(-11.2432877828146,20.4321606305034,45.2821292970099));
#61513=CARTESIAN_POINT('Ctrl Pts',(-11.2838716320031,20.400661136201,45.2079669722959));
#61514=CARTESIAN_POINT('Ctrl Pts',(-11.284297802453,20.4003300968063,45.2071841155039));
#61515=CARTESIAN_POINT('Ctrl Pts',(-11.2847224157265,20.4,45.2064));
#61516=CARTESIAN_POINT('',(15.912,21.13732749847,45.696));
#61517=CARTESIAN_POINT('',(15.912,20.4,45.2064));
#61518=CARTESIAN_POINT('Origin',(0.,14.688,44.9814350779728));
#61519=CARTESIAN_POINT('Origin',(0.,14.688,45.2064));
#61520=CARTESIAN_POINT('Origin',(0.,14.688,44.9814350779728));
#61521=CARTESIAN_POINT('',(6.88783275058272,4.08,45.2064));
#61522=CARTESIAN_POINT('Ctrl Pts',(6.88783275058275,4.07999999999999,45.2064));
#61523=CARTESIAN_POINT('Ctrl Pts',(6.81886324438962,4.05552784048444,45.2645314309206));
#61524=CARTESIAN_POINT('Ctrl Pts',(6.73479715088626,4.02711895305195,45.3128039443106));
#61525=CARTESIAN_POINT('Ctrl Pts',(6.37658245357399,3.90895311670654,45.4835230174535));
#61526=CARTESIAN_POINT('Ctrl Pts',(6.01691030549754,3.79918184362475,45.5580047227756));
#61527=CARTESIAN_POINT('Ctrl Pts',(5.4669145728647,3.63330799139618,45.6490772612781));
#61528=CARTESIAN_POINT('Ctrl Pts',(5.1442770940251,3.53803359519506,45.6769668597336));
#61529=CARTESIAN_POINT('Ctrl Pts',(4.82263423748175,3.42860301313298,45.6916369428731));
#61530=CARTESIAN_POINT('Ctrl Pts',(4.76176127218778,3.40713850397811,45.6937147455139));
#61531=CARTESIAN_POINT('Ctrl Pts',(4.67424460245221,3.37441113690961,45.6954366167826));
#61532=CARTESIAN_POINT('Ctrl Pts',(4.64655042016146,3.36378090096371,45.695796654937));
#61533=CARTESIAN_POINT('Ctrl Pts',(4.61048568759284,3.34947405358982,45.6959780669794));
#61534=CARTESIAN_POINT('Ctrl Pts',(4.60204627195492,3.34609305355812,45.696));
#61535=CARTESIAN_POINT('Ctrl Pts',(4.59359814877844,3.34267250153004,45.696));
#61536=CARTESIAN_POINT('',(11.2847224157265,20.4,45.2064));
#61537=CARTESIAN_POINT('Origin',(0.,14.688,45.2064));
#61538=CARTESIAN_POINT('Ctrl Pts',(10.4030656451586,21.13732749847,45.696));
#61539=CARTESIAN_POINT('Ctrl Pts',(10.4034528587117,21.1367029049737,45.696));
#61540=CARTESIAN_POINT('Ctrl Pts',(10.4038419091445,21.1360779805853,45.6959992685327));
#61541=CARTESIAN_POINT('Ctrl Pts',(10.4067993400092,21.1313473906548,45.6959881825164));
#61542=CARTESIAN_POINT('Ctrl Pts',(10.409442322896,21.1272325286132,45.6959469405597));
#61543=CARTESIAN_POINT('Ctrl Pts',(10.4165444903014,21.1164637513178,45.6957555036594));
#61544=CARTESIAN_POINT('Ctrl Pts',(10.4210983853722,21.1098376988435,45.6955548983378));
#61545=CARTESIAN_POINT('Ctrl Pts',(10.4423960109042,21.0800225292309,45.6942830109848));
#61546=CARTESIAN_POINT('Ctrl Pts',(10.4606745049416,21.0575445714608,45.6923105556957));
#61547=CARTESIAN_POINT('Ctrl Pts',(10.5332222285603,20.9760257865206,45.6818919339335));
#61548=CARTESIAN_POINT('Ctrl Pts',(10.5968068470649,20.9192489972096,45.6676377403279));
#61549=CARTESIAN_POINT('Ctrl Pts',(10.7768228876743,20.7700779575399,45.6142654321202));
#61550=CARTESIAN_POINT('Ctrl Pts',(10.9210832070263,20.6659568730065,45.5556873871454));
#61551=CARTESIAN_POINT('Ctrl Pts',(11.1395119114092,20.5079861571895,45.398243288761));
#61552=CARTESIAN_POINT('Ctrl Pts',(11.2127184779424,20.4549727268256,45.3235592719424));
#61553=CARTESIAN_POINT('Ctrl Pts',(11.2716513432665,20.4101014026675,45.2296098269067));
#61554=CARTESIAN_POINT('Ctrl Pts',(11.2783609804129,20.404945416479,45.2181473954941));
#61555=CARTESIAN_POINT('Ctrl Pts',(11.2847224157265,20.4,45.2064));
#61556=CARTESIAN_POINT('Origin',(-17.544,2.448,45.696));
#61557=CARTESIAN_POINT('',(16.64932749847,21.13732749847,45.696));
#61558=CARTESIAN_POINT('',(15.912,21.13732749847,45.696));
#61559=CARTESIAN_POINT('',(16.64932749847,3.34267250153002,45.696));
#61560=CARTESIAN_POINT('',(16.64932749847,4.08,45.696));
#61561=CARTESIAN_POINT('',(-15.912,3.34267250153002,45.696));
#61562=CARTESIAN_POINT('Origin',(-15.912,3.34267250153002,44.896));
#61563=CARTESIAN_POINT('',(15.912,4.08,45.2064));
#61564=CARTESIAN_POINT('Origin',(16.64932749847,3.34267250153002,44.896));
#61565=CARTESIAN_POINT('',(-15.912,4.08,45.2064));
#61566=CARTESIAN_POINT('Origin',(15.912,21.13732749847,44.896));
#61567=CARTESIAN_POINT('',(15.912,20.4,45.2064));
#61568=CARTESIAN_POINT('',(15.912,20.4,45.2064));
#61569=CARTESIAN_POINT('Origin',(16.64932749847,21.13732749847,44.896));
#61570=CARTESIAN_POINT('Origin',(16.64932749847,4.08,44.896));
#61571=CARTESIAN_POINT('',(15.912,4.08,45.2064));
#61572=CARTESIAN_POINT('Origin',(-14.28,5.712,44.4064));
#61573=CARTESIAN_POINT('',(-13.6272,5.712,45.0432));
#61574=CARTESIAN_POINT('Origin',(-14.28,5.712,45.0432));
#61575=CARTESIAN_POINT('',(-13.1429627027995,5.712,45.2064));
#61576=CARTESIAN_POINT('Origin',(-13.1429627027995,5.712,44.4064));
#61577=CARTESIAN_POINT('Origin',(-14.28,5.712,45.2064));
#61578=CARTESIAN_POINT('Origin',(-11.3999163752914,12.24,45.2064));
#61579=CARTESIAN_POINT('',(-13.1429627027995,18.768,45.2064));
#61580=CARTESIAN_POINT('Origin',(-14.28,18.768,45.2064));
#61581=CARTESIAN_POINT('Origin',(-14.28,18.768,44.4064));
#61582=CARTESIAN_POINT('',(-13.6272,18.768,45.0432));
#61583=CARTESIAN_POINT('Origin',(-14.28,18.768,45.0432));
#61584=CARTESIAN_POINT('Origin',(-13.1429627027995,18.768,44.4064));
#61585=CARTESIAN_POINT('Origin',(14.28,5.712,44.4064));
#61586=CARTESIAN_POINT('',(14.9328,5.712,45.0432));
#61587=CARTESIAN_POINT('Origin',(14.28,5.712,45.0432));
#61588=CARTESIAN_POINT('',(15.4170372972005,5.712,45.2064));
#61589=CARTESIAN_POINT('Origin',(15.4170372972005,5.712,44.4064));
#61590=CARTESIAN_POINT('Origin',(14.28,5.712,45.2064));
#61591=CARTESIAN_POINT('Origin',(11.3999163752914,12.24,45.2064));
#61592=CARTESIAN_POINT('',(15.4170372972005,18.768,45.2064));
#61593=CARTESIAN_POINT('Origin',(14.28,18.768,45.2064));
#61594=CARTESIAN_POINT('Origin',(14.28,18.768,44.4064));
#61595=CARTESIAN_POINT('',(14.9328,18.768,45.0432));
#61596=CARTESIAN_POINT('Origin',(14.28,18.768,45.0432));
#61597=CARTESIAN_POINT('Origin',(15.4170372972005,18.768,44.4064));
#61598=CARTESIAN_POINT('Origin',(0.,14.688,46.4864022969699));
#61599=CARTESIAN_POINT('',(8.16,14.688,46.8384));
#61600=CARTESIAN_POINT('Origin',(0.,14.688,46.8384));
#61601=CARTESIAN_POINT('',(7.0176,14.688,47.1648));
#61602=CARTESIAN_POINT('Origin',(7.4416006562771,14.688,46.4864022969699));
#61603=CARTESIAN_POINT('Origin',(0.,14.688,47.1648));
#61604=CARTESIAN_POINT('Origin',(0.,14.688,47.1648));
#61605=CARTESIAN_POINT('Origin',(14.28,18.768,45.0432));
#61606=CARTESIAN_POINT('Origin',(14.28,5.712,45.0432));
#61607=CARTESIAN_POINT('Origin',(-14.28,18.768,45.0432));
#61608=CARTESIAN_POINT('Origin',(-14.28,5.712,45.0432));
#61609=CARTESIAN_POINT('Origin',(-6.528,6.12,42.432));
#61610=CARTESIAN_POINT('Origin',(6.528,6.12,42.432));
#61611=CARTESIAN_POINT('Origin',(0.,14.688,46.8384));
#61612=CARTESIAN_POINT('Origin',(0.,14.688,40.7184));
#61613=CARTESIAN_POINT('',(-3.975,14.688,40.7184));
#61614=CARTESIAN_POINT('Origin',(0.,14.688,40.7184));
#61615=CARTESIAN_POINT('Origin',(0.,14.688,39.268));
#61616=CARTESIAN_POINT('',(-3.975,14.688,39.368));
#61617=CARTESIAN_POINT('Origin',(0.,14.688,39.368));
#61618=CARTESIAN_POINT('',(-4.175,14.688,39.168));
#61619=CARTESIAN_POINT('',(-4.075,14.688,39.268));
#61620=CARTESIAN_POINT('Origin',(0.,14.688,39.168));
#61621=CARTESIAN_POINT('Origin',(0.,14.688,38.352));
#61622=CARTESIAN_POINT('',(-3.975,14.688,38.352));
#61623=CARTESIAN_POINT('Origin',(17.544,2.448,39.168));
#61624=CARTESIAN_POINT('Origin',(-13.056,22.032,39.168));
#61625=CARTESIAN_POINT('Origin',(0.,22.032,42.432));
#61626=CARTESIAN_POINT('',(0.,0.,0.));
#61627=CARTESIAN_POINT('Origin',(0.1632,0.,0.));
#61628=CARTESIAN_POINT('',(0.326400000000001,-5.712,-6.99518251672968E-16));
#61629=CARTESIAN_POINT('',(0.3264,5.712,6.99518251672968E-16));
#61630=CARTESIAN_POINT('Origin',(0.3264,0.,0.));
#61631=CARTESIAN_POINT('',(0.,5.3856,6.59545780148798E-16));
#61632=CARTESIAN_POINT('',(0.1632,5.5488,6.79532015910883E-16));
#61633=CARTESIAN_POINT('Origin',(0.,0.,0.));
#61634=CARTESIAN_POINT('Origin',(0.3264,0.,0.));
#61635=CARTESIAN_POINT('Origin',(3.264,0.,0.));
#61636=CARTESIAN_POINT('',(6.0384,5.712,6.99518251672968E-16));
#61637=CARTESIAN_POINT('',(6.0384,-5.712,-6.99518251672968E-16));
#61638=CARTESIAN_POINT('Origin',(6.0384,0.,0.));
#61639=CARTESIAN_POINT('Origin',(6.0384,0.,0.));
#61640=CARTESIAN_POINT('',(3.264,-5.712,-6.99518251672968E-16));
#61641=CARTESIAN_POINT('Origin',(0.,5.712,0.));
#61642=CARTESIAN_POINT('',(0.,-2.448,-2.99793536431272E-16));
#61643=CARTESIAN_POINT('Origin',(0.,0.,0.));
#61644=CARTESIAN_POINT('Origin',(6.2832,0.,0.));
#61645=CARTESIAN_POINT('',(6.528,5.2224,-6.39559544386714E-16));
#61646=CARTESIAN_POINT('',(6.2832,5.4672,-6.69538898029841E-16));
#61647=CARTESIAN_POINT('Origin',(6.528,0.,0.));
#61648=CARTESIAN_POINT('Origin',(6.528,2.448,0.));
#61649=CARTESIAN_POINT('',(6.528,2.51932419206087,3.71418222699114));
#61650=CARTESIAN_POINT('',(6.528,3.06045755186719,3.28264277270907));
#61651=CARTESIAN_POINT('Origin',(6.528,0.,0.));
#61652=CARTESIAN_POINT('',(6.528,2.54018621271673,2.70413797072631));
#61653=CARTESIAN_POINT('',(6.528,3.20400206468608,3.44225408264517));
#61654=CARTESIAN_POINT('',(6.528,3.20158419452848,1.87477113412423));
#61655=CARTESIAN_POINT('',(6.528,2.54018621271673,2.70413797072631));
#61656=CARTESIAN_POINT('',(6.528,3.88135593761115,2.2532687557348));
#61657=CARTESIAN_POINT('',(6.528,3.20158419452848,1.87477113412423));
#61658=CARTESIAN_POINT('',(6.528,4.18166229617943,1.62967617664105));
#61659=CARTESIAN_POINT('Origin',(6.528,0.,0.));
#61660=CARTESIAN_POINT('',(6.528,3.46191019016123,1.33419863410882));
#61661=CARTESIAN_POINT('',(6.528,4.380244185348,1.71119936790692));
#61662=CARTESIAN_POINT('',(6.528,3.69796039690208,0.299995104866347));
#61663=CARTESIAN_POINT('',(6.528,3.46191019016123,1.33419863410882));
#61664=CARTESIAN_POINT('',(6.528,4.47463753801084,0.346067772877413));
#61665=CARTESIAN_POINT('',(6.528,3.69796039690208,0.299995104866347));
#61666=CARTESIAN_POINT('',(6.528,4.47463753801084,-0.346067772877415));
#61667=CARTESIAN_POINT('Origin',(6.528,0.,0.));
#61668=CARTESIAN_POINT('',(6.528,3.69796039690209,-0.299995104866348));
#61669=CARTESIAN_POINT('',(6.528,4.6889252249322,-0.358779368128298));
#61670=CARTESIAN_POINT('',(6.528,3.46191019016123,-1.33419863410883));
#61671=CARTESIAN_POINT('',(6.528,3.69796039690209,-0.299995104866348));
#61672=CARTESIAN_POINT('',(6.528,4.18166229617943,-1.62967617664105));
#61673=CARTESIAN_POINT('',(6.528,3.46191019016123,-1.33419863410883));
#61674=CARTESIAN_POINT('',(6.528,3.88135593761115,-2.2532687557348));
#61675=CARTESIAN_POINT('Origin',(6.528,0.,0.));
#61676=CARTESIAN_POINT('',(6.528,3.20158419452848,-1.87477113412423));
#61677=CARTESIAN_POINT('',(6.528,4.06890711782452,-2.35769745016552));
#61678=CARTESIAN_POINT('',(6.528,2.54018621271673,-2.70413797072631));
#61679=CARTESIAN_POINT('',(6.528,3.20158419452848,-1.87477113412423));
#61680=CARTESIAN_POINT('',(6.528,3.06045755186718,-3.28264277270907));
#61681=CARTESIAN_POINT('',(6.528,2.54018621271673,-2.70413797072631));
#61682=CARTESIAN_POINT('',(6.528,2.51932419206087,-3.71418222699114));
#61683=CARTESIAN_POINT('Origin',(6.528,0.,0.));
#61684=CARTESIAN_POINT('',(6.528,2.07109497757512,-3.07822574770973));
#61685=CARTESIAN_POINT('',(6.528,2.6429920541607,-3.88964463693579));
#61686=CARTESIAN_POINT('',(6.528,1.11534720250423,-3.53848961816564));
#61687=CARTESIAN_POINT('',(6.528,2.07109497757512,-3.07822574770973));
#61688=CARTESIAN_POINT('',(6.528,1.33309165535894,-4.28544170867046));
#61689=CARTESIAN_POINT('',(6.528,1.11534720250423,-3.53848961816564));
#61690=CARTESIAN_POINT('',(6.528,0.658309392789363,-4.43945635673618));
#61691=CARTESIAN_POINT('Origin',(6.528,0.,0.));
#61692=CARTESIAN_POINT('',(6.528,0.5304,-3.672));
#61693=CARTESIAN_POINT('',(6.528,0.693599999999999,-4.6512));
#61694=CARTESIAN_POINT('',(6.528,-0.5304,-3.672));
#61695=CARTESIAN_POINT('',(6.528,0.5304,-3.672));
#61696=CARTESIAN_POINT('',(6.528,-0.658309392789364,-4.43945635673618));
#61697=CARTESIAN_POINT('',(6.528,-0.5304,-3.672));
#61698=CARTESIAN_POINT('',(6.528,-1.33309165535895,-4.28544170867045));
#61699=CARTESIAN_POINT('Origin',(6.528,0.,0.));
#61700=CARTESIAN_POINT('',(6.528,-1.11534720250423,-3.53848961816564));
#61701=CARTESIAN_POINT('',(6.528,-1.39316804060647,-4.49152815983967));
#61702=CARTESIAN_POINT('',(6.528,-2.07109497757512,-3.07822574770973));
#61703=CARTESIAN_POINT('',(6.528,-1.11534720250423,-3.53848961816564));
#61704=CARTESIAN_POINT('',(6.528,-2.51932419206087,-3.71418222699114));
#61705=CARTESIAN_POINT('',(6.528,-2.07109497757512,-3.07822574770973));
#61706=CARTESIAN_POINT('',(6.528,-3.06045755186719,-3.28264277270907));
#61707=CARTESIAN_POINT('Origin',(6.528,0.,0.));
#61708=CARTESIAN_POINT('',(6.528,-2.54018621271673,-2.70413797072631));
#61709=CARTESIAN_POINT('',(6.528,-3.20400206468608,-3.44225408264517));
#61710=CARTESIAN_POINT('',(6.528,-3.20158419452848,-1.87477113412423));
#61711=CARTESIAN_POINT('',(6.528,-2.54018621271673,-2.70413797072631));
#61712=CARTESIAN_POINT('',(6.528,-3.88135593761115,-2.2532687557348));
#61713=CARTESIAN_POINT('',(6.528,-3.20158419452848,-1.87477113412423));
#61714=CARTESIAN_POINT('',(6.528,-4.18166229617943,-1.62967617664105));
#61715=CARTESIAN_POINT('Origin',(6.528,0.,0.));
#61716=CARTESIAN_POINT('',(6.528,-3.46191019016123,-1.33419863410883));
#61717=CARTESIAN_POINT('',(6.528,-4.380244185348,-1.71119936790692));
#61718=CARTESIAN_POINT('',(6.528,-3.69796039690208,-0.299995104866347));
#61719=CARTESIAN_POINT('',(6.528,-3.46191019016123,-1.33419863410883));
#61720=CARTESIAN_POINT('',(6.528,-4.47463753801084,-0.346067772877414));
#61721=CARTESIAN_POINT('',(6.528,-3.69796039690209,-0.299995104866347));
#61722=CARTESIAN_POINT('',(6.528,-4.47463753801084,0.346067772877414));
#61723=CARTESIAN_POINT('Origin',(6.528,0.,0.));
#61724=CARTESIAN_POINT('',(6.528,-3.69796039690209,0.299995104866347));
#61725=CARTESIAN_POINT('',(6.528,-4.6889252249322,0.358779368128297));
#61726=CARTESIAN_POINT('',(6.528,-3.46191019016123,1.33419863410883));
#61727=CARTESIAN_POINT('',(6.528,-3.69796039690209,0.299995104866347));
#61728=CARTESIAN_POINT('',(6.528,-4.18166229617943,1.62967617664105));
#61729=CARTESIAN_POINT('',(6.528,-3.46191019016123,1.33419863410883));
#61730=CARTESIAN_POINT('',(6.528,-3.88135593761115,2.2532687557348));
#61731=CARTESIAN_POINT('Origin',(6.528,0.,0.));
#61732=CARTESIAN_POINT('',(6.528,-3.20158419452848,1.87477113412423));
#61733=CARTESIAN_POINT('',(6.528,-4.06890711782452,2.35769745016552));
#61734=CARTESIAN_POINT('',(6.528,-2.54018621271673,2.70413797072631));
#61735=CARTESIAN_POINT('',(6.528,-3.20158419452848,1.87477113412423));
#61736=CARTESIAN_POINT('',(6.528,-3.06045755186718,3.28264277270907));
#61737=CARTESIAN_POINT('',(6.528,-2.54018621271673,2.70413797072631));
#61738=CARTESIAN_POINT('',(6.528,-2.51932419206087,3.71418222699114));
#61739=CARTESIAN_POINT('Origin',(6.528,0.,0.));
#61740=CARTESIAN_POINT('',(6.528,-2.07109497757512,3.07822574770973));
#61741=CARTESIAN_POINT('',(6.528,-2.6429920541607,3.88964463693579));
#61742=CARTESIAN_POINT('',(6.528,-1.11534720250423,3.53848961816564));
#61743=CARTESIAN_POINT('',(6.528,-2.07109497757512,3.07822574770973));
#61744=CARTESIAN_POINT('',(6.528,-1.33309165535894,4.28544170867046));
#61745=CARTESIAN_POINT('',(6.528,-1.11534720250423,3.53848961816564));
#61746=CARTESIAN_POINT('',(6.528,-0.658309392789364,4.43945635673618));
#61747=CARTESIAN_POINT('Origin',(6.528,0.,0.));
#61748=CARTESIAN_POINT('',(6.528,-0.5304,3.672));
#61749=CARTESIAN_POINT('',(6.528,-0.6936,4.6512));
#61750=CARTESIAN_POINT('',(6.528,0.5304,3.672));
#61751=CARTESIAN_POINT('',(6.528,-0.5304,3.672));
#61752=CARTESIAN_POINT('',(6.528,0.658309392789364,4.43945635673618));
#61753=CARTESIAN_POINT('',(6.528,0.5304,3.672));
#61754=CARTESIAN_POINT('',(6.528,1.33309165535895,4.28544170867045));
#61755=CARTESIAN_POINT('Origin',(6.528,0.,0.));
#61756=CARTESIAN_POINT('',(6.528,1.11534720250423,3.53848961816564));
#61757=CARTESIAN_POINT('',(6.528,1.39316804060647,4.49152815983967));
#61758=CARTESIAN_POINT('',(6.528,2.07109497757512,3.07822574770973));
#61759=CARTESIAN_POINT('',(6.528,1.11534720250423,3.53848961816564));
#61760=CARTESIAN_POINT('',(6.528,2.07109497757512,3.07822574770973));
#61761=CARTESIAN_POINT('Origin',(1.632,1.39316804060647,4.49152815983967));
#61762=CARTESIAN_POINT('',(1.632,1.33309165535895,4.28544170867045));
#61763=CARTESIAN_POINT('',(1.632,1.33309165535895,4.28544170867045));
#61764=CARTESIAN_POINT('',(1.632,1.11534720250423,3.53848961816564));
#61765=CARTESIAN_POINT('',(1.632,0.735220717938668,2.23450107296974));
#61766=CARTESIAN_POINT('',(1.632,1.11534720250423,3.53848961816564));
#61767=CARTESIAN_POINT('Origin',(1.632,2.07109497757512,3.07822574770973));
#61768=CARTESIAN_POINT('',(1.632,2.51932419206087,3.71418222699114));
#61769=CARTESIAN_POINT('',(1.632,2.51932419206087,3.71418222699114));
#61770=CARTESIAN_POINT('',(1.632,2.07109497757512,3.07822574770973));
#61771=CARTESIAN_POINT('',(1.632,2.07109497757512,3.07822574770973));
#61772=CARTESIAN_POINT('',(1.632,1.00265212841353,1.5622978904732));
#61773=CARTESIAN_POINT('Origin',(1.632,1.11534720250423,3.53848961816564));
#61774=CARTESIAN_POINT('',(1.632,1.35428414627195,3.42342365055166));
#61775=CARTESIAN_POINT('Origin',(1.632,0.,0.));
#61776=CARTESIAN_POINT('',(1.632,3.06045755186719,3.28264277270907));
#61777=CARTESIAN_POINT('Origin',(1.632,0.,0.));
#61778=CARTESIAN_POINT('',(1.632,3.06045755186719,3.28264277270907));
#61779=CARTESIAN_POINT('Origin',(1.632,3.20400206468608,3.44225408264517));
#61780=CARTESIAN_POINT('',(1.632,2.54018621271673,2.70413797072631));
#61781=CARTESIAN_POINT('',(1.632,1.63192465850191,1.69421558786437));
#61782=CARTESIAN_POINT('',(1.632,2.54018621271673,2.70413797072631));
#61783=CARTESIAN_POINT('Origin',(1.632,3.20158419452848,1.87477113412423));
#61784=CARTESIAN_POINT('',(1.632,3.88135593761115,2.2532687557348));
#61785=CARTESIAN_POINT('',(1.632,3.88135593761115,2.2532687557348));
#61786=CARTESIAN_POINT('',(1.632,3.20158419452848,1.87477113412423));
#61787=CARTESIAN_POINT('',(1.632,3.20158419452848,1.87477113412423));
#61788=CARTESIAN_POINT('',(1.632,1.58121400337067,0.972547307195736));
#61789=CARTESIAN_POINT('Origin',(1.632,2.54018621271673,2.70413797072631));
#61790=CARTESIAN_POINT('',(1.632,2.70553570816967,2.49679626157579));
#61791=CARTESIAN_POINT('Origin',(1.632,0.,0.));
#61792=CARTESIAN_POINT('',(1.632,4.18166229617943,1.62967617664105));
#61793=CARTESIAN_POINT('Origin',(1.632,0.,0.));
#61794=CARTESIAN_POINT('',(1.632,4.18166229617943,1.62967617664105));
#61795=CARTESIAN_POINT('Origin',(1.632,4.380244185348,1.71119936790692));
#61796=CARTESIAN_POINT('',(1.632,3.46191019016123,1.33419863410882));
#61797=CARTESIAN_POINT('',(1.632,2.20540590620635,0.818369927391835));
#61798=CARTESIAN_POINT('',(1.632,3.46191019016123,1.33419863410882));
#61799=CARTESIAN_POINT('Origin',(1.632,3.69796039690208,0.299995104866347));
#61800=CARTESIAN_POINT('',(1.632,4.47463753801084,0.346067772877413));
#61801=CARTESIAN_POINT('',(1.632,4.47463753801084,0.346067772877413));
#61802=CARTESIAN_POINT('',(1.632,3.69796039690208,0.299995104866347));
#61803=CARTESIAN_POINT('',(1.632,3.69796039690208,0.299995104866347));
#61804=CARTESIAN_POINT('',(1.632,1.84659705264313,0.190171802218178));
#61805=CARTESIAN_POINT('Origin',(1.632,3.46191019016123,1.33419863410882));
#61806=CARTESIAN_POINT('',(1.632,3.52092274184644,1.07564775179821));
#61807=CARTESIAN_POINT('Origin',(1.632,0.,0.));
#61808=CARTESIAN_POINT('',(1.632,4.47463753801084,-0.346067772877415));
#61809=CARTESIAN_POINT('Origin',(1.632,0.,0.));
#61810=CARTESIAN_POINT('',(1.632,4.47463753801084,-0.346067772877415));
#61811=CARTESIAN_POINT('Origin',(1.632,4.6889252249322,-0.358779368128298));
#61812=CARTESIAN_POINT('',(1.632,3.69796039690209,-0.299995104866348));
#61813=CARTESIAN_POINT('',(1.632,2.34207946665818,-0.219563933849153));
#61814=CARTESIAN_POINT('',(1.632,3.69796039690209,-0.299995104866348));
#61815=CARTESIAN_POINT('Origin',(1.632,3.46191019016123,-1.33419863410883));
#61816=CARTESIAN_POINT('',(1.632,4.18166229617943,-1.62967617664105));
#61817=CARTESIAN_POINT('',(1.632,4.18166229617943,-1.62967617664105));
#61818=CARTESIAN_POINT('',(1.632,3.46191019016123,-1.33419863410883));
#61819=CARTESIAN_POINT('',(1.632,3.46191019016123,-1.33419863410883));
#61820=CARTESIAN_POINT('',(1.632,1.74623890861297,-0.629869560492788));
#61821=CARTESIAN_POINT('Origin',(1.632,3.69796039690209,-0.299995104866348));
#61822=CARTESIAN_POINT('',(1.632,3.63894784521687,-0.558545987176968));
#61823=CARTESIAN_POINT('Origin',(1.632,0.,0.));
#61824=CARTESIAN_POINT('',(1.632,3.88135593761115,-2.2532687557348));
#61825=CARTESIAN_POINT('Origin',(1.632,0.,0.));
#61826=CARTESIAN_POINT('',(1.632,3.88135593761115,-2.2532687557348));
#61827=CARTESIAN_POINT('Origin',(1.632,4.06890711782452,-2.35769745016552));
#61828=CARTESIAN_POINT('',(1.632,3.20158419452848,-1.87477113412423));
#61829=CARTESIAN_POINT('',(1.632,2.01487546501869,-1.21401046521638));
#61830=CARTESIAN_POINT('',(1.632,3.20158419452848,-1.87477113412423));
#61831=CARTESIAN_POINT('Origin',(1.632,2.54018621271673,-2.70413797072631));
#61832=CARTESIAN_POINT('',(1.632,3.06045755186718,-3.28264277270907));
#61833=CARTESIAN_POINT('',(1.632,3.06045755186718,-3.28264277270907));
#61834=CARTESIAN_POINT('',(1.632,2.54018621271673,-2.70413797072631));
#61835=CARTESIAN_POINT('',(1.632,2.54018621271673,-2.70413797072631));
#61836=CARTESIAN_POINT('',(1.632,1.30001673251724,-1.32515753190494));
#61837=CARTESIAN_POINT('Origin',(1.632,3.20158419452848,-1.87477113412423));
#61838=CARTESIAN_POINT('',(1.632,3.03623469907554,-2.08211284327475));
#61839=CARTESIAN_POINT('Origin',(1.632,0.,0.));
#61840=CARTESIAN_POINT('',(1.632,2.51932419206087,-3.71418222699114));
#61841=CARTESIAN_POINT('Origin',(1.632,0.,0.));
#61842=CARTESIAN_POINT('',(1.632,2.51932419206087,-3.71418222699114));
#61843=CARTESIAN_POINT('Origin',(1.632,2.6429920541607,-3.88964463693579));
#61844=CARTESIAN_POINT('',(1.632,2.07109497757512,-3.07822574770973));
#61845=CARTESIAN_POINT('',(1.632,1.28860066670632,-1.96800733508623));
#61846=CARTESIAN_POINT('',(1.632,2.07109497757512,-3.07822574770973));
#61847=CARTESIAN_POINT('Origin',(1.632,1.11534720250423,-3.53848961816564));
#61848=CARTESIAN_POINT('',(1.632,1.33309165535894,-4.28544170867046));
#61849=CARTESIAN_POINT('',(1.632,1.33309165535894,-4.28544170867046));
#61850=CARTESIAN_POINT('',(1.632,1.11534720250423,-3.53848961816564));
#61851=CARTESIAN_POINT('',(1.632,1.11534720250423,-3.53848961816564));
#61852=CARTESIAN_POINT('',(1.632,0.596310298887548,-1.75798180213273));
#61853=CARTESIAN_POINT('Origin',(1.632,2.07109497757512,-3.07822574770973));
#61854=CARTESIAN_POINT('',(1.632,1.83215803380739,-3.19329171532371));
#61855=CARTESIAN_POINT('Origin',(1.632,0.,0.));
#61856=CARTESIAN_POINT('',(1.632,0.658309392789363,-4.43945635673618));
#61857=CARTESIAN_POINT('Origin',(1.632,0.,0.));
#61858=CARTESIAN_POINT('',(1.632,0.658309392789363,-4.43945635673618));
#61859=CARTESIAN_POINT('Origin',(1.632,0.693599999999999,-4.6512));
#61860=CARTESIAN_POINT('',(1.632,0.5304,-3.672));
#61861=CARTESIAN_POINT('',(1.632,0.307102702702703,-2.33221621621622));
#61862=CARTESIAN_POINT('',(1.632,0.5304,-3.672));
#61863=CARTESIAN_POINT('Origin',(1.632,-0.5304,-3.672));
#61864=CARTESIAN_POINT('',(1.632,-0.658309392789364,-4.43945635673618));
#61865=CARTESIAN_POINT('',(1.632,-0.658309392789364,-4.43945635673618));
#61866=CARTESIAN_POINT('',(1.632,-0.5304,-3.672));
#61867=CARTESIAN_POINT('',(1.632,-0.5304,-3.672));
#61868=CARTESIAN_POINT('',(1.632,-0.225502702702703,-1.84261621621622));
#61869=CARTESIAN_POINT('Origin',(1.632,0.5304,-3.672));
#61870=CARTESIAN_POINT('',(1.632,0.2652,-3.672));
#61871=CARTESIAN_POINT('Origin',(1.632,0.,0.));
#61872=CARTESIAN_POINT('',(1.632,-1.33309165535895,-4.28544170867045));
#61873=CARTESIAN_POINT('Origin',(1.632,0.,0.));
#61874=CARTESIAN_POINT('',(1.632,-1.33309165535895,-4.28544170867045));
#61875=CARTESIAN_POINT('Origin',(1.632,-1.39316804060647,-4.49152815983967));
#61876=CARTESIAN_POINT('',(1.632,-1.11534720250423,-3.53848961816564));
#61877=CARTESIAN_POINT('',(1.632,-0.735220717938668,-2.23450107296974));
#61878=CARTESIAN_POINT('',(1.632,-1.11534720250423,-3.53848961816564));
#61879=CARTESIAN_POINT('Origin',(1.632,-2.07109497757512,-3.07822574770973));
#61880=CARTESIAN_POINT('',(1.632,-2.51932419206087,-3.71418222699114));
#61881=CARTESIAN_POINT('',(1.632,-2.51932419206087,-3.71418222699114));
#61882=CARTESIAN_POINT('',(1.632,-2.07109497757512,-3.07822574770973));
#61883=CARTESIAN_POINT('',(1.632,-2.07109497757512,-3.07822574770973));
#61884=CARTESIAN_POINT('',(1.632,-1.00265212841353,-1.5622978904732));
#61885=CARTESIAN_POINT('Origin',(1.632,-1.11534720250423,-3.53848961816564));
#61886=CARTESIAN_POINT('',(1.632,-1.35428414627195,-3.42342365055166));
#61887=CARTESIAN_POINT('Origin',(1.632,0.,0.));
#61888=CARTESIAN_POINT('',(1.632,-3.06045755186719,-3.28264277270907));
#61889=CARTESIAN_POINT('Origin',(1.632,0.,0.));
#61890=CARTESIAN_POINT('',(1.632,-3.06045755186719,-3.28264277270907));
#61891=CARTESIAN_POINT('Origin',(1.632,-3.20400206468608,-3.44225408264517));
#61892=CARTESIAN_POINT('',(1.632,-2.54018621271673,-2.70413797072631));
#61893=CARTESIAN_POINT('',(1.632,-1.63192465850191,-1.69421558786437));
#61894=CARTESIAN_POINT('',(1.632,-2.54018621271673,-2.70413797072631));
#61895=CARTESIAN_POINT('Origin',(1.632,-3.20158419452848,-1.87477113412423));
#61896=CARTESIAN_POINT('',(1.632,-3.88135593761115,-2.2532687557348));
#61897=CARTESIAN_POINT('',(1.632,-3.88135593761115,-2.2532687557348));
#61898=CARTESIAN_POINT('',(1.632,-3.20158419452848,-1.87477113412423));
#61899=CARTESIAN_POINT('',(1.632,-3.20158419452848,-1.87477113412423));
#61900=CARTESIAN_POINT('',(1.632,-1.58121400337067,-0.972547307195736));
#61901=CARTESIAN_POINT('Origin',(1.632,-2.54018621271673,-2.70413797072631));
#61902=CARTESIAN_POINT('',(1.632,-2.70553570816967,-2.49679626157579));
#61903=CARTESIAN_POINT('Origin',(1.632,0.,0.));
#61904=CARTESIAN_POINT('',(1.632,-4.18166229617943,-1.62967617664105));
#61905=CARTESIAN_POINT('Origin',(1.632,0.,0.));
#61906=CARTESIAN_POINT('',(1.632,-4.18166229617943,-1.62967617664105));
#61907=CARTESIAN_POINT('Origin',(1.632,-4.380244185348,-1.71119936790692));
#61908=CARTESIAN_POINT('',(1.632,-3.46191019016123,-1.33419863410883));
#61909=CARTESIAN_POINT('',(1.632,-2.20540590620635,-0.818369927391835));
#61910=CARTESIAN_POINT('',(1.632,-3.46191019016123,-1.33419863410883));
#61911=CARTESIAN_POINT('Origin',(1.632,-3.69796039690209,-0.299995104866347));
#61912=CARTESIAN_POINT('',(1.632,-4.47463753801084,-0.346067772877414));
#61913=CARTESIAN_POINT('',(1.632,-4.47463753801084,-0.346067772877414));
#61914=CARTESIAN_POINT('',(1.632,-3.69796039690209,-0.299995104866347));
#61915=CARTESIAN_POINT('',(1.632,-3.69796039690209,-0.299995104866347));
#61916=CARTESIAN_POINT('',(1.632,-1.84659705264313,-0.190171802218178));
#61917=CARTESIAN_POINT('Origin',(1.632,-3.46191019016123,-1.33419863410883));
#61918=CARTESIAN_POINT('',(1.632,-3.52092274184644,-1.07564775179821));
#61919=CARTESIAN_POINT('Origin',(1.632,0.,0.));
#61920=CARTESIAN_POINT('',(1.632,-4.47463753801084,0.346067772877414));
#61921=CARTESIAN_POINT('Origin',(1.632,0.,0.));
#61922=CARTESIAN_POINT('',(1.632,-4.47463753801084,0.346067772877414));
#61923=CARTESIAN_POINT('Origin',(1.632,-4.6889252249322,0.358779368128297));
#61924=CARTESIAN_POINT('',(1.632,-3.69796039690209,0.299995104866347));
#61925=CARTESIAN_POINT('',(1.632,-2.34207946665818,0.219563933849153));
#61926=CARTESIAN_POINT('',(1.632,-3.69796039690209,0.299995104866347));
#61927=CARTESIAN_POINT('Origin',(1.632,-3.46191019016123,1.33419863410883));
#61928=CARTESIAN_POINT('',(1.632,-4.18166229617943,1.62967617664105));
#61929=CARTESIAN_POINT('',(1.632,-4.18166229617943,1.62967617664105));
#61930=CARTESIAN_POINT('',(1.632,-3.46191019016123,1.33419863410883));
#61931=CARTESIAN_POINT('',(1.632,-3.46191019016123,1.33419863410883));
#61932=CARTESIAN_POINT('',(1.632,-1.74623890861297,0.629869560492787));
#61933=CARTESIAN_POINT('Origin',(1.632,-3.69796039690209,0.299995104866347));
#61934=CARTESIAN_POINT('',(1.632,-3.63894784521687,0.558545987176967));
#61935=CARTESIAN_POINT('Origin',(1.632,0.,0.));
#61936=CARTESIAN_POINT('',(1.632,-3.88135593761115,2.2532687557348));
#61937=CARTESIAN_POINT('Origin',(1.632,0.,0.));
#61938=CARTESIAN_POINT('',(1.632,-3.88135593761115,2.2532687557348));
#61939=CARTESIAN_POINT('Origin',(1.632,-4.06890711782452,2.35769745016552));
#61940=CARTESIAN_POINT('',(1.632,-3.20158419452848,1.87477113412423));
#61941=CARTESIAN_POINT('',(1.632,-2.01487546501869,1.21401046521638));
#61942=CARTESIAN_POINT('',(1.632,-3.20158419452848,1.87477113412423));
#61943=CARTESIAN_POINT('Origin',(1.632,-2.54018621271673,2.70413797072631));
#61944=CARTESIAN_POINT('',(1.632,-3.06045755186718,3.28264277270907));
#61945=CARTESIAN_POINT('',(1.632,-3.06045755186718,3.28264277270907));
#61946=CARTESIAN_POINT('',(1.632,-2.54018621271673,2.70413797072631));
#61947=CARTESIAN_POINT('',(1.632,-2.54018621271673,2.70413797072631));
#61948=CARTESIAN_POINT('',(1.632,-1.30001673251724,1.32515753190494));
#61949=CARTESIAN_POINT('Origin',(1.632,-3.20158419452848,1.87477113412423));
#61950=CARTESIAN_POINT('',(1.632,-3.03623469907554,2.08211284327475));
#61951=CARTESIAN_POINT('Origin',(1.632,0.,0.));
#61952=CARTESIAN_POINT('',(1.632,-2.51932419206087,3.71418222699114));
#61953=CARTESIAN_POINT('Origin',(1.632,0.,0.));
#61954=CARTESIAN_POINT('',(1.632,-2.51932419206087,3.71418222699114));
#61955=CARTESIAN_POINT('Origin',(1.632,-2.6429920541607,3.88964463693579));
#61956=CARTESIAN_POINT('',(1.632,-2.07109497757512,3.07822574770973));
#61957=CARTESIAN_POINT('',(1.632,-1.28860066670632,1.96800733508623));
#61958=CARTESIAN_POINT('',(1.632,-2.07109497757512,3.07822574770973));
#61959=CARTESIAN_POINT('Origin',(1.632,-1.11534720250423,3.53848961816564));
#61960=CARTESIAN_POINT('',(1.632,-1.33309165535894,4.28544170867046));
#61961=CARTESIAN_POINT('',(1.632,-1.33309165535894,4.28544170867046));
#61962=CARTESIAN_POINT('',(1.632,-1.11534720250423,3.53848961816564));
#61963=CARTESIAN_POINT('',(1.632,-1.11534720250423,3.53848961816564));
#61964=CARTESIAN_POINT('',(1.632,-0.596310298887548,1.75798180213273));
#61965=CARTESIAN_POINT('Origin',(1.632,-2.07109497757512,3.07822574770973));
#61966=CARTESIAN_POINT('',(1.632,-1.83215803380739,3.19329171532371));
#61967=CARTESIAN_POINT('Origin',(1.632,0.,0.));
#61968=CARTESIAN_POINT('',(1.632,-0.658309392789364,4.43945635673618));
#61969=CARTESIAN_POINT('Origin',(1.632,0.,0.));
#61970=CARTESIAN_POINT('',(1.632,-0.658309392789364,4.43945635673618));
#61971=CARTESIAN_POINT('Origin',(1.632,0.5304,3.672));
#61972=CARTESIAN_POINT('',(1.632,0.658309392789364,4.43945635673618));
#61973=CARTESIAN_POINT('',(1.632,0.658309392789364,4.43945635673618));
#61974=CARTESIAN_POINT('',(1.632,0.5304,3.672));
#61975=CARTESIAN_POINT('',(1.632,0.5304,3.672));
#61976=CARTESIAN_POINT('',(1.632,0.225502702702703,1.84261621621622));
#61977=CARTESIAN_POINT('Origin',(1.632,-0.6936,4.6512));
#61978=CARTESIAN_POINT('',(1.632,-0.5304,3.672));
#61979=CARTESIAN_POINT('',(1.632,-0.307102702702703,2.33221621621622));
#61980=CARTESIAN_POINT('',(1.632,-0.5304,3.672));
#61981=CARTESIAN_POINT('Origin',(1.632,-0.5304,3.672));
#61982=CARTESIAN_POINT('',(1.632,-0.2652,3.672));
#61983=CARTESIAN_POINT('Origin',(1.632,0.,0.));
#61984=CARTESIAN_POINT('Origin',(1.632,0.,0.));
#61985=CARTESIAN_POINT('',(1.632,-2.448,-2.99793536431272E-16));
#61986=CARTESIAN_POINT('Origin',(1.632,0.,0.));
#61987=CARTESIAN_POINT('Origin',(1.632,0.,0.));
#61988=CARTESIAN_POINT('Origin',(3.264,0.,0.));
#61989=CARTESIAN_POINT('',(3.264,-2.448,-2.99793536431272E-16));
#61990=CARTESIAN_POINT('',(0.,0.,0.));
#61991=CARTESIAN_POINT('Origin',(-1.72497344927317,0.,0.));
#61992=CARTESIAN_POINT('',(1.21707771886868,1.78943621037804,2.68030513402633));
#61993=CARTESIAN_POINT('',(0.970338898719273,1.78943621037804,2.68030513402633));
#61994=CARTESIAN_POINT('',(-1.72497344927317,1.78943621037804,2.68030513402633));
#61995=CARTESIAN_POINT('',(0.58586766091457,-1.87152408986075,-2.62364539211588));
#61996=CARTESIAN_POINT('Ctrl Pts',(0.58586766091457,-1.87152408986075,-2.62364539211588));
#61997=CARTESIAN_POINT('Ctrl Pts',(0.59198764571749,-1.79127517131912,-2.68088932633323));
#61998=CARTESIAN_POINT('Ctrl Pts',(0.59810763052041,-1.70824895664009,-2.73455380169506));
#61999=CARTESIAN_POINT('Ctrl Pts',(0.60422761532333,-1.62280149583887,-2.78435501824088));
#62000=CARTESIAN_POINT('Ctrl Pts',(0.61033956178225,-1.53746626670259,-2.83409082297227));
#62001=CARTESIAN_POINT('Ctrl Pts',(0.616451508241169,-1.44971648895612,
-2.87997323007931));
#62002=CARTESIAN_POINT('Ctrl Pts',(0.622563454700089,-1.35993908319214,
-2.92176030031667));
#62003=CARTESIAN_POINT('Ctrl Pts',(0.62880158690121,-1.2683081552065,-2.9644100961207));
#62004=CARTESIAN_POINT('Ctrl Pts',(0.635039719102331,-1.17456531372328,
-3.00279328572004));
#62005=CARTESIAN_POINT('Ctrl Pts',(0.641277851303452,-1.07915085300422,
-3.03670067655017));
#62006=CARTESIAN_POINT('Ctrl Pts',(0.647379645712096,-0.985821727530616,
-3.06986700280113));
#62007=CARTESIAN_POINT('Ctrl Pts',(0.65348144012074,-0.89089374539159,-3.09875102118765));
#62008=CARTESIAN_POINT('Ctrl Pts',(0.659583234529385,-0.794800091963228,
-3.12320514476959));
#62009=CARTESIAN_POINT('Ctrl Pts',(0.665683183521829,-0.698735500934035,
-3.14765187248848));
#62010=CARTESIAN_POINT('Ctrl Pts',(0.671783132514273,-0.601506367318778,
-3.16767125788266));
#62011=CARTESIAN_POINT('Ctrl Pts',(0.677883081506717,-0.503560139985367,
-3.18316583732578));
#62012=CARTESIAN_POINT('Ctrl Pts',(0.683982884505863,-0.405616256850698,
-3.19866004592895));
#62013=CARTESIAN_POINT('Ctrl Pts',(0.690082687505009,-0.30695575120951,
-3.20962959565981));
#62014=CARTESIAN_POINT('Ctrl Pts',(0.696182490504155,-0.208034236627888,
-3.21602850094502));
#62015=CARTESIAN_POINT('Ctrl Pts',(0.702523835256058,-0.105195599473501,
-3.22268079192129));
#62016=CARTESIAN_POINT('Ctrl Pts',(0.708865180007961,-0.00207536863801527,
-3.22439290423859));
#62017=CARTESIAN_POINT('Ctrl Pts',(0.715206524759864,0.100812806682847,
-3.22117282065224));
#62018=CARTESIAN_POINT('Ctrl Pts',(0.721314650644506,0.19991701115185,-3.21807116372079));
#62019=CARTESIAN_POINT('Ctrl Pts',(0.727422776529149,0.29880548247049,-3.21039382167964));
#62020=CARTESIAN_POINT('Ctrl Pts',(0.733530902413792,0.397024509110286,
-3.19820091640062));
#62021=CARTESIAN_POINT('Ctrl Pts',(0.739643164081569,0.495310039388279,
-3.18599975536312));
#62022=CARTESIAN_POINT('Ctrl Pts',(0.745755425749347,0.59292478846357,-3.16927702307148));
#62023=CARTESIAN_POINT('Ctrl Pts',(0.751867687417125,0.689425970731327,
-3.14814380125514));
#62024=CARTESIAN_POINT('Ctrl Pts',(0.757988843515511,0.786067579426479,
-3.12697982683278));
#62025=CARTESIAN_POINT('Ctrl Pts',(0.764109999613896,0.881591964901016,
-3.10139267837718));
#62026=CARTESIAN_POINT('Ctrl Pts',(0.770231155712282,0.975572625816714,
-3.07154287195492));
#62027=CARTESIAN_POINT('Ctrl Pts',(0.770913646317185,0.986051188540249,
-3.06821470777909));
#62028=CARTESIAN_POINT('Ctrl Pts',(0.771596136922087,0.99651058265728,-3.06483360044361));
#62029=CARTESIAN_POINT('Ctrl Pts',(0.77227862752699,1.00695023444242,-3.06139980856084));
#62030=CARTESIAN_POINT('Ctrl Pts',(0.778461682484641,1.10152873891206,-3.03029121340689));
#62031=CARTESIAN_POINT('Ctrl Pts',(0.784644737442292,1.19482414783666,-2.99474310349924));
#62032=CARTESIAN_POINT('Ctrl Pts',(0.790827792399944,1.2863904560637,-2.95488022719166));
#62033=CARTESIAN_POINT('Ctrl Pts',(0.797002694600637,1.3778360282045,-2.91506991265887));
#62034=CARTESIAN_POINT('Ctrl Pts',(0.80317759680133,1.4675566384062,-2.87095631233905));
#62035=CARTESIAN_POINT('Ctrl Pts',(0.809352499002023,1.55512216672304,-2.82271369590801));
#62036=CARTESIAN_POINT('Ctrl Pts',(0.815521064788214,1.64259783912549,-2.77452058393946));
#62037=CARTESIAN_POINT('Ctrl Pts',(0.821689630574404,1.72792244976038,-2.72220708804443));
#62038=CARTESIAN_POINT('Ctrl Pts',(0.827858196360595,1.81068744465614,-2.66599485000715));
#62039=CARTESIAN_POINT('Ctrl Pts',(0.834022504977734,1.8933953201846,-2.6098214062388));
#62040=CARTESIAN_POINT('Ctrl Pts',(0.840186813594873,1.97354673523881,-2.54975481228269));
#62041=CARTESIAN_POINT('Ctrl Pts',(0.846351122212013,2.05076003749252,-2.48606130880227));
#62042=CARTESIAN_POINT('Ctrl Pts',(0.852513243557509,2.12794594227525,-2.42239040558453));
#62043=CARTESIAN_POINT('Ctrl Pts',(0.858675364903006,2.20219547258825,-2.35509542523953));
#62044=CARTESIAN_POINT('Ctrl Pts',(0.864837486248502,2.27315885622364,-2.28448383160662));
#62045=CARTESIAN_POINT('Ctrl Pts',(0.870999052686446,2.34411584950814,-2.21387859664541));
#62046=CARTESIAN_POINT('Ctrl Pts',(0.87716061912439,2.4117869778883,-2.13995764742067));
#62047=CARTESIAN_POINT('Ctrl Pts',(0.883322185562333,2.4758589676832,-2.06306566416164));
#62048=CARTESIAN_POINT('Ctrl Pts',(0.889484828557319,2.53994215222094,-1.98616024623353));
#62049=CARTESIAN_POINT('Ctrl Pts',(0.895647471552306,2.60042467190617,-1.90628309533125));
#62050=CARTESIAN_POINT('Ctrl Pts',(0.901810114547291,2.65703385441066,-1.82381157442748));
#62051=CARTESIAN_POINT('Ctrl Pts',(0.907979443228864,2.71370445070343,-1.7412505823761));
#62052=CARTESIAN_POINT('Ctrl Pts',(0.914148771910437,2.76649307349234,-1.6560899573173));
#62053=CARTESIAN_POINT('Ctrl Pts',(0.92031810059201,2.81517075098734,-1.56873554345064));
#62054=CARTESIAN_POINT('Ctrl Pts',(0.926490943813296,2.86387615915443,-1.48133136557036));
#62055=CARTESIAN_POINT('Ctrl Pts',(0.932663787034581,2.90846576506642,-1.39173129711002));
#62056=CARTESIAN_POINT('Ctrl Pts',(0.938836630255866,2.9487578174585,-1.30036337093806));
#62057=CARTESIAN_POINT('Ctrl Pts',(0.945019777252445,2.98911712577124,-1.20884293245587));
#62058=CARTESIAN_POINT('Ctrl Pts',(0.951202924249024,3.02516439562367,-1.11554914552634));
#62059=CARTESIAN_POINT('Ctrl Pts',(0.957386071245603,3.05676697446734,-1.02092763029796));
#62060=CARTESIAN_POINT('Ctrl Pts',(0.961965996252608,3.08017535230666,-0.950840432947641));
#62061=CARTESIAN_POINT('Ctrl Pts',(0.966545921259613,3.10114617417517,-0.880025126616937));
#62062=CARTESIAN_POINT('Ctrl Pts',(0.971125846266619,3.11964365813319,-0.808666191187291));
#62063=CARTESIAN_POINT('Ctrl Pts',(0.9772898628455,3.14453899978408,-0.712625828000808));
#62064=CARTESIAN_POINT('Ctrl Pts',(0.983453879424382,3.16504011821803,-0.615261367917324));
#62065=CARTESIAN_POINT('Ctrl Pts',(0.989617896003263,3.18100867365013,-0.517011973422887));
#62066=CARTESIAN_POINT('Ctrl Pts',(0.995773445998527,3.19695529547643,-0.418897529362669));
#62067=CARTESIAN_POINT('Ctrl Pts',(1.00192899599379,3.20838165831193,-0.319900992765871));
#62068=CARTESIAN_POINT('Ctrl Pts',(1.00808454598905,3.21519955765861,-0.220475320459806));
#62069=CARTESIAN_POINT('Ctrl Pts',(1.01423347326855,3.22201012167221,-0.121156619580885));
#62070=CARTESIAN_POINT('Ctrl Pts',(1.02038240054804,3.22422204917994,-0.0214101330237101));
#62071=CARTESIAN_POINT('Ctrl Pts',(1.02653132782754,3.22179858874209,0.0783033593116213));
#62072=CARTESIAN_POINT('Ctrl Pts',(1.0326756475632,3.21937694426329,0.177942133852175));
#62073=CARTESIAN_POINT('Ctrl Pts',(1.03881996729886,3.21232682783494,0.277547529115844));
#62074=CARTESIAN_POINT('Ctrl Pts',(1.04496428703453,3.20066353678552,0.376656988242065));
#62075=CARTESIAN_POINT('Ctrl Pts',(1.05110621065712,3.18900479409382,0.475727797447691));
#62076=CARTESIAN_POINT('Ctrl Pts',(1.05724813427972,3.1727365019672,0.574302622559335));
#62077=CARTESIAN_POINT('Ctrl Pts',(1.06339005790232,3.15192589226522,0.671923159422321));
#62078=CARTESIAN_POINT('Ctrl Pts',(1.06953124130622,3.13111779063779,0.769531931152668));
#62079=CARTESIAN_POINT('Ctrl Pts',(1.07567242471013,3.1057685505429,0.866186217138891));
#62080=CARTESIAN_POINT('Ctrl Pts',(1.08181360811403,3.07599649092961,0.96143806367792));
#62081=CARTESIAN_POINT('Ctrl Pts',(1.08795570614685,3.04621999725459,1.05670409642284));
#62082=CARTESIAN_POINT('Ctrl Pts',(1.09409780417966,3.01201950586568,1.15056685899043));
#62083=CARTESIAN_POINT('Ctrl Pts',(1.10023990221247,2.97356284238373,1.24259469856217));
#62084=CARTESIAN_POINT('Ctrl Pts',(1.10638856068393,2.93506510294043,1.33472083402439));
#62085=CARTESIAN_POINT('Ctrl Pts',(1.11253721915539,2.89230228172724,1.42500772996328));
#62086=CARTESIAN_POINT('Ctrl Pts',(1.11868587762685,2.84548985531016,1.51304495829667));
#62087=CARTESIAN_POINT('Ctrl Pts',(1.12483794886281,2.79865144602419,1.60113105100084));
#62088=CARTESIAN_POINT('Ctrl Pts',(1.13099002009876,2.74775917783632,1.68696461480813));
#62089=CARTESIAN_POINT('Ctrl Pts',(1.13714209133472,2.69307278616028,1.77016285435632));
#62090=CARTESIAN_POINT('Ctrl Pts',(1.14330451496477,2.63829437099227,1.85350109569095));
#62091=CARTESIAN_POINT('Ctrl Pts',(1.14946693859481,2.57970933561407,1.93419480215496));
#62092=CARTESIAN_POINT('Ctrl Pts',(1.15562936222486,2.51761882014655,2.01189289947151));
#62093=CARTESIAN_POINT('Ctrl Pts',(1.16041059648533,2.46944470593019,2.07217645463832));
#62094=CARTESIAN_POINT('Ctrl Pts',(1.1651918307458,2.41916124120921,2.13065737238373));
#62095=CARTESIAN_POINT('Ctrl Pts',(1.16997306500627,2.36692389664468,2.18718742452318));
#62096=CARTESIAN_POINT('Ctrl Pts',(1.17614724738719,2.29946790623175,2.26018674497009));
#62097=CARTESIAN_POINT('Ctrl Pts',(1.1823214297681,2.22851335131468,2.33019050162449));
#62098=CARTESIAN_POINT('Ctrl Pts',(1.18849561214902,2.1543568113567,2.39684465325998));
#62099=CARTESIAN_POINT('Ctrl Pts',(1.19466057704773,2.08031098024166,2.46339929642315));
#62100=CARTESIAN_POINT('Ctrl Pts',(1.20082554194645,2.00307299067149,2.5266139917632));
#62101=CARTESIAN_POINT('Ctrl Pts',(1.20699050684516,1.92297788170925,2.58616968293981));
#62102=CARTESIAN_POINT('Ctrl Pts',(1.210352910853,1.87929359156197,2.61865166750778));
#62103=CARTESIAN_POINT('Ctrl Pts',(1.21371531486084,1.83476007336656,2.65004583235345));
#62104=CARTESIAN_POINT('Ctrl Pts',(1.21707771886868,1.78943621037804,2.68030513402633));
#62105=CARTESIAN_POINT('',(0.585799999999996,1.87158653173902,-2.62360084935058));
#62106=CARTESIAN_POINT('Origin',(0.585799999999996,0.,0.));
#62107=CARTESIAN_POINT('Ctrl Pts',(0.585799999999996,1.87158653173884,-2.62360084935071));
#62108=CARTESIAN_POINT('Ctrl Pts',(0.592116907679877,1.95489173876411,-2.56417378233677));
#62109=CARTESIAN_POINT('Ctrl Pts',(0.598433815359758,2.03541956961639,-2.5007358573198));
#62110=CARTESIAN_POINT('Ctrl Pts',(0.604750723039639,2.11277861187854,-2.43357434644775));
#62111=CARTESIAN_POINT('Ctrl Pts',(0.611063991591541,2.19009308811734,-2.36645152686989));
#62112=CARTESIAN_POINT('Ctrl Pts',(0.617377260143442,2.26424210505644,-2.29560965736233));
#62113=CARTESIAN_POINT('Ctrl Pts',(0.623690528695344,2.3348670426893,-2.22137647765149));
#62114=CARTESIAN_POINT('Ctrl Pts',(0.630001626341581,2.40546769494986,-2.14716882405743));
#62115=CARTESIAN_POINT('Ctrl Pts',(0.636312723987817,2.4725464023986,-2.06957247583033));
#62116=CARTESIAN_POINT('Ctrl Pts',(0.642623821634054,2.53578159308669,-1.98895180300145));
#62117=CARTESIAN_POINT('Ctrl Pts',(0.648935997183835,2.59902758402538,-1.9083173605696));
#62118=CARTESIAN_POINT('Ctrl Pts',(0.655248172733616,2.65842849049503,-1.8246578754955));
#62119=CARTESIAN_POINT('Ctrl Pts',(0.661560348283396,2.71370335737527,-1.73837040088416));
#62120=CARTESIAN_POINT('Ctrl Pts',(0.667873475567062,2.76898655846033,-1.65206991606536));
#62121=CARTESIAN_POINT('Ctrl Pts',(0.674186602850728,2.8201422624078,-1.5631409939926));
#62122=CARTESIAN_POINT('Ctrl Pts',(0.680499730134394,2.86693369117845,-1.47200841467904));
#62123=CARTESIAN_POINT('Ctrl Pts',(0.686815142455302,2.91374205611284,-1.38084284991654));
#62124=CARTESIAN_POINT('Ctrl Pts',(0.693130554776209,2.95618281591122,-1.28747240051333));
#62125=CARTESIAN_POINT('Ctrl Pts',(0.699445967097116,2.9940661496825,-1.19234451976995));
#62126=CARTESIAN_POINT('Ctrl Pts',(0.705764999607745,3.03197119935269,-1.09716210878236));
#62127=CARTESIAN_POINT('Ctrl Pts',(0.712084032118375,3.06531347215733,-1.0002206370582));
#62128=CARTESIAN_POINT('Ctrl Pts',(0.718403064629004,3.09395229576761,-0.901984896777288));
#62129=CARTESIAN_POINT('Ctrl Pts',(0.724731470229132,3.12263359965576,-0.803603442356719));
#62130=CARTESIAN_POINT('Ctrl Pts',(0.731059875829262,3.14659740761162,-0.703924274890147));
#62131=CARTESIAN_POINT('Ctrl Pts',(0.737388281429391,3.16575359991218,-0.603424980542821));
#62132=CARTESIAN_POINT('Ctrl Pts',(0.74372187585346,3.1849254988718,-0.50284328421663));
#62133=CARTESIAN_POINT('Ctrl Pts',(0.75005547027753,3.1992818684031,-0.40144052147717));
#62134=CARTESIAN_POINT('Ctrl Pts',(0.756389064701599,3.20878440969236,-0.299700141166575));
#62135=CARTESIAN_POINT('Ctrl Pts',(0.762733850894677,3.21830374243367,-0.19777998066182));
#62136=CARTESIAN_POINT('Ctrl Pts',(0.769078637087755,3.22295209404247,-0.0955214153485939));
#62137=CARTESIAN_POINT('Ctrl Pts',(0.775423423280833,3.22274326031057,0.00659095007003059));
#62138=CARTESIAN_POINT('Ctrl Pts',(0.7784980217671,3.2226420622786,0.0560732359329862));
#62139=CARTESIAN_POINT('Ctrl Pts',(0.781572620253367,3.22140106071772,0.105521249986489));
#62140=CARTESIAN_POINT('Ctrl Pts',(0.784647218739633,3.21902619190892,0.154880400000556));
#62141=CARTESIAN_POINT('Ctrl Pts',(0.790757168417377,3.21430676952652,0.252968629754527));
#62142=CARTESIAN_POINT('Ctrl Pts',(0.796867118095121,3.20508966068731,0.351050336190424));
#62143=CARTESIAN_POINT('Ctrl Pts',(0.802977067772864,3.19136495852951,0.448672780509321));
#62144=CARTESIAN_POINT('Ctrl Pts',(0.80907773518726,3.17766110700166,0.546146916366667));
#62145=CARTESIAN_POINT('Ctrl Pts',(0.815178402601655,3.15946332634572,0.643162741113106));
#62146=CARTESIAN_POINT('Ctrl Pts',(0.82127907001605,3.13681369133633,0.739268170791191));
#62147=CARTESIAN_POINT('Ctrl Pts',(0.827489896212018,3.11375507546858,0.837108960933415));
#62148=CARTESIAN_POINT('Ctrl Pts',(0.833700722407985,3.08608224683887,0.934005690625308));
#62149=CARTESIAN_POINT('Ctrl Pts',(0.839911548603953,3.05389490892766,1.02948698278597));
#62150=CARTESIAN_POINT('Ctrl Pts',(0.845999056097287,3.02234666485472,1.12307245163689));
#62151=CARTESIAN_POINT('Ctrl Pts',(0.852086563590622,2.9864616711278,1.21529772588378));
#62152=CARTESIAN_POINT('Ctrl Pts',(0.858174071083956,2.9463849432905,1.30573095561493));
#62153=CARTESIAN_POINT('Ctrl Pts',(0.864258621066954,2.90632768603896,1.39612024992391));
#62154=CARTESIAN_POINT('Ctrl Pts',(0.870343171049953,2.86208291936874,1.48471882347684));
#62155=CARTESIAN_POINT('Ctrl Pts',(0.876427721032951,2.81384418973302,1.57111375730904));
#62156=CARTESIAN_POINT('Ctrl Pts',(0.882511025615258,2.76561533371941,1.65749100761318));
#62157=CARTESIAN_POINT('Ctrl Pts',(0.888594330197564,2.71339435643726,1.7416651269668));
#62158=CARTESIAN_POINT('Ctrl Pts',(0.89467763477987,2.65742072344934,1.82324783314885));
#62159=CARTESIAN_POINT('Ctrl Pts',(0.900982740108154,2.59940625995823,1.90780509121223));
#62160=CARTESIAN_POINT('Ctrl Pts',(0.907287845436437,2.53736051465106,1.98957791235419));
#62161=CARTESIAN_POINT('Ctrl Pts',(0.913592950764721,2.47159830858911,2.06816811779881));
#62162=CARTESIAN_POINT('Ctrl Pts',(0.919681880675533,2.40809081067382,2.14406379720673));
#62163=CARTESIAN_POINT('Ctrl Pts',(0.925770810586345,2.34111788180747,2.21699122991317));
#62164=CARTESIAN_POINT('Ctrl Pts',(0.931859740497157,2.27100209004627,2.2866278817301));
#62165=CARTESIAN_POINT('Ctrl Pts',(0.937951885881013,2.20084927118152,2.35630130762393));
#62166=CARTESIAN_POINT('Ctrl Pts',(0.944044031264868,2.1275506154588,2.42268019643455));
#62167=CARTESIAN_POINT('Ctrl Pts',(0.950136176648724,2.05146263451116,2.48548156736366));
#62168=CARTESIAN_POINT('Ctrl Pts',(0.956235946814951,1.97527942367991,2.54836153897543));
#62169=CARTESIAN_POINT('Ctrl Pts',(0.962335716981179,1.89630027968192,2.60765479757206));
#62170=CARTESIAN_POINT('Ctrl Pts',(0.968435487147407,1.81491111748615,2.663121326212));
#62171=CARTESIAN_POINT('Ctrl Pts',(0.969069957671363,1.80644538468387,2.66889070383266));
#62172=CARTESIAN_POINT('Ctrl Pts',(0.969704428195318,1.79795359929468,2.67461872021029));
#62173=CARTESIAN_POINT('Ctrl Pts',(0.970338898719273,1.78943621037804,2.68030513402633));
#62174=CARTESIAN_POINT('Origin',(-1.72497344927317,0.,0.));
#62175=CARTESIAN_POINT('',(2.46694827513675,1.78943621037803,2.68030513402633));
#62176=CARTESIAN_POINT('',(2.22053406624882,1.78943621037804,2.68030513402633));
#62177=CARTESIAN_POINT('',(-1.72497344927317,1.78943621037804,2.68030513402633));
#62178=CARTESIAN_POINT('',(1.64657344923657,-3.22274952152685,0.00175613167923087));
#62179=CARTESIAN_POINT('Ctrl Pts',(1.6465734492731,-3.22274952152717,0.00175613108471597));
#62180=CARTESIAN_POINT('Ctrl Pts',(1.65280034903924,-3.22280473869681,-0.0995752037854233));
#62181=CARTESIAN_POINT('Ctrl Pts',(1.65902724880537,-3.2180764441791,-0.200906486064027));
#62182=CARTESIAN_POINT('Ctrl Pts',(1.66525414857151,-3.20859114138214,-0.301762240752683));
#62183=CARTESIAN_POINT('Ctrl Pts',(1.67148276993094,-3.19910321611906,-0.402645879717201));
#62184=CARTESIAN_POINT('Ctrl Pts',(1.67771139129037,-3.18485570519006,-0.50305331217472));
#62185=CARTESIAN_POINT('Ctrl Pts',(1.6839400126498,-3.16592690778675,-0.602515043008761));
#62186=CARTESIAN_POINT('Ctrl Pts',(1.69017185848045,-3.14698831120654,-0.702028263806664));
#62187=CARTESIAN_POINT('Ctrl Pts',(1.6964037043111,-3.12336368506292,-0.800594397529432));
#62188=CARTESIAN_POINT('Ctrl Pts',(1.70263555014175,-3.0951820835199,-0.897755775452007));
#62189=CARTESIAN_POINT('Ctrl Pts',(1.70887643902191,-3.06695958757336,-0.995058144531123));
#62190=CARTESIAN_POINT('Ctrl Pts',(1.71511732790207,-3.03416703117107,-1.09095128516009));
#62191=CARTESIAN_POINT('Ctrl Pts',(1.72135821678223,-2.99698289431817,-1.18499413233327));
#62192=CARTESIAN_POINT('Ctrl Pts',(1.72760426415207,-2.95976802242259,-1.27911471187209));
#62193=CARTESIAN_POINT('Ctrl Pts',(1.73385031152191,-2.91815451181887,-1.3713815703785));
#62194=CARTESIAN_POINT('Ctrl Pts',(1.74009635889175,-2.87236752200162,-1.46137687851227));
#62195=CARTESIAN_POINT('Ctrl Pts',(1.74635354898619,-2.82649884983587,-1.55153273504968));
#62196=CARTESIAN_POINT('Ctrl Pts',(1.75261073908064,-2.77644203880034,-1.63940858621195));
#62197=CARTESIAN_POINT('Ctrl Pts',(1.75886792917508,-2.72246647293615,-1.72461412096696));
#62198=CARTESIAN_POINT('Ctrl Pts',(1.76141685985845,-2.70047897153262,-1.7593234711149));
#62199=CARTESIAN_POINT('Ctrl Pts',(1.76396579054183,-2.67784165713318,-1.79359007414299));
#62200=CARTESIAN_POINT('Ctrl Pts',(1.7665147212252,-2.65457462769775,-1.82738915080596));
#62201=CARTESIAN_POINT('Ctrl Pts',(1.77268729314374,-2.59823044640725,-1.90923807390272));
#62202=CARTESIAN_POINT('Ctrl Pts',(1.77885986506227,-2.53799813444767,-1.988622600153));
#62203=CARTESIAN_POINT('Ctrl Pts',(1.78503243698081,-2.47412053420035,-2.06515015065447));
#62204=CARTESIAN_POINT('Ctrl Pts',(1.79119665166003,-2.41032941984574,-2.14157408809759));
#62205=CARTESIAN_POINT('Ctrl Pts',(1.79736086633924,-2.34290310289145,-2.21514840768785));
#62206=CARTESIAN_POINT('Ctrl Pts',(1.80352508101845,-2.27212760626152,-2.28550950629489));
#62207=CARTESIAN_POINT('Ctrl Pts',(1.809682770457,-2.20142703031047,-2.35579612289155));
#62208=CARTESIAN_POINT('Ctrl Pts',(1.81584045989556,-2.12738462948071,-2.4228759763318));
#62209=CARTESIAN_POINT('Ctrl Pts',(1.82199814933411,-2.05032595519718,-2.48641932102065));
#62210=CARTESIAN_POINT('Ctrl Pts',(1.82815134253488,-1.97332354781798,-2.54991626746387));
#62211=CARTESIAN_POINT('Ctrl Pts',(1.83430453573565,-1.89330957988632,-2.60988156373336));
#62212=CARTESIAN_POINT('Ctrl Pts',(1.84045772893642,-1.81064495922136,-2.66602370472325));
#62213=CARTESIAN_POINT('Ctrl Pts',(1.84660859180534,-1.7280116452279,-2.72214458361151));
#62214=CARTESIAN_POINT('Ctrl Pts',(1.85275945467427,-1.64273003205378,-2.77444494045738));
#62215=CARTESIAN_POINT('Ctrl Pts',(1.85891031754319,-1.55519175338522,-2.82267535729892));
#62216=CARTESIAN_POINT('Ctrl Pts',(1.86506049577754,-1.46766321834669,-2.87090040575369));
#62217=CARTESIAN_POINT('Ctrl Pts',(1.87121067401189,-1.37787889760995,-2.91505620527407));
#62218=CARTESIAN_POINT('Ctrl Pts',(1.87736085224624,-1.28625599776136,-2.95493875921701));
#62219=CARTESIAN_POINT('Ctrl Pts',(1.88351199054027,-1.19461879532692,-2.99482753893595));
#62220=CARTESIAN_POINT('Ctrl Pts',(1.8896631288343,-1.10114284197652,-3.0304415747476));
#62221=CARTESIAN_POINT('Ctrl Pts',(1.89581426712834,-1.00626539882668,-3.061624978606));
#62222=CARTESIAN_POINT('Ctrl Pts',(1.90197198119414,-0.911286528529178,
-3.09284171856203));
#62223=CARTESIAN_POINT('Ctrl Pts',(1.90812969525993,-0.814903590014241,
-3.11961823239626));
#62224=CARTESIAN_POINT('Ctrl Pts',(1.91428740932573,-0.717568975034798,
-3.14184855277391));
#62225=CARTESIAN_POINT('Ctrl Pts',(1.9204485590456,-0.620180052878697,-3.16409127640538));
#62226=CARTESIAN_POINT('Ctrl Pts',(1.92660970876546,-0.521838824287656,
-3.18178267821856));
#62227=CARTESIAN_POINT('Ctrl Pts',(1.93277085848533,-0.423005768012119,
-3.19486833574225));
#62228=CARTESIAN_POINT('Ctrl Pts',(1.93894230378675,-0.324007556881048,
-3.20797586003765));
#62229=CARTESIAN_POINT('Ctrl Pts',(1.94511374908818,-0.224516309361872,
-3.21646222973386));
#62230=CARTESIAN_POINT('Ctrl Pts',(1.9512851943896,-0.124995636520338,-3.22032508504202));
#62231=CARTESIAN_POINT('Ctrl Pts',(1.95597744291468,-0.0493284779298773,
-3.22326207568797));
#62232=CARTESIAN_POINT('Ctrl Pts',(1.96066969143976,0.0263556273248075,
-3.22352738288182));
#62233=CARTESIAN_POINT('Ctrl Pts',(1.96536193996483,0.101854934327927,-3.22114003651705));
#62234=CARTESIAN_POINT('Ctrl Pts',(1.97153433126488,0.201170062931038,-3.21799961549003));
#62235=CARTESIAN_POINT('Ctrl Pts',(1.97770672256493,0.300514518760375,-3.2102561973682));
#62236=CARTESIAN_POINT('Ctrl Pts',(1.98387911386498,0.399426776188079,-3.19790178288265));
#62237=CARTESIAN_POINT('Ctrl Pts',(1.99004314898721,0.498205126290214,-3.18556409379236));
#62238=CARTESIAN_POINT('Ctrl Pts',(1.99620718410944,0.596552013751196,-3.1686278691003));
#62239=CARTESIAN_POINT('Ctrl Pts',(2.00237121923168,0.694006938371615,-3.14713710092078));
#62240=CARTESIAN_POINT('Ctrl Pts',(2.00852873041156,0.791358717844935,-3.12566907831778));
#62241=CARTESIAN_POINT('Ctrl Pts',(2.01468624159145,0.887819989502827,-3.09965618882277));
#62242=CARTESIAN_POINT('Ctrl Pts',(2.02084375277134,0.982937360234891,-3.0691939835003));
#62243=CARTESIAN_POINT('Ctrl Pts',(2.02699677043197,1.07798531789979,-3.03875400834556));
#62244=CARTESIAN_POINT('Ctrl Pts',(2.0331497880926,1.17169091208353,-3.00387130491829));
#62245=CARTESIAN_POINT('Ctrl Pts',(2.03930280575323,1.26361379977512,-2.96469184360161));
#62246=CARTESIAN_POINT('Ctrl Pts',(2.04545349480919,1.35550189932253,-2.92552720972109));
#62247=CARTESIAN_POINT('Ctrl Pts',(2.05160418386515,1.44560823380423,-2.88206921913371));
#62248=CARTESIAN_POINT('Ctrl Pts',(2.05775487292111,1.53351125056552,-2.83451244606352));
#62249=CARTESIAN_POINT('Ctrl Pts',(2.06390487928364,1.62140451056433,-2.78696095153957));
#62250=CARTESIAN_POINT('Ctrl Pts',(2.07005488564617,1.7070945570307,-2.7353117857095));
#62251=CARTESIAN_POINT('Ctrl Pts',(2.0762048920087,1.79018421900486,-2.67980559453964));
#62252=CARTESIAN_POINT('Ctrl Pts',(2.08235586058764,1.87328688100408,-2.62429071899366));
#62253=CARTESIAN_POINT('Ctrl Pts',(2.08850682916659,1.95378798918882,-2.56491786077052));
#62254=CARTESIAN_POINT('Ctrl Pts',(2.09465779774553,2.03131999898255,-2.50197054823464));
#62255=CARTESIAN_POINT('Ctrl Pts',(2.10081534652916,2.10893495124091,-2.43895589570257));
#62256=CARTESIAN_POINT('Ctrl Pts',(2.10697289531279,2.18357412451723,-2.3723594272501));
#62257=CARTESIAN_POINT('Ctrl Pts',(2.11313044409641,2.25490378730162,-2.30250439142096));
#62258=CARTESIAN_POINT('Ctrl Pts',(2.11929143073562,2.32627327454985,-2.23261035443522));
#62259=CARTESIAN_POINT('Ctrl Pts',(2.12545241737482,2.39432927567538,-2.15945444496975));
#62260=CARTESIAN_POINT('Ctrl Pts',(2.13161340401402,2.45877704760324,-2.08339458400935));
#62261=CARTESIAN_POINT('Ctrl Pts',(2.13778469158107,2.52333257367623,-2.00720755394673));
#62262=CARTESIAN_POINT('Ctrl Pts',(2.14395597914812,2.58426755499085,-1.92810721834254));
#62263=CARTESIAN_POINT('Ctrl Pts',(2.15012726671517,2.64132935127803,-1.84648228276828));
#62264=CARTESIAN_POINT('Ctrl Pts',(2.15482123071161,2.68473131795583,-1.78439726329146));
#62265=CARTESIAN_POINT('Ctrl Pts',(2.15951519470805,2.72589339377815,-1.72085231729032));
#62266=CARTESIAN_POINT('Ctrl Pts',(2.16420915870449,2.76472240631613,-1.65602765028654));
#62267=CARTESIAN_POINT('Ctrl Pts',(2.1703812373919,2.81577855436516,-1.57078989687891));
#62268=CARTESIAN_POINT('Ctrl Pts',(2.17655331607932,2.86297903973375,-1.48303869173317));
#62269=CARTESIAN_POINT('Ctrl Pts',(2.18272539476673,2.90606756231055,-1.393157882577));
#62270=CARTESIAN_POINT('Ctrl Pts',(2.1888891115705,2.94909770889593,-1.30339884323399));
#62271=CARTESIAN_POINT('Ctrl Pts',(2.19505282837426,2.98802677922563,-1.21151632272987));
#62272=CARTESIAN_POINT('Ctrl Pts',(2.20121654517802,3.02264275951866,-1.11792142426442));
#62273=CARTESIAN_POINT('Ctrl Pts',(2.20737373278518,3.05722207126441,-1.02442567044058));
#62274=CARTESIAN_POINT('Ctrl Pts',(2.21353092039234,3.08749722638055,-0.929221550063133));
#62275=CARTESIAN_POINT('Ctrl Pts',(2.21968810799949,3.11330342310276,-0.832742071830553));
#62276=CARTESIAN_POINT('Ctrl Pts',(2.22584079549085,3.13909075879927,-0.73633310774381));
#62277=CARTESIAN_POINT('Ctrl Pts',(2.2319934829822,3.16041551802508,-0.638651057405087));
#62278=CARTESIAN_POINT('Ctrl Pts',(2.23814617047355,3.17716236682762,-0.540145218727602));
#62279=CARTESIAN_POINT('Ctrl Pts',(2.24429652541123,3.19390286670967,-0.44167672473183));
#62280=CARTESIAN_POINT('Ctrl Pts',(2.2504468803489,3.20606883194019,-0.342385490731476));
#62281=CARTESIAN_POINT('Ctrl Pts',(2.25659723528658,3.21359597362361,-0.242731293429856));
#62282=CARTESIAN_POINT('Ctrl Pts',(2.26274690396581,3.2211222754263,-0.143088215573441));
#62283=CARTESIAN_POINT('Ctrl Pts',(2.26889657264504,3.22401075002825,-0.0430826881038844));
#62284=CARTESIAN_POINT('Ctrl Pts',(2.27504624132427,3.22224904753393,0.0568211067005552));
#62285=CARTESIAN_POINT('Ctrl Pts',(2.28119686903602,3.22048707030448,0.156740481366882));
#62286=CARTESIAN_POINT('Ctrl Pts',(2.28734749674778,3.21407348323025,0.256557657479677));
#62287=CARTESIAN_POINT('Ctrl Pts',(2.29349812445953,3.20304802887491,0.355810184256337));
#62288=CARTESIAN_POINT('Ctrl Pts',(2.29965532950994,3.19201078415435,0.455168849383647));
#62289=CARTESIAN_POINT('Ctrl Pts',(2.30581253456035,3.17635187186371,0.553961226813639));
#62290=CARTESIAN_POINT('Ctrl Pts',(2.31196973961076,3.15616273100808,0.651731829739503));
#62291=CARTESIAN_POINT('Ctrl Pts',(2.31813038038822,3.13596232459011,0.749556988767112));
#62292=CARTESIAN_POINT('Ctrl Pts',(2.32429102116568,3.11122676294175,0.846358816950549));
#62293=CARTESIAN_POINT('Ctrl Pts',(2.33045166194313,3.08209773392253,0.941695875030569));
#62294=CARTESIAN_POINT('Ctrl Pts',(2.33662260373307,3.05291999917572,1.03719234318832));
#62295=CARTESIAN_POINT('Ctrl Pts',(2.34279354552301,3.01933426948965,1.13121873977146));
#62296=CARTESIAN_POINT('Ctrl Pts',(2.34896448731295,2.98153089518619,1.22335239548964));
#62297=CARTESIAN_POINT('Ctrl Pts',(2.35366178402335,2.95275511479446,1.29348417320747));
#62298=CARTESIAN_POINT('Ctrl Pts',(2.35835908073374,2.92153655702733,1.36251964955495));
#62299=CARTESIAN_POINT('Ctrl Pts',(2.36305637744414,2.88797665975281,1.43028262075123));
#62300=CARTESIAN_POINT('Ctrl Pts',(2.36922850018484,2.84387984877527,1.51932135968647));
#62301=CARTESIAN_POINT('Ctrl Pts',(2.37540062292555,2.79558387048185,1.60647556528312));
#62302=CARTESIAN_POINT('Ctrl Pts',(2.38157274566625,2.74327306222189,1.6913221066928));
#62303=CARTESIAN_POINT('Ctrl Pts',(2.38773684236677,2.6910302773417,1.77605831624753));
#62304=CARTESIAN_POINT('Ctrl Pts',(2.39390093906729,2.63478326276098,1.85849245816756));
#62305=CARTESIAN_POINT('Ctrl Pts',(2.40006503576781,2.57476326090943,1.93822385517541));
#62306=CARTESIAN_POINT('Ctrl Pts',(2.40622186982413,2.51481397565102,2.0178613112871));
#62307=CARTESIAN_POINT('Ctrl Pts',(2.41237870388045,2.45110080597488,2.09480201206285));
#62308=CARTESIAN_POINT('Ctrl Pts',(2.41853553793677,2.38389885062525,2.168673288554));
#62309=CARTESIAN_POINT('Ctrl Pts',(2.42468813289258,2.31674316513447,2.24249370322843));
#62310=CARTESIAN_POINT('Ctrl Pts',(2.4308407278484,2.24610375926931,2.31324857355045));
#62311=CARTESIAN_POINT('Ctrl Pts',(2.43699332280421,2.17229620568289,2.38059798312855));
#62312=CARTESIAN_POINT('Ctrl Pts',(2.44314380416744,2.09851400710507,2.44792425625549));
#62313=CARTESIAN_POINT('Ctrl Pts',(2.44929428553067,2.02156614221978,2.51184709906017));
#62314=CARTESIAN_POINT('Ctrl Pts',(2.4554447668939,1.94180462797299,2.57206383071701));
#62315=CARTESIAN_POINT('Ctrl Pts',(2.45927926964151,1.89207750460312,2.60960580659732));
#62316=CARTESIAN_POINT('Ctrl Pts',(2.46311377238913,1.84125746650579,2.64570801633063));
#62317=CARTESIAN_POINT('Ctrl Pts',(2.46694827513675,1.78943621037803,2.68030513402633));
#62318=CARTESIAN_POINT('Ctrl Pts',(1.21707771886868,1.78943621037804,2.68030513402633));
#62319=CARTESIAN_POINT('Ctrl Pts',(1.22340032573857,1.70420999519611,2.73720420629387));
#62320=CARTESIAN_POINT('Ctrl Pts',(1.22972293260845,1.61618729446822,2.79008771147135));
#62321=CARTESIAN_POINT('Ctrl Pts',(1.23604553947834,1.52578684091609,2.83867787510089));
#62322=CARTESIAN_POINT('Ctrl Pts',(1.24219858989544,1.43781070071279,2.88596497245497));
#62323=CARTESIAN_POINT('Ctrl Pts',(1.24835164031254,1.34758313548586,2.92918587595363));
#62324=CARTESIAN_POINT('Ctrl Pts',(1.25450469072965,1.25551775368136,2.96812950066046));
#62325=CARTESIAN_POINT('Ctrl Pts',(1.26065635079051,1.16347317516455,3.00706432558379));
#62326=CARTESIAN_POINT('Ctrl Pts',(1.26680801085137,1.06959200506838,3.04172362352167));
#62327=CARTESIAN_POINT('Ctrl Pts',(1.27295967091224,0.974309102690366,3.07194390165489));
#62328=CARTESIAN_POINT('Ctrl Pts',(1.27911158389948,0.879022282742172,3.10216542229918));
#62329=CARTESIAN_POINT('Ctrl Pts',(1.28526349688673,0.7823340300486,3.12794742984124));
#62330=CARTESIAN_POINT('Ctrl Pts',(1.29141540987398,0.684694716996577,3.14917619497814));
#62331=CARTESIAN_POINT('Ctrl Pts',(1.29786581602997,0.582317907167919,3.17143498791085));
#62332=CARTESIAN_POINT('Ctrl Pts',(1.30431622218597,0.478895929833729,3.18868741957029));
#62333=CARTESIAN_POINT('Ctrl Pts',(1.31076662834196,0.374958615110494,3.20086294605914));
#62334=CARTESIAN_POINT('Ctrl Pts',(1.31692766278283,0.275684032981056,3.21249226617007));
#62335=CARTESIAN_POINT('Ctrl Pts',(1.32308869722371,0.175939800375313,3.21949038117817));
#62336=CARTESIAN_POINT('Ctrl Pts',(1.32924973166458,0.076190108328905,3.22184925623357));
#62337=CARTESIAN_POINT('Ctrl Pts',(1.33541511191715,-0.023629944203698,
3.22420979516976));
#62338=CARTESIAN_POINT('Ctrl Pts',(1.34158049216972,-0.123455030898768,
3.22192459052998));
#62339=CARTESIAN_POINT('Ctrl Pts',(1.34774587242229,-0.222824135759187,
3.21503763073205));
#62340=CARTESIAN_POINT('Ctrl Pts',(1.35392043030039,-0.322341158898122,
3.20814041918395));
#62341=CARTESIAN_POINT('Ctrl Pts',(1.36009498817849,-0.421400416785637,
3.19662783719734));
#62342=CARTESIAN_POINT('Ctrl Pts',(1.36626954605659,-0.519549453305405,
3.1805952160044));
#62343=CARTESIAN_POINT('Ctrl Pts',(1.36711979195303,-0.533064723092881,
3.17838749997879));
#62344=CARTESIAN_POINT('Ctrl Pts',(1.36797003784947,-0.546562755769955,
3.17609415400508));
#62345=CARTESIAN_POINT('Ctrl Pts',(1.36882028374592,-0.56004239262392,3.17371550094902));
#62346=CARTESIAN_POINT('Ctrl Pts',(1.37499381742182,-0.657916422248695,
3.15644438584421));
#62347=CARTESIAN_POINT('Ctrl Pts',(1.38116735109773,-0.75516218775552,3.13461128406342));
#62348=CARTESIAN_POINT('Ctrl Pts',(1.38734088477363,-0.851321599816241,
3.10827429551935));
#62349=CARTESIAN_POINT('Ctrl Pts',(1.39350608513824,-0.947351211610776,
3.08197285781789));
#62350=CARTESIAN_POINT('Ctrl Pts',(1.39967128550285,-1.04229696956204,3.05117973097203));
#62351=CARTESIAN_POINT('Ctrl Pts',(1.40583648586747,-1.13570923744721,3.01600432534124));
#62352=CARTESIAN_POINT('Ctrl Pts',(1.4119951834889,-1.2290229787717,2.98086602095867));
#62353=CARTESIAN_POINT('Ctrl Pts',(1.41815388111033,-1.32080604162271,2.9413547794624));
#62354=CARTESIAN_POINT('Ctrl Pts',(1.42431257873176,-1.4106231976854,2.89763002411485));
#62355=CARTESIAN_POINT('Ctrl Pts',(1.43046680993421,-1.50037521642912,2.85393697889329));
#62356=CARTESIAN_POINT('Ctrl Pts',(1.43662104113665,-1.58816377375753,2.80603668460894));
#62357=CARTESIAN_POINT('Ctrl Pts',(1.4427752723391,-1.67357376430967,2.75413660117184));
#62358=CARTESIAN_POINT('Ctrl Pts',(1.44892719120158,-1.75895166361803,2.70225601824304));
#62359=CARTESIAN_POINT('Ctrl Pts',(1.45507911006407,-1.84195240132714,2.64637885756395));
#62360=CARTESIAN_POINT('Ctrl Pts',(1.46123102892656,-1.92218641645228,2.58675799851983));
#62361=CARTESIAN_POINT('Ctrl Pts',(1.46738227994742,-2.00241172151206,2.52714361181266));
#62362=CARTESIAN_POINT('Ctrl Pts',(1.47353353096828,-2.07987055265335,2.46378659371234));
#62363=CARTESIAN_POINT('Ctrl Pts',(1.47968478198914,-2.15420406316013,2.39698193918194));
#62364=CARTESIAN_POINT('Ctrl Pts',(1.48583700867722,-2.22854936391411,2.33016668857736));
#62365=CARTESIAN_POINT('Ctrl Pts',(1.49198923536531,-2.2997680364378,2.2599030055844));
#62366=CARTESIAN_POINT('Ctrl Pts',(1.4981414620534,-2.36753668152556,2.18652409639842));
#62367=CARTESIAN_POINT('Ctrl Pts',(1.50430028217181,-2.43537795525044,2.11306654597416));
#62368=CARTESIAN_POINT('Ctrl Pts',(1.51045910229022,-2.49976152299853,2.03648742203356));
#62369=CARTESIAN_POINT('Ctrl Pts',(1.51661792240863,-2.56040312316878,1.95715441633192));
#62370=CARTESIAN_POINT('Ctrl Pts',(1.52278018970818,-2.62107866532407,1.87777700679389));
#62371=CARTESIAN_POINT('Ctrl Pts',(1.52894245700773,-2.6780078215014,1.7956430026586));
#62372=CARTESIAN_POINT('Ctrl Pts',(1.53510472430728,-2.73094986828718,1.71114884782191));
#62373=CARTESIAN_POINT('Ctrl Pts',(1.54127729460607,-2.78398043149739,1.62651342303203));
#62374=CARTESIAN_POINT('Ctrl Pts',(1.54744986490486,-2.83301035644263,1.53951034383121));
#62375=CARTESIAN_POINT('Ctrl Pts',(1.55362243520364,-2.87784498461981,1.45056051476614));
#62376=CARTESIAN_POINT('Ctrl Pts',(1.55830412429761,-2.91185055759974,1.38309503045632));
#62377=CARTESIAN_POINT('Ctrl Pts',(1.56298581339158,-2.94344365280984,1.31451014118222));
#62378=CARTESIAN_POINT('Ctrl Pts',(1.56766750248555,-2.97255827287987,1.24499593446463));
#62379=CARTESIAN_POINT('Ctrl Pts',(1.57453989941227,-3.01529652855551,1.14295386994037));
#62380=CARTESIAN_POINT('Ctrl Pts',(1.58141229633898,-3.05282061275208,1.03860409475009));
#62381=CARTESIAN_POINT('Ctrl Pts',(1.5882846932657,-3.08490276173312,0.932465824119787));
#62382=CARTESIAN_POINT('Ctrl Pts',(1.59513648219888,-3.11688870720235,0.826645826257836));
#62383=CARTESIAN_POINT('Ctrl Pts',(1.60198827113206,-3.14346516490069,0.719048267582058));
#62384=CARTESIAN_POINT('Ctrl Pts',(1.60884006006525,-3.16445263402091,0.610210692743205));
#62385=CARTESIAN_POINT('Ctrl Pts',(1.61565487371116,-3.18532684546384,0.50196045365489));
#62386=CARTESIAN_POINT('Ctrl Pts',(1.62246968735706,-3.20067211544954,0.392483786661898));
#62387=CARTESIAN_POINT('Ctrl Pts',(1.62928450100298,-3.21035947712258,0.28232886878472));
#62388=CARTESIAN_POINT('Ctrl Pts',(1.63504748374751,-3.21855164510581,0.189175787286705));
#62389=CARTESIAN_POINT('Ctrl Pts',(1.64081046649204,-3.22269841813423,0.0955380707283682));
#62390=CARTESIAN_POINT('Ctrl Pts',(1.64657344923657,-3.22274952152685,0.00175613167923302));
#62391=CARTESIAN_POINT('',(1.40002655078068,-3.22274939283074,0.00197825911163994));
#62392=CARTESIAN_POINT('Ctrl Pts',(0.970338898719273,1.78943621037804,2.68030513402633));
#62393=CARTESIAN_POINT('Ctrl Pts',(0.974724078305945,1.73056778607964,2.71960711078642));
#62394=CARTESIAN_POINT('Ctrl Pts',(0.979109257892617,1.67047586253169,2.75692070227038));
#62395=CARTESIAN_POINT('Ctrl Pts',(0.983494437479289,1.6093118116581,2.79217353603921));
#62396=CARTESIAN_POINT('Ctrl Pts',(0.989675583431169,1.52309779966941,2.8418642970299));
#62397=CARTESIAN_POINT('Ctrl Pts',(0.995856729383049,1.43443090023847,2.88764431992224));
#62398=CARTESIAN_POINT('Ctrl Pts',(1.00203787533493,1.34370061336218,2.92926376827866));
#62399=CARTESIAN_POINT('Ctrl Pts',(1.00821066572557,1.25309297404582,2.97082695621794));
#62400=CARTESIAN_POINT('Ctrl Pts',(1.0143834561162,1.16042788175746,3.00824057022586));
#62401=CARTESIAN_POINT('Ctrl Pts',(1.02055624650684,1.06612126559161,3.04129955932548));
#62402=CARTESIAN_POINT('Ctrl Pts',(1.02672250133371,0.971914498418576,3.07432354656733));
#62403=CARTESIAN_POINT('Ctrl Pts',(1.03288875616058,0.876070069259749,3.10300193334037));
#62404=CARTESIAN_POINT('Ctrl Pts',(1.03905501098746,0.7790249504798,3.12717727176282));
#62405=CARTESIAN_POINT('Ctrl Pts',(1.04521671673993,0.682051425475667,3.15133477514337));
#62406=CARTESIAN_POINT('Ctrl Pts',(1.05137842249239,0.583879390990891,3.1709957314356));
#62407=CARTESIAN_POINT('Ctrl Pts',(1.05754012824486,0.484961218254331,3.18605244452901));
#62408=CARTESIAN_POINT('Ctrl Pts',(1.06369946807815,0.386081027273421,3.20110337627424));
#62409=CARTESIAN_POINT('Ctrl Pts',(1.06985880791144,0.286455694870284,3.21155351289783));
#62410=CARTESIAN_POINT('Ctrl Pts',(1.07601814774473,0.186547178965657,3.21734637745456));
#62411=CARTESIAN_POINT('Ctrl Pts',(1.08217675666867,0.0866505188881857,
3.22313855459039));
#62412=CARTESIAN_POINT('Ctrl Pts',(1.0883353655926,-0.013528825689528,3.22427453348602));
#62413=CARTESIAN_POINT('Ctrl Pts',(1.09449397451654,-0.113525377969389,
3.22074984298019));
#62414=CARTESIAN_POINT('Ctrl Pts',(1.10065348649824,-0.213536593083651,
3.21722463563701));
#62415=CARTESIAN_POINT('Ctrl Pts',(1.10681299847994,-0.313364529969851,
3.20903741670471));
#62416=CARTESIAN_POINT('Ctrl Pts',(1.11297251046164,-0.412546311658843,
3.19623577090876));
#62417=CARTESIAN_POINT('Ctrl Pts',(1.11913845611142,-0.511831689649731,
3.18342075367361));
#62418=CARTESIAN_POINT('Ctrl Pts',(1.1253044017612,-0.610469134487032,3.16598174018904));
#62419=CARTESIAN_POINT('Ctrl Pts',(1.13147034741098,-0.708003590241276,
3.14401788778395));
#62420=CARTESIAN_POINT('Ctrl Pts',(1.13763966237117,-0.805591342582289,
3.12204203348316));
#62421=CARTESIAN_POINT('Ctrl Pts',(1.14380897733136,-0.902074487851182,
3.09553653020164));
#62422=CARTESIAN_POINT('Ctrl Pts',(1.14997829229155,-0.997012811986731,
3.06465055352716));
#62423=CARTESIAN_POINT('Ctrl Pts',(1.15615770773974,-1.09210657046299,3.03371400990339));
#62424=CARTESIAN_POINT('Ctrl Pts',(1.16233712318792,-1.18565005041696,2.99838282009929));
#62425=CARTESIAN_POINT('Ctrl Pts',(1.16851653863611,-1.2772225817404,2.95885451470538));
#62426=CARTESIAN_POINT('Ctrl Pts',(1.17312491116372,-1.34551388553319,2.92937581106951));
#62427=CARTESIAN_POINT('Ctrl Pts',(1.17773328369132,-1.41270944558138,2.89756384378956));
#62428=CARTESIAN_POINT('Ctrl Pts',(1.18234165621892,-1.47864453547035,2.86351670157931));
#62429=CARTESIAN_POINT('Ctrl Pts',(1.18852471287063,-1.5671096918085,2.81783562700175));
#62430=CARTESIAN_POINT('Ctrl Pts',(1.19470776952234,-1.65360548738925,2.76797396991164));
#62431=CARTESIAN_POINT('Ctrl Pts',(1.20089082617404,-1.7377112728214,2.71412547514101));
#62432=CARTESIAN_POINT('Ctrl Pts',(1.20706573011307,-1.82170615998072,2.66034798268056));
#62433=CARTESIAN_POINT('Ctrl Pts',(1.21324063405209,-1.90331694006354,2.60259433364497));
#62434=CARTESIAN_POINT('Ctrl Pts',(1.21941553799112,-1.98214648415018,2.54110465700866));
#62435=CARTESIAN_POINT('Ctrl Pts',(1.22558410555742,-2.06089513736343,2.47967807795466));
#62436=CARTESIAN_POINT('Ctrl Pts',(1.23175267312373,-2.13686788981976,2.41452335863386));
#62437=CARTESIAN_POINT('Ctrl Pts',(1.23792124069003,-2.20969640222499,2.34592399120132));
#62438=CARTESIAN_POINT('Ctrl Pts',(1.24408555114311,-2.28247465349265,2.27737196624675));
#62439=CARTESIAN_POINT('Ctrl Pts',(1.2502498615962,-2.35211266494071,2.20538031540524));
#62440=CARTESIAN_POINT('Ctrl Pts',(1.25641417204928,-2.41827571657017,2.13027231150082));
#62441=CARTESIAN_POINT('Ctrl Pts',(1.26257629526443,-2.48441529203994,2.05519095762916));
#62442=CARTESIAN_POINT('Ctrl Pts',(1.26873841847957,-2.54708207223402,1.97699577233909));
#62443=CARTESIAN_POINT('Ctrl Pts',(1.27490054169472,-2.60597933810157,1.89604568823848));
#62444=CARTESIAN_POINT('Ctrl Pts',(1.28106211003392,-2.66487130049253,1.81510289338753));
#62445=CARTESIAN_POINT('Ctrl Pts',(1.28722367837312,-2.71999416898764,1.73140604281522));
#62446=CARTESIAN_POINT('Ctrl Pts',(1.29338524671231,-2.77109315175436,1.64534504186815));
#62447=CARTESIAN_POINT('Ctrl Pts',(1.29954789163807,-2.82220106284499,1.55926900382149));
#62448=CARTESIAN_POINT('Ctrl Pts',(1.30571053656383,-2.86928347053962,1.47082836672944));
#62449=CARTESIAN_POINT('Ctrl Pts',(1.31187318148959,-2.91213084404561,1.38043888298549));
#62450=CARTESIAN_POINT('Ctrl Pts',(1.31804251213623,-2.95502470174525,1.28995133763535));
#62451=CARTESIAN_POINT('Ctrl Pts',(1.32421184278288,-2.99367416495057,1.19751111535027));
#62452=CARTESIAN_POINT('Ctrl Pts',(1.33038117342953,-3.0279173592827,1.10355517662438));
#62453=CARTESIAN_POINT('Ctrl Pts',(1.33655401863793,-3.06218006137476,1.00954571281323));
#62454=CARTESIAN_POINT('Ctrl Pts',(1.34272686384633,-3.09203136623493,0.914019225727417));
#62455=CARTESIAN_POINT('Ctrl Pts',(1.34889970905473,-3.11735953592752,0.817427113730492));
#62456=CARTESIAN_POINT('Ctrl Pts',(1.35508285805436,-3.14272998372102,0.720673768959608));
#62457=CARTESIAN_POINT('Ctrl Pts',(1.36126600705399,-3.16356212508625,0.622851669525752));
#62458=CARTESIAN_POINT('Ctrl Pts',(1.36744915605362,-3.17979548502384,0.524421811066224));
#62459=CARTESIAN_POINT('Ctrl Pts',(1.37202906235527,-3.19181966032345,0.451514053375713));
#62460=CARTESIAN_POINT('Ctrl Pts',(1.37660896865692,-3.20132180253824,0.378273034406715));
#62461=CARTESIAN_POINT('Ctrl Pts',(1.38118887495857,-3.20829576914891,0.304886569335508));
#62462=CARTESIAN_POINT('Ctrl Pts',(1.38746810021468,-3.21785734189577,0.204270942163111));
#62463=CARTESIAN_POINT('Ctrl Pts',(1.39374732547078,-3.22268726269155,0.103193402978869));
#62464=CARTESIAN_POINT('Ctrl Pts',(1.40002655072689,-3.22274939283021,0.00197825997873392));
#62465=CARTESIAN_POINT('Ctrl Pts',(1.40002655078068,-3.22274939283074,0.00197825911163994));
#62466=CARTESIAN_POINT('Ctrl Pts',(1.40611289410352,-3.22280961446214,-0.096127810451189));
#62467=CARTESIAN_POINT('Ctrl Pts',(1.41219923742636,-3.21838586447631,-0.194419403685365));
#62468=CARTESIAN_POINT('Ctrl Pts',(1.41828558074921,-3.20945371439036,-0.292445580725625));
#62469=CARTESIAN_POINT('Ctrl Pts',(1.4243642957019,-3.20053275949065,-0.390348895823498));
#62470=CARTESIAN_POINT('Ctrl Pts',(1.43044301065459,-3.18711466954245,-0.48798701409589));
#62471=CARTESIAN_POINT('Ctrl Pts',(1.43652172560728,-3.16922703223334,-0.584908181393845));
#62472=CARTESIAN_POINT('Ctrl Pts',(1.44259457085173,-3.15135666752429,-0.681735760000863));
#62473=CARTESIAN_POINT('Ctrl Pts',(1.44866741609618,-3.12902541369874,-0.777847326044531));
#62474=CARTESIAN_POINT('Ctrl Pts',(1.45474026134062,-3.10231262737273,-0.872796611212326));
#62475=CARTESIAN_POINT('Ctrl Pts',(1.46080994861889,-3.07561373207676,-0.967696521397057));
#62476=CARTESIAN_POINT('Ctrl Pts',(1.46687963589716,-3.04453794865945,-1.06143492126537));
#62477=CARTESIAN_POINT('Ctrl Pts',(1.47294932317543,-3.00921544023296,-1.15357704413861));
#62478=CARTESIAN_POINT('Ctrl Pts',(1.47901757973629,-2.97390125785778,-1.24569744771508));
#62479=CARTESIAN_POINT('Ctrl Pts',(1.48508583629715,-2.93434249874623,-1.33622190438346));
#62480=CARTESIAN_POINT('Ctrl Pts',(1.49115409285801,-2.89071839202695,-1.42473321730671));
#62481=CARTESIAN_POINT('Ctrl Pts',(1.49722264422245,-2.84709216599334,-1.51324883022158));
#62482=CARTESIAN_POINT('Ctrl Pts',(1.50329119558689,-2.79940039902377,-1.59975070469585));
#62483=CARTESIAN_POINT('Ctrl Pts',(1.50935974695134,-2.74786890398481,-1.6838450192976));
#62484=CARTESIAN_POINT('Ctrl Pts',(1.51543427654096,-2.6962866444614,-1.76802217652837));
#62485=CARTESIAN_POINT('Ctrl Pts',(1.52150880613059,-2.64085733711762,-1.8497866555326));
#62486=CARTESIAN_POINT('Ctrl Pts',(1.52758333572022,-2.58185073403517,-1.92877275739317));
#62487=CARTESIAN_POINT('Ctrl Pts',(1.53366085369367,-2.52281510246989,-2.00779771671344));
#62488=CARTESIAN_POINT('Ctrl Pts',(1.53973837166712,-2.46019895644871,-2.08404123304722));
#62489=CARTESIAN_POINT('Ctrl Pts',(1.54581588964056,-2.39431159208105,-2.1571716581038));
#62490=CARTESIAN_POINT('Ctrl Pts',(1.55190370974851,-2.32831254059168,-2.23042604815372));
#62491=CARTESIAN_POINT('Ctrl Pts',(1.55799152985646,-2.25903151012212,-2.30055648906815));
#62492=CARTESIAN_POINT('Ctrl Pts',(1.56407934996441,-2.18681383281671,-2.36726906436541));
#62493=CARTESIAN_POINT('Ctrl Pts',(1.56939826454235,-2.12371741245714,-2.4255556896251));
#62494=CARTESIAN_POINT('Ctrl Pts',(1.57471717912028,-2.05837998910448,-2.48123379851504));
#62495=CARTESIAN_POINT('Ctrl Pts',(1.58003609369822,-1.99105012604439,-2.53413436069965));
#62496=CARTESIAN_POINT('Ctrl Pts',(1.58621005733018,-1.91289656298442,-2.59553902179205));
#62497=CARTESIAN_POINT('Ctrl Pts',(1.59238402096213,-1.83176267791174,-2.65343255355774));
#62498=CARTESIAN_POINT('Ctrl Pts',(1.59855798459408,-1.74799729359038,-2.70751233129245));
#62499=CARTESIAN_POINT('Ctrl Pts',(1.60472359529448,-1.6643452378476,-2.76151894295278));
#62500=CARTESIAN_POINT('Ctrl Pts',(1.61088920599487,-1.57806912081644,-2.81172182289254));
#62501=CARTESIAN_POINT('Ctrl Pts',(1.61705481669526,-1.48955036306467,-2.8578588625742));
#62502=CARTESIAN_POINT('Ctrl Pts',(1.62321390456034,-1.40112525269132,-2.90394709211749));
#62503=CARTESIAN_POINT('Ctrl Pts',(1.62937299242542,-1.3104626014072,-2.94597783359531));
#62504=CARTESIAN_POINT('Ctrl Pts',(1.63553208029051,-1.21797149036223,-2.98373306633901));
#62505=CARTESIAN_POINT('Ctrl Pts',(1.64168666964908,-1.1255479334542,-3.02146072322019));
#62506=CARTESIAN_POINT('Ctrl Pts',(1.64784125900765,-1.03129897269383,-3.05491891651411));
#62507=CARTESIAN_POINT('Ctrl Pts',(1.65399584836623,-0.935656064375376,
-3.08393665494244));
#62508=CARTESIAN_POINT('Ctrl Pts',(1.66014810554239,-0.840049398395078,
-3.11294339756662));
#62509=CARTESIAN_POINT('Ctrl Pts',(1.66630036271855,-0.743050249374499,
-3.13751290288959));
#62510=CARTESIAN_POINT('Ctrl Pts',(1.67245261989471,-0.645106886623676,
-3.15752350226102));
#62511=CARTESIAN_POINT('Ctrl Pts',(1.67860418890626,-0.547174479389529,
-3.17753186333423));
#62512=CARTESIAN_POINT('Ctrl Pts',(1.68475575791781,-0.448298493720705,
-3.19298224541561));
#62513=CARTESIAN_POINT('Ctrl Pts',(1.69090732692936,-0.348938103326894,
-3.20380395195253));
#62514=CARTESIAN_POINT('Ctrl Pts',(1.69705985078779,-0.249562290207691,
-3.21462733823534));
#62515=CARTESIAN_POINT('Ctrl Pts',(1.70321237464623,-0.149702354603581,
-3.22082057490184));
#62516=CARTESIAN_POINT('Ctrl Pts',(1.70936489850467,-0.0498223097291922,
-3.22236486139501));
#62517=CARTESIAN_POINT('Ctrl Pts',(1.71552398134482,0.050164213625006,-3.22391079419578));
#62518=CARTESIAN_POINT('Ctrl Pts',(1.72168306418496,0.150170454167541,-3.22079787329112));
#62519=CARTESIAN_POINT('Ctrl Pts',(1.72784214702511,0.249732798242018,-3.21305945976451));
#62520=CARTESIAN_POINT('Ctrl Pts',(1.73400465833322,0.349350563929725,-3.20531673863179));
#62521=CARTESIAN_POINT('Ctrl Pts',(1.74016716964133,0.448523510269242,-3.19294345083693));
#62522=CARTESIAN_POINT('Ctrl Pts',(1.74632968094944,0.546795625717764,-3.17602457581737));
#62523=CARTESIAN_POINT('Ctrl Pts',(1.75250246174458,0.645231506255649,-3.15907750642074));
#62524=CARTESIAN_POINT('Ctrl Pts',(1.75867524253972,0.742763133199492,-3.13756981248004));
#62525=CARTESIAN_POINT('Ctrl Pts',(1.76484802333487,0.838946982297594,-3.11163711306344));
#62526=CARTESIAN_POINT('Ctrl Pts',(1.76952645303586,0.911845954626379,-3.09198238771289));
#62527=CARTESIAN_POINT('Ctrl Pts',(1.77420488273686,0.983970983093657,-3.06978684944512));
#62528=CARTESIAN_POINT('Ctrl Pts',(1.77888331243785,1.05513677840373,-3.04512790229898));
#62529=CARTESIAN_POINT('Ctrl Pts',(1.78505684657086,1.14904531065251,-3.01258859710041));
#62530=CARTESIAN_POINT('Ctrl Pts',(1.79123038070387,1.24161168933727,-2.97564417336767));
#62531=CARTESIAN_POINT('Ctrl Pts',(1.79740391483688,1.33239278795469,-2.9344244786851));
#62532=CARTESIAN_POINT('Ctrl Pts',(1.80356911567004,1.42305134637076,-2.89326042410563));
#62533=CARTESIAN_POINT('Ctrl Pts',(1.8097343165032,1.51192902275237,-2.84783274704531));
#62534=CARTESIAN_POINT('Ctrl Pts',(1.81589951733636,1.59859915563183,-2.79832062175034));
#62535=CARTESIAN_POINT('Ctrl Pts',(1.82205821543712,1.68517787337393,-2.74886071926367));
#62536=CARTESIAN_POINT('Ctrl Pts',(1.82821691353788,1.76955330183398,-2.69532514767589));
#62537=CARTESIAN_POINT('Ctrl Pts',(1.83437561163864,1.85132091907383,-2.6379401845189));
#62538=CARTESIAN_POINT('Ctrl Pts',(1.84052984333481,1.93302923688781,-2.58059683802489));
#62539=CARTESIAN_POINT('Ctrl Pts',(1.84668407503097,2.01213314926246,-2.51940989890954));
#62540=CARTESIAN_POINT('Ctrl Pts',(1.85283830672713,2.08825560415908,-2.45464989238755));
#62541=CARTESIAN_POINT('Ctrl Pts',(1.85899022609203,2.16434945754348,-2.38991421816173));
#62542=CARTESIAN_POINT('Ctrl Pts',(1.86514214545692,2.23746374903061,-2.32160842514124));
#62543=CARTESIAN_POINT('Ctrl Pts',(1.87129406482181,2.30725383552129,-2.25004384423332));
#62544=CARTESIAN_POINT('Ctrl Pts',(1.8774453163532,2.37703634581417,-2.17848703215689));
#62545=CARTESIAN_POINT('Ctrl Pts',(1.88359656788458,2.44349506545273,-2.10367244637228));
#62546=CARTESIAN_POINT('Ctrl Pts',(1.88974781941597,2.50632234230045,-2.02594814321236));
#62547=CARTESIAN_POINT('Ctrl Pts',(1.89590004662217,2.56915958443593,-1.94821151188724));
#62548=CARTESIAN_POINT('Ctrl Pts',(1.90205227382837,2.62836396670925,-1.86756458413676));
#62549=CARTESIAN_POINT('Ctrl Pts',(1.90820450103458,2.68366888381557,-1.78438753765545));
#62550=CARTESIAN_POINT('Ctrl Pts',(1.91436332167981,2.73903307207479,-1.70112134902012));
#62551=CARTESIAN_POINT('Ctrl Pts',(1.92052214232505,2.79048920905492,-1.61531998918389));
#62552=CARTESIAN_POINT('Ctrl Pts',(1.92668096297029,2.83781479041402,-1.52739149461015));
#62553=CARTESIAN_POINT('Ctrl Pts',(1.93284323080231,2.88516686062997,-1.43941378510362));
#62554=CARTESIAN_POINT('Ctrl Pts',(1.93900549863433,2.92838358324439,-1.34930696127557));
#62555=CARTESIAN_POINT('Ctrl Pts',(1.94516776646635,2.96728999288113,-1.25750056089352));
#62556=CARTESIAN_POINT('Ctrl Pts',(1.95134033730146,3.00626145208564,-1.16554066480937));
#62557=CARTESIAN_POINT('Ctrl Pts',(1.95751290813657,3.04090805260098,-1.07187592353269));
#62558=CARTESIAN_POINT('Ctrl Pts',(1.96368547897169,3.07110418390735,-0.976952738921796));
#62559=CARTESIAN_POINT('Ctrl Pts',(1.96836716304029,3.09400691773524,-0.904956746813321));
#62560=CARTESIAN_POINT('Ctrl Pts',(1.9730488471089,3.11435045411151,-0.832237156790994));
#62561=CARTESIAN_POINT('Ctrl Pts',(1.9777305311775,3.13209970296924,-0.758992103489897));
#62562=CARTESIAN_POINT('Ctrl Pts',(1.98390158482016,3.15549546509521,-0.662445829466025));
#62563=CARTESIAN_POINT('Ctrl Pts',(1.99007263846282,3.17446435259434,-0.5646462106067));
#62564=CARTESIAN_POINT('Ctrl Pts',(1.99624369210548,3.18887569945224,-0.466035766806547));
#62565=CARTESIAN_POINT('Ctrl Pts',(2.00240636985073,3.20326748596116,-0.367559165784109));
#62566=CARTESIAN_POINT('Ctrl Pts',(2.00856904759598,3.21311396454698,-0.26827435339916));
#62567=CARTESIAN_POINT('Ctrl Pts',(2.01473172534123,3.21833485185556,-0.168636721481037));
#62568=CARTESIAN_POINT('Ctrl Pts',(2.02088786132567,3.22355019712586,-0.0691048561764178));
#62569=CARTESIAN_POINT('Ctrl Pts',(2.02704399731011,3.22414969018264,0.0307786525172366));
#62570=CARTESIAN_POINT('Ctrl Pts',(2.03320013329455,3.22010463541055,0.130551520509984));
#62571=CARTESIAN_POINT('Ctrl Pts',(2.03935175454817,3.21606254716382,0.230251217987271));
#62572=CARTESIAN_POINT('Ctrl Pts',(2.04550337580178,3.20738270066198,0.329840003189144));
#62573=CARTESIAN_POINT('Ctrl Pts',(2.05165499705539,3.19408847376308,0.42885473563181));
#62574=CARTESIAN_POINT('Ctrl Pts',(2.05780427710877,3.1807993064161,0.527831784786608));
#62575=CARTESIAN_POINT('Ctrl Pts',(2.06395355716215,3.16289930586048,0.626234785062532));
#62576=CARTESIAN_POINT('Ctrl Pts',(2.07010283721553,3.14046370306913,0.723605757443461));
#62577=CARTESIAN_POINT('Ctrl Pts',(2.07625142360946,3.11803063108917,0.820965746051489));
#62578=CARTESIAN_POINT('Ctrl Pts',(2.08240001000338,3.09106307162903,0.917293514740002));
#62579=CARTESIAN_POINT('Ctrl Pts',(2.08854859639731,3.05968715741981,1.01214231273091));
#62580=CARTESIAN_POINT('Ctrl Pts',(2.0946981356625,3.02830638075845,1.1070058098231));
#62581=CARTESIAN_POINT('Ctrl Pts',(2.10084767492769,2.99251602889572,1.20038946835059));
#62582=CARTESIAN_POINT('Ctrl Pts',(2.10699721419288,2.95249145840519,1.29186367335891));
#62583=CARTESIAN_POINT('Ctrl Pts',(2.1131533279081,2.91242409779212,1.38343567310666));
#62584=CARTESIAN_POINT('Ctrl Pts',(2.11930944162332,2.86811365356512,1.47309374398627));
#62585=CARTESIAN_POINT('Ctrl Pts',(2.12546555533855,2.81978277213684,1.56043028695944));
#62586=CARTESIAN_POINT('Ctrl Pts',(2.13162510146531,2.77142494327337,1.64781552542007));
#62587=CARTESIAN_POINT('Ctrl Pts',(2.13778464759208,2.71904244094299,1.73287628818928));
#62588=CARTESIAN_POINT('Ctrl Pts',(2.14394419371885,2.6629017123353,1.81523332741048));
#62589=CARTESIAN_POINT('Ctrl Pts',(2.15011404678936,2.60666704184946,1.89772817700813));
#62590=CARTESIAN_POINT('Ctrl Pts',(2.15628389985988,2.54666184486046,1.97750991862143));
#62591=CARTESIAN_POINT('Ctrl Pts',(2.16245375293039,2.48319345044674,2.05423169339742));
#62592=CARTESIAN_POINT('Ctrl Pts',(2.16716175192598,2.4347629394222,2.11277539524198));
#62593=CARTESIAN_POINT('Ctrl Pts',(2.17186975092156,2.38431676498116,2.16953804500934));
#62594=CARTESIAN_POINT('Ctrl Pts',(2.17657774991715,2.3320052453869,2.22438060996494));
#62595=CARTESIAN_POINT('Ctrl Pts',(2.18275082151698,2.26341501071306,2.29628952084339));
#62596=CARTESIAN_POINT('Ctrl Pts',(2.18892389311682,2.19137498214984,2.36514939853218));
#62597=CARTESIAN_POINT('Ctrl Pts',(2.19509696471665,2.11618713243843,2.43061094850698));
#62598=CARTESIAN_POINT('Ctrl Pts',(2.20126084637904,2.04111121592341,2.49597504496293));
#62599=CARTESIAN_POINT('Ctrl Pts',(2.20742472804142,1.96289712224357,2.55795059180821));
#62600=CARTESIAN_POINT('Ctrl Pts',(2.21358860970381,1.88188474811586,2.61622387369829));
#62601=CARTESIAN_POINT('Ctrl Pts',(2.21590376188548,1.85145652366623,2.63811130163582));
#62602=CARTESIAN_POINT('Ctrl Pts',(2.21821891406715,1.82063390650502,2.65947680130358));
#62603=CARTESIAN_POINT('Ctrl Pts',(2.22053406624882,1.78943621037804,2.68030513402633));
#62604=CARTESIAN_POINT('Origin',(-1.72497344927317,0.,0.));
#62605=CARTESIAN_POINT('',(3.71684364332268,1.78943621037804,2.68030513402633));
#62606=CARTESIAN_POINT('',(3.47041119666184,1.78943621037803,2.68030513402633));
#62607=CARTESIAN_POINT('',(-1.72497344927317,1.78943621037804,2.68030513402633));
#62608=CARTESIAN_POINT('',(2.89657344930667,-3.22274890153366,-0.00266085768222635));
#62609=CARTESIAN_POINT('Ctrl Pts',(2.89657344930667,-3.22274890153366,-0.0026608576822207));
#62610=CARTESIAN_POINT('Ctrl Pts',(2.90385415680925,-3.22265127549824,-0.120902506046961));
#62611=CARTESIAN_POINT('Ctrl Pts',(2.91113486431182,-3.21604242047407,-0.238865259363918));
#62612=CARTESIAN_POINT('Ctrl Pts',(2.91841557181439,-3.20303727403663,-0.355906987332332));
#62613=CARTESIAN_POINT('Ctrl Pts',(2.92578180427762,-3.18987935884191,-0.474323580198954));
#62614=CARTESIAN_POINT('Ctrl Pts',(2.93314803674085,-3.17017407925754,-0.591797313652501));
#62615=CARTESIAN_POINT('Ctrl Pts',(2.94051426920408,-3.14408976635058,-0.707684324843768));
#62616=CARTESIAN_POINT('Ctrl Pts',(2.94687552402374,-3.12156414527831,-0.807760831002979));
#62617=CARTESIAN_POINT('Ctrl Pts',(2.9532367788434,-3.09428217040264,-0.906654364654217));
#62618=CARTESIAN_POINT('Ctrl Pts',(2.95959803366306,-3.06238066868043,-1.00396324763031));
#62619=CARTESIAN_POINT('Ctrl Pts',(2.96577029116436,-3.03142698282921,-1.09838101580951));
#62620=CARTESIAN_POINT('Ctrl Pts',(2.97194254866565,-2.99604816420421,-1.19153210136813));
#62621=CARTESIAN_POINT('Ctrl Pts',(2.97811480616694,-2.95636635020544,-1.28297138154869));
#62622=CARTESIAN_POINT('Ctrl Pts',(2.98427870432196,-2.91673827894566,-1.37428682169089));
#62623=CARTESIAN_POINT('Ctrl Pts',(2.99044260247699,-2.87281896696189,-1.46389466950883));
#62624=CARTESIAN_POINT('Ctrl Pts',(2.99660650063201,-2.8247801555252,-1.55136541003435));
#62625=CARTESIAN_POINT('Ctrl Pts',(3.00276387187365,-2.77679221208686,-1.6387435283373));
#62626=CARTESIAN_POINT('Ctrl Pts',(3.00892124311529,-2.72469364943321,-1.72398865971088));
#62627=CARTESIAN_POINT('Ctrl Pts',(3.01507861435693,-2.66870368702595,-1.80669261175058));
#62628=CARTESIAN_POINT('Ctrl Pts',(3.02123148816823,-2.61275462047277,-1.88933615566336));
#62629=CARTESIAN_POINT('Ctrl Pts',(3.02738436197953,-2.55292004798889,-1.96944185189964));
#62630=CARTESIAN_POINT('Ctrl Pts',(3.03353723579083,-2.48946390168153,-2.04662821360515));
#62631=CARTESIAN_POINT('Ctrl Pts',(3.0396877786396,-2.42603179518119,-2.12378533393139));
#62632=CARTESIAN_POINT('Ctrl Pts',(3.04583832148837,-2.35898111656308,-2.19802498210599));
#62633=CARTESIAN_POINT('Ctrl Pts',(3.05198886433714,-2.28861715374865,-2.26899737462771));
#62634=CARTESIAN_POINT('Ctrl Pts',(3.05813872230041,-2.21826102621949,-2.33996186411328));
#62635=CARTESIAN_POINT('Ctrl Pts',(3.06428858026368,-2.14459265383724,-2.40765951280687));
#62636=CARTESIAN_POINT('Ctrl Pts',(3.07043843822696,-2.06795467750557,-2.47177689411541));
#62637=CARTESIAN_POINT('Ctrl Pts',(3.07658925637862,-1.99130473554876,-2.53590428618606));
#62638=CARTESIAN_POINT('Ctrl Pts',(3.08274007453028,-1.91168460190081,-2.59645002181334));
#62639=CARTESIAN_POINT('Ctrl Pts',(3.08889089268194,-1.82946973436362,-2.65314116728596));
#62640=CARTESIAN_POINT('Ctrl Pts',(3.09504828879816,-1.74716694250944,-2.70989294084684));
#62641=CARTESIAN_POINT('Ctrl Pts',(3.10120568491439,-1.66226423382163,-2.76278164543452));
#62642=CARTESIAN_POINT('Ctrl Pts',(3.10736308103061,-1.57516567043588,-2.81157796854014));
#62643=CARTESIAN_POINT('Ctrl Pts',(3.11352391352038,-1.48801849832103,-2.86040152432513));
#62644=CARTESIAN_POINT('Ctrl Pts',(3.11968474601016,-1.39867341941258,-2.90512795579674));
#62645=CARTESIAN_POINT('Ctrl Pts',(3.12584557849993,-1.30755680027941,-2.94557511812941));
#62646=CARTESIAN_POINT('Ctrl Pts',(3.13201671107229,-1.21628784642471,-2.9860899026727));
#62647=CARTESIAN_POINT('Ctrl Pts',(3.13818784364465,-1.12324184126048,-3.02231096981099));
#62648=CARTESIAN_POINT('Ctrl Pts',(3.14435897621701,-1.02886284865085,-3.0541052374085));
#62649=CARTESIAN_POINT('Ctrl Pts',(3.14905440161224,-0.957052769466965,
-3.07829651992425));
#62650=CARTESIAN_POINT('Ctrl Pts',(3.15374982700747,-0.884471360269048,
-3.09992604749025));
#62651=CARTESIAN_POINT('Ctrl Pts',(3.1584452524027,-0.811317954453893,-3.11895507169962));
#62652=CARTESIAN_POINT('Ctrl Pts',(3.16461750160968,-0.715156049402839,
-3.14396918004966));
#62653=CARTESIAN_POINT('Ctrl Pts',(3.17078975081665,-0.617666974353875,
-3.16457593251688));
#62654=CARTESIAN_POINT('Ctrl Pts',(3.17696200002363,-0.519291210154257,
-3.18063738919678));
#62655=CARTESIAN_POINT('Ctrl Pts',(3.18312588983436,-0.421048681338786,
-3.19667709301542));
#62656=CARTESIAN_POINT('Ctrl Pts',(3.18928977964509,-0.321922275196099,
-3.20818366725772));
#62657=CARTESIAN_POINT('Ctrl Pts',(3.19545366945582,-0.222366164594063,
-3.21506933849703));
#62658=CARTESIAN_POINT('Ctrl Pts',(3.2016110323146,-0.122915474103324,-3.22194771848898));
#62659=CARTESIAN_POINT('Ctrl Pts',(3.20776839517339,-0.0230364147158,-3.22421489357896));
#62660=CARTESIAN_POINT('Ctrl Pts',(3.21392575803217,0.0768091053907777,
-3.22183455873033));
#62661=CARTESIAN_POINT('Ctrl Pts',(3.22007862343751,0.176581696454737,-3.21945596252297));
#62662=CARTESIAN_POINT('Ctrl Pts',(3.22623148884285,0.276320364000828,-3.21243661580049));
#62663=CARTESIAN_POINT('Ctrl Pts',(3.23238435424819,0.375561488131964,-3.20079226616351));
#62664=CARTESIAN_POINT('Ctrl Pts',(3.23853488867949,0.474765015392593,-3.18915232791453));
#62665=CARTESIAN_POINT('Ctrl Pts',(3.24468542311079,0.573470942832583,-3.17289091883314));
#62666=CARTESIAN_POINT('Ctrl Pts',(3.25083595754209,0.671219958122833,-3.1520757177323));
#62667=CARTESIAN_POINT('Ctrl Pts',(3.25698580708638,0.76895808866282,-3.13126283448873));
#62668=CARTESIAN_POINT('Ctrl Pts',(3.26313565663066,0.865739094052329,-3.10589725785115));
#62669=CARTESIAN_POINT('Ctrl Pts',(3.26928550617495,0.961114048533461,-3.07609774685585));
#62670=CARTESIAN_POINT('Ctrl Pts',(3.2754363159161,1.05650389422965,-3.04629358316184));
#62671=CARTESIAN_POINT('Ctrl Pts',(3.28158712565725,1.15048683832345,-3.01205423960778));
#62672=CARTESIAN_POINT('Ctrl Pts',(3.2877379353984,1.24263027357175,-2.97354797602174));
#62673=CARTESIAN_POINT('Ctrl Pts',(3.2938953231697,1.33487225231609,-2.93500053161991));
#62674=CARTESIAN_POINT('Ctrl Pts',(3.300052710941,1.42527039219857,-2.89217722258056));
#62675=CARTESIAN_POINT('Ctrl Pts',(3.3062100987123,1.51341331384771,-2.84529395739149));
#62676=CARTESIAN_POINT('Ctrl Pts',(3.31237092288049,1.60160542747125,-2.79838452696602));
#62677=CARTESIAN_POINT('Ctrl Pts',(3.31853174704868,1.68753944272647,-2.74741084962619));
#62678=CARTESIAN_POINT('Ctrl Pts',(3.32469257121686,1.77083159789182,-2.69263310059278));
#62679=CARTESIAN_POINT('Ctrl Pts',(3.33086369559309,1.85426300821244,-2.63776376929774));
#62680=CARTESIAN_POINT('Ctrl Pts',(3.33703481996932,1.93504338424352,-2.57907791786674));
#62681=CARTESIAN_POINT('Ctrl Pts',(3.34320594434554,2.01282066713522,-2.51687713733772));
#62682=CARTESIAN_POINT('Ctrl Pts',(3.34790145327781,2.07200014631612,-2.46954956739062));
#62683=CARTESIAN_POINT('Ctrl Pts',(3.35259696221008,2.12944165980346,-2.42018790724988));
#62684=CARTESIAN_POINT('Ctrl Pts',(3.35729247114235,2.18500482297474,-2.36893889454269));
#62685=CARTESIAN_POINT('Ctrl Pts',(3.36346471603464,2.25804258203986,-2.30157208479331));
#62686=CARTESIAN_POINT('Ctrl Pts',(3.36963696092693,2.32809045580273,-2.23070574890648));
#62687=CARTESIAN_POINT('Ctrl Pts',(3.37580920581922,2.39479423544368,-2.15663583675727));
#62688=CARTESIAN_POINT('Ctrl Pts',(3.38197309122092,2.46140767362416,-2.08266624252222));
#62689=CARTESIAN_POINT('Ctrl Pts',(3.38813697662262,2.5246857317135,-2.00550201584714));
#62690=CARTESIAN_POINT('Ctrl Pts',(3.39430086202433,2.58430899788456,-1.92547775005397));
#62691=CARTESIAN_POINT('Ctrl Pts',(3.40045822038607,2.64386912799526,-1.8455382232763));
#62692=CARTESIAN_POINT('Ctrl Pts',(3.40661557874781,2.6997819022575,-1.76274502481236));
#62693=CARTESIAN_POINT('Ctrl Pts',(3.41277293710955,2.75176702188678,-1.67746708455229));
#62694=CARTESIAN_POINT('Ctrl Pts',(3.41892579790345,2.80371416961501,-1.59225143453088));
#62695=CARTESIAN_POINT('Ctrl Pts',(3.42507865869735,2.85173914117513,-1.50455502092003));
#62696=CARTESIAN_POINT('Ctrl Pts',(3.43123151949125,2.89560449933464,-1.41477635898151));
#62697=CARTESIAN_POINT('Ctrl Pts',(3.43738204924227,2.93945323887819,-1.32503171014963));
#62698=CARTESIAN_POINT('Ctrl Pts',(3.44353257899329,2.97914530582987,-1.23320677031985));
#62699=CARTESIAN_POINT('Ctrl Pts',(3.44968310874432,3.0144892770641,-1.13972451099621));
#62700=CARTESIAN_POINT('Ctrl Pts',(3.45583295354482,3.04982931223552,-1.04625266227533));
#62701=CARTESIAN_POINT('Ctrl Pts',(3.46198279834532,3.08082206077932,-0.951124267311737));
#62702=CARTESIAN_POINT('Ctrl Pts',(3.46813264314583,3.10732468480901,-0.854781179996733));
#62703=CARTESIAN_POINT('Ctrl Pts',(3.47428344808497,3.1338314465355,-0.758423051209431));
#62704=CARTESIAN_POINT('Ctrl Pts',(3.4804342530241,3.15584657612648,-0.660850272249102));
#62705=CARTESIAN_POINT('Ctrl Pts',(3.48658505796324,3.17327769977594,-0.562517735369062));
#62706=CARTESIAN_POINT('Ctrl Pts',(3.49274244087121,3.19072746511363,-0.464080036909504));
#62707=CARTESIAN_POINT('Ctrl Pts',(3.49889982377918,3.20358335904078,-0.364881386549443));
#62708=CARTESIAN_POINT('Ctrl Pts',(3.50505720668715,3.21180456834944,-0.265384583632243));
#62709=CARTESIAN_POINT('Ctrl Pts',(3.51121802595036,3.220030365808,-0.165832252844545));
#62710=CARTESIAN_POINT('Ctrl Pts',(3.51737884521358,3.22361631196527,-0.0659818722363817));
#62711=CARTESIAN_POINT('Ctrl Pts',(3.52353966447679,3.22257376432983,0.0337030555450616));
#62712=CARTESIAN_POINT('Ctrl Pts',(3.52971078393028,3.22152947367312,0.133554645206927));
#62713=CARTESIAN_POINT('Ctrl Pts',(3.53588190338377,3.21584125693355,0.233239795633299));
#62714=CARTESIAN_POINT('Ctrl Pts',(3.54205302283725,3.20557245304592,0.332299278923597));
#62715=CARTESIAN_POINT('Ctrl Pts',(3.54674857851883,3.19775900188832,0.407672851430785));
#62716=CARTESIAN_POINT('Ctrl Pts',(3.55144413420041,3.18729466636823,0.482684279285471));
#62717=CARTESIAN_POINT('Ctrl Pts',(3.55613968988199,3.1742269775727,0.557136121023987));
#62718=CARTESIAN_POINT('Ctrl Pts',(3.56231279094659,3.15704729340199,0.655015642568272));
#62719=CARTESIAN_POINT('Ctrl Pts',(3.56848589201118,3.13530584823963,0.752272099629848));
#62720=CARTESIAN_POINT('Ctrl Pts',(3.57465899307578,3.10906010156392,0.848447315608531));
#62721=CARTESIAN_POINT('Ctrl Pts',(3.58082173739428,3.08285838794904,0.944461176332702));
#62722=CARTESIAN_POINT('Ctrl Pts',(3.58698448171277,3.0521675228787,1.03939698999922));
#62723=CARTESIAN_POINT('Ctrl Pts',(3.59314722603127,3.01709620244243,1.1328053971038));
#62724=CARTESIAN_POINT('Ctrl Pts',(3.59930404400262,2.98205860802314,1.22612397886146));
#62725=CARTESIAN_POINT('Ctrl Pts',(3.60546086197397,2.94264907967364,1.31791766835387));
#62726=CARTESIAN_POINT('Ctrl Pts',(3.61161767994533,2.89902635809779,1.40775130529305));
#62727=CARTESIAN_POINT('Ctrl Pts',(3.61777022437955,2.85543391568907,1.49752258739491));
#62728=CARTESIAN_POINT('Ctrl Pts',(3.62392276881378,2.80763428156778,1.58533613155658));
#62729=CARTESIAN_POINT('Ctrl Pts',(3.630075313248,2.75583426623992,1.67077678327114));
#62730=CARTESIAN_POINT('Ctrl Pts',(3.6362252329377,2.70405634938012,1.75618098504453));
#62731=CARTESIAN_POINT('Ctrl Pts',(3.6423751526274,2.64828166987867,1.83921393652311));
#62732=CARTESIAN_POINT('Ctrl Pts',(3.6485250723171,2.58876244520109,1.91948601579081));
#62733=CARTESIAN_POINT('Ctrl Pts',(3.65467598423213,2.52923361771805,1.99977104612038));
#62734=CARTESIAN_POINT('Ctrl Pts',(3.66082689614716,2.46595928868833,2.0772939592081));
#62735=CARTESIAN_POINT('Ctrl Pts',(3.66697780806219,2.39923406070027,2.15169549064817));
#62736=CARTESIAN_POINT('Ctrl Pts',(3.67312908450406,2.332504878317,2.22610143141091));
#62737=CARTESIAN_POINT('Ctrl Pts',(3.67928036094594,2.26232468623143,2.29738530431221));
#62738=CARTESIAN_POINT('Ctrl Pts',(3.68543163738781,2.18902626992494,2.36522336198477));
#62739=CARTESIAN_POINT('Ctrl Pts',(3.69158813076747,2.11566568875208,2.43311895355781));
#62740=CARTESIAN_POINT('Ctrl Pts',(3.69774462414714,2.03918192636869,2.49756260392495));
#62741=CARTESIAN_POINT('Ctrl Pts',(3.7039011175268,1.95994206271907,2.55826985935506));
#62742=CARTESIAN_POINT('Ctrl Pts',(3.7082152927921,1.90441456700022,2.60081059214712));
#62743=CARTESIAN_POINT('Ctrl Pts',(3.71252946805739,1.84753438604866,2.64151739378657));
#62744=CARTESIAN_POINT('Ctrl Pts',(3.71684364332268,1.78943621037804,2.68030513402633));
#62745=CARTESIAN_POINT('Ctrl Pts',(2.46694827513675,1.78943621037803,2.68030513402633));
#62746=CARTESIAN_POINT('Ctrl Pts',(2.47309858708958,1.70631803001642,2.7357968315169));
#62747=CARTESIAN_POINT('Ctrl Pts',(2.47924889904241,1.62062286331172,2.78741412951648));
#62748=CARTESIAN_POINT('Ctrl Pts',(2.48539921099525,1.53275181053506,2.83492318234577));
#62749=CARTESIAN_POINT('Ctrl Pts',(2.49177457642762,1.44166536212804,2.88417069620453));
#62750=CARTESIAN_POINT('Ctrl Pts',(2.49814994186,1.34824116592263,2.92900328203538));
#62751=CARTESIAN_POINT('Ctrl Pts',(2.50452530729238,1.25295192047284,2.9692135402297));
#62752=CARTESIAN_POINT('Ctrl Pts',(2.51068485063132,1.16088845472983,3.00806258043689));
#62753=CARTESIAN_POINT('Ctrl Pts',(2.51684439397026,1.06708461404918,3.04259710715594));
#62754=CARTESIAN_POINT('Ctrl Pts',(2.5230039373092,0.971983818768544,3.07268042896623));
#62755=CARTESIAN_POINT('Ctrl Pts',(2.52948721378829,0.87188471803028,3.10434486932706));
#62756=CARTESIAN_POINT('Ctrl Pts',(2.53597049026739,0.770349159965806,3.13107732305021));
#62757=CARTESIAN_POINT('Ctrl Pts',(2.54245376674648,0.667906563794865,3.1527794696965));
#62758=CARTESIAN_POINT('Ctrl Pts',(2.54893704322558,0.565463967623921,3.17448161634279));
#62759=CARTESIAN_POINT('Ctrl Pts',(2.55542031970468,0.462114891302979,3.19115344258992));
#62760=CARTESIAN_POINT('Ctrl Pts',(2.56190359618377,0.358393190207404,3.20276004154432));
#62761=CARTESIAN_POINT('Ctrl Pts',(2.56807585854909,0.259647200551854,3.21380985164366));
#62762=CARTESIAN_POINT('Ctrl Pts',(2.57424812091441,0.160215915954576,3.2203080957865));
#62763=CARTESIAN_POINT('Ctrl Pts',(2.58042038327972,0.0605549853338471,
3.22218104026624));
#62764=CARTESIAN_POINT('Ctrl Pts',(2.58658428659543,-0.0389709752201438,
3.22405144823102));
#62765=CARTESIAN_POINT('Ctrl Pts',(2.59274818991113,-0.138725533162269,
3.22130899885287));
#62766=CARTESIAN_POINT('Ctrl Pts',(2.59891209322684,-0.238246639486325,
3.21393156449752));
#62767=CARTESIAN_POINT('Ctrl Pts',(2.60506946991764,-0.337662368276467,
3.20656194170966));
#62768=CARTESIAN_POINT('Ctrl Pts',(2.61122684660845,-0.436844706088377,
3.19456712292281));
#62769=CARTESIAN_POINT('Ctrl Pts',(2.61738422329925,-0.535331285272566,
3.17797702595667));
#62770=CARTESIAN_POINT('Ctrl Pts',(2.62353710297378,-0.633745935164174,
3.16139904550376));
#62771=CARTESIAN_POINT('Ctrl Pts',(2.62968998264831,-0.731465409659298,
3.1402325313951));
#62772=CARTESIAN_POINT('Ctrl Pts',(2.63584286232284,-0.828033067762345,
3.11455916642983));
#62773=CARTESIAN_POINT('Ctrl Pts',(2.64199341128746,-0.92456414605074,3.08889552653142));
#62774=CARTESIAN_POINT('Ctrl Pts',(2.64814396025207,-1.01994385556388,3.05872853944413));
#62775=CARTESIAN_POINT('Ctrl Pts',(2.65429450921669,-1.11372722245748,3.02419067461976));
#62776=CARTESIAN_POINT('Ctrl Pts',(2.66044437354207,-1.20750014999481,2.98965665432655));
#62777=CARTESIAN_POINT('Ctrl Pts',(2.66659423786746,-1.29967668058446,2.95075287371668));
#62778=CARTESIAN_POINT('Ctrl Pts',(2.67274410219285,-1.38982940309251,2.90766087995136));
#62779=CARTESIAN_POINT('Ctrl Pts',(2.67889492694671,-1.47999620481225,2.86456215648021));
#62780=CARTESIAN_POINT('Ctrl Pts',(2.68504575170057,-1.56813817873332,2.81727410803243));
#62781=CARTESIAN_POINT('Ctrl Pts',(2.69119657645443,-1.65385112258556,2.76602495050614));
#62782=CARTESIAN_POINT('Ctrl Pts',(2.69735397950775,-1.73965573632506,2.71472098206936));
#62783=CARTESIAN_POINT('Ctrl Pts',(2.70351138256106,-1.82302575882768,2.6594476682448));
#62784=CARTESIAN_POINT('Ctrl Pts',(2.70966878561438,-1.9035847918134,2.60047736057762));
#62785=CARTESIAN_POINT('Ctrl Pts',(2.71582962523795,-1.98418878641267,2.54147414039789));
#62786=CARTESIAN_POINT('Ctrl Pts',(2.72199046486152,-2.06197832891767,2.47877008981964));
#62787=CARTESIAN_POINT('Ctrl Pts',(2.72815130448509,-2.13661066740312,2.41267743771089));
#62788=CARTESIAN_POINT('Ctrl Pts',(2.73432244444248,-2.21136778401089,2.34647428501759));
#62789=CARTESIAN_POINT('Ctrl Pts',(2.74049358439987,-2.2829568412898,2.27687151723568));
#62790=CARTESIAN_POINT('Ctrl Pts',(2.74666472435726,-2.35107237070964,2.2042178363732));
#62791=CARTESIAN_POINT('Ctrl Pts',(2.75136008787931,-2.40289864176029,2.1489386747888));
#62792=CARTESIAN_POINT('Ctrl Pts',(2.75605545140136,-2.45271484194789,2.09189407818914));
#62793=CARTESIAN_POINT('Ctrl Pts',(2.76075081492341,-2.50040295090739,2.03324928269841));
#62794=CARTESIAN_POINT('Ctrl Pts',(2.76690134343908,-2.56287033445203,1.95642956783138));
#62795=CARTESIAN_POINT('Ctrl Pts',(2.77305187195475,-2.62191048814613,1.87658535584688));
#62796=CARTESIAN_POINT('Ctrl Pts',(2.77920240047041,-2.67721494782827,1.79405621027461));
#62797=CARTESIAN_POINT('Ctrl Pts',(2.78534493015722,-2.73244748346243,1.71163439474877));
#62798=CARTESIAN_POINT('Ctrl Pts',(2.79148745984403,-2.78395373460758,1.62653494104741));
#62799=CARTESIAN_POINT('Ctrl Pts',(2.79762998953084,-2.83146485192257,1.53913103887456));
#62800=CARTESIAN_POINT('Ctrl Pts',(2.80376620097837,-2.87892709904517,1.45181704082852));
#62801=CARTESIAN_POINT('Ctrl Pts',(2.80990241242589,-2.92240217001727,1.36220368580563));
#62802=CARTESIAN_POINT('Ctrl Pts',(2.81603862387342,-2.96166458789849,1.27069289416762));
#62803=CARTESIAN_POINT('Ctrl Pts',(2.82217019162361,-3.00089729318147,1.17925135510072));
#62804=CARTESIAN_POINT('Ctrl Pts',(2.8283017593738,-3.03592351039349,1.08591563407114));
#62805=CARTESIAN_POINT('Ctrl Pts',(2.834433327124,-3.06656427008512,0.991111063371452));
#62806=CARTESIAN_POINT('Ctrl Pts',(2.84056261682008,-3.09719364585161,0.896341715301602));
#62807=CARTESIAN_POINT('Ctrl Pts',(2.84669190651617,-3.12344066455406,0.800105016553149));
#62808=CARTESIAN_POINT('Ctrl Pts',(2.85282119621226,-3.14517528780142,0.702844201443844));
#62809=CARTESIAN_POINT('Ctrl Pts',(2.85894917939328,-3.16690527811184,0.605604118381222));
#62810=CARTESIAN_POINT('Ctrl Pts',(2.86507716257431,-3.18412469451779,0.507340780662209));
#62811=CARTESIAN_POINT('Ctrl Pts',(2.87120514575533,-3.19675425206134,0.408509258680556));
#62812=CARTESIAN_POINT('Ctrl Pts',(2.87733501507794,-3.20938769687629,0.30964731718919));
#62813=CARTESIAN_POINT('Ctrl Pts',(2.88346488440056,-3.21742840928701,0.210217276517037));
#62814=CARTESIAN_POINT('Ctrl Pts',(2.88959475372317,-3.22084886858185,0.110680297501366));
#62815=CARTESIAN_POINT('Ctrl Pts',(2.89192098557315,-3.22214690299898,0.0729068836403979));
#62816=CARTESIAN_POINT('Ctrl Pts',(2.89424721742312,-3.2227800936602,0.0351180933736112));
#62817=CARTESIAN_POINT('Ctrl Pts',(2.8965734492731,-3.22274890153411,-0.00266085713696655));
#62818=CARTESIAN_POINT('',(2.65002655068888,-3.22274940472809,0.00195878144663014));
#62819=CARTESIAN_POINT('Ctrl Pts',(2.22053406624882,1.78943621037804,2.68030513402633));
#62820=CARTESIAN_POINT('Ctrl Pts',(2.22698785384915,1.70246857774578,2.7383668184918));
#62821=CARTESIAN_POINT('Ctrl Pts',(2.23344164144948,1.61258358561053,2.79225052418815));
#62822=CARTESIAN_POINT('Ctrl Pts',(2.23989542904981,1.52022580284294,2.84165991471016));
#62823=CARTESIAN_POINT('Ctrl Pts',(2.24604743268732,1.43218673947039,2.88875888496492));
#62824=CARTESIAN_POINT('Ctrl Pts',(2.25219943632483,1.34190135858284,2.93179231733081));
#62825=CARTESIAN_POINT('Ctrl Pts',(2.25835143996234,1.24978285820519,2.97054883310079));
#62826=CARTESIAN_POINT('Ctrl Pts',(2.26450181180627,1.15768879187974,3.00929506886484));
#62827=CARTESIAN_POINT('Ctrl Pts',(2.27065218365019,1.06376297245931,3.04376647412016));
#62828=CARTESIAN_POINT('Ctrl Pts',(2.27680255549412,0.968439931846692,3.07379922260787));
#62829=CARTESIAN_POINT('Ctrl Pts',(2.28295294065452,0.873116684845393,3.10383203612099));
#62830=CARTESIAN_POINT('Ctrl Pts',(2.28910332581493,0.776396625153268,3.12942604385474));
#62831=CARTESIAN_POINT('Ctrl Pts',(2.29525371097533,0.67872988283739,3.15046715720757));
#62832=CARTESIAN_POINT('Ctrl Pts',(2.30140575411951,0.581036812109558,3.17151394269696));
#62833=CARTESIAN_POINT('Ctrl Pts',(2.30755779726369,0.482396976245193,3.18800530393077));
#62834=CARTESIAN_POINT('Ctrl Pts',(2.31370984040787,0.383270145989764,3.19987836607784));
#62835=CARTESIAN_POINT('Ctrl Pts',(2.31986883114248,0.284031370385205,3.21176483664404));
#62836=CARTESIAN_POINT('Ctrl Pts',(2.32602782187709,0.184304934504294,3.21902254740279));
#62837=CARTESIAN_POINT('Ctrl Pts',(2.3321868126117,0.0845549822087228,3.2216405785692));
#62838=CARTESIAN_POINT('Ctrl Pts',(2.33834986641296,-0.0152607748138019,
3.22426033684246));
#62839=CARTESIAN_POINT('Ctrl Pts',(2.34451292021421,-0.115099645594101,
3.2222343312196));
#62840=CARTESIAN_POINT('Ctrl Pts',(2.35067597401546,-0.214500279457155,
3.21560370577794));
#62841=CARTESIAN_POINT('Ctrl Pts',(2.35684856104054,-0.314054669643128,
3.20896282385654));
#62842=CARTESIAN_POINT('Ctrl Pts',(2.36302114806561,-0.413169039665234,
3.19770315608448));
#62843=CARTESIAN_POINT('Ctrl Pts',(2.36919373509068,-0.511390087318214,
3.18191730582249));
#62844=CARTESIAN_POINT('Ctrl Pts',(2.37127081294605,-0.544441506793105,
3.17660536127248));
#62845=CARTESIAN_POINT('Ctrl Pts',(2.37334789080142,-0.577391886665494,
3.17078132761479));
#62846=CARTESIAN_POINT('Ctrl Pts',(2.37542496865678,-0.610224342440297,
3.16445000187921));
#62847=CARTESIAN_POINT('Ctrl Pts',(2.38159736003055,-0.707791588790864,
3.14563538679203));
#62848=CARTESIAN_POINT('Ctrl Pts',(2.38776975140431,-0.804659501487889,
3.12227111501522));
#62849=CARTESIAN_POINT('Ctrl Pts',(2.39394214277808,-0.900371102754934,
3.09442231116308));
#62850=CARTESIAN_POINT('Ctrl Pts',(2.40010617797621,-0.995953129777267,
3.06661120898637));
#62851=CARTESIAN_POINT('Ctrl Pts',(2.40627021317434,-1.09038154341743,3.03432776212098));
#62852=CARTESIAN_POINT('Ctrl Pts',(2.41243424837247,-1.18320860454814,2.99768826942083));
#62853=CARTESIAN_POINT('Ctrl Pts',(2.41859175963029,-1.27593741863991,2.96108755551667));
#62854=CARTESIAN_POINT('Ctrl Pts',(2.42474927088812,-1.36706784796038,2.92014012026545));
#62855=CARTESIAN_POINT('Ctrl Pts',(2.43090678214594,-1.45616732866535,2.87501204752739));
#62856=CARTESIAN_POINT('Ctrl Pts',(2.43705979988732,-1.54520178797373,2.82991690753249));
#62857=CARTESIAN_POINT('Ctrl Pts',(2.44321281762869,-1.63220785903381,2.78064739136689));
#62858=CARTESIAN_POINT('Ctrl Pts',(2.44936583537007,-1.71677384112069,2.72741730231069));
#62859=CARTESIAN_POINT('Ctrl Pts',(2.45551652450848,-1.80130781930221,2.67420735812468));
#62860=CARTESIAN_POINT('Ctrl Pts',(2.46166721364688,-1.88340317621615,2.61704005043262));
#62861=CARTESIAN_POINT('Ctrl Pts',(2.46781790278529,-1.96267445496097,2.556174201095));
#62862=CARTESIAN_POINT('Ctrl Pts',(2.47396790923187,-2.04193693504074,2.49531510752353));
#62863=CARTESIAN_POINT('Ctrl Pts',(2.48011791567845,-2.11837561563714,2.43075855299986));
#62864=CARTESIAN_POINT('Ctrl Pts',(2.48626792212503,-2.1916364039487,2.36280499309334));
#62865=CARTESIAN_POINT('Ctrl Pts',(2.49241889078954,-2.26490865449929,2.29484080130632));
#62866=CARTESIAN_POINT('Ctrl Pts',(2.49856985945406,-2.33500170669935,2.22347884386782));
#62867=CARTESIAN_POINT('Ctrl Pts',(2.50472082811857,-2.40159750585018,2.14905723106534));
#62868=CARTESIAN_POINT('Ctrl Pts',(2.51087837698962,-2.46826454810708,2.07455600322823));
#62869=CARTESIAN_POINT('Ctrl Pts',(2.51703592586067,-2.53142657611034,1.9969889081573));
#62870=CARTESIAN_POINT('Ctrl Pts',(2.52319347473172,-2.59080520688077,1.91672792604988));
#62871=CARTESIAN_POINT('Ctrl Pts',(2.52935446145952,-2.65021698967818,1.83642213296905));
#62872=CARTESIAN_POINT('Ctrl Pts',(2.53551544818731,-2.7058409267516,1.75341981840851));
#62873=CARTESIAN_POINT('Ctrl Pts',(2.54167643491511,-2.7574426183601,1.6681210294674));
#62874=CARTESIAN_POINT('Ctrl Pts',(2.54784772257175,-2.80913058597878,1.5826796242873));
#62875=CARTESIAN_POINT('Ctrl Pts',(2.55401901022839,-2.85678266769303,1.49493445708755));
#62876=CARTESIAN_POINT('Ctrl Pts',(2.56019029788503,-2.9002109070008,1.40530931022803));
#62877=CARTESIAN_POINT('Ctrl Pts',(2.5648842610555,-2.93324300130765,1.33713923585895));
#62878=CARTESIAN_POINT('Ctrl Pts',(2.56957822422597,-2.96383242873378,1.26788202310293));
#62879=CARTESIAN_POINT('Ctrl Pts',(2.57427218739644,-2.99191570283412,1.19773034930013));
#62880=CARTESIAN_POINT('Ctrl Pts',(2.5812281548249,-3.03353220744489,1.09377283188832));
#62881=CARTESIAN_POINT('Ctrl Pts',(2.58818412225336,-3.06976700649434,0.987543649318438));
#62882=CARTESIAN_POINT('Ctrl Pts',(2.59514008968182,-3.10039628824057,0.879579682782686));
#62883=CARTESIAN_POINT('Ctrl Pts',(2.60207254730286,-3.13092204901395,0.77198061330658));
#62884=CARTESIAN_POINT('Ctrl Pts',(2.6090050049239,-3.15587999011657,0.662658666473282));
#62885=CARTESIAN_POINT('Ctrl Pts',(2.61593746254494,-3.17509501101313,0.552167758511445));
#62886=CARTESIAN_POINT('Ctrl Pts',(2.62282775611551,-3.19419316381541,0.442348869691205));
#62887=CARTESIAN_POINT('Ctrl Pts',(2.62971804968608,-3.20761793720828,0.331375411940045));
#62888=CARTESIAN_POINT('Ctrl Pts',(2.63660834325665,-3.21524508618567,0.219810368861196));
#62889=CARTESIAN_POINT('Ctrl Pts',(2.6410810790674,-3.22019614117566,0.147389512145142));
#62890=CARTESIAN_POINT('Ctrl Pts',(2.64555381487814,-3.22270518073489,0.074719756395053));
#62891=CARTESIAN_POINT('Ctrl Pts',(2.65002655068888,-3.22274940472809,0.00195878144664628));
#62892=CARTESIAN_POINT('Ctrl Pts',(2.65002655072688,-3.22274940472846,0.00195878082847808));
#62893=CARTESIAN_POINT('Ctrl Pts',(2.65623082264165,-3.22281074919503,-0.0989702461627191));
#62894=CARTESIAN_POINT('Ctrl Pts',(2.66243509455643,-3.21812646153104,-0.199913400276856));
#62895=CARTESIAN_POINT('Ctrl Pts',(2.6686393664712,-3.20871911843152,-0.30039837135389));
#62896=CARTESIAN_POINT('Ctrl Pts',(2.67484458885946,-3.19931033415883,-0.400898736388821));
#62897=CARTESIAN_POINT('Ctrl Pts',(2.68104981124771,-3.18517709478693,-0.500940356932082));
#62898=CARTESIAN_POINT('Ctrl Pts',(2.68725503363597,-3.16639382626989,-0.60005641356455));
#62899=CARTESIAN_POINT('Ctrl Pts',(2.69346275534655,-3.14760299227988,-0.699212391888294));
#62900=CARTESIAN_POINT('Ctrl Pts',(2.69967047705712,-3.12415848302303,-0.797441648834382));
#62901=CARTESIAN_POINT('Ctrl Pts',(2.7058781987677,-3.09618558234046,-0.894288768914743));
#62902=CARTESIAN_POINT('Ctrl Pts',(2.71209432393503,-3.06817481445441,-0.991266991938087));
#62903=CARTESIAN_POINT('Ctrl Pts',(2.71831044910236,-3.03562353304882,-1.08685893474145));
#62904=CARTESIAN_POINT('Ctrl Pts',(2.72452657426969,-2.99870658257103,-1.18062542499523));
#62905=CARTESIAN_POINT('Ctrl Pts',(2.73074730314363,-2.96176229113661,-1.27446135937998));
#62906=CARTESIAN_POINT('Ctrl Pts',(2.73696803201756,-2.92044606429033,-1.36646876259605));
#62907=CARTESIAN_POINT('Ctrl Pts',(2.74318876089149,-2.87497959467187,-1.45623140081525));
#62908=CARTESIAN_POINT('Ctrl Pts',(2.74942070735249,-2.82943113722022,-1.54615590434469));
#62909=CARTESIAN_POINT('Ctrl Pts',(2.75565265381348,-2.77971769847653,-1.63382719011838));
#62910=CARTESIAN_POINT('Ctrl Pts',(2.76188460027447,-2.72610544442492,-1.71885620933713));
#62911=CARTESIAN_POINT('Ctrl Pts',(2.76562953556167,-2.69388847605383,-1.76995231173488));
#62912=CARTESIAN_POINT('Ctrl Pts',(2.76937447084887,-2.66026441834211,-1.82009485367877));
#62913=CARTESIAN_POINT('Ctrl Pts',(2.77311940613607,-2.62529792475211,-1.86920527732838));
#62914=CARTESIAN_POINT('Ctrl Pts',(2.77929171094779,-2.56766706064283,-1.95014779861423));
#62915=CARTESIAN_POINT('Ctrl Pts',(2.78546401575951,-2.50618786891869,-2.02856497857034));
#62916=CARTESIAN_POINT('Ctrl Pts',(2.79163632057123,-2.44110933590487,-2.10406814829228));
#62917=CARTESIAN_POINT('Ctrl Pts',(2.7978002664343,-2.3761189366,-2.1794690665639));
#62918=CARTESIAN_POINT('Ctrl Pts',(2.80396421229737,-2.30753916564686,-2.25196349228689));
#62919=CARTESIAN_POINT('Ctrl Pts',(2.81012815816044,-2.23566172760433,-2.32119240956566));
#62920=CARTESIAN_POINT('Ctrl Pts',(2.81628557744201,-2.16386039567438,-2.39034802506969));
#62921=CARTESIAN_POINT('Ctrl Pts',(2.82244299672357,-2.08876864956578,-2.45624470655207));
#62922=CARTESIAN_POINT('Ctrl Pts',(2.82860041600513,-2.01071718314817,-2.5185579151357));
#62923=CARTESIAN_POINT('Ctrl Pts',(2.8347533381567,-1.93272272236467,-2.58082561267217));
#62924=CARTESIAN_POINT('Ctrl Pts',(2.84090626030827,-1.85177317745502,-2.63951477061048));
#62925=CARTESIAN_POINT('Ctrl Pts',(2.84705918245984,-1.7682339904531,-2.69433964405126));
#62926=CARTESIAN_POINT('Ctrl Pts',(2.85320977381804,-1.68472644899764,-2.74914374923776));
#62927=CARTESIAN_POINT('Ctrl Pts',(2.85936036517623,-1.59863157740502,-2.80008624049596));
#62928=CARTESIAN_POINT('Ctrl Pts',(2.86551095653443,-1.51034487473563,-2.84692394030115));
#62929=CARTESIAN_POINT('Ctrl Pts',(2.87166086311904,-1.4220680014303,-2.89375642545012));
#62930=CARTESIAN_POINT('Ctrl Pts',(2.87781076970365,-1.33160016592131,-2.93648482417372));
#62931=CARTESIAN_POINT('Ctrl Pts',(2.88396067628826,-1.23936171878009,-2.97491177894782));
#62932=CARTESIAN_POINT('Ctrl Pts',(2.89011154311597,-1.14710886957738,-3.01334473368594));
#62933=CARTESIAN_POINT('Ctrl Pts',(2.89626240994369,-1.05308526061636,-3.0474747433944));
#62934=CARTESIAN_POINT('Ctrl Pts',(2.90241327677141,-0.957730533264694,
-3.0771528704555));
#62935=CARTESIAN_POINT('Ctrl Pts',(2.9085707213467,-0.862273833403293,-3.10686273535682));
#62936=CARTESIAN_POINT('Ctrl Pts',(2.914728165922,-0.765483588118864,-3.13211108134687));
#62937=CARTESIAN_POINT('Ctrl Pts',(2.9208856104973,-0.667813777359608,-3.15279912478875));
#62938=CARTESIAN_POINT('Ctrl Pts',(2.9270464914016,-0.570089459312684,-3.17349871375453));
#62939=CARTESIAN_POINT('Ctrl Pts',(2.93320737230589,-0.471485026918437,
-3.1896328616928));
#62940=CARTESIAN_POINT('Ctrl Pts',(2.93936825321019,-0.372461729326465,
-3.20115445155137));
#62941=CARTESIAN_POINT('Ctrl Pts',(2.94553943361812,-0.273272888717306,
-3.21269530272313));
#62942=CARTESIAN_POINT('Ctrl Pts',(2.95171061402605,-0.173664217725312,
-3.21960816307786));
#62943=CARTESIAN_POINT('Ctrl Pts',(2.95788179443398,-0.0740992724655996,
-3.22189802140292));
#62944=CARTESIAN_POINT('Ctrl Pts',(2.96257673791456,0.0016482765836582,
-3.22364011200862));
#62945=CARTESIAN_POINT('Ctrl Pts',(2.96727168139514,0.0773704706349393,
-3.22270751540126));
#62946=CARTESIAN_POINT('Ctrl Pts',(2.97196662487572,0.152865534961373,-3.21912250321745));
#62947=CARTESIAN_POINT('Ctrl Pts',(2.97813888724918,0.252116004504065,-3.21440942500851));
#62948=CARTESIAN_POINT('Ctrl Pts',(2.98431114962264,0.3513229829132,-3.20509368556077));
#62949=CARTESIAN_POINT('Ctrl Pts',(2.9904834119961,0.450024894527647,-3.19117457322619));
#62950=CARTESIAN_POINT('Ctrl Pts',(2.99664731532029,0.548593134873285,-3.1772743114425));
#62951=CARTESIAN_POINT('Ctrl Pts',(3.00281121864447,0.646657241635713,-3.15878312828077));
#62952=CARTESIAN_POINT('Ctrl Pts',(3.00897512196866,0.743757484854407,-3.13575228074908));
#62953=CARTESIAN_POINT('Ctrl Pts',(3.01513249866829,0.840754913866283,-3.11274581933881));
#62954=CARTESIAN_POINT('Ctrl Pts',(3.02128987536792,0.936790088033487,-3.08520934963691));
#62955=CARTESIAN_POINT('Ctrl Pts',(3.02744725206756,1.03141119745655,-3.05324556894156));
#62956=CARTESIAN_POINT('Ctrl Pts',(3.03360013175136,1.12596320072481,-3.02130513286761));
#62957=CARTESIAN_POINT('Ctrl Pts',(3.03975301143516,1.21910278225954,-2.98494395308761));
#62958=CARTESIAN_POINT('Ctrl Pts',(3.04590589111896,1.31039197699404,-2.94431493375448));
#62959=CARTESIAN_POINT('Ctrl Pts',(3.05205644009313,1.4016465913993,-2.90370130468598));
#62960=CARTESIAN_POINT('Ctrl Pts',(3.0582069890673,1.49105181533694,-2.85882322477603));
#62961=CARTESIAN_POINT('Ctrl Pts',(3.06435753804148,1.57818923945029,-2.80988189911663));
#62962=CARTESIAN_POINT('Ctrl Pts',(3.07050740237668,1.66531696399429,-2.7609460212862));
#62963=CARTESIAN_POINT('Ctrl Pts',(3.07665726671188,1.75017701186951,-2.7079480096469));
#62964=CARTESIAN_POINT('Ctrl Pts',(3.08280713104708,1.8323760803352,-2.65113475001091));
#62965=CARTESIAN_POINT('Ctrl Pts',(3.08895795581103,1.91458798588874,-2.59431261780716));
#62966=CARTESIAN_POINT('Ctrl Pts',(3.09510878057498,1.9941377292465,-2.5336743011308));
#62967=CARTESIAN_POINT('Ctrl Pts',(3.10125960533894,2.07066230816602,-2.46950909454503));
#62968=CARTESIAN_POINT('Ctrl Pts',(3.10741700840269,2.14726873003199,-2.40527526334686));
#62969=CARTESIAN_POINT('Ctrl Pts',(3.11357441146643,2.22084319318331,-2.33750728957088));
#62970=CARTESIAN_POINT('Ctrl Pts',(3.11973181453018,2.29105713233226,-2.26653364830295));
#62971=CARTESIAN_POINT('Ctrl Pts',(3.12589265416439,2.36131025929246,-2.19552039521874));
#62972=CARTESIAN_POINT('Ctrl Pts',(3.13205349379859,2.42819883626417,-2.12129823426576));
#62973=CARTESIAN_POINT('Ctrl Pts',(3.1382143334328,2.49143382992998,-2.04422969198191));
#62974=CARTESIAN_POINT('Ctrl Pts',(3.14438547340107,2.55477454645137,-1.96703229847354));
#62975=CARTESIAN_POINT('Ctrl Pts',(3.15055661336933,2.6144492185164,-1.88697936634528));
#62976=CARTESIAN_POINT('Ctrl Pts',(3.1567277533376,2.67021139739144,-1.80446353682773));
#62977=CARTESIAN_POINT('Ctrl Pts',(3.16142311676352,2.71263851727304,-1.74168067823614));
#62978=CARTESIAN_POINT('Ctrl Pts',(3.16611848018944,2.75280155671635,-1.67747265830885));
#62979=CARTESIAN_POINT('Ctrl Pts',(3.17081384361537,2.79061012582739,-1.61202130511033));
#62980=CARTESIAN_POINT('Ctrl Pts',(3.1769860681354,2.84031085315475,-1.52598314140801));
#62981=CARTESIAN_POINT('Ctrl Pts',(3.18315829265544,2.88611633399345,-1.43749286806601));
#62982=CARTESIAN_POINT('Ctrl Pts',(3.18933051717548,2.92777638832986,-1.34693837366012));
#62983=CARTESIAN_POINT('Ctrl Pts',(3.19549438190015,2.96938001738102,-1.25650652823439));
#62984=CARTESIAN_POINT('Ctrl Pts',(3.20165824662482,3.00684919972532,-1.16401640990137));
#62985=CARTESIAN_POINT('Ctrl Pts',(3.20782211134949,3.0399784693731,-1.06988245534169));
#62986=CARTESIAN_POINT('Ctrl Pts',(3.21397944875849,3.07307265629101,-0.975848185324895));
#62987=CARTESIAN_POINT('Ctrl Pts',(3.22013678616748,3.10183592401484,-0.880173947369748));
#62988=CARTESIAN_POINT('Ctrl Pts',(3.22629412357647,3.12611036071096,-0.78329533073776));
#62989=CARTESIAN_POINT('Ctrl Pts',(3.23244696308815,3.15036706507955,-0.68648748334266));
#62990=CARTESIAN_POINT('Ctrl Pts',(3.23859980259983,3.17014135250086,-0.588477426529155));
#62991=CARTESIAN_POINT('Ctrl Pts',(3.24475264211151,3.18532503143249,-0.489716251138973));
#62992=CARTESIAN_POINT('Ctrl Pts',(3.25090315038462,3.20050295744665,-0.39099249519726));
#62993=CARTESIAN_POINT('Ctrl Pts',(3.25705365865773,3.21109366507162,-0.291518615015593));
#62994=CARTESIAN_POINT('Ctrl Pts',(3.26320416693084,3.21704016779057,-0.191755368430845));
#62995=CARTESIAN_POINT('Ctrl Pts',(3.26935399008264,3.22298600811291,-0.0920032347368021));
#62996=CARTESIAN_POINT('Ctrl Pts',(3.27550381323444,3.22428864621116,0.00803776766592394));
#62997=CARTESIAN_POINT('Ctrl Pts',(3.28165363638624,3.2209430979592,0.107903300269344));
#62998=CARTESIAN_POINT('Ctrl Pts',(3.28780441953062,3.21759702746432,0.207784421966731));
#62999=CARTESIAN_POINT('Ctrl Pts',(3.29395520267501,3.20960134396411,0.307489585282811));
#63000=CARTESIAN_POINT('Ctrl Pts',(3.3001059858194,3.19700312176381,0.406557009449417));
#63001=CARTESIAN_POINT('Ctrl Pts',(3.30626334683947,3.18439142655731,0.505730379994744));
#63002=CARTESIAN_POINT('Ctrl Pts',(3.31242070785954,3.16716741857891,0.604264217714333));
#63003=CARTESIAN_POINT('Ctrl Pts',(3.31857806887961,3.14542975161115,0.701704524838918));
#63004=CARTESIAN_POINT('Ctrl Pts',(3.32473886616897,3.12367995339477,0.799199210963468));
#63005=CARTESIAN_POINT('Ctrl Pts',(3.33089966345832,3.09741159392134,0.895598732033169));
#63006=CARTESIAN_POINT('Ctrl Pts',(3.33706046074768,3.06677334679193,0.990463932663182));
#63007=CARTESIAN_POINT('Ctrl Pts',(3.34323155831427,3.03608387537701,1.08548773904182));
#63008=CARTESIAN_POINT('Ctrl Pts',(3.34940265588086,3.00101007536719,1.178971694106));
#63009=CARTESIAN_POINT('Ctrl Pts',(3.35557375344745,2.96174897914172,1.27049618143975));
#63010=CARTESIAN_POINT('Ctrl Pts',(3.3602695230833,2.93187405632025,1.34013985566801));
#63011=CARTESIAN_POINT('Ctrl Pts',(3.36496529271915,2.8995756340568,1.40864937726985));
#63012=CARTESIAN_POINT('Ctrl Pts',(3.369661062355,2.86495782129977,1.47585034629982));
#63013=CARTESIAN_POINT('Ctrl Pts',(3.37583326514642,2.8194555549831,1.56418049040802));
#63014=CARTESIAN_POINT('Ctrl Pts',(3.38200546793785,2.76978438610278,1.65055979252062));
#63015=CARTESIAN_POINT('Ctrl Pts',(3.38817767072928,2.71613533611053,1.73456807258515));
#63016=CARTESIAN_POINT('Ctrl Pts',(3.3943418226725,2.66255626443436,1.81846677460538));
#63017=CARTESIAN_POINT('Ctrl Pts',(3.40050597461572,2.60500985405945,1.90000023739665));
#63018=CARTESIAN_POINT('Ctrl Pts',(3.40667012655894,2.54373367116966,1.97877148065605));
#63019=CARTESIAN_POINT('Ctrl Pts',(3.41282693327524,2.48253050521263,2.05744885980216));
#63020=CARTESIAN_POINT('Ctrl Pts',(3.41898373999155,2.41760667358952,2.13337022645203));
#63021=CARTESIAN_POINT('Ctrl Pts',(3.42514054670785,2.34924314121892,2.20616731594316));
#63022=CARTESIAN_POINT('Ctrl Pts',(3.43129310438258,2.28092678906758,2.27891416545218));
#63023=CARTESIAN_POINT('Ctrl Pts',(3.43744566205732,2.20917575047399,2.34854070754722));
#63024=CARTESIAN_POINT('Ctrl Pts',(3.44359821973205,2.1343109395226,2.41471206895028));
#63025=CARTESIAN_POINT('Ctrl Pts',(3.44974841764773,2.05947484230707,2.48085805091315));
#63026=CARTESIAN_POINT('Ctrl Pts',(3.4558986155634,1.98152767094381,2.54355119831489));
#63027=CARTESIAN_POINT('Ctrl Pts',(3.46204881347908,1.90082614629056,2.60249448108506));
#63028=CARTESIAN_POINT('Ctrl Pts',(3.46483627454,1.86424970426183,2.62920941087715));
#63029=CARTESIAN_POINT('Ctrl Pts',(3.46762373560092,1.82710793091848,2.65515458680447));
#63030=CARTESIAN_POINT('Ctrl Pts',(3.47041119666184,1.78943621037803,2.68030513402633));
#63031=CARTESIAN_POINT('Origin',(-1.72497344927317,0.,0.));
#63032=CARTESIAN_POINT('',(4.96704894786217,1.78943621037804,2.68030513402633));
#63033=CARTESIAN_POINT('',(4.7207101123806,1.78943616882057,2.68030516177109));
#63034=CARTESIAN_POINT('',(-1.72497344927317,1.78943621037804,2.68030513402633));
#63035=CARTESIAN_POINT('',(4.14657344921911,-3.22274994184251,-0.000612253281709201));
#63036=CARTESIAN_POINT('Ctrl Pts',(4.1465734492731,-3.22274994184235,-0.000612254151029935));
#63037=CARTESIAN_POINT('Ctrl Pts',(4.14860941488238,-3.22274371421397,-0.0333929040906794));
#63038=CARTESIAN_POINT('Ctrl Pts',(4.15064538049165,-3.22223735157171,-0.066168248405641));
#63039=CARTESIAN_POINT('Ctrl Pts',(4.15268134610092,-3.22123125223858,-0.0989281663706331));
#63040=CARTESIAN_POINT('Ctrl Pts',(4.15885359442719,-3.21818115409513,-0.198243374794371));
#63041=CARTESIAN_POINT('Ctrl Pts',(4.16502584275346,-3.21052833720515,-0.297592198081419));
#63042=CARTESIAN_POINT('Ctrl Pts',(4.17119809107972,-3.19826435630236,-0.396513139386145));
#63043=CARTESIAN_POINT('Ctrl Pts',(4.17736197996862,-3.18601698522712,-0.49530010626698));
#63044=CARTESIAN_POINT('Ctrl Pts',(4.18352586885752,-3.16917091607389,-0.593659915717286));
#63045=CARTESIAN_POINT('Ctrl Pts',(4.18968975774641,-3.14776969585369,-0.691132045534844));
#63046=CARTESIAN_POINT('Ctrl Pts',(4.19584711964366,-3.12639113755816,-0.788500961328129));
#63047=CARTESIAN_POINT('Ctrl Pts',(4.20200448154091,-3.10046711038163,-0.884983644310407));
#63048=CARTESIAN_POINT('Ctrl Pts',(4.20816184343815,-3.07009272710254,-0.980126629314843));
#63049=CARTESIAN_POINT('Ctrl Pts',(4.21431470782583,-3.03974053012367,-1.07520011921845));
#63050=CARTESIAN_POINT('Ctrl Pts',(4.2204675722135,-3.00494457162692,-1.16893544412282));
#63051=CARTESIAN_POINT('Ctrl Pts',(4.22662043660117,-2.96585039615279,-1.2608921405657));
#63052=CARTESIAN_POINT('Ctrl Pts',(4.23277096998064,-2.92677103147865,-1.3528139992809));
#63053=CARTESIAN_POINT('Ctrl Pts',(4.23892150336011,-2.88339685516167,-1.44295816912987));
#63054=CARTESIAN_POINT('Ctrl Pts',(4.24507203673957,-2.83592203354208,-1.53090293035533));
#63055=CARTESIAN_POINT('Ctrl Pts',(4.251221885199,-2.78845249869272,-1.61883789810019));
#63056=CARTESIAN_POINT('Ctrl Pts',(4.25737173365843,-2.73688343276047,-1.70457356193074));
#63057=CARTESIAN_POINT('Ctrl Pts',(4.26352158211785,-2.68145509702484,-1.78771253985072));
#63058=CARTESIAN_POINT('Ctrl Pts',(4.26967239074222,-2.62601810736143,-1.87086449811191));
#63059=CARTESIAN_POINT('Ctrl Pts',(4.27582319936658,-2.56672089207044,-1.95141860375034));
#63060=CARTESIAN_POINT('Ctrl Pts',(4.28197400799094,-2.50384662286267,-2.02900706052966));
#63061=CARTESIAN_POINT('Ctrl Pts',(4.28813139460239,-2.44090511271866,-2.10667849434459));
#63062=CARTESIAN_POINT('Ctrl Pts',(4.29428878121383,-2.37437918357418,-2.18137760777539));
#63063=CARTESIAN_POINT('Ctrl Pts',(4.30044616782528,-2.30459175906569,-2.25277038034206));
#63064=CARTESIAN_POINT('Ctrl Pts',(4.3066069908079,-2.2347653869469,-2.32420299644649));
#63065=CARTESIAN_POINT('Ctrl Pts',(4.31276781379052,-2.16167421232127,-2.39232530076201));
#63066=CARTESIAN_POINT('Ctrl Pts',(4.31892863677314,-2.08567586774788,-2.45684222879576));
#63067=CARTESIAN_POINT('Ctrl Pts',(4.32509975993361,-2.00955046280174,-2.52146702161224));
#63068=CARTESIAN_POINT('Ctrl Pts',(4.33127088309407,-1.93050852333384,-2.58247413233613));
#63069=CARTESIAN_POINT('Ctrl Pts',(4.33744200625453,-1.84893850573749,-2.63961057061477));
#63070=CARTESIAN_POINT('Ctrl Pts',(4.34213752578321,-1.78687304364591,-2.68308487095854));
#63071=CARTESIAN_POINT('Ctrl Pts',(4.34683304531188,-1.72334459615962,-2.72431912931856));
#63072=CARTESIAN_POINT('Ctrl Pts',(4.35152856484056,-1.65853347065144,-2.76321991329479));
#63073=CARTESIAN_POINT('Ctrl Pts',(4.35770081291735,-1.57333941654742,-2.81435489156858));
#63074=CARTESIAN_POINT('Ctrl Pts',(4.36387306099414,-1.48562834827015,-2.86163619811208));
#63075=CARTESIAN_POINT('Ctrl Pts',(4.37004530907093,-1.3957839145922,-2.90480719261463));
#63076=CARTESIAN_POINT('Ctrl Pts',(4.37620919770796,-1.30606116253211,-2.94791971809199));
#63077=CARTESIAN_POINT('Ctrl Pts',(4.38237308634498,-1.21421117603225,-2.98693280975896));
#63078=CARTESIAN_POINT('Ctrl Pts',(4.38853697498201,-1.1206448967466,-3.02163409066945));
#63079=CARTESIAN_POINT('Ctrl Pts',(4.39469433662532,-1.02717769558391,-3.05629862610066));
#63080=CARTESIAN_POINT('Ctrl Pts',(4.40085169826864,-0.931998219814458,
-3.08666027783024));
#63081=CARTESIAN_POINT('Ctrl Pts',(4.40700905991195,-0.835539356792753,
-3.11255386230509));
#63082=CARTESIAN_POINT('Ctrl Pts',(4.41316192404367,-0.739150950060656,
-3.13842853337137));
#63083=CARTESIAN_POINT('Ctrl Pts',(4.41931478817538,-0.64148543228148,-3.15984151350616));
#63084=CARTESIAN_POINT('Ctrl Pts',(4.4254676523071,-0.542992022632832,-3.17667707295802));
#63085=CARTESIAN_POINT('Ctrl Pts',(4.43161818542945,-0.444535927161101,
-3.19350625426694));
#63086=CARTESIAN_POINT('Ctrl Pts',(4.4377687185518,-0.345252990723664,-3.20576138754103));
#63087=CARTESIAN_POINT('Ctrl Pts',(4.44391925167414,-0.245602955433838,
-3.21337777903286));
#63088=CARTESIAN_POINT('Ctrl Pts',(4.45006909987557,-0.145964017132235,
-3.22099332236637));
#63089=CARTESIAN_POINT('Ctrl Pts',(4.456218948077,-0.0459584943661108,-3.22397111782779));
#63090=CARTESIAN_POINT('Ctrl Pts',(4.46236879627843,0.0539494198851558,
-3.2222984068199));
#63091=CARTESIAN_POINT('Ctrl Pts',(4.46851960464423,0.15387293257334,-3.22062543465475));
#63092=CARTESIAN_POINT('Ctrl Pts',(4.47467041301002,0.253698372121929,-3.21430052112014));
#63093=CARTESIAN_POINT('Ctrl Pts',(4.48082122137582,0.352963231245526,-3.20336300157955));
#63094=CARTESIAN_POINT('Ctrl Pts',(4.48697860772943,0.452334249266459,-3.19241378489835));
#63095=CARTESIAN_POINT('Ctrl Pts',(4.49313599408304,0.55114305709235,-3.17684215927443));
#63096=CARTESIAN_POINT('Ctrl Pts',(4.49929338043665,0.648934065630894,-3.15673916264296));
#63097=CARTESIAN_POINT('Ctrl Pts',(4.50545420316144,0.746779650280764,-3.13662494674502));
#63098=CARTESIAN_POINT('Ctrl Pts',(4.51161502588623,0.84360588347207,-3.11197443072196));
#63099=CARTESIAN_POINT('Ctrl Pts',(4.51777584861102,0.938971178766004,-3.08292891386532));
#63100=CARTESIAN_POINT('Ctrl Pts',(4.52394697151633,1.03449591376486,-3.05383483627573));
#63101=CARTESIAN_POINT('Ctrl Pts',(4.53011809442164,1.12855442262882,-3.02033122640812));
#63102=CARTESIAN_POINT('Ctrl Pts',(4.53628921732695,1.2207238452979,-2.98260806275667));
#63103=CARTESIAN_POINT('Ctrl Pts',(4.54098473941138,1.29085428448887,-2.95390502916985));
#63104=CARTESIAN_POINT('Ctrl Pts',(4.5456802614958,1.35989143043535,-2.9227601029014));
#63105=CARTESIAN_POINT('Ctrl Pts',(4.55037578358022,1.42765919263351,-2.88927444044159));
#63106=CARTESIAN_POINT('Ctrl Pts',(4.55654803161821,1.51673968884811,-2.84525764940055));
#63107=CARTESIAN_POINT('Ctrl Pts',(4.56272027965621,1.60393941745078,-2.7970398038875));
#63108=CARTESIAN_POINT('Ctrl Pts',(4.5688925276942,1.68883504750651,-2.74480486461491));
#63109=CARTESIAN_POINT('Ctrl Pts',(4.57505641629111,1.77361569838222,-2.69264067021437));
#63110=CARTESIAN_POINT('Ctrl Pts',(4.58122030488801,1.85609808650302,-2.63647042144559));
#63111=CARTESIAN_POINT('Ctrl Pts',(4.58738419348492,1.9358813581292,-2.57652497169111));
#63112=CARTESIAN_POINT('Ctrl Pts',(4.59354155508686,2.01558014655881,-2.51664299869198));
#63113=CARTESIAN_POINT('Ctrl Pts',(4.5996989166888,2.09258515534237,-2.45299403178666));
#63114=CARTESIAN_POINT('Ctrl Pts',(4.60585627829074,2.16652336397703,-2.38585290322804));
#63115=CARTESIAN_POINT('Ctrl Pts',(4.61200914237935,2.24040756602563,-2.31876081647343));
#63116=CARTESIAN_POINT('Ctrl Pts',(4.61816200646796,2.31122910097951,-2.24818193057484));
#63117=CARTESIAN_POINT('Ctrl Pts',(4.62431487055656,2.37864771852987,-2.17443155643784));
#63118=CARTESIAN_POINT('Ctrl Pts',(4.63046540363475,2.44604079456037,-2.10070912260447));
#63119=CARTESIAN_POINT('Ctrl Pts',(4.63661593671293,2.5100332220557,-2.02381790818875));
#63120=CARTESIAN_POINT('Ctrl Pts',(4.64276646979111,2.5703219927888,-1.94410967177425));
#63121=CARTESIAN_POINT('Ctrl Pts',(4.64891631794738,2.63060404977859,-1.8644103116502));
#63122=CARTESIAN_POINT('Ctrl Pts',(4.65506616610365,2.68718300795863,-1.78189489965333));
#63123=CARTESIAN_POINT('Ctrl Pts',(4.66121601425992,2.73979714078375,-1.69694702034364));
#63124=CARTESIAN_POINT('Ctrl Pts',(4.6673668225796,2.79241948814749,-1.61198587829261));
#63125=CARTESIAN_POINT('Ctrl Pts',(4.67351763089927,2.84107555187938,-1.52459188391078));
#63126=CARTESIAN_POINT('Ctrl Pts',(4.67966843921895,2.88554833880993,-1.43517537147599));
#63127=CARTESIAN_POINT('Ctrl Pts',(4.68582582552524,2.93006868719609,-1.34566323248436));
#63128=CARTESIAN_POINT('Ctrl Pts',(4.69198321183152,2.97039663123149,-1.25412464586935));
#63129=CARTESIAN_POINT('Ctrl Pts',(4.69814059813781,3.00636241114835,-1.16099208237363));
#63130=CARTESIAN_POINT('Ctrl Pts',(4.70430142081453,3.04234826317642,-1.06780754260558));
#63131=CARTESIAN_POINT('Ctrl Pts',(4.71046224349125,3.07396696539453,-0.973027666433112));
#63132=CARTESIAN_POINT('Ctrl Pts',(4.71662306616797,3.10109860971386,-0.877100322272653));
#63133=CARTESIAN_POINT('Ctrl Pts',(4.72279418902449,3.12827561499052,-0.781012598736921));
#63134=CARTESIAN_POINT('Ctrl Pts',(4.728965311881,3.15095047898476,-0.683773998425126));
#63135=CARTESIAN_POINT('Ctrl Pts',(4.73513643473751,3.16905436853162,-0.585842958300801));
#63136=CARTESIAN_POINT('Ctrl Pts',(4.73983195726496,3.18282936915601,-0.511328576440075));
#63137=CARTESIAN_POINT('Ctrl Pts',(4.7445274797924,3.19395907252953,-0.436413526130888));
#63138=CARTESIAN_POINT('Ctrl Pts',(4.74922300231984,3.20243335845127,-0.361300632684886));
#63139=CARTESIAN_POINT('Ctrl Pts',(4.75539525044793,3.21357277799652,-0.262564993944416));
#63140=CARTESIAN_POINT('Ctrl Pts',(4.76156749857602,3.22016128260903,-0.163139920551488));
#63141=CARTESIAN_POINT('Ctrl Pts',(4.76773974670411,3.22212472232074,-0.0634809917178259));
#63142=CARTESIAN_POINT('Ctrl Pts',(4.77390363539251,3.22408550283025,0.0360429631504318));
#63143=CARTESIAN_POINT('Ctrl Pts',(4.7800675240809,3.22143366034395,0.135799713468046));
#63144=CARTESIAN_POINT('Ctrl Pts',(4.7862314127693,3.21414664507579,0.235327232695285));
#63145=CARTESIAN_POINT('Ctrl Pts',(4.792388774464,3.20686734608953,0.33474936139342));
#63146=CARTESIAN_POINT('Ctrl Pts',(4.79854613615871,3.19496266387674,0.433942310753885));
#63147=CARTESIAN_POINT('Ctrl Pts',(4.80470349785342,3.17846209378533,0.532443687980034));
#63148=CARTESIAN_POINT('Ctrl Pts',(4.81085636203633,3.16197357617878,0.630873117003702));
#63149=CARTESIAN_POINT('Ctrl Pts',(4.81700922621924,3.14089591646675,0.728611551091125));
#63150=CARTESIAN_POINT('Ctrl Pts',(4.82316209040215,3.11531038017994,0.825202276804377));
#63151=CARTESIAN_POINT('Ctrl Pts',(4.82931262357554,3.08973453696072,0.921756409169636));
#63152=CARTESIAN_POINT('Ctrl Pts',(4.83546315674894,3.05965432167019,1.01716327769536));
#63153=CARTESIAN_POINT('Ctrl Pts',(4.84161368992234,3.02520179712534,1.11097778968331));
#63154=CARTESIAN_POINT('Ctrl Pts',(4.84776353817463,2.99075310920095,1.2047818545217));
#63155=CARTESIAN_POINT('Ctrl Pts',(4.85391338642692,2.95193322979036,1.29699350761948));
#63156=CARTESIAN_POINT('Ctrl Pts',(4.8600632346792,2.90892331543334,1.38718517416685));
#63157=CARTESIAN_POINT('Ctrl Pts',(4.86621404309559,2.86590668602025,1.47739092216747));
#63158=CARTESIAN_POINT('Ctrl Pts',(4.87236485151199,2.81869890927398,1.56557566508484));
#63159=CARTESIAN_POINT('Ctrl Pts',(4.87851565992838,2.76752783162929,1.65133499437797));
#63160=CARTESIAN_POINT('Ctrl Pts',(4.88467304633186,2.71630202903372,1.73718603905602));
#63161=CARTESIAN_POINT('Ctrl Pts',(4.89083043273534,2.66110468458998,1.82060611669234));
#63162=CARTESIAN_POINT('Ctrl Pts',(4.89698781913883,2.60220780570796,1.90121858249191));
#63163=CARTESIAN_POINT('Ctrl Pts',(4.90314864191316,2.54327805711392,1.98187603723803));
#63164=CARTESIAN_POINT('Ctrl Pts',(4.9093094646875,2.48064493462321,2.05972242124727));
#63165=CARTESIAN_POINT('Ctrl Pts',(4.91547028746184,2.41462035361907,2.1344146997218));
#63166=CARTESIAN_POINT('Ctrl Pts',(4.92164141041565,2.34848538719095,2.20923185500286));
#63167=CARTESIAN_POINT('Ctrl Pts',(4.92781253336947,2.27894793900684,2.28088405963915));
#63168=CARTESIAN_POINT('Ctrl Pts',(4.93398365632328,2.20635643154003,2.34906552899274));
#63169=CARTESIAN_POINT('Ctrl Pts',(4.93867917790202,2.15112256368568,2.40094386021644));
#63170=CARTESIAN_POINT('Ctrl Pts',(4.94337469948076,2.09412131139111,2.45081359014625));
#63171=CARTESIAN_POINT('Ctrl Pts',(4.9480702210595,2.0355178209157,2.49855653592922));
#63172=CARTESIAN_POINT('Ctrl Pts',(4.95439646332706,1.95656176198702,2.56288026153138));
#63173=CARTESIAN_POINT('Ctrl Pts',(4.96072270559462,1.87441123637086,2.62357376170643));
#63174=CARTESIAN_POINT('Ctrl Pts',(4.96704894786217,1.78943621037804,2.68030513402633));
#63175=CARTESIAN_POINT('Ctrl Pts',(3.71684364332268,1.78943621037804,2.68030513402633));
#63176=CARTESIAN_POINT('Ctrl Pts',(3.72320085420584,1.70382486360772,2.73746132941066));
#63177=CARTESIAN_POINT('Ctrl Pts',(3.729558065089,1.61556784701393,2.79044800209424));
#63178=CARTESIAN_POINT('Ctrl Pts',(3.73591527597216,1.52511857513192,2.83903696599526));
#63179=CARTESIAN_POINT('Ctrl Pts',(3.74227248685532,1.43466930324992,2.88762592989628));
#63180=CARTESIAN_POINT('Ctrl Pts',(3.74862969773848,1.34202825831221,2.93181703204401));
#63181=CARTESIAN_POINT('Ctrl Pts',(3.75498690862164,1.24766919048137,2.97143722020566));
#63182=CARTESIAN_POINT('Ctrl Pts',(3.76115915673829,1.15605549551158,3.00990466076362));
#63183=CARTESIAN_POINT('Ctrl Pts',(3.76733140485495,1.06249987373899,3.04419896492224));
#63184=CARTESIAN_POINT('Ctrl Pts',(3.77350365297161,0.967418642046842,3.07412080659174));
#63185=CARTESIAN_POINT('Ctrl Pts',(3.77966754165257,0.872466184413464,3.10400212336554));
#63186=CARTESIAN_POINT('Ctrl Pts',(3.78583143033354,0.775992634399417,3.12952261879608));
#63187=CARTESIAN_POINT('Ctrl Pts',(3.79199531901451,0.67843501282167,3.15053066893145));
#63188=CARTESIAN_POINT('Ctrl Pts',(3.79815268070577,0.580980695768812,3.17151647347901));
#63189=CARTESIAN_POINT('Ctrl Pts',(3.80431004239703,0.482445011648844,3.18799924143239));
#63190=CARTESIAN_POINT('Ctrl Pts',(3.81046740408829,0.383279974942234,3.19987718878526));
#63191=CARTESIAN_POINT('Ctrl Pts',(3.81662026827382,0.284187371096189,3.21174646015986));
#63192=CARTESIAN_POINT('Ctrl Pts',(3.82277313245936,0.184466758610693,3.21901754661746));
#63193=CARTESIAN_POINT('Ctrl Pts',(3.82892599664489,0.0845792668482427,
3.22163994110444));
#63194=CARTESIAN_POINT('Ctrl Pts',(3.83507652982463,-0.0152703826485386,
3.22426134210017));
#63195=CARTESIAN_POINT('Ctrl Pts',(3.84122706300438,-0.115286352056842,
3.22223753913711));
#63196=CARTESIAN_POINT('Ctrl Pts',(3.84737759618413,-0.215004372247607,
3.2155700400418));
#63197=CARTESIAN_POINT('Ctrl Pts',(3.85352744444649,-0.314711287936841,
3.20890328343269));
#63198=CARTESIAN_POINT('Ctrl Pts',(3.85967729270886,-0.41411988696594,3.19759388777563));
#63199=CARTESIAN_POINT('Ctrl Pts',(3.86582714097123,-0.512768898671985,
3.18169540010585));
#63200=CARTESIAN_POINT('Ctrl Pts',(3.87197794940145,-0.611433312320612,
3.16579443022575));
#63201=CARTESIAN_POINT('Ctrl Pts',(3.87812875783167,-0.709337474206959,
3.14530301432027));
#63202=CARTESIAN_POINT('Ctrl Pts',(3.88427956626189,-0.80602920865643,3.12032602099407));
#63203=CARTESIAN_POINT('Ctrl Pts',(3.89043695268496,-0.902824350250759,
3.09532231597859));
#63204=CARTESIAN_POINT('Ctrl Pts',(3.89659433910804,-0.998404053776648,
3.06582356306365));
#63205=CARTESIAN_POINT('Ctrl Pts',(3.90275172553111,-1.09233036180624,3.03198481908737));
#63206=CARTESIAN_POINT('Ctrl Pts',(3.90891254832827,-1.18630908914307,2.99812719005583));
#63207=CARTESIAN_POINT('Ctrl Pts',(3.91507337112543,-1.27863218196992,2.95992491246381));
#63208=CARTESIAN_POINT('Ctrl Pts',(3.92123419392259,-1.36888270774741,2.91758079492756));
#63209=CARTESIAN_POINT('Ctrl Pts',(3.92740531690434,-1.45928412198666,2.87516588291444));
#63210=CARTESIAN_POINT('Ctrl Pts',(3.93357643988609,-1.54760566334814,2.82859550181945));
#63211=CARTESIAN_POINT('Ctrl Pts',(3.93974756286785,-1.63345587410689,2.77811797262926));
#63212=CARTESIAN_POINT('Ctrl Pts',(3.94444308436566,-1.6987781033675,2.73971032394524));
#63213=CARTESIAN_POINT('Ctrl Pts',(3.94913860586347,-1.76267009048399,2.69904158402108));
#63214=CARTESIAN_POINT('Ctrl Pts',(3.95383412736128,-1.82497196443557,2.65623697954911));
#63215=CARTESIAN_POINT('Ctrl Pts',(3.9599753003298,-1.90645526386844,2.60025374530473));
#63216=CARTESIAN_POINT('Ctrl Pts',(3.96611647329832,-1.98551067995544,2.54041410671207));
#63217=CARTESIAN_POINT('Ctrl Pts',(3.97225764626685,-2.06174767113923,2.47695662114862));
#63218=CARTESIAN_POINT('Ctrl Pts',(3.97839048445549,-2.1378811937278,2.41358525987713));
#63219=CARTESIAN_POINT('Ctrl Pts',(3.98452332264413,-2.21120355799046,2.3466060871575));
#63220=CARTESIAN_POINT('Ctrl Pts',(3.99065616083278,-2.28135294761985,2.27630101060607));
#63221=CARTESIAN_POINT('Ctrl Pts',(3.99678253559132,-2.35142840644222,2.20607002894093));
#63222=CARTESIAN_POINT('Ctrl Pts',(4.00290891034986,-2.41833722883924,2.13252041972971));
#63223=CARTESIAN_POINT('Ctrl Pts',(4.0090352851084,-2.48175127719434,2.05597377430848));
#63224=CARTESIAN_POINT('Ctrl Pts',(4.01515727946341,-2.54511998403313,1.97948186030816));
#63225=CARTESIAN_POINT('Ctrl Pts',(4.02127927381843,-2.60499860428731,1.89999750682691));
#63226=CARTESIAN_POINT('Ctrl Pts',(4.02740126817344,-2.66109712391762,1.81787779005558));
#63227=CARTESIAN_POINT('Ctrl Pts',(4.03352105751895,-2.71717543807858,1.73578765102412));
#63228=CARTESIAN_POINT('Ctrl Pts',(4.03964084686445,-2.76947610886918,1.65106439674511));
#63229=CARTESIAN_POINT('Ctrl Pts',(4.04576063620995,-2.81775115050717,1.56409591020357));
#63230=CARTESIAN_POINT('Ctrl Pts',(4.05187990105706,-2.86602205471813,1.47713487732244));
#63231=CARTESIAN_POINT('Ctrl Pts',(4.05799916590417,-2.91026780271043,1.38792937895106));
#63232=CARTESIAN_POINT('Ctrl Pts',(4.06411843075128,-2.95028581219471,1.2968928979922));
#63233=CARTESIAN_POINT('Ctrl Pts',(4.07023885074343,-2.99031137595325,1.2058392319071));
#63234=CARTESIAN_POINT('Ctrl Pts',(4.07635927073557,-3.0261074398551,1.11295429910164));
#63235=CARTESIAN_POINT('Ctrl Pts',(4.08247969072771,-3.05751953874999,1.01867160197094));
#63236=CARTESIAN_POINT('Ctrl Pts',(4.08860663556407,-3.08896512538787,0.924288392144779));
#63237=CARTESIAN_POINT('Ctrl Pts',(4.09473358040043,-3.1160172793467,0.828504861050562));
#63238=CARTESIAN_POINT('Ctrl Pts',(4.10086052523678,-3.13857149017669,0.731769474322391));
#63239=CARTESIAN_POINT('Ctrl Pts',(4.10699115011104,-3.16113924778292,0.634975985244822));
#63240=CARTESIAN_POINT('Ctrl Pts',(4.1131217749853,-3.17920360524386,0.537229934087183));
#63241=CARTESIAN_POINT('Ctrl Pts',(4.11925239985956,-3.19271160062645,0.438987696553426));
#63242=CARTESIAN_POINT('Ctrl Pts',(4.12539264638702,-3.20624079600899,0.340591273637435));
#63243=CARTESIAN_POINT('Ctrl Pts',(4.13153289291448,-3.21519931595962,0.241697546589613));
#63244=CARTESIAN_POINT('Ctrl Pts',(4.13767313944194,-3.21958624004559,0.1427655610052));
#63245=CARTESIAN_POINT('Ctrl Pts',(4.14063990936766,-3.22170586087619,0.0949648028090939));
#63246=CARTESIAN_POINT('Ctrl Pts',(4.14360667929339,-3.22275901660992,0.0471550793021853));
#63247=CARTESIAN_POINT('Ctrl Pts',(4.14657344921911,-3.22274994184251,-0.000612253281710953));
#63248=CARTESIAN_POINT('',(3.90002655072689,-3.222749015224,-0.00251939927735915));
#63249=CARTESIAN_POINT('Ctrl Pts',(3.47041119666184,1.78943621037803,2.68030513402633));
#63250=CARTESIAN_POINT('Ctrl Pts',(3.47656128588147,1.70631955428236,2.73579581388027));
#63251=CARTESIAN_POINT('Ctrl Pts',(3.4827113751011,1.62062143679504,2.78741528527276));
#63252=CARTESIAN_POINT('Ctrl Pts',(3.48886146432073,1.5327422123689,2.8349283717446));
#63253=CARTESIAN_POINT('Ctrl Pts',(3.4950132591234,1.4448386167004,2.88245463485692));
#63254=CARTESIAN_POINT('Ctrl Pts',(3.50116505392607,1.35475309436674,2.92587204395454));
#63255=CARTESIAN_POINT('Ctrl Pts',(3.50731684872874,1.26290954461645,2.96499191307779));
#63256=CARTESIAN_POINT('Ctrl Pts',(3.51347561751752,1.17096187636731,3.00415613046566));
#63257=CARTESIAN_POINT('Ctrl Pts',(3.5196343863063,1.07725260334655,3.03901291458188));
#63258=CARTESIAN_POINT('Ctrl Pts',(3.52579315509507,0.982224312330869,3.06942225227585));
#63259=CARTESIAN_POINT('Ctrl Pts',(3.5319560303526,0.88713265951016,3.09985186593717));
#63260=CARTESIAN_POINT('Ctrl Pts',(3.53811890561013,0.790720656657336,3.12582801726841));
#63261=CARTESIAN_POINT('Ctrl Pts',(3.54428178086766,0.693442729433876,3.1472614672911));
#63262=CARTESIAN_POINT('Ctrl Pts',(3.55045414406345,0.596015039813806,3.16872791477718));
#63263=CARTESIAN_POINT('Ctrl Pts',(3.55662650725925,0.49771919223111,3.18563763084689));
#63264=CARTESIAN_POINT('Ctrl Pts',(3.56279887045505,0.39901621521905,3.19795303631749));
#63265=CARTESIAN_POINT('Ctrl Pts',(3.56470200733491,0.368582932253415,3.20175026950001));
#63266=CARTESIAN_POINT('Ctrl Pts',(3.56660514421478,0.338110950773104,3.20511110214546));
#63267=CARTESIAN_POINT('Ctrl Pts',(3.56850828109465,0.307613771781163,3.20803543152356));
#63268=CARTESIAN_POINT('Ctrl Pts',(3.57468053030192,0.208705390125472,3.21751960992225));
#63269=CARTESIAN_POINT('Ctrl Pts',(3.58085277950919,0.109183892706614,3.22244196246382));
#63270=CARTESIAN_POINT('Ctrl Pts',(3.58702502871646,0.00950603695194093,
3.22273598015126));
#63271=CARTESIAN_POINT('Ctrl Pts',(3.59318891852752,-0.0900368199293453,
3.22302959963533));
#63272=CARTESIAN_POINT('Ctrl Pts',(3.59935280833858,-0.189735183693171,
3.21870734211687));
#63273=CARTESIAN_POINT('Ctrl Pts',(3.60551669814965,-0.289126714756948,
3.20975439953182));
#63274=CARTESIAN_POINT('Ctrl Pts',(3.61167406100881,-0.388412999983746,
3.2008109372307));
#63275=CARTESIAN_POINT('Ctrl Pts',(3.61783142386798,-0.487392668215522,
3.18724657711801));
#63276=CARTESIAN_POINT('Ctrl Pts',(3.62398878672715,-0.585603885382707,
3.16909855509807));
#63277=CARTESIAN_POINT('Ctrl Pts',(3.63014165213293,-0.683743367233776,
3.150963788734));
#63278=CARTESIAN_POINT('Ctrl Pts',(3.63629451753871,-0.781115088106869,
3.12825209553679));
#63279=CARTESIAN_POINT('Ctrl Pts',(3.64244738294449,-0.877263759601254,
3.10105237920779));
#63280=CARTESIAN_POINT('Ctrl Pts',(3.64859791737628,-0.973376005781941,
3.07386296731861));
#63281=CARTESIAN_POINT('Ctrl Pts',(3.65474845180807,-1.06826570573873,3.04218902881309));
#63282=CARTESIAN_POINT('Ctrl Pts',(3.66089898623986,-1.16149004099436,3.00617006291575));
#63283=CARTESIAN_POINT('Ctrl Pts',(3.66704883578467,-1.25470399534181,2.9701551078765));
#63284=CARTESIAN_POINT('Ctrl Pts',(3.67319868532948,-1.34625254849613,2.92979624393343));
#63285=CARTESIAN_POINT('Ctrl Pts',(3.67934853487429,-1.4357112196894,2.88528176373781));
#63286=CARTESIAN_POINT('Ctrl Pts',(3.68549934461603,-1.52518385836927,2.840760333345));
#63287=CARTESIAN_POINT('Ctrl Pts',(3.69165015435776,-1.61256557804487,2.79208219148369));
#63288=CARTESIAN_POINT('Ctrl Pts',(3.6978009640995,-1.69745584298123,2.73948192613656));
#63289=CARTESIAN_POINT('Ctrl Pts',(3.70395835187143,-1.78243689445615,2.68682540703617));
#63290=CARTESIAN_POINT('Ctrl Pts',(3.71011573964336,-1.86492080049206,2.63023861761331));
#63291=CARTESIAN_POINT('Ctrl Pts',(3.71627312741529,-1.9445355248577,2.56999983561603));
#63292=CARTESIAN_POINT('Ctrl Pts',(3.72243395158413,-2.02419468166819,2.50972743475765));
#63293=CARTESIAN_POINT('Ctrl Pts',(3.72859477575297,-2.10098113406282,2.4457992603061));
#63294=CARTESIAN_POINT('Ctrl Pts',(3.73475559992181,-2.17455711951252,2.37853292944988));
#63295=CARTESIAN_POINT('Ctrl Pts',(3.74092672429874,-2.2482561157705,2.31115413682127));
#63296=CARTESIAN_POINT('Ctrl Pts',(3.74709784867567,-2.3187336168382,2.240426347702));
#63297=CARTESIAN_POINT('Ctrl Pts',(3.7532689730526,-2.38568971657671,2.16670305734776));
#63298=CARTESIAN_POINT('Ctrl Pts',(3.75796448197983,-2.43663553209621,2.11060819572134));
#63299=CARTESIAN_POINT('Ctrl Pts',(3.76265999090706,-2.48554343781636,2.05277984879521));
#63300=CARTESIAN_POINT('Ctrl Pts',(3.7673554998343,-2.53229803443386,1.99338511765851));
#63301=CARTESIAN_POINT('Ctrl Pts',(3.77352308979459,-2.59371058527001,1.91536964518692));
#63302=CARTESIAN_POINT('Ctrl Pts',(3.77969067975488,-2.65162685585028,1.83437075499305));
#63303=CARTESIAN_POINT('Ctrl Pts',(3.78585826971516,-2.70574288779974,1.75073498497664));
#63304=CARTESIAN_POINT('Ctrl Pts',(3.79201770503995,-2.75978736886495,1.6672097961149));
#63305=CARTESIAN_POINT('Ctrl Pts',(3.79817714036473,-2.81004136009811,1.58105501493636));
#63306=CARTESIAN_POINT('Ctrl Pts',(3.80433657568952,-2.85624109874265,1.49265010915264));
#63307=CARTESIAN_POINT('Ctrl Pts',(3.81048951699238,-2.90239212803315,1.40433841051642));
#63308=CARTESIAN_POINT('Ctrl Pts',(3.81664245829524,-2.94449719937154,1.31378168439207));
#63309=CARTESIAN_POINT('Ctrl Pts',(3.8227953995981,-2.98233639688537,1.22138739894956));
#63310=CARTESIAN_POINT('Ctrl Pts',(3.82923132885883,-3.0219159063419,1.12474368727824));
#63311=CARTESIAN_POINT('Ctrl Pts',(3.83566725811956,-3.05682748145951,1.02608974805838));
#63312=CARTESIAN_POINT('Ctrl Pts',(3.84210318738029,-3.08687391680823,0.925919534424568));
#63313=CARTESIAN_POINT('Ctrl Pts',(3.84824844188452,-3.11556332352516,0.830273446410853));
#63314=CARTESIAN_POINT('Ctrl Pts',(3.85439369638874,-3.1398173607693,0.733245531105524));
#63315=CARTESIAN_POINT('Ctrl Pts',(3.86053895089296,-3.15951455436372,0.635283671491602));
#63316=CARTESIAN_POINT('Ctrl Pts',(3.86668277880153,-3.17920717533534,0.537344553322039));
#63317=CARTESIAN_POINT('Ctrl Pts',(3.87282660671009,-3.19434497486423,0.438472348615513));
#63318=CARTESIAN_POINT('Ctrl Pts',(3.87897043461866,-3.20485745082501,0.339125761910541));
#63319=CARTESIAN_POINT('Ctrl Pts',(3.88511547167601,-3.21537199571542,0.239759623094642));
#63320=CARTESIAN_POINT('Ctrl Pts',(3.89126050873337,-3.2212593575108,0.13991934830266));
#63321=CARTESIAN_POINT('Ctrl Pts',(3.89740554579072,-3.22250090277616,0.0400686174806361));
#63322=CARTESIAN_POINT('Ctrl Pts',(3.89827921410278,-3.2226774190032,0.0258723777117459));
#63323=CARTESIAN_POINT('Ctrl Pts',(3.89915288241483,-3.22276011248822,0.0116759280118308));
#63324=CARTESIAN_POINT('Ctrl Pts',(3.90002655072689,-3.222749015224,-0.00251939927735915));
#63325=CARTESIAN_POINT('Ctrl Pts',(3.89829624432446,-3.2227489236479,-0.00263393741439584));
#63326=CARTESIAN_POINT('Ctrl Pts',(3.91595129500457,-3.22253094053598,-0.269346743677202));
#63327=CARTESIAN_POINT('Ctrl Pts',(3.93437946122793,-3.18920692885496,-0.534984637514666));
#63328=CARTESIAN_POINT('Ctrl Pts',(3.95516903211871,-3.11145621610261,-0.841051025868991));
#63329=CARTESIAN_POINT('Ctrl Pts',(3.95836463507959,-3.09828573428671,-0.88834265120157));
#63330=CARTESIAN_POINT('Ctrl Pts',(3.96329871450964,-3.07593784755422,-0.962030744259893));
#63331=CARTESIAN_POINT('Ctrl Pts',(3.9650709584551,-3.06748927056815,-0.988638708584469));
#63332=CARTESIAN_POINT('Ctrl Pts',(3.96729513049513,-3.05633221135099,-1.0222559740767));
#63333=CARTESIAN_POINT('Ctrl Pts',(3.96776489670188,-3.0539438401511,-1.02936916922689));
#63334=CARTESIAN_POINT('Ctrl Pts',(3.96851370572064,-3.05008524048497,-1.04072944893667));
#63335=CARTESIAN_POINT('Ctrl Pts',(3.96879367818867,-3.04863095098841,-1.04498185887322));
#63336=CARTESIAN_POINT('Ctrl Pts',(3.96932484246404,-3.04584968754368,-1.05305917867508));
#63337=CARTESIAN_POINT('Ctrl Pts',(3.969576127422,-3.0445244175548,-1.05688458403497));
#63338=CARTESIAN_POINT('Ctrl Pts',(3.97015138851569,-3.0414687597898,-1.065651329487));
#63339=CARTESIAN_POINT('Ctrl Pts',(3.97047507361979,-3.03973353906192,-1.07059095140779));
#63340=CARTESIAN_POINT('Ctrl Pts',(3.97149612218472,-3.03420991239585,-1.08619326721662));
#63341=CARTESIAN_POINT('Ctrl Pts',(3.97219090358894,-3.03037733126317,-1.09684039188465));
#63342=CARTESIAN_POINT('Ctrl Pts',(3.9786022981665,-2.99433214620401,-1.19534474085333));
#63343=CARTESIAN_POINT('Ctrl Pts',(3.9841068925916,-2.95835994717107,-1.28178943134916));
#63344=CARTESIAN_POINT('Ctrl Pts',(3.99110972518947,-2.9067957229066,-1.39191977411194));
#63345=CARTESIAN_POINT('Ctrl Pts',(3.99271202593447,-2.89458882724424,-1.41713006231336));
#63346=CARTESIAN_POINT('Ctrl Pts',(4.00428852625473,-2.80357307851722,-1.59901625877954));
#63347=CARTESIAN_POINT('Ctrl Pts',(4.01395094561155,-2.71241849951249,-1.74918976159062));
#63348=CARTESIAN_POINT('Ctrl Pts',(4.03042749383148,-2.54072946932644,-1.98608731183182));
#63349=CARTESIAN_POINT('Ctrl Pts',(4.03710638507521,-2.46684469302928,-2.077142998892));
#63350=CARTESIAN_POINT('Ctrl Pts',(4.04688930567678,-2.35462230345866,-2.2009924256654));
#63351=CARTESIAN_POINT('Ctrl Pts',(4.04984446173679,-2.32021887943467,-2.23722994215407));
#63352=CARTESIAN_POINT('Ctrl Pts',(4.05481852288709,-2.26161748433221,-2.29614944032516));
#63353=CARTESIAN_POINT('Ctrl Pts',(4.05681737097479,-2.23788630487701,-2.31928451462677));
#63354=CARTESIAN_POINT('Ctrl Pts',(4.05953126288423,-2.20544780410219,-2.34994675160794));
#63355=CARTESIAN_POINT('Ctrl Pts',(4.06023220235083,-2.19705027461547,-2.35779978739771));
#63356=CARTESIAN_POINT('Ctrl Pts',(4.06134673295185,-2.18366818196363,-2.3701806211883));
#63357=CARTESIAN_POINT('Ctrl Pts',(4.06175905420739,-2.17871108628348,-2.37473807132339));
#63358=CARTESIAN_POINT('Ctrl Pts',(4.06261551701357,-2.16840137748681,-2.3841571496871));
#63359=CARTESIAN_POINT('Ctrl Pts',(4.06305975755903,-2.16304661734325,-2.38901636204808));
#63360=CARTESIAN_POINT('Ctrl Pts',(4.06407683804947,-2.15077090230105,-2.4000809349523));
#63361=CARTESIAN_POINT('Ctrl Pts',(4.06465017307326,-2.14383938624236,-2.40627443397515));
#63362=CARTESIAN_POINT('Ctrl Pts',(4.06614639141237,-2.12572092676786,-2.42232334344498));
#63363=CARTESIAN_POINT('Ctrl Pts',(4.06707125096456,-2.11449231445283,-2.43213118042316));
#63364=CARTESIAN_POINT('Ctrl Pts',(4.07304170814661,-2.04182604505612,-2.49471928250622));
#63365=CARTESIAN_POINT('Ctrl Pts',(4.07817919892415,-1.97848995924225,-2.54524133945071));
#63366=CARTESIAN_POINT('Ctrl Pts',(4.09479480746094,-1.77132421879356,-2.69808585921478));
#63367=CARTESIAN_POINT('Ctrl Pts',(4.10659923276721,-1.62097840437645,-2.79099829066499));
#63368=CARTESIAN_POINT('Ctrl Pts',(4.12776499001686,-1.34209428532099,-2.93318331527292));
#63369=CARTESIAN_POINT('Ctrl Pts',(4.13704889169592,-1.21655833503412,-2.98743525391738));
#63370=CARTESIAN_POINT('Ctrl Pts',(4.15046970054646,-1.02646704459472,-3.05560960579081));
#63371=CARTESIAN_POINT('Ctrl Pts',(4.15475995277674,-0.96431830660466,-3.07578867983054));
#63372=CARTESIAN_POINT('Ctrl Pts',(4.16116457666881,-0.868801600061347,
-3.10362176838711));
#63373=CARTESIAN_POINT('Ctrl Pts',(4.16333993794741,-0.835856478455067,
-3.11265617682662));
#63374=CARTESIAN_POINT('Ctrl Pts',(4.16599120262217,-0.794997073074134,
-3.12316532883506));
#63375=CARTESIAN_POINT('Ctrl Pts',(4.16649413383713,-0.787214208670261,
-3.12513612669384));
#63376=CARTESIAN_POINT('Ctrl Pts',(4.16728330530509,-0.774949785126235,
-3.12819303351709));
#63377=CARTESIAN_POINT('Ctrl Pts',(4.16757065511968,-0.770473185579285,
-3.1292986267456));
#63378=CARTESIAN_POINT('Ctrl Pts',(4.16810781299591,-0.762084023043602,
-3.13135141899449));
#63379=CARTESIAN_POINT('Ctrl Pts',(4.16835774720863,-0.7581721014789,-3.1323008846829));
#63380=CARTESIAN_POINT('Ctrl Pts',(4.16892494087611,-0.749275239999326,
-3.1344426055548));
#63381=CARTESIAN_POINT('Ctrl Pts',(4.16924193404962,-0.744289240698065,
-3.13563029705974));
#63382=CARTESIAN_POINT('Ctrl Pts',(4.17018281216945,-0.729450130204712,
-3.13912766342682));
#63383=CARTESIAN_POINT('Ctrl Pts',(4.17080473928084,-0.719588837954609,
-3.14140285388979));
#63384=CARTESIAN_POINT('Ctrl Pts',(4.17525598443436,-0.648647645853428,
-3.15741877596831));
#63385=CARTESIAN_POINT('Ctrl Pts',(4.17899106165022,-0.587184829443091,
-3.16942459992701));
#63386=CARTESIAN_POINT('Ctrl Pts',(4.18916173011016,-0.415915283632065,
-3.19772539964168));
#63387=CARTESIAN_POINT('Ctrl Pts',(4.19544934182919,-0.305554179850657,
-3.21015162654846));
#63388=CARTESIAN_POINT('Ctrl Pts',(4.21755431393519,0.0874498216113729,
-3.23394607130042));
#63389=CARTESIAN_POINT('Ctrl Pts',(4.23308729682306,0.370654043767491,-3.21382288440688));
#63390=CARTESIAN_POINT('Ctrl Pts',(4.25155477586855,0.674258455400089,-3.15154467992324));
#63391=CARTESIAN_POINT('Ctrl Pts',(4.25318660356209,0.700849430980891,-3.14573812355095));
#63392=CARTESIAN_POINT('Ctrl Pts',(4.25606612717574,0.747333206683158,-3.13496903519134));
#63393=CARTESIAN_POINT('Ctrl Pts',(4.25730916102787,0.767258366310866,-3.13015212773323));
#63394=CARTESIAN_POINT('Ctrl Pts',(4.25913808920433,0.79636166062724,-3.12282183015479));
#63395=CARTESIAN_POINT('Ctrl Pts',(4.25971917100869,0.80557703922378,-3.12045729152429));
#63396=CARTESIAN_POINT('Ctrl Pts',(4.26072098326376,0.82141035321995,-3.11631987013151));
#63397=CARTESIAN_POINT('Ctrl Pts',(4.26114107475744,0.828033389607171,-3.11456661606368));
#63398=CARTESIAN_POINT('Ctrl Pts',(4.26197727760211,0.841183904282025,-3.11104049355862));
#63399=CARTESIAN_POINT('Ctrl Pts',(4.26239336944931,0.84771149261833,-3.10926816752015));
#63400=CARTESIAN_POINT('Ctrl Pts',(4.26337473982638,0.863068973691513,-3.10504645305774));
#63401=CARTESIAN_POINT('Ctrl Pts',(4.26394057395368,0.8718940603346,-3.10257993833628));
#63402=CARTESIAN_POINT('Ctrl Pts',(4.26561682598403,0.897949418412696,-3.0951778053476));
#63403=CARTESIAN_POINT('Ctrl Pts',(4.26673069783869,0.915148953000686,-3.09013610988973));
#63404=CARTESIAN_POINT('Ctrl Pts',(4.28126486133419,1.13806839036644,-3.02276747256088));
#63405=CARTESIAN_POINT('Ctrl Pts',(4.29537687310971,1.33705338690073,-2.94016644205476));
#63406=CARTESIAN_POINT('Ctrl Pts',(4.32639973344547,1.74301069113347,-2.72186915882474));
#63407=CARTESIAN_POINT('Ctrl Pts',(4.3433250456539,1.94566558426213,-2.58090206230544));
#63408=CARTESIAN_POINT('Ctrl Pts',(4.36091782157502,2.15160899024179,-2.39947951108252));
#63409=CARTESIAN_POINT('Ctrl Pts',(4.36272024665419,2.17265890588032,-2.38043621678441));
#63410=CARTESIAN_POINT('Ctrl Pts',(4.36497671263521,2.1989843404895,-2.35598013265586));
#63411=CARTESIAN_POINT('Ctrl Pts',(4.36544921676442,2.20449536471763,-2.35082426073199));
#63412=CARTESIAN_POINT('Ctrl Pts',(4.36620136122019,2.21326639038375,-2.34256050775859));
#63413=CARTESIAN_POINT('Ctrl Pts',(4.36648194556313,2.21653803426503,-2.33946510778919));
#63414=CARTESIAN_POINT('Ctrl Pts',(4.36701357296606,2.2227364224219,-2.33357595321866));
#63415=CARTESIAN_POINT('Ctrl Pts',(4.36726471197749,2.22566435921892,-2.33078357924211));
#63416=CARTESIAN_POINT('Ctrl Pts',(4.36783872799068,2.23235606072812,-2.32437759496224));
#63417=CARTESIAN_POINT('Ctrl Pts',(4.36816131830814,2.236116308802,-2.32076035821279));
#63418=CARTESIAN_POINT('Ctrl Pts',(4.36917547428718,2.24793568927166,-2.30933510190075));
#63419=CARTESIAN_POINT('Ctrl Pts',(4.36986450719853,2.25596294352708,-2.30149401086866));
#63420=CARTESIAN_POINT('Ctrl Pts',(4.37604781438054,2.32795000107118,-2.23043791581065));
#63421=CARTESIAN_POINT('Ctrl Pts',(4.38134639890174,2.38928527954381,-2.16460704429943));
#63422=CARTESIAN_POINT('Ctrl Pts',(4.40288769430563,2.63216283490052,-1.88100424711725));
#63423=CARTESIAN_POINT('Ctrl Pts',(4.41816305212166,2.78733281025583,-1.64233218336919));
#63424=CARTESIAN_POINT('Ctrl Pts',(4.43885838217843,2.94193992404305,-1.31790304328928));
#63425=CARTESIAN_POINT('Ctrl Pts',(4.44328939140737,2.97216077692852,-1.24825399633594));
#63426=CARTESIAN_POINT('Ctrl Pts',(4.45051345702558,3.01657237848328,-1.1351176767666));
#63427=CARTESIAN_POINT('Ctrl Pts',(4.45325439504823,3.03234611333544,-1.09228100074657));
#63428=CARTESIAN_POINT('Ctrl Pts',(4.45681548597968,3.05143810003533,-1.03682796817928));
#63429=CARTESIAN_POINT('Ctrl Pts',(4.45760763056258,3.05559745101562,-1.02450520913099));
#63430=CARTESIAN_POINT('Ctrl Pts',(4.4588891876824,3.06218513172882,-1.00459111132922));
#63431=CARTESIAN_POINT('Ctrl Pts',(4.45937705490786,3.06466011764314,-0.997015267418113));
#63432=CARTESIAN_POINT('Ctrl Pts',(4.46030931507377,3.06932687629583,-0.982548915553051));
#63433=CARTESIAN_POINT('Ctrl Pts',(4.46075354100511,3.07152361369001,-0.975660050526738));
#63434=CARTESIAN_POINT('Ctrl Pts',(4.46177050000567,3.07649085479769,-0.959899972315114));
#63435=CARTESIAN_POINT('Ctrl Pts',(4.46234372773577,3.07924619518045,-0.951024081226524));
#63436=CARTESIAN_POINT('Ctrl Pts',(4.46383948733479,3.08631989785583,-0.927884237699482));
#63437=CARTESIAN_POINT('Ctrl Pts',(4.46476399346217,3.09057773973611,-0.913602152527389));
#63438=CARTESIAN_POINT('Ctrl Pts',(4.47072877998744,3.11731407203665,-0.82159425254196));
#63439=CARTESIAN_POINT('Ctrl Pts',(4.47586075644791,3.13695602921426,-0.743080826215379));
#63440=CARTESIAN_POINT('Ctrl Pts',(4.48165066748825,3.15543798602923,-0.655291066412104));
#63441=CARTESIAN_POINT('Ctrl Pts',(4.48222057837829,3.15721853205701,-0.646657872358586));
#63442=CARTESIAN_POINT('Ctrl Pts',(4.48567380185249,3.16777390325158,-0.594395934104295));
#63443=CARTESIAN_POINT('Ctrl Pts',(4.48858136530917,3.17567936920568,-0.550598125370181));
#63444=CARTESIAN_POINT('Ctrl Pts',(4.49187560835493,3.18354548803674,-0.501184932064398));
#63445=CARTESIAN_POINT('Ctrl Pts',(4.49224042986894,3.18440172683359,-0.495715495199595));
#63446=CARTESIAN_POINT('Ctrl Pts',(4.49280733337037,3.18570916257407,-0.487220740518793));
#63447=CARTESIAN_POINT('Ctrl Pts',(4.493009186346,3.18617015481057,-0.484196925819996));
#63448=CARTESIAN_POINT('Ctrl Pts',(4.50975732666851,3.22404370250798,-0.233374463300362));
#63449=CARTESIAN_POINT('Ctrl Pts',(4.52700603721973,3.23242676764566,0.0179129766843247));
#63450=CARTESIAN_POINT('Ctrl Pts',(4.54804329181867,3.20614746278597,0.333283250996289));
#63451=CARTESIAN_POINT('Ctrl Pts',(4.55237211309135,3.19866283930282,0.398768713610387));
#63452=CARTESIAN_POINT('Ctrl Pts',(4.55882751035107,3.18422781735199,0.497987521690504));
#63453=CARTESIAN_POINT('Ctrl Pts',(4.56101615934486,3.17873677105047,0.531912713801335));
#63454=CARTESIAN_POINT('Ctrl Pts',(4.56368135787895,3.1712918014787,0.573664167029947));
#63455=CARTESIAN_POINT('Ctrl Pts',(4.56418526891043,3.16985005671571,0.581577929329981));
#63456=CARTESIAN_POINT('Ctrl Pts',(4.56497563082301,3.16753462372559,0.594022948643385));
#63457=CARTESIAN_POINT('Ctrl Pts',(4.56526319678306,3.16668081961353,0.598557802843704));
#63458=CARTESIAN_POINT('Ctrl Pts',(4.56580054184501,3.16506404260327,0.607044783962373));
#63459=CARTESIAN_POINT('Ctrl Pts',(4.56605044804377,3.16430341426244,0.61099727187183));
#63460=CARTESIAN_POINT('Ctrl Pts',(4.56661729652616,3.16255834201078,0.619974606973294));
#63461=CARTESIAN_POINT('Ctrl Pts',(4.56693397380988,3.1615693289951,0.624998526984795));
#63462=CARTESIAN_POINT('Ctrl Pts',(4.56789410013189,3.15852799447007,0.640255731409609));
#63463=CARTESIAN_POINT('Ctrl Pts',(4.56853542235707,3.15643790680179,0.650481545441991));
#63464=CARTESIAN_POINT('Ctrl Pts',(4.57327594307221,3.14055540117806,0.726307746699716));
#63465=CARTESIAN_POINT('Ctrl Pts',(4.57726698820174,3.12476776345976,0.791479041925194));
#63466=CARTESIAN_POINT('Ctrl Pts',(4.59921349909911,3.02498801926229,1.15359302946905));
#63467=CARTESIAN_POINT('Ctrl Pts',(4.61571281244848,2.90071888045702,1.4377754474775));
#63468=CARTESIAN_POINT('Ctrl Pts',(4.63782943042713,2.69819458869133,1.76395446119005));
#63469=CARTESIAN_POINT('Ctrl Pts',(4.64222709895316,2.65624028263549,1.82652011784748));
#63470=CARTESIAN_POINT('Ctrl Pts',(4.64940142303995,2.5855543073107,1.92434044217195));
#63471=CARTESIAN_POINT('Ctrl Pts',(4.65212687825173,2.55820042827832,1.96055794824799));
#63472=CARTESIAN_POINT('Ctrl Pts',(4.65567055075485,2.52205243337528,2.00637422989547));
#63473=CARTESIAN_POINT('Ctrl Pts',(4.65646110003356,2.5139515553092,2.01651521118285));
#63474=CARTESIAN_POINT('Ctrl Pts',(4.65774069804726,2.50078160397146,2.03279914339153));
#63475=CARTESIAN_POINT('Ctrl Pts',(4.6582282101251,2.49575057705763,2.03897279124818));
#63476=CARTESIAN_POINT('Ctrl Pts',(4.65916020544569,2.4861073345068,2.05071699338566));
#63477=CARTESIAN_POINT('Ctrl Pts',(4.65960452335164,2.48149914416054,2.05629080186186));
#63478=CARTESIAN_POINT('Ctrl Pts',(4.6606222765999,2.47091906603581,2.06900051136248));
#63479=CARTESIAN_POINT('Ctrl Pts',(4.66119620937051,2.46493497673199,2.07612612923487));
#63480=CARTESIAN_POINT('Ctrl Pts',(4.66296453911603,2.44644381899632,2.0979520318141));
#63481=CARTESIAN_POINT('Ctrl Pts',(4.66416309851909,2.4338356597759,2.11256574865444));
#63482=CARTESIAN_POINT('Ctrl Pts',(4.68114258440495,2.25419393527325,2.31704001804854));
#63483=CARTESIAN_POINT('Ctrl Pts',(4.69790376698204,2.06554702547489,2.4866702066965));
#63484=CARTESIAN_POINT('Ctrl Pts',(4.71689863682896,1.83606345053158,2.64873209885375));
#63485=CARTESIAN_POINT('Ctrl Pts',(4.71880447807139,1.81285064742445,2.66467309289869));
#63486=CARTESIAN_POINT('Ctrl Pts',(4.7207101123806,1.78943616882057,2.68030516177109));
#63487=CARTESIAN_POINT('Origin',(-1.72497344927317,0.,0.));
#63488=CARTESIAN_POINT('',(6.21703160867442,1.78943621037803,2.68030513402633));
#63489=CARTESIAN_POINT('',(5.97308385260372,1.78943621012791,2.68030513419332));
#63490=CARTESIAN_POINT('',(-1.72497344927317,1.78943621037804,2.68030513402633));
#63491=CARTESIAN_POINT('',(5.3965734492289,-3.22274863470805,0.00296647727227422));
#63492=CARTESIAN_POINT('Ctrl Pts',(5.3965734492731,-3.22274863470871,0.00296647655588668));
#63493=CARTESIAN_POINT('Ctrl Pts',(5.40274171710666,-3.22284065656237,-0.0970050882467916));
#63494=CARTESIAN_POINT('Ctrl Pts',(5.40890998494021,-3.21827644653641,-0.197093019516699));
#63495=CARTESIAN_POINT('Ctrl Pts',(5.41507825277377,-3.20905173235025,-0.29682409201389));
#63496=CARTESIAN_POINT('Ctrl Pts',(5.42116256464214,-3.1999525752579,-0.395197730191385));
#63497=CARTESIAN_POINT('Ctrl Pts',(5.42724687651051,-3.18631903927338,-0.493223706962624));
#63498=CARTESIAN_POINT('Ctrl Pts',(5.43333118837888,-3.16819941223115,-0.590449021371175));
#63499=CARTESIAN_POINT('Ctrl Pts',(5.43941381045283,-3.15008481754844,-0.687647333417328));
#63500=CARTESIAN_POINT('Ctrl Pts',(5.44549643252677,-3.12748668799687,-0.784044987656764));
#63501=CARTESIAN_POINT('Ctrl Pts',(5.45157905460072,-3.10050477759769,-0.879197182999313));
#63502=CARTESIAN_POINT('Ctrl Pts',(5.45766170092831,-3.07352275961178,-0.974349757748389));
#63503=CARTESIAN_POINT('Ctrl Pts',(5.46374434725589,-3.04215704853434,-1.06825643594335));
#63504=CARTESIAN_POINT('Ctrl Pts',(5.46982699358348,-3.00655750993043,-1.16048675217812));
#63505=CARTESIAN_POINT('Ctrl Pts',(5.47605906722472,-2.97008342706819,-1.25498281388799));
#63506=CARTESIAN_POINT('Ctrl Pts',(5.48229114086597,-2.92916493292472,-1.34771860642642));
#63507=CARTESIAN_POINT('Ctrl Pts',(5.48852321450722,-2.88401526439077,-1.43825363453774));
#63508=CARTESIAN_POINT('Ctrl Pts',(5.49461453428551,-2.83988531908591,-1.52674389301489));
#63509=CARTESIAN_POINT('Ctrl Pts',(5.50070585406379,-2.79171358696322,-1.61313138708066));
#63510=CARTESIAN_POINT('Ctrl Pts',(5.50679717384208,-2.73974460436993,-1.6970318398091));
#63511=CARTESIAN_POINT('Ctrl Pts',(5.51309962441481,-2.6859743286283,-1.78384036006361));
#63512=CARTESIAN_POINT('Ctrl Pts',(5.51940207498753,-2.62813907424609,-1.86798585899725));
#63513=CARTESIAN_POINT('Ctrl Pts',(5.52570452556026,-2.56655578273067,-1.94907900728312));
#63514=CARTESIAN_POINT('Ctrl Pts',(5.53200697613298,-2.50497249121526,-2.03017215556899));
#63515=CARTESIAN_POINT('Ctrl Pts',(5.53830942670571,-2.43964155430169,-2.10821260448766));
#63516=CARTESIAN_POINT('Ctrl Pts',(5.54461187727843,-2.3709213396552,-2.18285353692538));
#63517=CARTESIAN_POINT('Ctrl Pts',(5.55078412537011,-2.30362081760956,-2.25595246050808));
#63518=CARTESIAN_POINT('Ctrl Pts',(5.55695637346178,-2.23281805406449,-2.32606467171766));
#63519=CARTESIAN_POINT('Ctrl Pts',(5.56312862155345,-2.15880867791026,-2.39283569320573));
#63520=CARTESIAN_POINT('Ctrl Pts',(5.56929251020499,-2.08489953702532,-2.45951628275576));
#63521=CARTESIAN_POINT('Ctrl Pts',(5.57545639885653,-2.00779273520899,-2.5228643884479));
#63522=CARTESIAN_POINT('Ctrl Pts',(5.58162028750807,-1.92782257632733,-2.58256029488232));
#63523=CARTESIAN_POINT('Ctrl Pts',(5.58777764916552,-1.84793709852667,-2.64219298881399));
#63524=CARTESIAN_POINT('Ctrl Pts',(5.59393501082297,-1.7651946377974,-2.69818091372776));
#63525=CARTESIAN_POINT('Ctrl Pts',(5.60009237248042,-1.67996387002175,-2.75024343612007));
#63526=CARTESIAN_POINT('Ctrl Pts',(5.60624523662563,-1.59479535722517,-2.80226793056395));
#63527=CARTESIAN_POINT('Ctrl Pts',(5.61239810077084,-1.50714252051476,-2.85037249727189));
#63528=CARTESIAN_POINT('Ctrl Pts',(5.61855096491605,-1.41740366000132,-2.89431933744618));
#63529=CARTESIAN_POINT('Ctrl Pts',(5.62470149805149,-1.3276987970142,-2.93824952838014));
#63530=CARTESIAN_POINT('Ctrl Pts',(5.63085203118693,-1.23590987019932,-2.97802493176923));
#63531=CARTESIAN_POINT('Ctrl Pts',(5.63700256432237,-1.14245967763006,-3.01345374072499));
#63532=CARTESIAN_POINT('Ctrl Pts',(5.64315241253649,-1.04901989164323,-3.04887860434033));
#63533=CARTESIAN_POINT('Ctrl Pts',(5.6493022607506,-0.953919613870974,-3.07995768186979));
#63534=CARTESIAN_POINT('Ctrl Pts',(5.65545210896471,-0.85760056883472,-3.10654773451727));
#63535=CARTESIAN_POINT('Ctrl Pts',(5.66160291734275,-0.761266485691932,
-3.13314193861832));
#63536=CARTESIAN_POINT('Ctrl Pts',(5.66775372572079,-0.663713676084884,
-3.15524561014111));
#63537=CARTESIAN_POINT('Ctrl Pts',(5.67390453409883,-0.565396948671176,
-3.17276596252124));
#63538=CARTESIAN_POINT('Ctrl Pts',(5.68006192046393,-0.46697507635262,-3.1903050520566));
#63539=CARTESIAN_POINT('Ctrl Pts',(5.68621930682905,-0.367788083289609,
-3.20325095803661));
#63540=CARTESIAN_POINT('Ctrl Pts',(5.69237669319415,-0.268298732007348,
-3.21156244729933));
#63541=CARTESIAN_POINT('Ctrl Pts',(5.69853751593004,-0.168753856793466,
-3.21987857511437));
#63542=CARTESIAN_POINT('Ctrl Pts',(5.70469833866593,-0.0689067214065487,
-3.22355511941268));
#63543=CARTESIAN_POINT('Ctrl Pts',(5.71085916140181,0.0307791609832923,
-3.2226030170887));
#63544=CARTESIAN_POINT('Ctrl Pts',(5.71703028431745,0.130631706585357,-3.22164932296026));
#63545=CARTESIAN_POINT('Ctrl Pts',(5.72320140723309,0.230322026786169,-3.21605154903976));
#63546=CARTESIAN_POINT('Ctrl Pts',(5.72937253014873,0.329390835988332,-3.20587261750477));
#63547=CARTESIAN_POINT('Ctrl Pts',(5.73406805210517,0.404770920807088,-3.19812760947802));
#63548=CARTESIAN_POINT('Ctrl Pts',(5.73876357406162,0.47979127179733,-3.18773142797412));
#63549=CARTESIAN_POINT('Ctrl Pts',(5.74345909601806,0.554254408827507,-3.17473142372631));
#63550=CARTESIAN_POINT('Ctrl Pts',(5.74963134411001,0.65213595633563,-3.15764296111061));
#63551=CARTESIAN_POINT('Ctrl Pts',(5.75580359220197,0.749398752610503,-3.13599343576414));
#63552=CARTESIAN_POINT('Ctrl Pts',(5.76197584029392,0.845584758578796,-3.1098398638128));
#63553=CARTESIAN_POINT('Ctrl Pts',(5.76813972894573,0.941640494158123,-3.08372171318868));
#63554=CARTESIAN_POINT('Ctrl Pts',(5.77430361759753,1.03662192261712,-3.05311175354045));
#63555=CARTESIAN_POINT('Ctrl Pts',(5.78046750624934,1.13007933498806,-3.01811833086991));
#63556=CARTESIAN_POINT('Ctrl Pts',(5.78662486790704,1.22343778451035,-2.98316196303218));
#63557=CARTESIAN_POINT('Ctrl Pts',(5.79278222956474,1.31527502176757,-2.94383151175955));
#63558=CARTESIAN_POINT('Ctrl Pts',(5.79893959122244,1.40515562853039,-2.9002853690817));
#63559=CARTESIAN_POINT('Ctrl Pts',(5.80509245536788,1.49497058393905,-2.85677103374626));
#63560=CARTESIAN_POINT('Ctrl Pts',(5.81124531951332,1.58283136057116,-2.80904731792483));
#63561=CARTESIAN_POINT('Ctrl Pts',(5.81739818365876,1.6683225550101,-2.7573206949763));
#63562=CARTESIAN_POINT('Ctrl Pts',(5.82354871679442,1.75378136114909,-2.70561366863523));
#63563=CARTESIAN_POINT('Ctrl Pts',(5.82969924993009,1.83687199761976,-2.64990697305706));
#63564=CARTESIAN_POINT('Ctrl Pts',(5.83584978306576,1.91720450351031,-2.5904525578014));
#63565=CARTESIAN_POINT('Ctrl Pts',(5.84199963128007,1.99752806359925,-2.53100476336998));
#63566=CARTESIAN_POINT('Ctrl Pts',(5.84814947949438,2.07509375460424,-2.46781033741245));
#63567=CARTESIAN_POINT('Ctrl Pts',(5.85429932770869,2.14954223780144,-2.40116341185009));
#63568=CARTESIAN_POINT('Ctrl Pts',(5.86045013608695,2.2240023444969,-2.33450608083164));
#63569=CARTESIAN_POINT('Ctrl Pts',(5.86660094446522,2.29534395303616,-2.26439546930261));
#63570=CARTESIAN_POINT('Ctrl Pts',(5.87275175284348,2.36324309083601,-2.19116399571457));
#63571=CARTESIAN_POINT('Ctrl Pts',(5.87890913920876,2.43121484342397,-2.11785420466759));
#63572=CARTESIAN_POINT('Ctrl Pts',(5.88506652557405,2.49573647768147,-2.04141720585072));
#63573=CARTESIAN_POINT('Ctrl Pts',(5.89122391193933,2.55652308746937,-1.9622199840324));
#63574=CARTESIAN_POINT('Ctrl Pts',(5.89738473467538,2.61734362160708,-1.88297856310071));
#63575=CARTESIAN_POINT('Ctrl Pts',(5.90354555741143,2.67442473190287,-1.80097420790359));
#63576=CARTESIAN_POINT('Ctrl Pts',(5.90970638014748,2.72752499225266,-1.71660274354235));
#63577=CARTESIAN_POINT('Ctrl Pts',(5.91587750306326,2.7807140300675,-1.63209021989668));
#63578=CARTESIAN_POINT('Ctrl Pts',(5.92204862597904,2.82990870962749,-1.54520306020906));
#63579=CARTESIAN_POINT('Ctrl Pts',(5.92821974889481,2.87491362120401,-1.45636164228383));
#63580=CARTESIAN_POINT('Ctrl Pts',(5.93291527084911,2.90915723508805,-1.38876343787074));
#63581=CARTESIAN_POINT('Ctrl Pts',(5.93761079280341,2.94097614644785,-1.3200343281168));
#63582=CARTESIAN_POINT('Ctrl Pts',(5.94230631475771,2.97030340761317,-1.25036603809507));
#63583=CARTESIAN_POINT('Ctrl Pts',(5.94847856285123,3.00885399550898,-1.15878730106632));
#63584=CARTESIAN_POINT('Ctrl Pts',(5.95465081094475,3.04323321164755,-1.06526284977028));
#63585=CARTESIAN_POINT('Ctrl Pts',(5.96082305903828,3.07324135208549,-0.970208819961856));
#63586=CARTESIAN_POINT('Ctrl Pts',(5.96698694769168,3.1032088507266,-0.875283527439711));
#63587=CARTESIAN_POINT('Ctrl Pts',(5.97315083634509,3.12881691071329,-0.778833184511968));
#63588=CARTESIAN_POINT('Ctrl Pts',(5.9793147249985,3.14991351142471,-0.681294674163874));
#63589=CARTESIAN_POINT('Ctrl Pts',(5.98547208665783,3.17098777276636,-0.58385944817328));
#63590=CARTESIAN_POINT('Ctrl Pts',(5.99162944831715,3.18755998108103,-0.485338767800381));
#63591=CARTESIAN_POINT('Ctrl Pts',(5.99778680997648,3.19952794206126,-0.386184554933584));
#63592=CARTESIAN_POINT('Ctrl Pts',(6.00393967412358,3.21148716130211,-0.287102767126425));
#63593=CARTESIAN_POINT('Ctrl Pts',(6.01009253827068,3.21884876767893,-0.187388796797091));
#63594=CARTESIAN_POINT('Ctrl Pts',(6.01624540241778,3.22156183554115,-0.08750372726211));
#63595=CARTESIAN_POINT('Ctrl Pts',(6.02239593555511,3.22427387555884,0.0123435008600179));
#63596=CARTESIAN_POINT('Ctrl Pts',(6.02854646869244,3.22234086457052,0.112361265656007));
#63597=CARTESIAN_POINT('Ctrl Pts',(6.03469700182977,3.21576388893388,0.212085296823836));
#63598=CARTESIAN_POINT('Ctrl Pts',(6.04084685004577,3.20918764570707,0.311798222756611));
#63599=CARTESIAN_POINT('Ctrl Pts',(6.04699669826177,3.1979684945882,0.411217046659547));
#63600=CARTESIAN_POINT('Ctrl Pts',(6.05314654647777,3.18215956384424,0.509880449453238));
#63601=CARTESIAN_POINT('Ctrl Pts',(6.05929735485773,3.16634816488239,0.608559256373909));
#63602=CARTESIAN_POINT('Ctrl Pts',(6.06544816323768,3.14594563168597,0.706481978976487));
#63603=CARTESIAN_POINT('Ctrl Pts',(6.07159897161763,3.12105642232688,0.803196346575431));
#63604=CARTESIAN_POINT('Ctrl Pts',(6.07775635798462,3.09614059518254,0.900014145433683));
#63605=CARTESIAN_POINT('Ctrl Pts',(6.08391374435162,3.06672861867615,0.995620587257379));
#63606=CARTESIAN_POINT('Ctrl Pts',(6.09007113071861,3.03297515199977,1.08957757404048));
#63607=CARTESIAN_POINT('Ctrl Pts',(6.09623195345638,2.9992028478785,1.18358699720231));
#63608=CARTESIAN_POINT('Ctrl Pts',(6.10239277619414,2.96108439406214,1.27594473054054));
#63609=CARTESIAN_POINT('Ctrl Pts',(6.10855359893191,2.91882222058803,1.36623365757895));
#63610=CARTESIAN_POINT('Ctrl Pts',(6.1147247218494,2.87648938967076,1.45667353721176));
#63611=CARTESIAN_POINT('Ctrl Pts',(6.1208958447669,2.82999920333809,1.54503731709485));
#63612=CARTESIAN_POINT('Ctrl Pts',(6.1270669676844,2.7795996271054,1.63093331423929));
#63613=CARTESIAN_POINT('Ctrl Pts',(6.13176248962205,2.74125128774916,1.69629038852556));
#63614=CARTESIAN_POINT('Ctrl Pts',(6.1364580115597,2.70064055927373,1.7602192735415));
#63615=CARTESIAN_POINT('Ctrl Pts',(6.14115353349736,2.65789252322745,1.82255998460178));
#63616=CARTESIAN_POINT('Ctrl Pts',(6.14747670642878,2.60032635103439,1.90651041693621));
#63617=CARTESIAN_POINT('Ctrl Pts',(6.1537998793602,2.53867505022404,1.98788218939877));
#63618=CARTESIAN_POINT('Ctrl Pts',(6.16012305229163,2.47319949154006,2.06625309135788));
#63619=CARTESIAN_POINT('Ctrl Pts',(6.16628612829986,2.4093817137839,2.14263971415732));
#63620=CARTESIAN_POINT('Ctrl Pts',(6.1724492043081,2.34193129278647,2.21617522801198));
#63621=CARTESIAN_POINT('Ctrl Pts',(6.17861228031634,2.2711344639199,2.28649640482885));
#63622=CARTESIAN_POINT('Ctrl Pts',(6.18501550170935,2.19757902365759,2.35955765917228));
#63623=CARTESIAN_POINT('Ctrl Pts',(6.19141872310237,2.12041131911197,2.42914856902415));
#63624=CARTESIAN_POINT('Ctrl Pts',(6.19782194449538,2.03999865167889,2.49489940952503));
#63625=CARTESIAN_POINT('Ctrl Pts',(6.20422516588839,1.9595859842458,2.5606502500259));
#63626=CARTESIAN_POINT('Ctrl Pts',(6.21062838728141,1.87592872881404,2.62256064723214));
#63627=CARTESIAN_POINT('Ctrl Pts',(6.21703160867442,1.78943621037803,2.68030513402633));
#63628=CARTESIAN_POINT('Ctrl Pts',(4.96704894786217,1.78943621037804,2.68030513402633));
#63629=CARTESIAN_POINT('Ctrl Pts',(4.97321265127211,1.7066444304683,2.73557891872023));
#63630=CARTESIAN_POINT('Ctrl Pts',(4.97937635468204,1.62117190020534,2.78709141305354));
#63631=CARTESIAN_POINT('Ctrl Pts',(4.98554005809198,1.53339585901294,2.83457487148637));
#63632=CARTESIAN_POINT('Ctrl Pts',(4.99169728016169,1.44571211726273,2.88200839947501));
#63633=CARTESIAN_POINT('Ctrl Pts',(4.9978545022314,1.3557300601906,2.92542110895884));
#63634=CARTESIAN_POINT('Ctrl Pts',(5.00401172430111,1.26385524948627,2.96458892105567));
#63635=CARTESIAN_POINT('Ctrl Pts',(5.0101645101877,1.17204663315991,3.00372851335058));
#63636=CARTESIAN_POINT('Ctrl Pts',(5.01631729607428,1.07834837282433,3.03862911890848));
#63637=CARTESIAN_POINT('Ctrl Pts',(5.02247008196086,0.983189112428774,3.06911334618022));
#63638=CARTESIAN_POINT('Ctrl Pts',(5.02862057796086,0.888065267521128,3.09958622811596));
#63639=CARTESIAN_POINT('Ctrl Pts',(5.03477107396086,0.791481916196883,3.12564586532792));
#63640=CARTESIAN_POINT('Ctrl Pts',(5.04092156996085,0.693885249456781,3.14716393330349));
#63641=CARTESIAN_POINT('Ctrl Pts',(5.04707142212159,0.596298799220411,3.16867974874905));
#63642=CARTESIAN_POINT('Ctrl Pts',(5.05322127428233,0.497699668663595,3.18565484666855));
#63643=CARTESIAN_POINT('Ctrl Pts',(5.05937112644307,0.398545708663082,3.19801170739043));
#63644=CARTESIAN_POINT('Ctrl Pts',(5.06552197984165,0.299375605722082,3.21037057989345));
#63645=CARTESIAN_POINT('Ctrl Pts',(5.07167283324024,0.199650924991649,3.2181096680155));
#63646=CARTESIAN_POINT('Ctrl Pts',(5.07782368663882,0.0998351228974701,
3.22120327063289));
#63647=CARTESIAN_POINT('Ctrl Pts',(5.08398114074791,-8.77952618458383E-5,
3.22430019311079));
#63648=CARTESIAN_POINT('Ctrl Pts',(5.090138594857,-0.100101595050854,3.22274166192651));
#63649=CARTESIAN_POINT('Ctrl Pts',(5.09629604896609,-0.199742454542215,
3.21655413670491));
#63650=CARTESIAN_POINT('Ctrl Pts',(5.10245697636141,-0.299439519279874,
3.21036312123462));
#63651=CARTESIAN_POINT('Ctrl Pts',(5.10861790375672,-0.398762792994233,
3.19953795893322));
#63652=CARTESIAN_POINT('Ctrl Pts',(5.11477883115204,-0.497255301095885,
3.18415683156971));
#63653=CARTESIAN_POINT('Ctrl Pts',(5.12095001215027,-0.595911729822317,
3.16875010546721));
#63654=CARTESIAN_POINT('Ctrl Pts',(5.12712119314849,-0.69373420557751,3.14877235621637));
#63655=CARTESIAN_POINT('Ctrl Pts',(5.13329237414672,-0.790277517156108,
3.1243525742748));
#63656=CARTESIAN_POINT('Ctrl Pts',(5.13783406269752,-0.861328690825979,
3.10638080451323));
#63657=CARTESIAN_POINT('Ctrl Pts',(5.14237575124833,-0.931687305210557,
3.0860041857128));
#63658=CARTESIAN_POINT('Ctrl Pts',(5.14691743979913,-1.00118270264739,3.06329083803998));
#63659=CARTESIAN_POINT('Ctrl Pts',(5.15308968788507,-1.09562837610406,3.03242293172482));
#63660=CARTESIAN_POINT('Ctrl Pts',(5.15926193597101,-1.18881139356646,2.99712875767385));
#63661=CARTESIAN_POINT('Ctrl Pts',(5.16543418405695,-1.28028652250361,2.95753004765727));
#63662=CARTESIAN_POINT('Ctrl Pts',(5.17159807270263,-1.37163776126896,2.9179849685133));
#63663=CARTESIAN_POINT('Ctrl Pts',(5.17776196134831,-1.46128531392066,2.87414711198939));
#63664=CARTESIAN_POINT('Ctrl Pts',(5.18392584999398,-1.54879951053223,2.82618782791858));
#63665=CARTESIAN_POINT('Ctrl Pts',(5.19008321164546,-1.63622103761536,2.77827932834229));
#63666=CARTESIAN_POINT('Ctrl Pts',(5.19624057329693,-1.72151332099658,2.72625828529251));
#63667=CARTESIAN_POINT('Ctrl Pts',(5.20239793494841,-1.80426797008067,2.67034354618296));
#63668=CARTESIAN_POINT('Ctrl Pts',(5.20855079908749,-1.88696217281123,2.61446964879198));
#63669=CARTESIAN_POINT('Ctrl Pts',(5.21470366322658,-1.96712206760512,2.55470795228538));
#63670=CARTESIAN_POINT('Ctrl Pts',(5.22085652736567,-2.04436592872084,2.49132204100261));
#63671=CARTESIAN_POINT('Ctrl Pts',(5.2270070604949,-2.12158052603394,2.42796014344428));
#63672=CARTESIAN_POINT('Ctrl Pts',(5.23315759362414,-2.19588094935975,2.36097703455927));
#63673=CARTESIAN_POINT('Ctrl Pts',(5.23930812675337,-2.26691713867827,2.29067768332141));
#63674=CARTESIAN_POINT('Ctrl Pts',(5.24545797496119,-2.3379454174294,2.22038616059688));
#63675=CARTESIAN_POINT('Ctrl Pts',(5.25160782316901,-2.40570987612532,2.14677943527788));
#63676=CARTESIAN_POINT('Ctrl Pts',(5.25775767137683,-2.46989677767706,2.07019986236123));
#63677=CARTESIAN_POINT('Ctrl Pts',(5.26390847974851,-2.534093700605,1.9936083332247));
#63678=CARTESIAN_POINT('Ctrl Pts',(5.27005928812018,-2.59471167789402,1.91404336751283));
#63679=CARTESIAN_POINT('Ctrl Pts',(5.27621009649185,-2.65147743549569,1.831880173908));
#63680=CARTESIAN_POINT('Ctrl Pts',(5.28236748285051,-2.70830390128277,1.74962911080928));
#63681=CARTESIAN_POINT('Ctrl Pts',(5.28852486920918,-2.7612696732588,1.66477462916039));
#63682=CARTESIAN_POINT('Ctrl Pts',(5.29468225556784,-2.81014507257187,1.57772058159867));
#63683=CARTESIAN_POINT('Ctrl Pts',(5.30084307829723,-2.8590477487166,1.49061795011468));
#63684=CARTESIAN_POINT('Ctrl Pts',(5.30700390102661,-2.90385531124304,1.40131369632026));
#63685=CARTESIAN_POINT('Ctrl Pts',(5.313164723756,-2.94438522871155,1.3102340201068));
#63686=CARTESIAN_POINT('Ctrl Pts',(5.31933584666511,-2.98498290749258,1.21900206925798));
#63687=CARTESIAN_POINT('Ctrl Pts',(5.32550696957422,-3.02128849784746,1.12598917173341));
#63688=CARTESIAN_POINT('Ctrl Pts',(5.33167809248334,-3.05316851493949,1.0316392692614));
#63689=CARTESIAN_POINT('Ctrl Pts',(5.33637361450182,-3.07742557875266,0.959849734192361));
#63690=CARTESIAN_POINT('Ctrl Pts',(5.34106913652031,-3.09912148371401,0.887286509939943));
#63691=CARTESIAN_POINT('Ctrl Pts',(5.34576465853879,-3.11821729824784,0.814148907392219));
#63692=CARTESIAN_POINT('Ctrl Pts',(5.35378219689036,-3.15082313520839,0.689267471194136));
#63693=CARTESIAN_POINT('Ctrl Pts',(5.36179973524192,-3.17594116881185,0.562355834688537));
#63694=CARTESIAN_POINT('Ctrl Pts',(5.36981727359349,-3.19336690303654,0.434195100261212));
#63695=CARTESIAN_POINT('Ctrl Pts',(5.37766287724397,-3.21041894545287,0.308782750262963));
#63696=CARTESIAN_POINT('Ctrl Pts',(5.38550848089445,-3.22010509332094,0.182174046725123));
#63697=CARTESIAN_POINT('Ctrl Pts',(5.39335408454493,-3.22227854034219,0.0551232342140707));
#63698=CARTESIAN_POINT('Ctrl Pts',(5.39442720610625,-3.22257582439639,0.0377452257951675));
#63699=CARTESIAN_POINT('Ctrl Pts',(5.39550032766758,-3.22273262524449,0.0203589843103794));
#63700=CARTESIAN_POINT('Ctrl Pts',(5.3965734492289,-3.22274863470805,0.00296647727227207));
#63701=CARTESIAN_POINT('Ctrl Pts',(4.7207101123806,1.78943616882057,2.68030516177109));
#63702=CARTESIAN_POINT('Ctrl Pts',(4.72889755303781,1.68883730094667,2.74746738467149));
#63703=CARTESIAN_POINT('Ctrl Pts',(4.73708536016951,1.58451588245051,2.80892691062836));
#63704=CARTESIAN_POINT('Ctrl Pts',(4.74884783452162,1.42647606285484,2.89041694398679));
#63705=CARTESIAN_POINT('Ctrl Pts',(4.75256209441039,1.37530740771152,2.91511138750835));
#63706=CARTESIAN_POINT('Ctrl Pts',(4.75820039870415,1.29526386001628,2.951163970324));
#63707=CARTESIAN_POINT('Ctrl Pts',(4.76017023922003,1.26683476155088,2.96347888543182));
#63708=CARTESIAN_POINT('Ctrl Pts',(4.76260486192707,1.23105341746289,2.97836960271926));
#63709=CARTESIAN_POINT('Ctrl Pts',(4.76309176059549,1.22386468696764,2.98133078305861));
#63710=CARTESIAN_POINT('Ctrl Pts',(4.76386143184421,1.21244756476756,2.98598546723698));
#63711=CARTESIAN_POINT('Ctrl Pts',(4.76414522539568,1.2082262345078,2.98769604791423));
#63712=CARTESIAN_POINT('Ctrl Pts',(4.7646793889452,1.20025852239082,2.99090510085465));
#63713=CARTESIAN_POINT('Ctrl Pts',(4.76492986938302,1.19651299707394,2.9924054690019));
#63714=CARTESIAN_POINT('Ctrl Pts',(4.76550313818908,1.18791953235429,2.99582909188413));
#63715=CARTESIAN_POINT('Ctrl Pts',(4.7658256379411,1.183069744287,2.99774761182303));
#63716=CARTESIAN_POINT('Ctrl Pts',(4.76682112480404,1.16805262906288,3.00364608959917));
#63717=CARTESIAN_POINT('Ctrl Pts',(4.76749174880313,1.15786958805199,3.00758620838922));
#63718=CARTESIAN_POINT('Ctrl Pts',(4.77304955350832,1.07294473958257,3.03995088744119));
#63719=CARTESIAN_POINT('Ctrl Pts',(4.77778229359266,0.99718178801852,3.06563903517259));
#63720=CARTESIAN_POINT('Ctrl Pts',(4.78422070594391,0.890788434429024,3.09734999329969));
#63721=CARTESIAN_POINT('Ctrl Pts',(4.78600620843527,0.860914799047926,3.10578602234764));
#63722=CARTESIAN_POINT('Ctrl Pts',(4.79521992937685,0.70518558911452,3.14734279102525));
#63723=CARTESIAN_POINT('Ctrl Pts',(4.80246024979137,0.577525821225902,3.17325071235259));
#63724=CARTESIAN_POINT('Ctrl Pts',(4.81791077308689,0.303824174325026,3.21172787220646));
#63725=CARTESIAN_POINT('Ctrl Pts',(4.82611557127025,0.157792829201598,3.22220458553662));
#63726=CARTESIAN_POINT('Ctrl Pts',(4.84044737504432,-0.0897860164447993,
3.22309289531064));
#63727=CARTESIAN_POINT('Ctrl Pts',(4.84642857739393,-0.191086800961918,
3.21867550892016));
#63728=CARTESIAN_POINT('Ctrl Pts',(4.85356406895485,-0.308472370281793,
3.20799560519337));
#63729=CARTESIAN_POINT('Ctrl Pts',(4.85456901366792,-0.324928464367025,
3.20637060917226));
#63730=CARTESIAN_POINT('Ctrl Pts',(4.85611132938527,-0.350063723618893,
3.20369308318399));
#63731=CARTESIAN_POINT('Ctrl Pts',(4.85664582190098,-0.358752486085077,
3.20273174543012));
#63732=CARTESIAN_POINT('Ctrl Pts',(4.85757885129767,-0.373881165912992,
3.20099554956769));
#63733=CARTESIAN_POINT('Ctrl Pts',(4.85797688410912,-0.380322884056235,
3.20023657523345));
#63734=CARTESIAN_POINT('Ctrl Pts',(4.85887257845724,-0.394790977802582,
3.19848761903127));
#63735=CARTESIAN_POINT('Ctrl Pts',(4.85937057827695,-0.402815984910783,
3.19748686403015));
#63736=CARTESIAN_POINT('Ctrl Pts',(4.86070444850037,-0.424258832628833,
3.1947308376034));
#63737=CARTESIAN_POINT('Ctrl Pts',(4.86154203241878,-0.437669416811398,
3.19292125715712));
#63738=CARTESIAN_POINT('Ctrl Pts',(4.86413108754685,-0.478953414903274,
3.18708555267426));
#63739=CARTESIAN_POINT('Ctrl Pts',(4.86589141249331,-0.506785175817478,
3.18277856566573));
#63740=CARTESIAN_POINT('Ctrl Pts',(4.88588015665175,-0.820078004787635,
3.13008285547919));
#63741=CARTESIAN_POINT('Ctrl Pts',(4.90540610792843,-1.0977720546638,3.0438087459221));
#63742=CARTESIAN_POINT('Ctrl Pts',(4.93008522002194,-1.42863846504036,2.88977820878815));
#63743=CARTESIAN_POINT('Ctrl Pts',(4.93517866564755,-1.49599355223374,2.85549119888724));
#63744=CARTESIAN_POINT('Ctrl Pts',(4.94487292969805,-1.62329795077774,2.78494511671459));
#63745=CARTESIAN_POINT('Ctrl Pts',(4.94947982821201,-1.68339593601877,2.74903528895032));
#63746=CARTESIAN_POINT('Ctrl Pts',(4.95629943418041,-1.77241189675349,2.69183143069109));
#63747=CARTESIAN_POINT('Ctrl Pts',(4.95858225983423,-1.80221980310142,2.67196639642683));
#63748=CARTESIAN_POINT('Ctrl Pts',(4.96134598561325,-1.8383982849353,2.64697482946214));
#63749=CARTESIAN_POINT('Ctrl Pts',(4.96185666719518,-1.84508726255124,2.64231659701204));
#63750=CARTESIAN_POINT('Ctrl Pts',(4.96265525495301,-1.85555464825873,2.63496793574492));
#63751=CARTESIAN_POINT('Ctrl Pts',(4.96294431461668,-1.85934498715676,2.63229468229927));
#63752=CARTESIAN_POINT('Ctrl Pts',(4.9634829712892,-1.86641132885161,2.62728804862885));
#63753=CARTESIAN_POINT('Ctrl Pts',(4.96373270189526,-1.86968870011267,2.62495674323502));
#63754=CARTESIAN_POINT('Ctrl Pts',(4.96429724730185,-1.87710039171547,2.6196636322268));
#63755=CARTESIAN_POINT('Ctrl Pts',(4.9646118057091,-1.8812320594972,2.61669818010314));
#63756=CARTESIAN_POINT('Ctrl Pts',(4.96553886718725,-1.89341389838191,2.60791105445327));
#63757=CARTESIAN_POINT('Ctrl Pts',(4.96614949669855,-1.9014442792053,2.60206185892142));
#63758=CARTESIAN_POINT('Ctrl Pts',(4.97034096077725,-1.95659864984875,2.56149665843523));
#63759=CARTESIAN_POINT('Ctrl Pts',(4.97383957269568,-2.00279973559225,2.52553709947713));
#63760=CARTESIAN_POINT('Ctrl Pts',(4.97807834840705,-2.0585144629996,2.47968168293472));
#63761=CARTESIAN_POINT('Ctrl Pts',(4.97887508315419,-2.06897518071685,2.47096028997393));
#63762=CARTESIAN_POINT('Ctrl Pts',(4.99744292493297,-2.31237927941527,2.26539805839744));
#63763=CARTESIAN_POINT('Ctrl Pts',(5.01377036702038,-2.51628163786418,2.03653832142762));
#63764=CARTESIAN_POINT('Ctrl Pts',(5.03565214846368,-2.72629913496094,1.72017166620206));
#63765=CARTESIAN_POINT('Ctrl Pts',(5.04001533731903,-2.76543433339587,1.65652325924747));
#63766=CARTESIAN_POINT('Ctrl Pts',(5.0471381840054,-2.82459988479309,1.55234922817117));
#63767=CARTESIAN_POINT('Ctrl Pts',(5.04984758127164,-2.84605163645033,1.51266070543106));
#63768=CARTESIAN_POINT('Ctrl Pts',(5.05337318101048,-2.87258045047479,1.46101569725888));
#63769=CARTESIAN_POINT('Ctrl Pts',(5.05416206613419,-2.87842881188627,1.44945951282848));
#63770=CARTESIAN_POINT('Ctrl Pts',(5.05543962031527,-2.88775779067507,1.43074659975042));
#63771=CARTESIAN_POINT('Ctrl Pts',(5.05592676172055,-2.89128187600284,1.42361160503911));
#63772=CARTESIAN_POINT('Ctrl Pts',(5.05685848179972,-2.89795878723938,1.40996622475054));
#63773=CARTESIAN_POINT('Ctrl Pts',(5.05730289688509,-2.90111619504801,1.40345812511326));
#63774=CARTESIAN_POINT('Ctrl Pts',(5.05832148536821,-2.90829019451131,1.38854330607284));
#63775=CARTESIAN_POINT('Ctrl Pts',(5.05889615910528,-2.91229228069936,1.38012971752261));
#63776=CARTESIAN_POINT('Ctrl Pts',(5.0606690047254,-2.92449867193768,1.35417870018272));
#63777=CARTESIAN_POINT('Ctrl Pts',(5.06187136995943,-2.93258134722859,1.33658484568682));
#63778=CARTESIAN_POINT('Ctrl Pts',(5.07246486218908,-3.00207419271817,1.18165192915195));
#63779=CARTESIAN_POINT('Ctrl Pts',(5.08218257105554,-3.05394721594373,1.0402622234695));
#63780=CARTESIAN_POINT('Ctrl Pts',(5.10765835347028,-3.16079546099927,0.671004030380826));
#63781=CARTESIAN_POINT('Ctrl Pts',(5.12373565919984,-3.20115791289747,0.439829622649969));
#63782=CARTESIAN_POINT('Ctrl Pts',(5.14391216714926,-3.22056034376836,0.137403283518766));
#63783=CARTESIAN_POINT('Ctrl Pts',(5.14845698894086,-3.2227657577853,0.0683430641451825));
#63784=CARTESIAN_POINT('Ctrl Pts',(5.15327882890425,-3.22274859674846,-0.00648848231940785));
#63785=CARTESIAN_POINT('Ctrl Pts',(5.15364864015279,-3.22273189273413,-0.012237924310271));
#63786=CARTESIAN_POINT('Ctrl Pts',(5.15593699760881,-3.22253295606829,-0.0478804029247589));
#63787=CARTESIAN_POINT('Ctrl Pts',(5.15783771205345,-3.2219501873581,-0.0777710069350208));
#63788=CARTESIAN_POINT('Ctrl Pts',(5.16021625910801,-3.2206859222111,-0.115598417512247));
#63789=CARTESIAN_POINT('Ctrl Pts',(5.160714460794,-3.22039086388161,-0.123545500365449));
#63790=CARTESIAN_POINT('Ctrl Pts',(5.16150081984549,-3.21987703759093,-0.136128478418687));
#63791=CARTESIAN_POINT('Ctrl Pts',(5.16179004787196,-3.21967766956908,-0.140765068709603));
#63792=CARTESIAN_POINT('Ctrl Pts',(5.1623288540976,-3.21928683871364,-0.14941882904711));
#63793=CARTESIAN_POINT('Ctrl Pts',(5.16257856662343,-3.21909787388023,-0.153436029083458));
#63794=CARTESIAN_POINT('Ctrl Pts',(5.1631428602973,-3.2186531029101,-0.16252873917902));
#63795=CARTESIAN_POINT('Ctrl Pts',(5.16345718599811,-3.21839281182433,-0.167603990324072));
#63796=CARTESIAN_POINT('Ctrl Pts',(5.1644032282774,-3.21757153438086,-0.182909703286286));
#63797=CARTESIAN_POINT('Ctrl Pts',(5.16503290865684,-3.21697375851345,-0.193138246030363));
#63798=CARTESIAN_POINT('Ctrl Pts',(5.1710497340141,-3.21077041105784,-0.291248051758102));
#63799=CARTESIAN_POINT('Ctrl Pts',(5.17624751060617,-3.20161329406831,-0.378876658762356));
#63800=CARTESIAN_POINT('Ctrl Pts',(5.19051055988408,-3.16592145925169,-0.623103970351996));
#63801=CARTESIAN_POINT('Ctrl Pts',(5.19932033984886,-3.13139041662638,-0.778278640275637));
#63802=CARTESIAN_POINT('Ctrl Pts',(5.22151862429023,-3.01679153699887,-1.15837951672596));
#63803=CARTESIAN_POINT('Ctrl Pts',(5.23497187064074,-2.92295486118273,-1.37810986937873));
#63804=CARTESIAN_POINT('Ctrl Pts',(5.2505422799499,-2.79612047061904,-1.60256447391179));
#63805=CARTESIAN_POINT('Ctrl Pts',(5.25173279219761,-2.78631155790587,-1.61955872236515));
#63806=CARTESIAN_POINT('Ctrl Pts',(5.25349384726213,-2.77164251610682,-1.64444556176316));
#63807=CARTESIAN_POINT('Ctrl Pts',(5.25406002257949,-2.76690242461355,-1.65240866995258));
#63808=CARTESIAN_POINT('Ctrl Pts',(5.25507124026892,-2.75839407345961,-1.66656299846736));
#63809=CARTESIAN_POINT('Ctrl Pts',(5.25551579258902,-2.75463913523243,-1.67276218442448));
#63810=CARTESIAN_POINT('Ctrl Pts',(5.25644683101464,-2.74674503778029,-1.68569622132734));
#63811=CARTESIAN_POINT('Ctrl Pts',(5.25693345971092,-2.74260195079536,-1.69242860732217));
#63812=CARTESIAN_POINT('Ctrl Pts',(5.25820519658536,-2.73173049087484,-1.709949634755));
#63813=CARTESIAN_POINT('Ctrl Pts',(5.25899174813754,-2.72496301622357,-1.72071374171957));
#63814=CARTESIAN_POINT('Ctrl Pts',(5.26243886861109,-2.6951160670158,-1.76756957999835));
#63815=CARTESIAN_POINT('Ctrl Pts',(5.26512373764345,-2.67138281874331,-1.80323775056653));
#63816=CARTESIAN_POINT('Ctrl Pts',(5.27224390785945,-2.6072114551608,-1.89563126465691));
#63817=CARTESIAN_POINT('Ctrl Pts',(5.27672122105514,-2.56563463777498,-1.95153457568684));
#63818=CARTESIAN_POINT('Ctrl Pts',(5.2974457883047,-2.36767535309622,-2.20043695879772));
#63819=CARTESIAN_POINT('Ctrl Pts',(5.31443132934196,-2.19112515066032,-2.37628934424008));
#63820=CARTESIAN_POINT('Ctrl Pts',(5.33490508172688,-1.95200347036751,-2.56494945488731));
#63821=CARTESIAN_POINT('Ctrl Pts',(5.33866429867843,-1.90692482542808,-2.5986383834123));
#63822=CARTESIAN_POINT('Ctrl Pts',(5.34758456467734,-1.79666181233802,-2.67662685626281));
#63823=CARTESIAN_POINT('Ctrl Pts',(5.3527019746806,-1.7306849062489,-2.71975313086025));
#63824=CARTESIAN_POINT('Ctrl Pts',(5.35835849975618,-1.65386987484029,-2.76603512924918));
#63825=CARTESIAN_POINT('Ctrl Pts',(5.3590417944759,-1.64452365985475,-2.77160203480083));
#63826=CARTESIAN_POINT('Ctrl Pts',(5.36004772851081,-1.63066179579676,-2.77976380092835));
#63827=CARTESIAN_POINT('Ctrl Pts',(5.36037268704531,-1.62616787663143,-2.7823951407277));
#63828=CARTESIAN_POINT('Ctrl Pts',(5.36094810680071,-1.6181815122442,-2.78704546587128));
#63829=CARTESIAN_POINT('Ctrl Pts',(5.36119884950261,-1.61469164134779,-2.78906879431733));
#63830=CARTESIAN_POINT('Ctrl Pts',(5.36173207231841,-1.60724924467579,-2.79336503448279));
#63831=CARTESIAN_POINT('Ctrl Pts',(5.36201443259025,-1.60329570529989,-2.79563610514005));
#63832=CARTESIAN_POINT('Ctrl Pts',(5.36277810595028,-1.59256944029108,-2.80176746202727));
#63833=CARTESIAN_POINT('Ctrl Pts',(5.36325838249179,-1.58578745278571,-2.80561160729328));
#63834=CARTESIAN_POINT('Ctrl Pts',(5.36565503026636,-1.55176734975486,-2.82473200947441));
#63835=CARTESIAN_POINT('Ctrl Pts',(5.3675484636385,-1.52432103483468,-2.83963701674303));
#63836=CARTESIAN_POINT('Ctrl Pts',(5.37286635493834,-1.44577798590673,-2.88082360150712));
#63837=CARTESIAN_POINT('Ctrl Pts',(5.37624055838102,-1.39418716725492,-2.9061420397093));
#63838=CARTESIAN_POINT('Ctrl Pts',(5.38838782095632,-1.20341077218617,-2.99351583033522));
#63839=CARTESIAN_POINT('Ctrl Pts',(5.39686388171164,-1.06054321444173,-3.04706230016531));
#63840=CARTESIAN_POINT('Ctrl Pts',(5.4192689498355,-0.676129051834861,-3.16080983430566));
#63841=CARTESIAN_POINT('Ctrl Pts',(5.43325256142525,-0.430526723808855,
-3.20351254883275));
#63842=CARTESIAN_POINT('Ctrl Pts',(5.4494331686977,-0.16308008567044,-3.21867981603252));
#63843=CARTESIAN_POINT('Ctrl Pts',(5.45061182313246,-0.143677569434873,
-3.21960426185394));
#63844=CARTESIAN_POINT('Ctrl Pts',(5.45236472346193,-0.114945883282471,
-3.22071297098948));
#63845=CARTESIAN_POINT('Ctrl Pts',(5.45293473085194,-0.105622122146385,
-3.22103221995875));
#63846=CARTESIAN_POINT('Ctrl Pts',(5.4539490639417,-0.0890652365479059,
-3.22152716796304));
#63847=CARTESIAN_POINT('Ctrl Pts',(5.45439288001523,-0.0818326300813433,
-3.2217190022693));
#63848=CARTESIAN_POINT('Ctrl Pts',(5.45532607225916,-0.0666500331294796,
-3.2220705397702));
#63849=CARTESIAN_POINT('Ctrl Pts',(5.45581560443624,-0.0586999843869909,
-3.22222517838115));
#63850=CARTESIAN_POINT('Ctrl Pts',(5.45710321026734,-0.03782753653005,-3.22255390312858));
#63851=CARTESIAN_POINT('Ctrl Pts',(5.45790279455177,-0.0249046186859661,
-3.22267968207177));
#63852=CARTESIAN_POINT('Ctrl Pts',(5.46148736685304,0.0328534524901184,
-3.22289441478089));
#63853=CARTESIAN_POINT('Ctrl Pts',(5.46429911226672,0.0776850015226813,
-3.22212545869696));
#63854=CARTESIAN_POINT('Ctrl Pts',(5.47183364470494,0.196508924898696,-3.2176061592622));
#63855=CARTESIAN_POINT('Ctrl Pts',(5.47660473649848,0.270409438435103,-3.21223948265726));
#63856=CARTESIAN_POINT('Ctrl Pts',(5.50113489293887,0.643728589395928,-3.17215552209636));
#63857=CARTESIAN_POINT('Ctrl Pts',(5.52201745608186,0.937351417354883,-3.09811035649627));
#63858=CARTESIAN_POINT('Ctrl Pts',(5.54316047746374,1.23420901119516,-2.97711536924643));
#63859=CARTESIAN_POINT('Ctrl Pts',(5.54442429546548,1.25196243184823,-2.96969323383597));
#63860=CARTESIAN_POINT('Ctrl Pts',(5.5494447111496,1.32256125468897,-2.93943249825612));
#63861=CARTESIAN_POINT('Ctrl Pts',(5.55315196123961,1.37486073885267,-2.91533713726405));
#63862=CARTESIAN_POINT('Ctrl Pts',(5.55740256890582,1.43535388935104,-2.8854764739557));
#63863=CARTESIAN_POINT('Ctrl Pts',(5.5580230141851,1.44419748027931,-2.88106038003475));
#63864=CARTESIAN_POINT('Ctrl Pts',(5.55895822408513,1.45755058417665,-2.87431550318754));
#63865=CARTESIAN_POINT('Ctrl Pts',(5.55927482193106,1.46207504634677,-2.87201669162833));
#63866=CARTESIAN_POINT('Ctrl Pts',(5.55984106051881,1.47017467851059,-2.86787728925892));
#63867=CARTESIAN_POINT('Ctrl Pts',(5.56009094908147,1.47375183625143,-2.86604069359192));
#63868=CARTESIAN_POINT('Ctrl Pts',(5.56062862265659,1.48145448869857,-2.86206773913658));
#63869=CARTESIAN_POINT('Ctrl Pts',(5.56091626397239,1.48557878881347,-2.85992916142469));
#63870=CARTESIAN_POINT('Ctrl Pts',(5.56170915873222,1.4969569285186,-2.85399798841326));
#63871=CARTESIAN_POINT('Ctrl Pts',(5.56221323642519,1.50420102729836,-2.85018663189046));
#63872=CARTESIAN_POINT('Ctrl Pts',(5.56494347213424,1.54348843436372,-2.82932474259023));
#63873=CARTESIAN_POINT('Ctrl Pts',(5.56713834889372,1.57525798469487,-2.81176058566938));
#63874=CARTESIAN_POINT('Ctrl Pts',(5.57356807147927,1.66858876870023,-2.75808303758214));
#63875=CARTESIAN_POINT('Ctrl Pts',(5.57772378592383,1.72925749493823,-2.72045592663381));
#63876=CARTESIAN_POINT('Ctrl Pts',(5.59160704639625,1.93061550028086,-2.58611194428732));
#63877=CARTESIAN_POINT('Ctrl Pts',(5.60103092599434,2.06485659210997,-2.48024679972452));
#63878=CARTESIAN_POINT('Ctrl Pts',(5.62235895618099,2.34385979448734,-2.22179574286274));
#63879=CARTESIAN_POINT('Ctrl Pts',(5.63430901274956,2.48334679359652,-2.06470952215054));
#63880=CARTESIAN_POINT('Ctrl Pts',(5.64804667526959,2.61714378049107,-1.88069087504285));
#63881=CARTESIAN_POINT('Ctrl Pts',(5.6491350233813,2.62757754494847,-1.86608573232329));
#63882=CARTESIAN_POINT('Ctrl Pts',(5.65078648714904,2.64315652529494,-1.84388861739465));
#63883=CARTESIAN_POINT('Ctrl Pts',(5.65134613264727,2.64839234682038,-1.83636042898387));
#63884=CARTESIAN_POINT('Ctrl Pts',(5.65232082451493,2.65743520192789,-1.82323928315217));
#63885=CARTESIAN_POINT('Ctrl Pts',(5.65273530943965,2.66125690321684,-1.81765646645598));
#63886=CARTESIAN_POINT('Ctrl Pts',(5.65360088360612,2.66918818435974,-1.80599166058628));
#63887=CARTESIAN_POINT('Ctrl Pts',(5.65405208879384,2.67329461774508,-1.79990758844639));
#63888=CARTESIAN_POINT('Ctrl Pts',(5.6551203284501,2.68295044730295,-1.78549562009286));
#63889=CARTESIAN_POINT('Ctrl Pts',(5.65573803518012,2.68848188463367,-1.77715583571859));
#63890=CARTESIAN_POINT('Ctrl Pts',(5.65778528712872,2.70664219023806,-1.74949659775619));
#63891=CARTESIAN_POINT('Ctrl Pts',(5.65922112716679,2.7191021310095,-1.73006758480355));
#63892=CARTESIAN_POINT('Ctrl Pts',(5.67516639794492,2.85440497721602,-1.51401483145189));
#63893=CARTESIAN_POINT('Ctrl Pts',(5.69048380481867,2.95587114539125,-1.30485813474027));
#63894=CARTESIAN_POINT('Ctrl Pts',(5.71492101471144,3.07792294450576,-0.96408667233382));
#63895=CARTESIAN_POINT('Ctrl Pts',(5.72377684203181,3.11435944439208,-0.838951000405578));
#63896=CARTESIAN_POINT('Ctrl Pts',(5.73504785141941,3.15156641821013,-0.674689902675033));
#63897=CARTESIAN_POINT('Ctrl Pts',(5.73759119740044,3.15934387811338,-0.637278417531664));
#63898=CARTESIAN_POINT('Ctrl Pts',(5.74530553644627,3.18108114465367,-0.52251123320743));
#63899=CARTESIAN_POINT('Ctrl Pts',(5.75041028835494,3.19287925535904,-0.444769182042483));
#63900=CARTESIAN_POINT('Ctrl Pts',(5.75605443042392,3.2030603355405,-0.355865486786565));
#63901=CARTESIAN_POINT('Ctrl Pts',(5.75673731320433,3.20424262222793,-0.345057942485485));
#63902=CARTESIAN_POINT('Ctrl Pts',(5.75774275838028,3.20591018079604,-0.32906622532779));
#63903=CARTESIAN_POINT('Ctrl Pts',(5.75806763678374,3.2064376022514,-0.323886664994365));
#63904=CARTESIAN_POINT('Ctrl Pts',(5.75864296738437,3.20735138934002,-0.314691753231164));
#63905=CARTESIAN_POINT('Ctrl Pts',(5.75889370074057,3.20774276931626,-0.310676939637066));
#63906=CARTESIAN_POINT('Ctrl Pts',(5.75942696083544,3.20856053681283,-0.302121894131053));
#63907=CARTESIAN_POINT('Ctrl Pts',(5.7597093675177,3.20898482486157,-0.297581504344874));
#63908=CARTESIAN_POINT('Ctrl Pts',(5.76047329679431,3.21010862814966,-0.285273521559014));
#63909=CARTESIAN_POINT('Ctrl Pts',(5.76095378165595,3.21078959236411,-0.277504203862379));
#63910=CARTESIAN_POINT('Ctrl Pts',(5.76335314240504,3.21405956354168,-0.238571824618321));
#63911=CARTESIAN_POINT('Ctrl Pts',(5.76524901810381,3.21622322327722,-0.207373438937877));
#63912=CARTESIAN_POINT('Ctrl Pts',(5.77057560098595,3.22107869908176,-0.118671502974028));
#63913=CARTESIAN_POINT('Ctrl Pts',(5.7739558555122,3.22268463764689,-0.0611182975021338));
#63914=CARTESIAN_POINT('Ctrl Pts',(5.78613207429108,3.22291632152688,0.149231078375076));
#63915=CARTESIAN_POINT('Ctrl Pts',(5.79462973340814,3.21222010033394,0.301840421944264));
#63916=CARTESIAN_POINT('Ctrl Pts',(5.81702568812176,3.1558783932238,0.698579115131917));
#63917=CARTESIAN_POINT('Ctrl Pts',(5.83097945610616,3.09282206715676,0.939153625007292));
#63918=CARTESIAN_POINT('Ctrl Pts',(5.84712547503115,2.99576923190468,1.18821797460142));
#63919=CARTESIAN_POINT('Ctrl Pts',(5.84830470697859,2.9885496161645,1.20626133657158));
#63920=CARTESIAN_POINT('Ctrl Pts',(5.85005830329574,2.97762271635811,1.23286965720333));
#63921=CARTESIAN_POINT('Ctrl Pts',(5.85062842422423,2.97404062098887,1.24148580920065));
#63922=CARTESIAN_POINT('Ctrl Pts',(5.8516428854621,2.96761460890325,1.2567551260341));
#63923=CARTESIAN_POINT('Ctrl Pts',(5.85208671568457,2.96478559910676,1.26341452570482));
#63924=CARTESIAN_POINT('Ctrl Pts',(5.85301986263168,2.9588009165535,1.27737148518713));
#63925=CARTESIAN_POINT('Ctrl Pts',(5.85350933508997,2.95564062033671,1.28466699832001));
#63926=CARTESIAN_POINT('Ctrl Pts',(5.85479661463763,2.94727424481757,1.30378640735182));
#63927=CARTESIAN_POINT('Ctrl Pts',(5.85559593096266,2.94202404568027,1.31559073308843));
#63928=CARTESIAN_POINT('Ctrl Pts',(5.85917762242479,2.91825392711395,1.36818055093342));
#63929=CARTESIAN_POINT('Ctrl Pts',(5.86198670215332,2.8989565989596,1.40860722495973));
#63930=CARTESIAN_POINT('Ctrl Pts',(5.86951245628708,2.84556802897912,1.51470585722151));
#63931=CARTESIAN_POINT('Ctrl Pts',(5.8742772969735,2.81004869436329,1.57962533104583));
#63932=CARTESIAN_POINT('Ctrl Pts',(5.89867019027559,2.61966248410134,1.9008239562834));
#63933=CARTESIAN_POINT('Ctrl Pts',(5.91940508677537,2.43187999099283,2.13580939587745));
#63934=CARTESIAN_POINT('Ctrl Pts',(5.94428996814489,2.1579990584637,2.39482412440752));
#63935=CARTESIAN_POINT('Ctrl Pts',(5.94932930149055,2.09968983458391,2.44610861811486));
#63936=CARTESIAN_POINT('Ctrl Pts',(5.9549094112946,2.03118878406254,2.50210054715396));
#63937=CARTESIAN_POINT('Ctrl Pts',(5.95559015323106,2.02276268848518,2.50891732397592));
#63938=CARTESIAN_POINT('Ctrl Pts',(5.95659305738822,2.01024333330193,2.51894151184184));
#63939=CARTESIAN_POINT('Ctrl Pts',(5.9569175189599,2.00617654931791,2.52218164552797));
#63940=CARTESIAN_POINT('Ctrl Pts',(5.95749238614854,1.99894149602068,2.52791746776035));
#63941=CARTESIAN_POINT('Ctrl Pts',(5.95774307124977,1.99577637252504,2.53041706045841));
#63942=CARTESIAN_POINT('Ctrl Pts',(5.95827652688141,1.98901936935805,2.53573270315456));
#63943=CARTESIAN_POINT('Ctrl Pts',(5.95855917623622,1.98542620965538,2.53854705691229));
#63944=CARTESIAN_POINT('Ctrl Pts',(5.95931474457315,1.97578671202714,2.54606423822666));
#63945=CARTESIAN_POINT('Ctrl Pts',(5.9597866825447,1.96972952012782,2.55075319404933));
#63946=CARTESIAN_POINT('Ctrl Pts',(5.9620926199515,1.9399593527002,2.57362941123228));
#63947=CARTESIAN_POINT('Ctrl Pts',(5.96390568285206,1.91600998027129,2.59150854571359));
#63948=CARTESIAN_POINT('Ctrl Pts',(5.96819555235161,1.85815175216488,2.63346133104188));
#63949=CARTESIAN_POINT('Ctrl Pts',(5.97065400470327,1.82401930717595,2.65721662634895));
#63950=CARTESIAN_POINT('Ctrl Pts',(5.97308385260372,1.78943621012791,2.68030513419332));
#63951=CARTESIAN_POINT('Origin',(-1.72497344927317,0.,0.));
#63952=CARTESIAN_POINT('',(7.46680874532645,1.78773599488616,2.67780888195836));
#63953=CARTESIAN_POINT('',(7.21834907457188,1.78943621037019,2.68030513403157));
#63954=CARTESIAN_POINT('',(-1.72497344927317,1.78943621037804,2.68030513402633));
#63955=CARTESIAN_POINT('',(6.64657350830208,-3.22229727948493,-0.000739368720723987));
#63956=CARTESIAN_POINT('Ctrl Pts',(6.6465741241696,-3.21757478926457,-0.000748300723235639));
#63957=CARTESIAN_POINT('Ctrl Pts',(6.67694781268516,-3.21857998498449,-0.494633764188327));
#63958=CARTESIAN_POINT('Ctrl Pts',(6.77360390744728,-2.87916867694032,-2.06497840680236));
#63959=CARTESIAN_POINT('Ctrl Pts',(6.93654240845592,-0.430758100710129,
-3.78721504552185));
#63960=CARTESIAN_POINT('Ctrl Pts',(7.13538962719558,2.95292374036488,-2.41014350732934));
#63961=CARTESIAN_POINT('Ctrl Pts',(7.31214507281908,3.54954199346338,0.78188138285321));
#63962=CARTESIAN_POINT('Ctrl Pts',(7.42261811219602,2.381146258819,2.27471913214447));
#63963=CARTESIAN_POINT('Ctrl Pts',(7.46680874532643,1.78773599488645,2.67780888195817));
#63964=CARTESIAN_POINT('Ctrl Pts',(6.21703160867442,1.78943621037803,2.68030513402633));
#63965=CARTESIAN_POINT('Ctrl Pts',(6.22318199248066,1.70635893534742,2.73576952213351));
#63966=CARTESIAN_POINT('Ctrl Pts',(6.22933237628689,1.6206664666419,2.78739051154453));
#63967=CARTESIAN_POINT('Ctrl Pts',(6.23548276009313,1.53275288481828,2.83492260151512));
#63968=CARTESIAN_POINT('Ctrl Pts',(6.24163263185455,1.44484662216293,2.88245073424318));
#63969=CARTESIAN_POINT('Ctrl Pts',(6.24778250361596,1.35471999623927,2.92589043788173));
#63970=CARTESIAN_POINT('Ctrl Pts',(6.25393237537738,1.26279218109299,2.96504190018799));
#63971=CARTESIAN_POINT('Ctrl Pts',(6.26008338015052,1.1708474297737,3.00420057550087));
#63972=CARTESIAN_POINT('Ctrl Pts',(6.26623438492366,1.07710122971745,3.03906926992255));
#63973=CARTESIAN_POINT('Ctrl Pts',(6.2723853896968,0.981992300571668,3.06949648706721));
#63974=CARTESIAN_POINT('Ctrl Pts',(6.27854306737219,0.886780192740341,3.09995671310282));
#63975=CARTESIAN_POINT('Ctrl Pts',(6.28470074504757,0.790202818575205,3.12596570894925));
#63976=CARTESIAN_POINT('Ctrl Pts',(6.29085842272296,0.692713482170955,3.14742205528883));
#63977=CARTESIAN_POINT('Ctrl Pts',(6.29701969212446,0.59516728098533,3.16889091695049));
#63978=CARTESIAN_POINT('Ctrl Pts',(6.30318096152596,0.496708486284033,3.18580176775673));
#63979=CARTESIAN_POINT('Ctrl Pts',(6.30934223092745,0.397797938362765,3.19810480796586));
#63980=CARTESIAN_POINT('Ctrl Pts',(6.31551360593972,0.298725159019201,3.21042802741526));
#63981=CARTESIAN_POINT('Ctrl Pts',(6.32168498095198,0.199199579665378,3.21812830966896));
#63982=CARTESIAN_POINT('Ctrl Pts',(6.32785635596424,0.0996845383678606,
3.22120793419338));
#63983=CARTESIAN_POINT('Ctrl Pts',(6.33190448805516,0.0344073462664452,
3.22322802320766));
#63984=CARTESIAN_POINT('Ctrl Pts',(6.33595262014608,-0.0308653211708774,
3.22326103675657));
#63985=CARTESIAN_POINT('Ctrl Pts',(6.340000752237,-0.0960040035847728,3.22131972858884));
#63986=CARTESIAN_POINT('Ctrl Pts',(6.34617300032967,-0.195321935722083,
3.21835978672765));
#63987=CARTESIAN_POINT('Ctrl Pts',(6.35234524842235,-0.294677661022926,
3.21079715891031));
#63988=CARTESIAN_POINT('Ctrl Pts',(6.35851749651503,-0.393609690530847,
3.19862298091229));
#63989=CARTESIAN_POINT('Ctrl Pts',(6.36468138516757,-0.492407730548108,
3.18646529112255));
#63990=CARTESIAN_POINT('Ctrl Pts',(6.37084527382011,-0.590782788007754,
3.16970851774315));
#63991=CARTESIAN_POINT('Ctrl Pts',(6.37700916247265,-0.688274301395501,
3.14839578969013));
#63992=CARTESIAN_POINT('Ctrl Pts',(6.38316652413105,-0.785662580190206,
3.12710562986619));
#63993=CARTESIAN_POINT('Ctrl Pts',(6.38932388578945,-0.882168752945351,
3.10126919886733));
#63994=CARTESIAN_POINT('Ctrl Pts',(6.39548124744785,-0.977339268365972,
3.07098119776235));
#63995=CARTESIAN_POINT('Ctrl Pts',(6.40163411159406,-1.07244026853358,3.04071531987537));
#63996=CARTESIAN_POINT('Ctrl Pts',(6.40778697574027,-1.16620713835917,3.0060044678594));
#63997=CARTESIAN_POINT('Ctrl Pts',(6.41393983988647,-1.25819928246394,2.96699378632771));
#63998=CARTESIAN_POINT('Ctrl Pts',(6.42009037302291,-1.35015657538704,2.92799788397485));
#63999=CARTESIAN_POINT('Ctrl Pts',(6.42624090615936,-1.44034007909369,2.88470555829441));
#64000=CARTESIAN_POINT('Ctrl Pts',(6.4323914392958,-1.5283278977627,2.83731059269517));
#64001=CARTESIAN_POINT('Ctrl Pts',(6.43854128751092,-1.61630591813751,2.78992090498353));
#64002=CARTESIAN_POINT('Ctrl Pts',(6.44469113572604,-1.70208835717323,2.7384296916691));
#64003=CARTESIAN_POINT('Ctrl Pts',(6.45084098394116,-1.78527761495446,2.68307685317482));
#64004=CARTESIAN_POINT('Ctrl Pts',(6.45699179232021,-1.86847986091403,2.62771537254866));
#64005=CARTESIAN_POINT('Ctrl Pts',(6.46314260069927,-1.94908775977593,2.56849130986104));
#64006=CARTESIAN_POINT('Ctrl Pts',(6.46929340907832,-2.02673325841858,2.50568750280637));
#64007=CARTESIAN_POINT('Ctrl Pts',(6.47545079544441,-2.104461795103,2.44281653016908));
#64008=CARTESIAN_POINT('Ctrl Pts',(6.4816081818105,-2.17922126673205,2.3763584420281));
#64009=CARTESIAN_POINT('Ctrl Pts',(6.48776556817658,-2.25067735984032,2.3066358586483));
#64010=CARTESIAN_POINT('Ctrl Pts',(6.49392639091343,-2.32217333182166,2.23687436384849));
#64011=CARTESIAN_POINT('Ctrl Pts',(6.50008721365028,-2.39036195736178,2.16384506306423));
#64012=CARTESIAN_POINT('Ctrl Pts',(6.50624803638714,-2.45494784745847,2.08790532083211));
#64013=CARTESIAN_POINT('Ctrl Pts',(6.51241915930372,-2.51964171765855,2.01183861617514));
#64014=CARTESIAN_POINT('Ctrl Pts',(6.5185902822203,-2.58072055510864,1.93285209432769));
#64015=CARTESIAN_POINT('Ctrl Pts',(6.52476140513689,-2.63793101694836,1.85133398184169));
#64016=CARTESIAN_POINT('Ctrl Pts',(6.52945692708347,-2.68146166489912,1.78930797921684));
#64017=CARTESIAN_POINT('Ctrl Pts',(6.53415244903006,-2.72275359754839,1.72581695680638));
#64018=CARTESIAN_POINT('Ctrl Pts',(6.53884797097664,-2.76171321871341,1.66104113738451));
#64019=CARTESIAN_POINT('Ctrl Pts',(6.54522897047855,-2.814657561446,1.5730137623305));
#64020=CARTESIAN_POINT('Ctrl Pts',(6.55160996998045,-2.86346905836085,1.48232057530728));
#64021=CARTESIAN_POINT('Ctrl Pts',(6.55799096948236,-2.90787957691214,1.38937177482388));
#64022=CARTESIAN_POINT('Ctrl Pts',(6.56436131346836,-2.95221593514005,1.29657818786482));
#64023=CARTESIAN_POINT('Ctrl Pts',(6.57073165745436,-2.99216577134845,1.20153683592625));
#64024=CARTESIAN_POINT('Ctrl Pts',(6.57710200144036,-3.0275054200815,1.10468479390148));
#64025=CARTESIAN_POINT('Ctrl Pts',(6.58345995029587,-3.06277630650617,1.00802120224957));
#64026=CARTESIAN_POINT('Ctrl Pts',(6.58981789915138,-3.09345474225247,0.909554307574703));
#64027=CARTESIAN_POINT('Ctrl Pts',(6.59617584800689,-3.11936447139286,0.809742463448692));
#64028=CARTESIAN_POINT('Ctrl Pts',(6.60252648263553,-3.14524439380762,0.710045443535499));
#64029=CARTESIAN_POINT('Ctrl Pts',(6.60887711726416,-3.1663664260796,0.609006931994015));
#64030=CARTESIAN_POINT('Ctrl Pts',(6.6152277518928,-3.18260348814076,0.50710215911025));
#64031=CARTESIAN_POINT('Ctrl Pts',(6.62157054481824,-3.19882050083223,0.405323217270099));
#64032=CARTESIAN_POINT('Ctrl Pts',(6.62791333774369,-3.21016449675425,0.302680532611692));
#64033=CARTESIAN_POINT('Ctrl Pts',(6.63425613066913,-3.21655923055724,0.199660408737013));
#64034=CARTESIAN_POINT('Ctrl Pts',(6.63836190353712,-3.22069862543501,0.132974134341265));
#64035=CARTESIAN_POINT('Ctrl Pts',(6.64246767640511,-3.22276523869596,0.0661299544462664));
#64036=CARTESIAN_POINT('Ctrl Pts',(6.6465734492731,-3.22274991538269,-0.000738512616256426));
#64037=CARTESIAN_POINT('',(6.3999017287312,-3.22274859466306,0.0029702797283874));
#64038=CARTESIAN_POINT('Ctrl Pts',(5.97308385260372,1.78943621012791,2.68030513419332));
#64039=CARTESIAN_POINT('Ctrl Pts',(5.97382137809763,1.77893929148273,2.6873131296931));
#64040=CARTESIAN_POINT('Ctrl Pts',(5.97455626689363,1.76840085472424,2.69425969489273));
#64041=CARTESIAN_POINT('Ctrl Pts',(5.98318330575682,1.64380063053863,2.77534567482014));
#64042=CARTESIAN_POINT('Ctrl Pts',(5.99079261356728,1.52518809352019,2.84225796292038));
#64043=CARTESIAN_POINT('Ctrl Pts',(6.01229269678686,1.1788490015796,3.00969270911703));
#64044=CARTESIAN_POINT('Ctrl Pts',(6.02616469092226,0.943264145075388,3.09162894070542));
#64045=CARTESIAN_POINT('Ctrl Pts',(6.04149556839256,0.693084938689063,3.14734973413928));
#64046=CARTESIAN_POINT('Ctrl Pts',(6.04195784563979,0.685548664864803,3.14899985833507));
#64047=CARTESIAN_POINT('Ctrl Pts',(6.04410465739919,0.650586473199476,3.15652363919426));
#64048=CARTESIAN_POINT('Ctrl Pts',(6.04579931469567,0.62309118595241,3.1620660242917));
#64049=CARTESIAN_POINT('Ctrl Pts',(6.04818425143307,0.58456082007855,3.16931076653259));
#64050=CARTESIAN_POINT('Ctrl Pts',(6.04886486996055,0.573583407319249,3.17131584002005));
#64051=CARTESIAN_POINT('Ctrl Pts',(6.04996374001142,0.555891145472322,3.17445254552118));
#64052=CARTESIAN_POINT('Ctrl Pts',(6.05038084803096,0.549182671943636,3.17561999003182));
#64053=CARTESIAN_POINT('Ctrl Pts',(6.05124712165015,0.535265257883513,3.17799655394394));
#64054=CARTESIAN_POINT('Ctrl Pts',(6.05169638797248,0.528055808980083,3.17920242425297));
#64055=CARTESIAN_POINT('Ctrl Pts',(6.05275158514046,0.511142986195283,3.1819721889565));
#64056=CARTESIAN_POINT('Ctrl Pts',(6.05335814304593,0.501436476991041,3.18351623519368));
#64057=CARTESIAN_POINT('Ctrl Pts',(6.05528345677849,0.470676666321469,3.18826513174473));
#64058=CARTESIAN_POINT('Ctrl Pts',(6.05660740683802,0.44959892094112,3.19130566535268));
#64059=CARTESIAN_POINT('Ctrl Pts',(6.064666679993,0.321762238951724,3.20845493654918));
#64060=CARTESIAN_POINT('Ctrl Pts',(6.07156351342504,0.214392382068316,3.2174128660244));
#64061=CARTESIAN_POINT('Ctrl Pts',(6.09225405842035,-0.101761957662599,
3.22789431233396));
#64062=CARTESIAN_POINT('Ctrl Pts',(6.10643511298629,-0.310470080563394,
3.21453701411536));
#64063=CARTESIAN_POINT('Ctrl Pts',(6.13153438876407,-0.677276735840849,
3.15499269748844));
#64064=CARTESIAN_POINT('Ctrl Pts',(6.14243818045279,-0.835967764825255,
3.11670566790433));
#64065=CARTESIAN_POINT('Ctrl Pts',(6.15349346429487,-1.00252927274747,3.06287397228893));
#64066=CARTESIAN_POINT('Ctrl Pts',(6.15424883353228,-1.01394107149312,3.05911513792747));
#64067=CARTESIAN_POINT('Ctrl Pts',(6.15533620328506,-1.03041809104095,3.05358558160261));
#64068=CARTESIAN_POINT('Ctrl Pts',(6.15567113257438,-1.03550016349634,3.05186594707372));
#64069=CARTESIAN_POINT('Ctrl Pts',(6.15625868381738,-1.04442794500729,3.04882016159024));
#64070=CARTESIAN_POINT('Ctrl Pts',(6.15651162437462,-1.04827546782294,3.04749941006308));
#64071=CARTESIAN_POINT('Ctrl Pts',(6.15703909915638,-1.05630776115386,3.04472512727521));
#64072=CARTESIAN_POINT('Ctrl Pts',(6.15731355172057,-1.0604920297935,3.04327025455244));
#64073=CARTESIAN_POINT('Ctrl Pts',(6.15803372556163,-1.07148425274696,3.03942282852475));
#64074=CARTESIAN_POINT('Ctrl Pts',(6.158478603651,-1.07828724146511,3.03701601275));
#64075=CARTESIAN_POINT('Ctrl Pts',(6.16021892737412,-1.10494660587794,3.02748337876476));
#64076=CARTESIAN_POINT('Ctrl Pts',(6.1615044775537,-1.12474143331095,3.02018532102644));
#64077=CARTESIAN_POINT('Ctrl Pts',(6.16489885401067,-1.17722620165466,3.00024737443334));
#64078=CARTESIAN_POINT('Ctrl Pts',(6.16698978400142,-1.20978485802285,2.987267421338));
#64079=CARTESIAN_POINT('Ctrl Pts',(6.1765516726158,-1.35930219680581,2.92481464276314));
#64080=CARTESIAN_POINT('Ctrl Pts',(6.18374221081456,-1.47349319523562,2.86898354333662));
#64081=CARTESIAN_POINT('Ctrl Pts',(6.19770433795226,-1.69022356439396,2.74665471137447));
#64082=CARTESIAN_POINT('Ctrl Pts',(6.20447050041648,-1.79286398885752,2.68078467120398));
#64083=CARTESIAN_POINT('Ctrl Pts',(6.22174523216218,-2.041157682195,2.50078948819136));
#64084=CARTESIAN_POINT('Ctrl Pts',(6.23236606783285,-2.18115881205774,2.37966482749067));
#64085=CARTESIAN_POINT('Ctrl Pts',(6.24460345092098,-2.32247442787637,2.23440150736585));
#64086=CARTESIAN_POINT('Ctrl Pts',(6.2456881639417,-2.33484097019767,2.22147590313542));
#64087=CARTESIAN_POINT('Ctrl Pts',(6.24733502941737,-2.35337233938425,2.20178109697871));
#64088=CARTESIAN_POINT('Ctrl Pts',(6.24789373916421,-2.35961711808893,2.19508733769179));
#64089=CARTESIAN_POINT('Ctrl Pts',(6.24886725733398,-2.37042469176068,2.18340332139101));
#64090=CARTESIAN_POINT('Ctrl Pts',(6.2492815076807,-2.37500048041929,2.17842511922576));
#64091=CARTESIAN_POINT('Ctrl Pts',(6.25014703678115,-2.38451285786626,2.16801058960294));
#64092=CARTESIAN_POINT('Ctrl Pts',(6.25059843290165,-2.38944659574495,2.16257172149734));
#64093=CARTESIAN_POINT('Ctrl Pts',(6.25166792727152,-2.4010715459777,2.14966822706807));
#64094=CARTESIAN_POINT('Ctrl Pts',(6.25228670214189,-2.40774657355811,2.14218918147963));
#64095=CARTESIAN_POINT('Ctrl Pts',(6.25359196767678,-2.42171984071978,2.12638499487344));
#64096=CARTESIAN_POINT('Ctrl Pts',(6.25427877361462,-2.42901028008742,2.11805315978178));
#64097=CARTESIAN_POINT('Ctrl Pts',(6.25955085600118,-2.48449703295501,2.05397720278075));
#64098=CARTESIAN_POINT('Ctrl Pts',(6.26421311525487,-2.53080813159671,1.99663632618325));
#64099=CARTESIAN_POINT('Ctrl Pts',(6.27570067550211,-2.63823803695987,1.85387171413791));
#64100=CARTESIAN_POINT('Ctrl Pts',(6.28259802645541,-2.69722277558864,1.76695388816216));
#64101=CARTESIAN_POINT('Ctrl Pts',(6.29553432983563,-2.79819382187388,1.60129800499984));
#64102=CARTESIAN_POINT('Ctrl Pts',(6.30153843165868,-2.84135898120196,1.52339161236876));
#64103=CARTESIAN_POINT('Ctrl Pts',(6.31623877924124,-2.93870800537018,1.32912240599941));
#64104=CARTESIAN_POINT('Ctrl Pts',(6.32494511627583,-2.9892778123745,1.21111162310591));
#64105=CARTESIAN_POINT('Ctrl Pts',(6.33971242560796,-3.06446338854289,1.00200092214054));
#64106=CARTESIAN_POINT('Ctrl Pts',(6.34584922200872,-3.09236978229926,0.912246987247727));
#64107=CARTESIAN_POINT('Ctrl Pts',(6.35249324569459,-3.11920321585724,0.810442538773199));
#64108=CARTESIAN_POINT('Ctrl Pts',(6.35320484388622,-3.12203188112718,0.79947654918524));
#64109=CARTESIAN_POINT('Ctrl Pts',(6.35424075017343,-3.12608409086974,0.78341767112212));
#64110=CARTESIAN_POINT('Ctrl Pts',(6.35456761827228,-3.12735308021812,0.778336497403659));
#64111=CARTESIAN_POINT('Ctrl Pts',(6.35514590202078,-3.12958111450049,0.769321780665932));
#64112=CARTESIAN_POINT('Ctrl Pts',(6.35539760459214,-3.13054513902967,0.765389500619389));
#64113=CARTESIAN_POINT('Ctrl Pts',(6.35592772856685,-3.13256341375496,0.757089301730397));
#64114=CARTESIAN_POINT('Ctrl Pts',(6.35620604917879,-3.13361593727993,0.752721004226726));
#64115=CARTESIAN_POINT('Ctrl Pts',(6.35677270642933,-3.13574426683613,0.743805946100877));
#64116=CARTESIAN_POINT('Ctrl Pts',(6.35706099989135,-3.13681932845788,0.739259016657208));
#64117=CARTESIAN_POINT('Ctrl Pts',(6.35777869344282,-3.13947613799955,0.727912002815692));
#64118=CARTESIAN_POINT('Ctrl Pts',(6.35820740949357,-3.14104569359581,0.721109047052204));
#64119=CARTESIAN_POINT('Ctrl Pts',(6.35940976951335,-3.14539775027651,0.701962015149182));
#64120=CARTESIAN_POINT('Ctrl Pts',(6.36018067173886,-3.14812971049966,0.689606420923647));
#64121=CARTESIAN_POINT('Ctrl Pts',(6.37468856005444,-3.19841392860664,0.455662524500434));
#64122=CARTESIAN_POINT('Ctrl Pts',(6.38723176905914,-3.22253967884565,0.229656840923317));
#64123=CARTESIAN_POINT('Ctrl Pts',(6.39990164604897,-3.2227486308868,0.0029706257346402));
#64124=CARTESIAN_POINT('Ctrl Pts',(6.39990166558323,-3.22274863120894,0.00297027623255133));
#64125=CARTESIAN_POINT('Ctrl Pts',(6.41277784774664,-3.222960960657,-0.227407097632205));
#64126=CARTESIAN_POINT('Ctrl Pts',(6.42573644257657,-3.1984720160562,-0.457120151576906));
#64127=CARTESIAN_POINT('Ctrl Pts',(6.44079109024918,-3.14530149897629,-0.702587204161363));
#64128=CARTESIAN_POINT('Ctrl Pts',(6.44204399814821,-3.14070098266663,-0.722874543574654));
#64129=CARTESIAN_POINT('Ctrl Pts',(6.44401815107632,-3.13318070024313,-0.754609697770681));
#64130=CARTESIAN_POINT('Ctrl Pts',(6.44473515966878,-3.13039379046217,-0.766088641883618));
#64131=CARTESIAN_POINT('Ctrl Pts',(6.44594696810494,-3.12559072010532,-0.78540801266658));
#64132=CARTESIAN_POINT('Ctrl Pts',(6.44644068997747,-3.12360799595938,-0.793256693429814));
#64133=CARTESIAN_POINT('Ctrl Pts',(6.44741776269864,-3.11963342914898,-0.808744179914984));
#64134=CARTESIAN_POINT('Ctrl Pts',(6.44790106332227,-3.11764304864468,-0.816383304761118));
#64135=CARTESIAN_POINT('Ctrl Pts',(6.4488300379962,-3.11377066222345,-0.831024910474995));
#64136=CARTESIAN_POINT('Ctrl Pts',(6.44927556687871,-3.11189304939165,-0.838028511765836));
#64137=CARTESIAN_POINT('Ctrl Pts',(6.45029364337235,-3.10755607600124,-0.853990099987739));
#64138=CARTESIAN_POINT('Ctrl Pts',(6.45086668019823,-3.10508159562469,-0.862943878816772));
#64139=CARTESIAN_POINT('Ctrl Pts',(6.45266129072657,-3.09722842281783,-0.890889028782707));
#64140=CARTESIAN_POINT('Ctrl Pts',(6.45388727979266,-3.09171402376146,-0.909841487326335));
#64141=CARTESIAN_POINT('Ctrl Pts',(6.46958377096014,-3.01922682830068,-1.15070216269025));
#64142=CARTESIAN_POINT('Ctrl Pts',(6.48486602613934,-2.9286907098309,-1.36476249732738));
#64143=CARTESIAN_POINT('Ctrl Pts',(6.50745821405934,-2.76585436836356,-1.65734875183981));
#64144=CARTESIAN_POINT('Ctrl Pts',(6.51446175078708,-2.71140048421781,-1.74501077904379));
#64145=CARTESIAN_POINT('Ctrl Pts',(6.53088022225938,-2.57307049723676,-1.94554895291717));
#64146=CARTESIAN_POINT('Ctrl Pts',(6.54023563212587,-2.4858180065267,-2.05586252342072));
#64147=CARTESIAN_POINT('Ctrl Pts',(6.55021057344749,-2.38047906322105,-2.1724902683892));
#64148=CARTESIAN_POINT('Ctrl Pts',(6.55126054899762,-2.36922814285503,-2.18475457927284));
#64149=CARTESIAN_POINT('Ctrl Pts',(6.55260237375811,-2.35463233100135,-2.20041970523343));
#64150=CARTESIAN_POINT('Ctrl Pts',(6.55290059229195,-2.35137446021599,-2.20390073322507));
#64151=CARTESIAN_POINT('Ctrl Pts',(6.55348289142529,-2.34498552285598,-2.21069700638276));
#64152=CARTESIAN_POINT('Ctrl Pts',(6.55376702130051,-2.3418551224516,-2.21401285960518));
#64153=CARTESIAN_POINT('Ctrl Pts',(6.5543014601919,-2.33594227210772,-2.22024943105404));
#64154=CARTESIAN_POINT('Ctrl Pts',(6.55455188114838,-2.33316140900805,-2.22317153508758));
#64155=CARTESIAN_POINT('Ctrl Pts',(6.55512453924631,-2.32677870521814,-2.22985325225507));
#64156=CARTESIAN_POINT('Ctrl Pts',(6.55544648999754,-2.32317324227626,-2.23360935638398));
#64157=CARTESIAN_POINT('Ctrl Pts',(6.55643861215128,-2.31201049711778,-2.24518222797489));
#64158=CARTESIAN_POINT('Ctrl Pts',(6.55710644347141,-2.30442265263173,-2.25296960066857));
#64159=CARTESIAN_POINT('Ctrl Pts',(6.56257968698295,-2.24164300533202,-2.31675109437592));
#64160=CARTESIAN_POINT('Ctrl Pts',(6.56723584154511,-2.18445337731023,-2.37075193363298));
#64161=CARTESIAN_POINT('Ctrl Pts',(6.57400062266901,-2.09683274350277,-2.44762092280927));
#64162=CARTESIAN_POINT('Ctrl Pts',(6.57617951410607,-2.0678849459238,-2.47212616005106));
#64163=CARTESIAN_POINT('Ctrl Pts',(6.5822332578483,-1.98568409489452,-2.53925739233174));
#64164=CARTESIAN_POINT('Ctrl Pts',(6.58607189690449,-1.93149978239982,-2.58071280100383));
#64165=CARTESIAN_POINT('Ctrl Pts',(6.59751860008124,-1.76540025308559,-2.69962863215977));
#64166=CARTESIAN_POINT('Ctrl Pts',(6.60507068768653,-1.64985595492655,-2.7717516927804));
#64167=CARTESIAN_POINT('Ctrl Pts',(6.61910560286572,-1.4317232796006,-2.88942570756378));
#64168=CARTESIAN_POINT('Ctrl Pts',(6.62552776846441,-1.33065798105164,-2.93733868755377));
#64169=CARTESIAN_POINT('Ctrl Pts',(6.63444981263702,-1.19080439043145,-2.99493931834794));
#64170=CARTESIAN_POINT('Ctrl Pts',(6.63679906609222,-1.15402284443624,-3.00930352296862));
#64171=CARTESIAN_POINT('Ctrl Pts',(6.64082664512479,-1.0911223610592,-3.032545122067));
#64172=CARTESIAN_POINT('Ctrl Pts',(6.64249344409555,-1.0651359638427,-3.04176975303239));
#64173=CARTESIAN_POINT('Ctrl Pts',(6.64467473172646,-1.03120393356188,-3.05332678392861));
#64174=CARTESIAN_POINT('Ctrl Pts',(6.64517913145368,-1.0233626877562,-3.05596381021701));
#64175=CARTESIAN_POINT('Ctrl Pts',(6.64617434143269,-1.00790225700872,-3.06109700681205));
#64176=CARTESIAN_POINT('Ctrl Pts',(6.64666508757715,-1.00028373542448,-3.06359499470874));
#64177=CARTESIAN_POINT('Ctrl Pts',(6.6475995516659,-0.985787041364879,-3.06828838281788));
#64178=CARTESIAN_POINT('Ctrl Pts',(6.64804308920575,-0.978910648088813,
-3.07048915203513));
#64179=CARTESIAN_POINT('Ctrl Pts',(6.64905388346546,-0.963250121997491,
-3.07544330251065));
#64180=CARTESIAN_POINT('Ctrl Pts',(6.64962161328873,-0.954461500116476,
-3.07818218214338));
#64181=CARTESIAN_POINT('Ctrl Pts',(6.65109382911773,-0.931691119135956,
-3.08517143375974));
#64182=CARTESIAN_POINT('Ctrl Pts',(6.65200018867653,-0.917692086100695,
-3.08936439109155));
#64183=CARTESIAN_POINT('Ctrl Pts',(6.65765262601639,-0.830515814075435,
-3.11483041108697));
#64184=CARTESIAN_POINT('Ctrl Pts',(6.66247979776866,-0.756637045949777,
-3.13359598546297));
#64185=CARTESIAN_POINT('Ctrl Pts',(6.6699678015346,-0.642994869656276,-3.15820861050688));
#64186=CARTESIAN_POINT('Ctrl Pts',(6.67257014033762,-0.603668809639296,
-3.16596079991464));
#64187=CARTESIAN_POINT('Ctrl Pts',(6.67815697430394,-0.519580394928984,
-3.18091315895159));
#64188=CARTESIAN_POINT('Ctrl Pts',(6.68114627075611,-0.474790189092412,
-3.18790625992317));
#64189=CARTESIAN_POINT('Ctrl Pts',(6.69658279853086,-0.244368222847626,
-3.21891837639952));
#64190=CARTESIAN_POINT('Ctrl Pts',(6.709352441565,-0.0570513147570352,-3.22767549083771));
#64191=CARTESIAN_POINT('Ctrl Pts',(6.73052173880749,0.257276037426847,-3.21499066527969));
#64192=CARTESIAN_POINT('Ctrl Pts',(6.73898942867085,0.384200416649385,-3.20230435455845));
#64193=CARTESIAN_POINT('Ctrl Pts',(6.7483637614936,0.529546698612316,-3.17900733851338));
#64194=CARTESIAN_POINT('Ctrl Pts',(6.74961240372288,0.549012715273,-3.17570345728896));
#64195=CARTESIAN_POINT('Ctrl Pts',(6.75127395353869,0.575076612694543,-3.17103292406748));
#64196=CARTESIAN_POINT('Ctrl Pts',(6.75169541057584,0.581701854110343,-3.16982426497883));
#64197=CARTESIAN_POINT('Ctrl Pts',(6.75239442313732,0.592714540929362,-3.16777950352941));
#64198=CARTESIAN_POINT('Ctrl Pts',(6.75267263317171,0.597104085607614,-3.16695503939359));
#64199=CARTESIAN_POINT('Ctrl Pts',(6.7532025038105,0.605476903571851,-3.1653643921128));
#64200=CARTESIAN_POINT('Ctrl Pts',(6.75345424941978,0.609460396678054,-3.16459982314387));
#64201=CARTESIAN_POINT('Ctrl Pts',(6.75403328048411,0.618635133722468,-3.16282091035401));
#64202=CARTESIAN_POINT('Ctrl Pts',(6.75436026180352,0.623825327791362,-3.16180130637613));
#64203=CARTESIAN_POINT('Ctrl Pts',(6.75523444516756,0.637725041050718,-3.15903517541197));
#64204=CARTESIAN_POINT('Ctrl Pts',(6.75578034124197,0.646429964006964,-3.15726539483563));
#64205=CARTESIAN_POINT('Ctrl Pts',(6.7596832781468,0.708835525872825,-3.14430892907404));
#64206=CARTESIAN_POINT('Ctrl Pts',(6.76296783799149,0.762253851803676,-3.13178804442739));
#64207=CARTESIAN_POINT('Ctrl Pts',(6.76682137170641,0.825565353494423,-3.11523214759048));
#64208=CARTESIAN_POINT('Ctrl Pts',(6.76744231779076,0.835787461827807,-3.11250523048514));
#64209=CARTESIAN_POINT('Ctrl Pts',(6.77440546891616,0.950613957072339,-3.08126688312451));
#64210=CARTESIAN_POINT('Ctrl Pts',(6.7805479430104,1.05373662377573,-3.04754243911072));
#64211=CARTESIAN_POINT('Ctrl Pts',(6.80253774613786,1.41936937893766,-2.90718374429777));
#64212=CARTESIAN_POINT('Ctrl Pts',(6.81809505291899,1.66920859283577,-2.77129153495518));
#64213=CARTESIAN_POINT('Ctrl Pts',(6.83740520208559,1.93109223551615,-2.58043983867366));
#64214=CARTESIAN_POINT('Ctrl Pts',(6.83986259152405,1.96365072711764,-2.55575088271706));
#64215=CARTESIAN_POINT('Ctrl Pts',(6.84310109955373,2.00551186272474,-2.52273560546881));
#64216=CARTESIAN_POINT('Ctrl Pts',(6.84386008801061,2.01524882828709,-2.51496419853156));
#64217=CARTESIAN_POINT('Ctrl Pts',(6.8451043559084,2.0310896923243,-2.50216999932124));
#64218=CARTESIAN_POINT('Ctrl Pts',(6.84558827852859,2.03722066388927,-2.497180812162));
#64219=CARTESIAN_POINT('Ctrl Pts',(6.84651768419625,2.04893802932612,-2.48757372691249));
#64220=CARTESIAN_POINT('Ctrl Pts',(6.84696301905348,2.05452732774937,-2.48295943442657));
#64221=CARTESIAN_POINT('Ctrl Pts',(6.84797959230421,2.06722843763702,-2.47240167684161));
#64222=CARTESIAN_POINT('Ctrl Pts',(6.84855131484562,2.07433024656088,-2.46644632829341));
#64223=CARTESIAN_POINT('Ctrl Pts',(6.85033775734316,2.09639162670946,-2.44778368606331));
#64224=CARTESIAN_POINT('Ctrl Pts',(6.85155683524338,2.11126064583525,-2.43497048938502));
#64225=CARTESIAN_POINT('Ctrl Pts',(6.86310869874889,2.25039316012435,-2.31284226104784));
#64226=CARTESIAN_POINT('Ctrl Pts',(6.87383972080921,2.36615976996346,-2.19426099354943));
#64227=CARTESIAN_POINT('Ctrl Pts',(6.89345434934639,2.55517831926851,-1.96821614723181));
#64228=CARTESIAN_POINT('Ctrl Pts',(6.90220502793478,2.63202073044741,-1.86420894114727));
#64229=CARTESIAN_POINT('Ctrl Pts',(6.9190178968012,2.76738879535141,-1.65586855642765));
#64230=CARTESIAN_POINT('Ctrl Pts',(6.92706745972506,2.8267704290833,-1.55232520473732));
#64231=CARTESIAN_POINT('Ctrl Pts',(6.93808400264493,2.90188431920851,-1.40267769396412));
#64232=CARTESIAN_POINT('Ctrl Pts',(6.94121813379093,2.92252412319212,-1.35915068414243));
#64233=CARTESIAN_POINT('Ctrl Pts',(6.94606776273347,2.95341931601618,-1.29003496762093));
#64234=CARTESIAN_POINT('Ctrl Pts',(6.94781571105146,2.96433487376341,-1.2647508653687));
#64235=CARTESIAN_POINT('Ctrl Pts',(6.95001384645631,2.97779726074388,-1.23243531524486));
#64236=CARTESIAN_POINT('Ctrl Pts',(6.95048137584784,2.98064516138895,-1.22553162214712));
#64237=CARTESIAN_POINT('Ctrl Pts',(6.95122746015266,2.98516546230746,-1.2144648416895));
#64238=CARTESIAN_POINT('Ctrl Pts',(6.95150693305045,2.98685319056344,-1.21030810443518));
#64239=CARTESIAN_POINT('Ctrl Pts',(6.95203772450084,2.99004822486201,-1.20239160960812));
#64240=CARTESIAN_POINT('Ctrl Pts',(6.95228913390641,2.99155710433421,-1.19863257986645));
#64241=CARTESIAN_POINT('Ctrl Pts',(6.95286543614774,2.99500556283479,-1.18999445706198));
#64242=CARTESIAN_POINT('Ctrl Pts',(6.95319003432388,2.99694030640924,-1.18511346713992));
#64243=CARTESIAN_POINT('Ctrl Pts',(6.95405371182265,3.00206761242918,-1.17208539756747));
#64244=CARTESIAN_POINT('Ctrl Pts',(6.95459153401772,3.00523896416154,-1.16392993827157));
#64245=CARTESIAN_POINT('Ctrl Pts',(6.95832550725685,3.02710271983819,-1.10701991064165));
#64246=CARTESIAN_POINT('Ctrl Pts',(6.96145605413339,3.04464228220179,-1.05782705047883));
#64247=CARTESIAN_POINT('Ctrl Pts',(6.98349153082733,3.16150106403291,-0.703043295171254));
#64248=CARTESIAN_POINT('Ctrl Pts',(7.00059796009312,3.21582939435065,-0.384516819152284));
#64249=CARTESIAN_POINT('Ctrl Pts',(7.02354659429729,3.22364935835346,0.0142683079844779));
#64250=CARTESIAN_POINT('Ctrl Pts',(7.02806554300593,3.22237493104741,0.0917457403873097));
#64251=CARTESIAN_POINT('Ctrl Pts',(7.03542064431528,3.2158795514194,0.215367132216485));
#64252=CARTESIAN_POINT('Ctrl Pts',(7.03820221362001,3.21245105132584,0.26157637574521));
#64253=CARTESIAN_POINT('Ctrl Pts',(7.0418089856256,3.20677944532132,0.320708738415351));
#64254=CARTESIAN_POINT('Ctrl Pts',(7.0426052767562,3.20545197263471,0.333715671020363));
#64255=CARTESIAN_POINT('Ctrl Pts',(7.04389192683434,3.20318632791259,0.354652893595549));
#64256=CARTESIAN_POINT('Ctrl Pts',(7.04438071788972,3.20229775473078,0.362588491946789));
#64257=CARTESIAN_POINT('Ctrl Pts',(7.04531367500036,3.20054880436754,0.377699806791281));
#64258=CARTESIAN_POINT('Ctrl Pts',(7.04575766971974,3.19969376322551,0.384876101374628));
#64259=CARTESIAN_POINT('Ctrl Pts',(7.04677260050641,3.19768752625469,0.40124541578703));
#64260=CARTESIAN_POINT('Ctrl Pts',(7.04734402415462,3.19652081597348,0.410436437748819));
#64261=CARTESIAN_POINT('Ctrl Pts',(7.04883204598333,3.19338640414859,0.434304171531368));
#64262=CARTESIAN_POINT('Ctrl Pts',(7.04975058505057,3.19135716647256,0.448972453306252));
#64263=CARTESIAN_POINT('Ctrl Pts',(7.05561540897138,3.17780321955445,0.54220840077987));
#64264=CARTESIAN_POINT('Ctrl Pts',(7.0606499344613,3.16347993881912,0.620335502024622));
#64265=CARTESIAN_POINT('Ctrl Pts',(7.06609761137538,3.14518907872737,0.702800789693252));
#64266=CARTESIAN_POINT('Ctrl Pts',(7.06642507918124,3.14407904229985,0.707750143954934));
#64267=CARTESIAN_POINT('Ctrl Pts',(7.06706438648791,3.14189139619561,0.71739755364541));
#64268=CARTESIAN_POINT('Ctrl Pts',(7.0673761926074,3.14081492151291,0.722095855055939));
#64269=CARTESIAN_POINT('Ctrl Pts',(7.07163012442392,3.12599925968216,0.786099264453137));
#64270=CARTESIAN_POINT('Ctrl Pts',(7.07561923715654,3.11059363260896,0.845002949504906));
#64271=CARTESIAN_POINT('Ctrl Pts',(7.09556025874728,3.02611840228877,1.13426272846525));
#64272=CARTESIAN_POINT('Ctrl Pts',(7.11209313398907,2.93309142370641,1.35679951334675));
#64273=CARTESIAN_POINT('Ctrl Pts',(7.1326162753722,2.78313897319671,1.62630727125358));
#64274=CARTESIAN_POINT('Ctrl Pts',(7.13708637175668,2.74821706590087,1.68464895624599));
#64275=CARTESIAN_POINT('Ctrl Pts',(7.14372720747798,2.69249894086202,1.77138350379706));
#64276=CARTESIAN_POINT('Ctrl Pts',(7.14596405582013,2.67304181216371,1.80061039075857));
#64277=CARTESIAN_POINT('Ctrl Pts',(7.14867973121104,2.64851213245526,1.83618262873122));
#64278=CARTESIAN_POINT('Ctrl Pts',(7.14918714612422,2.64388905966814,1.8428330920991));
#64279=CARTESIAN_POINT('Ctrl Pts',(7.14998176575461,2.63658571321376,1.85325517568702));
#64280=CARTESIAN_POINT('Ctrl Pts',(7.1502701053596,2.63392234437909,1.85703851703648));
#64281=CARTESIAN_POINT('Ctrl Pts',(7.15080812635734,2.62892769936669,1.86410109753713));
#64282=CARTESIAN_POINT('Ctrl Pts',(7.15105793821985,2.62659845506331,1.86738167133472));
#64283=CARTESIAN_POINT('Ctrl Pts',(7.15162357823566,2.62130146123447,1.87481258901128));
#64284=CARTESIAN_POINT('Ctrl Pts',(7.15193914589485,2.61833000322528,1.87896024163595));
#64285=CARTESIAN_POINT('Ctrl Pts',(7.15287192304153,2.60949892455134,1.89122530430338));
#64286=CARTESIAN_POINT('Ctrl Pts',(7.15348722432998,2.60361124981536,1.89932257789342));
#64287=CARTESIAN_POINT('Ctrl Pts',(7.15778551053343,2.56205281956822,1.95592118110281));
#64288=CARTESIAN_POINT('Ctrl Pts',(7.16138142958591,2.52506416323742,2.00344562829945));
#64289=CARTESIAN_POINT('Ctrl Pts',(7.18336192184959,2.28679808374598,2.29248830535901));
#64290=CARTESIAN_POINT('Ctrl Pts',(7.20013846113611,2.05240281582212,2.50452306939585));
#64291=CARTESIAN_POINT('Ctrl Pts',(7.21827755053244,1.79046916109811,2.67961529540315));
#64292=CARTESIAN_POINT('Ctrl Pts',(7.21831331056787,1.78995273479898,2.67996028989249));
#64293=CARTESIAN_POINT('Ctrl Pts',(7.21834907457188,1.78943621037019,2.68030513403157));
#64294=CARTESIAN_POINT('Origin',(-1.72497344927317,0.,0.));
#64295=CARTESIAN_POINT('',(8.71691228903198,1.78943621037803,2.68030513402633));
#64296=CARTESIAN_POINT('',(8.46829646867762,1.78943615355263,2.68030517196433));
#64297=CARTESIAN_POINT('',(-1.72497344927317,1.78943621037804,2.68030513402633));
#64298=CARTESIAN_POINT('',(7.8965734492731,-3.22274887139593,-0.00269711257784768));
#64299=CARTESIAN_POINT('Ctrl Pts',(7.8965734492731,-3.22274887139593,-0.00269711257784768));
#64300=CARTESIAN_POINT('Ctrl Pts',(7.90619705313966,-3.2226187285209,-0.158203340630839));
#64301=CARTESIAN_POINT('Ctrl Pts',(7.91582065700621,-3.21123025196946,-0.313254007322803));
#64302=CARTESIAN_POINT('Ctrl Pts',(7.92544426087277,-3.18879700715618,-0.466573905883924));
#64303=CARTESIAN_POINT('Ctrl Pts',(7.9272223412999,-3.18465218635178,-0.494901662772128));
#64304=CARTESIAN_POINT('Ctrl Pts',(7.92900042172702,-3.18013043580562,-0.523170431299474));
#64305=CARTESIAN_POINT('Ctrl Pts',(7.93077850215415,-3.17523324768117,-0.551372274711115));
#64306=CARTESIAN_POINT('Ctrl Pts',(7.93695075024691,-3.15823364541348,-0.649269294190383));
#64307=CARTESIAN_POINT('Ctrl Pts',(7.94312299833967,-3.13667242061309,-0.74655170305749));
#64308=CARTESIAN_POINT('Ctrl Pts',(7.94929524643243,-3.11060617359134,-0.842761410670567));
#64309=CARTESIAN_POINT('Ctrl Pts',(7.95545913508506,-3.08457522962746,-0.93884081579429));
#64310=CARTESIAN_POINT('Ctrl Pts',(7.96162302373769,-3.05405150327207,-1.03384999174038));
#64311=CARTESIAN_POINT('Ctrl Pts',(7.96778691239031,-3.01914293225304,-1.12733913137375));
#64312=CARTESIAN_POINT('Ctrl Pts',(7.97394427404886,-2.98427132621656,-1.22072927456257));
#64313=CARTESIAN_POINT('Ctrl Pts',(7.9801016357074,-2.94502425764515,-1.31260217674605));
#64314=CARTESIAN_POINT('Ctrl Pts',(7.98625899736594,-2.90155972324655,-1.40252227609168));
#64315=CARTESIAN_POINT('Ctrl Pts',(7.99241186151225,-2.85812693658118,-1.49237669523702));
#64316=CARTESIAN_POINT('Ctrl Pts',(7.99856472565856,-2.81048299723078,-1.58028075753251));
#64317=CARTESIAN_POINT('Ctrl Pts',(8.00471758980487,-2.75883400138122,-1.66581887230362));
#64318=CARTESIAN_POINT('Ctrl Pts',(8.0108681229414,-2.70720457273012,-1.75132458099905));
#64319=CARTESIAN_POINT('Ctrl Pts',(8.01701865607794,-2.65157332675075,-1.83446575175514));
#64320=CARTESIAN_POINT('Ctrl Pts',(8.02316918921448,-2.59219185890672,-1.91485219511004));
#64321=CARTESIAN_POINT('Ctrl Pts',(8.02931903742969,-2.5328170037633,-1.99522968665721));
#64322=CARTESIAN_POINT('Ctrl Pts',(8.03546888564489,-2.46969301514349,-2.07285271131146));
#64323=CARTESIAN_POINT('Ctrl Pts',(8.0416187338601,-2.4031136986529,-2.14736166349471));
#64324=CARTESIAN_POINT('Ctrl Pts',(8.04776954223923,-2.33652398726221,-2.22188224861678));
#64325=CARTESIAN_POINT('Ctrl Pts',(8.05392035061836,-2.26647816592401,-2.29328747162887));
#64326=CARTESIAN_POINT('Ctrl Pts',(8.06007115899749,-2.19330835886251,-2.36125305832388));
#64327=CARTESIAN_POINT('Ctrl Pts',(8.06622854536368,-2.12006030029093,-2.42929133087122));
#64328=CARTESIAN_POINT('Ctrl Pts',(8.07238593172987,-2.04368190334552,-2.49388232527394));
#64329=CARTESIAN_POINT('Ctrl Pts',(8.07854331809606,-1.96453989401621,-2.55474080237483));
#64330=CARTESIAN_POINT('Ctrl Pts',(8.08470414083302,-1.88535371638699,-2.61563324393393));
#64331=CARTESIAN_POINT('Ctrl Pts',(8.09086496356998,-1.8034012111174,-2.67278877128187));
#64332=CARTESIAN_POINT('Ctrl Pts',(8.09702578630694,-1.71907798398794,-2.72596559909841));
#64333=CARTESIAN_POINT('Ctrl Pts',(8.10319690922362,-1.63461377822112,-2.77923133239189));
#64334=CARTESIAN_POINT('Ctrl Pts',(8.10936803214031,-1.54777131145734,-2.8285048646833));
#64335=CARTESIAN_POINT('Ctrl Pts',(8.115539155057,-1.45897078394203,-2.87359040472082));
#64336=CARTESIAN_POINT('Ctrl Pts',(8.1202346770026,-1.39140369261068,-2.90789536761548));
#64337=CARTESIAN_POINT('Ctrl Pts',(8.12493019894819,-1.32270349535213,-2.93977665558864));
#64338=CARTESIAN_POINT('Ctrl Pts',(8.12962572089379,-1.25306185638666,-2.96916714695701));
#64339=CARTESIAN_POINT('Ctrl Pts',(8.13579796898656,-1.16151815192487,-3.00780085081264));
#64340=CARTESIAN_POINT('Ctrl Pts',(8.14197021707933,-1.06802494737793,-3.04226495087972));
#64341=CARTESIAN_POINT('Ctrl Pts',(8.14814246517209,-0.972998197045154,
-3.07235936554416));
#64342=CARTESIAN_POINT('Ctrl Pts',(8.15430635382472,-0.87810014705278,-3.10241302156539));
#64343=CARTESIAN_POINT('Ctrl Pts',(8.16047024247735,-0.781673089943199,
-3.12810862511497));
#64344=CARTESIAN_POINT('Ctrl Pts',(8.16663413112998,-0.68415377052273,-3.14929375904814));
#64345=CARTESIAN_POINT('Ctrl Pts',(8.17279149278853,-0.586737715138465,
-3.17045645986292));
#64346=CARTESIAN_POINT('Ctrl Pts',(8.17894885444708,-0.488232119018895,
-3.18711809484292));
#64347=CARTESIAN_POINT('Ctrl Pts',(8.18510621610563,-0.38908881109783,-3.19917605948445));
#64348=CARTESIAN_POINT('Ctrl Pts',(8.19125908025193,-0.290017920271235,
-3.21122521664536));
#64349=CARTESIAN_POINT('Ctrl Pts',(8.19741194439824,-0.190310673636845,
-3.21867733671003));
#64350=CARTESIAN_POINT('Ctrl Pts',(8.20356480854455,-0.0904281080926534,
-3.22148107549413));
#64351=CARTESIAN_POINT('Ctrl Pts',(8.20971534168108,0.00941661698724765,
-3.22428375208307));
#64352=CARTESIAN_POINT('Ctrl Pts',(8.21586587481762,0.109436095279572,-3.22244153438794));
#64353=CARTESIAN_POINT('Ctrl Pts',(8.22201640795416,0.209166055687512,-3.21595508731825));
#64354=CARTESIAN_POINT('Ctrl Pts',(8.22816625616937,0.30888491020014,-3.20946936257715));
#64355=CARTESIAN_POINT('Ctrl Pts',(8.23431610438458,0.408313877467575,-3.19834046488288));
#64356=CARTESIAN_POINT('Ctrl Pts',(8.24046595259978,0.506991590372671,-3.18262110371175));
#64357=CARTESIAN_POINT('Ctrl Pts',(8.24661676097892,0.605684709638605,-3.16689928830711));
#64358=CARTESIAN_POINT('Ctrl Pts',(8.25276756935806,0.703625912563291,-3.14658565421469));
#64359=CARTESIAN_POINT('Ctrl Pts',(8.2589183777372,0.800362833824376,-3.12178424890841));
#64360=CARTESIAN_POINT('Ctrl Pts',(8.26507576410339,0.897203210464985,-3.09695631971894));
#64361=CARTESIAN_POINT('Ctrl Pts',(8.27123315046958,0.992836312011732,-3.06763114339496));
#64362=CARTESIAN_POINT('Ctrl Pts',(8.27739053683577,1.08682390024517,-3.03396298137533));
#64363=CARTESIAN_POINT('Ctrl Pts',(8.28355135957273,1.1808639419356,-3.00027602951843));
#64364=CARTESIAN_POINT('Ctrl Pts',(8.28971218230969,1.27325623976038,-2.96224143041404));
#64365=CARTESIAN_POINT('Ctrl Pts',(8.29587300504664,1.36358349365661,-2.92006123537285));
#64366=CARTESIAN_POINT('Ctrl Pts',(8.30204412796333,1.45406176422536,-2.87781051994688));
#64367=CARTESIAN_POINT('Ctrl Pts',(8.30821525088002,1.5424677097967,-2.83140056621136));
#64368=CARTESIAN_POINT('Ctrl Pts',(8.31438637379671,1.62840942244908,-2.78107898402384));
#64369=CARTESIAN_POINT('Ctrl Pts',(8.31908189574229,1.69380128115092,-2.74278998918649));
#64370=CARTESIAN_POINT('Ctrl Pts',(8.32377741768787,1.75776700488079,-2.702237309696));
#64371=CARTESIAN_POINT('Ctrl Pts',(8.32847293963344,1.82014649547395,-2.65954588182153));
#64372=CARTESIAN_POINT('Ctrl Pts',(8.33464518772621,1.90214412988047,-2.60342814084842));
#64373=CARTESIAN_POINT('Ctrl Pts',(8.34081743581898,1.98168837106901,-2.54341591556368));
#64374=CARTESIAN_POINT('Ctrl Pts',(8.34698968391174,2.05838599785357,-2.47975092425436));
#64375=CARTESIAN_POINT('Ctrl Pts',(8.35315357256437,2.13497974851229,-2.41617215820293));
#64376=CARTESIAN_POINT('Ctrl Pts',(8.359317461217,2.20873421638767,-2.34895073414032));
#64377=CARTESIAN_POINT('Ctrl Pts',(8.36548134986963,2.27928503443018,-2.27837163218001));
#64378=CARTESIAN_POINT('Ctrl Pts',(8.37163871152817,2.34976114561178,-2.2078672670307));
#64379=CARTESIAN_POINT('Ctrl Pts',(8.37779607318672,2.41704004592167,-2.13401259811834));
#64380=CARTESIAN_POINT('Ctrl Pts',(8.38395343484526,2.48079111500584,-2.05713222866399));
#64381=CARTESIAN_POINT('Ctrl Pts',(8.39010629899157,2.54449561849438,-1.98030801482001));
#64382=CARTESIAN_POINT('Ctrl Pts',(8.39625916313787,2.60467713750001,-1.90046282777002));
#64383=CARTESIAN_POINT('Ctrl Pts',(8.40241202728418,2.66104319346577,-1.81795673353617));
#64384=CARTESIAN_POINT('Ctrl Pts',(8.40856256042071,2.71738789517699,-1.7354818966984));
#64385=CARTESIAN_POINT('Ctrl Pts',(8.41471309355725,2.76991976126253,-1.65034851400117));
#64386=CARTESIAN_POINT('Ctrl Pts',(8.42086362669379,2.81838831491438,-1.56294749395304));
#64387=CARTESIAN_POINT('Ctrl Pts',(8.427013474909,2.86685147112417,-1.47555620685351));
#64388=CARTESIAN_POINT('Ctrl Pts',(8.43316332312421,2.91125200385418,-1.38589816433056));
#64389=CARTESIAN_POINT('Ctrl Pts',(8.43931317133941,2.9513847868615,-1.29438997306936));
#64390=CARTESIAN_POINT('Ctrl Pts',(8.44546397971855,2.99152383572274,-1.20286749481093));
#64391=CARTESIAN_POINT('Ctrl Pts',(8.45161478809768,3.02739363690701,-1.1094946919004));
#64392=CARTESIAN_POINT('Ctrl Pts',(8.45776559647682,3.05883711751518,-1.01470835761388));
#64393=CARTESIAN_POINT('Ctrl Pts',(8.46392298284301,3.09031422537939,-0.91982065400463));
#64394=CARTESIAN_POINT('Ctrl Pts',(8.4700803692092,3.11735542286021,-0.82351681339229));
#64395=CARTESIAN_POINT('Ctrl Pts',(8.47623775557539,3.13985351616262,-0.72624889641308));
#64396=CARTESIAN_POINT('Ctrl Pts',(8.48239857831235,3.16236416540771,-0.628926695260844));
#64397=CARTESIAN_POINT('Ctrl Pts',(8.4885594010493,3.18032658305296,-0.530639773553441));
#64398=CARTESIAN_POINT('Ctrl Pts',(8.49472022378626,3.19368509804519,-0.431848419036193));
#64399=CARTESIAN_POINT('Ctrl Pts',(8.50089134670295,3.20706594692224,-0.332891896853729));
#64400=CARTESIAN_POINT('Ctrl Pts',(8.50706246961964,3.21582748011222,-0.233429690190807));
#64401=CARTESIAN_POINT('Ctrl Pts',(8.51323359253633,3.21996608060853,-0.133925360669872));
#64402=CARTESIAN_POINT('Ctrl Pts',(8.51792911448191,3.22311508439872,-0.0582138946606126));
#64403=CARTESIAN_POINT('Ctrl Pts',(8.52262463642749,3.22358873069806,0.0175218913677458));
#64404=CARTESIAN_POINT('Ctrl Pts',(8.52732015837307,3.22140555029293,0.0930797670919089));
#64405=CARTESIAN_POINT('Ctrl Pts',(8.53349260195626,3.21853567596613,0.192403490967159));
#64406=CARTESIAN_POINT('Ctrl Pts',(8.53966504553945,3.21106286005284,0.291769188819021));
#64407=CARTESIAN_POINT('Ctrl Pts',(8.54583748912264,3.19897781935079,0.390715336020603));
#64408=CARTESIAN_POINT('Ctrl Pts',(8.55200152301338,3.18690924400386,0.489526673295419));
#64409=CARTESIAN_POINT('Ctrl Pts',(8.55816555690411,3.17024098656387,0.587919168678262));
#64410=CARTESIAN_POINT('Ctrl Pts',(8.56432959079485,3.14901576313197,0.68543218924002));
#64411=CARTESIAN_POINT('Ctrl Pts',(8.5706872032214,3.12712397171115,0.786007559567762));
#64412=CARTESIAN_POINT('Ctrl Pts',(8.57704481564794,3.10038424253534,0.885646832468236));
#64413=CARTESIAN_POINT('Ctrl Pts',(8.58340242807449,3.06890128795359,0.983850825733655));
#64414=CARTESIAN_POINT('Ctrl Pts',(8.5895550653343,3.03843337226252,1.07888863355971));
#64415=CARTESIAN_POINT('Ctrl Pts',(8.5957077025941,3.00352353248956,1.17258184148595));
#64416=CARTESIAN_POINT('Ctrl Pts',(8.60186033985391,2.96431812219575,1.26449026604472));
#64417=CARTESIAN_POINT('Ctrl Pts',(8.60801062858697,2.92512767702192,1.35636360818526));
#64418=CARTESIAN_POINT('Ctrl Pts',(8.61416091732003,2.88164509029373,1.44645312187698));
#64419=CARTESIAN_POINT('Ctrl Pts',(8.62031120605309,2.83406528913763,1.53433747898083));
#64420=CARTESIAN_POINT('Ctrl Pts',(8.62646079228314,2.78649092267814,1.62221179769012));
#64421=CARTESIAN_POINT('Ctrl Pts',(8.63261037851319,2.73482047968976,1.70788107903586));
#64422=CARTESIAN_POINT('Ctrl Pts',(8.63875996474324,2.67929491867307,1.79094843624061));
#64423=CARTESIAN_POINT('Ctrl Pts',(8.64491049345735,2.62376084782272,1.87402852432784));
#64424=CARTESIAN_POINT('Ctrl Pts',(8.65106102217145,2.56437072741458,1.95450553560679));
#64425=CARTESIAN_POINT('Ctrl Pts',(8.65721155088556,2.50140834880026,2.03201226252509));
#64426=CARTESIAN_POINT('Ctrl Pts',(8.66336781025768,2.4383873059839,2.10959120511231));
#64427=CARTESIAN_POINT('Ctrl Pts',(8.66952406962979,2.37178763653722,2.18419400263338));
#64428=CARTESIAN_POINT('Ctrl Pts',(8.6756803290019,2.30193266163687,2.25548743818036));
#64429=CARTESIAN_POINT('Ctrl Pts',(8.6818400435129,2.23203848133186,2.32682088645363));
#64430=CARTESIAN_POINT('Ctrl Pts',(8.6879997580239,2.15888567516763,2.39484097870944));
#64431=CARTESIAN_POINT('Ctrl Pts',(8.69415947253489,2.08283216097789,2.45925349480207));
#64432=CARTESIAN_POINT('Ctrl Pts',(8.70032745329708,2.00667658402995,2.52375245159536));
#64433=CARTESIAN_POINT('Ctrl Pts',(8.70649543405928,1.92761287423558,2.58463390673216));
#64434=CARTESIAN_POINT('Ctrl Pts',(8.71266341482147,1.84602926593963,2.64164598532703));
#64435=CARTESIAN_POINT('Ctrl Pts',(8.71407970622497,1.82729604228813,2.65473709567949));
#64436=CARTESIAN_POINT('Ctrl Pts',(8.71549599762847,1.80843006291833,2.66762438097374));
#64437=CARTESIAN_POINT('Ctrl Pts',(8.71691228903198,1.78943621037803,2.68030513402633));
#64438=CARTESIAN_POINT('Ctrl Pts',(7.46680874532643,1.78773599488645,2.67780888195817));
#64439=CARTESIAN_POINT('Ctrl Pts',(7.48890051844257,1.49107844583294,2.87932143490233));
#64440=CARTESIAN_POINT('Ctrl Pts',(7.57727469780527,0.178346421750044,3.49141846844679));
#64441=CARTESIAN_POINT('Ctrl Pts',(7.72052921189373,-2.37587491464765,2.8569912360958));
#64442=CARTESIAN_POINT('Ctrl Pts',(7.84169195286606,-3.21676692519514,0.884675566243836));
#64443=CARTESIAN_POINT('Ctrl Pts',(7.89657228759183,-3.22473260027238,-0.00267998977119858));
#64444=CARTESIAN_POINT('Ctrl Pts',(7.21834907457188,1.78943621037019,2.68030513403157));
#64445=CARTESIAN_POINT('Ctrl Pts',(7.22270752708506,1.72648891861646,2.72233026086458));
#64446=CARTESIAN_POINT('Ctrl Pts',(7.22712570793226,1.66208432132251,2.76212247942874));
#64447=CARTESIAN_POINT('Ctrl Pts',(7.23434679459875,1.55653469802985,2.8223070531524));
#64448=CARTESIAN_POINT('Ctrl Pts',(7.23709827465172,1.51624967549766,2.84415259211747));
#64449=CARTESIAN_POINT('Ctrl Pts',(7.2406712221416,1.46393554127367,2.87109385277185));
#64450=CARTESIAN_POINT('Ctrl Pts',(7.24146444832933,1.45232109917454,2.87698637423482));
#64451=CARTESIAN_POINT('Ctrl Pts',(7.242747333946,1.43353858973617,2.88637285487775));
#64452=CARTESIAN_POINT('Ctrl Pts',(7.24323544218663,1.42639263486401,2.88991093202463));
#64453=CARTESIAN_POINT('Ctrl Pts',(7.24416788331957,1.41274275071359,2.89660624724723));
#64454=CARTESIAN_POINT('Ctrl Pts',(7.24461204807172,1.4062411754839,2.89976819527053));
#64455=CARTESIAN_POINT('Ctrl Pts',(7.24562847364143,1.39136450800361,2.90694145125416));
#64456=CARTESIAN_POINT('Ctrl Pts',(7.24620122725826,1.38298263633295,2.91093847751239));
#64457=CARTESIAN_POINT('Ctrl Pts',(7.24796238515516,1.35721364019772,2.9230904042695));
#64458=CARTESIAN_POINT('Ctrl Pts',(7.24915490299827,1.339771044767,2.9311260461726));
#64459=CARTESIAN_POINT('Ctrl Pts',(7.26636363369988,1.08818779358593,3.04431331168145));
#64460=CARTESIAN_POINT('Ctrl Pts',(7.28339245695585,0.842425806593474,3.12125955627945));
#64461=CARTESIAN_POINT('Ctrl Pts',(7.31480604515554,0.385788925354882,3.20632482919754));
#64462=CARTESIAN_POINT('Ctrl Pts',(7.32897325131086,0.178154020570992,3.22453532280229));
#64463=CARTESIAN_POINT('Ctrl Pts',(7.34396457217594,-0.0560925156146685,
3.22236907424466));
#64464=CARTESIAN_POINT('Ctrl Pts',(7.34563235886566,-0.082380248798944,
3.22180421839427));
#64465=CARTESIAN_POINT('Ctrl Pts',(7.3477443166181,-0.116002420128938,3.22066995927508));
#64466=CARTESIAN_POINT('Ctrl Pts',(7.34820424156187,-0.123344945932712,
3.22039711446887));
#64467=CARTESIAN_POINT('Ctrl Pts',(7.34894106001226,-0.1351422229402,3.21991832624934));
#64468=CARTESIAN_POINT('Ctrl Pts',(7.34921883227003,-0.139597538732707,
3.219728245659));
#64469=CARTESIAN_POINT('Ctrl Pts',(7.34974839061793,-0.148106734812386,
3.21934751580332));
#64470=CARTESIAN_POINT('Ctrl Pts',(7.35000026191529,-0.152160637404317,
3.21915845726415));
#64471=CARTESIAN_POINT('Ctrl Pts',(7.35058027282254,-0.161511244223582,
3.21870467816941));
#64472=CARTESIAN_POINT('Ctrl Pts',(7.35090810714367,-0.166807692851852,
3.21843453900193));
#64473=CARTESIAN_POINT('Ctrl Pts',(7.35178606111625,-0.181021241547621,
3.21767441271638));
#64474=CARTESIAN_POINT('Ctrl Pts',(7.35233485704669,-0.18993708945039,3.21716042848042));
#64475=CARTESIAN_POINT('Ctrl Pts',(7.35629992751171,-0.254569196113896,
3.21316487132701));
#64476=CARTESIAN_POINT('Ctrl Pts',(7.35964110389463,-0.310192698922484,
3.20827295343363));
#64477=CARTESIAN_POINT('Ctrl Pts',(7.36388001593474,-0.381759299429711,
3.20009996864341));
#64478=CARTESIAN_POINT('Ctrl Pts',(7.36482855264889,-0.397839923285166,
3.19814061361746));
#64479=CARTESIAN_POINT('Ctrl Pts',(7.36758259199126,-0.444693921748337,
3.19207279257889));
#64480=CARTESIAN_POINT('Ctrl Pts',(7.36937665827904,-0.475424082876621,
3.1876407323286));
#64481=CARTESIAN_POINT('Ctrl Pts',(7.37940064766516,-0.647903425998109,
3.1602150804739));
#64482=CARTESIAN_POINT('Ctrl Pts',(7.38737871077107,-0.788061880049574,
3.1282104714415));
#64483=CARTESIAN_POINT('Ctrl Pts',(7.4087114387015,-1.15352247208885,3.01862732089911));
#64484=CARTESIAN_POINT('Ctrl Pts',(7.4221429349017,-1.3731169717395,2.92527821812058));
#64485=CARTESIAN_POINT('Ctrl Pts',(7.43772508804782,-1.59807114336533,2.79869542911663));
#64486=CARTESIAN_POINT('Ctrl Pts',(7.43895311889632,-1.61562169637333,2.78860072249558));
#64487=CARTESIAN_POINT('Ctrl Pts',(7.44076542579327,-1.64125529643807,2.7735336011334));
#64488=CARTESIAN_POINT('Ctrl Pts',(7.44134503125993,-1.64941358763059,2.76868965371863));
#64489=CARTESIAN_POINT('Ctrl Pts',(7.44237026776526,-1.66377365981172,2.76007743226706));
#64490=CARTESIAN_POINT('Ctrl Pts',(7.44281535011461,-1.66998435330849,2.75632408862421));
#64491=CARTESIAN_POINT('Ctrl Pts',(7.44368572440453,-1.68208365884651,2.74895614152154));
#64492=CARTESIAN_POINT('Ctrl Pts',(7.44411094202572,-1.68797343135774,2.74534351169583));
#64493=CARTESIAN_POINT('Ctrl Pts',(7.44513599471266,-1.70212015086395,2.73660355571567));
#64494=CARTESIAN_POINT('Ctrl Pts',(7.44573650945716,-1.71036557188482,2.73145778593083));
#64495=CARTESIAN_POINT('Ctrl Pts',(7.44794320959085,-1.74050901352501,2.71245598106358));
#64496=CARTESIAN_POINT('Ctrl Pts',(7.4495577912694,-1.76226250376938,2.69837356196476));
#64497=CARTESIAN_POINT('Ctrl Pts',(7.45182879486827,-1.79243385255415,2.6783212730013));
#64498=CARTESIAN_POINT('Ctrl Pts',(7.45247694652471,-1.80099685848298,2.67257072290762));
#64499=CARTESIAN_POINT('Ctrl Pts',(7.46932952229248,-2.02239549025275,2.52234159511696));
#64500=CARTESIAN_POINT('Ctrl Pts',(7.48654117351857,-2.21715924931966,2.35296506792326));
#64501=CARTESIAN_POINT('Ctrl Pts',(7.51666749577766,-2.51578605915985,2.02293344967028));
#64502=CARTESIAN_POINT('Ctrl Pts',(7.5294015190845,-2.6294647486432,1.87279693867572));
#64503=CARTESIAN_POINT('Ctrl Pts',(7.54301924288254,-2.74272515668253,1.69239558152509));
#64504=CARTESIAN_POINT('Ctrl Pts',(7.54460594958143,-2.75578740826049,1.67104157396195));
#64505=CARTESIAN_POINT('Ctrl Pts',(7.54663030078882,-2.77229541433005,1.64333436165265));
#64506=CARTESIAN_POINT('Ctrl Pts',(7.54708216675351,-2.77597001345854,1.63711947495283));
#64507=CARTESIAN_POINT('Ctrl Pts',(7.54780916399143,-2.78186596359057,1.62707066686433));
#64508=CARTESIAN_POINT('Ctrl Pts',(7.54808513316946,-2.78410032191038,1.62324446478614));
#64509=CARTESIAN_POINT('Ctrl Pts',(7.54861345297472,-2.78837075005443,1.61589686187077));
#64510=CARTESIAN_POINT('Ctrl Pts',(7.54886588036278,-2.79040803900595,1.61237622283212));
#64511=CARTESIAN_POINT('Ctrl Pts',(7.54945013220286,-2.79511609391671,1.60420458435597));
#64512=CARTESIAN_POINT('Ctrl Pts',(7.54978163678369,-2.79778193752195,1.59955073630183));
#64513=CARTESIAN_POINT('Ctrl Pts',(7.55085275697486,-2.80637705568191,1.58445873837941));
#64514=CARTESIAN_POINT('Ctrl Pts',(7.55158941752886,-2.81225971487244,1.57399395772257));
#64515=CARTESIAN_POINT('Ctrl Pts',(7.56110271878308,-2.88782989607416,1.43778442494053));
#64516=CARTESIAN_POINT('Ctrl Pts',(7.56937603927794,-2.94909592709333,1.30752823497906));
#64517=CARTESIAN_POINT('Ctrl Pts',(7.57974609714761,-3.01594038878124,1.13657448266298));
#64518=CARTESIAN_POINT('Ctrl Pts',(7.58197942455634,-3.02973129467388,1.09928447119959));
#64519=CARTESIAN_POINT('Ctrl Pts',(7.59357586053911,-3.09791659065456,0.903874532714543));
#64520=CARTESIAN_POINT('Ctrl Pts',(7.60283908487744,-3.14063237330092,0.741958632983487));
#64521=CARTESIAN_POINT('Ctrl Pts',(7.61754121784672,-3.18671880527437,0.488918089834536));
#64522=CARTESIAN_POINT('Ctrl Pts',(7.62276108635313,-3.19912812791481,0.399743609464253));
#64523=CARTESIAN_POINT('Ctrl Pts',(7.63115261927296,-3.21275994624103,0.258763558664508));
#64524=CARTESIAN_POINT('Ctrl Pts',(7.63424774807744,-3.21649401203621,0.207245902521712));
#64525=CARTESIAN_POINT('Ctrl Pts',(7.63820568676686,-3.2196440883069,0.142104749163024));
#64526=CARTESIAN_POINT('Ctrl Pts',(7.63903211384361,-3.22021405487645,0.128542783039022));
#64527=CARTESIAN_POINT('Ctrl Pts',(7.64035578381674,-3.22098717899455,0.106886428842214));
#64528=CARTESIAN_POINT('Ctrl Pts',(7.64085129074333,-3.22124554242144,0.0987940760160971));
#64529=CARTESIAN_POINT('Ctrl Pts',(7.64178959254758,-3.22167619797546,0.0834982463755718));
#64530=CARTESIAN_POINT('Ctrl Pts',(7.64223218538996,-3.22185483152836,0.0762949864943477));
#64531=CARTESIAN_POINT('Ctrl Pts',(7.6432337200344,-3.22220378767923,0.0600217215070409));
#64532=CARTESIAN_POINT('Ctrl Pts',(7.64379310228614,-3.2223599733766,0.0509515031461113));
#64533=CARTESIAN_POINT('Ctrl Pts',(7.64522977226866,-3.22266209169762,0.0277053106459614));
#64534=CARTESIAN_POINT('Ctrl Pts',(7.64610878618116,-3.22275278284227,0.0135289262543614));
#64535=CARTESIAN_POINT('Ctrl Pts',(7.65220990883545,-3.22273308219942,-0.0845383608562378));
#64536=CARTESIAN_POINT('Ctrl Pts',(7.6575312104897,-3.2194406456586,-0.168389637158447));
#64537=CARTESIAN_POINT('Ctrl Pts',(7.67504296064636,-3.19823618548505,-0.438724581475063));
#64538=CARTESIAN_POINT('Ctrl Pts',(7.68760645982744,-3.16734462500883,-0.623783053174723));
#64539=CARTESIAN_POINT('Ctrl Pts',(7.71400303989104,-3.06988932484729,-1.00152525256368));
#64540=CARTESIAN_POINT('Ctrl Pts',(7.72779509991838,-3.00077010396966,-1.19275638655029));
#64541=CARTESIAN_POINT('Ctrl Pts',(7.74218279297676,-2.90450098161446,-1.39660270344779));
#64542=CARTESIAN_POINT('Ctrl Pts',(7.74360945166138,-2.8946671433494,-1.4168723514056));
#64543=CARTESIAN_POINT('Ctrl Pts',(7.74547683978982,-2.88140089693966,-1.44350219663691));
#64544=CARTESIAN_POINT('Ctrl Pts',(7.74592884596621,-2.87815879463476,-1.44995574961309));
#64545=CARTESIAN_POINT('Ctrl Pts',(7.74662845224725,-2.87309205126529,-1.45995737752749));
#64546=CARTESIAN_POINT('Ctrl Pts',(7.7468769871049,-2.87128249500649,-1.46351300422069));
#64547=CARTESIAN_POINT('Ctrl Pts',(7.74735068042781,-2.86781513221406,-1.47029489790246));
#64548=CARTESIAN_POINT('Ctrl Pts',(7.74757590620517,-2.86615849890056,-1.47352169265097));
#64549=CARTESIAN_POINT('Ctrl Pts',(7.74810904511639,-2.86221805367737,-1.48116511485671));
#64550=CARTESIAN_POINT('Ctrl Pts',(7.74841665244911,-2.85992946946638,-1.4855792522561));
#64551=CARTESIAN_POINT('Ctrl Pts',(7.74932304378566,-2.85314181685436,-1.49859721131012));
#64552=CARTESIAN_POINT('Ctrl Pts',(7.74992003611143,-2.84861402411091,-1.50718611197421));
#64553=CARTESIAN_POINT('Ctrl Pts',(7.75467735501518,-2.81208203248767,-1.57573198345415));
#64554=CARTESIAN_POINT('Ctrl Pts',(7.75872544100792,-2.77822464329277,-1.63468835572986));
#64555=CARTESIAN_POINT('Ctrl Pts',(7.76911074259544,-2.68489030338494,-1.78592413821137));
#64556=CARTESIAN_POINT('Ctrl Pts',(7.77532039022041,-2.62251862462263,-1.8763156318332));
#64557=CARTESIAN_POINT('Ctrl Pts',(7.79778594579357,-2.37860363324139,-2.19381416530985));
#64558=CARTESIAN_POINT('Ctrl Pts',(7.81376844982143,-2.17122107756117,-2.39924142148023));
#64559=CARTESIAN_POINT('Ctrl Pts',(7.83221571778979,-1.92521365419544,-2.58456438404546));
#64560=CARTESIAN_POINT('Ctrl Pts',(7.83326266245454,-1.91122343905189,-2.59492690026823));
#64561=CARTESIAN_POINT('Ctrl Pts',(7.83539163323463,-1.88272327787785,-2.61568138959773));
#64562=CARTESIAN_POINT('Ctrl Pts',(7.83647384194945,-1.86820961477891,-2.62606719038239));
#64563=CARTESIAN_POINT('Ctrl Pts',(7.83811753888044,-1.84613069399354,-2.64159092821861));
#64564=CARTESIAN_POINT('Ctrl Pts',(7.83867560323731,-1.83862844166152,-2.64681820723603));
#64565=CARTESIAN_POINT('Ctrl Pts',(7.83964831225718,-1.82554208631229,-2.65585378699152));
#64566=CARTESIAN_POINT('Ctrl Pts',(7.84006240116454,-1.81996803353047,-2.65967659737022));
#64567=CARTESIAN_POINT('Ctrl Pts',(7.84092790106714,-1.8083113601468,-2.6676172029867));
#64568=CARTESIAN_POINT('Ctrl Pts',(7.84137943041316,-1.80222661083344,-2.67173179018521));
#64569=CARTESIAN_POINT('Ctrl Pts',(7.84244979749895,-1.78779463378079,-2.68141914698121));
#64570=CARTESIAN_POINT('Ctrl Pts',(7.84306931489334,-1.77943537162435,-2.68697377153767));
#64571=CARTESIAN_POINT('Ctrl Pts',(7.84512867852354,-1.75162881239101,-2.70526421333121));
#64572=CARTESIAN_POINT('Ctrl Pts',(7.84657492258486,-1.73207001980036,-2.71782842747284));
#64573=CARTESIAN_POINT('Ctrl Pts',(7.86125885491315,-1.53321556647318,-2.84255057561658));
#64574=CARTESIAN_POINT('Ctrl Pts',(7.87515985370853,-1.34346252634109,-2.93699193180482));
#64575=CARTESIAN_POINT('Ctrl Pts',(7.89891384783124,-1.01367689469022,-3.06244653104838));
#64576=CARTESIAN_POINT('Ctrl Pts',(7.90854442742319,-0.878324532900173,
-3.10397574460313));
#64577=CARTESIAN_POINT('Ctrl Pts',(7.92257474510199,-0.674750275792142,
-3.15204998618005));
#64578=CARTESIAN_POINT('Ctrl Pts',(7.92708076162079,-0.608339768478786,
-3.1655379889609));
#64579=CARTESIAN_POINT('Ctrl Pts',(7.93538218785758,-0.483244892185699,
-3.18686212858442));
#64580=CARTESIAN_POINT('Ctrl Pts',(7.93919359632799,-0.424672437409031,
-3.19519486756528));
#64581=CARTESIAN_POINT('Ctrl Pts',(7.94354923417066,-0.355997838730246,
-3.20304268251034));
#64582=CARTESIAN_POINT('Ctrl Pts',(7.94417484120883,-0.346090755795727,
-3.20412828739532));
#64583=CARTESIAN_POINT('Ctrl Pts',(7.9451162831124,-0.331113954737074,-3.20569915069122));
#64584=CARTESIAN_POINT('Ctrl Pts',(7.94543398734691,-0.326047972262028,
-3.2062183669239));
#64585=CARTESIAN_POINT('Ctrl Pts',(7.94600142585887,-0.316978200581188,
-3.20712621573901));
#64586=CARTESIAN_POINT('Ctrl Pts',(7.9462514124226,-0.312974910094125,-3.20751936074983));
#64587=CARTESIAN_POINT('Ctrl Pts',(7.94678842735814,-0.304358736245893,
-3.20834923143567));
#64588=CARTESIAN_POINT('Ctrl Pts',(7.94707531537645,-0.299745661070816,
-3.20878350321358));
#64589=CARTESIAN_POINT('Ctrl Pts',(7.94786402773044,-0.287036210177492,
-3.20995231532249));
#64590=CARTESIAN_POINT('Ctrl Pts',(7.94836469671031,-0.278937898661748,
-3.21066617770283));
#64591=CARTESIAN_POINT('Ctrl Pts',(7.95104403753049,-0.23544231261744,-3.21433448249454));
#64592=CARTESIAN_POINT('Ctrl Pts',(7.95319279001972,-0.199999078006694,
-3.21673434779658));
#64593=CARTESIAN_POINT('Ctrl Pts',(7.95944714467249,-0.0954702002396502,
-3.22207752418574));
#64594=CARTESIAN_POINT('Ctrl Pts',(7.9634786461395,-0.0263181613410355,
-3.2233843685004));
#64595=CARTESIAN_POINT('Ctrl Pts',(7.98087270299436,0.276513093002135,-3.21935971904321));
#64596=CARTESIAN_POINT('Ctrl Pts',(7.99360517135268,0.509175480666166,-3.19084444158489));
#64597=CARTESIAN_POINT('Ctrl Pts',(8.01544678785245,0.883335987896204,-3.10298522450987));
#64598=CARTESIAN_POINT('Ctrl Pts',(8.02419495284562,1.02734211337299,-3.05832618779181));
#64599=CARTESIAN_POINT('Ctrl Pts',(8.03446039186819,1.18573573371273,-2.99675212621991));
#64600=CARTESIAN_POINT('Ctrl Pts',(8.03563542747638,1.20372028013837,-2.98957354785839));
#64601=CARTESIAN_POINT('Ctrl Pts',(8.03738396599581,1.23026085342746,-2.97870149737942));
#64602=CARTESIAN_POINT('Ctrl Pts',(8.03795326127324,1.23886753363927,-2.97513220028749));
#64603=CARTESIAN_POINT('Ctrl Pts',(8.03896679114146,1.25412832149066,-2.96872565954965));
#64604=CARTESIAN_POINT('Ctrl Pts',(8.03941051899496,1.26078860947899,-2.96590322992612));
#64605=CARTESIAN_POINT('Ctrl Pts',(8.04034399781915,1.2747556767722,-2.95992885904588));
#64606=CARTESIAN_POINT('Ctrl Pts',(8.04083390651544,1.28206038835007,-2.95677223419126));
#64607=CARTESIAN_POINT('Ctrl Pts',(8.04212356929794,1.30122228321234,-2.9484073414143));
#64608=CARTESIAN_POINT('Ctrl Pts',(8.04292484281843,1.31305980335427,-2.94315463850966));
#64609=CARTESIAN_POINT('Ctrl Pts',(8.04652762976241,1.36597813536117,-2.91929020866937));
#64610=CARTESIAN_POINT('Ctrl Pts',(8.04935623574506,1.40669555042735,-2.89988946068429));
#64611=CARTESIAN_POINT('Ctrl Pts',(8.0569463639148,1.51371440293524,-2.84611356417834));
#64612=CARTESIAN_POINT('Ctrl Pts',(8.06175707318743,1.57924780534192,-2.81027910631698));
#64613=CARTESIAN_POINT('Ctrl Pts',(8.0865696889267,1.90583122703549,-2.61666731688652));
#64614=CARTESIAN_POINT('Ctrl Pts',(8.10772226585456,2.14473463461321,-2.42470856356327));
#64615=CARTESIAN_POINT('Ctrl Pts',(8.12866537074368,2.3621339315205,-2.19239962717325));
#64616=CARTESIAN_POINT('Ctrl Pts',(8.12953423746365,2.37112050556997,-2.18267734518999));
#64617=CARTESIAN_POINT('Ctrl Pts',(8.13425672408314,2.41979877218243,-2.12935847504616));
#64618=CARTESIAN_POINT('Ctrl Pts',(8.1380556964434,2.45835130896937,-2.0847310411057));
#64619=CARTESIAN_POINT('Ctrl Pts',(8.14239880609919,2.50195997198617,-2.03135742642959));
#64620=CARTESIAN_POINT('Ctrl Pts',(8.1430238032365,2.5082239172878,-2.0236179190327));
#64621=CARTESIAN_POINT('Ctrl Pts',(8.14396450901897,2.51763606645736,-2.01187775760692));
#64622=CARTESIAN_POINT('Ctrl Pts',(8.14428208274589,2.52081075441575,-2.00789855718698));
#64623=CARTESIAN_POINT('Ctrl Pts',(8.14484937945983,2.52647713959923,-2.00076160623584));
#64624=CARTESIAN_POINT('Ctrl Pts',(8.14509935420658,2.52897235580575,-1.99760670956104));
#64625=CARTESIAN_POINT('Ctrl Pts',(8.1456364456459,2.53433006029252,-1.99080641701001));
#64626=CARTESIAN_POINT('Ctrl Pts',(8.14592342159382,2.53719058263645,-1.98715952870808));
#64627=CARTESIAN_POINT('Ctrl Pts',(8.14671262186991,2.54505077302131,-1.97709390806203));
#64628=CARTESIAN_POINT('Ctrl Pts',(8.14721368847115,2.55003405928935,-1.97066234002228));
#64629=CARTESIAN_POINT('Ctrl Pts',(8.14989890865197,2.57669663283906,-1.93598039497329));
#64630=CARTESIAN_POINT('Ctrl Pts',(8.15205298719722,2.59793193104523,-1.90738972379317));
#64631=CARTESIAN_POINT('Ctrl Pts',(8.15832749232466,2.65913933760219,-1.82206241155872));
#64632=CARTESIAN_POINT('Ctrl Pts',(8.16237324929399,2.69775958907222,-1.76437749985757));
#64633=CARTESIAN_POINT('Ctrl Pts',(8.17973042986077,2.85771841028123,-1.50790778402274));
#64634=CARTESIAN_POINT('Ctrl Pts',(8.19241897208323,2.95917509220752,-1.29754939409999));
#64635=CARTESIAN_POINT('Ctrl Pts',(8.21423633109631,3.08762041836164,-0.935705033314829));
#64636=CARTESIAN_POINT('Ctrl Pts',(8.22301093996192,3.12808059903206,-0.789966183615571));
#64637=CARTESIAN_POINT('Ctrl Pts',(8.23330566319194,3.16202789838621,-0.622954609428063));
#64638=CARTESIAN_POINT('Ctrl Pts',(8.23448122518939,3.16571547391526,-0.603935748589158));
#64639=CARTESIAN_POINT('Ctrl Pts',(8.2362303982389,3.17092259661065,-0.575720675520048));
#64640=CARTESIAN_POINT('Ctrl Pts',(8.23679979717346,3.1725741302277,-0.566549022814592));
#64641=CARTESIAN_POINT('Ctrl Pts',(8.23781344390923,3.17543693747565,-0.550245534027593));
#64642=CARTESIAN_POINT('Ctrl Pts',(8.23825718455265,3.17666402775737,-0.543116511440173));
#64643=CARTESIAN_POINT('Ctrl Pts',(8.23919062140869,3.17919040083367,-0.52813754582156));
#64644=CARTESIAN_POINT('Ctrl Pts',(8.23968047509605,3.18048463359583,-0.5202868110051));
#64645=CARTESIAN_POINT('Ctrl Pts',(8.24096983736731,3.18380834860684,-0.499649455315324));
#64646=CARTESIAN_POINT('Ctrl Pts',(8.24177086409802,3.18578986035285,-0.486855354974451));
#64647=CARTESIAN_POINT('Ctrl Pts',(8.24537098411578,3.19432249874531,-0.429478595514511));
#64648=CARTESIAN_POINT('Ctrl Pts',(8.24819712074888,3.20001496834759,-0.384775207446276));
#64649=CARTESIAN_POINT('Ctrl Pts',(8.25577909867849,3.21263625367078,-0.265798766116731));
#64650=CARTESIAN_POINT('Ctrl Pts',(8.26058399714788,3.21792663024815,-0.191383023850869));
#64651=CARTESIAN_POINT('Ctrl Pts',(8.28535563960879,3.23167087840233,0.187420129541721));
#64652=CARTESIAN_POINT('Ctrl Pts',(8.30646911244158,3.19953801753341,0.491667855125711));
#64653=CARTESIAN_POINT('Ctrl Pts',(8.32732401693764,3.12220475326432,0.798816005853322));
#64654=CARTESIAN_POINT('Ctrl Pts',(8.32813348089154,3.11912625778183,0.810753309034786));
#64655=CARTESIAN_POINT('Ctrl Pts',(8.33289547681894,3.1005567195806,0.881087829253506));
#64656=CARTESIAN_POINT('Ctrl Pts',(8.33679078898704,3.08349328818076,0.939062303224461));
#64657=CARTESIAN_POINT('Ctrl Pts',(8.34123026524498,3.06170987306873,1.00605697594325));
#64658=CARTESIAN_POINT('Ctrl Pts',(8.34185935373205,3.05856669159628,1.01557263896808));
#64659=CARTESIAN_POINT('Ctrl Pts',(8.34280499636105,3.05375558950356,1.02991281945204));
#64660=CARTESIAN_POINT('Ctrl Pts',(8.34312344443103,3.05212054441772,1.03474818158688));
#64661=CARTESIAN_POINT('Ctrl Pts',(8.34369169241847,3.04917610173499,1.04338815988678));
#64662=CARTESIAN_POINT('Ctrl Pts',(8.34394174762198,3.0478710653295,1.04719421375755));
#64663=CARTESIAN_POINT('Ctrl Pts',(8.34447833247837,3.04505048285536,1.05537032025078));
#64664=CARTESIAN_POINT('Ctrl Pts',(8.34476472399109,3.04353266147634,1.05973954119427));
#64665=CARTESIAN_POINT('Ctrl Pts',(8.34555068255149,3.03933329498006,1.0717444556795));
#64666=CARTESIAN_POINT('Ctrl Pts',(8.34604910758547,3.03663236414828,1.07937340368117));
#64667=CARTESIAN_POINT('Ctrl Pts',(8.34869554778818,3.02209135181638,1.11995880689307));
#64668=CARTESIAN_POINT('Ctrl Pts',(8.35081450688765,3.00974289594773,1.15273232184558));
#64669=CARTESIAN_POINT('Ctrl Pts',(8.35695661735589,2.97195371437118,1.24827691267065));
#64670=CARTESIAN_POINT('Ctrl Pts',(8.36090879376775,2.94506465179451,1.31045776817446));
#64671=CARTESIAN_POINT('Ctrl Pts',(8.38223417320864,2.78716028414156,1.64615047639399));
#64672=CARTESIAN_POINT('Ctrl Pts',(8.39853242484469,2.62000650643114,1.90096299897209));
#64673=CARTESIAN_POINT('Ctrl Pts',(8.42125583970566,2.36211550142134,2.19411153584632));
#64674=CARTESIAN_POINT('Ctrl Pts',(8.42641767180924,2.30191591544548,2.25718766143644));
#64675=CARTESIAN_POINT('Ctrl Pts',(8.43261442510955,2.22827466976914,2.32833458440022));
#64676=CARTESIAN_POINT('Ctrl Pts',(8.43354026665903,2.21723662900804,2.3388483617885));
#64677=CARTESIAN_POINT('Ctrl Pts',(8.43503615047883,2.19934816541908,2.35564675256177));
#64678=CARTESIAN_POINT('Ctrl Pts',(8.43560406137452,2.19254432902844,2.36198080813105));
#64679=CARTESIAN_POINT('Ctrl Pts',(8.43661726402921,2.18038409009594,2.3732036094462));
#64680=CARTESIAN_POINT('Ctrl Pts',(8.43706205882664,2.17503839012877,2.37810389855715));
#64681=CARTESIAN_POINT('Ctrl Pts',(8.43799246817082,2.163841352113,2.38829864855058));
#64682=CARTESIAN_POINT('Ctrl Pts',(8.43847822120258,2.1579870229891,2.39358973899537));
#64683=CARTESIAN_POINT('Ctrl Pts',(8.43974516870894,2.14269600578364,2.40730792717624));
#64684=CARTESIAN_POINT('Ctrl Pts',(8.44052778648832,2.13322909022716,2.4157009895102));
#64685=CARTESIAN_POINT('Ctrl Pts',(8.4438838856222,2.09254386136987,2.45134554373438));
#64686=CARTESIAN_POINT('Ctrl Pts',(8.44647997823743,2.06085206379877,2.47804828428357));
#64687=CARTESIAN_POINT('Ctrl Pts',(8.45333417366201,1.97665070641126,2.54626176672654));
#64688=CARTESIAN_POINT('Ctrl Pts',(8.457630814468,1.92334955940649,2.58675905927182));
#64689=CARTESIAN_POINT('Ctrl Pts',(8.4640766961298,1.84263371133385,2.64421111819046));
#64690=CARTESIAN_POINT('Ctrl Pts',(8.46618101539425,1.81616623104617,2.66245952977608));
#64691=CARTESIAN_POINT('Ctrl Pts',(8.46829646867762,1.78943615355263,2.68030517196433));
#64692=CARTESIAN_POINT('Origin',(-1.72497344927317,0.,0.));
#64693=CARTESIAN_POINT('',(9.96714565479784,1.78929966408855,2.68008864808371));
#64694=CARTESIAN_POINT('',(9.72309722109888,1.78943620850078,2.68030513527963));
#64695=CARTESIAN_POINT('',(-1.72497344927317,1.78943621037804,2.68030513402633));
#64696=CARTESIAN_POINT('',(9.1465734492731,-3.22274934639606,0.00205251157118864));
#64697=CARTESIAN_POINT('Ctrl Pts',(9.14657521538943,-3.22641437747227,0.00202632845199172));
#64698=CARTESIAN_POINT('Ctrl Pts',(9.20528648803684,-3.21937259504748,-0.945983535466743));
#64699=CARTESIAN_POINT('Ctrl Pts',(9.33028016693079,-2.27611929708021,-2.97641430368825));
#64700=CARTESIAN_POINT('Ctrl Pts',(9.52155625207129,1.17754617868619,-3.6251807319632));
#64701=CARTESIAN_POINT('Ctrl Pts',(9.72040347081094,3.6862456230291,-0.969609998419201));
#64702=CARTESIAN_POINT('Ctrl Pts',(9.8689332717198,3.03086015932743,1.67926548359054));
#64703=CARTESIAN_POINT('Ctrl Pts',(9.9511806663821,2.00582045219481,2.53867724580072));
#64704=CARTESIAN_POINT('Ctrl Pts',(9.96714565479787,1.78929966408823,2.68008864808392));
#64705=CARTESIAN_POINT('Ctrl Pts',(8.71691228903198,1.78943621037803,2.68030513402633));
#64706=CARTESIAN_POINT('Ctrl Pts',(8.71999731839222,1.74806295018164,2.70792691820193));
#64707=CARTESIAN_POINT('Ctrl Pts',(8.72308234775247,1.70608288115806,2.73456856151953));
#64708=CARTESIAN_POINT('Ctrl Pts',(8.72616737711272,1.66354743586698,2.76020424808028));
#64709=CARTESIAN_POINT('Ctrl Pts',(8.73233962520549,1.57844635888673,2.81149381424136));
#64710=CARTESIAN_POINT('Ctrl Pts',(8.73851187329825,1.490821275427,2.85893428471293));
#64711=CARTESIAN_POINT('Ctrl Pts',(8.74468412139102,1.40105536769202,2.90226832308134));
#64712=CARTESIAN_POINT('Ctrl Pts',(8.75084801004365,1.31141103522761,2.94554367160221));
#64713=CARTESIAN_POINT('Ctrl Pts',(8.75701189869628,1.21963202918873,2.98472345510216));
#64714=CARTESIAN_POINT('Ctrl Pts',(8.76317578734891,1.12612890497739,3.01959455090819));
#64715=CARTESIAN_POINT('Ctrl Pts',(8.76933314900746,1.03272479201893,3.05442872141451));
#64716=CARTESIAN_POINT('Ctrl Pts',(8.77549051066601,0.937600595267945,3.08496312397248));
#64717=CARTESIAN_POINT('Ctrl Pts',(8.78164787232456,0.841188901471771,3.11103178938125));
#64718=CARTESIAN_POINT('Ctrl Pts',(8.78780073647087,0.744847629521407,3.13708141349468));
#64719=CARTESIAN_POINT('Ctrl Pts',(8.79395360061718,0.647221148303937,3.1586716726401));
#64720=CARTESIAN_POINT('Ctrl Pts',(8.80010646476349,0.548758466147658,3.17568602168591));
#64721=CARTESIAN_POINT('Ctrl Pts',(8.80625699790003,0.450333086533505,3.19269392485336));
#64722=CARTESIAN_POINT('Ctrl Pts',(8.81240753103656,0.351072563005815,3.2051292886564));
#64723=CARTESIAN_POINT('Ctrl Pts',(8.8185580641731,0.251436519468654,3.21292658477866));
#64724=CARTESIAN_POINT('Ctrl Pts',(8.82470791238831,0.151811571368268,3.22072301259662));
#64725=CARTESIAN_POINT('Ctrl Pts',(8.83085776060352,0.0518116194499468,
3.22388236570905));
#64726=CARTESIAN_POINT('Ctrl Pts',(8.83700760881872,-0.0480991672336635,
3.22239104278352));
#64727=CARTESIAN_POINT('Ctrl Pts',(8.84315841719786,-0.148025552795578,
3.22089948702061));
#64728=CARTESIAN_POINT('Ctrl Pts',(8.849309225577,-0.247862311103922,3.21475581947906));
#64729=CARTESIAN_POINT('Ctrl Pts',(8.85546003395614,-0.347146864219039,
3.20399853576166));
#64730=CARTESIAN_POINT('Ctrl Pts',(8.86161742032233,-0.446537597280619,
3.19322974765841));
#64731=CARTESIAN_POINT('Ctrl Pts',(8.86777480668852,-0.545374513179239,
3.17783753750097));
#64732=CARTESIAN_POINT('Ctrl Pts',(8.87393219305471,-0.643201858289325,
3.15791211593882));
#64733=CARTESIAN_POINT('Ctrl Pts',(8.88009301579167,-0.741083799783258,
3.13797557421427));
#64734=CARTESIAN_POINT('Ctrl Pts',(8.88625383852863,-0.837954627269075,
3.11350088915814));
#64735=CARTESIAN_POINT('Ctrl Pts',(8.89241466126559,-0.933372498500471,
3.08462855811571));
#64736=CARTESIAN_POINT('Ctrl Pts',(8.89858578418228,-1.028949897325,3.05570795589074));
#64737=CARTESIAN_POINT('Ctrl Pts',(8.90475690709897,-1.12306907804891,3.02237516665914));
#64738=CARTESIAN_POINT('Ctrl Pts',(8.91092803001566,-1.21530683639517,2.98481940088696));
#64739=CARTESIAN_POINT('Ctrl Pts',(8.91562355196123,-1.28548926905317,2.9562437389294));
#64740=CARTESIAN_POINT('Ctrl Pts',(8.92031907390679,-1.35458284365331,2.92522420355102));
#64741=CARTESIAN_POINT('Ctrl Pts',(8.92501459585236,-1.42241128634469,2.89186163136815));
#64742=CARTESIAN_POINT('Ctrl Pts',(8.93118684394513,-1.51157155029196,2.84800664039748));
#64743=CARTESIAN_POINT('Ctrl Pts',(8.93735909203789,-1.59885867678112,2.79994718722595));
#64744=CARTESIAN_POINT('Ctrl Pts',(8.94353134013065,-1.68384900158579,2.74786646370572));
#64745=CARTESIAN_POINT('Ctrl Pts',(8.94969522878329,-1.76872421897398,2.69585627618527));
#64746=CARTESIAN_POINT('Ctrl Pts',(8.95585911743592,-1.85130845041722,2.63983586828306));
#64747=CARTESIAN_POINT('Ctrl Pts',(8.96202300608855,-1.93120042371355,2.58003536525153));
#64748=CARTESIAN_POINT('Ctrl Pts',(8.96818036774709,-2.0110077987201,2.52029818548109));
#64749=CARTESIAN_POINT('Ctrl Pts',(8.97433772940562,-2.08812823751872,2.45678912733547));
#64750=CARTESIAN_POINT('Ctrl Pts',(8.98049509106415,-2.16218822125454,2.38978234539637));
#64751=CARTESIAN_POINT('Ctrl Pts',(8.98664795521046,-2.23619410947009,2.32282450711817));
#64752=CARTESIAN_POINT('Ctrl Pts',(8.99280081935677,-2.3071436659334,2.2523743150494));
#64753=CARTESIAN_POINT('Ctrl Pts',(8.99895368350307,-2.3746960684403,2.17874646185236));
#64754=CARTESIAN_POINT('Ctrl Pts',(9.00510421663961,-2.44222287875038,2.10514650253386));
#64755=CARTESIAN_POINT('Ctrl Pts',(9.01125474977615,-2.50635479905214,2.02837159385722));
#64756=CARTESIAN_POINT('Ctrl Pts',(9.01740528291268,-2.56678818299062,1.94877294371605));
#64757=CARTESIAN_POINT('Ctrl Pts',(9.02355513112789,-2.62721483708751,1.86918315765416));
#64758=CARTESIAN_POINT('Ctrl Pts',(9.0297049793431,-2.68394351101071,1.78677060126456));
#64759=CARTESIAN_POINT('Ctrl Pts',(9.0358548275583,-2.73671178223863,1.70191838331227));
#64760=CARTESIAN_POINT('Ctrl Pts',(9.04200563593743,-2.78948829207482,1.61705291754709));
#64761=CARTESIAN_POINT('Ctrl Pts',(9.04815644431656,-2.83830294163955,1.52974740255392));
#64762=CARTESIAN_POINT('Ctrl Pts',(9.05430725269569,-2.88293799314867,1.44041177798571));
#64763=CARTESIAN_POINT('Ctrl Pts',(9.06046463906188,-2.92762077965016,1.35098061336065));
#64764=CARTESIAN_POINT('Ctrl Pts',(9.06662202542807,-2.96811484769521,1.25951539302503));
#64765=CARTESIAN_POINT('Ctrl Pts',(9.07277941179426,-3.00424965263439,1.16644827881316));
#64766=CARTESIAN_POINT('Ctrl Pts',(9.07894023453122,-3.04040462401761,1.07332922485084));
#64767=CARTESIAN_POINT('Ctrl Pts',(9.08510105726818,-3.07219534907949,0.978606908438986));
#64768=CARTESIAN_POINT('Ctrl Pts',(9.09126188000514,-3.09950110681261,0.882728979567017));
#64769=CARTESIAN_POINT('Ctrl Pts',(9.09743300292183,-3.12685251659971,0.786690753939032));
#64770=CARTESIAN_POINT('Ctrl Pts',(9.10360412583852,-3.149703881888,0.689493479684278));
#64771=CARTESIAN_POINT('Ctrl Pts',(9.10977524875521,-3.16798553732232,0.591595468049439));
#64772=CARTESIAN_POINT('Ctrl Pts',(9.11447077070081,-3.18189579570684,0.517106227068816));
#64773=CARTESIAN_POINT('Ctrl Pts',(9.11916629264641,-3.19316148928379,0.442211515810729));
#64774=CARTESIAN_POINT('Ctrl Pts',(9.12386181459201,-3.2017721296376,0.367114140800825));
#64775=CARTESIAN_POINT('Ctrl Pts',(9.13143235948571,-3.21565498230386,0.246035365001745));
#64776=CARTESIAN_POINT('Ctrl Pts',(9.1390029043794,-3.22267158184634,0.124154455016588));
#64777=CARTESIAN_POINT('Ctrl Pts',(9.1465734492731,-3.22274934639606,0.00205251157118864));
#64778=CARTESIAN_POINT('',(8.90087508401166,-3.22274906885896,-0.00275535252744801));
#64779=CARTESIAN_POINT('Ctrl Pts',(8.46829646867762,1.78943615355263,2.68030517196433));
#64780=CARTESIAN_POINT('Ctrl Pts',(8.47579862762055,1.6946416754658,2.74359224390675));
#64781=CARTESIAN_POINT('Ctrl Pts',(8.48344479637332,1.59654484078101,2.80181370844835));
#64782=CARTESIAN_POINT('Ctrl Pts',(8.50195209470057,1.35386705840831,2.92894985201071));
#64783=CARTESIAN_POINT('Ctrl Pts',(8.51284534894163,1.20684476031786,2.9925294065602));
#64784=CARTESIAN_POINT('Ctrl Pts',(8.52879445311386,0.978937359159517,3.07154700259383));
#64785=CARTESIAN_POINT('Ctrl Pts',(8.53407697800821,0.901182328413188,3.09525318779629));
#64786=CARTESIAN_POINT('Ctrl Pts',(8.53989482736868,0.81200845620102,3.11879463803361));
#64787=CARTESIAN_POINT('Ctrl Pts',(8.54058342794267,0.801395218346658,3.12153863332567));
#64788=CARTESIAN_POINT('Ctrl Pts',(8.54159216788618,0.785757875946686,3.12549657372907));
#64789=CARTESIAN_POINT('Ctrl Pts',(8.54191468279844,0.780744659996072,3.1267526363276));
#64790=CARTESIAN_POINT('Ctrl Pts',(8.54248803414816,0.77180764340262,3.12896897425712));
#64791=CARTESIAN_POINT('Ctrl Pts',(8.54273914039506,0.767885040845833,3.12993393620606));
#64792=CARTESIAN_POINT('Ctrl Pts',(8.54327103542302,0.759557911930897,3.13196581692718));
#64793=CARTESIAN_POINT('Ctrl Pts',(8.54355171220243,0.755152960527299,3.13303081803977));
#64794=CARTESIAN_POINT('Ctrl Pts',(8.54429658617214,0.743434690794448,3.13583783726263));
#64795=CARTESIAN_POINT('Ctrl Pts',(8.54475985009215,0.736117444730943,3.13756357566068));
#64796=CARTESIAN_POINT('Ctrl Pts',(8.54694896760837,0.701405947062481,3.14562200541563));
#64797=CARTESIAN_POINT('Ctrl Pts',(8.54865638451767,0.673934621407378,3.1516218611702));
#64798=CARTESIAN_POINT('Ctrl Pts',(8.56494784998084,0.408430681921393,3.20597856931094));
#64799=CARTESIAN_POINT('Ctrl Pts',(8.57826032314767,0.165693583213242,3.22764541142062));
#64800=CARTESIAN_POINT('Ctrl Pts',(8.59708224166964,-0.170220816540769,
3.21959625910126));
#64801=CARTESIAN_POINT('Ctrl Pts',(8.60232269816301,-0.26309707283633,3.21334000292403));
#64802=CARTESIAN_POINT('Ctrl Pts',(8.61026033107898,-0.40083817832454,3.19804953755053));
#64803=CARTESIAN_POINT('Ctrl Pts',(8.61288901739599,-0.445994088857983,
3.19206533874573));
#64804=CARTESIAN_POINT('Ctrl Pts',(8.61601869660511,-0.499077665618734,
3.18388217956807));
#64805=CARTESIAN_POINT('Ctrl Pts',(8.61649533017392,-0.507143748292799,
3.18260733782146));
#64806=CARTESIAN_POINT('Ctrl Pts',(8.62148221528932,-0.591340166951187,
3.16897191262809));
#64807=CARTESIAN_POINT('Ctrl Pts',(8.62606392763189,-0.667003094716916,
3.1539136949829));
#64808=CARTESIAN_POINT('Ctrl Pts',(8.63162150771758,-0.756324351548435,
3.13277931512577));
#64809=CARTESIAN_POINT('Ctrl Pts',(8.63251280455146,-0.770576451799622,
3.12930418510241));
#64810=CARTESIAN_POINT('Ctrl Pts',(8.63396956607379,-0.793749191193171,
3.12348600795123));
#64811=CARTESIAN_POINT('Ctrl Pts',(8.63453312964858,-0.80268447730299,3.12120173130421));
#64812=CARTESIAN_POINT('Ctrl Pts',(8.63554022614174,-0.818599010302545,
3.11706037483392));
#64813=CARTESIAN_POINT('Ctrl Pts',(8.63598327553756,-0.825582078876997,
3.11521812233369));
#64814=CARTESIAN_POINT('Ctrl Pts',(8.63691921490108,-0.840295115951148,
3.11128362743157));
#64815=CARTESIAN_POINT('Ctrl Pts',(8.63741227681921,-0.848023586332021,
3.10918601685229));
#64816=CARTESIAN_POINT('Ctrl Pts',(8.6387191632251,-0.868448260122921,3.10356066806939));
#64817=CARTESIAN_POINT('Ctrl Pts',(8.63953458164963,-0.881130683297891,
3.09998385666104));
#64818=CARTESIAN_POINT('Ctrl Pts',(8.6432371330804,-0.938436432090628,3.083441901165));
#64819=CARTESIAN_POINT('Ctrl Pts',(8.64615308705334,-0.982796233532079,
3.06959086756475));
#64820=CARTESIAN_POINT('Ctrl Pts',(8.65405420063484,-1.10087972481441,3.0298981494575));
#64821=CARTESIAN_POINT('Ctrl Pts',(8.65909400260583,-1.17398544258651,3.00232834996836));
#64822=CARTESIAN_POINT('Ctrl Pts',(8.67890603670013,-1.45302467700679,2.88534616579206));
#64823=CARTESIAN_POINT('Ctrl Pts',(8.69421953878989,-1.65038777242848,2.77717544333505));
#64824=CARTESIAN_POINT('Ctrl Pts',(8.71905093925936,-1.95344401973431,2.56728895159755));
#64825=CARTESIAN_POINT('Ctrl Pts',(8.72864030112209,-2.06637437228752,2.47730167892635));
#64826=CARTESIAN_POINT('Ctrl Pts',(8.73850911137816,-2.18177419710493,2.37194499658698));
#64827=CARTESIAN_POINT('Ctrl Pts',(8.73926395522007,-2.19059586220245,2.36380022277344));
#64828=CARTESIAN_POINT('Ctrl Pts',(8.74035070909394,-2.20329235956693,2.3519458132815));
#64829=CARTESIAN_POINT('Ctrl Pts',(8.740685543336,-2.20720364321955,2.34827562451455));
#64830=CARTESIAN_POINT('Ctrl Pts',(8.7412729844112,-2.21406503361762,2.3418048883254));
#64831=CARTESIAN_POINT('Ctrl Pts',(8.74152590947406,-2.2170190241985,2.33900849830813));
#64832=CARTESIAN_POINT('Ctrl Pts',(8.7420534112226,-2.22317957448665,2.33315446823612));
#64833=CARTESIAN_POINT('Ctrl Pts',(8.7423279060333,-2.22638511886519,2.33009581264913));
#64834=CARTESIAN_POINT('Ctrl Pts',(8.74288523333201,-2.23289285678557,2.32386059118233));
#64835=CARTESIAN_POINT('Ctrl Pts',(8.74316802979512,-2.23619460511071,2.32068357296242));
#64836=CARTESIAN_POINT('Ctrl Pts',(8.74434994580997,-2.2499916264596,2.30735097648105));
#64837=CARTESIAN_POINT('Ctrl Pts',(8.74524416969898,-2.26042478779632,2.29713095953601));
#64838=CARTESIAN_POINT('Ctrl Pts',(8.75306418934751,-2.35156838881662,2.20662711441993));
#64839=CARTESIAN_POINT('Ctrl Pts',(8.75968384018178,-2.42805126080892,2.12218052517605));
#64840=CARTESIAN_POINT('Ctrl Pts',(8.77127008488088,-2.55638544950768,1.96443853329002));
#64841=CARTESIAN_POINT('Ctrl Pts',(8.7762819666804,-2.60994561832455,1.89269918634697));
#64842=CARTESIAN_POINT('Ctrl Pts',(8.79552434089202,-2.80420308197538,1.60855222531929));
#64843=CARTESIAN_POINT('Ctrl Pts',(8.80970634072327,-2.9225020827472,1.38201240868437));
#64844=CARTESIAN_POINT('Ctrl Pts',(8.82535694447938,-3.0153657940286,1.13742471245656));
#64845=CARTESIAN_POINT('Ctrl Pts',(8.82577329668741,-3.01781125126521,1.13092046533894));
#64846=CARTESIAN_POINT('Ctrl Pts',(8.82789580542811,-3.03015040431871,1.09777668066512));
#64847=CARTESIAN_POINT('Ctrl Pts',(8.82961252472462,-3.03971223508363,1.07101566859724));
#64848=CARTESIAN_POINT('Ctrl Pts',(8.83202358737759,-3.0525543651526,1.03351600618123));
#64849=CARTESIAN_POINT('Ctrl Pts',(8.83270798571006,-3.05613452465505,1.02288085789969));
#64850=CARTESIAN_POINT('Ctrl Pts',(8.83381136565364,-3.06180148247826,1.0057513474394));
#64851=CARTESIAN_POINT('Ctrl Pts',(8.83422918569213,-3.06392335451921,0.999268616279226));
#64852=CARTESIAN_POINT('Ctrl Pts',(8.83509570522546,-3.06827409109658,0.985832129140286));
#64853=CARTESIAN_POINT('Ctrl Pts',(8.83554450149965,-3.07049993268714,0.978877442231301));
#64854=CARTESIAN_POINT('Ctrl Pts',(8.8365964407798,-3.07565265923587,0.962587140210561));
#64855=CARTESIAN_POINT('Ctrl Pts',(8.83720019957919,-3.0785606948493,0.953245680561477));
#64856=CARTESIAN_POINT('Ctrl Pts',(8.83915575477198,-3.08782017987653,0.923017176599575));
#64857=CARTESIAN_POINT('Ctrl Pts',(8.84051309451524,-3.09400183495431,0.902079142337461));
#64858=CARTESIAN_POINT('Ctrl Pts',(8.84369819396764,-3.10793531702774,0.853055940438917));
#64859=CARTESIAN_POINT('Ctrl Pts',(8.84553126408412,-3.11551986500512,0.824925604795923));
#64860=CARTESIAN_POINT('Ctrl Pts',(8.86445762735885,-3.18938949060584,0.535387322419601));
#64861=CARTESIAN_POINT('Ctrl Pts',(8.88264150706362,-3.22297908382601,0.266799226859869));
#64862=CARTESIAN_POINT('Ctrl Pts',(8.90087535058479,-3.22274882416508,-0.00275296978013415));
#64863=CARTESIAN_POINT('Ctrl Pts',(8.90087550980276,-3.22274882215359,-0.00275532351062157));
#64864=CARTESIAN_POINT('Ctrl Pts',(8.91224051534764,-3.2226051804775,-0.170765011173096));
#64865=CARTESIAN_POINT('Ctrl Pts',(8.92354587169548,-3.20932355738335,-0.33853059364086));
#64866=CARTESIAN_POINT('Ctrl Pts',(8.93521580475408,-3.18065427738746,-0.519406634633492));
#64867=CARTESIAN_POINT('Ctrl Pts',(8.93617153842345,-3.17818944722932,-0.534281519399871));
#64868=CARTESIAN_POINT('Ctrl Pts',(8.93757479794722,-3.17439548953985,-0.556221631992641));
#64869=CARTESIAN_POINT('Ctrl Pts',(8.93802655248072,-3.1731470110333,-0.563300343135838));
#64870=CARTESIAN_POINT('Ctrl Pts',(8.93877518056322,-3.17103276706671,-0.575057728145776));
#64871=CARTESIAN_POINT('Ctrl Pts',(8.93907278167319,-3.17018031222907,-0.579738724902492));
#64872=CARTESIAN_POINT('Ctrl Pts',(8.9396540323799,-3.16849180496538,-0.588895556064934));
#64873=CARTESIAN_POINT('Ctrl Pts',(8.93993773047647,-3.16765662785408,-0.59337153850793));
#64874=CARTESIAN_POINT('Ctrl Pts',(8.9404718161381,-3.1660634018941,-0.601810917507669));
#64875=CARTESIAN_POINT('Ctrl Pts',(8.94072231371672,-3.16530740419647,-0.605774613508901));
#64876=CARTESIAN_POINT('Ctrl Pts',(8.94129575706035,-3.16355672083868,-0.614860686567186));
#64877=CARTESIAN_POINT('Ctrl Pts',(8.94161841357336,-3.16255703966688,-0.619982065558459));
#64878=CARTESIAN_POINT('Ctrl Pts',(8.94261486241257,-3.1594245648203,-0.635825040282631));
#64879=CARTESIAN_POINT('Ctrl Pts',(8.94328628502152,-3.15724962777492,-0.646538365906115));
#64880=CARTESIAN_POINT('Ctrl Pts',(8.94886844489445,-3.13863364347941,-0.735902605545982));
#64881=CARTESIAN_POINT('Ctrl Pts',(8.95362323213689,-3.11930940579938,-0.813931849445874));
#64882=CARTESIAN_POINT('Ctrl Pts',(8.963502097128,-3.07219572738373,-0.977667298684386));
#64883=CARTESIAN_POINT('Ctrl Pts',(8.96859789207978,-3.04369043916722,-1.06309461745316));
#64884=CARTESIAN_POINT('Ctrl Pts',(8.97718317709771,-2.98927715702551,-1.20593853762057));
#64885=CARTESIAN_POINT('Ctrl Pts',(8.9806909060247,-2.9651971265437,-1.26399043265779));
#64886=CARTESIAN_POINT('Ctrl Pts',(8.98737364882772,-2.91616952070017,-1.37305975243089));
#64887=CARTESIAN_POINT('Ctrl Pts',(8.99054673292551,-2.89154103096361,-1.42419384395159));
#64888=CARTESIAN_POINT('Ctrl Pts',(9.00276854552756,-2.7920892662199,-1.61745085841725));
#64889=CARTESIAN_POINT('Ctrl Pts',(9.01193861273916,-2.70804015747543,-1.75454256784271));
#64890=CARTESIAN_POINT('Ctrl Pts',(9.02413588741151,-2.58808546656617,-1.92091501708622));
#64891=CARTESIAN_POINT('Ctrl Pts',(9.02681088604528,-2.56129498884497,-1.95649394798408));
#64892=CARTESIAN_POINT('Ctrl Pts',(9.03030404766566,-2.52574517798408,-2.0017237039221));
#64893=CARTESIAN_POINT('Ctrl Pts',(9.03109567469073,-2.51765185174411,-2.01189354505197));
#64894=CARTESIAN_POINT('Ctrl Pts',(9.03237659625531,-2.50449804783152,-2.02821857301368));
#64895=CARTESIAN_POINT('Ctrl Pts',(9.03286434829349,-2.49947581793827,-2.03440450384066));
#64896=CARTESIAN_POINT('Ctrl Pts',(9.03379652246052,-2.48985215096608,-2.04616864358906));
#64897=CARTESIAN_POINT('Ctrl Pts',(9.03424077812246,-2.48525477296027,-2.05175012216357));
#64898=CARTESIAN_POINT('Ctrl Pts',(9.03525799416341,-2.47470345625165,-2.06447252541605));
#64899=CARTESIAN_POINT('Ctrl Pts',(9.03583145009875,-2.46873734307671,-2.07160322759412));
#64900=CARTESIAN_POINT('Ctrl Pts',(9.03759687789056,-2.45031637426936,-2.09342739292402));
#64901=CARTESIAN_POINT('Ctrl Pts',(9.03879299236848,-2.43776075092453,-2.10803488556374));
#64902=CARTESIAN_POINT('Ctrl Pts',(9.05586602196239,-2.25750943097432,-2.31397933176139));
#64903=CARTESIAN_POINT('Ctrl Pts',(9.07273631454037,-2.06789827110646,-2.48487293425201));
#64904=CARTESIAN_POINT('Ctrl Pts',(9.10065334617837,-1.73076510456206,-2.72317873296563));
#64905=CARTESIAN_POINT('Ctrl Pts',(9.11143511507569,-1.59472751437499,-2.80501315475837));
#64906=CARTESIAN_POINT('Ctrl Pts',(9.12512728749325,-1.40913016953806,-2.89877718813971));
#64907=CARTESIAN_POINT('Ctrl Pts',(9.12834357305445,-1.36453698370567,-2.92003362905785));
#64908=CARTESIAN_POINT('Ctrl Pts',(9.13329989218605,-1.29397457197227,-2.95169922486625));
#64909=CARTESIAN_POINT('Ctrl Pts',(9.13507425458027,-1.26832997059556,-2.96280909260864));
#64910=CARTESIAN_POINT('Ctrl Pts',(9.13729991857155,-1.2356292731601,-2.97647341814763));
#64911=CARTESIAN_POINT('Ctrl Pts',(9.1377690926105,-1.22870532632373,-2.97933833818105));
#64912=CARTESIAN_POINT('Ctrl Pts',(9.13851934174205,-1.21758306089822,-2.98389502807778));
#64913=CARTESIAN_POINT('Ctrl Pts',(9.13880133447235,-1.2133911120123,-2.98560212665149));
#64914=CARTESIAN_POINT('Ctrl Pts',(9.13933405370763,-1.20544995654027,-2.98881653717928));
#64915=CARTESIAN_POINT('Ctrl Pts',(9.13958488256228,-1.20170155650504,-2.9903256110171));
#64916=CARTESIAN_POINT('Ctrl Pts',(9.1401561478938,-1.19314340157343,-2.99375236053776));
#64917=CARTESIAN_POINT('Ctrl Pts',(9.14047630733692,-1.18833186480008,-2.99566549416561));
#64918=CARTESIAN_POINT('Ctrl Pts',(9.14147525414747,-1.17327239592296,-3.00161135545591));
#64919=CARTESIAN_POINT('Ctrl Pts',(9.14215161585377,-1.16300825742728,-3.00560320827811));
#64920=CARTESIAN_POINT('Ctrl Pts',(9.14788766440358,-1.07540582415381,-3.03915694671186));
#64921=CARTESIAN_POINT('Ctrl Pts',(9.15278168804475,-0.996967814978466,
-3.06578382271361));
#64922=CARTESIAN_POINT('Ctrl Pts',(9.16686966593601,-0.763743074814681,
-3.13505485880144));
#64923=CARTESIAN_POINT('Ctrl Pts',(9.17577891644022,-0.606693655685152,
-3.1691958176426));
#64924=CARTESIAN_POINT('Ctrl Pts',(9.19793182318241,-0.214292285908086,
-3.22424712106936));
#64925=CARTESIAN_POINT('Ctrl Pts',(9.21122842923173,0.0220131353451677,
-3.23128224789386));
#64926=CARTESIAN_POINT('Ctrl Pts',(9.22680682806551,0.279721004876056,-3.21066896726612));
#64927=CARTESIAN_POINT('Ctrl Pts',(9.22819023182167,0.302464112998689,-3.20860631379817));
#64928=CARTESIAN_POINT('Ctrl Pts',(9.23018820073404,0.335096371752607,-3.20529675243454));
#64929=CARTESIAN_POINT('Ctrl Pts',(9.23079660292102,0.345004999948714,-3.20424537075899));
#64930=CARTESIAN_POINT('Ctrl Pts',(9.23185525135656,0.36219660348664,-3.20234054269281));
#64931=CARTESIAN_POINT('Ctrl Pts',(9.23230482977598,0.369481875210079,-3.20150815607772));
#64932=CARTESIAN_POINT('Ctrl Pts',(9.23317135436664,0.383493411875749,-3.19985878991128));
#64933=CARTESIAN_POINT('Ctrl Pts',(9.23358818332162,0.390220072232276,-3.19904544613428));
#64934=CARTESIAN_POINT('Ctrl Pts',(9.23468224203442,0.40784024945324,-3.19685852813553));
#64935=CARTESIAN_POINT('Ctrl Pts',(9.23536055872445,0.418729329706685,-3.1954504943188));
#64936=CARTESIAN_POINT('Ctrl Pts',(9.23771202446459,0.456353415744524,-3.19038982312557));
#64937=CARTESIAN_POINT('Ctrl Pts',(9.23939400886271,0.483049024088982,-3.18645715999095));
#64938=CARTESIAN_POINT('Ctrl Pts',(9.24164246422415,0.51844063841155,-3.18078848381864));
#64939=CARTESIAN_POINT('Ctrl Pts',(9.24219944087821,0.527183924948733,-3.17935106289005));
#64940=CARTESIAN_POINT('Ctrl Pts',(9.25891251672479,0.788826771570012,-3.13522729858176));
#64941=CARTESIAN_POINT('Ctrl Pts',(9.27606973854272,1.03568860024296,-3.06254739481556));
#64942=CARTESIAN_POINT('Ctrl Pts',(9.30618997581978,1.44460000158168,-2.88700974242692));
#64943=CARTESIAN_POINT('Ctrl Pts',(9.31897241823912,1.61107388810878,-2.79752558416033));
#64944=CARTESIAN_POINT('Ctrl Pts',(9.33263140044182,1.78966634581512,-2.68026798232784));
#64945=CARTESIAN_POINT('Ctrl Pts',(9.33421565278191,1.81039709216274,-2.66630916186032));
#64946=CARTESIAN_POINT('Ctrl Pts',(9.33623615299508,1.83688604780093,-2.64802171331546));
#64947=CARTESIAN_POINT('Ctrl Pts',(9.3366865740106,1.84279434496339,-2.64391345382737));
#64948=CARTESIAN_POINT('Ctrl Pts',(9.33741388889364,1.85234085162141,-2.63722786456178));
#64949=CARTESIAN_POINT('Ctrl Pts',(9.33769160498529,1.8559875196805,-2.63466274266243));
#64950=CARTESIAN_POINT('Ctrl Pts',(9.33822112365766,1.86294361389825,-2.6297481107604));
#64951=CARTESIAN_POINT('Ctrl Pts',(9.33847301118517,1.86625391508573,-2.62739992372382));
#64952=CARTESIAN_POINT('Ctrl Pts',(9.33905314923752,1.87388097487463,-2.62196792475276));
#64953=CARTESIAN_POINT('Ctrl Pts',(9.33938109403584,1.87819458808512,-2.61887968350456));
#64954=CARTESIAN_POINT('Ctrl Pts',(9.34025953676007,1.8897541368965,-2.61056061576621));
#64955=CARTESIAN_POINT('Ctrl Pts',(9.34080870865557,1.89698603654271,-2.60531023259536));
#64956=CARTESIAN_POINT('Ctrl Pts',(9.34478188790707,1.94933636742768,-2.56697017301981));
#64957=CARTESIAN_POINT('Ctrl Pts',(9.34813045205917,1.99361129656449,-2.53273824835489));
#64958=CARTESIAN_POINT('Ctrl Pts',(9.37013789024603,2.28343370469918,-2.29634496191581));
#64959=CARTESIAN_POINT('Ctrl Pts',(9.38708912513479,2.49879953537757,-2.05993196855712));
#64960=CARTESIAN_POINT('Ctrl Pts',(9.40982523295586,2.71892855776573,-1.7318957997226));
#64961=CARTESIAN_POINT('Ctrl Pts',(9.41431388588081,2.75949098806638,-1.66650645985457));
#64962=CARTESIAN_POINT('Ctrl Pts',(9.42162387105256,2.8205549434693,-1.5597154418363));
#64963=CARTESIAN_POINT('Ctrl Pts',(9.42439147636278,2.84257451167856,-1.51921435807367));
#64964=CARTESIAN_POINT('Ctrl Pts',(9.42798255387318,2.8697034942563,-1.46665938338225));
#64965=CARTESIAN_POINT('Ctrl Pts',(9.42877742659947,2.87561935197151,-1.45502619445156));
#64966=CARTESIAN_POINT('Ctrl Pts',(9.43006233452078,2.88503827499106,-1.4362226131326));
#64967=CARTESIAN_POINT('Ctrl Pts',(9.4305508095628,2.88858569315519,-1.42907450264978));
#64968=CARTESIAN_POINT('Ctrl Pts',(9.43148352719014,2.89529570289232,-1.4154266506862));
#64969=CARTESIAN_POINT('Ctrl Pts',(9.43192759991667,2.89846305138215,-1.40892929172338));
#64970=CARTESIAN_POINT('Ctrl Pts',(9.4329432191861,2.9056444767612,-1.39407092941752));
#64971=CARTESIAN_POINT('Ctrl Pts',(9.43351525571424,2.90964435925304,-1.38570317217162));
#64972=CARTESIAN_POINT('Ctrl Pts',(9.4350059047907,2.91995040821661,-1.36390154049367));
#64973=CARTESIAN_POINT('Ctrl Pts',(9.43592646952617,2.9261999471462,-1.35044128197498));
#64974=CARTESIAN_POINT('Ctrl Pts',(9.44182600409199,2.96551508401014,-1.26420995249721));
#64975=CARTESIAN_POINT('Ctrl Pts',(9.44689440918493,2.99595413964917,-1.19027874119255));
#64976=CARTESIAN_POINT('Ctrl Pts',(9.45232646143493,3.02509565988156,-1.11127503054821));
#64977=CARTESIAN_POINT('Ctrl Pts',(9.45260328141914,3.02657139333901,-1.10724954084855));
#64978=CARTESIAN_POINT('Ctrl Pts',(9.45320921850452,3.02978126913138,-1.09843931317509));
#64979=CARTESIAN_POINT('Ctrl Pts',(9.45353843293577,3.03151211723777,-1.09365339395287));
#64980=CARTESIAN_POINT('Ctrl Pts',(9.45780945528202,3.05379719549257,-1.03157416258614));
#64981=CARTESIAN_POINT('Ctrl Pts',(9.46179819635579,3.07273457301046,-0.973716650350957));
#64982=CARTESIAN_POINT('Ctrl Pts',(9.47139175739874,3.11391114044204,-0.83471511462636));
#64983=CARTESIAN_POINT('Ctrl Pts',(9.47702893715218,3.13463338340288,-0.753169448658125));
#64984=CARTESIAN_POINT('Ctrl Pts',(9.49348833839362,3.18543560395888,-0.514485094867738));
#64985=CARTESIAN_POINT('Ctrl Pts',(9.50439107007879,3.20703993925166,-0.355797007696331));
#64986=CARTESIAN_POINT('Ctrl Pts',(9.519356838288,3.22074719636618,-0.131014046475662));
#64987=CARTESIAN_POINT('Ctrl Pts',(9.52364321072553,3.22274014830239,-0.0657591063378676));
#64988=CARTESIAN_POINT('Ctrl Pts',(9.5300427223429,3.22275509668956,0.0336522451780141));
#64989=CARTESIAN_POINT('Ctrl Pts',(9.53221674279805,3.2222178393868,0.067788702774648));
#64990=CARTESIAN_POINT('Ctrl Pts',(9.53486660012739,3.22088440998653,0.109934569285275));
#64991=CARTESIAN_POINT('Ctrl Pts',(9.53536943133128,3.22060060609335,0.117956480589242));
#64992=CARTESIAN_POINT('Ctrl Pts',(9.53615848086697,3.22010659777117,0.13058453245184));
#64993=CARTESIAN_POINT('Ctrl Pts',(9.53644580820198,3.21991647691811,0.1351913585726));
#64994=CARTESIAN_POINT('Ctrl Pts',(9.53698294629936,3.21954184550008,0.143819584395547));
#64995=CARTESIAN_POINT('Ctrl Pts',(9.53723288311561,3.2193596888457,0.147841001910388));
#64996=CARTESIAN_POINT('Ctrl Pts',(9.5378001113901,3.21892844877052,0.156982418848073));
#64997=CARTESIAN_POINT('Ctrl Pts',(9.53811713643678,3.21867468516704,0.162102159335523));
#64998=CARTESIAN_POINT('Ctrl Pts',(9.5390793551515,3.21786567718921,0.177672652391502));
#64999=CARTESIAN_POINT('Ctrl Pts',(9.53972240837416,3.21727173462848,0.18812145135249));
#65000=CARTESIAN_POINT('Ctrl Pts',(9.5445067231819,3.2124541016798,0.266163126042912));
#65001=CARTESIAN_POINT('Ctrl Pts',(9.54853756729726,3.20615125333803,0.333616286835064));
#65002=CARTESIAN_POINT('Ctrl Pts',(9.57048108520218,3.15942202685472,0.706414661652402));
#65003=CARTESIAN_POINT('Ctrl Pts',(9.58695246412331,3.07751141456086,1.00495322649634));
#65004=CARTESIAN_POINT('Ctrl Pts',(9.60903085842283,2.92441801111841,1.35630144035339));
#65005=CARTESIAN_POINT('Ctrl Pts',(9.61342288661609,2.89197162552098,1.42417457591874));
#65006=CARTESIAN_POINT('Ctrl Pts',(9.62058879222815,2.83620861836092,1.53104338944347));
#65007=CARTESIAN_POINT('Ctrl Pts',(9.62331162368465,2.81438970362274,1.57079071505846));
#65008=CARTESIAN_POINT('Ctrl Pts',(9.62685234361941,2.785258219264,1.62130273620062));
#65009=CARTESIAN_POINT('Ctrl Pts',(9.62764262153349,2.77870831173117,1.63250299264775));
#65010=CARTESIAN_POINT('Ctrl Pts',(9.62892188620645,2.76802973272116,1.65051276000309));
#65011=CARTESIAN_POINT('Ctrl Pts',(9.62940933777753,2.76394309995595,1.65734713037626));
#65012=CARTESIAN_POINT('Ctrl Pts',(9.63034128794528,2.75609656990768,1.6703597117097));
#65013=CARTESIAN_POINT('Ctrl Pts',(9.63078562148982,2.75234111774853,1.6765405570258));
#65014=CARTESIAN_POINT('Ctrl Pts',(9.6318035101147,2.74370540923748,1.69064626996315));
#65015=CARTESIAN_POINT('Ctrl Pts',(9.63237756309586,2.73881158192146,1.69856271554553));
#65016=CARTESIAN_POINT('Ctrl Pts',(9.63414662535567,2.72365846178123,1.72283924120721));
#65017=CARTESIAN_POINT('Ctrl Pts',(9.63534580207198,2.71328650530564,1.73912816705631));
#65018=CARTESIAN_POINT('Ctrl Pts',(9.64576089042307,2.6223540992812,1.87914190738608));
#65019=CARTESIAN_POINT('Ctrl Pts',(9.65529088838688,2.5335377332488,1.99727085087541));
#65020=CARTESIAN_POINT('Ctrl Pts',(9.68080555917827,2.28138840766265,2.28864545183788));
#65021=CARTESIAN_POINT('Ctrl Pts',(9.69714489084295,2.10643103788596,2.45062561851598));
#65022=CARTESIAN_POINT('Ctrl Pts',(9.71637844323449,1.8740305301894,2.62235688793788));
#65023=CARTESIAN_POINT('Ctrl Pts',(9.71976084273286,1.83207611166568,2.65183770981903));
#65024=CARTESIAN_POINT('Ctrl Pts',(9.72309722109888,1.78943620850078,2.68030513527963));
#65025=CARTESIAN_POINT('Origin',(-1.72497344927317,0.,0.));
#65026=CARTESIAN_POINT('',(11.2169460942912,1.78943621037803,2.68030513402634));
#65027=CARTESIAN_POINT('',(10.9707498958509,1.78943619500353,2.68030514429072));
#65028=CARTESIAN_POINT('',(-1.72497344927317,1.78943621037804,2.68030513402633));
#65029=CARTESIAN_POINT('',(10.3965734181394,-3.22264900191168,0.00167813006824187));
#65030=CARTESIAN_POINT('Ctrl Pts',(10.3965734492731,-3.22274956332349,0.00167767645253299));
#65031=CARTESIAN_POINT('Ctrl Pts',(10.4028071609904,-3.22280237398476,-0.0997694978905451));
#65032=CARTESIAN_POINT('Ctrl Pts',(10.4090408727076,-3.21806073881439,-0.201213091985544));
#65033=CARTESIAN_POINT('Ctrl Pts',(10.4152745844248,-3.2085521348123,-0.302176704415585));
#65034=CARTESIAN_POINT('Ctrl Pts',(10.4215102145758,-3.19904060452368,-0.40317138854223));
#65035=CARTESIAN_POINT('Ctrl Pts',(10.4277458447268,-3.18475922563231,-0.503685381087188));
#65036=CARTESIAN_POINT('Ctrl Pts',(10.4339814748778,-3.16578725712547,-0.603248377637264));
#65037=CARTESIAN_POINT('Ctrl Pts',(10.440220511964,-3.14680492298318,-0.702865772007254));
#65038=CARTESIAN_POINT('Ctrl Pts',(10.4464595490503,-3.12312697832341,-0.801530726483487));
#65039=CARTESIAN_POINT('Ctrl Pts',(10.4526985861366,-3.09488341232439,-0.898784861142722));
#65040=CARTESIAN_POINT('Ctrl Pts',(10.4589468229978,-3.06659819976241,-0.996182401929993));
#65041=CARTESIAN_POINT('Ctrl Pts',(10.4651950598589,-3.03373404194455,-1.09216456804687));
#65042=CARTESIAN_POINT('Ctrl Pts',(10.4714432967201,-2.9964703228284,-1.18628966399809));
#65043=CARTESIAN_POINT('Ctrl Pts',(10.4776968263823,-2.9591750380959,-1.28049449210534));
#65044=CARTESIAN_POINT('Ctrl Pts',(10.4839503560444,-2.91747294016046,-1.3728387366443));
#65045=CARTESIAN_POINT('Ctrl Pts',(10.4902038857066,-2.87159005554164,-1.46290400075138));
#65046=CARTESIAN_POINT('Ctrl Pts',(10.4964685379496,-2.82562556323518,-1.55312945570087));
#65047=CARTESIAN_POINT('Ctrl Pts',(10.5027331901926,-2.77546564344743,-1.64106747487174));
#65048=CARTESIAN_POINT('Ctrl Pts',(10.5089978424356,-2.72138049366528,-1.72632724916168));
#65049=CARTESIAN_POINT('Ctrl Pts',(10.5112626768803,-2.70182730772331,-1.75715087129783));
#65050=CARTESIAN_POINT('Ctrl Pts',(10.5135275113249,-2.68176147800805,-1.78762475090533));
#65051=CARTESIAN_POINT('Ctrl Pts',(10.5157923457695,-2.66119704885975,-1.81773150647729));
#65052=CARTESIAN_POINT('Ctrl Pts',(10.5219645938623,-2.60515376547963,-1.89978004874445));
#65053=CARTESIAN_POINT('Ctrl Pts',(10.5281368419551,-2.54521377229132,-1.97937873407576));
#65054=CARTESIAN_POINT('Ctrl Pts',(10.5343090900478,-2.48161843053037,-2.05613412202414));
#65055=CARTESIAN_POINT('Ctrl Pts',(10.5404729787005,-2.41810921969672,-2.13278555561742));
#65056=CARTESIAN_POINT('Ctrl Pts',(10.5466368673531,-2.35095477495504,-2.20660101426971));
#65057=CARTESIAN_POINT('Ctrl Pts',(10.5528007560057,-2.28043974554222,-2.27721587238701));
#65058=CARTESIAN_POINT('Ctrl Pts',(10.5589581176643,-2.20999938509354,-2.34775595583071));
#65059=CARTESIAN_POINT('Ctrl Pts',(10.5651154793228,-2.1362058199504,-2.41510187100397));
#65060=CARTESIAN_POINT('Ctrl Pts',(10.5712728409814,-2.05938335307498,-2.47892270302598));
#65061=CARTESIAN_POINT('Ctrl Pts',(10.5774257051277,-1.98261699951621,-2.54269691849556));
#65062=CARTESIAN_POINT('Ctrl Pts',(10.583578569274,-1.90282647595889,-2.6029508932634));
#65063=CARTESIAN_POINT('Ctrl Pts',(10.5897314334203,-1.8203715827754,-2.65939182203822));
#65064=CARTESIAN_POINT('Ctrl Pts',(10.5958819665568,-1.73794792759052,-2.71581136819297));
#65065=CARTESIAN_POINT('Ctrl Pts',(10.6020324996934,-1.65286226648796,-2.76842049362427));
#65066=CARTESIAN_POINT('Ctrl Pts',(10.6081830328299,-1.5655052804415,-2.81696836677478));
#65067=CARTESIAN_POINT('Ctrl Pts',(10.6143328810451,-1.47815802244004,-2.86551083365024));
#65068=CARTESIAN_POINT('Ctrl Pts',(10.6204827292603,-1.3885403220472,-2.90999273639795));
#65069=CARTESIAN_POINT('Ctrl Pts',(10.6266325774755,-1.29706859957037,-2.95020857067912));
#65070=CARTESIAN_POINT('Ctrl Pts',(10.6327833858547,-1.20558259579014,-2.99043068378084));
#65071=CARTESIAN_POINT('Ctrl Pts',(10.6389341942338,-1.11224239265235,-3.02638523062204));
#65072=CARTESIAN_POINT('Ctrl Pts',(10.6450850026129,-1.01748464066806,-3.05791474186325));
#65073=CARTESIAN_POINT('Ctrl Pts',(10.6512423889791,-0.922625549928435,
-3.08947797236604));
#65074=CARTESIAN_POINT('Ctrl Pts',(10.6573997753453,-0.826346296011019,
-3.11660657983079));
#65075=CARTESIAN_POINT('Ctrl Pts',(10.6635571617115,-0.729098842059141,
-3.13919296014247));
#65076=CARTESIAN_POINT('Ctrl Pts',(10.6697179844484,-0.631797115354364,
-3.16179194566886));
#65077=CARTESIAN_POINT('Ctrl Pts',(10.6758788071854,-0.533526539772602,
-3.1798435772076));
#65078=CARTESIAN_POINT('Ctrl Pts',(10.6820396299224,-0.434747352333379,
-3.19329176589599));
#65079=CARTESIAN_POINT('Ctrl Pts',(10.6882107528391,-0.335803017570888,
-3.20676243839319));
#65080=CARTESIAN_POINT('Ctrl Pts',(10.6943818757557,-0.23634880528944,-3.21561425614854));
#65081=CARTESIAN_POINT('Ctrl Pts',(10.7005529986724,-0.136848273637104,
-3.21984318135256));
#65082=CARTESIAN_POINT('Ctrl Pts',(10.705248520618,-0.0611396973734168,
-3.22306091196168));
#65083=CARTESIAN_POINT('Ctrl Pts',(10.7099440425636,0.0145956274916145,
-3.22360330825906));
#65084=CARTESIAN_POINT('Ctrl Pts',(10.7146395645092,0.0901554538964496,
-3.22148871744613));
#65085=CARTESIAN_POINT('Ctrl Pts',(10.7208118126019,0.18947859620559,-3.21870909480496));
#65086=CARTESIAN_POINT('Ctrl Pts',(10.7269840606947,0.288847887914431,-3.21132686240753));
#65087=CARTESIAN_POINT('Ctrl Pts',(10.7331563087875,0.3878018569203,-3.19933231819847));
#65088=CARTESIAN_POINT('Ctrl Pts',(10.7393201974401,0.486621806721703,-3.18735401890903));
#65089=CARTESIAN_POINT('Ctrl Pts',(10.7454840860928,0.585027124420842,-3.17077587567332));
#65090=CARTESIAN_POINT('Ctrl Pts',(10.7516479747454,0.682557170960763,-3.14964018117468));
#65091=CARTESIAN_POINT('Ctrl Pts',(10.7578053364039,0.779983942105353,-3.1285268674426));
#65092=CARTESIAN_POINT('Ctrl Pts',(10.7639626980625,0.876536862540032,-3.10286568854105));
#65093=CARTESIAN_POINT('Ctrl Pts',(10.770120059721,0.971762209784996,-3.07275052194834));
#65094=CARTESIAN_POINT('Ctrl Pts',(10.7762729238673,1.06691800172549,-3.04265735233062));
#65095=CARTESIAN_POINT('Ctrl Pts',(10.7824257880136,1.16074773549109,-3.00811679376037));
#65096=CARTESIAN_POINT('Ctrl Pts',(10.78857865216,1.25281055291525,-2.96927319069906));
#65097=CARTESIAN_POINT('Ctrl Pts',(10.7947291852965,1.3448384923831,-2.93044430351902));
#65098=CARTESIAN_POINT('Ctrl Pts',(10.800879718433,1.43510044582828,-2.88731577973072));
#65099=CARTESIAN_POINT('Ctrl Pts',(10.8070302515696,1.52317416630603,-2.84008063646051));
#65100=CARTESIAN_POINT('Ctrl Pts',(10.8131800997848,1.61123807892349,-2.79285075328018));
#65101=CARTESIAN_POINT('Ctrl Pts',(10.819329948,1.69711386024882,-2.74151536512039));
#65102=CARTESIAN_POINT('Ctrl Pts',(10.8254797962152,1.7804034754763,-2.68631365015553));
#65103=CARTESIAN_POINT('Ctrl Pts',(10.8316306045943,1.86370609455052,-2.63110331665354));
#65104=CARTESIAN_POINT('Ctrl Pts',(10.8377814129734,1.94442138342291,-2.57202569734984));
#65105=CARTESIAN_POINT('Ctrl Pts',(10.8439322213526,2.02218077607909,-2.50936296126251));
#65106=CARTESIAN_POINT('Ctrl Pts',(10.8500896077188,2.10002332858144,-2.44663321046075));
#65107=CARTESIAN_POINT('Ctrl Pts',(10.8562469940849,2.17490333342493,-2.38031095965062));
#65108=CARTESIAN_POINT('Ctrl Pts',(10.8624043804511,2.24648589196946,-2.31071822161037));
#65109=CARTESIAN_POINT('Ctrl Pts',(10.8685652031881,2.3181083999661,-2.24108664461532));
#65110=CARTESIAN_POINT('Ctrl Pts',(10.874726025925,2.38642949976062,-2.16818126244611));
#65111=CARTESIAN_POINT('Ctrl Pts',(10.880886848662,2.45115315403284,-2.09235890276379));
#65112=CARTESIAN_POINT('Ctrl Pts',(10.8870579715787,2.51598501873414,-2.01640977690659));
#65113=CARTESIAN_POINT('Ctrl Pts',(10.8932290944954,2.57720715764875,-1.93753427548303));
#65114=CARTESIAN_POINT('Ctrl Pts',(10.8994002174121,2.63456552349819,-1.85612016445453));
#65115=CARTESIAN_POINT('Ctrl Pts',(10.9040957393577,2.67820870955119,-1.79417329511235));
#65116=CARTESIAN_POINT('Ctrl Pts',(10.9087912613032,2.71961584377549,-1.73075734395263));
#65117=CARTESIAN_POINT('Ctrl Pts',(10.9134867832488,2.75869300294346,-1.66605236352607));
#65118=CARTESIAN_POINT('Ctrl Pts',(10.9196590313416,2.81005979963616,-1.58099788041255));
#65119=CARTESIAN_POINT('Ctrl Pts',(10.9258312794343,2.85757979342656,-1.49341589779036));
#65120=CARTESIAN_POINT('Ctrl Pts',(10.9320035275271,2.90099530016819,-1.40368936410521));
#65121=CARTESIAN_POINT('Ctrl Pts',(10.9381674161797,2.94435200672493,-1.31408435236384));
#65122=CARTESIAN_POINT('Ctrl Pts',(10.9443313048324,2.98361508772724,-1.2223409501225));
#65123=CARTESIAN_POINT('Ctrl Pts',(10.950495193485,3.01857104790268,-1.12886951914901));
#65124=CARTESIAN_POINT('Ctrl Pts',(10.9566525551436,3.05348999291475,-1.03549706586832));
#65125=CARTESIAN_POINT('Ctrl Pts',(10.9628099168021,3.08411073317958,-0.940400626330777));
#65126=CARTESIAN_POINT('Ctrl Pts',(10.9689672784607,3.1102669068782,-0.844012636444691));
#65127=CARTESIAN_POINT('Ctrl Pts',(10.975120142607,3.13640397536295,-0.747695051090338));
#65128=CARTESIAN_POINT('Ctrl Pts',(10.9812730067533,3.15808284738326,-0.650088208949003));
#65129=CARTESIAN_POINT('Ctrl Pts',(10.9874258708996,3.17518657026213,-0.551641012368562));
#65130=CARTESIAN_POINT('Ctrl Pts',(10.9935764040361,3.19228381340342,-0.453231112463453));
#65131=CARTESIAN_POINT('Ctrl Pts',(10.9997269371727,3.20480927717755,-0.353981918203898));
#65132=CARTESIAN_POINT('Ctrl Pts',(11.0058774703092,3.21269701606526,-0.254352993820366));
#65133=CARTESIAN_POINT('Ctrl Pts',(11.0120273185245,3.22058387657698,-0.154735164080839));
#65134=CARTESIAN_POINT('Ctrl Pts',(11.0181771667397,3.22383400470857,-0.0547381213100465));
#65135=CARTESIAN_POINT('Ctrl Pts',(11.0243270149549,3.22243337777737,0.0451739779774047));
#65136=CARTESIAN_POINT('Ctrl Pts',(11.030477823334,3.221032532169,0.145101676347971));
#65137=CARTESIAN_POINT('Ctrl Pts',(11.0366286317132,3.21497949533838,0.244943970519831));
#65138=CARTESIAN_POINT('Ctrl Pts',(11.0427794400923,3.20431234296101,0.344238247799028));
#65139=CARTESIAN_POINT('Ctrl Pts',(11.0489368264585,3.19363378258881,0.443638715424195));
#65140=CARTESIAN_POINT('Ctrl Pts',(11.0550942128247,3.17833129933227,0.542489563089042));
#65141=CARTESIAN_POINT('Ctrl Pts',(11.0612515991909,3.15849469008713,0.640334955465823));
#65142=CARTESIAN_POINT('Ctrl Pts',(11.0674124219278,3.1386470102448,0.738234954298347));
#65143=CARTESIAN_POINT('Ctrl Pts',(11.0735732446648,3.11426027108816,0.83512795910089));
#65144=CARTESIAN_POINT('Ctrl Pts',(11.0797340674017,3.08547456881628,0.930572000270806));
#65145=CARTESIAN_POINT('Ctrl Pts',(11.0859051903184,3.05664074019508,1.02617561278701));
#65146=CARTESIAN_POINT('Ctrl Pts',(11.0920763132351,3.02339340266776,1.12032501302636));
#65147=CARTESIAN_POINT('Ctrl Pts',(11.0982474361518,2.98592138245298,1.21259682512783));
#65148=CARTESIAN_POINT('Ctrl Pts',(11.1029429580973,2.95740944132999,1.2828051688165));
#65149=CARTESIAN_POINT('Ctrl Pts',(11.1076384800429,2.92645263936735,1.35192687335538));
#65150=CARTESIAN_POINT('Ctrl Pts',(11.1123340019885,2.89315165312483,1.41978557343038));
#65151=CARTESIAN_POINT('Ctrl Pts',(11.1185060393616,2.8493791111084,1.50898256533272));
#65152=CARTESIAN_POINT('Ctrl Pts',(11.1246780767348,2.80140069572558,1.59631036494504));
#65153=CARTESIAN_POINT('Ctrl Pts',(11.1308501141079,2.74939919461041,1.68134518501575));
#65154=CARTESIAN_POINT('Ctrl Pts',(11.1370141305733,2.69746527235467,1.76626949758132));
#65155=CARTESIAN_POINT('Ctrl Pts',(11.1431781470386,2.64151887807904,1.8489063846602));
#65156=CARTESIAN_POINT('Ctrl Pts',(11.1493421635039,2.58178978586484,1.9288543397841));
#65157=CARTESIAN_POINT('Ctrl Pts',(11.1554989370549,2.52213087722364,2.00870835353142));
#65158=CARTESIAN_POINT('Ctrl Pts',(11.1616557106059,2.45869837090181,2.08587937444902));
#65159=CARTESIAN_POINT('Ctrl Pts',(11.1678124841569,2.39176600122626,2.1599937402405));
#65160=CARTESIAN_POINT('Ctrl Pts',(11.1739650205478,2.32487969515251,2.23405709970052));
#65161=CARTESIAN_POINT('Ctrl Pts',(11.1801175569387,2.25449860285767,2.30506766354026));
#65162=CARTESIAN_POINT('Ctrl Pts',(11.1862700933296,2.180937051948,2.37268437385598));
#65163=CARTESIAN_POINT('Ctrl Pts',(11.1924205778935,2.1074000332913,2.44027853448071));
#65164=CARTESIAN_POINT('Ctrl Pts',(11.1985710624573,2.03068498090266,2.50448079474425));
#65165=CARTESIAN_POINT('Ctrl Pts',(11.2047215470212,1.95114281282732,2.56498719030959));
#65166=CARTESIAN_POINT('Ctrl Pts',(11.2087963961112,1.8984441469199,2.60507418318789));
#65167=CARTESIAN_POINT('Ctrl Pts',(11.2128712452012,1.84450530305379,2.64353968249036));
#65168=CARTESIAN_POINT('Ctrl Pts',(11.2169460942912,1.78943621037803,2.68030513402633));
#65169=CARTESIAN_POINT('Ctrl Pts',(9.96714565479787,1.78929966408823,2.68008864808392));
#65170=CARTESIAN_POINT('Ctrl Pts',(10.0174630726286,1.1068834492758,3.12577995893357));
#65171=CARTESIAN_POINT('Ctrl Pts',(10.134062896706,-0.878469227045605,3.57370670682763));
#65172=CARTESIAN_POINT('Ctrl Pts',(10.2772050334654,-2.93845908265942,1.93904361562529));
#65173=CARTESIAN_POINT('Ctrl Pts',(10.370029752394,-3.22029997028472,0.433048261942794));
#65174=CARTESIAN_POINT('Ctrl Pts',(10.3965720650762,-3.21827862215745,0.00169784412032958));
#65175=CARTESIAN_POINT('Ctrl Pts',(9.72309722109888,1.78943620850078,2.68030513527963));
#65176=CARTESIAN_POINT('Ctrl Pts',(9.7242170283104,1.7751247408481,2.68985981548279));
#65177=CARTESIAN_POINT('Ctrl Pts',(9.72533164044246,1.76073605209593,2.69930033597531));
#65178=CARTESIAN_POINT('Ctrl Pts',(9.72871374303097,1.71661506552156,2.7277454696974));
#65179=CARTESIAN_POINT('Ctrl Pts',(9.73096215783177,1.68664511362727,2.74637782173567));
#65180=CARTESIAN_POINT('Ctrl Pts',(9.73368993023612,1.64941476940892,2.76868457807351));
#65181=CARTESIAN_POINT('Ctrl Pts',(9.73419817379337,1.64243999751583,2.77282784037055));
#65182=CARTESIAN_POINT('Ctrl Pts',(9.73499380012874,1.6314603398369,2.77929418300549));
#65183=CARTESIAN_POINT('Ctrl Pts',(9.73528232250075,1.6274660254918,2.78163501068398));
#65184=CARTESIAN_POINT('Ctrl Pts',(9.73582050426074,1.61999135292766,2.78599385566529));
#65185=CARTESIAN_POINT('Ctrl Pts',(9.73607029491332,1.61651229760799,2.78801394173177));
#65186=CARTESIAN_POINT('Ctrl Pts',(9.73663565439229,1.60861597043393,2.7925791324879));
#65187=CARTESIAN_POINT('Ctrl Pts',(9.73695096377379,1.60419644835263,2.79512026708795));
#65188=CARTESIAN_POINT('Ctrl Pts',(9.73788227665554,1.59109718297368,2.80261077389247));
#65189=CARTESIAN_POINT('Ctrl Pts',(9.73849638086095,1.58240033436922,2.80753033528512));
#65190=CARTESIAN_POINT('Ctrl Pts',(9.74276796523527,1.52150554517015,2.84160394762827));
#65191=CARTESIAN_POINT('Ctrl Pts',(9.74633960102522,1.46852418426929,2.86934311564922));
#65192=CARTESIAN_POINT('Ctrl Pts',(9.75058938439789,1.40346964295228,2.90112900219003));
#65193=CARTESIAN_POINT('Ctrl Pts',(9.75132662156438,1.39210894695473,2.90659753211927));
#65194=CARTESIAN_POINT('Ctrl Pts',(9.76981632473928,1.10539376941059,3.04254272970068));
#65195=CARTESIAN_POINT('Ctrl Pts',(9.78613082430114,0.812935778881522,3.13338987824595));
#65196=CARTESIAN_POINT('Ctrl Pts',(9.80799496037242,0.438341017266595,3.19367310124625));
#65197=CARTESIAN_POINT('Ctrl Pts',(9.81235558095486,0.364250191463403,3.202969146157));
#65198=CARTESIAN_POINT('Ctrl Pts',(9.81947459180323,0.2449983516337,3.21374028439948));
#65199=CARTESIAN_POINT('Ctrl Pts',(9.82218279112177,0.20001127873527,3.21685342973216));
#65200=CARTESIAN_POINT('Ctrl Pts',(9.82570704234468,0.14204055902889,3.21964434965233));
#65201=CARTESIAN_POINT('Ctrl Pts',(9.82649580296943,0.129102300021097,3.22018910114445));
#65202=CARTESIAN_POINT('Ctrl Pts',(9.82777320426698,0.108209008553722,3.22094267155724));
#65203=CARTESIAN_POINT('Ctrl Pts',(9.82826031796067,0.100255784043493,3.22120003398721));
#65204=CARTESIAN_POINT('Ctrl Pts',(9.82919201756163,0.0850709966132224,
3.22163511507204));
#65205=CARTESIAN_POINT('Ctrl Pts',(9.82963644001139,0.077839619679537,3.22181794665359));
#65206=CARTESIAN_POINT('Ctrl Pts',(9.83065509138243,0.0612921126182172,
3.22218057562408));
#65207=CARTESIAN_POINT('Ctrl Pts',(9.83122982086193,0.0519757279983785,
3.2223443183149));
#65208=CARTESIAN_POINT('Ctrl Pts',(9.83300300638038,0.0232943657432221,
3.22272400054317));
#65209=CARTESIAN_POINT('Ctrl Pts',(9.8342056581021,0.00392832252921362,
3.22280578891355));
#65210=CARTESIAN_POINT('Ctrl Pts',(9.84481509158386,-0.16612887688819,3.22199120692338));
#65211=CARTESIAN_POINT('Ctrl Pts',(9.85454958421465,-0.316562037210817,
3.21070131167907));
#65212=CARTESIAN_POINT('Ctrl Pts',(9.87998875949124,-0.696358851500265,
3.15524482243257));
#65213=CARTESIAN_POINT('Ctrl Pts',(9.89600695041051,-0.922722733447225,
3.09662011878858));
#65214=CARTESIAN_POINT('Ctrl Pts',(9.91615920122354,-1.2057548975785,2.98949836462194));
#65215=CARTESIAN_POINT('Ctrl Pts',(9.92073187157282,-1.26993080403929,2.96280651262359));
#65216=CARTESIAN_POINT('Ctrl Pts',(9.92750682114723,-1.36564500857909,2.91931524183972));
#65217=CARTESIAN_POINT('Ctrl Pts',(9.92977820623368,-1.39784724941572,2.90403359031089));
#65218=CARTESIAN_POINT('Ctrl Pts',(9.93252998454896,-1.43708442503564,2.88460953153163));
#65219=CARTESIAN_POINT('Ctrl Pts',(9.93303986006551,-1.44436432053156,2.88097127841597));
#65220=CARTESIAN_POINT('Ctrl Pts',(9.93383746880248,-1.45576893942671,2.87521752985387));
#65221=CARTESIAN_POINT('Ctrl Pts',(9.93412635090912,-1.45990295175398,2.87312067638743));
#65222=CARTESIAN_POINT('Ctrl Pts',(9.93466485027207,-1.4676157879915,2.86918762727532));
#65223=CARTESIAN_POINT('Ctrl Pts',(9.93491460035531,-1.47119566029323,2.86735367038217));
#65224=CARTESIAN_POINT('Ctrl Pts',(9.93547941308754,-1.4792976736869,2.86318386769925));
#65225=CARTESIAN_POINT('Ctrl Pts',(9.93579421834005,-1.48381770832149,2.86084401478782));
#65226=CARTESIAN_POINT('Ctrl Pts',(9.93672267622904,-1.49716055424297,2.8538967931669));
#65227=CARTESIAN_POINT('Ctrl Pts',(9.93733444687229,-1.5059676840556,2.84925919703602));
#65228=CARTESIAN_POINT('Ctrl Pts',(9.94154927397929,-1.56673762903177,2.81689890129026));
#65229=CARTESIAN_POINT('Ctrl Pts',(9.94506906754459,-1.61795726223066,2.7877951050235));
#65230=CARTESIAN_POINT('Ctrl Pts',(9.9601105285728,-1.83708548414832,2.65520770474694));
#65231=CARTESIAN_POINT('Ctrl Pts',(9.97100128985003,-1.99610579756827,2.53783131175034));
#65232=CARTESIAN_POINT('Ctrl Pts',(9.99470044078522,-2.3123985528551,2.25613407300244));
#65233=CARTESIAN_POINT('Ctrl Pts',(10.0075163036593,-2.46504196299989,2.08827099512459));
#65234=CARTESIAN_POINT('Ctrl Pts',(10.0224614780322,-2.61158264873225,1.88844326831934));
#65235=CARTESIAN_POINT('Ctrl Pts',(10.0237676669307,-2.62415093308953,1.87093927063035));
#65236=CARTESIAN_POINT('Ctrl Pts',(10.0256736052011,-2.64213905263031,1.84534915377964));
#65237=CARTESIAN_POINT('Ctrl Pts',(10.026267958528,-2.64769945929229,1.8373621969502));
#65238=CARTESIAN_POINT('Ctrl Pts',(10.0273101924407,-2.657363804548,1.82334537947321));
#65239=CARTESIAN_POINT('Ctrl Pts',(10.0277574637398,-2.66148362753223,1.81732651484466));
#65240=CARTESIAN_POINT('Ctrl Pts',(10.0286254025381,-2.66942463159479,1.80564016909386));
#65241=CARTESIAN_POINT('Ctrl Pts',(10.0290459729667,-2.67324828726924,1.7999744102273));
#65242=CARTESIAN_POINT('Ctrl Pts',(10.0301633898312,-2.68334292216137,1.78491342092498));
#65243=CARTESIAN_POINT('Ctrl Pts',(10.0308614140203,-2.68958253735429,1.77549737472506));
#65244=CARTESIAN_POINT('Ctrl Pts',(10.0333497530227,-2.71158951157577,1.74190498787643));
#65245=CARTESIAN_POINT('Ctrl Pts',(10.035150325361,-2.72708106450095,1.71755042030322));
#65246=CARTESIAN_POINT('Ctrl Pts',(10.0373655062192,-2.74560927301591,1.68753913862809));
#65247=CARTESIAN_POINT('Ctrl Pts',(10.0377685601623,-2.74895924693956,1.68207659819142));
#65248=CARTESIAN_POINT('Ctrl Pts',(10.0540903884395,-2.88375849933772,1.46079179042319));
#65249=CARTESIAN_POINT('Ctrl Pts',(10.0709790884471,-2.98935975393753,1.23030711642551));
#65250=CARTESIAN_POINT('Ctrl Pts',(10.1019689068757,-3.13000161150293,0.79457011166922));
#65251=CARTESIAN_POINT('Ctrl Pts',(10.1158968899463,-3.17425201923646,0.593628257732955));
#65252=CARTESIAN_POINT('Ctrl Pts',(10.1298458127443,-3.20088609811125,0.375056110129359));
#65253=CARTESIAN_POINT('Ctrl Pts',(10.1307831431634,-3.20258342439748,0.360275351213151));
#65254=CARTESIAN_POINT('Ctrl Pts',(10.1320853574264,-3.20481250574597,0.339601762408255));
#65255=CARTESIAN_POINT('Ctrl Pts',(10.1324549312643,-3.20543045259679,0.333718697269679));
#65256=CARTESIAN_POINT('Ctrl Pts',(10.1330821623206,-3.20645425034305,0.323706528123644));
#65257=CARTESIAN_POINT('Ctrl Pts',(10.1333402819942,-3.20686833023153,0.319578298871961));
#65258=CARTESIAN_POINT('Ctrl Pts',(10.1338317752187,-3.20764298779661,0.311702104883322));
#65259=CARTESIAN_POINT('Ctrl Pts',(10.1340652291919,-3.20800496984906,0.307954303625351));
#65260=CARTESIAN_POINT('Ctrl Pts',(10.1346144597447,-3.20884245598749,0.299121609191988));
#65261=CARTESIAN_POINT('Ctrl Pts',(10.134929925151,-3.20931244464507,0.294036184726138));
#65262=CARTESIAN_POINT('Ctrl Pts',(10.1358613281048,-3.21066724024816,0.278986562221429));
#65263=CARTESIAN_POINT('Ctrl Pts',(10.1364753760229,-3.21151775507444,0.269019226943299));
#65264=CARTESIAN_POINT('Ctrl Pts',(10.1423322201904,-3.21921784167636,0.1735343665046));
#65265=CARTESIAN_POINT('Ctrl Pts',(10.1473964818277,-3.22269714196437,0.0877708669080378));
#65266=CARTESIAN_POINT('Ctrl Pts',(10.1614615971817,-3.22284531126189,-0.155513546596334));
#65267=CARTESIAN_POINT('Ctrl Pts',(10.1702053842559,-3.21139874199951,-0.312795122825867));
#65268=CARTESIAN_POINT('Ctrl Pts',(10.182884821753,-3.17842100158645,-0.537177319232002));
#65269=CARTESIAN_POINT('Ctrl Pts',(10.1867660237474,-3.16613619377615,-0.605393121046213));
#65270=CARTESIAN_POINT('Ctrl Pts',(10.2003368748682,-3.11597686409796,-0.84023413326679));
#65271=CARTESIAN_POINT('Ctrl Pts',(10.2101985353254,-3.06706809071662,-1.00418451432855));
#65272=CARTESIAN_POINT('Ctrl Pts',(10.2217039401308,-2.99828820939168,-1.18185183055689));
#65273=CARTESIAN_POINT('Ctrl Pts',(10.2228995794535,-2.99100524156142,-1.20016396972577));
#65274=CARTESIAN_POINT('Ctrl Pts',(10.2246667940159,-2.98004514245773,-1.22700232058778));
#65275=CARTESIAN_POINT('Ctrl Pts',(10.2252339572216,-2.97649829017663,-1.23558151149479));
#65276=CARTESIAN_POINT('Ctrl Pts',(10.2262463041613,-2.97011554517664,-1.2508332321287));
#65277=CARTESIAN_POINT('Ctrl Pts',(10.2266909939114,-2.96729409999333,-1.25751176896197));
#65278=CARTESIAN_POINT('Ctrl Pts',(10.227621671401,-2.96135238791694,-1.27144483211296));
#65279=CARTESIAN_POINT('Ctrl Pts',(10.2281077993873,-2.95822794719211,-1.2786975159146));
#65280=CARTESIAN_POINT('Ctrl Pts',(10.2293767979458,-2.95001784100771,-1.29756427620765));
#65281=CARTESIAN_POINT('Ctrl Pts',(10.2301611004046,-2.94489027682285,-1.30915986924683));
#65282=CARTESIAN_POINT('Ctrl Pts',(10.2335850374336,-2.92227564295642,-1.3594959542296));
#65283=CARTESIAN_POINT('Ctrl Pts',(10.2362485701396,-2.90409220539152,-1.3979171530288));
#65284=CARTESIAN_POINT('Ctrl Pts',(10.2432997457529,-2.85444537153338,-1.49766798205524));
#65285=CARTESIAN_POINT('Ctrl Pts',(10.2477284009941,-2.82176639780071,-1.55836485655799));
#65286=CARTESIAN_POINT('Ctrl Pts',(10.2648409901199,-2.68987320655635,-1.78556926750999));
#65287=CARTESIAN_POINT('Ctrl Pts',(10.2779381718605,-2.57766739839873,-1.94403971976498));
#65288=CARTESIAN_POINT('Ctrl Pts',(10.303865643101,-2.32903098828973,-2.23552968987077));
#65289=CARTESIAN_POINT('Ctrl Pts',(10.3166378124708,-2.19366101476323,-2.36851166465479));
#65290=CARTESIAN_POINT('Ctrl Pts',(10.3293401042552,-2.0382951890375,-2.49631902173543));
#65291=CARTESIAN_POINT('Ctrl Pts',(10.3300795223942,-2.02916974372735,-2.50374241828974));
#65292=CARTESIAN_POINT('Ctrl Pts',(10.3311481740507,-2.01585921023581,-2.51444974075624));
#65293=CARTESIAN_POINT('Ctrl Pts',(10.3314801992703,-2.01170644514313,-2.51777342781664));
#65294=CARTESIAN_POINT('Ctrl Pts',(10.3320643936386,-2.00436886839051,-2.52361635176553));
#65295=CARTESIAN_POINT('Ctrl Pts',(10.3323168699729,-2.00118750110262,-2.52613986897755));
#65296=CARTESIAN_POINT('Ctrl Pts',(10.3328452126039,-1.99450843883459,-2.53141728427047));
#65297=CARTESIAN_POINT('Ctrl Pts',(10.3331209905702,-1.99100981332341,-2.53416994369122));
#65298=CARTESIAN_POINT('Ctrl Pts',(10.3338484512345,-1.98174864253183,-2.5414254587406));
#65299=CARTESIAN_POINT('Ctrl Pts',(10.3342992594775,-1.97597641376645,-2.54591599610226));
#65300=CARTESIAN_POINT('Ctrl Pts',(10.3363433829882,-1.94965550341923,-2.5662490542001));
#65301=CARTESIAN_POINT('Ctrl Pts',(10.3379210977266,-1.92893054594401,-2.58186324951926));
#65302=CARTESIAN_POINT('Ctrl Pts',(10.3516667065893,-1.74501523835665,-2.71697425225623));
#65303=CARTESIAN_POINT('Ctrl Pts',(10.3629371012686,-1.57107655501851,-2.82112898772703));
#65304=CARTESIAN_POINT('Ctrl Pts',(10.3877311799588,-1.1706688430331,-3.01229440063833));
#65305=CARTESIAN_POINT('Ctrl Pts',(10.4012327373334,-0.941875378491943,
-3.09147790260617));
#65306=CARTESIAN_POINT('Ctrl Pts',(10.4161281187374,-0.698899990141334,
-3.14606348481142));
#65307=CARTESIAN_POINT('Ctrl Pts',(10.4165886969103,-0.691394335867417,
-3.1477214802931));
#65308=CARTESIAN_POINT('Ctrl Pts',(10.4187360982335,-0.656435764466007,
-3.15531274465253));
#65309=CARTESIAN_POINT('Ctrl Pts',(10.4204330798588,-0.628912608161079,
-3.16091367875017));
#65310=CARTESIAN_POINT('Ctrl Pts',(10.422820768766,-0.590350840207027,-3.16823738374792));
#65311=CARTESIAN_POINT('Ctrl Pts',(10.4235017853887,-0.579370628540423,
-3.17026369631467));
#65312=CARTESIAN_POINT('Ctrl Pts',(10.4246011302531,-0.561676403519434,
-3.17343403335881));
#65313=CARTESIAN_POINT('Ctrl Pts',(10.4250183130926,-0.554968841715986,
-3.17461391825002));
#65314=CARTESIAN_POINT('Ctrl Pts',(10.4258846115094,-0.541055336556297,
-3.17701591187964));
#65315=CARTESIAN_POINT('Ctrl Pts',(10.4263338273917,-0.533848881150081,
-3.17823478557589));
#65316=CARTESIAN_POINT('Ctrl Pts',(10.4273886769716,-0.516946642286728,
-3.18103446045096));
#65317=CARTESIAN_POINT('Ctrl Pts',(10.4279949365267,-0.507247693449419,
-3.18259545710934));
#65318=CARTESIAN_POINT('Ctrl Pts',(10.4299667277611,-0.475754086150861,
-3.18751657392744));
#65319=CARTESIAN_POINT('Ctrl Pts',(10.4313379322094,-0.453932408916524,
-3.19069728879393));
#65320=CARTESIAN_POINT('Ctrl Pts',(10.4345604543195,-0.402842076917451,
-3.19760947292065));
#65321=CARTESIAN_POINT('Ctrl Pts',(10.4364172527804,-0.373551789251474,
-3.20116338975306));
#65322=CARTESIAN_POINT('Ctrl Pts',(10.4429590063349,-0.270892359774016,
-3.2121913901471));
#65323=CARTESIAN_POINT('Ctrl Pts',(10.4477080674907,-0.197323449741024,
-3.21754848855274));
#65324=CARTESIAN_POINT('Ctrl Pts',(10.4720769771105,0.175468752340868,-3.23186110226117));
#65325=CARTESIAN_POINT('Ctrl Pts',(10.4928047832428,0.474662806166883,-3.20161979873633));
#65326=CARTESIAN_POINT('Ctrl Pts',(10.5177168547732,0.841170418536165,-3.11201549386957));
#65327=CARTESIAN_POINT('Ctrl Pts',(10.5227843773255,0.916288802256226,-3.09073214964787));
#65328=CARTESIAN_POINT('Ctrl Pts',(10.5283920864336,1.00089395866206,-3.06340441741788));
#65329=CARTESIAN_POINT('Ctrl Pts',(10.5290737534882,1.01120444271738,-3.06001649082249));
#65330=CARTESIAN_POINT('Ctrl Pts',(10.5300777557858,1.02643207013185,-3.0549274679298));
#65331=CARTESIAN_POINT('Ctrl Pts',(10.5304023975709,1.03136239318668,-3.0532664875073));
#65332=CARTESIAN_POINT('Ctrl Pts',(10.5309774650425,1.04010791172096,-3.05029660243918));
#65333=CARTESIAN_POINT('Ctrl Pts',(10.5312281709373,1.04392468599982,-3.04899246989969));
#65334=CARTESIAN_POINT('Ctrl Pts',(10.5317615417091,1.05205360617127,-3.04619789041504));
#65335=CARTESIAN_POINT('Ctrl Pts',(10.5320440858951,1.05636502373971,-3.04470545620776));
#65336=CARTESIAN_POINT('Ctrl Pts',(10.5328087734813,1.06804731944303,-3.04063372799684));
#65337=CARTESIAN_POINT('Ctrl Pts',(10.5332898756308,1.0754120738229,-3.03803677049178));
#65338=CARTESIAN_POINT('Ctrl Pts',(10.5356972953418,1.11233460981676,-3.02486606916646));
#65339=CARTESIAN_POINT('Ctrl Pts',(10.5376004270362,1.1417474393168,-3.01388718749809));
#65340=CARTESIAN_POINT('Ctrl Pts',(10.5429528616661,1.22492045291542,-2.98144890046001));
#65341=CARTESIAN_POINT('Ctrl Pts',(10.5463511199705,1.27827149882508,-2.95896780277302));
#65342=CARTESIAN_POINT('Ctrl Pts',(10.5586066870712,1.47113673242454,-2.87150728269124));
#65343=CARTESIAN_POINT('Ctrl Pts',(10.5671623297528,1.60655966041255,-2.79799384641693));
#65344=CARTESIAN_POINT('Ctrl Pts',(10.589531218879,1.94372765879357,-2.58238432939216));
#65345=CARTESIAN_POINT('Ctrl Pts',(10.6034021450438,2.13530823631491,-2.42635973749053));
#65346=CARTESIAN_POINT('Ctrl Pts',(10.6194523721098,2.3208319350965,-2.23612063388472));
#65347=CARTESIAN_POINT('Ctrl Pts',(10.6206333251522,2.33429365170153,-2.22206423898009));
#65348=CARTESIAN_POINT('Ctrl Pts',(10.622388995463,2.35402353745781,-2.20108562353435));
#65349=CARTESIAN_POINT('Ctrl Pts',(10.6229594545618,2.36039043564438,-2.19425653137055));
#65350=CARTESIAN_POINT('Ctrl Pts',(10.6239742975914,2.37163895355098,-2.18208583659073));
#65351=CARTESIAN_POINT('Ctrl Pts',(10.624418170063,2.3765324474879,-2.17675525701232));
#65352=CARTESIAN_POINT('Ctrl Pts',(10.625351182649,2.38676293509036,-2.16553536602062));
#65353=CARTESIAN_POINT('Ctrl Pts',(10.6258404776851,2.39209617223901,-2.15964270905134));
#65354=CARTESIAN_POINT('Ctrl Pts',(10.627126787901,2.40603281485262,-2.14412924859541));
#65355=CARTESIAN_POINT('Ctrl Pts',(10.627925308176,2.41460025327575,-2.13447645803894));
#65356=CARTESIAN_POINT('Ctrl Pts',(10.6314984553164,2.45255988323372,-2.09118696136463));
#65357=CARTESIAN_POINT('Ctrl Pts',(10.6342996304876,2.48130766314658,-2.05699412870558));
#65358=CARTESIAN_POINT('Ctrl Pts',(10.6417993727623,2.55558353607874,-1.96482643519855));
#65359=CARTESIAN_POINT('Ctrl Pts',(10.6465456971064,2.59984705735918,-1.90587093827602));
#65360=CARTESIAN_POINT('Ctrl Pts',(10.6708943001748,2.8133044833873,-1.60027408578584));
#65361=CARTESIAN_POINT('Ctrl Pts',(10.6916025761996,2.94957062066833,-1.33249807195055));
#65362=CARTESIAN_POINT('Ctrl Pts',(10.7165210401835,3.07249120300411,-0.975732475722724));
#65363=CARTESIAN_POINT('Ctrl Pts',(10.7216090816676,3.09530589282189,-0.900744022280118));
#65364=CARTESIAN_POINT('Ctrl Pts',(10.7272368731575,3.11814697053601,-0.814490663607777));
#65365=CARTESIAN_POINT('Ctrl Pts',(10.7279192110614,3.12087476727411,-0.803975289369373));
#65366=CARTESIAN_POINT('Ctrl Pts',(10.7289240095848,3.1248307704871,-0.788401741682506));
#65367=CARTESIAN_POINT('Ctrl Pts',(10.7292487819674,3.12609994296325,-0.783354197017556));
#65368=CARTESIAN_POINT('Ctrl Pts',(10.7298239946462,3.12833102816343,-0.774389314858562));
#65369=CARTESIAN_POINT('Ctrl Pts',(10.7300747156756,3.12929781782347,-0.770473231703493));
#65370=CARTESIAN_POINT('Ctrl Pts',(10.730608025257,3.13134216978543,-0.76212504368436));
#65371=CARTESIAN_POINT('Ctrl Pts',(10.7308904934686,3.13241767255121,-0.757692478378062));
#65372=CARTESIAN_POINT('Ctrl Pts',(10.7316547620564,3.13530769291171,-0.745670254177494));
#65373=CARTESIAN_POINT('Ctrl Pts',(10.7321355231264,3.13710407497373,-0.738076204030587));
#65374=CARTESIAN_POINT('Ctrl Pts',(10.7345384862177,3.14597300160057,-0.699966193493866));
#65375=CARTESIAN_POINT('Ctrl Pts',(10.7364376051507,3.15262823995214,-0.669353532881595));
#65376=CARTESIAN_POINT('Ctrl Pts',(10.7417757375914,3.17027144166617,-0.58208786926934));
#65377=CARTESIAN_POINT('Ctrl Pts',(10.745164034441,3.18018611901837,-0.525227916032883));
#65378=CARTESIAN_POINT('Ctrl Pts',(10.7573768535991,3.21083602520803,-0.316462106376153));
#65379=CARTESIAN_POINT('Ctrl Pts',(10.7659014796836,3.22225482488633,-0.163389725945583));
#65380=CARTESIAN_POINT('Ctrl Pts',(10.7882859263881,3.22350722279396,0.237111557682078));
#65381=CARTESIAN_POINT('Ctrl Pts',(10.8022022832353,3.19584058820361,0.483529069628185));
#65382=CARTESIAN_POINT('Ctrl Pts',(10.8183046115567,3.13592297253823,0.743291725833529));
#65383=CARTESIAN_POINT('Ctrl Pts',(10.8194842042186,3.13138236488608,0.762194160719128));
#65384=CARTESIAN_POINT('Ctrl Pts',(10.8212382352313,3.12440935112047,0.790108132561338));
#65385=CARTESIAN_POINT('Ctrl Pts',(10.821808427056,3.12210830819242,0.799152278065535));
#65386=CARTESIAN_POINT('Ctrl Pts',(10.8228229683182,3.11795353117459,0.815190587172139));
#65387=CARTESIAN_POINT('Ctrl Pts',(10.8232668073812,3.11611545678689,0.822188770657707));
#65388=CARTESIAN_POINT('Ctrl Pts',(10.8241999260801,3.11220838095086,0.836863046753264));
#65389=CARTESIAN_POINT('Ctrl Pts',(10.8246893612792,3.1101345142624,0.844537782971282));
#65390=CARTESIAN_POINT('Ctrl Pts',(10.8259764372727,3.10461669839605,0.864661527429642));
#65391=CARTESIAN_POINT('Ctrl Pts',(10.8267755864329,3.10112629315396,0.877097547071779));
#65392=CARTESIAN_POINT('Ctrl Pts',(10.8303554819545,3.08520505807529,0.932540301366794));
#65393=CARTESIAN_POINT('Ctrl Pts',(10.8331629000169,3.07195417578322,0.975304506446505));
#65394=CARTESIAN_POINT('Ctrl Pts',(10.8406831837549,3.03447088267411,1.08791959432837));
#65395=CARTESIAN_POINT('Ctrl Pts',(10.845444129525,3.00871946608693,1.1572330658912));
#65396=CARTESIAN_POINT('Ctrl Pts',(10.8699004850444,2.86634931776009,1.50347268331905));
#65397=CARTESIAN_POINT('Ctrl Pts',(10.890712285405,2.71381761622682,1.7639560446698));
#65398=CARTESIAN_POINT('Ctrl Pts',(10.9155966251401,2.4798461379286,2.05970069838304));
#65399=CARTESIAN_POINT('Ctrl Pts',(10.9205758654179,2.4301064643684,2.11815688440933));
#65400=CARTESIAN_POINT('Ctrl Pts',(10.9260970994815,2.37103048902065,2.1827617290786));
#65401=CARTESIAN_POINT('Ctrl Pts',(10.9267758536748,2.36369773219541,2.19070020414672));
#65402=CARTESIAN_POINT('Ctrl Pts',(10.9277763978277,2.35278196808258,2.20239904329441));
#65403=CARTESIAN_POINT('Ctrl Pts',(10.9281004717222,2.34922967206045,2.20618777171223));
#65404=CARTESIAN_POINT('Ctrl Pts',(10.9286749084147,2.34290301571094,2.21290290836365));
#65405=CARTESIAN_POINT('Ctrl Pts',(10.9289255491392,2.34013231224789,2.21583270684163));
#65406=CARTESIAN_POINT('Ctrl Pts',(10.9294591889812,2.33421127349482,2.22207024151147));
#65407=CARTESIAN_POINT('Ctrl Pts',(10.9297420658761,2.33105941349185,2.22537647127609));
#65408=CARTESIAN_POINT('Ctrl Pts',(10.9305085887633,2.32248325499181,2.23433445513798));
#65409=CARTESIAN_POINT('Ctrl Pts',(10.9309911849699,2.3170453190932,2.23997319613711));
#65410=CARTESIAN_POINT('Ctrl Pts',(10.9334182343379,2.28950636297631,2.26832148214583));
#65411=CARTESIAN_POINT('Ctrl Pts',(10.9353390460352,2.26709089235329,2.29072495001229));
#65412=CARTESIAN_POINT('Ctrl Pts',(10.9407546571137,2.20225113750743,2.35364576343924));
#65413=CARTESIAN_POINT('Ctrl Pts',(10.9441969491787,2.15904451397014,2.39334203342413));
#65414=CARTESIAN_POINT('Ctrl Pts',(10.9554913726172,2.01169529692556,2.5214798547272));
#65415=CARTESIAN_POINT('Ctrl Pts',(10.9631176861465,1.90302858750051,2.60446813034321));
#65416=CARTESIAN_POINT('Ctrl Pts',(10.9707498958509,1.78943619500353,2.68030514429072));
#65417=CARTESIAN_POINT('Origin',(-1.72497344927317,0.,0.));
#65418=CARTESIAN_POINT('',(12.4667878339183,1.79025515774613,2.68151164616949));
#65419=CARTESIAN_POINT('',(12.2173276938518,1.7894362103767,2.68030513402722));
#65420=CARTESIAN_POINT('',(-1.72497344927317,1.78943621037804,2.68030513402633));
#65421=CARTESIAN_POINT('',(11.6465734492731,-3.22274887732977,-0.00269001295207406));
#65422=CARTESIAN_POINT('Ctrl Pts',(11.6465747305505,-3.22026798849898,-0.00270873231344248));
#65423=CARTESIAN_POINT('Ctrl Pts',(11.6673417064361,-3.2229090083008,-0.339678147765568));
#65424=CARTESIAN_POINT('Ctrl Pts',(11.7543910885683,-3.01891887064386,-1.7490389311053));
#65425=CARTESIAN_POINT('Ctrl Pts',(11.907722876947,-0.972955838686834,-3.68536392752478));
#65426=CARTESIAN_POINT('Ctrl Pts',(12.1065700956867,2.57407380339523,-2.81117313536718));
#65427=CARTESIAN_POINT('Ctrl Pts',(12.2929250813438,3.68232104515272,0.428156541268224));
#65428=CARTESIAN_POINT('Ctrl Pts',(12.4129976607543,2.50903651599755,2.1911214231777));
#65429=CARTESIAN_POINT('Ctrl Pts',(12.4667878339183,1.79025515774624,2.68151164616941));
#65430=CARTESIAN_POINT('Ctrl Pts',(11.2169460942912,1.78943621037803,2.68030513402633));
#65431=CARTESIAN_POINT('Ctrl Pts',(11.2230963946181,1.70631866388706,2.7357964083296));
#65432=CARTESIAN_POINT('Ctrl Pts',(11.2292466949449,1.62062521831425,2.78741264291572));
#65433=CARTESIAN_POINT('Ctrl Pts',(11.2353969952718,1.53275713616186,2.83492030294414));
#65434=CARTESIAN_POINT('Ctrl Pts',(11.2417123473931,1.44253099279797,2.88370289657322));
#65435=CARTESIAN_POINT('Ctrl Pts',(11.2480276995145,1.35001224982185,2.92815301162533));
#65436=CARTESIAN_POINT('Ctrl Pts',(11.2543430516358,1.255660393657,2.96806915995924));
#65437=CARTESIAN_POINT('Ctrl Pts',(11.2605026451217,1.16363558372603,3.00700083669474));
#65438=CARTESIAN_POINT('Ctrl Pts',(11.2666622386076,1.06986747153118,3.04161951169496));
#65439=CARTESIAN_POINT('Ctrl Pts',(11.2728218320935,0.974799396232359,3.07178835527532));
#65440=CARTESIAN_POINT('Ctrl Pts',(11.2792150635326,0.876125318268297,3.10310152548705));
#65441=CARTESIAN_POINT('Ctrl Pts',(11.2856082949717,0.776051206474808,3.12962045609803));
#65442=CARTESIAN_POINT('Ctrl Pts',(11.2920015264108,0.675084567951585,3.15125028974431));
#65443=CARTESIAN_POINT('Ctrl Pts',(11.2983947578499,0.574117929428362,3.1728801233906));
#65444=CARTESIAN_POINT('Ctrl Pts',(11.304787989289,0.472259284429195,3.18962084680127));
#65445=CARTESIAN_POINT('Ctrl Pts',(11.3111812207281,0.370020441882947,3.20143755758077));
#65446=CARTESIAN_POINT('Ctrl Pts',(11.3173534688209,0.271315505744682,3.21284582134635));
#65447=CARTESIAN_POINT('Ctrl Pts',(11.3235257169136,0.171908744046664,3.21970506464383));
#65448=CARTESIAN_POINT('Ctrl Pts',(11.3296979650064,0.0722555323739138,
3.22193989710258));
#65449=CARTESIAN_POINT('Ctrl Pts',(11.335861853659,-0.0272627130683952,
3.22417170279573));
#65450=CARTESIAN_POINT('Ctrl Pts',(11.3420257423116,-0.127026314615012,
3.22179153662295));
#65451=CARTESIAN_POINT('Ctrl Pts',(11.3481896309643,-0.226573308854009,
3.21477559064625));
#65452=CARTESIAN_POINT('Ctrl Pts',(11.3543469926228,-0.32601489193455,3.20776707391438));
#65453=CARTESIAN_POINT('Ctrl Pts',(11.3605043542813,-0.425239892800191,
3.19613256703912));
#65454=CARTESIAN_POINT('Ctrl Pts',(11.3666617159398,-0.523785840049014,
3.17990030602598));
#65455=CARTESIAN_POINT('Ctrl Pts',(11.3728145800861,-0.622259806532849,
3.16367990151835));
#65456=CARTESIAN_POINT('Ctrl Pts',(11.3789674442324,-0.720055278225169,
3.14286849019346));
#65457=CARTESIAN_POINT('Ctrl Pts',(11.3851203083787,-0.816715322076124,
3.11754609351427));
#65458=CARTESIAN_POINT('Ctrl Pts',(11.3912708415153,-0.913338746313807,
3.09223329021345));
#65459=CARTESIAN_POINT('Ctrl Pts',(11.3974213746518,-1.00882717769941,3.06241300725973));
#65460=CARTESIAN_POINT('Ctrl Pts',(11.4035719077884,-1.10273516554363,3.02821609486071));
#65461=CARTESIAN_POINT('Ctrl Pts',(11.4097217560036,-1.19663269582537,2.99402299061855));
#65462=CARTESIAN_POINT('Ctrl Pts',(11.4158716042188,-1.28894972431919,2.95545437454502));
#65463=CARTESIAN_POINT('Ctrl Pts',(11.422021452434,-1.37925818446261,2.91269023809483));
#65464=CARTESIAN_POINT('Ctrl Pts',(11.4281722608131,-1.46958074429175,2.86991942496248));
#65465=CARTESIAN_POINT('Ctrl Pts',(11.4343230691923,-1.55789372027088,2.8229519762973));
#65466=CARTESIAN_POINT('Ctrl Pts',(11.4404738775714,-1.64379208487014,2.77201463636437));
#65467=CARTESIAN_POINT('Ctrl Pts',(11.4466312639376,-1.72978231354553,2.72102282145167));
#65468=CARTESIAN_POINT('Ctrl Pts',(11.4527886503038,-1.81335239988673,2.66605285922856));
#65469=CARTESIAN_POINT('Ctrl Pts',(11.45894603667,-1.89412495974367,2.60737573038027));
#65470=CARTESIAN_POINT('Ctrl Pts',(11.465106859407,-1.97494259789311,2.54866585446068));
#65471=CARTESIAN_POINT('Ctrl Pts',(11.4712676821439,-2.05295926112704,2.48624496305228));
#65472=CARTESIAN_POINT('Ctrl Pts',(11.4774285048809,-2.127831066487,2.42042403619548));
#65473=CARTESIAN_POINT('Ctrl Pts',(11.4835996277976,-2.20282804880539,2.35449306439738));
#65474=CARTESIAN_POINT('Ctrl Pts',(11.4897707507142,-2.27466935819926,2.28515100441456));
#65475=CARTESIAN_POINT('Ctrl Pts',(11.4959418736309,-2.34304826231248,2.21274544468506));
#65476=CARTESIAN_POINT('Ctrl Pts',(11.5006373955765,-2.39507682327521,2.1576530572407));
#65477=CARTESIAN_POINT('Ctrl Pts',(11.5053329175221,-2.44510160318005,2.10078782162479));
#65478=CARTESIAN_POINT('Ctrl Pts',(11.5100284394677,-2.49300396984336,2.04231456167879));
#65479=CARTESIAN_POINT('Ctrl Pts',(11.5161753576691,-2.55571306436904,1.96576708729302));
#65480=CARTESIAN_POINT('Ctrl Pts',(11.5223222758705,-2.61501043062012,1.8861856458203));
#65481=CARTESIAN_POINT('Ctrl Pts',(11.5284691940719,-2.67058657367766,1.80390823352869));
#65482=CARTESIAN_POINT('Ctrl Pts',(11.5346081463955,-2.72609069482889,1.72173744569416));
#65483=CARTESIAN_POINT('Ctrl Pts',(11.5407470987191,-2.77788292895277,1.6368779856665));
#65484=CARTESIAN_POINT('Ctrl Pts',(11.5468860510426,-2.82569326207592,1.54970163294705));
#65485=CARTESIAN_POINT('Ctrl Pts',(11.5530187220747,-2.87345467632444,1.46261447787151));
#65486=CARTESIAN_POINT('Ctrl Pts',(11.5591513931068,-2.91724207532969,1.37321552164076));
#65487=CARTESIAN_POINT('Ctrl Pts',(11.5652840641389,-2.95682870747237,1.28190544002561));
#65488=CARTESIAN_POINT('Ctrl Pts',(11.5714121324141,-2.99638562863891,1.19066388941475));
#65489=CARTESIAN_POINT('Ctrl Pts',(11.5775402006893,-3.03174787601952,1.09751446474921));
#65490=CARTESIAN_POINT('Ctrl Pts',(11.5836682689645,-3.06273511933149,1.00288142435361));
#65491=CARTESIAN_POINT('Ctrl Pts',(11.5897941624647,-3.09371136565719,0.908281968044084));
#65492=CARTESIAN_POINT('Ctrl Pts',(11.5959200559648,-3.12031555343767,0.812200356622423));
#65493=CARTESIAN_POINT('Ctrl Pts',(11.602045949465,-3.14241621670073,0.715078935164695));
#65494=CARTESIAN_POINT('Ctrl Pts',(11.6081705753739,-3.16451230681726,0.61797761041113));
#65495=CARTESIAN_POINT('Ctrl Pts',(11.6142952012828,-3.18210663260681,0.519837331328192));
#65496=CARTESIAN_POINT('Ctrl Pts',(11.6204198271917,-3.19511844360702,0.421112447954533));
#65497=CARTESIAN_POINT('Ctrl Pts',(11.6265465006768,-3.20813460469738,0.322354559018285));
#65498=CARTESIAN_POINT('Ctrl Pts',(11.6326731741619,-3.21656513731015,0.223012110210783));
#65499=CARTESIAN_POINT('Ctrl Pts',(11.638799847647,-3.2203810356016,0.123545732575258));
#65500=CARTESIAN_POINT('Ctrl Pts',(11.641391048189,-3.22199492244333,0.081477662150113));
#65501=CARTESIAN_POINT('Ctrl Pts',(11.6439822487311,-3.22278399919107,0.0393874569608355));
#65502=CARTESIAN_POINT('Ctrl Pts',(11.6465734492731,-3.22274887732977,-0.00269001295207406));
#65503=CARTESIAN_POINT('',(11.3976152427918,-3.22274951656853,0.0017652074350194));
#65504=CARTESIAN_POINT('Ctrl Pts',(10.9707498958509,1.78943619500353,2.68030514429072));
#65505=CARTESIAN_POINT('Ctrl Pts',(10.9718368339688,1.77325897948024,2.6911054425528));
#65506=CARTESIAN_POINT('Ctrl Pts',(10.9729237869157,1.75698185694029,2.70176070299239));
#65507=CARTESIAN_POINT('Ctrl Pts',(10.9875885956393,1.53619922227114,2.84344859257259));
#65508=CARTESIAN_POINT('Ctrl Pts',(11.0012823145276,1.31765202879979,2.95108085726157));
#65509=CARTESIAN_POINT('Ctrl Pts',(11.0171292205013,1.07071394942961,3.03974852536468));
#65510=CARTESIAN_POINT('Ctrl Pts',(11.0183149464139,1.05226214588065,3.04618512393336));
#65511=CARTESIAN_POINT('Ctrl Pts',(11.0200702493911,1.0249902733019,3.05542110014015));
#65512=CARTESIAN_POINT('Ctrl Pts',(11.0206355003337,1.01621462759011,3.05835102422926));
#65513=CARTESIAN_POINT('Ctrl Pts',(11.0216456627691,1.00054408801691,3.06350805268522));
#65514=CARTESIAN_POINT('Ctrl Pts',(11.022090087887,0.993654043688113,3.06574977795534));
#65515=CARTESIAN_POINT('Ctrl Pts',(11.0230044453405,0.979487662776576,3.07030613838045));
#65516=CARTESIAN_POINT('Ctrl Pts',(11.0234744596856,0.972210547718029,3.07261818555624));
#65517=CARTESIAN_POINT('Ctrl Pts',(11.0246938897476,0.953343721318345,3.07853872057092));
#65518=CARTESIAN_POINT('Ctrl Pts',(11.0254446014442,0.941741796796257,3.08210760466307));
#65519=CARTESIAN_POINT('Ctrl Pts',(11.0270846667164,0.916425070743717,3.08973902594954));
#65520=CARTESIAN_POINT('Ctrl Pts',(11.0279748425143,0.902702878308592,3.09377595530366));
#65521=CARTESIAN_POINT('Ctrl Pts',(11.0305656686192,0.862822576045433,3.10522042298376));
#65522=CARTESIAN_POINT('Ctrl Pts',(11.0322740408339,0.836597534483415,3.11238833782364));
#65523=CARTESIAN_POINT('Ctrl Pts',(11.0518854871312,0.536413459545543,3.19036762710496));
#65524=CARTESIAN_POINT('Ctrl Pts',(11.0710092006518,0.254411689949558,3.22511944150195));
#65525=CARTESIAN_POINT('Ctrl Pts',(11.0975325258762,-0.137952484776181,
3.22165853962935));
#65526=CARTESIAN_POINT('Ctrl Pts',(11.1048982611787,-0.247365993983254,
3.21510927837613));
#65527=CARTESIAN_POINT('Ctrl Pts',(11.1124168568245,-0.361312424122708,
3.20243609595026));
#65528=CARTESIAN_POINT('Ctrl Pts',(11.1127511832243,-0.36638413259871,3.2018598164832));
#65529=CARTESIAN_POINT('Ctrl Pts',(11.1169490120882,-0.430129084324271,
3.19446327175443));
#65530=CARTESIAN_POINT('Ctrl Pts',(11.1207552645447,-0.488610045497838,
3.18604267260742));
#65531=CARTESIAN_POINT('Ctrl Pts',(11.1251057086072,-0.556648412653623,
3.17432817338858));
#65532=CARTESIAN_POINT('Ctrl Pts',(11.1257310630043,-0.566458405833313,
3.17259226631824));
#65533=CARTESIAN_POINT('Ctrl Pts',(11.1266721999898,-0.581269898261237,
3.16990043887911));
#65534=CARTESIAN_POINT('Ctrl Pts',(11.1269898501709,-0.58627733014959,3.16897812867731));
#65535=CARTESIAN_POINT('Ctrl Pts',(11.127557229945,-0.595236781301901,3.16730593989917));
#65536=CARTESIAN_POINT('Ctrl Pts',(11.1278072116061,-0.599189586693744,
3.16656052879805));
#65537=CARTESIAN_POINT('Ctrl Pts',(11.1283442581897,-0.60769320316757,3.16494044296602));
#65538=CARTESIAN_POINT('Ctrl Pts',(11.1286311825967,-0.612243509586681,
3.16406335624155));
#65539=CARTESIAN_POINT('Ctrl Pts',(11.1294200968633,-0.624773891949282,
3.16162004048108));
#65540=CARTESIAN_POINT('Ctrl Pts',(11.1299209303861,-0.632750023117147,
3.16003340299419));
#65541=CARTESIAN_POINT('Ctrl Pts',(11.1326027023724,-0.675567655438603,
3.15134736687674));
#65542=CARTESIAN_POINT('Ctrl Pts',(11.1347536571604,-0.710297485816712,
3.14370157835538));
#65543=CARTESIAN_POINT('Ctrl Pts',(11.1410163408013,-0.812267226869926,
3.11947666494039));
#65544=CARTESIAN_POINT('Ctrl Pts',(11.145053734089,-0.879110470177674,3.10130275835436));
#65545=CARTESIAN_POINT('Ctrl Pts',(11.1577397054458,-1.09029099463534,3.03650754478775));
#65546=CARTESIAN_POINT('Ctrl Pts',(11.1661509258008,-1.23194855734697,2.98184841461059));
#65547=CARTESIAN_POINT('Ctrl Pts',(11.1876080596871,-1.57918355028459,2.81887988327354));
#65548=CARTESIAN_POINT('Ctrl Pts',(11.2007322267722,-1.77784822848497,2.69798787723824));
#65549=CARTESIAN_POINT('Ctrl Pts',(11.2158089183299,-1.97592310769465,2.54600900866633));
#65550=CARTESIAN_POINT('Ctrl Pts',(11.2168876356507,-1.98994601667987,2.53506387115332));
#65551=CARTESIAN_POINT('Ctrl Pts',(11.2185269142277,-2.01102696603919,2.51832711156122));
#65552=CARTESIAN_POINT('Ctrl Pts',(11.2190840778183,-2.01815234209973,2.51262054842001));
#65553=CARTESIAN_POINT('Ctrl Pts',(11.2200556580019,-2.03050804388148,2.50263866345888));
#65554=CARTESIAN_POINT('Ctrl Pts',(11.2204695220742,-2.03574937626996,2.4983770075835));
#65555=CARTESIAN_POINT('Ctrl Pts',(11.2213041390252,-2.0462751502121,2.48976353007093));
#65556=CARTESIAN_POINT('Ctrl Pts',(11.2217249077217,-2.05155920084512,2.48541128796058));
#65557=CARTESIAN_POINT('Ctrl Pts',(11.2227338125685,-2.06417510733382,2.47495247128393));
#65558=CARTESIAN_POINT('Ctrl Pts',(11.2233225910699,-2.07149375642266,2.46883013243413));
#65559=CARTESIAN_POINT('Ctrl Pts',(11.225191312501,-2.09458314865225,2.44933999474911));
#65560=CARTESIAN_POINT('Ctrl Pts',(11.2264761514391,-2.11025225930368,2.43585310445739));
#65561=CARTESIAN_POINT('Ctrl Pts',(11.2294840622157,-2.14645148418414,2.404083873935));
#65562=CARTESIAN_POINT('Ctrl Pts',(11.2312118246945,-2.16687934674344,2.38568796537753));
#65563=CARTESIAN_POINT('Ctrl Pts',(11.237176870011,-2.23614780132993,2.32168596204598));
#65564=CARTESIAN_POINT('Ctrl Pts',(11.2414664326412,-2.28380137768591,2.2748259112261));
#65565=CARTESIAN_POINT('Ctrl Pts',(11.2552982617909,-2.43068994919603,2.1211131561897));
#65566=CARTESIAN_POINT('Ctrl Pts',(11.2650488663257,-2.52413955721057,2.00900135770178));
#65567=CARTESIAN_POINT('Ctrl Pts',(11.2838536365566,-2.68748177603925,1.7835764632471));
#65568=CARTESIAN_POINT('Ctrl Pts',(11.2928713978114,-2.75859073274239,1.67149084831187));
#65569=CARTESIAN_POINT('Ctrl Pts',(11.3035754993457,-2.83595355167587,1.53109484604014));
#65570=CARTESIAN_POINT('Ctrl Pts',(11.3054163610485,-2.84900159904479,1.50667645141132));
#65571=CARTESIAN_POINT('Ctrl Pts',(11.3126311950841,-2.89917968335977,1.40978889754674));
#65572=CARTESIAN_POINT('Ctrl Pts',(11.3179253588035,-2.93387582409759,1.33608486955994));
#65573=CARTESIAN_POINT('Ctrl Pts',(11.3237545640332,-2.97003741146751,1.25104581404986));
#65574=CARTESIAN_POINT('Ctrl Pts',(11.3244435323143,-2.97427788081487,1.24093067906316));
#65575=CARTESIAN_POINT('Ctrl Pts',(11.3254527073168,-2.98044087341587,1.22601651032825));
#65576=CARTESIAN_POINT('Ctrl Pts',(11.3257752924799,-2.98240356605414,1.22123431560168));
#65577=CARTESIAN_POINT('Ctrl Pts',(11.3263487229751,-2.98587955837324,1.21270653676102));
#65578=CARTESIAN_POINT('Ctrl Pts',(11.3265998383929,-2.98739732881588,1.20896281245088));
#65579=CARTESIAN_POINT('Ctrl Pts',(11.3271317027224,-2.9906026122995,1.20101378401744));
#65580=CARTESIAN_POINT('Ctrl Pts',(11.3274123398188,-2.99228829153394,1.19680778533733));
#65581=CARTESIAN_POINT('Ctrl Pts',(11.3281665194033,-2.99680308307457,1.1854736007213));
#65582=CARTESIAN_POINT('Ctrl Pts',(11.3286390689375,-2.99961565315903,1.1783387937617));
#65583=CARTESIAN_POINT('Ctrl Pts',(11.3309374204723,-3.01321363547832,1.14347981896391));
#65584=CARTESIAN_POINT('Ctrl Pts',(11.3327424821882,-3.02364071801884,1.11561618237339));
#65585=CARTESIAN_POINT('Ctrl Pts',(11.3377492264172,-3.05178482937016,1.03711361747349));
#65586=CARTESIAN_POINT('Ctrl Pts',(11.3409074667142,-3.06862616184151,0.986169078056509));
#65587=CARTESIAN_POINT('Ctrl Pts',(11.3623755437678,-3.17588836406284,0.632287999099733));
#65588=CARTESIAN_POINT('Ctrl Pts',(11.3792697007114,-3.2225763519801,0.317912807196488));
#65589=CARTESIAN_POINT('Ctrl Pts',(11.3976152427918,-3.22274951656853,0.0017652074350194));
#65590=CARTESIAN_POINT('Ctrl Pts',(11.3976154732117,-3.22274951874103,0.00176123662453421));
#65591=CARTESIAN_POINT('Ctrl Pts',(11.4030792833307,-3.22280097590727,-0.0923962181032172));
#65592=CARTESIAN_POINT('Ctrl Pts',(11.4086442726123,-3.21872604207397,-0.186504860719464));
#65593=CARTESIAN_POINT('Ctrl Pts',(11.4150735136718,-3.20948468991639,-0.292356193350574));
#65594=CARTESIAN_POINT('Ctrl Pts',(11.4158081189327,-3.20836384239092,-0.304410195696163));
#65595=CARTESIAN_POINT('Ctrl Pts',(11.4170449194469,-3.20636824705999,-0.324634789139963));
#65596=CARTESIAN_POINT('Ctrl Pts',(11.4175459637667,-3.20553011141684,-0.332808931539696));
#65597=CARTESIAN_POINT('Ctrl Pts',(11.4184631617949,-3.2039417628058,-0.347736852810806));
#65598=CARTESIAN_POINT('Ctrl Pts',(11.41887900224,-3.20320143059321,-0.354491653189587));
#65599=CARTESIAN_POINT('Ctrl Pts',(11.4196944510381,-3.20171021030252,-0.367711368535341));
#65600=CARTESIAN_POINT('Ctrl Pts',(11.420094001709,-3.2009610903856,-0.374176453233502));
#65601=CARTESIAN_POINT('Ctrl Pts',(11.4210105781851,-3.19920042452651,-0.388979105426583));
#65602=CARTESIAN_POINT('Ctrl Pts',(11.4215280130225,-3.19817586278079,-0.397315050482128));
#65603=CARTESIAN_POINT('Ctrl Pts',(11.4229443857749,-3.19528796698414,-0.420076095344427));
#65604=CARTESIAN_POINT('Ctrl Pts',(11.4238453764884,-3.1933595606329,-0.4344926042981));
#65605=CARTESIAN_POINT('Ctrl Pts',(11.4282934748942,-3.18339222412179,-0.505353428532012));
#65606=CARTESIAN_POINT('Ctrl Pts',(11.431884648095,-3.17395443872685,-0.561587652131957));
#65607=CARTESIAN_POINT('Ctrl Pts',(11.436089493383,-3.16132581214271,-0.626271369944102));
#65608=CARTESIAN_POINT('Ctrl Pts',(11.4366582334135,-3.15958483873269,-0.634996349361112));
#65609=CARTESIAN_POINT('Ctrl Pts',(11.440006725582,-3.14914215379932,-0.686224060302044));
#65610=CARTESIAN_POINT('Ctrl Pts',(11.442810917839,-3.13961935580033,-0.728553217834638));
#65611=CARTESIAN_POINT('Ctrl Pts',(11.455929507767,-3.09148973603396,-0.923978321230943));
#65612=CARTESIAN_POINT('Ctrl Pts',(11.4665281641835,-3.04252339067055,-1.07428438254756));
#65613=CARTESIAN_POINT('Ctrl Pts',(11.4910622932218,-2.90517930777043,-1.40996812232759));
#65614=CARTESIAN_POINT('Ctrl Pts',(11.5050073547806,-2.80970595055505,-1.59174251365625));
#65615=CARTESIAN_POINT('Ctrl Pts',(11.5197868151541,-2.68333164367721,-1.78508551439961));
#65616=CARTESIAN_POINT('Ctrl Pts',(11.521442551638,-2.66878384496777,-1.80676282240783));
#65617=CARTESIAN_POINT('Ctrl Pts',(11.5235415179782,-2.6498160353469,-1.83429720984378));
#65618=CARTESIAN_POINT('Ctrl Pts',(11.5240002692345,-2.64563773796944,-1.84031851513517));
#65619=CARTESIAN_POINT('Ctrl Pts',(11.5247356574136,-2.63888650232743,-1.84997714550969));
#65620=CARTESIAN_POINT('Ctrl Pts',(11.525013167092,-2.63632652874139,-1.8536234368134));
#65621=CARTESIAN_POINT('Ctrl Pts',(11.5255425405405,-2.63141944797384,-1.86058209483606));
#65622=CARTESIAN_POINT('Ctrl Pts',(11.525794488299,-2.62907365017095,-1.86389532563395));
#65623=CARTESIAN_POINT('Ctrl Pts',(11.526375096267,-2.62364404829406,-1.87153351160692));
#65624=CARTESIAN_POINT('Ctrl Pts',(11.5267034491326,-2.62055578809358,-1.87585530882985));
#65625=CARTESIAN_POINT('Ctrl Pts',(11.5277542090972,-2.61061700614116,-1.88969147247413));
#65626=CARTESIAN_POINT('Ctrl Pts',(11.5284738159496,-2.60372515030398,-1.89917623337547));
#65627=CARTESIAN_POINT('Ctrl Pts',(11.5409088711975,-2.4831811780661,-2.06318259227469));
#65628=CARTESIAN_POINT('Ctrl Pts',(11.551723860799,-2.3559893126563,-2.20731713202712));
#65629=CARTESIAN_POINT('Ctrl Pts',(11.5716761621756,-2.09726358159207,-2.4524849316899));
#65630=CARTESIAN_POINT('Ctrl Pts',(11.5808062213939,-1.96932393292658,-2.55635631036144));
#65631=CARTESIAN_POINT('Ctrl Pts',(11.5951825475722,-1.76287525931155,-2.69923579317916));
#65632=CARTESIAN_POINT('Ctrl Pts',(11.6002083844087,-1.68978363771895,-2.74558419614712));
#65633=CARTESIAN_POINT('Ctrl Pts',(11.6072971642213,-1.58631966490739,-2.80549455872093));
#65634=CARTESIAN_POINT('Ctrl Pts',(11.60927117705,-1.55746718152246,-2.82161401652705));
#65635=CARTESIAN_POINT('Ctrl Pts',(11.6122528586553,-1.51386493772445,-2.84510141472059));
#65636=CARTESIAN_POINT('Ctrl Pts',(11.613248771968,-1.49929769998549,-2.85280484805979));
#65637=CARTESIAN_POINT('Ctrl Pts',(11.61507719748,-1.47255171575014,-2.86668719804918));
#65638=CARTESIAN_POINT('Ctrl Pts',(11.6159084616364,-1.46039148888122,-2.87290110119645));
#65639=CARTESIAN_POINT('Ctrl Pts',(11.6172348221687,-1.44098995887658,-2.88266031635028));
#65640=CARTESIAN_POINT('Ctrl Pts',(11.61772814228,-1.43377412030901,-2.88625610975673));
#65641=CARTESIAN_POINT('Ctrl Pts',(11.6182245488201,-1.42651366986361,-2.8898401882122));
#65642=CARTESIAN_POINT('Ctrl Pts',(11.6182266852154,-1.42648242291999,-2.88985561245097));
#65643=CARTESIAN_POINT('Ctrl Pts',(11.6182309903186,-1.42641945644778,-2.88988669293767));
#65644=CARTESIAN_POINT('Ctrl Pts',(11.6182331590115,-1.42638773713914,-2.88990234905786));
#65645=CARTESIAN_POINT('Ctrl Pts',(11.6182375292541,-1.42632381797779,-2.889933897178));
#65646=CARTESIAN_POINT('Ctrl Pts',(11.6182397307896,-1.42629161833368,-2.88994978905521));
#65647=CARTESIAN_POINT('Ctrl Pts',(11.6182441672579,-1.42622673059869,-2.88998181253002));
#65648=CARTESIAN_POINT('Ctrl Pts',(11.6182464021847,-1.42619404259534,-2.889997944064));
#65649=CARTESIAN_POINT('Ctrl Pts',(11.6182509060011,-1.42612816987234,-2.89003045087171));
#65650=CARTESIAN_POINT('Ctrl Pts',(11.6182531748815,-1.42609498528727,-2.89004682605797));
#65651=CARTESIAN_POINT('Ctrl Pts',(11.6182577471864,-1.4260281108968,-2.890079824303));
#65652=CARTESIAN_POINT('Ctrl Pts',(11.6182600505973,-1.42599442129138,-2.89009644724134));
#65653=CARTESIAN_POINT('Ctrl Pts',(11.618264692537,-1.42592652847227,-2.89012994506363));
#65654=CARTESIAN_POINT('Ctrl Pts',(11.6182670310597,-1.42589232534842,-2.89014681988077));
#65655=CARTESIAN_POINT('Ctrl Pts',(11.6182717438154,-1.42582339682499,-2.89018082566915));
#65656=CARTESIAN_POINT('Ctrl Pts',(11.6182741180425,-1.42578867151328,-2.89019795657384));
#65657=CARTESIAN_POINT('Ctrl Pts',(11.618278902819,-1.42571868966853,-2.89023247888041));
#65658=CARTESIAN_POINT('Ctrl Pts',(11.6182813133581,-1.42568343328511,-2.89024987018454));
#65659=CARTESIAN_POINT('Ctrl Pts',(11.6182861713715,-1.42561238033184,-2.89028491764006));
#65660=CARTESIAN_POINT('Ctrl Pts',(11.6182886188383,-1.42557658387282,-2.89030257371206));
#65661=CARTESIAN_POINT('Ctrl Pts',(11.6182935513334,-1.42550444161099,-2.89033815514544));
#65662=CARTESIAN_POINT('Ctrl Pts',(11.6182960363549,-1.42546809590557,-2.89035608043327));
#65663=CARTESIAN_POINT('Ctrl Pts',(11.6183010445995,-1.42539484579282,-2.89039220483662));
#65664=CARTESIAN_POINT('Ctrl Pts',(11.6183035678154,-1.42535794148883,-2.89041040387482));
#65665=CARTESIAN_POINT('Ctrl Pts',(11.6183086530986,-1.4252835646723,-2.89044708038748));
#65666=CARTESIAN_POINT('Ctrl Pts',(11.61831121516,-1.42524609224698,-2.89046555779173));
#65667=CARTESIAN_POINT('Ctrl Pts',(11.6183163787931,-1.42517056955159,-2.89050279570591));
#65668=CARTESIAN_POINT('Ctrl Pts',(11.6183189803616,-1.42513251932988,-2.8905215561639));
#65669=CARTESIAN_POINT('Ctrl Pts',(11.6183242236813,-1.42505583120969,-2.8905593649484));
#65670=CARTESIAN_POINT('Ctrl Pts',(11.6183268654291,-1.42501719336021,-2.89057841322173));
#65671=CARTESIAN_POINT('Ctrl Pts',(11.6183321898058,-1.42493931977284,-2.89061680258362));
#65672=CARTESIAN_POINT('Ctrl Pts',(11.6183348724246,-1.42490008418203,-2.8906361435697));
#65673=CARTESIAN_POINT('Ctrl Pts',(11.6183402792324,-1.42482100503457,-2.89067512323426));
#65674=CARTESIAN_POINT('Ctrl Pts',(11.6183430034191,-1.42478116151051,-2.89069476186572));
#65675=CARTESIAN_POINT('Ctrl Pts',(11.6183484940705,-1.42470085614672,-2.89073434182901));
#65676=CARTESIAN_POINT('Ctrl Pts',(11.6183512605342,-1.42466039432034,-2.89075428312228));
#65677=CARTESIAN_POINT('Ctrl Pts',(11.6183568364996,-1.42457884123547,-2.89079447379136));
#65678=CARTESIAN_POINT('Ctrl Pts',(11.6183596459939,-1.42453775008669,-2.89081472308002));
#65679=CARTESIAN_POINT('Ctrl Pts',(11.6183652768917,-1.42445539364287,-2.89085530529253));
#65680=CARTESIAN_POINT('Ctrl Pts',(11.6183680983677,-1.42441412728829,-2.89087563872917));
#65681=CARTESIAN_POINT('Ctrl Pts',(11.6183739319694,-1.42432880620964,-2.89091767726326));
#65682=CARTESIAN_POINT('Ctrl Pts',(11.6183769440835,-1.4242847516575,-2.89093938212267));
#65683=CARTESIAN_POINT('Ctrl Pts',(11.6183831719932,-1.4241936635957,-2.89098425693097));
#65684=CARTESIAN_POINT('Ctrl Pts',(11.618386387773,-1.42414663031743,-2.89100742659102));
#65685=CARTESIAN_POINT('Ctrl Pts',(11.6183930369296,-1.42404938128599,-2.89105533072135));
#65686=CARTESIAN_POINT('Ctrl Pts',(11.6183964702986,-1.42399916564901,-2.89108006493495));
#65687=CARTESIAN_POINT('Ctrl Pts',(11.618403569509,-1.42389533434632,-2.89113120471877));
#65688=CARTESIAN_POINT('Ctrl Pts',(11.6184072353477,-1.42384171872246,-2.8911576100409));
#65689=CARTESIAN_POINT('Ctrl Pts',(11.6188556032743,-1.41728400732104,-2.89438701066855));
#65690=CARTESIAN_POINT('Ctrl Pts',(11.619301071121,-1.41076916561674,-2.89756802938455));
#65691=CARTESIAN_POINT('Ctrl Pts',(11.6203186765309,-1.39588840160288,-2.90477181616293));
#65692=CARTESIAN_POINT('Ctrl Pts',(11.6208913017214,-1.38751574950751,-2.90878046192627));
#65693=CARTESIAN_POINT('Ctrl Pts',(11.6226833516792,-1.36131748750213,-2.92118477677408));
#65694=CARTESIAN_POINT('Ctrl Pts',(11.6239071737684,-1.34343238389581,-2.92945305542688));
#65695=CARTESIAN_POINT('Ctrl Pts',(11.6356827956183,-1.17142594406243,-3.00706513261379));
#65696=CARTESIAN_POINT('Ctrl Pts',(11.646650579351,-1.01217578535702,-3.064337342645));
#65697=CARTESIAN_POINT('Ctrl Pts',(11.6701116120815,-0.672518935328235,
-3.15711548937967));
#65698=CARTESIAN_POINT('Ctrl Pts',(11.6826159514843,-0.492056530533508,
-3.190224904393));
#65699=CARTESIAN_POINT('Ctrl Pts',(11.7034103860448,-0.183907028303194,
-3.21998227296595));
#65700=CARTESIAN_POINT('Ctrl Pts',(11.7117821620842,-0.0574185693492307,
-3.22471988302917));
#65701=CARTESIAN_POINT('Ctrl Pts',(11.7207068582696,0.0834890059778667,
-3.22170082170197));
#65702=CARTESIAN_POINT('Ctrl Pts',(11.7216175048805,0.0979418457486973,
-3.22129384130052));
#65703=CARTESIAN_POINT('Ctrl Pts',(11.7228890511351,0.118235853103794,-3.2205856672979));
#65704=CARTESIAN_POINT('Ctrl Pts',(11.7232543552747,0.124079422455464,-3.22036582635705));
#65705=CARTESIAN_POINT('Ctrl Pts',(11.7238764975805,0.134054811634172,-3.21996334986497));
#65706=CARTESIAN_POINT('Ctrl Pts',(11.7241337805494,0.138186921520019,-3.21978866424567));
#65707=CARTESIAN_POINT('Ctrl Pts',(11.7246252767023,0.14609398827626,-3.21943914207546));
#65708=CARTESIAN_POINT('Ctrl Pts',(11.7248595646832,0.149868975183894,-3.21926562022571));
#65709=CARTESIAN_POINT('Ctrl Pts',(11.7254129406066,0.158798792764812,-3.21883940912449));
#65710=CARTESIAN_POINT('Ctrl Pts',(11.7257317057489,0.163953358006502,-3.21858097545954));
#65711=CARTESIAN_POINT('Ctrl Pts',(11.7266793887766,0.179308656952439,-3.2177741254784));
#65712=CARTESIAN_POINT('Ctrl Pts',(11.7273063229699,0.189507544197452,-3.2171895832011));
#65713=CARTESIAN_POINT('Ctrl Pts',(11.7337090286984,0.294059267496227,-3.2106983683862));
#65714=CARTESIAN_POINT('Ctrl Pts',(11.7392677841558,0.38812170402163,-3.20069057901056));
#65715=CARTESIAN_POINT('Ctrl Pts',(11.7611131741272,0.763381562901674,-3.14397374492723));
#65716=CARTESIAN_POINT('Ctrl Pts',(11.7764741001173,1.03825792402893,-3.06420658437873));
#65717=CARTESIAN_POINT('Ctrl Pts',(11.7970687682451,1.36478608382635,-2.92038216434556));
#65718=CARTESIAN_POINT('Ctrl Pts',(11.8012685460282,1.42950656879135,-2.88925300980226));
#65719=CARTESIAN_POINT('Ctrl Pts',(11.8072622704578,1.51878196931448,-2.84257924121321));
#65720=CARTESIAN_POINT('Ctrl Pts',(11.8089957409726,1.54425101628792,-2.82882380698595));
#65721=CARTESIAN_POINT('Ctrl Pts',(11.8116437641757,1.58260276374439,-2.807438345634));
#65722=CARTESIAN_POINT('Ctrl Pts',(11.8125494998335,1.59562369186246,-2.80005831987655));
#65723=CARTESIAN_POINT('Ctrl Pts',(11.8142257945611,1.61954036245628,-2.78628178738399));
#65724=CARTESIAN_POINT('Ctrl Pts',(11.8149954072263,1.6304508486999,-2.77991136678741));
#65725=CARTESIAN_POINT('Ctrl Pts',(11.8162454066413,1.64805683454,-2.76949227278751));
#65726=CARTESIAN_POINT('Ctrl Pts',(11.8167243538346,1.65477561402784,-2.7654830399795));
#65727=CARTESIAN_POINT('Ctrl Pts',(11.8176474422113,1.66767245046208,-2.75772340780324));
#65728=CARTESIAN_POINT('Ctrl Pts',(11.8180914493801,1.67385262838838,-2.75397661084079));
#65729=CARTESIAN_POINT('Ctrl Pts',(11.8191064903596,1.68792779920184,-2.74537851181137));
#65730=CARTESIAN_POINT('Ctrl Pts',(11.8196780121361,1.69581454967065,-2.74051390047317));
#65731=CARTESIAN_POINT('Ctrl Pts',(11.8214316948556,1.71989659673098,-2.72551613957464));
#65732=CARTESIAN_POINT('Ctrl Pts',(11.8226179187405,1.73602263766676,-2.71527308142578));
#65733=CARTESIAN_POINT('Ctrl Pts',(11.8400198874576,1.97018231416575,-2.56359913336304));
#65734=CARTESIAN_POINT('Ctrl Pts',(11.8572762406115,2.17037034543168,-2.39647568615865));
#65735=CARTESIAN_POINT('Ctrl Pts',(11.8887207414989,2.48874109729795,-2.05775185658825));
#65736=CARTESIAN_POINT('Ctrl Pts',(11.9026829934451,2.61462272152304,-1.89524083545589));
#65737=CARTESIAN_POINT('Ctrl Pts',(11.9174788617099,2.7381668774314,-1.69977701998558));
#65738=CARTESIAN_POINT('Ctrl Pts',(11.9191355373413,2.75185340937114,-1.67752874304802));
#65739=CARTESIAN_POINT('Ctrl Pts',(11.9212355165374,2.7690331145288,-1.64882591778891));
#65740=CARTESIAN_POINT('Ctrl Pts',(11.9216943595615,2.77277635363194,-1.64252323933809));
#65741=CARTESIAN_POINT('Ctrl Pts',(11.9224298595712,2.77876017988937,-1.63236922190783));
#65742=CARTESIAN_POINT('Ctrl Pts',(11.9227073897806,2.78101431474668,-1.62852595795106));
#65743=CARTESIAN_POINT('Ctrl Pts',(11.9232367776326,2.78530699158226,-1.6211721082669));
#65744=CARTESIAN_POINT('Ctrl Pts',(11.9234887193588,2.78734686483042,-1.61766235576016));
#65745=CARTESIAN_POINT('Ctrl Pts',(11.9240692803987,2.79204022854193,-1.60955184208211));
#65746=CARTESIAN_POINT('Ctrl Pts',(11.92439759253,2.79468899824165,-1.60494834004477));
#65747=CARTESIAN_POINT('Ctrl Pts',(11.9252776609965,2.80177433085987,-1.59256346597219));
#65748=CARTESIAN_POINT('Ctrl Pts',(11.9258280836053,2.80618989201173,-1.58477004281781));
#65749=CARTESIAN_POINT('Ctrl Pts',(11.9298283319623,2.83815844446283,-1.52779329544939));
#65750=CARTESIAN_POINT('Ctrl Pts',(11.9332015567738,2.86445112991647,-1.47790945149096));
#65751=CARTESIAN_POINT('Ctrl Pts',(11.9552060438616,3.03012217461485,-1.1425389407093));
#65752=CARTESIAN_POINT('Ctrl Pts',(11.9721397753154,3.12794966611081,-0.838460047124573));
#65753=CARTESIAN_POINT('Ctrl Pts',(11.9948518934996,3.1922289418811,-0.449110757560269));
#65754=CARTESIAN_POINT('Ctrl Pts',(11.9993370828402,3.20203165270326,-0.372851335452781));
#65755=CARTESIAN_POINT('Ctrl Pts',(12.0066419083099,3.21333437417297,-0.250443915989653));
#65756=CARTESIAN_POINT('Ctrl Pts',(12.0094079149258,3.21658594061573,-0.204485975277617));
#65757=CARTESIAN_POINT('Ctrl Pts',(12.012997195294,3.21949282842075,-0.145443284963265));
#65758=CARTESIAN_POINT('Ctrl Pts',(12.0137919051916,3.22005530523614,-0.13240711756587));
#65759=CARTESIAN_POINT('Ctrl Pts',(12.0150766131214,3.220834143467,-0.111394135025089));
#65760=CARTESIAN_POINT('Ctrl Pts',(12.0155650518879,3.22110007561357,-0.103419215386652));
#65761=CARTESIAN_POINT('Ctrl Pts',(12.0164977420998,3.22155045962202,-0.088218188554183));
#65762=CARTESIAN_POINT('Ctrl Pts',(12.0169418238561,3.22174022264801,-0.0809922780188563));
#65763=CARTESIAN_POINT('Ctrl Pts',(12.0179575225214,3.22211798695037,-0.0644924862200333));
#65764=CARTESIAN_POINT('Ctrl Pts',(12.0185296296927,3.22229026230542,-0.0552183409577267));
#65765=CARTESIAN_POINT('Ctrl Pts',(12.0202868625372,3.22269552504108,-0.0267937921074276));
#65766=CARTESIAN_POINT('Ctrl Pts',(12.0214760751535,3.2227978412322,-0.00764221514064361));
#65767=CARTESIAN_POINT('Ctrl Pts',(12.0387792645531,3.22180722401552,0.269753237045434));
#65768=CARTESIAN_POINT('Ctrl Pts',(12.0559195218478,3.18984880331787,0.526895148246636));
#65769=CARTESIAN_POINT('Ctrl Pts',(12.0873486623927,3.07775653403808,0.97784951508932));
#65770=CARTESIAN_POINT('Ctrl Pts',(12.1014157192694,3.00877757872783,1.17305043184118));
#65771=CARTESIAN_POINT('Ctrl Pts',(12.116311573329,2.91052126951814,1.38407743461582));
#65772=CARTESIAN_POINT('Ctrl Pts',(12.1179739504862,2.89916920904953,1.4077011073894));
#65773=CARTESIAN_POINT('Ctrl Pts',(12.1200800774014,2.88427056839706,1.43776031173633));
#65774=CARTESIAN_POINT('Ctrl Pts',(12.120539476472,2.88098884599977,1.44432499717204));
#65775=CARTESIAN_POINT('Ctrl Pts',(12.1212756540901,2.87567794129688,1.45485869054886));
#65776=CARTESIAN_POINT('Ctrl Pts',(12.1215533087006,2.87366292372441,1.45883475175053));
#65777=CARTESIAN_POINT('Ctrl Pts',(12.1220827840209,2.86979732086402,1.46642332707834));
#65778=CARTESIAN_POINT('Ctrl Pts',(12.1223346893922,2.86794816573895,1.47003651513041));
#65779=CARTESIAN_POINT('Ctrl Pts',(12.1229149669742,2.86366544997617,1.47836596215495));
#65780=CARTESIAN_POINT('Ctrl Pts',(12.123243032978,2.8612270468626,1.4830797398334));
#65781=CARTESIAN_POINT('Ctrl Pts',(12.124291951952,2.85337630155461,1.49816491150735));
#65782=CARTESIAN_POINT('Ctrl Pts',(12.1250100184607,2.84791905122703,1.50851301213808));
#65783=CARTESIAN_POINT('Ctrl Pts',(12.1375151949251,2.7514553837827,1.68903921497881));
#65784=CARTESIAN_POINT('Ctrl Pts',(12.148390680195,2.64538503910836,1.85076253007993));
#65785=CARTESIAN_POINT('Ctrl Pts',(12.1683845093426,2.42347221361037,2.13069321539516));
#65786=CARTESIAN_POINT('Ctrl Pts',(12.177495362016,2.31180279152574,2.25136323263004));
#65787=CARTESIAN_POINT('Ctrl Pts',(12.1918248093078,2.12835995277317,2.42148731095344));
#65788=CARTESIAN_POINT('Ctrl Pts',(12.1968227738933,2.06297622413764,2.47742694812193));
#65789=CARTESIAN_POINT('Ctrl Pts',(12.2048876579758,1.95617728974188,2.56163767281453));
#65790=CARTESIAN_POINT('Ctrl Pts',(12.2078854404039,1.91620444743983,2.59167460435374));
#65791=CARTESIAN_POINT('Ctrl Pts',(12.2117345993995,1.86463379678907,2.62858109694496));
#65792=CARTESIAN_POINT('Ctrl Pts',(12.2125520079288,1.8536683092901,2.63632539151649));
#65793=CARTESIAN_POINT('Ctrl Pts',(12.2138645988867,1.83603968070425,2.64861112072296));
#65794=CARTESIAN_POINT('Ctrl Pts',(12.2143580963784,1.82940724634574,2.6531965066852));
#65795=CARTESIAN_POINT('Ctrl Pts',(12.2152947508577,1.81681075893974,2.66183550015097));
#65796=CARTESIAN_POINT('Ctrl Pts',(12.2157377148675,1.81085016323904,2.66589408053177));
#65797=CARTESIAN_POINT('Ctrl Pts',(12.2165629633247,1.79973938080712,2.67340497611388));
#65798=CARTESIAN_POINT('Ctrl Pts',(12.2169450469949,1.79459275143243,2.67686250312364));
#65799=CARTESIAN_POINT('Ctrl Pts',(12.2173276938518,1.78943621037674,2.68030513402719));
#65800=CARTESIAN_POINT('Origin',(-1.72497344927317,0.,0.));
#65801=CARTESIAN_POINT('',(13.7170510877849,1.78943621037804,2.68030513402632));
#65802=CARTESIAN_POINT('',(13.4707798281485,1.78943605929599,2.68030523489233));
#65803=CARTESIAN_POINT('',(-1.72497344927317,1.78943621037804,2.68030513402633));
#65804=CARTESIAN_POINT('',(12.8965733803554,-3.22322736952655,-0.000539841530475302));
#65805=CARTESIAN_POINT('Ctrl Pts',(12.8965734492731,-3.22274995461277,-0.000540872794637355));
#65806=CARTESIAN_POINT('Ctrl Pts',(12.8983686230638,-3.22274510388462,-0.0294435724144985));
#65807=CARTESIAN_POINT('Ctrl Pts',(12.9001637968545,-3.22235144858765,-0.0583426038275036));
#65808=CARTESIAN_POINT('Ctrl Pts',(12.9019589706452,-3.22156922997986,-0.087231066409683));
#65809=CARTESIAN_POINT('Ctrl Pts',(12.908131218738,-3.21887977042166,-0.186556691036267));
#65810=CARTESIAN_POINT('Ctrl Pts',(12.9143034668308,-3.21158774489631,-0.285932643125343));
#65811=CARTESIAN_POINT('Ctrl Pts',(12.9204757149235,-3.19968303244483,-0.384897459571556));
#65812=CARTESIAN_POINT('Ctrl Pts',(12.9266396035761,-3.18779444324854,-0.483728242121913));
#65813=CARTESIAN_POINT('Ctrl Pts',(12.9328034922288,-3.17130563561325,-0.582148568311957));
#65814=CARTESIAN_POINT('Ctrl Pts',(12.9389673808814,-3.15025848405349,-0.679697760882756));
#65815=CARTESIAN_POINT('Ctrl Pts',(12.94512474254,-3.12923361950138,-0.777143657784523));
#65816=CARTESIAN_POINT('Ctrl Pts',(12.9512821041985,-3.10366009840369,-0.87371983272308));
#65817=CARTESIAN_POINT('Ctrl Pts',(12.9574394658571,-3.07363138632727,-0.968972478187012));
#65818=CARTESIAN_POINT('Ctrl Pts',(12.9635923300034,-3.04362460807703,-1.064155548407));
#65819=CARTESIAN_POINT('Ctrl Pts',(12.9697451941497,-3.00916923895926,-1.15801659817647));
#65820=CARTESIAN_POINT('Ctrl Pts',(12.975898058296,-2.97040922318094,-1.25011463847986));
#65821=CARTESIAN_POINT('Ctrl Pts',(12.9820485914325,-2.93166389161689,-1.34217778748273));
#65822=CARTESIAN_POINT('Ctrl Pts',(12.9881991245691,-2.88861732211819,-1.43247885424437));
#65823=CARTESIAN_POINT('Ctrl Pts',(12.9943496577056,-2.84146214843125,-1.52059541678004));
#65824=CARTESIAN_POINT('Ctrl Pts',(13.0004995059208,-2.79431222592883,-1.6087021666845));
#65825=CARTESIAN_POINT('Ctrl Pts',(13.006649354136,-2.74305481383244,-1.69462451302655));
#65826=CARTESIAN_POINT('Ctrl Pts',(13.0127992023512,-2.68792872889643,-1.77796420404721));
#65827=CARTESIAN_POINT('Ctrl Pts',(13.0189500107304,-2.63279403723115,-1.86131690673301));
#65828=CARTESIAN_POINT('Ctrl Pts',(13.0251008191095,-2.57378971267325,-1.94208579086444));
#65829=CARTESIAN_POINT('Ctrl Pts',(13.0312516274886,-2.51119758955371,-2.01990203443623));
#65830=CARTESIAN_POINT('Ctrl Pts',(13.0374090138548,-2.44853852723692,-2.09780149865334));
#65831=CARTESIAN_POINT('Ctrl Pts',(13.043566400221,-2.38228427709887,-2.17274167757312));
#65832=CARTESIAN_POINT('Ctrl Pts',(13.0497237865872,-2.31275654777633,-2.24438738038194));
#65833=CARTESIAN_POINT('Ctrl Pts',(13.0558846093242,-2.24319001577965,-2.31607306788301));
#65834=CARTESIAN_POINT('Ctrl Pts',(13.0620454320611,-2.17034668305933,-2.38446032038353));
#65835=CARTESIAN_POINT('Ctrl Pts',(13.0682062547981,-2.09458310839748,-2.44925277677008));
#65836=CARTESIAN_POINT('Ctrl Pts',(13.0743773777148,-2.01869286584251,-2.51415355861484));
#65837=CARTESIAN_POINT('Ctrl Pts',(13.0805485006314,-1.93987297214905,-2.57544727261753));
#65838=CARTESIAN_POINT('Ctrl Pts',(13.0867196235481,-1.85851096250388,-2.63287951960452));
#65839=CARTESIAN_POINT('Ctrl Pts',(13.0914151454937,-1.79660373638251,-2.67657892079172));
#65840=CARTESIAN_POINT('Ctrl Pts',(13.0961106674393,-1.73322539924232,-2.71804360465058));
#65841=CARTESIAN_POINT('Ctrl Pts',(13.1008061893849,-1.66855591829974,-2.75717948454701));
#65842=CARTESIAN_POINT('Ctrl Pts',(13.1069784374777,-1.58354809914073,-2.80862346944334));
#65843=CARTESIAN_POINT('Ctrl Pts',(13.1131506855704,-1.49600928952659,-2.8562229473945));
#65844=CARTESIAN_POINT('Ctrl Pts',(13.1193229336632,-1.40632220382896,-2.89971988673349));
#65845=CARTESIAN_POINT('Ctrl Pts',(13.1254868223158,-1.3167565866485,-2.94315791559855));
#65846=CARTESIAN_POINT('Ctrl Pts',(13.1316507109685,-1.22504886380467,-2.98250426174899));
#65847=CARTESIAN_POINT('Ctrl Pts',(13.1378145996211,-1.13160920309297,-3.01754505748883));
#65848=CARTESIAN_POINT('Ctrl Pts',(13.1439719612796,-1.03826848643223,-3.05254874823223));
#65849=CARTESIAN_POINT('Ctrl Pts',(13.1501293229382,-0.943199882470942,
-3.08325580097137));
#65850=CARTESIAN_POINT('Ctrl Pts',(13.1562866845967,-0.846835675922031,
-3.10949946140624));
#65851=CARTESIAN_POINT('Ctrl Pts',(13.162439548743,-0.750541856532804,-3.13572395272444));
#65852=CARTESIAN_POINT('Ctrl Pts',(13.1685924128893,-0.652954733899122,
-3.1574914197555));
#65853=CARTESIAN_POINT('Ctrl Pts',(13.1747452770356,-0.554523104018507,
-3.17468450237337));
#65854=CARTESIAN_POINT('Ctrl Pts',(13.1808958101722,-0.456128764915871,
-3.19187107139976));
#65855=CARTESIAN_POINT('Ctrl Pts',(13.1870463433087,-0.356890981709488,
-3.20448662482355));
#65856=CARTESIAN_POINT('Ctrl Pts',(13.1931968764452,-0.257269258577538,
-3.21246479997695));
#65857=CARTESIAN_POINT('Ctrl Pts',(13.1993467246604,-0.157658629287641,
-3.22044208668342));
#65858=CARTESIAN_POINT('Ctrl Pts',(13.2054965728757,-0.057664578065635,
-3.22378298715598));
#65859=CARTESIAN_POINT('Ctrl Pts',(13.2116464210909,0.0422487514944001,
-3.22247305737335));
#65860=CARTESIAN_POINT('Ctrl Pts',(13.21779722947,0.142177680329623,-3.22116292307392));
#65861=CARTESIAN_POINT('Ctrl Pts',(13.2239480378491,0.242025428091404,-3.2152005219422));
#65862=CARTESIAN_POINT('Ctrl Pts',(13.2300988462283,0.341329347712653,-3.20462350969502));
#65863=CARTESIAN_POINT('Ctrl Pts',(13.2362562325944,0.440739467992037,-3.19403518585344));
#65864=CARTESIAN_POINT('Ctrl Pts',(13.2424136189606,0.539604165966645,-3.17882244210764));
#65865=CARTESIAN_POINT('Ctrl Pts',(13.2485710053268,0.637467524982191,-3.1590746615256));
#65866=CARTESIAN_POINT('Ctrl Pts',(13.2547318280638,0.735385500480527,-3.13931585992069));
#65867=CARTESIAN_POINT('Ctrl Pts',(13.2608926508007,0.832300602756806,-3.11501708675905));
#65868=CARTESIAN_POINT('Ctrl Pts',(13.2670534735377,0.92777073521625,-3.08631803697809));
#65869=CARTESIAN_POINT('Ctrl Pts',(13.2732245964544,1.02340048264355,-3.05757100572073));
#65870=CARTESIAN_POINT('Ctrl Pts',(13.2793957193711,1.11758002481608,-3.02440914729465));
#65871=CARTESIAN_POINT('Ctrl Pts',(13.2855668422878,1.20988581463768,-2.98702090351549));
#65872=CARTESIAN_POINT('Ctrl Pts',(13.2902623642334,1.28012001150308,-2.95857270672186));
#65873=CARTESIAN_POINT('Ctrl Pts',(13.2949578861789,1.3492697890222,-2.92767866368436));
#65874=CARTESIAN_POINT('Ctrl Pts',(13.2996534081245,1.41715869056307,-2.89443929082328));
#65875=CARTESIAN_POINT('Ctrl Pts',(13.3058256562173,1.50639842746816,-2.8507462449544));
#65876=CARTESIAN_POINT('Ctrl Pts',(13.31199790431,1.59377266331493,-2.80284534308314));
#65877=CARTESIAN_POINT('Ctrl Pts',(13.3181701524028,1.67885740198553,-2.75091900758608));
#65878=CARTESIAN_POINT('Ctrl Pts',(13.3243340410554,1.76382690536929,-2.69906299899206));
#65879=CARTESIAN_POINT('Ctrl Pts',(13.3304979297081,1.84651270724534,-2.64319261727962));
#65880=CARTESIAN_POINT('Ctrl Pts',(13.3366618183607,1.92651311827456,-2.58353725880159));
#65881=CARTESIAN_POINT('Ctrl Pts',(13.3428191800192,2.00642881618858,-2.5239450698897));
#65882=CARTESIAN_POINT('Ctrl Pts',(13.3489765416778,2.0836644302682,-2.46057613061492));
#65883=CARTESIAN_POINT('Ctrl Pts',(13.3551339033363,2.15784594453925,-2.39370391697376));
#65884=CARTESIAN_POINT('Ctrl Pts',(13.3612867674826,2.23197327452057,-2.32688054870107));
#65885=CARTESIAN_POINT('Ctrl Pts',(13.3674396316289,2.30305061824771,-2.25655928354203));
#65886=CARTESIAN_POINT('Ctrl Pts',(13.3735924957753,2.37073658274529,-2.18305419486856));
#65887=CARTESIAN_POINT('Ctrl Pts',(13.3797430289118,2.43839690444613,-2.10957695356436));
#65888=CARTESIAN_POINT('Ctrl Pts',(13.3858935620483,2.5026681059385,-2.03291860462162));
#65889=CARTESIAN_POINT('Ctrl Pts',(13.3920440951849,2.56324590374062,-1.95342980407716));
#65890=CARTESIAN_POINT('Ctrl Pts',(13.3981939434001,2.62381695561926,-1.87394985537916));
#65891=CARTESIAN_POINT('Ctrl Pts',(13.4043437916153,2.68069515823319,-1.79164042722443));
#65892=CARTESIAN_POINT('Ctrl Pts',(13.4104936398305,2.73361739394918,-1.70688415131153));
#65893=CARTESIAN_POINT('Ctrl Pts',(13.4166444482096,2.78654789231168,-1.62211464256488));
#65894=CARTESIAN_POINT('Ctrl Pts',(13.4227952565888,2.83552096690627,-1.53489789574915));
#65895=CARTESIAN_POINT('Ctrl Pts',(13.4289460649679,2.88031813605132,-1.44564345453291));
#65896=CARTESIAN_POINT('Ctrl Pts',(13.4351034513341,2.92516321356555,-1.35629356008153));
#65897=CARTESIAN_POINT('Ctrl Pts',(13.4412608377003,2.96582327240875,-1.2649020085423));
#65898=CARTESIAN_POINT('Ctrl Pts',(13.4474182240665,3.00212698361132,-1.17190065140899));
#65899=CARTESIAN_POINT('Ctrl Pts',(13.4535790468034,3.03845095552267,-1.07884739122357));
#65900=CARTESIAN_POINT('Ctrl Pts',(13.4597398695404,3.0704135990708,-0.984182947825881));
#65901=CARTESIAN_POINT('Ctrl Pts',(13.4659006922773,3.0978933807268,-0.888354751295375));
#65902=CARTESIAN_POINT('Ctrl Pts',(13.472071815194,3.12541910538458,-0.792366341155497));
#65903=CARTESIAN_POINT('Ctrl Pts',(13.4782429381107,3.14844689724348,-0.695210714348815));
#65904=CARTESIAN_POINT('Ctrl Pts',(13.4844140610274,3.16690625898691,-0.59734605488738));
#65905=CARTESIAN_POINT('Ctrl Pts',(13.489109582973,3.18095173164045,-0.522882191113662));
#65906=CARTESIAN_POINT('Ctrl Pts',(13.4938051049186,3.1923533799869,-0.448008056453126));
#65907=CARTESIAN_POINT('Ctrl Pts',(13.4985006268642,3.20110034742735,-0.372926438055179));
#65908=CARTESIAN_POINT('Ctrl Pts',(13.504672874957,3.21259820724514,-0.27423189859225));
#65909=CARTESIAN_POINT('Ctrl Pts',(13.5108451230497,3.21954768556084,-0.17483140442333));
#65910=CARTESIAN_POINT('Ctrl Pts',(13.5170173711425,3.22187297866149,-0.0751802625091805));
#65911=CARTESIAN_POINT('Ctrl Pts',(13.5231812597951,3.22419512248036,0.0243359159779369));
#65912=CARTESIAN_POINT('Ctrl Pts',(13.5293451484477,3.22190551905884,0.124101637048659));
#65913=CARTESIAN_POINT('Ctrl Pts',(13.5355090371004,3.21497994111518,0.223654959093386));
#65914=CARTESIAN_POINT('Ctrl Pts',(13.5416663987589,3.20806169672486,0.323102863279242));
#65915=CARTESIAN_POINT('Ctrl Pts',(13.5478237604175,3.19651726749164,0.422338384645109));
#65916=CARTESIAN_POINT('Ctrl Pts',(13.553981122076,3.18037446959469,0.520899026347988));
#65917=CARTESIAN_POINT('Ctrl Pts',(13.5601339862223,3.16424346285687,0.619387676552421));
#65918=CARTESIAN_POINT('Ctrl Pts',(13.5662868503686,3.14352083528047,0.717201999793968));
#65919=CARTESIAN_POINT('Ctrl Pts',(13.5724397145149,3.11828619350824,0.813884990570474));
#65920=CARTESIAN_POINT('Ctrl Pts',(13.5785902476515,3.09306111186852,0.910531353040098));
#65921=CARTESIAN_POINT('Ctrl Pts',(13.584740780788,3.06332752212783,1.00604681485144));
#65922=CARTESIAN_POINT('Ctrl Pts',(13.5908913139245,3.0292158700759,1.09998580671767));
#65923=CARTESIAN_POINT('Ctrl Pts',(13.5970411621397,2.99510801668623,1.19391433756891));
#65924=CARTESIAN_POINT('Ctrl Pts',(13.603191010355,2.95662321854592,1.28626633921399));
#65925=CARTESIAN_POINT('Ctrl Pts',(13.6093408585702,2.91394107845225,1.37661358187711));
#65926=CARTESIAN_POINT('Ctrl Pts',(13.6154916669493,2.87125227447843,1.46697493028086));
#65927=CARTESIAN_POINT('Ctrl Pts',(13.6216424753284,2.8243650124737,1.55533050521576));
#65928=CARTESIAN_POINT('Ctrl Pts',(13.6277932837076,2.77350566894046,1.64127507348863));
#65929=CARTESIAN_POINT('Ctrl Pts',(13.6339506700738,2.72259193384072,1.72731155525029));
#65930=CARTESIAN_POINT('Ctrl Pts',(13.6401080564399,2.66769785615239,1.81093150689242));
#65931=CARTESIAN_POINT('Ctrl Pts',(13.6462654428061,2.60909407387347,1.891757298434));
#65932=CARTESIAN_POINT('Ctrl Pts',(13.6524262655431,2.55045758545717,1.97262819797613));
#65933=CARTESIAN_POINT('Ctrl Pts',(13.6585870882801,2.48810754045786,2.05070149248175));
#65934=CARTESIAN_POINT('Ctrl Pts',(13.664747911017,2.42235460662338,2.12563301683769));
#65935=CARTESIAN_POINT('Ctrl Pts',(13.6709190339337,2.35649174152399,2.20068981799534));
#65936=CARTESIAN_POINT('Ctrl Pts',(13.6770901568504,2.28721492504014,2.2725940439905));
#65937=CARTESIAN_POINT('Ctrl Pts',(13.6832612797671,2.2148714670262,2.34103864706528));
#65938=CARTESIAN_POINT('Ctrl Pts',(13.6879568017126,2.15982633191722,2.39311719745757));
#65939=CARTESIAN_POINT('Ctrl Pts',(13.6926523236582,2.10300653040755,2.44319357694469));
#65940=CARTESIAN_POINT('Ctrl Pts',(13.6973478456038,2.04457677858076,2.49114900377081));
#65941=CARTESIAN_POINT('Ctrl Pts',(13.7035210191478,1.96775954668602,2.55419570562972));
#65942=CARTESIAN_POINT('Ctrl Pts',(13.7096941926918,1.88788818637792,2.61379695146731));
#65943=CARTESIAN_POINT('Ctrl Pts',(13.7158673662358,1.8053048747192,2.6696426487107));
#65944=CARTESIAN_POINT('Ctrl Pts',(13.7162619400855,1.80002635549901,2.67321216633289));
#65945=CARTESIAN_POINT('Ctrl Pts',(13.7166565139352,1.79473676925109,2.67676635336204));
#65946=CARTESIAN_POINT('Ctrl Pts',(13.7170510877849,1.78943621037804,2.68030513402632));
#65947=CARTESIAN_POINT('Ctrl Pts',(12.4667878339183,1.79025515774624,2.68151164616941));
#65948=CARTESIAN_POINT('Ctrl Pts',(12.4792800670008,1.62332533145098,2.79539990134072));
#65949=CARTESIAN_POINT('Ctrl Pts',(12.5580547063299,0.504984143122603,3.41174297579092));
#65950=CARTESIAN_POINT('Ctrl Pts',(12.7013163267104,-2.11419727950624,3.1526668518075));
#65951=CARTESIAN_POINT('Ctrl Pts',(12.8320857140083,-3.22555599009752,1.03940890035993));
#65952=CARTESIAN_POINT('Ctrl Pts',(12.8965726950595,-3.22797463642135,-0.000529586957199449));
#65953=CARTESIAN_POINT('Ctrl Pts',(12.2173276938518,1.78943621037674,2.68030513402719));
#65954=CARTESIAN_POINT('Ctrl Pts',(12.2175082861032,1.78700255296618,2.68192990228168));
#65955=CARTESIAN_POINT('Ctrl Pts',(12.2176890037932,1.78456668780849,2.68355135254919));
#65956=CARTESIAN_POINT('Ctrl Pts',(12.21875701983,1.77016807067626,2.69310761627513));
#65957=CARTESIAN_POINT('Ctrl Pts',(12.2196472004852,1.75815477405948,2.70096564417186));
#65958=CARTESIAN_POINT('Ctrl Pts',(12.2250259925943,1.68549892884792,2.74780050765236));
#65959=CARTESIAN_POINT('Ctrl Pts',(12.2295869497539,1.62361922962322,2.78481121793989));
#65960=CARTESIAN_POINT('Ctrl Pts',(12.2548611819108,1.27957128225792,2.97522258044692));
#65961=CARTESIAN_POINT('Ctrl Pts',(12.2770413484719,0.976938385617913,3.08784228310247));
#65962=CARTESIAN_POINT('Ctrl Pts',(12.3028501154113,0.597203166083887,3.16764182028854));
#65963=CARTESIAN_POINT('Ctrl Pts',(12.3072540220057,0.531218693434361,3.1793732465229));
#65964=CARTESIAN_POINT('Ctrl Pts',(12.313808082369,0.430516074478871,3.19405411924663));
#65965=CARTESIAN_POINT('Ctrl Pts',(12.3160224408997,0.396039253244913,3.19851199073312));
#65966=CARTESIAN_POINT('Ctrl Pts',(12.3187145772716,0.353472729569948,3.20331699578125));
#65967=CARTESIAN_POINT('Ctrl Pts',(12.319220367574,0.345446573956067,3.20419247453594));
#65968=CARTESIAN_POINT('Ctrl Pts',(12.3200130132617,0.33282143975266,3.20552161215935));
#65969=CARTESIAN_POINT('Ctrl Pts',(12.3203009943319,0.328224698168925,3.20599554973681));
#65970=CARTESIAN_POINT('Ctrl Pts',(12.3208387011516,0.319623105208247,3.20686370570056));
#65971=CARTESIAN_POINT('Ctrl Pts',(12.3210885558094,0.315618578457668,3.20726030585165));
#65972=CARTESIAN_POINT('Ctrl Pts',(12.3216547516289,0.306526683270243,3.20814355543555));
#65973=CARTESIAN_POINT('Ctrl Pts',(12.3219708302213,0.301438906653007,3.20862560393892));
#65974=CARTESIAN_POINT('Ctrl Pts',(12.3229065071985,0.286342287769512,3.21001972959777));
#65975=CARTESIAN_POINT('Ctrl Pts',(12.3235241796891,0.276330188958877,3.21089710254032));
#65976=CARTESIAN_POINT('Ctrl Pts',(12.3278762048834,0.205474301993766,3.21677241839931));
#65977=CARTESIAN_POINT('Ctrl Pts',(12.3315210053964,0.144498824347654,3.22008784208063));
#65978=CARTESIAN_POINT('Ctrl Pts',(12.3352173604744,0.0814932148166845,
3.22172008329158));
#65979=CARTESIAN_POINT('Ctrl Pts',(12.3353327651569,0.079524905079508,3.22176926992739));
#65980=CARTESIAN_POINT('Ctrl Pts',(12.3419286388201,-0.033039973876497,
3.22447896583268));
#65981=CARTESIAN_POINT('Ctrl Pts',(12.348196521495,-0.143708579799369,3.22144495746909));
#65982=CARTESIAN_POINT('Ctrl Pts',(12.370286277878,-0.535933731974559,3.19043430586768));
#65983=CARTESIAN_POINT('Ctrl Pts',(12.3858229800298,-0.813666830578774,
3.13113870813219));
#65984=CARTESIAN_POINT('Ctrl Pts',(12.4051216551378,-1.11880799765079,3.0225940186862));
#65985=CARTESIAN_POINT('Ctrl Pts',(12.4075929575794,-1.15725310287701,3.00808426725228));
#65986=CARTESIAN_POINT('Ctrl Pts',(12.4108497053235,-1.20703952530353,2.98819845331322));
#65987=CARTESIAN_POINT('Ctrl Pts',(12.4116127630578,-1.21864273442523,2.98348525904341));
#65988=CARTESIAN_POINT('Ctrl Pts',(12.4128586131186,-1.23748534121262,2.97570317989714));
#65989=CARTESIAN_POINT('Ctrl Pts',(12.4133400148783,-1.24474157267366,2.97267519249744));
#65990=CARTESIAN_POINT('Ctrl Pts',(12.4142677089574,-1.25867706710805,2.96680001379763));
#65991=CARTESIAN_POINT('Ctrl Pts',(12.4147138654395,-1.26535793858731,2.96395674175801));
#65992=CARTESIAN_POINT('Ctrl Pts',(12.4157366975768,-1.28062542218801,2.95739811729555));
#65993=CARTESIAN_POINT('Ctrl Pts',(12.4163138784503,-1.28920554775183,2.95366791444566));
#65994=CARTESIAN_POINT('Ctrl Pts',(12.4178473921346,-1.31190791460179,2.94368031182628));
#65995=CARTESIAN_POINT('Ctrl Pts',(12.4188059224268,-1.32600148793925,2.93735871068346));
#65996=CARTESIAN_POINT('Ctrl Pts',(12.4254405491666,-1.42287926716492,2.89306536762836));
#65997=CARTESIAN_POINT('Ctrl Pts',(12.4312335199165,-1.50405952672247,2.85170385571505));
#65998=CARTESIAN_POINT('Ctrl Pts',(12.4397463988756,-1.61843272684388,2.78718735086989));
#65999=CARTESIAN_POINT('Ctrl Pts',(12.4423764169247,-1.65311718939539,2.76675643553268));
#66000=CARTESIAN_POINT('Ctrl Pts',(12.4454486558068,-1.6928984282206,2.74230815045632));
#66001=CARTESIAN_POINT('Ctrl Pts',(12.4458730682651,-1.69837787511089,2.73891797483863));
#66002=CARTESIAN_POINT('Ctrl Pts',(12.4464402168789,-1.70567876064533,2.73437052803579));
#66003=CARTESIAN_POINT('Ctrl Pts',(12.4465825549347,-1.70750927934305,2.73322781341703));
#66004=CARTESIAN_POINT('Ctrl Pts',(12.4630327794531,-1.91885819176681,2.6009965345449));
#66005=CARTESIAN_POINT('Ctrl Pts',(12.4800284580523,-2.11257915185544,2.44626063872923));
#66006=CARTESIAN_POINT('Ctrl Pts',(12.5011274510788,-2.33582100310214,2.22146702915632));
#66007=CARTESIAN_POINT('Ctrl Pts',(12.5057148641371,-2.38332093199774,2.17042811416539));
#66008=CARTESIAN_POINT('Ctrl Pts',(12.5125090539377,-2.4526026338903,2.09096473464335));
#66009=CARTESIAN_POINT('Ctrl Pts',(12.5147853718186,-2.47562613251794,2.06365421292259));
#66010=CARTESIAN_POINT('Ctrl Pts',(12.5175423022222,-2.50333678607804,2.02965238877069));
#66011=CARTESIAN_POINT('Ctrl Pts',(12.518052525847,-2.50845772518312,2.02331997670889));
#66012=CARTESIAN_POINT('Ctrl Pts',(12.5188505574029,-2.51645648056312,2.01335189216453));
#66013=CARTESIAN_POINT('Ctrl Pts',(12.5191395162065,-2.51935050474163,2.0097293586838));
#66014=CARTESIAN_POINT('Ctrl Pts',(12.5196780834841,-2.52474045729685,2.00295266139086));
#66015=CARTESIAN_POINT('Ctrl Pts',(12.5199278251179,-2.52723827219303,1.99980010408442));
#66016=CARTESIAN_POINT('Ctrl Pts',(12.5204925222027,-2.5328824512004,1.99264897517752));
#66017=CARTESIAN_POINT('Ctrl Pts',(12.5208072206912,-2.53602524359466,1.98864763459287));
#66018=CARTESIAN_POINT('Ctrl Pts',(12.5217350744747,-2.54528305293136,1.97680313899963));
#66019=CARTESIAN_POINT('Ctrl Pts',(12.5223463514273,-2.55137132380825,1.968939014804));
#66020=CARTESIAN_POINT('Ctrl Pts',(12.5265510556383,-2.59316490409663,1.91443553431141));
#66021=CARTESIAN_POINT('Ctrl Pts',(12.5300616715577,-2.62762833748178,1.86685242558578));
#66022=CARTESIAN_POINT('Ctrl Pts',(12.5343011110822,-2.66835372312316,1.80725937002168));
#66023=CARTESIAN_POINT('Ctrl Pts',(12.5350869306436,-2.67586391314629,1.79612091745949));
#66024=CARTESIAN_POINT('Ctrl Pts',(12.5536417794413,-2.85219836434135,1.53103629765233));
#66025=CARTESIAN_POINT('Ctrl Pts',(12.5699677570529,-2.98421278816317,1.25443891072778));
#66026=CARTESIAN_POINT('Ctrl Pts',(12.5918475413813,-3.09771585957471,0.892106056522236));
#66027=CARTESIAN_POINT('Ctrl Pts',(12.5962104392558,-3.11755823854856,0.820076958875613));
#66028=CARTESIAN_POINT('Ctrl Pts',(12.6033328513673,-3.14534151019582,0.703547590821815));
#66029=CARTESIAN_POINT('Ctrl Pts',(12.6060421129321,-3.15488053953082,0.659455003292693));
#66030=CARTESIAN_POINT('Ctrl Pts',(12.6095675599293,-3.16596294164801,0.602464902008854));
#66031=CARTESIAN_POINT('Ctrl Pts',(12.6103564309675,-3.16835852941827,0.589736828969605));
#66032=CARTESIAN_POINT('Ctrl Pts',(12.611633967861,-3.17210205589667,0.56916556154873));
#66033=CARTESIAN_POINT('Ctrl Pts',(12.6121211061404,-3.17349779534033,0.561331123891866));
#66034=CARTESIAN_POINT('Ctrl Pts',(12.6130528239263,-3.17610683168556,0.546365519946078));
#66035=CARTESIAN_POINT('Ctrl Pts',(12.6134972398592,-3.17732516559131,0.53923527184978));
#66036=CARTESIAN_POINT('Ctrl Pts',(12.6145158354977,-3.18005779573373,0.522911833884906));
#66037=CARTESIAN_POINT('Ctrl Pts',(12.6150905155675,-3.181556245963,0.513716089953671));
#66038=CARTESIAN_POINT('Ctrl Pts',(12.6168633997489,-3.18604588195182,0.485390659530308));
#66039=CARTESIAN_POINT('Ctrl Pts',(12.6180657974757,-3.18890452245745,0.466240683068948));
#66040=CARTESIAN_POINT('Ctrl Pts',(12.6286611072834,-3.21246413851608,0.298049476772166));
#66041=CARTESIAN_POINT('Ctrl Pts',(12.6383807299955,-3.22287293526502,0.147775904085055));
#66042=CARTESIAN_POINT('Ctrl Pts',(12.663765228805,-3.22255713465583,-0.235249454019123));
#66043=CARTESIAN_POINT('Ctrl Pts',(12.6797418286628,-3.19718744435591,-0.467115696392172));
#66044=CARTESIAN_POINT('Ctrl Pts',(12.6973545232474,-3.14022827584774,-0.725326481530957));
#66045=CARTESIAN_POINT('Ctrl Pts',(12.6994649411198,-3.13290593759274,-0.756328384760312));
#66046=CARTESIAN_POINT('Ctrl Pts',(12.7061664106279,-3.1080213560631,-0.855116119409178));
#66047=CARTESIAN_POINT('Ctrl Pts',(12.710698602809,-3.08870788244638,-0.922445470318466));
#66048=CARTESIAN_POINT('Ctrl Pts',(12.7157797890273,-3.06397403567384,-0.999145703616312));
#66049=CARTESIAN_POINT('Ctrl Pts',(12.7164427695479,-3.06068433859602,-1.00917808890834));
#66050=CARTESIAN_POINT('Ctrl Pts',(12.7174245619309,-3.05571844058919,-1.02407462561977));
#66051=CARTESIAN_POINT('Ctrl Pts',(12.7177455370936,-3.05407983901003,-1.02895109933651));
#66052=CARTESIAN_POINT('Ctrl Pts',(12.7183165509912,-3.05113763585001,-1.03763813964229));
#66053=CARTESIAN_POINT('Ctrl Pts',(12.7185668551912,-3.04983856513048,-1.04145019517142));
#66054=CARTESIAN_POINT('Ctrl Pts',(12.7191020520803,-3.04704081066854,-1.04960993148744));
#66055=CARTESIAN_POINT('Ctrl Pts',(12.7193868139527,-3.04553997141236,-1.05395682706434));
#66056=CARTESIAN_POINT('Ctrl Pts',(12.720163748881,-3.04141180678738,-1.06583082306111));
#66057=CARTESIAN_POINT('Ctrl Pts',(12.7206548231636,-3.03876582559905,-1.07335147188336));
#66058=CARTESIAN_POINT('Ctrl Pts',(12.7231967010293,-3.02488057960672,-1.11235448143615));
#66059=CARTESIAN_POINT('Ctrl Pts',(12.7252211031928,-3.01317939961965,-1.14367177412547));
#66060=CARTESIAN_POINT('Ctrl Pts',(12.7310122441603,-2.97790988991909,-1.23376650135124));
#66061=CARTESIAN_POINT('Ctrl Pts',(12.7347173096923,-2.9530929661366,-1.29204104550629));
#66062=CARTESIAN_POINT('Ctrl Pts',(12.759680734869,-2.77176770798535,-1.68525484019817));
#66063=CARTESIAN_POINT('Ctrl Pts',(12.7793114816512,-2.56036699912831,-1.99181835500209));
#66064=CARTESIAN_POINT('Ctrl Pts',(12.8019968630355,-2.29458726531418,-2.26298168424145));
#66065=CARTESIAN_POINT('Ctrl Pts',(12.8025934725884,-2.28758053693351,-2.27006433941809));
#66066=CARTESIAN_POINT('Ctrl Pts',(12.8048834608465,-2.26062389562583,-2.29706154748031));
#66067=CARTESIAN_POINT('Ctrl Pts',(12.8065865111038,-2.24044630668845,-2.31674608453141));
#66068=CARTESIAN_POINT('Ctrl Pts',(12.8089813892909,-2.21190711264614,-2.34386636671604));
#66069=CARTESIAN_POINT('Ctrl Pts',(12.8096634487079,-2.20376069033802,-2.3515274684278));
#66070=CARTESIAN_POINT('Ctrl Pts',(12.8107640375246,-2.19058671461077,-2.36378802700875));
#66071=CARTESIAN_POINT('Ctrl Pts',(12.8111814165442,-2.18558411136279,-2.36841425470458));
#66072=CARTESIAN_POINT('Ctrl Pts',(12.8120477811564,-2.17518667362029,-2.37796843676708));
#66073=CARTESIAN_POINT('Ctrl Pts',(12.812496865962,-2.16978968038776,-2.38289397431717));
#66074=CARTESIAN_POINT('Ctrl Pts',(12.813550810065,-2.15710660877617,-2.39439029879254));
#66075=CARTESIAN_POINT('Ctrl Pts',(12.8141562920881,-2.14980721212989,-2.4009462242707));
#66076=CARTESIAN_POINT('Ctrl Pts',(12.8161230258421,-2.1260559839001,-2.42208314961587));
#66077=CARTESIAN_POINT('Ctrl Pts',(12.8174899098611,-2.10948514511078,-2.43652892744612));
#66078=CARTESIAN_POINT('Ctrl Pts',(12.8207007622298,-2.07041864948751,-2.46988823534968));
#66079=CARTESIAN_POINT('Ctrl Pts',(12.8225501579173,-2.04780977320846,-2.48866557014003));
#66080=CARTESIAN_POINT('Ctrl Pts',(12.8290584038212,-1.96789026682442,-2.55321459396083));
#66081=CARTESIAN_POINT('Ctrl Pts',(12.8337806385978,-1.90928009563021,-2.59733421521482));
#66082=CARTESIAN_POINT('Ctrl Pts',(12.857947290195,-1.60620693452165,-2.80967259501224));
#66083=CARTESIAN_POINT('Ctrl Pts',(12.878480093807,-1.34089305313427,-2.94552639301652));
#66084=CARTESIAN_POINT('Ctrl Pts',(12.9034549364483,-0.984193596455357,
-3.0698627342375));
#66085=CARTESIAN_POINT('Ctrl Pts',(12.9087270931367,-0.906627829442088,
-3.09365847365901));
#66086=CARTESIAN_POINT('Ctrl Pts',(12.9145348243538,-0.817651136448685,
-3.1173200401385));
#66087=CARTESIAN_POINT('Ctrl Pts',(12.915223096416,-0.807047898911263,-3.12008193972554));
#66088=CARTESIAN_POINT('Ctrl Pts',(12.9162314476559,-0.791423744262382,
-3.1240666956274));
#66089=CARTESIAN_POINT('Ctrl Pts',(12.9165538997877,-0.78641377994868,-3.12533160309534));
#66090=CARTESIAN_POINT('Ctrl Pts',(12.9171271804215,-0.777481886066626,
-3.12756387562323));
#66091=CARTESIAN_POINT('Ctrl Pts',(12.9173782784857,-0.773561162090664,
-3.1285359209158));
#66092=CARTESIAN_POINT('Ctrl Pts',(12.917910201009,-0.765237290179472,-3.13058301199037));
#66093=CARTESIAN_POINT('Ctrl Pts',(12.9181909132995,-0.760833713043868,
-3.13165613804309));
#66094=CARTESIAN_POINT('Ctrl Pts',(12.9189455068588,-0.748967689231045,
-3.13452131303299));
#66095=CARTESIAN_POINT('Ctrl Pts',(12.9194183932892,-0.74150102369259,-3.13629601537658));
#66096=CARTESIAN_POINT('Ctrl Pts',(12.9217209379303,-0.705000426156909,
-3.14483396455468));
#66097=CARTESIAN_POINT('Ctrl Pts',(12.9235297645199,-0.675878811909328,
-3.15122107232191));
#66098=CARTESIAN_POINT('Ctrl Pts',(12.9285496328213,-0.59396137430529,-3.16799974301118));
#66099=CARTESIAN_POINT('Ctrl Pts',(12.9317169560221,-0.540985953826797,
-3.17747499758863));
#66100=CARTESIAN_POINT('Ctrl Pts',(12.9395397404302,-0.40777740105488,-3.19787243648056));
#66101=CARTESIAN_POINT('Ctrl Pts',(12.9441375043166,-0.327322177920481,
-3.2071064925347));
#66102=CARTESIAN_POINT('Ctrl Pts',(12.9596418103576,-0.0527331887067016,
-3.22817949065799));
#66103=CARTESIAN_POINT('Ctrl Pts',(12.970349173668,0.142078089434734,-3.22548241986068));
#66104=CARTESIAN_POINT('Ctrl Pts',(12.9841694255106,0.382449136231198,-3.20032538366344));
#66105=CARTESIAN_POINT('Ctrl Pts',(12.9868920797059,0.42932483451619,-3.19437471686906));
#66106=CARTESIAN_POINT('Ctrl Pts',(12.9947224233249,0.56240071229516,-3.17449925429227));
#66107=CARTESIAN_POINT('Ctrl Pts',(12.9998925138557,0.648183538491109,-3.15810007989066));
#66108=CARTESIAN_POINT('Ctrl Pts',(13.0060983581657,0.748041253378878,-3.13477023988422));
#66109=CARTESIAN_POINT('Ctrl Pts',(13.00702465875,0.762867884958379,-3.13119509952796));
#66110=CARTESIAN_POINT('Ctrl Pts',(13.0085211415974,0.786691751649836,-3.12527120513962));
#66111=CARTESIAN_POINT('Ctrl Pts',(13.0090891897106,0.795705289339191,-3.1229884898045));
#66112=CARTESIAN_POINT('Ctrl Pts',(13.0101025495026,0.811731236554076,-3.11885596920034));
#66113=CARTESIAN_POINT('Ctrl Pts',(13.0105473636733,0.818747546073128,-3.1170214326257));
#66114=CARTESIAN_POINT('Ctrl Pts',(13.0114777242701,0.833384155988676,-3.1131416066481));
#66115=CARTESIAN_POINT('Ctrl Pts',(13.0119634088592,0.841003249001174,-3.11109198640883));
#66116=CARTESIAN_POINT('Ctrl Pts',(13.0132299819313,0.860815188738119,-3.10568425884255));
#66117=CARTESIAN_POINT('Ctrl Pts',(13.0140122921546,0.8729958420741,-3.10228234646362));
#66118=CARTESIAN_POINT('Ctrl Pts',(13.0174158217113,0.925741765850736,-3.08721579221525));
#66119=CARTESIAN_POINT('Ctrl Pts',(13.02006058831,0.966094190786457,-3.07482697174894));
#66120=CARTESIAN_POINT('Ctrl Pts',(13.0270512426366,1.07105559185683,-3.04033212687478));
#66121=CARTESIAN_POINT('Ctrl Pts',(13.0314372770037,1.1352229695049,-3.01695993157272));
#66122=CARTESIAN_POINT('Ctrl Pts',(13.0407209396395,1.26757227455672,-2.96393312033488));
#66123=CARTESIAN_POINT('Ctrl Pts',(13.0456268607271,1.33556806564255,-2.93392157159599));
#66124=CARTESIAN_POINT('Ctrl Pts',(13.0674644228375,1.63035628042295,-2.79143775745219));
#66125=CARTESIAN_POINT('Ctrl Pts',(13.0849315394035,1.84446838418932,-2.65482919779079));
#66126=CARTESIAN_POINT('Ctrl Pts',(13.105376225506,2.08635025638369,-2.45698717147311));
#66127=CARTESIAN_POINT('Ctrl Pts',(13.1092029600397,2.13126816163645,-2.41812746900493));
#66128=CARTESIAN_POINT('Ctrl Pts',(13.113574032838,2.18245247804216,-2.37131151562391));
#66129=CARTESIAN_POINT('Ctrl Pts',(13.1142003890212,2.18978398008975,-2.36454292618618));
#66130=CARTESIAN_POINT('Ctrl Pts',(13.11514273502,2.2008115153091,-2.35426680640552));
#66131=CARTESIAN_POINT('Ctrl Pts',(13.115460599477,2.20453077802059,-2.35078445870171));
#66132=CARTESIAN_POINT('Ctrl Pts',(13.1160282121656,2.2111717768091,-2.34453686653071));
#66133=CARTESIAN_POINT('Ctrl Pts',(13.1162782133297,2.21409659722264,-2.34177496866304));
#66134=CARTESIAN_POINT('Ctrl Pts',(13.1168151347719,2.22037786377466,-2.33582130244095));
#66135=CARTESIAN_POINT('Ctrl Pts',(13.1171019151755,2.2237325905681,-2.33262778453086));
#66136=CARTESIAN_POINT('Ctrl Pts',(13.117890030471,2.23295080522356,-2.32381458479684));
#66137=CARTESIAN_POINT('Ctrl Pts',(13.1183902129057,2.23880000208949,-2.31817990610197));
#66138=CARTESIAN_POINT('Ctrl Pts',(13.1210623798833,2.27003735635501,-2.28785967402665));
#66139=CARTESIAN_POINT('Ctrl Pts',(13.1232046344547,2.2950398326074,-2.2627779165049));
#66140=CARTESIAN_POINT('Ctrl Pts',(13.1294344400404,2.36740885795147,-2.18774555316099));
#66141=CARTESIAN_POINT('Ctrl Pts',(13.1334485802628,2.41359657849865,-2.13668157410871));
#66142=CARTESIAN_POINT('Ctrl Pts',(13.150940014997,2.61051507064295,-1.90443200673598));
#66143=CARTESIAN_POINT('Ctrl Pts',(13.1637732408591,2.74274496155342,-1.70851163527425));
#66144=CARTESIAN_POINT('Ctrl Pts',(13.1856518047563,2.92184448168582,-1.36791255785595));
#66145=CARTESIAN_POINT('Ctrl Pts',(13.1943186110963,2.98200085172074,-1.23126852975339));
#66146=CARTESIAN_POINT('Ctrl Pts',(13.2044940247293,3.039023449488,-1.07276650536422));
#66147=CARTESIAN_POINT('Ctrl Pts',(13.2056674540597,3.04540554640454,-1.05451246283088));
#66148=CARTESIAN_POINT('Ctrl Pts',(13.2074140561683,3.05461701655015,-1.02738462255336));
#66149=CARTESIAN_POINT('Ctrl Pts',(13.2079830349804,3.05757290118923,-1.01855399046954));
#66150=CARTESIAN_POINT('Ctrl Pts',(13.2089962081628,3.06275659790965,-1.00284191214116));
#66151=CARTESIAN_POINT('Ctrl Pts',(13.2094398970793,3.06499960333466,-0.995965515964025));
#66152=CARTESIAN_POINT('Ctrl Pts',(13.2103735045716,3.06966249328517,-0.981505530450563));
#66153=CARTESIAN_POINT('Ctrl Pts',(13.2108635816401,3.0720774640332,-0.973920418796821));
#66154=CARTESIAN_POINT('Ctrl Pts',(13.2121541642164,3.07835110344488,-0.953960208133823));
#66155=CARTESIAN_POINT('Ctrl Pts',(13.2129561931015,3.08216322391658,-0.941570734479675));
#66156=CARTESIAN_POINT('Ctrl Pts',(13.2165671553425,3.09893769248793,-0.885859758819815));
#66157=CARTESIAN_POINT('Ctrl Pts',(13.2194033324161,3.11106161616452,-0.842293071962168));
#66158=CARTESIAN_POINT('Ctrl Pts',(13.2270184662554,3.14083241944924,-0.725882574918161));
#66159=CARTESIAN_POINT('Ctrl Pts',(13.2318470099064,3.15686092078427,-0.652657248439238));
#66160=CARTESIAN_POINT('Ctrl Pts',(13.2567846833419,3.22539771378096,-0.277347066708537));
#66161=CARTESIAN_POINT('Ctrl Pts',(13.2780565231288,3.23714975393023,0.0305091848345442));
#66162=CARTESIAN_POINT('Ctrl Pts',(13.3027840689352,3.19802319714815,0.404466412541073));
#66163=CARTESIAN_POINT('Ctrl Pts',(13.307280548735,3.18855910661355,0.473326460270088));
#66164=CARTESIAN_POINT('Ctrl Pts',(13.3123264121893,3.17510363626401,0.552218687450564));
#66165=CARTESIAN_POINT('Ctrl Pts',(13.3129880452872,3.17328121253321,0.562596599037311));
#66166=CARTESIAN_POINT('Ctrl Pts',(13.313968233868,3.17049404139079,0.578023803150978));
#66167=CARTESIAN_POINT('Ctrl Pts',(13.3142889424863,3.16956808015658,0.583079899869845));
#66168=CARTESIAN_POINT('Ctrl Pts',(13.3148596635336,3.16789513211846,0.592093075716802));
#66169=CARTESIAN_POINT('Ctrl Pts',(13.3151099403547,3.16715282382727,0.596050979003713));
#66170=CARTESIAN_POINT('Ctrl Pts',(13.3156452784644,3.16554640269932,0.604528500378822));
#66171=CARTESIAN_POINT('Ctrl Pts',(13.3159302081776,3.16468003136645,0.609047646012802));
#66172=CARTESIAN_POINT('Ctrl Pts',(13.3167080714707,3.16228378801627,0.621403704146416));
#66173=CARTESIAN_POINT('Ctrl Pts',(13.3171999018621,3.16073445224038,0.629236875177134));
#66174=CARTESIAN_POINT('Ctrl Pts',(13.3197523144135,3.1525163661566,0.669989772137144));
#66175=CARTESIAN_POINT('Ctrl Pts',(13.3217862338167,3.14536209054367,0.702810973070717));
#66176=CARTESIAN_POINT('Ctrl Pts',(13.3276123422465,3.1231445091183,0.797590725890267));
#66177=CARTESIAN_POINT('Ctrl Pts',(13.3313419632393,3.10675349864384,0.859224269780721));
#66178=CARTESIAN_POINT('Ctrl Pts',(13.3468383578079,3.02996967264681,1.11690247681396));
#66179=CARTESIAN_POINT('Ctrl Pts',(13.3580852468134,2.95276129958134,1.30743957168383));
#66180=CARTESIAN_POINT('Ctrl Pts',(13.3801102443004,2.77202014439468,1.65426857644279));
#66181=CARTESIAN_POINT('Ctrl Pts',(13.3907933963139,2.67197953989103,1.81141134429158));
#66182=CARTESIAN_POINT('Ctrl Pts',(13.4031008725692,2.54807952088654,1.97325332152803));
#66183=CARTESIAN_POINT('Ctrl Pts',(13.4041861748634,2.53708142364502,1.98737408293258));
#66184=CARTESIAN_POINT('Ctrl Pts',(13.405833785832,2.52027974522329,2.00857945289795));
#66185=CARTESIAN_POINT('Ctrl Pts',(13.4063926473557,2.51456253198622,2.01573229442725));
#66186=CARTESIAN_POINT('Ctrl Pts',(13.407366355856,2.50457036223762,2.0281248956465));
#66187=CARTESIAN_POINT('Ctrl Pts',(13.4077806442104,2.50030923373066,2.03337577106563));
#66188=CARTESIAN_POINT('Ctrl Pts',(13.4086461804021,2.49138682586354,2.04430016451609));
#66189=CARTESIAN_POINT('Ctrl Pts',(13.4090975453754,2.48672262437183,2.04997123558883));
#66190=CARTESIAN_POINT('Ctrl Pts',(13.4101668353825,2.47564670862519,2.06334470544812));
#66191=CARTESIAN_POINT('Ctrl Pts',(13.4107854363271,2.46921839445977,2.07103320018091));
#66192=CARTESIAN_POINT('Ctrl Pts',(13.4128386636382,2.44781439087196,2.0963918467958));
#66193=CARTESIAN_POINT('Ctrl Pts',(13.414279635533,2.43268433662111,2.11393021187192));
#66194=CARTESIAN_POINT('Ctrl Pts',(13.4275582750778,2.29229789045478,2.27315930625846));
#66195=CARTESIAN_POINT('Ctrl Pts',(13.4399191301818,2.15500790329576,2.40370579156247));
#66196=CARTESIAN_POINT('Ctrl Pts',(13.4586189051824,1.93676066724341,2.5774320677658));
#66197=CARTESIAN_POINT('Ctrl Pts',(13.4646996484832,1.8641442850022,2.63042823160763));
#66198=CARTESIAN_POINT('Ctrl Pts',(13.4707798281485,1.78943605929599,2.68030523489233));
#66199=CARTESIAN_POINT('Origin',(-1.72497344927317,0.,0.));
#66200=CARTESIAN_POINT('',(14.9670297268737,1.78943621037805,2.68030513402632));
#66201=CARTESIAN_POINT('',(14.7230445264018,1.78943621037785,2.68030513402645));
#66202=CARTESIAN_POINT('',(-1.72497344927317,1.78943621037804,2.68030513402633));
#66203=CARTESIAN_POINT('',(14.1465734492221,-3.22274864077389,0.00295988007753989));
#66204=CARTESIAN_POINT('Ctrl Pts',(14.1465734492731,-3.22274864077465,0.00295987925103317));
#66205=CARTESIAN_POINT('Ctrl Pts',(14.1527116181293,-3.2228400216292,-0.0965365865984671));
#66206=CARTESIAN_POINT('Ctrl Pts',(14.1588497869856,-3.21831936874255,-0.196145750536572));
#66207=CARTESIAN_POINT('Ctrl Pts',(14.1649879558418,-3.20918300970089,-0.29540137566902));
#66208=CARTESIAN_POINT('Ctrl Pts',(14.1710741749034,-3.20012397534469,-0.39381696047922));
#66209=CARTESIAN_POINT('Ctrl Pts',(14.177160393965,-3.18652710916992,-0.49188451750038));
#66210=CARTESIAN_POINT('Ctrl Pts',(14.1832466130266,-3.16844108362263,-0.589150797429849));
#66211=CARTESIAN_POINT('Ctrl Pts',(14.1893312277177,-3.15035982567973,-0.686391437279283));
#66212=CARTESIAN_POINT('Ctrl Pts',(14.1954158424088,-3.12779184018672,-0.782830782726507));
#66213=CARTESIAN_POINT('Ctrl Pts',(14.2015004571,-3.10083725806307,-0.878023838803871));
#66214=CARTESIAN_POINT('Ctrl Pts',(14.2075851795943,-3.07388219837611,-0.973218581448363));
#66215=CARTESIAN_POINT('Ctrl Pts',(14.2136699020886,-3.04254050992401,-1.06716656333512));
#66216=CARTESIAN_POINT('Ctrl Pts',(14.2197546245829,-3.00696242124333,-1.15943717368837));
#66217=CARTESIAN_POINT('Ctrl Pts',(14.2259325310195,-2.9708394750826,-1.25312085411097));
#66218=CARTESIAN_POINT('Ctrl Pts',(14.2321104374562,-2.93034944389814,-1.34507491116444));
#66219=CARTESIAN_POINT('Ctrl Pts',(14.2382883438928,-2.88569996812181,-1.43487046679544));
#66220=CARTESIAN_POINT('Ctrl Pts',(14.2443818447686,-2.84166051518834,-1.5234391918944));
#66221=CARTESIAN_POINT('Ctrl Pts',(14.2504753456443,-2.7935748445443,-1.60990766984916));
#66222=CARTESIAN_POINT('Ctrl Pts',(14.2565688465201,-2.74168740894939,-1.69389129347441));
#66223=CARTESIAN_POINT('Ctrl Pts',(14.2627889557372,-2.68872187682301,-1.77961989548011));
#66224=CARTESIAN_POINT('Ctrl Pts',(14.2690090649543,-2.63179511432025,-1.86275882929278));
#66225=CARTESIAN_POINT('Ctrl Pts',(14.2752291741714,-2.57121110622653,-1.94293360918929));
#66226=CARTESIAN_POINT('Ctrl Pts',(14.2814492833885,-2.51062709813282,-2.02310838908579));
#66227=CARTESIAN_POINT('Ctrl Pts',(14.2876693926056,-2.44638620976731,-2.10031868870361));
#66228=CARTESIAN_POINT('Ctrl Pts',(14.2938895018227,-2.37883175388096,-2.17423021992328));
#66229=CARTESIAN_POINT('Ctrl Pts',(14.3000617499155,-2.31179710112032,-2.24757303299623));
#66230=CARTESIAN_POINT('Ctrl Pts',(14.3062339980083,-2.24124938505372,-2.31794187018767));
#66231=CARTESIAN_POINT('Ctrl Pts',(14.312406246101,-2.16748294549879,-2.38498118304356));
#66232=CARTESIAN_POINT('Ctrl Pts',(14.3185701347537,-2.09381641218971,-2.45192970059862));
#66233=CARTESIAN_POINT('Ctrl Pts',(14.3247340234063,-2.01694013862246,-2.51555736712038));
#66234=CARTESIAN_POINT('Ctrl Pts',(14.3308979120589,-1.93718726555775,-2.57554325544358));
#66235=CARTESIAN_POINT('Ctrl Pts',(14.3370552737175,-1.8575188434882,-2.63546562419976));
#66236=CARTESIAN_POINT('Ctrl Pts',(14.343212635376,-1.77498022299545,-2.69175362180343));
#66237=CARTESIAN_POINT('Ctrl Pts',(14.3493699970346,-1.68993905853801,-2.74412527792149));
#66238=CARTESIAN_POINT('Ctrl Pts',(14.3555228611809,-1.60496001056795,-2.79645868029106));
#66239=CARTESIAN_POINT('Ctrl Pts',(14.3616757253272,-1.5174824216187,-2.84488120146152));
#66240=CARTESIAN_POINT('Ctrl Pts',(14.3678285894735,-1.42790372571685,-2.88915359795632));
#66241=CARTESIAN_POINT('Ctrl Pts',(14.37397912261,-1.33835896666301,-2.93340922187394));
#66242=CARTESIAN_POINT('Ctrl Pts',(14.3801296557466,-1.24671507129056,-2.97351765296854));
#66243=CARTESIAN_POINT('Ctrl Pts',(14.3862801888831,-1.15339413842594,-3.00928555041636));
#66244=CARTESIAN_POINT('Ctrl Pts',(14.3924300370983,-1.06008359774944,-3.04504946476299));
#66245=CARTESIAN_POINT('Ctrl Pts',(14.3985798853135,-0.965096796479779,
-3.07647365099464));
#66246=CARTESIAN_POINT('Ctrl Pts',(14.4047297335287,-0.868874936119754,
-3.10341326733693));
#66247=CARTESIAN_POINT('Ctrl Pts',(14.4108805419079,-0.772638052826602,
-3.13035708970947));
#66248=CARTESIAN_POINT('Ctrl Pts',(14.417031350287,-0.675166145768034,-3.15281483435817));
#66249=CARTESIAN_POINT('Ctrl Pts',(14.4231821586661,-0.576913683691185,
-3.17069206389865));
#66250=CARTESIAN_POINT('Ctrl Pts',(14.4293395450323,-0.478556145438334,
-3.18858841225689));
#66251=CARTESIAN_POINT('Ctrl Pts',(14.4354969313985,-0.379416813419197,
-3.20189438552719));
#66252=CARTESIAN_POINT('Ctrl Pts',(14.4416543177647,-0.279958297388894,
-3.21056707050688));
#66253=CARTESIAN_POINT('Ctrl Pts',(14.4478151405016,-0.180444274635945,
-3.2192445956183));
#66254=CARTESIAN_POINT('Ctrl Pts',(14.4539759632386,-0.0806111471565075,
-3.22328366531775));
#66255=CARTESIAN_POINT('Ctrl Pts',(14.4601367859755,0.0190775352223847,
-3.2226935333894));
#66256=CARTESIAN_POINT('Ctrl Pts',(14.4663079088922,0.118932885494522,-3.22210241482903));
#66257=CARTESIAN_POINT('Ctrl Pts',(14.4724790318089,0.218642874306915,-3.216866658042));
#66258=CARTESIAN_POINT('Ctrl Pts',(14.4786501547256,0.317747990616377,-3.20704751710343));
#66259=CARTESIAN_POINT('Ctrl Pts',(14.4833456766712,0.393155700823049,-3.19957626877693));
#66260=CARTESIAN_POINT('Ctrl Pts',(14.4880411986168,0.468213306109871,-3.18945255825233));
#66261=CARTESIAN_POINT('Ctrl Pts',(14.4927367205624,0.542723155715793,-3.17672301889068));
#66262=CARTESIAN_POINT('Ctrl Pts',(14.4989089686552,0.640666106989588,-3.15999008143301));
#66263=CARTESIAN_POINT('Ctrl Pts',(14.5050812167479,0.738006872541942,-3.13869386459617));
#66264=CARTESIAN_POINT('Ctrl Pts',(14.5112534648407,0.834287209290707,-3.11288972096891));
#66265=CARTESIAN_POINT('Ctrl Pts',(14.5174173534933,0.930437147892872,-3.08712052541742));
#66266=CARTESIAN_POINT('Ctrl Pts',(14.5235812421459,1.02552909642609,-3.05685564959215));
#66267=CARTESIAN_POINT('Ctrl Pts',(14.5297451307985,1.11911295547774,-3.02220180586636));
#66268=CARTESIAN_POINT('Ctrl Pts',(14.5359024924571,1.21259771778585,-2.98758465739014));
#66269=CARTESIAN_POINT('Ctrl Pts',(14.5420598541157,1.30457716035915,-2.94858793071974));
#66270=CARTESIAN_POINT('Ctrl Pts',(14.5482172157742,1.39461529270972,-2.90536843581673));
#66271=CARTESIAN_POINT('Ctrl Pts',(14.5543700799205,1.48458765864516,-2.86218050966321));
#66272=CARTESIAN_POINT('Ctrl Pts',(14.5605229440668,1.57262114314431,-2.81477613505698));
#66273=CARTESIAN_POINT('Ctrl Pts',(14.5666758082131,1.65829959581446,-2.76336027564659));
#66274=CARTESIAN_POINT('Ctrl Pts',(14.5728263413497,1.74394558924198,-2.71196389511103));
#66275=CARTESIAN_POINT('Ctrl Pts',(14.5789768744862,1.82723795159911,-2.6565592727689));
#66276=CARTESIAN_POINT('Ctrl Pts',(14.5851274076227,1.907785809704,-2.59739694055261));
#66277=CARTESIAN_POINT('Ctrl Pts',(14.5912772558379,1.98832469802615,-2.53824119663399));
#66278=CARTESIAN_POINT('Ctrl Pts',(14.5974271040532,2.06611933963936,-2.47532883193487));
#66279=CARTESIAN_POINT('Ctrl Pts',(14.6035769522684,2.14080933018176,-2.40895267166184));
#66280=CARTESIAN_POINT('Ctrl Pts',(14.6097277606475,2.21551098192824,-2.34256614820701));
#66281=CARTESIAN_POINT('Ctrl Pts',(14.6158785690267,2.28710669509953,-2.27271504359239));
#66282=CARTESIAN_POINT('Ctrl Pts',(14.6220293774058,2.35527129222109,-2.19973059771855));
#66283=CARTESIAN_POINT('Ctrl Pts',(14.628186763772,2.42350878802674,-2.12666809856943));
#66284=CARTESIAN_POINT('Ctrl Pts',(14.6343441501382,2.48830754328356,-2.05046588472324));
#66285=CARTESIAN_POINT('Ctrl Pts',(14.6405015365044,2.54938132119157,-1.9714899040217));
#66286=CARTESIAN_POINT('Ctrl Pts',(14.6466623592413,2.61048918371497,-1.89246984767889));
#66287=CARTESIAN_POINT('Ctrl Pts',(14.6528231819783,2.66786767939096,-1.81067329726025));
#66288=CARTESIAN_POINT('Ctrl Pts',(14.6589840047153,2.72127394644741,-1.72649519862829));
#66289=CARTESIAN_POINT('Ctrl Pts',(14.665155127632,2.77476950257646,-1.6421763639971));
#66290=CARTESIAN_POINT('Ctrl Pts',(14.6713262505487,2.82427934919663,-1.55546840527507));
#66291=CARTESIAN_POINT('Ctrl Pts',(14.6774973734654,2.86960655145587,-1.46679098795348));
#66292=CARTESIAN_POINT('Ctrl Pts',(14.6821928954109,2.90409539178722,-1.39931756946389));
#66293=CARTESIAN_POINT('Ctrl Pts',(14.6868884173565,2.93616365195819,-1.33070444888417));
#66294=CARTESIAN_POINT('Ctrl Pts',(14.691583939302,2.96574368857752,-1.2611431069322));
#66295=CARTESIAN_POINT('Ctrl Pts',(14.6977561873948,3.00462654904005,-1.16970495262861));
#66296=CARTESIAN_POINT('Ctrl Pts',(14.7039284354875,3.03934513022564,-1.0763059504372));
#66297=CARTESIAN_POINT('Ctrl Pts',(14.7101006835803,3.0696982184988,-0.981361508235005));
#66298=CARTESIAN_POINT('Ctrl Pts',(14.7162645722329,3.10001019779172,-0.886545654898761));
#66299=CARTESIAN_POINT('Ctrl Pts',(14.7224284608855,3.1259683047,-0.790188931883361));
#66300=CARTESIAN_POINT('Ctrl Pts',(14.7285923495381,3.14741893326219,-0.692727667299834));
#66301=CARTESIAN_POINT('Ctrl Pts',(14.7347497111967,3.16884684757155,-0.595369605277483));
#66302=CARTESIAN_POINT('Ctrl Pts',(14.7409070728552,3.18577667986992,-0.496909748861693));
#66303=CARTESIAN_POINT('Ctrl Pts',(14.7470644345138,3.19810459557383,-0.397799645889211));
#66304=CARTESIAN_POINT('Ctrl Pts',(14.7532172986601,3.21042350661716,-0.298761935757283));
#66305=CARTESIAN_POINT('Ctrl Pts',(14.7593701628064,3.21814713059089,-0.199075353121563));
#66306=CARTESIAN_POINT('Ctrl Pts',(14.7655230269527,3.22122286796484,-0.0992007933454522));
#66307=CARTESIAN_POINT('Ctrl Pts',(14.7716735600892,3.22429744009709,0.000635928999288105));
#66308=CARTESIAN_POINT('Ctrl Pts',(14.7778240932258,3.22272761107258,0.100660053293039));
#66309=CARTESIAN_POINT('Ctrl Pts',(14.7839746263623,3.21651278145447,0.200407308349853));
#66310=CARTESIAN_POINT('Ctrl Pts',(14.7901244745775,3.21029864391772,0.300143455585391));
#66311=CARTESIAN_POINT('Ctrl Pts',(14.7962743227927,3.19944056119897,0.399602361347613));
#66312=CARTESIAN_POINT('Ctrl Pts',(14.8024241710079,3.18398998614359,0.498322516687104));
#66313=CARTESIAN_POINT('Ctrl Pts',(14.8085749793871,3.16853699881972,0.597058085013978));
#66314=CARTESIAN_POINT('Ctrl Pts',(14.8147257877662,3.14849016215056,0.695054244632298));
#66315=CARTESIAN_POINT('Ctrl Pts',(14.8208765961454,3.12395229130314,0.791858348545924));
#66316=CARTESIAN_POINT('Ctrl Pts',(14.8270339825116,3.09938817840969,0.88876597968758));
#66317=CARTESIAN_POINT('Ctrl Pts',(14.8331913688777,3.07032354730051,0.984478587511042));
#66318=CARTESIAN_POINT('Ctrl Pts',(14.8393487552439,3.03691146539358,1.0785575153236));
#66319=CARTESIAN_POINT('Ctrl Pts',(14.8455095779809,3.00348073656488,1.17268894756889));
#66320=CARTESIAN_POINT('Ctrl Pts',(14.8516704007179,2.96569788932944,1.26518448195395));
#66321=CARTESIAN_POINT('Ctrl Pts',(14.8578312234548,2.92376383782047,1.35562626971939));
#66322=CARTESIAN_POINT('Ctrl Pts',(14.8640023463715,2.88175967745015,1.44621926564458));
#66323=CARTESIAN_POINT('Ctrl Pts',(14.8701734692882,2.83559065065569,1.53475127106041));
#66324=CARTESIAN_POINT('Ctrl Pts',(14.8763445922049,2.78550329909836,1.62082970518563));
#66325=CARTESIAN_POINT('Ctrl Pts',(14.8810401141505,2.74739252710284,1.68632559336259));
#66326=CARTESIAN_POINT('Ctrl Pts',(14.8857356360961,2.70701419507206,1.75040151652101));
#66327=CARTESIAN_POINT('Ctrl Pts',(14.8904311580417,2.66449280281853,1.81289703685241));
#66328=CARTESIAN_POINT('Ctrl Pts',(14.896814372111,2.60668812158707,1.89785506479306));
#66329=CARTESIAN_POINT('Ctrl Pts',(14.9031975861804,2.54471076740869,1.98020031839695));
#66330=CARTESIAN_POINT('Ctrl Pts',(14.9095808002497,2.4788277800295,2.05949760850894));
#66331=CARTESIAN_POINT('Ctrl Pts',(14.9157437809061,2.41521788501559,2.13605898648471));
#66332=CARTESIAN_POINT('Ctrl Pts',(14.9219067615624,2.34796770090169,2.20977885970649));
#66333=CARTESIAN_POINT('Ctrl Pts',(14.9280697422188,2.27736254300406,2.28029327285375));
#66334=CARTESIAN_POINT('Ctrl Pts',(14.93422696709,2.20682332529757,2.35074183055902));
#66335=CARTESIAN_POINT('Ctrl Pts',(14.9403841919612,2.1329356642205,2.41799057041968));
#66336=CARTESIAN_POINT('Ctrl Pts',(14.9465414168324,2.05602455353546,2.48170920894437));
#66337=CARTESIAN_POINT('Ctrl Pts',(14.9526938749316,1.97917298553922,2.54537851806749));
#66338=CARTESIAN_POINT('Ctrl Pts',(14.9588463330308,1.89930295711581,2.60552288544783));
#66339=CARTESIAN_POINT('Ctrl Pts',(14.9649987911301,1.81677481890174,2.66185026248746));
#66340=CARTESIAN_POINT('Ctrl Pts',(14.9656757697113,1.80769393106497,2.66804817999905));
#66341=CARTESIAN_POINT('Ctrl Pts',(14.9663527482925,1.79858089349769,2.67419992350421));
#66342=CARTESIAN_POINT('Ctrl Pts',(14.9670297268737,1.78943621037805,2.68030513402632));
#66343=CARTESIAN_POINT('Ctrl Pts',(13.7170510877849,1.78943621037804,2.68030513402632));
#66344=CARTESIAN_POINT('Ctrl Pts',(13.7232145029839,1.70663917467239,2.73558242761607));
#66345=CARTESIAN_POINT('Ctrl Pts',(13.729377918183,1.62116213230005,2.78709722951691));
#66346=CARTESIAN_POINT('Ctrl Pts',(13.735541333382,1.53338255777923,2.8345820669013));
#66347=CARTESIAN_POINT('Ctrl Pts',(13.7416983388329,1.44569427111637,2.88201752162333));
#66348=CARTESIAN_POINT('Ctrl Pts',(13.7478553442837,1.35570859301182,2.92543113856176));
#66349=CARTESIAN_POINT('Ctrl Pts',(13.7540123497345,1.26383127914569,2.96459913990964));
#66350=CARTESIAN_POINT('Ctrl Pts',(13.7601650149657,1.1720187317849,3.00373953080112));
#66351=CARTESIAN_POINT('Ctrl Pts',(13.7663176801968,1.07831759813188,3.03864008627275));
#66352=CARTESIAN_POINT('Ctrl Pts',(13.772470345428,0.983156677035549,3.06912373665521));
#66353=CARTESIAN_POINT('Ctrl Pts',(13.7786207852646,0.88803017526618,3.09959636122248));
#66354=CARTESIAN_POINT('Ctrl Pts',(13.7847712251012,0.79144534845544,3.1256551227528));
#66355=CARTESIAN_POINT('Ctrl Pts',(13.7909216649377,0.693848494545505,3.14717203678428));
#66356=CARTESIAN_POINT('Ctrl Pts',(13.7970715253643,0.596260834872262,3.16868692378731));
#66357=CARTESIAN_POINT('Ctrl Pts',(13.8032213857908,0.497661761876166,3.18566072054238));
#66358=CARTESIAN_POINT('Ctrl Pts',(13.8093712462173,0.39850918345149,3.19801625905886));
#66359=CARTESIAN_POINT('Ctrl Pts',(13.8155221722997,0.299339423737481,3.21037393855932));
#66360=CARTESIAN_POINT('Ctrl Pts',(13.8216730983822,0.199616399148244,3.21811171650219));
#66361=CARTESIAN_POINT('Ctrl Pts',(13.8278240244646,0.0998035720947606,
3.22120424833588));
#66362=CARTESIAN_POINT('Ctrl Pts',(13.8339815866838,-0.000116941437965382,
3.22430011665322));
#66363=CARTESIAN_POINT('Ctrl Pts',(13.840139148903,-0.100127015923435,3.22274071845078));
#66364=CARTESIAN_POINT('Ctrl Pts',(13.8462967111223,-0.199762881389789,
3.21655286816785));
#66365=CARTESIAN_POINT('Ctrl Pts',(13.852457804526,-0.299455885154504,3.21036146933107));
#66366=CARTESIAN_POINT('Ctrl Pts',(13.8586188979298,-0.398773820829627,
3.19953637987179));
#66367=CARTESIAN_POINT('Ctrl Pts',(13.8647799913335,-0.497259817801285,
3.18415612621307));
#66368=CARTESIAN_POINT('Ctrl Pts',(13.87095126572,-0.595908559299551,3.16875045724479));
#66369=CARTESIAN_POINT('Ctrl Pts',(13.8771225401064,-0.693722190827123,
3.1487746774174));
#66370=CARTESIAN_POINT('Ctrl Pts',(13.8832938144928,-0.790255683867928,
3.12435809673194));
#66371=CARTESIAN_POINT('Ctrl Pts',(13.8875942311097,-0.857524486316286,
3.10734354467486));
#66372=CARTESIAN_POINT('Ctrl Pts',(13.8918946477266,-0.92417195614628,3.08817363542435));
#66373=CARTESIAN_POINT('Ctrl Pts',(13.8961950643434,-0.990053149394673,
3.06690598549641));
#66374=CARTESIAN_POINT('Ctrl Pts',(13.9023673124362,-1.08461028318089,3.03638121931658));
#66375=CARTESIAN_POINT('Ctrl Pts',(13.908539560529,-1.17792084127548,3.00142562980689));
#66376=CARTESIAN_POINT('Ctrl Pts',(13.9147118086217,-1.26953915206813,2.96215933127611));
#66377=CARTESIAN_POINT('Ctrl Pts',(13.9208756972744,-1.36103337877134,2.92294621341257));
#66378=CARTESIAN_POINT('Ctrl Pts',(13.927039585927,-1.45083951786046,2.87943416029511));
#66379=CARTESIAN_POINT('Ctrl Pts',(13.9332034745796,-1.53852728006174,2.83179296047678));
#66380=CARTESIAN_POINT('Ctrl Pts',(13.9393608362382,-1.62612218894626,2.78420220832989));
#66381=CARTESIAN_POINT('Ctrl Pts',(13.9455181978967,-1.71160280099547,2.73249120842891));
#66382=CARTESIAN_POINT('Ctrl Pts',(13.9516755595552,-1.79455993366075,2.67687732386068));
#66383=CARTESIAN_POINT('Ctrl Pts',(13.9578284237016,-1.8774564720748,2.6213040612569));
#66384=CARTESIAN_POINT('Ctrl Pts',(13.9639812878479,-1.95783283603126,2.56183382296913));
#66385=CARTESIAN_POINT('Ctrl Pts',(13.9701341519942,-2.03530634521766,2.49872880553627));
#66386=CARTESIAN_POINT('Ctrl Pts',(13.9762846851307,-2.11275050360052,2.43564769541042));
#66387=CARTESIAN_POINT('Ctrl Pts',(13.9824352182672,-2.1872936559862,2.36893481632169));
#66388=CARTESIAN_POINT('Ctrl Pts',(13.9885857514038,-2.2585846373055,2.29889386415023));
#66389=CARTESIAN_POINT('Ctrl Pts',(13.994735599619,-2.32986767968476,2.22886071171598));
#66390=CARTESIAN_POINT('Ctrl Pts',(14.0008854478342,-2.39789896117152,2.15550052745351));
#66391=CARTESIAN_POINT('Ctrl Pts',(14.0070352960494,-2.4623635036378,2.07915452490972));
#66392=CARTESIAN_POINT('Ctrl Pts',(14.0131861044285,-2.52683811082871,2.00279660261188));
#66393=CARTESIAN_POINT('Ctrl Pts',(14.0193369128077,-2.58774459265207,1.92345226801713));
#66394=CARTESIAN_POINT('Ctrl Pts',(14.0254877211868,-2.64480831446049,1.84149573506448));
#66395=CARTESIAN_POINT('Ctrl Pts',(14.031645107553,-2.70193306311283,1.75945155363069));
#66396=CARTESIAN_POINT('Ctrl Pts',(14.0378024939192,-2.75520659652984,1.67478995244602));
#66397=CARTESIAN_POINT('Ctrl Pts',(14.0439598802854,-2.80439777096574,1.58791394751176));
#66398=CARTESIAN_POINT('Ctrl Pts',(14.0501207030223,-2.85361639846433,1.50098945801829));
#66399=CARTESIAN_POINT('Ctrl Pts',(14.0562815257593,-2.89874793352452,1.41184849117653));
#66400=CARTESIAN_POINT('Ctrl Pts',(14.0624423484963,-2.93960829835813,1.32091658128892));
#66401=CARTESIAN_POINT('Ctrl Pts',(14.068613471413,-2.98053697697379,1.22983264381422));
#66402=CARTESIAN_POINT('Ctrl Pts',(14.0747845943296,-3.01718006214866,1.13695218662884));
#66403=CARTESIAN_POINT('Ctrl Pts',(14.0809557172463,-3.04940245795269,1.04271866384566));
#66404=CARTESIAN_POINT('Ctrl Pts',(14.0856512391919,-3.07392003257883,0.971017681672536));
#66405=CARTESIAN_POINT('Ctrl Pts',(14.0903467611375,-3.09587927461857,0.898533715754632));
#66406=CARTESIAN_POINT('Ctrl Pts',(14.0950422830831,-3.11524052904747,0.825465934294087));
#66407=CARTESIAN_POINT('Ctrl Pts',(14.103012046215,-3.14810260775223,0.701447152662187));
#66408=CARTESIAN_POINT('Ctrl Pts',(14.1109818093469,-3.17357360472713,0.575393662707508));
#66409=CARTESIAN_POINT('Ctrl Pts',(14.1189515724789,-3.1914490294726,0.448074385318351));
#66410=CARTESIAN_POINT('Ctrl Pts',(14.1267580871456,-3.20895830335422,0.323363049506169));
#66411=CARTESIAN_POINT('Ctrl Pts',(14.1345646018123,-3.21918000356653,0.197437022552735));
#66412=CARTESIAN_POINT('Ctrl Pts',(14.142371116479,-3.22196690437122,0.0710410419164153));
#66413=CARTESIAN_POINT('Ctrl Pts',(14.14377189406,-3.22246697749405,0.0483609261964654));
#66414=CARTESIAN_POINT('Ctrl Pts',(14.1451726716411,-3.22272778695068,0.0256657426919609));
#66415=CARTESIAN_POINT('Ctrl Pts',(14.1465734492221,-3.22274864077389,0.00295988007751842));
#66416=CARTESIAN_POINT('',(13.9029341371857,-3.2227499320172,-0.000661954035870993));
#66417=CARTESIAN_POINT('Ctrl Pts',(13.4707798281485,1.78943605929599,2.68030523489233));
#66418=CARTESIAN_POINT('Ctrl Pts',(13.475472116723,1.73178109296317,2.71879707321372));
#66419=CARTESIAN_POINT('Ctrl Pts',(13.4801636509946,1.67288025823499,2.75543124047819));
#66420=CARTESIAN_POINT('Ctrl Pts',(13.493465968281,1.50136856300259,2.85457222591761));
#66421=CARTESIAN_POINT('Ctrl Pts',(13.5019812961287,1.38613982879161,2.91226967971131));
#66422=CARTESIAN_POINT('Ctrl Pts',(13.5107900562878,1.25789466570531,2.96714232882057));
#66423=CARTESIAN_POINT('Ctrl Pts',(13.5114645950295,1.24801312210909,2.97131214182194));
#66424=CARTESIAN_POINT('Ctrl Pts',(13.5124674222476,1.23322790220917,2.9774644371597));
#66425=CARTESIAN_POINT('Ctrl Pts',(13.5127979037898,1.22833998453966,2.97948425346831));
#66426=CARTESIAN_POINT('Ctrl Pts',(13.5133653525216,1.21992019566557,2.98293929071808));
#66427=CARTESIAN_POINT('Ctrl Pts',(13.5136026679237,1.21639072845848,2.98438028608694));
#66428=CARTESIAN_POINT('Ctrl Pts',(13.5140898232778,1.20912847488498,2.98733026366069));
#66429=CARTESIAN_POINT('Ctrl Pts',(13.5143396153137,1.2053954191628,2.98883851296559));
#66430=CARTESIAN_POINT('Ctrl Pts',(13.5149316619497,1.19652569748437,2.99240278539666));
#66431=CARTESIAN_POINT('Ctrl Pts',(13.515273539967,1.19138651387857,2.99445259612165));
#66432=CARTESIAN_POINT('Ctrl Pts',(13.515998713832,1.18044934496868,2.9987823729667));
#66433=CARTESIAN_POINT('Ctrl Pts',(13.5163817990303,1.17464996508667,3.00105878607369));
#66434=CARTESIAN_POINT('Ctrl Pts',(13.5174238949676,1.15881634818069,3.00722097907478));
#66435=CARTESIAN_POINT('Ctrl Pts',(13.518080993253,1.14876909012087,3.01107338514536));
#66436=CARTESIAN_POINT('Ctrl Pts',(13.5235938274091,1.06396343499389,3.04310403401477));
#66437=CARTESIAN_POINT('Ctrl Pts',(13.5283005706941,0.988193594633139,3.06854624511862));
#66438=CARTESIAN_POINT('Ctrl Pts',(13.5420905676021,0.759304431918389,3.13604347317865));
#66439=CARTESIAN_POINT('Ctrl Pts',(13.5508994701619,0.603940597876467,3.16963309849849));
#66440=CARTESIAN_POINT('Ctrl Pts',(13.5730984713102,0.21075901405121,3.22466578552728));
#66441=CARTESIAN_POINT('Ctrl Pts',(13.5865532958815,-0.0281045624538035,
3.23142020954005));
#66442=CARTESIAN_POINT('Ctrl Pts',(13.6021255296921,-0.285069768765774,
3.21017722171395));
#66443=CARTESIAN_POINT('Ctrl Pts',(13.6033160245126,-0.304609100386139,
3.20838212148868));
#66444=CARTESIAN_POINT('Ctrl Pts',(13.6050770586258,-0.33335060441998,3.20547669094511));
#66445=CARTESIAN_POINT('Ctrl Pts',(13.60564323057,-0.342566575631864,3.20450488844888));
#66446=CARTESIAN_POINT('Ctrl Pts',(13.6066544443938,-0.358982585442898,
3.20270223336299));
#66447=CARTESIAN_POINT('Ctrl Pts',(13.6070989962349,-0.36618428238834,3.20188681283525));
#66448=CARTESIAN_POINT('Ctrl Pts',(13.6080300358674,-0.381235016701606,
3.2001312341273));
#66449=CARTESIAN_POINT('Ctrl Pts',(13.6085166662575,-0.389083459426482,
3.19918647681224));
#66450=CARTESIAN_POINT('Ctrl Pts',(13.609788412441,-0.409546387809323,3.1966468349702));
#66451=CARTESIAN_POINT('Ctrl Pts',(13.6105749716476,-0.422154958041425,
3.19500616826451));
#66452=CARTESIAN_POINT('Ctrl Pts',(13.6140221714417,-0.477202963293567,
3.18751161019373));
#66453=CARTESIAN_POINT('Ctrl Pts',(13.6167071135228,-0.51953136647452,3.180886638509));
#66454=CARTESIAN_POINT('Ctrl Pts',(13.6238275203275,-0.6303054192645,3.16127899633989));
#66455=CARTESIAN_POINT('Ctrl Pts',(13.6283050005167,-0.698481106291388,
3.14691798264134));
#66456=CARTESIAN_POINT('Ctrl Pts',(13.6447324808073,-0.943339291470875,
3.08699063100358));
#66457=CARTESIAN_POINT('Ctrl Pts',(13.6570369473876,-1.11652416412197,3.0286565524379));
#66458=CARTESIAN_POINT('Ctrl Pts',(13.6755877892468,-1.36790432791554,2.91947908262879));
#66459=CARTESIAN_POINT('Ctrl Pts',(13.6817895632028,-1.45038972070421,2.87939072543201));
#66460=CARTESIAN_POINT('Ctrl Pts',(13.6951250068285,-1.62612411582044,2.78451258837201));
#66461=CARTESIAN_POINT('Ctrl Pts',(13.7022196045532,-1.71856270516239,2.72843133565982));
#66462=CARTESIAN_POINT('Ctrl Pts',(13.7097749313434,-1.81763559166391,2.66128791999342));
#66463=CARTESIAN_POINT('Ctrl Pts',(13.7105051270001,-1.82721776355131,2.65471802484882));
#66464=CARTESIAN_POINT('Ctrl Pts',(13.7115629374804,-1.84111281487212,2.64508018245146));
#66465=CARTESIAN_POINT('Ctrl Pts',(13.7118932661591,-1.84545386263266,2.64205329441554));
#66466=CARTESIAN_POINT('Ctrl Pts',(13.7124683645968,-1.85301537392027,2.63675314071104));
#66467=CARTESIAN_POINT('Ctrl Pts',(13.712713459211,-1.85623914591273,2.63448464313061));
#66468=CARTESIAN_POINT('Ctrl Pts',(13.7129589099059,-1.85946888746914,2.63220307331843));
#66469=CARTESIAN_POINT('Ctrl Pts',(13.7129596769703,-1.85947898083185,2.63219594302911));
#66470=CARTESIAN_POINT('Ctrl Pts',(13.7129612068001,-1.85949911101411,2.63218172221995));
#66471=CARTESIAN_POINT('Ctrl Pts',(13.7129619675692,-1.85950912156391,2.63217465026007));
#66472=CARTESIAN_POINT('Ctrl Pts',(13.7129634823091,-1.85952905323436,2.63216056934711));
#66473=CARTESIAN_POINT('Ctrl Pts',(13.7129642362126,-1.85953897346787,2.63215356102232));
#66474=CARTESIAN_POINT('Ctrl Pts',(13.7129657373464,-1.85955872615025,2.63213960622233));
#66475=CARTESIAN_POINT('Ctrl Pts',(13.7129664844812,-1.85956855734053,2.63213266063782));
#66476=CARTESIAN_POINT('Ctrl Pts',(13.7129679721254,-1.85958813256602,2.63211883087806));
#66477=CARTESIAN_POINT('Ctrl Pts',(13.7129687125591,-1.85959787560478,2.6321119474083));
#66478=CARTESIAN_POINT('Ctrl Pts',(13.7129701868977,-1.85961727579403,2.63209824098743));
#66479=CARTESIAN_POINT('Ctrl Pts',(13.7129709207116,-1.85962693174755,2.63209141888347));
#66480=CARTESIAN_POINT('Ctrl Pts',(13.7129723819031,-1.85964615898363,2.63207783433844));
#66481=CARTESIAN_POINT('Ctrl Pts',(13.7129731091826,-1.85965572897624,2.6320710728102));
#66482=CARTESIAN_POINT('Ctrl Pts',(13.7129745573532,-1.85967478492103,2.63205760897531));
#66483=CARTESIAN_POINT('Ctrl Pts',(13.7129752781642,-1.85968426981796,2.63205090741566));
#66484=CARTESIAN_POINT('Ctrl Pts',(13.712976713489,-1.85970315677204,2.63203756267377));
#66485=CARTESIAN_POINT('Ctrl Pts',(13.7129774279097,-1.85971255760438,2.63203092035831));
#66486=CARTESIAN_POINT('Ctrl Pts',(13.7129788505282,-1.8597312774026,2.6320176934211));
#66487=CARTESIAN_POINT('Ctrl Pts',(13.7129795586303,-1.85974059511145,2.63201110968891));
#66488=CARTESIAN_POINT('Ctrl Pts',(13.7129809687011,-1.85975914984145,2.63199799908929));
#66489=CARTESIAN_POINT('Ctrl Pts',(13.7129816705651,-1.85976838548415,2.6319914731972));
#66490=CARTESIAN_POINT('Ctrl Pts',(13.712983068205,-1.85978677667963,2.63197847785927));
#66491=CARTESIAN_POINT('Ctrl Pts',(13.7129837638899,-1.85979593103509,2.63197200926078));
#66492=CARTESIAN_POINT('Ctrl Pts',(13.7129851492796,-1.85981416107415,2.63195912751181));
#66493=CARTESIAN_POINT('Ctrl Pts',(13.7129858388699,-1.85982323525057,2.63195271542762));
#66494=CARTESIAN_POINT('Ctrl Pts',(13.7129872121093,-1.85984130544608,2.63193994634741));
#66495=CARTESIAN_POINT('Ctrl Pts',(13.7129878956613,-1.85985030018644,2.63193359025623));
#66496=CARTESIAN_POINT('Ctrl Pts',(13.7129892569308,-1.85986821291092,2.63192093217559));
#66497=CARTESIAN_POINT('Ctrl Pts',(13.7129899345292,-1.85987712932796,2.63191463129474));
#66498=CARTESIAN_POINT('Ctrl Pts',(13.7129912839212,-1.85989488579754,2.6319020833615));
#66499=CARTESIAN_POINT('Ctrl Pts',(13.7129919556219,-1.85990372462671,2.63189583717484));
#66500=CARTESIAN_POINT('Ctrl Pts',(13.7129932932905,-1.85992132686555,2.63188339796564));
#66501=CARTESIAN_POINT('Ctrl Pts',(13.7129939591565,-1.85993008893525,2.63187720589124));
#66502=CARTESIAN_POINT('Ctrl Pts',(13.7129952852474,-1.85994753886252,2.63186487405676));
#66503=CARTESIAN_POINT('Ctrl Pts',(13.7129959453508,-1.85995622512023,2.63185873542847));
#66504=CARTESIAN_POINT('Ctrl Pts',(13.7129972599885,-1.85997352437223,2.63184650981911));
#66505=CARTESIAN_POINT('Ctrl Pts',(13.7129979144007,-1.85998213575863,2.63184042397549));
#66506=CARTESIAN_POINT('Ctrl Pts',(13.7129992176853,-1.85999928565061,2.63182830366839));
#66507=CARTESIAN_POINT('Ctrl Pts',(13.7129998664553,-1.86000782280877,2.63182227015828));
#66508=CARTESIAN_POINT('Ctrl Pts',(13.7130011585583,-1.86002482559782,2.63181025356479));
#66509=CARTESIAN_POINT('Ctrl Pts',(13.7130018017641,-1.86003328955411,2.63180427166603));
#66510=CARTESIAN_POINT('Ctrl Pts',(13.7130030827644,-1.86005014627723,2.63179235805966));
#66511=CARTESIAN_POINT('Ctrl Pts',(13.7130037204523,-1.8600585376403,2.63178642734525));
#66512=CARTESIAN_POINT('Ctrl Pts',(13.7130049905155,-1.86007525047453,2.63177461519362));
#66513=CARTESIAN_POINT('Ctrl Pts',(13.7130056227575,-1.86008357019278,2.63176873499637));
#66514=CARTESIAN_POINT('Ctrl Pts',(13.7130068819857,-1.86010014048178,2.63175702335595));
#66515=CARTESIAN_POINT('Ctrl Pts',(13.713007508845,-1.86010838938452,2.63175119309275));
#66516=CARTESIAN_POINT('Ctrl Pts',(13.7130087573378,-1.86012481843846,2.63173958104355));
#66517=CARTESIAN_POINT('Ctrl Pts',(13.7130093788593,-1.86013299711738,2.63173380029919));
#66518=CARTESIAN_POINT('Ctrl Pts',(13.7130106167791,-1.86014928707204,2.63172228633755));
#66519=CARTESIAN_POINT('Ctrl Pts',(13.7130112330371,-1.8601573965026,2.63171655442548));
#66520=CARTESIAN_POINT('Ctrl Pts',(13.7130123086086,-1.86017155012259,2.63170655025804));
#66521=CARTESIAN_POINT('Ctrl Pts',(13.713012767825,-1.86017759302839,2.63170227893443));
#66522=CARTESIAN_POINT('Ctrl Pts',(13.713013677046,-1.86018955763162,2.63169382190114));
#66523=CARTESIAN_POINT('Ctrl Pts',(13.7130141332754,-1.86019556124156,2.63168957829215));
#66524=CARTESIAN_POINT('Ctrl Pts',(13.7130150448454,-1.86020755677272,2.63168109927472));
#66525=CARTESIAN_POINT('Ctrl Pts',(13.7130155001755,-1.86021354855704,2.63167686396316));
#66526=CARTESIAN_POINT('Ctrl Pts',(13.7130164099625,-1.86022552064425,2.6316684013944));
#66527=CARTESIAN_POINT('Ctrl Pts',(13.7130168643996,-1.86023150068554,2.63166417432223));
#66528=CARTESIAN_POINT('Ctrl Pts',(13.7130177724066,-1.86024344936588,2.63165572817666));
#66529=CARTESIAN_POINT('Ctrl Pts',(13.7130182259544,-1.8602494177128,2.63165150930987));
#66530=CARTESIAN_POINT('Ctrl Pts',(13.7130191321948,-1.86026134316285,2.63164307946337));
#66531=CARTESIAN_POINT('Ctrl Pts',(13.7130195848623,-1.86026729993606,2.631638868717));
#66532=CARTESIAN_POINT('Ctrl Pts',(13.7130204893233,-1.8602792019874,2.63163045528935));
#66533=CARTESIAN_POINT('Ctrl Pts',(13.7130209411047,-1.86028514710763,2.6316262527198));
#66534=CARTESIAN_POINT('Ctrl Pts',(13.7130218438284,-1.86029702631449,2.63161785531991));
#66535=CARTESIAN_POINT('Ctrl Pts',(13.7130222947422,-1.86030296002579,2.63161366075501));
#66536=CARTESIAN_POINT('Ctrl Pts',(13.7130231956894,-1.86031481587198,2.63160527974848));
#66537=CARTESIAN_POINT('Ctrl Pts',(13.7130236457219,-1.86032073799564,2.63160109331491));
#66538=CARTESIAN_POINT('Ctrl Pts',(13.7130245449389,-1.8603325710911,2.63159272827128));
#66539=CARTESIAN_POINT('Ctrl Pts',(13.7130249940981,-1.8603384817295,2.63158854989702));
#66540=CARTESIAN_POINT('Ctrl Pts',(13.7130258915968,-1.86035029223039,2.63158020070656));
#66541=CARTESIAN_POINT('Ctrl Pts',(13.7130263398986,-1.86035619159505,2.63157603024242));
#66542=CARTESIAN_POINT('Ctrl Pts',(13.7130272356506,-1.86036797912614,2.63156769717111));
#66543=CARTESIAN_POINT('Ctrl Pts',(13.7130276830874,-1.86037386711608,2.63156353468882));
#66544=CARTESIAN_POINT('Ctrl Pts',(13.7133048829,-1.86402164702195,2.62898473826822));
#66545=CARTESIAN_POINT('Ctrl Pts',(13.7135811096231,-1.8676582163532,2.62640252856947));
#66546=CARTESIAN_POINT('Ctrl Pts',(13.7141487305406,-1.87513398028595,2.62107085310928));
#66547=CARTESIAN_POINT('Ctrl Pts',(13.7144400617531,-1.87897251860471,2.61832048000925));
#66548=CARTESIAN_POINT('Ctrl Pts',(13.7151681126134,-1.88856873985323,2.61141266595074));
#66549=CARTESIAN_POINT('Ctrl Pts',(13.7156041177429,-1.89431878584141,2.60724458707641));
#66550=CARTESIAN_POINT('Ctrl Pts',(13.7168323983563,-1.91052450261047,2.59541551514139));
#66551=CARTESIAN_POINT('Ctrl Pts',(13.7176217835708,-1.92094793331699,2.58771030476677));
#66552=CARTESIAN_POINT('Ctrl Pts',(13.720216106041,-1.95521892891283,2.56205530311659));
#66553=CARTESIAN_POINT('Ctrl Pts',(13.722004327061,-1.97886434183239,2.54383656871033));
#66554=CARTESIAN_POINT('Ctrl Pts',(13.7296389589279,-2.07969913920053,2.46388662809098));
#66555=CARTESIAN_POINT('Ctrl Pts',(13.735309721038,-2.15428497136974,2.39894669424279));
#66556=CARTESIAN_POINT('Ctrl Pts',(13.7593860216655,-2.4620357535809,2.10504768684837));
#66557=CARTESIAN_POINT('Ctrl Pts',(13.7770964017509,-2.66259972762664,1.84483235428617));
#66558=CARTESIAN_POINT('Ctrl Pts',(13.7969862789744,-2.82320412401723,1.55424079467385));
#66559=CARTESIAN_POINT('Ctrl Pts',(13.7973059838386,-2.82577086204425,1.54956929771163));
#66560=CARTESIAN_POINT('Ctrl Pts',(13.7992709366899,-2.84145546747076,1.52085454470699));
#66561=CARTESIAN_POINT('Ctrl Pts',(13.8009262495942,-2.85427766985789,1.49665180732512));
#66562=CARTESIAN_POINT('Ctrl Pts',(13.8032646468596,-2.87183683464052,1.46246122029424));
#66563=CARTESIAN_POINT('Ctrl Pts',(13.8039385673435,-2.87683350937794,1.45260751072356));
#66564=CARTESIAN_POINT('Ctrl Pts',(13.8050294551156,-2.88481835889024,1.43665816459803));
#66565=CARTESIAN_POINT('Ctrl Pts',(13.8054453106767,-2.88783814294646,1.43057838118803));
#66566=CARTESIAN_POINT('Ctrl Pts',(13.8063112075927,-2.89407576595085,1.41791983480526));
#66567=CARTESIAN_POINT('Ctrl Pts',(13.8067613567944,-2.89729043131036,1.41133955950519));
#66568=CARTESIAN_POINT('Ctrl Pts',(13.8078225657722,-2.90480276983812,1.39582830716606));
#66569=CARTESIAN_POINT('Ctrl Pts',(13.8084342734203,-2.90908170977681,1.38688838666615));
#66570=CARTESIAN_POINT('Ctrl Pts',(13.8104417426095,-2.92295572100962,1.35755492591218));
#66571=CARTESIAN_POINT('Ctrl Pts',(13.811843466801,-2.93237794250448,1.33708080704151));
#66572=CARTESIAN_POINT('Ctrl Pts',(13.8151486393364,-2.953971720138,1.2888320867976));
#66573=CARTESIAN_POINT('Ctrl Pts',(13.8170579556481,-2.96596737648447,1.26098155892362));
#66574=CARTESIAN_POINT('Ctrl Pts',(13.823838915862,-3.00688527815918,1.1621663707528));
#66575=CARTESIAN_POINT('Ctrl Pts',(13.8287799402461,-3.03366598657939,1.09034806074541));
#66576=CARTESIAN_POINT('Ctrl Pts',(13.8564405433384,-3.16716600015925,0.689203114943928));
#66577=CARTESIAN_POINT('Ctrl Pts',(13.8806910018625,-3.22282100853309,0.345376931363903));
#66578=CARTESIAN_POINT('Ctrl Pts',(13.9029341371857,-3.2227499320172,-0.000661954035870993));
#66579=CARTESIAN_POINT('Ctrl Pts',(13.9029343323106,-3.22274993139226,-0.000664989615965877));
#66580=CARTESIAN_POINT('Ctrl Pts',(13.904215504374,-3.22274581871248,-0.0205963361621372));
#66581=CARTESIAN_POINT('Ctrl Pts',(13.9054885607806,-3.22255680548054,-0.0405278534713367));
#66582=CARTESIAN_POINT('Ctrl Pts',(13.9076135515616,-3.22192814459894,-0.074033680711978));
#66583=CARTESIAN_POINT('Ctrl Pts',(13.9084703521966,-3.22158759675995,-0.0876089400347084));
#66584=CARTESIAN_POINT('Ctrl Pts',(13.9096535050165,-3.22099568948733,-0.106452512377118));
#66585=CARTESIAN_POINT('Ctrl Pts',(13.9099837438076,-3.22081719442239,-0.11172273773818));
#66586=CARTESIAN_POINT('Ctrl Pts',(13.9105629791671,-3.2204807015838,-0.120985870745676));
#66587=CARTESIAN_POINT('Ctrl Pts',(13.9108122780473,-3.22032821198566,-0.124978949004372));
#66588=CARTESIAN_POINT('Ctrl Pts',(13.9113011899043,-3.22001406553136,-0.132822561126043));
#66589=CARTESIAN_POINT('Ctrl Pts',(13.9115408315839,-3.21985292762392,-0.136673113912842));
#66590=CARTESIAN_POINT('Ctrl Pts',(13.9120191671923,-3.21951694725458,-0.144371125512332));
#66591=CARTESIAN_POINT('Ctrl Pts',(13.9122578614134,-3.21934211555479,-0.148218551227557));
#66592=CARTESIAN_POINT('Ctrl Pts',(13.9129002099964,-3.21885227313186,-0.158588289752942));
#66593=CARTESIAN_POINT('Ctrl Pts',(13.9133031396712,-3.21852433359483,-0.165110016997159));
#66594=CARTESIAN_POINT('Ctrl Pts',(13.9147859447218,-3.21724111963642,-0.18917102367664));
#66595=CARTESIAN_POINT('Ctrl Pts',(13.9158590842077,-3.21616225834951,-0.206703793240447));
#66596=CARTESIAN_POINT('Ctrl Pts',(13.9185985462839,-3.21302142154262,-0.251736674087955));
#66597=CARTESIAN_POINT('Ctrl Pts',(13.9202542934914,-3.21074969519869,-0.279221259841623));
#66598=CARTESIAN_POINT('Ctrl Pts',(13.9374338652326,-3.18326959943628,-0.566691067286937));
#66599=CARTESIAN_POINT('Ctrl Pts',(13.9516129073683,-3.12689232925233,-0.822754421194623));
#66600=CARTESIAN_POINT('Ctrl Pts',(13.9714255379752,-3.01019132116688,-1.15457856374885));
#66601=CARTESIAN_POINT('Ctrl Pts',(13.9765692811185,-2.97659420506073,-1.23862381874234));
#66602=CARTESIAN_POINT('Ctrl Pts',(13.9875992713221,-2.89852797860838,-1.41231936371177));
#66603=CARTESIAN_POINT('Ctrl Pts',(13.9935011572372,-2.853331977305,-1.50153389217408));
#66604=CARTESIAN_POINT('Ctrl Pts',(14.0005497576198,-2.79594350547301,-1.60283782427328));
#66605=CARTESIAN_POINT('Ctrl Pts',(14.0015513664645,-2.78771037645488,-1.61711472012142));
#66606=CARTESIAN_POINT('Ctrl Pts',(14.0030896146388,-2.77494911995102,-1.63885666208952));
#66607=CARTESIAN_POINT('Ctrl Pts',(14.0036233991778,-2.77049947892214,-1.64636764184584));
#66608=CARTESIAN_POINT('Ctrl Pts',(14.0045982203501,-2.76233480772296,-1.66002274787548));
#66609=CARTESIAN_POINT('Ctrl Pts',(14.005038893793,-2.75862964764942,-1.66617273390393));
#66610=CARTESIAN_POINT('Ctrl Pts',(14.0059931505848,-2.75057571541557,-1.67944049332981));
#66611=CARTESIAN_POINT('Ctrl Pts',(14.0065069941959,-2.7462198076236,-1.68655385416343));
#66612=CARTESIAN_POINT('Ctrl Pts',(14.0079043020552,-2.73432343312714,-1.70581279722629));
#66613=CARTESIAN_POINT('Ctrl Pts',(14.0087897285464,-2.72672975359577,-1.71792513701592));
#66614=CARTESIAN_POINT('Ctrl Pts',(14.0130542472654,-2.68989430187898,-1.77582018755457));
#66615=CARTESIAN_POINT('Ctrl Pts',(14.0164731733668,-2.65958008668491,-1.82090688286336));
#66616=CARTESIAN_POINT('Ctrl Pts',(14.020649293548,-2.62164515003427,-1.87435863532592));
#66617=CARTESIAN_POINT('Ctrl Pts',(14.0213662998812,-2.61510022377665,-1.88347933387328));
#66618=CARTESIAN_POINT('Ctrl Pts',(14.0236300633617,-2.59433655904905,-1.91209772542658));
#66619=CARTESIAN_POINT('Ctrl Pts',(14.0251830186322,-2.57994664605889,-1.93146968611412));
#66620=CARTESIAN_POINT('Ctrl Pts',(14.030702084704,-2.52829218468731,-1.99940058543471));
#66621=CARTESIAN_POINT('Ctrl Pts',(14.0347087736727,-2.48986488953538,-2.04705549329416));
#66622=CARTESIAN_POINT('Ctrl Pts',(14.0549204115848,-2.29127835244114,-2.2794597095774));
#66623=CARTESIAN_POINT('Ctrl Pts',(14.0717370377799,-2.11183361977564,-2.44663774271791));
#66624=CARTESIAN_POINT('Ctrl Pts',(14.0924586966739,-1.86128058299915,-2.63177721136415));
#66625=CARTESIAN_POINT('Ctrl Pts',(14.0968678567232,-1.80609949481193,-2.66994803975714));
#66626=CARTESIAN_POINT('Ctrl Pts',(14.1026704461328,-1.7304386653517,-2.71886541668517));
#66627=CARTESIAN_POINT('Ctrl Pts',(14.1041419105404,-1.71097971748581,-2.73115279724182));
#66628=CARTESIAN_POINT('Ctrl Pts',(14.1062820343509,-1.6822509565403,-2.74886605000701));
#66629=CARTESIAN_POINT('Ctrl Pts',(14.1069601957909,-1.67308344247473,-2.75445541688525));
#66630=CARTESIAN_POINT('Ctrl Pts',(14.1080268012456,-1.65856059933289,-2.76321063206034));
#66631=CARTESIAN_POINT('Ctrl Pts',(14.108417116168,-1.65322383925897,-2.76640691106741));
#66632=CARTESIAN_POINT('Ctrl Pts',(14.1091520225251,-1.6431327096732,-2.77241103514451));
#66633=CARTESIAN_POINT('Ctrl Pts',(14.1094968206847,-1.63838032300039,-2.77522214744606));
#66634=CARTESIAN_POINT('Ctrl Pts',(14.1100915733927,-1.63015132766132,-2.78006122418263));
#66635=CARTESIAN_POINT('Ctrl Pts',(14.1103419002772,-1.62667811168026,-2.78209490904811));
#66636=CARTESIAN_POINT('Ctrl Pts',(14.1108285463644,-1.61990695112023,-2.78604263638415));
#66637=CARTESIAN_POINT('Ctrl Pts',(14.1110649094346,-1.61660942337796,-2.78795733013341));
#66638=CARTESIAN_POINT('Ctrl Pts',(14.1116283896445,-1.60872749470395,-2.79251524853918));
#66639=CARTESIAN_POINT('Ctrl Pts',(14.1119551553953,-1.60413994839402,-2.79515305349255));
#66640=CARTESIAN_POINT('Ctrl Pts',(14.1129427805934,-1.59022443850809,-2.80310882558141));
#66641=CARTESIAN_POINT('Ctrl Pts',(14.1136014155708,-1.58087626224603,-2.80839155102719));
#66642=CARTESIAN_POINT('Ctrl Pts',(14.1222084563203,-1.45784981981265,-2.87710578602502));
#66643=CARTESIAN_POINT('Ctrl Pts',(14.1297440702819,-1.34044074676066,-2.93364809932216));
#66644=CARTESIAN_POINT('Ctrl Pts',(14.1451446028459,-1.08917613345362,-3.0364066739481));
#66645=CARTESIAN_POINT('Ctrl Pts',(14.1529695774844,-0.955056731399472,
-3.08122360094422));
#66646=CARTESIAN_POINT('Ctrl Pts',(14.1725895787907,-0.616626357708059,
-3.17008206154289));
#66647=CARTESIAN_POINT('Ctrl Pts',(14.184478592267,-0.41018881889637,-3.20333818142817));
#66648=CARTESIAN_POINT('Ctrl Pts',(14.1983384781767,-0.180900128263713,
-3.21773829586386));
#66649=CARTESIAN_POINT('Ctrl Pts',(14.1996203355713,-0.159786380194437,
-3.21885583350487));
#66650=CARTESIAN_POINT('Ctrl Pts',(14.2014971775982,-0.129015546987957,
-3.22018102094396));
#66651=CARTESIAN_POINT('Ctrl Pts',(14.2020869975005,-0.119365813841638,
-3.2205531540873));
#66652=CARTESIAN_POINT('Ctrl Pts',(14.2031239783926,-0.102436861993183,
-3.22112981409548));
#66653=CARTESIAN_POINT('Ctrl Pts',(14.2035705488083,-0.0951583167500675,
-3.22135305164167));
#66654=CARTESIAN_POINT('Ctrl Pts',(14.2044391229376,-0.0810249372306493,
-3.22173858916093));
#66655=CARTESIAN_POINT('Ctrl Pts',(14.204861036382,-0.0741702134103058,
-3.22190368503225));
#66656=CARTESIAN_POINT('Ctrl Pts',(14.205986733496,-0.0559099602525115,
-3.22228517854179));
#66657=CARTESIAN_POINT('Ctrl Pts',(14.2066917276389,-0.0445037985140977,
-3.22246289382074));
#66658=CARTESIAN_POINT('Ctrl Pts',(14.2092307360877,-0.00353386313378993,
-3.22288366971615));
#66659=CARTESIAN_POINT('Ctrl Pts',(14.2110755657518,0.0260312731350481,
-3.22278046344612));
#66660=CARTESIAN_POINT('Ctrl Pts',(14.2342540185632,0.394860917139358,-3.21641748073574));
#66661=CARTESIAN_POINT('Ctrl Pts',(14.2574473391875,0.731025103735886,-3.15701530245414));
#66662=CARTESIAN_POINT('Ctrl Pts',(14.288153653159,1.1632912229544,-3.00779467591996));
#66663=CARTESIAN_POINT('Ctrl Pts',(14.2959779260124,1.27277573590477,-2.96312728248251));
#66664=CARTESIAN_POINT('Ctrl Pts',(14.3043358080653,1.39146986954189,-2.90690600898772));
#66665=CARTESIAN_POINT('Ctrl Pts',(14.3051698618159,1.40333541110378,-2.90119642222333));
#66666=CARTESIAN_POINT('Ctrl Pts',(14.3064523366813,1.42161797961378,-2.89226061366347));
#66667=CARTESIAN_POINT('Ctrl Pts',(14.3069036903497,1.42805961936003,-2.88908547176378));
#66668=CARTESIAN_POINT('Ctrl Pts',(14.3076517531045,1.43874892792106,-2.88377213003578));
#66669=CARTESIAN_POINT('Ctrl Pts',(14.3079491881449,1.44300253520505,-2.88164603302372));
#66670=CARTESIAN_POINT('Ctrl Pts',(14.3085256554515,1.45125363579077,-2.87749900273544));
#66671=CARTESIAN_POINT('Ctrl Pts',(14.3088047527989,1.45525164964701,-2.87547913623503));
#66672=CARTESIAN_POINT('Ctrl Pts',(14.3093268774783,1.46273731810461,-2.87167763481586));
#66673=CARTESIAN_POINT('Ctrl Pts',(14.3095700226823,1.46622589705797,-2.86989799802544));
#66674=CARTESIAN_POINT('Ctrl Pts',(14.3101299809209,1.47426592871497,-2.86577803153793));
#66675=CARTESIAN_POINT('Ctrl Pts',(14.3104465069657,1.47881504761461,-2.86343322087745));
#66676=CARTESIAN_POINT('Ctrl Pts',(14.3114057242902,1.49261334336807,-2.85627933560318));
#66677=CARTESIAN_POINT('Ctrl Pts',(14.3120462946643,1.50184490055567,-2.85143615349296));
#66678=CARTESIAN_POINT('Ctrl Pts',(14.3167679378365,1.56999953848465,-2.81525715370515));
#66679=CARTESIAN_POINT('Ctrl Pts',(14.3207418257078,1.6279648599433,-2.78214005176248));
#66680=CARTESIAN_POINT('Ctrl Pts',(14.3426896464391,1.94811558478924,-2.5857939849455));
#66681=CARTESIAN_POINT('Ctrl Pts',(14.3592009975871,2.18681205147607,-2.38733680873805));
#66682=CARTESIAN_POINT('Ctrl Pts',(14.3813340928892,2.4440914760308,-2.1019545067161));
#66683=CARTESIAN_POINT('Ctrl Pts',(14.3857341947261,2.49256676315334,-2.04423717344593));
#66684=CARTESIAN_POINT('Ctrl Pts',(14.3929121501563,2.56693565923299,-1.94910755786534));
#66685=CARTESIAN_POINT('Ctrl Pts',(14.3956387366972,2.59413871364243,-1.91275272082248));
#66686=CARTESIAN_POINT('Ctrl Pts',(14.3991836820937,2.62811964878319,-1.86528099464661));
#66687=CARTESIAN_POINT('Ctrl Pts',(14.3999743481373,2.63561163539639,-1.85467985834762));
#66688=CARTESIAN_POINT('Ctrl Pts',(14.4012540894808,2.64759648489574,-1.83750206752296));
#66689=CARTESIAN_POINT('Ctrl Pts',(14.4017416274903,2.65212942369649,-1.83095344374043));
#66690=CARTESIAN_POINT('Ctrl Pts',(14.4026736419855,2.66073201189848,-1.8184265244883));
#66691=CARTESIAN_POINT('Ctrl Pts',(14.4031179530116,2.66480590900591,-1.81245119384582));
#66692=CARTESIAN_POINT('Ctrl Pts',(14.4041356475997,2.67407497961227,-1.79875710834075));
#66693=CARTESIAN_POINT('Ctrl Pts',(14.4047095283861,2.67925689008154,-1.79102949317902));
#66694=CARTESIAN_POINT('Ctrl Pts',(14.4064775419898,2.6950828502744,-1.76720636981167));
#66695=CARTESIAN_POINT('Ctrl Pts',(14.4076758350766,2.70561571061902,-1.75103784188162));
#66696=CARTESIAN_POINT('Ctrl Pts',(14.4246654213182,2.85221418552439,-1.52152011888532));
#66697=CARTESIAN_POINT('Ctrl Pts',(14.4414383828598,2.96280666625669,-1.29300977619716));
#66698=CARTESIAN_POINT('Ctrl Pts',(14.4728185426104,3.11459202453157,-0.85441663366588));
#66699=CARTESIAN_POINT('Ctrl Pts',(14.4872192208717,3.16387849642374,-0.64853607561234));
#66700=CARTESIAN_POINT('Ctrl Pts',(14.5024328071761,3.19627895368416,-0.413061615847468));
#66701=CARTESIAN_POINT('Ctrl Pts',(14.5041130587061,3.19956581077213,-0.386778721202662));
#66702=CARTESIAN_POINT('Ctrl Pts',(14.5062384445783,3.20335232666292,-0.353136942635103));
#66703=CARTESIAN_POINT('Ctrl Pts',(14.5066995750162,3.20415116975536,-0.345813696777634));
#66704=CARTESIAN_POINT('Ctrl Pts',(14.5074378624624,3.20539372001431,-0.334048777774984));
#66705=CARTESIAN_POINT('Ctrl Pts',(14.5077159043965,3.20585331609835,-0.329608862866269));
#66706=CARTESIAN_POINT('Ctrl Pts',(14.5082456549275,3.20671303508197,-0.32113164383283));
#66707=CARTESIAN_POINT('Ctrl Pts',(14.5084974477463,3.2071147539433,-0.317094587182505));
#66708=CARTESIAN_POINT('Ctrl Pts',(14.5090768531731,3.20802317653495,-0.307787093319658));
#66709=CARTESIAN_POINT('Ctrl Pts',(14.5094041603489,3.20852451584369,-0.302516161849091));
#66710=CARTESIAN_POINT('Ctrl Pts',(14.5104221666001,3.21004674249933,-0.286082372272008));
#66711=CARTESIAN_POINT('Ctrl Pts',(14.5111103628342,3.21102239493499,-0.274915260769156));
#66712=CARTESIAN_POINT('Ctrl Pts',(14.5176069921243,3.21972106140518,-0.168980381820534));
#66713=CARTESIAN_POINT('Ctrl Pts',(14.5231963998168,3.22330565110424,-0.0739093700151808));
#66714=CARTESIAN_POINT('Ctrl Pts',(14.5367032274469,3.22176233073709,0.160802273314587));
#66715=CARTESIAN_POINT('Ctrl Pts',(14.5444750960817,3.21177292296152,0.300214516479386));
#66716=CARTESIAN_POINT('Ctrl Pts',(14.5658855549688,3.15964155633866,0.679749956806448));
#66717=CARTESIAN_POINT('Ctrl Pts',(14.5795790608378,3.09929183890609,0.916385890315111));
#66718=CARTESIAN_POINT('Ctrl Pts',(14.5956346641905,3.00469667411899,1.1655246046522));
#66719=CARTESIAN_POINT('Ctrl Pts',(14.5970319733792,2.99627713411096,1.1870016851379));
#66720=CARTESIAN_POINT('Ctrl Pts',(14.599046467676,2.98387640023237,1.21766140436178));
#66721=CARTESIAN_POINT('Ctrl Pts',(14.5996573463794,2.98008174235401,1.22691909793273));
#66722=CARTESIAN_POINT('Ctrl Pts',(14.6007189073718,2.97342870361746,1.24293731957862));
#66723=CARTESIAN_POINT('Ctrl Pts',(14.601168911418,2.97059020758859,1.24970606666598));
#66724=CARTESIAN_POINT('Ctrl Pts',(14.6020352653524,2.96509069730047,1.26269572731159));
#66725=CARTESIAN_POINT('Ctrl Pts',(14.6024514946043,2.96243316366149,1.26891807959101));
#66726=CARTESIAN_POINT('Ctrl Pts',(14.6034335400205,2.95612703373186,1.28355547136469));
#66727=CARTESIAN_POINT('Ctrl Pts',(14.6039999136637,2.95246208376798,1.29196336200113));
#66728=CARTESIAN_POINT('Ctrl Pts',(14.6056788153165,2.9415157719382,1.31678585310519));
#66729=CARTESIAN_POINT('Ctrl Pts',(14.6067948126359,2.93413314490471,1.3331551621737));
#66730=CARTESIAN_POINT('Ctrl Pts',(14.6206375805125,2.84126188978362,1.53456758078043));
#66731=CARTESIAN_POINT('Ctrl Pts',(14.6339823251602,2.73855735501287,1.71112318763954));
#66732=CARTESIAN_POINT('Ctrl Pts',(14.6595098741317,2.5172433211441,2.02006774846566));
#66733=CARTESIAN_POINT('Ctrl Pts',(14.6715528773686,2.4030128061943,2.15469642417142));
#66734=CARTESIAN_POINT('Ctrl Pts',(14.6880677156243,2.22777418122208,2.32986114775148));
#66735=CARTESIAN_POINT('Ctrl Pts',(14.6927781300022,2.1755284700299,2.37871984003691));
#66736=CARTESIAN_POINT('Ctrl Pts',(14.6997325016839,2.09433871536258,2.44973140536204));
#66737=CARTESIAN_POINT('Ctrl Pts',(14.7020496758095,2.06657617604555,2.47319667478674));
#66738=CARTESIAN_POINT('Ctrl Pts',(14.70484923715,2.0320784729426,2.5013679658587));
#66739=CARTESIAN_POINT('Ctrl Pts',(14.7053623126116,2.02571592961146,2.50652340838883));
#66740=CARTESIAN_POINT('Ctrl Pts',(14.7061638075118,2.01571245248916,2.5145660582924));
#66741=CARTESIAN_POINT('Ctrl Pts',(14.706453394149,2.0120848621521,2.51746969411458));
#66742=CARTESIAN_POINT('Ctrl Pts',(14.7069925199739,2.00530632102573,2.52287143746179));
#66743=CARTESIAN_POINT('Ctrl Pts',(14.7072421950402,2.00215700757154,2.52537146740743));
#66744=CARTESIAN_POINT('Ctrl Pts',(14.707805957418,1.99502314413299,2.53101283297701));
#66745=CARTESIAN_POINT('Ctrl Pts',(14.708119791282,1.99103586090291,2.53415064819724));
#66746=CARTESIAN_POINT('Ctrl Pts',(14.709042759419,1.97926286280839,2.54337053735513));
#66747=CARTESIAN_POINT('Ctrl Pts',(14.7096500447466,1.97145648566775,2.54942630829948));
#66748=CARTESIAN_POINT('Ctrl Pts',(14.7137736555209,1.91805009855655,2.59046414027467));
#66749=CARTESIAN_POINT('Ctrl Pts',(14.7172107414847,1.87154598619488,2.6242593674698));
#66750=CARTESIAN_POINT('Ctrl Pts',(14.7207375929196,1.82208491536441,2.65821941469869));
#66751=CARTESIAN_POINT('Ctrl Pts',(14.7208854110345,1.82000863697762,2.65964141509207));
#66752=CARTESIAN_POINT('Ctrl Pts',(14.7217058337026,1.80846691779303,2.66752625712666));
#66753=CARTESIAN_POINT('Ctrl Pts',(14.7223762419931,1.7989686232505,2.67394106579032));
#66754=CARTESIAN_POINT('Ctrl Pts',(14.7230445264018,1.78943621037797,2.68030513402637));
#66755=CARTESIAN_POINT('Origin',(-1.72497344927317,0.,0.));
#66756=CARTESIAN_POINT('',(16.2168686787502,1.78943621037802,2.68030513402634));
#66757=CARTESIAN_POINT('',(15.9683010644095,1.78943598014216,2.68030528773733));
#66758=CARTESIAN_POINT('',(-1.72497344927317,1.78943621037804,2.68030513402633));
#66759=CARTESIAN_POINT('',(15.3965734493107,-3.22274990038605,-0.000801287517437093));
#66760=CARTESIAN_POINT('Ctrl Pts',(15.3965734493107,-3.22274990038605,-0.000801287517414983));
#66761=CARTESIAN_POINT('Ctrl Pts',(15.403151483107,-3.22272326425235,-0.107930870065952));
#66762=CARTESIAN_POINT('Ctrl Pts',(15.4097295169033,-3.21735064918231,-0.214916416866613));
#66763=CARTESIAN_POINT('Ctrl Pts',(15.4163075506996,-3.2067002897671,-0.321233270549037));
#66764=CARTESIAN_POINT('Ctrl Pts',(15.4229099905891,-3.19601041494748,-0.427944585423264));
#66765=CARTESIAN_POINT('Ctrl Pts',(15.4295124304787,-3.18000365239334,-0.533981909528027));
#66766=CARTESIAN_POINT('Ctrl Pts',(15.4361148703683,-3.15879978879431,-0.638828190371247));
#66767=CARTESIAN_POINT('Ctrl Pts',(15.4427299993246,-3.13755517401168,-0.743875972701292));
#66768=CARTESIAN_POINT('Ctrl Pts',(15.449345128281,-3.11109360027254,-0.847727819155364));
#66769=CARTESIAN_POINT('Ctrl Pts',(15.4559602572373,-3.07958468072366,-0.949881969905816));
#66770=CARTESIAN_POINT('Ctrl Pts',(15.4625955718556,-3.04797961363123,-1.05234783780807));
#66771=CARTESIAN_POINT('Ctrl Pts',(15.4692308864739,-3.01129650796592,-1.15310533350681));
#66772=CARTESIAN_POINT('Ctrl Pts',(15.4758662010922,-2.96975371305879,-1.25167106153076));
#66773=CARTESIAN_POINT('Ctrl Pts',(15.4795684054817,-2.94657471906928,-1.30666626400921));
#66774=CARTESIAN_POINT('Ctrl Pts',(15.4832706098711,-2.92188366837227,-1.36097957634467));
#66775=CARTESIAN_POINT('Ctrl Pts',(15.4869728142606,-2.8957245434024,-1.41453063990744));
#66776=CARTESIAN_POINT('Ctrl Pts',(15.4931450623534,-2.85211252412471,-1.50381000300276));
#66777=CARTESIAN_POINT('Ctrl Pts',(15.4993173104461,-2.8042909571443,-1.59122768554707));
#66778=CARTESIAN_POINT('Ctrl Pts',(15.5054895585389,-2.75244187987435,-1.67635952600084));
#66779=CARTESIAN_POINT('Ctrl Pts',(15.5116534471915,-2.70066302487203,-1.76137606737506));
#66780=CARTESIAN_POINT('Ctrl Pts',(15.5178173358442,-2.64486772534409,-1.84411255228448));
#66781=CARTESIAN_POINT('Ctrl Pts',(15.5239812244968,-2.58528501290985,-1.9241670833178));
#66782=CARTESIAN_POINT('Ctrl Pts',(15.5301385861553,-2.52576539311624,-2.00413684392777));
#66783=CARTESIAN_POINT('Ctrl Pts',(15.5362959478139,-2.46246659163317,-2.08142995020427));
#66784=CARTESIAN_POINT('Ctrl Pts',(15.5424533094724,-2.39566174482634,-2.15567213807565));
#66785=CARTESIAN_POINT('Ctrl Pts',(15.5486061736187,-2.32890569418134,-2.22986009733957));
#66786=CARTESIAN_POINT('Ctrl Pts',(15.554759037765,-2.25864897942454,-2.30100124686958));
#66787=CARTESIAN_POINT('Ctrl Pts',(15.5609119019113,-2.18520536389433,-2.36875390872658));
#66788=CARTESIAN_POINT('Ctrl Pts',(15.5670624350479,-2.11178957244427,-2.43648090251863));
#66789=CARTESIAN_POINT('Ctrl Pts',(15.5732129681844,-2.03518959814623,-2.50082166519245));
#66790=CARTESIAN_POINT('Ctrl Pts',(15.5793635013209,-1.95575582067506,-2.56147159507882));
#66791=CARTESIAN_POINT('Ctrl Pts',(15.5855133495362,-1.87633088892305,-2.62211477100907));
#66792=CARTESIAN_POINT('Ctrl Pts',(15.5916631977514,-1.79407312664577,-2.67906766769473));
#66793=CARTESIAN_POINT('Ctrl Pts',(15.5978130459666,-1.70936492653555,-2.73206682027181));
#66794=CARTESIAN_POINT('Ctrl Pts',(15.6039638543457,-1.62464350109758,-2.78507424750427));
#66795=CARTESIAN_POINT('Ctrl Pts',(15.6101146627248,-1.53747124619339,-2.8341264741131));
#66796=CARTESIAN_POINT('Ctrl Pts',(15.616265471104,-1.44825750699312,-2.87900464673784));
#66797=CARTESIAN_POINT('Ctrl Pts',(15.6224228574701,-1.3589483580865,-2.92393081436099));
#66798=CARTESIAN_POINT('Ctrl Pts',(15.6285802438363,-1.26759375392542,-2.96467381837952));
#66799=CARTESIAN_POINT('Ctrl Pts',(15.6347376302025,-1.17462539029952,-3.00106193787528));
#66800=CARTESIAN_POINT('Ctrl Pts',(15.6408984529395,-1.08160514203481,-3.03747036518719));
#66801=CARTESIAN_POINT('Ctrl Pts',(15.6470592756764,-0.986969752166327,
-3.06951892850637));
#66802=CARTESIAN_POINT('Ctrl Pts',(15.6532200984134,-0.891166540265468,
-3.09708568819322));
#66803=CARTESIAN_POINT('Ctrl Pts',(15.6593912213301,-0.795203156526662,
-3.12469853629901));
#66804=CARTESIAN_POINT('Ctrl Pts',(15.6655623442468,-0.698068473542096,
-3.14781451301599));
#66805=CARTESIAN_POINT('Ctrl Pts',(15.6717334671635,-0.600220611140134,
-3.16636270513385));
#66806=CARTESIAN_POINT('Ctrl Pts',(15.676428989109,-0.525769528016257,-3.18047576758883));
#66807=CARTESIAN_POINT('Ctrl Pts',(15.6811245110546,-0.450905774207009,
-3.19194537925502));
#66808=CARTESIAN_POINT('Ctrl Pts',(15.6858200330002,-0.375832126923022,
-3.20076049945517));
#66809=CARTESIAN_POINT('Ctrl Pts',(15.691992281093,-0.277148065463111,-3.21234794585055));
#66810=CARTESIAN_POINT('Ctrl Pts',(15.6981645291858,-0.177753920732704,
-3.21938765345787));
#66811=CARTESIAN_POINT('Ctrl Pts',(15.7043367772785,-0.0781049306931113,
-3.22180340528429));
#66812=CARTESIAN_POINT('Ctrl Pts',(15.7105006659312,0.0214090988338605,
-3.22421588531533));
#66813=CARTESIAN_POINT('Ctrl Pts',(15.7166645545838,0.121176857218107,-3.2220168465318));
#66814=CARTESIAN_POINT('Ctrl Pts',(15.7228284432364,0.220736425033003,-3.21518164232811));
#66815=CARTESIAN_POINT('Ctrl Pts',(15.728985804895,0.320190568375327,-3.20835367598024));
#66816=CARTESIAN_POINT('Ctrl Pts',(15.7351431665535,0.419436528467584,-3.19689933390213));
#66817=CARTESIAN_POINT('Ctrl Pts',(15.7413005282121,0.518011783406816,-3.18084601242369));
#66818=CARTESIAN_POINT('Ctrl Pts',(15.7474533923584,0.616515036173647,-3.16480441674826));
#66819=CARTESIAN_POINT('Ctrl Pts',(15.7536062565047,0.7143481303619,-3.14417058999656));
#66820=CARTESIAN_POINT('Ctrl Pts',(15.759759120651,0.811053988393693,-3.11902372392559));
#66821=CARTESIAN_POINT('Ctrl Pts',(15.7659096537875,0.907723209455384,-3.09388638473334));
#66822=CARTESIAN_POINT('Ctrl Pts',(15.7720601869241,1.0032656229845,-3.0642395127072));
#66823=CARTESIAN_POINT('Ctrl Pts',(15.7782107200606,1.09723554146382,-3.03021314911156));
#66824=CARTESIAN_POINT('Ctrl Pts',(15.7843605682758,1.1911949954842,-2.99619057468048));
#66825=CARTESIAN_POINT('Ctrl Pts',(15.790510416491,1.28358189417931,-2.95778962618623));
#66826=CARTESIAN_POINT('Ctrl Pts',(15.7966602647062,1.37396784491287,-2.91518951762068));
#66827=CARTESIAN_POINT('Ctrl Pts',(15.8028110730854,1.46436790743041,-2.87258275798243));
#66828=CARTESIAN_POINT('Ctrl Pts',(15.8089618814645,1.55276600851309,-2.82577572127488));
#66829=CARTESIAN_POINT('Ctrl Pts',(15.8151126898436,1.63875670963832,-2.77499441605121));
#66830=CARTESIAN_POINT('Ctrl Pts',(15.8212700762098,1.72483937358922,-2.72415880271912));
#66831=CARTESIAN_POINT('Ctrl Pts',(15.827427462576,1.80850912162653,-2.66934065480024));
#66832=CARTESIAN_POINT('Ctrl Pts',(15.8335848489422,1.8893880782495,-2.61081026738227));
#66833=CARTESIAN_POINT('Ctrl Pts',(15.8397456716792,1.97031217254386,-2.55224721478779));
#66834=CARTESIAN_POINT('Ctrl Pts',(15.8459064944161,2.04844203398604,-2.48996806757623));
#66835=CARTESIAN_POINT('Ctrl Pts',(15.8520673171531,2.12343321559177,-2.42428318094681));
#66836=CARTESIAN_POINT('Ctrl Pts',(15.8582384400698,2.19854977373921,-2.3584884768195));
#66837=CARTESIAN_POINT('Ctrl Pts',(15.8644095629864,2.27051685708402,-2.28927696092124));
#66838=CARTESIAN_POINT('Ctrl Pts',(15.8705806859031,2.33902710271958,-2.21699566423646));
#66839=CARTESIAN_POINT('Ctrl Pts',(15.8752762078487,2.39115559962716,-2.16199782682172));
#66840=CARTESIAN_POINT('Ctrl Pts',(15.8799717297943,2.44128353743214,-2.10522350623952));
#66841=CARTESIAN_POINT('Ctrl Pts',(15.8846672517399,2.48929198490435,-2.04683731067981));
#66842=CARTESIAN_POINT('Ctrl Pts',(15.8908394998326,2.55239893058178,-1.97008884940888));
#66843=CARTESIAN_POINT('Ctrl Pts',(15.8970117479254,2.61206422714657,-1.8902840508331));
#66844=CARTESIAN_POINT('Ctrl Pts',(15.9031839960182,2.667977608358,-1.80776465387515));
#66845=CARTESIAN_POINT('Ctrl Pts',(15.9093478846708,2.72381526277492,-1.72535701781023));
#66846=CARTESIAN_POINT('Ctrl Pts',(15.9155117733234,2.77591086024843,-1.64024244732748));
#66847=CARTESIAN_POINT('Ctrl Pts',(15.9216756619761,2.82399390327054,-1.55279618649417));
#66848=CARTESIAN_POINT('Ctrl Pts',(15.9278330236346,2.8720260307497,-1.46544252324972));
#66849=CARTESIAN_POINT('Ctrl Pts',(15.9339903852932,2.91605384290952,-1.37576245688326));
#66850=CARTESIAN_POINT('Ctrl Pts',(15.9401477469517,2.95585029545812,-1.28415987841863));
#66851=CARTESIAN_POINT('Ctrl Pts',(15.946300611098,2.99561767954489,-1.19262420908497));
#66852=CARTESIAN_POINT('Ctrl Pts',(15.9524534752443,3.03115967630921,-1.09916921675777));
#66853=CARTESIAN_POINT('Ctrl Pts',(15.9586063393906,3.06229575603652,-1.00422221896386));
#66854=CARTESIAN_POINT('Ctrl Pts',(15.9647568725272,3.09342003987426,-0.90931119179668));
#66855=CARTESIAN_POINT('Ctrl Pts',(15.9709074056637,3.12014158812306,-0.812909694593116));
#66856=CARTESIAN_POINT('Ctrl Pts',(15.9770579388002,3.1423288048497,-0.715462958308727));
#66857=CARTESIAN_POINT('Ctrl Pts',(15.9832077870154,3.16451355081524,-0.61802707366056));
#66858=CARTESIAN_POINT('Ctrl Pts',(15.9893576352306,3.18216487272335,-0.519546604882973));
#66859=CARTESIAN_POINT('Ctrl Pts',(15.9955074834458,3.19520189069667,-0.42047882252074));
#66860=CARTESIAN_POINT('Ctrl Pts',(16.001658291825,3.20824094411444,-0.321395572896909));
#66861=CARTESIAN_POINT('Ctrl Pts',(16.0078091002041,3.21666420597336,-0.221725258258982));
#66862=CARTESIAN_POINT('Ctrl Pts',(16.0139599085833,3.2204425719225,-0.121931142245125));
#66863=CARTESIAN_POINT('Ctrl Pts',(16.0201172949494,3.22422497864819,-0.0220303013322788));
#66864=CARTESIAN_POINT('Ctrl Pts',(16.0262746813156,3.22335255343781,0.0779941704340612));
#66865=CARTESIAN_POINT('Ctrl Pts',(16.0324320676818,3.21784834977617,0.177678249492705));
#66866=CARTESIAN_POINT('Ctrl Pts',(16.0385928904188,3.21234107427797,0.277417961158298));
#66867=CARTESIAN_POINT('Ctrl Pts',(16.0447537131557,3.2021969165482,0.376816469649774));
#66868=CARTESIAN_POINT('Ctrl Pts',(16.0509145358927,3.18749070413578,0.475416210859515));
#66869=CARTESIAN_POINT('Ctrl Pts',(16.0570856588094,3.17275990464505,0.574180799379308));
#66870=CARTESIAN_POINT('Ctrl Pts',(16.0632567817261,3.15345189936077,0.67214352673028));
#66871=CARTESIAN_POINT('Ctrl Pts',(16.0694279046428,3.12969241956978,0.768858193288883));
#66872=CARTESIAN_POINT('Ctrl Pts',(16.0741234265884,3.11161416051055,0.842447043392282));
#66873=CARTESIAN_POINT('Ctrl Pts',(16.0788189485339,3.09095978518413,0.915313567983737));
#66874=CARTESIAN_POINT('Ctrl Pts',(16.0835144704795,3.06780345613332,0.987268715718499));
#66875=CARTESIAN_POINT('Ctrl Pts',(16.089685502756,3.03737053395065,1.08183488839853));
#66876=CARTESIAN_POINT('Ctrl Pts',(16.0958565350325,3.00250740618948,1.17515899787367));
#66877=CARTESIAN_POINT('Ctrl Pts',(16.1020275673089,2.96333370680217,1.26679552597493));
#66878=CARTESIAN_POINT('Ctrl Pts',(16.1081908020022,2.92420950645555,1.35831626413793));
#66879=CARTESIAN_POINT('Ctrl Pts',(16.1143540366956,2.8807857250492,1.4481532619653));
#66880=CARTESIAN_POINT('Ctrl Pts',(16.1205172713889,2.83323169421114,1.53587620901473));
#66881=CARTESIAN_POINT('Ctrl Pts',(16.1266743676933,2.78572502570034,1.62351178675282));
#66882=CARTESIAN_POINT('Ctrl Pts',(16.1328314639976,2.73409648872252,1.70903711853518));
#66883=CARTESIAN_POINT('Ctrl Pts',(16.138988560302,2.67856303153204,1.7920428701931));
#66884=CARTESIAN_POINT('Ctrl Pts',(16.145141171698,2.62307002562788,1.87498815939114));
#66885=CARTESIAN_POINT('Ctrl Pts',(16.151293783094,2.56367799531519,1.95541715741891));
#66886=CARTESIAN_POINT('Ctrl Pts',(16.15744639449,2.50064874131153,2.03294698284954));
#66887=CARTESIAN_POINT('Ctrl Pts',(16.1635967978572,2.43764210703775,2.11044898463326));
#66888=CARTESIAN_POINT('Ctrl Pts',(16.1697472012245,2.37100111535886,2.18505354373481));
#66889=CARTESIAN_POINT('Ctrl Pts',(16.1758976045917,2.30102910816362,2.25640922837231));
#66890=CARTESIAN_POINT('Ctrl Pts',(16.182046812984,2.23107069597825,2.32775104916232));
#66891=CARTESIAN_POINT('Ctrl Pts',(16.1881960213763,2.15778286269837,2.39584494405235));
#66892=CARTESIAN_POINT('Ctrl Pts',(16.1943452297685,2.08150641312365,2.46037570598986));
#66893=CARTESIAN_POINT('Ctrl Pts',(16.200496116594,2.00520914380899,2.5249240816691));
#66894=CARTESIAN_POINT('Ctrl Pts',(16.2066470034194,1.9259219639394,2.58590710539825));
#66895=CARTESIAN_POINT('Ctrl Pts',(16.2127978902448,1.84401883694316,2.64304977090837));
#66896=CARTESIAN_POINT('Ctrl Pts',(16.2141548197466,1.82595042299473,2.65565585046137));
#66897=CARTESIAN_POINT('Ctrl Pts',(16.2155117492484,1.80775481277862,2.66807519421725));
#66898=CARTESIAN_POINT('Ctrl Pts',(16.2168686787502,1.78943621037802,2.68030513402634));
#66899=CARTESIAN_POINT('Ctrl Pts',(14.9670297268737,1.78943621037805,2.68030513402632));
#66900=CARTESIAN_POINT('Ctrl Pts',(14.9731800598208,1.70635700013351,2.73577081412889));
#66901=CARTESIAN_POINT('Ctrl Pts',(14.9793303927678,1.62066352453859,2.7873922156097));
#66902=CARTESIAN_POINT('Ctrl Pts',(14.9854807257148,1.53275005607261,2.83492413092651));
#66903=CARTESIAN_POINT('Ctrl Pts',(14.9916306108541,1.44484298861588,2.88245258542855));
#66904=CARTESIAN_POINT('Ctrl Pts',(14.9977804959933,1.35471663189435,2.92589193935345));
#66905=CARTESIAN_POINT('Ctrl Pts',(15.0039303811325,1.26279030761724,2.9650426980885));
#66906=CARTESIAN_POINT('Ctrl Pts',(15.0100814635135,1.17084608739051,3.00420107857948));
#66907=CARTESIAN_POINT('Ctrl Pts',(15.0162325458945,1.07710160317344,3.03906903518434));
#66908=CARTESIAN_POINT('Ctrl Pts',(15.0223836282755,0.981995675153088,3.0694954074702));
#66909=CARTESIAN_POINT('Ctrl Pts',(15.0285414183548,0.886786034999967,3.09995495943294));
#66910=CARTESIAN_POINT('Ctrl Pts',(15.034699208434,0.790212401369721,3.12596312440363));
#66911=CARTESIAN_POINT('Ctrl Pts',(15.0408569985133,0.692728123241261,3.14741883291224));
#66912=CARTESIAN_POINT('Ctrl Pts',(15.0470184380535,0.595186070318326,3.16888725730871));
#66913=CARTESIAN_POINT('Ctrl Pts',(15.0531798775936,0.496732726148102,3.18579777944097));
#66914=CARTESIAN_POINT('Ctrl Pts',(15.0593413171338,0.397828923788017,3.19810095367511));
#66915=CARTESIAN_POINT('Ctrl Pts',(15.0655127909436,0.298764050719617,3.21042416435822));
#66916=CARTESIAN_POINT('Ctrl Pts',(15.0716842647535,0.199247687356821,3.21812501017596));
#66917=CARTESIAN_POINT('Ctrl Pts',(15.0778557385634,0.0997430830037804,
3.22120612191969));
#66918=CARTESIAN_POINT('Ctrl Pts',(15.081663284636,0.0383528256379945,3.22310704142136));
#66919=CARTESIAN_POINT('Ctrl Pts',(15.0854708307087,-0.0230329793170104,
3.22325054454222));
#66920=CARTESIAN_POINT('Ctrl Pts',(15.0892783767813,-0.0843066070415162,
3.22164708782777));
#66921=CARTESIAN_POINT('Ctrl Pts',(15.0954506248741,-0.183634632138016,
3.21904779356874));
#66922=CARTESIAN_POINT('Ctrl Pts',(15.1016228729669,-0.283017162718341,
3.21184598092432));
#66923=CARTESIAN_POINT('Ctrl Pts',(15.1077951210596,-0.381992745054684,
3.20003111004027));
#66924=CARTESIAN_POINT('Ctrl Pts',(15.1139590097123,-0.480834278914442,
3.18823224073365));
#66925=CARTESIAN_POINT('Ctrl Pts',(15.120122898365,-0.579269532494049,3.17183278228601));
#66926=CARTESIAN_POINT('Ctrl Pts',(15.1262867870176,-0.67683779071223,3.15087419100855));
#66927=CARTESIAN_POINT('Ctrl Pts',(15.1324441486762,-0.774302733072408,
3.12993779296156));
#66928=CARTESIAN_POINT('Ctrl Pts',(15.1386015103347,-0.870902082932757,
3.10445195074111));
#66929=CARTESIAN_POINT('Ctrl Pts',(15.1447588719933,-0.966181948124195,
3.0745097179256));
#66930=CARTESIAN_POINT('Ctrl Pts',(15.1509117361396,-1.0613922181895,3.04458935576939));
#66931=CARTESIAN_POINT('Ctrl Pts',(15.1570646002859,-1.15528450661803,3.01021920449644));
#66932=CARTESIAN_POINT('Ctrl Pts',(15.1632174644322,-1.24741769390861,2.97154280794064));
#66933=CARTESIAN_POINT('Ctrl Pts',(15.1693679975688,-1.33951597658323,2.93288106392001));
#66934=CARTESIAN_POINT('Ctrl Pts',(15.1755185307053,-1.42985608225006,2.88991648418273));
#66935=CARTESIAN_POINT('Ctrl Pts',(15.1816690638418,-1.51801541423247,2.8428413189365));
#66936=CARTESIAN_POINT('Ctrl Pts',(15.1878189120571,-1.60616492882119,2.79577139596491));
#66937=CARTESIAN_POINT('Ctrl Pts',(15.1939687602723,-1.69213376937722,2.74459200216956));
#66938=CARTESIAN_POINT('Ctrl Pts',(15.2001186084875,-1.77552346751651,2.6895415926879));
#66939=CARTESIAN_POINT('Ctrl Pts',(15.2062694168666,-1.85892618512797,2.63448258829235));
#66940=CARTESIAN_POINT('Ctrl Pts',(15.2124202252458,-1.93974859796171,2.57555160710201));
#66941=CARTESIAN_POINT('Ctrl Pts',(15.2185710336249,-2.01762162832546,2.51303014852853));
#66942=CARTESIAN_POINT('Ctrl Pts',(15.2247284199911,-2.09557794006541,2.45044182632989));
#66943=CARTESIAN_POINT('Ctrl Pts',(15.2308858063573,-2.17057823130809,2.38425563145967));
#66944=CARTESIAN_POINT('Ctrl Pts',(15.2370431927234,-2.2422870193426,2.31479296814806));
#66945=CARTESIAN_POINT('Ctrl Pts',(15.2432040154604,-2.31403582727659,2.24529153847488));
#66946=CARTESIAN_POINT('Ctrl Pts',(15.2493648381974,-2.3824891761296,2.17251031522878));
#66947=CARTESIAN_POINT('Ctrl Pts',(15.2555256609343,-2.44735038123923,2.09680558801912));
#66948=CARTESIAN_POINT('Ctrl Pts',(15.261696783851,-2.51232002674694,2.02097429130244));
#66949=CARTESIAN_POINT('Ctrl Pts',(15.2678679067677,-2.57368526532954,1.94221007028928));
#66950=CARTESIAN_POINT('Ctrl Pts',(15.2740390296844,-2.63119134612786,1.86090022907244));
#66951=CARTESIAN_POINT('Ctrl Pts',(15.2787345516299,-2.6749469264387,1.7990326971865));
#66952=CARTESIAN_POINT('Ctrl Pts',(15.2834300735755,-2.71646912576312,1.73569202629276));
#66953=CARTESIAN_POINT('Ctrl Pts',(15.288125595521,-2.75566369413806,1.67105809812507));
#66954=CARTESIAN_POINT('Ctrl Pts',(15.2944981381896,-2.80885672831925,1.58333995520794));
#66955=CARTESIAN_POINT('Ctrl Pts',(15.3008706808582,-2.85793822589388,1.492946968511));
#66956=CARTESIAN_POINT('Ctrl Pts',(15.3072432235268,-2.90263902050083,1.40028721309809));
#66957=CARTESIAN_POINT('Ctrl Pts',(15.3136052317173,-2.94726592002897,1.30778063393155));
#66958=CARTESIAN_POINT('Ctrl Pts',(15.3199672399077,-2.98752635647166,1.21301509644927));
#66959=CARTESIAN_POINT('Ctrl Pts',(15.3263292480982,-3.02319551557037,1.1164257418813));
#66960=CARTESIAN_POINT('Ctrl Pts',(15.3326790949963,-3.05879649131245,1.02002102262786));
#66961=CARTESIAN_POINT('Ctrl Pts',(15.3390289418944,-3.08982353762513,0.921799800806557));
#66962=CARTESIAN_POINT('Ctrl Pts',(15.3453787887925,-3.11609915948835,0.822218700064662));
#66963=CARTESIAN_POINT('Ctrl Pts',(15.3517214721691,-3.14234513875027,0.722749940826297));
#66964=CARTESIAN_POINT('Ctrl Pts',(15.3580641555458,-3.16385025754267,0.621924735618091));
#66965=CARTESIAN_POINT('Ctrl Pts',(15.3644068389225,-3.18048614095612,0.52021675260036));
#66966=CARTESIAN_POINT('Ctrl Pts',(15.370741969782,-3.19710221527828,0.418629877832159));
#66967=CARTESIAN_POINT('Ctrl Pts',(15.3770771006416,-3.20886053925029,0.316162708355363));
#66968=CARTESIAN_POINT('Ctrl Pts',(15.3834122315011,-3.21568353572234,0.213300165457598));
#66969=CARTESIAN_POINT('Ctrl Pts',(15.3877993040918,-3.22040845482382,0.142067944284031));
#66970=CARTESIAN_POINT('Ctrl Pts',(15.3921863766824,-3.22276766474656,0.0706463933296931));
#66971=CARTESIAN_POINT('Ctrl Pts',(15.3965734492731,-3.22274990038621,-0.000801286904994983));
#66972=CARTESIAN_POINT('Ctrl Pts',(14.7230445264018,1.78943621037797,2.68030513402637));
#66973=CARTESIAN_POINT('Ctrl Pts',(14.7231109020367,1.78848942791742,2.68093722878183));
#66974=CARTESIAN_POINT('Ctrl Pts',(14.7231772567185,1.78754230888135,2.68156882298579));
#66975=CARTESIAN_POINT('Ctrl Pts',(14.740998021613,1.53300616988584,2.8511135885443));
#66976=CARTESIAN_POINT('Ctrl Pts',(14.7573121250989,1.25673265540303,2.9832222007102));
#66977=CARTESIAN_POINT('Ctrl Pts',(14.7791757212824,0.894772783146178,3.09694562165537));
#66978=CARTESIAN_POINT('Ctrl Pts',(14.7835362633534,0.822801268485764,3.1168393313995));
#66979=CARTESIAN_POINT('Ctrl Pts',(14.7906551569377,0.706355328689767,3.14471189485576));
#66980=CARTESIAN_POINT('Ctrl Pts',(14.7933633196308,0.66228946747602,3.15428646533951));
#66981=CARTESIAN_POINT('Ctrl Pts',(14.7968875296238,0.605329505237608,3.16541647293248));
#66982=CARTESIAN_POINT('Ctrl Pts',(14.7976762864409,0.592605465375178,3.16782322924968));
#66983=CARTESIAN_POINT('Ctrl Pts',(14.7989536830623,0.572039874526359,3.17158497674564));
#66984=CARTESIAN_POINT('Ctrl Pts',(14.7994407959081,0.564207120008644,3.17298774134116));
#66985=CARTESIAN_POINT('Ctrl Pts',(14.8003724948821,0.549244199334205,3.17561028759485));
#66986=CARTESIAN_POINT('Ctrl Pts',(14.8008169175567,0.542114955278675,3.17683510165145));
#66987=CARTESIAN_POINT('Ctrl Pts',(14.8018355708504,0.525793088696647,3.17958267912424));
#66988=CARTESIAN_POINT('Ctrl Pts',(14.8024103020343,0.516597896706989,3.18108959253035));
#66989=CARTESIAN_POINT('Ctrl Pts',(14.8041834979483,0.488271595204182,3.18560566704075));
#66990=CARTESIAN_POINT('Ctrl Pts',(14.8053861584324,0.469120065326275,3.18848223368005));
#66991=CARTESIAN_POINT('Ctrl Pts',(14.8159960790056,0.300718782544522,3.21222612231473));
#66992=CARTESIAN_POINT('Ctrl Pts',(14.8257310844947,0.150223831730027,3.22277047595897));
#66993=CARTESIAN_POINT('Ctrl Pts',(14.8512025107649,-0.234086092629859,
3.22271816971552));
#66994=CARTESIAN_POINT('Ctrl Pts',(14.867254889849,-0.467015383726354,3.19727902450478));
#66995=CARTESIAN_POINT('Ctrl Pts',(14.8874126177165,-0.762645635207184,
3.13197524460535));
#66996=CARTESIAN_POINT('Ctrl Pts',(14.8919617223615,-0.829661344020823,
3.11489336394149));
#66997=CARTESIAN_POINT('Ctrl Pts',(14.8987058986138,-0.930197392890896,
3.08579194146998));
#66998=CARTESIAN_POINT('Ctrl Pts',(14.9009693826722,-0.964151033816046,
3.07535235914933));
#66999=CARTESIAN_POINT('Ctrl Pts',(14.9037129064292,-1.00565666227512,3.06183577739324));
#67000=CARTESIAN_POINT('Ctrl Pts',(14.9042222226442,-1.01337707916199,3.05928922282954));
#67001=CARTESIAN_POINT('Ctrl Pts',(14.9050191520123,-1.02548255968639,3.05524541578073));
#67002=CARTESIAN_POINT('Ctrl Pts',(14.9053079108635,-1.02987410570936,3.05376789522469));
#67003=CARTESIAN_POINT('Ctrl Pts',(14.9058463012314,-1.03807228041073,3.05098995151447));
#67004=CARTESIAN_POINT('Ctrl Pts',(14.9060960650402,-1.04187962023797,3.04969188620403));
#67005=CARTESIAN_POINT('Ctrl Pts',(14.9066610642988,-1.05050158088802,3.04673430492583));
#67006=CARTESIAN_POINT('Ctrl Pts',(14.9069760416528,-1.05531469179807,3.04507050794947));
#67007=CARTESIAN_POINT('Ctrl Pts',(14.9079054737319,-1.06953562417976,3.04011684648877));
#67008=CARTESIAN_POINT('Ctrl Pts',(14.9085180405688,-1.07893225633188,3.0367947056147));
#67009=CARTESIAN_POINT('Ctrl Pts',(14.9127492429446,-1.14398953195297,3.01345388902557));
#67010=CARTESIAN_POINT('Ctrl Pts',(14.9162838824298,-1.19910931367296,2.99194824296677));
#67011=CARTESIAN_POINT('Ctrl Pts',(14.9207680918513,-1.26946239458452,2.96224220838299));
#67012=CARTESIAN_POINT('Ctrl Pts',(14.9217732865504,-1.28526140170285,2.95542159792267));
#67013=CARTESIAN_POINT('Ctrl Pts',(14.9309017188953,-1.42889426110301,2.8920440450787));
#67014=CARTESIAN_POINT('Ctrl Pts',(14.9387201600622,-1.55298555893522,2.82734838787098));
#67015=CARTESIAN_POINT('Ctrl Pts',(14.9554249674204,-1.80847568802037,2.67223525482221));
#67016=CARTESIAN_POINT('Ctrl Pts',(14.9642923982549,-1.93815656787172,2.57972304022086));
#67017=CARTESIAN_POINT('Ctrl Pts',(14.9778115373712,-2.11864765716188,2.42964490453971));
#67018=CARTESIAN_POINT('Ctrl Pts',(14.9822289224596,-2.17509998416226,2.37923960578189));
#67019=CARTESIAN_POINT('Ctrl Pts',(14.989432666156,-2.26260332415189,2.29539048986673));
#67020=CARTESIAN_POINT('Ctrl Pts',(14.9921672826353,-2.29481018978089,2.26319181233338));
#67021=CARTESIAN_POINT('Ctrl Pts',(14.9957212625431,-2.33531615542333,2.22094234234419));
#67022=CARTESIAN_POINT('Ctrl Pts',(14.9965127568558,-2.34425253016377,2.2115077437988));
#67023=CARTESIAN_POINT('Ctrl Pts',(14.9977935154294,-2.35857548584112,2.19620188536729));
#67024=CARTESIAN_POINT('Ctrl Pts',(14.998281237909,-2.36399784137874,2.19036418155847));
#67025=CARTESIAN_POINT('Ctrl Pts',(14.9992133899913,-2.37430007600982,2.17918998768938));
#67026=CARTESIAN_POINT('Ctrl Pts',(14.9996576532661,-2.37918375708191,2.17385705649335));
#67027=CARTESIAN_POINT('Ctrl Pts',(15.0006749352364,-2.39030605223147,2.16162924635957));
#67028=CARTESIAN_POINT('Ctrl Pts',(15.001248449718,-2.39653283605589,2.15472373747882));
#67029=CARTESIAN_POINT('Ctrl Pts',(15.0030142337181,-2.41556982077244,2.13342710418028));
#67030=CARTESIAN_POINT('Ctrl Pts',(15.004210648287,-2.42828074395567,2.11894817549581));
#67031=CARTESIAN_POINT('Ctrl Pts',(15.0212721603102,-2.60686763581553,1.91180372236777));
#67032=CARTESIAN_POINT('Ctrl Pts',(15.0381290141231,-2.74947143401784,1.70032551873446));
#67033=CARTESIAN_POINT('Ctrl Pts',(15.0653273647175,-2.93348460514272,1.34265383993753));
#67034=CARTESIAN_POINT('Ctrl Pts',(15.0753954484817,-2.99208155291536,1.20644206339538));
#67035=CARTESIAN_POINT('Ctrl Pts',(15.088938678542,-3.05985094226806,1.0132313997135));
#67036=CARTESIAN_POINT('Ctrl Pts',(15.0926420034621,-3.07718681979923,0.959295432964452));
#67037=CARTESIAN_POINT('Ctrl Pts',(15.0982656059838,-3.10177403119091,0.875254955112782));
#67038=CARTESIAN_POINT('Ctrl Pts',(15.1002314095604,-3.1100280791091,0.845457801342096));
#67039=CARTESIAN_POINT('Ctrl Pts',(15.1026617548289,-3.11981850414629,0.808028728741279));
#67040=CARTESIAN_POINT('Ctrl Pts',(15.1031483212269,-3.12175744311823,0.800505087169984));
#67041=CARTESIAN_POINT('Ctrl Pts',(15.1039175880348,-3.12478959995272,0.788560874766613));
#67042=CARTESIAN_POINT('Ctrl Pts',(15.1042013076125,-3.1259006740415,0.784144931645784));
#67043=CARTESIAN_POINT('Ctrl Pts',(15.10473541078,-3.12797866879361,0.775811376743137));
#67044=CARTESIAN_POINT('Ctrl Pts',(15.1049859044795,-3.12894757979536,0.771894350149719));
#67045=CARTESIAN_POINT('Ctrl Pts',(15.1055593084457,-3.1311524458972,0.762908345985083));
#67046=CARTESIAN_POINT('Ctrl Pts',(15.1058819296038,-3.13238344779115,0.757838189019702));
#67047=CARTESIAN_POINT('Ctrl Pts',(15.1068781614429,-3.13615483938944,0.742138680627024));
#67048=CARTESIAN_POINT('Ctrl Pts',(15.1075494038975,-3.13865351086278,0.731499244486191));
#67049=CARTESIAN_POINT('Ctrl Pts',(15.1131260617385,-3.15905091643544,0.642617359995613));
#67050=CARTESIAN_POINT('Ctrl Pts',(15.1178758687404,-3.17407673875217,0.563736680675645));
#67051=CARTESIAN_POINT('Ctrl Pts',(15.1242663352804,-3.19064097886558,0.454778629523579));
#67052=CARTESIAN_POINT('Ctrl Pts',(15.1259883526809,-3.19472723681376,0.425125184903111));
#67053=CARTESIAN_POINT('Ctrl Pts',(15.1352016288248,-3.21449585385841,0.265223841976268));
#67054=CARTESIAN_POINT('Ctrl Pts',(15.1424995742806,-3.22262790300222,0.134162465310681));
#67055=CARTESIAN_POINT('Ctrl Pts',(15.1553204624045,-3.22283895868667,-0.0951862285488035));
#67056=CARTESIAN_POINT('Ctrl Pts',(15.1608197253378,-3.21844527033867,-0.193288392988242));
#67057=CARTESIAN_POINT('Ctrl Pts',(15.1698768604655,-3.20407840080513,-0.35172904129138));
#67058=CARTESIAN_POINT('Ctrl Pts',(15.1733781283162,-3.19685446179728,-0.412253244994023));
#67059=CARTESIAN_POINT('Ctrl Pts',(15.1820158470909,-3.17508980198272,-0.559087030677871));
#67060=CARTESIAN_POINT('Ctrl Pts',(15.1871969743326,-3.158741832144,-0.645074818197823));
#67061=CARTESIAN_POINT('Ctrl Pts',(15.1934149677491,-3.13545869355486,-0.745150498364081));
#67062=CARTESIAN_POINT('Ctrl Pts',(15.1943418804486,-3.13189482547814,-0.759990311719795));
#67063=CARTESIAN_POINT('Ctrl Pts',(15.1958391620589,-3.12598957568767,-0.78383240986947));
#67064=CARTESIAN_POINT('Ctrl Pts',(15.1964073931163,-3.12371436250361,-0.792850964999574));
#67065=CARTESIAN_POINT('Ctrl Pts',(15.197420962456,-3.11959561171698,-0.808884035419884));
#67066=CARTESIAN_POINT('Ctrl Pts',(15.1978658025011,-3.11776736885509,-0.815902442536883));
#67067=CARTESIAN_POINT('Ctrl Pts',(15.1987960983281,-3.11390116040694,-0.830541603241341));
#67068=CARTESIAN_POINT('Ctrl Pts',(15.1992816918438,-3.11185887609818,-0.838161156926052));
#67069=CARTESIAN_POINT('Ctrl Pts',(15.200547766653,-3.10647135981199,-0.857970296477163));
#67070=CARTESIAN_POINT('Ctrl Pts',(15.2013296676057,-3.10308237571739,-0.870147746745694));
#67071=CARTESIAN_POINT('Ctrl Pts',(15.204729019631,-3.08808269305092,-0.922843078558261));
#67072=CARTESIAN_POINT('Ctrl Pts',(15.2073699464865,-3.07574982212357,-0.96314943106514));
#67073=CARTESIAN_POINT('Ctrl Pts',(15.2143482361777,-3.04141714958041,-1.06796223163581));
#67074=CARTESIAN_POINT('Ctrl Pts',(15.2187255700755,-3.01815637667191,-1.13203029760212));
#67075=CARTESIAN_POINT('Ctrl Pts',(15.2328222448072,-2.9378529266205,-1.33309865482892));
#67076=CARTESIAN_POINT('Ctrl Pts',(15.2427558789215,-2.8733776754647,-1.46690988692199));
#67077=CARTESIAN_POINT('Ctrl Pts',(15.255315224363,-2.78135503792632,-1.62836966183403));
#67078=CARTESIAN_POINT('Ctrl Pts',(15.257853505674,-2.76222066299254,-1.66062054375748));
#67079=CARTESIAN_POINT('Ctrl Pts',(15.2738409268937,-2.63817479943112,-1.86162096321881));
#67080=CARTESIAN_POINT('Ctrl Pts',(15.2872793758239,-2.51839415295489,-2.02071989769385));
#67081=CARTESIAN_POINT('Ctrl Pts',(15.3004851134808,-2.37768012851168,-2.17551462653088));
#67082=CARTESIAN_POINT('Ctrl Pts',(15.3011419386871,-2.37061588937,-2.18321025003884));
#67083=CARTESIAN_POINT('Ctrl Pts',(15.302122791084,-2.35996619158621,-2.19469915400406));
#67084=CARTESIAN_POINT('Ctrl Pts',(15.3024488831076,-2.35640881691023,-2.198518203362));
#67085=CARTESIAN_POINT('Ctrl Pts',(15.303010798871,-2.35024944718996,-2.20509852227101));
#67086=CARTESIAN_POINT('Ctrl Pts',(15.3032469556684,-2.34765183821192,-2.20786385536685));
#67087=CARTESIAN_POINT('Ctrl Pts',(15.3037389346192,-2.34222135147988,-2.21362456174629));
#67088=CARTESIAN_POINT('Ctrl Pts',(15.3039946846047,-2.33938760754884,-2.21661908805895));
#67089=CARTESIAN_POINT('Ctrl Pts',(15.3046078462457,-2.3325680496375,-2.22379793399773));
#67090=CARTESIAN_POINT('Ctrl Pts',(15.3049648293645,-2.32857668705824,-2.22797701315815));
#67091=CARTESIAN_POINT('Ctrl Pts',(15.3061862429921,-2.31484911027079,-2.24227302157284));
#67092=CARTESIAN_POINT('Ctrl Pts',(15.3070464946323,-2.30505786383752,-2.25233722334539));
#67093=CARTESIAN_POINT('Ctrl Pts',(15.3091041753893,-2.28135148221348,-2.27638797342363));
#67094=CARTESIAN_POINT('Ctrl Pts',(15.3102969940665,-2.26737291084877,-2.29031153256187));
#67095=CARTESIAN_POINT('Ctrl Pts',(15.3147081530182,-2.21484036184344,-2.34168497068751));
#67096=CARTESIAN_POINT('Ctrl Pts',(15.3178722262048,-2.17547738976182,-2.37829878942329));
#67097=CARTESIAN_POINT('Ctrl Pts',(15.3256834473043,-2.07469185987813,-2.46744813403822));
#67098=CARTESIAN_POINT('Ctrl Pts',(15.3302731419139,-2.01217375151787,-2.51869107470802));
#67099=CARTESIAN_POINT('Ctrl Pts',(15.3458566208664,-1.79165955667816,-2.68597853535667));
#67100=CARTESIAN_POINT('Ctrl Pts',(15.3566468053936,-1.62505228326975,-2.78993353290938));
#67101=CARTESIAN_POINT('Ctrl Pts',(15.3703716835656,-1.41079657455153,-2.89787870123314));
#67102=CARTESIAN_POINT('Ctrl Pts',(15.372903387189,-1.37115997513711,-2.91684213785507));
#67103=CARTESIAN_POINT('Ctrl Pts',(15.376288466089,-1.31814348395038,-2.94088749506775));
#67104=CARTESIAN_POINT('Ctrl Pts',(15.3771212493929,-1.3050989191316,-2.94669956156003));
#67105=CARTESIAN_POINT('Ctrl Pts',(15.3824145608504,-1.22219410977495,-2.98297969580263));
#67106=CARTESIAN_POINT('Ctrl Pts',(15.386943377462,-1.151314763883,-3.01104619992293));
#67107=CARTESIAN_POINT('Ctrl Pts',(15.3924426477417,-1.06574143531627,-3.04146779143902));
#67108=CARTESIAN_POINT('Ctrl Pts',(15.3933305980832,-1.05193866599805,-3.046269220761));
#67109=CARTESIAN_POINT('Ctrl Pts',(15.3947829677527,-1.02938884784141,-3.05394186381261));
#67110=CARTESIAN_POINT('Ctrl Pts',(15.395345505136,-1.02066121084517,-3.05686980382081));
#67111=CARTESIAN_POINT('Ctrl Pts',(15.3963514560325,-1.00506633998423,-3.06202732573919));
#67112=CARTESIAN_POINT('Ctrl Pts',(15.3967943901735,-0.998203906188465,
-3.06427130842962));
#67113=CARTESIAN_POINT('Ctrl Pts',(15.3977308002374,-0.983705241246241,
-3.06895842943831));
#67114=CARTESIAN_POINT('Ctrl Pts',(15.3982244507343,-0.976067327852589,
-3.07139616671605));
#67115=CARTESIAN_POINT('Ctrl Pts',(15.3995345521572,-0.9558119294269,-3.07777774908896));
#67116=CARTESIAN_POINT('Ctrl Pts',(15.400352611083,-0.943179238304977,-3.08167247339529));
#67117=CARTESIAN_POINT('Ctrl Pts',(15.4041416232694,-0.884742878128455,
-3.09929573406158));
#67118=CARTESIAN_POINT('Ctrl Pts',(15.4071432244256,-0.838663184494064,
-3.11208092343156));
#67119=CARTESIAN_POINT('Ctrl Pts',(15.4153111159994,-0.713913224274812,
-3.14372203765289));
#67120=CARTESIAN_POINT('Ctrl Pts',(15.4205363034389,-0.634793459361312,
-3.16064800500406));
#67121=CARTESIAN_POINT('Ctrl Pts',(15.4485974163442,-0.213283363532098,
-3.23435579154359));
#67122=CARTESIAN_POINT('Ctrl Pts',(15.4729307886101,0.135909696031122,-3.23852275724333));
#67123=CARTESIAN_POINT('Ctrl Pts',(15.4967462405727,0.504058717654823,-3.18318763662073));
#67124=CARTESIAN_POINT('Ctrl Pts',(15.4983523187759,0.529054262969654,-3.17912887477608));
#67125=CARTESIAN_POINT('Ctrl Pts',(15.5004172824748,0.561446927873938,-3.17347633531926));
#67126=CARTESIAN_POINT('Ctrl Pts',(15.5008905744842,0.56888907210638,-3.17215067895932));
#67127=CARTESIAN_POINT('Ctrl Pts',(15.5016436787339,0.580760578997237,-3.16999290572147));
#67128=CARTESIAN_POINT('Ctrl Pts',(15.5019244391387,0.585192923528332,-3.16917767177688));
#67129=CARTESIAN_POINT('Ctrl Pts',(15.5024310026801,0.593202241155556,-3.16768715531785));
#67130=CARTESIAN_POINT('Ctrl Pts',(15.5026569863704,0.596779740329687,-3.1670151175114));
#67131=CARTESIAN_POINT('Ctrl Pts',(15.5031975247657,0.605347415102063,-3.16539063591076));
#67132=CARTESIAN_POINT('Ctrl Pts',(15.5035117477796,0.610336479364641,-3.16443245364495));
#67133=CARTESIAN_POINT('Ctrl Pts',(15.5044571775658,0.625372430026128,-3.16150781937738));
#67134=CARTESIAN_POINT('Ctrl Pts',(15.5050863520346,0.635412350050198,-3.15950526510695));
#67135=CARTESIAN_POINT('Ctrl Pts',(15.5110795427846,0.731346983542837,-3.13989443523806));
#67136=CARTESIAN_POINT('Ctrl Pts',(15.5162558297956,0.816507745941176,-3.11883370608293));
#67137=CARTESIAN_POINT('Ctrl Pts',(15.5304697659594,1.05263149988107,-3.05010159669894));
#67138=CARTESIAN_POINT('Ctrl Pts',(15.5392525652299,1.20109819810997,-2.99474911639553));
#67139=CARTESIAN_POINT('Ctrl Pts',(15.561470987037,1.56222477878012,-2.82891467766525));
#67140=CARTESIAN_POINT('Ctrl Pts',(15.5749707882375,1.76772718792067,-2.70525833464536));
#67141=CARTESIAN_POINT('Ctrl Pts',(15.5905959944686,1.97324424675203,-2.54809929497118));
#67142=CARTESIAN_POINT('Ctrl Pts',(15.591786958381,1.98872748382345,-2.53603348619014));
#67143=CARTESIAN_POINT('Ctrl Pts',(15.593548556136,2.01135777207077,-2.51806341900508));
#67144=CARTESIAN_POINT('Ctrl Pts',(15.5941148185644,2.01859131530457,-2.51226841088885));
#67145=CARTESIAN_POINT('Ctrl Pts',(15.5951261357562,2.03143668054732,-2.50188631001886));
#67146=CARTESIAN_POINT('Ctrl Pts',(15.595570700121,2.03705823804988,-2.49731131995249));
#67147=CARTESIAN_POINT('Ctrl Pts',(15.5965017063793,2.04877813077054,-2.48770742106146));
#67148=CARTESIAN_POINT('Ctrl Pts',(15.5969882906561,2.05487348657019,-2.48267496751795));
#67149=CARTESIAN_POINT('Ctrl Pts',(15.5982597846743,2.07072277277213,-2.46949111058253));
#67150=CARTESIAN_POINT('Ctrl Pts',(15.5990461367697,2.08044702611454,-2.4613043921902));
#67151=CARTESIAN_POINT('Ctrl Pts',(15.6024911951489,2.12270832461477,-2.42529578505876));
#67152=CARTESIAN_POINT('Ctrl Pts',(15.6051741656447,2.1547363615124,-2.39688573025646));
#67153=CARTESIAN_POINT('Ctrl Pts',(15.6122881886908,2.23731771231515,-2.32063995671971));
#67154=CARTESIAN_POINT('Ctrl Pts',(15.6167611636337,2.28690180192743,-2.27179209815806));
#67155=CARTESIAN_POINT('Ctrl Pts',(15.6373150395803,2.50431372361843,-2.04327334661744));
#67156=CARTESIAN_POINT('Ctrl Pts',(15.6541170110741,2.65281417726106,-1.84637534088398));
#67157=CARTESIAN_POINT('Ctrl Pts',(15.6797977590894,2.84648061589473,-1.51729306187853));
#67158=CARTESIAN_POINT('Ctrl Pts',(15.6888201663959,2.90800355561298,-1.39576313229773));
#67159=CARTESIAN_POINT('Ctrl Pts',(15.6980958187008,2.96591460070476,-1.2607871936792));
#67160=CARTESIAN_POINT('Ctrl Pts',(15.698773833461,2.97011529001045,-1.25085927992975));
#67161=CARTESIAN_POINT('Ctrl Pts',(15.6997809665278,2.97630779311625,-1.23601682739945));
#67162=CARTESIAN_POINT('Ctrl Pts',(15.7001123034902,2.9783373689397,-1.23111826999285));
#67163=CARTESIAN_POINT('Ctrl Pts',(15.700680832198,2.98180674810264,-1.22268583055916));
#67164=CARTESIAN_POINT('Ctrl Pts',(15.7009183751292,2.98325237358707,-1.21915437871109));
#67165=CARTESIAN_POINT('Ctrl Pts',(15.7014107207519,2.98624052192831,-1.21181762946941));
#67166=CARTESIAN_POINT('Ctrl Pts',(15.7016654588692,2.98778204406975,-1.20801195325481));
#67167=CARTESIAN_POINT('Ctrl Pts',(15.7022719817961,2.99144138693292,-1.19892799457506));
#67168=CARTESIAN_POINT('Ctrl Pts',(15.7026233617654,2.99355252982742,-1.19364699973163));
#67169=CARTESIAN_POINT('Ctrl Pts',(15.7038059384463,3.00062718525627,-1.17581302487944));
#67170=CARTESIAN_POINT('Ctrl Pts',(15.7046333068759,3.00552588949837,-1.16323424847324));
#67171=CARTESIAN_POINT('Ctrl Pts',(15.7066001968583,3.01704402313385,-1.13309969751068));
#67172=CARTESIAN_POINT('Ctrl Pts',(15.7077356284515,3.02358954148022,-1.11551597171177));
#67173=CARTESIAN_POINT('Ctrl Pts',(15.7235587087532,3.11326505178351,-0.868024261195266));
#67174=CARTESIAN_POINT('Ctrl Pts',(15.736949543964,3.1701366631343,-0.629408072058027));
#67175=CARTESIAN_POINT('Ctrl Pts',(15.7627845220379,3.22545553185205,-0.171624807649652));
#67176=CARTESIAN_POINT('Ctrl Pts',(15.7751026879613,3.22969604652536,0.0454146241689535));
#67177=CARTESIAN_POINT('Ctrl Pts',(15.7892592668255,3.21069222996387,0.279095864381373));
#67178=CARTESIAN_POINT('Ctrl Pts',(15.7903465476792,3.20908966795408,0.296955518588385));
#67179=CARTESIAN_POINT('Ctrl Pts',(15.7919966615134,3.20644288773968,0.323922174146647));
#67180=CARTESIAN_POINT('Ctrl Pts',(15.7925560324063,3.20550870291503,0.333039817511544));
#67181=CARTESIAN_POINT('Ctrl Pts',(15.7935303797795,3.20381747362355,0.348879515359437));
#67182=CARTESIAN_POINT('Ctrl Pts',(15.7939447958039,3.2030781316616,0.355603433474069));
#67183=CARTESIAN_POINT('Ctrl Pts',(15.7948103564142,3.20149228802624,0.369619512855863));
#67184=CARTESIAN_POINT('Ctrl Pts',(15.7952616173622,3.20064202917643,0.376911202039747));
#67185=CARTESIAN_POINT('Ctrl Pts',(15.7963302239336,3.19857323153404,0.394140958194536));
#67186=CARTESIAN_POINT('Ctrl Pts',(15.796948243093,3.19733328341281,0.404076333835586));
#67187=CARTESIAN_POINT('Ctrl Pts',(15.798997581415,3.19307834974241,0.436923632570207));
#67188=CARTESIAN_POINT('Ctrl Pts',(15.8004352130785,3.18986327516766,0.45980849184632));
#67189=CARTESIAN_POINT('Ctrl Pts',(15.8038381076063,3.18171570045026,0.513597182729975));
#67190=CARTESIAN_POINT('Ctrl Pts',(15.805809715637,3.17657869430164,0.544467218981702));
#67191=CARTESIAN_POINT('Ctrl Pts',(15.8128778197582,3.15669554481401,0.654069296796966));
#67192=CARTESIAN_POINT('Ctrl Pts',(15.8180503151655,3.13946581219031,0.732315558280276));
#67193=CARTESIAN_POINT('Ctrl Pts',(15.8455858022309,3.03390834483839,1.13890478421955));
#67194=CARTESIAN_POINT('Ctrl Pts',(15.8693825382955,2.89696416664439,1.45232811371252));
#67195=CARTESIAN_POINT('Ctrl Pts',(15.8933141668011,2.69622765946527,1.76564732350463));
#67196=CARTESIAN_POINT('Ctrl Pts',(15.8953636228226,2.67845390515615,1.79249516892775));
#67197=CARTESIAN_POINT('Ctrl Pts',(15.8979019589517,2.65566267829451,1.82582590032601));
#67198=CARTESIAN_POINT('Ctrl Pts',(15.8984145599822,2.65101959655277,1.8325609352295));
#67199=CARTESIAN_POINT('Ctrl Pts',(15.8992185662069,2.64367214466132,1.84313243797375));
#67200=CARTESIAN_POINT('Ctrl Pts',(15.8995111226179,2.64098499098507,1.84698074446687));
#67201=CARTESIAN_POINT('Ctrl Pts',(15.900052949987,2.63598276068994,1.85411126416736));
#67202=CARTESIAN_POINT('Ctrl Pts',(15.9003023695789,2.63366997724544,1.85739498917685));
#67203=CARTESIAN_POINT('Ctrl Pts',(15.9008619838766,2.62845818105451,1.86476546996866));
#67204=CARTESIAN_POINT('Ctrl Pts',(15.9011719409318,2.6255557822597,1.86884978063817));
#67205=CARTESIAN_POINT('Ctrl Pts',(15.9020921042403,2.6168931604609,1.88097997452616));
#67206=CARTESIAN_POINT('Ctrl Pts',(15.9027004356467,2.61110532934405,1.88900620509603));
#67207=CARTESIAN_POINT('Ctrl Pts',(15.9078416680229,2.56168290411548,1.95688121330853));
#67208=CARTESIAN_POINT('Ctrl Pts',(15.912241021053,2.516030131726,2.01524135599555));
#67209=CARTESIAN_POINT('Ctrl Pts',(15.923829090987,2.38808002716268,2.16767149428997));
#67210=CARTESIAN_POINT('Ctrl Pts',(15.9308516713183,2.30225526879232,2.25861703209239));
#67211=CARTESIAN_POINT('Ctrl Pts',(15.9436357222225,2.13604899462007,2.41539455626853));
#67212=CARTESIAN_POINT('Ctrl Pts',(15.9493991598353,2.05735765213357,2.48276364463649));
#67213=CARTESIAN_POINT('Ctrl Pts',(15.9595464858926,1.91510056143496,2.59313777271369));
#67214=CARTESIAN_POINT('Ctrl Pts',(15.9638922988872,1.85301808146851,2.63785635465237));
#67215=CARTESIAN_POINT('Ctrl Pts',(15.9683010644095,1.78943598014216,2.68030528773732));
#67216=CARTESIAN_POINT('Origin',(-1.72497344927317,0.,0.));
#67217=CARTESIAN_POINT('',(17.4669156580687,1.78943621037803,2.68030513402633));
#67218=CARTESIAN_POINT('',(17.218344821656,1.78943620926209,2.68030513477136));
#67219=CARTESIAN_POINT('',(-1.72497344927317,1.78943621037804,2.68030513402633));
#67220=CARTESIAN_POINT('',(16.646573449236,-3.2227488963424,-0.00266713776262383));
#67221=CARTESIAN_POINT('Ctrl Pts',(16.6465734492731,-3.2227488963419,-0.0026671383622827));
#67222=CARTESIAN_POINT('Ctrl Pts',(16.6563207021309,-3.22261856278451,-0.160151404718748));
#67223=CARTESIAN_POINT('Ctrl Pts',(16.6660679549888,-3.21094182220305,-0.317172978826481));
#67224=CARTESIAN_POINT('Ctrl Pts',(16.6758152078467,-3.18793726157565,-0.472412509103579));
#67225=CARTESIAN_POINT('Ctrl Pts',(16.6772288474639,-3.18460092068508,-0.494926827072348));
#67226=CARTESIAN_POINT('Ctrl Pts',(16.6786424870812,-3.18102638060837,-0.517403721746265));
#67227=CARTESIAN_POINT('Ctrl Pts',(16.6800561266984,-3.17721437437539,-0.539839218436775));
#67228=CARTESIAN_POINT('Ctrl Pts',(16.6862283747912,-3.16057035286246,-0.637797318908653));
#67229=CARTESIAN_POINT('Ctrl Pts',(16.692400622884,-3.13936250720821,-0.735157376286323));
#67230=CARTESIAN_POINT('Ctrl Pts',(16.6985728709767,-3.11364577400216,-0.831461097429376));
#67231=CARTESIAN_POINT('Ctrl Pts',(16.7047367596294,-3.08796387048676,-0.92763438875508));
#67232=CARTESIAN_POINT('Ctrl Pts',(16.710900648282,-3.05778532814494,-1.02275377146286));
#67233=CARTESIAN_POINT('Ctrl Pts',(16.7170645369346,-3.02321645072212,-1.11636904945593));
#67234=CARTESIAN_POINT('Ctrl Pts',(16.7232218985932,-2.98868417857741,-1.20988519743548));
#67235=CARTESIAN_POINT('Ctrl Pts',(16.7293792602517,-2.94977096356845,-1.30190000192231));
#67236=CARTESIAN_POINT('Ctrl Pts',(16.7355366219103,-2.9066332198159,-1.39197733026175));
#67237=CARTESIAN_POINT('Ctrl Pts',(16.7416894860566,-2.86352698509944,-1.48198886355627));
#67238=CARTESIAN_POINT('Ctrl Pts',(16.7478423502029,-2.81620254362144,-1.57006534375197));
#67239=CARTESIAN_POINT('Ctrl Pts',(16.7539952143492,-2.7648644811798,-1.65579043456904));
#67240=CARTESIAN_POINT('Ctrl Pts',(16.7601457474857,-2.71354586813964,-1.74148304847468));
#67241=CARTESIAN_POINT('Ctrl Pts',(16.7662962806223,-2.65821687840365,-1.82482567081586));
#67242=CARTESIAN_POINT('Ctrl Pts',(16.7724468137588,-2.59912768898054,-1.90542720114799));
#67243=CARTESIAN_POINT('Ctrl Pts',(16.778596661974,-2.54004507970996,-1.98601975572046));
#67244=CARTESIAN_POINT('Ctrl Pts',(16.7847465101892,-2.47720336007928,-2.06387147483843));
#67245=CARTESIAN_POINT('Ctrl Pts',(16.7908963584045,-2.41089502801246,-2.13862168847247));
#67246=CARTESIAN_POINT('Ctrl Pts',(16.7970471667836,-2.34457634335384,-2.21338357271296));
#67247=CARTESIAN_POINT('Ctrl Pts',(16.8031979751627,-2.27479025950479,-2.2850426646788));
#67248=CARTESIAN_POINT('Ctrl Pts',(16.8093487835419,-2.20186772104511,-2.35327348634187));
#67249=CARTESIAN_POINT('Ctrl Pts',(16.815506169908,-2.128867195517,-2.421577277513));
#67250=CARTESIAN_POINT('Ctrl Pts',(16.8216635562742,-2.0527238350218,-2.48644517967099));
#67251=CARTESIAN_POINT('Ctrl Pts',(16.8278209426404,-1.97380332741507,-2.54759062393965));
#67252=CARTESIAN_POINT('Ctrl Pts',(16.8339817653774,-1.89483877512612,-2.60877019281981));
#67253=CARTESIAN_POINT('Ctrl Pts',(16.8401425881143,-1.81309434452169,-2.66622291678952));
#67254=CARTESIAN_POINT('Ctrl Pts',(16.8463034108513,-1.72896476084045,-2.71970557565923));
#67255=CARTESIAN_POINT('Ctrl Pts',(16.852474533768,-1.64469452227114,-2.7732776513199));
#67256=CARTESIAN_POINT('Ctrl Pts',(16.8586456566847,-1.55803154251315,-2.82286618787387));
#67257=CARTESIAN_POINT('Ctrl Pts',(16.8648167796014,-1.46939530811457,-2.86827386959316));
#67258=CARTESIAN_POINT('Ctrl Pts',(16.8695123015469,-1.40195322514026,-2.90282394563104));
#67259=CARTESIAN_POINT('Ctrl Pts',(16.8742078234925,-1.33336924323071,-2.93495447708597));
#67260=CARTESIAN_POINT('Ctrl Pts',(16.8789033454381,-1.2638347816207,-2.96459764677532));
#67261=CARTESIAN_POINT('Ctrl Pts',(16.8850755935309,-1.1724319614384,-3.00356349544968));
#67262=CARTESIAN_POINT('Ctrl Pts',(16.8912478416236,-1.07906451399484,-3.03836684654929));
#67263=CARTESIAN_POINT('Ctrl Pts',(16.8974200897164,-0.98414766434149,-3.0688061094294));
#67264=CARTESIAN_POINT('Ctrl Pts',(16.903583978369,-0.889359366183593,-3.09920414661798));
#67265=CARTESIAN_POINT('Ctrl Pts',(16.9097478670217,-0.793026246694331,
-3.12524971196125));
#67266=CARTESIAN_POINT('Ctrl Pts',(16.9159117556743,-0.695584494367052,
-3.14678880347826));
#67267=CARTESIAN_POINT('Ctrl Pts',(16.9220691173328,-0.598245923939434,
-3.16830508706821));
#67268=CARTESIAN_POINT('Ctrl Pts',(16.9282264789914,-0.499801476377009,
-3.18532429066935));
#67269=CARTESIAN_POINT('Ctrl Pts',(16.93438384065,-0.400702605073226,-3.19774216984227));
#67270=CARTESIAN_POINT('Ctrl Pts',(16.9405367047963,-0.301676118406173,
-3.21015097864273));
#67271=CARTESIAN_POINT('Ctrl Pts',(16.9466895689426,-0.201996588068138,
-3.21796509128979));
#67272=CARTESIAN_POINT('Ctrl Pts',(16.9528424330889,-0.102124861484679,
-3.2211314898909));
#67273=CARTESIAN_POINT('Ctrl Pts',(16.9589929662254,-0.00229097125920541,
-3.22429668890334));
#67274=CARTESIAN_POINT('Ctrl Pts',(16.965143499362,0.0977345368565912,-3.22281765878928));
#67275=CARTESIAN_POINT('Ctrl Pts',(16.9712940324985,0.197487392412191,-3.2166933786636));
#67276=CARTESIAN_POINT('Ctrl Pts',(16.9774438807137,0.297229139522876,-3.21056978053573));
#67277=CARTESIAN_POINT('Ctrl Pts',(16.9835937289289,0.396697860879073,-3.1998019874695));
#67278=CARTESIAN_POINT('Ctrl Pts',(16.9897435771441,0.495432001014504,-3.18444103334805));
#67279=CARTESIAN_POINT('Ctrl Pts',(16.9958943855233,0.594181556320692,-3.16907768095047));
#67280=CARTESIAN_POINT('Ctrl Pts',(17.0020451939024,0.692195873352404,-3.14911980989199));
#67281=CARTESIAN_POINT('Ctrl Pts',(17.0081960022815,0.789022211968121,-3.1246698244008));
#67282=CARTESIAN_POINT('Ctrl Pts',(17.0143533886477,0.885952101590818,-3.10019369085265));
#67283=CARTESIAN_POINT('Ctrl Pts',(17.0205107750139,0.981691053794507,-3.07121595614433));
#67284=CARTESIAN_POINT('Ctrl Pts',(17.0266681613801,1.07580027311818,-3.03788928943417));
#67285=CARTESIAN_POINT('Ctrl Pts',(17.0328289841171,1.16996201377982,-3.00454402347158));
#67286=CARTESIAN_POINT('Ctrl Pts',(17.038989806854,1.26249180795012,-2.9668451558868));
#67287=CARTESIAN_POINT('Ctrl Pts',(17.045150629591,1.35297162465931,-2.92499322142236));
#67288=CARTESIAN_POINT('Ctrl Pts',(17.0513217525077,1.44360271310833,-2.88307131538666));
#67289=CARTESIAN_POINT('Ctrl Pts',(17.0574928754244,1.53217659261148,-2.83698267375057));
#67290=CARTESIAN_POINT('Ctrl Pts',(17.063663998341,1.61830045874771,-2.78697348170322));
#67291=CARTESIAN_POINT('Ctrl Pts',(17.0683595202866,1.68383091551223,-2.74892218019634));
#67292=CARTESIAN_POINT('Ctrl Pts',(17.0730550422322,1.74794346625185,-2.70860203059588));
#67293=CARTESIAN_POINT('Ctrl Pts',(17.0777505641778,1.81047756020777,-2.66613738702343));
#67294=CARTESIAN_POINT('Ctrl Pts',(17.0839228122705,1.89267842022412,-2.61031775326647));
#67295=CARTESIAN_POINT('Ctrl Pts',(17.0900950603633,1.9724400442519,-2.55059475248506));
#67296=CARTESIAN_POINT('Ctrl Pts',(17.0962673084561,2.04936833600685,-2.48720867356813));
#67297=CARTESIAN_POINT('Ctrl Pts',(17.1024311971087,2.12619243923277,-2.42390844216154));
#67298=CARTESIAN_POINT('Ctrl Pts',(17.1085950857613,2.2001905050555,-2.35695526718765));
#67299=CARTESIAN_POINT('Ctrl Pts',(17.114758974414,2.27099713405129,-2.28663280384736));
#67300=CARTESIAN_POINT('Ctrl Pts',(17.1209163360725,2.34172878530586,-2.21638480556116));
#67301=CARTESIAN_POINT('Ctrl Pts',(17.1270736977311,2.40927541187636,-2.14277491637476));
#67302=CARTESIAN_POINT('Ctrl Pts',(17.1332310593896,2.47330521693873,-2.06612653687127));
#67303=CARTESIAN_POINT('Ctrl Pts',(17.1393839235359,2.53728825280869,-1.98953414352619));
#67304=CARTESIAN_POINT('Ctrl Pts',(17.1455367876822,2.59775929671622,-1.90990800476759));
#67305=CARTESIAN_POINT('Ctrl Pts',(17.1516896518285,2.65442456461577,-1.82760712224055));
#67306=CARTESIAN_POINT('Ctrl Pts',(17.1578401849651,2.71106836490448,-1.74533741936523));
#67307=CARTESIAN_POINT('Ctrl Pts',(17.1639907181016,2.763909008008,-1.66039534357055));
#67308=CARTESIAN_POINT('Ctrl Pts',(17.1701412512381,2.81269459936232,-1.57317089129504));
#67309=CARTESIAN_POINT('Ctrl Pts',(17.1762910994534,2.86147475796937,-1.4859561523056));
#67310=CARTESIAN_POINT('Ctrl Pts',(17.1824409476686,2.90620055057427,-1.39645992125861));
#67311=CARTESIAN_POINT('Ctrl Pts',(17.1885907958838,2.94666533956786,-1.30509805726981));
#67312=CARTESIAN_POINT('Ctrl Pts',(17.1947416042629,2.98713644625085,-1.21372192912952));
#67313=CARTESIAN_POINT('Ctrl Pts',(17.200892412642,3.02334505201687,-1.12047998669558));
#67314=CARTESIAN_POINT('Ctrl Pts',(17.2070432210212,3.05513249898531,-1.02580845002554));
#67315=CARTESIAN_POINT('Ctrl Pts',(17.2132006073874,3.08695394106489,-0.931035666803198));
#67316=CARTESIAN_POINT('Ctrl Pts',(17.2193579937535,3.11434464406396,-0.834830648913799));
#67317=CARTESIAN_POINT('Ctrl Pts',(17.2255153801197,3.13719577344072,-0.737645064787729));
#67318=CARTESIAN_POINT('Ctrl Pts',(17.2316762028567,3.16005965578577,-0.640405242437708));
#67319=CARTESIAN_POINT('Ctrl Pts',(17.2378370255936,3.17837883945993,-0.542184191049059));
#67320=CARTESIAN_POINT('Ctrl Pts',(17.2439978483306,3.19209598245055,-0.443441993188545));
#67321=CARTESIAN_POINT('Ctrl Pts',(17.2501689712473,3.20583605891033,-0.344534709847042));
#67322=CARTESIAN_POINT('Ctrl Pts',(17.256340094164,3.214958686299,-0.245104972405858));
#67323=CARTESIAN_POINT('Ctrl Pts',(17.2625112170807,3.21945856441972,-0.145616326297994));
#67324=CARTESIAN_POINT('Ctrl Pts',(17.2672067390262,3.22288245934995,-0.0699167935805051));
#67325=CARTESIAN_POINT('Ctrl Pts',(17.2719022609718,3.22363110273314,0.00581677334481895));
#67326=CARTESIAN_POINT('Ctrl Pts',(17.2765977829174,3.22172229092571,0.0813820782016825));
#67327=CARTESIAN_POINT('Ctrl Pts',(17.2827702109138,3.21921309097379,0.180715317117513));
#67328=CARTESIAN_POINT('Ctrl Pts',(17.2889426389102,3.21210115545655,0.280107242932961));
#67329=CARTESIAN_POINT('Ctrl Pts',(17.2951150669066,3.20037552543264,0.379096371272234));
#67330=CARTESIAN_POINT('Ctrl Pts',(17.3012790891514,3.18866586363608,0.477950693984469));
#67331=CARTESIAN_POINT('Ctrl Pts',(17.3074431113961,3.172355046599,0.576402881916098));
#67332=CARTESIAN_POINT('Ctrl Pts',(17.3136071336409,3.15148411714757,0.673992152674372));
#67333=CARTESIAN_POINT('Ctrl Pts',(17.3199949888254,3.12985530569827,0.775125163622305));
#67334=CARTESIAN_POINT('Ctrl Pts',(17.3263828440099,3.10332887786078,0.875330920908748));
#67335=CARTESIAN_POINT('Ctrl Pts',(17.3327706991944,3.07200934862504,0.974102727878518));
#67336=CARTESIAN_POINT('Ctrl Pts',(17.3389233296928,3.04184312143185,1.06923738801037));
#67337=CARTESIAN_POINT('Ctrl Pts',(17.3450759601912,3.00723071574878,1.16304138810687));
#67338=CARTESIAN_POINT('Ctrl Pts',(17.3512285906897,2.96831713035872,1.25507409188422));
#67339=CARTESIAN_POINT('Ctrl Pts',(17.3573788863308,2.929418312257,1.34707187023743));
#67340=CARTESIAN_POINT('Ctrl Pts',(17.363529181972,2.88622172737016,1.43729928857426));
#67341=CARTESIAN_POINT('Ctrl Pts',(17.3696794776131,2.83892100630479,1.52533441659899));
#67342=CARTESIAN_POINT('Ctrl Pts',(17.3758290844128,2.79162558298445,1.61335968456978));
#67343=CARTESIAN_POINT('Ctrl Pts',(17.3819786912125,2.74022714357916,1.69919276816272));
#67344=CARTESIAN_POINT('Ctrl Pts',(17.3881282980121,2.68496542556838,1.78243603700172));
#67345=CARTESIAN_POINT('Ctrl Pts',(17.394278860962,2.62969511538211,1.86569224863005));
#67346=CARTESIAN_POINT('Ctrl Pts',(17.4004294239118,2.57056057432557,1.94635748428125));
#67347=CARTESIAN_POINT('Ctrl Pts',(17.4065799868617,2.5078444643747,2.02406366130248));
#67348=CARTESIAN_POINT('Ctrl Pts',(17.412736350793,2.44506920292928,2.10184312789014));
#67349=CARTESIAN_POINT('Ctrl Pts',(17.4188927147243,2.37870590385022,2.17665762742585));
#67350=CARTESIAN_POINT('Ctrl Pts',(17.4250490786555,2.30907687291099,2.24817293762904));
#67351=CARTESIAN_POINT('Ctrl Pts',(17.4312089072886,2.23940865588232,2.31972849548906));
#67352=CARTESIAN_POINT('Ctrl Pts',(17.4373687359217,2.16647136398159,2.38798087018275));
#67353=CARTESIAN_POINT('Ctrl Pts',(17.4435285645548,2.09062202041369,2.4526347323361));
#67354=CARTESIAN_POINT('Ctrl Pts',(17.4496967946728,2.01466922476066,2.51737677688546));
#67355=CARTESIAN_POINT('Ctrl Pts',(17.4558650247908,1.93579679350734,2.57851024843153));
#67356=CARTESIAN_POINT('Ctrl Pts',(17.4620332549088,1.85439222095044,2.6357820572609));
#67357=CARTESIAN_POINT('Ctrl Pts',(17.4636607226287,1.83291388574586,2.65089304020906));
#67358=CARTESIAN_POINT('Ctrl Pts',(17.4652881903487,1.81125941470005,2.66573543763448));
#67359=CARTESIAN_POINT('Ctrl Pts',(17.4669156580687,1.78943621037803,2.68030513402633));
#67360=CARTESIAN_POINT('Ctrl Pts',(16.2168686787502,1.78943621037802,2.68030513402634));
#67361=CARTESIAN_POINT('Ctrl Pts',(16.2230266939213,1.70630275993286,2.73580702619216));
#67362=CARTESIAN_POINT('Ctrl Pts',(16.2291847090924,1.62063435401742,2.78740441593627));
#67363=CARTESIAN_POINT('Ctrl Pts',(16.2353427242635,1.53283923964877,2.8348759104929));
#67364=CARTESIAN_POINT('Ctrl Pts',(16.2415045012076,1.44499049350348,2.88237640416426));
#67365=CARTESIAN_POINT('Ctrl Pts',(16.2476662781518,1.35501284322985,2.92574579597347));
#67366=CARTESIAN_POINT('Ctrl Pts',(16.2538280550959,1.26333585366192,2.96481029466512));
#67367=CARTESIAN_POINT('Ctrl Pts',(16.2599997290293,1.17151161335968,3.00393753839395));
#67368=CARTESIAN_POINT('Ctrl Pts',(16.2661714029626,1.07798299073099,3.03874593220572));
#67369=CARTESIAN_POINT('Ctrl Pts',(16.272343076896,0.983196062854421,3.06911111960574));
#67370=CARTESIAN_POINT('Ctrl Pts',(16.2756826143371,0.931906170033793,3.08554194231637));
#67371=CARTESIAN_POINT('Ctrl Pts',(16.2790221517781,0.880248060733309,3.10067268616429));
#67372=CARTESIAN_POINT('Ctrl Pts',(16.2823616892192,0.828293496285961,3.11448991754836));
#67373=CARTESIAN_POINT('Ctrl Pts',(16.288533937312,0.732269281262086,3.14002740037728));
#67374=CARTESIAN_POINT('Ctrl Pts',(16.2947061854047,0.634893910508744,3.1611648236009));
#67375=CARTESIAN_POINT('Ctrl Pts',(16.3008784334975,0.536607106782113,3.17776185002132));
#67376=CARTESIAN_POINT('Ctrl Pts',(16.3070423221501,0.438453418678726,3.19433639810862));
#67377=CARTESIAN_POINT('Ctrl Pts',(16.3132062108028,0.339391175663221,3.20638270016883));
#67378=CARTESIAN_POINT('Ctrl Pts',(16.3193700994554,0.23987406558232,3.21381051015162));
#67379=CARTESIAN_POINT('Ctrl Pts',(16.3255274611139,0.140462335015088,3.22123045476329));
#67380=CARTESIAN_POINT('Ctrl Pts',(16.3316848227725,0.0405971257550134,
3.22404159804077));
#67381=CARTESIAN_POINT('Ctrl Pts',(16.337842184431,-0.0592598587934908,
3.222205119423));
#67382=CARTESIAN_POINT('Ctrl Pts',(16.3439950485773,-0.159043904957785,
3.22036998222149));
#67383=CARTESIAN_POINT('Ctrl Pts',(16.3501479127236,-0.258819305362028,
3.21389398044223));
#67384=CARTESIAN_POINT('Ctrl Pts',(16.35630077687,-0.358122361369344,3.20279033606436));
#67385=CARTESIAN_POINT('Ctrl Pts',(16.3624513100065,-0.457387796459263,
3.19169089829709));
#67386=CARTESIAN_POINT('Ctrl Pts',(16.368601843143,-0.556180811514087,3.17596734970656));
#67387=CARTESIAN_POINT('Ctrl Pts',(16.3747523762796,-0.654041732521595,
3.15568486617725));
#67388=CARTESIAN_POINT('Ctrl Pts',(16.3809022244948,-0.751891755769422,
3.13540464129858));
#67389=CARTESIAN_POINT('Ctrl Pts',(16.38705207271,-0.848809465998504,3.11056657898061));
#67390=CARTESIAN_POINT('Ctrl Pts',(16.3932019209252,-0.944345297372316,
3.08128699115009));
#67391=CARTESIAN_POINT('Ctrl Pts',(16.3993527293043,-1.03989604457104,3.05200283195405));
#67392=CARTESIAN_POINT('Ctrl Pts',(16.4055035376835,-1.1340640690317,3.01827589717565));
#67393=CARTESIAN_POINT('Ctrl Pts',(16.4116543460626,-1.22641585355492,2.98027208768749));
#67394=CARTESIAN_POINT('Ctrl Pts',(16.4178117324288,-1.31886640376962,2.9422276349942));
#67395=CARTESIAN_POINT('Ctrl Pts',(16.423969118795,-1.4094964328398,2.89989733959456));
#67396=CARTESIAN_POINT('Ctrl Pts',(16.4301265051612,-1.49789339158082,2.8534948659422));
#67397=CARTESIAN_POINT('Ctrl Pts',(16.4362873278981,-1.58633968370895,2.80706649557091));
#67398=CARTESIAN_POINT('Ctrl Pts',(16.4424481506351,-1.67255004880547,2.7565616405934));
#67399=CARTESIAN_POINT('Ctrl Pts',(16.448608973372,-1.7561393138044,2.70223838197347));
#67400=CARTESIAN_POINT('Ctrl Pts',(16.4547800962887,-1.83986833034136,2.64782430117748));
#67401=CARTESIAN_POINT('Ctrl Pts',(16.4609512192054,-1.92096714054579,2.58957931854786));
#67402=CARTESIAN_POINT('Ctrl Pts',(16.4671223421221,-1.99908204816339,2.5278031029356));
#67403=CARTESIAN_POINT('Ctrl Pts',(16.4718178640677,-2.05851859933026,2.48079843619378));
#67404=CARTESIAN_POINT('Ctrl Pts',(16.4765133860133,-2.11622827998603,2.43175023148924));
#67405=CARTESIAN_POINT('Ctrl Pts',(16.4812089079588,-2.17206990711811,2.38080446091062));
#67406=CARTESIAN_POINT('Ctrl Pts',(16.4872889959218,-2.2443775246516,2.31483633850555));
#67407=CARTESIAN_POINT('Ctrl Pts',(16.4933690838848,-2.3138226346073,2.24543804555174));
#67408=CARTESIAN_POINT('Ctrl Pts',(16.4994491718478,-2.38005449792452,2.17289165615989));
#67409=CARTESIAN_POINT('Ctrl Pts',(16.5055793500724,-2.44683200653065,2.09974759982019));
#67410=CARTESIAN_POINT('Ctrl Pts',(16.5117095282969,-2.51034268704653,2.02340358087469));
#67411=CARTESIAN_POINT('Ctrl Pts',(16.5178397065214,-2.57026084270078,1.94419051612208));
#67412=CARTESIAN_POINT('Ctrl Pts',(16.5239044002319,-2.62953893355454,1.86582363052726));
#67413=CARTESIAN_POINT('Ctrl Pts',(16.5299690939424,-2.68530058600998,1.78464905108463));
#67414=CARTESIAN_POINT('Ctrl Pts',(16.5360337876529,-2.73726824252463,1.70102325997211));
#67415=CARTESIAN_POINT('Ctrl Pts',(16.5420946861043,-2.78920337790466,1.61744980151786));
#67416=CARTESIAN_POINT('Ctrl Pts',(16.5481555845558,-2.83734899587132,1.53142855711569));
#67417=CARTESIAN_POINT('Ctrl Pts',(16.5542164830072,-2.88147004464528,1.44334609304627));
#67418=CARTESIAN_POINT('Ctrl Pts',(16.5602753222,-2.92557610279544,1.35529355598717));
#67419=CARTESIAN_POINT('Ctrl Pts',(16.5663341613929,-2.96566010800427,1.26518159138569));
#67420=CARTESIAN_POINT('Ctrl Pts',(16.5723930005857,-3.00153287295572,1.17342148227573));
#67421=CARTESIAN_POINT('Ctrl Pts',(16.5785747046399,-3.03813308786114,1.07980060533149));
#67422=CARTESIAN_POINT('Ctrl Pts',(16.5847564086941,-3.07034918648835,0.984464442450112));
#67423=CARTESIAN_POINT('Ctrl Pts',(16.5909381127483,-3.09803229148831,0.887870195127457));
#67424=CARTESIAN_POINT('Ctrl Pts',(16.5970005632215,-3.12518135128422,0.793139383807464));
#67425=CARTESIAN_POINT('Ctrl Pts',(16.6030630136948,-3.14797068691146,0.697199052244218));
#67426=CARTESIAN_POINT('Ctrl Pts',(16.609125464168,-3.16631103188143,0.600493140581918));
#67427=CARTESIAN_POINT('Ctrl Pts',(16.6153667950127,-3.18519253223647,0.500933797048542));
#67428=CARTESIAN_POINT('Ctrl Pts',(16.6216081258573,-3.19935830376747,0.400563491805864));
#67429=CARTESIAN_POINT('Ctrl Pts',(16.627849456702,-3.20876825168828,0.299873088918141));
#67430=CARTESIAN_POINT('Ctrl Pts',(16.6340907875467,-3.2181781996091,0.199182686030418));
#67431=CARTESIAN_POINT('Ctrl Pts',(16.6403321183913,-3.22283235110456,0.0981727012668687));
#67432=CARTESIAN_POINT('Ctrl Pts',(16.646573449236,-3.2227488963424,-0.00266713776262558));
#67433=CARTESIAN_POINT('',(16.397001193014,-3.22274992098439,-0.00071364915948762));
#67434=CARTESIAN_POINT('Ctrl Pts',(15.9683010644095,1.78943598014216,2.68030528773732));
#67435=CARTESIAN_POINT('Ctrl Pts',(15.9744111699109,1.70131758392898,2.73913523872003));
#67436=CARTESIAN_POINT('Ctrl Pts',(15.9806437554029,1.61031895692001,2.79360584986089));
#67437=CARTESIAN_POINT('Ctrl Pts',(15.9881249457863,1.50100645402874,2.85191445822639));
#67438=CARTESIAN_POINT('Ctrl Pts',(15.9892077917178,1.48518103854343,2.86018770625233));
#67439=CARTESIAN_POINT('Ctrl Pts',(15.9908522949314,1.46114730347362,2.87249887356432));
#67440=CARTESIAN_POINT('Ctrl Pts',(15.991410523563,1.45298903337334,2.87663415944084));
#67441=CARTESIAN_POINT('Ctrl Pts',(15.9923834385129,1.43877101168713,2.88376511386765));
#67442=CARTESIAN_POINT('Ctrl Pts',(15.992797568485,1.43271920501153,2.8867765647031));
#67443=CARTESIAN_POINT('Ctrl Pts',(15.9936538956602,1.42020620145379,2.89295414398068));
#67444=CARTESIAN_POINT('Ctrl Pts',(15.9940961792845,1.41374379107446,2.89611771613011));
#67445=CARTESIAN_POINT('Ctrl Pts',(15.9951387239813,1.39851206812112,2.90351103827247));
#67446=CARTESIAN_POINT('Ctrl Pts',(15.9957396100857,1.38973411158864,2.90772272574307));
#67447=CARTESIAN_POINT('Ctrl Pts',(15.997012525266,1.37114198072267,2.91653986054752));
#67448=CARTESIAN_POINT('Ctrl Pts',(15.9976848798145,1.36132340055682,2.92113568393084));
#67449=CARTESIAN_POINT('Ctrl Pts',(15.9995033858335,1.33477332771783,2.93340015604154));
#67450=CARTESIAN_POINT('Ctrl Pts',(16.0006527480568,1.31799921591922,2.94097506891944));
#67451=CARTESIAN_POINT('Ctrl Pts',(16.0098667153589,1.18359436543072,3.00028929492527));
#67452=CARTESIAN_POINT('Ctrl Pts',(16.018165684055,1.06304416223038,3.04508806783611));
#67453=CARTESIAN_POINT('Ctrl Pts',(16.0445596502099,0.680859249907262,3.16165087517386));
#67454=CARTESIAN_POINT('Ctrl Pts',(16.0632944570895,0.412653181284849,3.2076944093041));
#67455=CARTESIAN_POINT('Ctrl Pts',(16.0820290354376,0.128649797679572,3.2202083437708));
#67456=CARTESIAN_POINT('Ctrl Pts',(16.0828982768621,0.115430785474178,3.22070928379955));
#67457=CARTESIAN_POINT('Ctrl Pts',(16.0877893049261,0.0407935520529635,
3.22307758054531));
#67458=CARTESIAN_POINT('Ctrl Pts',(16.0917526929636,-0.0206699549010299,
3.22326963576358));
#67459=CARTESIAN_POINT('Ctrl Pts',(16.0962603126204,-0.092171009264649,
3.22144741371853));
#67460=CARTESIAN_POINT('Ctrl Pts',(16.0968923923274,-0.10223499888431,3.22114373253747));
#67461=CARTESIAN_POINT('Ctrl Pts',(16.0978416425163,-0.117408838105377,
3.22061467490167));
#67462=CARTESIAN_POINT('Ctrl Pts',(16.0981607281436,-0.122519730306948,
3.22042429440686));
#67463=CARTESIAN_POINT('Ctrl Pts',(16.0987296716682,-0.131651506416395,
3.22006236581669));
#67464=CARTESIAN_POINT('Ctrl Pts',(16.0989797874212,-0.135672528732226,
3.21989545241152));
#67465=CARTESIAN_POINT('Ctrl Pts',(16.0995160115931,-0.144307409481603,
3.21952081281911));
#67466=CARTESIAN_POINT('Ctrl Pts',(16.0998019837475,-0.148921120330165,
3.21931070155764));
#67467=CARTESIAN_POINT('Ctrl Pts',(16.1005856181057,-0.161587044799179,
3.21870660080785));
#67468=CARTESIAN_POINT('Ctrl Pts',(16.1010821495033,-0.169638323574166,
3.21829231077317));
#67469=CARTESIAN_POINT('Ctrl Pts',(16.1037011887418,-0.212236766076815,
3.21594004452639));
#67470=CARTESIAN_POINT('Ctrl Pts',(16.1057953492502,-0.246754167624729,
3.21347591017222));
#67471=CARTESIAN_POINT('Ctrl Pts',(16.1118446440377,-0.347528374177671,
3.20464837686346));
#67472=CARTESIAN_POINT('Ctrl Pts',(16.1157313326968,-0.413638642460783,
3.19678767576636));
#67473=CARTESIAN_POINT('Ctrl Pts',(16.1249567225218,-0.572218270836931,
3.17292960036643));
#67474=CARTESIAN_POINT('Ctrl Pts',(16.1302349329642,-0.664325252683203,
3.15493098941956));
#67475=CARTESIAN_POINT('Ctrl Pts',(16.1426761042349,-0.880317490871748,
3.10284368921993));
#67476=CARTESIAN_POINT('Ctrl Pts',(16.1498085647131,-1.00320497091956,3.06531840584928));
#67477=CARTESIAN_POINT('Ctrl Pts',(16.1664215780302,-1.27833215820242,2.96298256846807));
#67478=CARTESIAN_POINT('Ctrl Pts',(16.1759724715495,-1.42846375938282,2.89359274938661));
#67479=CARTESIAN_POINT('Ctrl Pts',(16.1871324931095,-1.58975921206449,2.80342102454104));
#67480=CARTESIAN_POINT('Ctrl Pts',(16.1883248621219,-1.60682493959801,2.7936745301117));
#67481=CARTESIAN_POINT('Ctrl Pts',(16.1900881480807,-1.63181014318447,2.77910043163032));
#67482=CARTESIAN_POINT('Ctrl Pts',(16.1906546814246,-1.63979984697515,2.77439362951903));
#67483=CARTESIAN_POINT('Ctrl Pts',(16.1916566786765,-1.65386339416463,2.76602670321143));
#67484=CARTESIAN_POINT('Ctrl Pts',(16.1920916183248,-1.659945705292,2.76238087591891));
#67485=CARTESIAN_POINT('Ctrl Pts',(16.1929999880696,-1.67260185712784,2.75473769787025));
#67486=CARTESIAN_POINT('Ctrl Pts',(16.1934735455634,-1.67917350871398,2.75073682538486));
#67487=CARTESIAN_POINT('Ctrl Pts',(16.1944407235126,-1.69254124746841,2.74253268750756));
#67488=CARTESIAN_POINT('Ctrl Pts',(16.1949344088852,-1.69933615025632,2.73832760330379));
#67489=CARTESIAN_POINT('Ctrl Pts',(16.1961445497975,-1.71592198604141,2.72797780782076));
#67490=CARTESIAN_POINT('Ctrl Pts',(16.1968620200333,-1.72569557740239,2.72180564160397));
#67491=CARTESIAN_POINT('Ctrl Pts',(16.1988370017323,-1.75243412638133,2.70471794303886));
#67492=CARTESIAN_POINT('Ctrl Pts',(16.2000984769707,-1.76932990841859,2.69369563314341));
#67493=CARTESIAN_POINT('Ctrl Pts',(16.2109888188054,-1.91360957536704,2.59762875079558));
#67494=CARTESIAN_POINT('Ctrl Pts',(16.2209531248965,-2.03486617573846,2.50377403991726));
#67495=CARTESIAN_POINT('Ctrl Pts',(16.2424460007868,-2.27532453105108,2.28861532452761));
#67496=CARTESIAN_POINT('Ctrl Pts',(16.25399747391,-2.39254884207164,2.1657716825991));
#67497=CARTESIAN_POINT('Ctrl Pts',(16.2751706692155,-2.59094393291775,1.9220006607759));
#67498=CARTESIAN_POINT('Ctrl Pts',(16.2847988289659,-2.67467119925028,1.80366893425787));
#67499=CARTESIAN_POINT('Ctrl Pts',(16.2947029690045,-2.75642449651405,1.66984602855923));
#67500=CARTESIAN_POINT('Ctrl Pts',(16.2954579452262,-2.76262754158888,1.65956344899287));
#67501=CARTESIAN_POINT('Ctrl Pts',(16.2965448542827,-2.77151808681189,1.64463790205908));
#67502=CARTESIAN_POINT('Ctrl Pts',(16.296879712477,-2.77425160688929,1.64002266968465));
#67503=CARTESIAN_POINT('Ctrl Pts',(16.2974671813133,-2.77903778234854,1.63189555819161));
#67504=CARTESIAN_POINT('Ctrl Pts',(16.297720110279,-2.78109532785786,1.62838659005661));
#67505=CARTESIAN_POINT('Ctrl Pts',(16.2982476052231,-2.78538004415174,1.62104756289266));
#67506=CARTESIAN_POINT('Ctrl Pts',(16.2985220893806,-2.78760595761773,1.61721681203778));
#67507=CARTESIAN_POINT('Ctrl Pts',(16.2992424369652,-2.7934376760502,1.60713273187644));
#67508=CARTESIAN_POINT('Ctrl Pts',(16.2996874564643,-2.79703040851733,1.60087181374437));
#67509=CARTESIAN_POINT('Ctrl Pts',(16.301668906611,-2.8129802530347,1.57285901948052));
#67510=CARTESIAN_POINT('Ctrl Pts',(16.3031908843387,-2.82510528331116,1.55097505698315));
#67511=CARTESIAN_POINT('Ctrl Pts',(16.3160153682931,-2.92603551018716,1.36369866004603));
#67512=CARTESIAN_POINT('Ctrl Pts',(16.3265401636377,-3.00050002832363,1.19095625801945));
#67513=CARTESIAN_POINT('Ctrl Pts',(16.3514993649324,-3.14077162809572,0.7671733290003));
#67514=CARTESIAN_POINT('Ctrl Pts',(16.3658858189897,-3.19218097387089,0.512799416071989));
#67515=CARTESIAN_POINT('Ctrl Pts',(16.3833188965377,-3.21522846088223,0.222464671532063));
#67516=CARTESIAN_POINT('Ctrl Pts',(16.3852888400579,-3.21731807968137,0.189865322853617));
#67517=CARTESIAN_POINT('Ctrl Pts',(16.3879966107665,-3.21949151182315,0.14537248388479));
#67518=CARTESIAN_POINT('Ctrl Pts',(16.3887209270774,-3.22000561539516,0.133501253434329));
#67519=CARTESIAN_POINT('Ctrl Pts',(16.3898721200999,-3.22071631611739,0.114683324781635));
#67520=CARTESIAN_POINT('Ctrl Pts',(16.3902976382364,-3.22095611797239,0.107738288395413));
#67521=CARTESIAN_POINT('Ctrl Pts',(16.3911517513287,-3.22139163868266,0.0938197257307931));
#67522=CARTESIAN_POINT('Ctrl Pts',(16.3915803494882,-3.22158718048736,0.0868462319927856));
#67523=CARTESIAN_POINT('Ctrl Pts',(16.3924407430093,-3.22193368692295,0.0728693967865503));
#67524=CARTESIAN_POINT('Ctrl Pts',(16.3928725419104,-3.22208446335216,0.065866089161238));
#67525=CARTESIAN_POINT('Ctrl Pts',(16.3939263155754,-3.22239617563137,0.04880250781653));
#67526=CARTESIAN_POINT('Ctrl Pts',(16.394549049548,-3.22253283271506,0.0387419136726294));
#67527=CARTESIAN_POINT('Ctrl Pts',(16.3957811749886,-3.22270957562087,0.0188828806645124));
#67528=CARTESIAN_POINT('Ctrl Pts',(16.3963904821978,-3.22275209071569,0.00908458474906739));
#67529=CARTESIAN_POINT('Ctrl Pts',(16.397001193014,-3.22274992098439,-0.00071364915948762));
#67530=CARTESIAN_POINT('Ctrl Pts',(16.3970011089261,-3.22274992128285,-0.000712300053586545));
#67531=CARTESIAN_POINT('Ctrl Pts',(16.4000499952323,-3.222739109685,-0.0496285902397631));
#67532=CARTESIAN_POINT('Ctrl Pts',(16.4031335870394,-3.22161459570378,-0.0985365305315511));
#67533=CARTESIAN_POINT('Ctrl Pts',(16.4185052177376,-3.21058390395279,-0.339461510791843));
#67534=CARTESIAN_POINT('Ctrl Pts',(16.4312857109541,-3.18462237739346,-0.53032325674288));
#67535=CARTESIAN_POINT('Ctrl Pts',(16.4561576032861,-3.10259562993228,-0.889401700762396));
#67536=CARTESIAN_POINT('Ctrl Pts',(16.4681680705531,-3.049364880723,-1.0575979878311));
#67537=CARTESIAN_POINT('Ctrl Pts',(16.4828813413233,-2.96463328870021,-1.26464671447841));
#67538=CARTESIAN_POINT('Ctrl Pts',(16.4859767176357,-2.94563659456967,-1.3082841445284));
#67539=CARTESIAN_POINT('Ctrl Pts',(16.4907729904448,-2.91423179777867,-1.37626878528022));
#67540=CARTESIAN_POINT('Ctrl Pts',(16.4925055193836,-2.90246931044543,-1.40090497920624));
#67541=CARTESIAN_POINT('Ctrl Pts',(16.4946871106681,-2.88710181709131,-1.43206706930084));
#67542=CARTESIAN_POINT('Ctrl Pts',(16.4951532041314,-2.88378572056338,-1.43873309328605));
#67543=CARTESIAN_POINT('Ctrl Pts',(16.4958975389548,-2.87843672747348,-1.44939285543799));
#67544=CARTESIAN_POINT('Ctrl Pts',(16.4961766908395,-2.87641857442559,-1.45339390006555));
#67545=CARTESIAN_POINT('Ctrl Pts',(16.4967072451973,-2.87255968088809,-1.461004743599));
#67546=CARTESIAN_POINT('Ctrl Pts',(16.4969587370425,-2.87072049997563,-1.46461523693213));
#67547=CARTESIAN_POINT('Ctrl Pts',(16.4975357192614,-2.86647807306831,-1.4729048469192));
#67548=CARTESIAN_POINT('Ctrl Pts',(16.4978609126101,-2.86407017960254,-1.47758155061002));
#67549=CARTESIAN_POINT('Ctrl Pts',(16.4988915053716,-2.85638611900982,-1.49241647257229));
#67550=CARTESIAN_POINT('Ctrl Pts',(16.4995942536309,-2.85106720501054,-1.50255262475929));
#67551=CARTESIAN_POINT('Ctrl Pts',(16.506352429903,-2.79916285360483,-1.60019775203507));
#67552=CARTESIAN_POINT('Ctrl Pts',(16.5121696974556,-2.74861177364789,-1.68555128366764));
#67553=CARTESIAN_POINT('Ctrl Pts',(16.5262668709858,-2.61392722851102,-1.89074104311305));
#67554=CARTESIAN_POINT('Ctrl Pts',(16.5343913260252,-2.52541670116867,-2.00743420474199));
#67555=CARTESIAN_POINT('Ctrl Pts',(16.5559208039694,-2.2724097377441,-2.29766441150014));
#67556=CARTESIAN_POINT('Ctrl Pts',(16.5694050719756,-2.09605762214324,-2.45959907477577));
#67557=CARTESIAN_POINT('Ctrl Pts',(16.5846280695142,-1.8927551213189,-2.60840401901072));
#67558=CARTESIAN_POINT('Ctrl Pts',(16.5854319686233,-1.8820043438503,-2.61617146175146));
#67559=CARTESIAN_POINT('Ctrl Pts',(16.5867674645548,-1.86412210903003,-2.62892412003284));
#67560=CARTESIAN_POINT('Ctrl Pts',(16.58729760397,-1.85701779562866,-2.63394726041709));
#67561=CARTESIAN_POINT('Ctrl Pts',(16.5883294362001,-1.84317982421048,-2.64364765356918));
#67562=CARTESIAN_POINT('Ctrl Pts',(16.588831001631,-1.83644848195097,-2.64832810500794));
#67563=CARTESIAN_POINT('Ctrl Pts',(16.5893362927831,-1.82966255946109,-2.65300819505124));
#67564=CARTESIAN_POINT('Ctrl Pts',(16.589339036157,-1.82962571656205,-2.65303360359336));
#67565=CARTESIAN_POINT('Ctrl Pts',(16.5893440699943,-1.82955811300148,-2.65308022401251));
#67566=CARTESIAN_POINT('Ctrl Pts',(16.5893463611346,-1.82952734329172,-2.65310144247141));
#67567=CARTESIAN_POINT('Ctrl Pts',(16.589351015401,-1.82946483691802,-2.65314454458581));
#67568=CARTESIAN_POINT('Ctrl Pts',(16.5893533784737,-1.82943310096691,-2.65316642769948));
#67569=CARTESIAN_POINT('Ctrl Pts',(16.5893581796194,-1.82936862161112,-2.65321088689635));
#67570=CARTESIAN_POINT('Ctrl Pts',(16.5893606176394,-1.82933587890988,-2.65323346244046));
#67571=CARTESIAN_POINT('Ctrl Pts',(16.5893655718598,-1.82926934332688,-2.65327933579337));
#67572=CARTESIAN_POINT('Ctrl Pts',(16.5893680880116,-1.82923555108999,-2.65330263309941));
#67573=CARTESIAN_POINT('Ctrl Pts',(16.5893732018518,-1.82916687133701,-2.65334998089165));
#67574=CARTESIAN_POINT('Ctrl Pts',(16.5893757994974,-1.82913198438932,-2.65337403092339));
#67575=CARTESIAN_POINT('Ctrl Pts',(16.5893810799027,-1.82906106714463,-2.65342291711476));
#67576=CARTESIAN_POINT('Ctrl Pts',(16.5893837626122,-1.82902503751554,-2.6534477527465));
#67577=CARTESIAN_POINT('Ctrl Pts',(16.589389216898,-1.82895178448462,-2.6534982446901));
#67578=CARTESIAN_POINT('Ctrl Pts',(16.5893919884389,-1.82891456155067,-2.6535239006067));
#67579=CARTESIAN_POINT('Ctrl Pts',(16.5893976243923,-1.82883886809789,-2.65357606998867));
#67580=CARTESIAN_POINT('Ctrl Pts',(16.5894004887657,-1.82880039809474,-2.65360258302006));
#67581=CARTESIAN_POINT('Ctrl Pts',(16.5894063146363,-1.82872215336613,-2.65365650577095));
#67582=CARTESIAN_POINT('Ctrl Pts',(16.5894092760919,-1.82868237919014,-2.65368391502683));
#67583=CARTESIAN_POINT('Ctrl Pts',(16.5894153006245,-1.82860146567853,-2.65373967161695));
#67584=CARTESIAN_POINT('Ctrl Pts',(16.5894183636691,-1.82856032676909,-2.65376801856559));
#67585=CARTESIAN_POINT('Ctrl Pts',(16.5894245961762,-1.82847661933577,-2.6538256946744));
#67586=CARTESIAN_POINT('Ctrl Pts',(16.5894277656057,-1.82843405124559,-2.65385502343617));
#67587=CARTESIAN_POINT('Ctrl Pts',(16.5894342159882,-1.8283474168431,-2.65391471013784));
#67588=CARTESIAN_POINT('Ctrl Pts',(16.5894374969081,-1.82830335096306,-2.65394506767194));
#67589=CARTESIAN_POINT('Ctrl Pts',(16.5894441757122,-1.8282136478684,-2.65400686195763));
#67590=CARTESIAN_POINT('Ctrl Pts',(16.5894475735653,-1.82816801105835,-2.65403829831325));
#67591=CARTESIAN_POINT('Ctrl Pts',(16.589454492026,-1.82807508829159,-2.65410230348491));
#67592=CARTESIAN_POINT('Ctrl Pts',(16.5894580126124,-1.82802780260412,-2.65413487198798));
#67593=CARTESIAN_POINT('Ctrl Pts',(16.5894651827376,-1.82793149879386,-2.65420119843224));
#67594=CARTESIAN_POINT('Ctrl Pts',(16.5894688322551,-1.82788248094004,-2.65423495604939));
#67595=CARTESIAN_POINT('Ctrl Pts',(16.5894762668778,-1.82778262362344,-2.65430372171122));
#67596=CARTESIAN_POINT('Ctrl Pts',(16.589480051958,-1.82773178447891,-2.65433872938543));
#67597=CARTESIAN_POINT('Ctrl Pts',(16.5894877648009,-1.82762818923377,-2.65441006035623));
#67598=CARTESIAN_POINT('Ctrl Pts',(16.5894916925427,-1.82757543339558,-2.65444638330694));
#67599=CARTESIAN_POINT('Ctrl Pts',(16.5894996983117,-1.82746790258163,-2.65452041468055));
#67600=CARTESIAN_POINT('Ctrl Pts',(16.5895037763236,-1.82741312779065,-2.65455812279566));
#67601=CARTESIAN_POINT('Ctrl Pts',(16.5895120908056,-1.82730144923561,-2.65463499956085));
#67602=CARTESIAN_POINT('Ctrl Pts',(16.5895163272605,-1.8272445456507,-2.65467416788987));
#67603=CARTESIAN_POINT('Ctrl Pts',(16.5895249674066,-1.82712849152999,-2.6547540456877));
#67604=CARTESIAN_POINT('Ctrl Pts',(16.5895293710878,-1.82706934110019,-2.65479475486668));
#67605=CARTESIAN_POINT('Ctrl Pts',(16.5895383551484,-1.82694866611953,-2.65487780122581));
#67606=CARTESIAN_POINT('Ctrl Pts',(16.5895429355172,-1.82688714168104,-2.65492013809043));
#67607=CARTESIAN_POINT('Ctrl Pts',(16.5895522831516,-1.82676158160453,-2.65500653342234));
#67608=CARTESIAN_POINT('Ctrl Pts',(16.5895570504099,-1.82669754603437,-2.65505059158082));
#67609=CARTESIAN_POINT('Ctrl Pts',(16.5895667828414,-1.82656681559989,-2.6551405305939));
#67610=CARTESIAN_POINT('Ctrl Pts',(16.5895717480099,-1.82650012076539,-2.655186411139));
#67611=CARTESIAN_POINT('Ctrl Pts',(16.5895818881815,-1.82636391158558,-2.65528010425945));
#67612=CARTESIAN_POINT('Ctrl Pts',(16.5895870631839,-1.82629439721301,-2.65532791653434));
#67613=CARTESIAN_POINT('Ctrl Pts',(16.5895976359233,-1.82615237556289,-2.65542559140141));
#67614=CARTESIAN_POINT('Ctrl Pts',(16.5896030336617,-1.82607986822302,-2.65547545368331));
#67615=CARTESIAN_POINT('Ctrl Pts',(16.5896138302346,-1.82593483778435,-2.65557518033504));
#67616=CARTESIAN_POINT('Ctrl Pts',(16.5896192289933,-1.82586231570136,-2.65562504400514));
#67617=CARTESIAN_POINT('Ctrl Pts',(16.5900599168791,-1.81994246762946,-2.65969496919288));
#67618=CARTESIAN_POINT('Ctrl Pts',(16.5904959396648,-1.81408191918375,-2.66369568529113));
#67619=CARTESIAN_POINT('Ctrl Pts',(16.591504967565,-1.80051223134995,-2.67289350852866));
#67620=CARTESIAN_POINT('Ctrl Pts',(16.5920784966523,-1.79279374769735,-2.67807665657474));
#67621=CARTESIAN_POINT('Ctrl Pts',(16.5938094626318,-1.76948300733419,-2.69358444559813));
#67622=CARTESIAN_POINT('Ctrl Pts',(16.5949707319381,-1.75382341528902,-2.70380670223369));
#67623=CARTESIAN_POINT('Ctrl Pts',(16.6123839859193,-1.51872855643692,-2.85437007948953));
#67624=CARTESIAN_POINT('Ctrl Pts',(16.6296819605777,-1.2832067758928,-2.96770774649493));
#67625=CARTESIAN_POINT('Ctrl Pts',(16.6572047251047,-0.897963175961086,
-3.09858713093773));
#67626=CARTESIAN_POINT('Ctrl Pts',(16.6671559738335,-0.756191328804278,
-3.13620125858548));
#67627=CARTESIAN_POINT('Ctrl Pts',(16.6803723668195,-0.559670177165497,
-3.17423465839397));
#67628=CARTESIAN_POINT('Ctrl Pts',(16.6838747666673,-0.506743431103136,
-3.18311296651785));
#67629=CARTESIAN_POINT('Ctrl Pts',(16.6885824578689,-0.43410785577902,-3.19343955929563));
#67630=CARTESIAN_POINT('Ctrl Pts',(16.6898387962672,-0.41457346000359,-3.19603422049542));
#67631=CARTESIAN_POINT('Ctrl Pts',(16.6919739475725,-0.381094225339752,
-3.20016898380726));
#67632=CARTESIAN_POINT('Ctrl Pts',(16.692857204112,-0.36716110907499,-3.20179747491863));
#67633=CARTESIAN_POINT('Ctrl Pts',(16.6940971675271,-0.347475687395216,
-3.20396809886131));
#67634=CARTESIAN_POINT('Ctrl Pts',(16.6944579947098,-0.341732121548773,
-3.20458579073638));
#67635=CARTESIAN_POINT('Ctrl Pts',(16.695074822161,-0.331887015517989,-3.20561781330294));
#67636=CARTESIAN_POINT('Ctrl Pts',(16.6953312488285,-0.327786298622197,
-3.20603972202199));
#67637=CARTESIAN_POINT('Ctrl Pts',(16.6958228403389,-0.319909419738118,
-3.20683487631056));
#67638=CARTESIAN_POINT('Ctrl Pts',(16.6960580739086,-0.316133409862919,
-3.20720932093361));
#67639=CARTESIAN_POINT('Ctrl Pts',(16.6966160841305,-0.307160224968528,
-3.20808313769721));
#67640=CARTESIAN_POINT('Ctrl Pts',(16.6969385249232,-0.301962460593134,
-3.20857655284675));
#67641=CARTESIAN_POINT('Ctrl Pts',(16.6979044748694,-0.286354080106295,
-3.2100199665271));
#67642=CARTESIAN_POINT('Ctrl Pts',(16.6985458919845,-0.275939895179967,
-3.21093195597616));
#67643=CARTESIAN_POINT('Ctrl Pts',(16.7113012782673,-0.0678953651523029,
-3.22813114898002));
#67644=CARTESIAN_POINT('Ctrl Pts',(16.7224514374401,0.130850733931946,-3.22619652195971));
#67645=CARTESIAN_POINT('Ctrl Pts',(16.7426345563512,0.489757196123863,-3.18945684997258));
#67646=CARTESIAN_POINT('Ctrl Pts',(16.7516572405222,0.649845765068287,-3.16072692886614));
#67647=CARTESIAN_POINT('Ctrl Pts',(16.7674877532071,0.917119915435433,-3.09158984444052));
#67648=CARTESIAN_POINT('Ctrl Pts',(16.774132776632,1.02556697036692,-3.05732644301238));
#67649=CARTESIAN_POINT('Ctrl Pts',(16.782007587846,1.14813590376406,-3.0113451500305));
#67650=CARTESIAN_POINT('Ctrl Pts',(16.7830503796093,1.16425224123502,-3.00515097244806));
#67651=CARTESIAN_POINT('Ctrl Pts',(16.7847265393173,1.18996952152383,-2.99502882916147));
#67652=CARTESIAN_POINT('Ctrl Pts',(16.7853571466778,1.19960276526942,-2.99118343658588));
#67653=CARTESIAN_POINT('Ctrl Pts',(16.7865622845142,1.21793122413258,-2.98376431244321));
#67654=CARTESIAN_POINT('Ctrl Pts',(16.7871365299466,1.22662970818898,-2.98019890191331));
#67655=CARTESIAN_POINT('Ctrl Pts',(16.7881491865587,1.24190691290999,-2.97385873231898));
#67656=CARTESIAN_POINT('Ctrl Pts',(16.7885870486961,1.24849227439157,-2.97110006220009));
#67657=CARTESIAN_POINT('Ctrl Pts',(16.7894464887863,1.26137794841352,-2.96565172631269));
#67658=CARTESIAN_POINT('Ctrl Pts',(16.789868005233,1.2676789628405,-2.96296380952248));
#67659=CARTESIAN_POINT('Ctrl Pts',(16.7909912595639,1.2844194801497,-2.95575938527642));
#67660=CARTESIAN_POINT('Ctrl Pts',(16.7916941982392,1.29484365182372,-2.95120769459627));
#67661=CARTESIAN_POINT('Ctrl Pts',(16.7942180094451,1.3320820077969,-2.93471237707476));
#67662=CARTESIAN_POINT('Ctrl Pts',(16.7960495278954,1.35875618585592,-2.9224579974887));
#67663=CARTESIAN_POINT('Ctrl Pts',(16.7981705747803,1.38923904778023,-2.90794633130796));
#67664=CARTESIAN_POINT('Ctrl Pts',(16.7984478243401,1.39321562963116,-2.90604322175106));
#67665=CARTESIAN_POINT('Ctrl Pts',(16.8161358892818,1.64640819996547,-2.78423137039711));
#67666=CARTESIAN_POINT('Ctrl Pts',(16.8347287356816,1.87911001732313,-2.63277178333459));
#67667=CARTESIAN_POINT('Ctrl Pts',(16.8614757591024,2.18003477909586,-2.37648569884837));
#67668=CARTESIAN_POINT('Ctrl Pts',(16.8694943973193,2.26617002311396,-2.2944961337676));
#67669=CARTESIAN_POINT('Ctrl Pts',(16.8804727589352,2.38049713103802,-2.17293784162986));
#67670=CARTESIAN_POINT('Ctrl Pts',(16.88359864053,2.41262537835953,-2.1372095714432));
#67671=CARTESIAN_POINT('Ctrl Pts',(16.8884369192417,2.46186179003618,-2.07993019144936));
#67672=CARTESIAN_POINT('Ctrl Pts',(16.8901815919505,2.4795124529342,-2.05885676796523));
#67673=CARTESIAN_POINT('Ctrl Pts',(16.8923762140806,2.50161051591836,-2.03177707613838));
#67674=CARTESIAN_POINT('Ctrl Pts',(16.8928434394751,2.50630896560232,-2.02597843819934));
#67675=CARTESIAN_POINT('Ctrl Pts',(16.8935891534087,2.51379879986591,-2.01666885561076));
#67676=CARTESIAN_POINT('Ctrl Pts',(16.8938685583511,2.51660303700085,-2.0131683571283));
#67677=CARTESIAN_POINT('Ctrl Pts',(16.894399299443,2.52192605618841,-2.00649518796544));
#67678=CARTESIAN_POINT('Ctrl Pts',(16.8946507261324,2.52444613381322,-2.00332366077946));
#67679=CARTESIAN_POINT('Ctrl Pts',(16.8952271715592,2.53022011442161,-1.99602888840464));
#67680=CARTESIAN_POINT('Ctrl Pts',(16.8955518951387,2.53346991844349,-1.99190243838388));
#67681=CARTESIAN_POINT('Ctrl Pts',(16.8964161244271,2.5421110088815,-1.98087502614272));
#67682=CARTESIAN_POINT('Ctrl Pts',(16.8969543704657,2.54748432576062,-1.97395994508968));
#67683=CARTESIAN_POINT('Ctrl Pts',(16.9006970477109,2.58478198210128,-1.92555453338215));
#67684=CARTESIAN_POINT('Ctrl Pts',(16.9038355291246,2.61572151822829,-1.88331087098912));
#67685=CARTESIAN_POINT('Ctrl Pts',(16.9206036247207,2.77805219641848,-1.64994758631482));
#67686=CARTESIAN_POINT('Ctrl Pts',(16.9332885187166,2.88956170917061,-1.44580705464937));
#67687=CARTESIAN_POINT('Ctrl Pts',(16.9575267891894,3.05449517460461,-1.04692249901461));
#67688=CARTESIAN_POINT('Ctrl Pts',(16.9689398215512,3.11346845739485,-0.855736560816484));
#67689=CARTESIAN_POINT('Ctrl Pts',(16.9822474294151,3.15865912079881,-0.6398653513746));
#67690=CARTESIAN_POINT('Ctrl Pts',(16.9835157488638,3.16274561271978,-0.619350681485886));
#67691=CARTESIAN_POINT('Ctrl Pts',(16.985376381522,3.16841850936224,-0.589350623475699));
#67692=CARTESIAN_POINT('Ctrl Pts',(16.9859636565608,3.17016267878636,-0.579895330844444));
#67693=CARTESIAN_POINT('Ctrl Pts',(16.9869976991082,3.17315227420335,-0.563271817436396));
#67694=CARTESIAN_POINT('Ctrl Pts',(16.9874438865121,3.17441579262071,-0.556106887011703));
#67695=CARTESIAN_POINT('Ctrl Pts',(16.9883128596609,3.17682508852709,-0.542168891009394));
#67696=CARTESIAN_POINT('Ctrl Pts',(16.9887355590261,3.17797349491455,-0.535396314824354));
#67697=CARTESIAN_POINT('Ctrl Pts',(16.9897487539236,3.18066983177097,-0.519180654185753));
#67698=CARTESIAN_POINT('Ctrl Pts',(16.9903398949484,3.18219736723143,-0.509734286893273));
#67699=CARTESIAN_POINT('Ctrl Pts',(16.9924778336904,3.18755743055467,-0.475623997131077));
#67700=CARTESIAN_POINT('Ctrl Pts',(16.9940323649592,3.19114539014042,-0.450923055724328));
#67701=CARTESIAN_POINT('Ctrl Pts',(16.9963249230625,3.19598463621889,-0.414650626003227));
#67702=CARTESIAN_POINT('Ctrl Pts',(16.9970558038624,3.19746079580874,-0.403109650266346));
#67703=CARTESIAN_POINT('Ctrl Pts',(17.0139876568164,3.23012185742507,-0.136283741417817));
#67704=CARTESIAN_POINT('Ctrl Pts',(17.0311949611847,3.23069377974112,0.121767434515482));
#67705=CARTESIAN_POINT('Ctrl Pts',(17.061322455295,3.17861375631521,0.563810703728457));
#67706=CARTESIAN_POINT('Ctrl Pts',(17.0740619293645,3.14031391012763,0.748271657561799));
#67707=CARTESIAN_POINT('Ctrl Pts',(17.0876849085203,3.07893068489434,0.952328818867472));
#67708=CARTESIAN_POINT('Ctrl Pts',(17.0892719388212,3.07143948521891,0.976219197871528));
#67709=CARTESIAN_POINT('Ctrl Pts',(17.0912966405999,3.06142989123675,1.00688465927331));
#67710=CARTESIAN_POINT('Ctrl Pts',(17.0917485395012,3.05916632499223,1.01374113779552));
#67711=CARTESIAN_POINT('Ctrl Pts',(17.0924755768789,3.05547651792626,1.02479287848273));
#67712=CARTESIAN_POINT('Ctrl Pts',(17.0927515534256,3.05406465063036,1.02899285989948));
#67713=CARTESIAN_POINT('Ctrl Pts',(17.0932798781394,3.05134008239275,1.03704281937484));
#67714=CARTESIAN_POINT('Ctrl Pts',(17.0935323031022,3.05002875780627,1.0408932146617));
#67715=CARTESIAN_POINT('Ctrl Pts',(17.0941165369165,3.04697158040114,1.04981451335244));
#67716=CARTESIAN_POINT('Ctrl Pts',(17.0944480259587,3.04522034503873,1.05488358379804));
#67717=CARTESIAN_POINT('Ctrl Pts',(17.0955190451632,3.03950865609358,1.07128370115698));
#67718=CARTESIAN_POINT('Ctrl Pts',(17.0962556210477,3.03549749315963,1.08259716349494));
#67719=CARTESIAN_POINT('Ctrl Pts',(17.1057476315043,2.98274381406795,1.22879010151195));
#67720=CARTESIAN_POINT('Ctrl Pts',(17.1140021921056,2.92510673743358,1.36031157830405));
#67721=CARTESIAN_POINT('Ctrl Pts',(17.1243731128257,2.8403807253697,1.52314243035026));
#67722=CARTESIAN_POINT('Ctrl Pts',(17.1266258691787,2.82120889966688,1.55836643903213));
#67723=CARTESIAN_POINT('Ctrl Pts',(17.1408324359696,2.69586295771963,1.77876369311601));
#67724=CARTESIAN_POINT('Ctrl Pts',(17.1526309064463,2.57217792746988,1.95334893858489));
#67725=CARTESIAN_POINT('Ctrl Pts',(17.1703307977481,2.37244900266836,2.18309005397934));
#67726=CARTESIAN_POINT('Ctrl Pts',(17.1757172272911,2.30987577937546,2.24919274636321));
#67727=CARTESIAN_POINT('Ctrl Pts',(17.1822011779251,2.23304559841401,2.32376503428086));
#67728=CARTESIAN_POINT('Ctrl Pts',(17.1831795005784,2.22141335862531,2.33488741798036));
#67729=CARTESIAN_POINT('Ctrl Pts',(17.1846893319437,2.20340342271436,2.35185154839321));
#67730=CARTESIAN_POINT('Ctrl Pts',(17.185218148771,2.19708459330411,2.35775563544508));
#67731=CARTESIAN_POINT('Ctrl Pts',(17.1861836763199,2.18552823061081,2.36846668830334));
#67732=CARTESIAN_POINT('Ctrl Pts',(17.1866200299798,2.1802983940587,2.37328190739672));
#67733=CARTESIAN_POINT('Ctrl Pts',(17.1875726947395,2.16886517728149,2.38373902053944));
#67734=CARTESIAN_POINT('Ctrl Pts',(17.1880892917213,2.16265563699862,2.3893740747106));
#67735=CARTESIAN_POINT('Ctrl Pts',(17.1895012111658,2.14565839384658,2.40467824992613));
#67736=CARTESIAN_POINT('Ctrl Pts',(17.1903985651119,2.1348274720379,2.41429888008091));
#67737=CARTESIAN_POINT('Ctrl Pts',(17.1948030728425,2.08153279899714,2.46099915322595));
#67738=CARTESIAN_POINT('Ctrl Pts',(17.1983532666532,2.03816818752887,2.49703132074851));
#67739=CARTESIAN_POINT('Ctrl Pts',(17.2025512209128,1.98645892302093,2.53775251143482));
#67740=CARTESIAN_POINT('Ctrl Pts',(17.203155178146,1.97900917220977,2.54356630648374));
#67741=CARTESIAN_POINT('Ctrl Pts',(17.2052627443095,1.95297666163645,2.56369851136851));
#67742=CARTESIAN_POINT('Ctrl Pts',(17.2067726140065,1.93426354186359,2.57784646640258));
#67743=CARTESIAN_POINT('Ctrl Pts',(17.2116091374084,1.87411874636929,2.62229500740112));
#67744=CARTESIAN_POINT('Ctrl Pts',(17.2149624125329,1.83211947298785,2.65180876073935));
#67745=CARTESIAN_POINT('Ctrl Pts',(17.218344821656,1.78943620926209,2.68030513477136));
#67746=CARTESIAN_POINT('Origin',(-1.72497344927317,0.,0.));
#67747=CARTESIAN_POINT('',(18.7170794495574,1.78943621037806,2.68030513402632));
#67748=CARTESIAN_POINT('',(18.4731355395702,1.78943620771753,2.68030513580255));
#67749=CARTESIAN_POINT('',(-1.72497344927317,1.78943621037804,2.68030513402633));
#67750=CARTESIAN_POINT('',(17.8965734493264,-3.22274931384398,0.00210300217175629));
#67751=CARTESIAN_POINT('Ctrl Pts',(17.8965734493264,-3.22274931384398,0.002103002171752));
#67752=CARTESIAN_POINT('Ctrl Pts',(17.9026568563018,-3.22281334652089,-0.0960239842600718));
#67753=CARTESIAN_POINT('Ctrl Pts',(17.9087402632772,-3.21839149416545,-0.194328558742725));
#67754=CARTESIAN_POINT('Ctrl Pts',(17.9148236702526,-3.20946154458654,-0.292359635244282));
#67755=CARTESIAN_POINT('Ctrl Pts',(17.9208998680669,-3.2005421774732,-0.390274539702337));
#67756=CARTESIAN_POINT('Ctrl Pts',(17.9269760658813,-3.1871253663105,-0.487916147950806));
#67757=CARTESIAN_POINT('Ctrl Pts',(17.9330522636956,-3.16924092933091,-0.584832877285252));
#67758=CARTESIAN_POINT('Ctrl Pts',(17.9391231590748,-3.15137209932627,-0.681665031580054));
#67759=CARTESIAN_POINT('Ctrl Pts',(17.945194054454,-3.12904347202547,-0.777773125995886));
#67760=CARTESIAN_POINT('Ctrl Pts',(17.9512649498332,-3.10233661305032,-0.872711350807052));
#67761=CARTESIAN_POINT('Ctrl Pts',(17.9573330655231,-3.07564198238142,-0.967606106122657));
#67762=CARTESIAN_POINT('Ctrl Pts',(17.9634011812131,-3.04457322120995,-1.06133162549463));
#67763=CARTESIAN_POINT('Ctrl Pts',(17.9694692969031,-3.00926263391265,-1.15345392740113));
#67764=CARTESIAN_POINT('Ctrl Pts',(17.9755363610955,-2.97395816531805,-1.24556026613567));
#67765=CARTESIAN_POINT('Ctrl Pts',(17.9816034252879,-2.93441349103862,-1.33606352173451));
#67766=CARTESIAN_POINT('Ctrl Pts',(17.9876704894804,-2.89080986879401,-1.42454760011141));
#67767=CARTESIAN_POINT('Ctrl Pts',(17.99373822901,-2.84720139294191,-1.51304152783025));
#67768=CARTESIAN_POINT('Ctrl Pts',(17.9998059685396,-2.79953327099698,-1.5995154313789));
#67769=CARTESIAN_POINT('Ctrl Pts',(18.0058737080692,-2.74803318804049,-1.68357689456942));
#67770=CARTESIAN_POINT('Ctrl Pts',(18.0119476112746,-2.6964807907403,-1.7677237483074));
#67771=CARTESIAN_POINT('Ctrl Pts',(18.01802151448,-2.64108889635926,-1.84945288785606));
#67772=CARTESIAN_POINT('Ctrl Pts',(18.0240954176853,-2.58212890738195,-1.92840033918336));
#67773=CARTESIAN_POINT('Ctrl Pts',(18.03017265551,-2.52313654891948,-2.00739113326562));
#67774=CARTESIAN_POINT('Ctrl Pts',(18.0362498933347,-2.46057248211144,-2.08359685528342));
#67775=CARTESIAN_POINT('Ctrl Pts',(18.0423271311594,-2.3947474046535,-2.15668783796018));
#67776=CARTESIAN_POINT('Ctrl Pts',(18.0484141616522,-2.32881625875608,-2.22989659712535));
#67777=CARTESIAN_POINT('Ctrl Pts',(18.0545011921449,-2.25961392689952,-2.29998028044469));
#67778=CARTESIAN_POINT('Ctrl Pts',(18.0605882226376,-2.18748671269529,-2.36664730035584));
#67779=CARTESIAN_POINT('Ctrl Pts',(18.0643877010504,-2.14246545090453,-2.40826035015047));
#67780=CARTESIAN_POINT('Ctrl Pts',(18.0681871794632,-2.09630526690075,-2.44854301873974));
#67781=CARTESIAN_POINT('Ctrl Pts',(18.071986657876,-2.04909615611315,-2.48743291477425));
#67782=CARTESIAN_POINT('Ctrl Pts',(18.0781589059687,-1.972405012655,-2.55060950391345));
#67783=CARTESIAN_POINT('Ctrl Pts',(18.0843311540615,-1.89265440894733,-2.61034721978994));
#67784=CARTESIAN_POINT('Ctrl Pts',(18.0905034021542,-1.81018580212359,-2.66633548607263));
#67785=CARTESIAN_POINT('Ctrl Pts',(18.0966672908069,-1.72782888740473,-2.72224792413959));
#67786=CARTESIAN_POINT('Ctrl Pts',(18.1028311794595,-1.6427616424801,-2.77442076406159));
#67787=CARTESIAN_POINT('Ctrl Pts',(18.1089950681121,-1.55535906571456,-2.82258316780915));
#67788=CARTESIAN_POINT('Ctrl Pts',(18.1151524297707,-1.46804904028062,-2.87069457197792));
#67789=CARTESIAN_POINT('Ctrl Pts',(18.1213097914292,-1.37840897771133,-2.91480377430139));
#67790=CARTESIAN_POINT('Ctrl Pts',(18.1274671530877,-1.28684256276156,-2.95468336394363));
#67791=CARTESIAN_POINT('Ctrl Pts',(18.133620017234,-1.19534303052784,-2.99453382439838));
#67792=CARTESIAN_POINT('Ctrl Pts',(18.1397728813803,-1.10192034043838,-3.03016064156325));
#67793=CARTESIAN_POINT('Ctrl Pts',(18.1459257455266,-1.00700164596564,-3.06138289789476));
#67794=CARTESIAN_POINT('Ctrl Pts',(18.1520762786632,-0.912118911396808,
-3.09259332568876));
#67795=CARTESIAN_POINT('Ctrl Pts',(18.1582268117997,-0.815741710762389,
-3.11940237270234));
#67796=CARTESIAN_POINT('Ctrl Pts',(18.1643773449362,-0.718315155376485,
-3.14167803889203));
#67797=CARTESIAN_POINT('Ctrl Pts',(18.1705271931515,-0.62089944937957,-3.16395122447089));
#67798=CARTESIAN_POINT('Ctrl Pts',(18.1766770413667,-0.522435044406073,
-3.18169193609567));
#67799=CARTESIAN_POINT('Ctrl Pts',(18.1828268895819,-0.423379137392556,
-3.19481887882877));
#67800=CARTESIAN_POINT('Ctrl Pts',(18.188977697961,-0.324307764971698,-3.20794787104608));
#67801=CARTESIAN_POINT('Ctrl Pts',(18.1951285063401,-0.224645137730853,
-3.21646160652262));
#67802=CARTESIAN_POINT('Ctrl Pts',(18.2012793147192,-0.124854492697445,
-3.22033056038557));
#67803=CARTESIAN_POINT('Ctrl Pts',(18.2074367010854,-0.0249571264768749,
-3.22420365190441));
#67804=CARTESIAN_POINT('Ctrl Pts',(18.2135940874516,0.075068096033463,-3.22342202563264));
#67805=CARTESIAN_POINT('Ctrl Pts',(18.2197514738178,0.174757130536443,-3.21800831382187));
#67806=CARTESIAN_POINT('Ctrl Pts',(18.2259122965547,0.274501800412089,-3.21259158067705));
#67807=CARTESIAN_POINT('Ctrl Pts',(18.2320731192917,0.373909476447318,-3.20253765747931));
#67808=CARTESIAN_POINT('Ctrl Pts',(18.2382339420287,0.472522526797308,-3.18792095638664));
#67809=CARTESIAN_POINT('Ctrl Pts',(18.2444050649454,0.571300446708627,-3.1732798178682));
#67810=CARTESIAN_POINT('Ctrl Pts',(18.2505761878621,0.66928066080252,-3.15406074754169));
#67811=CARTESIAN_POINT('Ctrl Pts',(18.2567473107787,0.766016855504997,-3.13038907159833));
#67812=CARTESIAN_POINT('Ctrl Pts',(18.2614428327244,0.839622086075572,-3.11237762127033));
#67813=CARTESIAN_POINT('Ctrl Pts',(18.26613835467,0.912507329936493,-3.09178940003567));
#67814=CARTESIAN_POINT('Ctrl Pts',(18.2708338766156,0.98448346849884,-3.06869839879264));
#67815=CARTESIAN_POINT('Ctrl Pts',(18.2770061247084,1.07909586497143,-3.03834535390593));
#67816=CARTESIAN_POINT('Ctrl Pts',(18.2831783728012,1.1724697320842,-3.0035592298004));
#67817=CARTESIAN_POINT('Ctrl Pts',(18.2893506208939,1.26415918089062,-2.96445933145826));
#67818=CARTESIAN_POINT('Ctrl Pts',(18.2955145095465,1.35572444926094,-2.92541238841785));
#67819=CARTESIAN_POINT('Ctrl Pts',(18.3016783981991,1.44560943763035,-2.88206345244063));
#67820=CARTESIAN_POINT('Ctrl Pts',(18.3078422868518,1.53338354917857,-2.83458153059822));
#67821=CARTESIAN_POINT('Ctrl Pts',(18.3139996485103,1.6210647159745,-2.78714988776617));
#67822=CARTESIAN_POINT('Ctrl Pts',(18.3201570101689,1.70663906983877,-2.73559416540845));
#67823=CARTESIAN_POINT('Ctrl Pts',(18.3263143718274,1.78969703426868,-2.68013098337187));
#67824=CARTESIAN_POINT('Ctrl Pts',(18.3324672359738,1.87269433079679,-2.62470831322245));
#67825=CARTESIAN_POINT('Ctrl Pts',(18.3386201001201,1.95317853208352,-2.56538409836791));
#67826=CARTESIAN_POINT('Ctrl Pts',(18.3447729642664,2.0307664824223,-2.50241984014876));
#67827=CARTESIAN_POINT('Ctrl Pts',(18.3509234974029,2.10832503860151,-2.4394794359101));
#67828=CARTESIAN_POINT('Ctrl Pts',(18.3570740305394,2.18298918713755,-2.37290200184059));
#67829=CARTESIAN_POINT('Ctrl Pts',(18.363224563676,2.25440721217204,-2.30299059577036));
#67830=CARTESIAN_POINT('Ctrl Pts',(18.3693744118912,2.32581728411885,-2.23308697501121));
#67831=CARTESIAN_POINT('Ctrl Pts',(18.3755242601064,2.39398164084689,-2.15985042424882));
#67832=CARTESIAN_POINT('Ctrl Pts',(18.3816741083216,2.45858468526504,-2.0836215846166));
#67833=CARTESIAN_POINT('Ctrl Pts',(18.3878249167007,2.52319781603173,-2.0073808435229));
#67834=CARTESIAN_POINT('Ctrl Pts',(18.3939757250798,2.58424824922221,-1.92814721702782));
#67835=CARTESIAN_POINT('Ctrl Pts',(18.4001265334589,2.64146067124637,-1.84629441984713));
#67836=CARTESIAN_POINT('Ctrl Pts',(18.4062839198251,2.69873427914218,-1.76435408512538));
#67837=CARTESIAN_POINT('Ctrl Pts',(18.4124413061913,2.75216143014478,-1.67978934298297));
#67838=CARTESIAN_POINT('Ctrl Pts',(18.4185986925575,2.80151024920306,-1.59300278910937));
#67839=CARTESIAN_POINT('Ctrl Pts',(18.4247595152944,2.85088660930384,-1.50616780059813));
#67840=CARTESIAN_POINT('Ctrl Pts',(18.4309203380314,2.89617990777551,-1.4171089181667));
#67841=CARTESIAN_POINT('Ctrl Pts',(18.4370811607683,2.9372052945644,-1.32625134121811));
#67842=CARTESIAN_POINT('Ctrl Pts',(18.443252283685,2.97829927103286,-1.23524186095851));
#67843=CARTESIAN_POINT('Ctrl Pts',(18.4494234066017,3.01511092275271,-1.14242808334039));
#67844=CARTESIAN_POINT('Ctrl Pts',(18.4555945295184,3.04750434891383,-1.04825321647552));
#67845=CARTESIAN_POINT('Ctrl Pts',(18.460290051464,3.07215205816974,-0.976596864777705));
#67846=CARTESIAN_POINT('Ctrl Pts',(18.4649855734096,3.0942428605833,-0.904152885904801));
#67847=CARTESIAN_POINT('Ctrl Pts',(18.4696810953552,3.11373673960027,-0.831120375735952));
#67848=CARTESIAN_POINT('Ctrl Pts',(18.475853343448,3.1393613791988,-0.735119382274197));
#67849=CARTESIAN_POINT('Ctrl Pts',(18.4820255915408,3.16058718753498,-0.637763239425528));
#67850=CARTESIAN_POINT('Ctrl Pts',(18.4881978396335,3.17727342830439,-0.539491542371941));
#67851=CARTESIAN_POINT('Ctrl Pts',(18.4943617282861,3.19393706991237,-0.441352940482053));
#67852=CARTESIAN_POINT('Ctrl Pts',(18.5005256169388,3.20607329211211,-0.342301673477271));
#67853=CARTESIAN_POINT('Ctrl Pts',(18.5066895055914,3.21359143704915,-0.242791347095304));
#67854=CARTESIAN_POINT('Ctrl Pts',(18.5128468672499,3.22110162095865,-0.14338639304334));
#67855=CARTESIAN_POINT('Ctrl Pts',(18.5190042289085,3.22400341708432,-0.0435237767830685));
#67856=CARTESIAN_POINT('Ctrl Pts',(18.525161590567,3.22225758576355,0.0563348337112121));
#67857=CARTESIAN_POINT('Ctrl Pts',(18.5313144547133,3.22051302964767,0.156120504633599));
#67858=CARTESIAN_POINT('Ctrl Pts',(18.5374673188597,3.21412760301785,0.255901742607642));
#67859=CARTESIAN_POINT('Ctrl Pts',(18.543620183006,3.20311410691901,0.355214837185091));
#67860=CARTESIAN_POINT('Ctrl Pts',(18.5497707161425,3.19210478327815,0.454490307041912));
#67861=CARTESIAN_POINT('Ctrl Pts',(18.555921249279,3.17647092187352,0.553297554657986));
#67862=CARTESIAN_POINT('Ctrl Pts',(18.5620717824156,3.1562772812874,0.651176847046182));
#67863=CARTESIAN_POINT('Ctrl Pts',(18.5682216306308,3.13608588945837,0.749045239628971));
#67864=CARTESIAN_POINT('Ctrl Pts',(18.574371478846,3.11133581574808,0.845985457016277));
#67865=CARTESIAN_POINT('Ctrl Pts',(18.5805213270612,3.08214296393584,0.941547827973059));
#67866=CARTESIAN_POINT('Ctrl Pts',(18.5866721354403,3.05294555430002,1.03712511889828));
#67867=CARTESIAN_POINT('Ctrl Pts',(18.5928229438194,3.01930411572692,1.13132372064531));
#67868=CARTESIAN_POINT('Ctrl Pts',(18.5989737521986,2.98138415548961,1.22370996559459));
#67869=CARTESIAN_POINT('Ctrl Pts',(18.6051311385648,2.94342364171983,1.31619501308906));
#67870=CARTESIAN_POINT('Ctrl Pts',(18.6112885249309,2.90117563440664,1.40686343072131));
#67871=CARTESIAN_POINT('Ctrl Pts',(18.6174459112971,2.85485342341849,1.49530247551983));
#67872=CARTESIAN_POINT('Ctrl Pts',(18.6236067340341,2.8085053605051,1.58379087719327));
#67873=CARTESIAN_POINT('Ctrl Pts',(18.629767556771,2.75807878497181,1.67004705324089));
#67874=CARTESIAN_POINT('Ctrl Pts',(18.635928379508,2.70383142802998,1.75368559647885));
#67875=CARTESIAN_POINT('Ctrl Pts',(18.6420995024247,2.64949337581088,1.8374639736423));
#67876=CARTESIAN_POINT('Ctrl Pts',(18.6482706253414,2.59132203573088,1.91861562311033));
#67877=CARTESIAN_POINT('Ctrl Pts',(18.6544417482581,2.52961675544487,1.99678657674589));
#67878=CARTESIAN_POINT('Ctrl Pts',(18.6591372702037,2.48266606240976,2.05626577255204));
#67879=CARTESIAN_POINT('Ctrl Pts',(18.6638327921493,2.4336702646636,2.11401995360804));
#67880=CARTESIAN_POINT('Ctrl Pts',(18.6685283140949,2.38277520607407,2.1699078044513));
#67881=CARTESIAN_POINT('Ctrl Pts',(18.6747006593625,2.31587276633024,2.24337335645331));
#67882=CARTESIAN_POINT('Ctrl Pts',(18.6808730046302,2.24545175883948,2.31387122200969));
#67883=CARTESIAN_POINT('Ctrl Pts',(18.6870453498979,2.1718058916275,2.38104530229731));
#67884=CARTESIAN_POINT('Ctrl Pts',(18.6932084687882,2.09827010972772,2.44811897125324));
#67885=CARTESIAN_POINT('Ctrl Pts',(18.6993715876786,2.021519372625,2.51187844534637));
#67886=CARTESIAN_POINT('Ctrl Pts',(18.705534706569,1.94188611155576,2.57200231186654));
#67887=CARTESIAN_POINT('Ctrl Pts',(18.7093829542318,1.89216315208627,2.60954361732096));
#67888=CARTESIAN_POINT('Ctrl Pts',(18.7132312018946,1.84131715179318,2.64566816899642));
#67889=CARTESIAN_POINT('Ctrl Pts',(18.7170794495574,1.78943621037806,2.68030513402632));
#67890=CARTESIAN_POINT('Ctrl Pts',(17.4669156580687,1.78943621037803,2.68030513402633));
#67891=CARTESIAN_POINT('Ctrl Pts',(17.4697587725981,1.75131203222926,2.70575775283613));
#67892=CARTESIAN_POINT('Ctrl Pts',(17.4726018871276,1.7126728546953,2.73037800620175));
#67893=CARTESIAN_POINT('Ctrl Pts',(17.475445001657,1.67355890093987,2.75414563296586));
#67894=CARTESIAN_POINT('Ctrl Pts',(17.4816172497498,1.58864461979969,2.80574386703093));
#67895=CARTESIAN_POINT('Ctrl Pts',(17.4877894978425,1.50119237257124,2.85350219556718));
#67896=CARTESIAN_POINT('Ctrl Pts',(17.4939617459353,1.41158440453206,2.89716189250478));
#67897=CARTESIAN_POINT('Ctrl Pts',(17.5001256345879,1.32209779785631,2.94076245853624));
#67898=CARTESIAN_POINT('Ctrl Pts',(17.5062895232406,1.23046166048895,2.98027523764615));
#67899=CARTESIAN_POINT('Ctrl Pts',(17.5124534118932,1.13708577126703,3.01548561782046));
#67900=CARTESIAN_POINT('Ctrl Pts',(17.5186107735517,1.04380875856788,3.05065871342394));
#67901=CARTESIAN_POINT('Ctrl Pts',(17.5247681352103,0.948796060755513,3.08153831512958));
#67902=CARTESIAN_POINT('Ctrl Pts',(17.5309254968688,0.852479659083573,3.1079568840878));
#67903=CARTESIAN_POINT('Ctrl Pts',(17.5370783610152,0.756233609653304,3.13435615617118));
#67904=CARTESIAN_POINT('Ctrl Pts',(17.5432312251615,0.658686167264141,3.15630075933928));
#67905=CARTESIAN_POINT('Ctrl Pts',(17.5493840893078,0.560285914103534,3.17367251885842));
#67906=CARTESIAN_POINT('Ctrl Pts',(17.5555346224443,0.461922939833879,3.19103769709441));
#67907=CARTESIAN_POINT('Ctrl Pts',(17.5616851555809,0.362708224050383,3.20383339855629));
#67908=CARTESIAN_POINT('Ctrl Pts',(17.5678356887174,0.26310114969074,3.21199242644366));
#67909=CARTESIAN_POINT('Ctrl Pts',(17.5739855369326,0.163505167541867,3.22015054574438));
#67910=CARTESIAN_POINT('Ctrl Pts',(17.5801353851478,0.063517346610522,3.22367298256498));
#67911=CARTESIAN_POINT('Ctrl Pts',(17.586285233363,-0.036398196497658,3.22254445024296));
#67912=CARTESIAN_POINT('Ctrl Pts',(17.5924360417421,-0.136329339226623,
3.22141574172538));
#67913=CARTESIAN_POINT('Ctrl Pts',(17.5985868501213,-0.236187747329852,
3.21563462665637));
#67914=CARTESIAN_POINT('Ctrl Pts',(17.6047376585004,-0.335510706137782,
3.20523792074269));
#67915=CARTESIAN_POINT('Ctrl Pts',(17.6108950448666,-0.434939885965303,
3.19483009606336));
#67916=CARTESIAN_POINT('Ctrl Pts',(17.6170524312328,-0.533832040144026,
3.17979686887251));
#67917=CARTESIAN_POINT('Ctrl Pts',(17.623209817599,-0.631731090493708,3.16022679436202));
#67918=CARTESIAN_POINT('Ctrl Pts',(17.6293706403359,-0.729684777245112,
3.1406457980045));
#67919=CARTESIAN_POINT('Ctrl Pts',(17.6355314630729,-0.826643834866129,
3.11652301682949));
#67920=CARTESIAN_POINT('Ctrl Pts',(17.6416922858098,-0.92216591387072,3.08799734290608));
#67921=CARTESIAN_POINT('Ctrl Pts',(17.6478634087265,-1.01784769469178,3.05942397737054));
#67922=CARTESIAN_POINT('Ctrl Pts',(17.6540345316432,-1.11208728788402,3.02643315905609));
#67923=CARTESIAN_POINT('Ctrl Pts',(17.6602056545599,-1.20446080492819,2.98921256050682));
#67924=CARTESIAN_POINT('Ctrl Pts',(17.6649011765055,-1.27474653449925,2.96089192264634));
#67925=CARTESIAN_POINT('Ctrl Pts',(17.6695966984511,-1.34395228700999,2.9301234737808));
#67926=CARTESIAN_POINT('Ctrl Pts',(17.6742922203967,-1.41190142362904,2.89700740980314));
#67927=CARTESIAN_POINT('Ctrl Pts',(17.6804644684894,-1.50122033934532,2.85347645305443));
#67928=CARTESIAN_POINT('Ctrl Pts',(17.6866367165822,-1.588681396552,2.8057342603715));
#67929=CARTESIAN_POINT('Ctrl Pts',(17.692808964675,-1.67386026863737,2.75396248405407));
#67930=CARTESIAN_POINT('Ctrl Pts',(17.6989728533276,-1.75892377794558,2.70226082531096));
#67931=CARTESIAN_POINT('Ctrl Pts',(17.7051367419802,-1.84171087771072,2.6465406539447));
#67932=CARTESIAN_POINT('Ctrl Pts',(17.7113006306329,-1.92181946278051,2.58703063665238));
#67933=CARTESIAN_POINT('Ctrl Pts',(17.7174579922914,-2.00184322018855,2.52758363502328));
#67934=CARTESIAN_POINT('Ctrl Pts',(17.72361535395,-2.0791937549697,2.46435502349232));
#67935=CARTESIAN_POINT('Ctrl Pts',(17.7297727156085,-2.15349655526324,2.39761759856933));
#67936=CARTESIAN_POINT('Ctrl Pts',(17.7359255797548,-2.2277450826763,2.33092892056129));
#67937=CARTESIAN_POINT('Ctrl Pts',(17.7420784439011,-2.29894997938641,2.26073681410068));
#67938=CARTESIAN_POINT('Ctrl Pts',(17.7482313080474,-2.36676928277229,2.18735473223379));
#67939=CARTESIAN_POINT('Ctrl Pts',(17.754381841184,-2.43456289284608,2.11400045113507));
#67940=CARTESIAN_POINT('Ctrl Pts',(17.7605323743205,-2.49897316368225,2.03745891460282));
#67941=CARTESIAN_POINT('Ctrl Pts',(17.766682907457,-2.55969517567515,1.95808022566118));
#67942=CARTESIAN_POINT('Ctrl Pts',(17.7728327556722,-2.62041042568495,1.87871037630401));
#67943=CARTESIAN_POINT('Ctrl Pts',(17.7789826038874,-2.67743796951116,1.79650434768742));
#67944=CARTESIAN_POINT('Ctrl Pts',(17.7851324521027,-2.73051399527618,1.71184429318233));
#67945=CARTESIAN_POINT('Ctrl Pts',(17.7912832604818,-2.78359830769865,1.62717102086636));
#67946=CARTESIAN_POINT('Ctrl Pts',(17.7974340688609,-2.83272964590099,1.54004332970663));
#67947=CARTESIAN_POINT('Ctrl Pts',(17.8035848772401,-2.87768878502424,1.45087036603747));
#67948=CARTESIAN_POINT('Ctrl Pts',(17.8097422636063,-2.92269600573557,1.36160203626944));
#67949=CARTESIAN_POINT('Ctrl Pts',(17.8158996499724,-2.96352192135572,1.27028445476588));
#67950=CARTESIAN_POINT('Ctrl Pts',(17.8220570363386,-2.99999441915956,1.17734916125654));
#67951=CARTESIAN_POINT('Ctrl Pts',(17.8282178590756,-3.03648727187019,1.08436200156448));
#67952=CARTESIAN_POINT('Ctrl Pts',(17.8343786818125,-3.06862172855124,0.989755743208075));
#67953=CARTESIAN_POINT('Ctrl Pts',(17.8405395045495,-3.09627544355293,0.893977594882056));
#67954=CARTESIAN_POINT('Ctrl Pts',(17.8467106274662,-3.12397539235274,0.798039316621462));
#67955=CARTESIAN_POINT('Ctrl Pts',(17.8528817503829,-3.14717953487941,0.700925657501339));
#67956=CARTESIAN_POINT('Ctrl Pts',(17.8590528732996,-3.16581654208732,0.603094672788866));
#67957=CARTESIAN_POINT('Ctrl Pts',(17.8637483952451,-3.17999718271397,0.52865643166556));
#67958=CARTESIAN_POINT('Ctrl Pts',(17.8684439171907,-3.19153474824845,0.453803120398392));
#67959=CARTESIAN_POINT('Ctrl Pts',(17.8731394391363,-3.20041801394429,0.378737506092117));
#67960=CARTESIAN_POINT('Ctrl Pts',(17.8809507758485,-3.21519596201036,0.253860485889424));
#67961=CARTESIAN_POINT('Ctrl Pts',(17.8887621125608,-3.22266709330376,0.128101959648026));
#67962=CARTESIAN_POINT('Ctrl Pts',(17.8965734492731,-3.22274931384342,0.00210300303191614));
#67963=CARTESIAN_POINT('Ctrl Pts',(17.218344821656,1.78943620926209,2.68030513477136));
#67964=CARTESIAN_POINT('Ctrl Pts',(17.218996255307,1.78121564418187,2.68579338184603));
#67965=CARTESIAN_POINT('Ctrl Pts',(17.2196487630733,1.77296970763706,2.69124389172866));
#67966=CARTESIAN_POINT('Ctrl Pts',(17.236471424427,1.56006568899324,2.83056880659984));
#67967=CARTESIAN_POINT('Ctrl Pts',(17.2532926280998,1.34087819022421,2.94074052014517));
#67968=CARTESIAN_POINT('Ctrl Pts',(17.2740174238738,1.0484075159506,3.04818902544994));
#67969=CARTESIAN_POINT('Ctrl Pts',(17.2784255491868,0.984749776020059,3.06934581850393));
#67970=CARTESIAN_POINT('Ctrl Pts',(17.2849851458498,0.887141057238322,3.0984363953252));
#67971=CARTESIAN_POINT('Ctrl Pts',(17.2872009426343,0.853647615099221,3.10783097013015));
#67972=CARTESIAN_POINT('Ctrl Pts',(17.2898945850584,0.812197532181473,3.11873659378563));
#67973=CARTESIAN_POINT('Ctrl Pts',(17.2904004797907,0.804380230094272,3.12076196167777));
#67974=CARTESIAN_POINT('Ctrl Pts',(17.2911932523726,0.79207725323583,3.12390021368537));
#67975=CARTESIAN_POINT('Ctrl Pts',(17.2914812564977,0.787596722164427,3.12503285167271));
#67976=CARTESIAN_POINT('Ctrl Pts',(17.2920189834721,0.779210243314774,3.12713369599776));
#67977=CARTESIAN_POINT('Ctrl Pts',(17.2922688353303,0.775304960996747,3.12810421399642));
#67978=CARTESIAN_POINT('Ctrl Pts',(17.2928349951901,0.766436372916174,3.13029055529922));
#67979=CARTESIAN_POINT('Ctrl Pts',(17.2931510407565,0.761471999657033,3.1315018871014));
#67980=CARTESIAN_POINT('Ctrl Pts',(17.29410737286,0.746409457751866,3.13513928582453));
#67981=CARTESIAN_POINT('Ctrl Pts',(17.29474555719,0.736302303227153,3.13752838159355));
#67982=CARTESIAN_POINT('Ctrl Pts',(17.2994078367798,0.662073595017321,3.15469587434005));
#67983=CARTESIAN_POINT('Ctrl Pts',(17.303327763258,0.597519209537753,3.1675573717906));
#67984=CARTESIAN_POINT('Ctrl Pts',(17.3106504595164,0.474009369588108,3.18825395626274));
#67985=CARTESIAN_POINT('Ctrl Pts',(17.3140650369906,0.41514433878044,3.19645178341192));
#67986=CARTESIAN_POINT('Ctrl Pts',(17.3254168135382,0.216768991329332,3.21850543603342));
#67987=CARTESIAN_POINT('Ctrl Pts',(17.3331875647572,0.0765881523064569,
3.22488802704263));
#67988=CARTESIAN_POINT('Ctrl Pts',(17.3530210348043,-0.277439556604902,
3.21790371907984));
#67989=CARTESIAN_POINT('Ctrl Pts',(17.3651732031636,-0.490328704767302,
3.19240293092688));
#67990=CARTESIAN_POINT('Ctrl Pts',(17.3794578096054,-0.721809880852266,
3.14096305293035));
#67991=CARTESIAN_POINT('Ctrl Pts',(17.380866369542,-0.744456347208361,3.13567267224105));
#67992=CARTESIAN_POINT('Ctrl Pts',(17.3828942238259,-0.776792857861574,
3.12774858067602));
#67993=CARTESIAN_POINT('Ctrl Pts',(17.3835070945248,-0.786531285234542,
3.12531388210939));
#67994=CARTESIAN_POINT('Ctrl Pts',(17.3845710019956,-0.803376015042545,
3.1210188239924));
#67995=CARTESIAN_POINT('Ctrl Pts',(17.3850213521265,-0.810487663876386,
3.11917958228552));
#67996=CARTESIAN_POINT('Ctrl Pts',(17.3858875844682,-0.824130441794685,
3.11560142774978));
#67997=CARTESIAN_POINT('Ctrl Pts',(17.3863033433176,-0.830662517449225,
3.11386624996699));
#67998=CARTESIAN_POINT('Ctrl Pts',(17.3872830738975,-0.846017478948949,
3.10973561084354));
#67999=CARTESIAN_POINT('Ctrl Pts',(17.3878475966572,-0.854835691112436,
3.10732313776235));
#68000=CARTESIAN_POINT('Ctrl Pts',(17.3895174142792,-0.880831918339204,
3.10009209486116));
#68001=CARTESIAN_POINT('Ctrl Pts',(17.3906261259373,-0.897980105891992,
3.09516842413682));
#68002=CARTESIAN_POINT('Ctrl Pts',(17.402967686621,-1.08759881269832,3.03901576874802));
#68003=CARTESIAN_POINT('Ctrl Pts',(17.4146758129753,-1.25550035156639,2.97358157797115));
#68004=CARTESIAN_POINT('Ctrl Pts',(17.433466353701,-1.5080701036121,2.84993223668737));
#68005=CARTESIAN_POINT('Ctrl Pts',(17.4403206066947,-1.59694044066333,2.80110140496957));
#68006=CARTESIAN_POINT('Ctrl Pts',(17.460474393217,-1.85083920250379,2.64557851648796));
#68007=CARTESIAN_POINT('Ctrl Pts',(17.4737674548813,-2.00861045809417,2.52788313360291));
#68008=CARTESIAN_POINT('Ctrl Pts',(17.4871655174868,-2.16586164017598,2.38650087129517));
#68009=CARTESIAN_POINT('Ctrl Pts',(17.4881116942534,-2.17695822764668,2.37638295499818));
#68010=CARTESIAN_POINT('Ctrl Pts',(17.489424054336,-2.19234333798265,2.36215653691083));
#68011=CARTESIAN_POINT('Ctrl Pts',(17.4897950241741,-2.19669162946884,2.35811337785725));
#68012=CARTESIAN_POINT('Ctrl Pts',(17.4904239228963,-2.20406251590948,2.35122164800931));
#68013=CARTESIAN_POINT('Ctrl Pts',(17.4906823200298,-2.20709080965138,2.3483792220818));
#68014=CARTESIAN_POINT('Ctrl Pts',(17.4911738297685,-2.21285086271516,2.34295172092911));
#68015=CARTESIAN_POINT('Ctrl Pts',(17.4914070246026,-2.2155835956161,2.34036771435768));
#68016=CARTESIAN_POINT('Ctrl Pts',(17.491954954221,-2.22200415097917,2.33427526748916));
#68017=CARTESIAN_POINT('Ctrl Pts',(17.4922693814721,-2.2256882105153,2.33076284975408));
#68018=CARTESIAN_POINT('Ctrl Pts',(17.4931956853666,-2.2365397688213,2.32036767974182));
#68019=CARTESIAN_POINT('Ctrl Pts',(17.4938057013579,-2.24368385258729,2.3134604129694));
#68020=CARTESIAN_POINT('Ctrl Pts',(17.4995103242819,-2.31045621059005,2.24830123459879));
#68021=CARTESIAN_POINT('Ctrl Pts',(17.5044364285496,-2.36784105968864,2.18778375211872));
#68022=CARTESIAN_POINT('Ctrl Pts',(17.5115345959294,-2.44869744046942,2.09559980242966));
#68023=CARTESIAN_POINT('Ctrl Pts',(17.5137836070429,-2.47403515419072,2.0656253087844));
#68024=CARTESIAN_POINT('Ctrl Pts',(17.5239945856777,-2.58734981215462,1.92649714339337));
#68025=CARTESIAN_POINT('Ctrl Pts',(17.5317672934675,-2.66869582655016,1.81213560991748));
#68026=CARTESIAN_POINT('Ctrl Pts',(17.5519599646978,-2.85809864132709,1.50530953802706));
#68027=CARTESIAN_POINT('Ctrl Pts',(17.5644783940036,-2.95430152447993,1.30643300124577));
#68028=CARTESIAN_POINT('Ctrl Pts',(17.5789888136548,-3.03627896164313,1.08052175918995));
#68029=CARTESIAN_POINT('Ctrl Pts',(17.5802015031873,-3.0429229984093,1.0616669924705));
#68030=CARTESIAN_POINT('Ctrl Pts',(17.5819953737513,-3.05244517678235,1.03382063303629));
#68031=CARTESIAN_POINT('Ctrl Pts',(17.5825720206181,-3.05546000049047,1.02487601248616));
#68032=CARTESIAN_POINT('Ctrl Pts',(17.5835938814549,-3.06072086425352,1.00903811343204));
#68033=CARTESIAN_POINT('Ctrl Pts',(17.5840385588038,-3.06298302973659,1.0021502289661));
#68034=CARTESIAN_POINT('Ctrl Pts',(17.5849095589254,-3.06736082280074,0.988667342908383));
#68035=CARTESIAN_POINT('Ctrl Pts',(17.5853358121773,-3.0694784711606,0.982073034998844));
#68036=CARTESIAN_POINT('Ctrl Pts',(17.5864879909021,-3.07513568388318,0.964259553575727));
#68037=CARTESIAN_POINT('Ctrl Pts',(17.5872152334363,-3.07863507505134,0.953027822114359));
#68038=CARTESIAN_POINT('Ctrl Pts',(17.5899197131768,-3.09138392002294,0.911305783384572));
#68039=CARTESIAN_POINT('Ctrl Pts',(17.5919096936923,-3.10024229841894,0.880698782386737));
#68040=CARTESIAN_POINT('Ctrl Pts',(17.6120433145843,-3.18463193221272,0.572054289843209));
#68041=CARTESIAN_POINT('Ctrl Pts',(17.6314669497433,-3.22299288741503,0.285259651166556));
#68042=CARTESIAN_POINT('Ctrl Pts',(17.6596739779669,-3.22263943885347,-0.131835884447859));
#68043=CARTESIAN_POINT('Ctrl Pts',(17.6683619514602,-3.21477208702586,-0.260827695952668));
#68044=CARTESIAN_POINT('Ctrl Pts',(17.6800887164683,-3.19303344089445,-0.439605475919181));
#68045=CARTESIAN_POINT('Ctrl Pts',(17.68336176788,-3.18568105890001,-0.490053491736329));
#68046=CARTESIAN_POINT('Ctrl Pts',(17.6871192593359,-3.17567832006897,-0.54887176034701));
#68047=CARTESIAN_POINT('Ctrl Pts',(17.6876644348986,-3.17418751190498,-0.557428601003604));
#68048=CARTESIAN_POINT('Ctrl Pts',(17.6885348904489,-3.17174337731699,-0.571129475717084));
#68049=CARTESIAN_POINT('Ctrl Pts',(17.6888613910862,-3.17081210024894,-0.576277325099635));
#68050=CARTESIAN_POINT('Ctrl Pts',(17.6894392563615,-3.1691379969091,-0.585404393940074));
#68051=CARTESIAN_POINT('Ctrl Pts',(17.6896909064771,-3.16840020426217,-0.589384504583058));
#68052=CARTESIAN_POINT('Ctrl Pts',(17.6902211700118,-3.16682703890943,-0.597782808165955));
#68053=CARTESIAN_POINT('Ctrl Pts',(17.6904996817189,-3.16598992070272,-0.602200633265005));
#68054=CARTESIAN_POINT('Ctrl Pts',(17.6912421688003,-3.16372933332074,-0.613995698080348));
#68055=CARTESIAN_POINT('Ctrl Pts',(17.6917052038299,-3.16228929689642,-0.621369791003705));
#68056=CARTESIAN_POINT('Ctrl Pts',(17.6938884455929,-3.15535668754718,-0.656221707228936));
#68057=CARTESIAN_POINT('Ctrl Pts',(17.6955903359931,-3.14953148252711,-0.683633176718141));
#68058=CARTESIAN_POINT('Ctrl Pts',(17.7116371207942,-3.09065237982463,-0.943951555649504));
#68059=CARTESIAN_POINT('Ctrl Pts',(17.7247500515091,-3.01220774887604,-1.17039091274974));
#68060=CARTESIAN_POINT('Ctrl Pts',(17.7505932821299,-2.81368186425124,-1.58709819479223));
#68061=CARTESIAN_POINT('Ctrl Pts',(17.7632318171866,-2.6973706685749,-1.77759879206017));
#68062=CARTESIAN_POINT('Ctrl Pts',(17.7777512614815,-2.55154090473208,-1.96877506872042));
#68063=CARTESIAN_POINT('Ctrl Pts',(17.778833784184,-2.54059612375943,-1.98287860845329));
#68064=CARTESIAN_POINT('Ctrl Pts',(17.7804778784141,-2.52386836668892,-2.00406827814829));
#68065=CARTESIAN_POINT('Ctrl Pts',(17.781036023722,-2.51817135367504,-2.01122207293809));
#68066=CARTESIAN_POINT('Ctrl Pts',(17.7820088342172,-2.50821075188735,-2.0236210305915));
#68067=CARTESIAN_POINT('Ctrl Pts',(17.7824229433581,-2.50396094698811,-2.02887723290264));
#68068=CARTESIAN_POINT('Ctrl Pts',(17.7832884468379,-2.49505861724397,-2.03981715100268));
#68069=CARTESIAN_POINT('Ctrl Pts',(17.7837399594041,-2.49040313894979,-2.04549840310207));
#68070=CARTESIAN_POINT('Ctrl Pts',(17.7848102166945,-2.47934137779691,-2.05890373661293));
#68071=CARTESIAN_POINT('Ctrl Pts',(17.7854296406917,-2.47291838758104,-2.06661387516059));
#68072=CARTESIAN_POINT('Ctrl Pts',(17.7874883783825,-2.45150268554474,-2.09207842713798));
#68073=CARTESIAN_POINT('Ctrl Pts',(17.7889340845569,-2.43635422972455,-2.10970035413202));
#68074=CARTESIAN_POINT('Ctrl Pts',(17.8034796649227,-2.28288025927146,-2.28437629246379));
#68075=CARTESIAN_POINT('Ctrl Pts',(17.8172282167309,-2.12978444742709,-2.42773677416274));
#68076=CARTESIAN_POINT('Ctrl Pts',(17.8407842890914,-1.85225478291416,-2.64104135461136));
#68077=CARTESIAN_POINT('Ctrl Pts',(17.8503726521199,-1.73510142564146,-2.71944293848149));
#68078=CARTESIAN_POINT('Ctrl Pts',(17.8649765268354,-1.54674434223661,-2.82835497076971));
#68079=CARTESIAN_POINT('Ctrl Pts',(17.8700817997819,-1.47893606540631,-2.86439513020792));
#68080=CARTESIAN_POINT('Ctrl Pts',(17.8785730916323,-1.36184144777993,-2.9213630241878));
#68081=CARTESIAN_POINT('Ctrl Pts',(17.8820088150027,-1.31320361822395,-2.94354736842773));
#68082=CARTESIAN_POINT('Ctrl Pts',(17.8859309811665,-1.25592658562948,-2.96796961556646));
#68083=CARTESIAN_POINT('Ctrl Pts',(17.886484214146,-1.24780572141544,-2.9713929584096));
#68084=CARTESIAN_POINT('Ctrl Pts',(17.8873650411718,-1.23480740621754,-2.97680970037566));
#68085=CARTESIAN_POINT('Ctrl Pts',(17.887693901688,-1.22993900229697,-2.97882449537912));
#68086=CARTESIAN_POINT('Ctrl Pts',(17.8882744608355,-1.22131671303639,-2.98236809888988));
#68087=CARTESIAN_POINT('Ctrl Pts',(17.8885264542168,-1.21756486051184,-2.9839017748561));
#68088=CARTESIAN_POINT('Ctrl Pts',(17.8890558515707,-1.20966302881378,-2.98711448726941));
#68089=CARTESIAN_POINT('Ctrl Pts',(17.8893331596651,-1.20551245278582,-2.98879195162424));
#68090=CARTESIAN_POINT('Ctrl Pts',(17.8900690302999,-1.19446840769231,-2.99322867792044));
#68091=CARTESIAN_POINT('Ctrl Pts',(17.8905266817445,-1.187568825033,-2.99597279421586));
#68092=CARTESIAN_POINT('Ctrl Pts',(17.8926474999511,-1.15545440166465,-3.00861703816584));
#68093=CARTESIAN_POINT('Ctrl Pts',(17.894293597801,-1.13012396598836,-3.01822320108332));
#68094=CARTESIAN_POINT('Ctrl Pts',(17.8987566630976,-1.06044611590274,-3.04364718355415));
#68095=CARTESIAN_POINT('Ctrl Pts',(17.9015407890691,-1.01586705930184,-3.05881492316037));
#68096=CARTESIAN_POINT('Ctrl Pts',(17.9110170677043,-0.861047873108858,
-3.10773279739154));
#68097=CARTESIAN_POINT('Ctrl Pts',(17.9175241502935,-0.74933407218692,-3.13654407024733));
#68098=CARTESIAN_POINT('Ctrl Pts',(17.9397888966039,-0.359881347184209,
-3.21498294552861));
#68099=CARTESIAN_POINT('Ctrl Pts',(17.9553426193508,-0.077377678183578,
-3.23413448481953));
#68100=CARTESIAN_POINT('Ctrl Pts',(17.9728184250106,0.213937365374667,-3.2156566024651));
#68101=CARTESIAN_POINT('Ctrl Pts',(17.9734155425346,0.223865171433876,-3.21498070958324));
#68102=CARTESIAN_POINT('Ctrl Pts',(17.9755188615752,0.25874186052237,-3.21244394830643));
#68103=CARTESIAN_POINT('Ctrl Pts',(17.9770324388021,0.283671575761402,-3.2103385887447));
#68104=CARTESIAN_POINT('Ctrl Pts',(17.9791381362927,0.318108239451829,-3.2070261081837));
#68105=CARTESIAN_POINT('Ctrl Pts',(17.9797224667968,0.327638535033711,-3.20606648368826));
#68106=CARTESIAN_POINT('Ctrl Pts',(17.9807283100963,0.343998398663553,-3.2043454691331));
#68107=CARTESIAN_POINT('Ctrl Pts',(17.9811491708191,0.350830107200836,-3.20360469136875));
#68108=CARTESIAN_POINT('Ctrl Pts',(17.9820169687281,0.364888676387711,-3.20203477982202));
#68109=CARTESIAN_POINT('Ctrl Pts',(17.9824639866112,0.372115198423704,-3.20120301684624));
#68110=CARTESIAN_POINT('Ctrl Pts',(17.983503156922,0.388878623196843,-3.19921603925885));
#68111=CARTESIAN_POINT('Ctrl Pts',(17.9840958810206,0.398413263188915,-3.19804263854369));
#68112=CARTESIAN_POINT('Ctrl Pts',(17.9859808196012,0.428648153774528,-3.1941844078));
#68113=CARTESIAN_POINT('Ctrl Pts',(17.9872780326044,0.449327311523937,-3.19134112950069));
#68114=CARTESIAN_POINT('Ctrl Pts',(18.0009472029659,0.665854576657254,-3.15942351688875));
#68115=CARTESIAN_POINT('Ctrl Pts',(18.0138982512026,0.858618047448988,-3.11256626904443));
#68116=CARTESIAN_POINT('Ctrl Pts',(18.0426237318469,1.26347051668131,-2.97366774463613));
#68117=CARTESIAN_POINT('Ctrl Pts',(18.0584422536356,1.47248204088198,-2.87590981722368));
#68118=CARTESIAN_POINT('Ctrl Pts',(18.077098668881,1.71690593136426,-2.72790185009183));
#68119=CARTESIAN_POINT('Ctrl Pts',(18.0806794503136,1.7637576385851,-2.69784624742659));
#68120=CARTESIAN_POINT('Ctrl Pts',(18.0847479701244,1.81719289233825,-2.66157982333475));
#68121=CARTESIAN_POINT('Ctrl Pts',(18.0853081217614,1.82455443092031,-2.6565387813808));
#68122=CARTESIAN_POINT('Ctrl Pts',(18.0861978441412,1.83625618219817,-2.64845405740705));
#68123=CARTESIAN_POINT('Ctrl Pts',(18.0865287212972,1.84060991958709,-2.6454301702621));
#68124=CARTESIAN_POINT('Ctrl Pts',(18.087111594041,1.84828336680693,-2.64007246587258));
#68125=CARTESIAN_POINT('Ctrl Pts',(18.0873638923026,1.85160615270468,-2.63774310444972));
#68126=CARTESIAN_POINT('Ctrl Pts',(18.0878926039503,1.85857221079515,-2.63284006281744));
#68127=CARTESIAN_POINT('Ctrl Pts',(18.0881689263029,1.86221453292502,-2.63026509938734));
#68128=CARTESIAN_POINT('Ctrl Pts',(18.088899379119,1.87184681421547,-2.62342545788328));
#68129=CARTESIAN_POINT('Ctrl Pts',(18.0893526221596,1.87782758714492,-2.61914779735983));
#68130=CARTESIAN_POINT('Ctrl Pts',(18.0914237025256,1.90517138709063,-2.59944873781665));
#68131=CARTESIAN_POINT('Ctrl Pts',(18.0930254312597,1.92636017694078,-2.58378565830548));
#68132=CARTESIAN_POINT('Ctrl Pts',(18.107186686904,2.11376046229517,-2.44166950653747));
#68133=CARTESIAN_POINT('Ctrl Pts',(18.1187919837638,2.26752971679767,-2.29957975580011));
#68134=CARTESIAN_POINT('Ctrl Pts',(18.1447488558559,2.5764955199715,-1.95272209802431));
#68135=CARTESIAN_POINT('Ctrl Pts',(18.1590974014191,2.72317476170245,-1.74233981235439));
#68136=CARTESIAN_POINT('Ctrl Pts',(18.1756981063697,2.85251160315852,-1.49988831870937));
#68137=CARTESIAN_POINT('Ctrl Pts',(18.1768651687894,2.86141111983531,-1.48283977327762));
#68138=CARTESIAN_POINT('Ctrl Pts',(18.1786040933243,2.87438314414717,-1.45743796932309));
#68139=CARTESIAN_POINT('Ctrl Pts',(18.1791718154387,2.87857307825575,-1.44914489409222));
#68140=CARTESIAN_POINT('Ctrl Pts',(18.1801835738701,2.88595962933506,-1.43436636140056));
#68141=CARTESIAN_POINT('Ctrl Pts',(18.1806271098279,2.88917040657127,-1.42788802127776));
#68142=CARTESIAN_POINT('Ctrl Pts',(18.1815612363618,2.89587500817863,-1.41424504177749));
#68143=CARTESIAN_POINT('Ctrl Pts',(18.1820519884977,2.89936410202991,-1.40707814396426));
#68144=CARTESIAN_POINT('Ctrl Pts',(18.1833462586601,2.90847836808413,-1.38817882030668));
#68145=CARTESIAN_POINT('Ctrl Pts',(18.1841513159129,2.91405909671061,-1.37642523504178));
#68146=CARTESIAN_POINT('Ctrl Pts',(18.1877952441244,2.93891924628962,-1.32323831571081));
#68147=CARTESIAN_POINT('Ctrl Pts',(18.1906619729058,2.95738642937206,-1.28143323564138));
#68148=CARTESIAN_POINT('Ctrl Pts',(18.1983782706955,3.00419238989113,-1.16907042778489));
#68149=CARTESIAN_POINT('Ctrl Pts',(18.2032790627917,3.03093237427858,-1.09788206104661));
#68150=CARTESIAN_POINT('Ctrl Pts',(18.2287185772952,3.15473996469066,-0.729154204719931));
#68151=CARTESIAN_POINT('Ctrl Pts',(18.2504686754304,3.21059606269129,-0.419618568786852));
#68152=CARTESIAN_POINT('Ctrl Pts',(18.2750292354069,3.22303290713635,-0.0449510719625321));
#68153=CARTESIAN_POINT('Ctrl Pts',(18.2790293408244,3.22330135641951,0.0170675943606899));
#68154=CARTESIAN_POINT('Ctrl Pts',(18.2835736626479,3.22153250228033,0.0891502898599032));
#68155=CARTESIAN_POINT('Ctrl Pts',(18.2842073232337,3.2212374896472,0.0992395038693905));
#68156=CARTESIAN_POINT('Ctrl Pts',(18.2851584794236,3.22072139776817,0.114444100032095));
#68157=CARTESIAN_POINT('Ctrl Pts',(18.2854779014298,3.2205355241234,0.119560498489084));
#68158=CARTESIAN_POINT('Ctrl Pts',(18.2860472125515,3.22018174616714,0.128698424547651));
#68159=CARTESIAN_POINT('Ctrl Pts',(18.2862973608781,3.22001850022707,0.132720087590041));
#68160=CARTESIAN_POINT('Ctrl Pts',(18.2868333976551,3.21965190815539,0.141352219116043));
#68161=CARTESIAN_POINT('Ctrl Pts',(18.287119150823,3.21944619402374,0.14596254300184));
#68162=CARTESIAN_POINT('Ctrl Pts',(18.2879015721003,3.2188546711652,0.158609269246529));
#68163=CARTESIAN_POINT('Ctrl Pts',(18.2883971152335,3.21844866690736,0.166644760228525));
#68164=CARTESIAN_POINT('Ctrl Pts',(18.2910019841578,3.21614880508485,0.209013877060418));
#68165=CARTESIAN_POINT('Ctrl Pts',(18.2930833254905,3.21373555381913,0.243318624275949));
#68166=CARTESIAN_POINT('Ctrl Pts',(18.2990848569302,3.20509277813615,0.343289866775975));
#68167=CARTESIAN_POINT('Ctrl Pts',(18.3029378835285,3.19739573311508,0.408814539826498));
#68168=CARTESIAN_POINT('Ctrl Pts',(18.3211497671374,3.15084616686602,0.721824333985837));
#68169=CARTESIAN_POINT('Ctrl Pts',(18.3347468557573,3.08523952595941,0.96445501732195));
#68170=CARTESIAN_POINT('Ctrl Pts',(18.3492148114757,2.99102920573645,1.19994649356021));
#68171=CARTESIAN_POINT('Ctrl Pts',(18.3493928710357,2.9898661101187,1.20284161073554));
#68172=CARTESIAN_POINT('Ctrl Pts',(18.3498882776976,2.98662003149034,1.21088778266241));
#68173=CARTESIAN_POINT('Ctrl Pts',(18.3502058185659,2.98452793305053,1.21603513566622));
#68174=CARTESIAN_POINT('Ctrl Pts',(18.3530717558043,2.96554348532392,1.26239994852628));
#68175=CARTESIAN_POINT('Ctrl Pts',(18.3556385441123,2.94781206785718,1.30326727496762));
#68176=CARTESIAN_POINT('Ctrl Pts',(18.3586692120556,2.92608353283526,1.35063319291652));
#68177=CARTESIAN_POINT('Ctrl Pts',(18.3591101126738,2.92290306504024,1.3575023146057));
#68178=CARTESIAN_POINT('Ctrl Pts',(18.364329719472,2.88502450850945,1.43856153043603));
#68179=CARTESIAN_POINT('Ctrl Pts',(18.3691878440013,2.84753709651971,1.51140876445932));
#68180=CARTESIAN_POINT('Ctrl Pts',(18.3750511455947,2.79996631707882,1.59578516216952));
#68181=CARTESIAN_POINT('Ctrl Pts',(18.3759605039468,2.79252368158289,1.60877379908814));
#68182=CARTESIAN_POINT('Ctrl Pts',(18.3774409514536,2.78030406481381,1.62975876121442));
#68183=CARTESIAN_POINT('Ctrl Pts',(18.3780100345254,2.77558237895084,1.63778715569596));
#68184=CARTESIAN_POINT('Ctrl Pts',(18.3790233251997,2.76713213321772,1.65201381328183));
#68185=CARTESIAN_POINT('Ctrl Pts',(18.3794670269255,2.76341736857454,1.65822022893991));
#68186=CARTESIAN_POINT('Ctrl Pts',(18.3804005919381,2.75557106268429,1.67122979668467));
#68187=CARTESIAN_POINT('Ctrl Pts',(18.3808906134647,2.75143515417554,1.67803024566919));
#68188=CARTESIAN_POINT('Ctrl Pts',(18.3821808926254,2.7404994530043,1.6958620932737));
#68189=CARTESIAN_POINT('Ctrl Pts',(18.382982672336,2.73365829417609,1.70686783733203));
#68190=CARTESIAN_POINT('Ctrl Pts',(18.3865909356843,2.70266866321686,1.75605833624521));
#68191=CARTESIAN_POINT('Ctrl Pts',(18.3894246130884,2.67778617344998,1.79377246550688));
#68192=CARTESIAN_POINT('Ctrl Pts',(18.3970314882563,2.60959364588803,1.89254895481142));
#68193=CARTESIAN_POINT('Ctrl Pts',(18.4018541406598,2.56493699668418,1.95264367164623));
#68194=CARTESIAN_POINT('Ctrl Pts',(18.4267506066009,2.32723677743884,2.25028006525773));
#68195=CARTESIAN_POINT('Ctrl Pts',(18.4479831610657,2.10318708427647,2.46096588443852));
#68196=CARTESIAN_POINT('Ctrl Pts',(18.4697976226025,1.83186531289969,2.65161139403311));
#68197=CARTESIAN_POINT('Ctrl Pts',(18.4714725545752,1.81073557249715,2.66608516732623));
#68198=CARTESIAN_POINT('Ctrl Pts',(18.4731355395702,1.78943620771753,2.68030513580255));
#68199=CARTESIAN_POINT('Origin',(-1.72497344927317,0.,0.));
#68200=CARTESIAN_POINT('',(19.9669438677106,1.78943621037804,2.68030513402633));
#68201=CARTESIAN_POINT('',(19.7206814315572,1.78943602647606,2.6803052568037));
#68202=CARTESIAN_POINT('',(-1.72497344927317,1.78943621037804,2.68030513402633));
#68203=CARTESIAN_POINT('',(19.146573449238,-3.22274959114088,0.00162336111893835));
#68204=CARTESIAN_POINT('Ctrl Pts',(19.1465734492731,-3.22274959114116,0.00162336054795465));
#68205=CARTESIAN_POINT('Ctrl Pts',(19.1528129930212,-3.22280074318622,-0.0999253881336108));
#68206=CARTESIAN_POINT('Ctrl Pts',(19.1590525367692,-3.21804785151634,-0.201467213136769));
#68207=CARTESIAN_POINT('Ctrl Pts',(19.1652920805173,-3.2085193226538,-0.302524905846155));
#68208=CARTESIAN_POINT('Ctrl Pts',(19.1715337357476,-3.19898756930556,-0.403616796813063));
#68209=CARTESIAN_POINT('Ctrl Pts',(19.1777753909778,-3.18467700214314,-0.504223814665632));
#68210=CARTESIAN_POINT('Ctrl Pts',(19.1840170462081,-3.16566779601905,-0.603874960358412));
#68211=CARTESIAN_POINT('Ctrl Pts',(19.1902622883947,-3.14664766567892,-0.703583373600274));
#68212=CARTESIAN_POINT('Ctrl Pts',(19.1965075305812,-3.12292360146622,-0.802334412752572));
#68213=CARTESIAN_POINT('Ctrl Pts',(19.2027527727677,-3.09462648393053,-0.89966909886679));
#68214=CARTESIAN_POINT('Ctrl Pts',(19.2090073720642,-3.0662869694417,-0.997149619415189));
#68215=CARTESIAN_POINT('Ctrl Pts',(19.2152619713607,-3.03336083914884,-1.09320914994683));
#68216=CARTESIAN_POINT('Ctrl Pts',(19.2215165706571,-2.99602833737228,-1.18740547588526));
#68217=CARTESIAN_POINT('Ctrl Pts',(19.2277765972731,-2.95866344096807,-1.28168353904353));
#68218=CARTESIAN_POINT('Ctrl Pts',(19.2340366238891,-2.9168847279077,-1.37409479835277));
#68219=CARTESIAN_POINT('Ctrl Pts',(19.2402966505051,-2.87091904732102,-1.46422040220363));
#68220=CARTESIAN_POINT('Ctrl Pts',(19.2465677868719,-2.82487179084231,-1.55450595313753));
#68221=CARTESIAN_POINT('Ctrl Pts',(19.2528389232386,-2.77462293690911,-1.64249738896081));
#68222=CARTESIAN_POINT('Ctrl Pts',(19.2591100596054,-2.72044345063527,-1.7278035173004));
#68223=CARTESIAN_POINT('Ctrl Pts',(19.2610966965082,-2.70327989996263,-1.75482769484693));
#68224=CARTESIAN_POINT('Ctrl Pts',(19.263083333411,-2.68572219265785,-1.78158262996471));
#68225=CARTESIAN_POINT('Ctrl Pts',(19.2650699703137,-2.66777977423865,-1.80805659166497));
#68226=CARTESIAN_POINT('Ctrl Pts',(19.2712422184065,-2.6120347824327,-1.89030808884741));
#68227=CARTESIAN_POINT('Ctrl Pts',(19.2774144664993,-2.5523842109608,-1.97012389438097));
#68228=CARTESIAN_POINT('Ctrl Pts',(19.283586714592,-2.48906799086659,-2.04710969401822));
#68229=CARTESIAN_POINT('Ctrl Pts',(19.2897506032447,-2.42583752366879,-2.12399122724014));
#68230=CARTESIAN_POINT('Ctrl Pts',(19.2959144918973,-2.35895154903475,-2.1980500402326));
#68231=CARTESIAN_POINT('Ctrl Pts',(19.30207838055,-2.28869339035218,-2.26892047623054));
#68232=CARTESIAN_POINT('Ctrl Pts',(19.3082357422085,-2.21850962863106,-2.33971586692139));
#68233=CARTESIAN_POINT('Ctrl Pts',(19.314393103867,-2.14496108614528,-2.40732928604279));
#68234=CARTESIAN_POINT('Ctrl Pts',(19.3205504655256,-2.06837086215162,-2.47142864333611));
#68235=CARTESIAN_POINT('Ctrl Pts',(19.3267033296719,-1.99183658183785,-2.53548118063415));
#68236=CARTESIAN_POINT('Ctrl Pts',(19.3328561938182,-1.91226536930191,-2.59602448134056));
#68237=CARTESIAN_POINT('Ctrl Pts',(19.3390090579645,-1.83001595935445,-2.65276443564219));
#68238=CARTESIAN_POINT('Ctrl Pts',(19.345159591101,-1.74779770955839,-2.70948289403805));
#68239=CARTESIAN_POINT('Ctrl Pts',(19.3513101242376,-1.66290363557621,-2.76240062269866));
#68240=CARTESIAN_POINT('Ctrl Pts',(19.3574606573741,-1.57572350502502,-2.81126537313923));
#68241=CARTESIAN_POINT('Ctrl Pts',(19.3636105055893,-1.48855308282425,-2.8601246820174));
#68242=CARTESIAN_POINT('Ctrl Pts',(19.3697603538045,-1.39909748909988,-2.90493169761945));
#68243=CARTESIAN_POINT('Ctrl Pts',(19.3759102020197,-1.30777239521821,-2.94547940491955));
#68244=CARTESIAN_POINT('Ctrl Pts',(19.3820610103988,-1.21643304292602,-2.98603344285488));
#68245=CARTESIAN_POINT('Ctrl Pts',(19.388211818778,-1.12322400776556,-3.02232667534786));
#68246=CARTESIAN_POINT('Ctrl Pts',(19.3943626271571,-1.0285813655908,-3.05420004859855));
#68247=CARTESIAN_POINT('Ctrl Pts',(19.4005200135233,-0.933837507764791,
-3.08610750885438));
#68248=CARTESIAN_POINT('Ctrl Pts',(19.4066773998895,-0.837657393797968,
-3.1135855319858));
#68249=CARTESIAN_POINT('Ctrl Pts',(19.4128347862557,-0.740492593138584,
-3.13652487348768));
#68250=CARTESIAN_POINT('Ctrl Pts',(19.4189956089926,-0.643273565854203,
-3.1594770171881));
#68251=CARTESIAN_POINT('Ctrl Pts',(19.4251564317296,-0.545069184423238,
-3.17788535481417));
#68252=CARTESIAN_POINT('Ctrl Pts',(19.4313172544666,-0.446339479169904,
-3.19169212673064));
#68253=CARTESIAN_POINT('Ctrl Pts',(19.4374883773832,-0.347444709321798,
-3.20552198196541));
#68254=CARTESIAN_POINT('Ctrl Pts',(19.4436595002999,-0.248023294036869,
-3.21473486429637));
#68255=CARTESIAN_POINT('Ctrl Pts',(19.4498306232166,-0.148538773745802,
-3.21932505273918));
#68256=CARTESIAN_POINT('Ctrl Pts',(19.4545261451622,-0.0728423803045645,
-3.22281766354254));
#68257=CARTESIAN_POINT('Ctrl Pts',(19.4592216671079,0.00289047582658457,
-3.22363505479609));
#68258=CARTESIAN_POINT('Ctrl Pts',(19.4639171890535,0.0784574822998072,
-3.22179483921171));
#68259=CARTESIAN_POINT('Ctrl Pts',(19.4700894371462,0.177790062784492,-3.21937588190247));
#68260=CARTESIAN_POINT('Ctrl Pts',(19.476261685239,0.277185504657452,-3.21235451274927));
#68261=CARTESIAN_POINT('Ctrl Pts',(19.4824339333318,0.376182374086792,-3.20071935413376));
#68262=CARTESIAN_POINT('Ctrl Pts',(19.4885978219844,0.475045166208819,-3.18909995370077));
#68263=CARTESIAN_POINT('Ctrl Pts',(19.494761710637,0.573510031211977,-3.17287923409625));
#68264=CARTESIAN_POINT('Ctrl Pts',(19.5009255992897,0.671116179509239,-3.15209781512264));
#68265=CARTESIAN_POINT('Ctrl Pts',(19.5070829609482,0.768618971826402,-3.13133840177023));
#68266=CARTESIAN_POINT('Ctrl Pts',(19.5132403226067,0.865264432706953,-3.10602798023603));
#68267=CARTESIAN_POINT('Ctrl Pts',(19.5193976842653,0.960598501788612,-3.07625877989181));
#68268=CARTESIAN_POINT('Ctrl Pts',(19.5255505484116,1.05586293615248,-3.04651132381893));
#68269=CARTESIAN_POINT('Ctrl Pts',(19.5317034125579,1.14981746976196,-3.01231169313222));
#68270=CARTESIAN_POINT('Ctrl Pts',(19.5378562767042,1.24202072323521,-2.97380263056483));
#68271=CARTESIAN_POINT('Ctrl Pts',(19.5440068098408,1.33418904554799,-2.9353081571382));
#68272=CARTESIAN_POINT('Ctrl Pts',(19.5501573429773,1.42460700566302,-2.89250766306926));
#68273=CARTESIAN_POINT('Ctrl Pts',(19.5563078761138,1.5128516585648,-2.84559263101339));
#68274=CARTESIAN_POINT('Ctrl Pts',(19.562457724329,1.60108648457133,-2.79868282339992));
#68275=CARTESIAN_POINT('Ctrl Pts',(19.5686075725443,1.68714810099244,-2.7476595926638));
#68276=CARTESIAN_POINT('Ctrl Pts',(19.5747574207595,1.77063760717915,-2.69276067011959));
#68277=CARTESIAN_POINT('Ctrl Pts',(19.5809082291386,1.85414014842151,-2.63785317631243));
#68278=CARTESIAN_POINT('Ctrl Pts',(19.5870590375178,1.93506941881528,-2.57906902747991));
#68279=CARTESIAN_POINT('Ctrl Pts',(19.5932098458969,2.01305583020682,-2.5166890524994));
#68280=CARTESIAN_POINT('Ctrl Pts',(19.5993672322631,2.09112564422955,-2.45424236520383));
#68281=CARTESIAN_POINT('Ctrl Pts',(19.6055246186293,2.16624597466008,-2.38819244443255));
#68282=CARTESIAN_POINT('Ctrl Pts',(19.6116820049955,2.23808075582248,-2.31886008480828));
#68283=CARTESIAN_POINT('Ctrl Pts',(19.6178428277325,2.30995562719977,-2.24948903154353));
#68284=CARTESIAN_POINT('Ctrl Pts',(19.6240036504694,2.37854099947952,-2.17683220711775));
#68285=CARTESIAN_POINT('Ctrl Pts',(19.6301644732064,2.44353954163502,-2.10124536191424));
#68286=CARTESIAN_POINT('Ctrl Pts',(19.6363355961231,2.50864675380018,-2.02553214428875));
#68287=CARTESIAN_POINT('Ctrl Pts',(19.6425067190398,2.57015488978245,-1.946879463304));
#68288=CARTESIAN_POINT('Ctrl Pts',(19.6486778419564,2.62780849598165,-1.86567415990753));
#68289=CARTESIAN_POINT('Ctrl Pts',(19.653373363902,2.67167632632685,-1.80388616940059));
#68290=CARTESIAN_POINT('Ctrl Pts',(19.6580688858476,2.71331345388933,-1.74062098755121));
#68291=CARTESIAN_POINT('Ctrl Pts',(19.6627644077931,2.75262530228131,-1.67605832468346));
#68292=CARTESIAN_POINT('Ctrl Pts',(19.6689366558859,2.80430059718442,-1.59119091753042));
#68293=CARTESIAN_POINT('Ctrl Pts',(19.6751089039787,2.85213829201417,-1.50378205960815));
#68294=CARTESIAN_POINT('Ctrl Pts',(19.6812811520714,2.89587931381894,-1.41421376117458));
#68295=CARTESIAN_POINT('Ctrl Pts',(19.6874450407241,2.93956109457451,-1.32476677037754));
#68296=CARTESIAN_POINT('Ctrl Pts',(19.6936089293767,2.97915704135858,-1.23316653903017));
#68297=CARTESIAN_POINT('Ctrl Pts',(19.6997728180293,3.01445217026319,-1.13982265098371));
#68298=CARTESIAN_POINT('Ctrl Pts',(19.7059301796879,3.04970992485577,-1.04657760557381));
#68299=CARTESIAN_POINT('Ctrl Pts',(19.7120875413464,3.08067576291136,-0.951592978288173));
#68300=CARTESIAN_POINT('Ctrl Pts',(19.718244903005,3.10718175351252,-0.855300598116752));
#68301=CARTESIAN_POINT('Ctrl Pts',(19.7243977671513,3.13366838338359,-0.759078552640999));
#68302=CARTESIAN_POINT('Ctrl Pts',(19.7305506312976,3.15570152753199,-0.661551070956055));
#68303=CARTESIAN_POINT('Ctrl Pts',(19.7367034954439,3.17316260406615,-0.563166627789823));
#68304=CARTESIAN_POINT('Ctrl Pts',(19.7428540285804,3.19061706547943,-0.464819457524949));
#68305=CARTESIAN_POINT('Ctrl Pts',(19.749004561717,3.2035028251813,-0.365616398092275));
#68306=CARTESIAN_POINT('Ctrl Pts',(19.7551550948535,3.2117522693879,-0.266016771241406));
#68307=CARTESIAN_POINT('Ctrl Pts',(19.7613049430687,3.22000079493912,-0.166428235771939));
#68308=CARTESIAN_POINT('Ctrl Pts',(19.7674547912839,3.2236139956172,-0.0664436535774133));
#68309=CARTESIAN_POINT('Ctrl Pts',(19.7736046394991,3.22257616345777,0.0334728728044253));
#68310=CARTESIAN_POINT('Ctrl Pts',(19.7797554478783,3.22153816926361,0.13340499896078));
#68311=CARTESIAN_POINT('Ctrl Pts',(19.7859062562574,3.21584770440904,0.233268613806891));
#68312=CARTESIAN_POINT('Ctrl Pts',(19.7920570646366,3.20554116455006,0.33260096944389));
#68313=CARTESIAN_POINT('Ctrl Pts',(19.7982144510028,3.19522360235362,0.43203955614976));
#68314=CARTESIAN_POINT('Ctrl Pts',(19.804371837369,3.18028015205904,0.530945316200336));
#68315=CARTESIAN_POINT('Ctrl Pts',(19.8105292237351,3.16079895481053,0.628862091216109));
#68316=CARTESIAN_POINT('Ctrl Pts',(19.8166900464721,3.14130688531643,0.726833512525474));
#68317=CARTESIAN_POINT('Ctrl Pts',(19.8228508692091,3.11727212998798,0.823814427981407));
#68318=CARTESIAN_POINT('Ctrl Pts',(19.829011691946,3.08883317928826,0.919362362198937));
#68319=CARTESIAN_POINT('Ctrl Pts',(19.8351828148627,3.06034668196753,1.01507004145994));
#68320=CARTESIAN_POINT('Ctrl Pts',(19.8413539377794,3.02744142452246,1.10933954368935));
#68321=CARTESIAN_POINT('Ctrl Pts',(19.8475250606961,2.99030469462921,1.20174681018029));
#68322=CARTESIAN_POINT('Ctrl Pts',(19.8522205826417,2.96204787126753,1.27205821923747));
#68323=CARTESIAN_POINT('Ctrl Pts',(19.8569161045872,2.93134225754545,1.34129187371315));
#68324=CARTESIAN_POINT('Ctrl Pts',(19.8616116265328,2.8982878889683,1.40927104389456));
#68325=CARTESIAN_POINT('Ctrl Pts',(19.8677836353661,2.85483971489893,1.49862597476367));
#68326=CARTESIAN_POINT('Ctrl Pts',(19.8739556441994,2.80717894706068,1.58612701454832));
#68327=CARTESIAN_POINT('Ctrl Pts',(19.8801276530327,2.75548683046381,1.67134972092632));
#68328=CARTESIAN_POINT('Ctrl Pts',(19.8862916465573,2.70386184408032,1.75646175243086));
#68329=CARTESIAN_POINT('Ctrl Pts',(19.892455640082,2.6482161353862,1.83930096185228));
#68330=CARTESIAN_POINT('Ctrl Pts',(19.8986196336066,2.58877801620846,1.91946501538731));
#68331=CARTESIAN_POINT('Ctrl Pts',(19.9047764049644,2.5294095388971,1.99953514309861));
#68332=CARTESIAN_POINT('Ctrl Pts',(19.9109331763222,2.46625774731003,2.07693600293512));
#68333=CARTESIAN_POINT('Ctrl Pts',(19.91708994768,2.39959501652406,2.15129294127343));
#68334=CARTESIAN_POINT('Ctrl Pts',(19.9232424841021,2.33297813970292,2.22559873318562));
#68335=CARTESIAN_POINT('Ctrl Pts',(19.9293950205242,2.26285541225963,2.29686444243887));
#68336=CARTESIAN_POINT('Ctrl Pts',(19.9355475569464,2.18953992099314,2.36474787173545));
#68337=CARTESIAN_POINT('Ctrl Pts',(19.941698105571,2.11624811692488,2.43260936885619));
#68338=CARTESIAN_POINT('Ctrl Pts',(19.9478486541956,2.03976591450839,2.49709045991259));
#68339=CARTESIAN_POINT('Ctrl Pts',(19.9539992028202,1.96044313657274,2.55788589869932));
#68340=CARTESIAN_POINT('Ctrl Pts',(19.958314091117,1.904794616892,2.60053665123055));
#68341=CARTESIAN_POINT('Ctrl Pts',(19.9626289794138,1.84774884604552,2.64137421513157));
#68342=CARTESIAN_POINT('Ctrl Pts',(19.9669438677106,1.78943621037804,2.68030513402633));
#68343=CARTESIAN_POINT('Ctrl Pts',(18.7170794495574,1.78943621037806,2.68030513402632));
#68344=CARTESIAN_POINT('Ctrl Pts',(18.7233417863607,1.70500923028825,2.73667061771235));
#68345=CARTESIAN_POINT('Ctrl Pts',(18.7296041231639,1.61783995710172,2.78909426977908));
#68346=CARTESIAN_POINT('Ctrl Pts',(18.7358664599671,1.52833574574161,2.83730636533816));
#68347=CARTESIAN_POINT('Ctrl Pts',(18.7420176376459,1.44042027195277,2.88466267582925));
#68348=CARTESIAN_POINT('Ctrl Pts',(18.7481688153247,1.35025247487346,2.92795551133685));
#68349=CARTESIAN_POINT('Ctrl Pts',(18.7543199930036,1.25824587160605,2.96697402905491));
#68350=CARTESIAN_POINT('Ctrl Pts',(18.7604698971959,1.16625831658886,3.00598446871703));
#68351=CARTESIAN_POINT('Ctrl Pts',(18.7666198013881,1.07243311178441,3.04072217979505));
#68352=CARTESIAN_POINT('Ctrl Pts',(18.7727697055804,0.977204988616989,3.07102392903769));
#68353=CARTESIAN_POINT('Ctrl Pts',(18.7789199815786,0.881971108225357,3.10132751023877));
#68354=CARTESIAN_POINT('Ctrl Pts',(18.7850702575768,0.785334555129725,3.12719446558737));
#68355=CARTESIAN_POINT('Ctrl Pts',(18.7912205335749,0.68774553153598,3.14851133813304));
#68356=CARTESIAN_POINT('Ctrl Pts',(18.7975667835132,0.587046906767896,3.17050745686296));
#68357=CARTESIAN_POINT('Ctrl Pts',(18.8039130334515,0.485334571628309,3.18765853116547));
#68358=CARTESIAN_POINT('Ctrl Pts',(18.8102592833898,0.383113188613054,3.19989716197423));
#68359=CARTESIAN_POINT('Ctrl Pts',(18.8164188211197,0.283899247844779,3.21177572158992));
#68360=CARTESIAN_POINT('Ctrl Pts',(18.8225783588495,0.184206240647182,3.21902689963705));
#68361=CARTESIAN_POINT('Ctrl Pts',(18.8287378965794,0.0844980762081079,
3.22164207161769));
#68362=CARTESIAN_POINT('Ctrl Pts',(18.8351775026219,-0.0197437234809175,
3.22437615297694));
#68363=CARTESIAN_POINT('Ctrl Pts',(18.8416171086644,-0.124001549914439,
3.22204267337145));
#68364=CARTESIAN_POINT('Ctrl Pts',(18.8480567147069,-0.227750211563248,
3.2146924275322));
#68365=CARTESIAN_POINT('Ctrl Pts',(18.8544963207495,-0.331498873212073,
3.20734218169296));
#68366=CARTESIAN_POINT('Ctrl Pts',(18.860935926792,-0.434737848062131,3.1949753062194));
#68367=CARTESIAN_POINT('Ctrl Pts',(18.8673755328345,-0.536954836311479,
3.17770311172421));
#68368=CARTESIAN_POINT('Ctrl Pts',(18.8735477809273,-0.634928005260677,
3.16114801987125));
#68369=CARTESIAN_POINT('Ctrl Pts',(18.8797200290201,-0.732307274235706,
3.14002856287555));
#68370=CARTESIAN_POINT('Ctrl Pts',(18.8858922771128,-0.828634300415547,
3.11439926128216));
#68371=CARTESIAN_POINT('Ctrl Pts',(18.8920561657655,-0.924830865214518,
3.08880467096564));
#68372=CARTESIAN_POINT('Ctrl Pts',(18.8982200544181,-1.01997760371505,3.05871248697548));
#68373=CARTESIAN_POINT('Ctrl Pts',(18.9043839430707,-1.11362422350716,3.02422860434162));
#68374=CARTESIAN_POINT('Ctrl Pts',(18.9105413047293,-1.20717168009763,2.98978123698418));
#68375=CARTESIAN_POINT('Ctrl Pts',(18.9166986663878,-1.29922177067461,2.95095156570248));
#68376=CARTESIAN_POINT('Ctrl Pts',(18.9228560280464,-1.3893382207761,2.90789560864738));
#68377=CARTESIAN_POINT('Ctrl Pts',(18.9290088921927,-1.47938884725696,2.86487110088904));
#68378=CARTESIAN_POINT('Ctrl Pts',(18.935161756339,-1.56750825057104,2.81762663153629));
#68379=CARTESIAN_POINT('Ctrl Pts',(18.9413146204853,-1.6532799088945,2.76636640836781));
#68380=CARTESIAN_POINT('Ctrl Pts',(18.9474651536218,-1.73901907266471,2.71512560511125));
#68381=CARTESIAN_POINT('Ctrl Pts',(18.9536156867584,-1.82241188631285,2.65987229357431));
#68382=CARTESIAN_POINT('Ctrl Pts',(18.9597662198949,-1.9030670224539,2.60085629563582));
#68383=CARTESIAN_POINT('Ctrl Pts',(18.9659160681101,-1.9837131768653,2.5418468696996));
#68384=CARTESIAN_POINT('Ctrl Pts',(18.9720659163253,-2.06162190933523,2.47907584692133));
#68385=CARTESIAN_POINT('Ctrl Pts',(18.9782157645405,-2.13643228446384,2.41283539770134));
#68386=CARTESIAN_POINT('Ctrl Pts',(18.9843665729197,-2.21125433959241,2.34658460648745));
#68387=CARTESIAN_POINT('Ctrl Pts',(18.9905173812988,-2.28297675130363,2.27686360090969));
#68388=CARTESIAN_POINT('Ctrl Pts',(18.996668189678,-2.35127374128403,2.2040030299544));
#68389=CARTESIAN_POINT('Ctrl Pts',(19.0028255760442,-2.41964377153594,2.13106453820222));
#68390=CARTESIAN_POINT('Ctrl Pts',(19.0089829624104,-2.48458076714167,2.05498009380272));
#68391=CARTESIAN_POINT('Ctrl Pts',(19.0151403487766,-2.54579782738497,1.97611512432397));
#68392=CARTESIAN_POINT('Ctrl Pts',(19.0213011715135,-2.607049052208,1.89720614115809));
#68393=CARTESIAN_POINT('Ctrl Pts',(19.0274619942505,-2.66457595712857,1.81551389772774));
#68394=CARTESIAN_POINT('Ctrl Pts',(19.0336228169875,-2.71813496374011,1.73143289832253));
#68395=CARTESIAN_POINT('Ctrl Pts',(19.0397939399042,-2.77178351478708,1.64721132525664));
#68396=CARTESIAN_POINT('Ctrl Pts',(19.0459650628209,-2.8214507004121,1.56059339587594));
#68397=CARTESIAN_POINT('Ctrl Pts',(19.0521361857376,-2.86693882417383,1.47199841743963));
#68398=CARTESIAN_POINT('Ctrl Pts',(19.0568317076831,-2.90155010744723,1.40458772555615));
#68399=CARTESIAN_POINT('Ctrl Pts',(19.0615272296287,-2.93374288370895,1.33603293883333));
#68400=CARTESIAN_POINT('Ctrl Pts',(19.0662227515742,-2.96344916204088,1.26652541486509));
#68401=CARTESIAN_POINT('Ctrl Pts',(19.0730622090646,-3.00671907541927,1.16528134424656));
#68402=CARTESIAN_POINT('Ctrl Pts',(19.079901666555,-3.04484207353096,1.06171188840576));
#68403=CARTESIAN_POINT('Ctrl Pts',(19.0867411240455,-3.07758863484432,0.956329314188925));
#68404=CARTESIAN_POINT('Ctrl Pts',(19.093561136033,-3.11024209325389,0.851246356886852));
#68405=CARTESIAN_POINT('Ctrl Pts',(19.1003811480205,-3.13754949825345,0.744360810177043));
#68406=CARTESIAN_POINT('Ctrl Pts',(19.107201160008,-3.15932940831118,0.63620378203852));
#68407=CARTESIAN_POINT('Ctrl Pts',(19.1139862885523,-3.18099791706078,0.528599962539821));
#68408=CARTESIAN_POINT('Ctrl Pts',(19.1207714170965,-3.197195216958,0.419737885761649));
#68409=CARTESIAN_POINT('Ctrl Pts',(19.1275565456408,-3.20779026533691,0.310159920218187));
#68410=CARTESIAN_POINT('Ctrl Pts',(19.1338955135065,-3.21768862920311,0.207787327297706));
#68411=CARTESIAN_POINT('Ctrl Pts',(19.1402344813723,-3.22269762399439,0.104790240090867));
#68412=CARTESIAN_POINT('Ctrl Pts',(19.146573449238,-3.22274959114088,0.00162336111892945));
#68413=CARTESIAN_POINT('',(18.9023069674493,-3.22275003535735,0.00201018136784693));
#68414=CARTESIAN_POINT('Ctrl Pts',(18.4731355395702,1.78943620771753,2.68030513580255));
#68415=CARTESIAN_POINT('Ctrl Pts',(18.476024270916,1.75243759205303,2.70500630195752));
#68416=CARTESIAN_POINT('Ctrl Pts',(18.4788769810994,1.71492714727499,2.72894162742002));
#68417=CARTESIAN_POINT('Ctrl Pts',(18.4823483894815,1.66791014521011,2.75759040523856));
#68418=CARTESIAN_POINT('Ctrl Pts',(18.4830115716966,1.65886444919064,2.76304141157852));
#68419=CARTESIAN_POINT('Ctrl Pts',(18.4839936041243,1.64537225142197,2.77108177211625));
#68420=CARTESIAN_POINT('Ctrl Pts',(18.4843146191607,1.64094619178575,2.77370503659756));
#68421=CARTESIAN_POINT('Ctrl Pts',(18.4848856768894,1.63304435144863,2.77836281440048));
#68422=CARTESIAN_POINT('Ctrl Pts',(18.4851359852072,1.6295710310706,2.78040141662612));
#68423=CARTESIAN_POINT('Ctrl Pts',(18.4856654291219,1.62220359998114,2.78470704841974));
#68424=CARTESIAN_POINT('Ctrl Pts',(18.4859444562345,1.6183085690645,2.78697241486077));
#68425=CARTESIAN_POINT('Ctrl Pts',(18.4866981320776,1.60775503423643,2.79308081090891));
#68426=CARTESIAN_POINT('Ctrl Pts',(18.4871717751755,1.60108745759378,2.7969082255881));
#68427=CARTESIAN_POINT('Ctrl Pts',(18.4882198329573,1.58625721943527,2.80535087337655));
#68428=CARTESIAN_POINT('Ctrl Pts',(18.488793523456,1.57808794804422,2.80995443417332));
#68429=CARTESIAN_POINT('Ctrl Pts',(18.4905286388476,1.5532285548915,2.82382063293728));
#68430=CARTESIAN_POINT('Ctrl Pts',(18.4916834377403,1.5364758044674,2.83297088783571));
#68431=CARTESIAN_POINT('Ctrl Pts',(18.50896109981,1.28289343695959,2.96856493832906));
#68432=CARTESIAN_POINT('Ctrl Pts',(18.5235323797865,1.03121843864519,3.06509810180271));
#68433=CARTESIAN_POINT('Ctrl Pts',(18.5494369907781,0.584023003599997,3.17520044154092));
#68434=CARTESIAN_POINT('Ctrl Pts',(18.5604454691664,0.393891621412011,3.20434308689518));
#68435=CARTESIAN_POINT('Ctrl Pts',(18.5731190962936,0.18441182878952,3.21751947184798));
#68436=CARTESIAN_POINT('Ctrl Pts',(18.5742066736896,0.166502078349412,3.21849597050111));
#68437=CARTESIAN_POINT('Ctrl Pts',(18.575857162619,0.139428459714096,3.2197455326491));
#68438=CARTESIAN_POINT('Ctrl Pts',(18.5764166098233,0.130269848601947,3.22012908968073));
#68439=CARTESIAN_POINT('Ctrl Pts',(18.5773910529248,0.114349790326214,3.22072778270735));
#68440=CARTESIAN_POINT('Ctrl Pts',(18.5778054880914,0.107589038748581,3.22096071421027));
#68441=CARTESIAN_POINT('Ctrl Pts',(18.5786710524421,0.0934903612106258,
3.22140202448157));
#68442=CARTESIAN_POINT('Ctrl Pts',(18.5791222978726,0.0861523635538499,
3.22160662089677));
#68443=CARTESIAN_POINT('Ctrl Pts',(18.5801908023742,0.0688056796694947,
3.22203096864952));
#68444=CARTESIAN_POINT('Ctrl Pts',(18.5808087346269,0.0587965857734008,
3.22222915733301));
#68445=CARTESIAN_POINT('Ctrl Pts',(18.5828574924463,0.0256879690323781,
3.22273042155132));
#68446=CARTESIAN_POINT('Ctrl Pts',(18.5842946255916,0.00258652631420823,
3.22283175279419));
#68447=CARTESIAN_POINT('Ctrl Pts',(18.6010332299844,-0.26501048133997,3.22112840264514));
#68448=CARTESIAN_POINT('Ctrl Pts',(18.61724099708,-0.508485757515415,3.19175419317788));
#68449=CARTESIAN_POINT('Ctrl Pts',(18.6418861061547,-0.863162548035848,
3.10733177933052));
#68450=CARTESIAN_POINT('Ctrl Pts',(18.6500494271499,-0.978428136077582,
3.07298548146399));
#68451=CARTESIAN_POINT('Ctrl Pts',(18.6656380460207,-1.19776200678344,2.99403350077649));
#68452=CARTESIAN_POINT('Ctrl Pts',(18.673066719152,-1.30194566601167,2.95022268005662));
#68453=CARTESIAN_POINT('Ctrl Pts',(18.6809368654072,-1.41415793606447,2.89593021724134));
#68454=CARTESIAN_POINT('Ctrl Pts',(18.6816723772746,-1.42466378610514,2.89077629673106));
#68455=CARTESIAN_POINT('Ctrl Pts',(18.6827364387447,-1.4398938282097,2.88320160531408));
#68456=CARTESIAN_POINT('Ctrl Pts',(18.6830677469511,-1.44464033144697,2.88082627853905));
#68457=CARTESIAN_POINT('Ctrl Pts',(18.6836511155358,-1.45300627108334,2.87661377553958));
#68458=CARTESIAN_POINT('Ctrl Pts',(18.683903480282,-1.45662813050576,2.87478147475325));
#68459=CARTESIAN_POINT('Ctrl Pts',(18.6841558598204,-1.46025304276704,2.87293902017468));
#68460=CARTESIAN_POINT('Ctrl Pts',(18.6841563102148,-1.46025951176447,2.87293573211349));
#68461=CARTESIAN_POINT('Ctrl Pts',(18.6841572108481,-1.46027244754318,2.87292915706233));
#68462=CARTESIAN_POINT('Ctrl Pts',(18.6841576602452,-1.46027890223328,2.87292587621836));
#68463=CARTESIAN_POINT('Ctrl Pts',(18.684158557766,-1.46029179334282,2.8729193237625));
#68464=CARTESIAN_POINT('Ctrl Pts',(18.6841590058816,-1.46029822964437,2.87291605221069));
#68465=CARTESIAN_POINT('Ctrl Pts',(18.684159900896,-1.46031108479031,2.87290951792614));
#68466=CARTESIAN_POINT('Ctrl Pts',(18.6841603477541,-1.46031750304842,2.87290625549155));
#68467=CARTESIAN_POINT('Ctrl Pts',(18.6841612402268,-1.46033032172228,2.87289973963768));
#68468=CARTESIAN_POINT('Ctrl Pts',(18.6841616858266,-1.46033672192511,2.87289648632678));
#68469=CARTESIAN_POINT('Ctrl Pts',(18.6841625757727,-1.46034950434424,2.87288998879404));
#68470=CARTESIAN_POINT('Ctrl Pts',(18.6841630201143,-1.46035588649246,2.87288674460695));
#68471=CARTESIAN_POINT('Ctrl Pts',(18.6841639075422,-1.4603686327767,2.87288026533531));
#68472=CARTESIAN_POINT('Ctrl Pts',(18.6841643506206,-1.4603749967993,2.87287703030858));
#68473=CARTESIAN_POINT('Ctrl Pts',(18.6841652355712,-1.46038770753736,2.8728705689997));
#68474=CARTESIAN_POINT('Ctrl Pts',(18.6841656774042,-1.46039405368954,2.87286734300405));
#68475=CARTESIAN_POINT('Ctrl Pts',(18.6841665598646,-1.46040672869427,2.87286089975396));
#68476=CARTESIAN_POINT('Ctrl Pts',(18.6841670004615,-1.46041305710831,2.87285768272259));
#68477=CARTESIAN_POINT('Ctrl Pts',(18.6841678804205,-1.46042569621865,2.87285125761405));
#68478=CARTESIAN_POINT('Ctrl Pts',(18.6841683197752,-1.46043200680808,2.87284804959136));
#68479=CARTESIAN_POINT('Ctrl Pts',(18.6841691972552,-1.46044461034698,2.87284164246109));
#68480=CARTESIAN_POINT('Ctrl Pts',(18.684169635365,-1.4604509030723,2.87283844346761));
#68481=CARTESIAN_POINT('Ctrl Pts',(18.6841705104098,-1.46046347166695,2.87283205399764));
#68482=CARTESIAN_POINT('Ctrl Pts',(18.6841709472997,-1.46046974688777,2.87282886385099));
#68483=CARTESIAN_POINT('Ctrl Pts',(18.6841718198684,-1.46048227995116,2.87282249234063));
#68484=CARTESIAN_POINT('Ctrl Pts',(18.6841722555346,-1.46048853761152,2.87281931106969));
#68485=CARTESIAN_POINT('Ctrl Pts',(18.684173125644,-1.46050103538487,2.87281295739716));
#68486=CARTESIAN_POINT('Ctrl Pts',(18.6841735600824,-1.46050727542684,2.87280978503182));
#68487=CARTESIAN_POINT('Ctrl Pts',(18.6841744277575,-1.46051973826814,2.87280344901599));
#68488=CARTESIAN_POINT('Ctrl Pts',(18.684174860972,-1.46052596074721,2.87280028552847));
#68489=CARTESIAN_POINT('Ctrl Pts',(18.6841757262361,-1.46053838899034,2.87279396700046));
#68490=CARTESIAN_POINT('Ctrl Pts',(18.6841761582447,-1.46054459416561,2.87279081225946));
#68491=CARTESIAN_POINT('Ctrl Pts',(18.6841770210724,-1.46055698744658,2.87278451140517));
#68492=CARTESIAN_POINT('Ctrl Pts',(18.6841774518729,-1.46056317528688,2.87278136542696));
#68493=CARTESIAN_POINT('Ctrl Pts',(18.6841783122832,-1.46057553387815,2.87277508210872));
#68494=CARTESIAN_POINT('Ctrl Pts',(18.6841787418776,-1.46058170440909,2.8727719448807));
#68495=CARTESIAN_POINT('Ctrl Pts',(18.6841795998783,-1.46059402842215,2.87276567904267));
#68496=CARTESIAN_POINT('Ctrl Pts',(18.684180028265,-1.46060018162263,2.87276255057599));
#68497=CARTESIAN_POINT('Ctrl Pts',(18.6841808838898,-1.46061247154269,2.87275630197232));
#68498=CARTESIAN_POINT('Ctrl Pts',(18.6841813110869,-1.46061860767264,2.87275318213524));
#68499=CARTESIAN_POINT('Ctrl Pts',(18.6841821643033,-1.46063086303052,2.87274695100528));
#68500=CARTESIAN_POINT('Ctrl Pts',(18.6841825903017,-1.46063698195809,2.87274383986526));
#68501=CARTESIAN_POINT('Ctrl Pts',(18.6841834411658,-1.46064920356114,2.87273762579936));
#68502=CARTESIAN_POINT('Ctrl Pts',(18.6841838659907,-1.46065530564827,2.87273452317278));
#68503=CARTESIAN_POINT('Ctrl Pts',(18.6841847144447,-1.4606674926646,2.87272832659474));
#68504=CARTESIAN_POINT('Ctrl Pts',(18.6841851380758,-1.46067357762199,2.8727252326291));
#68505=CARTESIAN_POINT('Ctrl Pts',(18.6841859841906,-1.46068573106895,2.87271905302245));
#68506=CARTESIAN_POINT('Ctrl Pts',(18.6841864066461,-1.46069179915524,2.87271596758665));
#68507=CARTESIAN_POINT('Ctrl Pts',(18.6841872503922,-1.46070391861135,2.87270980516652));
#68508=CARTESIAN_POINT('Ctrl Pts',(18.6841876716662,-1.4607099697425,2.87270672830369));
#68509=CARTESIAN_POINT('Ctrl Pts',(18.6841885130783,-1.46072205570476,2.87270058281817));
#68510=CARTESIAN_POINT('Ctrl Pts',(18.6841889331813,-1.46072809003067,2.87269751445249));
#68511=CARTESIAN_POINT('Ctrl Pts',(18.6841897722531,-1.46074014240808,2.87269138594864));
#68512=CARTESIAN_POINT('Ctrl Pts',(18.6841901911871,-1.46074615995923,2.87268832606503));
#68513=CARTESIAN_POINT('Ctrl Pts',(18.6841910279453,-1.46075817913488,2.87268221434885));
#68514=CARTESIAN_POINT('Ctrl Pts',(18.684191445729,-1.46076418017749,2.87267916281231));
#68515=CARTESIAN_POINT('Ctrl Pts',(18.6841922801366,-1.46077616561937,2.87267306815513));
#68516=CARTESIAN_POINT('Ctrl Pts',(18.6841926967576,-1.46078214997686,2.87267002505586));
#68517=CARTESIAN_POINT('Ctrl Pts',(18.6841935288435,-1.46079410210191,2.87266394724643));
#68518=CARTESIAN_POINT('Ctrl Pts',(18.684193944294,-1.4608000696619,2.87266091264197));
#68519=CARTESIAN_POINT('Ctrl Pts',(18.6841947741202,-1.46081198935764,2.87265485122977));
#68520=CARTESIAN_POINT('Ctrl Pts',(18.6841951884342,-1.46081794060716,2.87265182487283));
#68521=CARTESIAN_POINT('Ctrl Pts',(18.6844709114871,-1.46477846073263,2.87063778736576));
#68522=CARTESIAN_POINT('Ctrl Pts',(18.68474569995,-1.46872890091856,2.86861859811481));
#68523=CARTESIAN_POINT('Ctrl Pts',(18.6854750564779,-1.47922277631883,2.86322750164909));
#68524=CARTESIAN_POINT('Ctrl Pts',(18.6859287292191,-1.48575889714807,2.85984129808454));
#68525=CARTESIAN_POINT('Ctrl Pts',(18.6869281793814,-1.50017565401075,2.8523095654072));
#68526=CARTESIAN_POINT('Ctrl Pts',(18.6874733243851,-1.50805085773481,2.8481536939787));
#68527=CARTESIAN_POINT('Ctrl Pts',(18.6891006642262,-1.5315901730399,2.83560661484554));
#68528=CARTESIAN_POINT('Ctrl Pts',(18.6901771619395,-1.54720249322364,2.82711828696506));
#68529=CARTESIAN_POINT('Ctrl Pts',(18.694036143216,-1.60327516571804,2.79602827086923));
#68530=CARTESIAN_POINT('Ctrl Pts',(18.696778131406,-1.64331885159899,2.77268262778019));
#68531=CARTESIAN_POINT('Ctrl Pts',(18.7062765686993,-1.78202583038118,2.68775473309759));
#68532=CARTESIAN_POINT('Ctrl Pts',(18.7128414671115,-1.87785225682153,2.62170102572494));
#68533=CARTESIAN_POINT('Ctrl Pts',(18.7351687553292,-2.19314880293415,2.37818887708171));
#68534=CARTESIAN_POINT('Ctrl Pts',(18.7507272520347,-2.39276519082314,2.17723264891625));
#68535=CARTESIAN_POINT('Ctrl Pts',(18.7682333897745,-2.56995237866755,1.9446258434106));
#68536=CARTESIAN_POINT('Ctrl Pts',(18.7688551435811,-2.57619053772006,1.93635410220001));
#68537=CARTESIAN_POINT('Ctrl Pts',(18.7709658706776,-2.59718065100408,1.90824043289281));
#68538=CARTESIAN_POINT('Ctrl Pts',(18.772461901902,-2.61174383850366,1.88825923894307));
#68539=CARTESIAN_POINT('Ctrl Pts',(18.7745469773166,-2.63160009617297,1.86034656300099));
#68540=CARTESIAN_POINT('Ctrl Pts',(18.7751284311644,-2.63709029435138,1.85255584990574));
#68541=CARTESIAN_POINT('Ctrl Pts',(18.7761306277284,-2.64647206549712,1.83911669475803));
#68542=CARTESIAN_POINT('Ctrl Pts',(18.7765507291151,-2.65038033389599,1.83347994124274));
#68543=CARTESIAN_POINT('Ctrl Pts',(18.7774181756086,-2.65839992538469,1.82183435255886));
#68544=CARTESIAN_POINT('Ctrl Pts',(18.7778656053226,-2.66250893744366,1.81582398048249));
#68545=CARTESIAN_POINT('Ctrl Pts',(18.7789078034674,-2.67201597139271,1.80181611425027));
#68546=CARTESIAN_POINT('Ctrl Pts',(18.7795031540309,-2.67739849299595,1.79380823038807));
#68547=CARTESIAN_POINT('Ctrl Pts',(18.7814047516953,-2.69443632822417,1.76821254724416));
#68548=CARTESIAN_POINT('Ctrl Pts',(18.7827161232096,-2.70595473348776,1.7505346855386));
#68549=CARTESIAN_POINT('Ctrl Pts',(18.796955438228,-2.82851975276614,1.55832770704123));
#68550=CARTESIAN_POINT('Ctrl Pts',(18.810518611536,-2.92266862332685,1.37364057529463));
#68551=CARTESIAN_POINT('Ctrl Pts',(18.8362270285434,-3.06282551573948,1.01786593336279));
#68552=CARTESIAN_POINT('Ctrl Pts',(18.8482228433012,-3.11372614614363,0.84950627088044));
#68553=CARTESIAN_POINT('Ctrl Pts',(18.8618745076466,-3.15686347303331,0.648999801147239));
#68554=CARTESIAN_POINT('Ctrl Pts',(18.8638281707892,-3.16267180529422,0.620076502959375));
#68555=CARTESIAN_POINT('Ctrl Pts',(18.8703929424111,-3.1809727708513,0.521986097404746));
#68556=CARTESIAN_POINT('Ctrl Pts',(18.874942651001,-3.1916007672669,0.452485929125252));
#68557=CARTESIAN_POINT('Ctrl Pts',(18.8800411533158,-3.2012029426253,0.372194797411296));
#68558=CARTESIAN_POINT('Ctrl Pts',(18.8807047899899,-3.2024062579273,0.361695194360419));
#68559=CARTESIAN_POINT('Ctrl Pts',(18.8816873632619,-3.20411873890622,0.346073915746262));
#68560=CARTESIAN_POINT('Ctrl Pts',(18.8820084681183,-3.20466730495548,0.34095676206605));
#68561=CARTESIAN_POINT('Ctrl Pts',(18.8825796246021,-3.20562331706386,0.331832687463649));
#68562=CARTESIAN_POINT('Ctrl Pts',(18.8828299422166,-3.20603551076065,0.32782630729504));
#68563=CARTESIAN_POINT('Ctrl Pts',(18.8833145048134,-3.20682024522696,0.320055906575915));
#68564=CARTESIAN_POINT('Ctrl Pts',(18.8835487997507,-3.20719366770239,0.316292027614158));
#68565=CARTESIAN_POINT('Ctrl Pts',(18.8840630801918,-3.20800007045058,0.308015681483374));
#68566=CARTESIAN_POINT('Ctrl Pts',(18.8843429031406,-3.20843015872852,0.303502931127059));
#68567=CARTESIAN_POINT('Ctrl Pts',(18.8850316171246,-3.2094672166819,0.29237288514179));
#68568=CARTESIAN_POINT('Ctrl Pts',(18.885439906633,-3.21006324774873,0.2857545558346));
#68569=CARTESIAN_POINT('Ctrl Pts',(18.8874029618911,-3.21283794034375,0.253839690028737));
#68570=CARTESIAN_POINT('Ctrl Pts',(18.8889428689628,-3.21473815024191,0.228519006920698));
#68571=CARTESIAN_POINT('Ctrl Pts',(18.8945016334168,-3.22056952438101,0.136207284159294));
#68572=CARTESIAN_POINT('Ctrl Pts',(18.8984358349785,-3.22270761219489,0.0691171422643548));
#68573=CARTESIAN_POINT('Ctrl Pts',(18.9023083833077,-3.22274937597677,0.00200552769956143));
#68574=CARTESIAN_POINT('Ctrl Pts',(18.9023081109937,-3.22274937303652,0.0020102469239669));
#68575=CARTESIAN_POINT('Ctrl Pts',(18.9195468469855,-3.22293572278098,-0.29673838686921));
#68576=CARTESIAN_POINT('Ctrl Pts',(18.9355977504742,-3.18158379616016,-0.594088851345514));
#68577=CARTESIAN_POINT('Ctrl Pts',(18.9567435757215,-3.08170305669619,-0.945316117520925));
#68578=CARTESIAN_POINT('Ctrl Pts',(18.9606333022897,-3.061597713524,-1.00853105112119));
#68579=CARTESIAN_POINT('Ctrl Pts',(18.9670453919786,-3.02582990050013,-1.11003470961203));
#68580=CARTESIAN_POINT('Ctrl Pts',(18.9695294300397,-3.01135515118264,-1.14872257692395));
#68581=CARTESIAN_POINT('Ctrl Pts',(18.9728006031635,-2.99151929683866,-1.19878576325663));
#68582=CARTESIAN_POINT('Ctrl Pts',(18.9735650997096,-2.98682920126305,-1.2104240269658));
#68583=CARTESIAN_POINT('Ctrl Pts',(18.9748127150365,-2.97908784689376,-1.22931487759577));
#68584=CARTESIAN_POINT('Ctrl Pts',(18.9752944357453,-2.97607775321187,-1.2365842765004));
#68585=CARTESIAN_POINT('Ctrl Pts',(18.9762223411069,-2.97023941000974,-1.25053912515274));
#68586=CARTESIAN_POINT('Ctrl Pts',(18.9766683883441,-2.96741513051169,-1.25722619211876));
#68587=CARTESIAN_POINT('Ctrl Pts',(18.9776904036008,-2.96090354187435,-1.27249954762327));
#68588=CARTESIAN_POINT('Ctrl Pts',(18.9782668740921,-2.95720144507192,-1.28107942505656));
#68589=CARTESIAN_POINT('Ctrl Pts',(18.9797972805776,-2.9472963411418,-1.30376349268296));
#68590=CARTESIAN_POINT('Ctrl Pts',(18.9807533998814,-2.94102946844005,-1.31783937558592));
#68591=CARTESIAN_POINT('Ctrl Pts',(18.9873378469139,-2.89733798955403,-1.41410985412766));
#68592=CARTESIAN_POINT('Ctrl Pts',(18.9930810500932,-2.85657687981357,-1.49473743890401));
#68593=CARTESIAN_POINT('Ctrl Pts',(19.0016449537475,-2.79205539432489,-1.6100606741569));
#68594=CARTESIAN_POINT('Ctrl Pts',(19.0043791285299,-2.7709147162206,-1.64617742202777));
#68595=CARTESIAN_POINT('Ctrl Pts',(19.0200950127406,-2.64629319190259,-1.8498756819759));
#68596=CARTESIAN_POINT('Ctrl Pts',(19.0334970490938,-2.52833077215714,-2.008093287704));
#68597=CARTESIAN_POINT('Ctrl Pts',(19.0536628440086,-2.32858226792262,-2.23029106093209));
#68598=CARTESIAN_POINT('Ctrl Pts',(19.0604898934677,-2.2569249137759,-2.30277794456624));
#68599=CARTESIAN_POINT('Ctrl Pts',(19.0697388502625,-2.15282297989842,-2.39854897784718));
#68600=CARTESIAN_POINT('Ctrl Pts',(19.072300640028,-2.12320330959228,-2.42480761971353));
#68601=CARTESIAN_POINT('Ctrl Pts',(19.0758429349648,-2.08103133123277,-2.46082878928617));
#68602=CARTESIAN_POINT('Ctrl Pts',(19.0768516905573,-2.0688802740121,-2.47105325047359));
#68603=CARTESIAN_POINT('Ctrl Pts',(19.0785936213724,-2.04764146121901,-2.48865807989506));
#68604=CARTESIAN_POINT('Ctrl Pts',(19.0793295196284,-2.03858826010307,-2.49607942742557));
#68605=CARTESIAN_POINT('Ctrl Pts',(19.0803980093954,-2.02532215566365,-2.50683397531472));
#68606=CARTESIAN_POINT('Ctrl Pts',(19.080733341867,-2.02114116458665,-2.51020612855282));
#68607=CARTESIAN_POINT('Ctrl Pts',(19.0813068557279,-2.0139599064157,-2.51596855549932));
#68608=CARTESIAN_POINT('Ctrl Pts',(19.0815454059082,-2.01096377745318,-2.51836394575818));
#68609=CARTESIAN_POINT('Ctrl Pts',(19.0820210370105,-2.00497159709823,-2.52313715188626));
#68610=CARTESIAN_POINT('Ctrl Pts',(19.0822581199902,-2.00197559359882,-2.52551498023637));
#68611=CARTESIAN_POINT('Ctrl Pts',(19.0828250551498,-1.99478957741151,-2.53119745988811));
#68612=CARTESIAN_POINT('Ctrl Pts',(19.0831545460625,-1.99059555934513,-2.53449706237245));
#68613=CARTESIAN_POINT('Ctrl Pts',(19.0843382355519,-1.97546592575178,-2.54633943212475));
#68614=CARTESIAN_POINT('Ctrl Pts',(19.0851882538767,-1.96448316397013,-2.55482211552728));
#68615=CARTESIAN_POINT('Ctrl Pts',(19.0872300856562,-1.93782671200865,-2.57513705235195));
#68616=CARTESIAN_POINT('Ctrl Pts',(19.0884172700055,-1.92209880590669,-2.58689764505222));
#68617=CARTESIAN_POINT('Ctrl Pts',(19.1033631089563,-1.72135179479103,-2.73416519312427));
#68618=CARTESIAN_POINT('Ctrl Pts',(19.1159908096351,-1.52246130869292,-2.84971101512472));
#68619=CARTESIAN_POINT('Ctrl Pts',(19.1414042041509,-1.10763575568693,-3.03476691685052));
#68620=CARTESIAN_POINT('Ctrl Pts',(19.1541295882859,-0.893318733522047,
-3.10461415695245));
#68621=CARTESIAN_POINT('Ctrl Pts',(19.1690739985333,-0.650708539150723,
-3.15645985714619));
#68622=CARTESIAN_POINT('Ctrl Pts',(19.1704851698305,-0.627871768440136,
-3.16108168689464));
#68623=CARTESIAN_POINT('Ctrl Pts',(19.1725161237013,-0.595120116044307,
-3.16734123967173));
#68624=CARTESIAN_POINT('Ctrl Pts',(19.1731294552611,-0.585244215527582,
-3.16918091715226));
#68625=CARTESIAN_POINT('Ctrl Pts',(19.1741939060691,-0.568130981929209,
-3.17228604140608));
#68626=CARTESIAN_POINT('Ctrl Pts',(19.1746443367307,-0.560897585502903,
-3.17357297667568));
#68627=CARTESIAN_POINT('Ctrl Pts',(19.1755105428876,-0.547003429586606,
-3.1759959802576));
#68628=CARTESIAN_POINT('Ctrl Pts',(19.1759261943944,-0.540343366909256,
-3.17713585849257));
#68629=CARTESIAN_POINT('Ctrl Pts',(19.1769053955744,-0.524670437350793,
-3.1797675940332));
#68630=CARTESIAN_POINT('Ctrl Pts',(19.1774694948035,-0.515654749329727,
-3.18124208393997));
#68631=CARTESIAN_POINT('Ctrl Pts',(19.1791372364645,-0.489039973718108,
-3.1854787432568));
#68632=CARTESIAN_POINT('Ctrl Pts',(19.180244283749,-0.47142433346498,-3.1881333091497));
#68633=CARTESIAN_POINT('Ctrl Pts',(19.1955012724945,-0.229380358965879,
-3.22255792709559));
#68634=CARTESIAN_POINT('Ctrl Pts',(19.2104259549474,-0.00227779418153801,
-3.23070457876806));
#68635=CARTESIAN_POINT('Ctrl Pts',(19.2383467692494,0.410827569834983,-3.20195296405217));
#68636=CARTESIAN_POINT('Ctrl Pts',(19.25116025723,0.59640741267276,-3.17263051532355));
#68637=CARTESIAN_POINT('Ctrl Pts',(19.2666534464151,0.824945988472334,-3.11574767733978));
#68638=CARTESIAN_POINT('Ctrl Pts',(19.2697751598095,0.871241837265544,-3.10312063028053));
#68639=CARTESIAN_POINT('Ctrl Pts',(19.2740152450062,0.934699273685092,-3.08428054678533));
#68640=CARTESIAN_POINT('Ctrl Pts',(19.2751747590292,0.952113850784152,-3.07894924819312));
#68641=CARTESIAN_POINT('Ctrl Pts',(19.2768996563874,0.97812655918964,-3.0707439076663));
#68642=CARTESIAN_POINT('Ctrl Pts',(19.2774708904556,0.986758955563268,-3.06798084746457));
#68643=CARTESIAN_POINT('Ctrl Pts',(19.2785067135553,1.00244681280718,-3.06288641005989));
#68644=CARTESIAN_POINT('Ctrl Pts',(19.2789719660595,1.00950605243815,-3.06056699095498));
#68645=CARTESIAN_POINT('Ctrl Pts',(19.2797148610513,1.02079966756017,-3.05681297883345));
#68646=CARTESIAN_POINT('Ctrl Pts',(19.2799934097384,1.02503913751544,-3.05539397066856));
#68647=CARTESIAN_POINT('Ctrl Pts',(19.2805222645747,1.03309790130835,-3.0526779321963));
#68648=CARTESIAN_POINT('Ctrl Pts',(19.2807726614675,1.03691766787931,-3.05138256887592));
#68649=CARTESIAN_POINT('Ctrl Pts',(19.2813450695905,1.04565907643052,-3.04839986341412));
#68650=CARTESIAN_POINT('Ctrl Pts',(19.2816667953427,1.05057906152651,-3.04670777525024));
#68651=CARTESIAN_POINT('Ctrl Pts',(19.2826575403915,1.06575014572033,-3.04144899586515));
#68652=CARTESIAN_POINT('Ctrl Pts',(19.283324228998,1.07598747053171,-3.03784238213104));
#68653=CARTESIAN_POINT('Ctrl Pts',(19.2887631296341,1.15971543410778,-3.0078686360866));
#68654=CARTESIAN_POINT('Ctrl Pts',(19.2933881634955,1.23225066000184,-2.9788880777403));
#68655=CARTESIAN_POINT('Ctrl Pts',(19.3152928300221,1.57731349268273,-2.82625769550204));
#68656=CARTESIAN_POINT('Ctrl Pts',(19.331344018382,1.83278134337235,-2.66769432609381));
#68657=CARTESIAN_POINT('Ctrl Pts',(19.3528508765832,2.11938731689852,-2.42894099797097));
#68658=CARTESIAN_POINT('Ctrl Pts',(19.3571607082895,2.17441326483933,-2.37980730101956));
#68659=CARTESIAN_POINT('Ctrl Pts',(19.363300864777,2.24902466230523,-2.30843588754094));
#68660=CARTESIAN_POINT('Ctrl Pts',(19.3650672573436,2.27006485408745,-2.28774859884894));
#68661=CARTESIAN_POINT('Ctrl Pts',(19.3681756822099,2.30632898732159,-2.25109984372946));
#68662=CARTESIAN_POINT('Ctrl Pts',(19.3695121309953,2.32167882765504,-2.23526537309219));
#68663=CARTESIAN_POINT('Ctrl Pts',(19.3714541900308,2.34362972834558,-2.21215138939556));
#68664=CARTESIAN_POINT('Ctrl Pts',(19.3720541096453,2.35036212944019,-2.20499703635156));
#68665=CARTESIAN_POINT('Ctrl Pts',(19.37310282391,2.36204606663375,-2.19246650170605));
#68666=CARTESIAN_POINT('Ctrl Pts',(19.3735509861827,2.36701224562379,-2.18710402351447));
#68667=CARTESIAN_POINT('Ctrl Pts',(19.3744182691767,2.37657066735608,-2.17671215569577));
#68668=CARTESIAN_POINT('Ctrl Pts',(19.3748372846858,2.38116529759328,-2.17168500710666));
#68669=CARTESIAN_POINT('Ctrl Pts',(19.3759450511905,2.39325038769828,-2.15837781919581));
#68670=CARTESIAN_POINT('Ctrl Pts',(19.3766349421564,2.4007137627231,-2.15007340643303));
#68671=CARTESIAN_POINT('Ctrl Pts',(19.379066644222,2.42679829357903,-2.12074430061063));
#68672=CARTESIAN_POINT('Ctrl Pts',(19.3808181120334,2.44518720365318,-2.09951561195235));
#68673=CARTESIAN_POINT('Ctrl Pts',(19.38306372346,2.46825332616384,-2.07217330125616));
#68674=CARTESIAN_POINT('Ctrl Pts',(19.3835472137446,2.47318971572936,-2.06627909560131));
#68675=CARTESIAN_POINT('Ctrl Pts',(19.3992427125922,2.6324713538276,-1.87470324959702));
#68676=CARTESIAN_POINT('Ctrl Pts',(19.4153336306336,2.76545452620205,-1.67231467599055));
#68677=CARTESIAN_POINT('Ctrl Pts',(19.43978351188,2.92884217398956,-1.34996569972591));
#68678=CARTESIAN_POINT('Ctrl Pts',(19.4479275172098,2.9770849851421,-1.23995583202116));
#68679=CARTESIAN_POINT('Ctrl Pts',(19.4606189171491,3.04373297815114,-1.06149547851009));
#68680=CARTESIAN_POINT('Ctrl Pts',(19.4652585351681,3.06621638360191,-0.99468666545364));
#68681=CARTESIAN_POINT('Ctrl Pts',(19.4721207848168,3.09684534732681,-0.89272691668536));
#68682=CARTESIAN_POINT('Ctrl Pts',(19.4744145080525,3.10662076315755,-0.858090991551482));
#68683=CARTESIAN_POINT('Ctrl Pts',(19.4771896088989,3.11789985002776,-0.815404638342351));
#68684=CARTESIAN_POINT('Ctrl Pts',(19.4777010542599,3.11995526729352,-0.807504385468357));
#68685=CARTESIAN_POINT('Ctrl Pts',(19.4785005696449,3.12313210721124,-0.795100585288707));
#68686=CARTESIAN_POINT('Ctrl Pts',(19.4787897975237,3.12427384015181,-0.790602347714645));
#68687=CARTESIAN_POINT('Ctrl Pts',(19.4793286036165,3.12638683920144,-0.782201424224416));
#68688=CARTESIAN_POINT('Ctrl Pts',(19.4795783161567,3.12736050650948,-0.7782994275778));
#68689=CARTESIAN_POINT('Ctrl Pts',(19.4801426100491,3.12954800968427,-0.769462567671047));
#68690=CARTESIAN_POINT('Ctrl Pts',(19.4804569359534,3.1307574754239,-0.76452666329324));
#68691=CARTESIAN_POINT('Ctrl Pts',(19.4813826829569,3.13429265157615,-0.749950320125462));
#68692=CARTESIAN_POINT('Ctrl Pts',(19.4819922384185,3.13658557119324,-0.740301876927223));
#68693=CARTESIAN_POINT('Ctrl Pts',(19.4861618193415,3.15202629402446,-0.673968695595575));
#68694=CARTESIAN_POINT('Ctrl Pts',(19.489640590406,3.16368225291094,-0.616943401790247));
#68695=CARTESIAN_POINT('Ctrl Pts',(19.5116329106778,3.22867951346079,-0.248329020418671));
#68696=CARTESIAN_POINT('Ctrl Pts',(19.5284918153321,3.23747933245778,0.0693773877777829));
#68697=CARTESIAN_POINT('Ctrl Pts',(19.551101347747,3.19076258393137,0.459368671516029));
#68698=CARTESIAN_POINT('Ctrl Pts',(19.5555716426548,3.17894332183028,0.53507340137765));
#68699=CARTESIAN_POINT('Ctrl Pts',(19.5628542757283,3.15573701976109,0.655403009036923));
#68700=CARTESIAN_POINT('Ctrl Pts',(19.5656134022081,3.14607132942601,0.700331426457077));
#68701=CARTESIAN_POINT('Ctrl Pts',(19.569194947626,3.13243489022064,0.757719721663582));
#68702=CARTESIAN_POINT('Ctrl Pts',(19.5699889557391,3.12934416400893,0.770384717814093));
#68703=CARTESIAN_POINT('Ctrl Pts',(19.5712728017207,3.12423859589389,0.790768226232197));
#68704=CARTESIAN_POINT('Ctrl Pts',(19.5717610841462,3.12227177021382,0.798498705576408));
#68705=CARTESIAN_POINT('Ctrl Pts',(19.5726936563804,3.11846782146986,0.813220921952253));
#68706=CARTESIAN_POINT('Ctrl Pts',(19.5731377772321,3.11663583132536,0.820213944642812));
#68707=CARTESIAN_POINT('Ctrl Pts',(19.5741538189433,3.11239821819931,0.836170452012708));
#68708=CARTESIAN_POINT('Ctrl Pts',(19.5747262312626,3.10997738204567,0.84512979698253));
#68709=CARTESIAN_POINT('Ctrl Pts',(19.5762184919233,3.10357971890653,0.868407344718188));
#68710=CARTESIAN_POINT('Ctrl Pts',(19.577140299399,3.0995425324689,0.88270859601125));
#68711=CARTESIAN_POINT('Ctrl Pts',(19.5830607740857,3.07307198648957,0.97405622009607));
#68712=CARTESIAN_POINT('Ctrl Pts',(19.5881496000922,3.04786821438571,1.05026399134539));
#68713=CARTESIAN_POINT('Ctrl Pts',(19.5973198522107,2.99823172025703,1.18345083601292));
#68714=CARTESIAN_POINT('Ctrl Pts',(19.6013635934688,2.97494905316397,1.24081695350646));
#68715=CARTESIAN_POINT('Ctrl Pts',(19.6055919894123,2.94915916808336,1.29945467172816));
#68716=CARTESIAN_POINT('Ctrl Pts',(19.6057348377648,2.94828621570922,1.30143406777099));
#68717=CARTESIAN_POINT('Ctrl Pts',(19.6223122847033,2.84678458359205,1.53096005240015));
#68718=CARTESIAN_POINT('Ctrl Pts',(19.6394337723317,2.72015890655008,1.74606403498391));
#68719=CARTESIAN_POINT('Ctrl Pts',(19.660372700055,2.53013896625822,1.99722129746198));
#68720=CARTESIAN_POINT('Ctrl Pts',(19.6647204357496,2.48859631533556,2.04875222008995));
#68721=CARTESIAN_POINT('Ctrl Pts',(19.6712007096994,2.42304801360427,2.12512201853792));
#68722=CARTESIAN_POINT('Ctrl Pts',(19.6733958550939,2.40018308930761,2.15091297820777));
#68723=CARTESIAN_POINT('Ctrl Pts',(19.6760678633841,2.37147058838699,2.18227166883929));
#68724=CARTESIAN_POINT('Ctrl Pts',(19.676572251571,2.36601112074458,2.18818960970238));
#68725=CARTESIAN_POINT('Ctrl Pts',(19.6773631934099,2.35738672497007,2.19746824786598));
#68726=CARTESIAN_POINT('Ctrl Pts',(19.6776508648295,2.35423670217204,2.20084266185227));
#68727=CARTESIAN_POINT('Ctrl Pts',(19.6781883015933,2.34832662894692,2.20714653012446));
#68728=CARTESIAN_POINT('Ctrl Pts',(19.6784381944949,2.34556837135872,2.2100775500367));
#68729=CARTESIAN_POINT('Ctrl Pts',(19.6790048762536,2.33929028446925,2.21672387079241));
#68730=CARTESIAN_POINT('Ctrl Pts',(19.679321400731,2.33576710040752,2.22043594995841));
#68731=CARTESIAN_POINT('Ctrl Pts',(19.6802806086358,2.3250407105294,2.23168365309842));
#68732=CARTESIAN_POINT('Ctrl Pts',(19.6809211712189,2.31780968464217,2.2391928246317));
#68733=CARTESIAN_POINT('Ctrl Pts',(19.6856426191976,2.26402018096327,2.2945116260712));
#68734=CARTESIAN_POINT('Ctrl Pts',(19.6896163296568,2.21601937774936,2.34090379121807));
#68735=CARTESIAN_POINT('Ctrl Pts',(19.7028634509873,2.04821004438332,2.49329749758059));
#68736=CARTESIAN_POINT('Ctrl Pts',(19.7117666141936,1.92212096769904,2.59172161007445));
#68737=CARTESIAN_POINT('Ctrl Pts',(19.7206814315572,1.78943602647606,2.6803052568037));
#68738=CARTESIAN_POINT('Origin',(-1.72497344927317,0.,0.));
#68739=CARTESIAN_POINT('',(21.2168443958857,1.78943621037803,2.68030513402633));
#68740=CARTESIAN_POINT('',(20.9673281879432,1.78943621037181,2.68030513403048));
#68741=CARTESIAN_POINT('',(-1.72497344927317,1.78943621037804,2.68030513402633));
#68742=CARTESIAN_POINT('',(20.3965734493048,-3.22274885406294,-0.00271774465727977));
#68743=CARTESIAN_POINT('Ctrl Pts',(20.3965734493048,-3.22274885406294,-0.0027177446573006));
#68744=CARTESIAN_POINT('Ctrl Pts',(20.4039084698346,-3.22264841945202,-0.121814852024652));
#68745=CARTESIAN_POINT('Ctrl Pts',(20.4112434903643,-3.21594228569994,-0.24062621396647));
#68746=CARTESIAN_POINT('Ctrl Pts',(20.4185785108941,-3.20274814338226,-0.358499501480124));
#68747=CARTESIAN_POINT('Ctrl Pts',(20.4260054409484,-3.18938867537232,-0.477849768882879));
#68748=CARTESIAN_POINT('Ctrl Pts',(20.4334323710027,-3.16937766417932,-0.596238263840522));
#68749=CARTESIAN_POINT('Ctrl Pts',(20.4408593010569,-3.14288643768406,-0.713009398480532));
#68750=CARTESIAN_POINT('Ctrl Pts',(20.4466239616218,-3.12232438477968,-0.803645226482011));
#68751=CARTESIAN_POINT('Ctrl Pts',(20.4523886221867,-3.09785925306823,-0.893307093579976));
#68752=CARTESIAN_POINT('Ctrl Pts',(20.4581532827517,-3.06959081273735,-0.981697410029416));
#68753=CARTESIAN_POINT('Ctrl Pts',(20.4643255308444,-3.03932366605053,-1.07633732091077));
#68754=CARTESIAN_POINT('Ctrl Pts',(20.4704977789372,-3.00462231767946,-1.16974272713076));
#68755=CARTESIAN_POINT('Ctrl Pts',(20.47667002703,-2.96560566779542,-1.26146763162582));
#68756=CARTESIAN_POINT('Ctrl Pts',(20.4828339156826,-2.92664186046469,-1.35306830766535));
#68757=CARTESIAN_POINT('Ctrl Pts',(20.4889978043352,-2.88337453667252,-1.44299260958903));
#68758=CARTESIAN_POINT('Ctrl Pts',(20.4951616929879,-2.83597231254074,-1.53080978733556));
#68759=CARTESIAN_POINT('Ctrl Pts',(20.5013190546464,-2.78862028302699,-1.61853397472617));
#68760=CARTESIAN_POINT('Ctrl Pts',(20.507476416305,-2.73714226319858,-1.70415509374264));
#68761=CARTESIAN_POINT('Ctrl Pts',(20.5136337779635,-2.68175450101443,-1.7872633714114));
#68762=CARTESIAN_POINT('Ctrl Pts',(20.5197866421098,-2.62640719562852,-1.87031094442828));
#68763=CARTESIAN_POINT('Ctrl Pts',(20.5259395062561,-2.5671560658485,-1.95084896491966));
#68764=CARTESIAN_POINT('Ctrl Pts',(20.5320923704024,-2.50426226509231,-2.02849403995544));
#68765=CARTESIAN_POINT('Ctrl Pts',(20.538242903539,-2.44139229162379,-2.10610969919003));
#68766=CARTESIAN_POINT('Ctrl Pts',(20.5443934366755,-2.37488266238489,-2.18083425353745));
#68767=CARTESIAN_POINT('Ctrl Pts',(20.5505439698121,-2.30503611580601,-2.25231571217934));
#68768=CARTESIAN_POINT('Ctrl Pts',(20.5566938180273,-2.23519734731543,-2.32378921066968));
#68769=CARTESIAN_POINT('Ctrl Pts',(20.5628436662425,-2.16202270385255,-2.3920200207912));
#68770=CARTESIAN_POINT('Ctrl Pts',(20.5689935144577,-2.08585253992285,-2.4566922363612));
#68771=CARTESIAN_POINT('Ctrl Pts',(20.5751443228368,-2.00967048369248,-2.52137454907939));
#68772=CARTESIAN_POINT('Ctrl Pts',(20.581295131216,-1.93049230920649,-2.5824968825218));
#68773=CARTESIAN_POINT('Ctrl Pts',(20.5874459395951,-1.84869148110703,-2.63978358396712));
#68774=CARTESIAN_POINT('Ctrl Pts',(20.5936033259613,-1.76680317104507,-2.69713155072214));
#68775=CARTESIAN_POINT('Ctrl Pts',(20.5997607123275,-1.68228696297001,-2.75063544451039));
#68776=CARTESIAN_POINT('Ctrl Pts',(20.6059180986937,-1.59554524191772,-2.80006302491457));
#68777=CARTESIAN_POINT('Ctrl Pts',(20.6120789214306,-1.50875511124853,-2.84951819031709));
#68778=CARTESIAN_POINT('Ctrl Pts',(20.6182397441676,-1.41973738112053,-2.89489231454284));
#68779=CARTESIAN_POINT('Ctrl Pts',(20.6244005669046,-1.32891708296139,-2.93600016163375));
#68780=CARTESIAN_POINT('Ctrl Pts',(20.6305716898213,-1.23794494381707,-2.97717673626825));
#68781=CARTESIAN_POINT('Ctrl Pts',(20.636742812738,-1.1451646207189,-3.01407262579408));
#68782=CARTESIAN_POINT('Ctrl Pts',(20.6429139356546,-1.05101919823025,-3.0465515271289));
#68783=CARTESIAN_POINT('Ctrl Pts',(20.6476094576002,-0.979385250351234,
-3.07126427326021));
#68784=CARTESIAN_POINT('Ctrl Pts',(20.6523049795458,-0.906961354554591,
-3.09342082858202));
#68785=CARTESIAN_POINT('Ctrl Pts',(20.6570005014913,-0.833946570311851,
-3.1129809958246));
#68786=CARTESIAN_POINT('Ctrl Pts',(20.6631727495841,-0.737968877520492,
-3.13869277107705));
#68787=CARTESIAN_POINT('Ctrl Pts',(20.6693449976769,-0.640632042801461,
-3.1600069470349));
#68788=CARTESIAN_POINT('Ctrl Pts',(20.6755172457696,-0.542375533400338,
-3.17678238840319));
#68789=CARTESIAN_POINT('Ctrl Pts',(20.6816811344222,-0.44425209859308,-3.19353510980046));
#68790=CARTESIAN_POINT('Ctrl Pts',(20.6878450230749,-0.345211889220213,
-3.20576124213907));
#68791=CARTESIAN_POINT('Ctrl Pts',(20.6940089117275,-0.245708428536648,
-3.21336971583508));
#68792=CARTESIAN_POINT('Ctrl Pts',(20.7001662733861,-0.14631033291329,-3.22097013285364));
#68793=CARTESIAN_POINT('Ctrl Pts',(20.7063236350446,-0.0464503919433015,
-3.22396257943623));
#68794=CARTESIAN_POINT('Ctrl Pts',(20.7124809967031,0.053409762209582,-3.22230739685101));
#68795=CARTESIAN_POINT('Ctrl Pts',(20.7186338608495,0.153196975663071,-3.22065342325826));
#68796=CARTESIAN_POINT('Ctrl Pts',(20.7247867249958,0.25298396898358,-3.21435857703962));
#68797=CARTESIAN_POINT('Ctrl Pts',(20.7309395891421,0.352307020293586,-3.20343523829527));
#68798=CARTESIAN_POINT('Ctrl Pts',(20.7370901222786,0.451592443111013,-3.1925160378528));
#68799=CARTESIAN_POINT('Ctrl Pts',(20.7432406554151,0.550413841867864,-3.17697187651682));
#68800=CARTESIAN_POINT('Ctrl Pts',(20.7493911885517,0.648311424980942,-3.15686709551403));
#68801=CARTESIAN_POINT('Ctrl Pts',(20.7555410367669,0.746198106251643,-3.13676455337298));
#68802=CARTESIAN_POINT('Ctrl Pts',(20.7616908849821,0.843160750914965,-3.11210248866523));
#68803=CARTESIAN_POINT('Ctrl Pts',(20.7678407331973,0.938749582707908,-3.08299639692714));
#68804=CARTESIAN_POINT('Ctrl Pts',(20.7739915415764,1.03435333860067,-3.05388576091112));
#68805=CARTESIAN_POINT('Ctrl Pts',(20.7801423499556,1.12858244001119,-3.02032984626491));
#68806=CARTESIAN_POINT('Ctrl Pts',(20.7862931583347,1.22100306925711,-2.98249376652571));
#68807=CARTESIAN_POINT('Ctrl Pts',(20.7924505447009,1.31352253782048,-2.94461722296012));
#68808=CARTESIAN_POINT('Ctrl Pts',(20.7986079310671,1.40422926930088,-2.9024515385471));
#68809=CARTESIAN_POINT('Ctrl Pts',(20.8047653174333,1.49271032728007,-2.85620962839414));
#68810=CARTESIAN_POINT('Ctrl Pts',(20.8109261401702,1.58124076558128,-2.80994191113099));
#68811=CARTESIAN_POINT('Ctrl Pts',(20.8170869629072,1.66754268150185,-2.75959365659507));
#68812=CARTESIAN_POINT('Ctrl Pts',(20.8232477856442,1.75123043405774,-2.70542224603295));
#68813=CARTESIAN_POINT('Ctrl Pts',(20.8294189085608,1.8350581028114,-2.65116026716706));
#68814=CARTESIAN_POINT('Ctrl Pts',(20.8355900314775,1.91626252467126,-2.59306261757174));
#68815=CARTESIAN_POINT('Ctrl Pts',(20.8417611543942,1.99448945990918,-2.53142832345915));
#68816=CARTESIAN_POINT('Ctrl Pts',(20.8464566763398,2.054011251341,-2.48453164282019));
#68817=CARTESIAN_POINT('Ctrl Pts',(20.8511521982854,2.11180988520511,-2.43558829240713));
#68818=CARTESIAN_POINT('Ctrl Pts',(20.855847720231,2.1677439137054,-2.38474398774653));
#68819=CARTESIAN_POINT('Ctrl Pts',(20.8620199683238,2.24126900947336,-2.31790931715942));
#68820=CARTESIAN_POINT('Ctrl Pts',(20.8681922164166,2.31182970747074,-2.24755349730068));
#68821=CARTESIAN_POINT('Ctrl Pts',(20.8743644645093,2.37906965898984,-2.17396989863567));
#68822=CARTESIAN_POINT('Ctrl Pts',(20.880528353162,2.44621854347132,-2.10048595858426));
#68823=CARTESIAN_POINT('Ctrl Pts',(20.8866922418146,2.5100553302807,-2.02378324654332));
#68824=CARTESIAN_POINT('Ctrl Pts',(20.8928561304672,2.57025818620453,-1.94419402806114));
#68825=CARTESIAN_POINT('Ctrl Pts',(20.8990134921258,2.63039729281253,-1.86468908727887));
#68826=CARTESIAN_POINT('Ctrl Pts',(20.9051708537843,2.68690985812159,-1.78230406127739));
#68827=CARTESIAN_POINT('Ctrl Pts',(20.9113282154429,2.73951291161525,-1.69740583526549));
#68828=CARTESIAN_POINT('Ctrl Pts',(20.9174810795892,2.79207754234115,-1.61256962133473));
#68829=CARTESIAN_POINT('Ctrl Pts',(20.9236339437355,2.84073811061664,-1.52522422523414));
#68830=CARTESIAN_POINT('Ctrl Pts',(20.9297868078818,2.88525429152501,-1.43576642798769));
#68831=CARTESIAN_POINT('Ctrl Pts',(20.9359373410183,2.92975360749858,-1.34634252178686));
#68832=CARTESIAN_POINT('Ctrl Pts',(20.9420878741548,2.9701114625802,-1.25480819305112));
#68833=CARTESIAN_POINT('Ctrl Pts',(20.9482384072914,3.00613336716641,-1.16158501251899));
#68834=CARTESIAN_POINT('Ctrl Pts',(20.9543882555066,3.04215126036528,-1.0683722132893));
#68835=CARTESIAN_POINT('Ctrl Pts',(20.9605381037218,3.07383400648183,-0.97347134135303));
#68836=CARTESIAN_POINT('Ctrl Pts',(20.966687951937,3.10103556276004,-0.877323202131077));
#68837=CARTESIAN_POINT('Ctrl Pts',(20.9728387603161,3.12824136596472,-0.781160051485772));
#68838=CARTESIAN_POINT('Ctrl Pts',(20.9789895686952,3.15096447140595,-0.683749664773333));
#68839=CARTESIAN_POINT('Ctrl Pts',(20.9851403770744,3.16910920440028,-0.58554625187546));
#68840=CARTESIAN_POINT('Ctrl Pts',(20.9912977634406,3.18727334229416,-0.487237815257345));
#68841=CARTESIAN_POINT('Ctrl Pts',(20.9974551498068,3.20084925117145,-0.388135086858821));
#68842=CARTESIAN_POINT('Ctrl Pts',(21.0036125361729,3.20979275816905,-0.288700557854578));
#68843=CARTESIAN_POINT('Ctrl Pts',(21.0097733589099,3.21874125644122,-0.189210535514574));
#68844=CARTESIAN_POINT('Ctrl Pts',(21.0159341816469,3.22305218551559,-0.0893887777816784));
#68845=CARTESIAN_POINT('Ctrl Pts',(21.0220950043838,3.22273353676235,0.0103011420352819));
#68846=CARTESIAN_POINT('Ctrl Pts',(21.0282661273005,3.22241435526542,0.110157731814233));
#68847=CARTESIAN_POINT('Ctrl Pts',(21.0344372502172,3.21745015690376,0.209881609359754));
#68848=CARTESIAN_POINT('Ctrl Pts',(21.0406083731339,3.20790094414447,0.309013098520099));
#68849=CARTESIAN_POINT('Ctrl Pts',(21.0453038950794,3.20063508043062,0.384440875463251));
#68850=CARTESIAN_POINT('Ctrl Pts',(21.049999417025,3.19071581091794,0.459525772203122));
#68851=CARTESIAN_POINT('Ctrl Pts',(21.0546949389705,3.17818923053461,0.534070011715522));
#68852=CARTESIAN_POINT('Ctrl Pts',(21.0608680040607,3.16172090242125,0.63207113873379));
#68853=CARTESIAN_POINT('Ctrl Pts',(21.0670410691508,3.14068646221925,0.729482353170679));
#68854=CARTESIAN_POINT('Ctrl Pts',(21.0732141342409,3.11514003931512,0.82584508108713));
#68855=CARTESIAN_POINT('Ctrl Pts',(21.0793768581294,3.08963641212206,0.922046380866371));
#68856=CARTESIAN_POINT('Ctrl Pts',(21.0855395820179,3.05963595228572,1.01720227274774));
#68857=CARTESIAN_POINT('Ctrl Pts',(21.0917023059064,3.02524408820333,1.11086262395076));
#68858=CARTESIAN_POINT('Ctrl Pts',(21.0978591145962,2.99088523463951,1.2044330766605));
#68859=CARTESIAN_POINT('Ctrl Pts',(21.104015923286,2.9521435003847,1.29651043561477));
#68860=CARTESIAN_POINT('Ctrl Pts',(21.1101727319757,2.90917446053823,1.38665840085153));
#68861=CARTESIAN_POINT('Ctrl Pts',(21.1163252782469,2.86623516857617,1.47674395577471));
#68862=CARTESIAN_POINT('Ctrl Pts',(21.1224778245181,2.8190745739082,1.56490238096836));
#68863=CARTESIAN_POINT('Ctrl Pts',(21.1286303707893,2.76789646638622,1.65071703022253));
#68864=CARTESIAN_POINT('Ctrl Pts',(21.1347803034177,2.7167400996667,1.73649522483959));
#68865=CARTESIAN_POINT('Ctrl Pts',(21.140930236046,2.66156983598659,1.81993125087876));
#68866=CARTESIAN_POINT('Ctrl Pts',(21.1470801686744,2.60263505790736,1.90063366219047));
#68867=CARTESIAN_POINT('Ctrl Pts',(21.1532311967123,2.54368978252358,1.98135044799916));
#68868=CARTESIAN_POINT('Ctrl Pts',(21.1593822247501,2.48097890090506,2.0593322891714));
#68869=CARTESIAN_POINT('Ctrl Pts',(21.165533252788,2.4147944155433,2.13421777079118));
#68870=CARTESIAN_POINT('Ctrl Pts',(21.1716846498006,2.3486059600478,2.20910774448151));
#68871=CARTESIAN_POINT('Ctrl Pts',(21.1778360468132,2.27894378007838,2.28090066870694));
#68872=CARTESIAN_POINT('Ctrl Pts',(21.1839874438259,2.20613832156088,2.34927036942122));
#68873=CARTESIAN_POINT('Ctrl Pts',(21.1901443124187,2.13326810362314,2.41770088401225));
#68874=CARTESIAN_POINT('Ctrl Pts',(21.1963011810115,2.05724934509148,2.48270180114223));
#68875=CARTESIAN_POINT('Ctrl Pts',(21.2024580496043,1.97844711928728,2.54398595882207));
#68876=CARTESIAN_POINT('Ctrl Pts',(21.2072534983648,1.91706980866938,2.59171883366774));
#68877=CARTESIAN_POINT('Ctrl Pts',(21.2120489471252,1.85400463589929,2.63719769927644));
#68878=CARTESIAN_POINT('Ctrl Pts',(21.2168443958857,1.78943621037803,2.68030513402633));
#68879=CARTESIAN_POINT('Ctrl Pts',(19.9669438677106,1.78943621037804,2.68030513402633));
#68880=CARTESIAN_POINT('Ctrl Pts',(19.9730942171982,1.70631862674015,2.73579643312977));
#68881=CARTESIAN_POINT('Ctrl Pts',(19.9792445666858,1.62062618941371,2.78741199000142));
#68882=CARTESIAN_POINT('Ctrl Pts',(19.9853949161734,1.53276032849706,2.83491857694107));
#68883=CARTESIAN_POINT('Ctrl Pts',(19.9916502435984,1.44339471917444,2.88323603544441));
#68884=CARTESIAN_POINT('Ctrl Pts',(19.9979055710233,1.35178120773494,2.92730272350199));
#68885=CARTESIAN_POINT('Ctrl Pts',(20.0041608984482,1.25836630716031,2.9669229513932));
#68886=CARTESIAN_POINT('Ctrl Pts',(20.0103206012078,1.16637943233011,3.0059375081861));
#68887=CARTESIAN_POINT('Ctrl Pts',(20.0164803039674,1.07264629273122,3.04064050720801));
#68888=CARTESIAN_POINT('Ctrl Pts',(20.022640006727,0.977610152184573,3.07089497587359));
#68889=CARTESIAN_POINT('Ctrl Pts',(20.0289431464846,0.880360966750745,3.10185396070333));
#68890=CARTESIAN_POINT('Ctrl Pts',(20.0352462862422,0.781747811513302,3.12815453582589));
#68891=CARTESIAN_POINT('Ctrl Pts',(20.0415494259997,0.682256880388447,3.14970524202863));
#68892=CARTESIAN_POINT('Ctrl Pts',(20.0478525657573,0.582765949263606,3.17125594823137));
#68893=CARTESIAN_POINT('Ctrl Pts',(20.0541557055149,0.482397726816721,3.18805677235531));
#68894=CARTESIAN_POINT('Ctrl Pts',(20.0604588452725,0.381642573167133,3.20007289117707));
#68895=CARTESIAN_POINT('Ctrl Pts',(20.0666310933652,0.282979711661953,3.21183948200839));
#68896=CARTESIAN_POINT('Ctrl Pts',(20.072803341458,0.183598511516072,3.21905963072166));
#68897=CARTESIAN_POINT('Ctrl Pts',(20.0789755895508,0.0839540715665517,
3.22165629395307));
#68898=CARTESIAN_POINT('Ctrl Pts',(20.0851394782034,-0.0155554140324681,
3.22424944037008));
#68899=CARTESIAN_POINT('Ctrl Pts',(20.091303366856,-0.115327000405413,3.22223153622414));
#68900=CARTESIAN_POINT('Ctrl Pts',(20.0974672555086,-0.21489881363349,3.21557709632329));
#68901=CARTESIAN_POINT('Ctrl Pts',(20.1036246171672,-0.314365189423047,
3.20892970286535));
#68902=CARTESIAN_POINT('Ctrl Pts',(20.1097819788257,-0.413631781613563,
3.19765556333951));
#68903=CARTESIAN_POINT('Ctrl Pts',(20.1159393404843,-0.512236019325593,
3.18178123430972));
#68904=CARTESIAN_POINT('Ctrl Pts',(20.1220922046306,-0.610768233694957,
3.16591850034182));
#68905=CARTESIAN_POINT('Ctrl Pts',(20.1282450687769,-0.708638627907619,
3.14546232617529));
#68906=CARTESIAN_POINT('Ctrl Pts',(20.1343979329232,-0.805389981364252,
3.12049107360013));
#68907=CARTESIAN_POINT('Ctrl Pts',(20.1405484660597,-0.902104680614698,
3.09552928137263));
#68908=CARTESIAN_POINT('Ctrl Pts',(20.1466989991963,-0.997700761366174,
3.0660559179943));
#68909=CARTESIAN_POINT('Ctrl Pts',(20.1528495323328,-1.09173230074264,3.03220021535768));
#68910=CARTESIAN_POINT('Ctrl Pts',(20.158999380548,-1.18575336879797,2.99834828288092));
#68911=CARTESIAN_POINT('Ctrl Pts',(20.1651492287632,-1.27820983317403,2.96011512854095));
#68912=CARTESIAN_POINT('Ctrl Pts',(20.1712990769784,-1.36867297657283,2.91767918827607));
#68913=CARTESIAN_POINT('Ctrl Pts',(20.1774498853575,-1.4591502438078,2.87523662256964));
#68914=CARTESIAN_POINT('Ctrl Pts',(20.1836006937367,-1.54763317862179,2.82859015210215));
#68915=CARTESIAN_POINT('Ctrl Pts',(20.1897515021158,-1.63371593283588,2.77796504896987));
#68916=CARTESIAN_POINT('Ctrl Pts',(20.195908888482,-1.7198907483218,2.72728580477969));
#68917=CARTESIAN_POINT('Ctrl Pts',(20.2020662748482,-1.80365988226804,2.67261965185332));
#68918=CARTESIAN_POINT('Ctrl Pts',(20.2082236612143,-1.88464496906871,2.61423619879));
#68919=CARTESIAN_POINT('Ctrl Pts',(20.2143844839513,-1.96567525277091,2.55582016255263));
#68920=CARTESIAN_POINT('Ctrl Pts',(20.2205453066883,-2.04391805489442,2.49368296481865));
#68921=CARTESIAN_POINT('Ctrl Pts',(20.2267061294252,-2.11902836556457,2.42813433492316));
#68922=CARTESIAN_POINT('Ctrl Pts',(20.2328772523419,-2.19426425194636,2.36247611533522));
#68923=CARTESIAN_POINT('Ctrl Pts',(20.2390483752586,-2.26635687202856,2.29339537165235));
#68924=CARTESIAN_POINT('Ctrl Pts',(20.2452194981753,-2.33499823336709,2.22123857626158));
#68925=CARTESIAN_POINT('Ctrl Pts',(20.2499150201208,-2.38722649439675,2.166335470157));
#68926=CARTESIAN_POINT('Ctrl Pts',(20.2546105420664,-2.43745742487321,2.1096522517446));
#68927=CARTESIAN_POINT('Ctrl Pts',(20.259306064012,-2.48557179491179,2.0513533130202));
#68928=CARTESIAN_POINT('Ctrl Pts',(20.2654494495405,-2.5485222247117,1.97507790410108));
#68929=CARTESIAN_POINT('Ctrl Pts',(20.271592835069,-2.60807636476049,1.89575905697603));
#68930=CARTESIAN_POINT('Ctrl Pts',(20.2777362205975,-2.66392368938818,1.81373320519211));
#68931=CARTESIAN_POINT('Ctrl Pts',(20.2838716717915,-2.71969888581354,1.73181329182643));
#68932=CARTESIAN_POINT('Ctrl Pts',(20.2900071229855,-2.77177653159852,1.64719367652906));
#68933=CARTESIAN_POINT('Ctrl Pts',(20.2961425741796,-2.81988544742911,1.560244732687));
#68934=CARTESIAN_POINT('Ctrl Pts',(20.3022717794618,-2.86794538820766,1.47338430318737));
#68935=CARTESIAN_POINT('Ctrl Pts',(20.3084009847441,-2.91204441515768,1.3841996375125));
#68936=CARTESIAN_POINT('Ctrl Pts',(20.3145301900264,-2.95195450045975,1.29309017075973));
#68937=CARTESIAN_POINT('Ctrl Pts',(20.3206548317614,-2.99183487039829,1.20204854026701));
#68938=CARTESIAN_POINT('Ctrl Pts',(20.3267794734963,-3.02753232243455,1.10908535734209));
#68939=CARTESIAN_POINT('Ctrl Pts',(20.3329041152313,-3.05886516307952,1.01462381038419));
#68940=CARTESIAN_POINT('Ctrl Pts',(20.3390266838001,-3.09018739768616,0.92019423827334));
#68941=CARTESIAN_POINT('Ctrl Pts',(20.3451492523689,-3.11714781439698,0.824267724102018));
#68942=CARTESIAN_POINT('Ctrl Pts',(20.3512718209377,-3.13961351635457,0.727285728186446));
#68943=CARTESIAN_POINT('Ctrl Pts',(20.3573931590532,-3.16207470337753,0.630323222753389));
#68944=CARTESIAN_POINT('Ctrl Pts',(20.3635144971687,-3.180042877248,0.532306085458401));
#68945=CARTESIAN_POINT('Ctrl Pts',(20.3696358352842,-3.19343581795904,0.433687951269458));
#68946=CARTESIAN_POINT('Ctrl Pts',(20.3757593834993,-3.20683359417032,0.335034211157722));
#68947=CARTESIAN_POINT('Ctrl Pts',(20.3818829317143,-3.21565278223615,0.235779475920398));
#68948=CARTESIAN_POINT('Ctrl Pts',(20.3880064799293,-3.21986288635336,0.136383853825077));
#68949=CARTESIAN_POINT('Ctrl Pts',(20.3908621363773,-3.22182622697657,0.0900316836186007));
#68950=CARTESIAN_POINT('Ctrl Pts',(20.3937177928252,-3.22278795507048,0.0436489185283968));
#68951=CARTESIAN_POINT('Ctrl Pts',(20.3965734492731,-3.22274885406337,-0.00271774414203127));
#68952=CARTESIAN_POINT('Ctrl Pts',(19.7206814315572,1.78943602647607,2.6803052568037));
#68953=CARTESIAN_POINT('Ctrl Pts',(19.7289802291916,1.66591970175143,2.76276771542073));
#68954=CARTESIAN_POINT('Ctrl Pts',(19.7372902951155,1.53668781520546,2.8367029284314));
#68955=CARTESIAN_POINT('Ctrl Pts',(19.7502089053106,1.33477329037264,2.93431017825189));
#68956=CARTESIAN_POINT('Ctrl Pts',(19.7546090323161,1.26580402635902,2.96471498196429));
#68957=CARTESIAN_POINT('Ctrl Pts',(19.7617870253068,1.15367465474395,3.00952051990762));
#68958=CARTESIAN_POINT('Ctrl Pts',(19.7645136235498,1.11116371598277,3.02547415306848));
#68959=CARTESIAN_POINT('Ctrl Pts',(19.7680585821135,1.05608417200107,3.04482713786495));
#68960=CARTESIAN_POINT('Ctrl Pts',(19.7688492493658,1.04381109360894,3.04905632466441));
#68961=CARTESIAN_POINT('Ctrl Pts',(19.7701289921938,1.02396746701611,3.05576039989184));
#68962=CARTESIAN_POINT('Ctrl Pts',(19.7706165304726,1.01641262672995,3.05828160336431));
#68963=CARTESIAN_POINT('Ctrl Pts',(19.7715485451682,1.00198006699373,3.06303865620979));
#68964=CARTESIAN_POINT('Ctrl Pts',(19.7719928561243,0.995104006507827,3.06527941286962));
#68965=CARTESIAN_POINT('Ctrl Pts',(19.7730105501088,0.979364497026078,3.07035003105503));
#68966=CARTESIAN_POINT('Ctrl Pts',(19.7735844303595,0.970496249378194,3.07316468128043));
#68967=CARTESIAN_POINT('Ctrl Pts',(19.7753524407012,0.943198439125302,3.08169865919526));
#68968=CARTESIAN_POINT('Ctrl Pts',(19.7765507310396,0.924729857029722,3.08729081673171));
#68969=CARTESIAN_POINT('Ctrl Pts',(19.7935404217358,0.663376023866606,3.16387141920115));
#68970=CARTESIAN_POINT('Ctrl Pts',(19.8103135050892,0.413056312934985,3.20616328004224));
#68971=CARTESIAN_POINT('Ctrl Pts',(19.8374924096142,0.0115765992932028,
3.22617335865394));
#68972=CARTESIAN_POINT('Ctrl Pts',(19.8476256850581,-0.137612394891393,
3.22325837963423));
#68973=CARTESIAN_POINT('Ctrl Pts',(19.8612410909834,-0.342625340216841,
3.2049882277363));
#68974=CARTESIAN_POINT('Ctrl Pts',(19.8649539245169,-0.399042914708731,
3.1984538787418));
#68975=CARTESIAN_POINT('Ctrl Pts',(19.8705903113331,-0.485921673878087,
3.18605663299165));
#68976=CARTESIAN_POINT('Ctrl Pts',(19.8725596254666,-0.516518440073175,
3.18123963469908));
#68977=CARTESIAN_POINT('Ctrl Pts',(19.8749936903938,-0.554703442397623,
3.17466251550715));
#68978=CARTESIAN_POINT('Ctrl Pts',(19.8754805456949,-0.562359846195949,
3.17331520696098));
#68979=CARTESIAN_POINT('Ctrl Pts',(19.8762501641119,-0.574494140235761,
3.17113462175542));
#68980=CARTESIAN_POINT('Ctrl Pts',(19.8765339479639,-0.578975207605876,
3.1703195447861));
#68981=CARTESIAN_POINT('Ctrl Pts',(19.877068103554,-0.587422814508041,3.16876447217507));
#68982=CARTESIAN_POINT('Ctrl Pts',(19.8773185856887,-0.591389645411858,
3.16802653565467));
#68983=CARTESIAN_POINT('Ctrl Pts',(19.877891872028,-0.600481055493412,3.16631761954002));
#68984=CARTESIAN_POINT('Ctrl Pts',(19.8782143875523,-0.605604661108876,
3.16534164999124));
#68985=CARTESIAN_POINT('Ctrl Pts',(19.8792099711976,-0.62144785500857,3.16228388481651));
#68986=CARTESIAN_POINT('Ctrl Pts',(19.8798806755426,-0.63215938533121,3.16016001560192));
#68987=CARTESIAN_POINT('Ctrl Pts',(19.8854409268335,-0.721255145672709,
3.14202308066662));
#68988=CARTESIAN_POINT('Ctrl Pts',(19.8901758818645,-0.79903630007227,3.12314927901672));
#68989=CARTESIAN_POINT('Ctrl Pts',(19.8966037168646,-0.905701274256411,
3.0930199931721));
#68990=CARTESIAN_POINT('Ctrl Pts',(19.8983766981551,-0.935240404890352,
3.08421674845799));
#68991=CARTESIAN_POINT('Ctrl Pts',(19.9085320212259,-1.10473346694555,3.03104541172181));
#68992=CARTESIAN_POINT('Ctrl Pts',(19.9166721877592,-1.24165650023627,2.97757705066822));
#68993=CARTESIAN_POINT('Ctrl Pts',(19.9372657866948,-1.57446099334369,2.82065298361735));
#68994=CARTESIAN_POINT('Ctrl Pts',(19.9497983535513,-1.76419422005291,2.70603216277327));
#68995=CARTESIAN_POINT('Ctrl Pts',(19.9645078303311,-1.95911381884285,2.5590082354429));
#68996=CARTESIAN_POINT('Ctrl Pts',(19.9659056548041,-1.97738722001914,2.54491450616881));
#68997=CARTESIAN_POINT('Ctrl Pts',(19.9679207611938,-2.00336502004563,2.52442989490071));
#68998=CARTESIAN_POINT('Ctrl Pts',(19.9685317313592,-2.01119373941462,2.51819725931001));
#68999=CARTESIAN_POINT('Ctrl Pts',(19.9695934000173,-2.02471438806824,2.50732987190517));
#69000=CARTESIAN_POINT('Ctrl Pts',(19.970043419882,-2.0304197759055,2.50271192349335));
#69001=CARTESIAN_POINT('Ctrl Pts',(19.9709097679311,-2.04135371104809,2.49379998489755));
#69002=CARTESIAN_POINT('Ctrl Pts',(19.9713259753534,-2.04658461538731,2.48950893736709));
#69003=CARTESIAN_POINT('Ctrl Pts',(19.9723079135283,-2.05887378256289,2.47936290403284));
#69004=CARTESIAN_POINT('Ctrl Pts',(19.9728742014607,-2.06592061540058,2.47349422285426));
#69005=CARTESIAN_POINT('Ctrl Pts',(19.974552682025,-2.08668751057707,2.45604866797816));
#69006=CARTESIAN_POINT('Ctrl Pts',(19.9756683415232,-2.10033582563484,2.44438729026499));
#69007=CARTESIAN_POINT('Ctrl Pts',(19.9897993108338,-2.27123683098548,2.29587815510908));
#69008=CARTESIAN_POINT('Ctrl Pts',(20.0034626767976,-2.41491979028521,2.14422619535186));
#69009=CARTESIAN_POINT('Ctrl Pts',(20.0290237173945,-2.64848716836799,1.84422184490517));
#69010=CARTESIAN_POINT('Ctrl Pts',(20.0407569811577,-2.74302531105695,1.70042660936587));
#69011=CARTESIAN_POINT('Ctrl Pts',(20.0569667380699,-2.85998108597723,1.48718609848464));
#69012=CARTESIAN_POINT('Ctrl Pts',(20.0616693071054,-2.8922254505176,1.42346326695561));
#69013=CARTESIAN_POINT('Ctrl Pts',(20.0686134800997,-2.93763525762032,1.32579591356883));
#69014=CARTESIAN_POINT('Ctrl Pts',(20.0709280640983,-2.95238544904572,1.29261600684481));
#69015=CARTESIAN_POINT('Ctrl Pts',(20.0737249249903,-2.96977096124173,1.25165690673077));
#69016=CARTESIAN_POINT('Ctrl Pts',(20.0742378213022,-2.97294074380799,1.24410928445468));
#69017=CARTESIAN_POINT('Ctrl Pts',(20.0750390986676,-2.97786437509233,1.23225927076503));
#69018=CARTESIAN_POINT('Ctrl Pts',(20.0753286458914,-2.9796377104106,1.22796508996803));
#69019=CARTESIAN_POINT('Ctrl Pts',(20.0758677365172,-2.98292856148737,1.21994710079582));
#69020=CARTESIAN_POINT('Ctrl Pts',(20.0761174156275,-2.98444837802755,1.21622432586366));
#69021=CARTESIAN_POINT('Ctrl Pts',(20.0766812360623,-2.98787051527878,1.20779679547853));
#69022=CARTESIAN_POINT('Ctrl Pts',(20.0769951237206,-2.9897686881931,1.20309039859039));
#69023=CARTESIAN_POINT('Ctrl Pts',(20.0779183954819,-2.99533102130554,1.1892044919493));
#69024=CARTESIAN_POINT('Ctrl Pts',(20.0785259288192,-2.99896411953153,1.18001248577706));
#69025=CARTESIAN_POINT('Ctrl Pts',(20.0826545463061,-3.02346264146662,1.11718542665454));
#69026=CARTESIAN_POINT('Ctrl Pts',(20.0860961727694,-3.04293190898718,1.06301269342243));
#69027=CARTESIAN_POINT('Ctrl Pts',(20.0968283827786,-3.1000585176466,0.889598430721381));
#69028=CARTESIAN_POINT('Ctrl Pts',(20.1038951214382,-3.13223623259125,0.768667320473749));
#69029=CARTESIAN_POINT('Ctrl Pts',(20.1230422021435,-3.20071234172113,0.434076982630533));
#69030=CARTESIAN_POINT('Ctrl Pts',(20.1349950551912,-3.22263527377611,0.218170968691717));
#69031=CARTESIAN_POINT('Ctrl Pts',(20.1476543523149,-3.22275026120138,0.00035588477229578));
#69032=CARTESIAN_POINT('Ctrl Pts',(20.1477325700598,-3.2227501289256,-0.000989561080740707));
#69033=CARTESIAN_POINT('Ctrl Pts',(20.1484713113117,-3.22274092450776,-0.0136933996024656));
#69034=CARTESIAN_POINT('Ctrl Pts',(20.1491333204908,-3.22267264703738,-0.0250515796886401));
#69035=CARTESIAN_POINT('Ctrl Pts',(20.1543970996916,-3.22165477417427,-0.115142872878734));
#69036=CARTESIAN_POINT('Ctrl Pts',(20.1590721954234,-3.21788015495692,-0.193812107968267));
#69037=CARTESIAN_POINT('Ctrl Pts',(20.1647327461069,-3.20998153677356,-0.286974158346346));
#69038=CARTESIAN_POINT('Ctrl Pts',(20.1656299128291,-3.20863288654313,-0.301679668029256));
#69039=CARTESIAN_POINT('Ctrl Pts',(20.1670943754145,-3.2062749307442,-0.325582920431327));
#69040=CARTESIAN_POINT('Ctrl Pts',(20.1676597363297,-3.2053269870437,-0.33478660802144));
#69041=CARTESIAN_POINT('Ctrl Pts',(20.1686688439573,-3.20356819642222,-0.351170303752988));
#69042=CARTESIAN_POINT('Ctrl Pts',(20.1691120998742,-3.20277280809544,-0.358351935587643));
#69043=CARTESIAN_POINT('Ctrl Pts',(20.1700472373982,-3.20104682461974,-0.373471095635817));
#69044=CARTESIAN_POINT('Ctrl Pts',(20.1705392864184,-3.20011084302665,-0.381407948512044));
#69045=CARTESIAN_POINT('Ctrl Pts',(20.171840640307,-3.19756220801141,-0.402349616818439));
#69046=CARTESIAN_POINT('Ctrl Pts',(20.1726515150272,-3.19589975139659,-0.415348118001118));
#69047=CARTESIAN_POINT('Ctrl Pts',(20.1763596372003,-3.18795980514592,-0.47455734979508));
#69048=CARTESIAN_POINT('Ctrl Pts',(20.1792859593834,-3.1807592640557,-0.520636661804334));
#69049=CARTESIAN_POINT('Ctrl Pts',(20.1872007832742,-3.15882170635153,-0.643484217162877));
#69050=CARTESIAN_POINT('Ctrl Pts',(20.1922438068385,-3.14228815791712,-0.719895836793292));
#69051=CARTESIAN_POINT('Ctrl Pts',(20.2187049725916,-3.04252396783887,-1.11149059445214));
#69052=CARTESIAN_POINT('Ctrl Pts',(20.2414377149087,-2.91461933617843,-1.41326324249615));
#69053=CARTESIAN_POINT('Ctrl Pts',(20.2656694398784,-2.71893518199291,-1.73081753219396));
#69054=CARTESIAN_POINT('Ctrl Pts',(20.2686901346675,-2.6933369219396,-1.7703882746673));
#69055=CARTESIAN_POINT('Ctrl Pts',(20.2721911217662,-2.66211734992872,-1.81640322903893));
#69056=CARTESIAN_POINT('Ctrl Pts',(20.2727232850044,-2.65732850491791,-1.82340195678699));
#69057=CARTESIAN_POINT('Ctrl Pts',(20.2735769640072,-2.64957541455836,-1.8346374080525));
#69058=CARTESIAN_POINT('Ctrl Pts',(20.2738996280088,-2.64662854003478,-1.83888598570491));
#69059=CARTESIAN_POINT('Ctrl Pts',(20.2744731473428,-2.6413610066962,-1.84644141932421));
#69060=CARTESIAN_POINT('Ctrl Pts',(20.274724273071,-2.63904434414623,-1.84975101919495));
#69061=CARTESIAN_POINT('Ctrl Pts',(20.2752561030354,-2.63411645134774,-1.85676293808298));
#69062=CARTESIAN_POINT('Ctrl Pts',(20.2755366956653,-2.63150364402591,-1.86046409790142));
#69063=CARTESIAN_POINT('Ctrl Pts',(20.2762906304546,-2.62444884506474,-1.87041294540837));
#69064=CARTESIAN_POINT('Ctrl Pts',(20.2767629807737,-2.6199923182591,-1.87665036216145));
#69065=CARTESIAN_POINT('Ctrl Pts',(20.2790588566986,-2.5981551552206,-1.90698455296931));
#69066=CARTESIAN_POINT('Ctrl Pts',(20.2808616958443,-2.58046343998206,-1.93085703221845));
#69067=CARTESIAN_POINT('Ctrl Pts',(20.2858606978108,-2.52996707990865,-1.99706078127216));
#69068=CARTESIAN_POINT('Ctrl Pts',(20.2890135809553,-2.49643265780358,-2.03882560381484));
#69069=CARTESIAN_POINT('Ctrl Pts',(20.2946949604353,-2.4332854770754,-2.11357552274144));
#69070=CARTESIAN_POINT('Ctrl Pts',(20.2972365192397,-2.40400433104826,-2.14682163602927));
#69071=CARTESIAN_POINT('Ctrl Pts',(20.3189265061937,-2.14630771085541,-2.42752658386254));
#69072=CARTESIAN_POINT('Ctrl Pts',(20.3370540436743,-1.88111474928892,-2.63835918022059));
#69073=CARTESIAN_POINT('Ctrl Pts',(20.3575307933085,-1.58254420988207,-2.80743864052252));
#69074=CARTESIAN_POINT('Ctrl Pts',(20.3579103545594,-1.57700869249403,-2.81055181049625));
#69075=CARTESIAN_POINT('Ctrl Pts',(20.3602499104094,-1.54288268837285,-2.82961168477673));
#69076=CARTESIAN_POINT('Ctrl Pts',(20.3622241201737,-1.51406060524487,-2.84513789481262));
#69077=CARTESIAN_POINT('Ctrl Pts',(20.3649369693509,-1.47445105212665,-2.86570290559432));
#69078=CARTESIAN_POINT('Ctrl Pts',(20.3656620336859,-1.46386417026199,-2.87112534267082));
#69079=CARTESIAN_POINT('Ctrl Pts',(20.3668141252229,-1.44704288754362,-2.87962372010225));
#69080=CARTESIAN_POINT('Ctrl Pts',(20.3672397900481,-1.44082806517103,-2.88273834629208));
#69081=CARTESIAN_POINT('Ctrl Pts',(20.3681102278696,-1.42812009576557,-2.88905572341396));
#69082=CARTESIAN_POINT('Ctrl Pts',(20.3685550581731,-1.42162613950074,-2.89225674846581));
#69083=CARTESIAN_POINT('Ctrl Pts',(20.3695771448402,-1.40670617221827,-2.89954876511996));
#69084=CARTESIAN_POINT('Ctrl Pts',(20.3701549137137,-1.39827303206734,-2.90362494497681));
#69085=CARTESIAN_POINT('Ctrl Pts',(20.371946692167,-1.37212390766454,-2.91612385585074));
#69086=CARTESIAN_POINT('Ctrl Pts',(20.3731650260043,-1.35434895817158,-2.92442152104124));
#69087=CARTESIAN_POINT('Ctrl Pts',(20.383894223218,-1.19788448912377,-2.99572951795048));
#69088=CARTESIAN_POINT('Ctrl Pts',(20.3937400599149,-1.05498574185414,-3.04898599680294));
#69089=CARTESIAN_POINT('Ctrl Pts',(20.4239484558779,-0.61796845565421,-3.17744732993056));
#69090=CARTESIAN_POINT('Ctrl Pts',(20.4450494585192,-0.316476177380199,
-3.22147259843938));
#69091=CARTESIAN_POINT('Ctrl Pts',(20.4666801482623,0.0196649616159529,
-3.22285846637663));
#69092=CARTESIAN_POINT('Ctrl Pts',(20.4687786128436,0.0526185201255753,
-3.22248892931092));
#69093=CARTESIAN_POINT('Ctrl Pts',(20.4713690994219,0.0938075203182971,
-3.22139500005276));
#69094=CARTESIAN_POINT('Ctrl Pts',(20.471886002397,0.102052166157655,-3.22114435506224));
#69095=CARTESIAN_POINT('Ctrl Pts',(20.4726952759532,0.115002400335194,-3.22070088456942));
#69096=CARTESIAN_POINT('Ctrl Pts',(20.4729888222946,0.119708612528294,-3.22052939572251));
#69097=CARTESIAN_POINT('Ctrl Pts',(20.4735315705697,0.128426765546993,-3.2201925797929));
#69098=CARTESIAN_POINT('Ctrl Pts',(20.4737809253533,0.132438737043239,-3.22003007226678));
#69099=CARTESIAN_POINT('Ctrl Pts',(20.4743392504605,0.141436559095113,-3.21964876469827));
#69100=CARTESIAN_POINT('Ctrl Pts',(20.4746479881176,0.146422194650503,-3.21942588204558));
#69101=CARTESIAN_POINT('Ctrl Pts',(20.4755609918976,0.161194930861298,-3.2187310800625));
#69102=CARTESIAN_POINT('Ctrl Pts',(20.4761634266426,0.170980527275454,-3.21822610091376));
#69103=CARTESIAN_POINT('Ctrl Pts',(20.4810991872886,0.251449724622588,-3.21370547268204));
#69104=CARTESIAN_POINT('Ctrl Pts',(20.4853106083577,0.321991810443162,-3.20740593565496));
#69105=CARTESIAN_POINT('Ctrl Pts',(20.496282031536,0.508658250010303,-3.18451458339333));
#69106=CARTESIAN_POINT('Ctrl Pts',(20.5028950739508,0.624184381902098,-3.1639001265023));
#69107=CARTESIAN_POINT('Ctrl Pts',(20.5250913678361,1.00984891359085,-3.07312955714131));
#69108=CARTESIAN_POINT('Ctrl Pts',(20.5404931395569,1.27188178392693,-2.97425952398424));
#69109=CARTESIAN_POINT('Ctrl Pts',(20.557596185019,1.52391608826407,-2.83969077283677));
#69110=CARTESIAN_POINT('Ctrl Pts',(20.558004444565,1.52991261219465,-2.83646458243286));
#69111=CARTESIAN_POINT('Ctrl Pts',(20.5600625132314,1.56004156827878,-2.82013156283506));
#69112=CARTESIAN_POINT('Ctrl Pts',(20.5617221892684,1.5840154347542,-2.80673596150411));
#69113=CARTESIAN_POINT('Ctrl Pts',(20.5640657474983,1.61740036562644,-2.78751788422871));
#69114=CARTESIAN_POINT('Ctrl Pts',(20.5647404113197,1.62695753629128,-2.78195058689767));
#69115=CARTESIAN_POINT('Ctrl Pts',(20.5658321843213,1.64233587426611,-2.77288596107061));
#69116=CARTESIAN_POINT('Ctrl Pts',(20.5662481782628,1.64817503308301,-2.76941920557493));
#69117=CARTESIAN_POINT('Ctrl Pts',(20.5671141131238,1.66028724804923,-2.76217621225702));
#69118=CARTESIAN_POINT('Ctrl Pts',(20.5675641610904,1.6665584735681,-2.75839700303662));
#69119=CARTESIAN_POINT('Ctrl Pts',(20.5686246873165,1.68128017980863,-2.74945677654805));
#69120=CARTESIAN_POINT('Ctrl Pts',(20.5692358110827,1.68971982560838,-2.74427814125343));
#69121=CARTESIAN_POINT('Ctrl Pts',(20.571239436272,1.71724622852086,-2.72721259814539));
#69122=CARTESIAN_POINT('Ctrl Pts',(20.5726378687498,1.73623213424713,-2.71516502252512));
#69123=CARTESIAN_POINT('Ctrl Pts',(20.5759341089152,1.78044797794668,-2.68645429978394));
#69124=CARTESIAN_POINT('Ctrl Pts',(20.5778377420047,1.80557222550908,-2.66963303570567));
#69125=CARTESIAN_POINT('Ctrl Pts',(20.584592689814,1.89326706555523,-2.60911509350287));
#69126=CARTESIAN_POINT('Ctrl Pts',(20.5895128009219,1.95451471701099,-2.56355465203845));
#69127=CARTESIAN_POINT('Ctrl Pts',(20.6150868324603,2.25971459528024,-2.31922602001072));
#69128=CARTESIAN_POINT('Ctrl Pts',(20.6369653338288,2.47518190792737,-2.08771416490546));
#69129=CARTESIAN_POINT('Ctrl Pts',(20.6614812495578,2.68773441454902,-1.77927026347234));
#69130=CARTESIAN_POINT('Ctrl Pts',(20.6653497931549,2.72040261424747,-1.7289099694471));
#69131=CARTESIAN_POINT('Ctrl Pts',(20.6697624388816,2.75685443694016,-1.66912288949575));
#69132=CARTESIAN_POINT('Ctrl Pts',(20.6703903284589,2.76202157072408,-1.6605584770816));
#69133=CARTESIAN_POINT('Ctrl Pts',(20.6713345247138,2.7697631777192,-1.6475908211724));
#69134=CARTESIAN_POINT('Ctrl Pts',(20.6716527168457,2.77236715022545,-1.64320539186909));
#69135=CARTESIAN_POINT('Ctrl Pts',(20.6722206860638,2.77700658079784,-1.63534956474592));
#69136=CARTESIAN_POINT('Ctrl Pts',(20.6724707174041,2.7790459537,-1.63188153263245));
#69137=CARTESIAN_POINT('Ctrl Pts',(20.6730074491048,2.78341737050781,-1.62441580984607));
#69138=CARTESIAN_POINT('Ctrl Pts',(20.6732940105666,2.78574729038131,-1.62041692674965));
#69139=CARTESIAN_POINT('Ctrl Pts',(20.674080911474,2.7921339761048,-1.60940085730269));
#69140=CARTESIAN_POINT('Ctrl Pts',(20.6745801043479,2.79617292994234,-1.60237330519178));
#69141=CARTESIAN_POINT('Ctrl Pts',(20.6772377495427,2.81760488859402,-1.56475510807865));
#69142=CARTESIAN_POINT('Ctrl Pts',(20.6793668532931,2.83452329994665,-1.53389496366684));
#69143=CARTESIAN_POINT('Ctrl Pts',(20.6855470925973,2.88273761755558,-1.44242619997023));
#69144=CARTESIAN_POINT('Ctrl Pts',(20.6895261996228,2.91262036829977,-1.3810913659796));
#69145=CARTESIAN_POINT('Ctrl Pts',(20.7072058812553,3.03852030736128,-1.10038229044601));
#69146=CARTESIAN_POINT('Ctrl Pts',(20.7202345232669,3.11185683159875,-0.871668655335678));
#69147=CARTESIAN_POINT('Ctrl Pts',(20.7421869196752,3.18810132597748,-0.493495222717645));
#69148=CARTESIAN_POINT('Ctrl Pts',(20.7506972944325,3.2072144095353,-0.348274410371027));
#69149=CARTESIAN_POINT('Ctrl Pts',(20.7606998438942,3.21760665767313,-0.183021589053609));
#69150=CARTESIAN_POINT('Ctrl Pts',(20.761870168043,3.21864427205975,-0.163763642078358));
#69151=CARTESIAN_POINT('Ctrl Pts',(20.763613026169,3.2199260354401,-0.135205096803927));
#69152=CARTESIAN_POINT('Ctrl Pts',(20.7641813925414,3.22030287357123,-0.125910648938842));
#69153=CARTESIAN_POINT('Ctrl Pts',(20.7651938759245,3.22090114261816,-0.109387795067659));
#69154=CARTESIAN_POINT('Ctrl Pts',(20.7656374899645,3.22113849330376,-0.102160001131859));
#69155=CARTESIAN_POINT('Ctrl Pts',(20.7665713487827,3.22158615168371,-0.0869694189091101));
#69156=CARTESIAN_POINT('Ctrl Pts',(20.7670617535443,3.22179126850761,-0.0790065370297626));
#69157=CARTESIAN_POINT('Ctrl Pts',(20.7683541261965,3.22225313285796,-0.0580599140718856));
#69158=CARTESIAN_POINT('Ctrl Pts',(20.7691576251502,3.22246092477963,-0.0450753388185116));
#69159=CARTESIAN_POINT('Ctrl Pts',(20.7727845520275,3.22304280702763,0.0133592911564714));
#69160=CARTESIAN_POINT('Ctrl Pts',(20.7756355201495,3.22253383567223,0.0588110855641397));
#69161=CARTESIAN_POINT('Ctrl Pts',(20.7832995788939,3.2186230549001,0.17966166966234));
#69162=CARTESIAN_POINT('Ctrl Pts',(20.788163043942,3.21353380909361,0.254973863837604));
#69163=CARTESIAN_POINT('Ctrl Pts',(20.8133436301556,3.17409469394364,0.638068899788148));
#69164=CARTESIAN_POINT('Ctrl Pts',(20.8348469237467,3.09816268723872,0.939869210308037));
#69165=CARTESIAN_POINT('Ctrl Pts',(20.8594938006782,2.95531436473915,1.28707849822721));
#69166=CARTESIAN_POINT('Ctrl Pts',(20.8637490556735,2.92839638292575,1.34720084527485));
#69167=CARTESIAN_POINT('Ctrl Pts',(20.8685556706488,2.89511940848214,1.41580686341731));
#69168=CARTESIAN_POINT('Ctrl Pts',(20.8692078684748,2.89054087453619,1.4251311951832));
#69169=CARTESIAN_POINT('Ctrl Pts',(20.870176817732,2.88364264668812,1.43900964723685));
#69170=CARTESIAN_POINT('Ctrl Pts',(20.8704956517355,2.88135712920066,1.44358053932054));
#69171=CARTESIAN_POINT('Ctrl Pts',(20.8710643205662,2.87725249090699,1.45174097536426));
#69172=CARTESIAN_POINT('Ctrl Pts',(20.8713144122351,2.87543751686951,1.45533255415432));
#69173=CARTESIAN_POINT('Ctrl Pts',(20.8718507778918,2.87152382092332,1.46304130611008));
#69174=CARTESIAN_POINT('Ctrl Pts',(20.8721369148771,2.86942297704463,1.46715735248848));
#69175=CARTESIAN_POINT('Ctrl Pts',(20.872921462592,2.86362728553628,1.47845240753759));
#69176=CARTESIAN_POINT('Ctrl Pts',(20.8734187381169,2.85991427077189,1.48562213195255));
#69177=CARTESIAN_POINT('Ctrl Pts',(20.8760485056602,2.84007130371609,1.52358824330249));
#69178=CARTESIAN_POINT('Ctrl Pts',(20.878152373962,2.82347003969167,1.55413748202821));
#69179=CARTESIAN_POINT('Ctrl Pts',(20.8842379371014,2.77343162072368,1.64276753906209));
#69180=CARTESIAN_POINT('Ctrl Pts',(20.8881502039223,2.7386720319103,1.70008377590273));
#69181=CARTESIAN_POINT('Ctrl Pts',(20.9060935679682,2.56864360571242,1.96168359448551));
#69182=CARTESIAN_POINT('Ctrl Pts',(20.9194077657512,2.41215017058785,2.15120372201841));
#69183=CARTESIAN_POINT('Ctrl Pts',(20.9368538966456,2.19158867555922,2.36364232977687));
#69184=CARTESIAN_POINT('Ctrl Pts',(20.9403743784684,2.14629248909059,2.40484801886621));
#69185=CARTESIAN_POINT('Ctrl Pts',(20.9449700440704,2.08644489735947,2.45625275717279));
#69186=CARTESIAN_POINT('Ctrl Pts',(20.9460032546528,2.07294364156569,2.46765770720606));
#69187=CARTESIAN_POINT('Ctrl Pts',(20.9511075231225,2.00604131422766,2.52323576253808));
#69188=CARTESIAN_POINT('Ctrl Pts',(20.9552345537638,1.95132190911437,2.56578685885222));
#69189=CARTESIAN_POINT('Ctrl Pts',(20.9602906969076,1.88381310537646,2.61487411319555));
#69190=CARTESIAN_POINT('Ctrl Pts',(20.9611521193032,1.87229514930295,2.62313349026753));
#69191=CARTESIAN_POINT('Ctrl Pts',(20.9625696396051,1.85331729892081,2.63655358881213));
#69192=CARTESIAN_POINT('Ctrl Pts',(20.9631240044374,1.84588935405468,2.64175932421788));
#69193=CARTESIAN_POINT('Ctrl Pts',(20.9641209057462,1.83252160072759,2.65104395721525));
#69194=CARTESIAN_POINT('Ctrl Pts',(20.9645629958561,1.82658988094671,2.65513443834842));
#69195=CARTESIAN_POINT('Ctrl Pts',(20.9654935220019,1.81409738667375,2.66368751780943));
#69196=CARTESIAN_POINT('Ctrl Pts',(20.9659821164421,1.80753375719032,2.66814584228224));
#69197=CARTESIAN_POINT('Ctrl Pts',(20.9667568400117,1.79712010867691,2.67516321900054));
#69198=CARTESIAN_POINT('Ctrl Pts',(20.9670423576727,1.79328091100523,2.67773831936296));
#69199=CARTESIAN_POINT('Ctrl Pts',(20.9673281879432,1.78943621037185,2.68030513403046));
#69200=CARTESIAN_POINT('Origin',(-1.72497344927317,0.,0.));
#69201=CARTESIAN_POINT('',(22.4670531482195,1.78943621037803,2.68030513402633));
#69202=CARTESIAN_POINT('',(22.2208495079139,1.78943601979592,2.68030526126352));
#69203=CARTESIAN_POINT('',(-1.72497344927317,1.78943621037804,2.68030513402633));
#69204=CARTESIAN_POINT('',(21.6465734492304,-3.22274996585741,-0.000469111987035887));
#69205=CARTESIAN_POINT('Ctrl Pts',(21.6465734492731,-3.22274996585731,-0.000469112675110201));
#69206=CARTESIAN_POINT('Ctrl Pts',(21.6481278312453,-3.22274632312903,-0.0254942357564947));
#69207=CARTESIAN_POINT('Ctrl Pts',(21.6496822132174,-3.22245120008828,-0.0505169572527867));
#69208=CARTESIAN_POINT('Ctrl Pts',(21.6512365951896,-3.22186473262596,-0.0755328217469976));
#69209=CARTESIAN_POINT('Ctrl Pts',(21.6574088432824,-3.21953594681871,-0.174867557146353));
#69210=CARTESIAN_POINT('Ctrl Pts',(21.6635810913751,-3.21260480812707,-0.274269331810238));
#69211=CARTESIAN_POINT('Ctrl Pts',(21.6697533394679,-3.20105952006451,-0.373276722425059));
#69212=CARTESIAN_POINT('Ctrl Pts',(21.6759172281205,-3.18952986846744,-0.47215002148327));
#69213=CARTESIAN_POINT('Ctrl Pts',(21.6820811167731,-3.17339853837091,-0.570629570496825));
#69214=CARTESIAN_POINT('Ctrl Pts',(21.6882450054258,-3.15270573127254,-0.668254543195374));
#69215=CARTESIAN_POINT('Ctrl Pts',(21.6944023670843,-3.13203483596349,-0.765776139980608));
#69216=CARTESIAN_POINT('Ctrl Pts',(21.7005597287429,-3.10681215609342,-0.862444536922237));
#69217=CARTESIAN_POINT('Ctrl Pts',(21.7067170904014,-3.07712950881661,-0.95780559012259));
#69218=CARTESIAN_POINT('Ctrl Pts',(21.7128699545477,-3.04746854259035,-1.05309698889499));
#69219=CARTESIAN_POINT('Ctrl Pts',(21.719022818694,-3.01335421450438,-1.14708252897496));
#69220=CARTESIAN_POINT('Ctrl Pts',(21.7251756828403,-2.97492886656484,-1.23932070158585));
#69221=CARTESIAN_POINT('Ctrl Pts',(21.7313262159769,-2.93651807605081,-1.3315239298072));
#69222=CARTESIAN_POINT('Ctrl Pts',(21.7374767491134,-2.89379967775345,-1.42198070540096));
#69223=CARTESIAN_POINT('Ctrl Pts',(21.7436272822499,-2.84696477031514,-1.51026790970492));
#69224=CARTESIAN_POINT('Ctrl Pts',(21.7497771304652,-2.80013507839656,-1.59854528237514));
#69225=CARTESIAN_POINT('Ctrl Pts',(21.7559269786804,-2.74918999228949,-1.68465318037131));
#69226=CARTESIAN_POINT('Ctrl Pts',(21.7620768268956,-2.694366881103,-1.76819248740495));
#69227=CARTESIAN_POINT('Ctrl Pts',(21.7682276352747,-2.63953521049007,-1.85174483726922));
#69228=CARTESIAN_POINT('Ctrl Pts',(21.7743784436539,-2.58082455052733,-1.93272743643165));
#69229=CARTESIAN_POINT('Ctrl Pts',(21.780529252033,-2.51851539447775,-2.01077044196462));
#69230=CARTESIAN_POINT('Ctrl Pts',(21.7866866383992,-2.45613960185024,-2.08889691065372));
#69231=CARTESIAN_POINT('Ctrl Pts',(21.7928440247654,-2.39015789979764,-2.16407716785023));
#69232=CARTESIAN_POINT('Ctrl Pts',(21.7990014111316,-2.32089077774229,-2.23597485681096));
#69233=CARTESIAN_POINT('Ctrl Pts',(21.8051622338685,-2.25158499845486,-2.30791267109472));
#69234=CARTESIAN_POINT('Ctrl Pts',(21.8113230566055,-2.17899046327251,-2.37656397033987));
#69235=CARTESIAN_POINT('Ctrl Pts',(21.8174838793425,-2.10346265252566,-2.44163110070496));
#69236=CARTESIAN_POINT('Ctrl Pts',(21.8236550022592,-2.02780856805557,-2.50680701575122));
#69237=CARTESIAN_POINT('Ctrl Pts',(21.8298261251758,-1.94921175432683,-2.56838652443545));
#69238=CARTESIAN_POINT('Ctrl Pts',(21.8359972480925,-1.8680588202361,-2.62611382210256));
#69239=CARTESIAN_POINT('Ctrl Pts',(21.8406927700381,-1.80631067680886,-2.67003772326466));
#69240=CARTESIAN_POINT('Ctrl Pts',(21.8453882919836,-1.74308331769695,-2.71173226350374));
#69241=CARTESIAN_POINT('Ctrl Pts',(21.8500838139291,-1.67855636729737,-2.75110270333651));
#69242=CARTESIAN_POINT('Ctrl Pts',(21.8562560620219,-1.59373590406534,-2.80285501649537));
#69243=CARTESIAN_POINT('Ctrl Pts',(21.8624283101147,-1.50637050747736,-2.85077203819863));
#69244=CARTESIAN_POINT('Ctrl Pts',(21.8686005582074,-1.41684195245698,-2.89459434882643));
#69245=CARTESIAN_POINT('Ctrl Pts',(21.87476444686,-1.32743465124642,-2.93835730831069));
#69246=CARTESIAN_POINT('Ctrl Pts',(21.8809283355127,-1.23587040140118,-2.9780363901404));
#69247=CARTESIAN_POINT('Ctrl Pts',(21.8870922241653,-1.14255859144916,-3.01341623869085));
#69248=CARTESIAN_POINT('Ctrl Pts',(21.8932495858238,-1.0493455901658,-3.04875862321896));
#69249=CARTESIAN_POINT('Ctrl Pts',(21.8994069474824,-0.954389111677636,
-3.07981067210762));
#69250=CARTESIAN_POINT('Ctrl Pts',(21.9055643091409,-0.85812083235513,-3.10640406250992));
#69251=CARTESIAN_POINT('Ctrl Pts',(21.9117171732872,-0.761922870124273,
-3.13297802834285));
#69252=CARTESIAN_POINT('Ctrl Pts',(21.9178700374335,-0.664415429509654,
-3.15509969531556));
#69253=CARTESIAN_POINT('Ctrl Pts',(21.9240229015799,-0.566046877410062,
-3.17265007447628));
#69254=CARTESIAN_POINT('Ctrl Pts',(21.9301734347164,-0.467715592191445,
-3.19019380468387));
#69255=CARTESIAN_POINT('Ctrl Pts',(21.9363239678529,-0.368524270856346,
-3.20316961200751));
#69256=CARTESIAN_POINT('Ctrl Pts',(21.9424745009895,-0.268932173587789,
-3.2115094657356));
#69257=CARTESIAN_POINT('Ctrl Pts',(21.9486243492047,-0.169351166862188,
-3.21984839074034));
#69258=CARTESIAN_POINT('Ctrl Pts',(21.9547741974199,-0.0693699057953061,
-3.22355235229859));
#69259=CARTESIAN_POINT('Ctrl Pts',(21.9609240456351,0.030547521525458,-3.22260522115705));
#69260=CARTESIAN_POINT('Ctrl Pts',(21.9670748540142,0.130480548761247,-3.22165794214175));
#69261=CARTESIAN_POINT('Ctrl Pts',(21.9732256623934,0.230349288058754,-3.21605813219087));
#69262=CARTESIAN_POINT('Ctrl Pts',(21.9793764707725,0.329690958671108,-3.20584176687973));
#69263=CARTESIAN_POINT('Ctrl Pts',(21.9855338571387,0.429138870314394,-3.19561447566834));
#69264=CARTESIAN_POINT('Ctrl Pts',(21.9916912435049,0.528058154734965,-3.18076081458409));
#69265=CARTESIAN_POINT('Ctrl Pts',(21.9978486298711,0.625992573729931,-3.16136851065088));
#69266=CARTESIAN_POINT('Ctrl Pts',(22.004009452608,0.723981648865477,-3.14196538408248));
#69267=CARTESIAN_POINT('Ctrl Pts',(22.010170275345,0.820984342240742,-3.11801867440618));
#69268=CARTESIAN_POINT('Ctrl Pts',(22.0163310980819,0.916558052936471,-3.08966647036493));
#69269=CARTESIAN_POINT('Ctrl Pts',(22.0225022209986,1.01229155177081,-3.06126686473306));
#69270=CARTESIAN_POINT('Ctrl Pts',(22.0286733439153,1.10659088535593,-3.02844719527263));
#69271=CARTESIAN_POINT('Ctrl Pts',(22.034844466832,1.1990318251467,-2.99139436463756));
#69272=CARTESIAN_POINT('Ctrl Pts',(22.0395399887776,1.26936885575224,-2.96320137905889));
#69273=CARTESIAN_POINT('Ctrl Pts',(22.0442355107232,1.33863035514316,-2.93255862578227));
#69274=CARTESIAN_POINT('Ctrl Pts',(22.0489310326689,1.40663950287093,-2.89956597984302));
#69275=CARTESIAN_POINT('Ctrl Pts',(22.0551032807616,1.49603730299087,-2.85619725569856));
#69276=CARTESIAN_POINT('Ctrl Pts',(22.0612755288544,1.58358489327371,-2.80861392956884));
#69277=CARTESIAN_POINT('Ctrl Pts',(22.0674477769472,1.66885761801247,-2.75699688307799));
#69278=CARTESIAN_POINT('Ctrl Pts',(22.0736116655998,1.75401485286383,-2.70544974460175));
#69279=CARTESIAN_POINT('Ctrl Pts',(22.0797755542524,1.83690297764013,-2.6498799672432));
#69280=CARTESIAN_POINT('Ctrl Pts',(22.0859394429051,1.91711947270133,-2.59051548729));
#69281=CARTESIAN_POINT('Ctrl Pts',(22.0920968045636,1.99725102583408,-2.53121386888922));
#69282=CARTESIAN_POINT('Ctrl Pts',(22.0982541662222,2.07471622635874,-2.46812579351227));
#69283=CARTESIAN_POINT('Ctrl Pts',(22.1044115278807,2.1491400677625,-2.40152337728322));
#69284=CARTESIAN_POINT('Ctrl Pts',(22.110564392027,2.22350954787386,-2.33496960935496));
#69285=CARTESIAN_POINT('Ctrl Pts',(22.1167172561734,2.29484176286572,-2.2649068929557));
#69286=CARTESIAN_POINT('Ctrl Pts',(22.1228701203197,2.36279418159805,-2.19164805977292));
#69287=CARTESIAN_POINT('Ctrl Pts',(22.1290206534562,2.43072085658761,-2.1184169806656));
#69288=CARTESIAN_POINT('Ctrl Pts',(22.1351711865928,2.49526998446236,-2.04199250883538));
#69289=CARTESIAN_POINT('Ctrl Pts',(22.1413217197293,2.55613601049785,-1.96272419313976));
#69290=CARTESIAN_POINT('Ctrl Pts',(22.1474715679445,2.61699525851286,-1.88346470473751));
#69291=CARTESIAN_POINT('Ctrl Pts',(22.1536214161597,2.67417195558059,-1.8013623466216));
#69292=CARTESIAN_POINT('Ctrl Pts',(22.1597712643749,2.72740159644865,-1.71679879257569));
#69293=CARTESIAN_POINT('Ctrl Pts',(22.1659220727541,2.78063954795779,-1.63222203578531));
#69294=CARTESIAN_POINT('Ctrl Pts',(22.1720728811332,2.82992898782414,-1.54518368746661));
#69295=CARTESIAN_POINT('Ctrl Pts',(22.1782236895124,2.87504994873398,-1.45609249527107));
#69296=CARTESIAN_POINT('Ctrl Pts',(22.1843810758785,2.92021916429237,-1.36690602442718));
#69297=CARTESIAN_POINT('Ctrl Pts',(22.1905384622447,2.96121080212157,-1.2756627139547));
#69298=CARTESIAN_POINT('Ctrl Pts',(22.1966958486109,2.99785196630828,-1.18279379039694));
#69299=CARTESIAN_POINT('Ctrl Pts',(22.2028566713479,3.03451357953265,-1.08987303769683));
#69300=CARTESIAN_POINT('Ctrl Pts',(22.2090174940849,3.06681974342698,-0.995325276217104));
#69301=CARTESIAN_POINT('Ctrl Pts',(22.2151783168218,3.09464730062386,-0.899597491793666));
#69302=CARTESIAN_POINT('Ctrl Pts',(22.2213494397385,3.12252138226282,-0.80370966163823));
#69303=CARTESIAN_POINT('Ctrl Pts',(22.2275205626552,3.14590179897318,-0.706638290304755));
#69304=CARTESIAN_POINT('Ctrl Pts',(22.2336916855719,3.16471639021537,-0.60884130280574));
#69305=CARTESIAN_POINT('Ctrl Pts',(22.2383872075174,3.17903215207373,-0.534428929691776));
#69306=CARTESIAN_POINT('Ctrl Pts',(22.243082729463,3.1907055967668,-0.459596688545039));
#69307=CARTESIAN_POINT('Ctrl Pts',(22.2477782514085,3.19972513143753,-0.384547325757277));
#69308=CARTESIAN_POINT('Ctrl Pts',(22.2539504995013,3.21158127997964,-0.285895186186295));
#69309=CARTESIAN_POINT('Ctrl Pts',(22.260122747594,3.21889164035863,-0.186520581175701));
#69310=CARTESIAN_POINT('Ctrl Pts',(22.2662949956868,3.22157875612023,-0.0868785394378976));
#69311=CARTESIAN_POINT('Ctrl Pts',(22.2724588843394,3.22426223256224,0.0126285511977798));
#69312=CARTESIAN_POINT('Ctrl Pts',(22.278622772992,3.22233489826665,0.112401928243455));
#69313=CARTESIAN_POINT('Ctrl Pts',(22.2847866616447,3.21577084877965,0.211979741105177));
#69314=CARTESIAN_POINT('Ctrl Pts',(22.2909440233032,3.20921375002044,0.311452110174464));
#69315=CARTESIAN_POINT('Ctrl Pts',(22.2971013849618,3.19802972574339,0.410728895718908));
#69316=CARTESIAN_POINT('Ctrl Pts',(22.3032587466203,3.18224491259648,0.509347502942561));
#69317=CARTESIAN_POINT('Ctrl Pts',(22.3094116107666,3.16647162912644,0.607894076328115));
#69318=CARTESIAN_POINT('Ctrl Pts',(22.3155644749129,3.14610430657407,0.705782999587667));
#69319=CARTESIAN_POINT('Ctrl Pts',(22.3217173390592,3.12122089164884,0.802556981176296));
#69320=CARTESIAN_POINT('Ctrl Pts',(22.3278678721958,3.096346903794,0.899294299986199));
#69321=CARTESIAN_POINT('Ctrl Pts',(22.3340184053323,3.06696033120595,0.994917096198299));
#69322=CARTESIAN_POINT('Ctrl Pts',(22.3401689384688,3.03319000093142,1.08897932980826));
#69323=CARTESIAN_POINT('Ctrl Pts',(22.346318786684,2.99942343130967,1.1830310886791));
#69324=CARTESIAN_POINT('Ctrl Pts',(22.3524686348992,2.96127422133949,1.27552222162924));
#69325=CARTESIAN_POINT('Ctrl Pts',(22.3586184831144,2.91892041771169,1.36602384955966));
#69326=CARTESIAN_POINT('Ctrl Pts',(22.3647692914936,2.87656000146629,1.45653960733456));
#69327=CARTESIAN_POINT('Ctrl Pts',(22.3709200998727,2.82999387180943,1.54506484966208));
#69328=CARTESIAN_POINT('Ctrl Pts',(22.3770709082518,2.77944693233037,1.63119352403671));
#69329=CARTESIAN_POINT('Ctrl Pts',(22.383228294618,2.72884593538555,1.71741430879258));
#69330=CARTESIAN_POINT('Ctrl Pts',(22.3893856809842,2.67425584755697,1.80123303217076));
#69331=CARTESIAN_POINT('Ctrl Pts',(22.3955430673504,2.61594593386626,1.88227108398036));
#69332=CARTESIAN_POINT('Ctrl Pts',(22.4017038900874,2.55760347804303,1.96335436225068));
#69333=CARTESIAN_POINT('Ctrl Pts',(22.4078647128243,2.49553733188193,2.04165353802593));
#69334=CARTESIAN_POINT('Ctrl Pts',(22.4140255355613,2.43005691140302,2.11682332041255));
#69335=CARTESIAN_POINT('Ctrl Pts',(22.420196658478,2.36446701526989,2.19211877794061));
#69336=CARTESIAN_POINT('Ctrl Pts',(22.4263677813946,2.2954517431091,2.26427407730709));
#69337=CARTESIAN_POINT('Ctrl Pts',(22.4325389043113,2.22335728758057,2.33298091167981));
#69338=CARTESIAN_POINT('Ctrl Pts',(22.4372344262569,2.16850161501311,2.38525899023476));
#69339=CARTESIAN_POINT('Ctrl Pts',(22.4419299482026,2.11186401776716,2.43554135498066));
#69340=CARTESIAN_POINT('Ctrl Pts',(22.4466254701482,2.05360877953829,2.48370862685285));
#69341=CARTESIAN_POINT('Ctrl Pts',(22.4527985050484,1.97702269967905,2.5470324178519));
#69342=CARTESIAN_POINT('Ctrl Pts',(22.4589715399486,1.89737013881085,2.60692201962735));
#69343=CARTESIAN_POINT('Ctrl Pts',(22.4651445748488,1.81499212238597,2.66306611975311));
#69344=CARTESIAN_POINT('Ctrl Pts',(22.4657807659724,1.80650226874485,2.66885231385642));
#69345=CARTESIAN_POINT('Ctrl Pts',(22.4664169570959,1.79798349964587,2.67459875801627));
#69346=CARTESIAN_POINT('Ctrl Pts',(22.4670531482195,1.78943621037803,2.68030513402633));
#69347=CARTESIAN_POINT('Ctrl Pts',(21.2168443958857,1.78943621037803,2.68030513402633));
#69348=CARTESIAN_POINT('Ctrl Pts',(21.2230150525931,1.70635126714696,2.73577464160868));
#69349=CARTESIAN_POINT('Ctrl Pts',(21.2291857093005,1.62077675188503,2.7873158961107));
#69350=CARTESIAN_POINT('Ctrl Pts',(21.2353563660079,1.53312715272033,2.83472021478164));
#69351=CARTESIAN_POINT('Ctrl Pts',(21.2414182965754,1.44702192768618,2.88128927574313));
#69352=CARTESIAN_POINT('Ctrl Pts',(21.2474802271428,1.3589145411085,2.92386591393451));
#69353=CARTESIAN_POINT('Ctrl Pts',(21.2535421577103,1.26921500444823,2.96229823532059));
#69354=CARTESIAN_POINT('Ctrl Pts',(21.259714405803,1.1778830784366,3.00142996402264));
#69355=CARTESIAN_POINT('Ctrl Pts',(21.2658866538958,1.08457897127673,3.03640276884295));
#69356=CARTESIAN_POINT('Ctrl Pts',(21.2720589019886,0.989717541342602,3.06701430561691));
#69357=CARTESIAN_POINT('Ctrl Pts',(21.2782227906412,0.89498458784571,3.09758438337864));
#69358=CARTESIAN_POINT('Ctrl Pts',(21.2843866792939,0.798698913535267,3.12380480113236));
#69359=CARTESIAN_POINT('Ctrl Pts',(21.2905505679465,0.701296426591066,3.14552076523914));
#69360=CARTESIAN_POINT('Ctrl Pts',(21.296707929605,0.603997079968211,3.16721373412693));
#69361=CARTESIAN_POINT('Ctrl Pts',(21.3028652912636,0.505583693465033,3.18441163818673));
#69362=CARTESIAN_POINT('Ctrl Pts',(21.3090226529221,0.406507530472406,3.19700941352528));
#69363=CARTESIAN_POINT('Ctrl Pts',(21.3151755170684,0.307503735529606,3.2095979870901));
#69364=CARTESIAN_POINT('Ctrl Pts',(21.3213283812148,0.207838556199264,3.21759305769202));
#69365=CARTESIAN_POINT('Ctrl Pts',(21.3274812453611,0.107972742892041,3.22094077084512));
#69366=CARTESIAN_POINT('Ctrl Pts',(21.3336317784976,0.00814476370253209,
3.22428721571863));
#69367=CARTESIAN_POINT('Ctrl Pts',(21.3397823116341,-0.0918832647827476,
3.222989787007));
#69368=CARTESIAN_POINT('Ctrl Pts',(21.3459328447707,-0.191647074731872,
3.21704662093149));
#69369=CARTESIAN_POINT('Ctrl Pts',(21.3520826929859,-0.291399775016203,
3.21110411668498));
#69370=CARTESIAN_POINT('Ctrl Pts',(21.3582325412011,-0.390887881655189,
3.20051692946857));
#69371=CARTESIAN_POINT('Ctrl Pts',(21.3643823894163,-0.489649747289857,
3.18533525511507));
#69372=CARTESIAN_POINT('Ctrl Pts',(21.3705331977954,-0.588427032423949,
3.17015121047606));
#69373=CARTESIAN_POINT('Ctrl Pts',(21.3766840061746,-0.686477421965865,
3.15037131990363));
#69374=CARTESIAN_POINT('Ctrl Pts',(21.3828348145537,-0.783347990602642,
3.12609716549547));
#69375=CARTESIAN_POINT('Ctrl Pts',(21.3889922009199,-0.880322157548261,
3.10179705107303));
#69376=CARTESIAN_POINT('Ctrl Pts',(21.3951495872861,-0.976113561814008,
3.07299318073088));
#69377=CARTESIAN_POINT('Ctrl Pts',(21.4013069736523,-1.07028313148713,3.03983742673093));
#69378=CARTESIAN_POINT('Ctrl Pts',(21.4074677963893,-1.16450525617911,3.00666316886308));
#69379=CARTESIAN_POINT('Ctrl Pts',(21.4136286191262,-1.25710334114861,2.9691323537059));
#69380=CARTESIAN_POINT('Ctrl Pts',(21.4197894418632,-1.34765899203866,2.92744475672511));
#69381=CARTESIAN_POINT('Ctrl Pts',(21.4259605647799,-1.43836604145444,2.88568746292626));
#69382=CARTESIAN_POINT('Ctrl Pts',(21.4321316876966,-1.52702345013386,2.83975970547664));
#69383=CARTESIAN_POINT('Ctrl Pts',(21.4383028106132,-1.61323796734748,2.7899069560128));
#69384=CARTESIAN_POINT('Ctrl Pts',(21.4429983325588,-1.67883739926089,2.7519746895008));
#69385=CARTESIAN_POINT('Ctrl Pts',(21.4476938545044,-1.74302304664015,2.71177100438844));
#69386=CARTESIAN_POINT('Ctrl Pts',(21.4523893764499,-1.80563413322286,2.66941996310819));
#69387=CARTESIAN_POINT('Ctrl Pts',(21.4585372899088,-1.88761171661731,2.61396914428544));
#69388=CARTESIAN_POINT('Ctrl Pts',(21.4646852033676,-1.96718249968798,2.55463705375598));
#69389=CARTESIAN_POINT('Ctrl Pts',(21.4708331168264,-2.04395372661063,2.49166023485838));
#69390=CARTESIAN_POINT('Ctrl Pts',(21.4769726892617,-2.12062079614558,2.42876885814016));
#69391=CARTESIAN_POINT('Ctrl Pts',(21.4831122616971,-2.1944955217772,2.36224285512097));
#69392=CARTESIAN_POINT('Ctrl Pts',(21.4892518341324,-2.26521360153258,2.29236229726712));
#69393=CARTESIAN_POINT('Ctrl Pts',(21.4953849289502,-2.33585706946764,2.2225554675977));
#69394=CARTESIAN_POINT('Ctrl Pts',(21.501518023768,-2.40335020165196,2.14940142452263));
#69395=CARTESIAN_POINT('Ctrl Pts',(21.5076511185858,-2.46736211538117,2.0732201412493));
#69396=CARTESIAN_POINT('Ctrl Pts',(21.5137798105395,-2.53132807584215,1.99709354746641));
#69397=CARTESIAN_POINT('Ctrl Pts',(21.5199085024933,-2.59181750451994,1.91794436790151));
#69398=CARTESIAN_POINT('Ctrl Pts',(21.5260371944471,-2.64853740050429,1.83612831812757));
#69399=CARTESIAN_POINT('Ctrl Pts',(21.5321636552663,-2.70523664775598,1.75434205327671));
#69400=CARTESIAN_POINT('Ctrl Pts',(21.5382901160854,-2.75816883919948,1.66989120679491));
#69401=CARTESIAN_POINT('Ctrl Pts',(21.5444165769046,-2.80708278322244,1.58316259766209));
#69402=CARTESIAN_POINT('Ctrl Pts',(21.5505424801101,-2.855992275232,1.49644188233004));
#69403=CARTESIAN_POINT('Ctrl Pts',(21.5566683833156,-2.90088403178773,1.40744419831191));
#69404=CARTESIAN_POINT('Ctrl Pts',(21.5627942865211,-2.94155207588588,1.31658229797894));
#69405=CARTESIAN_POINT('Ctrl Pts',(21.5689213047369,-2.98222752220502,1.22570385935696));
#69406=CARTESIAN_POINT('Ctrl Pts',(21.5750483229527,-3.01867755048412,1.13296093063977));
#69407=CARTESIAN_POINT('Ctrl Pts',(21.5811753411685,-3.05074414799851,1.03878665083492));
#69408=CARTESIAN_POINT('Ctrl Pts',(21.5873089114137,-3.08284503646537,0.944511664188625));
#69409=CARTESIAN_POINT('Ctrl Pts',(21.593442481659,-3.11055299542423,0.848802686451053));
#69410=CARTESIAN_POINT('Ctrl Pts',(21.5995760519042,-3.13375984553868,0.752108232230822));
#69411=CARTESIAN_POINT('Ctrl Pts',(21.6057132516376,-3.1569804281099,0.655356559887253));
#69412=CARTESIAN_POINT('Ctrl Pts',(21.611850451371,-3.17569451746197,0.557618680284896));
#69413=CARTESIAN_POINT('Ctrl Pts',(21.6179876511044,-3.18984542193015,0.459351441372813));
#69414=CARTESIAN_POINT('Ctrl Pts',(21.6241346487006,-3.20401891790996,0.36092732164257));
#69415=CARTESIAN_POINT('Ctrl Pts',(21.6302816462967,-3.21361464287684,0.261972591016499));
#69416=CARTESIAN_POINT('Ctrl Pts',(21.6364286438928,-3.21862793008776,0.16294726189478));
#69417=CARTESIAN_POINT('Ctrl Pts',(21.639810245672,-3.2213858522582,0.108471198758849));
#69418=CARTESIAN_POINT('Ctrl Pts',(21.6431918474512,-3.2227578907038,0.0539737484253642));
#69419=CARTESIAN_POINT('Ctrl Pts',(21.6465734492304,-3.22274996585741,-0.000469111987035492));
#69420=CARTESIAN_POINT('',(21.3984065856094,-3.22274887336959,-0.00269475323696564));
#69421=CARTESIAN_POINT('Ctrl Pts',(20.9673281879432,1.78943621037185,2.68030513403046));
#69422=CARTESIAN_POINT('Ctrl Pts',(20.9678519537231,1.78239104114818,2.68500865854972));
#69423=CARTESIAN_POINT('Ctrl Pts',(20.9683767692861,1.77532739395979,2.6896843611713));
#69424=CARTESIAN_POINT('Ctrl Pts',(20.9698744965502,1.75515725249851,2.70292169002813));
#69425=CARTESIAN_POINT('Ctrl Pts',(20.9708499289186,1.74200684879726,2.71141563914688));
#69426=CARTESIAN_POINT('Ctrl Pts',(20.973754948643,1.70280415933879,2.73633404933602));
#69427=CARTESIAN_POINT('Ctrl Pts',(20.9756946761167,1.67657833274058,2.75248088512964));
#69428=CARTESIAN_POINT('Ctrl Pts',(20.9826153551802,1.5828538307409,2.80834913442632));
#69429=CARTESIAN_POINT('Ctrl Pts',(20.9876688686059,1.51414740036302,2.84598087202798));
#69430=CARTESIAN_POINT('Ctrl Pts',(21.0068117095735,1.2528231808831,2.97697020993401));
#69431=CARTESIAN_POINT('Ctrl Pts',(21.0213819277774,1.05244110936447,3.05356635293571));
#69432=CARTESIAN_POINT('Ctrl Pts',(21.046228958345,0.697074829497055,3.15024077252431));
#69433=CARTESIAN_POINT('Ctrl Pts',(21.0565237049827,0.545435375082559,3.18000671247934));
#69434=CARTESIAN_POINT('Ctrl Pts',(21.0670319800635,0.380291278217971,3.20025636091708));
#69435=CARTESIAN_POINT('Ctrl Pts',(21.0677881914932,0.368344508664027,3.20165341121864));
#69436=CARTESIAN_POINT('Ctrl Pts',(21.068876548389,0.351055409271595,3.20357713689932));
#69437=CARTESIAN_POINT('Ctrl Pts',(21.0692116299518,0.345719320114563,3.20415738145569));
#69438=CARTESIAN_POINT('Ctrl Pts',(21.0697993577351,0.336336263142779,3.20515397933855));
#69439=CARTESIAN_POINT('Ctrl Pts',(21.070052323158,0.332289924608085,3.20557600439013));
#69440=CARTESIAN_POINT('Ctrl Pts',(21.0705797549374,0.323836928368797,3.20644145759184));
#69441=CARTESIAN_POINT('Ctrl Pts',(21.0708541399769,0.319430161616614,3.20688346366882));
#69442=CARTESIAN_POINT('Ctrl Pts',(21.0715739424613,0.307845857021995,3.20802127352615));
#69443=CARTESIAN_POINT('Ctrl Pts',(21.0720185183005,0.300666820944817,3.20870207844611));
#69444=CARTESIAN_POINT('Ctrl Pts',(21.0739952453701,0.26864236383407,3.2116306114496));
#69445=CARTESIAN_POINT('Ctrl Pts',(21.0755130282646,0.243772813990065,3.21361397938985));
#69446=CARTESIAN_POINT('Ctrl Pts',(21.0882704438399,0.0326447176733997,
3.2279865072295));
#69447=CARTESIAN_POINT('Ctrl Pts',(21.0987407651758,-0.154368853068181,
3.22446149910762));
#69448=CARTESIAN_POINT('Ctrl Pts',(21.1216091184046,-0.561055231750271,
3.18130941823188));
#69449=CARTESIAN_POINT('Ctrl Pts',(21.1339621701854,-0.779023881877673,
3.13506357217085));
#69450=CARTESIAN_POINT('Ctrl Pts',(21.147853582335,-1.00363680752323,3.06251881433963));
#69451=CARTESIAN_POINT('Ctrl Pts',(21.1486688813881,-1.01675257093334,3.0581894203909));
#69452=CARTESIAN_POINT('Ctrl Pts',(21.1511575286567,-1.0565769869764,3.04475923543864));
#69453=CARTESIAN_POINT('Ctrl Pts',(21.152838833581,-1.08319380441311,3.03539204063635));
#69454=CARTESIAN_POINT('Ctrl Pts',(21.156281573473,-1.13707646557409,3.01563027823277));
#69455=CARTESIAN_POINT('Ctrl Pts',(21.1580436226883,-1.16433092019963,3.00521251935973));
#69456=CARTESIAN_POINT('Ctrl Pts',(21.1605081648904,-1.20198224083631,2.99023159652657));
#69457=CARTESIAN_POINT('Ctrl Pts',(21.1612001154945,-1.21250264174925,2.98598118660121));
#69458=CARTESIAN_POINT('Ctrl Pts',(21.1623125170718,-1.22933326762929,2.97907773212496));
#69459=CARTESIAN_POINT('Ctrl Pts',(21.1627317700714,-1.23565793130111,2.97645995985338));
#69460=CARTESIAN_POINT('Ctrl Pts',(21.163598848394,-1.24869955256265,2.97101331364428));
#69461=CARTESIAN_POINT('Ctrl Pts',(21.164046762773,-1.25541534443376,2.96818176565912));
#69462=CARTESIAN_POINT('Ctrl Pts',(21.1650805506339,-1.27086616197899,2.96160549100909));
#69463=CARTESIAN_POINT('Ctrl Pts',(21.1656669641665,-1.27959431115376,2.95784487115205));
#69464=CARTESIAN_POINT('Ctrl Pts',(21.1675209926088,-1.30707422927504,2.9458604483344));
#69465=CARTESIAN_POINT('Ctrl Pts',(21.1687933954435,-1.32576404059374,2.93749663818966));
#69466=CARTESIAN_POINT('Ctrl Pts',(21.1717680491982,-1.36905842856939,2.91762478032248));
#69467=CARTESIAN_POINT('Ctrl Pts',(21.1734748522124,-1.39359945035681,2.90598276643642));
#69468=CARTESIAN_POINT('Ctrl Pts',(21.1793476837579,-1.47700437773042,2.8651168303697));
#69469=CARTESIAN_POINT('Ctrl Pts',(21.1835642172386,-1.53511703010977,2.83440489336424));
#69470=CARTESIAN_POINT('Ctrl Pts',(21.196526801783,-1.70846614002117,2.73589648621368));
#69471=CARTESIAN_POINT('Ctrl Pts',(21.2054408652303,-1.82045272536734,2.66269259696062));
#69472=CARTESIAN_POINT('Ctrl Pts',(21.2245656616602,-2.04772807408802,2.49307242815482));
#69473=CARTESIAN_POINT('Ctrl Pts',(21.2347806636282,-2.16148944811625,2.39511269166931));
#69474=CARTESIAN_POINT('Ctrl Pts',(21.2460437697052,-2.28144957758011,2.27628267483768));
#69475=CARTESIAN_POINT('Ctrl Pts',(21.2473011018671,-2.29476395691983,2.26285956118005));
#69476=CARTESIAN_POINT('Ctrl Pts',(21.2495655036409,-2.31861475270052,2.23838697522766));
#69477=CARTESIAN_POINT('Ctrl Pts',(21.2505741230767,-2.32919220031012,2.22737835338654));
#69478=CARTESIAN_POINT('Ctrl Pts',(21.2523888155589,-2.34814564999663,2.20736963520577));
#69479=CARTESIAN_POINT('Ctrl Pts',(21.2531960696954,-2.35654909979147,2.19839601705703));
#69480=CARTESIAN_POINT('Ctrl Pts',(21.2579586936655,-2.40597351979519,2.14500913908558));
#69481=CARTESIAN_POINT('Ctrl Pts',(21.2618567675184,-2.44579267031167,2.09949330414281));
#69482=CARTESIAN_POINT('Ctrl Pts',(21.2662990106982,-2.49069513289802,2.04515421901408));
#69483=CARTESIAN_POINT('Ctrl Pts',(21.2669282221285,-2.49704381946209,2.03739789794604));
#69484=CARTESIAN_POINT('Ctrl Pts',(21.2678740130633,-2.50657112729013,2.02564676194547));
#69485=CARTESIAN_POINT('Ctrl Pts',(21.2681924873658,-2.50977654069463,2.02167389481635));
#69486=CARTESIAN_POINT('Ctrl Pts',(21.2687607639403,-2.51549161722652,2.01455594996598));
#69487=CARTESIAN_POINT('Ctrl Pts',(21.2690108216041,-2.5180048335561,2.01141378405463));
#69488=CARTESIAN_POINT('Ctrl Pts',(21.2695473914765,-2.52339430252902,2.00464963206559));
#69489=CARTESIAN_POINT('Ctrl Pts',(21.2698337656224,-2.52626863434576,2.00102617202707));
#69490=CARTESIAN_POINT('Ctrl Pts',(21.2706196279006,-2.53415015079322,1.99104647075088));
#69491=CARTESIAN_POINT('Ctrl Pts',(21.2711179744844,-2.53914125479659,1.98467748688704));
#69492=CARTESIAN_POINT('Ctrl Pts',(21.2737632729568,-2.5655939469439,1.950658952562));
#69493=CARTESIAN_POINT('Ctrl Pts',(21.2758811984931,-2.58662899950123,1.92267867988402));
#69494=CARTESIAN_POINT('Ctrl Pts',(21.2820194295138,-2.64698514081654,1.83961060355968));
#69495=CARTESIAN_POINT('Ctrl Pts',(21.2859688667637,-2.68503358972743,1.78361805399187));
#69496=CARTESIAN_POINT('Ctrl Pts',(21.3025387302631,-2.8394473357266,1.5402276787012));
#69497=CARTESIAN_POINT('Ctrl Pts',(21.3145880491841,-2.93817639072103,1.34234593432749));
#69498=CARTESIAN_POINT('Ctrl Pts',(21.3296145277263,-3.03176495316452,1.09386408300306));
#69499=CARTESIAN_POINT('Ctrl Pts',(21.3321724464895,-3.0467238542468,1.0514803570573));
#69500=CARTESIAN_POINT('Ctrl Pts',(21.3417543123333,-3.09899900316382,0.892872567378146));
#69501=CARTESIAN_POINT('Ctrl Pts',(21.3489062984102,-3.13058609446599,0.77488178170674));
#69502=CARTESIAN_POINT('Ctrl Pts',(21.3573904709786,-3.15913214990817,0.637446161202819));
#69503=CARTESIAN_POINT('Ctrl Pts',(21.3585031433111,-3.16270656563304,0.61946808411316));
#69504=CARTESIAN_POINT('Ctrl Pts',(21.3601840153322,-3.16785160621631,0.592384266764949));
#69505=CARTESIAN_POINT('Ctrl Pts',(21.3607485552872,-3.16953679392388,0.583300460893615));
#69506=CARTESIAN_POINT('Ctrl Pts',(21.3617567435741,-3.17247000074863,0.567101262646638));
#69507=CARTESIAN_POINT('Ctrl Pts',(21.3621999044332,-3.17373320423832,0.559988655876658));
#69508=CARTESIAN_POINT('Ctrl Pts',(21.3630578002243,-3.17612812586379,0.546235361246301));
#69509=CARTESIAN_POINT('Ctrl Pts',(21.3634724333618,-3.17726295870149,0.539595248257126));
#69510=CARTESIAN_POINT('Ctrl Pts',(21.364371520644,-3.17967467608105,0.525212430009469));
#69511=CARTESIAN_POINT('Ctrl Pts',(21.3648562092225,-3.18094411383787,0.517468535506325));
#69512=CARTESIAN_POINT('Ctrl Pts',(21.3660354170185,-3.18395807212842,0.498652379499739));
#69513=CARTESIAN_POINT('Ctrl Pts',(21.3667308679152,-3.18567312596127,0.487575563444652));
#69514=CARTESIAN_POINT('Ctrl Pts',(21.3700816293345,-3.193636698049,0.434305762110385));
#69515=CARTESIAN_POINT('Ctrl Pts',(21.3727615068429,-3.1991047094595,0.392002079868707));
#69516=CARTESIAN_POINT('Ctrl Pts',(21.3829354073375,-3.21650014504525,0.232592244963371));
#69517=CARTESIAN_POINT('Ctrl Pts',(21.3905985113232,-3.22284727235174,0.114984002839084));
#69518=CARTESIAN_POINT('Ctrl Pts',(21.3984065856094,-3.22274887336959,-0.00269475323696564));
#69519=CARTESIAN_POINT('Ctrl Pts',(21.3984063391797,-3.22274887647301,-0.00269103919059044));
#69520=CARTESIAN_POINT('Ctrl Pts',(21.4053592522661,-3.22266137514423,-0.107481341026377));
#69521=CARTESIAN_POINT('Ctrl Pts',(21.4124178111479,-3.21746293090191,-0.212202018047763));
#69522=CARTESIAN_POINT('Ctrl Pts',(21.4333807979378,-3.18702950541372,-0.520610649471097));
#69523=CARTESIAN_POINT('Ctrl Pts',(21.4473461277154,-3.14744181193964,-0.722369300118942));
#69524=CARTESIAN_POINT('Ctrl Pts',(21.4621449334735,-3.08148942459918,-0.944045988770399));
#69525=CARTESIAN_POINT('Ctrl Pts',(21.4638017771352,-3.07373608350206,-0.968992515927787));
#69526=CARTESIAN_POINT('Ctrl Pts',(21.465901937543,-3.06341934535991,-1.000816274256));
#69527=CARTESIAN_POINT('Ctrl Pts',(21.4663607969808,-3.06113489365175,-1.007781953453));
#69528=CARTESIAN_POINT('Ctrl Pts',(21.4670963169926,-3.05742375683328,-1.01896878541024));
#69529=CARTESIAN_POINT('Ctrl Pts',(21.4673738508741,-3.05601206722791,-1.02319482994292));
#69530=CARTESIAN_POINT('Ctrl Pts',(21.4679032413032,-3.05329744066672,-1.03126562080344));
#69531=CARTESIAN_POINT('Ctrl Pts',(21.4681551819514,-3.05199600732065,-1.03511082173638));
#69532=CARTESIAN_POINT('Ctrl Pts',(21.4687357346023,-3.04897514833649,-1.04398099298263));
#69533=CARTESIAN_POINT('Ctrl Pts',(21.4690640394512,-3.04725055335986,-1.04900421109233));
#69534=CARTESIAN_POINT('Ctrl Pts',(21.4699440756777,-3.04258414664137,-1.06248741052325));
#69535=CARTESIAN_POINT('Ctrl Pts',(21.4704944734817,-3.03961944526112,-1.07093950311423));
#69536=CARTESIAN_POINT('Ctrl Pts',(21.4744941835404,-3.01774091469842,-1.13249041130505));
#69537=CARTESIAN_POINT('Ctrl Pts',(21.4778669179693,-2.99747080990373,-1.18510101524148));
#69538=CARTESIAN_POINT('Ctrl Pts',(21.4853849419586,-2.94841071924306,-1.30310910564626));
#69539=CARTESIAN_POINT('Ctrl Pts',(21.4894940635605,-2.91880527371012,-1.36813598206786));
#69540=CARTESIAN_POINT('Ctrl Pts',(21.503106851959,-2.81237145587611,-1.58269839427308));
#69541=CARTESIAN_POINT('Ctrl Pts',(21.5123779091454,-2.72601526013585,-1.72719758130089));
#69542=CARTESIAN_POINT('Ctrl Pts',(21.5285682865577,-2.55959795295014,-1.96185580795392));
#69543=CARTESIAN_POINT('Ctrl Pts',(21.5353785385709,-2.48504409037869,-2.05547375218897));
#69544=CARTESIAN_POINT('Ctrl Pts',(21.5453281150155,-2.37188541426295,-2.1823893349222));
#69545=CARTESIAN_POINT('Ctrl Pts',(21.5483117875878,-2.3374269915095,-2.21925624675754));
#69546=CARTESIAN_POINT('Ctrl Pts',(21.5533295781173,-2.27875291025246,-2.27914842658912));
#69547=CARTESIAN_POINT('Ctrl Pts',(21.5553431669906,-2.25501868789961,-2.30263391933463));
#69548=CARTESIAN_POINT('Ctrl Pts',(21.558071114558,-2.22263794113817,-2.33369449471549));
#69549=CARTESIAN_POINT('Ctrl Pts',(21.5587711233171,-2.21430903133071,-2.34159879579519));
#69550=CARTESIAN_POINT('Ctrl Pts',(21.5598848488642,-2.20102730031208,-2.35406919229624));
#69551=CARTESIAN_POINT('Ctrl Pts',(21.5602973012798,-2.196102045028,-2.35866461065801));
#69552=CARTESIAN_POINT('Ctrl Pts',(21.5611534812305,-2.18586475551129,-2.36815646142));
#69553=CARTESIAN_POINT('Ctrl Pts',(21.5615973059204,-2.18055059632253,-2.37305053689877));
#69554=CARTESIAN_POINT('Ctrl Pts',(21.562610719315,-2.16839997426379,-2.38416537789433));
#69555=CARTESIAN_POINT('Ctrl Pts',(21.5631807902965,-2.16155313789057,-2.39037466242462));
#69556=CARTESIAN_POINT('Ctrl Pts',(21.5646630183904,-2.14372099763495,-2.40640707632165));
#69557=CARTESIAN_POINT('Ctrl Pts',(21.5655770915787,-2.13269495259623,-2.41618438042822));
#69558=CARTESIAN_POINT('Ctrl Pts',(21.5713640473561,-2.06271223297147,-2.47738904126479));
#69559=CARTESIAN_POINT('Ctrl Pts',(21.5763225158118,-2.00197078159039,-2.52672703138993));
#69560=CARTESIAN_POINT('Ctrl Pts',(21.5827236467789,-1.92266092929463,-2.58649125406766));
#69561=CARTESIAN_POINT('Ctrl Pts',(21.584088477052,-1.90569947744807,-2.59901356802136));
#69562=CARTESIAN_POINT('Ctrl Pts',(21.597413646922,-1.7395978438994,-2.71914304562033));
#69563=CARTESIAN_POINT('Ctrl Pts',(21.6097998460538,-1.5816430532419,-2.81395281304634));
#69564=CARTESIAN_POINT('Ctrl Pts',(21.6357801210014,-1.23687823788911,-2.98265540883846));
#69565=CARTESIAN_POINT('Ctrl Pts',(21.6493280160898,-1.04945885391843,-3.05364621893124));
#69566=CARTESIAN_POINT('Ctrl Pts',(21.6629530217962,-0.842154040696891,
-3.11080700940444));
#69567=CARTESIAN_POINT('Ctrl Pts',(21.663900522391,-0.827629739009613,-3.11470266861203));
#69568=CARTESIAN_POINT('Ctrl Pts',(21.6652143998596,-0.807329748057601,
-3.11999543806916));
#69569=CARTESIAN_POINT('Ctrl Pts',(21.6655855777811,-0.801576934557592,
-3.12147837971032));
#69570=CARTESIAN_POINT('Ctrl Pts',(21.6662147252357,-0.791794723459764,
-3.12397117999325));
#69571=CARTESIAN_POINT('Ctrl Pts',(21.6664731638829,-0.787767432375147,
-3.12498916648727));
#69572=CARTESIAN_POINT('Ctrl Pts',(21.6669646767908,-0.78009071428097,-3.12691384275272));
#69573=CARTESIAN_POINT('Ctrl Pts',(21.6671978335483,-0.776441663359776,
-3.12782193327113));
#69574=CARTESIAN_POINT('Ctrl Pts',(21.6677455714612,-0.767851869133542,
-3.129943602204));
#69575=CARTESIAN_POINT('Ctrl Pts',(21.6680598456194,-0.762909807289574,
-3.13115187633723));
#69576=CARTESIAN_POINT('Ctrl Pts',(21.668985398497,-0.748316089810579,-3.13468326030251));
#69577=CARTESIAN_POINT('Ctrl Pts',(21.669594820813,-0.738656431600315,-3.13697350877479));
#69578=CARTESIAN_POINT('Ctrl Pts',(21.6752781307853,-0.648118679711256,
-3.15799809132386));
#69579=CARTESIAN_POINT('Ctrl Pts',(21.6801848949831,-0.566547733442373,
-3.17364712772203));
#69580=CARTESIAN_POINT('Ctrl Pts',(21.6853264511989,-0.478753255741978,
-3.18699641596907));
#69581=CARTESIAN_POINT('Ctrl Pts',(21.6856599324352,-0.473048199826224,
-3.18784821416617));
#69582=CARTESIAN_POINT('Ctrl Pts',(21.692175467515,-0.361382277423468,-3.20421422500349));
#69583=CARTESIAN_POINT('Ctrl Pts',(21.6981945660834,-0.254709649677842,
-3.21445351072554));
#69584=CARTESIAN_POINT('Ctrl Pts',(21.7146124931097,0.0383715430467452,
-3.22790152918358));
#69585=CARTESIAN_POINT('Ctrl Pts',(21.7249462362604,0.224842207452441,-3.22028912312533));
#69586=CARTESIAN_POINT('Ctrl Pts',(21.7397652402321,0.479261986454161,-3.18768834944866));
#69587=CARTESIAN_POINT('Ctrl Pts',(21.7438759175802,0.548602867573561,-3.17648909401384));
#69588=CARTESIAN_POINT('Ctrl Pts',(21.7497509569,0.645480021266316,-3.15757576336131));
#69589=CARTESIAN_POINT('Ctrl Pts',(21.7514575663761,0.67336638113102,-3.1517466267172));
#69590=CARTESIAN_POINT('Ctrl Pts',(21.7540681899878,0.715612245020734,-3.14232964290477));
#69591=CARTESIAN_POINT('Ctrl Pts',(21.7549636882121,0.730030808355567,-3.13901122609289));
#69592=CARTESIAN_POINT('Ctrl Pts',(21.756618990719,0.756545824593602,-3.1327162577687));
#69593=CARTESIAN_POINT('Ctrl Pts',(21.7573778585297,0.768648900581918,-3.12976861720062));
#69594=CARTESIAN_POINT('Ctrl Pts',(21.758616250434,0.78831260068285,-3.12485868719982));
#69595=CARTESIAN_POINT('Ctrl Pts',(21.7590943968964,0.795883792032423,-3.12293892979737));
#69596=CARTESIAN_POINT('Ctrl Pts',(21.7595741792746,0.803459624498735,-3.12098865657142));
#69597=CARTESIAN_POINT('Ctrl Pts',(21.7595749232389,0.803471371750133,-3.12098563236441));
#69598=CARTESIAN_POINT('Ctrl Pts',(21.7595764132522,0.803494899068915,-3.12097957536063));
#69599=CARTESIAN_POINT('Ctrl Pts',(21.7595771592943,0.803506679026253,-3.12097654259178));
#69600=CARTESIAN_POINT('Ctrl Pts',(21.7595786534366,0.803530271336992,-3.12097046857126));
#69601=CARTESIAN_POINT('Ctrl Pts',(21.75957940155,0.803542083896503,-3.12096742726611));
#69602=CARTESIAN_POINT('Ctrl Pts',(21.7595808998809,0.803565742136834,-3.12096133598507));
#69603=CARTESIAN_POINT('Ctrl Pts',(21.7595816500864,0.803577587626535,-3.12095828605798));
#69604=CARTESIAN_POINT('Ctrl Pts',(21.7595831525948,0.803601311620237,-3.12095217755939));
#69605=CARTESIAN_POINT('Ctrl Pts',(21.7595839048972,0.80361319011538,-3.12094911898977));
#69606=CARTESIAN_POINT('Ctrl Pts',(21.7595854116088,0.803636980266337,-3.12094299316724));
#69607=CARTESIAN_POINT('Ctrl Pts',(21.7595861660175,0.803648891915093,-3.12093992591574));
#69608=CARTESIAN_POINT('Ctrl Pts',(21.7595876769495,0.80367274849331,-3.12093378269731));
#69609=CARTESIAN_POINT('Ctrl Pts',(21.7595884334747,0.803684693453638,-3.12093070672203));
#69610=CARTESIAN_POINT('Ctrl Pts',(21.7595899486348,0.803708616578942,-3.12092454607441));
#69611=CARTESIAN_POINT('Ctrl Pts',(21.7595907072781,0.803720594876109,-3.12092146136762));
#69612=CARTESIAN_POINT('Ctrl Pts',(21.7595922267072,0.803744585193873,-3.12091528312215));
#69613=CARTESIAN_POINT('Ctrl Pts',(21.7595929874866,0.803756597111661,-3.12091218960953));
#69614=CARTESIAN_POINT('Ctrl Pts',(21.7595945111751,0.803780654466387,-3.12090599380377));
#69615=CARTESIAN_POINT('Ctrl Pts',(21.7595952740906,0.803792700002387,-3.12090289148471));
#69616=CARTESIAN_POINT('Ctrl Pts',(21.7595968020794,0.803816825039296,-3.12089667795));
#69617=CARTESIAN_POINT('Ctrl Pts',(21.7595975671451,0.803828904417523,-3.12089356676554));
#69618=CARTESIAN_POINT('Ctrl Pts',(21.7595990994428,0.803853097269881,-3.12088733546504));
#69619=CARTESIAN_POINT('Ctrl Pts',(21.7595998666691,0.8038652106532,-3.12088421537198));
#69620=CARTESIAN_POINT('Ctrl Pts',(21.7596014032889,0.803889471526135,-3.12087796625033));
#69621=CARTESIAN_POINT('Ctrl Pts',(21.7596021726829,0.803901619024839,-3.12087483721898));
#69622=CARTESIAN_POINT('Ctrl Pts',(21.7596037136399,0.803925948158126,-3.12086857021187));
#69623=CARTESIAN_POINT('Ctrl Pts',(21.759604485204,0.803938129809925,-3.12086543223125));
#69624=CARTESIAN_POINT('Ctrl Pts',(21.7600495613914,0.810965074730206,-3.11905525477811));
#69625=CARTESIAN_POINT('Ctrl Pts',(21.7604946304961,0.817973679166252,-3.11722458183839));
#69626=CARTESIAN_POINT('Ctrl Pts',(21.7615091164916,0.833907191489558,-3.11300525505727));
#69627=CARTESIAN_POINT('Ctrl Pts',(21.7620790104874,0.84282808917369,-3.11060182782758));
#69628=CARTESIAN_POINT('Ctrl Pts',(21.7638541248432,0.870521361009193,-3.10301295728822));
#69629=CARTESIAN_POINT('Ctrl Pts',(21.7650636241495,0.889256882552385,-3.0976957602508));
#69630=CARTESIAN_POINT('Ctrl Pts',(21.781616872936,1.14382190177504,-3.02294969780754));
#69631=CARTESIAN_POINT('Ctrl Pts',(21.7978824599157,1.37095191580751,-2.92694324401145));
#69632=CARTESIAN_POINT('Ctrl Pts',(21.8249089152736,1.71920285461805,-2.730245959176));
#69633=CARTESIAN_POINT('Ctrl Pts',(21.8354053101026,1.84787082567989,-2.64485876462202));
#69634=CARTESIAN_POINT('Ctrl Pts',(21.8494525463479,2.01581805469811,-2.51514541576639));
#69635=CARTESIAN_POINT('Ctrl Pts',(21.8532459968199,2.06074113995951,-2.47847245072498));
#69636=CARTESIAN_POINT('Ctrl Pts',(21.8589905919686,2.12845425816945,-2.42008012596923));
#69637=CARTESIAN_POINT('Ctrl Pts',(21.860989509979,2.15195517820215,-2.39920704279093));
#69638=CARTESIAN_POINT('Ctrl Pts',(21.8634549156649,2.18091241672148,-2.37271987872689));
#69639=CARTESIAN_POINT('Ctrl Pts',(21.8639441862554,2.18665770758032,-2.36742616890325));
#69640=CARTESIAN_POINT('Ctrl Pts',(21.8647167439107,2.19572825647193,-2.35900737764558));
#69641=CARTESIAN_POINT('Ctrl Pts',(21.8650010648622,2.19906617839444,-2.35589607744367));
#69642=CARTESIAN_POINT('Ctrl Pts',(21.8655356609689,2.20534204267046,-2.35002134139359));
#69643=CARTESIAN_POINT('Ctrl Pts',(21.8657860489154,2.20828137099089,-2.34725951204898));
#69644=CARTESIAN_POINT('Ctrl Pts',(21.8663583636742,2.21499948234717,-2.34092330295013));
#69645=CARTESIAN_POINT('Ctrl Pts',(21.8666800053496,2.21877479469742,-2.33734529507545));
#69646=CARTESIAN_POINT('Ctrl Pts',(21.8676702360857,2.2303961751003,-2.32627773867471));
#69647=CARTESIAN_POINT('Ctrl Pts',(21.8683364979593,2.23821320637653,-2.31875761260266));
#69648=CARTESIAN_POINT('Ctrl Pts',(21.8737626164917,2.30184001445535,-2.2569259064803));
#69649=CARTESIAN_POINT('Ctrl Pts',(21.8783760651636,2.35570753384216,-2.20064223518734));
#69650=CARTESIAN_POINT('Ctrl Pts',(21.8993317313724,2.59564714188433,-1.93102115601129));
#69651=CARTESIAN_POINT('Ctrl Pts',(21.9145711648951,2.75514411314558,-1.69571050814438));
#69652=CARTESIAN_POINT('Ctrl Pts',(21.9356417208119,2.91969047795385,-1.36699253364841));
#69653=CARTESIAN_POINT('Ctrl Pts',(21.9405558977839,2.95453285515125,-1.28995932363136));
#69654=CARTESIAN_POINT('Ctrl Pts',(21.9484970984594,3.00486538604206,-1.16590671629488));
#69655=CARTESIAN_POINT('Ctrl Pts',(21.9514576696479,3.02237072212546,-1.11974518355661));
#69656=CARTESIAN_POINT('Ctrl Pts',(21.9552651919248,3.04325929456467,-1.06059845378057));
#69657=CARTESIAN_POINT('Ctrl Pts',(21.9560790753018,3.04763179827958,-1.04796785629027));
#69658=CARTESIAN_POINT('Ctrl Pts',(21.9573873356767,3.05451168473078,-1.02768708078981));
#69659=CARTESIAN_POINT('Ctrl Pts',(21.9578800475144,3.05706922374543,-1.02005398266347));
#69660=CARTESIAN_POINT('Ctrl Pts',(21.9588160685933,3.06186422872117,-1.00556304778099));
#69661=CARTESIAN_POINT('Ctrl Pts',(21.9592591884258,3.06410732447876,-0.998707114680354));
#69662=CARTESIAN_POINT('Ctrl Pts',(21.9602660262477,3.06914295118856,-0.98313925939995));
#69663=CARTESIAN_POINT('Ctrl Pts',(21.9608302034348,3.07192143254615,-0.974422889562584));
#69664=CARTESIAN_POINT('Ctrl Pts',(21.9622872624879,3.07898582751733,-0.95193065886192));
#69665=CARTESIAN_POINT('Ctrl Pts',(21.9631819543838,3.08321638208288,-0.938137748782555));
#69666=CARTESIAN_POINT('Ctrl Pts',(21.9686358045789,3.10835342098128,-0.854176364949277));
#69667=CARTESIAN_POINT('Ctrl Pts',(21.973269656034,3.12695485529495,-0.783345501650713));
#69668=CARTESIAN_POINT('Ctrl Pts',(21.9788107898022,3.14598981514643,-0.699309339643838));
#69669=CARTESIAN_POINT('Ctrl Pts',(21.9796463348711,3.14877610309654,-0.686654581773746));
#69670=CARTESIAN_POINT('Ctrl Pts',(21.9844468825204,3.1643046451757,-0.614044521965889));
#69671=CARTESIAN_POINT('Ctrl Pts',(21.9884581171415,3.17541007152699,-0.553755111952784));
#69672=CARTESIAN_POINT('Ctrl Pts',(22.008738159895,3.22235970054904,-0.250575547040934));
#69673=CARTESIAN_POINT('Ctrl Pts',(22.0256265048186,3.23208200282656,-0.00449090003082506));
#69674=CARTESIAN_POINT('Ctrl Pts',(22.0463974915761,3.2087950850084,0.306951396204653));
#69675=CARTESIAN_POINT('Ctrl Pts',(22.0507906125347,3.20173862004059,0.373438183203714));
#69676=CARTESIAN_POINT('Ctrl Pts',(22.0573305152761,3.18788454131705,0.47404009468864));
#69677=CARTESIAN_POINT('Ctrl Pts',(22.0595411937401,3.18259499070741,0.508341639117178));
#69678=CARTESIAN_POINT('Ctrl Pts',(22.0622294761317,3.17539364867108,0.550506906079189));
#69679=CARTESIAN_POINT('Ctrl Pts',(22.0627349988943,3.17400527168273,0.558456100608419));
#69680=CARTESIAN_POINT('Ctrl Pts',(22.0635273194852,3.171775043753,0.570948316359138));
#69681=CARTESIAN_POINT('Ctrl Pts',(22.063815241486,3.17095326719509,0.575494818423807));
#69682=CARTESIAN_POINT('Ctrl Pts',(22.0643528966968,3.16939740910222,0.583998133990971));
#69683=CARTESIAN_POINT('Ctrl Pts',(22.0646027585577,3.16866570133185,0.587955296572799));
#69684=CARTESIAN_POINT('Ctrl Pts',(22.0651690466496,3.16698768651334,0.596936083230726));
#69685=CARTESIAN_POINT('Ctrl Pts',(22.0654852099674,3.16603684026713,0.601958819952992));
#69686=CARTESIAN_POINT('Ctrl Pts',(22.0664422487253,3.16311621407032,0.61718833097298));
#69687=CARTESIAN_POINT('Ctrl Pts',(22.0670810173864,3.16110897478543,0.627387978888903));
#69688=CARTESIAN_POINT('Ctrl Pts',(22.0717577584071,3.1459892466723,0.702302766983671));
#69689=CARTESIAN_POINT('Ctrl Pts',(22.0756908313268,3.13093891541834,0.766616229065749));
#69690=CARTESIAN_POINT('Ctrl Pts',(22.0976418193456,3.0341928164051,1.12939327786391));
#69691=CARTESIAN_POINT('Ctrl Pts',(22.1141818005735,2.91182246501187,1.41533914346475));
#69692=CARTESIAN_POINT('Ctrl Pts',(22.1363540959125,2.71122023519462,1.74387391908023));
#69693=CARTESIAN_POINT('Ctrl Pts',(22.140759990471,2.66964965918646,1.80687047149689));
#69694=CARTESIAN_POINT('Ctrl Pts',(22.1479465902253,2.5995608288089,1.90537833147084));
#69695=CARTESIAN_POINT('Ctrl Pts',(22.1506758694124,2.57243360125697,1.94184658013414));
#69696=CARTESIAN_POINT('Ctrl Pts',(22.1542238445099,2.5365761289891,1.98798081951564));
#69697=CARTESIAN_POINT('Ctrl Pts',(22.1550147885536,2.52854515486869,1.99818557421186));
#69698=CARTESIAN_POINT('Ctrl Pts',(22.1562948713178,2.51548891864918,2.01457104900422));
#69699=CARTESIAN_POINT('Ctrl Pts',(22.1567824712413,2.51050197842521,2.02078223118013));
#69700=CARTESIAN_POINT('Ctrl Pts',(22.1577145318688,2.5009436389748,2.03259705184457));
#69701=CARTESIAN_POINT('Ctrl Pts',(22.1581588268218,2.49637629883038,2.03820392350124));
#69702=CARTESIAN_POINT('Ctrl Pts',(22.159176382698,2.4858908683867,2.05098773402139));
#69703=CARTESIAN_POINT('Ctrl Pts',(22.1597501403624,2.479960519063,2.05815449265041));
#69704=CARTESIAN_POINT('Ctrl Pts',(22.1615174043752,2.46163949274802,2.08010108946757));
#69705=CARTESIAN_POINT('Ctrl Pts',(22.1627150658736,2.44914727622373,2.09479524726676));
#69706=CARTESIAN_POINT('Ctrl Pts',(22.173047063414,2.340743409629,2.22001171879596));
#69707=CARTESIAN_POINT('Ctrl Pts',(22.1824897570267,2.23755261410307,2.32397919259026));
#69708=CARTESIAN_POINT('Ctrl Pts',(22.2015996342679,2.02069801692025,2.5145936183195));
#69709=CARTESIAN_POINT('Ctrl Pts',(22.2112252674824,1.90769779717072,2.60135086481549));
#69710=CARTESIAN_POINT('Ctrl Pts',(22.2208495079139,1.78943601979592,2.68030526126353));
#69711=CARTESIAN_POINT('Origin',(-1.72497344927317,0.,0.));
#69712=CARTESIAN_POINT('',(23.7170278226866,1.78943621037803,2.68030513402633));
#69713=CARTESIAN_POINT('',(23.4730037159736,1.78943621026388,2.68030513410254));
#69714=CARTESIAN_POINT('',(-1.72497344927317,1.78943621037804,2.68030513402633));
#69715=CARTESIAN_POINT('',(22.8965734492155,-3.22274864819489,0.00295178895409686));
#69716=CARTESIAN_POINT('Ctrl Pts',(22.8965734492731,-3.22274864819574,0.00295178801954905));
#69717=CARTESIAN_POINT('Ctrl Pts',(22.902681519152,-3.22283934391745,-0.0960693857917812));
#69718=CARTESIAN_POINT('Ctrl Pts',(22.9087895890309,-3.21836201049138,-0.195199612804562));
#69719=CARTESIAN_POINT('Ctrl Pts',(22.9148976589098,-3.20931356634111,-0.293979583302786));
#69720=CARTESIAN_POINT('Ctrl Pts',(22.9209858737207,-3.20029453532421,-0.392438456781707));
#69721=CARTESIAN_POINT('Ctrl Pts',(22.9270740885317,-3.18673409406454,-0.490548902010164));
#69722=CARTESIAN_POINT('Ctrl Pts',(22.9331623033426,-3.16868130723445,-0.58785741101304));
#69723=CARTESIAN_POINT('Ctrl Pts',(22.9392490004555,-3.15063302068541,-0.685141662506981));
#69724=CARTESIAN_POINT('Ctrl Pts',(22.9453356975685,-3.12809469411758,-0.781623938282448));
#69725=CARTESIAN_POINT('Ctrl Pts',(22.9514223946814,-3.10116684275637,-0.876859039919459));
#69726=CARTESIAN_POINT('Ctrl Pts',(22.9575092842943,-3.07423813976596,-0.972097153493533));
#69727=CARTESIAN_POINT('Ctrl Pts',(22.9635961739071,-3.04291975822478,-1.06608758733206));
#69728=CARTESIAN_POINT('Ctrl Pts',(22.96968306352,-3.00736229680926,-1.15839957623875));
#69729=CARTESIAN_POINT('Ctrl Pts',(22.9758067354239,-2.9715899662277,-1.25126939462153));
#69730=CARTESIAN_POINT('Ctrl Pts',(22.9819304073279,-2.93152730548399,-1.34243998677787));
#69731=CARTESIAN_POINT('Ctrl Pts',(22.9880540792318,-2.88737644976506,-1.43149390492664));
#69732=CARTESIAN_POINT('Ctrl Pts',(22.994149852758,-2.84342673761914,-1.52014210900724));
#69733=CARTESIAN_POINT('Ctrl Pts',(23.0002456262843,-2.79542626918373,-1.60669252181169));
#69734=CARTESIAN_POINT('Ctrl Pts',(23.0063413998106,-2.74361941971756,-1.69076019655321));
#69735=CARTESIAN_POINT('Ctrl Pts',(23.0124790209033,-2.69145691553949,-1.77540499700204));
#69736=CARTESIAN_POINT('Ctrl Pts',(23.0186166419961,-2.63543583487292,-1.85753246908233));
#69737=CARTESIAN_POINT('Ctrl Pts',(23.0247542630888,-2.57584755305794,-1.93678262742762));
#69738=CARTESIAN_POINT('Ctrl Pts',(23.0308918841816,-2.51625927124294,-2.01603278577293));
#69739=CARTESIAN_POINT('Ctrl Pts',(23.0370295052743,-2.45310412858725,-2.09240532528391));
#69740=CARTESIAN_POINT('Ctrl Pts',(23.0431671263671,-2.38671080430784,-2.16557823666111));
#69741=CARTESIAN_POINT('Ctrl Pts',(23.0493393744598,-2.31994290466667,-2.23916397221976));
#69742=CARTESIAN_POINT('Ctrl Pts',(23.0555116225526,-2.24965116623211,-2.3097885076005));
#69743=CARTESIAN_POINT('Ctrl Pts',(23.0616838706454,-2.17612863586824,-2.3770952279314));
#69744=CARTESIAN_POINT('Ctrl Pts',(23.067847759298,-2.10270568140966,-2.44431079079567));
#69745=CARTESIAN_POINT('Ctrl Pts',(23.0740116479506,-2.02606094968589,-2.50821717923666));
#69746=CARTESIAN_POINT('Ctrl Pts',(23.0801755366033,-1.94652641395983,-2.56849225855494));
#69747=CARTESIAN_POINT('Ctrl Pts',(23.0863328982618,-1.86707609802975,-2.62870351207937));
#69748=CARTESIAN_POINT('Ctrl Pts',(23.0924902599203,-1.78474240602476,-2.6852908402357));
#69749=CARTESIAN_POINT('Ctrl Pts',(23.0986476215789,-1.69989196613215,-2.73797093957905));
#69750=CARTESIAN_POINT('Ctrl Pts',(23.1048004857252,-1.61510350341615,-2.79061255987827));
#69751=CARTESIAN_POINT('Ctrl Pts',(23.1109533498715,-1.52780231559818,-2.83935239707996));
#69752=CARTESIAN_POINT('Ctrl Pts',(23.1171062140178,-1.43838496538052,-2.88394976618305));
#69753=CARTESIAN_POINT('Ctrl Pts',(23.1232567471543,-1.34900149088508,-2.92853023959327));
#69754=CARTESIAN_POINT('Ctrl Pts',(23.1294072802909,-1.25750383525661,-2.96897116958274));
#69755=CARTESIAN_POINT('Ctrl Pts',(23.1355578134274,-1.16431339250936,-3.00507768394152));
#69756=CARTESIAN_POINT('Ctrl Pts',(23.1417076616426,-1.07113332741884,-3.04118017749087));
#69757=CARTESIAN_POINT('Ctrl Pts',(23.1478575098579,-0.976261255028329,
-3.07294905811508));
#69758=CARTESIAN_POINT('Ctrl Pts',(23.1540073580731,-0.880137848004802,
-3.10023788297116));
#69759=CARTESIAN_POINT('Ctrl Pts',(23.1601581664522,-0.783999433419462,
-3.12753096837873));
#69760=CARTESIAN_POINT('Ctrl Pts',(23.1663089748313,-0.686609714050804,
-3.15034249006538));
#69761=CARTESIAN_POINT('Ctrl Pts',(23.1724597832105,-0.588422812743392,
-3.16857636107182));
#69762=CARTESIAN_POINT('Ctrl Pts',(23.1786171695767,-0.490130905374042,
-3.18682973230654));
#69763=CARTESIAN_POINT('Ctrl Pts',(23.1847745559429,-0.391040541524046,
-3.20049559744429));
#69764=CARTESIAN_POINT('Ctrl Pts',(23.190931942309,-0.29161417207902,-3.20952936380752));
#69765=CARTESIAN_POINT('Ctrl Pts',(23.197092765046,-0.192132313851934,-3.21856817181809));
#69766=CARTESIAN_POINT('Ctrl Pts',(23.203253587783,-0.0923145105519143,
-3.22296971367894));
#69767=CARTESIAN_POINT('Ctrl Pts',(23.2094144105199,0.00737565744893537,
-3.22274155994197));
#69768=CARTESIAN_POINT('Ctrl Pts',(23.2155855334366,0.10723249582668,-3.22251302475846));
#69769=CARTESIAN_POINT('Ctrl Pts',(23.2217566563533,0.206960838603117,-3.2176393541527));
#69770=CARTESIAN_POINT('Ctrl Pts',(23.22792777927,0.306100955347835,-3.20818013328977));
#69771=CARTESIAN_POINT('Ctrl Pts',(23.2326233012156,0.381535296900412,-3.2009827431633));
#69772=CARTESIAN_POINT('Ctrl Pts',(23.2373188231611,0.456629167056301,-3.19113163707705));
#69773=CARTESIAN_POINT('Ctrl Pts',(23.2420143451067,0.531184747029499,-3.17867273040545));
#69774=CARTESIAN_POINT('Ctrl Pts',(23.2481865931995,0.629187810720701,-3.1622955387251));
#69775=CARTESIAN_POINT('Ctrl Pts',(23.2543588412922,0.726605262142597,-3.14135291118325));
#69776=CARTESIAN_POINT('Ctrl Pts',(23.260531089385,0.82297866024604,-3.11589853610153));
#69777=CARTESIAN_POINT('Ctrl Pts',(23.2666949780376,0.919221534164408,-3.09047863538336));
#69778=CARTESIAN_POINT('Ctrl Pts',(23.2728588666903,1.01442274901521,-3.06055924241639));
#69779=CARTESIAN_POINT('Ctrl Pts',(23.2790227553429,1.10813182087535,-3.02624543453823));
#69780=CARTESIAN_POINT('Ctrl Pts',(23.2851801170014,1.20174166340283,-2.99196796184287));
#69781=CARTESIAN_POINT('Ctrl Pts',(23.29133747866,1.29386209857369,-2.95330547393786));
#69782=CARTESIAN_POINT('Ctrl Pts',(23.2974948403185,1.38405656938981,-2.91041319664904));
#69783=CARTESIAN_POINT('Ctrl Pts',(23.3036477044648,1.4741851595969,-2.86755224910057));
#69784=CARTESIAN_POINT('Ctrl Pts',(23.3098005686111,1.56239019127225,-2.82046784072556));
#69785=CARTESIAN_POINT('Ctrl Pts',(23.3159534327574,1.64825477253389,-2.76936342275969));
#69786=CARTESIAN_POINT('Ctrl Pts',(23.322103965894,1.73408682403813,-2.71827836567922));
#69787=CARTESIAN_POINT('Ctrl Pts',(23.3282544990305,1.81757981410254,-2.66317654707034));
#69788=CARTESIAN_POINT('Ctrl Pts',(23.3344050321671,1.89834196242879,-2.60430707793494));
#69789=CARTESIAN_POINT('Ctrl Pts',(23.3405548803823,1.97909511710892,-2.54544416448414));
#69790=CARTESIAN_POINT('Ctrl Pts',(23.3467047285975,2.05711768363793,-2.48281469052846));
#69791=CARTESIAN_POINT('Ctrl Pts',(23.3528545768127,2.13204819676772,-2.4167101706989));
#69792=CARTESIAN_POINT('Ctrl Pts',(23.3590053851918,2.20699040865387,-2.35059533009829));
#69793=CARTESIAN_POINT('Ctrl Pts',(23.3651561935709,2.27883928249741,-2.2810046533681));
#69794=CARTESIAN_POINT('Ctrl Pts',(23.3713070019501,2.34726844021977,-2.20826819749057));
#69795=CARTESIAN_POINT('Ctrl Pts',(23.3774643883162,2.41577077956085,-2.13545395355079));
#69796=CARTESIAN_POINT('Ctrl Pts',(23.3836217746824,2.48084580147416,-2.05948752938292));
#69797=CARTESIAN_POINT('Ctrl Pts',(23.3897791610486,2.54220594227285,-1.98073383107691));
#69798=CARTESIAN_POINT('Ctrl Pts',(23.3959399837856,2.60360032750285,-1.90193618118317));
#69799=CARTESIAN_POINT('Ctrl Pts',(23.4021008065225,2.66127545205123,-1.82034851401034));
#69800=CARTESIAN_POINT('Ctrl Pts',(23.4082616292595,2.71498702167986,-1.73636489097481));
#69801=CARTESIAN_POINT('Ctrl Pts',(23.4144327521762,2.7687883908116,-1.65224085708047));
#69802=CARTESIAN_POINT('Ctrl Pts',(23.4206038750928,2.81861275173148,-1.56571324254608));
#69803=CARTESIAN_POINT('Ctrl Pts',(23.4267749980095,2.8642616470605,-1.47720099501668));
#69804=CARTESIAN_POINT('Ctrl Pts',(23.4314705199551,2.89899525919308,-1.40985325193308));
#69805=CARTESIAN_POINT('Ctrl Pts',(23.4361660419008,2.93131244543431,-1.34135702503197));
#69806=CARTESIAN_POINT('Ctrl Pts',(23.4408615638464,2.96114486756336,-1.27190354815261));
#69807=CARTESIAN_POINT('Ctrl Pts',(23.4470338119391,3.00035948794444,-1.18060718213213));
#69808=CARTESIAN_POINT('Ctrl Pts',(23.4532060600319,3.0354169764317,-1.08733486045608));
#69809=CARTESIAN_POINT('Ctrl Pts',(23.4593783081247,3.06611461235053,-0.99250125764683));
#69810=CARTESIAN_POINT('Ctrl Pts',(23.4655421967773,3.0967706726479,-0.897796093587165));
#69811=CARTESIAN_POINT('Ctrl Pts',(23.4717060854299,3.12307848423293,-0.801534260890484));
#69812=CARTESIAN_POINT('Ctrl Pts',(23.4778699740825,3.14488285782888,-0.704151527040935));
#69813=CARTESIAN_POINT('Ctrl Pts',(23.484027335741,3.16666414258838,-0.606871912595596));
#69814=CARTESIAN_POINT('Ctrl Pts',(23.4901846973996,3.18395137565682,-0.508474178272502));
#69815=CARTESIAN_POINT('Ctrl Pts',(23.4963420590581,3.19663908354375,-0.409409491903414));
#69816=CARTESIAN_POINT('Ctrl Pts',(23.5024949232044,3.20931752396765,-0.31041716520136));
#69817=CARTESIAN_POINT('Ctrl Pts',(23.5086477873508,3.21740306370195,-0.210759284569266));
#69818=CARTESIAN_POINT('Ctrl Pts',(23.5148006514971,3.22084143003047,-0.110896551340821));
#69819=CARTESIAN_POINT('Ctrl Pts',(23.5209511846336,3.22427849373547,-0.0110716510632181));
#69820=CARTESIAN_POINT('Ctrl Pts',(23.5271017177701,3.22307186736618,0.0889575139673457));
#69821=CARTESIAN_POINT('Ctrl Pts',(23.5332522509067,3.21721926569915,0.188726677802104));
#69822=CARTESIAN_POINT('Ctrl Pts',(23.5394020991219,3.21136731577591,0.288484731375786));
#69823=CARTESIAN_POINT('Ctrl Pts',(23.5455519473371,3.20087044460797,0.387982407687484));
#69824=CARTESIAN_POINT('Ctrl Pts',(23.5517017955523,3.18577842894078,0.486758014002484));
#69825=CARTESIAN_POINT('Ctrl Pts',(23.5578526039314,3.1706840569863,0.58554904196229));
#69826=CARTESIAN_POINT('Ctrl Pts',(23.5640034123106,3.15099318114259,0.68361734657127));
#69827=CARTESIAN_POINT('Ctrl Pts',(23.5701542206897,3.12680697231633,0.780509910490545));
#69828=CARTESIAN_POINT('Ctrl Pts',(23.5763116070559,3.1025948975293,0.877506096241446));
#69829=CARTESIAN_POINT('Ctrl Pts',(23.5824689934221,3.07387799500923,0.973323608145693));
#69830=CARTESIAN_POINT('Ctrl Pts',(23.5886263797883,3.04080773838193,1.06752323660731));
#69831=CARTESIAN_POINT('Ctrl Pts',(23.5947872025252,3.00771902560189,1.16177543686332));
#69832=CARTESIAN_POINT('Ctrl Pts',(23.6009480252622,2.97027228308328,1.25440755279031));
#69833=CARTESIAN_POINT('Ctrl Pts',(23.6071088479991,2.92866690640633,1.34500100885479));
#69834=CARTESIAN_POINT('Ctrl Pts',(23.6132799709158,2.88699197037412,1.43574592665084));
#69835=CARTESIAN_POINT('Ctrl Pts',(23.6194510938325,2.8411447118201,1.5244449903503));
#69836=CARTESIAN_POINT('Ctrl Pts',(23.6256222167492,2.79137024530098,1.61070472655554));
#69837=CARTESIAN_POINT('Ctrl Pts',(23.6303177386948,2.75349754319713,1.67633856497353));
#69838=CARTESIAN_POINT('Ctrl Pts',(23.6350132606403,2.71335214004656,1.74056068135109));
#69839=CARTESIAN_POINT('Ctrl Pts',(23.6397087825859,2.6710579522838,1.8032101868727));
#69840=CARTESIAN_POINT('Ctrl Pts',(23.6461520359276,2.61302134425669,1.88917861391627));
#69841=CARTESIAN_POINT('Ctrl Pts',(23.6525952892694,2.55072347699362,1.97250029428709));
#69842=CARTESIAN_POINT('Ctrl Pts',(23.6590385426111,2.4844376228156,2.05272678670065));
#69843=CARTESIAN_POINT('Ctrl Pts',(23.6652014287937,2.42103608431474,2.12946236038559));
#69844=CARTESIAN_POINT('Ctrl Pts',(23.6713643149763,2.35398663560209,2.20336605360624));
#69845=CARTESIAN_POINT('Ctrl Pts',(23.6775272011589,2.28357367016464,2.27407318603223));
#69846=CARTESIAN_POINT('Ctrl Pts',(23.6836843482758,2.21322627540712,2.34471447384112));
#69847=CARTESIAN_POINT('Ctrl Pts',(23.6898414953927,2.1395218913356,2.41216480861059));
#69848=CARTESIAN_POINT('Ctrl Pts',(23.6959986425095,2.0627846731223,2.47609308282862));
#69849=CARTESIAN_POINT('Ctrl Pts',(23.7021510548996,1.98610646434281,2.53997219744256));
#69850=CARTESIAN_POINT('Ctrl Pts',(23.7083034672896,1.90640039290316,2.60033436134496));
#69851=CARTESIAN_POINT('Ctrl Pts',(23.7144558796797,1.82402606814533,2.65688661128515));
#69852=CARTESIAN_POINT('Ctrl Pts',(23.7153131940153,1.81254753175562,2.66476694366744));
#69853=CARTESIAN_POINT('Ctrl Pts',(23.716170508351,1.80101723805182,2.67257336124801));
#69854=CARTESIAN_POINT('Ctrl Pts',(23.7170278226866,1.78943621037803,2.68030513402633));
#69855=CARTESIAN_POINT('Ctrl Pts',(22.4670531482195,1.78943621037803,2.68030513402633));
#69856=CARTESIAN_POINT('Ctrl Pts',(22.4732162780277,1.70663396539659,2.73558590545395));
#69857=CARTESIAN_POINT('Ctrl Pts',(22.479379407836,1.62115245987748,2.7871029884318));
#69858=CARTESIAN_POINT('Ctrl Pts',(22.4855425376442,1.53336940281544,2.83458918311092));
#69859=CARTESIAN_POINT('Ctrl Pts',(22.4916993292816,1.44567662196684,2.88202654292384));
#69860=CARTESIAN_POINT('Ctrl Pts',(22.4978561209189,1.35568737542522,2.92544105046133));
#69861=CARTESIAN_POINT('Ctrl Pts',(22.5040129125562,1.26380761221948,2.96460922918959));
#69862=CARTESIAN_POINT('Ctrl Pts',(22.5101654596615,1.17199119151748,3.00375040512179));
#69863=CARTESIAN_POINT('Ctrl Pts',(22.5163180067668,1.07828724369721,3.03865090225139));
#69864=CARTESIAN_POINT('Ctrl Pts',(22.5224705538721,0.98312472179743,3.06913397294591));
#69865=CARTESIAN_POINT('Ctrl Pts',(22.5286209400674,0.887995623069388,3.09960633731522));
#69866=CARTESIAN_POINT('Ctrl Pts',(22.5347713262628,0.791409381473145,3.12566422577062));
#69867=CARTESIAN_POINT('Ctrl Pts',(22.5409217124581,0.69381240116912,3.14717999397619));
#69868=CARTESIAN_POINT('Ctrl Pts',(22.5470715836672,0.59622359288879,3.1686939606161));
#69869=CARTESIAN_POINT('Ctrl Pts',(22.5532214548764,0.497624638411956,3.18566646979002));
#69870=CARTESIAN_POINT('Ctrl Pts',(22.5593713260855,0.398473501923653,3.19802070518074));
#69871=CARTESIAN_POINT('Ctrl Pts',(22.5655223273652,0.299304145901022,3.21037721072613));
#69872=CARTESIAN_POINT('Ctrl Pts',(22.571673328645,0.199582837374169,3.21811370303971));
#69873=CARTESIAN_POINT('Ctrl Pts',(22.5778243299248,0.0997730440188858,
3.22120519405194));
#69874=CARTESIAN_POINT('Ctrl Pts',(22.5839820025074,-0.000145001850732199,
3.22430003805854));
#69875=CARTESIAN_POINT('Ctrl Pts',(22.5901396750899,-0.100151289225844,
3.22273980851612));
#69876=CARTESIAN_POINT('Ctrl Pts',(22.5962973476725,-0.199782100852666,
3.21655167449225));
#69877=CARTESIAN_POINT('Ctrl Pts',(22.6024586093376,-0.299470983641893,
3.210359933631));
#69878=CARTESIAN_POINT('Ctrl Pts',(22.6086198710027,-0.398783523223655,
3.19953496402935));
#69879=CARTESIAN_POINT('Ctrl Pts',(22.6147811326678,-0.497262953691921,
3.18415563648914));
#69880=CARTESIAN_POINT('Ctrl Pts',(22.6209525032228,-0.59590396108603,3.16875107581697));
#69881=CARTESIAN_POINT('Ctrl Pts',(22.6271238737778,-0.69370870411311,3.14877732116875));
#69882=CARTESIAN_POINT('Ctrl Pts',(22.6332952443328,-0.790232337502041,
3.12436400172356));
#69883=CARTESIAN_POINT('Ctrl Pts',(22.6373543925178,-0.853719650050794,
3.10830642092649));
#69884=CARTESIAN_POINT('Ctrl Pts',(22.6414135407027,-0.91665303363912,3.09032922842104));
#69885=CARTESIAN_POINT('Ctrl Pts',(22.6454726888877,-0.978910542606468,
3.07048069723194));
#69886=CARTESIAN_POINT('Ctrl Pts',(22.6516449369805,-1.07357788990984,3.04029947368625));
#69887=CARTESIAN_POINT('Ctrl Pts',(22.6578171850732,-1.16701475826756,3.00568292964486));
#69888=CARTESIAN_POINT('Ctrl Pts',(22.663989433166,-1.2587750428666,2.9667495603701));
#69889=CARTESIAN_POINT('Ctrl Pts',(22.6701533218186,-1.35041105109282,2.92786892085677));
#69890=CARTESIAN_POINT('Ctrl Pts',(22.6763172104713,-1.44037459246968,2.88468324490364));
#69891=CARTESIAN_POINT('Ctrl Pts',(22.6824810991239,-1.52823476404977,2.83736075754384));
#69892=CARTESIAN_POINT('Ctrl Pts',(22.6886384607824,-1.61600189974735,2.79008838036815));
#69893=CARTESIAN_POINT('Ctrl Pts',(22.694795822441,-1.70166971336131,2.73868810548877));
#69894=CARTESIAN_POINT('Ctrl Pts',(22.7009531840995,-1.78482823578486,2.68337580879852));
#69895=CARTESIAN_POINT('Ctrl Pts',(22.7071060482458,-1.86792601685632,2.62810391378437));
#69896=CARTESIAN_POINT('Ctrl Pts',(22.7132589123921,-1.94851779018614,2.56892591790401));
#69897=CARTESIAN_POINT('Ctrl Pts',(22.7194117765384,-2.02621992593659,2.50610262643762));
#69898=CARTESIAN_POINT('Ctrl Pts',(22.725562309675,-2.10389262426838,2.44330313554652));
#69899=CARTESIAN_POINT('Ctrl Pts',(22.7317128428115,-2.17867752285137,2.37686136594475));
#69900=CARTESIAN_POINT('Ctrl Pts',(22.737863375948,-2.25022235619732,2.3070797364135));
#69901=CARTESIAN_POINT('Ctrl Pts',(22.7440132241632,-2.32175922233442,2.23730587774131));
#69902=CARTESIAN_POINT('Ctrl Pts',(22.7501630723785,-2.39005642962478,2.16419320187664));
#69903=CARTESIAN_POINT('Ctrl Pts',(22.7563129205937,-2.4547977630544,2.0880817764166));
#69904=CARTESIAN_POINT('Ctrl Pts',(22.7624637289728,-2.5195492044234,2.01195846782667));
#69905=CARTESIAN_POINT('Ctrl Pts',(22.7686145373519,-2.58074338775064,1.93283581059582));
#69906=CARTESIAN_POINT('Ctrl Pts',(22.7747653457311,-2.63810432141074,1.85108701898478));
#69907=CARTESIAN_POINT('Ctrl Pts',(22.7809227320972,-2.69552659976824,1.76925080106174));
#69908=CARTESIAN_POINT('Ctrl Pts',(22.7870801184634,-2.74910719225307,1.68478319669865));
#69909=CARTESIAN_POINT('Ctrl Pts',(22.7932375048296,-2.79861349327314,1.59808637994619));
#69910=CARTESIAN_POINT('Ctrl Pts',(22.7993983275666,-2.84814742322464,1.51134117863749));
#69911=CARTESIAN_POINT('Ctrl Pts',(22.8055591503035,-2.89360233581464,1.42236467416699));
#69912=CARTESIAN_POINT('Ctrl Pts',(22.8117199730405,-2.93479260933334,1.33158172963676));
#69913=CARTESIAN_POINT('Ctrl Pts',(22.8178910959571,-2.97605174820308,1.24064700657218));
#69914=CARTESIAN_POINT('Ctrl Pts',(22.8240622188738,-3.01303184513153,1.14790021444844));
#69915=CARTESIAN_POINT('Ctrl Pts',(22.8302333417905,-3.04559619487645,1.05378431391536));
#69916=CARTESIAN_POINT('Ctrl Pts',(22.8349288637362,-3.07037395751986,0.982172828882028));
#69917=CARTESIAN_POINT('Ctrl Pts',(22.8396243856818,-3.09259624749288,0.909769075839418));
#69918=CARTESIAN_POINT('Ctrl Pts',(22.8443199076274,-3.11222268684338,0.836772077687444));
#69919=CARTESIAN_POINT('Ctrl Pts',(22.852243497083,-3.14534186926603,0.71359125742116));
#69920=CARTESIAN_POINT('Ctrl Pts',(22.8601670865385,-3.17116313898967,0.588370950078732));
#69921=CARTESIAN_POINT('Ctrl Pts',(22.868090675994,-3.18948195103085,0.461868429911007));
#69922=CARTESIAN_POINT('Ctrl Pts',(22.8758590689198,-3.20744195901301,0.337843669633462));
#69923=CARTESIAN_POINT('Ctrl Pts',(22.8836274618455,-3.21819054073371,0.212586230235369));
#69924=CARTESIAN_POINT('Ctrl Pts',(22.8913958547713,-3.22158001987508,0.0868316649713684));
#69925=CARTESIAN_POINT('Ctrl Pts',(22.893121719586,-3.22233304342142,0.058893405210885));
#69926=CARTESIAN_POINT('Ctrl Pts',(22.8948475844007,-3.22272302167004,0.0309307026174956));
#69927=CARTESIAN_POINT('Ctrl Pts',(22.8965734492154,-3.22274864819489,0.00295178895407324));
#69928=CARTESIAN_POINT('Ctrl Pts',(22.2208495079139,1.78943601979592,2.68030526126352));
#69929=CARTESIAN_POINT('Ctrl Pts',(22.2274108732164,1.70881056907048,2.73413274417209));
#69930=CARTESIAN_POINT('Ctrl Pts',(22.2339688700644,1.62573948420363,2.78433370019938));
#69931=CARTESIAN_POINT('Ctrl Pts',(22.2449657526838,1.48059623411035,2.86331938725809));
#69932=CARTESIAN_POINT('Ctrl Pts',(22.2494484428537,1.41970581754167,2.89399374300783));
#69933=CARTESIAN_POINT('Ctrl Pts',(22.2561057682776,1.32598625840515,2.93753555360142));
#69934=CARTESIAN_POINT('Ctrl Pts',(22.2583468774917,1.29384594146965,2.95183292413911));
#69935=CARTESIAN_POINT('Ctrl Pts',(22.2610670099127,1.25401890637395,2.96877412793341));
#69936=CARTESIAN_POINT('Ctrl Pts',(22.261574730624,1.24654933655056,2.97191823493393));
#69937=CARTESIAN_POINT('Ctrl Pts',(22.2623697217724,1.23479578628585,2.9768134549211));
#69938=CARTESIAN_POINT('Ctrl Pts',(22.2626581288331,1.23051982166127,2.97858354732088));
#69939=CARTESIAN_POINT('Ctrl Pts',(22.2631962091176,1.22251937160008,2.98187527158602));
#69940=CARTESIAN_POINT('Ctrl Pts',(22.2634460131047,1.21879588973386,2.98339912325581));
#69941=CARTESIAN_POINT('Ctrl Pts',(22.264011549362,1.21034531152132,2.98683909937323));
#69942=CARTESIAN_POINT('Ctrl Pts',(22.264327021526,1.20561652629364,2.9887509717349));
#69943=CARTESIAN_POINT('Ctrl Pts',(22.2652592571518,1.19159962078208,2.99437939932244));
#69944=CARTESIAN_POINT('Ctrl Pts',(22.2658741157098,1.18229860778889,2.99806398389566));
#69945=CARTESIAN_POINT('Ctrl Pts',(22.2701527655441,1.11719659446997,3.0235039861866));
#69946=CARTESIAN_POINT('Ctrl Pts',(22.2737304177496,1.06081165614945,3.0437451102979));
#69947=CARTESIAN_POINT('Ctrl Pts',(22.2781981997703,0.988474739313168,3.06745798001493));
#69948=CARTESIAN_POINT('Ctrl Pts',(22.2791457517092,0.973020097629172,3.07239526681861));
#69949=CARTESIAN_POINT('Ctrl Pts',(22.281697012377,0.93112817349355,3.08543065947846));
#69950=CARTESIAN_POINT('Ctrl Pts',(22.2832927991265,0.904622526772044,3.09330570471412));
#69951=CARTESIAN_POINT('Ctrl Pts',(22.3008608671207,0.609981108372839,3.17673491617553));
#69952=CARTESIAN_POINT('Ctrl Pts',(22.3159093867766,0.333233662088647,3.21755998755489));
#69953=CARTESIAN_POINT('Ctrl Pts',(22.336105817205,-0.0164871055455884,
3.22349355504828));
#69954=CARTESIAN_POINT('Ctrl Pts',(22.340269838053,-0.0876618243376626,
3.22234338610454));
#69955=CARTESIAN_POINT('Ctrl Pts',(22.3470945958057,-0.20221209011489,3.21669434896977));
#69956=CARTESIAN_POINT('Ctrl Pts',(22.3497103120254,-0.245637828466587,
3.21366987160982));
#69957=CARTESIAN_POINT('Ctrl Pts',(22.3531303322343,-0.301723771070749,
3.20862024191851));
#69958=CARTESIAN_POINT('Ctrl Pts',(22.3539093187466,-0.314452991684446,
3.20739776135162));
#69959=CARTESIAN_POINT('Ctrl Pts',(22.3551747183728,-0.335054887804643,
3.20529538928018));
#69960=CARTESIAN_POINT('Ctrl Pts',(22.3556596569679,-0.342932269942511,
3.20446216498833));
#69961=CARTESIAN_POINT('Ctrl Pts',(22.3565897782726,-0.358006565552584,
3.2028114719568));
#69962=CARTESIAN_POINT('Ctrl Pts',(22.3570348078889,-0.365203960426041,
3.20199876511555));
#69963=CARTESIAN_POINT('Ctrl Pts',(22.358048980791,-0.381571263369378,3.20009471915908));
#69964=CARTESIAN_POINT('Ctrl Pts',(22.3586186001243,-0.3907393124357,3.19898821934262));
#69965=CARTESIAN_POINT('Ctrl Pts',(22.360392016489,-0.419204557065618,3.19542853173744));
#69966=CARTESIAN_POINT('Ctrl Pts',(22.3616000806889,-0.43848410980067,3.1928400556282));
#69967=CARTESIAN_POINT('Ctrl Pts',(22.3782104746239,-0.702017099602754,
3.1550261588626));
#69968=CARTESIAN_POINT('Ctrl Pts',(22.3945423426646,-0.941409416115868,
3.09204112996409));
#69969=CARTESIAN_POINT('Ctrl Pts',(22.421592335161,-1.31431522152625,2.94657150086656));
#69970=CARTESIAN_POINT('Ctrl Pts',(22.4320446759238,-1.45323592316047,2.88059308397445));
#69971=CARTESIAN_POINT('Ctrl Pts',(22.4460360715767,-1.63721877248399,2.77650343362528));
#69972=CARTESIAN_POINT('Ctrl Pts',(22.4498165498814,-1.68674116967793,2.74670014527166));
#69973=CARTESIAN_POINT('Ctrl Pts',(22.4555437547966,-1.76185928233883,2.69869461088187));
#69974=CARTESIAN_POINT('Ctrl Pts',(22.4575379283654,-1.78803373429756,2.68142429975549));
#69975=CARTESIAN_POINT('Ctrl Pts',(22.4599983144102,-1.82040522898272,2.65938024726134));
#69976=CARTESIAN_POINT('Ctrl Pts',(22.4604872004205,-1.82684145539995,2.65496305003844));
#69977=CARTESIAN_POINT('Ctrl Pts',(22.4612592901032,-1.8370133857059,2.64792752779077));
#69978=CARTESIAN_POINT('Ctrl Pts',(22.4615435255639,-1.84075963781473,2.64532461677271));
#69979=CARTESIAN_POINT('Ctrl Pts',(22.4620780512621,-1.84780798030369,2.64040517726422));
#69980=CARTESIAN_POINT('Ctrl Pts',(22.4623284539103,-1.85111120961895,2.63809043097738));
#69981=CARTESIAN_POINT('Ctrl Pts',(22.4629009219724,-1.85866602180998,2.6327752011763));
#69982=CARTESIAN_POINT('Ctrl Pts',(22.4632227016896,-1.86291468098162,2.6297706236185));
#69983=CARTESIAN_POINT('Ctrl Pts',(22.4642137769317,-1.87600632211741,2.62046479554595));
#69984=CARTESIAN_POINT('Ctrl Pts',(22.4648807395162,-1.88482486181785,2.61412905447763));
#69985=CARTESIAN_POINT('Ctrl Pts',(22.4703278594223,-1.95689454147366,2.56179580592459));
#69986=CARTESIAN_POINT('Ctrl Pts',(22.4749603422434,-2.01848999116991,2.5135501610744));
#69987=CARTESIAN_POINT('Ctrl Pts',(22.4801507511789,-2.08682664808002,2.45589033218598));
#69988=CARTESIAN_POINT('Ctrl Pts',(22.4807984276688,-2.09534160600894,2.44862948233087));
#69989=CARTESIAN_POINT('Ctrl Pts',(22.4898374609906,-2.2139684370903,2.34640245183753));
#69990=CARTESIAN_POINT('Ctrl Pts',(22.4979306614987,-2.31757441650669,2.24412890790787));
#69991=CARTESIAN_POINT('Ctrl Pts',(22.5196984593772,-2.57563431365835,1.95238284104554));
#69992=CARTESIAN_POINT('Ctrl Pts',(22.533422902302,-2.71602935675514,1.75181437567194));
#69993=CARTESIAN_POINT('Ctrl Pts',(22.5495167272156,-2.84345895973308,1.5170340727136));
#69994=CARTESIAN_POINT('Ctrl Pts',(22.550916017264,-2.85426004808538,1.49661309916348));
#69995=CARTESIAN_POINT('Ctrl Pts',(22.5529328644647,-2.86942569849575,1.46717890685365));
#69996=CARTESIAN_POINT('Ctrl Pts',(22.5535440946468,-2.87396941525613,1.45825840663377));
#69997=CARTESIAN_POINT('Ctrl Pts',(22.5546060694255,-2.88177275009728,1.44276029460733));
#69998=CARTESIAN_POINT('Ctrl Pts',(22.5550561342987,-2.88505161159111,1.43619241327167));
#69999=CARTESIAN_POINT('Ctrl Pts',(22.5559224657763,-2.89130884895211,1.42355065414316));
#70000=CARTESIAN_POINT('Ctrl Pts',(22.5563386112618,-2.89429059964961,1.41747848259027));
#70001=CARTESIAN_POINT('Ctrl Pts',(22.5573202450676,-2.90126772981024,1.40315613915234));
#70002=CARTESIAN_POINT('Ctrl Pts',(22.5578862897191,-2.90524705564717,1.39489825211291));
#70003=CARTESIAN_POINT('Ctrl Pts',(22.5595635752927,-2.91690841232209,1.37043226479771));
#70004=CARTESIAN_POINT('Ctrl Pts',(22.560678276152,-2.9244903270729,1.35417708744585));
#70005=CARTESIAN_POINT('Ctrl Pts',(22.573782995581,-3.01165556281761,1.16315340203976));
#70006=CARTESIAN_POINT('Ctrl Pts',(22.5863179144167,-3.07558605548693,0.981703622427311));
#70007=CARTESIAN_POINT('Ctrl Pts',(22.617176466581,-3.18928353729458,0.535445553183421));
#70008=CARTESIAN_POINT('Ctrl Pts',(22.6357397919378,-3.22279985224095,0.267953609073662));
#70009=CARTESIAN_POINT('Ctrl Pts',(22.6547672674059,-3.22274470320708,-0.0288013055865189));
#70010=CARTESIAN_POINT('Ctrl Pts',(22.6565588762784,-3.22236926176266,-0.0570035763551874));
#70011=CARTESIAN_POINT('Ctrl Pts',(22.6588257315519,-3.22141542651251,-0.0930711313139109));
#70012=CARTESIAN_POINT('Ctrl Pts',(22.6593190022196,-3.22117836607331,-0.100943165610303));
#70013=CARTESIAN_POINT('Ctrl Pts',(22.6600964265175,-3.22075790366327,-0.113388882755708));
#70014=CARTESIAN_POINT('Ctrl Pts',(22.6603816359655,-3.22059361246074,-0.117963116023465));
#70015=CARTESIAN_POINT('Ctrl Pts',(22.6608918675772,-3.22028166114351,-0.126161570237166));
#70016=CARTESIAN_POINT('Ctrl Pts',(22.6611170897166,-3.22013762918286,-0.129785855167971));
#70017=CARTESIAN_POINT('Ctrl Pts',(22.6616501889978,-3.21978167422509,-0.138377197414176));
#70018=CARTESIAN_POINT('Ctrl Pts',(22.6619577604787,-3.21956437663612,-0.143344005546633));
#70019=CARTESIAN_POINT('Ctrl Pts',(22.6628639424556,-3.21888890482661,-0.158006304684478));
#70020=CARTESIAN_POINT('Ctrl Pts',(22.6634607625235,-3.21839841690283,-0.167700356792422));
#70021=CARTESIAN_POINT('Ctrl Pts',(22.6682125972535,-3.21412793969047,-0.245166086537417));
#70022=CARTESIAN_POINT('Ctrl Pts',(22.6722556617736,-3.20825120077412,-0.312810801882906));
#70023=CARTESIAN_POINT('Ctrl Pts',(22.6826228344595,-3.18732150853722,-0.488969930785459));
#70024=CARTESIAN_POINT('Ctrl Pts',(22.6888199653084,-3.16886602173882,-0.59699366117581));
#70025=CARTESIAN_POINT('Ctrl Pts',(22.7112943666572,-3.08139137487716,-0.987834565998656));
#70026=CARTESIAN_POINT('Ctrl Pts',(22.7272950901874,-2.9796848865569,-1.26184488157661));
#70027=CARTESIAN_POINT('Ctrl Pts',(22.745558489706,-2.83601185343854,-1.53080023909181));
#70028=CARTESIAN_POINT('Ctrl Pts',(22.7463976695727,-2.82935160326635,-1.54307553306671));
#70029=CARTESIAN_POINT('Ctrl Pts',(22.7485538739142,-2.81209144323197,-1.57439972315977));
#70030=CARTESIAN_POINT('Ctrl Pts',(22.7498748308684,-2.80137778860837,-1.59338483201151));
#70031=CARTESIAN_POINT('Ctrl Pts',(22.7517477766602,-2.78599616871477,-1.62000709089727));
#70032=CARTESIAN_POINT('Ctrl Pts',(22.7522940013489,-2.78148757318117,-1.62773600572995));
#70033=CARTESIAN_POINT('Ctrl Pts',(22.7532519218091,-2.77354150839616,-1.64122822746724));
#70034=CARTESIAN_POINT('Ctrl Pts',(22.7536631040142,-2.77011810150769,-1.64699978629364));
#70035=CARTESIAN_POINT('Ctrl Pts',(22.7545283605002,-2.76288792068777,-1.65910291435515));
#70036=CARTESIAN_POINT('Ctrl Pts',(22.7549825718224,-2.75907735528893,-1.66543216276936));
#70037=CARTESIAN_POINT('Ctrl Pts',(22.7560700868546,-2.74991790926392,-1.68052804771357));
#70038=CARTESIAN_POINT('Ctrl Pts',(22.7567041300957,-2.74454884692482,-1.68928228836126));
#70039=CARTESIAN_POINT('Ctrl Pts',(22.7588624679506,-2.72617500100832,-1.71892197376686));
#70040=CARTESIAN_POINT('Ctrl Pts',(22.7603940352187,-2.71297317988454,-1.73968369513315));
#70041=CARTESIAN_POINT('Ctrl Pts',(22.7686662402932,-2.64081009093741,-1.85035103100832));
#70042=CARTESIAN_POINT('Ctrl Pts',(22.7755652197611,-2.5776213611351,-1.93740565283392));
#70043=CARTESIAN_POINT('Ctrl Pts',(22.804303227976,-2.30250009082873,-2.27910078241128));
#70044=CARTESIAN_POINT('Ctrl Pts',(22.8274329197411,-2.05631105555062,-2.50346697543796));
#70045=CARTESIAN_POINT('Ctrl Pts',(22.8515441409584,-1.74579779287944,-2.70924718092675));
#70046=CARTESIAN_POINT('Ctrl Pts',(22.854190239538,-1.71086196003921,-2.73144320188437));
#70047=CARTESIAN_POINT('Ctrl Pts',(22.8573063110413,-1.66856258767506,-2.75718743093195));
#70048=CARTESIAN_POINT('Ctrl Pts',(22.8578162233416,-1.661602775722,-2.7613873066547));
#70049=CARTESIAN_POINT('Ctrl Pts',(22.8586445390974,-1.65023368643544,-2.76818939988169));
#70050=CARTESIAN_POINT('Ctrl Pts',(22.8589639573471,-1.64583401955077,-2.7708074914037));
#70051=CARTESIAN_POINT('Ctrl Pts',(22.8595332643613,-1.63796432200819,-2.7754651218513));
#70052=CARTESIAN_POINT('Ctrl Pts',(22.8597834123217,-1.63449670335813,-2.77750864807322));
#70053=CARTESIAN_POINT('Ctrl Pts',(22.8603194511805,-1.62704495357722,-2.78188130209477));
#70054=CARTESIAN_POINT('Ctrl Pts',(22.8606052067855,-1.62305965982871,-2.7842083616673));
#70055=CARTESIAN_POINT('Ctrl Pts',(22.8613876415603,-1.61211261705881,-2.7905689755301));
#70056=CARTESIAN_POINT('Ctrl Pts',(22.8618831956893,-1.60514068245339,-2.79458506581228));
#70057=CARTESIAN_POINT('Ctrl Pts',(22.8644882217917,-1.5682917462653,-2.81562801170943));
#70058=CARTESIAN_POINT('Ctrl Pts',(22.8665697052954,-1.53815733805271,-2.83220273474807));
#70059=CARTESIAN_POINT('Ctrl Pts',(22.8725717656503,-1.44946438257588,-2.87915291865768));
#70060=CARTESIAN_POINT('Ctrl Pts',(22.8764251648675,-1.39022910708218,-2.90821813289801));
#70061=CARTESIAN_POINT('Ctrl Pts',(22.8946346910125,-1.1020242299297,-3.03881249389938));
#70062=CARTESIAN_POINT('Ctrl Pts',(22.9082294073425,-0.862630799188419,
-3.11524017516068));
#70063=CARTESIAN_POINT('Ctrl Pts',(22.9226971690508,-0.613682589113914,
-3.16378274612327));
#70064=CARTESIAN_POINT('Ctrl Pts',(22.9228778414336,-0.610574408103934,
-3.16438405965394));
#70065=CARTESIAN_POINT('Ctrl Pts',(22.9233720341204,-0.602074554745427,
-3.16601546494393));
#70066=CARTESIAN_POINT('Ctrl Pts',(22.9236857387533,-0.596681139529607,
-3.16703636087621));
#70067=CARTESIAN_POINT('Ctrl Pts',(22.9265559817898,-0.547355710390877,
-3.1762424827151));
#70068=CARTESIAN_POINT('Ctrl Pts',(22.9291310329197,-0.503261764607915,
-3.18352665465697));
#70069=CARTESIAN_POINT('Ctrl Pts',(22.9321315502969,-0.452196011776676,
-3.19087511895151));
#70070=CARTESIAN_POINT('Ctrl Pts',(22.9325337640886,-0.445357133807378,
-3.19183681918605));
#70071=CARTESIAN_POINT('Ctrl Pts',(22.9377450543764,-0.356836538386813,
-3.20399477342219));
#70072=CARTESIAN_POINT('Ctrl Pts',(22.9426345742314,-0.274763415539632,
-3.21207380580703));
#70073=CARTESIAN_POINT('Ctrl Pts',(22.9485317719995,-0.177513123613066,
-3.21789237449484));
#70074=CARTESIAN_POINT('Ctrl Pts',(22.9494422995084,-0.162544675375431,
-3.21868318720646));
#70075=CARTESIAN_POINT('Ctrl Pts',(22.9509242792237,-0.138261361757858,
-3.21979630072893));
#70076=CARTESIAN_POINT('Ctrl Pts',(22.951493718465,-0.128949545598851,-3.22018267092986));
#70077=CARTESIAN_POINT('Ctrl Pts',(22.9525074106491,-0.112407276173173,
-3.22079718347781));
#70078=CARTESIAN_POINT('Ctrl Pts',(22.9529511562706,-0.105177455071535,
-3.2210413835318));
#70079=CARTESIAN_POINT('Ctrl Pts',(22.953884576831,-0.0899942067671539,
-3.22150305127324));
#70080=CARTESIAN_POINT('Ctrl Pts',(22.954374409147,-0.0820406834009596,
-3.22171541124716));
#70081=CARTESIAN_POINT('Ctrl Pts',(22.9556636546671,-0.0611447951435151,
-3.22219590545264));
#70082=CARTESIAN_POINT('Ctrl Pts',(22.9564645855179,-0.0482015576009701,
-3.22241551341154));
#70083=CARTESIAN_POINT('Ctrl Pts',(22.9600636699525,0.00978611332053737,
-3.22304994753245));
#70084=CARTESIAN_POINT('Ctrl Pts',(22.9628888477855,0.0548331444038588,
-3.22259828815631));
#70085=CARTESIAN_POINT('Ctrl Pts',(22.9704676618632,0.174370785408352,-3.21889273780565));
#70086=CARTESIAN_POINT('Ctrl Pts',(22.9752703049022,0.248779607193562,-3.2139979642511));
#70087=CARTESIAN_POINT('Ctrl Pts',(23.000026008594,0.625688575460499,-3.17603736397249));
#70088=CARTESIAN_POINT('Ctrl Pts',(23.0211242650034,0.922530263247596,-3.10283665511042));
#70089=CARTESIAN_POINT('Ctrl Pts',(23.0418864685821,1.21496437798842,-2.98497940361677));
#70090=CARTESIAN_POINT('Ctrl Pts',(23.0426147468595,1.22522613262556,-2.98078201303053));
#70091=CARTESIAN_POINT('Ctrl Pts',(23.0473901272484,1.29255214043378,-2.95283707209882));
#70092=CARTESIAN_POINT('Ctrl Pts',(23.0513774555037,1.34894934549943,-2.92750314784193));
#70093=CARTESIAN_POINT('Ctrl Pts',(23.055909009433,1.41366358303851,-2.896165488535));
#70094=CARTESIAN_POINT('Ctrl Pts',(23.0565421223481,1.42271951352171,-2.89172759007916));
#70095=CARTESIAN_POINT('Ctrl Pts',(23.0574926182821,1.43633968614678,-2.88497349401228));
#70096=CARTESIAN_POINT('Ctrl Pts',(23.0578119238001,1.44091938340558,-2.88268886398526));
#70097=CARTESIAN_POINT('Ctrl Pts',(23.0583811075739,1.44909089090398,-2.87858808295975));
#70098=CARTESIAN_POINT('Ctrl Pts',(23.0586312445717,1.45268474745262,-2.87677610991916));
#70099=CARTESIAN_POINT('Ctrl Pts',(23.0591673460186,1.4603932098794,-2.87287148050487));
#70100=CARTESIAN_POINT('Ctrl Pts',(23.0594531748458,1.4645067019542,-2.87077672268807));
#70101=CARTESIAN_POINT('Ctrl Pts',(23.0602360151932,1.47578234496753,-2.86500416311647));
#70102=CARTESIAN_POINT('Ctrl Pts',(23.0607318997247,1.48293529631653,-2.8613083186882));
#70103=CARTESIAN_POINT('Ctrl Pts',(23.0633416538298,1.52062981892973,-2.84165268967512));
#70104=CARTESIAN_POINT('Ctrl Pts',(23.0654274141257,1.5509291765247,-2.82522989707241));
#70105=CARTESIAN_POINT('Ctrl Pts',(23.0714453937451,1.63861449590422,-2.77586697823814));
#70106=CARTESIAN_POINT('Ctrl Pts',(23.0753100095356,1.69525905951608,-2.74164053634942));
#70107=CARTESIAN_POINT('Ctrl Pts',(23.0934545149861,1.95999245884838,-2.57033548781493));
#70108=CARTESIAN_POINT('Ctrl Pts',(23.1069830968265,2.15277646690291,-2.41117454206961));
#70109=CARTESIAN_POINT('Ctrl Pts',(23.1213476503981,2.32719314316601,-2.22941630567756));
#70110=CARTESIAN_POINT('Ctrl Pts',(23.1215031211226,2.32907758890771,-2.22744754696215));
#70111=CARTESIAN_POINT('Ctrl Pts',(23.1217424098329,2.33197287143755,-2.22441503383245));
#70112=CARTESIAN_POINT('Ctrl Pts',(23.1218261796772,2.33298548459705,-2.223352973442));
#70113=CARTESIAN_POINT('Ctrl Pts',(23.1222126583756,2.33765279818632,-2.2184510495001));
#70114=CARTESIAN_POINT('Ctrl Pts',(23.1225156054466,2.34129873660336,-2.21460287400643));
#70115=CARTESIAN_POINT('Ctrl Pts',(23.1253983026039,2.37587058679394,-2.17793255697847));
#70116=CARTESIAN_POINT('Ctrl Pts',(23.1279969107504,2.40611295690471,-2.14447464019431));
#70117=CARTESIAN_POINT('Ctrl Pts',(23.1309360622594,2.43920321932192,-2.10628459226064));
#70118=CARTESIAN_POINT('Ctrl Pts',(23.1312526780715,2.44275349825157,-2.10216613880255));
#70119=CARTESIAN_POINT('Ctrl Pts',(23.1317831101976,2.4486772012971,-2.09525915706361));
#70120=CARTESIAN_POINT('Ctrl Pts',(23.1319967323168,2.45105633188894,-2.09247552654274));
#70121=CARTESIAN_POINT('Ctrl Pts',(23.1368955426035,2.50546439023643,-2.02859689472836));
#70122=CARTESIAN_POINT('Ctrl Pts',(23.1416579449151,2.55519446275298,-1.96558815729063));
#70123=CARTESIAN_POINT('Ctrl Pts',(23.1474149539825,2.61128333717158,-1.88879266322114));
#70124=CARTESIAN_POINT('Ctrl Pts',(23.14831772023,2.61996480060724,-1.87673195308155));
#70125=CARTESIAN_POINT('Ctrl Pts',(23.1497895262613,2.63393204586875,-1.85704218366912));
#70126=CARTESIAN_POINT('Ctrl Pts',(23.1503565985699,2.63926889459873,-1.84944948385854));
#70127=CARTESIAN_POINT('Ctrl Pts',(23.1513676265266,2.64870429754152,-1.83590178541724));
#70128=CARTESIAN_POINT('Ctrl Pts',(23.1518110844487,2.65281576760036,-1.82995582551362));
#70129=CARTESIAN_POINT('Ctrl Pts',(23.1527454845022,2.66142182386746,-1.81741989281754));
#70130=CARTESIAN_POINT('Ctrl Pts',(23.1532365897923,2.66591201295986,-1.81082697370432));
#70131=CARTESIAN_POINT('Ctrl Pts',(23.1545327889721,2.67767603565589,-1.79341533499788));
#70132=CARTESIAN_POINT('Ctrl Pts',(23.1553394304044,2.68490872422207,-1.78256911515401));
#70133=CARTESIAN_POINT('Ctrl Pts',(23.1590007257693,2.71733716558785,-1.73329394443886));
#70134=CARTESIAN_POINT('Ctrl Pts',(23.1618835639994,2.74177400916559,-1.69437425023957));
#70135=CARTESIAN_POINT('Ctrl Pts',(23.1696533712203,2.80470551953948,-1.58921748167914));
#70136=CARTESIAN_POINT('Ctrl Pts',(23.1745924409433,2.8416828260965,-1.52211117706372));
#70137=CARTESIAN_POINT('Ctrl Pts',(23.2002992224889,3.0189254550657,-1.17143944820518));
#70138=CARTESIAN_POINT('Ctrl Pts',(23.2223046391506,3.1192542758292,-0.86970707193378));
#70139=CARTESIAN_POINT('Ctrl Pts',(23.2467766124118,3.18409092564452,-0.50105169839304));
#70140=CARTESIAN_POINT('Ctrl Pts',(23.2505159017358,3.19260072951787,-0.443609539480715));
#70141=CARTESIAN_POINT('Ctrl Pts',(23.2547988401157,3.20074130740883,-0.376126112401251));
#70142=CARTESIAN_POINT('Ctrl Pts',(23.2554208851005,3.20188277840435,-0.366281925311921));
#70143=CARTESIAN_POINT('Ctrl Pts',(23.2563580268791,3.20354072283646,-0.351383280397276));
#70144=CARTESIAN_POINT('Ctrl Pts',(23.2566749680653,3.20409066992438,-0.346332719164976));
#70145=CARTESIAN_POINT('Ctrl Pts',(23.2572415784886,3.2050545451561,-0.337281926182064));
#70146=CARTESIAN_POINT('Ctrl Pts',(23.2574914969327,3.20547292916926,-0.333282216927065));
#70147=CARTESIAN_POINT('Ctrl Pts',(23.2580289636593,3.20635811414663,-0.324664062596542));
#70148=CARTESIAN_POINT('Ctrl Pts',(23.2583163692893,3.20682242232495,-0.320045406178988));
#70149=CARTESIAN_POINT('Ctrl Pts',(23.2591079549104,3.20807618857256,-0.307296999875901));
#70150=CARTESIAN_POINT('Ctrl Pts',(23.2596109655516,3.20884472814982,-0.299165158145801));
#70151=CARTESIAN_POINT('Ctrl Pts',(23.2623251485984,3.21283802509867,-0.255125716406094));
#70152=CARTESIAN_POINT('Ctrl Pts',(23.2645054727785,3.21549114786066,-0.219167157834597));
#70153=CARTESIAN_POINT('Ctrl Pts',(23.2708796541556,3.22155646974443,-0.112624439867952));
#70154=CARTESIAN_POINT('Ctrl Pts',(23.2749959926902,3.22325161967196,-0.0419609880924475));
#70155=CARTESIAN_POINT('Ctrl Pts',(23.2868345377996,3.22141387676489,0.164352304784546));
#70156=CARTESIAN_POINT('Ctrl Pts',(23.2943837828787,3.21164228892319,0.299793938416747));
#70157=CARTESIAN_POINT('Ctrl Pts',(23.3157394214375,3.16016145118908,0.678395216161542));
#70158=CARTESIAN_POINT('Ctrl Pts',(23.3296159701596,3.09907215242517,0.917915604427136));
#70159=CARTESIAN_POINT('Ctrl Pts',(23.3456731400326,3.00436458876187,1.16631470638774));
#70160=CARTESIAN_POINT('Ctrl Pts',(23.346854426868,2.99726432717949,1.18444210657066));
#70161=CARTESIAN_POINT('Ctrl Pts',(23.3486043934329,2.98655353503294,1.21107426658455));
#70162=CARTESIAN_POINT('Ctrl Pts',(23.3491687852462,2.98306988589865,1.21962984132303));
#70163=CARTESIAN_POINT('Ctrl Pts',(23.3501779681718,2.97678904350251,1.23486720845194));
#70164=CARTESIAN_POINT('Ctrl Pts',(23.350622276325,2.97400600503284,1.24155479649283));
#70165=CARTESIAN_POINT('Ctrl Pts',(23.3515539856964,2.96813296359725,1.2555345461036));
#70166=CARTESIAN_POINT('Ctrl Pts',(23.3520415337854,2.96503858245989,1.26282480526295));
#70167=CARTESIAN_POINT('Ctrl Pts',(23.3533182972775,2.95688035032302,1.28185003348522));
#70168=CARTESIAN_POINT('Ctrl Pts',(23.3541089772319,2.95177354527153,1.29356632777188));
#70169=CARTESIAN_POINT('Ctrl Pts',(23.3575990587936,2.92899428944222,1.34499034597902));
#70170=CARTESIAN_POINT('Ctrl Pts',(23.3603235149241,2.91058999464136,1.3843670623726));
#70171=CARTESIAN_POINT('Ctrl Pts',(23.3675722184112,2.8600270086233,1.48708022067686));
#70172=CARTESIAN_POINT('Ctrl Pts',(23.3721403766003,2.82656244679744,1.54974371134979));
#70173=CARTESIAN_POINT('Ctrl Pts',(23.3948230457243,2.65267870303235,1.85095108828039));
#70174=CARTESIAN_POINT('Ctrl Pts',(23.413879664383,2.48400080679834,2.07181749617703));
#70175=CARTESIAN_POINT('Ctrl Pts',(23.4340191851042,2.2714106132874,2.28636228363493));
#70176=CARTESIAN_POINT('Ctrl Pts',(23.4357006804356,2.25337705599289,2.30413770461221));
#70177=CARTESIAN_POINT('Ctrl Pts',(23.4426113934844,2.1780166587465,2.3766883213659));
#70178=CARTESIAN_POINT('Ctrl Pts',(23.4477622470021,2.11888229736856,2.42955636580153));
#70179=CARTESIAN_POINT('Ctrl Pts',(23.4534514783769,2.04946758375718,2.48715075839427));
#70180=CARTESIAN_POINT('Ctrl Pts',(23.454135858154,2.04104724614253,2.49406543997786));
#70181=CARTESIAN_POINT('Ctrl Pts',(23.4551430796862,2.0285480606304,2.50422392804598));
#70182=CARTESIAN_POINT('Ctrl Pts',(23.4554682491299,2.02449626030841,2.50750066978949));
#70183=CARTESIAN_POINT('Ctrl Pts',(23.4560439036238,2.01729343453775,2.51329684625786));
#70184=CARTESIAN_POINT('Ctrl Pts',(23.4562946710023,2.01414561389936,2.51582020127053));
#70185=CARTESIAN_POINT('Ctrl Pts',(23.4568277961067,2.00743175951343,2.5211814815893));
#70186=CARTESIAN_POINT('Ctrl Pts',(23.4571100345536,2.00386445400851,2.52401774613138));
#70187=CARTESIAN_POINT('Ctrl Pts',(23.4578730362004,1.9941859016861,2.53167943930872));
#70188=CARTESIAN_POINT('Ctrl Pts',(23.4583527659639,1.98806311543579,2.53649034019516));
#70189=CARTESIAN_POINT('Ctrl Pts',(23.4607049111446,1.95786195695651,2.5600439781479));
#70190=CARTESIAN_POINT('Ctrl Pts',(23.4625554945712,1.93353471215768,2.57846704250105));
#70191=CARTESIAN_POINT('Ctrl Pts',(23.4673050996564,1.86974974284247,2.6253610231911));
#70192=CARTESIAN_POINT('Ctrl Pts',(23.4701728763249,1.82990213530993,2.65328910871129));
#70193=CARTESIAN_POINT('Ctrl Pts',(23.4730037159736,1.78943621026388,2.68030513410254));
#70194=CARTESIAN_POINT('Origin',(-1.72497344927317,0.,0.));
#70195=CARTESIAN_POINT('',(24.9668672316986,1.78943621037801,2.68030513402634));
#70196=CARTESIAN_POINT('',(24.7182540045911,1.78943620997144,2.68030513429778));
#70197=CARTESIAN_POINT('',(-1.72497344927317,1.78943621037804,2.68030513402633));
#70198=CARTESIAN_POINT('',(24.1465734493135,-3.22274988426607,-0.000863691533537469));
#70199=CARTESIAN_POINT('Ctrl Pts',(24.1465734493135,-3.22274988426607,-0.000863691533536827));
#70200=CARTESIAN_POINT('Ctrl Pts',(24.1531637169248,-3.22272112126392,-0.108189001818177));
#70201=CARTESIAN_POINT('Ctrl Pts',(24.159753984536,-3.21732684989644,-0.215366678563568));
#70202=CARTESIAN_POINT('Ctrl Pts',(24.1663442521473,-3.20663641291505,-0.321870281118511));
#70203=CARTESIAN_POINT('Ctrl Pts',(24.1729596534758,-3.19590520514317,-0.428780063147113));
#70204=CARTESIAN_POINT('Ctrl Pts',(24.1795750548042,-3.17983745155393,-0.535010296933113));
#70205=CARTESIAN_POINT('Ctrl Pts',(24.1861904561327,-3.15855403786441,-0.640042148917126));
#70206=CARTESIAN_POINT('Ctrl Pts',(24.1928189663141,-3.13722844969058,-0.745282128425083));
#70207=CARTESIAN_POINT('Ctrl Pts',(24.1994474764955,-3.11066664840652,-0.849318665726976));
#70208=CARTESIAN_POINT('Ctrl Pts',(24.2060759866769,-3.07903932648084,-0.951648248295786));
#70209=CARTESIAN_POINT('Ctrl Pts',(24.2127248996135,-3.04731465470002,-1.05429280442014));
#70210=CARTESIAN_POINT('Ctrl Pts',(24.2193738125501,-3.01049338766873,-1.15521958537512));
#70211=CARTESIAN_POINT('Ctrl Pts',(24.2260227254866,-2.96879493299132,-1.25394346297792));
#70212=CARTESIAN_POINT('Ctrl Pts',(24.2294319632594,-2.94741400228757,-1.30456424502275));
#70213=CARTESIAN_POINT('Ctrl Pts',(24.2328412010322,-2.92475153766232,-1.35460625311269));
#70214=CARTESIAN_POINT('Ctrl Pts',(24.2362504388049,-2.90084168137317,-1.40400680272856));
#70215=CARTESIAN_POINT('Ctrl Pts',(24.2424226868977,-2.85755412717028,-1.4934439345661));
#70216=CARTESIAN_POINT('Ctrl Pts',(24.2485949349905,-2.8100502931654,-1.58103468319132));
#70217=CARTESIAN_POINT('Ctrl Pts',(24.2547671830832,-2.75851067542112,-1.66635422887444));
#70218=CARTESIAN_POINT('Ctrl Pts',(24.2609310717359,-2.70704086082516,-1.75155822125774));
#70219=CARTESIAN_POINT('Ctrl Pts',(24.2670949603885,-2.65154634918866,-1.83449675610624));
#70220=CARTESIAN_POINT('Ctrl Pts',(24.2732588490411,-2.59225471131267,-1.91476710703345));
#70221=CARTESIAN_POINT('Ctrl Pts',(24.2794162106997,-2.53302585785589,-1.99495245900393));
#70222=CARTESIAN_POINT('Ctrl Pts',(24.2855735723582,-2.47000812856508,-2.07247489667289));
#70223=CARTESIAN_POINT('Ctrl Pts',(24.2917309340168,-2.40347329903488,-2.14695916666489));
#70224=CARTESIAN_POINT('Ctrl Pts',(24.2978837981631,-2.33698706843832,-2.22138903122562));
#70225=CARTESIAN_POINT('Ctrl Pts',(24.3040366623094,-2.26698913369767,-2.29278481721412));
#70226=CARTESIAN_POINT('Ctrl Pts',(24.3101895264557,-2.19379201543417,-2.36080370965425));
#70227=CARTESIAN_POINT('Ctrl Pts',(24.3163400595923,-2.12062262786547,-2.42879683316808));
#70228=CARTESIAN_POINT('Ctrl Pts',(24.3224905927288,-2.04425678287511,-2.49341530980454));
#70229=CARTESIAN_POINT('Ctrl Pts',(24.3286411258654,-1.96504375180514,-2.55435326765731));
#70230=CARTESIAN_POINT('Ctrl Pts',(24.3347909740806,-1.88583954187208,-2.61528443947927));
#70231=CARTESIAN_POINT('Ctrl Pts',(24.3409408222958,-1.80378912051081,-2.67253564252502));
#70232=CARTESIAN_POINT('Ctrl Pts',(24.347090670511,-1.71927392123948,-2.72584202518155));
#70233=CARTESIAN_POINT('Ctrl Pts',(24.3532414788901,-1.63474552677318,-2.77915673046072));
#70234=CARTESIAN_POINT('Ctrl Pts',(24.3593922872693,-1.54775195747746,-2.82852516026726));
#70235=CARTESIAN_POINT('Ctrl Pts',(24.3655430956484,-1.45870176115706,-2.87372697633183));
#70236=CARTESIAN_POINT('Ctrl Pts',(24.3717004820146,-1.36955633003137,-2.91897713351556));
#70237=CARTESIAN_POINT('Ctrl Pts',(24.3778578683808,-1.27835026787136,-2.96005158181559));
#70238=CARTESIAN_POINT('Ctrl Pts',(24.384015254747,-1.18551464409404,-2.99677703393806));
#70239=CARTESIAN_POINT('Ctrl Pts',(24.3901760774839,-1.09262720975868,-3.03352298213834));
#70240=CARTESIAN_POINT('Ctrl Pts',(24.3963369002209,-0.9981088135955,-3.06591495974254));
#70241=CARTESIAN_POINT('Ctrl Pts',(24.4024977229579,-0.902406329458462,
-3.0938294036765));
#70242=CARTESIAN_POINT('Ctrl Pts',(24.4086688458745,-0.806543841888507,
-3.12179051731708));
#70243=CARTESIAN_POINT('Ctrl Pts',(24.4148399687912,-0.709493734442499,
-3.14525904225619));
#70244=CARTESIAN_POINT('Ctrl Pts',(24.4210110917079,-0.61171386643955,-3.16416240229631));
#70245=CARTESIAN_POINT('Ctrl Pts',(24.4257066136534,-0.537314519313144,
-3.17854570710338));
#70246=CARTESIAN_POINT('Ctrl Pts',(24.430402135599,-0.462492905727497,-3.19028707697477));
#70247=CARTESIAN_POINT('Ctrl Pts',(24.4350976575445,-0.387451761467251,
-3.19937473501244));
#70248=CARTESIAN_POINT('Ctrl Pts',(24.4412699056373,-0.288810425123307,
-3.21132043149547));
#70249=CARTESIAN_POINT('Ctrl Pts',(24.44744215373,-0.189442497136187,-3.21872099751619));
#70250=CARTESIAN_POINT('Ctrl Pts',(24.4536144018228,-0.0898029357186574,
-3.22149856359371));
#70251=CARTESIAN_POINT('Ctrl Pts',(24.4597782904754,0.009701677955975,-3.22427236784944));
#70252=CARTESIAN_POINT('Ctrl Pts',(24.4659421791281,0.109476763457256,-3.22243560499243));
#70253=CARTESIAN_POINT('Ctrl Pts',(24.4721060677807,0.209060493896643,-3.21596195132836));
#70254=CARTESIAN_POINT('Ctrl Pts',(24.4782634294392,0.308538774277512,-3.20949515267117));
#70255=CARTESIAN_POINT('Ctrl Pts',(24.4844207910978,0.407825671368895,-3.19840125285889));
#70256=CARTESIAN_POINT('Ctrl Pts',(24.4905781527563,0.506458566839546,-3.18270596860201));
#70257=CARTESIAN_POINT('Ctrl Pts',(24.4967310169026,0.605019418035451,-3.16702214862756));
#70258=CARTESIAN_POINT('Ctrl Pts',(24.5028838810489,0.702926789677983,-3.14674369447273));
#70259=CARTESIAN_POINT('Ctrl Pts',(24.5090367451952,0.799723319653441,-3.12194813770224));
#70260=CARTESIAN_POINT('Ctrl Pts',(24.5151872783318,0.896483178307803,-3.09716197471709));
#70261=CARTESIAN_POINT('Ctrl Pts',(24.5213378114683,0.992132611183931,-3.06786221713491));
#70262=CARTESIAN_POINT('Ctrl Pts',(24.5274883446048,1.08622546151676,-3.03417728705043));
#70263=CARTESIAN_POINT('Ctrl Pts',(24.53363819282,1.18030783370098,-3.0004961081086));
#70264=CARTESIAN_POINT('Ctrl Pts',(24.5397880410353,1.27283355900908,-2.96243087394459));
#70265=CARTESIAN_POINT('Ctrl Pts',(24.5459378892505,1.36337359689445,-2.92015924185499));
#70266=CARTESIAN_POINT('Ctrl Pts',(24.5520886976296,1.45392777062112,-2.87788100997709));
#70267=CARTESIAN_POINT('Ctrl Pts',(24.5582395060087,1.54249524751428,-2.83139525950301));
#70268=CARTESIAN_POINT('Ctrl Pts',(24.5643903143879,1.62866977107641,-2.78092652532963));
#70269=CARTESIAN_POINT('Ctrl Pts',(24.5705477007541,1.71493645405328,-2.73040381732719));
#70270=CARTESIAN_POINT('Ctrl Pts',(24.5767050871202,1.79880469779382,-2.67588983958058));
#70271=CARTESIAN_POINT('Ctrl Pts',(24.5828624734864,1.87989564783416,-2.61765351331191));
#70272=CARTESIAN_POINT('Ctrl Pts',(24.5890232962234,1.96103185385717,-2.55938468597905));
#70273=CARTESIAN_POINT('Ctrl Pts',(24.5951841189604,2.03938733876293,-2.49738964253551));
#70274=CARTESIAN_POINT('Ctrl Pts',(24.6013449416973,2.11461653092351,-2.43197748543135));
#70275=CARTESIAN_POINT('Ctrl Pts',(24.607516064614,2.18997149755173,-2.36645596680145));
#70276=CARTESIAN_POINT('Ctrl Pts',(24.6136871875307,2.26218941674399,-2.29750622303378));
#70277=CARTESIAN_POINT('Ctrl Pts',(24.6198583104474,2.33096166753404,-2.22547416677591));
#70278=CARTESIAN_POINT('Ctrl Pts',(24.624553832393,2.38328952053481,-2.17066597294912));
#70279=CARTESIAN_POINT('Ctrl Pts',(24.6292493543386,2.43362327811525,-2.11407404354159));
#70280=CARTESIAN_POINT('Ctrl Pts',(24.6339448762842,2.4818434121291,-2.05586255381321));
#70281=CARTESIAN_POINT('Ctrl Pts',(24.640117124377,2.54522861906614,-1.97934374278115));
#70282=CARTESIAN_POINT('Ctrl Pts',(24.6462893724698,2.60518329728354,-1.89975611780241));
#70283=CARTESIAN_POINT('Ctrl Pts',(24.6524616205625,2.6613959417158,-1.8174402889555));
#70284=CARTESIAN_POINT('Ctrl Pts',(24.6586255092152,2.71753245404368,-1.73523594529733));
#70285=CARTESIAN_POINT('Ctrl Pts',(24.6647893978678,2.76993676310318,-1.65031109748117));
#70286=CARTESIAN_POINT('Ctrl Pts',(24.6709532865204,2.8183370106406,-1.56304000491138));
#70287=CARTESIAN_POINT('Ctrl Pts',(24.677110648179,2.86668600674453,-1.47586132444329));
#70288=CARTESIAN_POINT('Ctrl Pts',(24.6832680098375,2.91103916120595,-1.38634171633193));
#70289=CARTESIAN_POINT('Ctrl Pts',(24.6894253714961,2.95116796468241,-1.29488424453009));
#70290=CARTESIAN_POINT('Ctrl Pts',(24.6955782356424,2.99126745693846,-1.20349357586919));
#70291=CARTESIAN_POINT('Ctrl Pts',(24.7017310997887,3.02714855887914,-1.11016825428707));
#70292=CARTESIAN_POINT('Ctrl Pts',(24.707883963935,3.05862919036995,-1.01533493898166));
#70293=CARTESIAN_POINT('Ctrl Pts',(24.7140344970716,3.0900978954379,-0.920537551234397));
#70294=CARTESIAN_POINT('Ctrl Pts',(24.7201850302081,3.11716930590786,-0.824233716736039));
#70295=CARTESIAN_POINT('Ctrl Pts',(24.7263355633447,3.13971021005953,-0.72686818567603));
#70296=CARTESIAN_POINT('Ctrl Pts',(24.7324854115599,3.16224860406359,-0.629513497209272));
#70297=CARTESIAN_POINT('Ctrl Pts',(24.7386352597751,3.18025739682994,-0.531097770422997));
#70298=CARTESIAN_POINT('Ctrl Pts',(24.7447851079903,3.19365404864355,-0.432077979168888));
#70299=CARTESIAN_POINT('Ctrl Pts',(24.7509359163694,3.20705279205054,-0.333042728145924));
#70300=CARTESIAN_POINT('Ctrl Pts',(24.7570867247486,3.21583790598795,-0.233403655822401));
#70301=CARTESIAN_POINT('Ctrl Pts',(24.7632375331277,3.21997860416463,-0.133623917103257));
#70302=CARTESIAN_POINT('Ctrl Pts',(24.7693949194939,3.22412373061435,-0.0337374688609638));
#70303=CARTESIAN_POINT('Ctrl Pts',(24.7755523058601,3.22361450472336,0.0662895113338177));
#70304=CARTESIAN_POINT('Ctrl Pts',(24.7817096922263,3.21847229493312,0.165992919270579));
#70305=CARTESIAN_POINT('Ctrl Pts',(24.7878705149633,3.21332721533117,0.265751970601542));
#70306=CARTESIAN_POINT('Ctrl Pts',(24.7940313377002,3.20354404514045,0.365186657745472));
#70307=CARTESIAN_POINT('Ctrl Pts',(24.8001921604372,3.18919594997975,0.463839147908784));
#70308=CARTESIAN_POINT('Ctrl Pts',(24.8063632833539,3.17482386647119,0.562656573572241));
#70309=CARTESIAN_POINT('Ctrl Pts',(24.8125344062706,3.15587169574759,0.660688763402786));
#70310=CARTESIAN_POINT('Ctrl Pts',(24.8187055291873,3.13246354809509,0.757489064182118));
#70311=CARTESIAN_POINT('Ctrl Pts',(24.8234010511328,3.1146526127936,0.831143072177134));
#70312=CARTESIAN_POINT('Ctrl Pts',(24.8280965730784,3.09426295540948,0.904084113421489));
#70313=CARTESIAN_POINT('Ctrl Pts',(24.8327920950239,3.07136805154229,0.97612286852903));
#70314=CARTESIAN_POINT('Ctrl Pts',(24.838963105624,3.04127880990082,1.07079858861741));
#70315=CARTESIAN_POINT('Ctrl Pts',(24.845134116224,3.00675491308035,1.16424834859305));
#70316=CARTESIAN_POINT('Ctrl Pts',(24.8513051268241,2.96791437521401,1.25602620350772));
#70317=CARTESIAN_POINT('Ctrl Pts',(24.8574683454387,2.92912288035311,1.34768817275023));
#70318=CARTESIAN_POINT('Ctrl Pts',(24.8636315640533,2.88602574101968,1.43768203499338));
#70319=CARTESIAN_POINT('Ctrl Pts',(24.869794782668,2.83879072369699,1.52557687107268));
#70320=CARTESIAN_POINT('Ctrl Pts',(24.8759518684649,2.79160270839798,1.61338424587008));
#70321=CARTESIAN_POINT('Ctrl Pts',(24.8821089542619,2.74028520233278,1.69909636506283));
#70322=CARTESIAN_POINT('Ctrl Pts',(24.8882660400589,2.68505366458286,1.78230311137308));
#70323=CARTESIAN_POINT('Ctrl Pts',(24.8944186464997,2.62986230846105,1.86544932374433));
#70324=CARTESIAN_POINT('Ctrl Pts',(24.9005712529404,2.57076282129297,1.94609342622972));
#70325=CARTESIAN_POINT('Ctrl Pts',(24.9067238593812,2.50801561081939,2.02385159001006));
#70326=CARTESIAN_POINT('Ctrl Pts',(24.9128742926136,2.44529056375954,2.10158228824505));
#70327=CARTESIAN_POINT('Ctrl Pts',(24.919024725846,2.37892062463272,2.17642873457796));
#70328=CARTESIAN_POINT('Ctrl Pts',(24.9251751590784,2.30920786141307,2.24803839275224));
#70329=CARTESIAN_POINT('Ctrl Pts',(24.931324399548,2.23950861769477,2.31963416355747));
#70330=CARTESIAN_POINT('Ctrl Pts',(24.9374736400177,2.1664681453471,2.38799408663982));
#70331=CARTESIAN_POINT('Ctrl Pts',(24.9436228804873,2.09042610766343,2.45280171454994));
#70332=CARTESIAN_POINT('Ctrl Pts',(24.949773879861,2.0143623192193,2.51762787977487));
#70333=CARTESIAN_POINT('Ctrl Pts',(24.9559248792348,1.93529558449351,2.57889944242733));
#70334=CARTESIAN_POINT('Ctrl Pts',(24.9620758786086,1.85359888667893,2.63634002545245));
#70335=CARTESIAN_POINT('Ctrl Pts',(24.9636729963052,1.83238619685259,2.65125457284238));
#70336=CARTESIAN_POINT('Ctrl Pts',(24.9652701140019,1.81099635528114,2.6659110624332));
#70337=CARTESIAN_POINT('Ctrl Pts',(24.9668672316986,1.78943621037801,2.68030513402634));
#70338=CARTESIAN_POINT('Ctrl Pts',(23.7170278226866,1.78943621037803,2.68030513402633));
#70339=CARTESIAN_POINT('Ctrl Pts',(23.7231781072839,1.70635511262692,2.73577207427372));
#70340=CARTESIAN_POINT('Ctrl Pts',(23.7293283918812,1.62066068072026,2.78739386047531));
#70341=CARTESIAN_POINT('Ctrl Pts',(23.7354786764785,1.53274737844311,2.83492557863091));
#70342=CARTESIAN_POINT('Ctrl Pts',(23.7416285775026,1.44483955903163,2.88245433238841));
#70343=CARTESIAN_POINT('Ctrl Pts',(23.7477784785267,1.35471352665834,2.92589331889868));
#70344=CARTESIAN_POINT('Ctrl Pts',(23.7539283795508,1.26278875004462,2.96504336144697));
#70345=CARTESIAN_POINT('Ctrl Pts',(23.7600795420464,1.17084511776445,3.00420143447595));
#70346=CARTESIAN_POINT('Ctrl Pts',(23.766230704542,1.0771024079397,3.03906864569759));
#70347=CARTESIAN_POINT('Ctrl Pts',(23.7723818670376,0.98199954061988,3.06949417082397));
#70348=CARTESIAN_POINT('Ctrl Pts',(23.7785397717703,0.886792431852533,3.0999530451108));
#70349=CARTESIAN_POINT('Ctrl Pts',(23.784697676503,0.790222603632329,3.12596038125505));
#70350=CARTESIAN_POINT('Ctrl Pts',(23.7908555812357,0.692743449068784,3.14741545974984));
#70351=CARTESIAN_POINT('Ctrl Pts',(23.7970171931663,0.595205609849946,3.16888345468704));
#70352=CARTESIAN_POINT('Ctrl Pts',(23.8031788050969,0.496757782115097,3.18579366173425));
#70353=CARTESIAN_POINT('Ctrl Pts',(23.8093404170274,0.397860790924237,3.19809698938996));
#70354=CARTESIAN_POINT('Ctrl Pts',(23.8155119924076,0.298803881322749,3.21042021177231));
#70355=CARTESIAN_POINT('Ctrl Pts',(23.8216835677878,0.199296790707494,3.2181216466416));
#70356=CARTESIAN_POINT('Ctrl Pts',(23.827855143168,0.0998026789936531,3.22120427600699));
#70357=CARTESIAN_POINT('Ctrl Pts',(23.8314220958872,0.0422985944674917,
3.22298592696639));
#70358=CARTESIAN_POINT('Ctrl Pts',(23.8349890486064,-0.0152011876087444,
3.22322566903398));
#70359=CARTESIAN_POINT('Ctrl Pts',(23.8385560013256,-0.072608098951784,
3.22193197111091));
#70360=CARTESIAN_POINT('Ctrl Pts',(23.8447282494184,-0.171944907410476,
3.21969335872468));
#70361=CARTESIAN_POINT('Ctrl Pts',(23.8509004975111,-0.271352932954708,
3.21285245620611));
#70362=CARTESIAN_POINT('Ctrl Pts',(23.8570727456039,-0.370370763169425,
3.20139704821025));
#70363=CARTESIAN_POINT('Ctrl Pts',(23.8632366342565,-0.469254487688776,
3.18995715494998));
#70364=CARTESIAN_POINT('Ctrl Pts',(23.8694005229092,-0.567748639562157,
3.17391522765422));
#70365=CARTESIAN_POINT('Ctrl Pts',(23.8755644115618,-0.665392356215619,
3.15331104948272));
#70366=CARTESIAN_POINT('Ctrl Pts',(23.8817217732204,-0.762932677107381,
3.13272868925066));
#70367=CARTESIAN_POINT('Ctrl Pts',(23.8878791348789,-0.859623930451618,
3.10759377182921));
#70368=CARTESIAN_POINT('Ctrl Pts',(23.8940364965375,-0.955011889189508,
3.0779977020795));
#70369=CARTESIAN_POINT('Ctrl Pts',(23.9001893606838,-1.05033017384695,3.04842325014164));
#70370=CARTESIAN_POINT('Ctrl Pts',(23.9063422248301,-1.14434664294999,3.01439425276787));
#70371=CARTESIAN_POINT('Ctrl Pts',(23.9124950889764,-1.23661965869101,2.97605265112009));
#70372=CARTESIAN_POINT('Ctrl Pts',(23.9186456221129,-1.32885771684211,2.93772557517061));
#70373=CARTESIAN_POINT('Ctrl Pts',(23.9247961552494,-1.41935323337495,2.89508930784641));
#70374=CARTESIAN_POINT('Ctrl Pts',(23.930946688386,-1.50768291632923,2.84833456361941));
#70375=CARTESIAN_POINT('Ctrl Pts',(23.9370965366012,-1.59600276291951,2.80158502598512));
#70376=CARTESIAN_POINT('Ctrl Pts',(23.9432463848164,-1.68215687153482,2.75071812648771));
#70377=CARTESIAN_POINT('Ctrl Pts',(23.9493962330316,-1.76574591057609,2.6959708718352));
#70378=CARTESIAN_POINT('Ctrl Pts',(23.9555470414107,-1.84934800021229,2.64121506959975));
#70379=CARTESIAN_POINT('Ctrl Pts',(23.9616978497899,-1.93038386141096,2.58257794688646));
#70380=CARTESIAN_POINT('Ctrl Pts',(23.967848658169,-2.00848339677528,2.52033966111277));
#70381=CARTESIAN_POINT('Ctrl Pts',(23.9740060445352,-2.08666645575175,2.45803481455332));
#70382=CARTESIAN_POINT('Ctrl Pts',(23.9801634309013,-2.161906577763,2.39212138559079));
#70383=CARTESIAN_POINT('Ctrl Pts',(23.9863208172675,-2.2338671152758,2.32291955818306));
#70384=CARTESIAN_POINT('Ctrl Pts',(23.9924816400045,-2.30586781318681,2.25367910998342));
#70385=CARTESIAN_POINT('Ctrl Pts',(23.9986424627415,-2.37458498282635,2.181146923865));
#70386=CARTESIAN_POINT('Ctrl Pts',(24.0048032854784,-2.4397206477835,2.10567820981243));
#70387=CARTESIAN_POINT('Ctrl Pts',(24.0109744083951,-2.50496521200365,2.03008332083947));
#70388=CARTESIAN_POINT('Ctrl Pts',(24.0171455313118,-2.56661604264621,1.95154243913336));
#70389=CARTESIAN_POINT('Ctrl Pts',(24.0233166542285,-2.62441698421198,1.8704419412213));
#70390=CARTESIAN_POINT('Ctrl Pts',(24.0280121761741,-2.6683969199973,1.80873369575489));
#70391=CARTESIAN_POINT('Ctrl Pts',(24.0327076981197,-2.71014883855629,1.7455442114804));
#70392=CARTESIAN_POINT('Ctrl Pts',(24.0374032200653,-2.74957783738817,1.6810530267198));
#70393=CARTESIAN_POINT('Ctrl Pts',(24.0437674626396,-2.80301933248364,1.5936426070746));
#70394=CARTESIAN_POINT('Ctrl Pts',(24.0501317052139,-2.85237038776646,1.50354830229794));
#70395=CARTESIAN_POINT('Ctrl Pts',(24.0564959477882,-2.89736080226112,1.41117608540565));
#70396=CARTESIAN_POINT('Ctrl Pts',(24.0628497727577,-2.94227757211535,1.31895507224808));
#70397=CARTESIAN_POINT('Ctrl Pts',(24.0692035977272,-2.98284773162445,1.22446392104366));
#70398=CARTESIAN_POINT('Ctrl Pts',(24.0755574226967,-3.01884531640117,1.12813585978937));
#70399=CARTESIAN_POINT('Ctrl Pts',(24.0818993142109,-3.05477529220661,1.0319887173708));
#70400=CARTESIAN_POINT('Ctrl Pts',(24.0882412057251,-3.08614966305172,0.934011907863526));
#70401=CARTESIAN_POINT('Ctrl Pts',(24.0945830972393,-3.11278969277883,0.834660344709092));
#70402=CARTESIAN_POINT('Ctrl Pts',(24.1009179698234,-3.13940023847785,0.735418739550518));
#70403=CARTESIAN_POINT('Ctrl Pts',(24.1072528424075,-3.1612867648525,0.634805789739645));
#70404=CARTESIAN_POINT('Ctrl Pts',(24.1135877149915,-3.17831959942743,0.53329362118393));
#70405=CARTESIAN_POINT('Ctrl Pts',(24.1199153215362,-3.19533289750103,0.431897886132405));
#70406=CARTESIAN_POINT('Ctrl Pts',(24.1262429280809,-3.20750352637341,0.329605377401343));
#70407=CARTESIAN_POINT('Ctrl Pts',(24.1325705346256,-3.21475257350628,0.226899655431163));
#70408=CARTESIAN_POINT('Ctrl Pts',(24.1372381728414,-3.22009992391228,0.151137493313834));
#70409=CARTESIAN_POINT('Ctrl Pts',(24.1419058110573,-3.2227702560013,0.0751507821873924));
#70410=CARTESIAN_POINT('Ctrl Pts',(24.1465734492731,-3.22274988426624,-0.000863690875605038));
#70411=CARTESIAN_POINT('',(23.8997658991183,-3.22274856360171,0.00296078655014494));
#70412=CARTESIAN_POINT('Ctrl Pts',(23.4730037159736,1.78943621026388,2.68030513410254));
#70413=CARTESIAN_POINT('Ctrl Pts',(23.4734202769121,1.78348160816408,2.68428056976452));
#70414=CARTESIAN_POINT('Ctrl Pts',(23.4738360373049,1.77751361735375,2.68823625624975));
#70415=CARTESIAN_POINT('Ctrl Pts',(23.4858998166118,1.6036433398868,2.80264826426368));
#70416=CARTESIAN_POINT('Ctrl Pts',(23.4969429837364,1.42577717955715,2.89718490302514));
#70417=CARTESIAN_POINT('Ctrl Pts',(23.519539157923,1.05435708852739,3.05205071370242));
#70418=CARTESIAN_POINT('Ctrl Pts',(23.5310521832852,0.861633880524336,3.1119531568544));
#70419=CARTESIAN_POINT('Ctrl Pts',(23.5442947945494,0.647027675885696,3.15718151956633));
#70420=CARTESIAN_POINT('Ctrl Pts',(23.5453835197282,0.629427807902366,3.16073734678112));
#70421=CARTESIAN_POINT('Ctrl Pts',(23.5470354604113,0.60279463602389,3.16588696999589));
#70422=CARTESIAN_POINT('Ctrl Pts',(23.5475952029045,0.59378253929595,3.16758961567034));
#70423=CARTESIAN_POINT('Ctrl Pts',(23.5485700164668,0.578109659940522,3.1704814401998));
#70424=CARTESIAN_POINT('Ctrl Pts',(23.5489845257417,0.571452140823291,3.17168816109181));
#70425=CARTESIAN_POINT('Ctrl Pts',(23.5498501047665,0.55756457541276,3.17416023245832));
#70426=CARTESIAN_POINT('Ctrl Pts',(23.5503012903154,0.550333914612286,3.17542186458456));
#70427=CARTESIAN_POINT('Ctrl Pts',(23.5511989632057,0.535964674634535,3.17787850887425));
#70428=CARTESIAN_POINT('Ctrl Pts',(23.5516454261434,0.52882625330304,3.17907419574772));
#70429=CARTESIAN_POINT('Ctrl Pts',(23.5531490752581,0.504812778821286,3.18301333882105));
#70430=CARTESIAN_POINT('Ctrl Pts',(23.5542097575234,0.487920159737118,3.18564652093662));
#70431=CARTESIAN_POINT('Ctrl Pts',(23.5620983688909,0.362643093973924,3.20415460434085));
#70432=CARTESIAN_POINT('Ctrl Pts',(23.5690965471975,0.253544721579583,3.21462706749474));
#70433=CARTESIAN_POINT('Ctrl Pts',(23.5898330579131,-0.0637114018025083,
3.22883028399124));
#70434=CARTESIAN_POINT('Ctrl Pts',(23.6039565164935,-0.271951545080688,
3.21798517370643));
#70435=CARTESIAN_POINT('Ctrl Pts',(23.6235097243725,-0.55808966105122,3.17510107928485));
#70436=CARTESIAN_POINT('Ctrl Pts',(23.6289827422467,-0.638032406726126,
3.16000738112245));
#70437=CARTESIAN_POINT('Ctrl Pts',(23.6402207486007,-0.803263558192448,
3.12228382219302));
#70438=CARTESIAN_POINT('Ctrl Pts',(23.6459672121217,-0.888373604689581,
3.09914247916298));
#70439=CARTESIAN_POINT('Ctrl Pts',(23.652226583463,-0.982953433679048,3.06920866357304));
#70440=CARTESIAN_POINT('Ctrl Pts',(23.6529197591336,-0.993454501059695,
3.06582573477126));
#70441=CARTESIAN_POINT('Ctrl Pts',(23.6539387951978,-1.0089355553054,3.06075060493413));
#70442=CARTESIAN_POINT('Ctrl Pts',(23.6542670430012,-1.01392896772216,3.05910007513883));
#70443=CARTESIAN_POINT('Ctrl Pts',(23.6548469012831,-1.02276230808496,3.05615628537534));
#70444=CARTESIAN_POINT('Ctrl Pts',(23.6550988041043,-1.02660386155545,3.05486799905329));
#70445=CARTESIAN_POINT('Ctrl Pts',(23.6556284195854,-1.03468949533506,3.05213946218425));
#70446=CARTESIAN_POINT('Ctrl Pts',(23.6559060348698,-1.03893299233638,3.05069760651524));
#70447=CARTESIAN_POINT('Ctrl Pts',(23.6566435939825,-1.0502201754883,3.04683616441141));
#70448=CARTESIAN_POINT('Ctrl Pts',(23.6571026192863,-1.05725855699463,3.04440098804741));
#70449=CARTESIAN_POINT('Ctrl Pts',(23.6591987978795,-1.08945879916625,3.03313504193927));
#70450=CARTESIAN_POINT('Ctrl Pts',(23.6608194656517,-1.11451977263808,3.02401627680815));
#70451=CARTESIAN_POINT('Ctrl Pts',(23.6652122739396,-1.18278914021981,2.99821155030078));
#70452=CARTESIAN_POINT('Ctrl Pts',(23.6679525952223,-1.22575694448039,2.98090305390752));
#70453=CARTESIAN_POINT('Ctrl Pts',(23.6772013109621,-1.37133905243744,2.91857844963009));
#70454=CARTESIAN_POINT('Ctrl Pts',(23.6835343424194,-1.47197704944423,2.8691388935788));
#70455=CARTESIAN_POINT('Ctrl Pts',(23.6968768182774,-1.67975815318856,2.75324724807418));
#70456=CARTESIAN_POINT('Ctrl Pts',(23.7038636801026,-1.78598835084015,2.68555455362677));
#70457=CARTESIAN_POINT('Ctrl Pts',(23.721035208545,-2.03269792462533,2.50721762445044));
#70458=CARTESIAN_POINT('Ctrl Pts',(23.7313172082078,-2.16844439892737,2.39078160784915));
#70459=CARTESIAN_POINT('Ctrl Pts',(23.7431740645832,-2.30636372838925,2.25102681506842));
#70460=CARTESIAN_POINT('Ctrl Pts',(23.7442550904329,-2.31878012850893,2.23823458683127));
#70461=CARTESIAN_POINT('Ctrl Pts',(23.7458972905683,-2.33739995522785,2.21872993587714));
#70462=CARTESIAN_POINT('Ctrl Pts',(23.74645504988,-2.34368214618957,2.21209291712265));
#70463=CARTESIAN_POINT('Ctrl Pts',(23.7474273765545,-2.35456050885437,2.20050176999303));
#70464=CARTESIAN_POINT('Ctrl Pts',(23.7478413892577,-2.35916950724096,2.19555971556253));
#70465=CARTESIAN_POINT('Ctrl Pts',(23.7487068759005,-2.36875645519572,2.18521495226659));
#70466=CARTESIAN_POINT('Ctrl Pts',(23.7491584686572,-2.37373153838157,2.17980965084313));
#70467=CARTESIAN_POINT('Ctrl Pts',(23.7500572640548,-2.38357915797364,2.16903677065179));
#70468=CARTESIAN_POINT('Ctrl Pts',(23.7505044433147,-2.38845215223162,2.16366966746083));
#70469=CARTESIAN_POINT('Ctrl Pts',(23.7515507192917,-2.39979152802698,2.15109552088826));
#70470=CARTESIAN_POINT('Ctrl Pts',(23.7521504149913,-2.40624359415899,2.14387571474019));
#70471=CARTESIAN_POINT('Ctrl Pts',(23.7556466170595,-2.4435826896545,2.1017126919765));
#70472=CARTESIAN_POINT('Ctrl Pts',(23.7585733458551,-2.47373949083719,2.06613290091525));
#70473=CARTESIAN_POINT('Ctrl Pts',(23.7693838315092,-2.58108875235739,1.93375909647533));
#70474=CARTESIAN_POINT('Ctrl Pts',(23.777452816576,-2.65345106903884,1.83320337967078));
#70475=CARTESIAN_POINT('Ctrl Pts',(23.7919379743233,-2.7703705691159,1.64925325253249));
#70476=CARTESIAN_POINT('Ctrl Pts',(23.7982798247324,-2.81738467775259,1.56758779303045));
#70477=CARTESIAN_POINT('Ctrl Pts',(23.8090474016848,-2.89070842740288,1.42623782647081));
#70478=CARTESIAN_POINT('Ctrl Pts',(23.8134562506303,-2.91890847782342,1.36759748203578));
#70479=CARTESIAN_POINT('Ctrl Pts',(23.8288854891508,-3.01162955033319,1.15883395869922));
#70480=CARTESIAN_POINT('Ctrl Pts',(23.8398164531355,-3.06650388294999,1.00467722062702));
#70481=CARTESIAN_POINT('Ctrl Pts',(23.8508960753897,-3.11261056089464,0.835414503846904));
#70482=CARTESIAN_POINT('Ctrl Pts',(23.8516514028684,-3.11570328980735,0.823805145425565));
#70483=CARTESIAN_POINT('Ctrl Pts',(23.852738723673,-3.12008312673824,0.806986757929483));
#70484=CARTESIAN_POINT('Ctrl Pts',(23.8530736454099,-3.12142221626237,0.801791552741193));
#70485=CARTESIAN_POINT('Ctrl Pts',(23.8536611878988,-3.12375382013524,0.79265136161246));
#70486=CARTESIAN_POINT('Ctrl Pts',(23.8539141272245,-3.1247518464717,0.788707809388391));
#70487=CARTESIAN_POINT('Ctrl Pts',(23.8544416041466,-3.12682115478272,0.780465664475319));
#70488=CARTESIAN_POINT('Ctrl Pts',(23.8547160600656,-3.12789103888566,0.77616675839975));
#70489=CARTESIAN_POINT('Ctrl Pts',(23.8554362523553,-3.13068041336807,0.764859325197769));
#70490=CARTESIAN_POINT('Ctrl Pts',(23.85588114546,-3.13238524575619,0.757847156438468));
#70491=CARTESIAN_POINT('Ctrl Pts',(23.8568506860056,-3.13605999388658,0.742508242486001));
#70492=CARTESIAN_POINT('Ctrl Pts',(23.8573747995252,-3.13802033716632,0.734179230652083));
#70493=CARTESIAN_POINT('Ctrl Pts',(23.8589236345457,-3.14373463389994,0.709459550834804));
#70494=CARTESIAN_POINT('Ctrl Pts',(23.8599432893267,-3.14739357108795,0.693046923359981));
#70495=CARTESIAN_POINT('Ctrl Pts',(23.8746023698498,-3.19846082195336,0.455229022660595));
#70496=CARTESIAN_POINT('Ctrl Pts',(23.8871028727178,-3.22254052557432,0.229433624789051));
#70497=CARTESIAN_POINT('Ctrl Pts',(23.8997657266517,-3.2227486392817,0.00296150433855287));
#70498=CARTESIAN_POINT('Ctrl Pts',(23.8997657671943,-3.22274863994794,0.00296077924363577));
#70499=CARTESIAN_POINT('Ctrl Pts',(23.9124220347313,-3.22295659447685,-0.223393541721828));
#70500=CARTESIAN_POINT('Ctrl Pts',(23.9251913555592,-3.1993184214291,-0.449116445071595));
#70501=CARTESIAN_POINT('Ctrl Pts',(23.9399233137839,-3.14827503912222,-0.689088641369014));
#70502=CARTESIAN_POINT('Ctrl Pts',(23.9410697476223,-3.14415599829387,-0.707645329609252));
#70503=CARTESIAN_POINT('Ctrl Pts',(23.9428931480142,-3.13737487243252,-0.736966349291988));
#70504=CARTESIAN_POINT('Ctrl Pts',(23.9435666652802,-3.13482093605246,-0.747755430789164));
#70505=CARTESIAN_POINT('Ctrl Pts',(23.9448532600821,-3.12984921186356,-0.768285232313295));
#70506=CARTESIAN_POINT('Ctrl Pts',(23.9454660080507,-3.12744149242713,-0.778028273942384));
#70507=CARTESIAN_POINT('Ctrl Pts',(23.9465297708563,-3.12319285852936,-0.794882308526463));
#70508=CARTESIAN_POINT('Ctrl Pts',(23.9469800995703,-3.12137306036934,-0.801998586382847));
#70509=CARTESIAN_POINT('Ctrl Pts',(23.9478463390075,-3.11783201295848,-0.815651142850113));
#70510=CARTESIAN_POINT('Ctrl Pts',(23.9482621265365,-3.11611449615686,-0.822188356516703));
#70511=CARTESIAN_POINT('Ctrl Pts',(23.9492419984857,-3.11202505866147,-0.837556691490353));
#70512=CARTESIAN_POINT('Ctrl Pts',(23.9498066343287,-3.1096361014503,-0.846383182128466));
#70513=CARTESIAN_POINT('Ctrl Pts',(23.9514770064054,-3.102473398428,-0.872407547982178));
#70514=CARTESIAN_POINT('Ctrl Pts',(23.9525861626283,-3.09759437263171,-0.889575853826422));
#70515=CARTESIAN_POINT('Ctrl Pts',(23.9677321791505,-3.02931351866074,-1.12246760876618));
#70516=CARTESIAN_POINT('Ctrl Pts',(23.9825305107754,-2.94366080241747,-1.33097640330434));
#70517=CARTESIAN_POINT('Ctrl Pts',(24.0047132199061,-2.78754706084985,-1.62067303497832));
#70518=CARTESIAN_POINT('Ctrl Pts',(24.0117966993987,-2.73363077361013,-1.71004743944285));
#70519=CARTESIAN_POINT('Ctrl Pts',(24.0279815501492,-2.59986478255717,-1.90924472583986));
#70520=CARTESIAN_POINT('Ctrl Pts',(24.0370367020506,-2.5172130875698,-2.01696762923823));
#70521=CARTESIAN_POINT('Ctrl Pts',(24.0473045077119,-2.41161252548228,-2.13795800786652));
#70522=CARTESIAN_POINT('Ctrl Pts',(24.0488855059699,-2.39499668946518,-2.15655520791147));
#70523=CARTESIAN_POINT('Ctrl Pts',(24.0509120926539,-2.3732105572202,-2.1803768322985));
#70524=CARTESIAN_POINT('Ctrl Pts',(24.0513717239377,-2.36823648829482,-2.18577844662803));
#70525=CARTESIAN_POINT('Ctrl Pts',(24.0521081845331,-2.36021273018471,-2.1944323428019));
#70526=CARTESIAN_POINT('Ctrl Pts',(24.0523858910943,-2.35717471399041,-2.1976953399327));
#70527=CARTESIAN_POINT('Ctrl Pts',(24.0529154030411,-2.35135810384829,-2.20391676395785));
#70528=CARTESIAN_POINT('Ctrl Pts',(24.0531672933293,-2.34858070069279,-2.20687623745996));
#70529=CARTESIAN_POINT('Ctrl Pts',(24.0537474529866,-2.34215980453836,-2.21369220075607));
#70530=CARTESIAN_POINT('Ctrl Pts',(24.0540754165548,-2.33851235117037,-2.21754497002045));
#70531=CARTESIAN_POINT('Ctrl Pts',(24.0551236786137,-2.32679793023771,-2.22985775347512));
#70532=CARTESIAN_POINT('Ctrl Pts',(24.0558411955534,-2.31869432849218,-2.23828300928951));
#70533=CARTESIAN_POINT('Ctrl Pts',(24.0683826639981,-2.17559215281365,-2.38545409714793));
#70534=CARTESIAN_POINT('Ctrl Pts',(24.0792892444952,-2.02838551313346,-2.51182575214239));
#70535=CARTESIAN_POINT('Ctrl Pts',(24.0982675329639,-1.75226450068466,-2.70866067242313));
#70536=CARTESIAN_POINT('Ctrl Pts',(24.1063464504612,-1.62824791669422,-2.78497408957766));
#70537=CARTESIAN_POINT('Ctrl Pts',(24.1202262384422,-1.41248151978341,-2.89839252605533));
#70538=CARTESIAN_POINT('Ctrl Pts',(24.1259073469837,-1.32341629099745,-2.94012758488685));
#70539=CARTESIAN_POINT('Ctrl Pts',(24.1338588851236,-1.1991927212137,-2.99154821290174));
#70540=CARTESIAN_POINT('Ctrl Pts',(24.1360136075413,-1.16556834657176,-3.0048085078227));
#70541=CARTESIAN_POINT('Ctrl Pts',(24.1397328746014,-1.10765792045297,-3.02652811261941));
#70542=CARTESIAN_POINT('Ctrl Pts',(24.1412880863984,-1.08348020644468,-3.03526754483951));
#70543=CARTESIAN_POINT('Ctrl Pts',(24.1433459998904,-1.05155077689729,-3.04637885700123));
#70544=CARTESIAN_POINT('Ctrl Pts',(24.1438400218268,-1.04389055217857,-3.04901224824852));
#70545=CARTESIAN_POINT('Ctrl Pts',(24.1448176028796,-1.0287422708796,-3.05415606597899));
#70546=CARTESIAN_POINT('Ctrl Pts',(24.1453011113823,-1.02125475065553,-3.05666790275898));
#70547=CARTESIAN_POINT('Ctrl Pts',(24.1462302294854,-1.00687623019897,-3.06143273337718));
#70548=CARTESIAN_POINT('Ctrl Pts',(24.1466756929059,-0.9999867041967,-3.06369004861693));
#70549=CARTESIAN_POINT('Ctrl Pts',(24.1476932640905,-0.984258999632539,
-3.06878444118112));
#70550=CARTESIAN_POINT('Ctrl Pts',(24.1482658593667,-0.975416093114644,
-3.07160661009801));
#70551=CARTESIAN_POINT('Ctrl Pts',(24.1497793507929,-0.952062268652112,
-3.07894884599618));
#70552=CARTESIAN_POINT('Ctrl Pts',(24.1507223538793,-0.937531486267142,
-3.0834044916557));
#70553=CARTESIAN_POINT('Ctrl Pts',(24.157043774263,-0.840267451275416,-3.11247795038588));
#70554=CARTESIAN_POINT('Ctrl Pts',(24.1625268956404,-0.75661231091669,-3.13386405203334));
#70555=CARTESIAN_POINT('Ctrl Pts',(24.1720642044643,-0.612431507189188,
-3.16461382936763));
#70556=CARTESIAN_POINT('Ctrl Pts',(24.1760661171515,-0.552309744809216,
-3.17565840092317));
#70557=CARTESIAN_POINT('Ctrl Pts',(24.1921324067065,-0.312215380081605,
-3.21274036577006));
#70558=CARTESIAN_POINT('Ctrl Pts',(24.2045038562107,-0.130500535951932,
-3.22523488105438));
#70559=CARTESIAN_POINT('Ctrl Pts',(24.2265038557349,0.195408718925657,-3.22004830389745));
#70560=CARTESIAN_POINT('Ctrl Pts',(24.2361378471194,0.339237330303576,-3.20808712063632));
#70561=CARTESIAN_POINT('Ctrl Pts',(24.2466684543615,0.502539931309318,-3.18339619838852));
#70562=CARTESIAN_POINT('Ctrl Pts',(24.2479964620516,0.523254053050859,-3.18005707325042));
#70563=CARTESIAN_POINT('Ctrl Pts',(24.249771897695,0.551131169313726,-3.17528349980527));
#70564=CARTESIAN_POINT('Ctrl Pts',(24.2502288999336,0.558323493429724,-3.17402674044763));
#70565=CARTESIAN_POINT('Ctrl Pts',(24.2509621566829,0.569891514551294,-3.17196485124729));
#70566=CARTESIAN_POINT('Ctrl Pts',(24.2512392750444,0.574269872363887,-3.17117509295435));
#70567=CARTESIAN_POINT('Ctrl Pts',(24.2517683757404,0.582642154189509,-3.16964701170753));
#70568=CARTESIAN_POINT('Ctrl Pts',(24.2520204402399,0.586636306743029,-3.16891020737707));
#70569=CARTESIAN_POINT('Ctrl Pts',(24.2526019506715,0.595863437666562,-3.16719002853917));
#70570=CARTESIAN_POINT('Ctrl Pts',(24.2529310861547,0.601095413377917,-3.16620122831886));
#70571=CARTESIAN_POINT('Ctrl Pts',(24.2539868789534,0.617907629362031,-3.16298068367275));
#70572=CARTESIAN_POINT('Ctrl Pts',(24.2547106981569,0.629478242129024,-3.16069830835176));
#70573=CARTESIAN_POINT('Ctrl Pts',(24.2627052050788,0.757730710628542,-3.13466749441315));
#70574=CARTESIAN_POINT('Ctrl Pts',(24.2696314484577,0.873037727802388,-3.10453027186463));
#70575=CARTESIAN_POINT('Ctrl Pts',(24.2906645546229,1.2245995746501,-2.99149875270655));
#70576=CARTESIAN_POINT('Ctrl Pts',(24.3042753896284,1.45304638361967,-2.88745079745108));
#70577=CARTESIAN_POINT('Ctrl Pts',(24.3231511483848,1.73388731700391,-2.71768855264025));
#70578=CARTESIAN_POINT('Ctrl Pts',(24.3276981246716,1.79912095903847,-2.67495023443257));
#70579=CARTESIAN_POINT('Ctrl Pts',(24.3341532234949,1.88778939303036,-2.6121468591654));
#70580=CARTESIAN_POINT('Ctrl Pts',(24.335989619172,1.91258570430405,-2.59404622825271));
#70581=CARTESIAN_POINT('Ctrl Pts',(24.339201215045,1.95517875548305,-2.56201175696724));
#70582=CARTESIAN_POINT('Ctrl Pts',(24.3405701495425,1.97309474593036,-2.54823964576696));
#70583=CARTESIAN_POINT('Ctrl Pts',(24.342556502518,1.99873908623755,-2.52809412699337));
#70584=CARTESIAN_POINT('Ctrl Pts',(24.3431679316176,2.00658514545121,-2.52187111095803));
#70585=CARTESIAN_POINT('Ctrl Pts',(24.3442301406221,2.02013258745581,-2.51102285702446));
#70586=CARTESIAN_POINT('Ctrl Pts',(24.3446802399656,2.02584743657954,-2.50641449518807));
#70587=CARTESIAN_POINT('Ctrl Pts',(24.3455465589255,2.03679730607112,-2.49752278242673));
#70588=CARTESIAN_POINT('Ctrl Pts',(24.3459626571503,2.04203469078258,-2.49324239400952));
#70589=CARTESIAN_POINT('Ctrl Pts',(24.3469440586128,2.05433571617093,-2.48312430247615));
#70590=CARTESIAN_POINT('Ctrl Pts',(24.3475099175341,2.06138798238261,-2.47727291988379));
#70591=CARTESIAN_POINT('Ctrl Pts',(24.3491862910293,2.08216090180188,-2.45988715988291));
#70592=CARTESIAN_POINT('Ctrl Pts',(24.3503002602566,2.09581021539986,-2.44826844534009));
#70593=CARTESIAN_POINT('Ctrl Pts',(24.3632602826306,2.25280591310585,-2.31235392627357));
#70594=CARTESIAN_POINT('Ctrl Pts',(24.3756375758673,2.38497788563792,-2.17576951099838));
#70595=CARTESIAN_POINT('Ctrl Pts',(24.3971781736522,2.58740556101427,-1.92584047345257));
#70596=CARTESIAN_POINT('Ctrl Pts',(24.4061444276756,2.66407811116201,-1.8183000411561));
#70597=CARTESIAN_POINT('Ctrl Pts',(24.4206274598583,2.7776519434225,-1.63633214160681));
#70598=CARTESIAN_POINT('Ctrl Pts',(24.4261723155484,2.81865862069949,-1.56463990762252));
#70599=CARTESIAN_POINT('Ctrl Pts',(24.4352270262218,2.88209127682018,-1.44313474562486));
#70600=CARTESIAN_POINT('Ctrl Pts',(24.4387864063127,2.90608599981429,-1.39418538986573));
#70601=CARTESIAN_POINT('Ctrl Pts',(24.4435636557174,2.9371414275009,-1.32654239064565));
#70602=CARTESIAN_POINT('Ctrl Pts',(24.4448341301516,2.94528609370989,-1.30835941158712));
#70603=CARTESIAN_POINT('Ctrl Pts',(24.4469910027674,2.95892567642942,-1.27713608778465));
#70604=CARTESIAN_POINT('Ctrl Pts',(24.4478819609886,2.9645041931189,-1.26413316215955));
#70605=CARTESIAN_POINT('Ctrl Pts',(24.4491308157636,2.97224735064338,-1.2457515207129));
#70606=CARTESIAN_POINT('Ctrl Pts',(24.4494929116256,2.97448329079731,-1.24040328876596));
#70607=CARTESIAN_POINT('Ctrl Pts',(24.450111242884,2.97828604404049,-1.23123792461093));
#70608=CARTESIAN_POINT('Ctrl Pts',(24.4503679098844,2.97985997330581,-1.22742377658365));
#70609=CARTESIAN_POINT('Ctrl Pts',(24.4508594644979,2.98286555916548,-1.22010039846514));
#70610=CARTESIAN_POINT('Ctrl Pts',(24.4510944225759,2.98429835030322,-1.21659166655155));
#70611=CARTESIAN_POINT('Ctrl Pts',(24.4516510884338,2.98768367818449,-1.20825944224309));
#70612=CARTESIAN_POINT('Ctrl Pts',(24.4519724641509,2.98963073598998,-1.20343371399519));
#70613=CARTESIAN_POINT('Ctrl Pts',(24.4529331064894,2.99542830684835,-1.18896369107299));
#70614=CARTESIAN_POINT('Ctrl Pts',(24.4535703128601,2.99924394767685,-1.17930536728709));
#70615=CARTESIAN_POINT('Ctrl Pts',(24.4668959167809,3.07838646082462,-0.976107545030948));
#70616=CARTESIAN_POINT('Ctrl Pts',(24.4785268946649,3.13489020979572,-0.775719669317487));
#70617=CARTESIAN_POINT('Ctrl Pts',(24.5041585737129,3.21615993811243,-0.324498349993523));
#70618=CARTESIAN_POINT('Ctrl Pts',(24.5181153637159,3.23165206859308,-0.0734265439457822));
#70619=CARTESIAN_POINT('Ctrl Pts',(24.5353381615681,3.21581706078861,0.214631633178711));
#70620=CARTESIAN_POINT('Ctrl Pts',(24.53761405516,3.21307881532083,0.252330041067377));
#70621=CARTESIAN_POINT('Ctrl Pts',(24.5406487632862,3.20858564698239,0.3020648574759));
#70622=CARTESIAN_POINT('Ctrl Pts',(24.5413888612738,3.20742466442282,0.314152905241428));
#70623=CARTESIAN_POINT('Ctrl Pts',(24.5426065644947,3.20540798805554,0.33397260215336));
#70624=CARTESIAN_POINT('Ctrl Pts',(24.5430828968478,3.20459256464288,0.341708299336075));
#70625=CARTESIAN_POINT('Ctrl Pts',(24.5440074619479,3.20295852301971,0.356689542889614));
#70626=CARTESIAN_POINT('Ctrl Pts',(24.5444555846405,3.20214330410689,0.363935418394814));
#70627=CARTESIAN_POINT('Ctrl Pts',(24.5454924893318,3.20020348224519,0.380665805270519));
#70628=CARTESIAN_POINT('Ctrl Pts',(24.5460818237653,3.19906129718454,0.390148172859003));
#70629=CARTESIAN_POINT('Ctrl Pts',(24.5476688146303,3.19587935418773,0.415610684270149));
#70630=CARTESIAN_POINT('Ctrl Pts',(24.5486689194122,3.19376191747903,0.431580683851429));
#70631=CARTESIAN_POINT('Ctrl Pts',(24.5562773525415,3.17680772848648,0.552487088823846));
#70632=CARTESIAN_POINT('Ctrl Pts',(24.5630451041883,3.15692413316605,0.656639280067787));
#70633=CARTESIAN_POINT('Ctrl Pts',(24.5903246141465,3.05835349330857,1.06305383976668));
#70634=CARTESIAN_POINT('Ctrl Pts',(24.6119993037899,2.94107086922114,1.35412853763791));
#70635=CARTESIAN_POINT('Ctrl Pts',(24.6356478877074,2.75988257730599,1.66475738814796));
#70636=CARTESIAN_POINT('Ctrl Pts',(24.6387342229977,2.73507177555099,1.70521314851884));
#70637=CARTESIAN_POINT('Ctrl Pts',(24.643518035678,2.69462388859257,1.76801068495882));
#70638=CARTESIAN_POINT('Ctrl Pts',(24.6452469560196,2.67958210594207,1.79072598077847));
#70639=CARTESIAN_POINT('Ctrl Pts',(24.6474246732853,2.66006756088026,1.81939920994147));
#70640=CARTESIAN_POINT('Ctrl Pts',(24.6478904288879,2.65586027802726,1.82553529130181));
#70641=CARTESIAN_POINT('Ctrl Pts',(24.6486343520619,2.64908552716697,1.83534288417639));
#70642=CARTESIAN_POINT('Ctrl Pts',(24.648913428406,2.64653161775061,1.83902366204834));
#70643=CARTESIAN_POINT('Ctrl Pts',(24.6494439272661,2.6416529957989,1.84602368174154));
#70644=CARTESIAN_POINT('Ctrl Pts',(24.6496954388052,2.6393297260632,1.84934382445071));
#70645=CARTESIAN_POINT('Ctrl Pts',(24.6502725823676,2.63397495253043,1.85696559073099));
#70646=CARTESIAN_POINT('Ctrl Pts',(24.6505979168048,2.63093917340923,1.86126417320882));
#70647=CARTESIAN_POINT('Ctrl Pts',(24.6514648355828,2.62280393316453,1.87272378487449));
#70648=CARTESIAN_POINT('Ctrl Pts',(24.6520051478234,2.61768563390385,1.87987147765501));
#70649=CARTESIAN_POINT('Ctrl Pts',(24.6557905368795,2.58149524406424,1.92997686193812));
#70650=CARTESIAN_POINT('Ctrl Pts',(24.6589679542382,2.54939442962948,1.97218589222974));
#70651=CARTESIAN_POINT('Ctrl Pts',(24.66356306845,2.5006992428584,2.033037501982));
#70652=CARTESIAN_POINT('Ctrl Pts',(24.6650204354975,2.4849085069603,2.05230795959657));
#70653=CARTESIAN_POINT('Ctrl Pts',(24.6839448926844,2.27559942845645,2.30178357203485));
#70654=CARTESIAN_POINT('Ctrl Pts',(24.7000690263606,2.05099992471885,2.50399502260781));
#70655=CARTESIAN_POINT('Ctrl Pts',(24.7176902808396,1.79755176803132,2.67487365050067));
#70656=CARTESIAN_POINT('Ctrl Pts',(24.7179720150962,1.79349702741155,2.67759403485003));
#70657=CARTESIAN_POINT('Ctrl Pts',(24.7182540045911,1.78943620997144,2.68030513429778));
#70658=CARTESIAN_POINT('Origin',(-1.72497344927317,0.,0.));
#70659=CARTESIAN_POINT('',(26.2169191182387,1.78943621037807,2.6803051340263));
#70660=CARTESIAN_POINT('',(25.9683941809562,1.78943611353999,2.68030519867773));
#70661=CARTESIAN_POINT('',(-1.72497344927317,1.78943621037804,2.68030513402633));
#70662=CARTESIAN_POINT('',(25.3965734492343,-3.22274892221719,-0.00263568737792321));
#70663=CARTESIAN_POINT('Ctrl Pts',(25.3965734492731,-3.22274892221668,-0.00263568800522834));
#70664=CARTESIAN_POINT('Ctrl Pts',(25.4064511434359,-3.22261841837125,-0.16220735443242));
#70665=CARTESIAN_POINT('Ctrl Pts',(25.4163288375986,-3.21063356431501,-0.321308852596511));
#70666=CARTESIAN_POINT('Ctrl Pts',(25.4262065317614,-3.18701826592584,-0.47857301966895));
#70667=CARTESIAN_POINT('Ctrl Pts',(25.4272489382552,-3.1845261113816,-0.495169321022294));
#70668=CARTESIAN_POINT('Ctrl Pts',(25.428291344749,-3.18190446401791,-0.511745192054206));
#70669=CARTESIAN_POINT('Ctrl Pts',(25.4293337512428,-3.17915361093883,-0.528299044627735));
#70670=CARTESIAN_POINT('Ctrl Pts',(25.4355059993356,-3.16286538962451,-0.626316934559181));
#70671=CARTESIAN_POINT('Ctrl Pts',(25.4416782474284,-3.14201120273219,-0.723753356799299));
#70672=CARTESIAN_POINT('Ctrl Pts',(25.4478504955211,-3.11664432240526,-0.820149821751527));
#70673=CARTESIAN_POINT('Ctrl Pts',(25.4540143841738,-3.09131179794256,-0.916415731277972));
#70674=CARTESIAN_POINT('Ctrl Pts',(25.4601782728264,-3.06147883750468,-1.01164406664152));
#70675=CARTESIAN_POINT('Ctrl Pts',(25.4663421614791,-3.02725010945302,-1.10538424871928));
#70676=CARTESIAN_POINT('Ctrl Pts',(25.4724995231376,-2.99305762649246,-1.19902516852138));
#70677=CARTESIAN_POINT('Ctrl Pts',(25.4786568847961,-2.95447877809909,-1.29118066213792));
#70678=CARTESIAN_POINT('Ctrl Pts',(25.4848142464547,-2.91166839374426,-1.38141403184228));
#70679=CARTESIAN_POINT('Ctrl Pts',(25.490967110601,-2.86888927931282,-1.47158149252477));
#70680=CARTESIAN_POINT('Ctrl Pts',(25.4971199747473,-2.82188495965848,-1.55982922937228));
#70681=CARTESIAN_POINT('Ctrl Pts',(25.5032728388936,-2.7708585074938,-1.64574016598892));
#70682=CARTESIAN_POINT('Ctrl Pts',(25.5094233720301,-2.71985138667719,-1.73161855528651));
#70683=CARTESIAN_POINT('Ctrl Pts',(25.5155739051667,-2.6648253826722,-1.81516153037809));
#70684=CARTESIAN_POINT('Ctrl Pts',(25.5217244383032,-2.60602925073417,-1.89597708499283));
#70685=CARTESIAN_POINT('Ctrl Pts',(25.5278742865184,-2.54723966631388,-1.97678364001423));
#70686=CARTESIAN_POINT('Ctrl Pts',(25.5340241347336,-2.48468104421193,-2.05486302715625));
#70687=CARTESIAN_POINT('Ctrl Pts',(25.5401739829489,-2.41864457081421,-2.12985351669334));
#70688=CARTESIAN_POINT('Ctrl Pts',(25.546324791328,-2.35259778726936,-2.20485571435081));
#70689=CARTESIAN_POINT('Ctrl Pts',(25.5524755997072,-2.28307236100721,-2.27676773047784));
#70690=CARTESIAN_POINT('Ctrl Pts',(25.5586264080863,-2.21039805259985,-2.34526288751662));
#70691=CARTESIAN_POINT('Ctrl Pts',(25.5647837944525,-2.137646022594,-2.41383129675705));
#70692=CARTESIAN_POINT('Ctrl Pts',(25.5709411808187,-2.06173870246463,-2.47897525141644));
#70693=CARTESIAN_POINT('Ctrl Pts',(25.5770985671849,-1.98304073711152,-2.54040685667793));
#70694=CARTESIAN_POINT('Ctrl Pts',(25.5832593899218,-1.9042988512746,-2.60187274625429));
#70695=CARTESIAN_POINT('Ctrl Pts',(25.5894202126588,-1.8227635730985,-2.65962190935768));
#70696=CARTESIAN_POINT('Ctrl Pts',(25.5955810353958,-1.73882874207579,-2.71340969413598));
#70697=CARTESIAN_POINT('Ctrl Pts',(25.6017521583125,-1.65475358176889,-2.76728740584027));
#70698=CARTESIAN_POINT('Ctrl Pts',(25.6079232812291,-1.56827123162878,-2.81719029285439));
#70699=CARTESIAN_POINT('Ctrl Pts',(25.6140944041458,-1.47980045897549,-2.86291951757571));
#70700=CARTESIAN_POINT('Ctrl Pts',(25.6187899260914,-1.41248427355162,-2.89771425122965));
#70701=CARTESIAN_POINT('Ctrl Pts',(25.6234854480369,-1.34401741123988,-2.93009360253979));
#70702=CARTESIAN_POINT('Ctrl Pts',(25.6281809699825,-1.2745910437658,-2.9599890597183));
#70703=CARTESIAN_POINT('Ctrl Pts',(25.6343532180752,-1.18333031296776,-2.99928653946431));
#70704=CARTESIAN_POINT('Ctrl Pts',(25.640525466168,-1.09008985363507,-3.03442868273002));
#70705=CARTESIAN_POINT('Ctrl Pts',(25.6466977142608,-0.995284156096808,
-3.06521239249789));
#70706=CARTESIAN_POINT('Ctrl Pts',(25.6528616029134,-0.900606859514062,
-3.0959544100695));
#70707=CARTESIAN_POINT('Ctrl Pts',(25.659025491566,-0.804368947753559,-3.12234959380749));
#70708=CARTESIAN_POINT('Ctrl Pts',(25.6651893802186,-0.707006047244728,
-3.14424235892518));
#70709=CARTESIAN_POINT('Ctrl Pts',(25.6713467418772,-0.609746245138786,
-3.16611194160781));
#70710=CARTESIAN_POINT('Ctrl Pts',(25.6775041035357,-0.511364244079028,
-3.18348848943958));
#70711=CARTESIAN_POINT('Ctrl Pts',(25.6836614651943,-0.412311115966327,
-3.19626611941975));
#70712=CARTESIAN_POINT('Ctrl Pts',(25.6898143293406,-0.313330339078197,
-3.20903441625524));
#70713=CARTESIAN_POINT('Ctrl Pts',(25.6959671934869,-0.213679839265979,
-3.21721041845915));
#70714=CARTESIAN_POINT('Ctrl Pts',(25.7021200576332,-0.113820268406736,
-3.22073943512974));
#70715=CARTESIAN_POINT('Ctrl Pts',(25.7082705907697,-0.0139985293002585,
-3.22426711483397));
#70716=CARTESIAN_POINT('Ctrl Pts',(25.7144211239062,0.0860316898480511,
-3.22315129180131));
#70717=CARTESIAN_POINT('Ctrl Pts',(25.7205716570428,0.185806125355152,-3.2173892593655));
#70718=CARTESIAN_POINT('Ctrl Pts',(25.726721505258,0.2855694500142,-3.21162786858772));
#70719=CARTESIAN_POINT('Ctrl Pts',(25.7328713534732,0.385076614009189,-3.20122132211802));
#70720=CARTESIAN_POINT('Ctrl Pts',(25.7390212016884,0.483865879610104,-3.18621897757344));
#70721=CARTESIAN_POINT('Ctrl Pts',(25.7451720100675,0.582670568988227,-3.17121429074179));
#70722=CARTESIAN_POINT('Ctrl Pts',(25.7513228184466,0.680756707852433,-3.15161244585278));
#70723=CARTESIAN_POINT('Ctrl Pts',(25.7574736268258,0.777671187211214,-3.12751420253874));
#70724=CARTESIAN_POINT('Ctrl Pts',(25.7636310131919,0.874689311839299,-3.10339018733865));
#70725=CARTESIAN_POINT('Ctrl Pts',(25.7697883995581,0.970532852425206,-3.07476027630433));
#70726=CARTESIAN_POINT('Ctrl Pts',(25.7759457859243,1.06476246205168,-3.04177554430067));
#70727=CARTESIAN_POINT('Ctrl Pts',(25.7821066086613,1.15904466020469,-3.00877240387463));
#70728=CARTESIAN_POINT('Ctrl Pts',(25.7882674313982,1.25171073075715,-2.97140976485196));
#70729=CARTESIAN_POINT('Ctrl Pts',(25.7944282541352,1.34234191734396,-2.92988664276305));
#70730=CARTESIAN_POINT('Ctrl Pts',(25.8005993770519,1.43312462874343,-2.88829409883899));
#70731=CARTESIAN_POINT('Ctrl Pts',(25.8067704999686,1.52186527437194,-2.84252737696021));
#70732=CARTESIAN_POINT('Ctrl Pts',(25.8129416228852,1.60817015848789,-2.79283123440158));
#70733=CARTESIAN_POINT('Ctrl Pts',(25.8176371448309,1.67383834932636,-2.75501812791398));
#70734=CARTESIAN_POINT('Ctrl Pts',(25.8223326667765,1.73809688178141,-2.71493103980607));
#70735=CARTESIAN_POINT('Ctrl Pts',(25.8270281887221,1.80078475461697,-2.6726937404123));
#70736=CARTESIAN_POINT('Ctrl Pts',(25.8332004368149,1.88318775646201,-2.61717294982807));
#70737=CARTESIAN_POINT('Ctrl Pts',(25.8393726849076,1.96316571170811,-2.55773996097069));
#70738=CARTESIAN_POINT('Ctrl Pts',(25.8455449330004,2.04032365416872,-2.49463363016287));
#70739=CARTESIAN_POINT('Ctrl Pts',(25.851708821653,2.11737709707084,-2.43161276798599));
#70740=CARTESIAN_POINT('Ctrl Pts',(25.8578727103056,2.19161778520991,-2.36492872484808));
#70741=CARTESIAN_POINT('Ctrl Pts',(25.8640365989583,2.26267929160564,-2.29486382729761));
#70742=CARTESIAN_POINT('Ctrl Pts',(25.8701939606168,2.33366555036824,-2.22487312206267));
#70743=CARTESIAN_POINT('Ctrl Pts',(25.8763513222754,2.40147901262755,-2.1515089831154));
#70744=CARTESIAN_POINT('Ctrl Pts',(25.8825086839339,2.46578670946404,-2.07509360413705));
#70745=CARTESIAN_POINT('Ctrl Pts',(25.8886615480802,2.53004743412808,-1.99873404112688));
#70746=CARTESIAN_POINT('Ctrl Pts',(25.8948144122265,2.59080720565419,-1.91932800049423));
#70747=CARTESIAN_POINT('Ctrl Pts',(25.9009672763728,2.64777093838166,-1.83723341477383));
#70748=CARTESIAN_POINT('Ctrl Pts',(25.9071178095093,2.70471309042502,-1.7551699305497));
#70749=CARTESIAN_POINT('Ctrl Pts',(25.9132683426459,2.75786181386659,-1.67042028158036));
#70750=CARTESIAN_POINT('Ctrl Pts',(25.9194188757824,2.80696379970748,-1.58337354709233));
#70751=CARTESIAN_POINT('Ctrl Pts',(25.9255687239976,2.85606031756752,-1.49633650609977));
#70752=CARTESIAN_POINT('Ctrl Pts',(25.9317185722128,2.90111078035803,-1.40700326649594));
#70753=CARTESIAN_POINT('Ctrl Pts',(25.937868420428,2.941907041828,-1.31578893434426));
#70754=CARTESIAN_POINT('Ctrl Pts',(25.9440192288072,2.98270967273951,-1.22456036107502));
#70755=CARTESIAN_POINT('Ctrl Pts',(25.9501700371863,3.01925660569321,-1.13145050847048));
#70756=CARTESIAN_POINT('Ctrl Pts',(25.9563208455654,3.05138759991882,-1.03689501761829));
#70757=CARTESIAN_POINT('Ctrl Pts',(25.9624782319316,3.08355295666249,-0.942238404319069));
#70758=CARTESIAN_POINT('Ctrl Pts',(25.9686356182978,3.11129280404582,-0.846133477572178));
#70759=CARTESIAN_POINT('Ctrl Pts',(25.974793004664,3.13449666821515,-0.749031507647139));
#70760=CARTESIAN_POINT('Ctrl Pts',(25.980953827401,3.15771348221024,-0.651875346162331));
#70761=CARTESIAN_POINT('Ctrl Pts',(25.9871146501379,3.17638919038319,-0.553721460092493));
#70762=CARTESIAN_POINT('Ctrl Pts',(25.9932754728749,3.19046478051791,-0.45502972075985));
#70763=CARTESIAN_POINT('Ctrl Pts',(25.9994465957916,3.20456390340376,-0.356172980307013));
#70764=CARTESIAN_POINT('Ctrl Pts',(26.0056177187082,3.21404750471343,-0.256777023023595));
#70765=CARTESIAN_POINT('Ctrl Pts',(26.0117888416249,3.21890860112972,-0.157305372041514));
#70766=CARTESIAN_POINT('Ctrl Pts',(26.0164843635705,3.22260734205748,-0.0816187706800719));
#70767=CARTESIAN_POINT('Ctrl Pts',(26.0211798855161,3.22363097265403,-0.00588842137078513));
#70768=CARTESIAN_POINT('Ctrl Pts',(26.0258754074616,3.22199655461114,0.0696833163242371));
#70769=CARTESIAN_POINT('Ctrl Pts',(26.0320478199131,3.21984806028064,0.169024761244146));
#70770=CARTESIAN_POINT('Ctrl Pts',(26.0382202323645,3.21309709702631,0.268441605044972));
#70771=CARTESIAN_POINT('Ctrl Pts',(26.0443926448159,3.20173103033753,0.367472409676948));
#70772=CARTESIAN_POINT('Ctrl Pts',(26.050556655457,3.19038043499604,0.466368414820806));
#70773=CARTESIAN_POINT('Ctrl Pts',(26.0567206660981,3.17442727188708,0.564878997462854));
#70774=CARTESIAN_POINT('Ctrl Pts',(26.0628846767392,3.15391091004099,0.662543231815437));
#70775=CARTESIAN_POINT('Ctrl Pts',(26.0693027784683,3.13254882858017,0.764233353372993));
#70776=CARTESIAN_POINT('Ctrl Pts',(26.0757208801975,3.1062392263513,0.865005371543196));
#70777=CARTESIAN_POINT('Ctrl Pts',(26.0821389819266,3.0750863857692,0.964345001831263));
#70778=CARTESIAN_POINT('Ctrl Pts',(26.088291605933,3.04522214819242,1.05957555751343));
#70779=CARTESIAN_POINT('Ctrl Pts',(26.0944442299393,3.01090752128512,1.15348940611871));
#70780=CARTESIAN_POINT('Ctrl Pts',(26.1005968539457,2.97228614769764,1.24564546268379));
#70781=CARTESIAN_POINT('Ctrl Pts',(26.1067471567657,2.93367934470664,1.3377667517461));
#70782=CARTESIAN_POINT('Ctrl Pts',(26.1128974595858,2.89076919182726,1.42813116656454));
#70783=CARTESIAN_POINT('Ctrl Pts',(26.1190477624059,2.84374802133819,1.5163161786498));
#70784=CARTESIAN_POINT('Ctrl Pts',(26.1251973900478,2.79673201281737,1.60449150981415));
#70785=CARTESIAN_POINT('Ctrl Pts',(26.1313470176897,2.74560608890042,1.69048753100129));
#70786=CARTESIAN_POINT('Ctrl Pts',(26.1374966453317,2.69060876380754,1.77390587197349));
#70787=CARTESIAN_POINT('Ctrl Pts',(26.1436472427918,2.63560276544036,1.85733736831557));
#70788=CARTESIAN_POINT('Ctrl Pts',(26.1497978402519,2.57672439283207,1.93819001478082));
#70789=CARTESIAN_POINT('Ctrl Pts',(26.155948437712,2.51425517594452,2.01609485707796));
#70790=CARTESIAN_POINT('Ctrl Pts',(26.1621049069745,2.45172632145301,2.09407407293639));
#70791=CARTESIAN_POINT('Ctrl Pts',(26.168261376237,2.38560005268462,2.16909952858232));
#70792=CARTESIAN_POINT('Ctrl Pts',(26.1744178454995,2.31619765702528,2.24083599937403));
#70793=CARTESIAN_POINT('Ctrl Pts',(26.1805777890285,2.24675609566771,2.31261295304735));
#70794=CARTESIAN_POINT('Ctrl Pts',(26.1867377325574,2.17403504176792,2.38109692834211));
#70795=CARTESIAN_POINT('Ctrl Pts',(26.1928976760864,2.09839062061772,2.44599148931545));
#70796=CARTESIAN_POINT('Ctrl Pts',(26.1990661581254,2.02264134612869,2.51097600287598));
#70797=CARTESIAN_POINT('Ctrl Pts',(26.2052346401643,1.94396095872055,2.57236090548764));
#70798=CARTESIAN_POINT('Ctrl Pts',(26.2114031222033,1.86273620934477,2.62989189452644));
#70799=CARTESIAN_POINT('Ctrl Pts',(26.2132417875484,1.83852520720482,2.64704039802366));
#70800=CARTESIAN_POINT('Ctrl Pts',(26.2150804528936,1.81408831882809,2.66384679315958));
#70801=CARTESIAN_POINT('Ctrl Pts',(26.2169191182387,1.78943621037807,2.6803051340263));
#70802=CARTESIAN_POINT('Ctrl Pts',(24.9668672316986,1.78943621037801,2.68030513402634));
#70803=CARTESIAN_POINT('Ctrl Pts',(24.9730253659514,1.7063050378271,2.73580550541515));
#70804=CARTESIAN_POINT('Ctrl Pts',(24.9791835002043,1.62064010479516,2.7874008839277));
#70805=CARTESIAN_POINT('Ctrl Pts',(24.9853416344572,1.53284979617197,2.8348702024741));
#70806=CARTESIAN_POINT('Ctrl Pts',(24.9915035882499,1.44500503622206,2.8823689635343));
#70807=CARTESIAN_POINT('Ctrl Pts',(24.9976655420425,1.35503266701405,2.92573638099519));
#70808=CARTESIAN_POINT('Ctrl Pts',(25.0038274958352,1.26336234213593,2.96479900751684));
#70809=CARTESIAN_POINT('Ctrl Pts',(25.0099992767797,1.17154582041404,3.0039239315455));
#70810=CARTESIAN_POINT('Ctrl Pts',(25.0161710577242,1.07802634331453,3.03873020710462));
#70811=CARTESIAN_POINT('Ctrl Pts',(25.0223428386687,0.983249997689492,3.06909384094778));
#70812=CARTESIAN_POINT('Ctrl Pts',(25.0254416637003,0.935663196590666,3.08433929269846));
#70813=CARTESIAN_POINT('Ctrl Pts',(25.0285404887319,0.887759724998352,3.09846555476231));
#70814=CARTESIAN_POINT('Ctrl Pts',(25.0316393137636,0.839596895532805,3.11146181328193));
#70815=CARTESIAN_POINT('Ctrl Pts',(25.0378115618563,0.743666041329783,3.1373477962083));
#70816=CARTESIAN_POINT('Ctrl Pts',(25.0439838099491,0.646368063480807,3.15883865464586));
#70817=CARTESIAN_POINT('Ctrl Pts',(25.0501560580419,0.548142172272313,3.17579245566781));
#70818=CARTESIAN_POINT('Ctrl Pts',(25.0563199466945,0.450049314189568,3.19272329515574));
#70819=CARTESIAN_POINT('Ctrl Pts',(25.0624838353471,0.35103146490954,3.20512921747368));
#70820=CARTESIAN_POINT('Ctrl Pts',(25.0686477239998,0.251541981600455,3.21291832980431));
#70821=CARTESIAN_POINT('Ctrl Pts',(25.0748050856583,0.152157848550892,3.22069919417768));
#70822=CARTESIAN_POINT('Ctrl Pts',(25.0809624473169,0.0523035050232203,
3.22387293420183));
#70823=CARTESIAN_POINT('Ctrl Pts',(25.0871198089754,-0.0475594895811064,
3.22239905310481));
#70824=CARTESIAN_POINT('Ctrl Pts',(25.0932726731217,-0.147349541411322,
3.2209262485725));
#70825=CARTESIAN_POINT('Ctrl Pts',(25.099425537268,-0.247147798736351,3.21481257866312));
#70826=CARTESIAN_POINT('Ctrl Pts',(25.1055784014143,-0.346490517966515,
3.20406958155707));
#70827=CARTESIAN_POINT('Ctrl Pts',(25.1117289345509,-0.445795601252857,
3.19333065443057));
#70828=CARTESIAN_POINT('Ctrl Pts',(25.1178794676874,-0.544645057982626,
3.1779659315848));
#70829=CARTESIAN_POINT('Ctrl Pts',(25.1240300008239,-0.642578980517186,
3.15803891937663));
#70830=CARTESIAN_POINT('Ctrl Pts',(25.1301798490392,-0.740501997162669,
3.13811412623391));
#70831=CARTESIAN_POINT('Ctrl Pts',(25.1363296972544,-0.837509256657889,
3.11362814042592));
#70832=CARTESIAN_POINT('Ctrl Pts',(25.1424795454696,-0.933150773795894,
3.08469564071792));
#70833=CARTESIAN_POINT('Ctrl Pts',(25.1486303538487,-1.02880722325928,3.05575862383461));
#70834=CARTESIAN_POINT('Ctrl Pts',(25.1547811622278,-1.12309709102729,3.02237383992554));
#70835=CARTESIAN_POINT('Ctrl Pts',(25.160931970607,-1.21558626036452,2.98470561464829));
#70836=CARTESIAN_POINT('Ctrl Pts',(25.1670893569732,-1.30817434231957,2.94699710505669));
#70837=CARTESIAN_POINT('Ctrl Pts',(25.1732467433394,-1.39895747722821,2.90499617061417));
#70838=CARTESIAN_POINT('Ctrl Pts',(25.1794041297055,-1.48752234279973,2.8589149763803));
#70839=CARTESIAN_POINT('Ctrl Pts',(25.1855649524425,-1.57613663546532,2.81280806473009));
#70840=CARTESIAN_POINT('Ctrl Pts',(25.1917257751795,-1.66252981774675,2.76261657659059));
#70841=CARTESIAN_POINT('Ctrl Pts',(25.1978865979164,-1.74631578201306,2.70859719264274));
#70842=CARTESIAN_POINT('Ctrl Pts',(25.2040577208331,-1.83024182667576,2.65448749456194));
#70843=CARTESIAN_POINT('Ctrl Pts',(25.2102288437498,-1.91155159252995,2.59653736949879));
#70844=CARTESIAN_POINT('Ctrl Pts',(25.2163999666665,-1.98989029754131,2.53504520004101));
#70845=CARTESIAN_POINT('Ctrl Pts',(25.221095488612,-2.0494971330447,2.48825666008384));
#70846=CARTESIAN_POINT('Ctrl Pts',(25.2257910105576,-2.10738452960363,2.43941832528737));
#70847=CARTESIAN_POINT('Ctrl Pts',(25.2304865325031,-2.16341077510467,2.38867565413579));
#70848=CARTESIAN_POINT('Ctrl Pts',(25.2365666600861,-2.23595792206555,2.32297009081808));
#70849=CARTESIAN_POINT('Ctrl Pts',(25.2426467876691,-2.30565498701423,2.25382395116584));
#70850=CARTESIAN_POINT('Ctrl Pts',(25.248726915252,-2.37215020834902,2.18151803832325));
#70851=CARTESIAN_POINT('Ctrl Pts',(25.2548871875013,-2.43952193058788,2.1082590314582));
#70852=CARTESIAN_POINT('Ctrl Pts',(25.2610474597506,-2.50360638839096,2.03175658788883));
#70853=CARTESIAN_POINT('Ctrl Pts',(25.2672077319998,-2.56407194549882,1.95234541534174));
#70854=CARTESIAN_POINT('Ctrl Pts',(25.2732724589536,-2.62359968699002,1.87416590328558));
#70855=CARTESIAN_POINT('Ctrl Pts',(25.2793371859074,-2.67961968610552,1.79316760569218));
#70856=CARTESIAN_POINT('Ctrl Pts',(25.2854019128613,-2.73185329001641,1.70970616315392));
#70857=CARTESIAN_POINT('Ctrl Pts',(25.2914628587965,-2.78405432919192,1.62629675416471));
#70858=CARTESIAN_POINT('Ctrl Pts',(25.2975238047317,-2.83247342331725,1.54042762849967));
#70859=CARTESIAN_POINT('Ctrl Pts',(25.3035847506669,-2.87687433357412,1.45248464064942));
#70860=CARTESIAN_POINT('Ctrl Pts',(25.3096436515148,-2.92126026205435,1.36457132656472));
#70861=CARTESIAN_POINT('Ctrl Pts',(25.3157025523626,-2.96163049860683,1.27458594064752));
#70862=CARTESIAN_POINT('Ctrl Pts',(25.3217614532105,-2.99779459353714,1.18293919432044));
#70863=CARTESIAN_POINT('Ctrl Pts',(25.3279957862125,-3.03500580002009,1.08863886667117));
#70864=CARTESIAN_POINT('Ctrl Pts',(25.3342301192145,-3.0677633322663,0.992579940178667));
#70865=CARTESIAN_POINT('Ctrl Pts',(25.3404644522165,-3.09591328035451,0.8952309886418));
#70866=CARTESIAN_POINT('Ctrl Pts',(25.3465270595895,-3.12328783393962,0.800563528440829));
#70867=CARTESIAN_POINT('Ctrl Pts',(25.3525896669625,-3.14630527403118,0.704676649018005));
#70868=CARTESIAN_POINT('Ctrl Pts',(25.3586522743356,-3.16487541490557,0.608014120416877));
#70869=CARTESIAN_POINT('Ctrl Pts',(25.364972470152,-3.18423456509354,0.507244588220224));
#70870=CARTESIAN_POINT('Ctrl Pts',(25.3712926659685,-3.19876001937384,0.405632565462735));
#70871=CARTESIAN_POINT('Ctrl Pts',(25.3776128617849,-3.20840947697045,0.303687653002588));
#70872=CARTESIAN_POINT('Ctrl Pts',(25.3839330576014,-3.21805893456705,0.201742740542441));
#70873=CARTESIAN_POINT('Ctrl Pts',(25.3902532534178,-3.22283242446457,0.0994654874476783));
#70874=CARTESIAN_POINT('Ctrl Pts',(25.3965734492343,-3.22274892221719,-0.00263568737796789));
#70875=CARTESIAN_POINT('Ctrl Pts',(24.7182540045911,1.78943620997144,2.68030513429778));
#70876=CARTESIAN_POINT('Ctrl Pts',(24.7222453478997,1.73195847831639,2.71867865116884));
#70877=CARTESIAN_POINT('Ctrl Pts',(24.726288389885,1.67326334016704,2.75519200731721));
#70878=CARTESIAN_POINT('Ctrl Pts',(24.7330617147449,1.57466108917989,2.81221744338375));
#70879=CARTESIAN_POINT('Ctrl Pts',(24.7357526037413,1.53541891685696,2.83383361232678));
#70880=CARTESIAN_POINT('Ctrl Pts',(24.7392573642564,1.48429630346652,2.86062038174631));
#70881=CARTESIAN_POINT('Ctrl Pts',(24.7400443197473,1.47281643318138,2.86654778984984));
#70882=CARTESIAN_POINT('Ctrl Pts',(24.7413195042604,1.45421492987351,2.87601107694878));
#70883=CARTESIAN_POINT('Ctrl Pts',(24.7418062160466,1.44711523299443,2.87958994956608));
#70884=CARTESIAN_POINT('Ctrl Pts',(24.7427376194432,1.43352948044272,2.88637543331099));
#70885=CARTESIAN_POINT('Ctrl Pts',(24.7431821494981,1.42704571908599,2.88958654959459));
#70886=CARTESIAN_POINT('Ctrl Pts',(24.7442017171333,1.41217573494316,2.89688873130772));
#70887=CARTESIAN_POINT('Ctrl Pts',(24.7447772584621,1.40378247750127,2.90096524985512));
#70888=CARTESIAN_POINT('Ctrl Pts',(24.7465553994281,1.37785486583098,2.91341915367981));
#70889=CARTESIAN_POINT('Ctrl Pts',(24.7477622288225,1.36026260047563,2.92167431919034));
#70890=CARTESIAN_POINT('Ctrl Pts',(24.7586252128972,1.20197652185344,2.99421053964749));
#70891=CARTESIAN_POINT('Ctrl Pts',(24.7686273519858,1.05692070616148,3.04843407564396));
#70892=CARTESIAN_POINT('Ctrl Pts',(24.788281423995,0.772754196078471,3.13193255696457));
#70893=CARTESIAN_POINT('Ctrl Pts',(24.7978676326064,0.634482763091523,3.16284333564088));
#70894=CARTESIAN_POINT('Ctrl Pts',(24.8154557588334,0.377637103319876,3.2027374071815));
#70895=CARTESIAN_POINT('Ctrl Pts',(24.8234452104858,0.259718266130523,3.21444960419365));
#70896=CARTESIAN_POINT('Ctrl Pts',(24.8343875948278,0.0935378356830638,
3.22174875478681));
#70897=CARTESIAN_POINT('Ctrl Pts',(24.8375057453881,0.0456153291802165,
3.22278359779733));
#70898=CARTESIAN_POINT('Ctrl Pts',(24.8423333836376,-0.0297538041632178,
3.22272945871833));
#70899=CARTESIAN_POINT('Ctrl Pts',(24.844074983371,-0.0571923855762873,
3.22235932262176));
#70900=CARTESIAN_POINT('Ctrl Pts',(24.846266308942,-0.0920799727126928,
3.22144291763584));
#70901=CARTESIAN_POINT('Ctrl Pts',(24.8467332486345,-0.0995353699431762,
3.22122118236531));
#70902=CARTESIAN_POINT('Ctrl Pts',(24.847478614483,-0.111471720943126,3.22082469652651));
#70903=CARTESIAN_POINT('Ctrl Pts',(24.847757955557,-0.115953141308101,3.22066647449443));
#70904=CARTESIAN_POINT('Ctrl Pts',(24.8482886494012,-0.124482584165218,
3.22034750619765));
#70905=CARTESIAN_POINT('Ctrl Pts',(24.8485400924167,-0.128530585015484,
3.22018848257395));
#70906=CARTESIAN_POINT('Ctrl Pts',(24.849116672788,-0.137828274936922,3.21980566768868));
#70907=CARTESIAN_POINT('Ctrl Pts',(24.8494415145162,-0.1430777186857,3.21957667068159));
#70908=CARTESIAN_POINT('Ctrl Pts',(24.8504698776396,-0.159730563815079,
3.21880941272033));
#70909=CARTESIAN_POINT('Ctrl Pts',(24.8511707641062,-0.171131831573002,
3.21822339090448));
#70910=CARTESIAN_POINT('Ctrl Pts',(24.857843494033,-0.28013752918202,3.21203960568476));
#70911=CARTESIAN_POINT('Ctrl Pts',(24.8635837676913,-0.3774534862739,3.20206315653621));
#70912=CARTESIAN_POINT('Ctrl Pts',(24.8779271558124,-0.624308795738743,
3.16534279914013));
#70913=CARTESIAN_POINT('Ctrl Pts',(24.886348299795,-0.772685107795609,3.13243021670104));
#70914=CARTESIAN_POINT('Ctrl Pts',(24.9075991693126,-1.13687318358235,3.02418280067591));
#70915=CARTESIAN_POINT('Ctrl Pts',(24.920496757803,-1.34799813346745,2.93616128672216));
#70916=CARTESIAN_POINT('Ctrl Pts',(24.9356406438767,-1.56849676741873,2.81540031751905));
#70917=CARTESIAN_POINT('Ctrl Pts',(24.9370526181426,-1.58882149121871,2.80398061376712));
#70918=CARTESIAN_POINT('Ctrl Pts',(24.9390845250058,-1.6177263288978,2.78732489188102));
#70919=CARTESIAN_POINT('Ctrl Pts',(24.9396979981633,-1.62640894071049,2.78226750728392));
#70920=CARTESIAN_POINT('Ctrl Pts',(24.9407626159442,-1.64139925088342,2.77344191329835));
#70921=CARTESIAN_POINT('Ctrl Pts',(24.9412130713828,-1.64771801062409,2.76969256476));
#70922=CARTESIAN_POINT('Ctrl Pts',(24.9420792696397,-1.6598225302669,2.76245405021316));
#70923=CARTESIAN_POINT('Ctrl Pts',(24.9424948882769,-1.66561025368352,2.75896822983439));
#70924=CARTESIAN_POINT('Ctrl Pts',(24.9434739272598,-1.67919604927818,2.75072746922713));
#70925=CARTESIAN_POINT('Ctrl Pts',(24.9440378967102,-1.68698492373811,2.74595754632112));
#70926=CARTESIAN_POINT('Ctrl Pts',(24.9457050024538,-1.70989883212784,2.73179073397694));
#70927=CARTESIAN_POINT('Ctrl Pts',(24.9468115399456,-1.72496619371148,2.7223016439022));
#70928=CARTESIAN_POINT('Ctrl Pts',(24.9621143667602,-1.93137195359057,2.58991027985836));
#70929=CARTESIAN_POINT('Ctrl Pts',(24.9770908606751,-2.10921811592356,2.44724207780335));
#70930=CARTESIAN_POINT('Ctrl Pts',(25.0031998477566,-2.38399683153424,2.17445030253602));
#70931=CARTESIAN_POINT('Ctrl Pts',(25.0140993626502,-2.48891221880105,2.05353172791189));
#70932=CARTESIAN_POINT('Ctrl Pts',(25.0291588087393,-2.62420386046175,1.87192568433355));
#70933=CARTESIAN_POINT('Ctrl Pts',(25.0335349463593,-2.66232351270553,1.81730195120155));
#70934=CARTESIAN_POINT('Ctrl Pts',(25.040052546099,-2.7176450009886,1.73254763200282));
#70935=CARTESIAN_POINT('Ctrl Pts',(25.0422574210526,-2.73609718565112,1.70325807623763));
#70936=CARTESIAN_POINT('Ctrl Pts',(25.0449396243877,-2.75826198244533,1.66678535087545));
#70937=CARTESIAN_POINT('Ctrl Pts',(25.0454447242568,-2.76242338031803,1.65987940552182));
#70938=CARTESIAN_POINT('Ctrl Pts',(25.0462365309591,-2.76892779018727,1.64899296153188));
#70939=CARTESIAN_POINT('Ctrl Pts',(25.0465243595754,-2.77128820231631,1.6450229769809));
#70940=CARTESIAN_POINT('Ctrl Pts',(25.0470619332851,-2.77568938356153,1.637584258875));
#70941=CARTESIAN_POINT('Ctrl Pts',(25.0473118066221,-2.77773216749669,1.63411681492495));
#70942=CARTESIAN_POINT('Ctrl Pts',(25.0478782409987,-2.78235611130064,1.62623435775113));
#70943=CARTESIAN_POINT('Ctrl Pts',(25.04819453858,-2.78493325409513,1.62181703268784));
#70944=CARTESIAN_POINT('Ctrl Pts',(25.0491314597365,-2.79255217783527,1.60868618458253));
#70945=CARTESIAN_POINT('Ctrl Pts',(25.0497501498006,-2.7975637150224,1.59995505345611));
#70946=CARTESIAN_POINT('Ctrl Pts',(25.0541255827295,-2.83285774181815,1.53779272684827));
#70947=CARTESIAN_POINT('Ctrl Pts',(25.0577916787118,-2.86165063451717,1.48352494475262));
#70948=CARTESIAN_POINT('Ctrl Pts',(25.0621731504623,-2.89477254502612,1.41654028961094));
#70949=CARTESIAN_POINT('Ctrl Pts',(25.0629499656765,-2.9005943415028,1.40458070422258));
#70950=CARTESIAN_POINT('Ctrl Pts',(25.0813416713987,-3.03716455158955,1.11955705259713));
#70951=CARTESIAN_POINT('Ctrl Pts',(25.0975625961353,-3.12887064671542,0.829444519254396));
#70952=CARTESIAN_POINT('Ctrl Pts',(25.1192993635644,-3.19098294448296,0.457460293207525));
#70953=CARTESIAN_POINT('Ctrl Pts',(25.1236415852499,-3.20068368918857,0.383751007075289));
#70954=CARTESIAN_POINT('Ctrl Pts',(25.1298248044528,-3.21067933504703,0.280242928708544));
#70955=CARTESIAN_POINT('Ctrl Pts',(25.1316008331804,-3.21312324285893,0.250672757106428));
#70956=CARTESIAN_POINT('Ctrl Pts',(25.1347248287541,-3.2166779631481,0.198975130198541));
#70957=CARTESIAN_POINT('Ctrl Pts',(25.1360671343093,-3.21796955658273,0.176861856212914));
#70958=CARTESIAN_POINT('Ctrl Pts',(25.138016176275,-3.21950560520608,0.144907138208664));
#70959=CARTESIAN_POINT('Ctrl Pts',(25.1386171641455,-3.2199331069566,0.135074808901856));
#70960=CARTESIAN_POINT('Ctrl Pts',(25.1396671257129,-3.22059970874648,0.117934477711819));
#70961=CARTESIAN_POINT('Ctrl Pts',(25.1401154625857,-3.22085898864512,0.110627297157542));
#70962=CARTESIAN_POINT('Ctrl Pts',(25.1409826345581,-3.22131159178143,0.0965169001719425));
#70963=CARTESIAN_POINT('Ctrl Pts',(25.141401362908,-3.22150823561545,0.0897138233030848));
#70964=CARTESIAN_POINT('Ctrl Pts',(25.1423955790047,-3.2219232940922,0.0735856904937968));
#70965=CARTESIAN_POINT('Ctrl Pts',(25.1429716583337,-3.22212277615162,0.0642602468846168));
#70966=CARTESIAN_POINT('Ctrl Pts',(25.1446985126069,-3.22259832038217,0.0363661664544118));
#70967=CARTESIAN_POINT('Ctrl Pts',(25.14585304091,-3.2227543666048,0.0177961188830445));
#70968=CARTESIAN_POINT('Ctrl Pts',(25.1588113358357,-3.22270453128891,-0.189724329190089));
#70969=CARTESIAN_POINT('Ctrl Pts',(25.1711411472812,-3.20604255472005,-0.378270519167828));
#70970=CARTESIAN_POINT('Ctrl Pts',(25.1948083481093,-3.14417735314071,-0.726163397843209));
#70971=CARTESIAN_POINT('Ctrl Pts',(25.2060257990343,-3.10303275788517,-0.885635309103736));
#70972=CARTESIAN_POINT('Ctrl Pts',(25.2222300880156,-3.02503908865167,-1.11408070860695));
#70973=CARTESIAN_POINT('Ctrl Pts',(25.2273481028799,-2.99757872940744,-1.18598504394425));
#70974=CARTESIAN_POINT('Ctrl Pts',(25.2358734473504,-2.94660105045497,-1.3063500994954));
#70975=CARTESIAN_POINT('Ctrl Pts',(25.2393302040369,-2.92439567788134,-1.35532987529683));
#70976=CARTESIAN_POINT('Ctrl Pts',(25.2432736179026,-2.897127965109,-1.41168164410416));
#70977=CARTESIAN_POINT('Ctrl Pts',(25.2438278675962,-2.89324969933732,-1.41961321918727));
#70978=CARTESIAN_POINT('Ctrl Pts',(25.2447100024149,-2.88700291640514,-1.43225679716575));
#70979=CARTESIAN_POINT('Ctrl Pts',(25.2450391598449,-2.88465537686563,-1.43697902908275));
#70980=CARTESIAN_POINT('Ctrl Pts',(25.2456200589769,-2.88048274037477,-1.44532113343865));
#70981=CARTESIAN_POINT('Ctrl Pts',(25.2458720965956,-2.87866239267388,-1.44894334813071));
#70982=CARTESIAN_POINT('Ctrl Pts',(25.246401389914,-2.87481853156797,-1.45655620978659));
#70983=CARTESIAN_POINT('Ctrl Pts',(25.2466785504567,-2.87279354638554,-1.46054606984546));
#70984=CARTESIAN_POINT('Ctrl Pts',(25.247413610099,-2.86739090291708,-1.47113627678832));
#70985=CARTESIAN_POINT('Ctrl Pts',(25.2478706016622,-2.86399874080965,-1.47772925470652));
#70986=CARTESIAN_POINT('Ctrl Pts',(25.2499838971357,-2.84815921112237,-1.50825541547001));
#70987=CARTESIAN_POINT('Ctrl Pts',(25.2516232792896,-2.83543396556172,-1.53204426475609));
#70988=CARTESIAN_POINT('Ctrl Pts',(25.2560638194022,-2.79981448791345,-1.59666768377218));
#70989=CARTESIAN_POINT('Ctrl Pts',(25.2588325397859,-2.7763261925034,-1.63716895839225));
#70990=CARTESIAN_POINT('Ctrl Pts',(25.2682361255484,-2.69249802684546,-1.77471926813515));
#70991=CARTESIAN_POINT('Ctrl Pts',(25.2746888741484,-2.62788189543982,-1.86906780491483));
#70992=CARTESIAN_POINT('Ctrl Pts',(25.2969891978706,-2.38595905922603,-2.1848833116506));
#70993=CARTESIAN_POINT('Ctrl Pts',(25.3126208656007,-2.18460500275352,-2.38621041631845));
#70994=CARTESIAN_POINT('Ctrl Pts',(25.3306660999574,-1.94532532248448,-2.56946423624707));
#70995=CARTESIAN_POINT('Ctrl Pts',(25.3317407405264,-1.93104424527404,-2.58021417233837));
#70996=CARTESIAN_POINT('Ctrl Pts',(25.3340123029492,-1.90079862210402,-2.60258950920599));
#70997=CARTESIAN_POINT('Ctrl Pts',(25.335210183852,-1.88481521413602,-2.6141880454436));
#70998=CARTESIAN_POINT('Ctrl Pts',(25.3369885531623,-1.86104268936345,-2.63110748899963));
#70999=CARTESIAN_POINT('Ctrl Pts',(25.3375646470591,-1.85333498710995,-2.63654242007956));
#71000=CARTESIAN_POINT('Ctrl Pts',(25.3385872694928,-1.83964190586644,-2.64610810575319));
#71001=CARTESIAN_POINT('Ctrl Pts',(25.3390332683808,-1.83366616785781,-2.65025259789132));
#71002=CARTESIAN_POINT('Ctrl Pts',(25.3399610100135,-1.82122836919245,-2.65881666920786));
#71003=CARTESIAN_POINT('Ctrl Pts',(25.3404428726232,-1.81476413581595,-2.66323299447073));
#71004=CARTESIAN_POINT('Ctrl Pts',(25.3416885092651,-1.79804367037382,-2.67456717410993));
#71005=CARTESIAN_POINT('Ctrl Pts',(25.3424536185682,-1.78776365298968,-2.68144955641355));
#71006=CARTESIAN_POINT('Ctrl Pts',(25.3456858069415,-1.74429772470826,-2.71018855878836));
#71007=CARTESIAN_POINT('Ctrl Pts',(25.3481735967792,-1.71074983346264,-2.73148885335003));
#71008=CARTESIAN_POINT('Ctrl Pts',(25.368834892233,-1.43150596834491,-2.90162454436661));
#71009=CARTESIAN_POINT('Ctrl Pts',(25.3882605961333,-1.16735440949385,-3.01759018957438));
#71010=CARTESIAN_POINT('Ctrl Pts',(25.4130141012399,-0.815356616330881,
-3.11890616710155));
#71011=CARTESIAN_POINT('Ctrl Pts',(25.4183412625889,-0.738512094248152,
-3.13799027241118));
#71012=CARTESIAN_POINT('Ctrl Pts',(25.429573830687,-0.57284046609421,-3.17271054874872));
#71013=CARTESIAN_POINT('Ctrl Pts',(25.4354525674215,-0.483894699489564,
-3.18748924563328));
#71014=CARTESIAN_POINT('Ctrl Pts',(25.4418484224756,-0.38329620050824,-3.199894937584));
#71015=CARTESIAN_POINT('Ctrl Pts',(25.4425537732969,-0.372147153933057,
-3.20121072306947));
#71016=CARTESIAN_POINT('Ctrl Pts',(25.443582308523,-0.355805555300184,-3.20305279422941));
#71017=CARTESIAN_POINT('Ctrl Pts',(25.443908002188,-0.350618387654371,-3.20362475064689));
#71018=CARTESIAN_POINT('Ctrl Pts',(25.4444849497941,-0.341406985708713,
-3.20461779371705));
#71019=CARTESIAN_POINT('Ctrl Pts',(25.4447364860416,-0.337383325332505,
-3.205043903942));
#71020=CARTESIAN_POINT('Ctrl Pts',(25.445267062303,-0.328879618075118,-3.20592826486408));
#71021=CARTESIAN_POINT('Ctrl Pts',(25.4455459985672,-0.324399423301787,
-3.20638470202705));
#71022=CARTESIAN_POINT('Ctrl Pts',(25.4462908201649,-0.312411147834194,
-3.20758067002698));
#71023=CARTESIAN_POINT('Ctrl Pts',(25.4467557547441,-0.304901346314265,
-3.20830323562666));
#71024=CARTESIAN_POINT('Ctrl Pts',(25.4489614789434,-0.269152135997372,
-3.21161623760856));
#71025=CARTESIAN_POINT('Ctrl Pts',(25.4506834914283,-0.240880835208396,
-3.2138603396312));
#71026=CARTESIAN_POINT('Ctrl Pts',(25.4671451210339,0.0323950907180704,
-3.23192580310718));
#71027=CARTESIAN_POINT('Ctrl Pts',(25.4805872982264,0.278457756224323,-3.22007624882055));
#71028=CARTESIAN_POINT('Ctrl Pts',(25.500139552909,0.622799386095099,-3.16368743775459));
#71029=CARTESIAN_POINT('Ctrl Pts',(25.5059679258127,0.723917063142524,-3.14209160832866));
#71030=CARTESIAN_POINT('Ctrl Pts',(25.5127692398958,0.838192825270334,-3.11187586838479));
#71031=CARTESIAN_POINT('Ctrl Pts',(25.5136270518064,0.852540647959471,-3.1079757186906));
#71032=CARTESIAN_POINT('Ctrl Pts',(25.5159540479529,0.891275380439016,-3.09715810358835));
#71033=CARTESIAN_POINT('Ctrl Pts',(25.5174278753743,0.91560819202678,-3.09005205729914));
#71034=CARTESIAN_POINT('Ctrl Pts',(25.5234412026339,1.01400470287881,-3.06005251711778));
#71035=CARTESIAN_POINT('Ctrl Pts',(25.5280456936087,1.08731022428053,-3.03477873125652));
#71036=CARTESIAN_POINT('Ctrl Pts',(25.5336283849449,1.17333854641769,-3.00160125886792));
#71037=CARTESIAN_POINT('Ctrl Pts',(25.5345211155486,1.18701137817151,-2.99622052571694));
#71038=CARTESIAN_POINT('Ctrl Pts',(25.5359797584074,1.20921225452993,-2.98730789808527));
#71039=CARTESIAN_POINT('Ctrl Pts',(25.5365437613093,1.21776286347696,-2.98383249530038));
#71040=CARTESIAN_POINT('Ctrl Pts',(25.5375513488446,1.23297789515737,-2.97757203817173));
#71041=CARTESIAN_POINT('Ctrl Pts',(25.5379944481783,1.23964813290859,-2.97480120977447));
#71042=CARTESIAN_POINT('Ctrl Pts',(25.538930188915,1.2536903119907,-2.96891263425015));
#71043=CARTESIAN_POINT('Ctrl Pts',(25.5394230011528,1.26106005622917,-2.96578980390144));
#71044=CARTESIAN_POINT('Ctrl Pts',(25.5407285237656,1.28051519819183,-2.95746032190452));
#71045=CARTESIAN_POINT('Ctrl Pts',(25.5415428221267,1.2925803759799,-2.95220708823341));
#71046=CARTESIAN_POINT('Ctrl Pts',(25.5452892666182,1.3477676398697,-2.9277751425098));
#71047=CARTESIAN_POINT('Ctrl Pts',(25.5482512272447,1.3904955335118,-2.90772534571724));
#71048=CARTESIAN_POINT('Ctrl Pts',(25.5562855378268,1.50392941754613,-2.85142519024847));
#71049=CARTESIAN_POINT('Ctrl Pts',(25.5614144515166,1.57375712934127,-2.81348824446929));
#71050=CARTESIAN_POINT('Ctrl Pts',(25.5885625509803,1.93024461063403,-2.60238543815831));
#71051=CARTESIAN_POINT('Ctrl Pts',(25.6119709556168,2.18997949478353,-2.38792771561801));
#71052=CARTESIAN_POINT('Ctrl Pts',(25.6360031766948,2.43687159193019,-2.10930755518569));
#71053=CARTESIAN_POINT('Ctrl Pts',(25.6383945613085,2.46123192761313,-2.08083137479053));
#71054=CARTESIAN_POINT('Ctrl Pts',(25.6412462957966,2.49009690997284,-2.04587310177126));
#71055=CARTESIAN_POINT('Ctrl Pts',(25.6417393133049,2.49508037368628,-2.03979246530145));
#71056=CARTESIAN_POINT('Ctrl Pts',(25.6425456579893,2.50322064080885,-2.02978554654503));
#71057=CARTESIAN_POINT('Ctrl Pts',(25.6428599136691,2.50639054221406,-2.02587003340791));
#71058=CARTESIAN_POINT('Ctrl Pts',(25.6434236290191,2.51207232690855,-2.01881805354956));
#71059=CARTESIAN_POINT('Ctrl Pts',(25.6436733270412,2.51458752485737,-2.0156843228451));
#71060=CARTESIAN_POINT('Ctrl Pts',(25.6442124730355,2.52001498841045,-2.00889617849284));
#71061=CARTESIAN_POINT('Ctrl Pts',(25.6445017700227,2.52292515810312,-2.00524014647778));
#71062=CARTESIAN_POINT('Ctrl Pts',(25.6453038768717,2.53098760521193,-1.9950659978529));
#71063=CARTESIAN_POINT('Ctrl Pts',(25.6458154654982,2.53612268862311,-1.98853421025533));
#71064=CARTESIAN_POINT('Ctrl Pts',(25.6486619244838,2.5646491520489,-1.95195852169992));
#71065=CARTESIAN_POINT('Ctrl Pts',(25.6509622826641,2.58753308149023,-1.92152028296286));
#71066=CARTESIAN_POINT('Ctrl Pts',(25.6683877347154,2.75895266873513,-1.68489487662805));
#71067=CARTESIAN_POINT('Ctrl Pts',(25.6822241054221,2.88318962624129,-1.4621707869376));
#71068=CARTESIAN_POINT('Ctrl Pts',(25.7075109593749,3.05449218316946,-1.04618029976341));
#71069=CARTESIAN_POINT('Ctrl Pts',(25.7187183295096,3.11236148238462,-0.858839695299414));
#71070=CARTESIAN_POINT('Ctrl Pts',(25.7316159962583,3.15659880698721,-0.649864350481781));
#71071=CARTESIAN_POINT('Ctrl Pts',(25.7327042893211,3.16016903462346,-0.632274746273916));
#71072=CARTESIAN_POINT('Ctrl Pts',(25.7343556834629,3.16534098225953,-0.605655110023139));
#71073=CARTESIAN_POINT('Ctrl Pts',(25.7349153148007,3.16705143007519,-0.596646363263539));
#71074=CARTESIAN_POINT('Ctrl Pts',(25.7358899889036,3.16995701321921,-0.58097837276057));
#71075=CARTESIAN_POINT('Ctrl Pts',(25.7363044702751,3.17116967506644,-0.574322406062973));
#71076=CARTESIAN_POINT('Ctrl Pts',(25.7371700437387,3.17365429695081,-0.560437191614757));
#71077=CARTESIAN_POINT('Ctrl Pts',(25.7376212517982,3.17492253391829,-0.553207325056425));
#71078=CARTESIAN_POINT('Ctrl Pts',(25.7386895103552,3.17786148398446,-0.536110162028866));
#71079=CARTESIAN_POINT('Ctrl Pts',(25.7393072331797,3.17951094924722,-0.526239334540342));
#71080=CARTESIAN_POINT('Ctrl Pts',(25.7413545925632,3.18481274392778,-0.493576889058274));
#71081=CARTESIAN_POINT('Ctrl Pts',(25.7427905248514,3.18826612273365,-0.470754123963716));
#71082=CARTESIAN_POINT('Ctrl Pts',(25.7589760372603,3.22422897353678,-0.214501952103334));
#71083=CARTESIAN_POINT('Ctrl Pts',(25.7745627122902,3.23127677550765,0.0217340357278075));
#71084=CARTESIAN_POINT('Ctrl Pts',(25.7988741158303,3.20261910010179,0.3805437024416));
#71085=CARTESIAN_POINT('Ctrl Pts',(25.8073275007937,3.18555130897384,0.50383153661494));
#71086=CARTESIAN_POINT('Ctrl Pts',(25.8185247861165,3.15307712849567,0.667877081081072));
#71087=CARTESIAN_POINT('Ctrl Pts',(25.8213784835601,3.1439142465915,0.70975955228662));
#71088=CARTESIAN_POINT('Ctrl Pts',(25.8257350381447,3.12851590505007,0.773978422217284));
#71089=CARTESIAN_POINT('Ctrl Pts',(25.8272558795155,3.12287065136274,0.796450445278329));
#71090=CARTESIAN_POINT('Ctrl Pts',(25.8323186807997,3.10315441822898,0.871500100214371));
#71091=CARTESIAN_POINT('Ctrl Pts',(25.8358188808968,3.08799313335904,0.92378516090376));
#71092=CARTESIAN_POINT('Ctrl Pts',(25.8398061516744,3.0688308258754,0.984110489091247));
#71093=CARTESIAN_POINT('Ctrl Pts',(25.840362486052,3.06611314154838,0.992545364274838));
#71094=CARTESIAN_POINT('Ctrl Pts',(25.841247301742,3.06171974272827,1.00599090016046));
#71095=CARTESIAN_POINT('Ctrl Pts',(25.8415770673611,3.06006646285892,1.01100876259951));
#71096=CARTESIAN_POINT('Ctrl Pts',(25.8421586636162,3.05712234576144,1.01987105599639));
#71097=CARTESIAN_POINT('Ctrl Pts',(25.8424107925584,3.0558365830291,1.0237171417742));
#71098=CARTESIAN_POINT('Ctrl Pts',(25.8429398761243,3.05311850048225,1.03179695670407));
#71099=CARTESIAN_POINT('Ctrl Pts',(25.8432167370596,3.05168463605442,1.03603012528558));
#71100=CARTESIAN_POINT('Ctrl Pts',(25.8439501500001,3.0478557880578,1.04725703887878));
#71101=CARTESIAN_POINT('Ctrl Pts',(25.8444058016789,3.0454455219901,1.05424560013657));
#71102=CARTESIAN_POINT('Ctrl Pts',(25.8465039069506,3.03420264698613,1.08648397181839));
#71103=CARTESIAN_POINT('Ctrl Pts',(25.8481297338543,3.02507961861375,1.11163237375532));
#71104=CARTESIAN_POINT('Ctrl Pts',(25.8627208722192,2.93957878251326,1.33847145927029));
#71105=CARTESIAN_POINT('Ctrl Pts',(25.8746715512404,2.84343683712916,1.53216282296315));
#71106=CARTESIAN_POINT('Ctrl Pts',(25.9005871819413,2.596705524906,1.92476656642778));
#71107=CARTESIAN_POINT('Ctrl Pts',(25.9145434327586,2.44099546647484,2.1187552258836));
#71108=CARTESIAN_POINT('Ctrl Pts',(25.9306928394981,2.25076808839353,2.30662926390878));
#71109=CARTESIAN_POINT('Ctrl Pts',(25.9318725394989,2.23681221168371,2.32016522102951));
#71110=CARTESIAN_POINT('Ctrl Pts',(25.9336266998634,2.21597722546849,2.34001059767379));
#71111=CARTESIAN_POINT('Ctrl Pts',(25.934196912783,2.20919163218262,2.34641790617689));
#71112=CARTESIAN_POINT('Ctrl Pts',(25.9352114778584,2.19709593793012,2.35774030719268));
#71113=CARTESIAN_POINT('Ctrl Pts',(25.9356553195539,2.19179691339331,2.36266718047914));
#71114=CARTESIAN_POINT('Ctrl Pts',(25.936588429857,2.18064105876955,2.37296972915166));
#71115=CARTESIAN_POINT('Ctrl Pts',(25.9370778539771,2.17478084660683,2.37834165545747));
#71116=CARTESIAN_POINT('Ctrl Pts',(25.9383648694412,2.15934774873143,2.39238409969114));
#71117=CARTESIAN_POINT('Ctrl Pts',(25.9391639688925,2.14974258393941,2.40101878280846));
#71118=CARTESIAN_POINT('Ctrl Pts',(25.9427433305337,2.10662002080281,2.43931815410813));
#71119=CARTESIAN_POINT('Ctrl Pts',(25.9455502546513,2.07254002768217,2.46833921436925));
#71120=CARTESIAN_POINT('Ctrl Pts',(25.9530689124994,1.98061180210791,2.54337509983254));
#71121=CARTESIAN_POINT('Ctrl Pts',(25.957828700725,1.92176880674521,2.5881235048462));
#71122=CARTESIAN_POINT('Ctrl Pts',(25.9645599125487,1.83765515169878,2.64763862344991));
#71123=CARTESIAN_POINT('Ctrl Pts',(25.9664728856645,1.81365036753495,2.66413918124719));
#71124=CARTESIAN_POINT('Ctrl Pts',(25.9683941809562,1.78943611353999,2.68030519867773));
#71125=CARTESIAN_POINT('Origin',(-1.72497344927317,0.,0.));
#71126=CARTESIAN_POINT('',(27.4670789411482,1.78943621037803,2.68030513402633));
#71127=CARTESIAN_POINT('',(27.2231721927303,1.78943620958681,2.68030513455457));
#71128=CARTESIAN_POINT('',(-1.72497344927317,1.78943621037804,2.68030513402633));
#71129=CARTESIAN_POINT('',(26.6465734493259,-3.22274928133509,0.00215224399016846));
#71130=CARTESIAN_POINT('Ctrl Pts',(26.6465734493259,-3.22274928133509,0.00215224399017275));
#71131=CARTESIAN_POINT('Ctrl Pts',(26.6526554760797,-3.222814805559,-0.0959630935353457));
#71132=CARTESIAN_POINT('Ctrl Pts',(26.6587375028335,-3.218395510171,-0.194255137665291));
#71133=CARTESIAN_POINT('Ctrl Pts',(26.6648195295873,-3.20946944460621,-0.292272897544588));
#71134=CARTESIAN_POINT('Ctrl Pts',(26.6708944080508,-3.20055386996977,-0.390175455794581));
#71135=CARTESIAN_POINT('Ctrl Pts',(26.6769692865144,-3.1871420880131,-0.487803927892748));
#71136=CARTESIAN_POINT('Ctrl Pts',(26.683044164978,-3.16926418034635,-0.584706864739565));
#71137=CARTESIAN_POINT('Ctrl Pts',(26.6891138244146,-3.1514016318813,-0.681526550694873));
#71138=CARTESIAN_POINT('Ctrl Pts',(26.6951834838511,-3.12908066328959,-0.777621501811903));
#71139=CARTESIAN_POINT('Ctrl Pts',(26.7012531432877,-3.10238310089514,-0.872546077740451));
#71140=CARTESIAN_POINT('Ctrl Pts',(26.7073200794118,-3.07569751706474,-0.967428063259591));
#71141=CARTESIAN_POINT('Ctrl Pts',(26.7133870155359,-3.04463935925051,-1.06114028614752));
#71142=CARTESIAN_POINT('Ctrl Pts',(26.71945395166,-3.00934118336634,-1.15324897771264));
#71143=CARTESIAN_POINT('Ctrl Pts',(26.7255198934566,-2.97404879260072,-1.24534257332207));
#71144=CARTESIAN_POINT('Ctrl Pts',(26.7315858352533,-2.93451792458771,-1.33583274197713));
#71145=CARTESIAN_POINT('Ctrl Pts',(26.7376517770499,-2.89093007270836,-1.42430364642179));
#71146=CARTESIAN_POINT('Ctrl Pts',(26.7437184522027,-2.84733695117416,-1.51278524676247));
#71147=CARTESIAN_POINT('Ctrl Pts',(26.7497851273556,-2.79968607092538,-1.59924669734376));
#71148=CARTESIAN_POINT('Ctrl Pts',(26.7558518025084,-2.74820532985199,-1.68329588233119));
#71149=CARTESIAN_POINT('Ctrl Pts',(26.7619246713544,-2.69667203018429,-1.76743087624295));
#71150=CARTESIAN_POINT('Ctrl Pts',(26.7679975402005,-2.64130129923939,-1.84914830658508));
#71151=CARTESIAN_POINT('Ctrl Pts',(26.7740704090465,-2.58236471881335,-1.92808454729767));
#71152=CARTESIAN_POINT('Ctrl Pts',(26.7801466663091,-2.52339525414657,-2.0070648312568));
#71153=CARTESIAN_POINT('Ctrl Pts',(26.7862229235716,-2.46085626542934,-2.08326049281699));
#71154=CARTESIAN_POINT('Ctrl Pts',(26.7922991808342,-2.39505859088021,-2.15634225222966));
#71155=CARTESIAN_POINT('Ctrl Pts',(26.7983851600855,-2.32915564029945,-2.22954094218233));
#71156=CARTESIAN_POINT('Ctrl Pts',(26.8044711393368,-2.25998391095859,-2.2996154677175));
#71157=CARTESIAN_POINT('Ctrl Pts',(26.8105571185881,-2.18788977991652,-2.36627468258375));
#71158=CARTESIAN_POINT('Ctrl Pts',(26.8141261731988,-2.1456109813574,-2.40536623520674));
#71159=CARTESIAN_POINT('Ctrl Pts',(26.8176952278095,-2.10232775368222,-2.44328399756727));
#71160=CARTESIAN_POINT('Ctrl Pts',(26.8212642824202,-2.05811463398499,-2.47997615227986));
#71161=CARTESIAN_POINT('Ctrl Pts',(26.827436530513,-1.9816533932666,-2.54343079409588));
#71162=CARTESIAN_POINT('Ctrl Pts',(26.8336087786058,-1.90212022575668,-2.60345769436343));
#71163=CARTESIAN_POINT('Ctrl Pts',(26.8397810266985,-1.81985545862044,-2.65974503895193));
#71164=CARTESIAN_POINT('Ctrl Pts',(26.8459449153511,-1.73770210751716,-2.71595615026513));
#71165=CARTESIAN_POINT('Ctrl Pts',(26.8521088040038,-1.65282486541836,-2.76843752942246));
#71166=CARTESIAN_POINT('Ctrl Pts',(26.8582726926564,-1.56559774479115,-2.81691697854318));
#71167=CARTESIAN_POINT('Ctrl Pts',(26.8644300543149,-1.4784629897034,-2.86534509236316));
#71168=CARTESIAN_POINT('Ctrl Pts',(26.8705874159735,-1.38898368065712,-2.90977949119602));
#71169=CARTESIAN_POINT('Ctrl Pts',(26.876744777632,-1.29756267400655,-2.94999129990666));
#71170=CARTESIAN_POINT('Ctrl Pts',(26.8828976417783,-1.20620844386154,-2.99017373676758));
#71171=CARTESIAN_POINT('Ctrl Pts',(26.8890505059246,-1.11291573229104,-3.02613954125879));
#71172=CARTESIAN_POINT('Ctrl Pts',(26.8952033700709,-1.01811103303148,-3.05770624601507));
#71173=CARTESIAN_POINT('Ctrl Pts',(26.9013539032075,-0.923342250488869,
-3.08926099173969));
#71174=CARTESIAN_POINT('Ctrl Pts',(26.907504436344,-0.827063030111666,-3.11641981217568));
#71175=CARTESIAN_POINT('Ctrl Pts',(26.9136549694805,-0.729718000981313,
-3.13904909192957));
#71176=CARTESIAN_POINT('Ctrl Pts',(26.9198048176957,-0.632383812161213,
-3.16167585169435));
#71177=CARTESIAN_POINT('Ctrl Pts',(26.925954665911,-0.53398447365143,-3.17977397525972));
#71178=CARTESIAN_POINT('Ctrl Pts',(26.9321045141262,-0.434976884188812,
-3.19326050812041));
#71179=CARTESIAN_POINT('Ctrl Pts',(26.9382553225053,-0.335953836862382,
-3.20674914660743));
#71180=CARTESIAN_POINT('Ctrl Pts',(26.9444061308844,-0.236322780399072,
-3.2156247056528));
#71181=CARTESIAN_POINT('Ctrl Pts',(26.9505569392636,-0.136546841566313,
-3.21985597854287));
#71182=CARTESIAN_POINT('Ctrl Pts',(26.9567143256297,-0.0366641972741644,
-3.22409177657119));
#71183=CARTESIAN_POINT('Ctrl Pts',(26.9628717119959,0.0633632039644185,
-3.22367335174628));
#71184=CARTESIAN_POINT('Ctrl Pts',(26.9690290983621,0.163071238732657,-3.21862165120385));
#71185=CARTESIAN_POINT('Ctrl Pts',(26.9751899210991,0.262834919477191,-3.21356713136196));
#71186=CARTESIAN_POINT('Ctrl Pts',(26.981350743836,0.362278446458359,-3.20387422839628));
#71187=CARTESIAN_POINT('Ctrl Pts',(26.987511566573,0.460943920654126,-3.18961569229147));
#71188=CARTESIAN_POINT('Ctrl Pts',(26.9936826894897,0.559774352057922,-3.17533331757113));
#71189=CARTESIAN_POINT('Ctrl Pts',(26.9998538124063,0.65782370558901,-3.15647014471428));
#71190=CARTESIAN_POINT('Ctrl Pts',(27.006024935323,0.754645215550309,-3.13314987850039));
#71191=CARTESIAN_POINT('Ctrl Pts',(27.0107204572687,0.828315361319435,-3.11540581096789));
#71192=CARTESIAN_POINT('Ctrl Pts',(27.0154159792143,0.90127488150179,-3.09508237520985));
#71193=CARTESIAN_POINT('Ctrl Pts',(27.0201115011599,0.973334390090736,-3.07225287493831));
#71194=CARTESIAN_POINT('Ctrl Pts',(27.0262837492527,1.06805637618828,-3.04224357221505));
#71195=CARTESIAN_POINT('Ctrl Pts',(27.0324559973454,1.16155593781016,-3.00779672233859));
#71196=CARTESIAN_POINT('Ctrl Pts',(27.0386282454382,1.25338675574727,-2.96903001046088));
#71197=CARTESIAN_POINT('Ctrl Pts',(27.0447921340908,1.34509320178397,-2.93031580263069));
#71198=CARTESIAN_POINT('Ctrl Pts',(27.0509560227435,1.43513499963557,-2.88729352904775));
#71199=CARTESIAN_POINT('Ctrl Pts',(27.0571199113961,1.52308094164781,-2.84013063215219));
#71200=CARTESIAN_POINT('Ctrl Pts',(27.0632772730547,1.61093375695453,-2.79301767644904));
#71201=CARTESIAN_POINT('Ctrl Pts',(27.0694346347132,1.69669474794529,-2.74177301847029));
#71202=CARTESIAN_POINT('Ctrl Pts',(27.0755919963717,1.77995355426057,-2.6866117894432));
#71203=CARTESIAN_POINT('Ctrl Pts',(27.0817448605181,1.86315154597361,-2.63149085174804));
#71204=CARTESIAN_POINT('Ctrl Pts',(27.0878977246644,1.94385062570489,-2.57245926990061));
#71205=CARTESIAN_POINT('Ctrl Pts',(27.0940505888107,2.02166669074999,-2.50977715226113));
#71206=CARTESIAN_POINT('Ctrl Pts',(27.1002011219472,2.09945327521434,-2.44711878171333));
#71207=CARTESIAN_POINT('Ctrl Pts',(27.1063516550837,2.17435867734285,-2.3808128955805));
#71208=CARTESIAN_POINT('Ctrl Pts',(27.1125021882203,2.24603008317851,-2.31116127259807));
#71209=CARTESIAN_POINT('Ctrl Pts',(27.1186520364355,2.31769350771015,-2.24151740599732));
#71210=CARTESIAN_POINT('Ctrl Pts',(27.1248018846507,2.38612334044547,-2.16852884602008));
#71211=CARTESIAN_POINT('Ctrl Pts',(27.1309517328659,2.45100274948986,-2.09253508560624));
#71212=CARTESIAN_POINT('Ctrl Pts',(27.137102541245,2.51589228803133,-2.01652946043309));
#71213=CARTESIAN_POINT('Ctrl Pts',(27.1432533496242,2.57723001979068,-1.93751803326576));
#71214=CARTESIAN_POINT('Ctrl Pts',(27.1494041580033,2.63473927601702,-1.85587351667976));
#71215=CARTESIAN_POINT('Ctrl Pts',(27.1555615443695,2.69231003556436,-1.77414168529888));
#71216=CARTESIAN_POINT('Ctrl Pts',(27.1617189307357,2.74604389292233,-1.68977149713199));
#71217=CARTESIAN_POINT('Ctrl Pts',(27.1678763171019,2.7957075127245,-1.60316470326532));
#71218=CARTESIAN_POINT('Ctrl Pts',(27.1740371398389,2.84539884925609,-1.51650957508309));
#71219=CARTESIAN_POINT('Ctrl Pts',(27.1801979625758,2.89101522613878,-1.42761574185211));
#71220=CARTESIAN_POINT('Ctrl Pts',(27.1863587853128,2.93237025061843,-1.33690772897309));
#71221=CARTESIAN_POINT('Ctrl Pts',(27.1925299082295,2.97379441589353,-1.24604806283689));
#71222=CARTESIAN_POINT('Ctrl Pts',(27.1987010311462,3.01094283613897,-1.15336856191371));
#71223=CARTESIAN_POINT('Ctrl Pts',(27.2048721540629,3.04367800213099,-1.05931193793137));
#71224=CARTESIAN_POINT('Ctrl Pts',(27.2095676760084,3.06858573649026,-0.987745555605622));
#71225=CARTESIAN_POINT('Ctrl Pts',(27.214263197954,3.09093944077442,-0.915382267047877));
#71226=CARTESIAN_POINT('Ctrl Pts',(27.2189587198996,3.11069837576653,-0.842421021522788));
#71227=CARTESIAN_POINT('Ctrl Pts',(27.2251309679923,3.13667143056936,-0.746513705199134));
#71228=CARTESIAN_POINT('Ctrl Pts',(27.2313032160851,3.1582506037194,-0.649235276058583));
#71229=CARTESIAN_POINT('Ctrl Pts',(27.2374754641779,3.17529356364918,-0.551024815365045));
#71230=CARTESIAN_POINT('Ctrl Pts',(27.2436393528305,3.19231344129171,-0.452947366899128));
#71231=CARTESIAN_POINT('Ctrl Pts',(27.2498032414831,3.20480924330201,-0.353940820061735));
#71232=CARTESIAN_POINT('Ctrl Pts',(27.2559671301357,3.21268866535944,-0.254458448417352));
#71233=CARTESIAN_POINT('Ctrl Pts',(27.2621244917943,3.2205597438299,-0.155081419501796));
#71234=CARTESIAN_POINT('Ctrl Pts',(27.2682818534528,3.22382412668934,-0.0552299981218721));
#71235=CARTESIAN_POINT('Ctrl Pts',(27.2744392151113,3.22244089819566,0.044634293272634));
#71236=CARTESIAN_POINT('Ctrl Pts',(27.2805920792576,3.22105868005145,0.144425640946092));
#71237=CARTESIAN_POINT('Ctrl Pts',(27.286744943404,3.21503560589093,0.244229406919852));
#71238=CARTESIAN_POINT('Ctrl Pts',(27.2928978075503,3.20438279292017,0.343581837321375));
#71239=CARTESIAN_POINT('Ctrl Pts',(27.2990483406868,3.19373401576275,0.442896628099881));
#71240=CARTESIAN_POINT('Ctrl Pts',(27.3051988738233,3.17845903119077,0.541759991638729));
#71241=CARTESIAN_POINT('Ctrl Pts',(27.3113494069599,3.15862092804746,0.639711962840009));
#71242=CARTESIAN_POINT('Ctrl Pts',(27.3174992551751,3.13878503406872,0.737653026142318));
#71243=CARTESIAN_POINT('Ctrl Pts',(27.3236491033903,3.11438711801296,0.834682473156558));
#71244=CARTESIAN_POINT('Ctrl Pts',(27.3297989516055,3.08554145011797,0.930350214759962));
#71245=CARTESIAN_POINT('Ctrl Pts',(27.3359497599847,3.05669127860445,1.02603289278347));
#71246=CARTESIAN_POINT('Ctrl Pts',(27.3421005683638,3.02339210136452,1.12035302719587));
#71247=CARTESIAN_POINT('Ctrl Pts',(27.348251376743,2.98580784991265,1.21287635227174));
#71248=CARTESIAN_POINT('Ctrl Pts',(27.3544087631092,2.94818340395242,1.30549862649307));
#71249=CARTESIAN_POINT('Ctrl Pts',(27.3605661494753,2.90626489644451,1.39631985091888));
#71250=CARTESIAN_POINT('Ctrl Pts',(27.3667235358415,2.86026411716212,1.48492651083304));
#71251=CARTESIAN_POINT('Ctrl Pts',(27.3728843585785,2.81423766534207,1.57358262116629));
#71252=CARTESIAN_POINT('Ctrl Pts',(27.3790451813155,2.76412462247239,1.66002132986056));
#71253=CARTESIAN_POINT('Ctrl Pts',(27.3852060040524,2.71018131863378,1.74385629643858));
#71254=CARTESIAN_POINT('Ctrl Pts',(27.3913771269691,2.65614782785938,1.82783142533906));
#71255=CARTESIAN_POINT('Ctrl Pts',(27.3975482498858,2.59827153672217,1.90919376270899));
#71256=CARTESIAN_POINT('Ctrl Pts',(27.4037193728025,2.53685050562869,1.98758825579934));
#71257=CARTESIAN_POINT('Ctrl Pts',(27.4084148947481,2.49011609386717,2.04723753967971));
#71258=CARTESIAN_POINT('Ctrl Pts',(27.4131104166936,2.44133032726672,2.10516924605325));
#71259=CARTESIAN_POINT('Ctrl Pts',(27.4178059386392,2.39063853561046,2.16124153082303));
#71260=CARTESIAN_POINT('Ctrl Pts',(27.4239782232592,2.32400394852378,2.23494880019669));
#71261=CARTESIAN_POINT('Ctrl Pts',(27.4301505078792,2.25384011050068,2.30570123689203));
#71262=CARTESIAN_POINT('Ctrl Pts',(27.4363227924992,2.1804394257938,2.37314168834143));
#71263=CARTESIAN_POINT('Ctrl Pts',(27.4424858530913,2.10714843304184,2.4404813549686));
#71264=CARTESIAN_POINT('Ctrl Pts',(27.4486489136833,2.0306305303201,2.50451858811781));
#71265=CARTESIAN_POINT('Ctrl Pts',(27.4548119742754,1.95121696965503,2.56493077875997));
#71266=CARTESIAN_POINT('Ctrl Pts',(27.458900963233,1.89852867172407,2.60501228968278));
#71267=CARTESIAN_POINT('Ctrl Pts',(27.4629899521906,1.84456656031302,2.64349878566991));
#71268=CARTESIAN_POINT('Ctrl Pts',(27.4670789411481,1.78943621037803,2.68030513402633));
#71269=CARTESIAN_POINT('Ctrl Pts',(26.2169191182387,1.78943621037807,2.6803051340263));
#71270=CARTESIAN_POINT('Ctrl Pts',(26.2195202875596,1.75456074575711,2.703588833503));
#71271=CARTESIAN_POINT('Ctrl Pts',(26.2221214568805,1.71925451683826,2.72617587672373));
#71272=CARTESIAN_POINT('Ctrl Pts',(26.2247226262013,1.68354830089748,2.74805070569035));
#71273=CARTESIAN_POINT('Ctrl Pts',(26.2308948742941,1.59882193515356,2.79995692736014));
#71274=CARTESIAN_POINT('Ctrl Pts',(26.2370671223868,1.51154367717449,2.84803248428922));
#71275=CARTESIAN_POINT('Ctrl Pts',(26.2432393704796,1.4220948302714,2.89201726416274));
#71276=CARTESIAN_POINT('Ctrl Pts',(26.2494032591323,1.33276712922469,2.93594247285106));
#71277=CARTESIAN_POINT('Ctrl Pts',(26.2555671477849,1.24127506870981,2.97578772661281));
#71278=CARTESIAN_POINT('Ctrl Pts',(26.2617310364375,1.14802764559612,3.0113369269225));
#71279=CARTESIAN_POINT('Ctrl Pts',(26.2678883980961,1.05487896297127,3.04684848388184));
#71280=CARTESIAN_POINT('Ctrl Pts',(26.2740457597546,0.959979016796753,3.07807287760163));
#71281=CARTESIAN_POINT('Ctrl Pts',(26.2802031214132,0.863759177137005,3.10484100179246));
#71282=CARTESIAN_POINT('Ctrl Pts',(26.2863559855595,0.767609619187284,3.13158957378336));
#71283=CARTESIAN_POINT('Ctrl Pts',(26.2925088497058,0.67014250174516,3.15388823164449));
#71284=CARTESIAN_POINT('Ctrl Pts',(26.2986617138521,0.571805974942881,3.17161717259817));
#71285=CARTESIAN_POINT('Ctrl Pts',(26.3048122469887,0.473506702888822,3.18933939695068));
#71286=CARTESIAN_POINT('Ctrl Pts',(26.3109627801252,0.374339102950442,3.20249526736588));
#71287=CARTESIAN_POINT('Ctrl Pts',(26.3171133132617,0.274762311042314,3.21101591944523));
#71288=CARTESIAN_POINT('Ctrl Pts',(26.3232631614769,0.175196607972742,3.21953562266759));
#71289=CARTESIAN_POINT('Ctrl Pts',(26.3294130096922,0.0752222363223799,
3.22342109675458));
#71290=CARTESIAN_POINT('Ctrl Pts',(26.3355628579074,-0.0246967458693113,
3.22265536991523));
#71291=CARTESIAN_POINT('Ctrl Pts',(26.3417136662865,-0.124631328218802,
3.22188952352443));
#71292=CARTESIAN_POINT('Ctrl Pts',(26.3478644746657,-0.224510069529359,
3.21647103714928));
#71293=CARTESIAN_POINT('Ctrl Pts',(26.3540152830448,-0.323870124502197,
3.20643504611507));
#71294=CARTESIAN_POINT('Ctrl Pts',(26.360172669411,-0.423336440167089,3.19638832208203));
#71295=CARTESIAN_POINT('Ctrl Pts',(26.3663300557772,-0.522282528777776,
3.18171427606396));
#71296=CARTESIAN_POINT('Ctrl Pts',(26.3724874421434,-0.620251993612539,
3.16249980662761));
#71297=CARTESIAN_POINT('Ctrl Pts',(26.3786482648803,-0.718276134146572,
3.14327461380358));
#71298=CARTESIAN_POINT('Ctrl Pts',(26.3848090876173,-0.815322143541676,
3.11950405455751));
#71299=CARTESIAN_POINT('Ctrl Pts',(26.3909699103543,-0.910947170904252,
3.09132541385108));
#71300=CARTESIAN_POINT('Ctrl Pts',(26.397141033271,-1.00673207220099,3.06309966173173));
#71301=CARTESIAN_POINT('Ctrl Pts',(26.4033121561876,-1.1010908353553,3.03045124930332));
#71302=CARTESIAN_POINT('Ctrl Pts',(26.4094832791043,-1.19359889319449,2.99356630871355));
#71303=CARTESIAN_POINT('Ctrl Pts',(26.4141788010499,-1.26398699299218,2.96550106834522));
#71304=CARTESIAN_POINT('Ctrl Pts',(26.4188743229954,-1.33330401096612,2.93498411166095));
#71305=CARTESIAN_POINT('Ctrl Pts',(26.423569844941,-1.40137294563341,2.90211499250921));
#71306=CARTESIAN_POINT('Ctrl Pts',(26.4297420930338,-1.49084933548923,2.85890864391843));
#71307=CARTESIAN_POINT('Ctrl Pts',(26.4359143411265,-1.57848317027901,2.81148434118327));
#71308=CARTESIAN_POINT('Ctrl Pts',(26.4420865892193,-1.66384946660023,2.76002219465607));
#71309=CARTESIAN_POINT('Ctrl Pts',(26.4482504778719,-1.74910014630453,2.70862974635332));
#71310=CARTESIAN_POINT('Ctrl Pts',(26.4544143665245,-1.83208902288109,2.65321054616829));
#71311=CARTESIAN_POINT('Ctrl Pts',(26.4605782551772,-1.91241316352887,2.59399179922788));
#71312=CARTESIAN_POINT('Ctrl Pts',(26.4667356168357,-1.99265224826145,2.53483575952191));
#71313=CARTESIAN_POINT('Ctrl Pts',(26.4728929784943,-2.07023185919341,2.47188842824619));
#71314=CARTESIAN_POINT('Ctrl Pts',(26.4790503401528,-2.14477649639595,2.40542124024203));
#71315=CARTESIAN_POINT('Ctrl Pts',(26.4852032042991,-2.21926668407337,2.33900260176415));
#71316=CARTESIAN_POINT('Ctrl Pts',(26.4913560684454,-2.29072598222601,2.26906950636281));
#71317=CARTESIAN_POINT('Ctrl Pts',(26.4975089325918,-2.35881129232412,2.19593416333556));
#71318=CARTESIAN_POINT('Ctrl Pts',(26.5036594657283,-2.42687080833359,2.12282652759961));
#71319=CARTESIAN_POINT('Ctrl Pts',(26.5098099988648,-2.49155858048394,2.04651937237726));
#71320=CARTESIAN_POINT('Ctrl Pts',(26.5159605320014,-2.55256841993906,1.96736169120723));
#71321=CARTESIAN_POINT('Ctrl Pts',(26.5221103802166,-2.61357146535872,1.88821282501031));
#71322=CARTESIAN_POINT('Ctrl Pts',(26.5282602284318,-2.67089712720563,1.80621440801598));
#71323=CARTESIAN_POINT('Ctrl Pts',(26.534410076647,-2.72428020772443,1.72174763316257));
#71324=CARTESIAN_POINT('Ctrl Pts',(26.5405608850261,-2.77767162284053,1.63726767067469));
#71325=CARTESIAN_POINT('Ctrl Pts',(26.5467116934053,-2.82711900190601,1.55031895208767));
#71326=CARTESIAN_POINT('Ctrl Pts',(26.5528625017844,-2.87240163587749,1.46130982502286));
#71327=CARTESIAN_POINT('Ctrl Pts',(26.5590198881506,-2.91773269739892,1.37220550707428));
#71328=CARTESIAN_POINT('Ctrl Pts',(26.5651772745168,-2.95888992232304,1.28103676838367));
#71329=CARTESIAN_POINT('Ctrl Pts',(26.571334660883,-2.99569963211827,1.18823452088654));
#71330=CARTESIAN_POINT('Ctrl Pts',(26.5774954836199,-3.03252988501461,1.0953804814583));
#71331=CARTESIAN_POINT('Ctrl Pts',(26.5836563063569,-3.06500764963663,1.000891528498));
#71332=CARTESIAN_POINT('Ctrl Pts',(26.5898171290939,-3.09300895730525,0.905214423509421));
#71333=CARTESIAN_POINT('Ctrl Pts',(26.5959882520106,-3.12105707990655,0.809377357518942));
#71334=CARTESIAN_POINT('Ctrl Pts',(26.6021593749272,-3.14461369373555,0.712348593933028));
#71335=CARTESIAN_POINT('Ctrl Pts',(26.6083304978439,-3.1636058069966,0.614585926000115));
#71336=CARTESIAN_POINT('Ctrl Pts',(26.6130260197895,-3.17805664290023,0.54019966616785));
#71337=CARTESIAN_POINT('Ctrl Pts',(26.6177215417351,-3.1898659282748,0.465388741797828));
#71338=CARTESIAN_POINT('Ctrl Pts',(26.6224170636807,-3.19902170219092,0.390355877900522));
#71339=CARTESIAN_POINT('Ctrl Pts',(26.6304691922115,-3.21472250589836,0.261685567946234));
#71340=CARTESIAN_POINT('Ctrl Pts',(26.6385213207423,-3.22266253234392,0.132049290773541));
#71341=CARTESIAN_POINT('Ctrl Pts',(26.6465734492731,-3.22274928133452,0.0021522448421233));
#71342=CARTESIAN_POINT('',(26.4010094512492,-3.22274887269075,-0.00269556497428082));
#71343=CARTESIAN_POINT('Ctrl Pts',(25.9683941809562,1.78943611354,2.68030519867773));
#71344=CARTESIAN_POINT('Ctrl Pts',(25.9862750553894,1.56408187620045,2.83075709901863));
#71345=CARTESIAN_POINT('Ctrl Pts',(26.0050028600116,1.32059320147187,2.95223100368197));
#71346=CARTESIAN_POINT('Ctrl Pts',(26.0279673018825,0.992141898416267,3.06719381682171));
#71347=CARTESIAN_POINT('Ctrl Pts',(26.0329550845928,0.918714969711654,3.08998194997807));
#71348=CARTESIAN_POINT('Ctrl Pts',(26.038484691514,0.834103778514802,3.11295764977937));
#71349=CARTESIAN_POINT('Ctrl Pts',(26.0391637296948,0.823656116197414,3.11573828373809));
#71350=CARTESIAN_POINT('Ctrl Pts',(26.0401646110611,0.808168160785729,3.11977703822976));
#71351=CARTESIAN_POINT('Ctrl Pts',(26.040488740381,0.803138632926547,3.12107559690212));
#71352=CARTESIAN_POINT('Ctrl Pts',(26.0410632385907,0.794199046160189,3.12336064179676));
#71353=CARTESIAN_POINT('Ctrl Pts',(26.0413138856295,0.790290261880724,3.12435195301165));
#71354=CARTESIAN_POINT('Ctrl Pts',(26.0417984804571,0.782716445568047,3.12625763434061));
#71355=CARTESIAN_POINT('Ctrl Pts',(26.0420324803753,0.779051689627456,3.12717289187437));
#71356=CARTESIAN_POINT('Ctrl Pts',(26.0426891768176,0.768746072116618,3.12972743653648));
#71357=CARTESIAN_POINT('Ctrl Pts',(26.0431110277056,0.762101539419582,3.13135203962066));
#71358=CARTESIAN_POINT('Ctrl Pts',(26.0448562184165,0.734514802410653,3.13800404937277));
#71359=CARTESIAN_POINT('Ctrl Pts',(26.0461690268333,0.713527051522341,3.14284275995976));
#71360=CARTESIAN_POINT('Ctrl Pts',(26.0560544390594,0.553858272908785,3.17797233277397));
#71361=CARTESIAN_POINT('Ctrl Pts',(26.0641745783986,0.413342969048163,3.19928502823633));
#71362=CARTESIAN_POINT('Ctrl Pts',(26.0814424553223,0.107900091086263,3.22514375483868));
#71363=CARTESIAN_POINT('Ctrl Pts',(26.0905299155026,-0.0568856550565677,
3.22644683427784));
#71364=CARTESIAN_POINT('Ctrl Pts',(26.1090701465529,-0.383501672051364,
3.20399111385713));
#71365=CARTESIAN_POINT('Ctrl Pts',(26.1184930056003,-0.544850785095286,
3.18052817623539));
#71366=CARTESIAN_POINT('Ctrl Pts',(26.1295084298647,-0.722835616403641,
3.14070211854582));
#71367=CARTESIAN_POINT('Ctrl Pts',(26.1306967150248,-0.741908052521871,
3.13625151114838));
#71368=CARTESIAN_POINT('Ctrl Pts',(26.1324550938611,-0.769936639467185,
3.12944098557048));
#71369=CARTESIAN_POINT('Ctrl Pts',(26.1330208393143,-0.778925319812664,
3.12721579912497));
#71370=CARTESIAN_POINT('Ctrl Pts',(26.134031566098,-0.79493103856015,3.12318022560902));
#71371=CARTESIAN_POINT('Ctrl Pts',(26.1344760590866,-0.801951823373376,
3.12138484479681));
#71372=CARTESIAN_POINT('Ctrl Pts',(26.1354072568903,-0.816621854976992,
3.11758060918399));
#71373=CARTESIAN_POINT('Ctrl Pts',(26.135894105322,-0.824269873612342,3.11556724890667));
#71374=CARTESIAN_POINT('Ctrl Pts',(26.1371670437694,-0.844209482136554,
3.11023953752172));
#71375=CARTESIAN_POINT('Ctrl Pts',(26.1379545822111,-0.856488889992263,
3.10688049405498));
#71376=CARTESIAN_POINT('Ctrl Pts',(26.1414119246108,-0.910144754672631,
3.09186061641825));
#71377=CARTESIAN_POINT('Ctrl Pts',(26.1441062070609,-0.951303853931254,
3.07944576748346));
#71378=CARTESIAN_POINT('Ctrl Pts',(26.1512568797071,-1.05878190997055,3.04466675810205));
#71379=CARTESIAN_POINT('Ctrl Pts',(26.1557557282274,-1.12463921888404,3.02096015258786));
#71380=CARTESIAN_POINT('Ctrl Pts',(26.1760522224431,-1.41404286899356,2.90600870926));
#71381=CARTESIAN_POINT('Ctrl Pts',(26.1925389708112,-1.62767324440314,2.79196289073635));
#71382=CARTESIAN_POINT('Ctrl Pts',(26.218195257074,-1.94173101277219,2.57591706722954));
#71383=CARTESIAN_POINT('Ctrl Pts',(26.2274788640208,-2.05166462839362,2.48924690871577));
#71384=CARTESIAN_POINT('Ctrl Pts',(26.2370686372156,-2.16454180999246,2.38768088237464));
#71385=CARTESIAN_POINT('Ctrl Pts',(26.2378222359196,-2.17340773254435,2.37961343121592));
#71386=CARTESIAN_POINT('Ctrl Pts',(26.2389075300396,-2.18617280787062,2.36786713016513));
#71387=CARTESIAN_POINT('Ctrl Pts',(26.2392421388631,-2.19010798949337,2.36422784167202));
#71388=CARTESIAN_POINT('Ctrl Pts',(26.2398293187376,-2.19701311711815,2.35780988772424));
#71389=CARTESIAN_POINT('Ctrl Pts',(26.2400822071318,-2.19998690593365,2.3550353963162));
#71390=CARTESIAN_POINT('Ctrl Pts',(26.2406097732138,-2.20619056196325,2.34922549193433));
#71391=CARTESIAN_POINT('Ctrl Pts',(26.2408843685167,-2.20941941505017,2.34618904963226));
#71392=CARTESIAN_POINT('Ctrl Pts',(26.2414419415908,-2.21597514985097,2.33999844320824));
#71393=CARTESIAN_POINT('Ctrl Pts',(26.2417248831492,-2.21930158732189,2.33684382107471));
#71394=CARTESIAN_POINT('Ctrl Pts',(26.2429084624773,-2.2332146113743,2.3235929229163));
#71395=CARTESIAN_POINT('Ctrl Pts',(26.2438041869038,-2.24373932998335,2.31343152260835));
#71396=CARTESIAN_POINT('Ctrl Pts',(26.2513734583802,-2.33259386740233,2.22646749333747));
#71397=CARTESIAN_POINT('Ctrl Pts',(26.25776322999,-2.40703326878843,2.14577443549519));
#71398=CARTESIAN_POINT('Ctrl Pts',(26.2690676220834,-2.53374420816703,1.99350620570902));
#71399=CARTESIAN_POINT('Ctrl Pts',(26.2740224139885,-2.58745387204066,1.92328110857984));
#71400=CARTESIAN_POINT('Ctrl Pts',(26.2845955633612,-2.69604155936059,1.76850680122655));
#71401=CARTESIAN_POINT('Ctrl Pts',(26.2902049118871,-2.74997689519084,1.68341410550009));
#71402=CARTESIAN_POINT('Ctrl Pts',(26.3059853256336,-2.88853167898846,1.4403399727848));
#71403=CARTESIAN_POINT('Ctrl Pts',(26.316296699378,-2.96408694447702,1.27764225545488));
#71404=CARTESIAN_POINT('Ctrl Pts',(26.3281864926893,-3.03187410057892,1.09278314852782));
#71405=CARTESIAN_POINT('Ctrl Pts',(26.329267857943,-3.03787439526123,1.07599010698718));
#71406=CARTESIAN_POINT('Ctrl Pts',(26.330910487572,-3.04673881745804,1.05051591312671));
#71407=CARTESIAN_POINT('Ctrl Pts',(26.331468334425,-3.04970595377072,1.04187076855414));
#71408=CARTESIAN_POINT('Ctrl Pts',(26.3324407708177,-3.05480289781833,1.02681180846687));
#71409=CARTESIAN_POINT('Ctrl Pts',(26.3328548053832,-3.0569493922244,1.02040366855599));
#71410=CARTESIAN_POINT('Ctrl Pts',(26.3337202957956,-3.06138703336622,1.00701586846609));
#71411=CARTESIAN_POINT('Ctrl Pts',(26.3341718703257,-3.06367450106895,1.00003503812652));
#71412=CARTESIAN_POINT('Ctrl Pts',(26.3352425328886,-3.06903192745464,0.983494485798373));
#71413=CARTESIAN_POINT('Ctrl Pts',(26.3358623016034,-3.07208110432941,0.973928159617502));
#71414=CARTESIAN_POINT('Ctrl Pts',(26.3379233502066,-3.08204846273097,0.942144524659304));
#71415=CARTESIAN_POINT('Ctrl Pts',(26.3393710423203,-3.08877059467976,0.919866946691408));
#71416=CARTESIAN_POINT('Ctrl Pts',(26.3428014094527,-3.10404200772749,0.867200815584315));
#71417=CARTESIAN_POINT('Ctrl Pts',(26.3447905676136,-3.11238707298319,0.836756018406303));
#71418=CARTESIAN_POINT('Ctrl Pts',(26.3641168622528,-3.18856181589396,0.541930374655944));
#71419=CARTESIAN_POINT('Ctrl Pts',(26.3825654833146,-3.22297705881999,0.270117963095652));
#71420=CARTESIAN_POINT('Ctrl Pts',(26.4010094512492,-3.22274887269075,-0.00269556497428082));
#71421=CARTESIAN_POINT('Ctrl Pts',(26.4010096337881,-3.22274887043127,-0.00269826499466809));
#71422=CARTESIAN_POINT('Ctrl Pts',(26.4121186745204,-3.22261129329353,-0.167017398262714));
#71423=CARTESIAN_POINT('Ctrl Pts',(26.4231487577878,-3.20990655326697,-0.331110276176874));
#71424=CARTESIAN_POINT('Ctrl Pts',(26.4343606437183,-3.1828837039125,-0.505484950292156));
#71425=CARTESIAN_POINT('Ctrl Pts',(26.4351254551143,-3.18096512398751,-0.517421103233719));
#71426=CARTESIAN_POINT('Ctrl Pts',(26.436312386118,-3.17786906210822,-0.536014442295224));
#71427=CARTESIAN_POINT('Ctrl Pts',(26.4367369393384,-3.17673774542171,-0.542679055231531));
#71428=CARTESIAN_POINT('Ctrl Pts',(26.4374472336888,-3.17480467837527,-0.553853588593734));
#71429=CARTESIAN_POINT('Ctrl Pts',(26.4377335965835,-3.17401427392945,-0.558365411658908));
#71430=CARTESIAN_POINT('Ctrl Pts',(26.4382958196711,-3.17244058574248,-0.567237087864773));
#71431=CARTESIAN_POINT('Ctrl Pts',(26.4385717144258,-3.17165792730845,-0.571597040425067));
#71432=CARTESIAN_POINT('Ctrl Pts',(26.4390999847287,-3.17013925795697,-0.579957926456444));
#71433=CARTESIAN_POINT('Ctrl Pts',(26.439352436685,-3.16940466263672,-0.583959070395097));
#71434=CARTESIAN_POINT('Ctrl Pts',(26.4399368709176,-3.16768354891457,-0.593234598143494));
#71435=CARTESIAN_POINT('Ctrl Pts',(26.4402685326961,-3.16669142567133,-0.598507953219022));
#71436=CARTESIAN_POINT('Ctrl Pts',(26.4413406748695,-3.16343444176448,-0.615584716931534));
#71437=CARTESIAN_POINT('Ctrl Pts',(26.4420781923233,-3.16111668993797,-0.627378111070465));
#71438=CARTESIAN_POINT('Ctrl Pts',(26.4526362183705,-3.12683037130919,-0.796821729327422));
#71439=CARTESIAN_POINT('Ctrl Pts',(26.4618256011249,-3.08316323520662,-0.951899441759739));
#71440=CARTESIAN_POINT('Ctrl Pts',(26.4741650916175,-3.00808503580704,-1.15799714241869));
#71441=CARTESIAN_POINT('Ctrl Pts',(26.4774315163031,-2.98659147719117,-1.21235492469407));
#71442=CARTESIAN_POINT('Ctrl Pts',(26.483564048068,-2.94347758124824,-1.31327415113217));
#71443=CARTESIAN_POINT('Ctrl Pts',(26.4864293571623,-2.92220021164542,-1.35996144789546));
#71444=CARTESIAN_POINT('Ctrl Pts',(26.4962202709985,-2.84600862856226,-1.51708999299155));
#71445=CARTESIAN_POINT('Ctrl Pts',(26.503194254275,-2.78587726369822,-1.62487287463776));
#71446=CARTESIAN_POINT('Ctrl Pts',(26.5151650145065,-2.67529521899633,-1.79882481666908));
#71447=CARTESIAN_POINT('Ctrl Pts',(26.5200529671178,-2.62819487614635,-1.86696684381829));
#71448=CARTESIAN_POINT('Ctrl Pts',(26.5264392343859,-2.56460305482445,-1.95178569980153));
#71449=CARTESIAN_POINT('Ctrl Pts',(26.5278450121286,-2.55048052957625,-1.97020437306477));
#71450=CARTESIAN_POINT('Ctrl Pts',(26.5298695634986,-2.52997192029836,-1.99636175260268));
#71451=CARTESIAN_POINT('Ctrl Pts',(26.5304819425698,-2.52374651061654,-2.00422596314021));
#71452=CARTESIAN_POINT('Ctrl Pts',(26.5315452706214,-2.51289932347848,-2.01779793095763));
#71453=CARTESIAN_POINT('Ctrl Pts',(26.5319955350353,-2.50829453433871,-2.02351921851635));
#71454=CARTESIAN_POINT('Ctrl Pts',(26.5328617961108,-2.49941348619525,-2.03447671195646));
#71455=CARTESIAN_POINT('Ctrl Pts',(26.5332776700814,-2.49514022402318,-2.03971530558013));
#71456=CARTESIAN_POINT('Ctrl Pts',(26.534257967935,-2.48504483428835,-2.05201204887028));
#71457=CARTESIAN_POINT('Ctrl Pts',(26.5348229444268,-2.47920909225613,-2.05905889940944));
#71458=CARTESIAN_POINT('Ctrl Pts',(26.5364949871602,-2.46188749556562,-2.07979490313753));
#71459=CARTESIAN_POINT('Ctrl Pts',(26.5376054830227,-2.45031784828192,-2.09341331360936));
#71460=CARTESIAN_POINT('Ctrl Pts',(26.5501271182865,-2.31914607461688,-2.24523586001842));
#71461=CARTESIAN_POINT('Ctrl Pts',(26.5620294418599,-2.18812940259257,-2.37309753618723));
#71462=CARTESIAN_POINT('Ctrl Pts',(26.5811807517603,-1.96691318433478,-2.55501924394301));
#71463=CARTESIAN_POINT('Ctrl Pts',(26.5881986166319,-1.88369020936753,-2.61697930134381));
#71464=CARTESIAN_POINT('Ctrl Pts',(26.6048919483904,-1.67898925377064,-2.75454989631325));
#71465=CARTESIAN_POINT('Ctrl Pts',(26.6145534311206,-1.55516851535591,-2.82630616016101));
#71466=CARTESIAN_POINT('Ctrl Pts',(26.6263550834399,-1.3931016571962,-2.90634020776058));
#71467=CARTESIAN_POINT('Ctrl Pts',(26.6287982451854,-1.35892496187755,-2.92247649209751));
#71468=CARTESIAN_POINT('Ctrl Pts',(26.6326755752923,-1.30354428337436,-2.94744241322381));
#71469=CARTESIAN_POINT('Ctrl Pts',(26.6341291656382,-1.28251685610137,-2.95665267883043));
#71470=CARTESIAN_POINT('Ctrl Pts',(26.6360082368995,-1.25496077868726,-2.96837326685409));
#71471=CARTESIAN_POINT('Ctrl Pts',(26.63644557803,-1.24852049012467,-2.97108784712326));
#71472=CARTESIAN_POINT('Ctrl Pts',(26.6371178949995,-1.23857766707844,-2.97524070627342));
#71473=CARTESIAN_POINT('Ctrl Pts',(26.6373537614126,-1.23508139304846,-2.97669377843107));
#71474=CARTESIAN_POINT('Ctrl Pts',(26.6378395552432,-1.22786355836495,-2.97967864721995));
#71475=CARTESIAN_POINT('Ctrl Pts',(26.63808942663,-1.22414173171451,-2.98120961684502));
#71476=CARTESIAN_POINT('Ctrl Pts',(26.6386558362101,-1.21568411128581,-2.98467014160479));
#71477=CARTESIAN_POINT('Ctrl Pts',(26.6389721110374,-1.21094659867696,-2.98659539419578));
#71478=CARTESIAN_POINT('Ctrl Pts',(26.6399089028817,-1.19687082728374,-2.99227657381846));
#71479=CARTESIAN_POINT('Ctrl Pts',(26.6405274871799,-1.18751942777361,-2.99600008117042));
#71480=CARTESIAN_POINT('Ctrl Pts',(26.6449004774938,-1.12102156073245,-3.02211770283802));
#71481=CARTESIAN_POINT('Ctrl Pts',(26.6485643511902,-1.06325873553265,-3.04292076274468));
#71482=CARTESIAN_POINT('Ctrl Pts',(26.6529542810041,-0.992123082267575,
-3.06626664049294));
#71483=CARTESIAN_POINT('Ctrl Pts',(26.6537416294839,-0.97928708375435,-3.07039022569353));
#71484=CARTESIAN_POINT('Ctrl Pts',(26.6639610411744,-0.811740283079375,
-3.1230573279779));
#71485=CARTESIAN_POINT('Ctrl Pts',(26.6729763537689,-0.653594213380525,
-3.15994175292379));
#71486=CARTESIAN_POINT('Ctrl Pts',(26.6956874868583,-0.252017843874257,
-3.22214761244565));
#71487=CARTESIAN_POINT('Ctrl Pts',(26.7094251756833,-0.00727353578249663,
-3.23197667661168));
#71488=CARTESIAN_POINT('Ctrl Pts',(26.7254837568322,0.258400618041433,-3.21245099427739));
#71489=CARTESIAN_POINT('Ctrl Pts',(26.726831532051,0.280564897612453,-3.21059115585256));
#71490=CARTESIAN_POINT('Ctrl Pts',(26.7287870930218,0.312522259269744,-3.20757612260754));
#71491=CARTESIAN_POINT('Ctrl Pts',(26.7293890758968,0.322332400186727,-3.20660514645193));
#71492=CARTESIAN_POINT('Ctrl Pts',(26.7304402002458,0.339413459592343,-3.2048353419119));
#71493=CARTESIAN_POINT('Ctrl Pts',(26.7308887007493,0.346686436824137,-3.20405673770643));
#71494=CARTESIAN_POINT('Ctrl Pts',(26.7317557734559,0.360717235201576,-3.20250634695158));
#71495=CARTESIAN_POINT('Ctrl Pts',(26.7321742374839,0.367475393605659,-3.20173791244673));
#71496=CARTESIAN_POINT('Ctrl Pts',(26.7332785629056,0.385274652062921,-3.19965695562141));
#71497=CARTESIAN_POINT('Ctrl Pts',(26.7339655508869,0.396311407791546,-3.19830868651856));
#71498=CARTESIAN_POINT('Ctrl Pts',(26.7363771269379,0.434926744808454,-3.19338842377495));
#71499=CARTESIAN_POINT('Ctrl Pts',(26.7381111625164,0.46246525763062,-3.18951668842466));
#71500=CARTESIAN_POINT('Ctrl Pts',(26.7402515047593,0.496170128666749,-3.18433232831835));
#71501=CARTESIAN_POINT('Ctrl Pts',(26.7406471000612,0.502387866084007,-3.18335728514112));
#71502=CARTESIAN_POINT('Ctrl Pts',(26.75863090919,0.7845061799744,-3.13826937989728));
#71503=CARTESIAN_POINT('Ctrl Pts',(26.7774279093371,1.05345148678312,-3.0584898526404));
#71504=CARTESIAN_POINT('Ctrl Pts',(26.8042387666291,1.41556997101274,-2.89757853790005));
#71505=CARTESIAN_POINT('Ctrl Pts',(26.8121283714573,1.51980357024219,-2.84429252101251));
#71506=CARTESIAN_POINT('Ctrl Pts',(26.8229480253343,1.66199858984273,-2.76154626606062));
#71507=CARTESIAN_POINT('Ctrl Pts',(26.8260400570294,1.70255148836966,-2.73673090044666));
#71508=CARTESIAN_POINT('Ctrl Pts',(26.8308264346393,1.76541923705433,-2.69632194489141));
#71509=CARTESIAN_POINT('Ctrl Pts',(26.8325524383462,1.78810969535144,-2.681328205838));
#71510=CARTESIAN_POINT('Ctrl Pts',(26.8347257363155,1.81674199547524,-2.66188299049598));
#71511=CARTESIAN_POINT('Ctrl Pts',(26.8351899270656,1.82286115716929,-2.65769632153089));
#71512=CARTESIAN_POINT('Ctrl Pts',(26.8359340837868,1.83267776518594,-2.65093004346586));
#71513=CARTESIAN_POINT('Ctrl Pts',(26.8362149416402,1.83638429760424,-2.64836375871314));
#71514=CARTESIAN_POINT('Ctrl Pts',(26.8367467784661,1.84340628438653,-2.64348012950935));
#71515=CARTESIAN_POINT('Ctrl Pts',(26.8369978546372,1.84672272087482,-2.64116434869057));
#71516=CARTESIAN_POINT('Ctrl Pts',(26.8375713246262,1.85430066103077,-2.63585161993951));
#71517=CARTESIAN_POINT('Ctrl Pts',(26.8378934336712,1.85855925762253,-2.63285058266675));
#71518=CARTESIAN_POINT('Ctrl Pts',(26.8387461822136,1.8698385286706,-2.62486106545853));
#71519=CARTESIAN_POINT('Ctrl Pts',(26.8392756144362,1.87684657349928,-2.61985470584709));
#71520=CARTESIAN_POINT('Ctrl Pts',(26.8428415303304,1.92407575351156,-2.58582867229419));
#71521=CARTESIAN_POINT('Ctrl Pts',(26.8458188982536,1.96364496210872,-2.5559101172501));
#71522=CARTESIAN_POINT('Ctrl Pts',(26.8678764911133,2.25607770989934,-2.3239975929221));
#71523=CARTESIAN_POINT('Ctrl Pts',(26.8850926628562,2.47793538735777,-2.0858435978511));
#71524=CARTESIAN_POINT('Ctrl Pts',(26.9081913231658,2.70453079832163,-1.75433453757879));
#71525=CARTESIAN_POINT('Ctrl Pts',(26.9127311636779,2.74611018197335,-1.68850646065199));
#71526=CARTESIAN_POINT('Ctrl Pts',(26.9201173606876,2.80865392053139,-1.58105741273324));
#71527=CARTESIAN_POINT('Ctrl Pts',(26.9229085389498,2.83117065386919,-1.54037390900502));
#71528=CARTESIAN_POINT('Ctrl Pts',(26.926526107741,2.85888832972751,-1.48763115234238));
#71529=CARTESIAN_POINT('Ctrl Pts',(26.9273233709222,2.86490734440611,-1.47600637780861));
#71530=CARTESIAN_POINT('Ctrl Pts',(26.9286112149478,2.87448523603994,-1.45722888092234));
#71531=CARTESIAN_POINT('Ctrl Pts',(26.9291002225873,2.87808867272459,-1.4500989530794));
#71532=CARTESIAN_POINT('Ctrl Pts',(26.930033344504,2.88490102687603,-1.4364942904525));
#71533=CARTESIAN_POINT('Ctrl Pts',(26.9304772864347,2.88811475465547,-1.43002200820815));
#71534=CARTESIAN_POINT('Ctrl Pts',(26.9314917486236,2.89539612006079,-1.41523304904778));
#71535=CARTESIAN_POINT('Ctrl Pts',(26.9320627548254,2.89944972884628,-1.40690957143963));
#71536=CARTESIAN_POINT('Ctrl Pts',(26.9338133141717,2.91173975813742,-1.3813951320497));
#71537=CARTESIAN_POINT('Ctrl Pts',(26.9349969092012,2.91985945324567,-1.36414870087742));
#71538=CARTESIAN_POINT('Ctrl Pts',(26.9525107317908,3.03720649457058,-1.10905246030922));
#71539=CARTESIAN_POINT('Ctrl Pts',(26.9698977957588,3.11719092759398,-0.858885623109628));
#71540=CARTESIAN_POINT('Ctrl Pts',(27.0013582734629,3.20404110378433,-0.402019905246797));
#71541=CARTESIAN_POINT('Ctrl Pts',(27.0152016872114,3.22302808928914,-0.199007889242898));
#71542=CARTESIAN_POINT('Ctrl Pts',(27.0298840806747,3.22271096853025,0.0304712543785456));
#71543=CARTESIAN_POINT('Ctrl Pts',(27.0315342409979,3.22235994726802,0.0564885580357998));
#71544=CARTESIAN_POINT('Ctrl Pts',(27.0336271922966,3.22150647239905,0.089817575388892));
#71545=CARTESIAN_POINT('Ctrl Pts',(27.0340853976509,3.22129414546707,0.0971348517459847));
#71546=CARTESIAN_POINT('Ctrl Pts',(27.0348201205761,3.2209125534913,0.108902326003328));
#71547=CARTESIAN_POINT('Ctrl Pts',(27.0350975081195,3.22075899471722,0.113352954834058));
#71548=CARTESIAN_POINT('Ctrl Pts',(27.035626796076,3.2204477951274,0.121860767114268));
#71549=CARTESIAN_POINT('Ctrl Pts',(27.0358787799092,3.2202917127762,0.125917959286913));
#71550=CARTESIAN_POINT('Ctrl Pts',(27.0364596679059,3.21991357723222,0.135286268947646));
#71551=CARTESIAN_POINT('Ctrl Pts',(27.0367882637617,3.21968604915869,0.140597173600685));
#71552=CARTESIAN_POINT('Ctrl Pts',(27.0378405847351,3.21891361318267,0.157640950095602));
#71553=CARTESIAN_POINT('Ctrl Pts',(27.0385614978897,3.21831769657642,0.169371579920336));
#71554=CARTESIAN_POINT('Ctrl Pts',(27.0508935673475,3.20697436914158,0.370913082575582));
#71555=CARTESIAN_POINT('Ctrl Pts',(27.0616203192773,3.17951396796986,0.559441617585424));
#71556=CARTESIAN_POINT('Ctrl Pts',(27.0815126609903,3.09743822290574,0.905129658231472));
#71557=CARTESIAN_POINT('Ctrl Pts',(27.090671127175,3.04700341536141,1.06261516721349));
#71558=CARTESIAN_POINT('Ctrl Pts',(27.1051168285971,2.9518144187653,1.2963499831127));
#71559=CARTESIAN_POINT('Ctrl Pts',(27.1101839477628,2.91563640314851,1.37578858887188));
#71560=CARTESIAN_POINT('Ctrl Pts',(27.1183507704404,2.85349719420353,1.49874045733883));
#71561=CARTESIAN_POINT('Ctrl Pts',(27.1213790762972,2.82965666111281,1.54327960747503));
#71562=CARTESIAN_POINT('Ctrl Pts',(27.1252623657313,2.79814518715527,1.59896296564468));
#71563=CARTESIAN_POINT('Ctrl Pts',(27.1260826333789,2.79143677480003,1.61064576415304));
#71564=CARTESIAN_POINT('Ctrl Pts',(27.1273987367103,2.7805911672252,1.62926225913326));
#71565=CARTESIAN_POINT('Ctrl Pts',(27.1278928713464,2.77650077489499,1.63622314902888));
#71566=CARTESIAN_POINT('Ctrl Pts',(27.1288300439717,2.76870851826612,1.64937038823725));
#71567=CARTESIAN_POINT('Ctrl Pts',(27.1292728861002,2.76501196274502,1.65555983922217));
#71568=CARTESIAN_POINT('Ctrl Pts',(27.1302769789456,2.75659795575244,1.6695413271059));
#71569=CARTESIAN_POINT('Ctrl Pts',(27.1308386791731,2.75186818963315,1.67732584691534));
#71570=CARTESIAN_POINT('Ctrl Pts',(27.1322851961244,2.73962967443922,1.69727759415437));
#71571=CARTESIAN_POINT('Ctrl Pts',(27.1331717792957,2.73207290316657,1.70941499521389));
#71572=CARTESIAN_POINT('Ctrl Pts',(27.1384913559115,2.68640354481649,1.78169098624212));
#71573=CARTESIAN_POINT('Ctrl Pts',(27.1429948707185,2.64638991860623,1.84059932545311));
#71574=CARTESIAN_POINT('Ctrl Pts',(27.1484414938695,2.59645874091737,1.90911083082271));
#71575=CARTESIAN_POINT('Ctrl Pts',(27.1493168732594,2.58838727599272,1.92003996274891));
#71576=CARTESIAN_POINT('Ctrl Pts',(27.15056074101,2.57685231411846,1.93545390435554));
#71577=CARTESIAN_POINT('Ctrl Pts',(27.1509272280218,2.57344565101361,1.93998122292042));
#71578=CARTESIAN_POINT('Ctrl Pts',(27.1542208252032,2.54275782642465,1.9805410378715));
#71579=CARTESIAN_POINT('Ctrl Pts',(27.1571735936018,2.51473445496887,2.01600359557661));
#71580=CARTESIAN_POINT('Ctrl Pts',(27.1604927693031,2.48265541429687,2.05488853164906));
#71581=CARTESIAN_POINT('Ctrl Pts',(27.1608366038338,2.47932546493765,2.05890505418431));
#71582=CARTESIAN_POINT('Ctrl Pts',(27.161405992525,2.47379967420169,2.06553731463336));
#71583=CARTESIAN_POINT('Ctrl Pts',(27.1616313791936,2.47160939505537,2.068157688462));
#71584=CARTESIAN_POINT('Ctrl Pts',(27.1783784459326,2.30864378689708,2.26249545822776));
#71585=CARTESIAN_POINT('Ctrl Pts',(27.1955990383909,2.12611257465518,2.43482023122181));
#71586=CARTESIAN_POINT('Ctrl Pts',(27.2159207726962,1.8809818804662,2.617461929932));
#71587=CARTESIAN_POINT('Ctrl Pts',(27.2195749660459,1.83561176651236,2.64947722153259));
#71588=CARTESIAN_POINT('Ctrl Pts',(27.2231721927303,1.78943620958681,2.68030513455457));
#71589=CARTESIAN_POINT('Origin',(-1.72497344927317,0.,0.));
#71590=CARTESIAN_POINT('',(28.7169416469173,1.789436210378,2.68030513402635));
#71591=CARTESIAN_POINT('',(28.4706129526677,1.78943608566475,2.68030521728792));
#71592=CARTESIAN_POINT('',(-1.72497344927317,1.78943621037804,2.68030513402633));
#71593=CARTESIAN_POINT('',(27.8965734492388,-3.22274961841222,0.00156828692453643));
#71594=CARTESIAN_POINT('Ctrl Pts',(27.8965734492731,-3.22274961841249,0.00156828636609923));
#71595=CARTESIAN_POINT('Ctrl Pts',(27.9028189460097,-3.22279908535359,-0.10008379004733));
#71596=CARTESIAN_POINT('Ctrl Pts',(27.9090644427464,-3.21803473533519,-0.20172558506841));
#71597=CARTESIAN_POINT('Ctrl Pts',(27.915309939483,-3.2084859097739,-0.30287906709174));
#71598=CARTESIAN_POINT('Ctrl Pts',(27.9215577451443,-3.19893355406604,-0.404069944982713));
#71599=CARTESIAN_POINT('Ctrl Pts',(27.9278055508057,-3.18459324202756,-0.504771737031726));
#71600=CARTESIAN_POINT('Ctrl Pts',(27.934053356467,-3.16554606939534,-0.604512733559599));
#71601=CARTESIAN_POINT('Ctrl Pts',(27.9403049328509,-3.14648740127037,-0.704313926523192));
#71602=CARTESIAN_POINT('Ctrl Pts',(27.9465565092348,-3.122716297478,-0.803152762404056));
#71603=CARTESIAN_POINT('Ctrl Pts',(27.9528080856187,-3.09436453475874,-0.900569646683341));
#71604=CARTESIAN_POINT('Ctrl Pts',(27.9590691794596,-3.06596960905706,-0.998134839316647));
#71605=CARTESIAN_POINT('Ctrl Pts',(27.9653302733005,-3.03298021842741,-1.09427335940052));
#71606=CARTESIAN_POINT('Ctrl Pts',(27.9715913671414,-2.99557747238081,-1.18854245589487));
#71607=CARTESIAN_POINT('Ctrl Pts',(27.9778580248593,-2.95814148864664,-1.2828953239597));
#71608=CARTESIAN_POINT('Ctrl Pts',(27.9841246825773,-2.91628450781737,-1.37537508170243));
#71609=CARTESIAN_POINT('Ctrl Pts',(27.9903913402952,-2.87023420671054,-1.46556240437885));
#71610=CARTESIAN_POINT('Ctrl Pts',(27.9966690963733,-2.82410234971761,-1.55590945037606));
#71611=CARTESIAN_POINT('Ctrl Pts',(28.0029468524513,-2.77376255116826,-1.64395559618616));
#71612=CARTESIAN_POINT('Ctrl Pts',(28.0092246085293,-2.71948654939906,-1.72930924653099));
#71613=CARTESIAN_POINT('Ctrl Pts',(28.0109322706389,-2.70472250464632,-1.75252696840483));
#71614=CARTESIAN_POINT('Ctrl Pts',(28.0126399327485,-2.68966743765888,-1.77554564917328));
#71615=CARTESIAN_POINT('Ctrl Pts',(28.0143475948581,-2.67432732614984,-1.79835783844825));
#71616=CARTESIAN_POINT('Ctrl Pts',(28.0205198429509,-2.6188813608904,-1.88081120609726));
#71617=CARTESIAN_POINT('Ctrl Pts',(28.0266920910437,-2.55952099760056,-1.96084307949786));
#71618=CARTESIAN_POINT('Ctrl Pts',(28.0328643391364,-2.49648473396866,-2.03805827580112));
#71619=CARTESIAN_POINT('Ctrl Pts',(28.0390282277891,-2.43353384407167,-2.11516889500351));
#71620=CARTESIAN_POINT('Ctrl Pts',(28.0451921164417,-2.36691722140644,-2.18947008590427));
#71621=CARTESIAN_POINT('Ctrl Pts',(28.0513560050944,-2.29691685977599,-2.26059516538827));
#71622=CARTESIAN_POINT('Ctrl Pts',(28.0575133667529,-2.2269906221233,-2.33164492992122));
#71623=CARTESIAN_POINT('Ctrl Pts',(28.0636707284115,-2.15368807199885,-2.39952496153859));
#71624=CARTESIAN_POINT('Ctrl Pts',(28.06982809007,-2.07733110069408,-2.46390199898233));
#71625=CARTESIAN_POINT('Ctrl Pts',(28.0759809542163,-2.00102990269496,-2.52823201360518));
#71626=CARTESIAN_POINT('Ctrl Pts',(28.0821338183627,-1.92167905029059,-2.58906384201416));
#71627=CARTESIAN_POINT('Ctrl Pts',(28.088286682509,-1.83963620800017,-2.64610207375202));
#71628=CARTESIAN_POINT('Ctrl Pts',(28.0944372156455,-1.75762444760312,-2.70311869658181));
#71629=CARTESIAN_POINT('Ctrl Pts',(28.100587748782,-1.67292308003103,-2.75634433077547));
#71630=CARTESIAN_POINT('Ctrl Pts',(28.1067382819186,-1.58592095440542,-2.80552531424648));
#71631=CARTESIAN_POINT('Ctrl Pts',(28.1128881301338,-1.49892851730764,-2.8547008209395));
#71632=CARTESIAN_POINT('Ctrl Pts',(28.119037978349,-1.40963620968297,-2.89983235863566));
#71633=CARTESIAN_POINT('Ctrl Pts',(28.1251878265642,-1.3184589484762,-2.94071140435151));
#71634=CARTESIAN_POINT('Ctrl Pts',(28.1313386349433,-1.22726745193973,-2.98159683243382));
#71635=CARTESIAN_POINT('Ctrl Pts',(28.1374894433224,-1.1341908136752,-3.01822827206873));
#71636=CARTESIAN_POINT('Ctrl Pts',(28.1436402517016,-1.03966452913,-3.05044508709285));
#71637=CARTESIAN_POINT('Ctrl Pts',(28.1497976380678,-0.945037153372402,
-3.08269635641617));
#71638=CARTESIAN_POINT('Ctrl Pts',(28.155955024434,-0.848957447447346,-3.11052343292884));
#71639=CARTESIAN_POINT('Ctrl Pts',(28.1621124108001,-0.751876581154286,
-3.13381543317595));
#71640=CARTESIAN_POINT('Ctrl Pts',(28.1682732335371,-0.654741535079018,
-3.15712043243665));
#71641=CARTESIAN_POINT('Ctrl Pts',(28.1744340562741,-0.556604642579021,
-3.17588523344432));
#71642=CARTESIAN_POINT('Ctrl Pts',(28.180594879011,-0.457925721217903,-3.1900504065527));
#71643=CARTESIAN_POINT('Ctrl Pts',(28.1867660019277,-0.359081820166839,
-3.20423926218452));
#71644=CARTESIAN_POINT('Ctrl Pts',(28.1929371248444,-0.259694512704669,
-3.21381308762326));
#71645=CARTESIAN_POINT('Ctrl Pts',(28.1991082477611,-0.160227315433129,
-3.21876447878516));
#71646=CARTESIAN_POINT('Ctrl Pts',(28.2038037697067,-0.0845441028384395,
-3.22253192373409));
#71647=CARTESIAN_POINT('Ctrl Pts',(28.2084992916522,-0.00881471394602323,
-3.2236242991668));
#71648=CARTESIAN_POINT('Ctrl Pts',(28.2131948135978,0.0667584762774016,
-3.22205848307338));
#71649=CARTESIAN_POINT('Ctrl Pts',(28.2193670616906,0.166099185282368,-3.22000022298892));
#71650=CARTESIAN_POINT('Ctrl Pts',(28.2255393097833,0.265519466835396,-3.21333980965354));
#71651=CARTESIAN_POINT('Ctrl Pts',(28.2317115578761,0.364557931459154,-3.20206419003589));
#71652=CARTESIAN_POINT('Ctrl Pts',(28.2378754465287,0.463462262440905,-3.19080384165585));
#71653=CARTESIAN_POINT('Ctrl Pts',(28.2440393351813,0.561985376533668,-3.17494075954533));
#71654=CARTESIAN_POINT('Ctrl Pts',(28.250203223834,0.659666339695656,-3.15451389009028));
#71655=CARTESIAN_POINT('Ctrl Pts',(28.2563605854925,0.75724386765521,-3.13410865082098));
#71656=CARTESIAN_POINT('Ctrl Pts',(28.262517947151,0.853980594754985,-3.10914932036058));
#71657=CARTESIAN_POINT('Ctrl Pts',(28.2686753088095,0.949422128736799,-3.07972647875828));
#71658=CARTESIAN_POINT('Ctrl Pts',(28.2748281729558,1.04479394950559,-3.05032512843697));
#71659=CARTESIAN_POINT('Ctrl Pts',(28.2809810371022,1.13887204421094,-3.01646687654044));
#71660=CARTESIAN_POINT('Ctrl Pts',(28.2871339012485,1.23121451807512,-2.97829286219154));
#71661=CARTESIAN_POINT('Ctrl Pts',(28.293284434385,1.32352200803526,-2.94013331005053));
#71662=CARTESIAN_POINT('Ctrl Pts',(28.2994349675215,1.41409478270028,-2.89766141000608));
#71663=CARTESIAN_POINT('Ctrl Pts',(28.3055855006581,1.50250920456033,-2.851067107718));
#71664=CARTESIAN_POINT('Ctrl Pts',(28.3117353488733,1.59091378061973,-2.80447799415595));
#71665=CARTESIAN_POINT('Ctrl Pts',(28.3178851970885,1.67716009745321,-2.75376759356169));
#71666=CARTESIAN_POINT('Ctrl Pts',(28.3240350453037,1.76084839382784,-2.69917218725555));
#71667=CARTESIAN_POINT('Ctrl Pts',(28.3301858536828,1.8445497562946,-2.64456825707403));
#71668=CARTESIAN_POINT('Ctrl Pts',(28.336336662062,1.92569194119349,-2.58607835375549));
#71669=CARTESIAN_POINT('Ctrl Pts',(28.3424874704411,2.00390434310439,-2.523981962334));
#71670=CARTESIAN_POINT('Ctrl Pts',(28.3486448568073,2.08220038933238,-2.46181916187599));
#71671=CARTESIAN_POINT('Ctrl Pts',(28.3548022431735,2.15756005492245,-2.39604244198193));
#71672=CARTESIAN_POINT('Ctrl Pts',(28.3609596295397,2.22964611159373,-2.32697137488947));
#71673=CARTESIAN_POINT('Ctrl Pts',(28.3671204522766,2.30177239871393,-2.25786175998117));
#71674=CARTESIAN_POINT('Ctrl Pts',(28.3732812750136,2.37062113921173,-2.18545445124638));
#71675=CARTESIAN_POINT('Ctrl Pts',(28.3794420977505,2.43589371227412,-2.11010411710025));
#71676=CARTESIAN_POINT('Ctrl Pts',(28.3856132206672,2.5012754134941,-2.03462780595101));
#71677=CARTESIAN_POINT('Ctrl Pts',(28.3917843435839,2.56306873558721,-1.95619898240512));
#71678=CARTESIAN_POINT('Ctrl Pts',(28.3979554665006,2.62101682199957,-1.87520355729592));
#71679=CARTESIAN_POINT('Ctrl Pts',(28.4026509884462,2.66510871826058,-1.81357526026954));
#71680=CARTESIAN_POINT('Ctrl Pts',(28.4073465103919,2.70697529019553,-1.75046168185185));
#71681=CARTESIAN_POINT('Ctrl Pts',(28.4120420323375,2.74652130950348,-1.68604218777091));
#71682=CARTESIAN_POINT('Ctrl Pts',(28.4182142804302,2.79850442130151,-1.60136297551682));
#71683=CARTESIAN_POINT('Ctrl Pts',(28.424386528523,2.84665918645213,-1.51412839474084));
#71684=CARTESIAN_POINT('Ctrl Pts',(28.4305587766158,2.8907251466144,-1.42471951247646));
#71685=CARTESIAN_POINT('Ctrl Pts',(28.4367226652684,2.9347314256441,-1.33543172194218));
#71686=CARTESIAN_POINT('Ctrl Pts',(28.442886553921,2.97465971615513,-1.24397586919675));
#71687=CARTESIAN_POINT('Ctrl Pts',(28.4490504425736,3.01029354843852,-1.15076075477461));
#71688=CARTESIAN_POINT('Ctrl Pts',(28.4552078042322,3.04588964775434,-1.05764434662862));
#71689=CARTESIAN_POINT('Ctrl Pts',(28.4613651658908,3.07720017533033,-0.962772783923574));
#71690=CARTESIAN_POINT('Ctrl Pts',(28.4675225275494,3.1040556333647,-0.866577283037629));
#71691=CARTESIAN_POINT('Ctrl Pts',(28.4736753916957,3.13089147540787,-0.770452046084509));
#71692=CARTESIAN_POINT('Ctrl Pts',(28.479828255842,3.15327860118733,-0.673005210711577));
#71693=CARTESIAN_POINT('Ctrl Pts',(28.4859811199883,3.17109680116036,-0.574684818113822));
#71694=CARTESIAN_POINT('Ctrl Pts',(28.4921316531248,3.18890825071646,-0.476401674151972));
#71695=CARTESIAN_POINT('Ctrl Pts',(28.4982821862613,3.20215413645317,-0.377246057493469));
#71696=CARTESIAN_POINT('Ctrl Pts',(28.5044327193979,3.21076517721345,-0.277677041351127));
#71697=CARTESIAN_POINT('Ctrl Pts',(28.5105825676131,3.21937525905109,-0.178119113181222));
#71698=CARTESIAN_POINT('Ctrl Pts',(28.5167324158283,3.22335148463723,-0.0781483098141737));
#71699=CARTESIAN_POINT('Ctrl Pts',(28.5228822640435,3.22267646093287,0.0217713263081345));
#71700=CARTESIAN_POINT('Ctrl Pts',(28.5290330724226,3.22200133183836,0.1217065626904));
#71701=CARTESIAN_POINT('Ctrl Pts',(28.5351838808018,3.216673513986,0.22159018155417));
#71702=CARTESIAN_POINT('Ctrl Pts',(28.5413346891809,3.20672772253247,0.320959305896789));
#71703=CARTESIAN_POINT('Ctrl Pts',(28.5474920755471,3.19677129454414,0.420434700630556));
#71704=CARTESIAN_POINT('Ctrl Pts',(28.5536494619133,3.18218707423412,0.519394069039138));
#71705=CARTESIAN_POINT('Ctrl Pts',(28.5598068482795,3.163061545833,0.617380935705489));
#71706=CARTESIAN_POINT('Ctrl Pts',(28.5659676710165,3.1439253436812,0.715422487783006));
#71707=CARTESIAN_POINT('Ctrl Pts',(28.5721284937534,3.12024288906826,0.812490035242985));
#71708=CARTESIAN_POINT('Ctrl Pts',(28.5782893164904,3.09215106489531,0.908140602752004));
#71709=CARTESIAN_POINT('Ctrl Pts',(28.5844604394071,3.06401227445665,1.00395108689522));
#71710=CARTESIAN_POINT('Ctrl Pts',(28.5906315623237,3.03144953093479,1.09833944821386));
#71711=CARTESIAN_POINT('Ctrl Pts',(28.5968026852404,2.9946485809941,1.19088095074614));
#71712=CARTESIAN_POINT('Ctrl Pts',(28.601498207186,2.96664724794732,1.26129449814728));
#71713=CARTESIAN_POINT('Ctrl Pts',(28.6061937291315,2.93619322730563,1.33063918974492));
#71714=CARTESIAN_POINT('Ctrl Pts',(28.610889251077,2.90338591220099,1.39873793375773));
#71715=CARTESIAN_POINT('Ctrl Pts',(28.6170612315427,2.86026267471918,1.48824962652837));
#71716=CARTESIAN_POINT('Ctrl Pts',(28.6232332120084,2.81292017849583,1.57592275347687));
#71717=CARTESIAN_POINT('Ctrl Pts',(28.6294051924741,2.76153812358604,1.66133222279016));
#71718=CARTESIAN_POINT('Ctrl Pts',(28.6355691632302,2.71022274992083,1.74663085166076));
#71719=CARTESIAN_POINT('Ctrl Pts',(28.6417331339863,2.65487845658288,1.82967129146932));
#71720=CARTESIAN_POINT('Ctrl Pts',(28.6478971047424,2.59573209018716,1.91005038637011));
#71721=CARTESIAN_POINT('Ctrl Pts',(28.6540538745981,2.53665482001392,1.99033558045903));
#71722=CARTESIAN_POINT('Ctrl Pts',(28.6602106444537,2.47378456805033,2.06796526619833));
#71723=CARTESIAN_POINT('Ctrl Pts',(28.6663674143094,2.40739234662908,2.14256380345877));
#71724=CARTESIAN_POINT('Ctrl Pts',(28.6725199514532,2.34104576913317,2.21711105504159));
#71725=CARTESIAN_POINT('Ctrl Pts',(28.678672488597,2.2711823221187,2.28863097628703));
#71726=CARTESIAN_POINT('Ctrl Pts',(28.6848250257408,2.19811384756102,2.35678023490959));
#71727=CARTESIAN_POINT('Ctrl Pts',(28.6909756411917,2.12506819532269,2.42490820768825));
#71728=CARTESIAN_POINT('Ctrl Pts',(28.6971262566426,2.04881981890187,2.48966731064813));
#71729=CARTESIAN_POINT('Ctrl Pts',(28.7032768720936,1.96971744171717,2.55075101926769));
#71730=CARTESIAN_POINT('Ctrl Pts',(28.7078317970348,1.91113706165191,2.59598742042381));
#71731=CARTESIAN_POINT('Ctrl Pts',(28.712386721976,1.85099224515406,2.63920884383267));
#71732=CARTESIAN_POINT('Ctrl Pts',(28.7169416469173,1.789436210378,2.68030513402635));
#71733=CARTESIAN_POINT('Ctrl Pts',(27.4670789411481,1.78943621037803,2.68030513402633));
#71734=CARTESIAN_POINT('Ctrl Pts',(27.4733112001578,1.70540893037057,2.73640376831841));
#71735=CARTESIAN_POINT('Ctrl Pts',(27.4795434591674,1.61866637486224,2.78859711560752));
#71736=CARTESIAN_POINT('Ctrl Pts',(27.485775718177,1.52961023515413,2.83661948294299));
#71737=CARTESIAN_POINT('Ctrl Pts',(27.4919268250731,1.44171372214755,2.88401653663231));
#71738=CARTESIAN_POINT('Ctrl Pts',(27.4980779319692,1.35156391773072,2.92735038660131));
#71739=CARTESIAN_POINT('Ctrl Pts',(27.5042290388653,1.25957439429802,2.96641027299475));
#71740=CARTESIAN_POINT('Ctrl Pts',(27.5103789285969,1.16760307350456,3.00546243032303));
#71741=CARTESIAN_POINT('Ctrl Pts',(27.5165288183286,1.07379315695264,3.04024213522712));
#71742=CARTESIAN_POINT('Ctrl Pts',(27.5226787080602,0.978579412407021,3.07058624632384));
#71743=CARTESIAN_POINT('Ctrl Pts',(27.5288290258927,0.883359039924092,3.10093246970873));
#71744=CARTESIAN_POINT('Ctrl Pts',(27.5349793437251,0.786735059401567,3.12684235444456));
#71745=CARTESIAN_POINT('Ctrl Pts',(27.5411296615576,0.689157689316571,3.14820254141246));
#71746=CARTESIAN_POINT('Ctrl Pts',(27.5474232862094,0.589306696481606,3.17006043606597));
#71747=CARTESIAN_POINT('Ctrl Pts',(27.5537169108612,0.488457794806372,3.18715385470366));
#71748=CARTESIAN_POINT('Ctrl Pts',(27.5600105355129,0.387103143988446,3.19941693413257));
#71749=CARTESIAN_POINT('Ctrl Pts',(27.5661701684073,0.287906341554656,3.21141893164845));
#71750=CARTESIAN_POINT('Ctrl Pts',(27.5723298013017,0.188225555102932,3.21879425826122));
#71751=CARTESIAN_POINT('Ctrl Pts',(27.578489434196,0.0885246612456093,3.22153394314748));
#71752=CARTESIAN_POINT('Ctrl Pts',(27.5848500547265,-0.0144294535940865,
3.22436302342441));
#71753=CARTESIAN_POINT('Ctrl Pts',(27.591210675257,-0.117404501863241,3.22224875637744));
#71754=CARTESIAN_POINT('Ctrl Pts',(27.5975712957875,-0.219894358238718,
3.21523934314613));
#71755=CARTESIAN_POINT('Ctrl Pts',(27.603931916318,-0.322384214614165,3.20822992991483));
#71756=CARTESIAN_POINT('Ctrl Pts',(27.6102925368484,-0.424388388104331,
3.19632549798911));
#71757=CARTESIAN_POINT('Ctrl Pts',(27.6166531573789,-0.525412906889123,
3.17963187173835));
#71758=CARTESIAN_POINT('Ctrl Pts',(27.6228254054717,-0.623445542290536,
3.16343263421212));
#71759=CARTESIAN_POINT('Ctrl Pts',(27.6289976535645,-0.72090085505774,3.14266690515393));
#71760=CARTESIAN_POINT('Ctrl Pts',(27.6351699016572,-0.817320307424585,
3.11738754048504));
#71761=CARTESIAN_POINT('Ctrl Pts',(27.6413337903099,-0.913609173232671,
3.09214241315269));
#71762=CARTESIAN_POINT('Ctrl Pts',(27.6474976789625,-1.00886455063752,3.0623959098273));
#71763=CARTESIAN_POINT('Ctrl Pts',(27.6536615676151,-1.10263576568776,3.0282522898078));
#71764=CARTESIAN_POINT('Ctrl Pts',(27.6598189292737,-1.19630768560157,2.99414482475766));
#71765=CARTESIAN_POINT('Ctrl Pts',(27.6659762909323,-1.28849816172489,2.95564964766606));
#71766=CARTESIAN_POINT('Ctrl Pts',(27.6721336525908,-1.37877035596248,2.9129211915222));
#71767=CARTESIAN_POINT('Ctrl Pts',(27.6782865167371,-1.46897661281919,2.87022394545926));
#71768=CARTESIAN_POINT('Ctrl Pts',(27.6844393808835,-1.55726698211956,2.82329975325878));
#71769=CARTESIAN_POINT('Ctrl Pts',(27.6905922450298,-1.64322420329754,2.77235130894285));
#71770=CARTESIAN_POINT('Ctrl Pts',(27.6967427781663,-1.72914885962163,2.72142216642173));
#71771=CARTESIAN_POINT('Ctrl Pts',(27.7028933113028,-1.812741750898,2.66647202236397));
#71772=CARTESIAN_POINT('Ctrl Pts',(27.7090438444394,-1.89361064520634,2.60774927607338));
#71773=CARTESIAN_POINT('Ctrl Pts',(27.7151936926546,-1.97447053398155,2.54903306912825));
#71774=CARTESIAN_POINT('Ctrl Pts',(27.7213435408698,-2.05260667739641,2.4865453504305));
#71775=CARTESIAN_POINT('Ctrl Pts',(27.727493389085,-2.12765708154595,2.42057697788097));
#71776=CARTESIAN_POINT('Ctrl Pts',(27.7336441974642,-2.20271920317026,2.35459830581674));
#71777=CARTESIAN_POINT('Ctrl Pts',(27.7397950058433,-2.27469430232273,2.28513818731402));
#71778=CARTESIAN_POINT('Ctrl Pts',(27.7459458142225,-2.34325540223546,2.21252608626302));
#71779=CARTESIAN_POINT('Ctrl Pts',(27.7521032005887,-2.41188982487238,2.13983633014136));
#71780=CARTESIAN_POINT('Ctrl Pts',(27.7582605869548,-2.47710265859685,2.06398817660085));
#71781=CARTESIAN_POINT('Ctrl Pts',(27.764417973321,-2.53860567769926,1.98534600905058));
#71782=CARTESIAN_POINT('Ctrl Pts',(27.770578796058,-2.60014302097202,1.90665995215642));
#71783=CARTESIAN_POINT('Ctrl Pts',(27.776739618795,-2.65796617504315,1.82517713016482));
#71784=CARTESIAN_POINT('Ctrl Pts',(27.782900441532,-2.71183013064817,1.74129116032004));
#71785=CARTESIAN_POINT('Ctrl Pts',(27.7890715644487,-2.76578414052778,1.65726494288153));
#71786=CARTESIAN_POINT('Ctrl Pts',(27.7952426873654,-2.81576551251435,1.57082792840027));
#71787=CARTESIAN_POINT('Ctrl Pts',(27.801413810282,-2.86157502894539,1.48239870352621));
#71788=CARTESIAN_POINT('Ctrl Pts',(27.8061093322275,-2.89643085544834,1.41511413123345));
#71789=CARTESIAN_POINT('Ctrl Pts',(27.8108048541729,-2.92887234514541,1.34667668993071));
#71790=CARTESIAN_POINT('Ctrl Pts',(27.8155003761184,-2.95883081273827,1.2772774890722));
#71791=CARTESIAN_POINT('Ctrl Pts',(27.8223228167748,-3.00235949169766,1.1764427075586));
#71792=CARTESIAN_POINT('Ctrl Pts',(27.8291452574313,-3.04077590270347,1.07327399786143));
#71793=CARTESIAN_POINT('Ctrl Pts',(27.8359676980877,-3.07384959702334,0.968280030455798));
#71794=CARTESIAN_POINT('Ctrl Pts',(27.8427712225131,-3.10683158960843,0.863577174434908));
#71795=CARTESIAN_POINT('Ctrl Pts',(27.8495747469385,-3.13450030393611,0.75705940657642));
#71796=CARTESIAN_POINT('Ctrl Pts',(27.8563782713639,-3.15667327320979,0.649254502258558));
#71797=CARTESIAN_POINT('Ctrl Pts',(27.8631479113503,-3.17873581168638,0.541986512116085));
#71798=CARTESIAN_POINT('Ctrl Pts',(27.8699175513366,-3.19535709541191,0.433444429808308));
#71799=CARTESIAN_POINT('Ctrl Pts',(27.876687191323,-3.2064049839161,0.324167613462539));
#71800=CARTESIAN_POINT('Ctrl Pts',(27.8833159439616,-3.21722294768089,0.217165027483141));
#71801=CARTESIAN_POINT('Ctrl Pts',(27.8899446966002,-3.22269711590572,0.109458259196475));
#71802=CARTESIAN_POINT('Ctrl Pts',(27.8965734492388,-3.22274961841222,0.00156828692453539));
#71803=CARTESIAN_POINT('Ctrl Pts',(27.2231721927303,1.78943620958681,2.68030513455457));
#71804=CARTESIAN_POINT('Ctrl Pts',(27.2238480330952,1.78076083047407,2.68609702642393));
#71805=CARTESIAN_POINT('Ctrl Pts',(27.2245218578103,1.77205702048223,2.69184700624272));
#71806=CARTESIAN_POINT('Ctrl Pts',(27.22740730015,1.73454512105204,2.71636760973045));
#71807=CARTESIAN_POINT('Ctrl Pts',(27.2295972711144,1.70546450763826,2.73471951247519));
#71808=CARTESIAN_POINT('Ctrl Pts',(27.2322638556065,1.66922264459362,2.75678763313491));
#71809=CARTESIAN_POINT('Ctrl Pts',(27.2327678639155,1.66233518012192,2.76094622251951));
#71810=CARTESIAN_POINT('Ctrl Pts',(27.233558344089,1.65147266073824,2.76744953160831));
#71811=CARTESIAN_POINT('Ctrl Pts',(27.2338459315801,1.64750807689072,2.76981154528296));
#71812=CARTESIAN_POINT('Ctrl Pts',(27.234383295355,1.64007615292079,2.77421772320716));
#71813=CARTESIAN_POINT('Ctrl Pts',(27.2346331988297,1.63661009499939,2.77626388520872));
#71814=CARTESIAN_POINT('Ctrl Pts',(27.2352000132547,1.62872643314744,2.78089805290653));
#71815=CARTESIAN_POINT('Ctrl Pts',(27.2355166593318,1.6243065008625,2.78348202200232));
#71816=CARTESIAN_POINT('Ctrl Pts',(27.2364555620696,1.61115451809709,2.79112890457759));
#71817=CARTESIAN_POINT('Ctrl Pts',(27.2370758730568,1.60240472039727,2.79616139762017));
#71818=CARTESIAN_POINT('Ctrl Pts',(27.2414890166815,1.53973536954442,2.83181523239541));
#71819=CARTESIAN_POINT('Ctrl Pts',(27.245189423963,1.48496149192908,2.86091822272689));
#71820=CARTESIAN_POINT('Ctrl Pts',(27.2671600285214,1.14899766528563,3.02717467850755));
#71821=CARTESIAN_POINT('Ctrl Pts',(27.2838631665485,0.849890696075904,3.12437374701242));
#71822=CARTESIAN_POINT('Ctrl Pts',(27.3062590786234,0.466471820723136,3.18971854825837));
#71823=CARTESIAN_POINT('Ctrl Pts',(27.3106980235768,0.391083682982989,3.19983635496571));
#71824=CARTESIAN_POINT('Ctrl Pts',(27.3179339237413,0.269923907952096,3.21175151972092));
#71825=CARTESIAN_POINT('Ctrl Pts',(27.3206785407704,0.224347663239141,3.2152565288252));
#71826=CARTESIAN_POINT('Ctrl Pts',(27.3242437698862,0.165721903624434,3.21851256445583));
#71827=CARTESIAN_POINT('Ctrl Pts',(27.3250362924795,0.15272574021701,3.21915543542226));
#71828=CARTESIAN_POINT('Ctrl Pts',(27.3263183139507,0.131762377175069,3.22006518259725));
#71829=CARTESIAN_POINT('Ctrl Pts',(27.3268062654648,0.123797369539631,3.22038123732308));
#71830=CARTESIAN_POINT('Ctrl Pts',(27.3277385889466,0.108605666226845,3.22092760699104));
#71831=CARTESIAN_POINT('Ctrl Pts',(27.3281827935099,0.101379198276591,3.22116315901778));
#71832=CARTESIAN_POINT('Ctrl Pts',(27.3291995659685,0.0848649106216545,
3.22164582690221));
#71833=CARTESIAN_POINT('Ctrl Pts',(27.3297726278733,0.0755767243877204,
3.22187709928331));
#71834=CARTESIAN_POINT('Ctrl Pts',(27.3315356593533,0.0470621070573929,
3.22246373170955));
#71835=CARTESIAN_POINT('Ctrl Pts',(27.3327297552293,0.0278336591630101,
3.22268717155366));
#71836=CARTESIAN_POINT('Ctrl Pts',(27.349879662908,-0.247089536006223,3.22342121487121));
#71837=CARTESIAN_POINT('Ctrl Pts',(27.3668397170065,-0.501901568342063,
3.19367174408501));
#71838=CARTESIAN_POINT('Ctrl Pts',(27.398244351387,-0.953525121665733,3.08553146246579));
#71839=CARTESIAN_POINT('Ctrl Pts',(27.4124741627459,-1.15139496122458,3.01728671391873));
#71840=CARTESIAN_POINT('Ctrl Pts',(27.4275251235296,-1.36523747769293,2.91940716620469));
#71841=CARTESIAN_POINT('Ctrl Pts',(27.4291962726676,-1.38905712083657,2.90814923866551));
#71842=CARTESIAN_POINT('Ctrl Pts',(27.4313118537463,-1.41934547446522,2.89337692810322));
#71843=CARTESIAN_POINT('Ctrl Pts',(27.4317721047328,-1.42594304663215,2.89013114827778));
#71844=CARTESIAN_POINT('Ctrl Pts',(27.4325093204974,-1.43652512686493,2.88488007000728));
#71845=CARTESIAN_POINT('Ctrl Pts',(27.432787165695,-1.44051663297238,2.88288905252125));
#71846=CARTESIAN_POINT('Ctrl Pts',(27.4333167756684,-1.4481315260626,2.8790708766506));
#71847=CARTESIAN_POINT('Ctrl Pts',(27.4335686259894,-1.45175558478329,2.87724516712595));
#71848=CARTESIAN_POINT('Ctrl Pts',(27.434148472238,-1.46010583246841,2.87301872957268));
#71849=CARTESIAN_POINT('Ctrl Pts',(27.4344761634438,-1.46482958273714,2.8706131674218));
#71850=CARTESIAN_POINT('Ctrl Pts',(27.4353534844092,-1.47748828929879,2.86412735895395));
#71851=CARTESIAN_POINT('Ctrl Pts',(27.435901793436,-1.48541234092871,2.86002576126802));
#71852=CARTESIAN_POINT('Ctrl Pts',(27.4398563809841,-1.54264407668412,2.83009981109492));
#71853=CARTESIAN_POINT('Ctrl Pts',(27.4431880062344,-1.59129588585395,2.80303299529659));
#71854=CARTESIAN_POINT('Ctrl Pts',(27.447029180231,-1.64748836798729,2.76983605017949));
#71855=CARTESIAN_POINT('Ctrl Pts',(27.4475923480799,-1.65572952867481,2.76491761161707));
#71856=CARTESIAN_POINT('Ctrl Pts',(27.4589487261483,-1.82192944646596,2.66471764704984));
#71857=CARTESIAN_POINT('Ctrl Pts',(27.469161911215,-1.97145487287852,2.55607605126568));
#71858=CARTESIAN_POINT('Ctrl Pts',(27.4926815127812,-2.28924954169539,2.28060942763938));
#71859=CARTESIAN_POINT('Ctrl Pts',(27.5060231318166,-2.45007108750799,2.10688688602693));
#71860=CARTESIAN_POINT('Ctrl Pts',(27.5214564907231,-2.60207726935541,1.90149728140294));
#71861=CARTESIAN_POINT('Ctrl Pts',(27.5226400132841,-2.61353807531062,1.88571385154051));
#71862=CARTESIAN_POINT('Ctrl Pts',(27.5243987795243,-2.63027668331909,1.86221627693074));
#71863=CARTESIAN_POINT('Ctrl Pts',(27.5249697429993,-2.63566548231103,1.85458145017496));
#71864=CARTESIAN_POINT('Ctrl Pts',(27.5259851558146,-2.64516853006042,1.84099250066742));
#71865=CARTESIAN_POINT('Ctrl Pts',(27.5264290916484,-2.64929608922764,1.83504772967395));
#71866=CARTESIAN_POINT('Ctrl Pts',(27.5273014392519,-2.65735348543378,1.82335911194502));
#71867=CARTESIAN_POINT('Ctrl Pts',(27.5277297909691,-2.66128481199732,1.81761633627087));
#71868=CARTESIAN_POINT('Ctrl Pts',(27.5288946584354,-2.67190738908606,1.80199081800324));
#71869=CARTESIAN_POINT('Ctrl Pts',(27.529632543403,-2.67856234294779,1.79208364001474));
#71870=CARTESIAN_POINT('Ctrl Pts',(27.5324191975941,-2.7034159547631,1.75463653631705));
#71871=CARTESIAN_POINT('Ctrl Pts',(27.5344817311047,-2.72124565583472,1.72685527734292));
#71872=CARTESIAN_POINT('Ctrl Pts',(27.5535912642751,-2.88122298447622,1.46895582221554));
#71873=CARTESIAN_POINT('Ctrl Pts',(27.5717481779801,-2.99427029064344,1.22211448809788));
#71874=CARTESIAN_POINT('Ctrl Pts',(27.5983540607978,-3.11187394531926,0.847008138719422));
#71875=CARTESIAN_POINT('Ctrl Pts',(27.6066463246093,-3.14187405204064,0.727882507468044));
#71876=CARTESIAN_POINT('Ctrl Pts',(27.6179660007046,-3.17427470461006,0.559031598303127));
#71877=CARTESIAN_POINT('Ctrl Pts',(27.6211681570472,-3.18243645823766,0.510524205878982));
#71878=CARTESIAN_POINT('Ctrl Pts',(27.6261112276352,-3.19349129038588,0.434180159233793));
#71879=CARTESIAN_POINT('Ctrl Pts',(27.6278860510557,-3.19713746042052,0.406461828944376));
#71880=CARTESIAN_POINT('Ctrl Pts',(27.6301129859493,-3.20130477556738,0.37124338753867));
#71881=CARTESIAN_POINT('Ctrl Pts',(27.6305829885249,-3.20216087635693,0.363785161144907));
#71882=CARTESIAN_POINT('Ctrl Pts',(27.6313320858415,-3.203487910875,0.351856465842583));
#71883=CARTESIAN_POINT('Ctrl Pts',(27.631612111472,-3.2039755596557,0.34738794077672));
#71884=CARTESIAN_POINT('Ctrl Pts',(27.6321433158255,-3.2048846216203,0.338893070528992));
#71885=CARTESIAN_POINT('Ctrl Pts',(27.6323945879422,-3.205307792317,0.334867000195016));
#71886=CARTESIAN_POINT('Ctrl Pts',(27.6329697404343,-3.20626068533308,0.325633803812677));
#71887=CARTESIAN_POINT('Ctrl Pts',(27.6332933301567,-3.2067853090427,0.320426183581449));
#71888=CARTESIAN_POINT('Ctrl Pts',(27.634313777896,-3.2084032253391,0.303964082469341));
#71889=CARTESIAN_POINT('Ctrl Pts',(27.6350080581697,-3.2094499892626,0.292704962507583));
#71890=CARTESIAN_POINT('Ctrl Pts',(27.6413990189643,-3.21858085674732,0.188547626912244));
#71891=CARTESIAN_POINT('Ctrl Pts',(27.6468851710463,-3.22268952531855,0.0953351988905227));
#71892=CARTESIAN_POINT('Ctrl Pts',(27.6614374253509,-3.22285155288648,-0.157324226192558));
#71893=CARTESIAN_POINT('Ctrl Pts',(27.6702712317488,-3.21112892640575,-0.316512004701471));
#71894=CARTESIAN_POINT('Ctrl Pts',(27.6920848388944,-3.15375973317529,-0.702171279841489));
#71895=CARTESIAN_POINT('Ctrl Pts',(27.7051346273545,-3.0954924411043,-0.925824020369713));
#71896=CARTESIAN_POINT('Ctrl Pts',(27.7201256606333,-3.00757630179329,-1.15798062649805));
#71897=CARTESIAN_POINT('Ctrl Pts',(27.7212049559113,-3.0011353571452,-1.17457264181912));
#71898=CARTESIAN_POINT('Ctrl Pts',(27.7228449659654,-2.99118250973019,-1.19959498895647));
#71899=CARTESIAN_POINT('Ctrl Pts',(27.7234022787466,-2.98777159617318,-1.20806532540585));
#71900=CARTESIAN_POINT('Ctrl Pts',(27.7243740458556,-2.98177455170537,-1.22277705543178));
#71901=CARTESIAN_POINT('Ctrl Pts',(27.7247879471271,-2.97920469554067,-1.22902505485243));
#71902=CARTESIAN_POINT('Ctrl Pts',(27.7256534149903,-2.97379883315036,-1.24205155017328));
#71903=CARTESIAN_POINT('Ctrl Pts',(27.7261051010829,-2.97095925530326,-1.24882851314205));
#71904=CARTESIAN_POINT('Ctrl Pts',(27.7271764921108,-2.96418083222222,-1.26485199485873));
#71905=CARTESIAN_POINT('Ctrl Pts',(27.7277968802615,-2.96022187711769,-1.27408987499967));
#71906=CARTESIAN_POINT('Ctrl Pts',(27.7298620859044,-2.94693118832376,-1.30470619378309));
#71907=CARTESIAN_POINT('Ctrl Pts',(27.7313133512209,-2.93741073377235,-1.32600143883758));
#71908=CARTESIAN_POINT('Ctrl Pts',(27.7472500448558,-2.83092148646036,-1.55741949420045));
#71909=CARTESIAN_POINT('Ctrl Pts',(27.7625399367467,-2.71184042812416,-1.75657449958189));
#71910=CARTESIAN_POINT('Ctrl Pts',(27.7881359425568,-2.48346646917698,-2.05921291587329));
#71911=CARTESIAN_POINT('Ctrl Pts',(27.7981991066249,-2.3864243556292,-2.17093160042393));
#71912=CARTESIAN_POINT('Ctrl Pts',(27.8145905366298,-2.21254224802675,-2.34530723003864));
#71913=CARTESIAN_POINT('Ctrl Pts',(27.821032681864,-2.13986338382035,-2.41180391202702));
#71914=CARTESIAN_POINT('Ctrl Pts',(27.8279689574275,-2.0554677621893,-2.4821967121598));
#71915=CARTESIAN_POINT('Ctrl Pts',(27.828687324874,-2.04665009979174,-2.48947215640897));
#71916=CARTESIAN_POINT('Ctrl Pts',(27.8297312106478,-2.03372089361142,-2.50002490552392));
#71917=CARTESIAN_POINT('Ctrl Pts',(27.8300593444938,-2.0296398674067,-2.50333921211656));
#71918=CARTESIAN_POINT('Ctrl Pts',(27.8306390725323,-2.02239945024623,-2.50918999699666));
#71919=CARTESIAN_POINT('Ctrl Pts',(27.8308909586197,-2.01924336668597,-2.51173051982105));
#71920=CARTESIAN_POINT('Ctrl Pts',(27.8314206151855,-2.01258524567719,-2.51706938436435));
#71921=CARTESIAN_POINT('Ctrl Pts',(27.8316982880087,-2.0090821678938,-2.51986636551565));
#71922=CARTESIAN_POINT('Ctrl Pts',(27.8324361633962,-1.99974019449305,-2.52729346278987));
#71923=CARTESIAN_POINT('Ctrl Pts',(27.8328954460419,-1.9938910136549,-2.53191068578585));
#71924=CARTESIAN_POINT('Ctrl Pts',(27.8350349794586,-1.96648548843877,-2.55339017614526));
#71925=CARTESIAN_POINT('Ctrl Pts',(27.8366977922625,-1.94473015369002,-2.56999831011822));
#71926=CARTESIAN_POINT('Ctrl Pts',(27.8412170756525,-1.88444173658231,-2.61481879096467));
#71927=CARTESIAN_POINT('Ctrl Pts',(27.8440396845546,-1.84548780824245,-2.64245590499762));
#71928=CARTESIAN_POINT('Ctrl Pts',(27.8536955548271,-1.70838546890498,-2.73521620288345));
#71929=CARTESIAN_POINT('Ctrl Pts',(27.8603364431917,-1.60728737931182,-2.79582183036316));
#71930=CARTESIAN_POINT('Ctrl Pts',(27.8825148958391,-1.25706519991061,-2.98048002034257));
#71931=CARTESIAN_POINT('Ctrl Pts',(27.8978766973831,-0.995314585336189,
-3.07779234881496));
#71932=CARTESIAN_POINT('Ctrl Pts',(27.9149917990916,-0.716709782021276,
-3.14205439352657));
#71933=CARTESIAN_POINT('Ctrl Pts',(27.9154607824233,-0.709082995238445,
-3.14378434816814));
#71934=CARTESIAN_POINT('Ctrl Pts',(27.9175394978057,-0.675312720949102,
-3.15131518959347));
#71935=CARTESIAN_POINT('Ctrl Pts',(27.9191583856158,-0.649104398494685,
-3.15681771866805));
#71936=CARTESIAN_POINT('Ctrl Pts',(27.9214536904776,-0.612092166582058,
-3.1641081748379));
#71937=CARTESIAN_POINT('Ctrl Pts',(27.9221213924775,-0.601342596038615,
-3.16616873208228));
#71938=CARTESIAN_POINT('Ctrl Pts',(27.9232048813275,-0.583928199338438,
-3.16941496866566));
#71939=CARTESIAN_POINT('Ctrl Pts',(27.9236195856776,-0.577269707025343,
-3.17063449010249));
#71940=CARTESIAN_POINT('Ctrl Pts',(27.9244852047861,-0.563385926521309,
-3.17313215902541));
#71941=CARTESIAN_POINT('Ctrl Pts',(27.9249362341709,-0.556160023551465,
-3.17440662606845));
#71942=CARTESIAN_POINT('Ctrl Pts',(27.9260033142691,-0.5390842589185,-3.17735826700009));
#71943=CARTESIAN_POINT('Ctrl Pts',(27.9266200332169,-0.529230868168161,
-3.17901432517391));
#71944=CARTESIAN_POINT('Ctrl Pts',(27.9286606983437,-0.496679598192446,
-3.18432968187484));
#71945=CARTESIAN_POINT('Ctrl Pts',(27.9300908836919,-0.473950663811787,
-3.18779184863668));
#71946=CARTESIAN_POINT('Ctrl Pts',(27.9334734704151,-0.420401360956075,
-3.19536335451879));
#71947=CARTESIAN_POINT('Ctrl Pts',(27.9354321160453,-0.389555150379547,
-3.199270377393));
#71948=CARTESIAN_POINT('Ctrl Pts',(27.9424401598065,-0.279778423930402,
-3.21156373514226));
#71949=CARTESIAN_POINT('Ctrl Pts',(27.9475641468296,-0.200605221789714,
-3.21747936065744));
#71950=CARTESIAN_POINT('Ctrl Pts',(27.9746704427703,0.212784087038432,-3.23304974306907));
#71951=CARTESIAN_POINT('Ctrl Pts',(27.9980372784334,0.546731491541803,-3.19357592075675));
#71952=CARTESIAN_POINT('Ctrl Pts',(28.0220809468677,0.905253442884408,-3.09323153453452));
#71953=CARTESIAN_POINT('Ctrl Pts',(28.0245098501895,0.941709773456022,-3.08232836208689));
#71954=CARTESIAN_POINT('Ctrl Pts',(28.027400672289,0.985496463149671,-3.06838340786059));
#71955=CARTESIAN_POINT('Ctrl Pts',(28.0278962864641,0.993017840449468,-3.06595753202135));
#71956=CARTESIAN_POINT('Ctrl Pts',(28.0287060114665,1.00533115511809,-3.0619360440072));
#71957=CARTESIAN_POINT('Ctrl Pts',(28.0290210638473,1.01012834630088,-3.06035680826154));
#71958=CARTESIAN_POINT('Ctrl Pts',(28.0295856348363,1.0187365150749,-3.05750055260106));
#71959=CARTESIAN_POINT('Ctrl Pts',(28.0298353950201,1.02254881632375,-3.05622768051081));
#71960=CARTESIAN_POINT('Ctrl Pts',(28.0303740279289,1.03077943452877,-3.05346247196442));
#71961=CARTESIAN_POINT('Ctrl Pts',(28.0306627521813,1.0351968799202,-3.05196768180817));
#71962=CARTESIAN_POINT('Ctrl Pts',(28.0314616691937,1.04743507700694,-3.04779685125671));
#71963=CARTESIAN_POINT('Ctrl Pts',(28.0319706565559,1.05524886906468,-3.04510027994782));
#71964=CARTESIAN_POINT('Ctrl Pts',(28.0347762105434,1.09840549316296,-3.03002068949016));
#71965=CARTESIAN_POINT('Ctrl Pts',(28.0370394213258,1.13354250914406,-3.01705181828206));
#71966=CARTESIAN_POINT('Ctrl Pts',(28.0542719861256,1.40270933883836,-2.91233728714002));
#71967=CARTESIAN_POINT('Ctrl Pts',(28.0679738256536,1.62553600585687,-2.79409542300904));
#71968=CARTESIAN_POINT('Ctrl Pts',(28.0932840146536,1.99619110573798,-2.53791149606969));
#71969=CARTESIAN_POINT('Ctrl Pts',(28.1046757140041,2.14913753103029,-2.40976449089171));
#71970=CARTESIAN_POINT('Ctrl Pts',(28.1177812751899,2.30190864736685,-2.25558340020309));
#71971=CARTESIAN_POINT('Ctrl Pts',(28.1188698921541,2.31443835301224,-2.24272490199992));
#71972=CARTESIAN_POINT('Ctrl Pts',(28.1205216959687,2.3332050901733,-2.22314094891634));
#71973=CARTESIAN_POINT('Ctrl Pts',(28.1210814106269,2.33952206190571,-2.21649231685619));
#71974=CARTESIAN_POINT('Ctrl Pts',(28.1220561892657,2.35044985172532,-2.20489202332356));
#71975=CARTESIAN_POINT('Ctrl Pts',(28.1224706915524,2.35507363717263,-2.19995261366683));
#71976=CARTESIAN_POINT('Ctrl Pts',(28.1233362691803,2.36468105612943,-2.18962438357931));
#71977=CARTESIAN_POINT('Ctrl Pts',(28.1237874603628,2.36966189760876,-2.18423302968863));
#71978=CARTESIAN_POINT('Ctrl Pts',(28.1248556077881,2.38138920895217,-2.17145184664944));
#71979=CARTESIAN_POINT('Ctrl Pts',(28.125473235972,2.38811973648419,-2.16404755202499));
#71980=CARTESIAN_POINT('Ctrl Pts',(28.1275199636159,2.41025619884647,-2.13946605881892));
#71981=CARTESIAN_POINT('Ctrl Pts',(28.1289553534561,2.42551186621469,-2.12215506104539));
#71982=CARTESIAN_POINT('Ctrl Pts',(28.1436954109205,2.57941165068406,-1.94369355382461));
#71983=CARTESIAN_POINT('Ctrl Pts',(28.1576709689823,2.70194736839792,-1.76939494225287));
#71984=CARTESIAN_POINT('Ctrl Pts',(28.1814809518632,2.87579308642091,-1.46145307721002));
#71985=CARTESIAN_POINT('Ctrl Pts',(28.1910899214638,2.93702002618647,-1.33414549362111));
#71986=CARTESIAN_POINT('Ctrl Pts',(28.2048647682225,3.01370436490644,-1.14360619307692));
#71987=CARTESIAN_POINT('Ctrl Pts',(28.2091411314489,3.03591463867732,-1.08326924731916));
#71988=CARTESIAN_POINT('Ctrl Pts',(28.2174068066051,3.07593729136249,-0.963616677390161));
#71989=CARTESIAN_POINT('Ctrl Pts',(28.2213992222562,3.09387523539417,-0.904369703475032));
#71990=CARTESIAN_POINT('Ctrl Pts',(28.2259358603936,3.11274097505395,-0.834902961275591));
#71991=CARTESIAN_POINT('Ctrl Pts',(28.2265691916793,3.11533924569788,-0.825154969164982));
#71992=CARTESIAN_POINT('Ctrl Pts',(28.2275199508806,3.11918681177818,-0.810442716005799));
#71993=CARTESIAN_POINT('Ctrl Pts',(28.2278393028512,3.1204700938411,-0.805487527529994));
#71994=CARTESIAN_POINT('Ctrl Pts',(28.2284085374021,3.12274134848174,-0.796630549556623));
#71995=CARTESIAN_POINT('Ctrl Pts',(28.2286586789113,3.12373381920064,-0.792729959955686));
#71996=CARTESIAN_POINT('Ctrl Pts',(28.229194754541,3.12584875387049,-0.784352238683463));
#71997=CARTESIAN_POINT('Ctrl Pts',(28.2294805531749,3.12696890372939,-0.779874568213961));
#71998=CARTESIAN_POINT('Ctrl Pts',(28.2302632262783,3.13001602330244,-0.767581945025658));
#71999=CARTESIAN_POINT('Ctrl Pts',(28.2307589745625,3.13192335747994,-0.759762090783327));
#72000=CARTESIAN_POINT('Ctrl Pts',(28.233366777799,3.14183471465703,-0.718455033790611));
#72001=CARTESIAN_POINT('Ctrl Pts',(28.2354507733549,3.14933137284442,-0.684846800540951));
#72002=CARTESIAN_POINT('Ctrl Pts',(28.241462182205,3.16963895771056,-0.586406776887985));
#72003=CARTESIAN_POINT('Ctrl Pts',(28.2453221679367,3.18099691236946,-0.521290545033046));
#72004=CARTESIAN_POINT('Ctrl Pts',(28.2634922060828,3.22566073134494,-0.208714749865713));
#72005=CARTESIAN_POINT('Ctrl Pts',(28.2770469271652,3.23213914685798,0.0417116433594993));
#72006=CARTESIAN_POINT('Ctrl Pts',(28.2992390819529,3.1970764524655,0.429258378900335));
#72007=CARTESIAN_POINT('Ctrl Pts',(28.3073664286035,3.17551456022348,0.567151264390502));
#72008=CARTESIAN_POINT('Ctrl Pts',(28.3169418900405,3.14093327577061,0.72181678609747));
#72009=CARTESIAN_POINT('Ctrl Pts',(28.3180993837322,3.13660662499194,0.740391903908868));
#72010=CARTESIAN_POINT('Ctrl Pts',(28.3198267634744,3.1299347564821,0.767926905585768));
#72011=CARTESIAN_POINT('Ctrl Pts',(28.3203925899964,3.12771532704182,0.776917075577408));
#72012=CARTESIAN_POINT('Ctrl Pts',(28.3214022195633,3.12369494969013,0.792905824274794));
#72013=CARTESIAN_POINT('Ctrl Pts',(28.3218455299276,3.12190914304143,0.799908173562081));
#72014=CARTESIAN_POINT('Ctrl Pts',(28.3227804643318,3.1180998602555,0.814637728043578));
#72015=CARTESIAN_POINT('Ctrl Pts',(28.3232722546208,3.1160711796675,0.822363525387183));
#72016=CARTESIAN_POINT('Ctrl Pts',(28.3245721953189,3.11064330407087,0.842725955597413));
#72017=CARTESIAN_POINT('Ctrl Pts',(28.3253819094511,3.1071958552759,0.85534946673081));
#72018=CARTESIAN_POINT('Ctrl Pts',(28.3290771327382,3.09116256843338,0.912682231214344));
#72019=CARTESIAN_POINT('Ctrl Pts',(28.3319914698645,3.07768850032045,0.957135314934866));
#72020=CARTESIAN_POINT('Ctrl Pts',(28.3398662395477,3.03910939137692,1.075162056889));
#72021=CARTESIAN_POINT('Ctrl Pts',(28.3448805190001,3.01229648263755,1.14814094974775));
#72022=CARTESIAN_POINT('Ctrl Pts',(28.3711270365197,2.86051555190064,1.51921930548057));
#72023=CARTESIAN_POINT('Ctrl Pts',(28.393651532448,2.69388118092647,1.79820365230385));
#72024=CARTESIAN_POINT('Ctrl Pts',(28.417950484081,2.45666141037764,2.0864930467848));
#72025=CARTESIAN_POINT('Ctrl Pts',(28.4211735880942,2.4238548398555,2.12451568840209));
#72026=CARTESIAN_POINT('Ctrl Pts',(28.4248803846094,2.38437191999677,2.16817039242104));
#72027=CARTESIAN_POINT('Ctrl Pts',(28.4254230074428,2.37854697457605,2.17455894314404));
#72028=CARTESIAN_POINT('Ctrl Pts',(28.4262901744422,2.36916416439731,2.18476679930449));
#72029=CARTESIAN_POINT('Ctrl Pts',(28.4266159248978,2.36562265513643,2.18860098227811));
#72030=CARTESIAN_POINT('Ctrl Pts',(28.4271929370244,2.35931916174096,2.19539222639864));
#72031=CARTESIAN_POINT('Ctrl Pts',(28.4274444812251,2.35656090816645,2.19835270634656));
#72032=CARTESIAN_POINT('Ctrl Pts',(28.4279750351948,2.35072135488711,2.20459677716374));
#72033=CARTESIAN_POINT('Ctrl Pts',(28.4282539413585,2.34763875605334,2.20787909765711));
#72034=CARTESIAN_POINT('Ctrl Pts',(28.428998597427,2.33937452469762,2.21664189258255));
#72035=CARTESIAN_POINT('Ctrl Pts',(28.4294633973172,2.33418047708267,2.22211069702994));
#72036=CARTESIAN_POINT('Ctrl Pts',(28.4316675193693,2.3093828903969,2.24803715164135));
#72037=CARTESIAN_POINT('Ctrl Pts',(28.4333880974362,2.28952859473432,2.26825468425339));
#72038=CARTESIAN_POINT('Ctrl Pts',(28.4475416242872,2.12234246979009,2.43406726891935));
#72039=CARTESIAN_POINT('Ctrl Pts',(28.4590453248097,1.9616000965906,2.56536439196085));
#72040=CARTESIAN_POINT('Ctrl Pts',(28.4706129526677,1.78943608566483,2.68030521728786));
#72041=CARTESIAN_POINT('Origin',(-1.72497344927317,0.,0.));
#72042=CARTESIAN_POINT('',(29.9668448649094,1.78943621037805,2.68030513402632));
#72043=CARTESIAN_POINT('',(29.720404475637,1.78943621037806,2.68030513402631));
#72044=CARTESIAN_POINT('',(-1.72497344927317,1.78943621037804,2.68030513402633));
#72045=CARTESIAN_POINT('',(29.1465734493345,-3.22274883168487,-0.00274415265993233));
#72046=CARTESIAN_POINT('Ctrl Pts',(29.1465734493345,-3.22274883168487,-0.00274415265989018));
#72047=CARTESIAN_POINT('Ctrl Pts',(29.1539365945277,-3.22264704388241,-0.12228433941176));
#72048=CARTESIAN_POINT('Ctrl Pts',(29.1612997397209,-3.21589035883655,-0.241535363539396));
#72049=CARTESIAN_POINT('Ctrl Pts',(29.168662884914,-3.20259786199393,-0.35983954320209));
#72050=CARTESIAN_POINT('Ctrl Pts',(29.1761213949534,-3.18913320544464,-0.479675956658851));
#72051=CARTESIAN_POINT('Ctrl Pts',(29.1835799049927,-3.16896241550941,-0.598540812488225));
#72052=CARTESIAN_POINT('Ctrl Pts',(29.1910384150321,-3.14225835233315,-0.715772316936422));
#72053=CARTESIAN_POINT('Ctrl Pts',(29.1965025791201,-3.12269474214264,-0.801657054398812));
#72054=CARTESIAN_POINT('Ctrl Pts',(29.2019667432081,-3.09962565234784,-0.886665604916692));
#72055=CARTESIAN_POINT('Ctrl Pts',(29.2074309072961,-3.0731351666899,-0.97054510959247));
#72056=CARTESIAN_POINT('Ctrl Pts',(29.2136031553889,-3.04321186150635,-1.06529429801687));
#72057=CARTESIAN_POINT('Ctrl Pts',(29.2197754034816,-3.00884990132546,-1.15882509071326));
#72058=CARTESIAN_POINT('Ctrl Pts',(29.2259476515744,-2.97016656609833,-1.2506910618261));
#72059=CARTESIAN_POINT('Ctrl Pts',(29.232111540227,-2.9315356219968,-1.34243261342848));
#72060=CARTESIAN_POINT('Ctrl Pts',(29.2382754288797,-2.88859510281043,-1.4325134282371));
#72061=CARTESIAN_POINT('Ctrl Pts',(29.2444393175323,-2.84151205947572,-1.5205021467772));
#72062=CARTESIAN_POINT('Ctrl Pts',(29.2505966791908,-2.79447887277581,-1.60839769331532));
#72063=CARTESIAN_POINT('Ctrl Pts',(29.2567540408494,-2.74331208662058,-1.69420516700848));
#72064=CARTESIAN_POINT('Ctrl Pts',(29.2629114025079,-2.68822645963843,-1.77751401237791));
#72065=CARTESIAN_POINT('Ctrl Pts',(29.2690642666542,-2.63318106876631,-1.86076200659519));
#72066=CARTESIAN_POINT('Ctrl Pts',(29.2752171308005,-2.57422276693174,-1.94151463980089));
#72067=CARTESIAN_POINT('Ctrl Pts',(29.2813699949468,-2.51161131371327,-2.01938757333195));
#72068=CARTESIAN_POINT('Ctrl Pts',(29.2875205280834,-2.44902358081521,-2.09723100473777));
#72069=CARTESIAN_POINT('Ctrl Pts',(29.2936710612199,-2.38278571840238,-2.17219656607689));
#72070=CARTESIAN_POINT('Ctrl Pts',(29.2998215943565,-2.31319918481417,-2.2439311695939));
#72071=CARTESIAN_POINT('Ctrl Pts',(29.3059714425717,-2.24362040035934,-2.31565778476918));
#72072=CARTESIAN_POINT('Ctrl Pts',(29.3121212907869,-2.17069398856901,-2.38415384567149));
#72073=CARTESIAN_POINT('Ctrl Pts',(29.3182711390021,-2.09475915463473,-2.44910221235742));
#72074=CARTESIAN_POINT('Ctrl Pts',(29.3244219473812,-2.01881246514147,-2.51406071930641));
#72075=CARTESIAN_POINT('Ctrl Pts',(29.3305727557603,-1.9398567506914,-2.5754701494945));
#72076=CARTESIAN_POINT('Ctrl Pts',(29.3367235641395,-1.85826447255666,-2.63305349594985));
#72077=CARTESIAN_POINT('Ctrl Pts',(29.3428809505056,-1.77658493549327,-2.69069842496221));
#72078=CARTESIAN_POINT('Ctrl Pts',(29.3490383368718,-1.69226355973061,-2.74450884837043));
#72079=CARTESIAN_POINT('Ctrl Pts',(29.355195723238,-1.60570188437601,-2.79425106620922));
#72080=CARTESIAN_POINT('Ctrl Pts',(29.361356545975,-1.51909189988605,-2.8440210446421));
#72081=CARTESIAN_POINT('Ctrl Pts',(29.3675173687119,-1.4302395121695,-2.8897180973201));
#72082=CARTESIAN_POINT('Ctrl Pts',(29.3736781914489,-1.3395690772516,-2.93115544619716));
#72083=CARTESIAN_POINT('Ctrl Pts',(29.3798493143656,-1.24874705190247,-2.97266207350651));
#72084=CARTESIAN_POINT('Ctrl Pts',(29.3860204372823,-1.15610131115029,-3.00989460952773));
#72085=CARTESIAN_POINT('Ctrl Pts',(29.392191560199,-1.06207444171456,-3.04271514321612));
#72086=CARTESIAN_POINT('Ctrl Pts',(29.3968870821445,-0.990530699211425,
-3.06768783267297));
#72087=CARTESIAN_POINT('Ctrl Pts',(29.4015826040901,-0.918187732348987,
-3.09010721650955));
#72088=CARTESIAN_POINT('Ctrl Pts',(29.4062781260356,-0.845244453328345,
-3.10993237492677));
#72089=CARTESIAN_POINT('Ctrl Pts',(29.4124503741284,-0.749360753915163,
-3.13599248020334));
#72090=CARTESIAN_POINT('Ctrl Pts',(29.4186226222212,-0.652101953643976,
-3.15765995028383));
#72091=CARTESIAN_POINT('Ctrl Pts',(29.4247948703139,-0.55390700439437,-3.17479205507744));
#72092=CARTESIAN_POINT('Ctrl Pts',(29.4309587589665,-0.455845046364051,
-3.19190095684969));
#72093=CARTESIAN_POINT('Ctrl Pts',(29.4371226476192,-0.356849883553671,
-3.20448662825541));
#72094=CARTESIAN_POINT('Ctrl Pts',(29.4432865362718,-0.257374705550446,
-3.21245635354674));
#72095=CARTESIAN_POINT('Ctrl Pts',(29.4494438979303,-0.158004862658673,
-3.22041763962822));
#72096=CARTESIAN_POINT('Ctrl Pts',(29.4556012595889,-0.0581564457071889,
-3.22377266263295));
#72097=CARTESIAN_POINT('Ctrl Pts',(29.4617586212474,0.0417090601862012,
-3.22248008788237));
#72098=CARTESIAN_POINT('Ctrl Pts',(29.4679114853937,0.141501621471133,-3.22118845726519));
#72099=CARTESIAN_POINT('Ctrl Pts',(29.4740643495401,0.24131081385163,-3.2152559838167));
#72100=CARTESIAN_POINT('Ctrl Pts',(29.4802172136864,0.340672873554422,-3.2046933637595));
#72101=CARTESIAN_POINT('Ctrl Pts',(29.4863677468229,0.439997289986294,-3.19413474534608));
#72102=CARTESIAN_POINT('Ctrl Pts',(29.4925182799594,0.538874478867406,-3.17894951163492));
#72103=CARTESIAN_POINT('Ctrl Pts',(29.498668813096,0.63684441801961,-3.1592003339037));
#72104=CARTESIAN_POINT('Ctrl Pts',(29.5048186613112,0.734803447271938,-3.13945335543435));
#72105=CARTESIAN_POINT('Ctrl Pts',(29.5109685095264,0.831855001849586,-3.11514352923547));
#72106=CARTESIAN_POINT('Ctrl Pts',(29.5171183577416,0.927548889084868,-3.08638471692325));
#72107=CARTESIAN_POINT('Ctrl Pts',(29.5232691661207,1.023257716822,-3.05762141455319));
#72108=CARTESIAN_POINT('Ctrl Pts',(29.5294199744998,1.11760804015507,-3.02440787142227));
#72109=CARTESIAN_POINT('Ctrl Pts',(29.535570782879,1.21016544472654,-2.98690762476676));
#72110=CARTESIAN_POINT('Ctrl Pts',(29.5417281692452,1.30282183489,-2.94936727344181));
#72111=CARTESIAN_POINT('Ctrl Pts',(29.5478855556114,1.39368107399298,-2.90753122741089));
#72112=CARTESIAN_POINT('Ctrl Pts',(29.5540429419775,1.48232945523467,-2.86161090098631));
#72113=CARTESIAN_POINT('Ctrl Pts',(29.5602037647145,1.57102731017963,-2.81566494692396));
#72114=CARTESIAN_POINT('Ctrl Pts',(29.5663645874514,1.65751147405801,-2.76563039061914));
#72115=CARTESIAN_POINT('Ctrl Pts',(29.5725254101884,1.74139537386461,-2.71176321134109));
#72116=CARTESIAN_POINT('Ctrl Pts',(29.5786965331051,1.8254195178044,-2.65780597239864));
#72117=CARTESIAN_POINT('Ctrl Pts',(29.5848676560218,1.90683435964463,-2.60000356287951));
#72118=CARTESIAN_POINT('Ctrl Pts',(29.5910387789385,1.98528457621415,-2.53865372076347));
#72119=CARTESIAN_POINT('Ctrl Pts',(29.5957343008841,2.04497625931844,-2.4919734757084));
#72120=CARTESIAN_POINT('Ctrl Pts',(29.6004298228297,2.10295222776889,-2.44324031750513));
#72121=CARTESIAN_POINT('Ctrl Pts',(29.6051253447753,2.15907050560192,-2.39259944711602));
#72122=CARTESIAN_POINT('Ctrl Pts',(29.6112975928681,2.23283779650938,-2.32603219020704));
#72123=CARTESIAN_POINT('Ctrl Pts',(29.6174698409608,2.30365349464721,-2.25593304337086));
#72124=CARTESIAN_POINT('Ctrl Pts',(29.6236420890536,2.3711601884149,-2.18259408121992));
#72125=CARTESIAN_POINT('Ctrl Pts',(29.6298059777062,2.43857545388016,-2.10935444635694));
#72126=CARTESIAN_POINT('Ctrl Pts',(29.6359698663589,2.50269033102026,-2.0328840343408));
#72127=CARTESIAN_POINT('Ctrl Pts',(29.6421337550115,2.5631817822715,-1.95351393993785));
#72128=CARTESIAN_POINT('Ctrl Pts',(29.6482911166701,2.62360917861084,-1.8742278912025));
#72129=CARTESIAN_POINT('Ctrl Pts',(29.6544484783286,2.68042051528346,-1.79204860809198));
#72130=CARTESIAN_POINT('Ctrl Pts',(29.6606058399872,2.73333149146086,-1.7073419459172));
#72131=CARTESIAN_POINT('Ctrl Pts',(29.6667587041335,2.78620381995504,-1.62269715589984));
#72132=CARTESIAN_POINT('Ctrl Pts',(29.6729115682798,2.83518122269407,-1.53552902441922));
#72133=CARTESIAN_POINT('Ctrl Pts',(29.6790644324261,2.88002193561497,-1.44623345725253));
#72134=CARTESIAN_POINT('Ctrl Pts',(29.6852149655626,2.92484566065228,-1.35697171967064));
#72135=CARTESIAN_POINT('Ctrl Pts',(29.6913654986992,2.9655356151429,-1.26558453562675));
#72136=CARTESIAN_POINT('Ctrl Pts',(29.6975160318357,3.00189578002228,-1.17249276687937));
#72137=CARTESIAN_POINT('Ctrl Pts',(29.7036658800509,3.03825189584574,-1.07941136480051));
#72138=CARTESIAN_POINT('Ctrl Pts',(29.7098157282661,3.07027902263686,-0.984626160020059));
#72139=CARTESIAN_POINT('Ctrl Pts',(29.7159655764813,3.09782951801712,-0.888577424764883));
#72140=CARTESIAN_POINT('Ctrl Pts',(29.7221163848605,3.12538431480304,-0.792513693606092));
#72141=CARTESIAN_POINT('Ctrl Pts',(29.7282671932396,3.14846097214959,-0.695186457715568));
#72142=CARTESIAN_POINT('Ctrl Pts',(29.7344180016188,3.16696216674654,-0.597049576581456));
#72143=CARTESIAN_POINT('Ctrl Pts',(29.740575387985,3.18548314746118,-0.498807742879522));
#72144=CARTESIAN_POINT('Ctrl Pts',(29.7467327743511,3.19941881351695,-0.399754962557698));
#72145=CARTESIAN_POINT('Ctrl Pts',(29.7528901607173,3.20872331301471,-0.300353563348061));
#72146=CARTESIAN_POINT('Ctrl Pts',(29.7590509834543,3.21803300525307,-0.200896689292029));
#72147=CARTESIAN_POINT('Ctrl Pts',(29.7652118061913,3.22270636341255,-0.101091242797806));
#72148=CARTESIAN_POINT('Ctrl Pts',(29.7713726289282,3.22274969555418,-0.00140082313525882));
#72149=CARTESIAN_POINT('Ctrl Pts',(29.7775437518449,3.22279310014211,0.0984562673249473));
#72150=CARTESIAN_POINT('Ctrl Pts',(29.7837148747616,3.21819103660215,0.198197512701616));
#72151=CARTESIAN_POINT('Ctrl Pts',(29.7898859976783,3.20900183790008,0.297363022001526));
#72152=CARTESIAN_POINT('Ctrl Pts',(29.7945815196239,3.20200990389554,0.372816684397168));
#72153=CARTESIAN_POINT('Ctrl Pts',(29.7992770415694,3.19236333657,0.447937103491324));
#72154=CARTESIAN_POINT('Ctrl Pts',(29.8039725635149,3.18010751241009,0.522526336190751));
#72155=CARTESIAN_POINT('Ctrl Pts',(29.810145611432,3.16399518439208,0.620586341636635));
#72156=CARTESIAN_POINT('Ctrl Pts',(29.8163186593491,3.1433146578272,0.718073021349551));
#72157=CARTESIAN_POINT('Ctrl Pts',(29.8224917072661,3.11811839613133,0.81452761169121));
#72158=CARTESIAN_POINT('Ctrl Pts',(29.8286544219621,3.09296431109531,0.910820744254038));
#72159=CARTESIAN_POINT('Ctrl Pts',(29.8348171366581,3.06330964035645,1.00608480836208));
#72160=CARTESIAN_POINT('Ctrl Pts',(29.8409798513541,3.02925817651817,1.09986929336982));
#72161=CARTESIAN_POINT('Ctrl Pts',(29.8471366564326,2.9952393656805,1.19356384553765));
#72162=CARTESIAN_POINT('Ctrl Pts',(29.8532934615111,2.95683228615114,1.28578123187714));
#72163=CARTESIAN_POINT('Ctrl Pts',(29.8594502665896,2.91419092727959,1.37608459109945));
#72164=CARTESIAN_POINT('Ctrl Pts',(29.8656028148151,2.87157905090681,1.46632551402171));
#72165=CARTESIAN_POINT('Ctrl Pts',(29.8717553630405,2.82473889859891,1.55465464853763));
#72166=CARTESIAN_POINT('Ctrl Pts',(29.877907911266,2.77387274597147,1.64065461071388));
#72167=CARTESIAN_POINT('Ctrl Pts',(29.8840578514049,2.72302815568237,1.72661811720819));
#72168=CARTESIAN_POINT('Ctrl Pts',(29.8902077915439,2.6681611795069,1.81025404137264));
#72169=CARTESIAN_POINT('Ctrl Pts',(29.8963577316828,2.60951977773627,1.89117003257329));
#72170=CARTESIAN_POINT('Ctrl Pts',(29.9025088196169,2.5508674314176,1.97210112554378));
#72171=CARTESIAN_POINT('Ctrl Pts',(29.9086599075509,2.48843949847947,2.05031091321287));
#72172=CARTESIAN_POINT('Ctrl Pts',(29.914810995485,2.42252667572612,2.12543691223601));
#72173=CARTESIAN_POINT('Ctrl Pts',(29.9209624546204,2.35660987531491,2.2005674449069));
#72174=CARTESIAN_POINT('Ctrl Pts',(29.9271139137557,2.28720805933935,2.27261349720804));
#72175=CARTESIAN_POINT('Ctrl Pts',(29.933265372891,2.21465049758197,2.34124768789207));
#72176=CARTESIAN_POINT('Ctrl Pts',(29.939422434067,2.14202685875271,2.40994438269339));
#72177=CARTESIAN_POINT('Ctrl Pts',(29.9455794952429,2.06624205488755,2.47522271598359));
#72178=CARTESIAN_POINT('Ctrl Pts',(29.9517365564189,1.9876601493618,2.53679417634522));
#72179=CARTESIAN_POINT('Ctrl Pts',(29.9567726592491,1.923384913903,2.58715589875203));
#72180=CARTESIAN_POINT('Ctrl Pts',(29.9618087620792,1.85723906645935,2.63503831559634));
#72181=CARTESIAN_POINT('Ctrl Pts',(29.9668448649094,1.78943621037805,2.68030513402632));
#72182=CARTESIAN_POINT('Ctrl Pts',(28.7169416469173,1.789436210378,2.68030513402635));
#72183=CARTESIAN_POINT('Ctrl Pts',(28.7230920480723,1.70631863714223,2.7357964261851));
#72184=CARTESIAN_POINT('Ctrl Pts',(28.7292424492274,1.62062725861836,2.78741127799514));
#72185=CARTESIAN_POINT('Ctrl Pts',(28.7353928503824,1.53276367189768,2.83491676925633));
#72186=CARTESIAN_POINT('Ctrl Pts',(28.741588152002,1.44425864476448,2.88276907019202));
#72187=CARTESIAN_POINT('Ctrl Pts',(28.7477834536215,1.35354995273938,2.92645154487067));
#72188=CARTESIAN_POINT('Ctrl Pts',(28.753978755241,1.26107138082195,2.96577418812893));
#72189=CARTESIAN_POINT('Ctrl Pts',(28.7601385685403,1.1691225505343,3.00487158092436));
#72190=CARTESIAN_POINT('Ctrl Pts',(28.7662983818395,1.07542449523086,3.03965886479008));
#72191=CARTESIAN_POINT('Ctrl Pts',(28.7724581951388,0.980420403090224,3.06999892438164));
#72192=CARTESIAN_POINT('Ctrl Pts',(28.7786712409184,0.884595295242538,3.10060117968409));
#72193=CARTESIAN_POINT('Ctrl Pts',(28.7848842866981,0.78744190608317,3.12667886497971));
#72194=CARTESIAN_POINT('Ctrl Pts',(28.7910973324778,0.689425724449649,3.14814385518945));
#72195=CARTESIAN_POINT('Ctrl Pts',(28.7973103782574,0.591409542816158,3.16960884539918));
#72196=CARTESIAN_POINT('Ctrl Pts',(28.8035234240371,0.492531019570413,3.18646112753636));
#72197=CARTESIAN_POINT('Ctrl Pts',(28.8097364698167,0.393259672669308,3.19866603326325));
#72198=CARTESIAN_POINT('Ctrl Pts',(28.8159087179095,0.294640186622187,3.21079079602322));
#72199=CARTESIAN_POINT('Ctrl Pts',(28.8220809660022,0.195285858324367,3.21837175495798));
#72200=CARTESIAN_POINT('Ctrl Pts',(28.828253214095,0.0956515038647144,3.22133021472627));
#72201=CARTESIAN_POINT('Ctrl Pts',(28.8344171027476,-0.00384790990404077,
3.22428466767777));
#72202=CARTESIAN_POINT('Ctrl Pts',(28.8405809914002,-0.103626165660649,
3.22262905216384));
#72203=CARTESIAN_POINT('Ctrl Pts',(28.8467448800529,-0.203221485069067,
3.2163362060746));
#72204=CARTESIAN_POINT('Ctrl Pts',(28.8529022417114,-0.302711342146973,
3.21005002353357));
#72205=CARTESIAN_POINT('Ctrl Pts',(28.8590596033699,-0.402018216875769,
3.19913640000185));
#72206=CARTESIAN_POINT('Ctrl Pts',(28.8652169650284,-0.500679444997268,
3.18362021225165));
#72207=CARTESIAN_POINT('Ctrl Pts',(28.8713698291747,-0.599268608149499,
3.16811535796663));
#72208=CARTESIAN_POINT('Ctrl Pts',(28.877522693321,-0.697212634505651,3.14801469066403));
#72209=CARTESIAN_POINT('Ctrl Pts',(28.8836755574673,-0.794054021945161,
3.12339491142774));
#72210=CARTESIAN_POINT('Ctrl Pts',(28.8898260906039,-0.890858721069464,
3.09878445938353));
#72211=CARTESIAN_POINT('Ctrl Pts',(28.8959766237404,-0.986561190796377,
3.0696584041735));
#72212=CARTESIAN_POINT('Ctrl Pts',(28.902127156877,-1.08071504194242,3.03614435767132));
#72213=CARTESIAN_POINT('Ctrl Pts',(28.9082770050922,-1.17485840814676,3.00263404328226));
#72214=CARTESIAN_POINT('Ctrl Pts',(28.9144268533074,-1.26745308940907,2.96473685476253));
#72215=CARTESIAN_POINT('Ctrl Pts',(28.9205767015226,-1.35806972334827,2.92262967018142));
#72216=CARTESIAN_POINT('Ctrl Pts',(28.9267275099017,-1.44870050508751,2.88051591148691));
#72217=CARTESIAN_POINT('Ctrl Pts',(28.9328783182809,-1.53735223212915,2.83419103422965));
#72218=CARTESIAN_POINT('Ctrl Pts',(28.93902912666,-1.62361824099614,2.78387883536705));
#72219=CARTESIAN_POINT('Ctrl Pts',(28.9451865130262,-1.70997650711697,2.73351283008216));
#72220=CARTESIAN_POINT('Ctrl Pts',(28.9513438993924,-1.79394358421042,2.67915120720089));
#72221=CARTESIAN_POINT('Ctrl Pts',(28.9575012857586,-1.87514013020339,2.62106219968181));
#72222=CARTESIAN_POINT('Ctrl Pts',(28.9636621084956,-1.9563819911109,2.56294077331559));
#72223=CARTESIAN_POINT('Ctrl Pts',(28.9698229312325,-2.03484990052825,2.50108808850675));
#72224=CARTESIAN_POINT('Ctrl Pts',(28.9759837539695,-2.11019772621331,2.43581261980148));
#72225=CARTESIAN_POINT('Ctrl Pts',(28.9821548768862,-2.18567152470756,2.37042801809751));
#72226=CARTESIAN_POINT('Ctrl Pts',(28.9883259998029,-2.25801450496965,2.30160950151284));
#72227=CARTESIAN_POINT('Ctrl Pts',(28.9944971227196,-2.32691741852836,2.22970242181536));
#72228=CARTESIAN_POINT('Ctrl Pts',(28.9991926446652,-2.37934469101972,2.1749893209224));
#72229=CARTESIAN_POINT('Ctrl Pts',(29.0038881666108,-2.42978110979645,2.11848886705525));
#72230=CARTESIAN_POINT('Ctrl Pts',(29.0085836885564,-2.47810684884475,2.06036501819672));
#72231=CARTESIAN_POINT('Ctrl Pts',(29.0147236408184,-2.54129848850042,1.98436118701271));
#72232=CARTESIAN_POINT('Ctrl Pts',(29.0208635930804,-2.60110917768486,1.90530443147936));
#72233=CARTESIAN_POINT('Ctrl Pts',(29.0270035453424,-2.65722736051133,1.82352963152509));
#72234=CARTESIAN_POINT('Ctrl Pts',(29.0331355937507,-2.71327330337753,1.74186009884785));
#72235=CARTESIAN_POINT('Ctrl Pts',(29.039267642159,-2.76563593488611,1.65747982917819));
#72236=CARTESIAN_POINT('Ctrl Pts',(29.0453996905672,-2.81404291051849,1.57075779809003));
#72237=CARTESIAN_POINT('Ctrl Pts',(29.0515255272026,-2.86240084982258,1.48412361653038));
#72238=CARTESIAN_POINT('Ctrl Pts',(29.057651363838,-2.90681088164606,1.39515276731076));
#72239=CARTESIAN_POINT('Ctrl Pts',(29.0637772004734,-2.94704370153479,1.30424345263609));
#72240=CARTESIAN_POINT('Ctrl Pts',(29.0698985113498,-2.98724679747584,1.21340130162832));
#72241=CARTESIAN_POINT('Ctrl Pts',(29.0760198222262,-3.02327863810538,1.12062393158621));
#72242=CARTESIAN_POINT('Ctrl Pts',(29.0821411331026,-3.05495616561474,1.02633346855322));
#72243=CARTESIAN_POINT('Ctrl Pts',(29.0882604710991,-3.08662348355351,0.932073395049127));
#72244=CARTESIAN_POINT('Ctrl Pts',(29.0943798090956,-3.11393913225344,0.83630161145799));
#72245=CARTESIAN_POINT('Ctrl Pts',(29.1004991470922,-3.13676878203506,0.739458701044398));
#72246=CARTESIAN_POINT('Ctrl Pts',(29.1066172902293,-3.15959397410869,0.642634700137558));
#72247=CARTESIAN_POINT('Ctrl Pts',(29.1127354333664,-3.17793481269061,0.54474041657791));
#72248=CARTESIAN_POINT('Ctrl Pts',(29.1188535765035,-3.19170760561652,0.446228778486655));
#72249=CARTESIAN_POINT('Ctrl Pts',(29.1249740935066,-3.20548574244542,0.347678917455325));
#72250=CARTESIAN_POINT('Ctrl Pts',(29.1310946105096,-3.21469223594896,0.248511658979369));
#72251=CARTESIAN_POINT('Ctrl Pts',(29.1372151275126,-3.21929509697444,0.149186598246397));
#72252=CARTESIAN_POINT('Ctrl Pts',(29.1403345680994,-3.22164103466096,0.0985636483246456));
#72253=CARTESIAN_POINT('Ctrl Pts',(29.1434540086863,-3.22279195468255,0.0478997648342351));
#72254=CARTESIAN_POINT('Ctrl Pts',(29.1465734492731,-3.22274883168572,-0.00274415166250658));
#72255=CARTESIAN_POINT('',(28.9000265507269,-3.22274949573006,0.00180285098271473));
#72256=CARTESIAN_POINT('Ctrl Pts',(28.4706129526677,1.78943608566483,2.68030521728786));
#72257=CARTESIAN_POINT('Ctrl Pts',(28.4727295044825,1.75793489507861,2.7013361680963));
#72258=CARTESIAN_POINT('Ctrl Pts',(28.4748473913004,1.72605128848407,2.72181956088802));
#72259=CARTESIAN_POINT('Ctrl Pts',(28.4890742403561,1.51003995035203,2.85526737105806));
#72260=CARTESIAN_POINT('Ctrl Pts',(28.5013624938769,1.31536319151967,2.95001232999312));
#72261=CARTESIAN_POINT('Ctrl Pts',(28.5154841624719,1.09587243875544,3.03075935681712));
#72262=CARTESIAN_POINT('Ctrl Pts',(28.5165707468582,1.07900356595487,3.03680588210346));
#72263=CARTESIAN_POINT('Ctrl Pts',(28.5182199797039,1.05343481829922,3.04573088050518));
#72264=CARTESIAN_POINT('Ctrl Pts',(28.5187791713373,1.04477146750845,3.04871351406174));
#72265=CARTESIAN_POINT('Ctrl Pts',(28.5197532938551,1.02969094157001,3.05383363581636));
#72266=CARTESIAN_POINT('Ctrl Pts',(28.5201676649291,1.02327950743741,3.05598795137482));
#72267=CARTESIAN_POINT('Ctrl Pts',(28.5210242119371,1.01003396508126,3.06039224924279));
#72268=CARTESIAN_POINT('Ctrl Pts',(28.521466473438,1.0031990139534,3.06263955876425));
#72269=CARTESIAN_POINT('Ctrl Pts',(28.5225032579769,0.987186039440626,3.06784521674254));
#72270=CARTESIAN_POINT('Ctrl Pts',(28.5230983797989,0.978002186986164,3.07078528545501));
#72271=CARTESIAN_POINT('Ctrl Pts',(28.5243615879796,0.958525617742078,3.07692417423077));
#72272=CARTESIAN_POINT('Ctrl Pts',(28.5250300065371,0.948229790891023,3.08011265913365));
#72273=CARTESIAN_POINT('Ctrl Pts',(28.5268349413851,0.92045626586622,3.08856130954047));
#72274=CARTESIAN_POINT('Ctrl Pts',(28.5279746068773,0.902949755768552,3.09372468338722));
#72275=CARTESIAN_POINT('Ctrl Pts',(28.537049582533,0.763801217389873,3.13348350209853));
#72276=CARTESIAN_POINT('Ctrl Pts',(28.5452117401538,0.640277226405743,3.16103611379191));
#72277=CARTESIAN_POINT('Ctrl Pts',(28.5689797169024,0.284827672248869,3.21863040137646));
#72278=CARTESIAN_POINT('Ctrl Pts',(28.5850097161605,0.0508145721802403,
3.23080647441244));
#72279=CARTESIAN_POINT('Ctrl Pts',(28.6028215701293,-0.215184034125109,
3.21572543488327));
#72280=CARTESIAN_POINT('Ctrl Pts',(28.6050048580802,-0.247914768802032,
3.21336779972816));
#72281=CARTESIAN_POINT('Ctrl Pts',(28.6124861683806,-0.360676076150754,
3.20351225285942));
#72282=CARTESIAN_POINT('Ctrl Pts',(28.6177100565749,-0.440465734777603,
3.19352006309415));
#72283=CARTESIAN_POINT('Ctrl Pts',(28.6234706604028,-0.530594618158025,
3.17879008952027));
#72284=CARTESIAN_POINT('Ctrl Pts',(28.6241573930998,-0.541375115963997,
3.17697184028573));
#72285=CARTESIAN_POINT('Ctrl Pts',(28.6251639226805,-0.557232459611563,
3.17421426488825));
#72286=CARTESIAN_POINT('Ctrl Pts',(28.6254860804061,-0.562316495106303,
3.17331756584224));
#72287=CARTESIAN_POINT('Ctrl Pts',(28.6260590295858,-0.571374123468075,
3.17169757158011));
#72288=CARTESIAN_POINT('Ctrl Pts',(28.6263100894441,-0.575348529106249,
3.17097901999995));
#72289=CARTESIAN_POINT('Ctrl Pts',(28.6268421416797,-0.583782908579059,
3.16943774914286));
#72290=CARTESIAN_POINT('Ctrl Pts',(28.6271230211045,-0.588242485315028,
3.1686130892104));
#72291=CARTESIAN_POINT('Ctrl Pts',(28.627878534898,-0.600256045964039,3.1663653183137));
#72292=CARTESIAN_POINT('Ctrl Pts',(28.6283521702342,-0.607806761761256,
3.16492457934481));
#72293=CARTESIAN_POINT('Ctrl Pts',(28.6306640656055,-0.644753076792489,
3.15773782044793));
#72294=CARTESIAN_POINT('Ctrl Pts',(28.6324812895651,-0.674073902545802,
3.15160898561473));
#72295=CARTESIAN_POINT('Ctrl Pts',(28.637530472391,-0.756162766545356,3.13325213706511));
#72296=CARTESIAN_POINT('Ctrl Pts',(28.6407180921002,-0.808716082753272,
3.1201009711335));
#72297=CARTESIAN_POINT('Ctrl Pts',(28.6535268632144,-1.02140915835613,3.06114004849999));
#72298=CARTESIAN_POINT('Ctrl Pts',(28.6627656154892,-1.17822366782285,3.00427228577279));
#72299=CARTESIAN_POINT('Ctrl Pts',(28.6854293264578,-1.54743747174325,2.83699934920233));
#72300=CARTESIAN_POINT('Ctrl Pts',(28.6989100470409,-1.75326871871093,2.7146186528809));
#72301=CARTESIAN_POINT('Ctrl Pts',(28.7145128574428,-1.95934218713017,2.55880460220443));
#72302=CARTESIAN_POINT('Ctrl Pts',(28.7157037052972,-1.9748893587462,2.54682445269971));
#72303=CARTESIAN_POINT('Ctrl Pts',(28.7174651636032,-1.99761535818559,2.52897930859047));
#72304=CARTESIAN_POINT('Ctrl Pts',(28.7180314036468,-2.00488006208335,2.52322400836126));
#72305=CARTESIAN_POINT('Ctrl Pts',(28.7190426952652,-2.01778144644494,2.51291228039299));
#72306=CARTESIAN_POINT('Ctrl Pts',(28.7194872565306,-2.02342779457625,2.50836800596334));
#72307=CARTESIAN_POINT('Ctrl Pts',(28.7199376348755,-2.02912255966154,2.50375302438614));
#72308=CARTESIAN_POINT('Ctrl Pts',(28.7199426831262,-2.02918638854648,2.50370129404203));
#72309=CARTESIAN_POINT('Ctrl Pts',(28.7199525544446,-2.02931119283795,2.5036001380579));
#72310=CARTESIAN_POINT('Ctrl Pts',(28.7199573775245,-2.02937216868127,2.50355071241681));
#72311=CARTESIAN_POINT('Ctrl Pts',(28.7199668101851,-2.02949141543693,2.50345404647158));
#72312=CARTESIAN_POINT('Ctrl Pts',(28.7199714197684,-2.02954968663765,2.50340680625344));
#72313=CARTESIAN_POINT('Ctrl Pts',(28.719980436379,-2.02966366319617,2.50331439934023));
#72314=CARTESIAN_POINT('Ctrl Pts',(28.7199848434139,-2.02971936888273,2.50326923266861));
#72315=CARTESIAN_POINT('Ctrl Pts',(28.7199934652108,-2.0298283450773,2.50318086776095));
#72316=CARTESIAN_POINT('Ctrl Pts',(28.7199976799805,-2.02988161589276,2.50313766953882));
#72317=CARTESIAN_POINT('Ctrl Pts',(28.7200059269046,-2.02998584503108,2.5030531428194));
#72318=CARTESIAN_POINT('Ctrl Pts',(28.7200099590702,-2.03003680368479,2.5030118142929));
#72319=CARTESIAN_POINT('Ctrl Pts',(28.7200178498728,-2.03013652390136,2.50293093407779));
#72320=CARTESIAN_POINT('Ctrl Pts',(28.7200217085217,-2.03018528578732,2.50289138234451));
#72321=CARTESIAN_POINT('Ctrl Pts',(28.7200292608351,-2.03028072095256,2.50281396836442));
#72322=CARTESIAN_POINT('Ctrl Pts',(28.7200329545167,-2.03032739460655,2.50277610601144));
#72323=CARTESIAN_POINT('Ctrl Pts',(28.7200401849441,-2.03041875547619,2.50270198849596));
#72324=CARTESIAN_POINT('Ctrl Pts',(28.7200437217096,-2.03046344308596,2.50266573319381));
#72325=CARTESIAN_POINT('Ctrl Pts',(28.7200506458915,-2.03055092815146,2.50259475219629));
#72326=CARTESIAN_POINT('Ctrl Pts',(28.7200540333285,-2.0305937259991,2.50256002634706));
#72327=CARTESIAN_POINT('Ctrl Pts',(28.7200606660094,-2.03067752233993,2.50249203106638));
#72328=CARTESIAN_POINT('Ctrl Pts',(28.7200639112747,-2.03071852122213,2.50245876146894));
#72329=CARTESIAN_POINT('Ctrl Pts',(28.7200702663552,-2.03079880517355,2.50239360971951));
#72330=CARTESIAN_POINT('Ctrl Pts',(28.7200733761979,-2.03083809069897,2.50236172733389));
#72331=CARTESIAN_POINT('Ctrl Pts',(28.7200794668121,-2.03091502883903,2.50229928475532));
#72332=CARTESIAN_POINT('Ctrl Pts',(28.7200824476102,-2.0309526818909,2.50226872433223));
#72333=CARTESIAN_POINT('Ctrl Pts',(28.7200882861469,-2.03102643131658,2.50220886417468));
#72334=CARTESIAN_POINT('Ctrl Pts',(28.7200911439205,-2.0310625282243,2.50217956412083));
#72335=CARTESIAN_POINT('Ctrl Pts',(28.720096742103,-2.03113323756459,2.5021221664314));
#72336=CARTESIAN_POINT('Ctrl Pts',(28.7200994825457,-2.03116785050777,2.50209406848553));
#72337=CARTESIAN_POINT('Ctrl Pts',(28.7201048514603,-2.03123566029126,2.50203901981741));
#72338=CARTESIAN_POINT('Ctrl Pts',(28.7201074799629,-2.0312688575962,2.50201206881331));
#72339=CARTESIAN_POINT('Ctrl Pts',(28.7201126300838,-2.03133390056996,2.50195926197395));
#72340=CARTESIAN_POINT('Ctrl Pts',(28.7201151517418,-2.03136574680939,2.50193340576271));
#72341=CARTESIAN_POINT('Ctrl Pts',(28.720120093006,-2.03142814889091,2.50188273904716));
#72342=CARTESIAN_POINT('Ctrl Pts',(28.7201225126508,-2.03145870528253,2.50185792817662));
#72343=CARTESIAN_POINT('Ctrl Pts',(28.7201276943124,-2.03152414011088,2.50180479507587));
#72344=CARTESIAN_POINT('Ctrl Pts',(28.7201304563826,-2.03155901899685,2.50177647219966));
#72345=CARTESIAN_POINT('Ctrl Pts',(28.7201359554465,-2.03162845818275,2.50172008273973));
#72346=CARTESIAN_POINT('Ctrl Pts',(28.7201386919801,-2.03166301269002,2.50169202088279));
#72347=CARTESIAN_POINT('Ctrl Pts',(28.7201441397585,-2.03173180049443,2.50163615565982));
#72348=CARTESIAN_POINT('Ctrl Pts',(28.7201468510127,-2.03176603392591,2.50160835220658));
#72349=CARTESIAN_POINT('Ctrl Pts',(28.7201522486444,-2.03183418483247,2.50155299958952));
#72350=CARTESIAN_POINT('Ctrl Pts',(28.7201549350277,-2.03186810239707,2.50152545037433));
#72351=CARTESIAN_POINT('Ctrl Pts',(28.7201602833151,-2.03193562663903,2.50147060217975));
#72352=CARTESIAN_POINT('Ctrl Pts',(28.7201629452272,-2.03196923343427,2.50144330312541));
#72353=CARTESIAN_POINT('Ctrl Pts',(28.7201682449533,-2.03203614099672,2.50138895136757));
#72354=CARTESIAN_POINT('Ctrl Pts',(28.720170882781,-2.03206944195467,2.5013618985294));
#72355=CARTESIAN_POINT('Ctrl Pts',(28.7206759851055,-2.03844588039425,2.49618163325451));
#72356=CARTESIAN_POINT('Ctrl Pts',(28.721179424105,-2.04476934623587,2.49100435010067));
#72357=CARTESIAN_POINT('Ctrl Pts',(28.7225532920708,-2.06193840546178,2.47683790474673));
#72358=CARTESIAN_POINT('Ctrl Pts',(28.7234256375139,-2.07274476785869,2.46780167588261));
#72359=CARTESIAN_POINT('Ctrl Pts',(28.7253669157401,-2.09658027330571,2.44760353392396));
#72360=CARTESIAN_POINT('Ctrl Pts',(28.7264372253725,-2.10958015509097,2.43640789946328));
#72361=CARTESIAN_POINT('Ctrl Pts',(28.7296998049574,-2.14877495982948,2.40210405235703));
#72362=CARTESIAN_POINT('Ctrl Pts',(28.7319053879873,-2.17468346662151,2.37867386844445));
#72363=CARTESIAN_POINT('Ctrl Pts',(28.7400861426802,-2.26861112306329,2.29091368874828));
#72364=CARTESIAN_POINT('Ctrl Pts',(28.7461659480859,-2.33419368736704,2.22405464748236));
#72365=CARTESIAN_POINT('Ctrl Pts',(28.7671310659061,-2.5465483442188,1.98781472318676));
#72366=CARTESIAN_POINT('Ctrl Pts',(28.7824746059258,-2.67853733533576,1.80602848377298));
#72367=CARTESIAN_POINT('Ctrl Pts',(28.8003815918656,-2.8121610109073,1.57471495854765));
#72368=CARTESIAN_POINT('Ctrl Pts',(28.8032560882735,-2.83297843608909,1.53694832855815));
#72369=CARTESIAN_POINT('Ctrl Pts',(28.8113903376117,-2.89022355897624,1.42797782149335));
#72370=CARTESIAN_POINT('Ctrl Pts',(28.8165870148902,-2.9247704374252,1.35581459108444));
#72371=CARTESIAN_POINT('Ctrl Pts',(28.82232103569,-2.96094428794717,1.27241726824758));
#72372=CARTESIAN_POINT('Ctrl Pts',(28.8230068946184,-2.96523833001631,1.26237808723768));
#72373=CARTESIAN_POINT('Ctrl Pts',(28.8240123900179,-2.97148636917695,1.24756280157262));
#72374=CARTESIAN_POINT('Ctrl Pts',(28.8243343804688,-2.97347999505174,1.24280364739755));
#72375=CARTESIAN_POINT('Ctrl Pts',(28.8249071414465,-2.97701360861734,1.23431108152394));
#72376=CARTESIAN_POINT('Ctrl Pts',(28.8251581797195,-2.9785580154974,1.23057954674583));
#72377=CARTESIAN_POINT('Ctrl Pts',(28.8256903062262,-2.98182247472593,1.22264993903493));
#72378=CARTESIAN_POINT('Ctrl Pts',(28.8259712810604,-2.98354067259231,1.21845114789025));
#72379=CARTESIAN_POINT('Ctrl Pts',(28.8267273202313,-2.98814884432928,1.20712188346871));
#72380=CARTESIAN_POINT('Ctrl Pts',(28.8272013831376,-2.99102218193026,1.19998461134786));
#72381=CARTESIAN_POINT('Ctrl Pts',(28.8295186355071,-3.00498587026777,1.16493752107379));
#72382=CARTESIAN_POINT('Ctrl Pts',(28.8313406712834,-3.01571171473066,1.13688280614774));
#72383=CARTESIAN_POINT('Ctrl Pts',(28.8364066778901,-3.04474754066777,1.05763215788102));
#72384=CARTESIAN_POINT('Ctrl Pts',(28.8396059511832,-3.06215717023721,1.00611506704069));
#72385=CARTESIAN_POINT('Ctrl Pts',(28.8614999018027,-3.17387395674761,0.645708082223044));
#72386=CARTESIAN_POINT('Ctrl Pts',(28.8787363876768,-3.2225834237722,0.324626768808879));
#72387=CARTESIAN_POINT('Ctrl Pts',(28.8975369561408,-3.22274957354346,0.00165792806279125));
#72388=CARTESIAN_POINT('Ctrl Pts',(28.9000265507269,-3.22274949573006,0.00180285098271473));
#72389=CARTESIAN_POINT('Ctrl Pts',(28.9062469553981,-3.22280611626949,-0.0994111798219162));
#72390=CARTESIAN_POINT('Ctrl Pts',(28.9124673600693,-3.2180902853374,-0.200629471102156));
#72391=CARTESIAN_POINT('Ctrl Pts',(28.9186877647406,-3.20862730534657,-0.301377467446362));
#72392=CARTESIAN_POINT('Ctrl Pts',(28.9249096482869,-3.199162075572,-0.402149416203597));
#72393=CARTESIAN_POINT('Ctrl Pts',(28.9311315318332,-3.18494749082946,-0.502450428911549));
#72394=CARTESIAN_POINT('Ctrl Pts',(28.9373534153795,-3.16606066637834,-0.601811780635709));
#72395=CARTESIAN_POINT('Ctrl Pts',(28.9435782946896,-3.14716474814318,-0.701220973683151));
#72396=CARTESIAN_POINT('Ctrl Pts',(28.9498031739997,-3.12359219348165,-0.799689192911505));
#72397=CARTESIAN_POINT('Ctrl Pts',(28.9560280533098,-3.09547090486905,-0.896759410103493));
#72398=CARTESIAN_POINT('Ctrl Pts',(28.9622617721606,-3.06730968306884,-0.993967470310051));
#72399=CARTESIAN_POINT('Ctrl Pts',(28.9684954910114,-3.03458694818972,-1.08977316063798));
#72400=CARTESIAN_POINT('Ctrl Pts',(28.9747292098621,-2.99748007068733,-1.18373594535788));
#72401=CARTESIAN_POINT('Ctrl Pts',(28.9809679115004,-2.96034353261007,-1.27777383718453));
#72402=CARTESIAN_POINT('Ctrl Pts',(28.9872066131386,-2.9188160442815,-1.3699655066406));
#72403=CARTESIAN_POINT('Ctrl Pts',(28.9934453147768,-2.87312170876266,-1.45989356089297));
#72404=CARTESIAN_POINT('Ctrl Pts',(28.9996951751885,-2.82734564265821,-1.54998246380312));
#72405=CARTESIAN_POINT('Ctrl Pts',(29.0059450356002,-2.77738805389628,-1.63779930163882));
#72406=CARTESIAN_POINT('Ctrl Pts',(29.0121948960119,-2.72351734831205,-1.72295409571565));
#72407=CARTESIAN_POINT('Ctrl Pts',(29.0151140239309,-2.69835590944289,-1.76272742191107));
#72408=CARTESIAN_POINT('Ctrl Pts',(29.01803315185,-2.67234139295002,-1.80192046270654));
#72409=CARTESIAN_POINT('Ctrl Pts',(29.020952279769,-2.64550411478208,-1.84049600411711));
#72410=CARTESIAN_POINT('Ctrl Pts',(29.0271245278618,-2.58875896911496,-1.92206071059866));
#72411=CARTESIAN_POINT('Ctrl Pts',(29.0332967759546,-2.52813827528339,-2.00114221898893));
#72412=CARTESIAN_POINT('Ctrl Pts',(29.0394690240473,-2.46388676111151,-2.07734917404837));
#72413=CARTESIAN_POINT('Ctrl Pts',(29.0456329127,-2.39972226656004,-2.1534529175277));
#72414=CARTESIAN_POINT('Ctrl Pts',(29.0517968013526,-2.33193700313867,-2.22668951662612));
#72415=CARTESIAN_POINT('Ctrl Pts',(29.0579606900052,-2.26081873786643,-2.2966968012805));
#72416=CARTESIAN_POINT('Ctrl Pts',(29.0641180516638,-2.18977578032973,-2.36662995462615));
#72417=CARTESIAN_POINT('Ctrl Pts',(29.0702754133223,-2.11540714546243,-2.43334028887111));
#72418=CARTESIAN_POINT('Ctrl Pts',(29.0764327749809,-2.03803996333273,-2.49649968362881));
#72419=CARTESIAN_POINT('Ctrl Pts',(29.0825856391272,-1.96072929239533,-2.55961294496656));
#72420=CARTESIAN_POINT('Ctrl Pts',(29.0887385032735,-1.88042476420995,-2.61918014968364));
#72421=CARTESIAN_POINT('Ctrl Pts',(29.0948913674198,-1.79748867799225,-2.67491159012586));
#72422=CARTESIAN_POINT('Ctrl Pts',(29.1010419005564,-1.71458401207297,-2.7306219167373));
#72423=CARTESIAN_POINT('Ctrl Pts',(29.1071924336929,-1.62905012921972,-2.78249912452597));
#72424=CARTESIAN_POINT('Ctrl Pts',(29.1133429668295,-1.54127984800482,-2.83029574296296));
#72425=CARTESIAN_POINT('Ctrl Pts',(29.1194928150447,-1.45351934085925,-2.87808703878441));
#72426=CARTESIAN_POINT('Ctrl Pts',(29.1256426632599,-1.36352331196813,-2.92179844095367));
#72427=CARTESIAN_POINT('Ctrl Pts',(29.1317925114751,-1.27170992941109,-2.96122802531943));
#72428=CARTESIAN_POINT('Ctrl Pts',(29.1379433198542,-1.17988221220785,-3.0006637657501));
#72429=CARTESIAN_POINT('Ctrl Pts',(29.1440941282334,-1.08623697692175,-3.03581618911754));
#72430=CARTESIAN_POINT('Ctrl Pts',(29.1502449366125,-0.991212208981483,
-3.06653157806439));
#72431=CARTESIAN_POINT('Ctrl Pts',(29.1564023229787,-0.896085816725511,
-3.09727981560903));
#72432=CARTESIAN_POINT('Ctrl Pts',(29.1625597093449,-0.79957735983448,-3.12358140921857));
#72433=CARTESIAN_POINT('Ctrl Pts',(29.1687170957111,-0.70213970799351,-3.1453326362976));
#72434=CARTESIAN_POINT('Ctrl Pts',(29.1748779184481,-0.604647677252323,
-3.16709600250133));
#72435=CARTESIAN_POINT('Ctrl Pts',(29.181038741185,-0.506225846727573,-3.18430386996202));
#72436=CARTESIAN_POINT('Ctrl Pts',(29.187199563922,-0.407334917707618,-3.19690410042531));
#72437=CARTESIAN_POINT('Ctrl Pts',(29.1933706868387,-0.308278654545428,
-3.20952539700978));
#72438=CARTESIAN_POINT('Ctrl Pts',(29.1995418097554,-0.208752159497449,
-3.217523634414));
#72439=CARTESIAN_POINT('Ctrl Pts',(29.2057129326721,-0.109219008293064,
-3.22089875201433));
#72440=CARTESIAN_POINT('Ctrl Pts',(29.2104084546176,-0.0334856122647015,
-3.22346683224464));
#72441=CARTESIAN_POINT('Ctrl Pts',(29.2151039765632,0.0422515786952583,
-3.2233594471387));
#72442=CARTESIAN_POINT('Ctrl Pts',(29.2197994985087,0.117790482376118,-3.22059667837524));
#72443=CARTESIAN_POINT('Ctrl Pts',(29.2259717466015,0.217086121834415,-3.21696502795835));
#72444=CARTESIAN_POINT('Ctrl Pts',(29.2321439946942,0.316388421497807,-3.20873054124445));
#72445=CARTESIAN_POINT('Ctrl Pts',(29.238316242787,0.415235843009876,-3.19588747567556));
#72446=CARTESIAN_POINT('Ctrl Pts',(29.2444801314396,0.513949389620937,-3.18306180422889));
#72447=CARTESIAN_POINT('Ctrl Pts',(29.2506440200922,0.612208855622406,-3.16564001540881));
#72448=CARTESIAN_POINT('Ctrl Pts',(29.2568079087449,0.709553981755064,-3.14366835233546));
#72449=CARTESIAN_POINT('Ctrl Pts',(29.2629652704034,0.806796028306152,-3.12171995524291));
#72450=CARTESIAN_POINT('Ctrl Pts',(29.2691226320619,0.903125238486049,-3.0952313574475));
#72451=CARTESIAN_POINT('Ctrl Pts',(29.2752799937205,0.998088711923224,-3.06430032562597));
#72452=CARTESIAN_POINT('Ctrl Pts',(29.2814328578668,1.09298282133614,-3.03339188671058));
#72453=CARTESIAN_POINT('Ctrl Pts',(29.2875857220131,1.18651276557843,-2.99804759926694));
#72454=CARTESIAN_POINT('Ctrl Pts',(29.2937385861594,1.27823894109332,-2.95841558472988));
#72455=CARTESIAN_POINT('Ctrl Pts',(29.2998891192959,1.36993036618858,-2.91879858476339));
#72456=CARTESIAN_POINT('Ctrl Pts',(29.3060396524325,1.45981898207847,-2.87489725747929));
#72457=CARTESIAN_POINT('Ctrl Pts',(29.312190185569,1.54748421332389,-2.82690823551338));
#72458=CARTESIAN_POINT('Ctrl Pts',(29.3183400337842,1.63513968219823,-2.77892455758903));
#72459=CARTESIAN_POINT('Ctrl Pts',(29.3244898819994,1.72057187766139,-2.72685429857199));
#72460=CARTESIAN_POINT('Ctrl Pts',(29.3306397302146,1.80338483155499,-2.6709400427223));
#72461=CARTESIAN_POINT('Ctrl Pts',(29.3367905385938,1.88621071487524,-2.61501705708776));
#72462=CARTESIAN_POINT('Ctrl Pts',(29.3429413469729,1.96641618433717,-2.55524912564648));
#72463=CARTESIAN_POINT('Ctrl Pts',(29.3490921553521,2.0436351083236,-2.49192156909626));
#72464=CARTESIAN_POINT('Ctrl Pts',(29.3552495417182,2.1209366141514,-2.42852628683894));
#72465=CARTESIAN_POINT('Ctrl Pts',(29.3614069280844,2.19524485996242,-2.36156405358489));
#72466=CARTESIAN_POINT('Ctrl Pts',(29.3675643144506,2.26622772210905,-2.29135974348081));
#72467=CARTESIAN_POINT('Ctrl Pts',(29.3737251371876,2.33725019902376,-2.22111625311013));
#72468=CARTESIAN_POINT('Ctrl Pts',(29.3798859599245,2.40494330205086,-2.14762740205811));
#72469=CARTESIAN_POINT('Ctrl Pts',(29.3860467826615,2.46901406612221,-2.07125254466728));
#72470=CARTESIAN_POINT('Ctrl Pts',(29.3922179055782,2.53319194906604,-1.99474999738968));
#72471=CARTESIAN_POINT('Ctrl Pts',(29.3983890284949,2.59373513261231,-1.91535215142283));
#72472=CARTESIAN_POINT('Ctrl Pts',(29.4045601514116,2.65039290562038,-1.83344893802286));
#72473=CARTESIAN_POINT('Ctrl Pts',(29.4092556733572,2.69350302028513,-1.77112991746091));
#72474=CARTESIAN_POINT('Ctrl Pts',(29.4139511953028,2.73436456161787,-1.70736105306669));
#72475=CARTESIAN_POINT('Ctrl Pts',(29.4186467172484,2.77288515458528,-1.64232319656655));
#72476=CARTESIAN_POINT('Ctrl Pts',(29.4248189653411,2.82352034684489,-1.55683114895389));
#72477=CARTESIAN_POINT('Ctrl Pts',(29.4309912134339,2.87028719342223,-1.46884469800217));
#72478=CARTESIAN_POINT('Ctrl Pts',(29.4371634615267,2.91293130511126,-1.37874898883112));
#72479=CARTESIAN_POINT('Ctrl Pts',(29.4433273501793,2.95551766136126,-1.28877530160005));
#72480=CARTESIAN_POINT('Ctrl Pts',(29.4494912388319,2.9939921966713,-1.19669842330112));
#72481=CARTESIAN_POINT('Ctrl Pts',(29.4556551274846,3.0281449442721,-1.10293053225455));
#72482=CARTESIAN_POINT('Ctrl Pts',(29.4618124891431,3.06226152723814,-1.00926193282493));
#72483=CARTESIAN_POINT('Ctrl Pts',(29.4679698508016,3.09206527292834,-0.91390628647984));
#72484=CARTESIAN_POINT('Ctrl Pts',(29.4741272124602,3.11739353567447,-0.817297440492172));
#72485=CARTESIAN_POINT('Ctrl Pts',(29.4802800766065,3.14270329793646,-0.720759160355769));
#72486=CARTESIAN_POINT('Ctrl Pts',(29.4864329407528,3.16354396679903,-0.622969919402475));
#72487=CARTESIAN_POINT('Ctrl Pts',(29.4925858048991,3.17980244518916,-0.524379606839389));
#72488=CARTESIAN_POINT('Ctrl Pts',(29.4987363380356,3.1960547640622,-0.425826645171083));
#72489=CARTESIAN_POINT('Ctrl Pts',(29.5048868711722,3.20772827120792,-0.326473643028091));
#72490=CARTESIAN_POINT('Ctrl Pts',(29.5110374043087,3.21476096630608,-0.22678071349838));
#72491=CARTESIAN_POINT('Ctrl Pts',(29.5171872525239,3.22179287824564,-0.127098885740212));
#72492=CARTESIAN_POINT('Ctrl Pts',(29.5233371007391,3.22418497504372,-0.0270776391539264));
#72493=CARTESIAN_POINT('Ctrl Pts',(29.5294869489544,3.22192721670464,0.0728187665226462));
#72494=CARTESIAN_POINT('Ctrl Pts',(29.5356377573335,3.21966910586612,0.172730768832007));
#72495=CARTESIAN_POINT('Ctrl Pts',(29.5417885657126,3.21275970773648,0.272517457211904));
#72496=CARTESIAN_POINT('Ctrl Pts',(29.5479393740917,3.20124106551578,0.371716562659478));
#72497=CARTESIAN_POINT('Ctrl Pts',(29.5540967604579,3.18971010467375,0.471021756671506));
#72498=CARTESIAN_POINT('Ctrl Pts',(29.5602541468241,3.17356010651732,0.56973768060177));
#72499=CARTESIAN_POINT('Ctrl Pts',(29.5664115331903,3.15288477541773,0.667409286299719));
#72500=CARTESIAN_POINT('Ctrl Pts',(29.5725723559272,3.13219790563933,0.765135401465064));
#72501=CARTESIAN_POINT('Ctrl Pts',(29.5787331786642,3.10698078297506,0.861815617387977));
#72502=CARTESIAN_POINT('Ctrl Pts',(29.5848940014011,3.07737729028909,0.957009182669087));
#72503=CARTESIAN_POINT('Ctrl Pts',(29.5910651243178,3.04772430400328,1.05236190052986));
#72504=CARTESIAN_POINT('Ctrl Pts',(29.5972362472345,3.01367044747031,1.14622259450404));
#72505=CARTESIAN_POINT('Ctrl Pts',(29.6034073701512,2.9754081722579,1.23816952432246));
#72506=CARTESIAN_POINT('Ctrl Pts',(29.6081028920968,2.94629493705372,1.30813066958225));
#72507=CARTESIAN_POINT('Ctrl Pts',(29.6127984140423,2.91474625366956,1.37698424031645));
#72508=CARTESIAN_POINT('Ctrl Pts',(29.6174939359879,2.88086430806338,1.44455474144336));
#72509=CARTESIAN_POINT('Ctrl Pts',(29.6236660414796,2.8363276314235,1.53337388996756));
#72510=CARTESIAN_POINT('Ctrl Pts',(29.6298381469713,2.78760118013189,1.62028778915822));
#72511=CARTESIAN_POINT('Ctrl Pts',(29.636010252463,2.73487137736418,1.70487422168737));
#72512=CARTESIAN_POINT('Ctrl Pts',(29.6421743238165,2.68221021219859,1.789350549312));
#72513=CARTESIAN_POINT('Ctrl Pts',(29.64833839517,2.62555627850347,1.87150506521703));
#72514=CARTESIAN_POINT('Ctrl Pts',(29.6545024665236,2.56514279352223,1.95093823873053));
#72515=CARTESIAN_POINT('Ctrl Pts',(29.6606592480018,2.50480075592461,2.03027747142233));
#72516=CARTESIAN_POINT('Ctrl Pts',(29.6668160294801,2.4407082733548,2.10690142022294));
#72517=CARTESIAN_POINT('Ctrl Pts',(29.6729728109583,2.3731422778064,2.18043878423308));
#72518=CARTESIAN_POINT('Ctrl Pts',(29.6791253500184,2.30562283957199,2.25392547627254));
#72519=CARTESIAN_POINT('Ctrl Pts',(29.6852778890784,2.23463493812672,2.32432949173243));
#72520=CARTESIAN_POINT('Ctrl Pts',(29.6914304281385,2.16049581681903,2.39131248230077));
#72521=CARTESIAN_POINT('Ctrl Pts',(29.6975807723252,2.08638314410144,2.45827157717639));
#72522=CARTESIAN_POINT('Ctrl Pts',(29.7037311165119,2.00912180615334,2.52181178025222));
#72523=CARTESIAN_POINT('Ctrl Pts',(29.7098814606986,1.92906529208145,2.58163217004024));
#72524=CARTESIAN_POINT('Ctrl Pts',(29.7133891323447,1.88340736530937,2.61574900622882));
#72525=CARTESIAN_POINT('Ctrl Pts',(29.7168968039908,1.83684090763758,2.64865661731778));
#72526=CARTESIAN_POINT('Ctrl Pts',(29.720404475637,1.78943621037806,2.68030513402631));
#72527=CARTESIAN_POINT('Origin',(-1.72497344927317,0.,0.));
#72528=CARTESIAN_POINT('',(31.2170551299057,1.78943621037803,2.68030513402633));
#72529=CARTESIAN_POINT('',(30.9709191047552,1.78943620529092,2.68030513742261));
#72530=CARTESIAN_POINT('',(-1.72497344927317,1.78943621037804,2.68030513402633));
#72531=CARTESIAN_POINT('',(30.3965734492365,-3.22274997554544,-0.000397016205367042));
#72532=CARTESIAN_POINT('Ctrl Pts',(30.3965734492731,-3.22274997554537,-0.000397016795153058));
#72533=CARTESIAN_POINT('Ctrl Pts',(30.3978870394267,-3.22274737029783,-0.0215448914758832));
#72534=CARTESIAN_POINT('Ctrl Pts',(30.3992006295803,-3.22253660744666,-0.0426913043998582));
#72535=CARTESIAN_POINT('Ctrl Pts',(30.4005142197338,-3.22211775644669,-0.0638335812169476));
#72536=CARTESIAN_POINT('Ctrl Pts',(30.4066864678266,-3.22014967509443,-0.163176117705557));
#72537=CARTESIAN_POINT('Ctrl Pts',(30.4128587159193,-3.21357951462047,-0.262602404376855));
#72538=CARTESIAN_POINT('Ctrl Pts',(30.4190309640121,-3.20239380316626,-0.361651063792674));
#72539=CARTESIAN_POINT('Ctrl Pts',(30.4251948526647,-3.1912232411817,-0.460565575759197));
#72540=CARTESIAN_POINT('Ctrl Pts',(30.4313587413174,-3.17544960130822,-0.559103049188145));
#72541=CARTESIAN_POINT('Ctrl Pts',(30.43752262997,-3.15511141149656,-0.656802514873532));
#72542=CARTESIAN_POINT('Ctrl Pts',(30.4436799916286,-3.134794757967,-0.754398525764095));
#72543=CARTESIAN_POINT('Ctrl Pts',(30.4498373532871,-3.10992325187422,-0.851157870179716));
#72544=CARTESIAN_POINT('Ctrl Pts',(30.4559947149457,-3.08058706074934,-0.946626073824156));
#72545=CARTESIAN_POINT('Ctrl Pts',(30.462147579092,-3.05127229761354,-1.04202454477506));
#72546=CARTESIAN_POINT('Ctrl Pts',(30.4683004432383,-3.01749946034137,-1.13613333600877));
#72547=CARTESIAN_POINT('Ctrl Pts',(30.4744533073846,-2.97940928686148,-1.22851042480867));
#72548=CARTESIAN_POINT('Ctrl Pts',(30.4806038405211,-2.9413335438264,-1.32085251659069));
#72549=CARTESIAN_POINT('Ctrl Pts',(30.4867543736577,-2.89894387995318,-1.41146380838497));
#72550=CARTESIAN_POINT('Ctrl Pts',(30.4929049067942,-2.85242985626061,-1.49992049043043));
#72551=CARTESIAN_POINT('Ctrl Pts',(30.4990547550094,-2.8059210123543,-1.58836732196911));
#72552=CARTESIAN_POINT('Ctrl Pts',(30.5052046032246,-2.75528892392457,-1.67465963632566));
#72553=CARTESIAN_POINT('Ctrl Pts',(30.5113544514398,-2.70076950930567,-1.75839745794425));
#72554=CARTESIAN_POINT('Ctrl Pts',(30.517505259819,-2.6462415826758,-1.8421483533873));
#72555=CARTESIAN_POINT('Ctrl Pts',(30.5236560681981,-2.58782536138163,-1.92334359986204));
#72556=CARTESIAN_POINT('Ctrl Pts',(30.5298068765773,-2.52579999391996,-2.0016123383947));
#72557=CARTESIAN_POINT('Ctrl Pts',(30.5359642629434,-2.46370829337835,-2.07996478149378));
#72558=CARTESIAN_POINT('Ctrl Pts',(30.5421216493096,-2.39800000935009,-2.15538412574944));
#72559=CARTESIAN_POINT('Ctrl Pts',(30.5482790356758,-2.32899440781758,-2.22753285292371));
#72560=CARTESIAN_POINT('Ctrl Pts',(30.5544398584128,-2.25995029500473,-2.29972184552276));
#72561=CARTESIAN_POINT('Ctrl Pts',(30.5606006811498,-2.18760551448642,-2.36863628637636));
#72562=CARTESIAN_POINT('Ctrl Pts',(30.5667615038867,-2.11231446345453,-2.43397723283945));
#72563=CARTESIAN_POINT('Ctrl Pts',(30.5729326268034,-2.03689753453418,-2.49942742177238));
#72564=CARTESIAN_POINT('Ctrl Pts',(30.5791037497201,-1.95852483703355,-2.56129191324031));
#72565=CARTESIAN_POINT('Ctrl Pts',(30.5852748726368,-1.87758204846191,-2.61931350047939));
#72566=CARTESIAN_POINT('Ctrl Pts',(30.5899703945824,-1.81599380184881,-2.66346132250063));
#72567=CARTESIAN_POINT('Ctrl Pts',(30.5946659165279,-1.75291825438787,-2.70538516939721));
#72568=CARTESIAN_POINT('Ctrl Pts',(30.5993614384735,-1.68853468528847,-2.74498965008573));
#72569=CARTESIAN_POINT('Ctrl Pts',(30.6055336865663,-1.60390269630269,-2.79704960917627));
#72570=CARTESIAN_POINT('Ctrl Pts',(30.611705934659,-1.51671186461396,-2.8452835428674));
#72571=CARTESIAN_POINT('Ctrl Pts',(30.6178781827518,-1.42734302066416,-2.88943064700666));
#72572=CARTESIAN_POINT('Ctrl Pts',(30.6240420714044,-1.33809521421804,-2.93351796011536));
#72573=CARTESIAN_POINT('Ctrl Pts',(30.6302059600571,-1.24667564460432,-2.97352925447361));
#72574=CARTESIAN_POINT('Ctrl Pts',(30.6363698487097,-1.15349291568567,-3.00924768936739));
#72575=CARTESIAN_POINT('Ctrl Pts',(30.6425272103682,-1.06040885875063,-3.04492830170689));
#72576=CARTESIAN_POINT('Ctrl Pts',(30.6486845720268,-0.965565757693471,
-3.07632493733784));
#72577=CARTESIAN_POINT('Ctrl Pts',(30.6548419336853,-0.869394674850752,
-3.10326770708574));
#72578=CARTESIAN_POINT('Ctrl Pts',(30.6609947978316,-0.773293838104692,
-3.13019079706761));
#72579=CARTESIAN_POINT('Ctrl Pts',(30.6671476619779,-0.675867365100445,
-3.15266637231773));
#72580=CARTESIAN_POINT('Ctrl Pts',(30.6733005261242,-0.577563187726553,
-3.17057381662739));
#72581=CARTESIAN_POINT('Ctrl Pts',(30.6794510592608,-0.479296252845346,
-3.18847447670994));
#72582=CARTESIAN_POINT('Ctrl Pts',(30.6856015923973,-0.380152701174109,
-3.20181036685319));
#72583=CARTESIAN_POINT('Ctrl Pts',(30.6917521255338,-0.280591542845579,
-3.21051178919865));
#72584=CARTESIAN_POINT('Ctrl Pts',(30.6979019737491,-0.181041471614624,
-3.21921224255661));
#72585=CARTESIAN_POINT('Ctrl Pts',(30.7040518219643,-0.0810743189103917,
-3.22327921636538));
#72586=CARTESIAN_POINT('Ctrl Pts',(30.7102016701795,0.018845888805191,-3.2226948963523));
#72587=CARTESIAN_POINT('Ctrl Pts',(30.7163524785586,0.118781696869881,-3.22211048511046));
#72588=CARTESIAN_POINT('Ctrl Pts',(30.7225032869377,0.218670110979054,-3.21687334017127));
#72589=CARTESIAN_POINT('Ctrl Pts',(30.7286540953169,0.318048222807609,-3.20701775649417));
#72590=CARTESIAN_POINT('Ctrl Pts',(30.734811481683,0.417532614639169,-3.19715163275505));
#72591=CARTESIAN_POINT('Ctrl Pts',(30.7409688680492,0.51650518129978,-3.18265725017103));
#72592=CARTESIAN_POINT('Ctrl Pts',(30.7471262544154,0.614509369053244,-3.16362067856527));
#72593=CARTESIAN_POINT('Ctrl Pts',(30.7532870771524,0.712568251884493,-3.14457348285468));
#72594=CARTESIAN_POINT('Ctrl Pts',(30.7594478998893,0.809657257422227,-3.12097915239011));
#72595=CARTESIAN_POINT('Ctrl Pts',(30.7656087226263,0.905333286258208,-3.09297416789939));
#72596=CARTESIAN_POINT('Ctrl Pts',(30.771779845543,1.00116927429686,-3.06492236232878));
#72597=CARTESIAN_POINT('Ctrl Pts',(30.7779509684597,1.09558715600064,-3.03244531454632));
#72598=CARTESIAN_POINT('Ctrl Pts',(30.7841220913764,1.18816202696872,-2.99572838557997));
#72599=CARTESIAN_POINT('Ctrl Pts',(30.788817613322,1.25860096395163,-2.96779098292825));
#72600=CARTESIAN_POINT('Ctrl Pts',(30.7935131352676,1.32797327203204,-2.93739992342364));
#72601=CARTESIAN_POINT('Ctrl Pts',(30.7982086572132,1.39610176927607,-2.90465443939967));
#72602=CARTESIAN_POINT('Ctrl Pts',(30.8043809053059,1.48565645394122,-2.86161060877664));
#72603=CARTESIAN_POINT('Ctrl Pts',(30.8105531533987,1.57337624438467,-2.81434548575309));
#72604=CARTESIAN_POINT('Ctrl Pts',(30.8167254014915,1.65883583090921,-2.76303840881587));
#72605=CARTESIAN_POINT('Ctrl Pts',(30.8228892901441,1.7441796744684,-2.7118008200832));
#72606=CARTESIAN_POINT('Ctrl Pts',(30.8290531787967,1.82726902930238,-2.65653237974099));
#72607=CARTESIAN_POINT('Ctrl Pts',(30.8352170674494,1.90770055077724,-2.59745956100653));
#72608=CARTESIAN_POINT('Ctrl Pts',(30.8413744291079,1.98804690263037,-2.53844929498192));
#72609=CARTESIAN_POINT('Ctrl Pts',(30.8475317907664,2.06574066825636,-2.47564291529061));
#72610=CARTESIAN_POINT('Ctrl Pts',(30.853689152425,2.14040585554809,-2.40931117459648));
#72611=CARTESIAN_POINT('Ctrl Pts',(30.8598420165713,2.21501650526149,-2.34302788449404));
#72612=CARTESIAN_POINT('Ctrl Pts',(30.8659948807176,2.28660265103505,-2.27322464059985));
#72613=CARTESIAN_POINT('Ctrl Pts',(30.8721477448639,2.35482062808022,-2.20021302879241));
#72614=CARTESIAN_POINT('Ctrl Pts',(30.8782982780005,2.42301276077596,-2.12722907740074));
#72615=CARTESIAN_POINT('Ctrl Pts',(30.884448811137,2.48783896398199,-2.05103949030523));
#72616=CARTESIAN_POINT('Ctrl Pts',(30.8905993442735,2.54899241575982,-1.97199270457548));
#72617=CARTESIAN_POINT('Ctrl Pts',(30.8967491924887,2.61013905750953,-1.89295472146958));
#72618=CARTESIAN_POINT('Ctrl Pts',(30.9028990407039,2.6676134951822,-1.81106051587506));
#72619=CARTESIAN_POINT('Ctrl Pts',(30.9090488889191,2.72114983939361,-1.72669079862844));
#72620=CARTESIAN_POINT('Ctrl Pts',(30.9151996972983,2.77469454213108,-1.64230790890077));
#72621=CARTESIAN_POINT('Ctrl Pts',(30.9213505056774,2.82429969741022,-1.55544910664051));
#72622=CARTESIAN_POINT('Ctrl Pts',(30.9275013140565,2.86974385518543,-1.46652233809289));
#72623=CARTESIAN_POINT('Ctrl Pts',(30.9336587004227,2.91523661325236,-1.3775004667399));
#72624=CARTESIAN_POINT('Ctrl Pts',(30.9398160867889,2.95655928961141,-1.28640660033605));
#72625=CARTESIAN_POINT('Ctrl Pts',(30.9459734731551,2.99353742368518,-1.19367133478872));
#72626=CARTESIAN_POINT('Ctrl Pts',(30.9521342958921,3.03053619485585,-1.10088431469213));
#72627=CARTESIAN_POINT('Ctrl Pts',(30.958295118629,3.06318545315432,-1.00645448169995));
#72628=CARTESIAN_POINT('Ctrl Pts',(30.964455941366,3.09136041899844,-0.910828371511226));
#72629=CARTESIAN_POINT('Ctrl Pts',(30.9706270642827,3.11958249011152,-0.815042385578012));
#72630=CARTESIAN_POINT('Ctrl Pts',(30.9767981871994,3.14331522341325,-0.718056549559979));
#72631=CARTESIAN_POINT('Ctrl Pts',(30.982969310116,3.16248479609247,-0.620328523432538));
#72632=CARTESIAN_POINT('Ctrl Pts',(30.9876648320616,3.17707065840917,-0.545968622070545));
#72633=CARTESIAN_POINT('Ctrl Pts',(30.9923603540072,3.18901574554004,-0.471179261065576));
#72634=CARTESIAN_POINT('Ctrl Pts',(30.9970558759527,3.19830772852275,-0.396163143378616));
#72635=CARTESIAN_POINT('Ctrl Pts',(31.0032281240455,3.21052200947129,-0.297554704383292));
#72636=CARTESIAN_POINT('Ctrl Pts',(31.0094003721383,3.21819315552981,-0.198207298740116));
#72637=CARTESIAN_POINT('Ctrl Pts',(31.015572620231,3.22124205852399,-0.0985756709137832));
#72638=CARTESIAN_POINT('Ctrl Pts',(31.0217365088837,3.22428683220878,0.000921019914584459));
#72639=CARTESIAN_POINT('Ctrl Pts',(31.0279003975363,3.22272179245018,0.100700737468478));
#72640=CARTESIAN_POINT('Ctrl Pts',(31.0340642861889,3.2165193579639,0.200301728258884));
#72641=CARTESIAN_POINT('Ctrl Pts',(31.0402216478475,3.21032349128822,0.299797250713579));
#72642=CARTESIAN_POINT('Ctrl Pts',(31.046379009506,3.19950001942366,0.399113991517258));
#72643=CARTESIAN_POINT('Ctrl Pts',(31.0525363711645,3.18407339914241,0.497789264020125));
#72644=CARTESIAN_POINT('Ctrl Pts',(31.0586892353109,3.16865804690377,0.596392461294946));
#72645=CARTESIAN_POINT('Ctrl Pts',(31.0648420994572,3.14864629790938,0.694354693951464));
#72646=CARTESIAN_POINT('Ctrl Pts',(31.0709949636035,3.12411443790773,0.791218390431176));
#72647=CARTESIAN_POINT('Ctrl Pts',(31.07714549674,3.09959187179002,0.888045390143763));
#72648=CARTESIAN_POINT('Ctrl Pts',(31.0832960298766,3.07055270380325,0.983774260013495));
#72649=CARTESIAN_POINT('Ctrl Pts',(31.0894465630131,3.03712414055262,1.07795849519938));
#72650=CARTESIAN_POINT('Ctrl Pts',(31.0955964112283,3.0036992998957,1.17213224206007));
#72651=CARTESIAN_POINT('Ctrl Pts',(31.1017462594435,2.9658861810757,1.26476128686167));
#72652=CARTESIAN_POINT('Ctrl Pts',(31.1078961076587,2.92386127232947,1.35541610683653));
#72653=CARTESIAN_POINT('Ctrl Pts',(31.1140469160379,2.88182980231534,1.44608508057347));
#72654=CARTESIAN_POINT('Ctrl Pts',(31.120197724417,2.83558541895962,1.53477882312855));
#72655=CARTESIAN_POINT('Ctrl Pts',(31.1263485327961,2.78535154997316,1.62109046803753));
#72656=CARTESIAN_POINT('Ctrl Pts',(31.1325059191623,2.73506395833447,1.70749441900567));
#72657=CARTESIAN_POINT('Ctrl Pts',(31.1386633055285,2.68077858011121,1.79151080900805));
#72658=CARTESIAN_POINT('Ctrl Pts',(31.1448206918947,2.62276330379848,1.87276005263571));
#72659=CARTESIAN_POINT('Ctrl Pts',(31.1509815146316,2.56471564978715,1.95405464058799));
#72660=CARTESIAN_POINT('Ctrl Pts',(31.1571423373686,2.50293422077824,2.03257866529377));
#72661=CARTESIAN_POINT('Ctrl Pts',(31.1633031601056,2.43772717698457,2.10798571463159));
#72662=CARTESIAN_POINT('Ctrl Pts',(31.1694742830222,2.37241111459072,2.18351883579362));
#72663=CARTESIAN_POINT('Ctrl Pts',(31.1756454059389,2.30365829668805,2.25592425719654));
#72664=CARTESIAN_POINT('Ctrl Pts',(31.1818165288556,2.23181379417764,2.32489241699877));
#72665=CARTESIAN_POINT('Ctrl Pts',(31.1865120508012,2.17714830739939,2.37736933445314));
#72666=CARTESIAN_POINT('Ctrl Pts',(31.1912075727468,2.12069366115876,2.42785702150719));
#72667=CARTESIAN_POINT('Ctrl Pts',(31.1959030946924,2.06261370459727,2.47623550336141));
#72668=CARTESIAN_POINT('Ctrl Pts',(31.2020759937542,1.98625974149879,2.53983556501688));
#72669=CARTESIAN_POINT('Ctrl Pts',(31.2082488928159,1.90682698354292,2.60001274540606));
#72670=CARTESIAN_POINT('Ctrl Pts',(31.2144217918776,1.82465530069742,2.6564545161054));
#72671=CARTESIAN_POINT('Ctrl Pts',(31.2152995712203,1.81297057929927,2.66448047277323));
#72672=CARTESIAN_POINT('Ctrl Pts',(31.216177350563,1.80123053679588,2.67243095787333));
#72673=CARTESIAN_POINT('Ctrl Pts',(31.2170551299057,1.78943621037803,2.68030513402633));
#72674=CARTESIAN_POINT('Ctrl Pts',(29.9668448649094,1.78943621037805,2.68030513402632));
#72675=CARTESIAN_POINT('Ctrl Pts',(29.9730155973569,1.70635742939051,2.73577052754659));
#72676=CARTESIAN_POINT('Ctrl Pts',(29.9791863298045,1.62079052020137,2.78730753432573));
#72677=CARTESIAN_POINT('Ctrl Pts',(29.9853570622521,1.53315005596254,2.83470782769619));
#72678=CARTESIAN_POINT('Ctrl Pts',(29.9911779689196,1.45047802845725,2.87942094499099));
#72679=CARTESIAN_POINT('Ctrl Pts',(29.9969988755871,1.36596137328465,2.92045337514309));
#72680=CARTESIAN_POINT('Ctrl Pts',(30.0028197822546,1.27996288185344,2.95767012757972));
#72681=CARTESIAN_POINT('Ctrl Pts',(30.0089920303474,1.18877364707692,2.99713322883979));
#72682=CARTESIAN_POINT('Ctrl Pts',(30.0151642784402,1.09559714290483,3.03244459471753));
#72683=CARTESIAN_POINT('Ctrl Pts',(30.0213365265329,1.00084749025507,3.06340037601195));
#72684=CARTESIAN_POINT('Ctrl Pts',(30.0275004151856,0.906226162655928,3.09431423206347));
#72685=CARTESIAN_POINT('Ctrl Pts',(30.0336643038382,0.810036330658838,3.12088409478352));
#72686=CARTESIAN_POINT('Ctrl Pts',(30.0398281924908,0.712713337506968,3.14295358875051));
#72687=CARTESIAN_POINT('Ctrl Pts',(30.0459855541494,0.615493400499778,3.16499971314274));
#72688=CARTESIAN_POINT('Ctrl Pts',(30.0521429158079,0.517143109164207,3.18255484747094));
#72689=CARTESIAN_POINT('Ctrl Pts',(30.0583002774665,0.418113342424336,3.19551228997586));
#72690=CARTESIAN_POINT('Ctrl Pts',(30.0644531416128,0.319155909845194,3.20846026799591));
#72691=CARTESIAN_POINT('Ctrl Pts',(30.0706060057591,0.219520418012922,3.21681717485254));
#72692=CARTESIAN_POINT('Ctrl Pts',(30.0767588699054,0.119667418752613,3.22052748340844));
#72693=CARTESIAN_POINT('Ctrl Pts',(30.0829094030419,0.0198522487554531,
3.22423638631563));
#72694=CARTESIAN_POINT('Ctrl Pts',(30.0890599361785,-0.0801798313424153,
3.2233021726398));
#72695=CARTESIAN_POINT('Ctrl Pts',(30.095210469315,-0.179964563537114,3.21772129283611));
#72696=CARTESIAN_POINT('Ctrl Pts',(30.1013603175302,-0.279738183737156,
3.21214103451735));
#72697=CARTESIAN_POINT('Ctrl Pts',(30.1075101657454,-0.379264077098757,
3.20191516309571));
#72698=CARTESIAN_POINT('Ctrl Pts',(30.1136600139606,-0.478080417042818,
3.18709219780981));
#72699=CARTESIAN_POINT('Ctrl Pts',(30.1198108223397,-0.576912184991273,
3.17226691824295));
#72700=CARTESIAN_POINT('Ctrl Pts',(30.1259616307189,-0.675033749872496,
3.15284318364763));
#72701=CARTESIAN_POINT('Ctrl Pts',(30.132112439098,-0.771991820509954,3.12892093085871));
#72702=CARTESIAN_POINT('Ctrl Pts',(30.1382698254642,-0.869053583035296,
3.10497309439699));
#72703=CARTESIAN_POINT('Ctrl Pts',(30.1444272118304,-0.964948944027739,
3.07651723703857));
#72704=CARTESIAN_POINT('Ctrl Pts',(30.1505845981966,-1.05923828301367,3.04370363575336));
#72705=CARTESIAN_POINT('Ctrl Pts',(30.1567454209335,-1.15358024386045,3.01087172155198));
#72706=CARTESIAN_POINT('Ctrl Pts',(30.1629062436705,-1.24631399455558,2.97367738181617));
#72707=CARTESIAN_POINT('Ctrl Pts',(30.1690670664074,-1.33702041810612,2.93231887148504));
#72708=CARTESIAN_POINT('Ctrl Pts',(30.1752381893241,-1.42787849225677,2.8908912145305));
#72709=CARTESIAN_POINT('Ctrl Pts',(30.1814093122408,-1.51670208233278,2.84528567907598));
#72710=CARTESIAN_POINT('Ctrl Pts',(30.1875804351575,-1.60309704887808,2.79574630722789));
#72711=CARTESIAN_POINT('Ctrl Pts',(30.192275957103,-1.66883378218812,2.75805248540301));
#72712=CARTESIAN_POINT('Ctrl Pts',(30.1969714790486,-1.73316498791198,2.71808212643338));
#72713=CARTESIAN_POINT('Ctrl Pts',(30.2016670009941,-1.79592944037064,2.67595870814742));
#72714=CARTESIAN_POINT('Ctrl Pts',(30.207818424657,-1.87815474833823,2.62077442937924));
#72715=CARTESIAN_POINT('Ctrl Pts',(30.2139698483198,-1.95798373458385,2.56169632975944));
#72716=CARTESIAN_POINT('Ctrl Pts',(30.2201212719827,-2.03502252916728,2.49895995731857));
#72717=CARTESIAN_POINT('Ctrl Pts',(30.2262643515467,-2.11195682447542,2.43630868363202));
#72718=CARTESIAN_POINT('Ctrl Pts',(30.2324074311108,-2.18610811322559,2.37000927244701));
#72719=CARTESIAN_POINT('Ctrl Pts',(30.2385505106748,-2.25711084438849,2.30034088748687));
#72720=CARTESIAN_POINT('Ctrl Pts',(30.2446871053043,-2.32803862160367,2.23074604787349));
#72721=CARTESIAN_POINT('Ctrl Pts',(30.2508236999338,-2.39582413755272,2.1577896088));
#72722=CARTESIAN_POINT('Ctrl Pts',(30.2569602945633,-2.46013513106599,2.08179074342137));
#72723=CARTESIAN_POINT('Ctrl Pts',(30.2630924739142,-2.5243998528322,2.00584655921129));
#72724=CARTESIAN_POINT('Ctrl Pts',(30.269224653265,-2.58519473974204,1.92686463325162));
#72725=CARTESIAN_POINT('Ctrl Pts',(30.2753568326159,-2.64222529150039,1.84520000852365));
#72726=CARTESIAN_POINT('Ctrl Pts',(30.281486766945,-2.69923496408644,1.7635652816262));
#72727=CARTESIAN_POINT('Ctrl Pts',(30.2876167012741,-2.75248278917626,1.67925016568173));
#72728=CARTESIAN_POINT('Ctrl Pts',(30.2937466356033,-2.80171596576564,1.59264095441312));
#72729=CARTESIAN_POINT('Ctrl Pts',(30.2998759946897,-2.85094452223643,1.50603987068885));
#72730=CARTESIAN_POINT('Ctrl Pts',(30.3060053537762,-2.89615896302052,1.41714550021788));
#72731=CARTESIAN_POINT('Ctrl Pts',(30.3121347128627,-2.93715160641279,1.32637023618852));
#72732=CARTESIAN_POINT('Ctrl Pts',(30.3182651655735,-2.97815156387378,1.23557877567937));
#72733=CARTESIAN_POINT('Ctrl Pts',(30.3243956182843,-3.01492804798627,1.14290615409432));
#72734=CARTESIAN_POINT('Ctrl Pts',(30.3305260709951,-3.04732126375728,1.04878533454314));
#72735=CARTESIAN_POINT('Ctrl Pts',(30.3366630861763,-3.07974915551832,0.954563761407506));
#72736=CARTESIAN_POINT('Ctrl Pts',(30.3428001013574,-3.10778426918983,0.858891310021853));
#72737=CARTESIAN_POINT('Ctrl Pts',(30.3489371165386,-3.13131658115752,0.762216525055679));
#72738=CARTESIAN_POINT('Ctrl Pts',(30.3550777343895,-3.15486270751969,0.665484988181035));
#72739=CARTESIAN_POINT('Ctrl Pts',(30.3612183522404,-3.17390068635141,0.567750375655364));
#72740=CARTESIAN_POINT('Ctrl Pts',(30.3673589700913,-3.18837194979263,0.469469777808461));
#72741=CARTESIAN_POINT('Ctrl Pts',(30.3735094707065,-3.20286650341247,0.371031006303314));
#72742=CARTESIAN_POINT('Ctrl Pts',(30.3796599713218,-3.21277962373837,0.272044930090738));
#72743=CARTESIAN_POINT('Ctrl Pts',(30.3858104719371,-3.21810475772262,0.17297205214433));
#72744=CARTESIAN_POINT('Ctrl Pts',(30.3893981310369,-3.22121097079231,0.115181681190473));
#72745=CARTESIAN_POINT('Ctrl Pts',(30.3929857901367,-3.22275709095059,0.0573617640601762));
#72746=CARTESIAN_POINT('Ctrl Pts',(30.3965734492365,-3.22274997554544,-0.000397016205362354));
#72747=CARTESIAN_POINT('',(30.1500265507269,-3.22274893555634,-0.00261932634679408));
#72748=CARTESIAN_POINT('Ctrl Pts',(29.720404475637,1.78943621037806,2.68030513402631));
#72749=CARTESIAN_POINT('Ctrl Pts',(29.7265546697647,1.70631894054126,2.7357962236286));
#72750=CARTESIAN_POINT('Ctrl Pts',(29.7327048638924,1.6206233134869,2.78741395090235));
#72751=CARTESIAN_POINT('Ctrl Pts',(29.7388550580201,1.53275019332222,2.83492405672016));
#72752=CARTESIAN_POINT('Ctrl Pts',(29.7453122327457,1.44049097697766,2.88480558047833));
#72753=CARTESIAN_POINT('Ctrl Pts',(29.7517694074713,1.34583171789474,2.93015853342363));
#72754=CARTESIAN_POINT('Ctrl Pts',(29.7582265821969,1.24926354461491,2.97076726765935));
#72755=CARTESIAN_POINT('Ctrl Pts',(29.764385922519,1.15714953674241,3.0095029415158));
#72756=CARTESIAN_POINT('Ctrl Pts',(29.7705452628411,1.06329923530287,3.04392222124192));
#72757=CARTESIAN_POINT('Ctrl Pts',(29.7767046031631,0.968156156258745,3.07388861535325));
#72758=CARTESIAN_POINT('Ctrl Pts',(29.7828682965992,0.872945834840306,3.10387618821461));
#72759=CARTESIAN_POINT('Ctrl Pts',(29.7890319900352,0.776441336148424,3.12940450066375));
#72760=CARTESIAN_POINT('Ctrl Pts',(29.7951956834712,0.679097560101669,3.15038792315549));
#72761=CARTESIAN_POINT('Ctrl Pts',(29.8013685837513,0.58160837952145,3.17140268904566));
#72762=CARTESIAN_POINT('Ctrl Pts',(29.8075414840315,0.483277847267676,3.18785895065528));
#72763=CARTESIAN_POINT('Ctrl Pts',(29.8137143843116,0.384566885514254,3.19972278065864));
#72764=CARTESIAN_POINT('Ctrl Pts',(29.8145899744502,0.370565307525707,3.201405596205));
#72765=CARTESIAN_POINT('Ctrl Pts',(29.8154655645889,0.356556075577454,3.20299609869579));
#72766=CARTESIAN_POINT('Ctrl Pts',(29.8163411547275,0.342540503666624,3.20449427614527));
#72767=CARTESIAN_POINT('Ctrl Pts',(29.8225134028203,0.243741324487471,3.21505529379159));
#72768=CARTESIAN_POINT('Ctrl Pts',(29.8286856509131,0.144279373311957,3.2210614371678));
#72769=CARTESIAN_POINT('Ctrl Pts',(29.8348578990058,0.044610655767646,3.22244122551397));
#72770=CARTESIAN_POINT('Ctrl Pts',(29.8410217876585,-0.0549230745456297,
3.22381914513128));
#72771=CARTESIAN_POINT('Ctrl Pts',(29.8471856763111,-0.154662584116093,
3.22058315761827));
#72772=CARTESIAN_POINT('Ctrl Pts',(29.8533495649637,-0.254145722276558,
3.2127134192686));
#72773=CARTESIAN_POINT('Ctrl Pts',(29.8595069266223,-0.353523516896889,
3.20485201425172));
#72774=CARTESIAN_POINT('Ctrl Pts',(29.8656642882808,-0.452645049188138,
3.19236664748308));
#72775=CARTESIAN_POINT('Ctrl Pts',(29.8718216499394,-0.5510481070161,3.17528952164271));
#72776=CARTESIAN_POINT('Ctrl Pts',(29.8779745140857,-0.649379288449273,
3.15822486942121));
#72777=CARTESIAN_POINT('Ctrl Pts',(29.884127378232,-0.746992612111663,3.13657520040593));
#72778=CARTESIAN_POINT('Ctrl Pts',(29.8902802423783,-0.843431848303963,
3.11042445331285));
#72779=CARTESIAN_POINT('Ctrl Pts',(29.8964307755149,-0.939834548535634,
3.08428361341839));
#72780=CARTESIAN_POINT('Ctrl Pts',(29.9025813086514,-1.03506362634721,3.0536451972866));
#72781=CARTESIAN_POINT('Ctrl Pts',(29.9087318417879,-1.12867477005597,3.01864387199602));
#72782=CARTESIAN_POINT('Ctrl Pts',(29.9148816900032,-1.2222754892591,2.9836464444413));
#72783=CARTESIAN_POINT('Ctrl Pts',(29.9210315382184,-1.31425822570343,2.94428722580029));
#72784=CARTESIAN_POINT('Ctrl Pts',(29.9271813864336,-1.40419647279428,2.90074987344516));
#72785=CARTESIAN_POINT('Ctrl Pts',(29.9333321948127,-1.49414876176942,2.85720572368755));
#72786=CARTESIAN_POINT('Ctrl Pts',(29.9394830031919,-1.58205553636154,2.80948233381311));
#72787=CARTESIAN_POINT('Ctrl Pts',(29.945633811571,-1.66751372927036,2.75780991462335));
#72788=CARTESIAN_POINT('Ctrl Pts',(29.9517911979372,-1.7530633155138,2.70608223432244));
#72789=CARTESIAN_POINT('Ctrl Pts',(29.9579485843034,-1.83615871849149,2.65039731641945));
#72790=CARTESIAN_POINT('Ctrl Pts',(29.9641059706696,-1.91642489278621,2.59102936934519));
#72791=CARTESIAN_POINT('Ctrl Pts',(29.9702667934065,-1.99673586276528,2.53162828966134));
#72792=CARTESIAN_POINT('Ctrl Pts',(29.9764276161435,-2.07421412273621,2.46854036166959));
#72793=CARTESIAN_POINT('Ctrl Pts',(29.9825884388805,-2.14851847040971,2.40207950426465));
#72794=CARTESIAN_POINT('Ctrl Pts',(29.9887595617972,-2.22294704631827,2.33550753202896));
#72795=CARTESIAN_POINT('Ctrl Pts',(29.9949306847139,-2.29419080045137,2.26555167083688));
#72796=CARTESIAN_POINT('Ctrl Pts',(30.0011018076305,-2.36194599383186,2.19256212790462));
#72797=CARTESIAN_POINT('Ctrl Pts',(30.0057973295761,-2.41349998193723,2.13702539573097));
#72798=CARTESIAN_POINT('Ctrl Pts',(30.0104928515217,-2.46303505280887,2.07973307181364));
#72799=CARTESIAN_POINT('Ctrl Pts',(30.0151883734672,-2.51043399271408,2.02085099171751));
#72800=CARTESIAN_POINT('Ctrl Pts',(30.021344038126,-2.57257234125583,1.94365864895218));
#72801=CARTESIAN_POINT('Ctrl Pts',(30.0274997027848,-2.63126207956789,1.86345465956792));
#72802=CARTESIAN_POINT('Ctrl Pts',(30.0336553674436,-2.68619615029831,1.78058074925642));
#72803=CARTESIAN_POINT('Ctrl Pts',(30.0398029872817,-2.74105842784748,1.69781514662327));
#72804=CARTESIAN_POINT('Ctrl Pts',(30.0459506071198,-2.79217454934574,1.61238691446173));
#72805=CARTESIAN_POINT('Ctrl Pts',(30.0520982269579,-2.83927725477578,1.52467118849046));
#72806=CARTESIAN_POINT('Ctrl Pts',(30.0582394767409,-2.88633115321394,1.43704635200603));
#72807=CARTESIAN_POINT('Ctrl Pts',(30.0643807265238,-2.9293796938176,1.34713911356048));
#72808=CARTESIAN_POINT('Ctrl Pts',(30.0705219763068,-2.96819913856499,1.25535311220471));
#72809=CARTESIAN_POINT('Ctrl Pts',(30.0766585247557,-3.00698886571653,1.16363737613252));
#72810=CARTESIAN_POINT('Ctrl Pts',(30.0827950732045,-3.04155576315581,1.07004613669127));
#72811=CARTESIAN_POINT('Ctrl Pts',(30.0889316216534,-3.07172271706089,0.975006211258182));
#72812=CARTESIAN_POINT('Ctrl Pts',(30.0950657497165,-3.10187777247517,0.880003771601183));
#72813=CARTESIAN_POINT('Ctrl Pts',(30.1011998777796,-3.12763619914388,0.783554196195001));
#72814=CARTESIAN_POINT('Ctrl Pts',(30.1073340058427,-3.14886990419533,0.686101952302203));
#72815=CARTESIAN_POINT('Ctrl Pts',(30.1134667720909,-3.17009889523106,0.588671343418859));
#72816=CARTESIAN_POINT('Ctrl Pts',(30.1195995383391,-3.18680507343115,0.490238935921755));
#72817=CARTESIAN_POINT('Ctrl Pts',(30.1257323045873,-3.19891115011677,0.391260803248455));
#72818=CARTESIAN_POINT('Ctrl Pts',(30.1318667393409,-3.21102052043089,0.292255742181479));
#72819=CARTESIAN_POINT('Ctrl Pts',(30.1380011740944,-3.21852724015429,0.192705093162679));
#72820=CARTESIAN_POINT('Ctrl Pts',(30.144135608848,-3.22140581046504,0.0930707623373361));
#72821=CARTESIAN_POINT('Ctrl Pts',(30.146099256141,-3.22232724773277,0.0611775738249374));
#72822=CARTESIAN_POINT('Ctrl Pts',(30.1480629034339,-3.22277485870878,0.0292758256471393));
#72823=CARTESIAN_POINT('Ctrl Pts',(30.1500265507269,-3.22274893555634,-0.00261932634679408));
#72824=CARTESIAN_POINT('Ctrl Pts',(30.1484629751925,-3.22274884946717,-0.0027231889481761));
#72825=CARTESIAN_POINT('Ctrl Pts',(30.1525076918999,-3.2226973975967,-0.0636137329032254));
#72826=CARTESIAN_POINT('Ctrl Pts',(30.1565871213781,-3.22092026463483,-0.124489196182319));
#72827=CARTESIAN_POINT('Ctrl Pts',(30.1770332226003,-3.20346580768911,-0.427594650789332));
#72828=CARTESIAN_POINT('Ctrl Pts',(30.1937165015244,-3.16218169450938,-0.667570143758494));
#72829=CARTESIAN_POINT('Ctrl Pts',(30.211082995921,-3.08645744844924,-0.927736036973237));
#72830=CARTESIAN_POINT('Ctrl Pts',(30.2128746803827,-3.07821613849804,-0.954724709180287));
#72831=CARTESIAN_POINT('Ctrl Pts',(30.2151196606511,-3.06732714690351,-0.988776242510945));
#72832=CARTESIAN_POINT('Ctrl Pts',(30.2155911960253,-3.06500803781895,-0.995941772743104));
#72833=CARTESIAN_POINT('Ctrl Pts',(30.2163421605527,-3.0612630157065,-1.00737607929524));
#72834=CARTESIAN_POINT('Ctrl Pts',(30.2166225286293,-3.05985326048818,-1.01165005873636));
#72835=CARTESIAN_POINT('Ctrl Pts',(30.217153991692,-3.05715882342239,-1.0197616723132));
#72836=CARTESIAN_POINT('Ctrl Pts',(30.2174051816405,-3.05587588149516,-1.02359979337814));
#72837=CARTESIAN_POINT('Ctrl Pts',(30.2179796348581,-3.05292028144768,-1.0323868492942));
#72838=CARTESIAN_POINT('Ctrl Pts',(30.2183026099155,-3.05124281989081,-1.03733413442749));
#72839=CARTESIAN_POINT('Ctrl Pts',(30.219319185047,-3.0459135471012,-1.05292681844884));
#72840=CARTESIAN_POINT('Ctrl Pts',(30.2200102351208,-3.04221794987839,-1.06355732125542));
#72841=CARTESIAN_POINT('Ctrl Pts',(30.2262720008826,-3.00807503409262,-1.16013632046875));
#72842=CARTESIAN_POINT('Ctrl Pts',(30.2316414863821,-2.97404538874837,-1.24478477794849));
#72843=CARTESIAN_POINT('Ctrl Pts',(30.2392602759745,-2.91959731055285,-1.36519064838015));
#72844=CARTESIAN_POINT('Ctrl Pts',(30.2415976711563,-2.90201714353768,-1.40217354191918));
#72845=CARTESIAN_POINT('Ctrl Pts',(30.2529718163308,-2.81247825112063,-1.58163167710049));
#72846=CARTESIAN_POINT('Ctrl Pts',(30.2617869019478,-2.73070742261281,-1.71896251313565));
#72847=CARTESIAN_POINT('Ctrl Pts',(30.2776065823303,-2.56931083319896,-1.94924178698007));
#72848=CARTESIAN_POINT('Ctrl Pts',(30.2845269823892,-2.49395081926028,-2.04477565064196));
#72849=CARTESIAN_POINT('Ctrl Pts',(30.2945956494331,-2.37990992420549,-2.17363675140672));
#72850=CARTESIAN_POINT('Ctrl Pts',(30.297581798312,-2.34555801549107,-2.21066170438581));
#72851=CARTESIAN_POINT('Ctrl Pts',(30.3026031541494,-2.28706107148186,-2.27081157500828));
#72852=CARTESIAN_POINT('Ctrl Pts',(30.3046177872112,-2.26340022303195,-2.29439596776597));
#72853=CARTESIAN_POINT('Ctrl Pts',(30.3073464316548,-2.23112437449246,-2.32558235745632));
#72854=CARTESIAN_POINT('Ctrl Pts',(30.3080460740022,-2.22282861187287,-2.33351285247458));
#72855=CARTESIAN_POINT('Ctrl Pts',(30.309159456605,-2.20959641322487,-2.34602784208437));
#72856=CARTESIAN_POINT('Ctrl Pts',(30.3095719345827,-2.20468760425548,-2.35064151067801));
#72857=CARTESIAN_POINT('Ctrl Pts',(30.3104280696165,-2.19448544726556,-2.36017019747952));
#72858=CARTESIAN_POINT('Ctrl Pts',(30.310871823504,-2.18918997272894,-2.36508287408306));
#72859=CARTESIAN_POINT('Ctrl Pts',(30.3118845979425,-2.17708750405103,-2.37623501113201));
#72860=CARTESIAN_POINT('Ctrl Pts',(30.3124540985345,-2.17027014274783,-2.38246308115771));
#72861=CARTESIAN_POINT('Ctrl Pts',(30.3139338854978,-2.15252577873012,-2.39853426493817));
#72862=CARTESIAN_POINT('Ctrl Pts',(30.314846077536,-2.14155808975292,-2.40833195071775));
#72863=CARTESIAN_POINT('Ctrl Pts',(30.3206000894993,-2.07219656138116,-2.46944571655035));
#72864=CARTESIAN_POINT('Ctrl Pts',(30.3255263838029,-2.01203340162778,-2.51870614452558));
#72865=CARTESIAN_POINT('Ctrl Pts',(30.3318330975683,-1.93412038244038,-2.57792579716918));
#72866=CARTESIAN_POINT('Ctrl Pts',(30.3331361598672,-1.91797489253195,-2.58996049270319));
#72867=CARTESIAN_POINT('Ctrl Pts',(30.3453968930367,-1.7656106867121,-2.70132530484808));
#72868=CARTESIAN_POINT('Ctrl Pts',(30.3567112240603,-1.6219215758414,-2.78996385928485));
#72869=CARTESIAN_POINT('Ctrl Pts',(30.3818406144486,-1.29148044801831,-2.95962206631521));
#72870=CARTESIAN_POINT('Ctrl Pts',(30.3956460398804,-1.10262010665849,-3.03504995236058));
#72871=CARTESIAN_POINT('Ctrl Pts',(30.4102921367267,-0.88297389207063,-3.09954027179283));
#72872=CARTESIAN_POINT('Ctrl Pts',(30.4119402030115,-0.857952626019397,
-3.10655921955369));
#72873=CARTESIAN_POINT('Ctrl Pts',(30.4140308949078,-0.825779829014118,
-3.11516593055914));
#72874=CARTESIAN_POINT('Ctrl Pts',(30.4144888947993,-0.818704886209376,
-3.11703278980236));
#72875=CARTESIAN_POINT('Ctrl Pts',(30.4152233673394,-0.807314564566318,
-3.1199968880119));
#72876=CARTESIAN_POINT('Ctrl Pts',(30.4155007089138,-0.803003213570458,
-3.12110929429502));
#72877=CARTESIAN_POINT('Ctrl Pts',(30.4160299647778,-0.794755783334021,
-3.12321905962687));
#72878=CARTESIAN_POINT('Ctrl Pts',(30.4162819622733,-0.790820135862571,
-3.12421791212089));
#72879=CARTESIAN_POINT('Ctrl Pts',(30.4168629560509,-0.781726297196373,
-3.12650760939784));
#72880=CARTESIAN_POINT('Ctrl Pts',(30.4171916436612,-0.776566758632681,
-3.12779313665401));
#72881=CARTESIAN_POINT('Ctrl Pts',(30.4182445544558,-0.759992111116426,
-3.13187926015103));
#72882=CARTESIAN_POINT('Ctrl Pts',(30.4189659612436,-0.748564693650268,
-3.13463022037141));
#72883=CARTESIAN_POINT('Ctrl Pts',(30.4313017251401,-0.551994536310598,
-3.18081495905926));
#72884=CARTESIAN_POINT('Ctrl Pts',(30.4420312303724,-0.36334890615327,-3.20784697814671));
#72885=CARTESIAN_POINT('Ctrl Pts',(30.4628511491851,0.00798076035520758,
-3.22785481080897));
#72886=CARTESIAN_POINT('Ctrl Pts',(30.4729184139981,0.18984902859802,-3.22227622167041));
#72887=CARTESIAN_POINT('Ctrl Pts',(30.487766785037,0.446044141777314,-3.19264465485629));
#72888=CARTESIAN_POINT('Ctrl Pts',(30.4922186182654,0.521473374627156,-3.18119467296213));
#72889=CARTESIAN_POINT('Ctrl Pts',(30.498547455831,0.626122649257305,-3.16148721652626));
#72890=CARTESIAN_POINT('Ctrl Pts',(30.500355917757,0.655742651155446,-3.15547658464048));
#72891=CARTESIAN_POINT('Ctrl Pts',(30.5035214687553,0.707062485085161,-3.14430874263182));
#72892=CARTESIAN_POINT('Ctrl Pts',(30.5048725174265,0.728801716718271,-3.13934114839539));
#72893=CARTESIAN_POINT('Ctrl Pts',(30.5068307236203,0.760065040630739,-3.13185499198639));
#72894=CARTESIAN_POINT('Ctrl Pts',(30.5074320393701,0.769632199713784,-3.12951766740417));
#72895=CARTESIAN_POINT('Ctrl Pts',(30.508484452908,0.786318040804871,-3.12536005745325));
#72896=CARTESIAN_POINT('Ctrl Pts',(30.5089349196094,0.793441525938676,-3.12355920281921));
#72897=CARTESIAN_POINT('Ctrl Pts',(30.5098011142994,0.807103142441979,-3.12005572478635));
#72898=CARTESIAN_POINT('Ctrl Pts',(30.5102167180195,0.81364220721099,-3.1183568695464));
#72899=CARTESIAN_POINT('Ctrl Pts',(30.5111956833793,0.82900762134596,-3.11431329964828));
#72900=CARTESIAN_POINT('Ctrl Pts',(30.5117595939188,0.837829407609145,-3.11195161363531));
#72901=CARTESIAN_POINT('Ctrl Pts',(30.5134264110297,0.863818365991999,-3.10487557394435));
#72902=CARTESIAN_POINT('Ctrl Pts',(30.5145327171416,0.880956434355125,-3.10005648970598));
#72903=CARTESIAN_POINT('Ctrl Pts',(30.5299117550583,1.11763274437505,-3.03138398697964));
#72904=CARTESIAN_POINT('Ctrl Pts',(30.5449737274413,1.32976388134954,-2.94450016619016));
#72905=CARTESIAN_POINT('Ctrl Pts',(30.5710795249889,1.67038503282617,-2.7606273243974));
#72906=CARTESIAN_POINT('Ctrl Pts',(30.5818861196854,1.80414191769187,-2.67513045347115));
#72907=CARTESIAN_POINT('Ctrl Pts',(30.5968629480797,1.98444461280531,-2.54018553525053));
#72908=CARTESIAN_POINT('Ctrl Pts',(30.6012448433717,2.03657492920037,-2.49858494664192));
#72909=CARTESIAN_POINT('Ctrl Pts',(30.6077700056286,2.11377516631272,-2.43295546614008));
#72910=CARTESIAN_POINT('Ctrl Pts',(30.6099768492875,2.13980784328686,-2.41009136411543));
#72911=CARTESIAN_POINT('Ctrl Pts',(30.6126611149765,2.17144102525117,-2.38139171078626));
#72912=CARTESIAN_POINT('Ctrl Pts',(30.613166358437,2.1773937654689,-2.37595012568702));
#72913=CARTESIAN_POINT('Ctrl Pts',(30.6139583396298,2.18672369970377,-2.36735682993711));
#72914=CARTESIAN_POINT('Ctrl Pts',(30.6142461999564,2.19011460220398,-2.36422015238613));
#72915=CARTESIAN_POINT('Ctrl Pts',(30.614783801329,2.19644716989505,-2.35833703872997));
#72916=CARTESIAN_POINT('Ctrl Pts',(30.6150336707569,2.19939040245093,-2.35559241300943));
#72917=CARTESIAN_POINT('Ctrl Pts',(30.6156000554038,2.20606165135364,-2.34934793064447));
#72918=CARTESIAN_POINT('Ctrl Pts',(30.6159163073498,2.20978647465463,-2.34584471909132));
#72919=CARTESIAN_POINT('Ctrl Pts',(30.6168738781703,2.22106347408047,-2.33518796117636));
#72920=CARTESIAN_POINT('Ctrl Pts',(30.6175130868203,2.22858945800586,-2.32800661608087));
#72921=CARTESIAN_POINT('Ctrl Pts',(30.6222007495476,2.28375442661872,-2.27485515433697));
#72922=CARTESIAN_POINT('Ctrl Pts',(30.6261437506206,2.33000546512973,-2.22745958775654));
#72923=CARTESIAN_POINT('Ctrl Pts',(30.6338755019509,2.41941687517277,-2.13000041903725));
#72924=CARTESIAN_POINT('Ctrl Pts',(30.637662775036,2.4625622784975,-2.07996819594275));
#72925=CARTESIAN_POINT('Ctrl Pts',(30.6493123962766,2.59181367775369,-1.92042124981092));
#72926=CARTESIAN_POINT('Ctrl Pts',(30.6570305699771,2.67238009693623,-1.80662740954408));
#72927=CARTESIAN_POINT('Ctrl Pts',(30.6765116443411,2.85440597340829,-1.51057947252612));
#72928=CARTESIAN_POINT('Ctrl Pts',(30.6883664289255,2.94601220550981,-1.32305642531547));
#72929=CARTESIAN_POINT('Ctrl Pts',(30.7022919054544,3.02690551112755,-1.10656466533573));
#72930=CARTESIAN_POINT('Ctrl Pts',(30.7036795992858,3.03469449869471,-1.08502146971086));
#72931=CARTESIAN_POINT('Ctrl Pts',(30.7056826681184,3.04554505923698,-1.05397931396381));
#72932=CARTESIAN_POINT('Ctrl Pts',(30.7062918360714,3.04879333108799,-1.04454598888579));
#72933=CARTESIAN_POINT('Ctrl Pts',(30.7073513845387,3.05435357603803,-1.02815154320923));
#72934=CARTESIAN_POINT('Ctrl Pts',(30.707801094007,3.05668569652833,-1.02119729459456));
#72935=CARTESIAN_POINT('Ctrl Pts',(30.7086675634826,3.06112548359041,-1.00780663107401));
#72936=CARTESIAN_POINT('Ctrl Pts',(30.7090842052122,3.06323664337082,-1.00137140837751));
#72937=CARTESIAN_POINT('Ctrl Pts',(30.7101770816675,3.06871222449474,-0.984501421754472));
#72938=CARTESIAN_POINT('Ctrl Pts',(30.7108543987847,3.07204368843388,-0.97405612661003));
#72939=CARTESIAN_POINT('Ctrl Pts',(30.7131989522372,3.08336133153536,-0.937935738695031));
#72940=CARTESIAN_POINT('Ctrl Pts',(30.7148749547858,3.09107927440623,-0.912178381339127));
#72941=CARTESIAN_POINT('Ctrl Pts',(30.7171253692701,3.10094601046948,-0.877685709630992));
#72942=CARTESIAN_POINT('Ctrl Pts',(30.7176903941089,3.10338199794549,-0.869033104621488));
#72943=CARTESIAN_POINT('Ctrl Pts',(30.7343681768453,3.17406903101491,-0.613865710666124));
#72944=CARTESIAN_POINT('Ctrl Pts',(30.7514762168481,3.21275329840638,-0.360154796611872));
#72945=CARTESIAN_POINT('Ctrl Pts',(30.7815929127867,3.22719472706063,0.0845590682518872));
#72946=CARTESIAN_POINT('Ctrl Pts',(30.7944210539115,3.21666344999222,0.273909449555979));
#72947=CARTESIAN_POINT('Ctrl Pts',(30.8081294869286,3.18597574615162,0.486114166049166));
#72948=CARTESIAN_POINT('Ctrl Pts',(30.8097217645548,3.18209022427304,0.51093085147319));
#72949=CARTESIAN_POINT('Ctrl Pts',(30.8117521499249,3.17671321006679,0.542828701401955));
#72950=CARTESIAN_POINT('Ctrl Pts',(30.812204582021,3.17548761109585,0.549952954580014));
#72951=CARTESIAN_POINT('Ctrl Pts',(30.8129322692036,3.17347180115034,0.561439168057784));
#72952=CARTESIAN_POINT('Ctrl Pts',(30.8132083650399,3.17269655206728,0.56580367725317));
#72953=CARTESIAN_POINT('Ctrl Pts',(30.8137367693971,3.17119277849933,0.574169368670177));
#72954=CARTESIAN_POINT('Ctrl Pts',(30.8139891552782,3.17046568708685,0.578170761515104));
#72955=CARTESIAN_POINT('Ctrl Pts',(30.8145730980991,3.16876296624351,0.587441523919209));
#72956=CARTESIAN_POINT('Ctrl Pts',(30.8149043362293,3.16778176004689,0.59270988009287));
#72957=CARTESIAN_POINT('Ctrl Pts',(30.8159737255753,3.16456441155667,0.60974846013079));
#72958=CARTESIAN_POINT('Ctrl Pts',(30.8167089350636,3.16227574283745,0.621508838456927));
#72959=CARTESIAN_POINT('Ctrl Pts',(30.8259113450526,3.13266895832791,0.769245388484313));
#72960=CARTESIAN_POINT('Ctrl Pts',(30.8339103308113,3.09666237275746,0.903352498968228));
#72961=CARTESIAN_POINT('Ctrl Pts',(30.8519922706406,2.99405000668099,1.20602372996415));
#72962=CARTESIAN_POINT('Ctrl Pts',(30.8619505095565,2.92166437418214,1.37211806222729));
#72963=CARTESIAN_POINT('Ctrl Pts',(30.8813753106195,2.75869013229493,1.67392755718296));
#72964=CARTESIAN_POINT('Ctrl Pts',(30.8907569172403,2.67100855350224,1.81055445371313));
#72965=CARTESIAN_POINT('Ctrl Pts',(30.9017515178581,2.56139251919219,1.95596159008688));
#72966=CARTESIAN_POINT('Ctrl Pts',(30.9029644691363,2.54920778101746,1.97181567105065));
#72967=CARTESIAN_POINT('Ctrl Pts',(30.9047586544124,2.5310546669354,1.99498595166849));
#72968=CARTESIAN_POINT('Ctrl Pts',(30.9053353519348,2.52520025440604,2.00239115722437));
#72969=CARTESIAN_POINT('Ctrl Pts',(30.9063572704619,2.51479220037355,2.01543799553888));
#72970=CARTESIAN_POINT('Ctrl Pts',(30.9068019546391,2.51025187852354,2.02109020826043));
#72971=CARTESIAN_POINT('Ctrl Pts',(30.9076729436232,2.50133709237883,2.03211177804844));
#72972=CARTESIAN_POINT('Ctrl Pts',(30.9080991788263,2.49696431351498,2.03748245244718));
#72973=CARTESIAN_POINT('Ctrl Pts',(30.9092512481354,2.48511806238501,2.05193668087805));
#72974=CARTESIAN_POINT('Ctrl Pts',(30.9099783988559,2.47761216855141,2.06099341645721));
#72975=CARTESIAN_POINT('Ctrl Pts',(30.9126820459508,2.44959903315156,2.09442034719071));
#72976=CARTESIAN_POINT('Ctrl Pts',(30.9146712751398,2.42878098127011,2.11852657323258));
#72977=CARTESIAN_POINT('Ctrl Pts',(30.9339402741997,2.22521185499937,2.34730429157861));
#72978=CARTESIAN_POINT('Ctrl Pts',(30.9523649325636,2.01745175930793,2.52807646687659));
#72979=CARTESIAN_POINT('Ctrl Pts',(30.9709191047552,1.78943620529091,2.68030513742261));
#72980=CARTESIAN_POINT('Origin',(-1.72497344927317,0.,0.));
#72981=CARTESIAN_POINT('',(32.4670258968214,1.789436210378,2.68030513402635));
#72982=CARTESIAN_POINT('',(32.2229614699496,1.78943610001022,2.68030520771053));
#72983=CARTESIAN_POINT('',(-1.72497344927317,1.78943621037804,2.68030513402633));
#72984=CARTESIAN_POINT('',(31.646573449241,-3.22274865695249,0.00294221191095898));
#72985=CARTESIAN_POINT('Ctrl Pts',(31.6465734492731,-3.22274865695296,0.00294221139083024));
#72986=CARTESIAN_POINT('Ctrl Pts',(31.6526668782384,-3.22283885314083,-0.0958541035867903));
#72987=CARTESIAN_POINT('Ctrl Pts',(31.6587603072037,-3.21838176727151,-0.194756389147862));
#72988=CARTESIAN_POINT('Ctrl Pts',(31.664853736169,-3.20937494631332,-0.2933087391749));
#72989=CARTESIAN_POINT('Ctrl Pts',(31.6709440299356,-3.20037275955595,-0.391810381923121));
#72990=CARTESIAN_POINT('Ctrl Pts',(31.6770343237022,-3.18682552646746,-0.489962005563697));
#72991=CARTESIAN_POINT('Ctrl Pts',(31.6831246174688,-3.1687828431129,-0.587309846412713));
#72992=CARTESIAN_POINT('Ctrl Pts',(31.689213485821,-3.15074438259228,-0.684634903302244));
#72993=CARTESIAN_POINT('Ctrl Pts',(31.6953023541733,-3.12821264279287,-0.781156114813821));
#72994=CARTESIAN_POINT('Ctrl Pts',(31.7013912225256,-3.10128865968275,-0.876428098490201));
#72995=CARTESIAN_POINT('Ctrl Pts',(31.7074803735783,-3.07436342651702,-0.971704505556635));
#72996=CARTESIAN_POINT('Ctrl Pts',(31.7135695246311,-3.04304566681001,-1.06573114265188));
#72997=CARTESIAN_POINT('Ctrl Pts',(31.7196586756839,-3.0074864811343,-1.15807712536532));
#72998=CARTESIAN_POINT('Ctrl Pts',(31.7257538952436,-2.9718918568299,-1.25051514097915));
#72999=CARTESIAN_POINT('Ctrl Pts',(31.7318491148033,-2.93204752346106,-1.34126874151655));
#73000=CARTESIAN_POINT('Ctrl Pts',(31.737944334363,-2.8881529416912,-1.42992662325746));
#73001=CARTESIAN_POINT('Ctrl Pts',(31.7440424976996,-2.8442371603799,-1.51862732364161));
#73002=CARTESIAN_POINT('Ctrl Pts',(31.7501406610363,-2.79626745147484,-1.60522990161825));
#73003=CARTESIAN_POINT('Ctrl Pts',(31.7562388243729,-2.74448841329757,-1.6893492568961));
#73004=CARTESIAN_POINT('Ctrl Pts',(31.7623476079941,-2.69261919909692,-1.77361511062611));
#73005=CARTESIAN_POINT('Ctrl Pts',(31.7684563916154,-2.63692765202575,-1.85538873433251));
#73006=CARTESIAN_POINT('Ctrl Pts',(31.7745651752366,-2.57770082090494,-1.93431539320918));
#73007=CARTESIAN_POINT('Ctrl Pts',(31.7805250337949,-2.51991787126655,-2.0113179116403));
#73008=CARTESIAN_POINT('Ctrl Pts',(31.7864848923532,-2.45877035239737,-2.08561045375693));
#73009=CARTESIAN_POINT('Ctrl Pts',(31.7924447509115,-2.39455838703441,-2.15689770123277));
#73010=CARTESIAN_POINT('Ctrl Pts',(31.7986169990043,-2.32805812081721,-2.23072538908249));
#73011=CARTESIAN_POINT('Ctrl Pts',(31.804789247097,-2.25802328677941,-2.30160469149998));
#73012=CARTESIAN_POINT('Ctrl Pts',(31.8109614951898,-2.18474563496786,-2.36917793189725));
#73013=CARTESIAN_POINT('Ctrl Pts',(31.8171253838424,-2.11156722740795,-2.43665965386414));
#73014=CARTESIAN_POINT('Ctrl Pts',(31.8232892724951,-2.03515504805348,-2.50084392164774));
#73015=CARTESIAN_POINT('Ctrl Pts',(31.8294531611477,-1.95583989829263,-2.56140739726164));
#73016=CARTESIAN_POINT('Ctrl Pts',(31.8356105228063,-1.87660873601796,-2.62190674169649));
#73017=CARTESIAN_POINT('Ctrl Pts',(31.8417678844648,-1.79448105803267,-2.67879265432747));
#73018=CARTESIAN_POINT('Ctrl Pts',(31.8479252461234,-1.70982246141898,-2.73178050233307));
#73019=CARTESIAN_POINT('Ctrl Pts',(31.8540781102697,-1.62522570185443,-2.78472964650596));
#73020=CARTESIAN_POINT('Ctrl Pts',(31.860230974416,-1.53810206619429,-2.83378615712614));
#73021=CARTESIAN_POINT('Ctrl Pts',(31.8663838385623,-1.448847240588,-2.87870791084134));
#73022=CARTESIAN_POINT('Ctrl Pts',(31.8725343716988,-1.35962622913159,-2.9236126459707));
#73023=CARTESIAN_POINT('Ctrl Pts',(31.8786849048354,-1.26827601960228,-2.96438554165958));
#73024=CARTESIAN_POINT('Ctrl Pts',(31.8848354379719,-1.1752172956462,-3.0008301968812));
#73025=CARTESIAN_POINT('Ctrl Pts',(31.8909852861871,-1.08216893467882,-3.03727079363807));
#73026=CARTESIAN_POINT('Ctrl Pts',(31.8971351344023,-0.987412842012983,
-3.06938394979638));
#73027=CARTESIAN_POINT('Ctrl Pts',(31.9032849826175,-0.891389155669776,
-3.09702162337532));
#73028=CARTESIAN_POINT('Ctrl Pts',(31.9094357909966,-0.795350477333879,
-3.12466361197086));
#73029=CARTESIAN_POINT('Ctrl Pts',(31.9155865993758,-0.698044229694665,
-3.14782860993577));
#73030=CARTESIAN_POINT('Ctrl Pts',(31.9217374077549,-0.59992418370671,-3.1664188820028));
#73031=CARTESIAN_POINT('Ctrl Pts',(31.9278947941211,-0.501699203155232,
-3.1850290354515));
#73032=CARTESIAN_POINT('Ctrl Pts',(31.9340521804873,-0.402659113936038,
-3.19905461227844));
#73033=CARTESIAN_POINT('Ctrl Pts',(31.9402095668535,-0.30326620196804,-3.20844934091905));
#73034=CARTESIAN_POINT('Ctrl Pts',(31.9463703895904,-0.203817819890132,
-3.21784931265617));
#73035=CARTESIAN_POINT('Ctrl Pts',(31.9525312123274,-0.104016656822131,
-3.22261326864607));
#73036=CARTESIAN_POINT('Ctrl Pts',(31.9586920350644,-0.00432631756911811,
-3.22274709610858));
#73037=CARTESIAN_POINT('Ctrl Pts',(31.964863157981,0.0955306923469966,-3.22288114731506));
#73038=CARTESIAN_POINT('Ctrl Pts',(31.9710342808977,0.19527607421438,-3.21836962714771));
#73039=CARTESIAN_POINT('Ctrl Pts',(31.9772054038144,0.294449884276756,-3.20927045107598));
#73040=CARTESIAN_POINT('Ctrl Pts',(31.9819009257599,0.369909862607305,-3.20234701404389));
#73041=CARTESIAN_POINT('Ctrl Pts',(31.9865964477054,0.445039007553297,-3.19276864227843));
#73042=CARTESIAN_POINT('Ctrl Pts',(31.991291969651,0.519639334911914,-3.18058053256199));
#73043=CARTESIAN_POINT('Ctrl Pts',(31.9974642177437,0.617701218894503,-3.16455930258487));
#73044=CARTESIAN_POINT('Ctrl Pts',(32.0036364658365,0.715194071780944,-3.14397054045711));
#73045=CARTESIAN_POINT('Ctrl Pts',(32.0098087139293,0.811659260599448,-3.11886626952538));
#73046=CARTESIAN_POINT('Ctrl Pts',(32.0159726025819,0.907993800915114,-3.09379599879053));
#73047=CARTESIAN_POINT('Ctrl Pts',(32.0221364912345,1.00330302689841,-3.06422248315563));
#73048=CARTESIAN_POINT('Ctrl Pts',(32.0283003798871,1.09713607605518,-3.03024916353726));
#73049=CARTESIAN_POINT('Ctrl Pts',(32.0344577415457,1.19086976459878,-2.99631181855574));
#73050=CARTESIAN_POINT('Ctrl Pts',(32.0406151032042,1.2831299778011,-2.95798407916353));
#73051=CARTESIAN_POINT('Ctrl Pts',(32.0467724648627,1.37347959790967,-2.91541958500417));
#73052=CARTESIAN_POINT('Ctrl Pts',(32.052925329009,1.4637632240837,-2.87288618116304));
#73053=CARTESIAN_POINT('Ctrl Pts',(32.0590781931553,1.55213863999183,-2.82612235980595));
#73054=CARTESIAN_POINT('Ctrl Pts',(32.0652310573016,1.63818821775929,-2.77533005707333));
#73055=CARTESIAN_POINT('Ctrl Pts',(32.0713815904382,1.72420519568361,-2.72455699698134));
#73056=CARTESIAN_POINT('Ctrl Pts',(32.0775321235747,1.80789771263815,-2.66975870859827));
#73057=CARTESIAN_POINT('Ctrl Pts',(32.0836826567112,1.88887308637349,-2.61118287871108));
#73058=CARTESIAN_POINT('Ctrl Pts',(32.0898325049264,1.96983944271802,-2.55261357180891));
#73059=CARTESIAN_POINT('Ctrl Pts',(32.0959823531417,2.04808890547082,-2.49026781433787));
#73060=CARTESIAN_POINT('Ctrl Pts',(32.1021322013569,2.12325895326331,-2.42443580650988));
#73061=CARTESIAN_POINT('Ctrl Pts',(32.108283009736,2.19844073721022,-2.35859352045761));
#73062=CARTESIAN_POINT('Ctrl Pts',(32.1144338181151,2.27054182443136,-2.2892641891333));
#73063=CARTESIAN_POINT('Ctrl Pts',(32.1205846264943,2.33923464054728,-2.21677668224917));
#73064=CARTESIAN_POINT('Ctrl Pts',(32.1267420128604,2.40800092025162,-2.14421165354147));
#73065=CARTESIAN_POINT('Ctrl Pts',(32.1328993992266,2.47335135083689,-2.0684820206347));
#73066=CARTESIAN_POINT('Ctrl Pts',(32.1390567855928,2.53499704552073,-1.98995164305598));
#73067=CARTESIAN_POINT('Ctrl Pts',(32.1452176083298,2.59667714400032,-1.91137743852251));
#73068=CARTESIAN_POINT('Ctrl Pts',(32.1513784310667,2.65464813700084,-1.82999973029181));
#73069=CARTESIAN_POINT('Ctrl Pts',(32.1575392538037,2.70866430103904,-1.7462116901386));
#73070=CARTESIAN_POINT('Ctrl Pts',(32.1637103767203,2.76277077382688,-1.66228356611834));
#73071=CARTESIAN_POINT('Ctrl Pts',(32.169881499637,2.8129089921349,-1.57593743659895));
#73072=CARTESIAN_POINT('Ctrl Pts',(32.1760526225537,2.85887897867376,-1.48759152585556));
#73073=CARTESIAN_POINT('Ctrl Pts',(32.1807481444994,2.89385690466046,-1.42037034612784));
#73074=CARTESIAN_POINT('Ctrl Pts',(32.185443666445,2.92642259088435,-1.35199191599748));
#73075=CARTESIAN_POINT('Ctrl Pts',(32.1901391883907,2.95650700519601,-1.28264721990378));
#73076=CARTESIAN_POINT('Ctrl Pts',(32.1963114364834,2.99605286846886,-1.19149384586733));
#73077=CARTESIAN_POINT('Ctrl Pts',(32.2024836845762,3.03144880204087,-1.09834943445963));
#73078=CARTESIAN_POINT('Ctrl Pts',(32.208655932669,3.06249058087111,-1.00362792138109));
#73079=CARTESIAN_POINT('Ctrl Pts',(32.2148198213216,3.09349031798691,-0.909034695242089));
#73080=CARTESIAN_POINT('Ctrl Pts',(32.2209837099743,3.1201474873923,-0.812869022032163));
#73081=CARTESIAN_POINT('Ctrl Pts',(32.2271475986269,3.14230531854134,-0.715566102863193));
#73082=CARTESIAN_POINT('Ctrl Pts',(32.2333049602855,3.16443968657456,-0.618366218582687));
#73083=CARTESIAN_POINT('Ctrl Pts',(32.239462321944,3.1820840924887,-0.520031903682021));
#73084=CARTESIAN_POINT('Ctrl Pts',(32.2456196836025,3.19513142527696,-0.421013940039524));
#73085=CARTESIAN_POINT('Ctrl Pts',(32.2517725477488,3.20816922792196,-0.322068301936224));
#73086=CARTESIAN_POINT('Ctrl Pts',(32.2579254118952,3.21661657681269,-0.222440437251676));
#73087=CARTESIAN_POINT('Ctrl Pts',(32.2640782760415,3.22041752676248,-0.122590847215692));
#73088=CARTESIAN_POINT('Ctrl Pts',(32.270228809178,3.22421703672411,-0.0227790851513653));
#73089=CARTESIAN_POINT('Ctrl Pts',(32.2763793423145,3.22337362891887,0.0772538017767354));
#73090=CARTESIAN_POINT('Ctrl Pts',(32.2825298754511,3.21788333236684,0.177043558978158));
#73091=CARTESIAN_POINT('Ctrl Pts',(32.2886797236663,3.21239364721242,0.276822203625462));
#73092=CARTESIAN_POINT('Ctrl Pts',(32.2948295718815,3.20225812599177,0.37635733865508));
#73093=CARTESIAN_POINT('Ctrl Pts',(32.3009794200967,3.18752486869412,0.475187093634188));
#73094=CARTESIAN_POINT('Ctrl Pts',(32.3071302284758,3.17278931112146,0.574032278712152));
#73095=CARTESIAN_POINT('Ctrl Pts',(32.313281036855,3.15345465571844,0.672171435325801));
#73096=CARTESIAN_POINT('Ctrl Pts',(32.3194318452341,3.12962042779751,0.769151181766334));
#73097=CARTESIAN_POINT('Ctrl Pts',(32.3255892316003,3.10576071034205,0.866234643275956));
#73098=CARTESIAN_POINT('Ctrl Pts',(32.3317466179665,3.07739191503035,0.962155795950736));
#73099=CARTESIAN_POINT('Ctrl Pts',(32.3379040043327,3.04466391969892,1.05647488308223));
#73100=CARTESIAN_POINT('Ctrl Pts',(32.3440648270697,3.01191765922705,1.15084660867677));
#73101=CARTESIAN_POINT('Ctrl Pts',(32.3502256498066,2.97480751514342,1.24361408483356));
#73102=CARTESIAN_POINT('Ctrl Pts',(32.3563864725436,2.93353136184629,1.33435801476374));
#73103=CARTESIAN_POINT('Ctrl Pts',(32.3625575954603,2.89218619961718,1.42525365800025));
#73104=CARTESIAN_POINT('Ctrl Pts',(32.368728718377,2.84666131377875,1.51411861052658));
#73105=CARTESIAN_POINT('Ctrl Pts',(32.3748998412937,2.7972003885514,1.60055851151649));
#73106=CARTESIAN_POINT('Ctrl Pts',(32.3795953632392,2.75956625567364,1.66632943482297));
#73107=CARTESIAN_POINT('Ctrl Pts',(32.3842908851848,2.71965431070223,1.73069689768004));
#73108=CARTESIAN_POINT('Ctrl Pts',(32.3889864071303,2.67758788505995,1.7934995623864));
#73109=CARTESIAN_POINT('Ctrl Pts',(32.3951596181536,2.62228308071711,1.87606633697594));
#73110=CARTESIAN_POINT('Ctrl Pts',(32.4013328291769,2.5630582644798,1.95621797396748));
#73111=CARTESIAN_POINT('Ctrl Pts',(32.4075060402002,2.50015133106894,2.03355867489833));
#73112=CARTESIAN_POINT('Ctrl Pts',(32.4136691809538,2.43734701682694,2.11077321106451));
#73113=CARTESIAN_POINT('Ctrl Pts',(32.4198323217074,2.37087280745839,2.1851855998657));
#73114=CARTESIAN_POINT('Ctrl Pts',(32.425995462461,2.30100993230182,2.25642878326535));
#73115=CARTESIAN_POINT('Ctrl Pts',(32.4321528014495,2.23121282361269,2.32760490082366));
#73116=CARTESIAN_POINT('Ctrl Pts',(32.4383101404379,2.15803368874889,2.39561743152967));
#73117=CARTESIAN_POINT('Ctrl Pts',(32.4444674794264,2.08179381116393,2.46013253510854));
#73118=CARTESIAN_POINT('Ctrl Pts',(32.4506200279823,2.00561324848577,2.52459744569816));
#73119=CARTESIAN_POINT('Ctrl Pts',(32.4567725765383,1.92637700977985,2.5855700613177));
#73120=CARTESIAN_POINT('Ctrl Pts',(32.4629251250942,1.84444216790488,2.6427543684108));
#73121=CARTESIAN_POINT('Ctrl Pts',(32.4642920490033,1.82623854166322,2.65545911927611));
#73122=CARTESIAN_POINT('Ctrl Pts',(32.4656589729124,1.80790184371059,2.66797703282869));
#73123=CARTESIAN_POINT('Ctrl Pts',(32.4670258968214,1.789436210378,2.68030513402635));
#73124=CARTESIAN_POINT('Ctrl Pts',(31.2170551299057,1.78943621037803,2.68030513402633));
#73125=CARTESIAN_POINT('Ctrl Pts',(31.2232179771471,1.70662880253117,2.73558935230715));
#73126=CARTESIAN_POINT('Ctrl Pts',(31.2293808243885,1.62114288271662,2.78710868993221));
#73127=CARTESIAN_POINT('Ctrl Pts',(31.23554367163,1.53335639378915,2.83459622029769));
#73128=CARTESIAN_POINT('Ctrl Pts',(31.2417002522632,1.44565916937131,2.88203546360711));
#73129=CARTESIAN_POINT('Ctrl Pts',(31.2478568328964,1.35566640687756,2.92545084492418));
#73130=CARTESIAN_POINT('Ctrl Pts',(31.2540134135295,1.26378424804521,2.9646191891865));
#73131=CARTESIAN_POINT('Ctrl Pts',(31.2601658450428,1.17196401158862,3.00376113662746));
#73132=CARTESIAN_POINT('Ctrl Pts',(31.266318276556,1.07825730864577,3.03866156717211));
#73133=CARTESIAN_POINT('Ctrl Pts',(31.2724707080692,0.983093245736578,3.06914405538207));
#73134=CARTESIAN_POINT('Ctrl Pts',(31.2786210431498,0.887961609851441,3.09961615672595));
#73135=CARTESIAN_POINT('Ctrl Pts',(31.2847713782304,0.791374014071506,3.12567317470469));
#73136=CARTESIAN_POINT('Ctrl Pts',(31.290921713311,0.693776968053361,3.14718780518397));
#73137=CARTESIAN_POINT('Ctrl Pts',(31.2970715978239,0.596187071901783,3.16870085952193));
#73138=CARTESIAN_POINT('Ctrl Pts',(31.3032214823369,0.497588296812218,3.18567209466996));
#73139=CARTESIAN_POINT('Ctrl Pts',(31.3093713668498,0.398438662534779,3.1980250459772));
#73140=CARTESIAN_POINT('Ctrl Pts',(31.3155224458448,0.299269770584,3.21038039657823));
#73141=CARTESIAN_POINT('Ctrl Pts',(31.3216735248399,0.19955023796126,3.21811562776666));
#73142=CARTESIAN_POINT('Ctrl Pts',(31.327824603835,0.0997435368877103,3.22120610786536));
#73143=CARTESIAN_POINT('Ctrl Pts',(31.3339823890386,-0.000171978355588673,
3.22429995735733));
#73144=CARTESIAN_POINT('Ctrl Pts',(31.3401401742422,-0.100174416881713,
3.22273893209103));
#73145=CARTESIAN_POINT('Ctrl Pts',(31.3462979594459,-0.199800114916488,
3.21655055557648));
#73146=CARTESIAN_POINT('Ctrl Pts',(31.3524593916297,-0.299484816787854,
3.21035851396383));
#73147=CARTESIAN_POINT('Ctrl Pts',(31.3586208238136,-0.398791902276235,
3.19953371115868));
#73148=CARTESIAN_POINT('Ctrl Pts',(31.3647822559975,-0.497264710914674,
3.18415536206683));
#73149=CARTESIAN_POINT('Ctrl Pts',(31.3709537255055,-0.595897937370692,
3.16875196076784));
#73150=CARTESIAN_POINT('Ctrl Pts',(31.3771251950136,-0.693693747658595,
3.14878028696303));
#73151=CARTESIAN_POINT('Ctrl Pts',(31.3832966645216,-0.790207480306894,
3.1243702886449));
#73152=CARTESIAN_POINT('Ctrl Pts',(31.3871145474918,-0.84991418967032,3.10926942542937));
#73153=CARTESIAN_POINT('Ctrl Pts',(31.3909324304619,-0.909130543615332,
3.0924709655686));
#73154=CARTESIAN_POINT('Ctrl Pts',(31.3947503134321,-0.967755029328688,
3.07401492607128));
#73155=CARTESIAN_POINT('Ctrl Pts',(31.4009225615248,-1.06253134200341,3.04417764308534));
#73156=CARTESIAN_POINT('Ctrl Pts',(31.4070948096176,-1.15609328870176,3.00990060091551));
#73157=CARTESIAN_POINT('Ctrl Pts',(31.4132670577104,-1.24799433728965,2.97130067421541));
#73158=CARTESIAN_POINT('Ctrl Pts',(31.419430946363,-1.33977091885955,2.93275302567585));
#73159=CARTESIAN_POINT('Ctrl Pts',(31.4255948350156,-1.42989067639552,2.88989429627056));
#73160=CARTESIAN_POINT('Ctrl Pts',(31.4317587236682,-1.51792209895778,2.8428911452948));
#73161=CARTESIAN_POINT('Ctrl Pts',(31.4379160853268,-1.60586030429849,2.7959377663551));
#73162=CARTESIAN_POINT('Ctrl Pts',(31.4440734469853,-1.69171418998586,2.74484889418658));
#73163=CARTESIAN_POINT('Ctrl Pts',(31.4502308086439,-1.77507300576022,2.6898389146418));
#73164=CARTESIAN_POINT('Ctrl Pts',(31.4563836727902,-1.85837093388257,2.63486911595204));
#73165=CARTESIAN_POINT('Ctrl Pts',(31.4625365369365,-1.93917705401979,2.575984142714));
#73166=CARTESIAN_POINT('Ctrl Pts',(31.4686894010828,-2.01710679186687,2.51344340551056));
#73167=CARTESIAN_POINT('Ctrl Pts',(31.4748399342194,-2.09500700606836,2.45092636183685));
#73168=CARTESIAN_POINT('Ctrl Pts',(31.4809904673559,-2.17003266484376,2.38475657772647));
#73169=CARTESIAN_POINT('Ctrl Pts',(31.4871410004924,-2.24183040693022,2.31523519087437));
#73170=CARTESIAN_POINT('Ctrl Pts',(31.4932908487076,-2.3136201536439,2.24572154590089));
#73171=CARTESIAN_POINT('Ctrl Pts',(31.4994406969228,-2.38218238627006,2.17285734239147));
#73172=CARTESIAN_POINT('Ctrl Pts',(31.505590545138,-2.44719965707779,2.09698149750978));
#73173=CARTESIAN_POINT('Ctrl Pts',(31.5117413535172,-2.51222707890648,2.02109380627893));
#73174=CARTESIAN_POINT('Ctrl Pts',(31.5178921618963,-2.57370815692001,1.94219386960818));
#73175=CARTESIAN_POINT('Ctrl Pts',(31.5240429702755,-2.63136554615387,1.86065389715936));
#73176=CARTESIAN_POINT('Ctrl Pts',(31.5302003566416,-2.68908459712986,1.77902672172025));
#73177=CARTESIAN_POINT('Ctrl Pts',(31.5363577430078,-2.74297154224672,1.69475422784555));
#73178=CARTESIAN_POINT('Ctrl Pts',(31.542515129374,-2.79279231713283,1.60823774233284));
#73179=CARTESIAN_POINT('Ctrl Pts',(31.548675952111,-2.84264089645487,1.52167297290476));
#73180=CARTESIAN_POINT('Ctrl Pts',(31.554836774848,-2.88841858727227,1.43286210392005));
#73181=CARTESIAN_POINT('Ctrl Pts',(31.5609975975849,-2.92993822640096,1.34222932167883));
#73182=CARTESIAN_POINT('Ctrl Pts',(31.5671687205016,-2.97152728154169,1.25144501195721));
#73183=CARTESIAN_POINT('Ctrl Pts',(31.5733398434183,-3.00884390265784,1.15883310771925));
#73184=CARTESIAN_POINT('Ctrl Pts',(31.579510966335,-3.04174977699738,1.06483607031147));
#73185=CARTESIAN_POINT('Ctrl Pts',(31.5842064882806,-3.06678740097381,0.993315026584462));
#73186=CARTESIAN_POINT('Ctrl Pts',(31.5889020102262,-3.08927244588873,0.92099244102941));
#73187=CARTESIAN_POINT('Ctrl Pts',(31.5935975321718,-3.10916381139467,0.84806718861996));
#73188=CARTESIAN_POINT('Ctrl Pts',(31.6014764629116,-3.1425408657365,0.725701023670892));
#73189=CARTESIAN_POINT('Ctrl Pts',(31.6093553936514,-3.16870984081663,0.601290341548845));
#73190=CARTESIAN_POINT('Ctrl Pts',(31.6172343243912,-3.18746608133155,0.475581268408342));
#73191=CARTESIAN_POINT('Ctrl Pts',(31.6249655353474,-3.20587066654171,0.352229078161851));
#73192=CARTESIAN_POINT('Ctrl Pts',(31.6326967463036,-3.21713787939234,0.227626547890882));
#73193=CARTESIAN_POINT('Ctrl Pts',(31.6404279572598,-3.22111956307449,0.102500355505779));
#73194=CARTESIAN_POINT('Ctrl Pts',(31.6424764545869,-3.22217456835456,0.069346342234137));
#73195=CARTESIAN_POINT('Ctrl Pts',(31.6445249519139,-3.22271833466869,0.0361556929095487));
#73196=CARTESIAN_POINT('Ctrl Pts',(31.646573449241,-3.22274865695249,0.00294221191100407));
#73197=CARTESIAN_POINT('Ctrl Pts',(30.9709191047552,1.78943620529092,2.68030513742261));
#73198=CARTESIAN_POINT('Ctrl Pts',(30.9718568373112,1.77791224151339,2.6879988129389));
#73199=CARTESIAN_POINT('Ctrl Pts',(30.9727945355257,1.76633652017013,2.69561959581997));
#73200=CARTESIAN_POINT('Ctrl Pts',(30.9853875055158,1.61014525231306,2.79700820363487));
#73201=CARTESIAN_POINT('Ctrl Pts',(30.996967889745,1.45826721413129,2.87911338138045));
#73202=CARTESIAN_POINT('Ctrl Pts',(31.0088238281147,1.28701476112885,2.95464530819892));
#73203=CARTESIAN_POINT('Ctrl Pts',(31.009754705807,1.27345418040215,2.96051521913541));
#73204=CARTESIAN_POINT('Ctrl Pts',(31.0110495128099,1.25442372661726,2.96859789735097));
#73205=CARTESIAN_POINT('Ctrl Pts',(31.0114180622943,1.2489876751289,2.97088911788172));
#73206=CARTESIAN_POINT('Ctrl Pts',(31.0120440708352,1.23972065409924,2.97476510825769));
#73207=CARTESIAN_POINT('Ctrl Pts',(31.0123019881025,1.2358928779266,2.97635742888257));
#73208=CARTESIAN_POINT('Ctrl Pts',(31.0127934745622,1.22857984276965,2.97938304576577));
#73209=CARTESIAN_POINT('Ctrl Pts',(31.0130271228413,1.22509513918222,2.98081761665446));
#73210=CARTESIAN_POINT('Ctrl Pts',(31.0135773246771,1.21687026935222,2.98418674372764));
#73211=CARTESIAN_POINT('Ctrl Pts',(31.0138935643402,1.21212797641181,2.98611613028156));
#73212=CARTESIAN_POINT('Ctrl Pts',(31.0148287773001,1.19806029002336,2.99180048893859));
#73213=CARTESIAN_POINT('Ctrl Pts',(31.0154458391643,1.18872179803311,2.99552317921845));
#73214=CARTESIAN_POINT('Ctrl Pts',(31.0214196829157,1.09778478844465,3.03128202501158));
#73215=CARTESIAN_POINT('Ctrl Pts',(31.0265900173565,1.01492034094531,3.06002319245713));
#73216=CARTESIAN_POINT('Ctrl Pts',(31.0326872739042,0.913854592082875,3.09051893608328));
#73217=CARTESIAN_POINT('Ctrl Pts',(31.03371584146,0.896687161425791,3.09554351635211));
#73218=CARTESIAN_POINT('Ctrl Pts',(31.0425888804298,0.747675345730186,3.13781278533194));
#73219=CARTESIAN_POINT('Ctrl Pts',(31.0502061815097,0.613616203277497,3.16675955363183));
#73220=CARTESIAN_POINT('Ctrl Pts',(31.065972900184,0.334713752149143,3.20859960573247));
#73221=CARTESIAN_POINT('Ctrl Pts',(31.0741119362097,0.190029630775623,3.22040826776404));
#73222=CARTESIAN_POINT('Ctrl Pts',(31.0863632704994,-0.0215458968595493,
3.22336613798423));
#73223=CARTESIAN_POINT('Ctrl Pts',(31.0902688662274,-0.0881513830149897,
3.22223244938175));
#73224=CARTESIAN_POINT('Ctrl Pts',(31.0967049007624,-0.196057898045551,
3.21704766848016));
#73225=CARTESIAN_POINT('Ctrl Pts',(31.0991966434073,-0.237401156262834,
3.21426116727348));
#73226=CARTESIAN_POINT('Ctrl Pts',(31.102476540778,-0.291192910561514,3.20959219513189));
#73227=CARTESIAN_POINT('Ctrl Pts',(31.1032419044757,-0.303701410540815,
3.20843276639131));
#73228=CARTESIAN_POINT('Ctrl Pts',(31.1044905837684,-0.324035877437877,
3.20642796084972));
#73229=CARTESIAN_POINT('Ctrl Pts',(31.1049724967607,-0.331866168494229,
3.2056269842973));
#73230=CARTESIAN_POINT('Ctrl Pts',(31.1059005302566,-0.346910992517077,
3.20403230395705));
#73231=CARTESIAN_POINT('Ctrl Pts',(31.106346512395,-0.354125940409939,3.20324289720358));
#73232=CARTESIAN_POINT('Ctrl Pts',(31.1073680387804,-0.370616952115945,
3.201382174978));
#73233=CARTESIAN_POINT('Ctrl Pts',(31.1079440838551,-0.379891117504225,
3.20029490693649));
#73234=CARTESIAN_POINT('Ctrl Pts',(31.1094726305353,-0.404432688541827,
3.19730956566316));
#73235=CARTESIAN_POINT('Ctrl Pts',(31.1104273069893,-0.419691310744896,
3.19534246188166));
#73236=CARTESIAN_POINT('Ctrl Pts',(31.1169820348231,-0.523974464562714,
3.18113869804931));
#73237=CARTESIAN_POINT('Ctrl Pts',(31.1226957867421,-0.612459695148485,
3.16529353968943));
#73238=CARTESIAN_POINT('Ctrl Pts',(31.1312864919747,-0.74187806838251,3.13648864763356));
#73239=CARTESIAN_POINT('Ctrl Pts',(31.134078884545,-0.783405023158639,3.12637496625337));
#73240=CARTESIAN_POINT('Ctrl Pts',(31.1373152764683,-0.830936761069419,
3.1137923911115));
#73241=CARTESIAN_POINT('Ctrl Pts',(31.1377392146266,-0.837151321918574,
3.11212734625159));
#73242=CARTESIAN_POINT('Ctrl Pts',(31.1437071565212,-0.924473376089669,
3.08845098151552));
#73243=CARTESIAN_POINT('Ctrl Pts',(31.1493256040755,-1.00469048338039,3.0632949869048));
#73244=CARTESIAN_POINT('Ctrl Pts',(31.1713120903255,-1.31214008878246,2.95350287724719));
#73245=CARTESIAN_POINT('Ctrl Pts',(31.1879744780598,-1.53053146364814,2.84646744972768));
#73246=CARTESIAN_POINT('Ctrl Pts',(31.2053214238543,-1.75862822741037,2.70076649731007));
#73247=CARTESIAN_POINT('Ctrl Pts',(31.2071121718094,-1.7821959302303,2.68527293055207));
#73248=CARTESIAN_POINT('Ctrl Pts',(31.2093561502504,-1.81179541823263,2.66525263833305));
#73249=CARTESIAN_POINT('Ctrl Pts',(31.2098276008651,-1.81801795961574,2.66101201892952));
#73250=CARTESIAN_POINT('Ctrl Pts',(31.2105784621442,-1.82793545137813,2.65420229058835));
#73251=CARTESIAN_POINT('Ctrl Pts',(31.2108588112871,-1.83163993593818,2.6516472162485));
#73252=CARTESIAN_POINT('Ctrl Pts',(31.211390259989,-1.83866568211478,2.64677963759236));
#73253=CARTESIAN_POINT('Ctrl Pts',(31.2116414544237,-1.84198789962386,2.64446866465808));
#73254=CARTESIAN_POINT('Ctrl Pts',(31.2122159460476,-1.84958902990053,2.63915995682519));
#73255=CARTESIAN_POINT('Ctrl Pts',(31.2125389548908,-1.85386500684233,2.63615807465281));
#73256=CARTESIAN_POINT('Ctrl Pts',(31.213555742657,-1.86733138912021,2.62665524389273));
#73257=CARTESIAN_POINT('Ctrl Pts',(31.2142469700604,-1.87649516533766,2.62011644593684));
#73258=CARTESIAN_POINT('Ctrl Pts',(31.2205157131932,-1.95966021579396,2.56011403928519));
#73259=CARTESIAN_POINT('Ctrl Pts',(31.2258915021273,-2.03140047486081,2.50357097013144));
#73260=CARTESIAN_POINT('Ctrl Pts',(31.2477496771461,-2.31893160637899,2.25643951993253));
#73261=CARTESIAN_POINT('Ctrl Pts',(31.263250028093,-2.51110256810998,2.04042841684177));
#73262=CARTESIAN_POINT('Ctrl Pts',(31.2840254493609,-2.71236963561823,1.74194490322321));
#73263=CARTESIAN_POINT('Ctrl Pts',(31.2882440717604,-2.75067690512347,1.6808023622322));
#73264=CARTESIAN_POINT('Ctrl Pts',(31.2942628825759,-2.80148334426456,1.59331480534135));
#73265=CARTESIAN_POINT('Ctrl Pts',(31.296002010293,-2.81572737447259,1.568005187606));
#73266=CARTESIAN_POINT('Ctrl Pts',(31.299066340802,-2.84004982270219,1.52338726835963));
#73267=CARTESIAN_POINT('Ctrl Pts',(31.3003861769416,-2.85027831351838,1.50416264559979));
#73268=CARTESIAN_POINT('Ctrl Pts',(31.3023084145479,-2.86481405096525,1.47616175916599));
#73269=CARTESIAN_POINT('Ctrl Pts',(31.3029052880589,-2.86927757660002,1.46746695735861));
#73270=CARTESIAN_POINT('Ctrl Pts',(31.3039504519946,-2.87700599173559,1.45224219207693));
#73271=CARTESIAN_POINT('Ctrl Pts',(31.3043981226943,-2.88028838802071,1.44572115616103));
#73272=CARTESIAN_POINT('Ctrl Pts',(31.3052657481803,-2.88659593280366,1.4330834060438));
#73273=CARTESIAN_POINT('Ctrl Pts',(31.3056856021823,-2.88962386975111,1.42696812093962));
#73274=CARTESIAN_POINT('Ctrl Pts',(31.3067985817369,-2.89758600680907,1.41075835654535));
#73275=CARTESIAN_POINT('Ctrl Pts',(31.3074928676233,-2.90248684486014,1.4006476779333));
#73276=CARTESIAN_POINT('Ctrl Pts',(31.3099549579941,-2.91963250054836,1.36479888945936));
#73277=CARTESIAN_POINT('Ctrl Pts',(31.3117327388648,-2.93158835718976,1.33892478008489));
#73278=CARTESIAN_POINT('Ctrl Pts',(31.3139614120278,-2.94604759478254,1.30651062769269));
#73279=CARTESIAN_POINT('Ctrl Pts',(31.3144011621319,-2.94887522827616,1.30011589399433));
#73280=CARTESIAN_POINT('Ctrl Pts',(31.330557449065,-3.05183069479925,1.06521679209629));
#73281=CARTESIAN_POINT('Ctrl Pts',(31.3472172188721,-3.12508959796379,0.825909031198407));
#73282=CARTESIAN_POINT('Ctrl Pts',(31.3772841357442,-3.20512887646001,0.388905514104594));
#73283=CARTESIAN_POINT('Ctrl Pts',(31.3905150821367,-3.22278173040772,0.194399018396028));
#73284=CARTESIAN_POINT('Ctrl Pts',(31.4045794950268,-3.22274588361549,-0.0255161102361829));
#73285=CARTESIAN_POINT('Ctrl Pts',(31.4061643337136,-3.22245112344944,-0.0505069351096372));
#73286=CARTESIAN_POINT('Ctrl Pts',(31.4082060354822,-3.22168949455668,-0.0830116157642455));
#73287=CARTESIAN_POINT('Ctrl Pts',(31.4086769155593,-3.2214869939441,-0.090529985258089));
#73288=CARTESIAN_POINT('Ctrl Pts',(31.4094270818381,-3.22112132400558,-0.102543706001211));
#73289=CARTESIAN_POINT('Ctrl Pts',(31.4097073035252,-3.2209750611107,-0.107039487567294));
#73290=CARTESIAN_POINT('Ctrl Pts',(31.4102134432731,-3.22069334016856,-0.115174803177854));
#73291=CARTESIAN_POINT('Ctrl Pts',(31.4104395395049,-3.22056112682172,-0.118814372992826));
#73292=CARTESIAN_POINT('Ctrl Pts',(31.4109810724537,-3.2202291661926,-0.127544635872793));
#73293=CARTESIAN_POINT('Ctrl Pts',(31.4112961740388,-3.22002351742405,-0.13263508217206));
#73294=CARTESIAN_POINT('Ctrl Pts',(31.4122468511133,-3.21936525328147,-0.148024312619176));
#73295=CARTESIAN_POINT('Ctrl Pts',(31.4128803608031,-3.21887528854726,-0.158321554729984));
#73296=CARTESIAN_POINT('Ctrl Pts',(31.4190815910356,-3.21357380493439,-0.25950952887032));
#73297=CARTESIAN_POINT('Ctrl Pts',(31.42444690139,-3.20496276882851,-0.35016979713089));
#73298=CARTESIAN_POINT('Ctrl Pts',(31.4305789503432,-3.19044163039852,-0.455446966742716));
#73299=CARTESIAN_POINT('Ctrl Pts',(31.4314549030594,-3.18825258259106,-0.470526531380754));
#73300=CARTESIAN_POINT('Ctrl Pts',(31.4443682547491,-3.15429625737877,-0.693313947476272));
#73301=CARTESIAN_POINT('Ctrl Pts',(31.4558717632582,-3.10239592895722,-0.897450214191542));
#73302=CARTESIAN_POINT('Ctrl Pts',(31.4772782250561,-2.97376254982325,-1.25348205321784));
#73303=CARTESIAN_POINT('Ctrl Pts',(31.4870070420694,-2.90421593163919,-1.40712443249551));
#73304=CARTESIAN_POINT('Ctrl Pts',(31.4983639603198,-2.81350154599667,-1.57185038242648));
#73305=CARTESIAN_POINT('Ctrl Pts',(31.4995575221663,-2.80385428208745,-1.58899518952283));
#73306=CARTESIAN_POINT('Ctrl Pts',(31.5013222411697,-2.78942770440681,-1.61409315248506));
#73307=CARTESIAN_POINT('Ctrl Pts',(31.501889004364,-2.78476992405964,-1.62211592995961));
#73308=CARTESIAN_POINT('Ctrl Pts',(31.5029008938608,-2.77641087703687,-1.63637182644417));
#73309=CARTESIAN_POINT('Ctrl Pts',(31.5033455277716,-2.7727230822145,-1.6426128029758));
#73310=CARTESIAN_POINT('Ctrl Pts',(31.504276350482,-2.76497227876,-1.65562926867469));
#73311=CARTESIAN_POINT('Ctrl Pts',(31.5047626804751,-2.76090535392729,-1.66240235878185));
#73312=CARTESIAN_POINT('Ctrl Pts',(31.5060327838787,-2.75023935423209,-1.68001850480032));
#73313=CARTESIAN_POINT('Ctrl Pts',(31.5068179938066,-2.74360109905355,-1.690837568752));
#73314=CARTESIAN_POINT('Ctrl Pts',(31.5102512664145,-2.71438544528438,-1.7378283417913));
#73315=CARTESIAN_POINT('Ctrl Pts',(31.5129233886671,-2.69115620144992,-1.77358780696242));
#73316=CARTESIAN_POINT('Ctrl Pts',(31.520002316422,-2.62837500581031,-1.86616005695016));
#73317=CARTESIAN_POINT('Ctrl Pts',(31.5244505347263,-2.58769190148283,-1.92217533139614));
#73318=CARTESIAN_POINT('Ctrl Pts',(31.5436413408014,-2.40700544326516,-2.15481510779151));
#73319=CARTESIAN_POINT('Ctrl Pts',(31.5589735989678,-2.25049647183128,-2.31778903304238));
#73320=CARTESIAN_POINT('Ctrl Pts',(31.5847756108577,-1.95831544950045,-2.56432522365094));
#73321=CARTESIAN_POINT('Ctrl Pts',(31.5952579310794,-1.83107788513926,-2.65667643276602));
#73322=CARTESIAN_POINT('Ctrl Pts',(31.6059350802332,-1.68737804616615,-2.74572713596673));
#73323=CARTESIAN_POINT('Ctrl Pts',(31.6066911438714,-1.67712057384789,-2.7520044998854));
#73324=CARTESIAN_POINT('Ctrl Pts',(31.6077793275476,-1.66223455606751,-2.76100029853469));
#73325=CARTESIAN_POINT('Ctrl Pts',(31.6081143823965,-1.65763412973647,-2.76376472602513));
#73326=CARTESIAN_POINT('Ctrl Pts',(31.6087020792051,-1.64953451243075,-2.76860434243004));
#73327=CARTESIAN_POINT('Ctrl Pts',(31.6089550402622,-1.64603827043442,-2.77068441465842));
#73328=CARTESIAN_POINT('Ctrl Pts',(31.6094824795683,-1.63872743769506,-2.77501523667903));
#73329=CARTESIAN_POINT('Ctrl Pts',(31.6097568764401,-1.63491215102918,-2.77726474032212));
#73330=CARTESIAN_POINT('Ctrl Pts',(31.6104767439983,-1.6248721118458,-2.7831565165705));
#73331=CARTESIAN_POINT('Ctrl Pts',(31.6109213728019,-1.61863970631877,-2.78678579712752));
#73332=CARTESIAN_POINT('Ctrl Pts',(31.6128986631237,-1.59078789804133,-2.80287962348328));
#73333=CARTESIAN_POINT('Ctrl Pts',(31.6144169462331,-1.56903562772546,-2.81511413776269));
#73334=CARTESIAN_POINT('Ctrl Pts',(31.6271823437826,-1.38328140962469,-2.91676910785503));
#73335=CARTESIAN_POINT('Ctrl Pts',(31.637659149537,-1.21191015892472,-2.992039842147));
#73336=CARTESIAN_POINT('Ctrl Pts',(31.6625615569337,-0.790150275129712,
-3.13506056100569));
#73337=CARTESIAN_POINT('Ctrl Pts',(31.6769360845876,-0.536273405546267,
-3.18831218615426));
#73338=CARTESIAN_POINT('Ctrl Pts',(31.6932177673185,-0.265140164853087,
-3.21185390674351));
#73339=CARTESIAN_POINT('Ctrl Pts',(31.6940390270914,-0.251499817466008,
-3.21295077125242));
#73340=CARTESIAN_POINT('Ctrl Pts',(31.6962788801574,-0.214400406016497,
-3.21569635809882));
#73341=CARTESIAN_POINT('Ctrl Pts',(31.6977025952015,-0.190929958730246,
-3.21717520620153));
#73342=CARTESIAN_POINT('Ctrl Pts',(31.6997023643734,-0.158129455741269,
-3.21888174196235));
#73343=CARTESIAN_POINT('Ctrl Pts',(31.7002716222817,-0.148811032453913,
-3.21932599580344));
#73344=CARTESIAN_POINT('Ctrl Pts',(31.7012584037785,-0.132690953681515,
-3.22002437866627));
#73345=CARTESIAN_POINT('Ctrl Pts',(31.701675331044,-0.125890144987925,-3.2202974332603));
#73346=CARTESIAN_POINT('Ctrl Pts',(31.7025415457956,-0.111781990224092,
-3.22081912068506));
#73347=CARTESIAN_POINT('Ctrl Pts',(31.7029909350175,-0.104474567262003,
-3.22106443352196));
#73348=CARTESIAN_POINT('Ctrl Pts',(31.7040469771363,-0.0873306738823321,
-3.22158155970496));
#73349=CARTESIAN_POINT('Ctrl Pts',(31.7046542600163,-0.0774937087897892,
-3.22183319153665));
#73350=CARTESIAN_POINT('Ctrl Pts',(31.706632720485,-0.0455178241931978,
-3.22250461561555));
#73351=CARTESIAN_POINT('Ctrl Pts',(31.7080096244559,-0.023376073238716,
-3.22274128495128));
#73352=CARTESIAN_POINT('Ctrl Pts',(31.7112475528611,0.0284229655212935,
-3.2227611202018));
#73353=CARTESIAN_POINT('Ctrl Pts',(31.7131141291294,0.0580779214703715,
-3.22236310234424));
#73354=CARTESIAN_POINT('Ctrl Pts',(31.719700220006,0.16197589124951,-3.21953397939226));
#73355=CARTESIAN_POINT('Ctrl Pts',(31.7244848019074,0.236132105075009,-3.21494563817498));
#73356=CARTESIAN_POINT('Ctrl Pts',(31.7491120463682,0.61129144228927,-3.1786835341629));
#73357=CARTESIAN_POINT('Ctrl Pts',(31.7700875496439,0.906865114661656,-3.107291427219));
#73358=CARTESIAN_POINT('Ctrl Pts',(31.7909228106255,1.20071295762352,-2.99075065622397));
#73359=CARTESIAN_POINT('Ctrl Pts',(31.7918130847609,1.21327464854142,-2.98567676271985));
#73360=CARTESIAN_POINT('Ctrl Pts',(31.7967232695209,1.28260822550317,-2.95716184624025));
#73361=CARTESIAN_POINT('Ctrl Pts',(31.8006849569311,1.33873745854938,-2.93217892504118));
#73362=CARTESIAN_POINT('Ctrl Pts',(31.8051908758082,1.40319891665997,-2.9012500256173));
#73363=CARTESIAN_POINT('Ctrl Pts',(31.8058228817619,1.41225510188272,-2.89685250650147));
#73364=CARTESIAN_POINT('Ctrl Pts',(31.8067720430191,1.42588060306782,-2.89015712768423));
#73365=CARTESIAN_POINT('Ctrl Pts',(31.8070911129435,1.43046519599901,-2.88789075984663));
#73366=CARTESIAN_POINT('Ctrl Pts',(31.8076600393183,1.43864785995965,-2.88382143929574));
#73367=CARTESIAN_POINT('Ctrl Pts',(31.8079101535613,1.44224795455179,-2.88202265725333));
#73368=CARTESIAN_POINT('Ctrl Pts',(31.8084463865298,1.44997245888146,-2.87814502112768));
#73369=CARTESIAN_POINT('Ctrl Pts',(31.8087323689451,1.45409575697795,-2.876064050805));
#73370=CARTESIAN_POINT('Ctrl Pts',(31.8095160601535,1.4654046027778,-2.87032609950894));
#73371=CARTESIAN_POINT('Ctrl Pts',(31.8100126378669,1.47258098276264,-2.86665097628697));
#73372=CARTESIAN_POINT('Ctrl Pts',(31.8126323433805,1.51049089476066,-2.8470568616918));
#73373=CARTESIAN_POINT('Ctrl Pts',(31.814727106725,1.54098167602527,-2.83066974775283));
#73374=CARTESIAN_POINT('Ctrl Pts',(31.8207786512525,1.62933845920627,-2.78133190081705));
#73375=CARTESIAN_POINT('Ctrl Pts',(31.8246669260992,1.68645693630787,-2.74707392341374));
#73376=CARTESIAN_POINT('Ctrl Pts',(31.8427016850797,1.95018427174449,-2.57756929056213));
#73377=CARTESIAN_POINT('Ctrl Pts',(31.8561150851861,2.14186907493889,-2.4206389240634));
#73378=CARTESIAN_POINT('Ctrl Pts',(31.8736881265182,2.35649858237966,-2.19927288952568));
#73379=CARTESIAN_POINT('Ctrl Pts',(31.8772201950863,2.39796499777074,-2.15398470951607));
#73380=CARTESIAN_POINT('Ctrl Pts',(31.8810498038622,2.44093154423135,-2.10427882129607));
#73381=CARTESIAN_POINT('Ctrl Pts',(31.8813013979548,2.44374526815775,-2.10101052484569));
#73382=CARTESIAN_POINT('Ctrl Pts',(31.8862195519977,2.49857006570099,-2.03706935090795));
#73383=CARTESIAN_POINT('Ctrl Pts',(31.8909627159985,2.54830949233569,-1.97449260278181));
#73384=CARTESIAN_POINT('Ctrl Pts',(31.896698437439,2.60446459142978,-1.89818385869962));
#73385=CARTESIAN_POINT('Ctrl Pts',(31.8975999434085,2.61317716950491,-1.8861714765036));
#73386=CARTESIAN_POINT('Ctrl Pts',(31.8990700969091,2.62719960047433,-1.86655453585588));
#73387=CARTESIAN_POINT('Ctrl Pts',(31.8996367843073,2.63256019793536,-1.85898638442272));
#73388=CARTESIAN_POINT('Ctrl Pts',(31.9006473799141,2.64204047266189,-1.84547878637101));
#73389=CARTESIAN_POINT('Ctrl Pts',(31.9010907919559,2.64617299230767,-1.8395483966338));
#73390=CARTESIAN_POINT('Ctrl Pts',(31.9020253557007,2.65482585172728,-1.82704158194553));
#73391=CARTESIAN_POINT('Ctrl Pts',(31.9025166715137,2.65934178008565,-1.82046217758512));
#73392=CARTESIAN_POINT('Ctrl Pts',(31.9038140205991,2.671179125355,-1.80307792139402));
#73393=CARTESIAN_POINT('Ctrl Pts',(31.90462160638,2.67845936542319,-1.79224533199922));
#73394=CARTESIAN_POINT('Ctrl Pts',(31.9082932948113,2.71115726008248,-1.74294848642564));
#73395=CARTESIAN_POINT('Ctrl Pts',(31.9111857781073,2.73581248610222,-1.70398732405315));
#73396=CARTESIAN_POINT('Ctrl Pts',(31.9189876779968,2.79936400734458,-1.59862420252664));
#73397=CARTESIAN_POINT('Ctrl Pts',(31.9239497257552,2.83673020597455,-1.53133875064609));
#73398=CARTESIAN_POINT('Ctrl Pts',(31.9498188143069,3.0161655111583,-1.17908223516967));
#73399=CARTESIAN_POINT('Ctrl Pts',(31.9719797483963,3.11781930780934,-0.875584491674431));
#73400=CARTESIAN_POINT('Ctrl Pts',(31.996399167963,3.18305669505688,-0.507314728790725));
#73401=CARTESIAN_POINT('Ctrl Pts',(31.9999821251394,3.19134754878536,-0.452238746554153));
#73402=CARTESIAN_POINT('Ctrl Pts',(32.0040528369765,3.19930665256675,-0.388116136712351));
#73403=CARTESIAN_POINT('Ctrl Pts',(32.0046130908301,3.20036907026165,-0.379255865179498));
#73404=CARTESIAN_POINT('Ctrl Pts',(32.0055029445585,3.20200396159674,-0.365125041287943));
#73405=CARTESIAN_POINT('Ctrl Pts',(32.005833851441,3.20260024675012,-0.359857369428019));
#73406=CARTESIAN_POINT('Ctrl Pts',(32.0064167583648,3.20363002126332,-0.350554869469031));
#73407=CARTESIAN_POINT('Ctrl Pts',(32.0066690611967,3.20406889103615,-0.346520665869661));
#73408=CARTESIAN_POINT('Ctrl Pts',(32.0071977630978,3.20497415104665,-0.338050511253339));
#73409=CARTESIAN_POINT('Ctrl Pts',(32.0074740712038,3.20543895129553,-0.333614428838062));
#73410=CARTESIAN_POINT('Ctrl Pts',(32.008204445718,3.20664548457706,-0.321863868530349));
#73411=CARTESIAN_POINT('Ctrl Pts',(32.0086576250436,3.20737140583532,-0.314547740655233));
#73412=CARTESIAN_POINT('Ctrl Pts',(32.0107279953892,3.21058303116174,-0.281012095937483));
#73413=CARTESIAN_POINT('Ctrl Pts',(32.0123290913117,3.21277239367324,-0.254764300912664));
#73414=CARTESIAN_POINT('Ctrl Pts',(32.0264792356516,3.22943426055764,-0.0203491551274071));
#73415=CARTESIAN_POINT('Ctrl Pts',(32.0380755920255,3.22398056375685,0.188769188707624));
#73416=CARTESIAN_POINT('Ctrl Pts',(32.0640333990523,3.16691323639598,0.649778777265243));
#73417=CARTESIAN_POINT('Ctrl Pts',(32.0783918428295,3.10538295617856,0.898957528271592));
#73418=CARTESIAN_POINT('Ctrl Pts',(32.0950041113787,3.00826288004313,1.15621872492417));
#73419=CARTESIAN_POINT('Ctrl Pts',(32.0961709871799,3.00131092428477,1.17414650119475));
#73420=CARTESIAN_POINT('Ctrl Pts',(32.0979096866292,2.99076262547037,1.20064266146669));
#73421=CARTESIAN_POINT('Ctrl Pts',(32.0984773718535,2.98728889997552,1.20925965271242));
#73422=CARTESIAN_POINT('Ctrl Pts',(32.0994890887956,2.98104569454348,1.22455559563851));
#73423=CARTESIAN_POINT('Ctrl Pts',(32.0999326203038,2.97829089676763,1.23124050154442));
#73424=CARTESIAN_POINT('Ctrl Pts',(32.1008667622713,2.97245167289945,1.24527593671515));
#73425=CARTESIAN_POINT('Ctrl Pts',(32.1013575343809,2.96936242747509,1.25262439652089));
#73426=CARTESIAN_POINT('Ctrl Pts',(32.1026519136461,2.96115855889027,1.27193823797456));
#73427=CARTESIAN_POINT('Ctrl Pts',(32.1034570604981,2.95599871316007,1.28388414271871));
#73428=CARTESIAN_POINT('Ctrl Pts',(32.1071019687216,2.93238633113737,1.33765379915358));
#73429=CARTESIAN_POINT('Ctrl Pts',(32.1099696062844,2.91311828231345,1.37911160100351));
#73430=CARTESIAN_POINT('Ctrl Pts',(32.1176889196197,2.85945953894696,1.48841984917936));
#73431=CARTESIAN_POINT('Ctrl Pts',(32.1225918677153,2.82353920206244,1.55548300270557));
#73432=CARTESIAN_POINT('Ctrl Pts',(32.1470608962971,2.63534101101962,1.87881284115265));
#73433=CARTESIAN_POINT('Ctrl Pts',(32.1677063064154,2.45041758858012,2.11432602159685));
#73434=CARTESIAN_POINT('Ctrl Pts',(32.1887693412923,2.2204414365796,2.33585356160358));
#73435=CARTESIAN_POINT('Ctrl Pts',(32.1901691111009,2.20494099196384,2.35049086273359));
#73436=CARTESIAN_POINT('Ctrl Pts',(32.1952125600549,2.14826348814997,2.4029581883151));
#73437=CARTESIAN_POINT('Ctrl Pts',(32.1988108140421,2.10624615585131,2.43987133141046));
#73438=CARTESIAN_POINT('Ctrl Pts',(32.2028969345638,2.05642289285425,2.48139522862742));
#73439=CARTESIAN_POINT('Ctrl Pts',(32.2034579057847,2.04953536418456,2.48708708940991));
#73440=CARTESIAN_POINT('Ctrl Pts',(32.2043486812749,2.03852115084044,2.49611242105123));
#73441=CARTESIAN_POINT('Ctrl Pts',(32.2046797967259,2.03440981416464,2.49946442462005));
#73442=CARTESIAN_POINT('Ctrl Pts',(32.2052629435263,2.02713835303626,2.50536307375515));
#73443=CARTESIAN_POINT('Ctrl Pts',(32.205515278486,2.02398167220108,2.50791391897998));
#73444=CARTESIAN_POINT('Ctrl Pts',(32.2060439122908,2.01734689608931,2.51325465150519));
#73445=CARTESIAN_POINT('Ctrl Pts',(32.2063201206667,2.01386783590622,2.51604327914905));
#73446=CARTESIAN_POINT('Ctrl Pts',(32.2070499470418,2.0046425734538,2.52340636026616));
#73447=CARTESIAN_POINT('Ctrl Pts',(32.2075026803392,1.99888646051604,2.52796843864617));
#73448=CARTESIAN_POINT('Ctrl Pts',(32.2095337917484,1.97291511151948,2.5484081845814));
#73449=CARTESIAN_POINT('Ctrl Pts',(32.2110968997592,1.95252526584211,2.5640638635015));
#73450=CARTESIAN_POINT('Ctrl Pts',(32.2161530595648,1.88534548008219,2.61437952181738));
#73451=CARTESIAN_POINT('Ctrl Pts',(32.2195835957846,1.83782282852045,2.64800106618646));
#73452=CARTESIAN_POINT('Ctrl Pts',(32.2229614699496,1.78943610001022,2.68030520771053));
#73453=CARTESIAN_POINT('Origin',(-1.72497344927317,0.,0.));
#73454=CARTESIAN_POINT('',(33.7168658186985,1.789436210378,2.68030513402635));
#73455=CARTESIAN_POINT('',(33.4682079605267,1.78943620863048,2.68030513519304));
#73456=CARTESIAN_POINT('',(-1.72497344927317,1.78943621037804,2.68030513402633));
#73457=CARTESIAN_POINT('',(32.8965734493162,-3.22274986705245,-0.000925696185107025));
#73458=CARTESIAN_POINT('Ctrl Pts',(32.8965734493162,-3.22274986705245,-0.000925696185104952));
#73459=CARTESIAN_POINT('Ctrl Pts',(32.903176172867,-3.22271898196672,-0.108450073561471));
#73460=CARTESIAN_POINT('Ctrl Pts',(32.9097788964179,-3.21730268941124,-0.215823221241665));
#73461=CARTESIAN_POINT('Ctrl Pts',(32.9163816199687,-3.20657144425315,-0.322516876147978));
#73462=CARTESIAN_POINT('Ctrl Pts',(32.9230102303649,-3.19579812583817,-0.42962883754956));
#73463=CARTESIAN_POINT('Ctrl Pts',(32.9296388407611,-3.17966819140822,-0.536055648712403));
#73464=CARTESIAN_POINT('Ctrl Pts',(32.9362674511573,-3.15830363032908,-0.641276649465874));
#73465=CARTESIAN_POINT('Ctrl Pts',(32.9429096034773,-3.13689542250632,-0.746712611529645));
#73466=CARTESIAN_POINT('Ctrl Pts',(32.9495517557973,-3.11023131595963,-0.850937528863337));
#73467=CARTESIAN_POINT('Ctrl Pts',(32.9561939081173,-3.0784830880185,-0.953446086196845));
#73468=CARTESIAN_POINT('Ctrl Pts',(32.9628566866951,-3.04663627047854,-1.05627296925117));
#73469=CARTESIAN_POINT('Ctrl Pts',(32.9695194652728,-3.00967386291915,-1.1573725235921));
#73470=CARTESIAN_POINT('Ctrl Pts',(32.9761822438506,-2.96781633813462,-1.25625783404571));
#73471=CARTESIAN_POINT('Ctrl Pts',(32.9792975170168,-2.94824528046805,-1.30249301214636));
#73472=CARTESIAN_POINT('Ctrl Pts',(32.982412790183,-2.92760472747754,-1.34824447746458));
#73473=CARTESIAN_POINT('Ctrl Pts',(32.9855280633492,-2.90592057306307,-1.39346445435425));
#73474=CARTESIAN_POINT('Ctrl Pts',(32.991700311442,-2.86295805466186,-1.48305817574598));
#73475=CARTESIAN_POINT('Ctrl Pts',(32.9978725595347,-2.8157725799491,-1.57082083560781));
#73476=CARTESIAN_POINT('Ctrl Pts',(33.0040448076275,-2.76454310125707,-1.65632696162078));
#73477=CARTESIAN_POINT('Ctrl Pts',(33.0102086962801,-2.71338300567364,-1.74171728163733));
#73478=CARTESIAN_POINT('Ctrl Pts',(33.0163725849328,-2.65819001359854,-1.8248567729181));
#73479=CARTESIAN_POINT('Ctrl Pts',(33.0225364735854,-2.59919023201414,-1.9053418854112));
#73480=CARTESIAN_POINT('Ctrl Pts',(33.028693835244,-2.5402529258,-1.98574177153449));
#73481=CARTESIAN_POINT('Ctrl Pts',(33.0348511969025,-2.47751709956189,-2.06349251849753));
#73482=CARTESIAN_POINT('Ctrl Pts',(33.0410085585611,-2.41125316454014,-2.1382178885687));
#73483=CARTESIAN_POINT('Ctrl Pts',(33.0471614227074,-2.34503763058292,-2.21288867710229));
#73484=CARTESIAN_POINT('Ctrl Pts',(33.0533142868537,-2.2752993987495,-2.28453815822827));
#73485=CARTESIAN_POINT('Ctrl Pts',(33.059467151,-2.20234974282361,-2.35282238445336));
#73486=CARTESIAN_POINT('Ctrl Pts',(33.0656176841365,-2.12942772384154,-2.42108074123053));
#73487=CARTESIAN_POINT('Ctrl Pts',(33.0717682172731,-2.05329701500797,-2.48597607986439));
#73488=CARTESIAN_POINT('Ctrl Pts',(33.0779187504096,-1.97430577472716,-2.54720126224431));
#73489=CARTESIAN_POINT('Ctrl Pts',(33.0840685986248,-1.89532333088464,-2.60841962660824));
#73490=CARTESIAN_POINT('Ctrl Pts',(33.0902184468401,-1.81348133223696,-2.66596838118307));
#73491=CARTESIAN_POINT('Ctrl Pts',(33.0963682950553,-1.72916024809905,-2.71958129109869));
#73492=CARTESIAN_POINT('Ctrl Pts',(33.1025191034344,-1.64482599907298,-2.77320257149449));
#73493=CARTESIAN_POINT('Ctrl Pts',(33.1086699118135,-1.55801226235647,-2.82288655359849));
#73494=CARTESIAN_POINT('Ctrl Pts',(33.1148207201927,-1.46912678300237,-2.86841141713756));
#73495=CARTESIAN_POINT('Ctrl Pts',(33.1209781065589,-1.38014624499979,-2.91398496727912));
#73496=CARTESIAN_POINT('Ctrl Pts',(33.1271354929251,-1.28908992735148,-2.95539031831274));
#73497=CARTESIAN_POINT('Ctrl Pts',(33.1332928792913,-1.19638826741843,-2.99245261885356));
#73498=CARTESIAN_POINT('Ctrl Pts',(33.1394537020282,-1.10363487169103,-3.02953560346369));
#73499=CARTESIAN_POINT('Ctrl Pts',(33.1456145247652,-1.00923471541523,-3.06227056827951));
#73500=CARTESIAN_POINT('Ctrl Pts',(33.1517753475021,-0.913634220835751,
-3.09053232842141));
#73501=CARTESIAN_POINT('Ctrl Pts',(33.1579464704188,-0.817873893338074,
-3.11884133894226));
#73502=CARTESIAN_POINT('Ctrl Pts',(33.1641175933355,-0.720909640992276,
-3.14266210268172));
#73503=CARTESIAN_POINT('Ctrl Pts',(33.1702887162522,-0.623199056571544,
-3.16192038141196));
#73504=CARTESIAN_POINT('Ctrl Pts',(33.1749842381978,-0.548852426362706,
-3.17657373893411));
#73505=CARTESIAN_POINT('Ctrl Pts',(33.1796797601433,-0.474073939488129,
-3.18858671220633));
#73506=CARTESIAN_POINT('Ctrl Pts',(33.1843752820889,-0.399066287633495,
-3.197946788265));
#73507=CARTESIAN_POINT('Ctrl Pts',(33.1905475301817,-0.300468976946768,
-3.21025057733703));
#73508=CARTESIAN_POINT('Ctrl Pts',(33.1967197782744,-0.201128575823972,
-3.21801190419797));
#73509=CARTESIAN_POINT('Ctrl Pts',(33.2028920263672,-0.10149975673091,-3.22115124790556));
#73510=CARTESIAN_POINT('Ctrl Pts',(33.2090559150198,-0.00200587083171862,
-3.22428633981457));
#73511=CARTESIAN_POINT('Ctrl Pts',(33.2152198036724,0.0977752262974409,
-3.22281187710088));
#73512=CARTESIAN_POINT('Ctrl Pts',(33.2213836923251,0.197381806395091,-3.21669985932853));
#73513=CARTESIAN_POINT('Ctrl Pts',(33.2275410539836,0.296882912238404,-3.21059431362376));
#73514=CARTESIAN_POINT('Ctrl Pts',(33.2336984156422,0.396209437276115,-3.19986100234528));
#73515=CARTESIAN_POINT('Ctrl Pts',(33.2398557773007,0.494898672848096,-3.18452396224509));
#73516=CARTESIAN_POINT('Ctrl Pts',(33.246008641447,0.593515822993007,-3.1691981247556));
#73517=CARTESIAN_POINT('Ctrl Pts',(33.2521615055933,0.691496181225578,-3.14927531055976));
#73518=CARTESIAN_POINT('Ctrl Pts',(33.2583143697396,0.788382106926401,-3.12483139000783));
#73519=CARTESIAN_POINT('Ctrl Pts',(33.2644649028761,0.885231327438567,-3.10039673002403));
#73520=CARTESIAN_POINT('Ctrl Pts',(33.2706154360127,0.980986518567305,-3.07144447318973));
#73521=CARTESIAN_POINT('Ctrl Pts',(33.2767659691492,1.07520106018206,-3.03810142073687));
#73522=CARTESIAN_POINT('Ctrl Pts',(33.2829158173644,1.1694051100967,-3.00476208135527));
#73523=CARTESIAN_POINT('Ctrl Pts',(33.2890656655796,1.26206844210807,-2.96703306339426));
#73524=CARTESIAN_POINT('Ctrl Pts',(33.2952155137948,1.35276137341589,-2.92509046511282));
#73525=CARTESIAN_POINT('Ctrl Pts',(33.301366322174,1.44346846443605,-2.88314131841446));
#73526=CARTESIAN_POINT('Ctrl Pts',(33.3075171305531,1.53220414941774,-2.83697746706725));
#73527=CARTESIAN_POINT('Ctrl Pts',(33.3136679389322,1.61856135924482,-2.78682196935139));
#73528=CARTESIAN_POINT('Ctrl Pts',(33.3198253252984,1.70501092386053,-2.73661283279751));
#73529=CARTESIAN_POINT('Ctrl Pts',(33.3259827116646,1.7890765575395,-2.68240374396516));
#73530=CARTESIAN_POINT('Ctrl Pts',(33.3321400980308,1.87037843184976,-2.62446224666525));
#73531=CARTESIAN_POINT('Ctrl Pts',(33.3383009207678,1.95172567985723,-2.56648841284203));
#73532=CARTESIAN_POINT('Ctrl Pts',(33.3444617435047,2.03030575514491,-2.50477829054302));
#73533=CARTESIAN_POINT('Ctrl Pts',(33.3506225662417,2.10577196599746,-2.43963972539373));
#73534=CARTESIAN_POINT('Ctrl Pts',(33.3567936891584,2.18136434758539,-2.37439225613261));
#73535=CARTESIAN_POINT('Ctrl Pts',(33.3629648120751,2.25383215046458,-2.30570519356653));
#73536=CARTESIAN_POINT('Ctrl Pts',(33.3691359349917,2.32286549967818,-2.23392332744542));
#73537=CARTESIAN_POINT('Ctrl Pts',(33.3738314569373,2.37539201885263,-2.1793054998282));
#73538=CARTESIAN_POINT('Ctrl Pts',(33.378526978883,2.42593093258027,-2.12289670773472));
#73539=CARTESIAN_POINT('Ctrl Pts',(33.3832225008286,2.47436211737472,-2.06486069133026));
#73540=CARTESIAN_POINT('Ctrl Pts',(33.3893947489213,2.53802474986598,-1.98857253940306));
#73541=CARTESIAN_POINT('Ctrl Pts',(33.3955669970141,2.59826801926057,-1.90920313734829));
#73542=CARTESIAN_POINT('Ctrl Pts',(33.4017392451069,2.65477918577529,-1.8270919619095));
#73543=CARTESIAN_POINT('Ctrl Pts',(33.4079031337595,2.71121381587955,-1.74509199448522));
#73544=CARTESIAN_POINT('Ctrl Pts',(33.4140670224121,2.76392614559788,-1.66035798903141));
#73545=CARTESIAN_POINT('Ctrl Pts',(33.4202309110647,2.81264295951523,-1.57326321535508));
#73546=CARTESIAN_POINT('Ctrl Pts',(33.4263882727233,2.86130818678425,-1.48626066707487));
#73547=CARTESIAN_POINT('Ctrl Pts',(33.4325456343818,2.90598609877098,-1.39690269749423));
#73548=CARTESIAN_POINT('Ctrl Pts',(33.4387029960404,2.94644672409517,-1.30559153818063));
#73549=CARTESIAN_POINT('Ctrl Pts',(33.4448558601867,2.98687779582682,-1.21434707513717));
#73550=CARTESIAN_POINT('Ctrl Pts',(33.451008724333,3.02309752986778,-1.12115265475232));
#73551=CARTESIAN_POINT('Ctrl Pts',(33.4571615884793,3.05492229806421,-1.02643427226983));
#73552=CARTESIAN_POINT('Ctrl Pts',(33.4633121216158,3.08673500946175,-0.931751773803268));
#73553=CARTESIAN_POINT('Ctrl Pts',(33.4694626547523,3.11415592522857,-0.83554687173272));
#73554=CARTESIAN_POINT('Ctrl Pts',(33.4756131878889,3.13705021961368,-0.738263829617687));
#73555=CARTESIAN_POINT('Ctrl Pts',(33.4817630361041,3.15994196449776,-0.640991620909962));
#73556=CARTESIAN_POINT('Ctrl Pts',(33.4879128843193,3.17830799068462,-0.542641933681937));
#73557=CARTESIAN_POINT('Ctrl Pts',(33.4940627325345,3.19206409970979,-0.443671439067201));
#73558=CARTESIAN_POINT('Ctrl Pts',(33.5002135409136,3.20582235644969,-0.344685492380201));
#73559=CARTESIAN_POINT('Ctrl Pts',(33.5063643492928,3.21496920663792,-0.245078976067287));
#73560=CARTESIAN_POINT('Ctrl Pts',(33.5125151576719,3.21947218244898,-0.145314930193683));
#73561=CARTESIAN_POINT('Ctrl Pts',(33.5186725440381,3.22397997397121,-0.0454441915796242));
#73562=CARTESIAN_POINT('Ctrl Pts',(33.5248299304043,3.22383395411364,0.0545839782330701));
#73563=CARTESIAN_POINT('Ctrl Pts',(33.5309873167704,3.2190538059926,0.154305400503576));
#73564=CARTESIAN_POINT('Ctrl Pts',(33.5371481395074,3.21427099012257,0.254082476221889));
#73565=CARTESIAN_POINT('Ctrl Pts',(33.5433089622444,3.20484893645769,0.353552031016853));
#73566=CARTESIAN_POINT('Ctrl Pts',(33.5494697849813,3.190859147722,0.452255969445233));
#73567=CARTESIAN_POINT('Ctrl Pts',(33.555640907898,3.17684596968515,0.551124929389278));
#73568=CARTESIAN_POINT('Ctrl Pts',(33.5618120308147,3.15824988339817,0.649225289189306));
#73569=CARTESIAN_POINT('Ctrl Pts',(33.5679831537314,3.13519337651014,0.746109947921181));
#73570=CARTESIAN_POINT('Ctrl Pts',(33.5726786756769,3.11764999979536,0.819828142714125));
#73571=CARTESIAN_POINT('Ctrl Pts',(33.5773741976225,3.09752532918172,0.892842738917816));
#73572=CARTESIAN_POINT('Ctrl Pts',(33.582069719568,3.07489215235679,0.964964151600781));
#73573=CARTESIAN_POINT('Ctrl Pts',(33.5882407086637,3.04514698472547,1.05974817271529));
#73574=CARTESIAN_POINT('Ctrl Pts',(33.5944116977594,3.01096277059836,1.15332235267896));
#73575=CARTESIAN_POINT('Ctrl Pts',(33.6005826868551,2.97245590277785,1.24524032561636));
#73576=CARTESIAN_POINT('Ctrl Pts',(33.6067458895631,2.93399762188527,1.33704231893298));
#73577=CARTESIAN_POINT('Ctrl Pts',(33.612909092271,2.89122768971275,1.42719186031542));
#73578=CARTESIAN_POINT('Ctrl Pts',(33.619072294979,2.84431230542675,1.51525742753433));
#73579=CARTESIAN_POINT('Ctrl Pts',(33.6252293704408,2.79744356281732,1.60323544296687));
#73580=CARTESIAN_POINT('Ctrl Pts',(33.6313864459026,2.74643776143771,1.68913322053688));
#73581=CARTESIAN_POINT('Ctrl Pts',(33.6375435213645,2.69150886839109,1.772539865242));
#73582=CARTESIAN_POINT('Ctrl Pts',(33.6436961230225,2.6366198873276,1.85588590569292));
#73583=CARTESIAN_POINT('Ctrl Pts',(33.6498487246805,2.57781371995906,1.93674405032632));
#73584=CARTESIAN_POINT('Ctrl Pts',(33.6560013263384,2.51534937764723,2.01472952796888));
#73585=CARTESIAN_POINT('Ctrl Pts',(33.66215179013,2.45290674004298,2.09268790771966));
#73586=CARTESIAN_POINT('Ctrl Pts',(33.6683022539216,2.38680872279129,2.16777526396096));
#73587=CARTESIAN_POINT('Ctrl Pts',(33.6744527177132,2.31735611603887,2.23963796046532));
#73588=CARTESIAN_POINT('Ctrl Pts',(33.680601990954,2.24791695328996,2.31148674644293));
#73589=CARTESIAN_POINT('Ctrl Pts',(33.6867512641947,2.1751247975078,2.38011180499616));
#73590=CARTESIAN_POINT('Ctrl Pts',(33.6929005374355,2.09931816608955,2.44519545231591));
#73591=CARTESIAN_POINT('Ctrl Pts',(33.6990516521312,2.02348883369676,2.5102985895166));
#73592=CARTESIAN_POINT('Ctrl Pts',(33.7052027668269,1.94464355533572,2.57185791788098));
#73593=CARTESIAN_POINT('Ctrl Pts',(33.7113538815226,1.86315432946049,2.62959569270879));
#73594=CARTESIAN_POINT('Ctrl Pts',(33.7131911939146,1.83881383640885,2.64684172605761));
#73595=CARTESIAN_POINT('Ctrl Pts',(33.7150285063065,1.81423765800748,2.6637470907295));
#73596=CARTESIAN_POINT('Ctrl Pts',(33.7168658186985,1.789436210378,2.68030513402635));
#73597=CARTESIAN_POINT('Ctrl Pts',(32.4670258968214,1.789436210378,2.68030513402635));
#73598=CARTESIAN_POINT('Ctrl Pts',(32.4731761355784,1.70635327281358,2.73577330257738));
#73599=CARTESIAN_POINT('Ctrl Pts',(32.4793263743353,1.62065793516169,2.78739544615674));
#73600=CARTESIAN_POINT('Ctrl Pts',(32.4854766130923,1.53274485189673,2.83492694464673));
#73601=CARTESIAN_POINT('Ctrl Pts',(32.4916265325084,1.44483633337075,2.88245597514362));
#73602=CARTESIAN_POINT('Ctrl Pts',(32.4977764519246,1.3547106804889,2.92589457653808));
#73603=CARTESIAN_POINT('Ctrl Pts',(32.5039263713407,1.26278750833372,2.96504389028161));
#73604=CARTESIAN_POINT('Ctrl Pts',(32.5100776164577,1.1708445208569,3.00420164320566));
#73605=CARTESIAN_POINT('Ctrl Pts',(32.5162288615748,1.07710364398436,3.03906810147295));
#73606=CARTESIAN_POINT('Ctrl Pts',(32.5223801066918,0.98200389695119,3.06949277713317));
#73607=CARTESIAN_POINT('Ctrl Pts',(32.5285381283277,0.886799383286437,3.09995097013581));
#73608=CARTESIAN_POINT('Ctrl Pts',(32.5346961499636,0.790233425364579,3.12595747949633));
#73609=CARTESIAN_POINT('Ctrl Pts',(32.5408541715995,0.692759459672458,3.14741193578698));
#73610=CARTESIAN_POINT('Ctrl Pts',(32.5470159581728,0.595225899617504,3.16887950906372));
#73611=CARTESIAN_POINT('Ctrl Pts',(32.5531777447461,0.496783654244963,3.18578941460701));
#73612=CARTESIAN_POINT('Ctrl Pts',(32.5593395313194,0.397893539858509,3.1980929150728));
#73613=CARTESIAN_POINT('Ctrl Pts',(32.5655112110428,0.298844650944925,3.21041616961089));
#73614=CARTESIAN_POINT('Ctrl Pts',(32.5716828907662,0.199346889868214,3.21811821901011));
#73615=CARTESIAN_POINT('Ctrl Pts',(32.5778545704896,0.0998633265283507,
3.22120239639093));
#73616=CARTESIAN_POINT('Ctrl Pts',(32.5811809222831,0.0462446450407157,
3.22286467625991));
#73617=CARTESIAN_POINT('Ctrl Pts',(32.5845072740765,-0.00736995105583313,
3.22318641425991));
#73618=CARTESIAN_POINT('Ctrl Pts',(32.58783362587,-0.0609086335585425,3.22217437468211));
#73619=CARTESIAN_POINT('Ctrl Pts',(32.5940058739627,-0.160252915668906,
3.22029647368372));
#73620=CARTESIAN_POINT('Ctrl Pts',(32.6001781220555,-0.259685125527568,
3.21381657148514));
#73621=CARTESIAN_POINT('Ctrl Pts',(32.6063503701483,-0.358743898115725,
3.20272077741172));
#73622=CARTESIAN_POINT('Ctrl Pts',(32.6125142588009,-0.457668509557358,
3.19164001102757));
#73623=CARTESIAN_POINT('Ctrl Pts',(32.6186781474535,-0.556220261123532,
3.17595582638922));
#73624=CARTESIAN_POINT('Ctrl Pts',(32.6248420361061,-0.653938148823915,
3.15570633298042));
#73625=CARTESIAN_POINT('Ctrl Pts',(32.6309993977646,-0.751552562222665,
3.13547828193227));
#73626=CARTESIAN_POINT('Ctrl Pts',(32.6371567594232,-0.848334444220762,
3.11069462070218));
#73627=CARTESIAN_POINT('Ctrl Pts',(32.6433141210817,-0.943829238858411,
3.08144510422885));
#73628=CARTESIAN_POINT('Ctrl Pts',(32.649466985228,-1.03925428137959,3.05221695243501));
#73629=CARTESIAN_POINT('Ctrl Pts',(32.6556198493743,-1.13339369159259,3.01852955761725));
#73630=CARTESIAN_POINT('Ctrl Pts',(32.6617727135206,-1.22580531920612,2.98052325639408));
#73631=CARTESIAN_POINT('Ctrl Pts',(32.6679232466572,-1.31818193671698,2.94253135384068));
#73632=CARTESIAN_POINT('Ctrl Pts',(32.6740737797937,-1.40883167097371,2.90022396106922));
#73633=CARTESIAN_POINT('Ctrl Pts',(32.6802243129303,-1.49733054031327,2.85379025430131));
#73634=CARTESIAN_POINT('Ctrl Pts',(32.6863741611455,-1.58581955444775,2.80736171837578));
#73635=CARTESIAN_POINT('Ctrl Pts',(32.6925240093607,-1.67215779521927,2.75680798383333));
#73636=CARTESIAN_POINT('Ctrl Pts',(32.6986738575759,-1.75594507307874,2.70236460582774));
#73637=CARTESIAN_POINT('Ctrl Pts',(32.704824665955,-1.83974543248441,2.64791272768247));
#73638=CARTESIAN_POINT('Ctrl Pts',(32.7109754743341,-1.92099367362728,2.58957023654973));
#73639=CARTESIAN_POINT('Ctrl Pts',(32.7171262827133,-1.99931868428552,2.52761594415901));
#73640=CARTESIAN_POINT('Ctrl Pts',(32.7232836690795,-2.0777274596903,2.46559539469975));
#73641=CARTESIAN_POINT('Ctrl Pts',(32.7294410554456,-2.15320642046319,2.39995560068344));
#73642=CARTESIAN_POINT('Ctrl Pts',(32.7355984418118,-2.22541775868719,2.33101552157417));
#73643=CARTESIAN_POINT('Ctrl Pts',(32.7417592645488,-2.2976693972786,2.26203696775185));
#73644=CARTESIAN_POINT('Ctrl Pts',(32.7479200872858,-2.36664948169988,2.18975477506497));
#73645=CARTESIAN_POINT('Ctrl Pts',(32.7540809100227,-2.43205874772026,2.11452306919015));
#73646=CARTESIAN_POINT('Ctrl Pts',(32.7602520329394,-2.49757737043281,2.03916558464512));
#73647=CARTESIAN_POINT('Ctrl Pts',(32.7664231558561,-2.559512980297,1.96084907777183));
#73648=CARTESIAN_POINT('Ctrl Pts',(32.7725942787728,-2.61760802055093,1.87995899243772));
#73649=CARTESIAN_POINT('Ctrl Pts',(32.7772898007184,-2.66181173195385,1.81841084698782));
#73650=CARTESIAN_POINT('Ctrl Pts',(32.7819853226639,-2.70379281926605,1.75537338245911));
#73651=CARTESIAN_POINT('Ctrl Pts',(32.7866808446095,-2.7434557287003,1.69102579139454));
#73652=CARTESIAN_POINT('Ctrl Pts',(32.7930369414377,-2.79714545601391,1.60392162614735));
#73653=CARTESIAN_POINT('Ctrl Pts',(32.7993930382659,-2.84676563256974,1.51412452493224));
#73654=CARTESIAN_POINT('Ctrl Pts',(32.8057491350941,-2.89204502204965,1.42203837955867));
#73655=CARTESIAN_POINT('Ctrl Pts',(32.8120949271868,-2.93725100293519,1.33010152759587));
#73656=CARTESIAN_POINT('Ctrl Pts',(32.8184407192795,-2.9781300244835,1.23588337090644));
#73657=CARTESIAN_POINT('Ctrl Pts',(32.8247865113722,-3.0144549709217,1.13981524414507));
#73658=CARTESIAN_POINT('Ctrl Pts',(32.8311205920994,-3.05071287849111,1.0439244142327));
#73659=CARTESIAN_POINT('Ctrl Pts',(32.8374546728266,-3.08243331286468,0.94619078659277));
#73660=CARTESIAN_POINT('Ctrl Pts',(32.8437887535538,-3.10943629476629,0.847067583661478));
#73661=CARTESIAN_POINT('Ctrl Pts',(32.8501159540983,-3.13640994558483,0.748052049983551));
#73662=CARTESIAN_POINT('Ctrl Pts',(32.8564431546429,-3.15867623335824,0.647650326955835));
#73663=CARTESIAN_POINT('Ctrl Pts',(32.8627703551874,-3.17610418537993,0.546333017592838));
#73664=CARTESIAN_POINT('Ctrl Pts',(32.8690905736384,-3.19351290558005,0.445127512325509));
#73665=CARTESIAN_POINT('Ctrl Pts',(32.8754107920893,-3.20609385586696,0.343008825151237));
#73666=CARTESIAN_POINT('Ctrl Pts',(32.8817310105403,-3.21376678477098,0.240459176582594));
#73667=CARTESIAN_POINT('Ctrl Pts',(32.8866784901179,-3.21977316878248,0.160183107658706));
#73668=CARTESIAN_POINT('Ctrl Pts',(32.8916259696955,-3.22277300950498,0.07964327837657));
#73669=CARTESIAN_POINT('Ctrl Pts',(32.8965734492731,-3.22274986705265,-0.000925695482814911));
#73670=CARTESIAN_POINT('',(32.6496983329207,-3.22274855022239,0.00295378027726991));
#73671=CARTESIAN_POINT('Ctrl Pts',(32.2229614699496,1.78943610001022,2.68030520771053));
#73672=CARTESIAN_POINT('Ctrl Pts',(32.2311765813675,1.6717578365648,2.75887004136827));
#73673=CARTESIAN_POINT('Ctrl Pts',(32.2390848340268,1.54896895161024,2.82964254777507));
#73674=CARTESIAN_POINT('Ctrl Pts',(32.2606380892181,1.20284676547122,2.99980551990526));
#73675=CARTESIAN_POINT('Ctrl Pts',(32.2742759836249,0.972351721218044,3.08223738364988));
#73676=CARTESIAN_POINT('Ctrl Pts',(32.2893277163545,0.727339594247371,3.13961032517539));
#73677=CARTESIAN_POINT('Ctrl Pts',(32.2897852986577,0.719898064168698,3.14132498398815));
#73678=CARTESIAN_POINT('Ctrl Pts',(32.2919298039605,0.685056870534286,3.14922270076477));
#73679=CARTESIAN_POINT('Ctrl Pts',(32.2936268976391,0.657583863789359,3.15507367912768));
#73680=CARTESIAN_POINT('Ctrl Pts',(32.2960147192698,0.619088017945855,3.16274758200143));
#73681=CARTESIAN_POINT('Ctrl Pts',(32.296695755128,0.608126341141233,3.16487355034997));
#73682=CARTESIAN_POINT('Ctrl Pts',(32.2977951229357,0.590461253158554,3.16820445294952));
#73683=CARTESIAN_POINT('Ctrl Pts',(32.2982123093913,0.583764619345555,3.16944519044626));
#73684=CARTESIAN_POINT('Ctrl Pts',(32.299078609013,0.569873470822747,3.17197339336959));
#73685=CARTESIAN_POINT('Ctrl Pts',(32.2995278224637,0.56267841483191,3.17325762916782));
#73686=CARTESIAN_POINT('Ctrl Pts',(32.3004199791209,0.548405145610037,3.1757551750335));
#73687=CARTESIAN_POINT('Ctrl Pts',(32.3008628927341,0.541327120505095,3.17696932354594));
#73688=CARTESIAN_POINT('Ctrl Pts',(32.3023299333626,0.517909826850498,3.18090574467427));
#73689=CARTESIAN_POINT('Ctrl Pts',(32.3033573074268,0.50155383542279,3.18352566801759));
#73690=CARTESIAN_POINT('Ctrl Pts',(32.3111678022377,0.377548903745032,3.20240959009859));
#73691=CARTESIAN_POINT('Ctrl Pts',(32.3181193383071,0.269169598260056,3.21333370976967));
#73692=CARTESIAN_POINT('Ctrl Pts',(32.3387473180987,-0.0465317649755937,
3.22907143515109));
#73693=CARTESIAN_POINT('Ctrl Pts',(32.3528084420133,-0.254012200876999,
3.21939860024077));
#73694=CARTESIAN_POINT('Ctrl Pts',(32.3741337676163,-0.566280805953381,
3.17445577017493));
#73695=CARTESIAN_POINT('Ctrl Pts',(32.3814158743773,-0.672623503361394,
3.15363661035685));
#73696=CARTESIAN_POINT('Ctrl Pts',(32.3893345942766,-0.789744375024898,
3.12451194039179));
#73697=CARTESIAN_POINT('Ctrl Pts',(32.3901450609702,-0.801749793785433,
3.12145291808912));
#73698=CARTESIAN_POINT('Ctrl Pts',(32.3944323840439,-0.86537017552225,3.10485096321226));
#73699=CARTESIAN_POINT('Ctrl Pts',(32.3978625638344,-0.916664051078385,
3.09009593110946));
#73700=CARTESIAN_POINT('Ctrl Pts',(32.4017791283241,-0.975973399836583,
3.07142818171962));
#73701=CARTESIAN_POINT('Ctrl Pts',(32.4023320924848,-0.984364795491938,
3.06874911100708));
#73702=CARTESIAN_POINT('Ctrl Pts',(32.4032125736964,-0.99775661690011,3.06441300137637));
#73703=CARTESIAN_POINT('Ctrl Pts',(32.4035413556762,-1.00276407480465,3.06277807240332));
#73704=CARTESIAN_POINT('Ctrl Pts',(32.4041218249331,-1.01161729386561,3.05986346756012));
#73705=CARTESIAN_POINT('Ctrl Pts',(32.4043738066516,-1.01546467428422,3.05858880619186));
#73706=CARTESIAN_POINT('Ctrl Pts',(32.4049032317049,-1.0235571911871,3.05589075155576));
#73707=CARTESIAN_POINT('Ctrl Pts',(32.4051805789702,-1.02780175767006,3.05446577269861));
#73708=CARTESIAN_POINT('Ctrl Pts',(32.4059166649045,-1.03908020774752,3.05065321853523));
#73709=CARTESIAN_POINT('Ctrl Pts',(32.4063744915315,-1.0461088810643,3.04825014548098));
#73710=CARTESIAN_POINT('Ctrl Pts',(32.4084570554354,-1.07813981431673,3.03717507125781));
#73711=CARTESIAN_POINT('Ctrl Pts',(32.4100655686224,-1.10304384824495,3.02821931957473));
#73712=CARTESIAN_POINT('Ctrl Pts',(32.4144178833676,-1.17077003623107,3.00291786663811));
#73713=CARTESIAN_POINT('Ctrl Pts',(32.4171305753043,-1.21335963659518,2.98596333271594));
#73714=CARTESIAN_POINT('Ctrl Pts',(32.4262678153603,-1.35739138226532,2.92503466593221));
#73715=CARTESIAN_POINT('Ctrl Pts',(32.4325209947079,-1.45693124112177,2.8767505783729));
#73716=CARTESIAN_POINT('Ctrl Pts',(32.4460187442791,-1.66771884737423,2.76074984021439));
#73717=CARTESIAN_POINT('Ctrl Pts',(32.453233833109,-1.77773956052826,2.69122048375457));
#73718=CARTESIAN_POINT('Ctrl Pts',(32.4705399405685,-2.02659577081193,2.51201646809973));
#73719=CARTESIAN_POINT('Ctrl Pts',(32.4807172636519,-2.16118457848172,2.39720366811364));
#73720=CARTESIAN_POINT('Ctrl Pts',(32.492456832024,-2.29823435826055,2.25932588892734));
#73721=CARTESIAN_POINT('Ctrl Pts',(32.4935366252251,-2.31068247137538,2.24659322857556));
#73722=CARTESIAN_POINT('Ctrl Pts',(32.4951772654397,-2.32935484968002,2.22717466022778));
#73723=CARTESIAN_POINT('Ctrl Pts',(32.4957347067265,-2.33565739310087,2.22056423510824));
#73724=CARTESIAN_POINT('Ctrl Pts',(32.4967066348567,-2.34657314692069,2.20901735571762));
#73725=CARTESIAN_POINT('Ctrl Pts',(32.4971205681824,-2.35119911371783,2.20409299673621));
#73726=CARTESIAN_POINT('Ctrl Pts',(32.4979860413732,-2.36082329750307,2.19378324021374));
#73727=CARTESIAN_POINT('Ctrl Pts',(32.4984377005421,-2.36581864616443,2.18839522918309));
#73728=CARTESIAN_POINT('Ctrl Pts',(32.4993366785394,-2.37570719293694,2.17765595883385));
#73729=CARTESIAN_POINT('Ctrl Pts',(32.4997839741521,-2.38060084324102,2.17230517317434));
#73730=CARTESIAN_POINT('Ctrl Pts',(32.5008306807971,-2.39199030138518,2.15976707389633));
#73731=CARTESIAN_POINT('Ctrl Pts',(32.5014306918399,-2.39847181570245,2.15256692378927));
#73732=CARTESIAN_POINT('Ctrl Pts',(32.5049324961434,-2.4360229292316,2.11047217585016));
#73733=CARTESIAN_POINT('Ctrl Pts',(32.5078646251329,-2.46636186623155,2.07493597288023));
#73734=CARTESIAN_POINT('Ctrl Pts',(32.5185346819283,-2.57277335540922,1.94466319719758));
#73735=CARTESIAN_POINT('Ctrl Pts',(32.5264496047245,-2.64423973926204,1.84631200858033));
#73736=CARTESIAN_POINT('Ctrl Pts',(32.5407152334136,-2.76048784073444,1.6656933844388));
#73737=CARTESIAN_POINT('Ctrl Pts',(32.5469954517289,-2.80756216939516,1.58506175453716));
#73738=CARTESIAN_POINT('Ctrl Pts',(32.563861270865,-2.92387393894476,1.36435501323778));
#73739=CARTESIAN_POINT('Ctrl Pts',(32.5744845067112,-2.98654361969685,1.22109147762472));
#73740=CARTESIAN_POINT('Ctrl Pts',(32.5898837124654,-3.06428734487769,1.00110557192209));
#73741=CARTESIAN_POINT('Ctrl Pts',(32.5948914002713,-3.08737577887558,0.927460139995997));
#73742=CARTESIAN_POINT('Ctrl Pts',(32.6004405126205,-3.11066466246883,0.842614992459523));
#73743=CARTESIAN_POINT('Ctrl Pts',(32.6011202106373,-3.11347654986578,0.832164917042117));
#73744=CARTESIAN_POINT('Ctrl Pts',(32.6021218754553,-3.11756072589531,0.816675998147852));
#73745=CARTESIAN_POINT('Ctrl Pts',(32.6024461335052,-3.11887351482204,0.811648054911674));
#73746=CARTESIAN_POINT('Ctrl Pts',(32.6030207746317,-3.12118349457647,0.802712537983304));
#73747=CARTESIAN_POINT('Ctrl Pts',(32.6032714363748,-3.12218551568387,0.79880625421403));
#73748=CARTESIAN_POINT('Ctrl Pts',(32.6038049884276,-3.12430644504244,0.790473053812531));
#73749=CARTESIAN_POINT('Ctrl Pts',(32.6040877570126,-3.12542327446057,0.786045652245447));
#73750=CARTESIAN_POINT('Ctrl Pts',(32.6048536823619,-3.12842864524872,0.77402391046774));
#73751=CARTESIAN_POINT('Ctrl Pts',(32.6053357921226,-3.13029895605099,0.766424980761924));
#73752=CARTESIAN_POINT('Ctrl Pts',(32.6063975800741,-3.1343700289073,0.749621009189221));
#73753=CARTESIAN_POINT('Ctrl Pts',(32.6069765464908,-3.13655796767299,0.740412895633103));
#73754=CARTESIAN_POINT('Ctrl Pts',(32.6087317352373,-3.14309199999781,0.712365113551878));
#73755=CARTESIAN_POINT('Ctrl Pts',(32.6099011504097,-3.14730923633366,0.693495483819581));
#73756=CARTESIAN_POINT('Ctrl Pts',(32.624621409482,-3.19860803990296,0.453851897613045));
#73757=CARTESIAN_POINT('Ctrl Pts',(32.6370704181691,-3.2225416427767,0.228738105582529));
#73758=CARTESIAN_POINT('Ctrl Pts',(32.6496981158975,-3.22274864554512,0.00295468053696055));
#73759=CARTESIAN_POINT('Ctrl Pts',(32.6496981667624,-3.22274864637881,0.00295377107196897));
#73760=CARTESIAN_POINT('Ctrl Pts',(32.6625673399754,-3.22295954265633,-0.227147234168067));
#73761=CARTESIAN_POINT('Ctrl Pts',(32.6755727780319,-3.19852845568629,-0.456583634416496));
#73762=CARTESIAN_POINT('Ctrl Pts',(32.6903769391481,-3.14658318365223,-0.696688345641234));
#73763=CARTESIAN_POINT('Ctrl Pts',(32.6913194246516,-3.1431778142581,-0.711894372415847));
#73764=CARTESIAN_POINT('Ctrl Pts',(32.692852679855,-3.13747999714007,-0.736498745073295));
#73765=CARTESIAN_POINT('Ctrl Pts',(32.6934412837706,-3.13525524884396,-0.7459126325254));
#73766=CARTESIAN_POINT('Ctrl Pts',(32.6944731721616,-3.13128997221173,-0.762360265232649));
#73767=CARTESIAN_POINT('Ctrl Pts',(32.6949158564687,-3.12956803396871,-0.769398455606417));
#73768=CARTESIAN_POINT('Ctrl Pts',(32.6958087967532,-3.12605296241245,-0.783558790866895));
#73769=CARTESIAN_POINT('Ctrl Pts',(32.6962590710462,-3.12425918945861,-0.790680730901383));
#73770=CARTESIAN_POINT('Ctrl Pts',(32.6971253287643,-3.12076758725303,-0.804346274904442));
#73771=CARTESIAN_POINT('Ctrl Pts',(32.697541189421,-3.11907348066985,-0.810890797008091));
#73772=CARTESIAN_POINT('Ctrl Pts',(32.6985214216944,-3.11503828859942,-0.82627944564835));
#73773=CARTESIAN_POINT('Ctrl Pts',(32.6990863457372,-3.11268011898487,-0.835118995023577));
#73774=CARTESIAN_POINT('Ctrl Pts',(32.7007581312009,-3.10560571050519,-0.861190997037086));
#73775=CARTESIAN_POINT('Ctrl Pts',(32.7018684207584,-3.10078383407627,-0.878394191755366));
#73776=CARTESIAN_POINT('Ctrl Pts',(32.7168056648685,-3.03427294972694,-1.1083135332806));
#73777=CARTESIAN_POINT('Ctrl Pts',(32.7313699228012,-2.95097145910775,-1.31411696454995));
#73778=CARTESIAN_POINT('Ctrl Pts',(32.7534126488163,-2.79770703594818,-1.60316549806046));
#73779=CARTESIAN_POINT('Ctrl Pts',(32.7605947883641,-2.74358964678818,-1.69411327258968));
#73780=CARTESIAN_POINT('Ctrl Pts',(32.7770267228811,-2.60890753017515,-1.89702426789483));
#73781=CARTESIAN_POINT('Ctrl Pts',(32.7862301965882,-2.52542421113345,-2.00682342387298));
#73782=CARTESIAN_POINT('Ctrl Pts',(32.7966196283592,-2.41896787912752,-2.12962979218792));
#73783=CARTESIAN_POINT('Ctrl Pts',(32.7981866898664,-2.40256077640483,-2.14812254219514));
#73784=CARTESIAN_POINT('Ctrl Pts',(32.8001978843017,-2.38102404029111,-2.17184152341822));
#73785=CARTESIAN_POINT('Ctrl Pts',(32.8006558081043,-2.37608766996993,-2.17724102257574));
#73786=CARTESIAN_POINT('Ctrl Pts',(32.8013901879191,-2.36811759528246,-2.18589945786128));
#73787=CARTESIAN_POINT('Ctrl Pts',(32.8016675124697,-2.36509548464485,-2.18916895968573));
#73788=CARTESIAN_POINT('Ctrl Pts',(32.8021967564606,-2.35930422671847,-2.19540830280771));
#73789=CARTESIAN_POINT('Ctrl Pts',(32.8024487590276,-2.35653625001467,-2.19837916492099));
#73790=CARTESIAN_POINT('Ctrl Pts',(32.8030297920326,-2.35013026558368,-2.20522869019298));
#73791=CARTESIAN_POINT('Ctrl Pts',(32.803358513664,-2.34648824400342,-2.20910361073875));
#73792=CARTESIAN_POINT('Ctrl Pts',(32.8044116432076,-2.33476370463092,-2.22151619923804));
#73793=CARTESIAN_POINT('Ctrl Pts',(32.8051332330779,-2.32664394032802,-2.23001878126695));
#73794=CARTESIAN_POINT('Ctrl Pts',(32.8174551558295,-2.18654799573593,-2.37512160650147));
#73795=CARTESIAN_POINT('Ctrl Pts',(32.8281727860812,-2.04277405890123,-2.49985834596524));
#73796=CARTESIAN_POINT('Ctrl Pts',(32.8458443071347,-1.78703973249849,-2.68484421110534));
#73797=CARTESIAN_POINT('Ctrl Pts',(32.8528257549029,-1.6810345315686,-2.75245739061293));
#73798=CARTESIAN_POINT('Ctrl Pts',(32.866414386939,-1.47130746000319,-2.86958244327393));
#73799=CARTESIAN_POINT('Ctrl Pts',(32.8729903885499,-1.36835839841498,-2.92007549617023));
#73800=CARTESIAN_POINT('Ctrl Pts',(32.8821132914348,-1.22599878212761,-2.98071421989086));
#73801=CARTESIAN_POINT('Ctrl Pts',(32.88450168693,-1.1887626386916,-2.99575924523463));
#73802=CARTESIAN_POINT('Ctrl Pts',(32.8885910343187,-1.1251547325655,-3.02008697511983));
#73803=CARTESIAN_POINT('Ctrl Pts',(32.8902799870072,-1.0989251319401,-3.02972968905458));
#73804=CARTESIAN_POINT('Ctrl Pts',(32.8924857299937,-1.06474134905322,-3.04179427568128));
#73805=CARTESIAN_POINT('Ctrl Pts',(32.8929921391112,-1.05689803484748,-3.04452838677206));
#73806=CARTESIAN_POINT('Ctrl Pts',(32.8939907721223,-1.04144121961344,-3.04984957110577));
#73807=CARTESIAN_POINT('Ctrl Pts',(32.8944829292796,-1.03382842934866,-3.05243853289476));
#73808=CARTESIAN_POINT('Ctrl Pts',(32.8954185069251,-1.0193663305556,-3.05729650305064));
#73809=CARTESIAN_POINT('Ctrl Pts',(32.8958617405345,-1.01251892547061,-3.05957105615339));
#73810=CARTESIAN_POINT('Ctrl Pts',(32.8968696750525,-0.996957235469488,
-3.06468233570964));
#73811=CARTESIAN_POINT('Ctrl Pts',(32.8974348390197,-0.988238401577048,
-3.0675049155683));
#73812=CARTESIAN_POINT('Ctrl Pts',(32.8991502205219,-0.961796756548136,
-3.07594053348342));
#73813=CARTESIAN_POINT('Ctrl Pts',(32.9003042466146,-0.944037542640087,
-3.08143736933901));
#73814=CARTESIAN_POINT('Ctrl Pts',(32.9091296214775,-0.808466047018551,
-3.12211751476472));
#73815=CARTESIAN_POINT('Ctrl Pts',(32.9170162020647,-0.688788843543406,
-3.15068223854805));
#73816=CARTESIAN_POINT('Ctrl Pts',(32.9314599585764,-0.472247384519792,
-3.18943877585619));
#73817=CARTESIAN_POINT('Ctrl Pts',(32.9379387836329,-0.375992536273159,
-3.20221247288937));
#73818=CARTESIAN_POINT('Ctrl Pts',(32.9608420599428,-0.0371575738424513,
-3.23168999983551));
#73819=CARTESIAN_POINT('Ctrl Pts',(32.977550850477,0.206613648715612,-3.22529444914199));
#73820=CARTESIAN_POINT('Ctrl Pts',(32.9948892937291,0.474515380555603,-3.18774290089363));
#73821=CARTESIAN_POINT('Ctrl Pts',(32.996631151341,0.501625462550799,-3.18358943069423));
#73822=CARTESIAN_POINT('Ctrl Pts',(32.9988505644776,0.536467328899358,-3.17779525501121));
#73823=CARTESIAN_POINT('Ctrl Pts',(32.9993450589931,0.544249699825903,-3.17647165028942));
#73824=CARTESIAN_POINT('Ctrl Pts',(33.000126233559,0.556576124547202,-3.1743285743681));
#73825=CARTESIAN_POINT('Ctrl Pts',(33.0004139666241,0.561123353245616,-3.17352792071334));
#73826=CARTESIAN_POINT('Ctrl Pts',(33.0009514570549,0.569631081768674,-3.17201106417824));
#73827=CARTESIAN_POINT('Ctrl Pts',(33.0012013422472,0.573591917240838,-3.17129722247786));
#73828=CARTESIAN_POINT('Ctrl Pts',(33.0017679268232,0.58258498537413,-3.16965904700639));
#73829=CARTESIAN_POINT('Ctrl Pts',(33.0020843621892,0.587616347875645,-3.16873015071057));
#73830=CARTESIAN_POINT('Ctrl Pts',(33.0030220665662,0.602551149917696,-3.16593607486007));
#73831=CARTESIAN_POINT('Ctrl Pts',(33.0036413972635,0.612448188572382,-3.16403640007377));
#73832=CARTESIAN_POINT('Ctrl Pts',(33.0080316727549,0.682824626315074,-3.1501854950853));
#73833=CARTESIAN_POINT('Ctrl Pts',(33.0117112728667,0.742963630229042,-3.13654656267067));
#73834=CARTESIAN_POINT('Ctrl Pts',(33.0191069477058,0.865140373449977,-3.10512627443492));
#73835=CARTESIAN_POINT('Ctrl Pts',(33.0228152423561,0.927109021745268,-3.08719075515475));
#73836=CARTESIAN_POINT('Ctrl Pts',(33.0407195724168,1.22681237450783,-2.99060853692969));
#73837=CARTESIAN_POINT('Ctrl Pts',(33.0543494304512,1.45535940758955,-2.88630259273302));
#73838=CARTESIAN_POINT('Ctrl Pts',(33.0730876525826,1.73351806602429,-2.71783527292491));
#73839=CARTESIAN_POINT('Ctrl Pts',(33.0774568399969,1.79613087213766,-2.67686872444748));
#73840=CARTESIAN_POINT('Ctrl Pts',(33.0836758988301,1.88161796906975,-2.61658552704864));
#73841=CARTESIAN_POINT('Ctrl Pts',(33.085459931725,1.90573711377358,-2.59907136632971));
#73842=CARTESIAN_POINT('Ctrl Pts',(33.0885870899223,1.94728587053142,-2.5680113665687));
#73843=CARTESIAN_POINT('Ctrl Pts',(33.0899243877882,1.96482590761348,-2.55461616604637));
#73844=CARTESIAN_POINT('Ctrl Pts',(33.0918730166724,1.99004740172076,-2.53494127857654));
#73845=CARTESIAN_POINT('Ctrl Pts',(33.0924786743277,1.99783987514487,-2.52880441646763));
#73846=CARTESIAN_POINT('Ctrl Pts',(33.093534101271,2.01133742319527,-2.5180732686481));
#73847=CARTESIAN_POINT('Ctrl Pts',(33.0939832142364,2.01705542463182,-2.51349530112615));
#73848=CARTESIAN_POINT('Ctrl Pts',(33.0948499540363,2.02804105958321,-2.50463831338046));
#73849=CARTESIAN_POINT('Ctrl Pts',(33.0952674674882,2.03331088636543,-2.5003620654761));
#73850=CARTESIAN_POINT('Ctrl Pts',(33.0962557923294,2.04573322928038,-2.49021660168074));
#73851=CARTESIAN_POINT('Ctrl Pts',(33.096827178751,2.05287402600598,-2.48433319004402));
#73852=CARTESIAN_POINT('Ctrl Pts',(33.0988274660231,2.07772835918137,-2.46367499712194));
#73853=CARTESIAN_POINT('Ctrl Pts',(33.100262865557,2.0953081989451,-2.44874113225818));
#73854=CARTESIAN_POINT('Ctrl Pts',(33.1026028708073,2.12354950326985,-2.42422369314495));
#73855=CARTESIAN_POINT('Ctrl Pts',(33.1035026695099,2.13431020096048,-2.4147552593629));
#73856=CARTESIAN_POINT('Ctrl Pts',(33.1206723618894,2.33775714586359,-2.2333182224323));
#73857=CARTESIAN_POINT('Ctrl Pts',(33.1379568320403,2.50910827342829,-2.03890729429591));
#73858=CARTESIAN_POINT('Ctrl Pts',(33.1680927302765,2.76139522866264,-1.67206561218137));
#73859=CARTESIAN_POINT('Ctrl Pts',(33.180763473198,2.85378188818997,-1.50898969179775));
#73860=CARTESIAN_POINT('Ctrl Pts',(33.1943201670744,2.94187816157787,-1.31609043810097));
#73861=CARTESIAN_POINT('Ctrl Pts',(33.1959031082151,2.9519880934302,-1.29325463324993));
#73862=CARTESIAN_POINT('Ctrl Pts',(33.197923379484,2.96467535282437,-1.26367308000243));
#73863=CARTESIAN_POINT('Ctrl Pts',(33.1983748617183,2.96749654443497,-1.25703375528059));
#73864=CARTESIAN_POINT('Ctrl Pts',(33.1991013913038,2.97201401083069,-1.24630249206975));
#73865=CARTESIAN_POINT('Ctrl Pts',(33.1993772746335,2.97372416430878,-1.24221647770628));
#73866=CARTESIAN_POINT('Ctrl Pts',(33.1999055373488,2.97698879100295,-1.23437103419365));
#73867=CARTESIAN_POINT('Ctrl Pts',(33.2001579930885,2.97854456632494,-1.23061219657944));
#73868=CARTESIAN_POINT('Ctrl Pts',(33.2007424553745,2.98213606198424,-1.22188823815869));
#73869=CARTESIAN_POINT('Ctrl Pts',(33.2010741413267,2.98416651555158,-1.2169209371141));
#73870=CARTESIAN_POINT('Ctrl Pts',(33.2021464407145,2.99070513343733,-1.20081008825158));
#73871=CARTESIAN_POINT('Ctrl Pts',(33.2028840899951,2.99516342474455,-1.18964622173422));
#73872=CARTESIAN_POINT('Ctrl Pts',(33.2133726722157,3.05796367663419,-1.0297990653307));
#73873=CARTESIAN_POINT('Ctrl Pts',(33.2225014479099,3.10524489560186,-0.876981685410832));
#73874=CARTESIAN_POINT('Ctrl Pts',(33.2428961464341,3.18636220784537,-0.523729532728325));
#73875=CARTESIAN_POINT('Ctrl Pts',(33.2540525353336,3.21298617662333,-0.322358940721574));
#73876=CARTESIAN_POINT('Ctrl Pts',(33.2704018987214,3.22357849386231,-0.0376640062154653));
#73877=CARTESIAN_POINT('Ctrl Pts',(33.2751871762806,3.22349009030975,0.0445758759698111));
#73878=CARTESIAN_POINT('Ctrl Pts',(33.2829377205287,3.21835522125058,0.175067017576471));
#73879=CARTESIAN_POINT('Ctrl Pts',(33.2858405490179,3.21536414677462,0.223364759904355));
#73880=CARTESIAN_POINT('Ctrl Pts',(33.2895833981433,3.21016848981178,0.284801733147738));
#73881=CARTESIAN_POINT('Ctrl Pts',(33.2903917233395,3.20896822566466,0.298021272088014));
#73882=CARTESIAN_POINT('Ctrl Pts',(33.29169315569,3.20691088673237,0.319225003160697));
#73883=CARTESIAN_POINT('Ctrl Pts',(33.292184628672,3.20610557096026,0.32721415632135));
#73884=CARTESIAN_POINT('Ctrl Pts',(33.2931196637426,3.20451970993939,0.342378568573353));
#73885=CARTESIAN_POINT('Ctrl Pts',(33.2935630420846,3.20374489993098,0.3495543883647));
#73886=CARTESIAN_POINT('Ctrl Pts',(33.2945723505152,3.20192939663249,0.365855231564391));
#73887=CARTESIAN_POINT('Ctrl Pts',(33.2951387484922,3.20087379209316,0.37497850041957));
#73888=CARTESIAN_POINT('Ctrl Pts',(33.2968615278343,3.19755173555575,0.402653399892398));
#73889=CARTESIAN_POINT('Ctrl Pts',(33.2980217662429,3.19516291953437,0.421189691110196));
#73890=CARTESIAN_POINT('Ctrl Pts',(33.3070499158732,3.17540885225935,0.564620533241722));
#73891=CARTESIAN_POINT('Ctrl Pts',(33.315144556927,3.15089044560091,0.688404056098711));
#73892=CARTESIAN_POINT('Ctrl Pts',(33.3239498031942,3.11720526846814,0.818053212493782));
#73893=CARTESIAN_POINT('Ctrl Pts',(33.3244688436758,3.11519430753084,0.82567800572603));
#73894=CARTESIAN_POINT('Ctrl Pts',(33.3251944440819,3.11234768496992,0.836312865180888));
#73895=CARTESIAN_POINT('Ctrl Pts',(33.3254004337965,3.11153559058599,0.839329249481283));
#73896=CARTESIAN_POINT('Ctrl Pts',(33.325817361759,3.10988385910074,0.845428978342795));
#73897=CARTESIAN_POINT('Ctrl Pts',(33.3260283046359,3.10904401899641,0.848512264099187));
#73898=CARTESIAN_POINT('Ctrl Pts',(33.3427134654385,3.04228588910754,1.09217006680701));
#73899=CARTESIAN_POINT('Ctrl Pts',(33.3598799716314,2.94867366654491,1.32425269373299));
#73900=CARTESIAN_POINT('Ctrl Pts',(33.3808531683655,2.79761035461309,1.60120531676256));
#73901=CARTESIAN_POINT('Ctrl Pts',(33.3851937538263,2.76419705173627,1.65822133550961));
#73902=CARTESIAN_POINT('Ctrl Pts',(33.3916646254845,2.71074173108212,1.743324962901));
#73903=CARTESIAN_POINT('Ctrl Pts',(33.3938573166705,2.69196420165102,1.77218272966235));
#73904=CARTESIAN_POINT('Ctrl Pts',(33.3965267526353,2.66822976206699,1.80741037928458));
#73905=CARTESIAN_POINT('Ctrl Pts',(33.3970309607682,2.66370750508744,1.81406854141633));
#73906=CARTESIAN_POINT('Ctrl Pts',(33.3978216837897,2.65655272630586,1.82451814953452));
#73907=CARTESIAN_POINT('Ctrl Pts',(33.3981093154309,2.65393695970833,1.82832094561003));
#73908=CARTESIAN_POINT('Ctrl Pts',(33.39864671759,2.6490248736206,1.8354293724626));
#73909=CARTESIAN_POINT('Ctrl Pts',(33.3988966154917,2.64673055639167,1.83873628464068));
#73910=CARTESIAN_POINT('Ctrl Pts',(33.3994633600774,2.64150427428559,1.84623913210516));
#73911=CARTESIAN_POINT('Ctrl Pts',(33.3997799421479,2.63856851149864,1.85043237514224));
#73912=CARTESIAN_POINT('Ctrl Pts',(33.4007394962038,2.62962096770244,1.86314784636808));
#73913=CARTESIAN_POINT('Ctrl Pts',(33.4013803450961,2.62357772554077,1.87164800543243));
#73914=CARTESIAN_POINT('Ctrl Pts',(33.4061089720623,2.57849537198935,1.93441146181875));
#73915=CARTESIAN_POINT('Ctrl Pts',(33.4100892074513,2.53781446909569,1.98748214447525));
#73916=CARTESIAN_POINT('Ctrl Pts',(33.4320365420117,2.30015895988496,2.27830991968861));
#73917=CARTESIAN_POINT('Ctrl Pts',(33.4485434396639,2.07146289119973,2.4880731197027));
#73918=CARTESIAN_POINT('Ctrl Pts',(33.4669551839278,1.8074385196177,2.66822058804784));
#73919=CARTESIAN_POINT('Ctrl Pts',(33.4675809300173,1.79845237115226,2.67428572812347));
#73920=CARTESIAN_POINT('Ctrl Pts',(33.4682079605267,1.78943620863048,2.68030513519304));
#73921=CARTESIAN_POINT('Origin',(-1.72497344927317,0.,0.));
#73922=CARTESIAN_POINT('',(34.9669226703048,1.78943621037804,2.68030513402632));
#73923=CARTESIAN_POINT('',(34.7184445309107,1.78943583648355,2.68030538364725));
#73924=CARTESIAN_POINT('',(-1.72497344927317,1.78943621037804,2.68030513402633));
#73925=CARTESIAN_POINT('',(34.1465734492326,-3.22274894896891,-0.00260277156147679));
#73926=CARTESIAN_POINT('Ctrl Pts',(34.1465734492731,-3.22274894896838,-0.00260277221528181));
#73927=CARTESIAN_POINT('Ctrl Pts',(34.1565886751657,-3.22261829689253,-0.164375991421163));
#73928=CARTESIAN_POINT('Ctrl Pts',(34.1666039010584,-3.21030412491819,-0.325671211582515));
#73929=CARTESIAN_POINT('Ctrl Pts',(34.1766191269511,-3.18603596446093,-0.485069475087369));
#73930=CARTESIAN_POINT('Ctrl Pts',(34.1772832098965,-3.18442680739871,-0.495638749255301));
#73931=CARTESIAN_POINT('Ctrl Pts',(34.1779472928418,-3.18276510569429,-0.506199695768205));
#73932=CARTESIAN_POINT('Ctrl Pts',(34.1786113757872,-3.18105093180358,-0.516751905435821));
#73933=CARTESIAN_POINT('Ctrl Pts',(34.18478362388,-3.16511872544068,-0.614828292505281));
#73934=CARTESIAN_POINT('Ctrl Pts',(34.1909558719727,-3.1446184722633,-0.712339794952678));
#73935=CARTESIAN_POINT('Ctrl Pts',(34.1971281200655,-3.11960177926634,-0.808827732770278));
#73936=CARTESIAN_POINT('Ctrl Pts',(34.2032920087181,-3.09461896785424,-0.905184991274903));
#73937=CARTESIAN_POINT('Ctrl Pts',(34.2094558973707,-3.06513198265442,-1.0005210237516));
#73938=CARTESIAN_POINT('Ctrl Pts',(34.2156197860234,-3.03124385526426,-1.09438487399209));
#73939=CARTESIAN_POINT('Ctrl Pts',(34.2217771476819,-2.99739161230016,-1.18814933100392));
#73940=CARTESIAN_POINT('Ctrl Pts',(34.2279345093405,-2.95914763916692,-1.280444298722));
#73941=CARTESIAN_POINT('Ctrl Pts',(34.234091870999,-2.91666517864518,-1.37083252010545));
#73942=CARTESIAN_POINT('Ctrl Pts',(34.2402447351453,-2.87421374852202,-1.4611547193588));
#73943=CARTESIAN_POINT('Ctrl Pts',(34.2463975992916,-2.827530170422,-1.54957254935167));
#73944=CARTESIAN_POINT('Ctrl Pts',(34.2525504634379,-2.77681600129492,-1.63566819907109));
#73945=CARTESIAN_POINT('Ctrl Pts',(34.2587009965745,-2.72612104520764,-1.72173123149298));
#73946=CARTESIAN_POINT('Ctrl Pts',(34.264851529711,-2.67139875242658,-1.8054734578587));
#73947=CARTESIAN_POINT('Ctrl Pts',(34.2710020628476,-2.61289645317398,-1.88650197123959));
#73948=CARTESIAN_POINT('Ctrl Pts',(34.2771519110628,-2.55440066871804,-1.96752146131206));
#73949=CARTESIAN_POINT('Ctrl Pts',(34.283301759278,-2.49212596895196,-2.04582748703674));
#73950=CARTESIAN_POINT('Ctrl Pts',(34.2894516074932,-2.42636222488437,-2.12105726376121));
#73951=CARTESIAN_POINT('Ctrl Pts',(34.2956024158723,-2.36058821325039,-2.19629878596546));
#73952=CARTESIAN_POINT('Ctrl Pts',(34.3017532242514,-2.29132436123661,-2.26846277812617));
#73953=CARTESIAN_POINT('Ctrl Pts',(34.3079040326306,-2.21889924105963,-2.33722136746287));
#73954=CARTESIAN_POINT('Ctrl Pts',(34.3140614189968,-2.14639666577862,-2.40605349072919));
#73955=CARTESIAN_POINT('Ctrl Pts',(34.320218805363,-2.07072638681877,-2.47147263899648));
#73956=CARTESIAN_POINT('Ctrl Pts',(34.3263761917292,-1.99225200131635,-2.53318959530293));
#73957=CARTESIAN_POINT('Ctrl Pts',(34.3325370144661,-1.91373382010764,-2.59494099517557));
#73958=CARTESIAN_POINT('Ctrl Pts',(34.3386978372031,-1.83240876936569,-2.65298583601607));
#73959=CARTESIAN_POINT('Ctrl Pts',(34.34485865994,-1.74866979764436,-2.70707803753539));
#73960=CARTESIAN_POINT('Ctrl Pts',(34.3510297828567,-1.66479082409277,-2.76126067493014));
#73961=CARTESIAN_POINT('Ctrl Pts',(34.3572009057734,-1.57849024380117,-2.81147725445752));
#73962=CARTESIAN_POINT('Ctrl Pts',(34.3633720286901,-1.49018609934024,-2.85752741926182));
#73963=CARTESIAN_POINT('Ctrl Pts',(34.3680675506356,-1.4229966990001,-2.89256635177913));
#73964=CARTESIAN_POINT('Ctrl Pts',(34.3727630725812,-1.35464785899063,-2.9251940960375));
#73965=CARTESIAN_POINT('Ctrl Pts',(34.3774585945267,-1.28533050100755,-2.9553414465472));
#73966=CARTESIAN_POINT('Ctrl Pts',(34.3836308426195,-1.19421306282511,-2.99497003924548));
#73967=CARTESIAN_POINT('Ctrl Pts',(34.3898030907122,-1.10110082093646,-3.03045051134412));
#73968=CARTESIAN_POINT('Ctrl Pts',(34.395975338805,-1.00640752548339,-3.06157826213056));
#73969=CARTESIAN_POINT('Ctrl Pts',(34.4021392274576,-0.911842478753034,
-3.09266385476568));
#73970=CARTESIAN_POINT('Ctrl Pts',(34.4083031161103,-0.815701043574529,
-3.11940830888991));
#73971=CARTESIAN_POINT('Ctrl Pts',(34.4144670047629,-0.718418278569851,
-3.14165445896215));
#73972=CARTESIAN_POINT('Ctrl Pts',(34.4206243664214,-0.621238527111895,
-3.16387705239699));
#73973=CARTESIAN_POINT('Ctrl Pts',(34.42678172808,-0.522920269676796,-3.18161071535755));
#73974=CARTESIAN_POINT('Ctrl Pts',(34.4329390897385,-0.423914190725676,
-3.19474792767777));
#73975=CARTESIAN_POINT('Ctrl Pts',(34.4390919538848,-0.324980428633079,
-3.20787554420413));
#73976=CARTESIAN_POINT('Ctrl Pts',(34.4452448180311,-0.225360273193283,
-3.21641332816805));
#73977=CARTESIAN_POINT('Ctrl Pts',(34.4513976821774,-0.125514174661367,
-3.22030491637967));
#73978=CARTESIAN_POINT('Ctrl Pts',(34.457548215314,-0.0257059027782921,
-3.22419503026487));
#73979=CARTESIAN_POINT('Ctrl Pts',(34.4636987484505,0.0743277085494085,
-3.22344242902527));
#73980=CARTESIAN_POINT('Ctrl Pts',(34.469849281587,0.174122408527278,-3.21804272024917));
#73981=CARTESIAN_POINT('Ctrl Pts',(34.4759991298022,0.273905995400481,-3.21264361278284));
#73982=CARTESIAN_POINT('Ctrl Pts',(34.4821489780174,0.373450290077414,-3.2025984501153));
#73983=CARTESIAN_POINT('Ctrl Pts',(34.4882988262326,0.472293378652133,-3.18795491294676));
#73984=CARTESIAN_POINT('Ctrl Pts',(34.4944496346118,0.571151899407579,-3.17330908951101));
#73985=CARTESIAN_POINT('Ctrl Pts',(34.5006004429909,0.669308566883421,-3.15406352923284));
#73986=CARTESIAN_POINT('Ctrl Pts',(34.5067512513701,0.766309909212199,-3.13031734582026));
#73987=CARTESIAN_POINT('Ctrl Pts',(34.5129086377362,0.863414989705747,-3.10654576703244));
#73988=CARTESIAN_POINT('Ctrl Pts',(34.5190660241024,0.9593618550203,-3.0782640571445));
#73989=CARTESIAN_POINT('Ctrl Pts',(34.5252234104686,1.05371061257495,-3.04562169473606));
#73990=CARTESIAN_POINT('Ctrl Pts',(34.5313842332056,1.1481120251513,-3.01296111497801));
#73991=CARTESIAN_POINT('Ctrl Pts',(34.5375450559425,1.2409131503258,-2.97593519712689));
#73992=CARTESIAN_POINT('Ctrl Pts',(34.5437058786795,1.33169451185914,-2.93474143487706));
#73993=CARTESIAN_POINT('Ctrl Pts',(34.5498770015962,1.42262764928017,-2.89347880144346));
#73994=CARTESIAN_POINT('Ctrl Pts',(34.5560481245129,1.51153389102886,-2.84803460273548));
#73995=CARTESIAN_POINT('Ctrl Pts',(34.5622192474295,1.59801865523376,-2.79865216488668));
#73996=CARTESIAN_POINT('Ctrl Pts',(34.5669147693752,1.66382371434022,-2.7610777519674));
#73997=CARTESIAN_POINT('Ctrl Pts',(34.5716102913208,1.7282273812905,-2.72122425388253));
#73998=CARTESIAN_POINT('Ctrl Pts',(34.5763058132664,1.79106820649395,-2.67921485554752));
#73999=CARTESIAN_POINT('Ctrl Pts',(34.5824780613592,1.8736722637217,-2.62399364015239));
#74000=CARTESIAN_POINT('Ctrl Pts',(34.5886503094519,1.95386549571327,-2.56485144681597));
#74001=CARTESIAN_POINT('Ctrl Pts',(34.5948225575447,2.03125207158727,-2.50202569614551));
#74002=CARTESIAN_POINT('Ctrl Pts',(34.6009864461973,2.10853383825101,-2.43928503409976));
#74003=CARTESIAN_POINT('Ctrl Pts',(34.60715033485,2.18301616987677,-2.37287100199665));
#74004=CARTESIAN_POINT('Ctrl Pts',(34.6133142235026,2.2543316167588,-2.30306459400982));
#74005=CARTESIAN_POINT('Ctrl Pts',(34.6194715851611,2.32557154710797,-2.23333210462176));
#74006=CARTESIAN_POINT('Ctrl Pts',(34.6256289468197,2.39365095096647,-2.16021468318641));
#74007=CARTESIAN_POINT('Ctrl Pts',(34.6317863084782,2.45823569170938,-2.08403331223523));
#74008=CARTESIAN_POINT('Ctrl Pts',(34.6379391726245,2.5227732579191,-2.00790758632606));
#74009=CARTESIAN_POINT('Ctrl Pts',(34.6440920367709,2.58382095597386,-1.92872269075188));
#74010=CARTESIAN_POINT('Ctrl Pts',(34.6502449009172,2.64108240248834,-1.84683548421791));
#74011=CARTESIAN_POINT('Ctrl Pts',(34.6563954340537,2.69832215552999,-1.76497930061469));
#74012=CARTESIAN_POINT('Ctrl Pts',(34.6625459671902,2.75177825856786,-1.68042319585627));
#74013=CARTESIAN_POINT('Ctrl Pts',(34.6686965003268,2.80119599150795,-1.59355532682734));
#74014=CARTESIAN_POINT('Ctrl Pts',(34.674846348542,2.85060822130569,-1.50669713137549));
#74015=CARTESIAN_POINT('Ctrl Pts',(34.6809961967572,2.8959827603119,-1.41752806103303));
#74016=CARTESIAN_POINT('Ctrl Pts',(34.6871460449724,2.93710995637808,-1.32646246333802));
#74017=CARTESIAN_POINT('Ctrl Pts',(34.6932968533515,2.97824357355398,-1.23538264774704));
#74018=CARTESIAN_POINT('Ctrl Pts',(34.6994476617307,3.01512835184066,-1.14240611258294));
#74019=CARTESIAN_POINT('Ctrl Pts',(34.7055984701098,3.04760246969089,-1.04796791421971));
#74020=CARTESIAN_POINT('Ctrl Pts',(34.711755856476,3.08011131701301,-0.953428718847997));
#74021=CARTESIAN_POINT('Ctrl Pts',(34.7179132428422,3.1081999430433,-0.857425150343363));
#74022=CARTESIAN_POINT('Ctrl Pts',(34.7240706292084,3.13175623607276,-0.760408074864664));
#74023=CARTESIAN_POINT('Ctrl Pts',(34.7302314519454,3.15532567561472,-0.663336855204869));
#74024=CARTESIAN_POINT('Ctrl Pts',(34.7363922746823,3.17435766205571,-0.565251428568188));
#74025=CARTESIAN_POINT('Ctrl Pts',(34.7425530974193,3.18879151375422,-0.466611448969114));
#74026=CARTESIAN_POINT('Ctrl Pts',(34.748724220336,3.20324949717556,-0.367806554786105));
#74027=CARTESIAN_POINT('Ctrl Pts',(34.7548953432527,3.21309394736921,-0.268445688150943));
#74028=CARTESIAN_POINT('Ctrl Pts',(34.7610664661694,3.21831619798967,-0.168992343783121));
#74029=CARTESIAN_POINT('Ctrl Pts',(34.7657619881149,3.2222897361487,-0.0933196716711029));
#74030=CARTESIAN_POINT('Ctrl Pts',(34.7704575100605,3.22358834046245,-0.0175935384480273));
#74031=CARTESIAN_POINT('Ctrl Pts',(34.775153032006,3.22222833773311,0.057983635706201));
#74032=CARTESIAN_POINT('Ctrl Pts',(34.7813254289543,3.22044057552189,0.157331977492349));
#74033=CARTESIAN_POINT('Ctrl Pts',(34.7874978259026,3.2140506716445,0.256772428979356));
#74034=CARTESIAN_POINT('Ctrl Pts',(34.7936702228509,3.20304431621291,0.355843604517699));
#74035=CARTESIAN_POINT('Ctrl Pts',(34.7998342219306,3.19205293550307,0.454779988544348));
#74036=CARTESIAN_POINT('Ctrl Pts',(34.8059982210103,3.17645763513739,0.553347667295676));
#74037=CARTESIAN_POINT('Ctrl Pts',(34.81216222009,3.15629610985148,0.651085577659667));
#74038=CARTESIAN_POINT('Ctrl Pts',(34.8186105721823,3.13520450810396,0.75333226047749));
#74039=CARTESIAN_POINT('Ctrl Pts',(34.8250589242746,3.10911525674017,0.854670299241264));
#74040=CARTESIAN_POINT('Ctrl Pts',(34.8315072763669,3.07813236972921,0.954577747973023));
#74041=CARTESIAN_POINT('Ctrl Pts',(34.8376598941505,3.04857041981027,1.04990324152348));
#74042=CARTESIAN_POINT('Ctrl Pts',(34.8438125119341,3.01455391332712,1.14392599391152));
#74043=CARTESIAN_POINT('Ctrl Pts',(34.8499651297178,2.97622513545598,1.23620447563502));
#74044=CARTESIAN_POINT('Ctrl Pts',(34.8561154399878,2.93791073263305,1.32844834869898));
#74045=CARTESIAN_POINT('Ctrl Pts',(34.8622657502578,2.89528743899897,1.41894885049804));
#74046=CARTESIAN_POINT('Ctrl Pts',(34.8684160605278,2.84854628670866,1.50728285831768));
#74047=CARTESIAN_POINT('Ctrl Pts',(34.8745657092847,2.80181016178826,1.59560736513635));
#74048=CARTESIAN_POINT('Ctrl Pts',(34.8807153580415,2.75095726247121,1.68176545766543));
#74049=CARTESIAN_POINT('Ctrl Pts',(34.8868650067984,2.69622487749183,1.76535802954929));
#74050=CARTESIAN_POINT('Ctrl Pts',(34.8930156390435,2.64148373938572,1.84896397005169));
#74051=CARTESIAN_POINT('Ctrl Pts',(34.8991662712886,2.58286212168719,1.9300032119258));
#74052=CARTESIAN_POINT('Ctrl Pts',(34.9053169035337,2.52064041971634,2.00810593271178));
#74053=CARTESIAN_POINT('Ctrl Pts',(34.9114734788998,2.45835859529171,2.08628412117337));
#74054=CARTESIAN_POINT('Ctrl Pts',(34.9176300542659,2.39247001439353,2.16151978498113));
#74055=CARTESIAN_POINT('Ctrl Pts',(34.923786629632,2.32329494304472,2.23347670015222));
#74056=CARTESIAN_POINT('Ctrl Pts',(34.9299466888311,2.25408072746688,2.30547433371958));
#74057=CARTESIAN_POINT('Ctrl Pts',(34.9361067480301,2.18157663311518,2.37418922553548));
#74058=CARTESIAN_POINT('Ctrl Pts',(34.9422668072292,2.10613788409193,2.43932383575711));
#74059=CARTESIAN_POINT('Ctrl Pts',(34.9484355437554,2.0305928687687,2.50455019742104));
#74060=CARTESIAN_POINT('Ctrl Pts',(34.9546042802815,1.95210528873003,2.56618594352339));
#74061=CARTESIAN_POINT('Ctrl Pts',(34.9607730168077,1.87106114828943,2.62397556045437));
#74062=CARTESIAN_POINT('Ctrl Pts',(34.9628229013067,1.84413000501173,2.64317917523849));
#74063=CARTESIAN_POINT('Ctrl Pts',(34.9648727858058,1.81691676947684,2.66195845143838));
#74064=CARTESIAN_POINT('Ctrl Pts',(34.9669226703048,1.78943621037804,2.68030513402632));
#74065=CARTESIAN_POINT('Ctrl Pts',(33.7168658186985,1.789436210378,2.68030513402635));
#74066=CARTESIAN_POINT('Ctrl Pts',(33.7230240742904,1.7063073672797,2.73580395021653));
#74067=CARTESIAN_POINT('Ctrl Pts',(33.7291823298824,1.6206459620611,2.78739728776321));
#74068=CARTESIAN_POINT('Ctrl Pts',(33.7353405854743,1.53286051683291,2.83486440565237));
#74069=CARTESIAN_POINT('Ctrl Pts',(33.741502718378,1.44501980083312,2.88236140940956));
#74070=CARTESIAN_POINT('Ctrl Pts',(33.7476648512817,1.35505277321614,2.92572683291559));
#74071=CARTESIAN_POINT('Ctrl Pts',(33.7538269841854,1.2633891756319,2.96478757306424));
#74072=CARTESIAN_POINT('Ctrl Pts',(33.7599988749213,1.17158042733207,3.00391016649526));
#74073=CARTESIAN_POINT('Ctrl Pts',(33.7661707656571,1.07807015233765,3.03871431759347));
#74074=CARTESIAN_POINT('Ctrl Pts',(33.772342656393,0.983304446662363,3.06907639651965));
#74075=CARTESIAN_POINT('Ctrl Pts',(33.7752007503646,0.939420116285148,3.08313654088349));
#74076=CARTESIAN_POINT('Ctrl Pts',(33.7780588443362,0.895266726279772,3.09624481987067));
#74077=CARTESIAN_POINT('Ctrl Pts',(33.7809169383078,0.850889225077483,3.10839268580195));
#74078=CARTESIAN_POINT('Ctrl Pts',(33.7870891864005,0.75505299650007,3.13462682753091));
#74079=CARTESIAN_POINT('Ctrl Pts',(33.7932614344933,0.657833694385125,3.15647083783526));
#74080=CARTESIAN_POINT('Ctrl Pts',(33.7994336825861,0.559670010758543,3.17378118993064));
#74081=CARTESIAN_POINT('Ctrl Pts',(33.8055975712387,0.461639276006399,3.1910680975938));
#74082=CARTESIAN_POINT('Ctrl Pts',(33.8117614598913,0.362667125967397,3.20383347660308));
#74083=CARTESIAN_POINT('Ctrl Pts',(33.817925348544,0.263206581153961,3.21198378858568));
#74084=CARTESIAN_POINT('Ctrl Pts',(33.8240827102025,0.163851355956706,3.22012547013367));
#74085=CARTESIAN_POINT('Ctrl Pts',(33.8302400718611,0.0640091946955882,
3.22366176506024));
#74086=CARTESIAN_POINT('Ctrl Pts',(33.8363974335196,-0.0358584933163507,
3.22255050091648));
#74087=CARTESIAN_POINT('Ctrl Pts',(33.8425502976659,-0.135653235125919,
3.2214400484717));
#74088=CARTESIAN_POINT('Ctrl Pts',(33.8487031618122,-0.235473033576979,
3.21568879103823));
#74089=CARTESIAN_POINT('Ctrl Pts',(33.8548560259586,-0.334854106241301,
3.2053065828456));
#74090=CARTESIAN_POINT('Ctrl Pts',(33.8610065590951,-0.434197528431681,
3.1949283079478));
#74091=CARTESIAN_POINT('Ctrl Pts',(33.8671570922316,-0.533102123551234,
3.17992261342375));
#74092=CARTESIAN_POINT('Ctrl Pts',(33.8733076253682,-0.631107756398591,
3.16035133526536));
#74093=CARTESIAN_POINT('Ctrl Pts',(33.8794574735834,-0.729102475371115,
3.14078223655803));
#74094=CARTESIAN_POINT('Ctrl Pts',(33.8856073217986,-0.826198005135701,
3.1166486500967));
#74095=CARTESIAN_POINT('Ctrl Pts',(33.8917571700138,-0.921943947047824,
3.08806361997318));
#74096=CARTESIAN_POINT('Ctrl Pts',(33.8979079783929,-1.01770483758911,3.05947412692407));
#74097=CARTESIAN_POINT('Ctrl Pts',(33.9040587867721,-1.11211530549546,3.02643193404758));
#74098=CARTESIAN_POINT('Ctrl Pts',(33.9102095951512,-1.20474064021909,2.98909978961969));
#74099=CARTESIAN_POINT('Ctrl Pts',(33.9163669815174,-1.29746503318267,2.95172772029943));
#74100=CARTESIAN_POINT('Ctrl Pts',(33.9225243678836,-1.38840007699535,2.91005670057734));
#74101=CARTESIAN_POINT('Ctrl Pts',(33.9286817542498,-1.47713168170983,2.86429739332163));
#74102=CARTESIAN_POINT('Ctrl Pts',(33.9348425769867,-1.56591280657373,2.8185125482912));
#74103=CARTESIAN_POINT('Ctrl Pts',(33.9410033997237,-1.65248766698527,2.76863508874169));
#74104=CARTESIAN_POINT('Ctrl Pts',(33.9471642224607,-1.73646922583916,2.71492029168695));
#74105=CARTESIAN_POINT('Ctrl Pts',(33.9533353453774,-1.8205911921008,2.66111568973319));
#74106=CARTESIAN_POINT('Ctrl Pts',(33.9595064682941,-1.90211084157241,2.60346118628263));
#74107=CARTESIAN_POINT('Ctrl Pts',(33.9656775912107,-1.98067231111727,2.54225387372571));
#74108=CARTESIAN_POINT('Ctrl Pts',(33.9703731131563,-2.04044864506884,2.49568207743832));
#74109=CARTESIAN_POINT('Ctrl Pts',(33.9750686351019,-2.09851299431253,2.44705425646063));
#74110=CARTESIAN_POINT('Ctrl Pts',(33.9797641570475,-2.15472311950254,2.39651535375454));
#74111=CARTESIAN_POINT('Ctrl Pts',(33.9858444085629,-2.22750985180378,2.33107231178245));
#74112=CARTESIAN_POINT('Ctrl Pts',(33.9919246600783,-2.29745886960337,2.26217825259532));
#74113=CARTESIAN_POINT('Ctrl Pts',(33.9980049115937,-2.36421738820502,2.19011271486402));
#74114=CARTESIAN_POINT('Ctrl Pts',(34.0041952673286,-2.43218480327599,2.11674217852059));
#74115=CARTESIAN_POINT('Ctrl Pts',(34.0103856230635,-2.49684463175334,2.04008441524718));
#74116=CARTESIAN_POINT('Ctrl Pts',(34.0165759787985,-2.55785923176369,1.96047792973583));
#74117=CARTESIAN_POINT('Ctrl Pts',(34.022640822498,-2.617636735399,1.88248549880549));
#74118=CARTESIAN_POINT('Ctrl Pts',(34.0287056661975,-2.67391512789858,1.80166315333502));
#74119=CARTESIAN_POINT('Ctrl Pts',(34.034770509897,-2.72641465857697,1.71836569798068));
#74120=CARTESIAN_POINT('Ctrl Pts',(34.0408315863062,-2.77888157819644,1.63511998438839));
#74121=CARTESIAN_POINT('Ctrl Pts',(34.0468926627153,-2.82757405851386,1.54940259201758));
#74122=CARTESIAN_POINT('Ctrl Pts',(34.0529537391245,-2.87225467075501,1.46159866886435));
#74123=CARTESIAN_POINT('Ctrl Pts',(34.0590127840448,-2.91692030741171,1.3738241749199));
#74124=CARTESIAN_POINT('Ctrl Pts',(34.0650718289652,-2.95757654445578,1.28396493903239));
#74125=CARTESIAN_POINT('Ctrl Pts',(34.0711308738856,-2.99403166642841,1.1924311061541));
#74126=CARTESIAN_POINT('Ctrl Pts',(34.0774177551645,-3.03185759887512,1.09745535537644));
#74127=CARTESIAN_POINT('Ctrl Pts',(34.0837046364434,-3.06516000806082,1.00067704311448));
#74128=CARTESIAN_POINT('Ctrl Pts',(34.0899915177224,-3.09377983211648,0.902576264306415));
#74129=CARTESIAN_POINT('Ctrl Pts',(34.0960543632788,-3.12137977641379,0.80797134900856));
#74130=CARTESIAN_POINT('Ctrl Pts',(34.1021172088352,-3.14462512716138,0.712137083011762));
#74131=CARTESIAN_POINT('Ctrl Pts',(34.1081800543917,-3.16342477300057,0.61551707374071));
#74132=CARTESIAN_POINT('Ctrl Pts',(34.1142454973404,-3.18223247282267,0.51885567135453));
#74133=CARTESIAN_POINT('Ctrl Pts',(34.1203109402891,-3.19659061145951,0.421408298975774));
#74134=CARTESIAN_POINT('Ctrl Pts',(34.1263763832378,-3.20645977270616,0.323625228493059));
#74135=CARTESIAN_POINT('Ctrl Pts',(34.1324486615409,-3.21634005584711,0.225731962934236));
#74136=CARTESIAN_POINT('Ctrl Pts',(34.1385209398441,-3.22172124882492,0.127502691283429));
#74137=CARTESIAN_POINT('Ctrl Pts',(34.1445932181473,-3.22261599848899,0.0293885825244143));
#74138=CARTESIAN_POINT('Ctrl Pts',(34.1452532951757,-3.22271326078001,0.0187232496582979));
#74139=CARTESIAN_POINT('Ctrl Pts',(34.1459133722042,-3.22275755989923,0.00805927310546678));
#74140=CARTESIAN_POINT('Ctrl Pts',(34.1465734492326,-3.22274894896891,-0.00260277156152148));
#74141=CARTESIAN_POINT('Ctrl Pts',(33.4682079605267,1.78943620863048,2.68030513519304));
#74142=CARTESIAN_POINT('Ctrl Pts',(33.4719380796925,1.73580028482111,2.71611376865332));
#74143=CARTESIAN_POINT('Ctrl Pts',(33.4757140711437,1.68110222134406,2.7503039548369));
#74144=CARTESIAN_POINT('Ctrl Pts',(33.4822462518313,1.58621665213048,2.80572540357671));
#74145=CARTESIAN_POINT('Ctrl Pts',(33.4849724197114,1.54654012316622,2.82778917906105));
#74146=CARTESIAN_POINT('Ctrl Pts',(33.4885168940229,1.49493702531806,2.85507431585235));
#74147=CARTESIAN_POINT('Ctrl Pts',(33.4893075168186,1.48342536161371,2.86107239466536));
#74148=CARTESIAN_POINT('Ctrl Pts',(33.4905872050483,1.4647927675562,2.87063810685974));
#74149=CARTESIAN_POINT('Ctrl Pts',(33.4910747334261,1.45769422095793,2.87424921480799));
#74150=CARTESIAN_POINT('Ctrl Pts',(33.4920067407488,1.44412439818775,2.88108913212089));
#74151=CARTESIAN_POINT('Ctrl Pts',(33.4924510542796,1.43765548808053,2.88432254799983));
#74152=CARTESIAN_POINT('Ctrl Pts',(33.4934687704669,1.42283905956801,2.89166615425891));
#74153=CARTESIAN_POINT('Ctrl Pts',(33.4940426704232,1.41448454374745,2.89576200847203));
#74154=CARTESIAN_POINT('Ctrl Pts',(33.4958108007527,1.38874798984052,2.90824156572417));
#74155=CARTESIAN_POINT('Ctrl Pts',(33.4970091921931,1.3713085358095,2.91650524727887));
#74156=CARTESIAN_POINT('Ctrl Pts',(33.5140033041706,1.12409660014393,3.03093910101488));
#74157=CARTESIAN_POINT('Ctrl Pts',(33.5307812868111,0.882719776687108,3.10981336198634));
#74158=CARTESIAN_POINT('Ctrl Pts',(33.5579610837558,0.488602770142272,3.18897767916929));
#74159=CARTESIAN_POINT('Ctrl Pts',(33.5680903139525,0.340681186009445,3.2081538041494));
#74160=CARTESIAN_POINT('Ctrl Pts',(33.5817012053634,0.135288220629928,3.22040955632333));
#74161=CARTESIAN_POINT('Ctrl Pts',(33.5854134154499,0.0785340083628635,
3.22229325493868));
#74162=CARTESIAN_POINT('Ctrl Pts',(33.5910489641831,-0.00920999557223865,
3.2228856165061));
#74163=CARTESIAN_POINT('Ctrl Pts',(33.5930180482641,-0.0401791499890595,
3.22264834064953));
#74164=CARTESIAN_POINT('Ctrl Pts',(33.5954518694566,-0.0789131415843825,
3.22179308891856));
#74165=CARTESIAN_POINT('Ctrl Pts',(33.5959387058417,-0.0866843200401143,
3.22159336716264));
#74166=CARTESIAN_POINT('Ctrl Pts',(33.5967083012373,-0.0990073252826235,
3.22123203998006));
#74167=CARTESIAN_POINT('Ctrl Pts',(33.5969920808811,-0.103559601571538,
3.22108890212455));
#74168=CARTESIAN_POINT('Ctrl Pts',(33.597526233037,-0.11214425999312,3.22080075574038));
#74169=CARTESIAN_POINT('Ctrl Pts',(33.597776715927,-0.116176625634615,3.2206578264498));
#74170=CARTESIAN_POINT('Ctrl Pts',(33.5983500099586,-0.125420942573093,
3.22031277272218));
#74171=CARTESIAN_POINT('Ctrl Pts',(33.598672532392,-0.130632669263656,3.22010556870806));
#74172=CARTESIAN_POINT('Ctrl Pts',(33.5996681584257,-0.146754592217182,
3.21942540012344));
#74173=CARTESIAN_POINT('Ctrl Pts',(33.600338897959,-0.157663043697437,3.21890962749139));
#74174=CARTESIAN_POINT('Ctrl Pts',(33.6059002209114,-0.248479205585574,
3.21415289479418));
#74175=CARTESIAN_POINT('Ctrl Pts',(33.6106361461237,-0.328213636123482,
3.20699219837407));
#74176=CARTESIAN_POINT('Ctrl Pts',(33.6171305017668,-0.439300996965171,
3.19282838734028));
#74177=CARTESIAN_POINT('Ctrl Pts',(33.618967983285,-0.470935095321453,3.18831596815152));
#74178=CARTESIAN_POINT('Ctrl Pts',(33.6291419685417,-0.646804281906092,
3.16055455472443));
#74179=CARTESIAN_POINT('Ctrl Pts',(33.63724217855,-0.789400686117254,3.1279883233347));
#74180=CARTESIAN_POINT('Ctrl Pts',(33.6577556065832,-1.14033063572142,3.02230644677379));
#74181=CARTESIAN_POINT('Ctrl Pts',(33.6702485155395,-1.34425361407535,2.93728671015791));
#74182=CARTESIAN_POINT('Ctrl Pts',(33.684924566749,-1.55835455903518,2.82102652742668));
#74183=CARTESIAN_POINT('Ctrl Pts',(33.6863346669472,-1.57869298209044,2.8096953615356));
#74184=CARTESIAN_POINT('Ctrl Pts',(33.6883643495246,-1.60762599536752,2.79316255833346));
#74185=CARTESIAN_POINT('Ctrl Pts',(33.6889774921215,-1.61632212697993,2.78813937895873));
#74186=CARTESIAN_POINT('Ctrl Pts',(33.6900417201285,-1.63133875618909,2.77937140294921));
#74187=CARTESIAN_POINT('Ctrl Pts',(33.69049211775,-1.63767022433886,2.7756454686923));
#74188=CARTESIAN_POINT('Ctrl Pts',(33.6913583345557,-1.64980111489311,2.76845074172262));
#74189=CARTESIAN_POINT('Ctrl Pts',(33.6917740300083,-1.65560248133948,2.7649852894219));
#74190=CARTESIAN_POINT('Ctrl Pts',(33.692753447977,-1.66922325877094,2.75679066726143));
#74191=CARTESIAN_POINT('Ctrl Pts',(33.6933177206522,-1.67703350890455,2.7520464527282));
#74192=CARTESIAN_POINT('Ctrl Pts',(33.6949863123481,-1.70001885209107,2.7379501838192));
#74193=CARTESIAN_POINT('Ctrl Pts',(33.6960940411091,-1.71513646251771,2.72850548852349));
#74194=CARTESIAN_POINT('Ctrl Pts',(33.7112833465532,-1.9204797640668,2.59783680653195));
#74195=CARTESIAN_POINT('Ctrl Pts',(33.7261316492658,-2.0975066086757,2.45711771452616));
#74196=CARTESIAN_POINT('Ctrl Pts',(33.7518921242362,-2.37011219506015,2.18934252252009));
#74197=CARTESIAN_POINT('Ctrl Pts',(33.7625696361211,-2.47370592503951,2.07157734027799));
#74198=CARTESIAN_POINT('Ctrl Pts',(33.77767879054,-2.61071967280842,1.89081611880131));
#74199=CARTESIAN_POINT('Ctrl Pts',(33.7822989206574,-2.65127772735827,1.83351318076555));
#74200=CARTESIAN_POINT('Ctrl Pts',(33.7891357767719,-2.70969811537775,1.74497604168268));
#74201=CARTESIAN_POINT('Ctrl Pts',(33.7914230139312,-2.728960886787,1.71469472549758));
#74202=CARTESIAN_POINT('Ctrl Pts',(33.7941913451706,-2.75197679645455,1.67714274692081));
#74203=CARTESIAN_POINT('Ctrl Pts',(33.7947023364444,-2.75621244538718,1.67017275785686));
#74204=CARTESIAN_POINT('Ctrl Pts',(33.7955013003503,-2.76281585073487,1.65921296404043));
#74205=CARTESIAN_POINT('Ctrl Pts',(33.7957904282399,-2.76520149351232,1.65523405778063));
#74206=CARTESIAN_POINT('Ctrl Pts',(33.7963291454886,-2.76963924894492,1.64779615505152));
#74207=CARTESIAN_POINT('Ctrl Pts',(33.7965788687404,-2.77169345683387,1.64433850514248));
#74208=CARTESIAN_POINT('Ctrl Pts',(33.797143312002,-2.77632983038721,1.63650117134253));
#74209=CARTESIAN_POINT('Ctrl Pts',(33.7974577760024,-2.77890810102189,1.63211922904628));
#74210=CARTESIAN_POINT('Ctrl Pts',(33.7983843036132,-2.78649010781804,1.61916305394649));
#74211=CARTESIAN_POINT('Ctrl Pts',(33.7989944968837,-2.79146466324536,1.61057168611753));
#74212=CARTESIAN_POINT('Ctrl Pts',(33.8031770606525,-2.82542481065391,1.55129036973048));
#74213=CARTESIAN_POINT('Ctrl Pts',(33.8066676030247,-2.85306989054627,1.49984011774334));
#74214=CARTESIAN_POINT('Ctrl Pts',(33.8249994655882,-2.99323991185709,1.22105152298918));
#74215=CARTESIAN_POINT('Ctrl Pts',(33.8387685968133,-3.08003661397099,0.981760544420308));
#74216=CARTESIAN_POINT('Ctrl Pts',(33.8626163546827,-3.17630043159713,0.57064695878151));
#74217=CARTESIAN_POINT('Ctrl Pts',(33.8723315943972,-3.20178845264642,0.403809028733365));
#74218=CARTESIAN_POINT('Ctrl Pts',(33.883861381671,-3.21578592624298,0.2129790190033));
#74219=CARTESIAN_POINT('Ctrl Pts',(33.8852449534423,-3.21721447936017,0.190184485174906));
#74220=CARTESIAN_POINT('Ctrl Pts',(33.8872431221123,-3.21891813768289,0.157425799412396));
#74221=CARTESIAN_POINT('Ctrl Pts',(33.8878515543184,-3.21938950802269,0.147472206019382));
#74222=CARTESIAN_POINT('Ctrl Pts',(33.8889102380269,-3.22012759809292,0.130190568843589));
#74223=CARTESIAN_POINT('Ctrl Pts',(33.889359821574,-3.22041548554441,0.122863465972389));
#74224=CARTESIAN_POINT('Ctrl Pts',(33.8902263439641,-3.22092126585149,0.108764286047468));
#74225=CARTESIAN_POINT('Ctrl Pts',(33.890643165549,-3.22114281359467,0.101992372470458));
#74226=CARTESIAN_POINT('Ctrl Pts',(33.891628114379,-3.22161509829806,0.0860147060581472));
#74227=CARTESIAN_POINT('Ctrl Pts',(33.8921968072082,-3.22184773391983,0.0768085141895613));
#74228=CARTESIAN_POINT('Ctrl Pts',(33.8941787487881,-3.22251948245932,0.0447914674210797));
#74229=CARTESIAN_POINT('Ctrl Pts',(33.8955983401279,-3.22275581429867,0.0219774571189312));
#74230=CARTESIAN_POINT('Ctrl Pts',(33.9108867291927,-3.22269236757379,-0.222409689435768));
#74231=CARTESIAN_POINT('Ctrl Pts',(33.9254886145542,-3.19978513449874,-0.443342263224991));
#74232=CARTESIAN_POINT('Ctrl Pts',(33.9504104189607,-3.1240733957462,-0.805123469020129));
#74233=CARTESIAN_POINT('Ctrl Pts',(33.9605006650502,-3.08377248928053,-0.947843055054371));
#74234=CARTESIAN_POINT('Ctrl Pts',(33.9721730153332,-3.02479159950525,-1.11241445468042));
#74235=CARTESIAN_POINT('Ctrl Pts',(33.9739480628578,-3.01547352190336,-1.13743115704715));
#74236=CARTESIAN_POINT('Ctrl Pts',(33.9811360105444,-2.97627737508921,-1.23879444698446));
#74237=CARTESIAN_POINT('Ctrl Pts',(33.9864675844489,-2.94379925103353,-1.31411082859061));
#74238=CARTESIAN_POINT('Ctrl Pts',(33.9923332731715,-2.9037485989655,-1.39802801640957));
#74239=CARTESIAN_POINT('Ctrl Pts',(33.9930234146757,-2.89896580791011,-1.40791885896994));
#74240=CARTESIAN_POINT('Ctrl Pts',(33.9940339776451,-2.89185678254053,-1.42243054999275));
#74241=CARTESIAN_POINT('Ctrl Pts',(33.9943567868124,-2.88956991485426,-1.42707043566162));
#74242=CARTESIAN_POINT('Ctrl Pts',(33.9949304697766,-2.88547704674999,-1.43532438763105));
#74243=CARTESIAN_POINT('Ctrl Pts',(33.9951816145403,-2.88367541347753,-1.43894058093007));
#74244=CARTESIAN_POINT('Ctrl Pts',(33.9957133814653,-2.87983965191445,-1.44660348909123));
#74245=CARTESIAN_POINT('Ctrl Pts',(33.9959938924046,-2.8778037984006,-1.45064929390348));
#74246=CARTESIAN_POINT('Ctrl Pts',(33.9967473774967,-2.87230191772499,-1.46152589040197));
#74247=CARTESIAN_POINT('Ctrl Pts',(33.9972193618536,-2.86882002888239,-1.46834869141606));
#74248=CARTESIAN_POINT('Ctrl Pts',(33.9995106975204,-2.85174542602477,-1.50151399233557));
#74249=CARTESIAN_POINT('Ctrl Pts',(34.0013094608905,-2.8378135070946,-1.52768154079737));
#74250=CARTESIAN_POINT('Ctrl Pts',(34.0062942755146,-2.79778922692071,-1.60041936893558));
#74251=CARTESIAN_POINT('Ctrl Pts',(34.0094373440646,-2.7708971243481,-1.64654076885814));
#74252=CARTESIAN_POINT('Ctrl Pts',(34.0172331602429,-2.7004133406762,-1.76080240005062));
#74253=CARTESIAN_POINT('Ctrl Pts',(34.0218274655985,-2.65537865515775,-1.8280106233033));
#74254=CARTESIAN_POINT('Ctrl Pts',(34.0375782712077,-2.49102974793326,-2.05436867573003));
#74255=CARTESIAN_POINT('Ctrl Pts',(34.0485229735838,-2.35955981635353,-2.20411811531303));
#74256=CARTESIAN_POINT('Ctrl Pts',(34.062319302285,-2.18453738827689,-2.3697442260397));
#74257=CARTESIAN_POINT('Ctrl Pts',(34.064747572999,-2.15338359315616,-2.39808886705959));
#74258=CARTESIAN_POINT('Ctrl Pts',(34.0675486660572,-2.11713261360311,-2.42979497522419));
#74259=CARTESIAN_POINT('Ctrl Pts',(34.0679007827238,-2.11256998412559,-2.43376296849092));
#74260=CARTESIAN_POINT('Ctrl Pts',(34.0730991300267,-2.04513115690436,-2.49208012778898));
#74261=CARTESIAN_POINT('Ctrl Pts',(34.0780270488176,-1.98019140265298,-2.54398605067792));
#74262=CARTESIAN_POINT('Ctrl Pts',(34.0839663727014,-1.90123248354936,-2.60224102056088));
#74263=CARTESIAN_POINT('Ctrl Pts',(34.0848789899186,-1.88908065921275,-2.61107593468888));
#74264=CARTESIAN_POINT('Ctrl Pts',(34.0863637079333,-1.86928283909061,-2.62525927978279));
#74265=CARTESIAN_POINT('Ctrl Pts',(34.0869337834369,-1.8616745195216,-2.63066010709916));
#74266=CARTESIAN_POINT('Ctrl Pts',(34.0879481934027,-1.84812483077425,-2.64019024357382));
#74267=CARTESIAN_POINT('Ctrl Pts',(34.0883920179623,-1.84219278316576,-2.64433274394175));
#74268=CARTESIAN_POINT('Ctrl Pts',(34.0893251830207,-1.82971273657552,-2.65298550366578));
#74269=CARTESIAN_POINT('Ctrl Pts',(34.0898146793625,-1.8231619033622,-2.65749157164531));
#74270=CARTESIAN_POINT('Ctrl Pts',(34.0911020894005,-1.80592184261346,-2.66925660304347));
#74271=CARTESIAN_POINT('Ctrl Pts',(34.0919015128902,-1.79520559901843,-2.6764755489184));
#74272=CARTESIAN_POINT('Ctrl Pts',(34.0954843561959,-1.74713238270632,-2.70844123829686));
#74273=CARTESIAN_POINT('Ctrl Pts',(34.0982945017097,-1.70930660578123,-2.73247069606748));
#74274=CARTESIAN_POINT('Ctrl Pts',(34.1058237651811,-1.60769913970024,-2.79408308342598));
#74275=CARTESIAN_POINT('Ctrl Pts',(34.1105911047565,-1.5431055586311,-2.83026865217769));
#74276=CARTESIAN_POINT('Ctrl Pts',(34.1350940527639,-1.20977322716755,-3.00219855800697));
#74277=CARTESIAN_POINT('Ctrl Pts',(34.1559505400123,-0.924254100659246,
-3.10200905282167));
#74278=CARTESIAN_POINT('Ctrl Pts',(34.1772913978078,-0.606969066619641,
-3.1651561847723));
#74279=CARTESIAN_POINT('Ctrl Pts',(34.1787703826077,-0.584827328114436,
-3.1693220354944));
#74280=CARTESIAN_POINT('Ctrl Pts',(34.1838265784864,-0.508544881713805,
-3.18284751520198));
#74281=CARTESIAN_POINT('Ctrl Pts',(34.1873607449368,-0.45420606974951,-3.19105529844832));
#74282=CARTESIAN_POINT('Ctrl Pts',(34.1913822789209,-0.390861605494726,
-3.19897229603057));
#74283=CARTESIAN_POINT('Ctrl Pts',(34.1919402298768,-0.382038338056251,
-3.20003800884452));
#74284=CARTESIAN_POINT('Ctrl Pts',(34.1928271238649,-0.36795562183618,-3.20167990492449));
#74285=CARTESIAN_POINT('Ctrl Pts',(34.1931573605453,-0.362699044396027,
-3.20227965009078));
#74286=CARTESIAN_POINT('Ctrl Pts',(34.1937394973898,-0.353409609686988,
-3.20331635411682));
#74287=CARTESIAN_POINT('Ctrl Pts',(34.193991697711,-0.34937737694337,-3.20375864664951));
#74288=CARTESIAN_POINT('Ctrl Pts',(34.194520621874,-0.340904351111182,-3.20467185959086));
#74289=CARTESIAN_POINT('Ctrl Pts',(34.1947972531571,-0.33646342250337,-3.2051411622821));
#74290=CARTESIAN_POINT('Ctrl Pts',(34.1955294039,-0.324685144208438,-3.20636110242637));
#74291=CARTESIAN_POINT('Ctrl Pts',(34.1959840285445,-0.317346115838568,
-3.20709579016687));
#74292=CARTESIAN_POINT('Ctrl Pts',(34.1980705665225,-0.283550136825774,
-3.21036185720309));
#74293=CARTESIAN_POINT('Ctrl Pts',(34.199686075999,-0.257064107710861,-3.21259117942451));
#74294=CARTESIAN_POINT('Ctrl Pts',(34.21409152433,-0.0183803925095439,-3.2297102528033));
#74295=CARTESIAN_POINT('Ctrl Pts',(34.2258931363999,0.194808855475423,-3.22388609181496));
#74296=CARTESIAN_POINT('Ctrl Pts',(34.2518266971885,0.655173114240783,-3.16543964946339));
#74297=CARTESIAN_POINT('Ctrl Pts',(34.2659535153078,0.899856969521382,-3.10475341768069));
#74298=CARTESIAN_POINT('Ctrl Pts',(34.2822982124249,1.15309804491474,-3.00946117669203));
#74299=CARTESIAN_POINT('Ctrl Pts',(34.2834719114789,1.17113881898752,-3.00248655560916));
#74300=CARTESIAN_POINT('Ctrl Pts',(34.2852188387614,1.19777140328748,-2.99191376251029));
#74301=CARTESIAN_POINT('Ctrl Pts',(34.2857878707302,1.20641237946928,-2.98843997172863));
#74302=CARTESIAN_POINT('Ctrl Pts',(34.2868011038135,1.22173745400303,-2.98220178289296));
#74303=CARTESIAN_POINT('Ctrl Pts',(34.2872447992585,1.22842755825503,-2.97945223374505));
#74304=CARTESIAN_POINT('Ctrl Pts',(34.2881783850816,1.24246039339101,-2.97362961591066));
#74305=CARTESIAN_POINT('Ctrl Pts',(34.2886684338232,1.24980109980339,-2.97055182262154));
#74306=CARTESIAN_POINT('Ctrl Pts',(34.2899588616555,1.26906423405284,-2.9623911814377));
#74307=CARTESIAN_POINT('Ctrl Pts',(34.2907607634599,1.2809674422033,-2.95726359091311));
#74308=CARTESIAN_POINT('Ctrl Pts',(34.294370348991,1.33424200458382,-2.93393230933178));
#74309=CARTESIAN_POINT('Ctrl Pts',(34.2972052509489,1.37525690619207,-2.91493201110783));
#74310=CARTESIAN_POINT('Ctrl Pts',(34.3048161715812,1.48313836262008,-2.86217183828571));
#74311=CARTESIAN_POINT('Ctrl Pts',(34.30964170965,1.54924744292296,-2.82693437403859));
#74312=CARTESIAN_POINT('Ctrl Pts',(34.3345583713122,1.87919669710098,-2.63601368599455));
#74313=CARTESIAN_POINT('Ctrl Pts',(34.3558101807841,2.12105464443564,-2.4456150849873));
#74314=CARTESIAN_POINT('Ctrl Pts',(34.3805446715954,2.38055917866903,-2.17345975217112));
#74315=CARTESIAN_POINT('Ctrl Pts',(34.3850620962195,2.4270762221431,-2.12138916657322));
#74316=CARTESIAN_POINT('Ctrl Pts',(34.3901286790484,2.47863766626281,-2.05975342278005));
#74317=CARTESIAN_POINT('Ctrl Pts',(34.3907911039627,2.48536664892809,-2.05162897985243));
#74318=CARTESIAN_POINT('Ctrl Pts',(34.3917722350599,2.49531654551626,-2.03949487538844));
#74319=CARTESIAN_POINT('Ctrl Pts',(34.3920931003489,2.4985678677454,-2.03551040778731));
#74320=CARTESIAN_POINT('Ctrl Pts',(34.392663993498,2.50434824582372,-2.02839188620047));
#74321=CARTESIAN_POINT('Ctrl Pts',(34.3929142863809,2.50688097057737,-2.02526086723646));
#74322=CARTESIAN_POINT('Ctrl Pts',(34.393449541339,2.512294015095,-2.0185434110434));
#74323=CARTESIAN_POINT('Ctrl Pts',(34.3937343722852,2.51517251721996,-2.01495556521726));
#74324=CARTESIAN_POINT('Ctrl Pts',(34.3945116892489,2.52302221940756,-2.00512844564018));
#74325=CARTESIAN_POINT('Ctrl Pts',(34.3950030746773,2.52797799056766,-1.9988768059891));
#74326=CARTESIAN_POINT('Ctrl Pts',(34.3975492816733,2.55361970908719,-1.96628222627942));
#74327=CARTESIAN_POINT('Ctrl Pts',(34.399577594593,2.57391818456463,-1.93963522352443));
#74328=CARTESIAN_POINT('Ctrl Pts',(34.4053830945387,2.63148526249179,-1.86156792582208));
#74329=CARTESIAN_POINT('Ctrl Pts',(34.4090982417231,2.66765582003833,-1.80935438767603));
#74330=CARTESIAN_POINT('Ctrl Pts',(34.4330602878244,2.89416807216864,-1.46080108700049));
#74331=CARTESIAN_POINT('Ctrl Pts',(34.4518113554724,3.03637594754524,-1.13604757613463));
#74332=CARTESIAN_POINT('Ctrl Pts',(34.4738388306347,3.12800406265096,-0.775939869479387));
#74333=CARTESIAN_POINT('Ctrl Pts',(34.4749910462281,3.13260716192307,-0.757142286912593));
#74334=CARTESIAN_POINT('Ctrl Pts',(34.4765962884021,3.13875594932679,-0.731016222123901));
#74335=CARTESIAN_POINT('Ctrl Pts',(34.4770448809079,3.14044587520714,-0.723721859513328));
#74336=CARTESIAN_POINT('Ctrl Pts',(34.4791967128837,3.14841617263775,-0.688765417767764));
#74337=CARTESIAN_POINT('Ctrl Pts',(34.480910366545,3.15435641672236,-0.661027771455983));
#74338=CARTESIAN_POINT('Ctrl Pts',(34.4833178010663,3.16213275926679,-0.622221589080528));
#74339=CARTESIAN_POINT('Ctrl Pts',(34.4840016766316,3.16427850150988,-0.611215880881014));
#74340=CARTESIAN_POINT('Ctrl Pts',(34.4851044326133,3.1676368019304,-0.593499081402116));
#74341=CARTESIAN_POINT('Ctrl Pts',(34.4855221539621,3.168885582184,-0.586794882785151));
#74342=CARTESIAN_POINT('Ctrl Pts',(34.4863886381031,3.17142762870947,-0.572902867409919));
#74343=CARTESIAN_POINT('Ctrl Pts',(34.4868374982169,3.17271775873012,-0.565714523118713));
#74344=CARTESIAN_POINT('Ctrl Pts',(34.4878898824897,3.17568006867618,-0.548880227709062));
#74345=CARTESIAN_POINT('Ctrl Pts',(34.4884940239807,3.17733274505393,-0.539230958658211));
#74346=CARTESIAN_POINT('Ctrl Pts',(34.4904520581129,3.18253436628835,-0.508006546438726));
#74347=CARTESIAN_POINT('Ctrl Pts',(34.491811513763,3.18590765657875,-0.486403134856993));
#74348=CARTESIAN_POINT('Ctrl Pts',(34.4950023192994,3.19327052644359,-0.435881874109262));
#74349=CARTESIAN_POINT('Ctrl Pts',(34.496839005377,3.1970874933311,-0.406941191132162));
#74350=CARTESIAN_POINT('Ctrl Pts',(34.5032898435442,3.20903120086238,-0.305801833587352));
#74351=CARTESIAN_POINT('Ctrl Pts',(34.5079661539453,3.21510884141991,-0.233387719814971));
#74352=CARTESIAN_POINT('Ctrl Pts',(34.5317643456143,3.23330240527779,0.130715023243514));
#74353=CARTESIAN_POINT('Ctrl Pts',(34.5519386052257,3.20819256489968,0.422837264813661));
#74354=CARTESIAN_POINT('Ctrl Pts',(34.5719223956567,3.14198504625179,0.717036866251241));
#74355=CARTESIAN_POINT('Ctrl Pts',(34.5725648380975,3.13980976651225,0.726502946845154));
#74356=CARTESIAN_POINT('Ctrl Pts',(34.5783167751819,3.11991039252752,0.811339330235586));
#74357=CARTESIAN_POINT('Ctrl Pts',(34.5833430977989,3.09951658942662,0.88606518541743));
#74358=CARTESIAN_POINT('Ctrl Pts',(34.5889104651749,3.07322226182184,0.970329741651132));
#74359=CARTESIAN_POINT('Ctrl Pts',(34.5895907786374,3.06994370432798,0.980653118201075));
#74360=CARTESIAN_POINT('Ctrl Pts',(34.5905931741331,3.06501467198019,0.995906444367906));
#74361=CARTESIAN_POINT('Ctrl Pts',(34.5909175521902,3.06340425631236,1.00084911385299));
#74362=CARTESIAN_POINT('Ctrl Pts',(34.5914923265982,3.06052323347696,1.00961941566585));
#74363=CARTESIAN_POINT('Ctrl Pts',(34.5917430020978,3.05925739641625,1.01344857308127));
#74364=CARTESIAN_POINT('Ctrl Pts',(34.5922764972188,3.0565434218592,1.02160692593387));
#74365=CARTESIAN_POINT('Ctrl Pts',(34.5925591954394,3.05509327814732,1.02593540891315));
#74366=CARTESIAN_POINT('Ctrl Pts',(34.5933247326321,3.05113387133929,1.03767086332361));
#74367=CARTESIAN_POINT('Ctrl Pts',(34.5938065264061,3.04860681656638,1.04507186470845));
#74368=CARTESIAN_POINT('Ctrl Pts',(34.5962230110933,3.0357563017489,1.08226397634098));
#74369=CARTESIAN_POINT('Ctrl Pts',(34.5981343063317,3.02502256985817,1.11191288583828));
#74370=CARTESIAN_POINT('Ctrl Pts',(34.6035158791671,2.99322841875114,1.19586495752777));
#74371=CARTESIAN_POINT('Ctrl Pts',(34.6069344403413,2.97112800012848,1.24976341932747));
#74372=CARTESIAN_POINT('Ctrl Pts',(34.6267367759753,2.83274271150433,1.5628025391476));
#74373=CARTESIAN_POINT('Ctrl Pts',(34.6420328778033,2.6840707846814,1.80625876471057));
#74374=CARTESIAN_POINT('Ctrl Pts',(34.6592125547122,2.49606351048983,2.03862817651479));
#74375=CARTESIAN_POINT('Ctrl Pts',(34.6600679475698,2.48664755277495,2.05010288296596));
#74376=CARTESIAN_POINT('Ctrl Pts',(34.6669095603765,2.41092169336804,2.14109654099073));
#74377=CARTESIAN_POINT('Ctrl Pts',(34.6730105519655,2.34089994481689,2.21743589382977));
#74378=CARTESIAN_POINT('Ctrl Pts',(34.680239664614,2.25595243793691,2.30153264586878));
#74379=CARTESIAN_POINT('Ctrl Pts',(34.6812116344691,2.24449032281051,2.31271206567245));
#74380=CARTESIAN_POINT('Ctrl Pts',(34.682767615086,2.22607946068685,2.3304030700112));
#74381=CARTESIAN_POINT('Ctrl Pts',(34.683349207277,2.21918423713549,2.33697016510572));
#74382=CARTESIAN_POINT('Ctrl Pts',(34.6843782107073,2.20696122235134,2.34850863830448));
#74383=CARTESIAN_POINT('Ctrl Pts',(34.6848250702172,2.20164546124089,2.35349270718351));
#74384=CARTESIAN_POINT('Ctrl Pts',(34.6857512738721,2.19061182638981,2.36376777139543));
#74385=CARTESIAN_POINT('Ctrl Pts',(34.6862307259954,2.1848915848346,2.36905614366219));
#74386=CARTESIAN_POINT('Ctrl Pts',(34.6874631207535,2.17016643487082,2.38257087380289));
#74387=CARTESIAN_POINT('Ctrl Pts',(34.6882173449824,2.16113396010438,2.39076689027765));
#74388=CARTESIAN_POINT('Ctrl Pts',(34.6913454025323,2.12358988007634,2.42444755781927));
#74389=CARTESIAN_POINT('Ctrl Pts',(34.6937383177986,2.09467326617776,2.44947415665856));
#74390=CARTESIAN_POINT('Ctrl Pts',(34.7034148302954,1.97701218882663,2.54769957885559));
#74391=CARTESIAN_POINT('Ctrl Pts',(34.7108594538666,1.88491167208578,2.61656343737978));
#74392=CARTESIAN_POINT('Ctrl Pts',(34.7184445309107,1.78943583648355,2.68030538364725));
#74393=CARTESIAN_POINT('Origin',(-1.72497344927317,0.,0.));
#74394=CARTESIAN_POINT('',(36.2170783832723,1.78943621037801,2.68030513402635));
#74395=CARTESIAN_POINT('',(35.9732071344081,1.7894362098569,2.68030513437425));
#74396=CARTESIAN_POINT('',(-1.72497344927317,1.78943621037804,2.68030513402633));
#74397=CARTESIAN_POINT('',(35.3965734493253,-3.22274924894224,0.0022002141326696));
#74398=CARTESIAN_POINT('Ctrl Pts',(35.3965734493253,-3.22274924894224,0.00220021413262451));
#74399=CARTESIAN_POINT('Ctrl Pts',(35.4026541762509,-3.22281622665231,-0.0959049482773073));
#74400=CARTESIAN_POINT('Ctrl Pts',(35.4087349031765,-3.21839931530627,-0.194185885337791));
#74401=CARTESIAN_POINT('Ctrl Pts',(35.4148156301021,-3.20947683880307,-0.292191689968481));
#74402=CARTESIAN_POINT('Ctrl Pts',(35.4208892708103,-3.20056476016993,-0.390083282853154));
#74403=CARTESIAN_POINT('Ctrl Pts',(35.4269629115185,-3.18715758731565,-0.487699937740014));
#74404=CARTESIAN_POINT('Ctrl Pts',(35.4330365522267,-3.16928567806029,-0.584590329497458));
#74405=CARTESIAN_POINT('Ctrl Pts',(35.4391050586173,-3.15142887672161,-0.681398815514107));
#74406=CARTESIAN_POINT('Ctrl Pts',(35.4451735650079,-3.12911491984515,-0.777481819955843));
#74407=CARTESIAN_POINT('Ctrl Pts',(35.4512420713985,-3.10242590709074,-0.872393863752045));
#74408=CARTESIAN_POINT('Ctrl Pts',(35.4573079117998,-3.07574861923517,-0.967264211209651));
#74409=CARTESIAN_POINT('Ctrl Pts',(35.4633737522011,-3.04470021267832,-1.06096418915499));
#74410=CARTESIAN_POINT('Ctrl Pts',(35.4694395926024,-3.00941350713223,-1.15306023502247));
#74411=CARTESIAN_POINT('Ctrl Pts',(35.4755044967244,-2.97413224818665,-1.24514206561079));
#74412=CARTESIAN_POINT('Ctrl Pts',(35.4815694008465,-2.93461415028325,-1.33562003807765));
#74413=CARTESIAN_POINT('Ctrl Pts',(35.4876343049685,-2.89104095423344,-1.42407856645798));
#74414=CARTESIAN_POINT('Ctrl Pts',(35.493700001277,-2.84746206673425,-1.51254864912586));
#74415=CARTESIAN_POINT('Ctrl Pts',(35.4997656975855,-2.79982722847961,-1.59899836299989));
#74416=CARTESIAN_POINT('Ctrl Pts',(35.505831393894,-2.74836456137673,-1.68303588799185));
#74417=CARTESIAN_POINT('Ctrl Pts',(35.5119033144651,-2.69684908629595,-1.76715964737491));
#74418=CARTESIAN_POINT('Ctrl Pts',(35.5179752350362,-2.64149817683487,-1.84886589519704));
#74419=CARTESIAN_POINT('Ctrl Pts',(35.5240471556074,-2.58258360470976,-1.92779134949411));
#74420=CARTESIAN_POINT('Ctrl Pts',(35.5301225189983,-2.52363562762575,-2.00676155505496));
#74421=CARTESIAN_POINT('Ctrl Pts',(35.5361978823893,-2.46112025182293,-2.08294748478473));
#74422=CARTESIAN_POINT('Ctrl Pts',(35.5422732457803,-2.39534846607981,-2.15602024307499));
#74423=CARTESIAN_POINT('Ctrl Pts',(35.5483582611303,-2.32947218838389,-2.22920909240829));
#74424=CARTESIAN_POINT('Ctrl Pts',(35.5544432764804,-2.26032948940595,-2.29927458140149));
#74425=CARTESIAN_POINT('Ctrl Pts',(35.5605282918304,-2.18826682920184,-2.3659260019525));
#74426=CARTESIAN_POINT('Ctrl Pts',(35.5638661635418,-2.14873760846764,-2.40248694360725));
#74427=CARTESIAN_POINT('Ctrl Pts',(35.5672040352532,-2.10833035019661,-2.4380213303225));
#74428=CARTESIAN_POINT('Ctrl Pts',(35.5705419069646,-2.06710597654784,-2.4724866924253));
#74429=CARTESIAN_POINT('Ctrl Pts',(35.5767141550573,-1.99087564667602,-2.53621855029738));
#74430=CARTESIAN_POINT('Ctrl Pts',(35.5828864031501,-1.91156096397265,-2.59653384352848));
#74431=CARTESIAN_POINT('Ctrl Pts',(35.5890586512429,-1.8295011211476,-2.65311952429959));
#74432=CARTESIAN_POINT('Ctrl Pts',(35.5952225398955,-1.7475524168143,-2.70962856774117));
#74433=CARTESIAN_POINT('Ctrl Pts',(35.6013864285481,-1.66286629660897,-2.7624177941908));
#74434=CARTESIAN_POINT('Ctrl Pts',(35.6075503172008,-1.57581578216981,-2.81121364950524));
#74435=CARTESIAN_POINT('Ctrl Pts',(35.6137076788593,-1.48885744626015,-2.85995783447381));
#74436=CARTESIAN_POINT('Ctrl Pts',(35.6198650405179,-1.39954007048067,-2.90471684396876));
#74437=CARTESIAN_POINT('Ctrl Pts',(35.6260224021764,-1.30826567747346,-2.94526034157337));
#74438=CARTESIAN_POINT('Ctrl Pts',(35.6321752663227,-1.21705795388129,-2.98577422505315));
#74439=CARTESIAN_POINT('Ctrl Pts',(35.6383281304691,-1.1238964508519,-3.02207854267777));
#74440=CARTESIAN_POINT('Ctrl Pts',(35.6444809946154,-1.02920699676254,-3.05398927966603));
#74441=CARTESIAN_POINT('Ctrl Pts',(35.6506315277519,-0.934553415729537,
-3.08588792728618));
#74442=CARTESIAN_POINT('Ctrl Pts',(35.6567820608884,-0.838373445007394,
-3.11339616306775));
#74443=CARTESIAN_POINT('Ctrl Pts',(35.662932594025,-0.741111225582647,-3.13637875802898));
#74444=CARTESIAN_POINT('Ctrl Pts',(35.6690824422402,-0.643859837246461,
-3.15935879365603));
#74445=CARTESIAN_POINT('Ctrl Pts',(35.6752322904554,-0.545526862551012,
-3.17781409054637));
#74446=CARTESIAN_POINT('Ctrl Pts',(35.6813821386706,-0.446568896009425,
-3.19166003572074));
#74447=CARTESIAN_POINT('Ctrl Pts',(35.6875329470498,-0.347595479351526,
-3.20550814263581));
#74448=CARTESIAN_POINT('Ctrl Pts',(35.6936837554289,-0.247997307256176,
-3.2147454082297));
#74449=CARTESIAN_POINT('Ctrl Pts',(35.699834563808,-0.148237390124708,-3.21933894435939));
#74450=CARTESIAN_POINT('Ctrl Pts',(35.7059919501742,-0.0483707846683332,
-3.22393739305004));
#74451=CARTESIAN_POINT('Ctrl Pts',(35.7121493365404,0.0516574764825923,
-3.22388217518866));
#74452=CARTESIAN_POINT('Ctrl Pts',(35.7183067229066,0.151383196910882,-3.21919255251888));
#74453=CARTESIAN_POINT('Ctrl Pts',(35.7244675456436,0.251164573185612,-3.21450031262139));
#74454=CARTESIAN_POINT('Ctrl Pts',(35.7306283683805,0.350642639995108,-3.2051685576842));
#74455=CARTESIAN_POINT('Ctrl Pts',(35.7367891911175,0.44935923717731,-3.19126837455947));
#74456=CARTESIAN_POINT('Ctrl Pts',(35.7429603140342,0.548240877039232,-3.17734495194374));
#74457=CARTESIAN_POINT('Ctrl Pts',(35.7491314369508,0.646358077271314,-3.15883792525885));
#74458=CARTESIAN_POINT('Ctrl Pts',(35.7553025598675,0.743263625943796,-3.13586937624144));
#74459=CARTESIAN_POINT('Ctrl Pts',(35.7599980818131,0.816997715603227,-3.11839292545202));
#74460=CARTESIAN_POINT('Ctrl Pts',(35.7646936037587,0.890030550168058,-3.09833454312605));
#74461=CARTESIAN_POINT('Ctrl Pts',(35.7693891257042,0.962172478710912,-3.07576684482282));
#74462=CARTESIAN_POINT('Ctrl Pts',(35.775561373797,1.05700280556683,-3.04610167992207));
#74463=CARTESIAN_POINT('Ctrl Pts',(35.7817336218897,1.15062682894838,-3.0119945584408));
#74464=CARTESIAN_POINT('Ctrl Pts',(35.7879058699825,1.24259780526836,-2.97356154414908));
#74465=CARTESIAN_POINT('Ctrl Pts',(35.7940697586351,1.33444421986316,-2.93518058195853));
#74466=CARTESIAN_POINT('Ctrl Pts',(35.8002336472878,1.42464164003634,-2.89248553799921));
#74467=CARTESIAN_POINT('Ctrl Pts',(35.8063975359404,1.51275825298489,-2.84564228787213));
#74468=CARTESIAN_POINT('Ctrl Pts',(35.812554897599,1.60078155850296,-2.79884864046079));
#74469=CARTESIAN_POINT('Ctrl Pts',(35.8187122592575,1.68672805590052,-2.74791572249858));
#74470=CARTESIAN_POINT('Ctrl Pts',(35.824869620916,1.77018660637164,-2.69305717375671));
#74471=CARTESIAN_POINT('Ctrl Pts',(35.8310224850623,1.85358419634174,-2.63823869526046));
#74472=CARTESIAN_POINT('Ctrl Pts',(35.8371753492086,1.93449709053669,-2.57950052472488));
#74473=CARTESIAN_POINT('Ctrl Pts',(35.843328213355,2.0125402443185,-2.51710137410046));
#74474=CARTESIAN_POINT('Ctrl Pts',(35.8494787464915,2.09055383148716,-2.45472586336575));
#74475=CARTESIAN_POINT('Ctrl Pts',(35.855629279628,2.16569949961442,-2.38869239938264));
#74476=CARTESIAN_POINT('Ctrl Pts',(35.8617798127646,2.2376233412963,-2.31930147781309));
#74477=CARTESIAN_POINT('Ctrl Pts',(35.8679296609798,2.30953917356318,-2.2499182835934));
#74478=CARTESIAN_POINT('Ctrl Pts',(35.874079509195,2.37823358008963,-2.17717867672222));
#74479=CARTESIAN_POINT('Ctrl Pts',(35.8802293574102,2.44338849835483,-2.10142099746989));
#74480=CARTESIAN_POINT('Ctrl Pts',(35.8863801657894,2.5085535891317,-2.02565149031726));
#74481=CARTESIAN_POINT('Ctrl Pts',(35.8925309741685,2.57017781074956,-1.9468633042078));
#74482=CARTESIAN_POINT('Ctrl Pts',(35.8986817825477,2.62798314294445,-1.86542814466273));
#74483=CARTESIAN_POINT('Ctrl Pts',(35.9048391689139,2.68585029509895,-1.78390589421993));
#74484=CARTESIAN_POINT('Ctrl Pts',(35.9109965552801,2.73989015035574,-1.69973137241133));
#74485=CARTESIAN_POINT('Ctrl Pts',(35.9171539416463,2.7898679161095,-1.61330548042299));
#74486=CARTESIAN_POINT('Ctrl Pts',(35.9233147643832,2.83987357391408,-1.52683135507855));
#74487=CARTESIAN_POINT('Ctrl Pts',(35.9294755871202,2.8858124277765,-1.4381037430731));
#74488=CARTESIAN_POINT('Ctrl Pts',(35.9356364098571,2.92749654469965,-1.3475464902079));
#74489=CARTESIAN_POINT('Ctrl Pts',(35.9418075327738,2.96925035262258,-1.2568378361387));
#74490=CARTESIAN_POINT('Ctrl Pts',(35.9479786556905,3.00673505160855,-1.1642938338478));
#74491=CARTESIAN_POINT('Ctrl Pts',(35.9541497786072,3.03981152583318,-1.07035669284203));
#74492=CARTESIAN_POINT('Ctrl Pts',(35.9588453005528,3.06497895689897,-0.998881223457837));
#74493=CARTESIAN_POINT('Ctrl Pts',(35.9635408224984,3.08759526833057,-0.926599579291563));
#74494=CARTESIAN_POINT('Ctrl Pts',(35.968236344444,3.10761899878544,-0.853710560370323));
#74495=CARTESIAN_POINT('Ctrl Pts',(35.9744085925367,3.1339401263496,-0.75789818567932));
#74496=CARTESIAN_POINT('Ctrl Pts',(35.9805808406295,3.15587237980187,-0.660698752818934));
#74497=CARTESIAN_POINT('Ctrl Pts',(35.9867530887222,3.17327183418831,-0.562550823345912));
#74498=CARTESIAN_POINT('Ctrl Pts',(35.9929169773749,3.19064772346603,-0.464535821410606));
#74499=CARTESIAN_POINT('Ctrl Pts',(35.9990808660275,3.2035029405354,-0.365575300096989));
#74500=CARTESIAN_POINT('Ctrl Pts',(36.0052447546801,3.21174353582663,-0.266122194820102));
#74501=CARTESIAN_POINT('Ctrl Pts',(36.0114021163387,3.21997540508147,-0.166774401281577));
#74502=CARTESIAN_POINT('Ctrl Pts',(36.0175594779972,3.22360233163526,-0.0669354912772715));
#74503=CARTESIAN_POINT('Ctrl Pts',(36.0237168396557,3.22258172420588,0.0329331643525058));
#74504=CARTESIAN_POINT('Ctrl Pts',(36.029869703802,3.22156186225722,0.132728873073168));
#74505=CARTESIAN_POINT('Ctrl Pts',(36.0360225679483,3.21590121997748,0.232553851179046));
#74506=CARTESIAN_POINT('Ctrl Pts',(36.0421754320946,3.2056092305873,0.331944307487699));
#74507=CARTESIAN_POINT('Ctrl Pts',(36.0483259652312,3.19532114031261,0.431297109767358));
#74508=CARTESIAN_POINT('Ctrl Pts',(36.0544764983677,3.18040523396699,0.530215285760309));
#74509=CARTESIAN_POINT('Ctrl Pts',(36.0606270315042,3.16092292982288,0.628238644322294));
#74510=CARTESIAN_POINT('Ctrl Pts',(36.0667768797195,3.14144279522168,0.726251087035697));
#74511=CARTESIAN_POINT('Ctrl Pts',(36.0729267279347,3.11739735849586,0.823368484387686));
#74512=CARTESIAN_POINT('Ctrl Pts',(36.0790765761499,3.08889925483512,0.91914033530199));
#74513=CARTESIAN_POINT('Ctrl Pts',(36.085227384529,3.06039670182045,1.01492713889055));
#74514=CARTESIAN_POINT('Ctrl Pts',(36.0913781929082,3.02744022494843,1.1093675623996));
#74515=CARTESIAN_POINT('Ctrl Pts',(36.0975290012873,2.99019217781354,1.20202674772349));
#74516=CARTESIAN_POINT('Ctrl Pts',(36.1036863876535,2.95290429572424,1.29478502748874));
#74517=CARTESIAN_POINT('Ctrl Pts',(36.1098437740197,2.91131584069827,1.38575786127123));
#74518=CARTESIAN_POINT('Ctrl Pts',(36.1160011603858,2.86563709962124,1.47453096806218));
#74519=CARTESIAN_POINT('Ctrl Pts',(36.1221619831228,2.81993286573246,1.56335361816466));
#74520=CARTESIAN_POINT('Ctrl Pts',(36.1283228058598,2.77013401624417,1.64997371985045));
#74521=CARTESIAN_POINT('Ctrl Pts',(36.1344836285967,2.71649547672681,1.73400400444255));
#74522=CARTESIAN_POINT('Ctrl Pts',(36.1406547515134,2.66276725980429,1.81817477790597));
#74523=CARTESIAN_POINT('Ctrl Pts',(36.1468258744301,2.60518678068265,1.8997467304522));
#74524=CARTESIAN_POINT('Ctrl Pts',(36.1529969973468,2.54405080859028,1.97836372940144));
#74525=CARTESIAN_POINT('Ctrl Pts',(36.1576925192924,2.49753329427433,2.0381823149074));
#74526=CARTESIAN_POINT('Ctrl Pts',(36.1623880412379,2.44895820203773,2.09629078279533));
#74527=CARTESIAN_POINT('Ctrl Pts',(36.1670835631835,2.39847034566298,2.15254676220409));
#74528=CARTESIAN_POINT('Ctrl Pts',(36.173255787853,2.33210447702427,2.22649478075079));
#74529=CARTESIAN_POINT('Ctrl Pts',(36.1794280125225,2.26219872041211,2.29750085817463));
#74530=CARTESIAN_POINT('Ctrl Pts',(36.1856002371921,2.18904417262736,2.36520679281668));
#74531=CARTESIAN_POINT('Ctrl Pts',(36.191763242266,2.11599889749356,2.43281159352808));
#74532=CARTESIAN_POINT('Ctrl Pts',(36.1979262473398,2.03971479775672,2.49712576225517));
#74533=CARTESIAN_POINT('Ctrl Pts',(36.2040892524137,1.9605219423884,2.55782549754936));
#74534=CARTESIAN_POINT('Ctrl Pts',(36.2084189626999,1.90488640154891,2.60046902373868));
#74535=CARTESIAN_POINT('Ctrl Pts',(36.2127486729861,1.8478160898422,2.64132932155466));
#74536=CARTESIAN_POINT('Ctrl Pts',(36.2170783832723,1.78943621037801,2.68030513402635));
#74537=CARTESIAN_POINT('Ctrl Pts',(34.9669226703048,1.78943621037804,2.68030513402632));
#74538=CARTESIAN_POINT('Ctrl Pts',(34.9692818637851,1.75780908412248,2.70142016463737));
#74539=CARTESIAN_POINT('Ctrl Pts',(34.9716410572654,1.72582786777747,2.72196218169318));
#74540=CARTESIAN_POINT('Ctrl Pts',(34.9740002507457,1.69351550403383,2.74191954661275));
#74541=CARTESIAN_POINT('Ctrl Pts',(34.9801724988385,1.60897817076503,2.79413307152716));
#74542=CARTESIAN_POINT('Ctrl Pts',(34.9863447469312,1.52187505275975,2.84252522299456));
#74543=CARTESIAN_POINT('Ctrl Pts',(34.992516995024,1.43258650633541,2.88683450588455));
#74544=CARTESIAN_POINT('Ctrl Pts',(34.9986808836766,1.34341888866301,2.93108377809575));
#74545=CARTESIAN_POINT('Ctrl Pts',(35.0048447723292,1.25207211128199,2.97126098116774));
#74546=CARTESIAN_POINT('Ctrl Pts',(35.0110086609819,1.15895438370155,3.00714853291269));
#74547=CARTESIAN_POINT('Ctrl Pts',(35.0171660226404,1.06593525927433,3.04299808302407));
#74548=CARTESIAN_POINT('Ctrl Pts',(35.023323384299,0.971149315950608,3.07456685707849));
#74549=CARTESIAN_POINT('Ctrl Pts',(35.0294807459575,0.875027306918201,3.10168418357632));
#74550=CARTESIAN_POINT('Ctrl Pts',(35.0356336101038,0.778975508137488,3.12878170280693));
#74551=CARTESIAN_POINT('Ctrl Pts',(35.0417864742501,0.681590000702285,3.1514341213634));
#74552=CARTESIAN_POINT('Ctrl Pts',(35.0479393383964,0.583318496780982,3.16952001000359));
#74553=CARTESIAN_POINT('Ctrl Pts',(35.054089871533,0.485084222974071,3.18759904681313));
#74554=CARTESIAN_POINT('Ctrl Pts',(35.0602404046695,0.38596504636087,3.20111491272747));
#74555=CARTESIAN_POINT('Ctrl Pts',(35.066390937806,0.286419849779324,3.20999707665792));
#74556=CARTESIAN_POINT('Ctrl Pts',(35.0725407860212,0.186885738517858,3.21887825147354));
#74557=CARTESIAN_POINT('Ctrl Pts',(35.0786906342364,0.0869261342653877,
3.22312671159877));
#74558=CARTESIAN_POINT('Ctrl Pts',(35.0848404824516,-0.0129949696231923,
3.22272380033792));
#74559=CARTESIAN_POINT('Ctrl Pts',(35.0909912908308,-0.11293167400092,3.22232082617132));
#74560=CARTESIAN_POINT('Ctrl Pts',(35.0971420992099,-0.21282943166276,3.2172650399304));
#74561=CARTESIAN_POINT('Ctrl Pts',(35.1032929075891,-0.312225272783111,
3.20758989609575));
#74562=CARTESIAN_POINT('Ctrl Pts',(35.1094502939552,-0.41172741286698,3.19790440517061));
#74563=CARTESIAN_POINT('Ctrl Pts',(35.1156076803214,-0.510726131350203,
3.18358973379608));
#74564=CARTESIAN_POINT('Ctrl Pts',(35.1217650666876,-0.608764718986963,
3.16473112276805));
#74565=CARTESIAN_POINT('Ctrl Pts',(35.1279258894246,-0.706858020899713,
3.14586198695307));
#74566=CARTESIAN_POINT('Ctrl Pts',(35.1340867121615,-0.803989702561212,
3.12244396304012));
#74567=CARTESIAN_POINT('Ctrl Pts',(35.1402475348985,-0.899716417509094,
3.09461272707339));
#74568=CARTESIAN_POINT('Ctrl Pts',(35.1464186578152,-0.995603176400935,
3.06673496051411));
#74569=CARTESIAN_POINT('Ctrl Pts',(35.1525897807319,-1.09007986543974,3.0344293844264));
#74570=CARTESIAN_POINT('Ctrl Pts',(35.1587609036486,-1.18272124439707,2.99788058810751));
#74571=CARTESIAN_POINT('Ctrl Pts',(35.1634564255942,-1.25321078638775,2.97007111525829));
#74572=CARTESIAN_POINT('Ctrl Pts',(35.1681519475398,-1.32263815591294,2.93980605310689));
#74573=CARTESIAN_POINT('Ctrl Pts',(35.1728474694854,-1.39082599117186,2.9071843121448));
#74574=CARTESIAN_POINT('Ctrl Pts',(35.1790197175782,-1.48045867546171,2.86430314136796));
#74575=CARTESIAN_POINT('Ctrl Pts',(35.1851919656709,-1.56826413242229,2.81719735384842));
#74576=CARTESIAN_POINT('Ctrl Pts',(35.1913642137637,-1.65381672746355,2.76604551561643));
#74577=CARTESIAN_POINT('Ctrl Pts',(35.1975281024163,-1.7392534535725,2.71496295534004));
#74578=CARTESIAN_POINT('Ctrl Pts',(35.203691991069,-1.82244301278988,2.65984545701312));
#74579=CARTESIAN_POINT('Ctrl Pts',(35.2098558797216,-1.90298164997837,2.60091876119682));
#74580=CARTESIAN_POINT('Ctrl Pts',(35.2160132413801,-1.98343500411945,2.54205446335953));
#74581=CARTESIAN_POINT('Ctrl Pts',(35.2221706030387,-2.06124266835014,2.4793892422711));
#74582=CARTESIAN_POINT('Ctrl Pts',(35.2283279646973,-2.13602815962436,2.41319316752551));
#74583=CARTESIAN_POINT('Ctrl Pts',(35.2344808288436,-2.21075902544674,2.34704544427739));
#74584=CARTESIAN_POINT('Ctrl Pts',(35.2406336929899,-2.2824717828834,2.27737228197147));
#74585=CARTESIAN_POINT('Ctrl Pts',(35.2467865571362,-2.35082220201975,2.20448464204017));
#74586=CARTESIAN_POINT('Ctrl Pts',(35.2529370902727,-2.41914672663102,2.13162461555799));
#74587=CARTESIAN_POINT('Ctrl Pts',(35.2590876234092,-2.48411114721659,2.05555284772074));
#74588=CARTESIAN_POINT('Ctrl Pts',(35.2652381565458,-2.54540800974684,1.97661721798042));
#74589=CARTESIAN_POINT('Ctrl Pts',(35.271388004761,-2.60669804627883,1.89769037848562));
#74590=CARTESIAN_POINT('Ctrl Pts',(35.2775378529762,-2.66432107033355,1.81590065422547));
#74591=CARTESIAN_POINT('Ctrl Pts',(35.2836877011914,-2.71801050177438,1.73162827267985));
#74592=CARTESIAN_POINT('Ctrl Pts',(35.2898385095706,-2.7717083156425,1.64734273384997));
#74593=CARTESIAN_POINT('Ctrl Pts',(35.2959893179497,-2.82147108362984,1.56057413421501));
#74594=CARTESIAN_POINT('Ctrl Pts',(35.3021401263288,-2.86707661541854,1.47173001729943));
#74595=CARTESIAN_POINT('Ctrl Pts',(35.308297512695,-2.91273092008052,1.38279088597034));
#74596=CARTESIAN_POINT('Ctrl Pts',(35.3144548990612,-2.95421891166921,1.29177219211118));
#74597=CARTESIAN_POINT('Ctrl Pts',(35.3206122854274,-2.99136534813643,1.19910421418184));
#74598=CARTESIAN_POINT('Ctrl Pts',(35.3267731081644,-3.02853251562831,1.1063845192557));
#74599=CARTESIAN_POINT('Ctrl Pts',(35.3329339309013,-3.06135315998669,1.01201411748536));
#74600=CARTESIAN_POINT('Ctrl Pts',(35.3390947536383,-3.08970169113766,0.916439317293331));
#74601=CARTESIAN_POINT('Ctrl Pts',(35.345265876555,-3.11809761773861,0.820704727141216));
#74602=CARTESIAN_POINT('Ctrl Pts',(35.3514369994717,-3.14200639228661,0.723762138369761));
#74603=CARTESIAN_POINT('Ctrl Pts',(35.3576081223884,-3.16135336119834,0.626069076172855));
#74604=CARTESIAN_POINT('Ctrl Pts',(35.3623036443339,-3.17607420185096,0.551735778381997));
#74605=CARTESIAN_POINT('Ctrl Pts',(35.3669991662794,-3.18815505136534,0.47696822725851));
#74606=CARTESIAN_POINT('Ctrl Pts',(35.3716946882249,-3.1975832127869,0.401969103045743));
#74607=CARTESIAN_POINT('Ctrl Pts',(35.3799876085743,-3.21423460801356,0.269510609487901));
#74608=CARTESIAN_POINT('Ctrl Pts',(35.3882805289237,-3.2226579044307,0.135996438299877));
#74609=CARTESIAN_POINT('Ctrl Pts',(35.3965734492731,-3.22274924894167,0.00220021497454528));
#74610=CARTESIAN_POINT('',(35.1510759787713,-3.2227488984055,-0.00266464371426724));
#74611=CARTESIAN_POINT('Ctrl Pts',(34.7184445309107,1.78943583648354,2.68030538364725));
#74612=CARTESIAN_POINT('Ctrl Pts',(34.7284778164623,1.6631436028897,2.7646210926113));
#74613=CARTESIAN_POINT('Ctrl Pts',(34.7387622824405,1.53094595801515,2.83997492085281));
#74614=CARTESIAN_POINT('Ctrl Pts',(34.7619414468197,1.22213078041361,2.98810412560491));
#74615=CARTESIAN_POINT('Ctrl Pts',(34.7747870808691,1.04347616301321,3.05508516657453));
#74616=CARTESIAN_POINT('Ctrl Pts',(34.7875527957726,0.848617770828407,3.10903575152029));
#74617=CARTESIAN_POINT('Ctrl Pts',(34.7882908352342,0.837284743590831,3.11210695403658));
#74618=CARTESIAN_POINT('Ctrl Pts',(34.7893578671172,0.820797499870536,3.11647834515815));
#74619=CARTESIAN_POINT('Ctrl Pts',(34.789689639538,0.815656613366819,3.11782778576215));
#74620=CARTESIAN_POINT('Ctrl Pts',(34.790273542617,0.806582816664488,3.12018560447348));
#74621=CARTESIAN_POINT('Ctrl Pts',(34.7905259794676,0.802651311122227,3.12119927591796));
#74622=CARTESIAN_POINT('Ctrl Pts',(34.79101149322,0.795072951781387,3.12313796020713));
#74623=CARTESIAN_POINT('Ctrl Pts',(34.7912446315174,0.791426410539952,3.12406401249833));
#74624=CARTESIAN_POINT('Ctrl Pts',(34.7918800931694,0.781466912184462,3.12657470593548));
#74625=CARTESIAN_POINT('Ctrl Pts',(34.7922816817834,0.775150720267577,3.12814662208265));
#74626=CARTESIAN_POINT('Ctrl Pts',(34.7938430515433,0.750509310741564,3.13419993459638));
#74627=CARTESIAN_POINT('Ctrl Pts',(34.7949948929898,0.732149202625317,3.13853963496172));
#74628=CARTESIAN_POINT('Ctrl Pts',(34.8028754721779,0.605377675591414,3.16733107376819));
#74629=CARTESIAN_POINT('Ctrl Pts',(34.8093240711907,0.495790826396426,3.18632470560624));
#74630=CARTESIAN_POINT('Ctrl Pts',(34.8254589396022,0.214336675417558,3.22022907094288));
#74631=CARTESIAN_POINT('Ctrl Pts',(34.8349585888802,0.0418611685172514,
3.22708334719831));
#74632=CARTESIAN_POINT('Ctrl Pts',(34.8552830121383,-0.318953711024702,
3.21247873457031));
#74633=CARTESIAN_POINT('Ctrl Pts',(34.8661175392745,-0.506504546755326,
3.18828939790886));
#74634=CARTESIAN_POINT('Ctrl Pts',(34.8785953490578,-0.708348592382026,
3.14399124136648));
#74635=CARTESIAN_POINT('Ctrl Pts',(34.879681888505,-0.725818446321938,3.14000417468881));
#74636=CARTESIAN_POINT('Ctrl Pts',(34.8813310645041,-0.752169131473583,
3.13375862296668));
#74637=CARTESIAN_POINT('Ctrl Pts',(34.8818902445693,-0.761075264011493,
3.13160756627395));
#74638=CARTESIAN_POINT('Ctrl Pts',(34.8828643525772,-0.776539824538581,
3.12780261695751));
#74639=CARTESIAN_POINT('Ctrl Pts',(34.8832787207512,-0.783102474530881,
3.12616599415625));
#74640=CARTESIAN_POINT('Ctrl Pts',(34.8841442721017,-0.796777818220816,
3.12270981232525));
#74641=CARTESIAN_POINT('Ctrl Pts',(34.8845955719299,-0.803889536606635,
3.12088658478861));
#74642=CARTESIAN_POINT('Ctrl Pts',(34.8856644341053,-0.820688572717468,
3.11651859435406));
#74643=CARTESIAN_POINT('Ctrl Pts',(34.8862826708766,-0.830370337315541,
3.11395295109271));
#74644=CARTESIAN_POINT('Ctrl Pts',(34.8883334632527,-0.862369637508156,
3.10531337151894));
#74645=CARTESIAN_POINT('Ctrl Pts',(34.8897723436963,-0.884633342258211,
3.09904442237034));
#74646=CARTESIAN_POINT('Ctrl Pts',(34.8931786461193,-0.936889090710098,
3.08372142356578));
#74647=CARTESIAN_POINT('Ctrl Pts',(34.8951524302891,-0.966819975411211,
3.07446873626558));
#74648=CARTESIAN_POINT('Ctrl Pts',(34.9022306333465,-1.0728993418802,3.03997368300715));
#74649=CARTESIAN_POINT('Ctrl Pts',(34.9074112900613,-1.14822969579944,3.01232797092583));
#74650=CARTESIAN_POINT('Ctrl Pts',(34.9279205739658,-1.43770784080941,2.89365500312409));
#74651=CARTESIAN_POINT('Ctrl Pts',(34.9438283067615,-1.64276786542543,2.78236157455301));
#74652=CARTESIAN_POINT('Ctrl Pts',(34.9683962912241,-1.94333728080291,2.57434031387165));
#74653=CARTESIAN_POINT('Ctrl Pts',(34.9772017762032,-2.04787128812812,2.4919911341095));
#74654=CARTESIAN_POINT('Ctrl Pts',(34.9862787882194,-2.15506093622227,2.3962357750216));
#74655=CARTESIAN_POINT('Ctrl Pts',(34.9869561011829,-2.16305599863747,2.38902119764158));
#74656=CARTESIAN_POINT('Ctrl Pts',(34.9879623650819,-2.17493151774676,2.37819648916721));
#74657=CARTESIAN_POINT('Ctrl Pts',(34.9882935294953,-2.17883937728659,2.37461673053001));
#74658=CARTESIAN_POINT('Ctrl Pts',(34.9888618403155,-2.18554527553861,2.36844336354522));
#74659=CARTESIAN_POINT('Ctrl Pts',(34.9890993373077,-2.18834755619136,2.36585441044548));
#74660=CARTESIAN_POINT('Ctrl Pts',(34.9895916685124,-2.19415659740547,2.36046843914858));
#74661=CARTESIAN_POINT('Ctrl Pts',(34.9898464379053,-2.19716260816482,2.35767065121706));
#74662=CARTESIAN_POINT('Ctrl Pts',(34.9903536503233,-2.20314691579528,2.35207948481872));
#74663=CARTESIAN_POINT('Ctrl Pts',(34.9906060987866,-2.20612527484871,2.34928616979587));
#74664=CARTESIAN_POINT('Ctrl Pts',(34.9914615306586,-2.21621671301815,2.33978559402886));
#74665=CARTESIAN_POINT('Ctrl Pts',(34.9920624849962,-2.22330466482923,2.33305154640913));
#74666=CARTESIAN_POINT('Ctrl Pts',(34.9973176682873,-2.2852602306074,2.27365068924023));
#74667=CARTESIAN_POINT('Ctrl Pts',(35.0018309455731,-2.33828320461286,2.21908439305163));
#74668=CARTESIAN_POINT('Ctrl Pts',(35.0132013204803,-2.4694762310012,2.07414280623862));
#74669=CARTESIAN_POINT('Ctrl Pts',(35.0199206852879,-2.54464392427288,1.98120475746244));
#74670=CARTESIAN_POINT('Ctrl Pts',(35.0417498132851,-2.772675819174,1.66480899495109));
#74671=CARTESIAN_POINT('Ctrl Pts',(35.056732507421,-2.90258060168324,1.42629876383573));
#74672=CARTESIAN_POINT('Ctrl Pts',(35.0748970024127,-3.01318745895865,1.14363812459064));
#74673=CARTESIAN_POINT('Ctrl Pts',(35.0768870989167,-3.02474093199921,1.11272143610757));
#74674=CARTESIAN_POINT('Ctrl Pts',(35.0796184495736,-3.03982259703606,1.07039177998368));
#74675=CARTESIAN_POINT('Ctrl Pts',(35.0803458859634,-3.04376543881535,1.05912791086658));
#74676=CARTESIAN_POINT('Ctrl Pts',(35.0815008272551,-3.04990835125389,1.04126127572589));
#74677=CARTESIAN_POINT('Ctrl Pts',(35.0819269576981,-3.05214977867479,1.03467276116999));
#74678=CARTESIAN_POINT('Ctrl Pts',(35.0827976850688,-3.05667857196086,1.0212179240933));
#74679=CARTESIAN_POINT('Ctrl Pts',(35.0832423371441,-3.05896418299751,1.01435105685925));
#74680=CARTESIAN_POINT('Ctrl Pts',(35.0842629349958,-3.064148168375,0.998599470976569));
#74681=CARTESIAN_POINT('Ctrl Pts',(35.0848393881054,-3.0670310549673,0.989709758519929));
#74682=CARTESIAN_POINT('Ctrl Pts',(35.0866231039322,-3.07581218487464,0.962225295630317));
#74683=CARTESIAN_POINT('Ctrl Pts',(35.0878346349083,-3.08158020615633,0.943589700153594));
#74684=CARTESIAN_POINT('Ctrl Pts',(35.1038102468562,-3.15506376297686,0.698313372654338));
#74685=CARTESIAN_POINT('Ctrl Pts',(35.1194225230371,-3.19778273799733,0.464985913026927));
#74686=CARTESIAN_POINT('Ctrl Pts',(35.1406054601478,-3.22009290535345,0.151989361175707));
#74687=CARTESIAN_POINT('Ctrl Pts',(35.145849298648,-3.22281284297365,0.0746730076407296));
#74688=CARTESIAN_POINT('Ctrl Pts',(35.1510759787713,-3.2227488984055,-0.00266464371426724));
#74689=CARTESIAN_POINT('Ctrl Pts',(35.1510761725173,-3.22274889603389,-0.00266751051583289));
#74690=CARTESIAN_POINT('Ctrl Pts',(35.1619186355403,-3.22261610378722,-0.163100267507248));
#74691=CARTESIAN_POINT('Ctrl Pts',(35.1726751749668,-3.21050356731146,-0.323323489996479));
#74692=CARTESIAN_POINT('Ctrl Pts',(35.1836396978217,-3.18469468457042,-0.493946725074042));
#74693=CARTESIAN_POINT('Ctrl Pts',(35.1844042266867,-3.18282006570918,-0.505885402975079));
#74694=CARTESIAN_POINT('Ctrl Pts',(35.185590766742,-3.17979244483891,-0.524483786703438));
#74695=CARTESIAN_POINT('Ctrl Pts',(35.1860152095985,-3.17868559656821,-0.53115074588874));
#74696=CARTESIAN_POINT('Ctrl Pts',(35.1867253485776,-3.17679349744505,-0.542329799525009));
#74697=CARTESIAN_POINT('Ctrl Pts',(35.1870116660491,-3.17601959156579,-0.54684375416133));
#74698=CARTESIAN_POINT('Ctrl Pts',(35.1875738124882,-3.1744783170012,-0.555719888449237));
#74699=CARTESIAN_POINT('Ctrl Pts',(35.187849675962,-3.17371157297722,-0.56008216508376));
#74700=CARTESIAN_POINT('Ctrl Pts',(35.1883779254982,-3.1722233160601,-0.568448190912915));
#74701=CARTESIAN_POINT('Ctrl Pts',(35.1886303878206,-3.17150321685426,-0.572452145013885));
#74702=CARTESIAN_POINT('Ctrl Pts',(35.1892148988959,-3.16981555422855,-0.581735092873558));
#74703=CARTESIAN_POINT('Ctrl Pts',(35.1895466268871,-3.16884237758759,-0.587013077455503));
#74704=CARTESIAN_POINT('Ctrl Pts',(35.1906191997119,-3.16564608459058,-0.60410845141004));
#74705=CARTESIAN_POINT('Ctrl Pts',(35.1913570782785,-3.16336998101465,-0.615916007076254));
#74706=CARTESIAN_POINT('Ctrl Pts',(35.2017150564923,-3.13033552276273,-0.782271034266164));
#74707=CARTESIAN_POINT('Ctrl Pts',(35.2107296928083,-3.08834382341957,-0.934395614647729));
#74708=CARTESIAN_POINT('Ctrl Pts',(35.2229259068031,-3.01555139663591,-1.13844214108711));
#74709=CARTESIAN_POINT('Ctrl Pts',(35.2262256114441,-2.99419755406352,-1.19347472122739));
#74710=CARTESIAN_POINT('Ctrl Pts',(35.2324329478645,-2.95118760173036,-1.29588545677335));
#74711=CARTESIAN_POINT('Ctrl Pts',(35.2353399305116,-2.92987106400019,-1.34338485903844));
#74712=CARTESIAN_POINT('Ctrl Pts',(35.2452770916432,-2.85338841379238,-1.5033209881666));
#74713=CARTESIAN_POINT('Ctrl Pts',(35.2523552413528,-2.79282754015025,-1.61304385644462));
#74714=CARTESIAN_POINT('Ctrl Pts',(35.2644373740046,-2.68185930772172,-1.78902469339391));
#74715=CARTESIAN_POINT('Ctrl Pts',(35.2693265013199,-2.63499651587901,-1.85735573684857));
#74716=CARTESIAN_POINT('Ctrl Pts',(35.275714643997,-2.571695293704,-1.94243148472485));
#74717=CARTESIAN_POINT('Ctrl Pts',(35.2771210796786,-2.55763327006465,-1.96091018890047));
#74718=CARTESIAN_POINT('Ctrl Pts',(35.27914641218,-2.53721197019249,-1.98715213852997));
#74719=CARTESIAN_POINT('Ctrl Pts',(35.2797589075699,-2.53101399694575,-1.9950404374439));
#74720=CARTESIAN_POINT('Ctrl Pts',(35.2808223726937,-2.52021479204133,-2.00865350598104));
#74721=CARTESIAN_POINT('Ctrl Pts',(35.2812726573704,-2.51563061000929,-2.01439175377605));
#74722=CARTESIAN_POINT('Ctrl Pts',(35.2821389115726,-2.50678949345152,-2.02538137053575));
#74723=CARTESIAN_POINT('Ctrl Pts',(35.2825547582483,-2.50253556835076,-2.03063511951808));
#74724=CARTESIAN_POINT('Ctrl Pts',(35.2835349216485,-2.49248629412709,-2.04296679345692));
#74725=CARTESIAN_POINT('Ctrl Pts',(35.2840997906074,-2.48667729879733,-2.05003347642359));
#74726=CARTESIAN_POINT('Ctrl Pts',(35.2857713058927,-2.4694366033465,-2.07082580176271));
#74727=CARTESIAN_POINT('Ctrl Pts',(35.2868813787977,-2.45792092855606,-2.08448106910328));
#74728=CARTESIAN_POINT('Ctrl Pts',(35.2993592257815,-2.32775899610887,-2.23624853271456));
#74729=CARTESIAN_POINT('Ctrl Pts',(35.3112142879728,-2.19774735677507,-2.36413955524367));
#74730=CARTESIAN_POINT('Ctrl Pts',(35.3302774196647,-1.97829108725116,-2.54619632976771));
#74731=CARTESIAN_POINT('Ctrl Pts',(35.3372550672089,-1.89581365979886,-2.6081872249002));
#74732=CARTESIAN_POINT('Ctrl Pts',(35.3539780663021,-1.69142004017044,-2.74698714086701));
#74733=CARTESIAN_POINT('Ctrl Pts',(35.3637106042693,-1.5670374361554,-2.81979421102691));
#74734=CARTESIAN_POINT('Ctrl Pts',(35.3755913348369,-1.4042216184317,-2.90098612572683));
#74735=CARTESIAN_POINT('Ctrl Pts',(35.3780460684144,-1.36994889415371,-2.91732739926484));
#74736=CARTESIAN_POINT('Ctrl Pts',(35.3819399525753,-1.31442912741162,-2.942605012417));
#74737=CARTESIAN_POINT('Ctrl Pts',(35.3833987176301,-1.29336194231337,-2.95192532907449));
#74738=CARTESIAN_POINT('Ctrl Pts',(35.3852833763351,-1.26576731740669,-2.96378130377405));
#74739=CARTESIAN_POINT('Ctrl Pts',(35.3857212183762,-1.25932965607741,-2.96652243172272));
#74740=CARTESIAN_POINT('Ctrl Pts',(35.386394066545,-1.24939423049461,-2.97071472179452));
#74741=CARTESIAN_POINT('Ctrl Pts',(35.386629965975,-1.24590280008205,-2.97218070018979));
#74742=CARTESIAN_POINT('Ctrl Pts',(35.3871157713353,-1.23869574655169,-2.97519185989066));
#74743=CARTESIAN_POINT('Ctrl Pts',(35.3873656214303,-1.23497985548337,-2.97673621815444));
#74744=CARTESIAN_POINT('Ctrl Pts',(35.3879317586139,-1.22653899885447,-2.98022578928774));
#74745=CARTESIAN_POINT('Ctrl Pts',(35.388247783352,-1.22181230584003,-2.98216672253603));
#74746=CARTESIAN_POINT('Ctrl Pts',(35.3891831544763,-1.20777877409992,-2.98789037958972));
#74747=CARTESIAN_POINT('Ctrl Pts',(35.3898005768387,-1.19845873694612,-2.9916408791332));
#74748=CARTESIAN_POINT('Ctrl Pts',(35.3941468799826,-1.13246377650996,-3.01784017551127));
#74749=CARTESIAN_POINT('Ctrl Pts',(35.3977864750939,-1.0751752243457,-3.03872224836789));
#74750=CARTESIAN_POINT('Ctrl Pts',(35.4022265879943,-1.00334178480227,-3.06261979052757));
#74751=CARTESIAN_POINT('Ctrl Pts',(35.4030870938265,-0.989327105896628,
-3.0671756728886));
#74752=CARTESIAN_POINT('Ctrl Pts',(35.4065544973521,-0.932506101081867,
-3.08521703111218));
#74753=CARTESIAN_POINT('Ctrl Pts',(35.4091329354071,-0.889450192956968,
-3.09790419263125));
#74754=CARTESIAN_POINT('Ctrl Pts',(35.4260760431206,-0.602516370728571,
-3.17597849379441));
#74755=CARTESIAN_POINT('Ctrl Pts',(35.4398053805642,-0.351946954142931,
-3.21341035213004));
#74756=CARTESIAN_POINT('Ctrl Pts',(35.4609886234768,0.0159826061019054,
-3.22478327776359));
#74757=CARTESIAN_POINT('Ctrl Pts',(35.4677803679812,0.131631623585466,-3.22213458006225));
#74758=CARTESIAN_POINT('Ctrl Pts',(35.4758258847611,0.264234804030499,-3.21194652834045));
#74759=CARTESIAN_POINT('Ctrl Pts',(35.4768831839327,0.281578333453512,-3.2104725752219));
#74760=CARTESIAN_POINT('Ctrl Pts',(35.4784892248803,0.307793913794964,-3.20803056394151));
#74761=CARTESIAN_POINT('Ctrl Pts',(35.4790347043618,0.316675468334443,-3.20716601344246));
#74762=CARTESIAN_POINT('Ctrl Pts',(35.4800179034934,0.332643161557032,-3.20554470795251));
#74763=CARTESIAN_POINT('Ctrl Pts',(35.4804551989288,0.339730622306593,-3.20480131218513));
#74764=CARTESIAN_POINT('Ctrl Pts',(35.481395504283,0.354939228024015,-3.20315508130235));
#74765=CARTESIAN_POINT('Ctrl Pts',(35.4818987447456,0.363059507725923,-3.20224485671336));
#74766=CARTESIAN_POINT('Ctrl Pts',(35.4832613080726,0.384993352690459,-3.19970173011544));
#74767=CARTESIAN_POINT('Ctrl Pts',(35.4841224755046,0.398799832331221,-3.19801027629641));
#74768=CARTESIAN_POINT('Ctrl Pts',(35.4867809858683,0.441246170580943,-3.19253096495631));
#74769=CARTESIAN_POINT('Ctrl Pts',(35.4885876307851,0.469845772670512,-3.18844742899992));
#74770=CARTESIAN_POINT('Ctrl Pts',(35.507637912639,0.768783809597302,-3.14165489459676));
#74771=CARTESIAN_POINT('Ctrl Pts',(35.5260248103655,1.0326371498629,-3.06506506031414));
#74772=CARTESIAN_POINT('Ctrl Pts',(35.55268024069,1.39392490682922,-2.90818884758759));
#74773=CARTESIAN_POINT('Ctrl Pts',(35.5608028844359,1.50150592627978,-2.85413246914246));
#74774=CARTESIAN_POINT('Ctrl Pts',(35.5719355347804,1.64814583285149,-2.76985853927283));
#74775=CARTESIAN_POINT('Ctrl Pts',(35.5751136288798,1.68991843646663,-2.74457232164209));
#74776=CARTESIAN_POINT('Ctrl Pts',(35.5794232953742,1.74665404528642,-2.70844182810834));
#74777=CARTESIAN_POINT('Ctrl Pts',(35.5805974204871,1.76212064698642,-2.6984047789682));
#74778=CARTESIAN_POINT('Ctrl Pts',(35.5823419444932,1.78512859667937,-2.68319158470917));
#74779=CARTESIAN_POINT('Ctrl Pts',(35.5829183468193,1.79273514110954,-2.67811536447158));
#74780=CARTESIAN_POINT('Ctrl Pts',(35.5839647097358,1.80655389755418,-2.66880817339567));
#74781=CARTESIAN_POINT('Ctrl Pts',(35.5844353381918,1.8127730822346,-2.66458773662323));
#74782=CARTESIAN_POINT('Ctrl Pts',(35.5851838539894,1.82267157812968,-2.65781976558723));
#74783=CARTESIAN_POINT('Ctrl Pts',(35.5854626793158,1.82636039944118,-2.65528628964999));
#74784=CARTESIAN_POINT('Ctrl Pts',(35.5859917611571,1.83336335498208,-2.65045517474856));
#74785=CARTESIAN_POINT('Ctrl Pts',(35.5862421096316,1.83667841470282,-2.64815902579592));
#74786=CARTESIAN_POINT('Ctrl Pts',(35.5868140096072,1.84425451551665,-2.64289043200747));
#74787=CARTESIAN_POINT('Ctrl Pts',(35.5871352774869,1.84851267618509,-2.63991390777859));
#74788=CARTESIAN_POINT('Ctrl Pts',(35.5881232234822,1.86161325689899,-2.63070914817417));
#74789=CARTESIAN_POINT('Ctrl Pts',(35.5887875899389,1.87043164752207,-2.62444660838729));
#74790=CARTESIAN_POINT('Ctrl Pts',(35.5941572573658,1.94175587741265,-2.57325231492583));
#74791=CARTESIAN_POINT('Ctrl Pts',(35.5987195271814,2.00267073561076,-2.52613448806674));
#74792=CARTESIAN_POINT('Ctrl Pts',(35.6047616711685,2.0826110855344,-2.45958913330616));
#74793=CARTESIAN_POINT('Ctrl Pts',(35.6063199416966,2.10315973829833,-2.44204152643267));
#74794=CARTESIAN_POINT('Ctrl Pts',(35.6237749902183,2.33215990364585,-2.24145118054918));
#74795=CARTESIAN_POINT('Ctrl Pts',(35.6387662671737,2.51636259911403,-2.03248790616208));
#74796=CARTESIAN_POINT('Ctrl Pts',(35.658890701615,2.71128307532589,-1.74359181342733));
#74797=CARTESIAN_POINT('Ctrl Pts',(35.6630490833056,2.74907040725976,-1.68338325866498));
#74798=CARTESIAN_POINT('Ctrl Pts',(35.6698653824782,2.80671948699116,-1.58440337404542));
#74799=CARTESIAN_POINT('Ctrl Pts',(35.6724784229749,2.82784047241329,-1.54639138517793));
#74800=CARTESIAN_POINT('Ctrl Pts',(35.6758954238782,2.85416655670975,-1.49666771048175));
#74801=CARTESIAN_POINT('Ctrl Pts',(35.6766741227786,2.8600805708126,-1.48533500939412));
#74802=CARTESIAN_POINT('Ctrl Pts',(35.6779391693011,2.86954939238842,-1.4669241896655));
#74803=CARTESIAN_POINT('Ctrl Pts',(35.6784240439373,2.87314584181258,-1.45986754998023));
#74804=CARTESIAN_POINT('Ctrl Pts',(35.6793541197731,2.87998152516894,-1.44633206588444));
#74805=CARTESIAN_POINT('Ctrl Pts',(35.6797991681869,2.88322500452995,-1.439855410105));
#74806=CARTESIAN_POINT('Ctrl Pts',(35.6808134902275,2.89055477241374,-1.42509508001197));
#74807=CARTESIAN_POINT('Ctrl Pts',(35.6813832404057,2.89462732432263,-1.41680469008169));
#74808=CARTESIAN_POINT('Ctrl Pts',(35.6831574655498,2.90717058841364,-1.39099085410641));
#74809=CARTESIAN_POINT('Ctrl Pts',(35.6843662132921,2.91551811245241,-1.37340834988258));
#74810=CARTESIAN_POINT('Ctrl Pts',(35.7009476070123,3.02732062719227,-1.13230397110782));
#74811=CARTESIAN_POINT('Ctrl Pts',(35.717245886225,3.10495694190771,-0.897762264905472));
#74812=CARTESIAN_POINT('Ctrl Pts',(35.7442841419308,3.18649195883906,-0.506039312820335));
#74813=CARTESIAN_POINT('Ctrl Pts',(35.754758986728,3.20702199870698,-0.353298352941245));
#74814=CARTESIAN_POINT('Ctrl Pts',(35.7687787635256,3.22014467818334,-0.141901427182443));
#74815=CARTESIAN_POINT('Ctrl Pts',(35.772565735669,3.22217404457667,-0.0840418297419472));
#74816=CARTESIAN_POINT('Ctrl Pts',(35.7783016471311,3.22289863767436,0.00523574299113315));
#74817=CARTESIAN_POINT('Ctrl Pts',(35.7802981966691,3.22269474554549,0.0366305350771588));
#74818=CARTESIAN_POINT('Ctrl Pts',(35.7827610966504,3.22186730775691,0.075826090997907));
#74819=CARTESIAN_POINT('Ctrl Pts',(35.7832501753731,3.22167411116111,0.0836329441804956));
#74820=CARTESIAN_POINT('Ctrl Pts',(35.7840224995579,3.22132308875262,0.0959996654043833));
#74821=CARTESIAN_POINT('Ctrl Pts',(35.7843067778593,3.22118395481501,0.100559970901961));
#74822=CARTESIAN_POINT('Ctrl Pts',(35.7848413388266,3.220903572792,0.109151298472018));
#74823=CARTESIAN_POINT('Ctrl Pts',(35.7850917340939,3.22076444303738,0.113182303575542));
#74824=CARTESIAN_POINT('Ctrl Pts',(35.7856641252704,3.22042852499624,0.122412189675962));
#74825=CARTESIAN_POINT('Ctrl Pts',(35.7859858357635,3.22022671562632,0.127610852440287));
#74826=CARTESIAN_POINT('Ctrl Pts',(35.7869764874582,3.2195650855084,0.143652358469452));
#74827=CARTESIAN_POINT('Ctrl Pts',(35.7876430986058,3.21906307787263,0.154493522368231));
#74828=CARTESIAN_POINT('Ctrl Pts',(35.7930796772694,3.21450271169469,0.243269780588717));
#74829=CARTESIAN_POINT('Ctrl Pts',(35.7977026066793,3.20766910592091,0.321043645601942));
#74830=CARTESIAN_POINT('Ctrl Pts',(35.803761805331,3.19476370753438,0.424611395409422));
#74831=CARTESIAN_POINT('Ctrl Pts',(35.8052788302377,3.1911901855223,0.450683083871293));
#74832=CARTESIAN_POINT('Ctrl Pts',(35.8145419605233,3.16728853908643,0.610490690108467));
#74833=CARTESIAN_POINT('Ctrl Pts',(35.8220678377394,3.13887537559548,0.742886507228558));
#74834=CARTESIAN_POINT('Ctrl Pts',(35.8433012124546,3.03596051382057,1.10855066781525));
#74835=CARTESIAN_POINT('Ctrl Pts',(35.8570829529927,2.94312241202374,1.33564526553336));
#74836=CARTESIAN_POINT('Ctrl Pts',(35.8730327844104,2.81610925627517,1.56717194329522));
#74837=CARTESIAN_POINT('Ctrl Pts',(35.8742181785233,2.8065573374075,1.58421435701194));
#74838=CARTESIAN_POINT('Ctrl Pts',(35.8759791993935,2.79220526021841,1.60928393739835));
#74839=CARTESIAN_POINT('Ctrl Pts',(35.8765505298628,2.78752404393566,1.61737896237576));
#74840=CARTESIAN_POINT('Ctrl Pts',(35.8775663575245,2.77915707303021,1.63170337832467));
#74841=CARTESIAN_POINT('Ctrl Pts',(35.8780103397202,2.77548542390749,1.6379409671076));
#74842=CARTESIAN_POINT('Ctrl Pts',(35.8788825942787,2.76824337690093,1.65014986372986));
#74843=CARTESIAN_POINT('Ctrl Pts',(35.8793108059672,2.76467459224511,1.65612208617163));
#74844=CARTESIAN_POINT('Ctrl Pts',(35.8804748286046,2.75493714414894,1.67229813876974));
#74845=CARTESIAN_POINT('Ctrl Pts',(35.881212005277,2.7487311913592,1.68247929100381));
#74846=CARTESIAN_POINT('Ctrl Pts',(35.8839931462954,2.72517237336327,1.72065035759566));
#74847=CARTESIAN_POINT('Ctrl Pts',(35.8860508051543,2.70744779033035,1.74840740401792));
#74848=CARTESIAN_POINT('Ctrl Pts',(35.9052476929829,2.5394394191109,2.0028296290539));
#74849=CARTESIAN_POINT('Ctrl Pts',(35.923510490241,2.36148212710625,2.20984651698626));
#74850=CARTESIAN_POINT('Ctrl Pts',(35.9501514007285,2.0693086690558,2.47364362567509));
#74851=CARTESIAN_POINT('Ctrl Pts',(35.9583776039676,1.97435077787986,2.55007713701945));
#74852=CARTESIAN_POINT('Ctrl Pts',(35.9686858107573,1.84699442295384,2.64120041730075));
#74853=CARTESIAN_POINT('Ctrl Pts',(35.970958031864,1.81837287744804,2.66098631872296));
#74854=CARTESIAN_POINT('Ctrl Pts',(35.9732071344081,1.7894362098569,2.68030513437425));
#74855=CARTESIAN_POINT('Origin',(-1.72497344927317,0.,0.));
#74856=CARTESIAN_POINT('',(37.4669394326166,1.78943621037803,2.68030513402633));
#74857=CARTESIAN_POINT('',(37.2205445093424,1.78943610171058,2.68030520657533));
#74858=CARTESIAN_POINT('',(-1.72497344927317,1.78943621037804,2.68030513402633));
#74859=CARTESIAN_POINT('',(36.6465734492396,-3.22274964508592,0.00151248092928333));
#74860=CARTESIAN_POINT('Ctrl Pts',(36.6465734492731,-3.22274964508618,0.00151248038429142));
#74861=CARTESIAN_POINT('Ctrl Pts',(36.6528250213268,-3.222797401118,-0.100244696904469));
#74862=CARTESIAN_POINT('Ctrl Pts',(36.6590765933804,-3.21802138921175,-0.201988221218814));
#74863=CARTESIAN_POINT('Ctrl Pts',(36.6653281654341,-3.20845189099051,-0.303239221901459));
#74864=CARTESIAN_POINT('Ctrl Pts',(36.6715822484097,-3.19887854921391,-0.404530889693085));
#74865=CARTESIAN_POINT('Ctrl Pts',(36.6778363313853,-3.18450792857277,-0.505329227822775));
#74866=CARTESIAN_POINT('Ctrl Pts',(36.684090414361,-3.1654220506495,-0.605161799655191));
#74867=CARTESIAN_POINT('Ctrl Pts',(36.6903484556982,-3.14632409280857,-0.705057557957362));
#74868=CARTESIAN_POINT('Ctrl Pts',(36.6966064970355,-3.12250501607544,-0.803985927111695));
#74869=CARTESIAN_POINT('Ctrl Pts',(36.7028645383728,-3.0940974981539,-0.901486680111143));
#74870=CARTESIAN_POINT('Ctrl Pts',(36.7091322606066,-3.06564603513406,-0.999138262203995));
#74871=CARTESIAN_POINT('Ctrl Pts',(36.7153999828405,-3.03259207630555,-1.0953574213286));
#74872=CARTESIAN_POINT('Ctrl Pts',(36.7216677050743,-2.99511760116889,-1.18970085217601));
#74873=CARTESIAN_POINT('Ctrl Pts',(36.7279411298304,-2.95760903086611,-1.284130118914));
#74874=CARTESIAN_POINT('Ctrl Pts',(36.7342145545865,-2.91567210274627,-1.3766798814995));
#74875=CARTESIAN_POINT('Ctrl Pts',(36.7404879793427,-2.86953532638981,-1.46693032319225));
#74876=CARTESIAN_POINT('Ctrl Pts',(36.7467724924765,-2.82331700255023,-1.55734028397047));
#74877=CARTESIAN_POINT('Ctrl Pts',(36.7530570056102,-2.7728842156572,-1.64544245211922));
#74878=CARTESIAN_POINT('Ctrl Pts',(36.759341518744,-2.71850948289369,-1.7308448093105));
#74879=CARTESIAN_POINT('Ctrl Pts',(36.7607694189635,-2.70615503455451,-1.75024902439975));
#74880=CARTESIAN_POINT('Ctrl Pts',(36.762197319183,-2.69359725225644,-1.7695139980812));
#74881=CARTESIAN_POINT('Ctrl Pts',(36.7636252194025,-2.68083961826775,-1.78863537469939));
#74882=CARTESIAN_POINT('Ctrl Pts',(36.7697974674953,-2.62569341058482,-1.87128952570457));
#74883=CARTESIAN_POINT('Ctrl Pts',(36.775969715588,-2.56662403811661,-1.95153641178811));
#74884=CARTESIAN_POINT('Ctrl Pts',(36.7821419636808,-2.50386856205166,-2.02897998670991));
#74885=CARTESIAN_POINT('Ctrl Pts',(36.7883058523334,-2.44119807943436,-2.10631867522429));
#74886=CARTESIAN_POINT('Ctrl Pts',(36.7944697409861,-2.37485168704783,-2.1808612644059));
#74887=CARTESIAN_POINT('Ctrl Pts',(36.8006336296387,-2.30511004539246,-2.2522400496241));
#74888=CARTESIAN_POINT('Ctrl Pts',(36.8067909912972,-2.23544225375432,-2.32354325123983));
#74889=CARTESIAN_POINT('Ctrl Pts',(36.8129483529558,-2.16238666245251,-2.39168900038535));
#74890=CARTESIAN_POINT('Ctrl Pts',(36.8191057146143,-2.08626395056914,-2.45634286919714));
#74891=CARTESIAN_POINT('Ctrl Pts',(36.8252585787606,-2.01019684088149,-2.52094951298267));
#74892=CARTESIAN_POINT('Ctrl Pts',(36.831411442907,-1.93106739481383,-2.58206906705413));
#74893=CARTESIAN_POINT('Ctrl Pts',(36.8375643070533,-1.84923220187827,-2.63940482420497));
#74894=CARTESIAN_POINT('Ctrl Pts',(36.8437148401898,-1.76742801216814,-2.69671885973042));
#74895=CARTESIAN_POINT('Ctrl Pts',(36.8498653733263,-1.6829204677553,-2.75025169770129));
#74896=CARTESIAN_POINT('Ctrl Pts',(36.8560159064629,-1.59609749413888,-2.79974826577383));
#74897=CARTESIAN_POINT('Ctrl Pts',(36.8621657546781,-1.50928418910006,-2.84923932192494));
#74898=CARTESIAN_POINT('Ctrl Pts',(36.8683156028933,-1.42015634485385,-2.89469478667634));
#74899=CARTESIAN_POINT('Ctrl Pts',(36.8744654511085,-1.32912811845297,-2.93590463183627));
#74900=CARTESIAN_POINT('Ctrl Pts',(36.8806162594876,-1.23808567999067,-2.97712091100985));
#74901=CARTESIAN_POINT('Ctrl Pts',(36.8867670678668,-1.14514266579525,-3.01409007481787));
#74902=CARTESIAN_POINT('Ctrl Pts',(36.8929178762459,-1.05073398516574,-3.04664990685141));
#74903=CARTESIAN_POINT('Ctrl Pts',(36.8990752626121,-0.956224339095592,
-3.07924456002393));
#74904=CARTESIAN_POINT('Ctrl Pts',(36.9052326489783,-0.860246307979682,
-3.10742032303051));
#74905=CARTESIAN_POINT('Ctrl Pts',(36.9113900353445,-0.763250656020162,
-3.13106467492845));
#74906=CARTESIAN_POINT('Ctrl Pts',(36.9175508580815,-0.666200871835899,
-3.15472222248356));
#74907=CARTESIAN_POINT('Ctrl Pts',(36.9237116808184,-0.568132762157658,
-3.17384323946745));
#74908=CARTESIAN_POINT('Ctrl Pts',(36.9298725035554,-0.469505925725956,
-3.18836662700641));
#74909=CARTESIAN_POINT('Ctrl Pts',(36.9360436264721,-0.370714196684077,
-3.20291429596173));
#74910=CARTESIAN_POINT('Ctrl Pts',(36.9422147493888,-0.271362307421376,
-3.21284893828179));
#74911=CARTESIAN_POINT('Ctrl Pts',(36.9483858723055,-0.171913744599385,
-3.21816146688102));
#74912=CARTESIAN_POINT('Ctrl Pts',(36.953081394251,-0.0962447106994679,
-3.22220369630358));
#74913=CARTESIAN_POINT('Ctrl Pts',(36.9577769161965,-0.0205197875028225,
-3.22357104151303));
#74914=CARTESIAN_POINT('Ctrl Pts',(36.9624724381421,0.0550585900731698,
-3.22227964555517));
#74915=CARTESIAN_POINT('Ctrl Pts',(36.9686446862348,0.154406117836357,-3.22058210983277));
#74916=CARTESIAN_POINT('Ctrl Pts',(36.9748169343276,0.253849928258262,-3.21428274012976));
#74917=CARTESIAN_POINT('Ctrl Pts',(36.9809891824204,0.352928682299329,-3.20336680817393));
#74918=CARTESIAN_POINT('Ctrl Pts',(36.987153071073,0.451873248132202,-3.19246566030945));
#74919=CARTESIAN_POINT('Ctrl Pts',(36.9933169597256,0.550453312332139,-3.17696042484048));
#74920=CARTESIAN_POINT('Ctrl Pts',(36.9994808483783,0.648207802479794,-3.156888374223));
#74921=CARTESIAN_POINT('Ctrl Pts',(37.0056382100368,0.745858779566933,-3.13683757807052));
#74922=CARTESIAN_POINT('Ctrl Pts',(37.0117955716954,0.84268549745669,-3.1122296677612));
#74923=CARTESIAN_POINT('Ctrl Pts',(37.0179529333539,0.938233237985931,-3.08315357282741));
#74924=CARTESIAN_POINT('Ctrl Pts',(37.0241057975002,1.0337111877254,-3.05409871590111));
#74925=CARTESIAN_POINT('Ctrl Pts',(37.0302586616465,1.12791160314956,-3.02058228920045));
#74926=CARTESIAN_POINT('Ctrl Pts',(37.0364115257928,1.22039207991097,-2.98274382637708));
#74927=CARTESIAN_POINT('Ctrl Pts',(37.0425620589294,1.31283752048611,-2.94491969863802));
#74928=CARTESIAN_POINT('Ctrl Pts',(37.0487125920659,1.40356391554019,-2.90277695259075));
#74929=CARTESIAN_POINT('Ctrl Pts',(37.0548631252025,1.49214694065446,-2.85650399439517));
#74930=CARTESIAN_POINT('Ctrl Pts',(37.0610129734177,1.58072010119239,-2.81023618914088));
#74931=CARTESIAN_POINT('Ctrl Pts',(37.0671628216329,1.66714998131957,-2.75983928728214));
#74932=CARTESIAN_POINT('Ctrl Pts',(37.0733126698481,1.7510359644898,-2.70554811702976));
#74933=CARTESIAN_POINT('Ctrl Pts',(37.0794634782272,1.83493504461644,-2.65124847040191));
#74934=CARTESIAN_POINT('Ctrl Pts',(37.0856142866063,1.91628907419751,-2.59305358376017));
#74935=CARTESIAN_POINT('Ctrl Pts',(37.0917650949854,1.9947264354327,-2.53124159461043));
#74936=CARTESIAN_POINT('Ctrl Pts',(37.0979224813516,2.07324768156821,-2.46936350057819));
#74937=CARTESIAN_POINT('Ctrl Pts',(37.1040798677178,2.14884568873491,-2.40386084879743));
#74938=CARTESIAN_POINT('Ctrl Pts',(37.110237254084,2.22118207049317,-2.33505198490733));
#74939=CARTESIAN_POINT('Ctrl Pts',(37.1163980768209,2.29355882240419,-2.26620471953406));
#74940=CARTESIAN_POINT('Ctrl Pts',(37.1225588995579,2.36267002338088,-2.19404788114744));
#74941=CARTESIAN_POINT('Ctrl Pts',(37.1287197222949,2.42821576676111,-2.11893505151828));
#74942=CARTESIAN_POINT('Ctrl Pts',(37.1348908452116,2.49387109500778,-2.04369664196617));
#74943=CARTESIAN_POINT('Ctrl Pts',(37.1410619681282,2.55594878849473,-1.96549270990756));
#74944=CARTESIAN_POINT('Ctrl Pts',(37.1472330910449,2.61419059110094,-1.88470823097351));
#74945=CARTESIAN_POINT('Ctrl Pts',(37.1519286129905,2.65850597194506,-1.82324043997018));
#74946=CARTESIAN_POINT('Ctrl Pts',(37.1566241349361,2.70060143625978,-1.7602792971095));
#74947=CARTESIAN_POINT('Ctrl Pts',(37.1613196568817,2.74038110508653,-1.69600382115864));
#74948=CARTESIAN_POINT('Ctrl Pts',(37.1674919049745,2.79267134840589,-1.61151392026039));
#74949=CARTESIAN_POINT('Ctrl Pts',(37.1736641530672,2.84114254897881,-1.52445476677892));
#74950=CARTESIAN_POINT('Ctrl Pts',(37.17983640116,2.885532866509,-1.43520647949916));
#74951=CARTESIAN_POINT('Ctrl Pts',(37.1860002898126,2.92986306361038,-1.34607906644603));
#74952=CARTESIAN_POINT('Ctrl Pts',(37.1921641784653,2.97012317141227,-1.2547687981058));
#74953=CARTESIAN_POINT('Ctrl Pts',(37.1983280671179,3.00609523725876,-1.1616836863063));
#74954=CARTESIAN_POINT('Ctrl Pts',(37.2044854287765,3.04202921197908,-1.06869714312258));
#74955=CARTESIAN_POINT('Ctrl Pts',(37.210642790435,3.07368401626014,-0.973939895837431));
#74956=CARTESIAN_POINT('Ctrl Pts',(37.2168001520936,3.10088858765053,-0.87784254253181));
#74957=CARTESIAN_POINT('Ctrl Pts',(37.2229530162399,3.12807328804748,-0.781815381468874));
#74958=CARTESIAN_POINT('Ctrl Pts',(37.2291058803862,3.15081410029398,-0.684450477200166));
#74959=CARTESIAN_POINT('Ctrl Pts',(37.2352587445325,3.16898918878107,-0.586195431480566));
#74960=CARTESIAN_POINT('Ctrl Pts',(37.2414092776691,3.1871573916442,-0.487977609640144));
#74961=CARTESIAN_POINT('Ctrl Pts',(37.2475598108056,3.20076322877482,-0.388870743077388));
#74962=CARTESIAN_POINT('Ctrl Pts',(37.2537103439421,3.20973575255615,-0.289333650415608));
#74963=CARTESIAN_POINT('Ctrl Pts',(37.2598601921574,3.2187072771602,-0.18980764217155));
#74964=CARTESIAN_POINT('Ctrl Pts',(37.2660100403726,3.22304647522968,-0.0898519357018265));
#74965=CARTESIAN_POINT('Ctrl Pts',(37.2721598885878,3.2227342688803,0.0100694927657119));
#74966=CARTESIAN_POINT('Ctrl Pts',(37.2783106969669,3.22242201378675,0.110006521772982));
#74967=CARTESIAN_POINT('Ctrl Pts',(37.284461505346,3.21745691318152,0.209908827734067));
#74968=CARTESIAN_POINT('Ctrl Pts',(37.2906123137252,3.20787200126423,0.30931341064534));
#74969=CARTESIAN_POINT('Ctrl Pts',(37.2967697000914,3.19827683875502,0.408824301869322));
#74970=CARTESIAN_POINT('Ctrl Pts',(37.3029270864576,3.18405204071588,0.507835973901786));
#74971=CARTESIAN_POINT('Ctrl Pts',(37.3090844728238,3.16528243332354,0.605891640306602));
#74972=CARTESIAN_POINT('Ctrl Pts',(37.3152452955607,3.14650235081623,0.704002030518734));
#74973=CARTESIAN_POINT('Ctrl Pts',(37.3214061182977,3.12317250916127,0.801154930191059));
#74974=CARTESIAN_POINT('Ctrl Pts',(37.3275669410347,3.09542818189315,0.896906869882096));
#74975=CARTESIAN_POINT('Ctrl Pts',(37.3337380639514,3.0676374693337,0.992818895689989));
#74976=CARTESIAN_POINT('Ctrl Pts',(37.3399091868681,3.03541766905999,1.08732487163034));
#74977=CARTESIAN_POINT('Ctrl Pts',(37.3460803097848,2.99895298427561,1.17999939008645));
#74978=CARTESIAN_POINT('Ctrl Pts',(37.3507758317303,2.97120751072827,1.25051414746174));
#74979=CARTESIAN_POINT('Ctrl Pts',(37.3554713536758,2.94100548468902,1.3199689619039));
#74980=CARTESIAN_POINT('Ctrl Pts',(37.3601668756214,2.90844565560598,1.38818638189787));
#74981=CARTESIAN_POINT('Ctrl Pts',(37.3663388278917,2.86564791909001,1.47785365746173));
#74982=CARTESIAN_POINT('Ctrl Pts',(37.3725107801621,2.81862431437544,1.56569771632256));
#74983=CARTESIAN_POINT('Ctrl Pts',(37.3786827324324,2.76755299425081,1.65129282276444));
#74984=CARTESIAN_POINT('Ctrl Pts',(37.384846680592,2.71654790608681,1.7367769249929));
#74985=CARTESIAN_POINT('Ctrl Pts',(37.3910106287516,2.66150575392245,1.82001750060698));
#74986=CARTESIAN_POINT('Ctrl Pts',(37.3971745769113,2.60265191622203,1.90061057702145));
#74987=CARTESIAN_POINT('Ctrl Pts',(37.4033313459559,2.54386662524833,1.98110978714272));
#74988=CARTESIAN_POINT('Ctrl Pts',(37.4094881150005,2.48127873417071,2.05896728283734));
#74989=CARTESIAN_POINT('Ctrl Pts',(37.4156448840451,2.41515788910051,2.13380644230342));
#74990=CARTESIAN_POINT('Ctrl Pts',(37.4217974226011,2.34908247751702,2.2085941776845));
#74991=CARTESIAN_POINT('Ctrl Pts',(37.427949961157,2.27947922316048,2.28036737424976));
#74992=CARTESIAN_POINT('Ctrl Pts',(37.434102499713,2.20665871918159,2.34878156914599));
#74993=CARTESIAN_POINT('Ctrl Pts',(37.4402531847559,2.13386015309898,2.41717515359008));
#74994=CARTESIAN_POINT('Ctrl Pts',(37.4464038697989,2.05784657591176,2.48221144628947));
#74995=CARTESIAN_POINT('Ctrl Pts',(37.4525545548418,1.97896560744366,2.54358264797021));
#74996=CARTESIAN_POINT('Ctrl Pts',(37.4573495141001,1.91747147672217,2.59142649132029));
#74997=CARTESIAN_POINT('Ctrl Pts',(37.4621444733583,1.85423549402089,2.63704357283874));
#74998=CARTESIAN_POINT('Ctrl Pts',(37.4669394326166,1.78943621037803,2.68030513402633));
#74999=CARTESIAN_POINT('Ctrl Pts',(36.2170783832723,1.78943621037801,2.68030513402635));
#75000=CARTESIAN_POINT('Ctrl Pts',(36.2232805665494,1.70580874151773,2.7361368447749));
#75001=CARTESIAN_POINT('Ctrl Pts',(36.2294827498265,1.61949287711907,2.78809966004317));
#75002=CARTESIAN_POINT('Ctrl Pts',(36.2356849331037,1.53088469535462,2.83593187718411));
#75003=CARTESIAN_POINT('Ctrl Pts',(36.241835971149,1.44300720563696,2.88336965421863));
#75004=CARTESIAN_POINT('Ctrl Pts',(36.2479870091944,1.35287545759231,2.92674450276665));
#75005=CARTESIAN_POINT('Ctrl Pts',(36.2541380472397,1.26090307854026,2.96584574599349));
#75006=CARTESIAN_POINT('Ctrl Pts',(36.260287924438,1.16894805686143,3.00493960988669));
#75007=CARTESIAN_POINT('Ctrl Pts',(36.2664378016363,1.07515349425653,3.03976130157094));
#75008=CARTESIAN_POINT('Ctrl Pts',(36.2725876788347,0.979954194461434,3.07014777156694));
#75009=CARTESIAN_POINT('Ctrl Pts',(36.2787380404257,0.884747396330164,3.10053663494154));
#75010=CARTESIAN_POINT('Ctrl Pts',(36.2848884020167,0.788136055225419,3.12648945097924));
#75011=CARTESIAN_POINT('Ctrl Pts',(36.2910387636077,0.69057040552706,3.14789295839458));
#75012=CARTESIAN_POINT('Ctrl Pts',(36.297279765134,0.591566898226102,3.16961189645539));
#75013=CARTESIAN_POINT('Ctrl Pts',(36.3035207666603,0.491581175418993,3.18664624558934));
#75014=CARTESIAN_POINT('Ctrl Pts',(36.3097617681866,0.391093102908749,3.19893165718763));
#75015=CARTESIAN_POINT('Ctrl Pts',(36.315921497213,0.291913621147141,3.21105708386872));
#75016=CARTESIAN_POINT('Ctrl Pts',(36.3220812262394,0.192245238270418,3.21855655792975));
#75017=CARTESIAN_POINT('Ctrl Pts',(36.3282409552658,0.0925517978440608,
3.22142076221282));
#75018=CARTESIAN_POINT('Ctrl Pts',(36.3345225930421,-0.00911470059073392,
3.22434165268482));
#75019=CARTESIAN_POINT('Ctrl Pts',(36.3408042308183,-0.110806781691359,
3.22244185568611));
#75020=CARTESIAN_POINT('Ctrl Pts',(36.3470858685945,-0.212036920502237,
3.2157670790721));
#75021=CARTESIAN_POINT('Ctrl Pts',(36.3533675063707,-0.313267059313115,
3.2090923024581));
#75022=CARTESIAN_POINT('Ctrl Pts',(36.3596491441469,-0.414034794378422,
3.19764266511839));
#75023=CARTESIAN_POINT('Ctrl Pts',(36.3659307819232,-0.51386405013367,3.18151870974857));
#75024=CARTESIAN_POINT('Ctrl Pts',(36.3721030300159,-0.611954859471789,
3.16567554012869));
#75025=CARTESIAN_POINT('Ctrl Pts',(36.3782752781087,-0.709484931127417,
3.14526381279472));
#75026=CARTESIAN_POINT('Ctrl Pts',(36.3844475262015,-0.805995538434842,
3.12033471834724));
#75027=CARTESIAN_POINT('Ctrl Pts',(36.3906114148541,-0.902375435726782,
3.09543938684471));
#75028=CARTESIAN_POINT('Ctrl Pts',(36.3967753035068,-0.997738196136775,
3.06603895637837));
#75029=CARTESIAN_POINT('Ctrl Pts',(36.4029391921594,-1.09163277011398,3.0322360491415));
#75030=CARTESIAN_POINT('Ctrl Pts',(36.4090965538179,-1.18542791832857,2.99846893609048));
#75031=CARTESIAN_POINT('Ctrl Pts',(36.4152539154765,-1.27775756450784,2.96030876073085));
#75032=CARTESIAN_POINT('Ctrl Pts',(36.421411277135,-1.36818431268288,2.91790836885405));
#75033=CARTESIAN_POINT('Ctrl Pts',(36.4275641412813,-1.45854501058682,2.87553894743051));
#75034=CARTESIAN_POINT('Ctrl Pts',(36.4337170054276,-1.547005181805,2.82893565105665));
#75035=CARTESIAN_POINT('Ctrl Pts',(36.4398698695739,-1.63314683253052,2.7782996573256));
#75036=CARTESIAN_POINT('Ctrl Pts',(36.4460204027105,-1.71925584853101,2.72768284701764));
#75037=CARTESIAN_POINT('Ctrl Pts',(36.452170935847,-1.8030477153014,2.67303659493187));
#75038=CARTESIAN_POINT('Ctrl Pts',(36.4583214689835,-1.8841293015575,2.614607874522));
#75039=CARTESIAN_POINT('Ctrl Pts',(36.4644713171987,-1.96520185859486,2.55618566071519));
#75040=CARTESIAN_POINT('Ctrl Pts',(36.4706211654139,-2.04356438276439,2.49398206997094));
#75041=CARTESIAN_POINT('Ctrl Pts',(36.4767710136291,-2.11885382642875,2.42828664385575));
#75042=CARTESIAN_POINT('Ctrl Pts',(36.4829218220083,-2.19415502488912,2.36258096084006));
#75043=CARTESIAN_POINT('Ctrl Pts',(36.4890726303874,-2.26638186252413,2.29338264521252));
#75044=CARTESIAN_POINT('Ctrl Pts',(36.4952234387666,-2.33520616842251,2.22101997142337));
#75045=CARTESIAN_POINT('Ctrl Pts',(36.5013808251327,-2.40410407853083,2.14857990931386));
#75046=CARTESIAN_POINT('Ctrl Pts',(36.5075382114989,-2.46959189057255,2.07296904665602));
#75047=CARTESIAN_POINT('Ctrl Pts',(36.5136955978651,-2.53138005764479,1.9945507178957));
#75048=CARTESIAN_POINT('Ctrl Pts',(36.5198564206021,-2.5932027080252,1.91608862471373));
#75049=CARTESIAN_POINT('Ctrl Pts',(36.526017243339,-2.65132134887475,1.83481629847544));
#75050=CARTESIAN_POINT('Ctrl Pts',(36.532178066076,-2.70548954330138,1.75112646419008));
#75051=CARTESIAN_POINT('Ctrl Pts',(36.5383491889927,-2.75974830065476,1.66729671022655));
#75052=CARTESIAN_POINT('Ctrl Pts',(36.5445203119094,-2.81004320002142,1.58104175027761));
#75053=CARTESIAN_POINT('Ctrl Pts',(36.5506914348261,-2.85617350514434,1.49277944486502));
#75054=CARTESIAN_POINT('Ctrl Pts',(36.5553869567716,-2.8912734153203,1.42562187927663));
#75055=CARTESIAN_POINT('Ctrl Pts',(36.5600824787172,-2.9239631907279,1.35730268570755));
#75056=CARTESIAN_POINT('Ctrl Pts',(36.5647780006628,-2.95417345259417,1.28801272295263));
#75057=CARTESIAN_POINT('Ctrl Pts',(36.5715942880442,-2.99802839122183,1.18742746230242));
#75058=CARTESIAN_POINT('Ctrl Pts',(36.5784105754256,-3.03678939838922,1.08449244505177));
#75059=CARTESIAN_POINT('Ctrl Pts',(36.585226862807,-3.07022405146555,0.979715181214655));
#75060=CARTESIAN_POINT('Ctrl Pts',(36.5920141814928,-3.10351660984527,0.875383212666901));
#75061=CARTESIAN_POINT('Ctrl Pts',(36.5988015001786,-3.13152785282194,0.769224872399252));
#75062=CARTESIAN_POINT('Ctrl Pts',(36.6055888188644,-3.15407435744704,0.661764693977453));
#75063=CARTESIAN_POINT('Ctrl Pts',(36.6124195905936,-3.17676520688476,0.553616545532031));
#75064=CARTESIAN_POINT('Ctrl Pts',(36.6192503623228,-3.19392090784062,0.444150068994009));
#75065=CARTESIAN_POINT('Ctrl Pts',(36.626081134052,-3.20540400980987,0.333920194649572));
#75066=CARTESIAN_POINT('Ctrl Pts',(36.6329119057812,-3.21688711177912,0.223690320305166));
#75067=CARTESIAN_POINT('Ctrl Pts',(36.6397426775104,-3.22269746450369,0.112697322741449));
#75068=CARTESIAN_POINT('Ctrl Pts',(36.6465734492396,-3.22274964508592,0.00151248092933596));
#75069=CARTESIAN_POINT('Ctrl Pts',(35.9732071344081,1.7894362098569,2.68030513437425));
#75070=CARTESIAN_POINT('Ctrl Pts',(35.9741186123143,1.77770925091503,2.68813433437576));
#75071=CARTESIAN_POINT('Ctrl Pts',(35.9750262904335,1.76593053683883,2.69588682130556));
#75072=CARTESIAN_POINT('Ctrl Pts',(35.977713407941,1.73074853339878,2.71871329221958));
#75073=CARTESIAN_POINT('Ctrl Pts',(35.9794806339119,1.70719996623789,2.7335619348491));
#75074=CARTESIAN_POINT('Ctrl Pts',(35.9816994319375,1.67706897147055,2.75201987975685));
#75075=CARTESIAN_POINT('Ctrl Pts',(35.9821687391261,1.67066319774735,2.75591332156977));
#75076=CARTESIAN_POINT('Ctrl Pts',(35.9829169893021,1.66039664631732,2.7621044010783));
#75077=CARTESIAN_POINT('Ctrl Pts',(35.9831968595434,1.65654459551128,2.76441634874886));
#75078=CARTESIAN_POINT('Ctrl Pts',(35.9837279472292,1.64921170208059,2.76879661912018));
#75079=CARTESIAN_POINT('Ctrl Pts',(35.9839792573544,1.6457318381304,2.7708664120543));
#75080=CARTESIAN_POINT('Ctrl Pts',(35.9845547304197,1.63774067685999,2.77559912091324));
#75081=CARTESIAN_POINT('Ctrl Pts',(35.9848786015888,1.63322678629941,2.77825759606472));
#75082=CARTESIAN_POINT('Ctrl Pts',(35.9857390824225,1.62119064508468,2.78530686227322));
#75083=CARTESIAN_POINT('Ctrl Pts',(35.9862744496421,1.61365697967995,2.78967822172077));
#75084=CARTESIAN_POINT('Ctrl Pts',(35.9899584042047,1.56151310223042,2.819652452902));
#75085=CARTESIAN_POINT('Ctrl Pts',(35.9930433553004,1.51631034154117,2.84421637318373));
#75086=CARTESIAN_POINT('Ctrl Pts',(35.9969485933205,1.45743587726204,2.87440688941287));
#75087=CARTESIAN_POINT('Ctrl Pts',(35.9978135079042,1.44428969406905,2.88103481324579));
#75088=CARTESIAN_POINT('Ctrl Pts',(36.00874552682,1.27685295158687,2.96401747259804));
#75089=CARTESIAN_POINT('Ctrl Pts',(36.0183107427117,1.11671679414589,3.02798725712601));
#75090=CARTESIAN_POINT('Ctrl Pts',(36.0417314686228,0.716370608426992,3.15180566743302));
#75091=CARTESIAN_POINT('Ctrl Pts',(36.0556251678948,0.472954110497661,3.19739850834578));
#75092=CARTESIAN_POINT('Ctrl Pts',(36.071743569953,0.206626242784038,3.21618244905141));
#75093=CARTESIAN_POINT('Ctrl Pts',(36.0729663480509,0.186504645184643,3.21741199391175));
#75094=CARTESIAN_POINT('Ctrl Pts',(36.0747723446459,0.156914524420469,3.2189416117457));
#75095=CARTESIAN_POINT('Ctrl Pts',(36.07535093949,0.147453836660584,3.21938885983645));
#75096=CARTESIAN_POINT('Ctrl Pts',(36.0763750215052,0.130743654033602,3.22010501158632));
#75097=CARTESIAN_POINT('Ctrl Pts',(36.0768199641124,0.123494933816185,3.2203911546066));
#75098=CARTESIAN_POINT('Ctrl Pts',(36.0776905465913,0.109334797373467,3.22090224667221));
#75099=CARTESIAN_POINT('Ctrl Pts',(36.078116113773,0.102423497296265,3.22112943026915));
#75100=CARTESIAN_POINT('Ctrl Pts',(36.0792641296717,0.0838084266371843,
3.22168136132579));
#75101=CARTESIAN_POINT('Ctrl Pts',(36.0799878784939,0.07210361306308,3.22196457296839));
#75102=CARTESIAN_POINT('Ctrl Pts',(36.0826646126157,0.0289299351166631,
3.22277383408107));
#75103=CARTESIAN_POINT('Ctrl Pts',(36.0846300027322,-0.00254377873521497,
3.22290265795043));
#75104=CARTESIAN_POINT('Ctrl Pts',(36.1050154321242,-0.326576889170818,
3.21948256643101));
#75105=CARTESIAN_POINT('Ctrl Pts',(36.124761157141,-0.617302373908438,3.17656804775269));
#75106=CARTESIAN_POINT('Ctrl Pts',(36.1510765088031,-0.991124842285462,
3.06808695714326));
#75107=CARTESIAN_POINT('Ctrl Pts',(36.1575919963022,-1.08282312691447,3.03693627969966));
#75108=CARTESIAN_POINT('Ctrl Pts',(36.1674949724734,-1.22255751294971,2.98233188702151));
#75109=CARTESIAN_POINT('Ctrl Pts',(36.1709684349362,-1.27164646387149,2.96173366495804));
#75110=CARTESIAN_POINT('Ctrl Pts',(36.1762815803382,-1.3471912260389,2.92780949680161));
#75111=CARTESIAN_POINT('Ctrl Pts',(36.1781612735046,-1.37401008024242,2.91531972480208));
#75112=CARTESIAN_POINT('Ctrl Pts',(36.1805001655199,-1.40754799390382,2.89913518104887));
#75113=CARTESIAN_POINT('Ctrl Pts',(36.1809794746948,-1.41442992974098,2.89578385412785));
#75114=CARTESIAN_POINT('Ctrl Pts',(36.1817399068793,-1.42536374128204,2.89041109007756));
#75115=CARTESIAN_POINT('Ctrl Pts',(36.1820220099817,-1.42942335674865,2.88840560385652));
#75116=CARTESIAN_POINT('Ctrl Pts',(36.182554816216,-1.43709748504238,2.8845943746037));
#75117=CARTESIAN_POINT('Ctrl Pts',(36.1828056221963,-1.44071278531366,2.88279041172217));
#75118=CARTESIAN_POINT('Ctrl Pts',(36.1833766784246,-1.44895080290288,2.87866043713634));
#75119=CARTESIAN_POINT('Ctrl Pts',(36.1836966523751,-1.45357130889051,2.87633009100585));
#75120=CARTESIAN_POINT('Ctrl Pts',(36.1846944441557,-1.46799313462403,2.86901283598748));
#75121=CARTESIAN_POINT('Ctrl Pts',(36.1853698443605,-1.47777468214032,2.86398681794658));
#75122=CARTESIAN_POINT('Ctrl Pts',(36.1910752975701,-1.5605470088626,2.82091924096549));
#75123=CARTESIAN_POINT('Ctrl Pts',(36.1959416432411,-1.63208845255928,2.78014068176321));
#75124=CARTESIAN_POINT('Ctrl Pts',(36.2150917285888,-1.91284886304389,2.60552909192817));
#75125=CARTESIAN_POINT('Ctrl Pts',(36.2285735826886,-2.10785151510612,2.45045970750694));
#75126=CARTESIAN_POINT('Ctrl Pts',(36.2513750221016,-2.3912753237818,2.16596448068789));
#75127=CARTESIAN_POINT('Ctrl Pts',(36.2602676108545,-2.49153302444539,2.04984236909523));
#75128=CARTESIAN_POINT('Ctrl Pts',(36.270706176967,-2.59488306678859,1.91130448774902));
#75129=CARTESIAN_POINT('Ctrl Pts',(36.2718972951471,-2.60647772350059,1.89546216678164));
#75130=CARTESIAN_POINT('Ctrl Pts',(36.2736652099258,-2.62339113340421,1.87190392767963));
#75131=CARTESIAN_POINT('Ctrl Pts',(36.2742376608647,-2.62882228363083,1.86426895898914));
#75132=CARTESIAN_POINT('Ctrl Pts',(36.2752547564251,-2.63839121034164,1.85069225101053));
#75133=CARTESIAN_POINT('Ctrl Pts',(36.2756988814986,-2.64254242012419,1.84476002321267));
#75134=CARTESIAN_POINT('Ctrl Pts',(36.2765708572543,-2.65063936271733,1.83310579106032));
#75135=CARTESIAN_POINT('Ctrl Pts',(36.2769986453726,-2.654586647,1.82738490876055));
#75136=CARTESIAN_POINT('Ctrl Pts',(36.2781601109579,-2.66523568974777,1.81184371093194));
#75137=CARTESIAN_POINT('Ctrl Pts',(36.2788951435894,-2.67190161295433,1.80199907862279));
#75138=CARTESIAN_POINT('Ctrl Pts',(36.2816595673455,-2.696696129648,1.76494100805202));
#75139=CARTESIAN_POINT('Ctrl Pts',(36.2837024423475,-2.71446418660161,1.73748980719753));
#75140=CARTESIAN_POINT('Ctrl Pts',(36.3031422435098,-2.8782876996376,1.47573888429936));
#75141=CARTESIAN_POINT('Ctrl Pts',(36.3217015072401,-2.99405455496806,1.22389558357841));
#75142=CARTESIAN_POINT('Ctrl Pts',(36.348437615209,-3.1118041741739,0.846747939731584));
#75143=CARTESIAN_POINT('Ctrl Pts',(36.3564771865748,-3.140975310928,0.731152899988543));
#75144=CARTESIAN_POINT('Ctrl Pts',(36.3674813859943,-3.17285187458381,0.566960714525288));
#75145=CARTESIAN_POINT('Ctrl Pts',(36.3706128447901,-3.18096469716936,0.519516680882692));
#75146=CARTESIAN_POINT('Ctrl Pts',(36.3754587973901,-3.1920421341892,0.444681886771678));
#75147=CARTESIAN_POINT('Ctrl Pts',(36.3772056850026,-3.19572329295198,0.417405944967495));
#75148=CARTESIAN_POINT('Ctrl Pts',(36.379402682816,-3.19995846515099,0.382673660444147));
#75149=CARTESIAN_POINT('Ctrl Pts',(36.3798701138288,-3.20083645387982,0.375258986886533));
#75150=CARTESIAN_POINT('Ctrl Pts',(36.3806160782755,-3.20220069430102,0.363384643795507));
#75151=CARTESIAN_POINT('Ctrl Pts',(36.380895529182,-3.20270340990713,0.358926948953006));
#75152=CARTESIAN_POINT('Ctrl Pts',(36.381426304326,-3.20364235307471,0.350442069681884));
#75153=CARTESIAN_POINT('Ctrl Pts',(36.381677719315,-3.20408029034524,0.346415161029705));
#75154=CARTESIAN_POINT('Ctrl Pts',(36.3822540678485,-3.20506851836765,0.337166025535612));
#75155=CARTESIAN_POINT('Ctrl Pts',(36.3825787065722,-3.20561363823906,0.331943277488954));
#75156=CARTESIAN_POINT('Ctrl Pts',(36.3836057837671,-3.20730155176934,0.315379520007084));
#75157=CARTESIAN_POINT('Ctrl Pts',(36.384305596644,-3.20839696043669,0.304033614835384));
#75158=CARTESIAN_POINT('Ctrl Pts',(36.3909303954768,-3.21824106154852,0.196087170189352));
#75159=CARTESIAN_POINT('Ctrl Pts',(36.3966274657522,-3.22268558048147,0.0991332467784455));
#75160=CARTESIAN_POINT('Ctrl Pts',(36.4161689540792,-3.22290883677749,-0.240760994970365));
#75161=CARTESIAN_POINT('Ctrl Pts',(36.4293750420992,-3.19561283972274,-0.482885890304909));
#75162=CARTESIAN_POINT('Ctrl Pts',(36.4466838645332,-3.12773851163942,-0.779163845548733));
#75163=CARTESIAN_POINT('Ctrl Pts',(36.450192317602,-3.11241845861492,-0.838269228512858));
#75164=CARTESIAN_POINT('Ctrl Pts',(36.4587881355566,-3.07132427767243,-0.980095396770234));
#75165=CARTESIAN_POINT('Ctrl Pts',(36.463918368936,-3.04387670006028,-1.06227699931576));
#75166=CARTESIAN_POINT('Ctrl Pts',(36.4700803365586,-3.00775729576546,-1.15747358376793));
#75167=CARTESIAN_POINT('Ctrl Pts',(36.4710044139286,-3.00225941727521,-1.17166011556708));
#75168=CARTESIAN_POINT('Ctrl Pts',(36.472497995361,-2.99324417153111,-1.19444260767364));
#75169=CARTESIAN_POINT('Ctrl Pts',(36.4730653786993,-2.98978969638818,-1.20306333247977));
#75170=CARTESIAN_POINT('Ctrl Pts',(36.4740779774849,-2.98357199555874,-1.21838757430831));
#75171=CARTESIAN_POINT('Ctrl Pts',(36.4745226980718,-2.98082330790142,-1.22509695110969));
#75172=CARTESIAN_POINT('Ctrl Pts',(36.4754532961702,-2.97503427778503,-1.23909279093215));
#75173=CARTESIAN_POINT('Ctrl Pts',(36.4759393134086,-2.97198975695754,-1.2463774634127));
#75174=CARTESIAN_POINT('Ctrl Pts',(36.4772077062024,-2.96398958325967,-1.26532361923962));
#75175=CARTESIAN_POINT('Ctrl Pts',(36.4779915111077,-2.95899190717012,-1.27696710882121));
#75176=CARTESIAN_POINT('Ctrl Pts',(36.4814103401889,-2.93696042318549,-1.32747179849471));
#75177=CARTESIAN_POINT('Ctrl Pts',(36.4840691744175,-2.91922938776033,-1.36602247690401));
#75178=CARTESIAN_POINT('Ctrl Pts',(36.4911051830736,-2.87078292973119,-1.46610058839102));
#75179=CARTESIAN_POINT('Ctrl Pts',(36.4955231519047,-2.83885165664463,-1.52701202041522));
#75180=CARTESIAN_POINT('Ctrl Pts',(36.5104689705668,-2.72586286112991,-1.72673661569493));
#75181=CARTESIAN_POINT('Ctrl Pts',(36.5212580308052,-2.63638182239187,-1.86049154480157));
#75182=CARTESIAN_POINT('Ctrl Pts',(36.5403038706459,-2.46279362454057,-2.08215557903536));
#75183=CARTESIAN_POINT('Ctrl Pts',(36.5485062104486,-2.38298239156801,-2.17304412523397));
#75184=CARTESIAN_POINT('Ctrl Pts',(36.5583654369076,-2.2792765405919,-2.27854092800775));
#75185=CARTESIAN_POINT('Ctrl Pts',(36.5601615420715,-2.2600573257729,-2.29760554892307));
#75186=CARTESIAN_POINT('Ctrl Pts',(36.5635008379472,-2.2236744754282,-2.33279743531597));
#75187=CARTESIAN_POINT('Ctrl Pts',(36.5650464290956,-2.20656983617779,-2.34898311153141));
#75188=CARTESIAN_POINT('Ctrl Pts',(36.5701131039918,-2.14957312713693,-2.4017456092113));
#75189=CARTESIAN_POINT('Ctrl Pts',(36.5735931962215,-2.10893459104393,-2.43750739995751));
#75190=CARTESIAN_POINT('Ctrl Pts',(36.5775601725571,-2.06062544531364,-2.47790609138502));
#75191=CARTESIAN_POINT('Ctrl Pts',(36.5781155445077,-2.05381567615525,-2.4835533004731));
#75192=CARTESIAN_POINT('Ctrl Pts',(36.5789991226391,-2.04290550799125,-2.49252532837804));
#75193=CARTESIAN_POINT('Ctrl Pts',(36.5793286075796,-2.03882010328936,-2.49586818853822));
#75194=CARTESIAN_POINT('Ctrl Pts',(36.5799098819954,-2.03158215701297,-2.50176096816193));
#75195=CARTESIAN_POINT('Ctrl Pts',(36.5801619686742,-2.02843299594842,-2.50431499300444));
#75196=CARTESIAN_POINT('Ctrl Pts',(36.5806911484843,-2.02180064737811,-2.50967322579763));
#75197=CARTESIAN_POINT('Ctrl Pts',(36.5809681472508,-2.01831645036655,-2.51247612223156));
#75198=CARTESIAN_POINT('Ctrl Pts',(36.581702317734,-2.00904894645256,-2.51989973814567));
#75199=CARTESIAN_POINT('Ctrl Pts',(36.5821585858103,-2.00325549195663,-2.52450783243841));
#75200=CARTESIAN_POINT('Ctrl Pts',(36.5842636651153,-1.97637216857509,-2.54573992133799));
#75201=CARTESIAN_POINT('Ctrl Pts',(36.5858957145302,-1.95509017481341,-2.56212045281473));
#75202=CARTESIAN_POINT('Ctrl Pts',(36.6006000762666,-1.75963092139697,-2.70870957509641));
#75203=CARTESIAN_POINT('Ctrl Pts',(36.6126415570292,-1.57287101304347,-2.82126080471715));
#75204=CARTESIAN_POINT('Ctrl Pts',(36.6385496285038,-1.15372929339507,-3.01919566061869));
#75205=CARTESIAN_POINT('Ctrl Pts',(36.6524045964157,-0.920026144731918,
-3.09841289139467));
#75206=CARTESIAN_POINT('Ctrl Pts',(36.6684364760453,-0.660571862011332,
-3.15438448002207));
#75207=CARTESIAN_POINT('Ctrl Pts',(36.6696178495064,-0.641503477908418,
-3.15831757345088));
#75208=CARTESIAN_POINT('Ctrl Pts',(36.6713740264031,-0.613238650201305,
-3.16388102185212));
#75209=CARTESIAN_POINT('Ctrl Pts',(36.6719445680677,-0.604068637852739,
-3.16564461688406));
#75210=CARTESIAN_POINT('Ctrl Pts',(36.6729595043423,-0.587779199927651,
-3.16870407879051));
#75211=CARTESIAN_POINT('Ctrl Pts',(36.673403387158,-0.580662802089373,-3.17001587310287));
#75212=CARTESIAN_POINT('Ctrl Pts',(36.6743363670786,-0.565721861057963,
-3.17271799798426));
#75213=CARTESIAN_POINT('Ctrl Pts',(36.6748256189075,-0.557896481754156,
-3.17410337460058));
#75214=CARTESIAN_POINT('Ctrl Pts',(36.676111693057,-0.537352039781101,-3.17766216675373));
#75215=CARTESIAN_POINT('Ctrl Pts',(36.6769100194652,-0.524625004724335,
-3.17978814660827));
#75216=CARTESIAN_POINT('Ctrl Pts',(36.6804810888713,-0.467813515088797,
-3.18892783010006));
#75217=CARTESIAN_POINT('Ctrl Pts',(36.683280342245,-0.423600684910258,-3.1951013015825));
#75218=CARTESIAN_POINT('Ctrl Pts',(36.6907737645373,-0.30614901441594,-3.20902055904293));
#75219=CARTESIAN_POINT('Ctrl Pts',(36.6955155916123,-0.23275193445757,-3.21517734078655));
#75220=CARTESIAN_POINT('Ctrl Pts',(36.7198306769412,0.139059342776081,-3.23356830881318));
#75221=CARTESIAN_POINT('Ctrl Pts',(36.7405066947731,0.437878540012598,-3.20679320487276));
#75222=CARTESIAN_POINT('Ctrl Pts',(36.7654356679086,0.80552593068938,-3.12145216151649));
#75223=CARTESIAN_POINT('Ctrl Pts',(36.7705575909788,0.881665581068449,-3.10080695499617));
#75224=CARTESIAN_POINT('Ctrl Pts',(36.7762185304869,0.967367511749989,-3.0741561519716));
#75225=CARTESIAN_POINT('Ctrl Pts',(36.7769019718869,0.977741066551706,-3.07087257375926));
#75226=CARTESIAN_POINT('Ctrl Pts',(36.7779080799732,0.993055155222298,-3.06593968378723));
#75227=CARTESIAN_POINT('Ctrl Pts',(36.7782330670231,0.998008507813227,-3.06433087397199));
#75228=CARTESIAN_POINT('Ctrl Pts',(36.7788085185025,1.00679167227465,-3.06145461577495));
#75229=CARTESIAN_POINT('Ctrl Pts',(36.7790592645278,1.01062301867689,-3.06019197937034));
#75230=CARTESIAN_POINT('Ctrl Pts',(36.7795924740823,1.01877939006166,-3.05748702406157));
#75231=CARTESIAN_POINT('Ctrl Pts',(36.7798748178459,1.02310371362859,-3.05604272543634));
#75232=CARTESIAN_POINT('Ctrl Pts',(36.7806384001787,1.03481264310518,-3.05210437373569));
#75233=CARTESIAN_POINT('Ctrl Pts',(36.781118602623,1.04219134777408,-3.04959267970297));
#75234=CARTESIAN_POINT('Ctrl Pts',(36.783514286236,1.07907397612567,-3.03688842042406));
#75235=CARTESIAN_POINT('Ctrl Pts',(36.7854068516727,1.10843904017133,-3.02629393632444));
#75236=CARTESIAN_POINT('Ctrl Pts',(36.7907216554301,1.19136712430015,-2.99500561239376));
#75237=CARTESIAN_POINT('Ctrl Pts',(36.7940937095598,1.24453953762948,-2.97330395112609));
#75238=CARTESIAN_POINT('Ctrl Pts',(36.8062303632827,1.43645302021816,-2.88892561515328));
#75239=CARTESIAN_POINT('Ctrl Pts',(36.8146984536009,1.57129273925118,-2.81785976672978));
#75240=CARTESIAN_POINT('Ctrl Pts',(36.8371070735987,1.91187990190257,-2.60627945583568));
#75241=CARTESIAN_POINT('Ctrl Pts',(36.8511018884129,2.1072127423579,-2.45104231029528));
#75242=CARTESIAN_POINT('Ctrl Pts',(36.8672952836862,2.29645224480173,-2.26115052309472));
#75243=CARTESIAN_POINT('Ctrl Pts',(36.868473517801,2.3100340070721,-2.24727333926551));
#75244=CARTESIAN_POINT('Ctrl Pts',(36.8702198136267,2.32988396084766,-2.22662153160806));
#75245=CARTESIAN_POINT('Ctrl Pts',(36.8707836136004,2.3362499543421,-2.21994118482476));
#75246=CARTESIAN_POINT('Ctrl Pts',(36.8717921224686,2.34756073599831,-2.20796933925305));
#75247=CARTESIAN_POINT('Ctrl Pts',(36.872236350756,2.35251656297532,-2.20268831927018));
#75248=CARTESIAN_POINT('Ctrl Pts',(36.8731682884187,2.36285792177073,-2.19159366810999));
#75249=CARTESIAN_POINT('Ctrl Pts',(36.8736561460994,2.36823988871201,-2.18577679379563));
#75250=CARTESIAN_POINT('Ctrl Pts',(36.8749346018162,2.38226067001499,-2.170510443237));
#75251=CARTESIAN_POINT('Ctrl Pts',(36.8757266715596,2.39086465997479,-2.16102930433224));
#75252=CARTESIAN_POINT('Ctrl Pts',(36.8792313350736,2.42856868390872,-2.11898068880317));
#75253=CARTESIAN_POINT('Ctrl Pts',(36.8819692422436,2.45706030939448,-2.08587615776834));
#75254=CARTESIAN_POINT('Ctrl Pts',(36.8892617740853,2.53039459505167,-1.99708084030475));
#75255=CARTESIAN_POINT('Ctrl Pts',(36.8938609679564,2.57406992716853,-1.9404616563029));
#75256=CARTESIAN_POINT('Ctrl Pts',(36.9169210528835,2.78054479582112,-1.65354584610455));
#75257=CARTESIAN_POINT('Ctrl Pts',(36.9363631304863,2.91450025964948,-1.40402766612287));
#75258=CARTESIAN_POINT('Ctrl Pts',(36.9616399474412,3.04889490221409,-1.04877961788107));
#75259=CARTESIAN_POINT('Ctrl Pts',(36.9680439700766,3.07934484495578,-0.955687336357353));
#75260=CARTESIAN_POINT('Ctrl Pts',(36.9749438467709,3.10856379660807,-0.850340562763089));
#75261=CARTESIAN_POINT('Ctrl Pts',(36.9756614120413,3.11155723581187,-0.839320872941894));
#75262=CARTESIAN_POINT('Ctrl Pts',(36.97670435262,3.11584266434413,-0.823206940842209));
#75263=CARTESIAN_POINT('Ctrl Pts',(36.9770323368395,3.11718082319363,-0.818125230539963));
#75264=CARTESIAN_POINT('Ctrl Pts',(36.9776118939201,3.11952859825246,-0.809120077199282));
#75265=CARTESIAN_POINT('Ctrl Pts',(36.9778637580884,3.12054325234113,-0.805197979152317));
#75266=CARTESIAN_POINT('Ctrl Pts',(36.9783934688462,3.12266536032122,-0.796930809661828));
#75267=CARTESIAN_POINT('Ctrl Pts',(36.9786712174125,3.12377113961956,-0.792585349222883));
#75268=CARTESIAN_POINT('Ctrl Pts',(36.9794095091452,3.12669182348375,-0.78100666845305));
#75269=CARTESIAN_POINT('Ctrl Pts',(36.9798691305563,3.12849071041146,-0.773769379519499));
#75270=CARTESIAN_POINT('Ctrl Pts',(36.9820125721864,3.1367877872471,-0.73988657479942));
#75271=CARTESIAN_POINT('Ctrl Pts',(36.9836788768371,3.1429710245235,-0.713164092144977));
#75272=CARTESIAN_POINT('Ctrl Pts',(36.988209932356,3.15901296840076,-0.639569018783328));
#75273=CARTESIAN_POINT('Ctrl Pts',(36.9910406057058,3.16816944705662,-0.592548998008233));
#75274=CARTESIAN_POINT('Ctrl Pts',(37.0007336137894,3.19629145107302,-0.428755341376519));
#75275=CARTESIAN_POINT('Ctrl Pts',(37.0074020685398,3.20987547092154,-0.311148706877908));
#75276=CARTESIAN_POINT('Ctrl Pts',(37.0295626247875,3.23357570264587,0.0837801909215586));
#75277=CARTESIAN_POINT('Ctrl Pts',(37.044884553195,3.21438708930145,0.361565071211477));
#75278=CARTESIAN_POINT('Ctrl Pts',(37.0619370300203,3.15839107534176,0.640890675631692));
#75279=CARTESIAN_POINT('Ctrl Pts',(37.0623916430659,3.15687463751017,0.648319029873952));
#75280=CARTESIAN_POINT('Ctrl Pts',(37.0644690880412,3.14983780741904,0.682179203614099));
#75281=CARTESIAN_POINT('Ctrl Pts',(37.0661012904997,3.14401169270617,0.708545755175215));
#75282=CARTESIAN_POINT('Ctrl Pts',(37.0684123474123,3.13535080339916,0.745529025225156));
#75283=CARTESIAN_POINT('Ctrl Pts',(37.0690823240132,3.13279190056873,0.756209687104703));
#75284=CARTESIAN_POINT('Ctrl Pts',(37.070168517851,3.12856601318455,0.773458584215435));
#75285=CARTESIAN_POINT('Ctrl Pts',(37.0705836419275,3.12693280558143,0.780035068838096));
#75286=CARTESIAN_POINT('Ctrl Pts',(37.0714493542964,3.12348922551498,0.793716815164936));
#75287=CARTESIAN_POINT('Ctrl Pts',(37.071900054716,3.12167532328016,0.800821140574469));
#75288=CARTESIAN_POINT('Ctrl Pts',(37.0729649536656,3.11733985957578,0.81756284136249));
#75289=CARTESIAN_POINT('Ctrl Pts',(37.0735798128605,3.11479783700592,0.827194796095611));
#75290=CARTESIAN_POINT('Ctrl Pts',(37.0756081157084,3.10628524859561,0.858854101788282));
#75291=CARTESIAN_POINT('Ctrl Pts',(37.0770276947857,3.10012546085512,0.880829437268086));
#75292=CARTESIAN_POINT('Ctrl Pts',(37.0884058372798,3.04916199250557,1.0554842380729));
#75293=CARTESIAN_POINT('Ctrl Pts',(37.0987283662029,2.99334713802395,1.20469712668627));
#75294=CARTESIAN_POINT('Ctrl Pts',(37.1215802222119,2.84957042113543,1.51659379870485));
#75295=CARTESIAN_POINT('Ctrl Pts',(37.1341637674022,2.75816436501057,1.67709019465128));
#75296=CARTESIAN_POINT('Ctrl Pts',(37.1555686746182,2.57747707362098,1.93925200526032));
#75297=CARTESIAN_POINT('Ctrl Pts',(37.1644515391825,2.49458384830556,2.044785266828));
#75298=CARTESIAN_POINT('Ctrl Pts',(37.1735989676574,2.39818285805468,2.15289396878105));
#75299=CARTESIAN_POINT('Ctrl Pts',(37.1742760834683,2.39097759215961,2.16089324654482));
#75300=CARTESIAN_POINT('Ctrl Pts',(37.1752821031806,2.3801662523534,2.17277570195034));
#75301=CARTESIAN_POINT('Ctrl Pts',(37.1756132191062,2.37659055540104,2.17668623663545));
#75302=CARTESIAN_POINT('Ctrl Pts',(37.1761814687019,2.37042392839877,2.18339701288422));
#75303=CARTESIAN_POINT('Ctrl Pts',(37.1764189527889,2.36783765517095,2.18620149009971));
#75304=CARTESIAN_POINT('Ctrl Pts',(37.1769112799696,2.36245699275374,2.19201537055341));
#75305=CARTESIAN_POINT('Ctrl Pts',(37.177166058175,2.35966183218356,2.1950240238465));
#75306=CARTESIAN_POINT('Ctrl Pts',(37.1777728490376,2.35297946720843,2.20218926904811));
#75307=CARTESIAN_POINT('Ctrl Pts',(37.1781244559008,2.34908696505018,2.20634094863468));
#75308=CARTESIAN_POINT('Ctrl Pts',(37.1793085879291,2.33590991201172,2.22032097745005));
#75309=CARTESIAN_POINT('Ctrl Pts',(37.1801372710837,2.32657436194683,2.23010136837593));
#75310=CARTESIAN_POINT('Ctrl Pts',(37.1821077759072,2.3041112438841,2.25334027173706));
#75311=CARTESIAN_POINT('Ctrl Pts',(37.1832454875708,2.29092676943774,2.26674338604494));
#75312=CARTESIAN_POINT('Ctrl Pts',(37.197057997158,2.1283476524747,2.4291509929166));
#75313=CARTESIAN_POINT('Ctrl Pts',(37.2087592672923,1.96482590108901,2.5632107659461));
#75314=CARTESIAN_POINT('Ctrl Pts',(37.2205445093424,1.78943610171065,2.68030520657529));
#75315=CARTESIAN_POINT('Origin',(-1.72497344927317,0.,0.));
#75316=CARTESIAN_POINT('',(38.7168453967856,1.78943621037805,2.68030513402632));
#75317=CARTESIAN_POINT('',(38.470402238185,1.78943621037805,2.68030513402632));
#75318=CARTESIAN_POINT('',(-1.72497344927317,1.78943621037804,2.68030513402633));
#75319=CARTESIAN_POINT('',(37.8965734493324,-3.22274881024213,-0.00276922063369994));
#75320=CARTESIAN_POINT('Ctrl Pts',(37.8965734493324,-3.22274881024213,-0.00276922063374366));
#75321=CARTESIAN_POINT('Ctrl Pts',(37.903965412188,-3.22264570243583,-0.122763473181237));
#75322=CARTESIAN_POINT('Ctrl Pts',(37.9113573750437,-3.2158370897087,-0.242465150599442));
#75323=CARTESIAN_POINT('Ctrl Pts',(37.9187493378993,-3.20244346561688,-0.361211035307264));
#75324=CARTESIAN_POINT('Ctrl Pts',(37.9262403139818,-3.18887043776371,-0.481547487154726));
#75325=CARTESIAN_POINT('Ctrl Pts',(37.9337312900642,-3.16853487915056,-0.600902356567945));
#75326=CARTESIAN_POINT('Ctrl Pts',(37.9412222661466,-3.14161120691717,-0.718607394251148));
#75327=CARTESIAN_POINT('Ctrl Pts',(37.9463843547112,-3.12305789970835,-0.799718830508165));
#75328=CARTESIAN_POINT('Ctrl Pts',(37.9515464432757,-3.10137711637387,-0.880047272850072));
#75329=CARTESIAN_POINT('Ctrl Pts',(37.9567085318403,-3.07663900274975,-0.95938001295578));
#75330=CARTESIAN_POINT('Ctrl Pts',(37.9628807799331,-3.04705993359477,-1.05423722969816));
#75331=CARTESIAN_POINT('Ctrl Pts',(37.9690530280258,-3.01303781465099,-1.14789217570988));
#75332=CARTESIAN_POINT('Ctrl Pts',(37.9752252761186,-2.97468830410308,-1.23989800222935));
#75333=CARTESIAN_POINT('Ctrl Pts',(37.9813891647712,-2.93639073256224,-1.33177921982407));
#75334=CARTESIAN_POINT('Ctrl Pts',(37.9875530534238,-2.89377758413291,-1.42201535984317));
#75335=CARTESIAN_POINT('Ctrl Pts',(37.9937169420765,-2.8470143423638,-1.51017445908571));
#75336=CARTESIAN_POINT('Ctrl Pts',(37.999874303735,-2.80030061858893,-1.59824020590862));
#75337=CARTESIAN_POINT('Ctrl Pts',(38.0060316653936,-2.74944574071772,-1.68423290294603));
#75338=CARTESIAN_POINT('Ctrl Pts',(38.0121890270521,-2.69466297521651,-1.76774121762698));
#75339=CARTESIAN_POINT('Ctrl Pts',(38.0183418911984,-2.6399202246067,-1.85118853545768));
#75340=CARTESIAN_POINT('Ctrl Pts',(38.0244947553447,-2.58125552805605,-1.93215471669091));
#75341=CARTESIAN_POINT('Ctrl Pts',(38.030647619491,-2.51892724787893,-2.01025448199801));
#75342=CARTESIAN_POINT('Ctrl Pts',(38.0367981526276,-2.45662258074225,-2.08832465924473));
#75343=CARTESIAN_POINT('Ctrl Pts',(38.0429486857641,-2.39065735847169,-2.16353023918866));
#75344=CARTESIAN_POINT('Ctrl Pts',(38.0490992189006,-2.32133175534108,-2.2355170417926));
#75345=CARTESIAN_POINT('Ctrl Pts',(38.0552490671158,-2.25201387228662,-2.30749582797009));
#75346=CARTESIAN_POINT('Ctrl Pts',(38.0613989153311,-2.17933665367041,-2.37625623656383));
#75347=CARTESIAN_POINT('Ctrl Pts',(38.0675487635463,-2.10363815089778,-2.44147989805105));
#75348=CARTESIAN_POINT('Ctrl Pts',(38.0736995719254,-2.02792782946396,-2.50671374278271));
#75349=CARTESIAN_POINT('Ctrl Pts',(38.0798503803046,-1.94919561604475,-2.56840946006127));
#75350=CARTESIAN_POINT('Ctrl Pts',(38.0860011886837,-1.86781296363155,-2.62628869231658));
#75351=CARTESIAN_POINT('Ctrl Pts',(38.0921585750499,-1.78634327647428,-2.68422982356409));
#75352=CARTESIAN_POINT('Ctrl Pts',(38.0983159614161,-1.702217844763,-2.73834606712631));
#75353=CARTESIAN_POINT('Ctrl Pts',(38.1044733477823,-1.6158373563824,-2.78840226657115));
#75354=CARTESIAN_POINT('Ctrl Pts',(38.1106341705192,-1.52940865998501,-2.83848640183979));
#75355=CARTESIAN_POINT('Ctrl Pts',(38.1167949932562,-1.44072278615831,-2.88450578047512));
#75356=CARTESIAN_POINT('Ctrl Pts',(38.1229558159932,-1.3502034099302,-2.92627208480566));
#75357=CARTESIAN_POINT('Ctrl Pts',(38.1291269389099,-1.25953269582335,-2.96810821754381));
#75358=CARTESIAN_POINT('Ctrl Pts',(38.1352980618266,-1.16702275890909,-3.00567690916634));
#75359=CARTESIAN_POINT('Ctrl Pts',(38.1414691847433,-1.07311568222778,-3.03883864248446));
#75360=CARTESIAN_POINT('Ctrl Pts',(38.1461647066888,-1.00166308837199,-3.06407094601336));
#75361=CARTESIAN_POINT('Ctrl Pts',(38.1508602286344,-0.929402004252621,
-3.08675286277535));
#75362=CARTESIAN_POINT('Ctrl Pts',(38.1555557505799,-0.856531192177784,
-3.10684275098153));
#75363=CARTESIAN_POINT('Ctrl Pts',(38.1617279986727,-0.760742750325845,
-3.13325084269148));
#75364=CARTESIAN_POINT('Ctrl Pts',(38.1679002467655,-0.66356326681565,-3.15527132121878));
#75365=CARTESIAN_POINT('Ctrl Pts',(38.1740724948582,-0.565431172373414,
-3.17275986355861));
#75366=CARTESIAN_POINT('Ctrl Pts',(38.1802363835109,-0.467431984022516,
-3.19022472013264));
#75367=CARTESIAN_POINT('Ctrl Pts',(38.1864002721635,-0.368483172980994,
-3.20316976466903));
#75368=CARTESIAN_POINT('Ctrl Pts',(38.1925641608161,-0.269037589193264,
-3.21150063647839));
#75369=CARTESIAN_POINT('Ctrl Pts',(38.1987215224747,-0.169697309179329,
-3.21982268665679));
#75370=CARTESIAN_POINT('Ctrl Pts',(38.2048788841332,-0.0698617327023847,
-3.22354024184912));
#75371=CARTESIAN_POINT('Ctrl Pts',(38.2110362457918,0.030007808250163,-3.22261029197513));
#75372=CARTESIAN_POINT('Ctrl Pts',(38.2171891099381,0.1298044016469,-3.221681021363));
#75373=CARTESIAN_POINT('Ctrl Pts',(38.2233419740844,0.229634477148471,-3.21611099890156));
#75374=CARTESIAN_POINT('Ctrl Pts',(38.2294948382307,0.329034235200374,-3.20590923679478));
#75375=CARTESIAN_POINT('Ctrl Pts',(38.2356453713673,0.428396335699355,-3.19571133962092));
#75376=CARTESIAN_POINT('Ctrl Pts',(38.2417959045038,0.527328011053883,-3.18088523374493));
#75377=CARTESIAN_POINT('Ctrl Pts',(38.2479464376403,0.62536901455604,-3.16149191966913));
#75378=CARTESIAN_POINT('Ctrl Pts',(38.2540962858555,0.723399100244558,-3.14210076522636));
#75379=CARTESIAN_POINT('Ctrl Pts',(38.2602461340708,0.820538285155734,-3.11814349805032));
#75380=CARTESIAN_POINT('Ctrl Pts',(38.266395982286,0.916335966152786,-3.08973234433581));
#75381=CARTESIAN_POINT('Ctrl Pts',(38.2725467906651,1.01214860385687,-3.0613167548427));
#75382=CARTESIAN_POINT('Ctrl Pts',(38.2786975990443,1.10661890514633,-3.02844602113245));
#75383=CARTESIAN_POINT('Ctrl Pts',(38.2848484074234,1.199311864716,-2.99128210198427));
#75384=CARTESIAN_POINT('Ctrl Pts',(38.2910057937896,1.29210395484706,-2.95407843785237));
#75385=CARTESIAN_POINT('Ctrl Pts',(38.2971631801558,1.38311450363477,-2.91257258179275));
#75386=CARTESIAN_POINT('Ctrl Pts',(38.303320566522,1.47192903935023,-2.86697444453513));
#75387=CARTESIAN_POINT('Ctrl Pts',(38.3094813892589,1.56079314149801,-2.82135085945001));
#75388=CARTESIAN_POINT('Ctrl Pts',(38.3156422119959,1.64745841307979,-2.77163066105908));
#75389=CARTESIAN_POINT('Ctrl Pts',(38.3218030347328,1.73153735416595,-2.71806842327929));
#75390=CARTESIAN_POINT('Ctrl Pts',(38.3279741576495,1.81575686547165,-2.66441663566187));
#75391=CARTESIAN_POINT('Ctrl Pts',(38.3341452805662,1.89738105387448,-2.60691022831736));
#75392=CARTESIAN_POINT('Ctrl Pts',(38.3403164034829,1.97605351744507,-2.54584564706758));
#75393=CARTESIAN_POINT('Ctrl Pts',(38.3450119254285,2.03591430521375,-2.4993824530544));
#75394=CARTESIAN_POINT('Ctrl Pts',(38.3497074473741,2.09406684386339,-2.45086012958568));
#75395=CARTESIAN_POINT('Ctrl Pts',(38.3544029693197,2.15036863113482,-2.40042336114515));
#75396=CARTESIAN_POINT('Ctrl Pts',(38.3605752174125,2.2243771445932,-2.33412439557355));
#75397=CARTESIAN_POINT('Ctrl Pts',(38.3667474655052,2.29544690919835,-2.26428284598557));
#75398=CARTESIAN_POINT('Ctrl Pts',(38.372919713598,2.36321945516923,-2.19118948728987));
#75399=CARTESIAN_POINT('Ctrl Pts',(38.3790836022506,2.43090021277835,-2.11819512324686));
#75400=CARTESIAN_POINT('Ctrl Pts',(38.3852474909033,2.49529233492339,-2.0419580194834));
#75401=CARTESIAN_POINT('Ctrl Pts',(38.3914113795559,2.55607158394951,-1.96280809561858));
#75402=CARTESIAN_POINT('Ctrl Pts',(38.3975687412144,2.61678647331225,-1.88374198428087));
#75403=CARTESIAN_POINT('Ctrl Pts',(38.403726102873,2.67389583231662,-1.80176952755802));
#75404=CARTESIAN_POINT('Ctrl Pts',(38.4098834645315,2.72711403357044,-1.71725554603943));
#75405=CARTESIAN_POINT('Ctrl Pts',(38.4160363286778,2.78029336273509,-1.63280329593881));
#75406=CARTESIAN_POINT('Ctrl Pts',(38.4221891928241,2.82958695419273,-1.54581357835062));
#75407=CARTESIAN_POINT('Ctrl Pts',(38.4283420569704,2.87475160792161,-1.45668141858544));
#75408=CARTESIAN_POINT('Ctrl Pts',(38.434492590107,2.91989915104207,-1.36758302649827));
#75409=CARTESIAN_POINT('Ctrl Pts',(38.4406431232435,2.960920668463,-1.27634419204506));
#75410=CARTESIAN_POINT('Ctrl Pts',(38.44679365638,2.9976186142432,-1.18338506245544));
#75411=CARTESIAN_POINT('Ctrl Pts',(38.4529435045952,3.03431247335233,-1.09043628476366));
#75412=CARTESIAN_POINT('Ctrl Pts',(38.4590933528104,3.06668355855487,-0.99576799683915));
#75413=CARTESIAN_POINT('Ctrl Pts',(38.4652432010256,3.0945826297964,-0.899819931909951));
#75414=CARTESIAN_POINT('Ctrl Pts',(38.4713940094048,3.12248605686606,-0.803856886794599));
#75415=CARTESIAN_POINT('Ctrl Pts',(38.4775448177839,3.14591596186266,-0.706614084941657));
#75416=CARTESIAN_POINT('Ctrl Pts',(38.483695626163,3.1647733741324,-0.608545029461781));
#75417=CARTESIAN_POINT('Ctrl Pts',(38.4898530125292,3.18365095347711,-0.510371093950314));
#75418=CARTESIAN_POINT('Ctrl Pts',(38.4960103988954,3.19794619297597,-0.411369567671443));
#75419=CARTESIAN_POINT('Ctrl Pts',(38.5021677852616,3.20761156229836,-0.312002608819048));
#75420=CARTESIAN_POINT('Ctrl Pts',(38.5083286079985,3.21728232575888,-0.212580194341048));
#75421=CARTESIAN_POINT('Ctrl Pts',(38.5144894307355,3.22231805138747,-0.112792374975328));
#75422=CARTESIAN_POINT('Ctrl Pts',(38.5206502534724,3.22272336385277,-0.0131027698404472));
#75423=CARTESIAN_POINT('Ctrl Pts',(38.5268213763891,3.22312935395341,0.0867535047302972));
#75424=CARTESIAN_POINT('Ctrl Pts',(38.5329924993058,3.21888948591141,0.186510802894764));
#75425=CARTESIAN_POINT('Ctrl Pts',(38.5391636222225,3.21006042242216,0.285709024881714));
#75426=CARTESIAN_POINT('Ctrl Pts',(38.5438591441681,3.20334251031245,0.361187577908209));
#75427=CARTESIAN_POINT('Ctrl Pts',(38.5485546661136,3.19396877235967,0.436342528928671));
#75428=CARTESIAN_POINT('Ctrl Pts',(38.5532501880592,3.18198386601061,0.510975771390588));
#75429=CARTESIAN_POINT('Ctrl Pts',(38.5594232188451,3.16622774843368,0.609093362728268));
#75430=CARTESIAN_POINT('Ctrl Pts',(38.565596249631,3.14590140604225,0.706654222548105));
#75431=CARTESIAN_POINT('Ctrl Pts',(38.571769280417,3.12105563561883,0.803199403555509));
#75432=CARTESIAN_POINT('Ctrl Pts',(38.5779319860937,3.09625142262508,0.899583101561941));
#75433=CARTESIAN_POINT('Ctrl Pts',(38.5840946917705,3.06694292998563,0.994954083968358));
#75434=CARTESIAN_POINT('Ctrl Pts',(38.5902573974472,3.03323231316575,1.08886146817085));
#75435=CARTESIAN_POINT('Ctrl Pts',(38.596414199088,2.99955399201324,1.18267888660201));
#75436=CARTESIAN_POINT('Ctrl Pts',(38.6025710007288,2.96148207180857,1.27503508647626));
#75437=CARTESIAN_POINT('Ctrl Pts',(38.6087278023696,2.91916895414155,1.36549265090522));
#75438=CARTESIAN_POINT('Ctrl Pts',(38.6148803527234,2.87688505378917,1.45588775415739));
#75439=CARTESIAN_POINT('Ctrl Pts',(38.6210329030771,2.8303659597981,1.54438643542387));
#75440=CARTESIAN_POINT('Ctrl Pts',(38.6271854534308,2.77981243089773,1.63057057851736));
#75441=CARTESIAN_POINT('Ctrl Pts',(38.6333354012549,2.72928028614738,1.71671826570591));
#75442=CARTESIAN_POINT('Ctrl Pts',(38.6394853490789,2.67471731938183,1.80055298741101));
#75443=CARTESIAN_POINT('Ctrl Pts',(38.6456352969029,2.61637006536727,1.88168149365138));
#75444=CARTESIAN_POINT('Ctrl Pts',(38.6517864454348,2.55801141971113,1.96282583931522));
#75445=CARTESIAN_POINT('Ctrl Pts',(38.6579375939666,2.49586725562134,2.04126255476866));
#75446=CARTESIAN_POINT('Ctrl Pts',(38.6640887424984,2.43022696041206,2.1166280928369));
#75447=CARTESIAN_POINT('Ctrl Pts',(38.670240264458,2.36458268027065,2.19199820624339));
#75448=CARTESIAN_POINT('Ctrl Pts',(38.6763917864175,2.29544213822753,2.26429644875661));
#75449=CARTESIAN_POINT('Ctrl Pts',(38.6825433083771,2.22313342363478,2.33319423606735));
#75450=CARTESIAN_POINT('Ctrl Pts',(38.6887005649325,2.15075730112979,2.40215625154238));
#75451=CARTESIAN_POINT('Ctrl Pts',(38.694857821488,2.07520742646403,2.46771118470814));
#75452=CARTESIAN_POINT('Ctrl Pts',(38.7010150780434,1.99684684859484,2.5295691778951));
#75453=CARTESIAN_POINT('Ctrl Pts',(38.7062918509574,1.92969178186814,2.58258151870483));
#75454=CARTESIAN_POINT('Ctrl Pts',(38.7115686238715,1.86047308150388,2.63287920932439));
#75455=CARTESIAN_POINT('Ctrl Pts',(38.7168453967856,1.78943621037806,2.68030513402632));
#75456=CARTESIAN_POINT('Ctrl Pts',(37.4669394326166,1.78943621037803,2.68030513402633));
#75457=CARTESIAN_POINT('Ctrl Pts',(37.4730898879459,1.70631869509735,2.73579638749286));
#75458=CARTESIAN_POINT('Ctrl Pts',(37.4792403432753,1.62062842594005,2.78741050688953));
#75459=CARTESIAN_POINT('Ctrl Pts',(37.4853907986046,1.53276716638739,2.83491487987643));
#75460=CARTESIAN_POINT('Ctrl Pts',(37.491547626715,1.44481486957995,2.88246847441704));
#75461=CARTESIAN_POINT('Ctrl Pts',(37.4977044548254,1.35468747199566,2.92590360943848));
#75462=CARTESIAN_POINT('Ctrl Pts',(37.5038612829358,1.26281076315955,2.96503398613716));
#75463=CARTESIAN_POINT('Ctrl Pts',(37.5100212215073,1.17088763773931,3.00418413170266));
#75464=CARTESIAN_POINT('Ctrl Pts',(37.5161811600788,1.07721384803234,3.03902503514212));
#75465=CARTESIAN_POINT('Ctrl Pts',(37.5223410986503,0.982232556778373,3.06941961401575));
#75466=CARTESIAN_POINT('Ctrl Pts',(37.5285117579066,0.887085961198498,3.09986709125817));
#75467=CARTESIAN_POINT('Ctrl Pts',(37.534682417163,0.790627737122123,3.12585266730446));
#75468=CARTESIAN_POINT('Ctrl Pts',(37.5408530764194,0.693313810752102,3.14728986944647));
#75469=CARTESIAN_POINT('Ctrl Pts',(37.5469067490666,0.597844813067353,3.16832065381625));
#75470=CARTESIAN_POINT('Ctrl Pts',(37.5529604217139,0.501552670685782,3.18497403493035));
#75471=CARTESIAN_POINT('Ctrl Pts',(37.5590140943611,0.40487158721871,3.19721700238864));
#75472=CARTESIAN_POINT('Ctrl Pts',(37.5651863424538,0.306296776882969,3.20969977721769));
#75473=CARTESIAN_POINT('Ctrl Pts',(37.5713585905466,0.206970630375115,3.21764144642235));
#75474=CARTESIAN_POINT('Ctrl Pts',(37.5775308386393,0.107347675039233,3.22096166372152));
#75475=CARTESIAN_POINT('Ctrl Pts',(37.583694727292,0.00785964495559124,
3.2242773842543));
#75476=CARTESIAN_POINT('Ctrl Pts',(37.5898586159446,-0.0919239646534392,
3.22298407920088));
#75477=CARTESIAN_POINT('Ctrl Pts',(37.5960225045972,-0.191541477122879,
3.21705290989153));
#75478=CARTESIAN_POINT('Ctrl Pts',(37.6021798662558,-0.291053503761449,
3.21112802114779));
#75479=CARTESIAN_POINT('Ctrl Pts',(37.6083372279143,-0.390399351713373,
3.20057505750116));
#75480=CARTESIAN_POINT('Ctrl Pts',(37.6144945895728,-0.489116269441735,
3.18541721560417));
#75481=CARTESIAN_POINT('Ctrl Pts',(37.6206474537191,-0.587761081523434,
3.17027044542636));
#75482=CARTESIAN_POINT('Ctrl Pts',(37.6268003178654,-0.68577744867549,3.15052555000574));
#75483=CARTESIAN_POINT('Ctrl Pts',(37.6329531820117,-0.7827075932881,3.12625756870881));
#75484=CARTESIAN_POINT('Ctrl Pts',(37.6391037151483,-0.87960101595968,3.10199878132552));
#75485=CARTESIAN_POINT('Ctrl Pts',(37.6452542482848,-0.975408612867861,
3.07322041829767));
#75486=CARTESIAN_POINT('Ctrl Pts',(37.6514047814213,-1.06968353440715,3.04004846979752));
#75487=CARTESIAN_POINT('Ctrl Pts',(37.6575546296365,-1.16394795752231,3.00688021531459));
#75488=CARTESIAN_POINT('Ctrl Pts',(37.6637044778517,-1.25667963485141,2.96931949227251));
#75489=CARTESIAN_POINT('Ctrl Pts',(37.6698543260669,-1.34744856459123,2.92754161853953));
#75490=CARTESIAN_POINT('Ctrl Pts',(37.676005134446,-1.43823166590896,2.88575722210771));
#75491=CARTESIAN_POINT('Ctrl Pts',(37.6821559428252,-1.5270510163454,2.83975454883317));
#75492=CARTESIAN_POINT('Ctrl Pts',(37.6883067512043,-1.61349914248706,2.78975591758375));
#75493=CARTESIAN_POINT('Ctrl Pts',(37.6944641375705,-1.70003972064795,2.73970381525722));
#75494=CARTESIAN_POINT('Ctrl Pts',(37.7006215239367,-1.78420363382053,2.68564743915454));
#75495=CARTESIAN_POINT('Ctrl Pts',(37.7067789103029,-1.86561056846591,2.62785364305707));
#75496=CARTESIAN_POINT('Ctrl Pts',(37.7129397330398,-1.9470629354412,2.57002759286696));
#75497=CARTESIAN_POINT('Ctrl Pts',(37.7191005557767,-2.02575491758814,2.50846023648324));
#75498=CARTESIAN_POINT('Ctrl Pts',(37.7252613785137,-2.10133926486082,2.44345878959605));
#75499=CARTESIAN_POINT('Ctrl Pts',(37.7314325014303,-2.1770499803795,2.37834866784261));
#75500=CARTESIAN_POINT('Ctrl Pts',(37.737603624347,-2.24964236701193,2.30979328569732));
#75501=CARTESIAN_POINT('Ctrl Pts',(37.7437747472637,-2.31880592433699,2.23813686975566));
#75502=CARTESIAN_POINT('Ctrl Pts',(37.7484702692093,-2.37143151706016,2.18361449544191));
#75503=CARTESIAN_POINT('Ctrl Pts',(37.753165791155,-2.42207275915576,2.12729755105307));
#75504=CARTESIAN_POINT('Ctrl Pts',(37.7578613131006,-2.47060923006076,2.06934955839718));
#75505=CARTESIAN_POINT('Ctrl Pts',(37.7639979307526,-2.53404195757667,1.99361683288795));
#75506=CARTESIAN_POINT('Ctrl Pts',(37.7701345484046,-2.59410897624073,1.91482168154805));
#75507=CARTESIAN_POINT('Ctrl Pts',(37.7762711660567,-2.65049770048539,1.83329743964848));
#75508=CARTESIAN_POINT('Ctrl Pts',(37.7823999093046,-2.70681406767217,1.75187780827821));
#75509=CARTESIAN_POINT('Ctrl Pts',(37.7885286525526,-2.75946126721234,1.66773639906458));
#75510=CARTESIAN_POINT('Ctrl Pts',(37.7946573958006,-2.80816578952707,1.58124079792731));
#75511=CARTESIAN_POINT('Ctrl Pts',(37.8007799602126,-2.8568212092377,1.49483239935476));
#75512=CARTESIAN_POINT('Ctrl Pts',(37.8069025246246,-2.90154163422463,1.40607490455059));
#75513=CARTESIAN_POINT('Ctrl Pts',(37.8130250890366,-2.94209648297818,1.31536529046019));
#75514=CARTESIAN_POINT('Ctrl Pts',(37.8191431641036,-2.98262159505624,1.22472218882001));
#75515=CARTESIAN_POINT('Ctrl Pts',(37.8252612391705,-3.01898702253225,1.13213021254061));
#75516=CARTESIAN_POINT('Ctrl Pts',(37.8313793142374,-3.05100834218173,1.03801043272093));
#75517=CARTESIAN_POINT('Ctrl Pts',(37.8374955154327,-3.08301985419687,0.943919480332296));
#75518=CARTESIAN_POINT('Ctrl Pts',(37.843611716628,-3.11068975499154,0.848302067816363));
#75519=CARTESIAN_POINT('Ctrl Pts',(37.8497279178233,-3.13388228014506,0.75159790891994));
#75520=CARTESIAN_POINT('Ctrl Pts',(37.8558429582643,-3.1570704037392,0.654912102880492));
#75521=CARTESIAN_POINT('Ctrl Pts',(37.8619579987053,-3.17578274326909,0.557140389035435));
#75522=CARTESIAN_POINT('Ctrl Pts',(37.8680730391463,-3.18993413181391,0.458734996690495));
#75523=CARTESIAN_POINT('Ctrl Pts',(37.8741906184604,-3.20409139580304,0.360288747902387));
#75524=CARTESIAN_POINT('Ctrl Pts',(37.8803081977745,-3.21368386707593,0.261208730973718));
#75525=CARTESIAN_POINT('Ctrl Pts',(37.8864257770886,-3.21867805973883,0.161954037479339));
#75526=CARTESIAN_POINT('Ctrl Pts',(37.8898083344834,-3.2214394695148,0.107073719593024));
#75527=CARTESIAN_POINT('Ctrl Pts',(37.8931908918782,-3.22279599229166,0.0521400722480563));
#75528=CARTESIAN_POINT('Ctrl Pts',(37.8965734492731,-3.22274881024296,-0.0027692196713569));
#75529=CARTESIAN_POINT('',(37.6500265507268,-3.22274952462855,0.00175043035796299));
#75530=CARTESIAN_POINT('Ctrl Pts',(37.2205445093424,1.78943610171065,2.68030520657528));
#75531=CARTESIAN_POINT('Ctrl Pts',(37.2224802418693,1.76062823012852,2.69953803323102));
#75532=CARTESIAN_POINT('Ctrl Pts',(37.2244175279826,1.73150014886572,2.71831319089206));
#75533=CARTESIAN_POINT('Ctrl Pts',(37.2384264205786,1.51921349350945,2.85034643710809));
#75534=CARTESIAN_POINT('Ctrl Pts',(37.2506793919992,1.32545670170221,2.94544219845531));
#75535=CARTESIAN_POINT('Ctrl Pts',(37.2647609238842,1.10688342938587,3.02675533842266));
#75536=CARTESIAN_POINT('Ctrl Pts',(37.2658477158002,1.09003339531374,3.03286431974323));
#75537=CARTESIAN_POINT('Ctrl Pts',(37.2674972111626,1.06449314932949,3.04188360462719));
#75538=CARTESIAN_POINT('Ctrl Pts',(37.2680564562156,1.0558398564875,3.04489798249388));
#75539=CARTESIAN_POINT('Ctrl Pts',(37.2690306457383,1.04077698163362,3.05007321025528));
#75540=CARTESIAN_POINT('Ctrl Pts',(37.2694450302053,1.03437320372013,3.05225087234579));
#75541=CARTESIAN_POINT('Ctrl Pts',(37.2703015797915,1.02114369817172,3.05670326905425));
#75542=CARTESIAN_POINT('Ctrl Pts',(37.2707438303974,1.01431711874152,3.05897533639165));
#75543=CARTESIAN_POINT('Ctrl Pts',(37.2717805726071,0.998323800657221,3.06423891524433));
#75544=CARTESIAN_POINT('Ctrl Pts',(37.2723756628899,0.989151167606897,3.06721217150673));
#75545=CARTESIAN_POINT('Ctrl Pts',(37.2736387725998,0.969698526896517,3.07342129844191));
#75546=CARTESIAN_POINT('Ctrl Pts',(37.2743071240318,0.959415373500202,3.07664685125373));
#75547=CARTESIAN_POINT('Ctrl Pts',(37.276111827541,0.931676248972311,3.08519528912247));
#75548=CARTESIAN_POINT('Ctrl Pts',(37.2772513277758,0.914191124048758,3.09042152003924));
#75549=CARTESIAN_POINT('Ctrl Pts',(37.2863239427167,0.77522387491839,3.13067569978891));
#75550=CARTESIAN_POINT('Ctrl Pts',(37.2944837783438,0.651835218281041,3.15867160826862));
#75551=CARTESIAN_POINT('Ctrl Pts',(37.3181729803099,0.297772103565216,3.21737505629345));
#75552=CARTESIAN_POINT('Ctrl Pts',(37.3341202738711,0.0649749300655654,
3.23046947168723));
#75553=CARTESIAN_POINT('Ctrl Pts',(37.3519510734052,-0.201284597353794,
3.21663938647263));
#75554=CARTESIAN_POINT('Ctrl Pts',(37.3542244585613,-0.235368656332999,
3.21432514663897));
#75555=CARTESIAN_POINT('Ctrl Pts',(37.3617845294849,-0.349358402603648,
3.2047625414042));
#75556=CARTESIAN_POINT('Ctrl Pts',(37.3669985083002,-0.429036130022836,
3.19507193941178));
#75557=CARTESIAN_POINT('Ctrl Pts',(37.372749432629,-0.519066802190178,3.18069279046842));
#75558=CARTESIAN_POINT('Ctrl Pts',(37.3734358475626,-0.529848876295111,
3.17891446076409));
#75559=CARTESIAN_POINT('Ctrl Pts',(37.3744454834247,-0.545765125500566,
3.17620610307979));
#75560=CARTESIAN_POINT('Ctrl Pts',(37.3747710479647,-0.55090628356377,3.17531841696218));
#75561=CARTESIAN_POINT('Ctrl Pts',(37.3753471425832,-0.560019848654505,
3.17372204411346));
#75562=CARTESIAN_POINT('Ctrl Pts',(37.375597956577,-0.563993095990223,3.17301837885143));
#75563=CARTESIAN_POINT('Ctrl Pts',(37.3761309004313,-0.572447472313028,
3.17150472013617));
#75564=CARTESIAN_POINT('Ctrl Pts',(37.3764129120629,-0.576928194224971,
3.1706926936749));
#75565=CARTESIAN_POINT('Ctrl Pts',(37.3771746633321,-0.589049673858524,
3.1684694122481));
#75566=CARTESIAN_POINT('Ctrl Pts',(37.3776533753126,-0.596687133366817,
3.16704000644736));
#75567=CARTESIAN_POINT('Ctrl Pts',(37.3800297551351,-0.634694316697665,
3.15978431927256));
#75568=CARTESIAN_POINT('Ctrl Pts',(37.3819049479015,-0.664985483264241,
3.15354852399911));
#75569=CARTESIAN_POINT('Ctrl Pts',(37.3871580840239,-0.750508238316349,
3.13465550720659));
#75570=CARTESIAN_POINT('Ctrl Pts',(37.3904872358269,-0.80550446203134,3.1209759854939));
#75571=CARTESIAN_POINT('Ctrl Pts',(37.4033504534745,-1.01951930941039,3.06170811072668));
#75572=CARTESIAN_POINT('Ctrl Pts',(37.4125221773342,-1.17529979136804,3.00535422246439));
#75573=CARTESIAN_POINT('Ctrl Pts',(37.4349834602705,-1.54137475376134,2.84008520820448));
#75574=CARTESIAN_POINT('Ctrl Pts',(37.4483321848952,-1.74530262894262,2.71952509482192));
#75575=CARTESIAN_POINT('Ctrl Pts',(37.4637830694739,-1.94994091559425,2.56597633369436));
#75576=CARTESIAN_POINT('Ctrl Pts',(37.4649759369321,-1.96555858143066,2.55403280242161));
#75577=CARTESIAN_POINT('Ctrl Pts',(37.4667398217267,-1.98838112619948,2.5362460604074));
#75578=CARTESIAN_POINT('Ctrl Pts',(37.4673064511329,-1.99567182320074,2.53051329836606));
#75579=CARTESIAN_POINT('Ctrl Pts',(37.4683181876895,-2.00861644488968,2.52024405271185));
#75580=CARTESIAN_POINT('Ctrl Pts',(37.4687628029808,-2.01428002359491,2.51571979622008));
#75581=CARTESIAN_POINT('Ctrl Pts',(37.4692132547213,-2.01999251602909,2.51112480862423));
#75582=CARTESIAN_POINT('Ctrl Pts',(37.4692183221494,-2.02005677636714,2.51107311513518));
#75583=CARTESIAN_POINT('Ctrl Pts',(37.4692282303718,-2.02018241673396,2.5109720372448));
#75584=CARTESIAN_POINT('Ctrl Pts',(37.4692330711804,-2.02024379722798,2.51092265282469));
#75585=CARTESIAN_POINT('Ctrl Pts',(37.4692425379801,-2.02036382857398,2.51082607290054));
#75586=CARTESIAN_POINT('Ctrl Pts',(37.4692471639705,-2.02042247967589,2.5107788775174));
#75587=CARTESIAN_POINT('Ctrl Pts',(37.4692562121854,-2.02053719311496,2.5106865632567));
#75588=CARTESIAN_POINT('Ctrl Pts',(37.4692606344171,-2.02059325577748,2.5106414444092));
#75589=CARTESIAN_POINT('Ctrl Pts',(37.4692692855023,-2.02070292471747,2.51055317754345));
#75590=CARTESIAN_POINT('Ctrl Pts',(37.4692735143618,-2.02075653128325,2.51051002955799));
#75591=CARTESIAN_POINT('Ctrl Pts',(37.4692817884481,-2.02086141219338,2.51042560525908));
#75592=CARTESIAN_POINT('Ctrl Pts',(37.4692858336875,-2.02091268688959,2.51038432890291));
#75593=CARTESIAN_POINT('Ctrl Pts',(37.4692937497061,-2.02101302089148,2.5103035545236));
#75594=CARTESIAN_POINT('Ctrl Pts',(37.4692976204973,-2.02106208052516,2.51026405645501));
#75595=CARTESIAN_POINT('Ctrl Pts',(37.4693051962382,-2.02115809415445,2.51018675093464));
#75596=CARTESIAN_POINT('Ctrl Pts',(37.4693089012057,-2.02120504853464,2.51014894337206));
#75597=CARTESIAN_POINT('Ctrl Pts',(37.4693161534218,-2.02129695506833,2.51007493618464));
#75598=CARTESIAN_POINT('Ctrl Pts',(37.4693197006877,-2.02134190758624,2.51003873644738));
#75599=CARTESIAN_POINT('Ctrl Pts',(37.4693266451485,-2.02142990773995,2.50996786705512));
#75600=CARTESIAN_POINT('Ctrl Pts',(37.4693300423638,-2.02147295576501,2.50993319725155));
#75601=CARTESIAN_POINT('Ctrl Pts',(37.4693366939325,-2.021557238675,2.5098653143274));
#75602=CARTESIAN_POINT('Ctrl Pts',(37.4693399483097,-2.0215984739818,2.5098321010174));
#75603=CARTESIAN_POINT('Ctrl Pts',(37.4693463209997,-2.02167921793681,2.50976706186766));
#75604=CARTESIAN_POINT('Ctrl Pts',(37.4693494393407,-2.0217187270525,2.50973523578854));
#75605=CARTESIAN_POINT('Ctrl Pts',(37.4693555463853,-2.02179610037984,2.50967290564978));
#75606=CARTESIAN_POINT('Ctrl Pts',(37.469358535115,-2.02183396502238,2.50964240136828));
#75607=CARTESIAN_POINT('Ctrl Pts',(37.4693643889991,-2.02190812650292,2.50958265308271));
#75608=CARTESIAN_POINT('Ctrl Pts',(37.4693672541842,-2.02194442382091,2.50955340880635));
#75609=CARTESIAN_POINT('Ctrl Pts',(37.4693728667073,-2.02201552348668,2.50949612218786));
#75610=CARTESIAN_POINT('Ctrl Pts',(37.4693756140804,-2.02205032636458,2.50946807952319));
#75611=CARTESIAN_POINT('Ctrl Pts',(37.4693809964028,-2.02211850609953,2.50941314088107));
#75612=CARTESIAN_POINT('Ctrl Pts',(37.4693836313867,-2.02215188347209,2.50938624458392));
#75613=CARTESIAN_POINT('Ctrl Pts',(37.4693887940676,-2.02221727749147,2.50933354634355));
#75614=CARTESIAN_POINT('Ctrl Pts',(37.4693913217974,-2.02224929462391,2.5093077440966));
#75615=CARTESIAN_POINT('Ctrl Pts',(37.4693962748219,-2.02231202982677,2.5092571845217));
#75616=CARTESIAN_POINT('Ctrl Pts',(37.4693987001561,-2.02234274846107,2.50923242681953));
#75617=CARTESIAN_POINT('Ctrl Pts',(37.4694038885212,-2.02240846131369,2.50917946351515));
#75618=CARTESIAN_POINT('Ctrl Pts',(37.4694066516036,-2.02244345596416,2.5091512572877));
#75619=CARTESIAN_POINT('Ctrl Pts',(37.4694121526349,-2.02251312502412,2.50909510054678));
#75620=CARTESIAN_POINT('Ctrl Pts',(37.4694148901303,-2.02254779370764,2.50906715467144));
#75621=CARTESIAN_POINT('Ctrl Pts',(37.4694203397855,-2.02261680832958,2.50901152072062));
#75622=CARTESIAN_POINT('Ctrl Pts',(37.4694230519556,-2.02265115441582,2.50898383254784));
#75623=CARTESIAN_POINT('Ctrl Pts',(37.469428451374,-2.02271952913357,2.50892870980267));
#75624=CARTESIAN_POINT('Ctrl Pts',(37.4694311386296,-2.02275355787464,2.50890127516327));
#75625=CARTESIAN_POINT('Ctrl Pts',(37.469436488617,-2.02282130299522,2.50884665544236));
#75626=CARTESIAN_POINT('Ctrl Pts',(37.4694391513584,-2.02285501951226,2.50881947027076));
#75627=CARTESIAN_POINT('Ctrl Pts',(37.469444452708,-2.02292214517852,2.50876534552119));
#75628=CARTESIAN_POINT('Ctrl Pts',(37.4694470913267,-2.02295555447622,2.50873840584376));
#75629=CARTESIAN_POINT('Ctrl Pts',(37.469952018084,-2.0293485980074,2.50358314718528));
#75630=CARTESIAN_POINT('Ctrl Pts',(37.4704552800458,-2.03568866190087,2.49843070285088));
#75631=CARTESIAN_POINT('Ctrl Pts',(37.4718285307259,-2.0529015338585,2.48433312741732));
#75632=CARTESIAN_POINT('Ctrl Pts',(37.4727004337053,-2.06373532776098,2.47534084168917));
#75633=CARTESIAN_POINT('Ctrl Pts',(37.4746403731667,-2.08762805515924,2.45524347402416));
#75634=CARTESIAN_POINT('Ctrl Pts',(37.47570978232,-2.10065793828163,2.44410466662851));
#75635=CARTESIAN_POINT('Ctrl Pts',(37.4789689293492,-2.13993726725661,2.40997996257231));
#75636=CARTESIAN_POINT('Ctrl Pts',(37.4811719476923,-2.16590218476488,2.38667184598604));
#75637=CARTESIAN_POINT('Ctrl Pts',(37.4893402062464,-2.2600127153569,2.29939034352748));
#75638=CARTESIAN_POINT('Ctrl Pts',(37.4954097320415,-2.32573944324816,2.23288754040933));
#75639=CARTESIAN_POINT('Ctrl Pts',(37.5158149635961,-2.53331939408569,2.00373520968703));
#75640=CARTESIAN_POINT('Ctrl Pts',(37.53056655816,-2.66173139669831,1.82970878571906));
#75641=CARTESIAN_POINT('Ctrl Pts',(37.5494371625395,-2.80506226468721,1.58808011082096));
#75642=CARTESIAN_POINT('Ctrl Pts',(37.5537863979906,-2.83663282956752,1.53097607877595));
#75643=CARTESIAN_POINT('Ctrl Pts',(37.5624805230061,-2.89712487501739,1.4132549517848));
#75644=CARTESIAN_POINT('Ctrl Pts',(37.5668196693968,-2.92593040517308,1.35261039452751));
#75645=CARTESIAN_POINT('Ctrl Pts',(37.5717096171271,-2.95700568357344,1.28153967994256));
#75646=CARTESIAN_POINT('Ctrl Pts',(37.5723651612951,-2.96114189045629,1.27195333075637));
#75647=CARTESIAN_POINT('Ctrl Pts',(37.5733380984812,-2.96723738164278,1.25763512506905));
#75648=CARTESIAN_POINT('Ctrl Pts',(37.5736575989741,-2.96923204169334,1.25291854095699));
#75649=CARTESIAN_POINT('Ctrl Pts',(37.5742269959283,-2.97277441280395,1.24448626120758));
#75650=CARTESIAN_POINT('Ctrl Pts',(37.5744771519168,-2.97432640799353,1.24077241389976));
#75651=CARTESIAN_POINT('Ctrl Pts',(37.575013145255,-2.97764257128531,1.2327950233224));
#75652=CARTESIAN_POINT('Ctrl Pts',(37.5752988475505,-2.97940453591041,1.22853061170287));
#75653=CARTESIAN_POINT('Ctrl Pts',(37.5760809870765,-2.98421229836944,1.21682340220248));
#75654=CARTESIAN_POINT('Ctrl Pts',(37.5765763006831,-2.98723943096725,1.20937290329058));
#75655=CARTESIAN_POINT('Ctrl Pts',(37.5791778911401,-3.00304407218191,1.17005248170601));
#75656=CARTESIAN_POINT('Ctrl Pts',(37.5812562671334,-3.01534011683228,1.13798976877865));
#75657=CARTESIAN_POINT('Ctrl Pts',(37.5872467707994,-3.04970386362609,1.04391366794094));
#75658=CARTESIAN_POINT('Ctrl Pts',(37.5910920291017,-3.07038817643195,0.981410716644376));
#75659=CARTESIAN_POINT('Ctrl Pts',(37.612746686303,-3.17759684509134,0.620768231487759));
#75660=CARTESIAN_POINT('Ctrl Pts',(37.6294005054505,-3.22259519032419,0.312020770992711));
#75661=CARTESIAN_POINT('Ctrl Pts',(37.6474995143151,-3.22274960128745,0.00160309126306275));
#75662=CARTESIAN_POINT('Ctrl Pts',(37.6500265507268,-3.22274952462855,0.00175043035796299));
#75663=CARTESIAN_POINT('Ctrl Pts',(37.6562525068647,-3.22280455179977,-0.0995611065815355));
#75664=CARTESIAN_POINT('Ctrl Pts',(37.6624784630026,-3.21807793497928,-0.200873595969597));
#75665=CARTESIAN_POINT('Ctrl Pts',(37.6687044191406,-3.20859589316742,-0.301711711488305));
#75666=CARTESIAN_POINT('Ctrl Pts',(37.6749320374216,-3.19911131993544,-0.402576747752343));
#75667=CARTESIAN_POINT('Ctrl Pts',(37.6811596557026,-3.18486883519379,-0.502966740616681));
#75668=CARTESIAN_POINT('Ctrl Pts',(37.6873872739837,-3.16594645797127,-0.602412307111318));
#75669=CARTESIAN_POINT('Ctrl Pts',(37.6936180596769,-3.14701445668942,-0.701908452347799));
#75670=CARTESIAN_POINT('Ctrl Pts',(37.6998488453701,-3.12339790591718,-0.800458803920177));
#75671=CARTESIAN_POINT('Ctrl Pts',(37.7060796310633,-3.09522558791562,-0.897605772270008));
#75672=CARTESIAN_POINT('Ctrl Pts',(37.7123194068227,-3.06701262158846,-0.994892908766438));
#75673=CARTESIAN_POINT('Ctrl Pts',(37.7185591825822,-3.03423088150391,-1.09077221623046));
#75674=CARTESIAN_POINT('Ctrl Pts',(37.7247989583417,-2.99705858694311,-1.18480267932284));
#75675=CARTESIAN_POINT('Ctrl Pts',(37.7310438467765,-2.95985583457685,-1.27891018801024));
#75676=CARTESIAN_POINT('Ctrl Pts',(37.7372887352114,-2.91825553415589,-1.37116545338473));
#75677=CARTESIAN_POINT('Ctrl Pts',(37.7435336236463,-2.87248259932717,-1.46115066952817));
#75678=CARTESIAN_POINT('Ctrl Pts',(37.7497896545153,-2.82662799419841,-1.55129644167768));
#75679=CARTESIAN_POINT('Ctrl Pts',(37.7560456853843,-2.77658609542278,-1.63916371321967));
#75680=CARTESIAN_POINT('Ctrl Pts',(37.7623017162533,-2.72262606332809,-1.72436216665369));
#75681=CARTESIAN_POINT('Ctrl Pts',(37.7649444456067,-2.69983177670908,-1.76035247080442));
#75682=CARTESIAN_POINT('Ctrl Pts',(37.7675871749601,-2.67633881719068,-1.79586692679338));
#75683=CARTESIAN_POINT('Ctrl Pts',(37.7702299043134,-2.65216960257468,-1.8308779210201));
#75684=CARTESIAN_POINT('Ctrl Pts',(37.7764021524062,-2.59572099627804,-1.91264813410139));
#75685=CARTESIAN_POINT('Ctrl Pts',(37.782574400499,-2.5353878507564,-1.99194923775924));
#75686=CARTESIAN_POINT('Ctrl Pts',(37.7887466485917,-2.47141347119128,-2.06838899071579));
#75687=CARTESIAN_POINT('Ctrl Pts',(37.7949105372444,-2.40752573590673,-2.14472521680037));
#75688=CARTESIAN_POINT('Ctrl Pts',(37.801074425897,-2.34000684488508,-2.21820746458734));
#75689=CARTESIAN_POINT('Ctrl Pts',(37.8072383145497,-2.26914324819176,-2.2884725215055));
#75690=CARTESIAN_POINT('Ctrl Pts',(37.8133956762082,-2.1983546895634,-2.35866317415756));
#75691=CARTESIAN_POINT('Ctrl Pts',(37.8195530378668,-2.12422877332027,-2.42564310464567));
#75692=CARTESIAN_POINT('Ctrl Pts',(37.8257103995253,-2.04709143595346,-2.48908300692163));
#75693=CARTESIAN_POINT('Ctrl Pts',(37.8318632636716,-1.97001044189372,-2.55247657088702));
#75694=CARTESIAN_POINT('Ctrl Pts',(37.8380161278179,-1.88992273442372,-2.612334972445));
#75695=CARTESIAN_POINT('Ctrl Pts',(37.8441689919642,-1.80718955842861,-2.66836719032569));
#75696=CARTESIAN_POINT('Ctrl Pts',(37.8503195251008,-1.72448772585939,-2.72437818042625));
#75697=CARTESIAN_POINT('Ctrl Pts',(37.8564700582373,-1.63914277545373,-2.77656562378353));
#75698=CARTESIAN_POINT('Ctrl Pts',(37.8626205913738,-1.55154662461723,-2.82468062515727));
#75699=CARTESIAN_POINT('Ctrl Pts',(37.868770439589,-1.46396022845918,-2.87279026846034));
#75700=CARTESIAN_POINT('Ctrl Pts',(37.8749202878042,-1.37412351100675,-2.91682816229175));
#75701=CARTESIAN_POINT('Ctrl Pts',(37.8810701360194,-1.28245390438678,-2.95659086544336));
#75702=CARTESIAN_POINT('Ctrl Pts',(37.8872209443986,-1.19076998556788,-2.99635977666914));
#75703=CARTESIAN_POINT('Ctrl Pts',(37.8933717527777,-1.09725300772172,-3.03185199856225));
#75704=CARTESIAN_POINT('Ctrl Pts',(37.8995225611569,-1.00234039523467,-3.06291222443295));
#75705=CARTESIAN_POINT('Ctrl Pts',(37.905679947523,-0.907326278376747,-3.09400566768756));
#75706=CARTESIAN_POINT('Ctrl Pts',(37.9118373338892,-0.810913960021141,
-3.12065751466234));
#75707=CARTESIAN_POINT('Ctrl Pts',(37.9179947202554,-0.713555930245918,
-3.14276239905451));
#75708=CARTESIAN_POINT('Ctrl Pts',(37.9241555429924,-0.616143566006662,
-3.16487961994373));
#75709=CARTESIAN_POINT('Ctrl Pts',(37.9303163657293,-0.517784866882843,
-3.18244474826779));
#75710=CARTESIAN_POINT('Ctrl Pts',(37.9364771884663,-0.418940341809283,
-3.195403973288));
#75711=CARTESIAN_POINT('Ctrl Pts',(37.942648311383,-0.319930560175463,-3.20838486462658));
#75712=CARTESIAN_POINT('Ctrl Pts',(37.9488194342997,-0.220433763210126,
-3.21674443469551));
#75713=CARTESIAN_POINT('Ctrl Pts',(37.9549905572163,-0.120913523366501,
-3.22048093960624));
#75714=CARTESIAN_POINT('Ctrl Pts',(37.9596860791619,-0.0451899514139525,
-3.22332399443513));
#75715=CARTESIAN_POINT('Ctrl Pts',(37.9643816011074,0.0305471301858255,
-3.22349161534475));
#75716=CARTESIAN_POINT('Ctrl Pts',(37.9690771230529,0.1060955676368,-3.22100315011144));
#75717=CARTESIAN_POINT('Ctrl Pts',(37.9752493711457,0.205403739204771,-3.21773207077918));
#75718=CARTESIAN_POINT('Ctrl Pts',(37.9814216192384,0.304735284049323,-3.20985820967658));
#75719=CARTESIAN_POINT('Ctrl Pts',(37.9875938673312,0.403628687708124,-3.19737414841601));
#75720=CARTESIAN_POINT('Ctrl Pts',(37.9937577559838,0.50238815418949,-3.18490699505694));
#75721=CARTESIAN_POINT('Ctrl Pts',(37.9999216446364,0.600710231773359,-3.16784210583526));
#75722=CARTESIAN_POINT('Ctrl Pts',(38.0060855332891,0.698134496323708,-3.1462240523432));
#75723=CARTESIAN_POINT('Ctrl Pts',(38.0122428949476,0.795455597492531,-3.12462889039166));
#75724=CARTESIAN_POINT('Ctrl Pts',(38.0184002566062,0.891880353990418,-3.09849024311563));
#75725=CARTESIAN_POINT('Ctrl Pts',(38.0245576182647,0.986955513436086,-3.06790423204475));
#75726=CARTESIAN_POINT('Ctrl Pts',(38.030710482411,1.08196122727859,-3.03734056186712));
#75727=CARTESIAN_POINT('Ctrl Pts',(38.0368633465573,1.17561889171836,-3.00233611905558));
#75728=CARTESIAN_POINT('Ctrl Pts',(38.0430162107036,1.2674883682607,-2.96303742784728));
#75729=CARTESIAN_POINT('Ctrl Pts',(38.0491667438402,1.3593230400939,-2.92375362493015));
#75730=CARTESIAN_POINT('Ctrl Pts',(38.0553172769767,1.44937047120064,-2.88017897685373));
#75731=CARTESIAN_POINT('Ctrl Pts',(38.0614678101132,1.53720937493199,-2.83250858782833));
#75732=CARTESIAN_POINT('Ctrl Pts',(38.0676176583285,1.62503849695214,-2.78484350736164));
#75733=CARTESIAN_POINT('Ctrl Pts',(38.0737675065437,1.71065919878597,-2.73308379993163));
#75734=CARTESIAN_POINT('Ctrl Pts',(38.0799173547589,1.79367463405055,-2.67747061042015));
#75735=CARTESIAN_POINT('Ctrl Pts',(38.086068163138,1.87670303035475,-2.62184873812875));
#75736=CARTESIAN_POINT('Ctrl Pts',(38.0922189715171,1.95712499125445,-2.56237243053142));
#75737=CARTESIAN_POINT('Ctrl Pts',(38.0983697798963,2.03457335153321,-2.49932567700389));
#75738=CARTESIAN_POINT('Ctrl Pts',(38.1045271662624,2.11210453902418,-2.43621149807425));
#75739=CARTESIAN_POINT('Ctrl Pts',(38.1106845526286,2.18665543799785,-2.36951952299409));
#75740=CARTESIAN_POINT('Ctrl Pts',(38.1168419389948,2.25789274736271,-2.29957341781185));
#75741=CARTESIAN_POINT('Ctrl Pts',(38.1230027617318,2.32916981349981,-2.22958827646447));
#75742=CARTESIAN_POINT('Ctrl Pts',(38.1291635844687,2.39712931175495,-2.15634570671666));
#75743=CARTESIAN_POINT('Ctrl Pts',(38.1353244072057,2.46147697415873,-2.08020399677204));
#75744=CARTESIAN_POINT('Ctrl Pts',(38.1414955301223,2.52593221837693,-2.00393498673598));
#75745=CARTESIAN_POINT('Ctrl Pts',(38.147666653039,2.58676330012441,-1.92475749933256));
#75746=CARTESIAN_POINT('Ctrl Pts',(38.1538377759557,2.64371809405453,-1.84306055290343));
#75747=CARTESIAN_POINT('Ctrl Pts',(38.1585332979013,2.68705420782473,-1.78089847802216));
#75748=CARTESIAN_POINT('Ctrl Pts',(38.163228819847,2.72814702753737,-1.7172784041907));
#75749=CARTESIAN_POINT('Ctrl Pts',(38.1679243417926,2.76690352208694,-1.65238084652507));
#75750=CARTESIAN_POINT('Ctrl Pts',(38.1740965898854,2.81784880619728,-1.56707322126721));
#75751=CARTESIAN_POINT('Ctrl Pts',(38.1802688379781,2.86493482742254,-1.47925716296869));
#75752=CARTESIAN_POINT('Ctrl Pts',(38.1864410860709,2.9079057997536,-1.38931689051108));
#75753=CARTESIAN_POINT('Ctrl Pts',(38.1926049747235,2.95081857395892,-1.29949842947641));
#75754=CARTESIAN_POINT('Ctrl Pts',(38.1987688633762,2.98962719111635,-1.20756186102319));
#75755=CARTESIAN_POINT('Ctrl Pts',(38.2049327520288,3.02412018920187,-1.11391859835521));
#75756=CARTESIAN_POINT('Ctrl Pts',(38.2110901136874,3.05857666235845,-1.02037449533425));
#75757=CARTESIAN_POINT('Ctrl Pts',(38.2172474753459,3.08872645241741,-0.925127696404006));
#75758=CARTESIAN_POINT('Ctrl Pts',(38.2234048370044,3.11440533946282,-0.828611455403252));
#75759=CARTESIAN_POINT('Ctrl Pts',(38.2295577011507,3.14006546991815,-0.732165712612355));
#75760=CARTESIAN_POINT('Ctrl Pts',(38.2357105652971,3.16126107873318,-0.63445278976262));
#75761=CARTESIAN_POINT('Ctrl Pts',(38.2418634294434,3.17787743601157,-0.535922162434538));
#75762=CARTESIAN_POINT('Ctrl Pts',(38.2480139625799,3.1944874981906,-0.437428863389572));
#75763=CARTESIAN_POINT('Ctrl Pts',(38.2541644957165,3.20652168381173,-0.338118903262951));
#75764=CARTESIAN_POINT('Ctrl Pts',(38.260315028853,3.21391632227115,-0.238452166983385));
#75765=CARTESIAN_POINT('Ctrl Pts',(38.2664648770682,3.2213101372661,-0.138796529558336));
#75766=CARTESIAN_POINT('Ctrl Pts',(38.2726147252834,3.22406540015222,-0.0387846281554028));
#75767=CARTESIAN_POINT('Ctrl Pts',(38.2787645734986,3.22217038525106,0.0611193170038219));
#75768=CARTESIAN_POINT('Ctrl Pts',(38.2849153818778,3.22027507448489,0.161038859973051));
#75769=CARTESIAN_POINT('Ctrl Pts',(38.2910661902569,3.21372805206935,0.26084997888216));
#75770=CARTESIAN_POINT('Ctrl Pts',(38.2972169986361,3.20256968240682,0.360090255114835));
#75771=CARTESIAN_POINT('Ctrl Pts',(38.3033743850023,3.19139937941675,0.45943666394197));
#75772=CARTESIAN_POINT('Ctrl Pts',(38.3095317713685,3.17560792989481,0.558210578514013));
#75773=CARTESIAN_POINT('Ctrl Pts',(38.3156891577347,3.15528738529323,0.655956613435232));
#75774=CARTESIAN_POINT('Ctrl Pts',(38.3218499804716,3.13495550001538,0.753757199361873));
#75775=CARTESIAN_POINT('Ctrl Pts',(38.3280108032086,3.1100895940069,0.850528342502538));
#75776=CARTESIAN_POINT('Ctrl Pts',(38.3341716259455,3.08083194879438,0.945828771917954));
#75777=CARTESIAN_POINT('Ctrl Pts',(38.3403427488622,3.05152538819874,1.04128853257763));
#75778=CARTESIAN_POINT('Ctrl Pts',(38.3465138717789,3.01781256875866,1.13527225895367));
#75779=CARTESIAN_POINT('Ctrl Pts',(38.3526849946956,2.97988440941438,1.22735751475645));
#75780=CARTESIAN_POINT('Ctrl Pts',(38.3573805166412,2.9510253983464,1.29742391034098));
#75781=CARTESIAN_POINT('Ctrl Pts',(38.3620760385867,2.91972693349835,1.36639158192843));
#75782=CARTESIAN_POINT('Ctrl Pts',(38.3667715605322,2.88609056292363,1.43408466455198));
#75783=CARTESIAN_POINT('Ctrl Pts',(38.372943637077,2.84187689375485,1.52306452501239));
#75784=CARTESIAN_POINT('Ctrl Pts',(38.3791157136217,2.79346659890682,1.61015437971099));
#75785=CARTESIAN_POINT('Ctrl Pts',(38.3852877901665,2.7410445645196,1.69493134309847));
#75786=CARTESIAN_POINT('Ctrl Pts',(38.3914518381726,2.68869071987752,1.77959802996588));
#75787=CARTESIAN_POINT('Ctrl Pts',(38.3976158861788,2.63233573177939,1.86195743777999));
#75788=CARTESIAN_POINT('Ctrl Pts',(38.4037799341849,2.57221136227819,1.94160919607088));
#75789=CARTESIAN_POINT('Ctrl Pts',(38.4099367118373,2.51215790809682,2.0211670069331));
#75790=CARTESIAN_POINT('Ctrl Pts',(38.4160934894897,2.44834417686357,2.09802317649368));
#75791=CARTESIAN_POINT('Ctrl Pts',(38.4222502671421,2.38104574964331,2.17180540118252));
#75792=CARTESIAN_POINT('Ctrl Pts',(38.4284028046021,2.31379367106477,2.24553681181761));
#75793=CARTESIAN_POINT('Ctrl Pts',(38.434555342062,2.24306195790413,2.31619816520041));
#75794=CARTESIAN_POINT('Ctrl Pts',(38.440707879522,2.16916662225259,2.38344996326864));
#75795=CARTESIAN_POINT('Ctrl Pts',(38.4468582812357,2.09529693807963,2.45067841604664));
#75796=CARTESIAN_POINT('Ctrl Pts',(38.4530086829495,2.0182661329439,2.51449937172952));
#75797=CARTESIAN_POINT('Ctrl Pts',(38.4591590846632,1.93842661068593,2.57461061861491));
#75798=CARTESIAN_POINT('Ctrl Pts',(38.4629068025038,1.88977678001197,2.61123911913531));
#75799=CARTESIAN_POINT('Ctrl Pts',(38.4666545203444,1.84008476533747,2.64649093985225));
#75800=CARTESIAN_POINT('Ctrl Pts',(38.470402238185,1.78943621037805,2.68030513402632));
#75801=CARTESIAN_POINT('Origin',(-1.72497344927317,0.,0.));
#75802=CARTESIAN_POINT('',(39.9670570335907,1.78943621037801,2.68030513402635));
#75803=CARTESIAN_POINT('',(39.7209886430068,1.78943588752244,2.68030534957246));
#75804=CARTESIAN_POINT('',(-1.72497344927317,1.78943621037804,2.68030513402633));
#75805=CARTESIAN_POINT('',(39.1465734492125,-3.22274998364956,-0.000324633233694736));
#75806=CARTESIAN_POINT('Ctrl Pts',(39.1465734492731,-3.22274998364947,-0.000324634210066948));
#75807=CARTESIAN_POINT('Ctrl Pts',(39.1476462476081,-3.22274824391556,-0.0175955417198468));
#75808=CARTESIAN_POINT('Ctrl Pts',(39.1487190459431,-3.22260767174683,-0.0348656462574428));
#75809=CARTESIAN_POINT('Ctrl Pts',(39.1497918442782,-3.22232829810597,-0.0521334990721938));
#75810=CARTESIAN_POINT('Ctrl Pts',(39.1559640923709,-3.22072094715689,-0.151482526863611));
#75811=CARTESIAN_POINT('Ctrl Pts',(39.1621363404637,-3.21451185152515,-0.250932014651666));
#75812=CARTESIAN_POINT('Ctrl Pts',(39.1683085885565,-3.20368586415779,-0.350020636956677));
#75813=CARTESIAN_POINT('Ctrl Pts',(39.1744724772091,-3.19287453906453,-0.44897505768811));
#75814=CARTESIAN_POINT('Ctrl Pts',(39.1806363658617,-3.17745879738243,-0.547569156360143));
#75815=CARTESIAN_POINT('Ctrl Pts',(39.1868002545143,-3.15747549300735,-0.645341826908817));
#75816=CARTESIAN_POINT('Ctrl Pts',(39.1929576161729,-3.13751334912308,-0.743010965145803));
#75817=CARTESIAN_POINT('Ctrl Pts',(39.1991149778314,-3.11299334472704,-0.839859981307581));
#75818=CARTESIAN_POINT('Ctrl Pts',(39.20527233949,-3.08400399653836,-0.935434076691369));
#75819=CARTESIAN_POINT('Ctrl Pts',(39.2114252036363,-3.05503582299486,-1.03093836203507));
#75820=CARTESIAN_POINT('Ctrl Pts',(39.2175780677826,-3.02160492181605,-1.12516916364069));
#75821=CARTESIAN_POINT('Ctrl Pts',(39.2237309319289,-2.98385042499748,-1.21768395067947));
#75822=CARTESIAN_POINT('Ctrl Pts',(39.2298814650654,-2.9461102314528,-1.3101636885334));
#75823=CARTESIAN_POINT('Ctrl Pts',(39.236031998202,-2.90404986089225,-1.40092830185925));
#75824=CARTESIAN_POINT('Ctrl Pts',(39.2421825313385,-2.8578573342118,-1.48955329538484));
#75825=CARTESIAN_POINT('Ctrl Pts',(39.2483323795537,-2.8116699515158,-1.57816841966054));
#75826=CARTESIAN_POINT('Ctrl Pts',(39.2544822277689,-2.76135152832458,-1.66464401265235));
#75827=CARTESIAN_POINT('Ctrl Pts',(39.2606320759841,-2.70713652908706,-1.74857924481062));
#75828=CARTESIAN_POINT('Ctrl Pts',(39.2667828843632,-2.65291306536636,-1.83252758161467));
#75829=CARTESIAN_POINT('Ctrl Pts',(39.2729336927423,-2.59479205293229,-1.91393440487903));
#75830=CARTESIAN_POINT('Ctrl Pts',(39.2790845011215,-2.53305129183504,-1.99242784447339));
#75831=CARTESIAN_POINT('Ctrl Pts',(39.2852418874877,-2.47124450203038,-2.07100522894084));
#75832=CARTESIAN_POINT('Ctrl Pts',(39.2913992738538,-2.40581050236054,-2.14666266588568));
#75833=CARTESIAN_POINT('Ctrl Pts',(39.29755666022,-2.33706733115862,-2.21906148002508));
#75834=CARTESIAN_POINT('Ctrl Pts',(39.303717482957,-2.26828579513588,-2.29150069916012));
#75835=CARTESIAN_POINT('Ctrl Pts',(39.3098783056939,-2.19619172311498,-2.36067737301636));
#75836=CARTESIAN_POINT('Ctrl Pts',(39.3160391284309,-2.12113842447668,-2.42629127408656));
#75837=CARTESIAN_POINT('Ctrl Pts',(39.3222102513476,-2.04595964544425,-2.49201487397503));
#75838=CARTESIAN_POINT('Ctrl Pts',(39.3283813742643,-1.96781209748039,-2.55416353257134));
#75839=CARTESIAN_POINT('Ctrl Pts',(39.3345524971809,-1.88708052162202,-2.61247864439401));
#75840=CARTESIAN_POINT('Ctrl Pts',(39.3392480191266,-1.82565298383554,-2.65684980520591));
#75841=CARTESIAN_POINT('Ctrl Pts',(39.3439435410722,-1.76273007964743,-2.69900240601355));
#75842=CARTESIAN_POINT('Ctrl Pts',(39.3486390630179,-1.69849074071571,-2.73884040539112));
#75843=CARTESIAN_POINT('Ctrl Pts',(39.3548113111106,-1.61404834181067,-2.79120732402636));
#75844=CARTESIAN_POINT('Ctrl Pts',(39.3609835592034,-1.52703322459284,-2.83975753376277));
#75845=CARTESIAN_POINT('Ctrl Pts',(39.3671558072962,-1.4378252700014,-2.88422884935391));
#75846=CARTESIAN_POINT('Ctrl Pts',(39.3733196959488,-1.3487381350116,-2.92863993481582));
#75847=CARTESIAN_POINT('Ctrl Pts',(39.3794835846014,-1.25746445095498,-2.96898291417187));
#75848=CARTESIAN_POINT('Ctrl Pts',(39.3856474732541,-1.16441203164176,-3.00503946447762));
#75849=CARTESIAN_POINT('Ctrl Pts',(39.3918048349126,-1.07145814632625,-3.04105783419578));
#75850=CARTESIAN_POINT('Ctrl Pts',(39.3979621965712,-0.976729673163516,
-3.0727986426186));
#75851=CARTESIAN_POINT('Ctrl Pts',(39.4041195582297,-0.880657054772842,
-3.10009043648388));
#75852=CARTESIAN_POINT('Ctrl Pts',(39.410272422376,-0.784654610557619,-3.12736229564599));
#75853=CARTESIAN_POINT('Ctrl Pts',(39.4164252865223,-0.687310389687696,
-3.15019148284326));
#75854=CARTESIAN_POINT('Ctrl Pts',(39.4225781506686,-0.589071883135591,
-3.16845575620034));
#75855=CARTESIAN_POINT('Ctrl Pts',(39.4287286838052,-0.49087059419678,-3.18671311014582));
#75856=CARTESIAN_POINT('Ctrl Pts',(39.4348792169417,-0.391776119352182,
-3.20040890728105));
#75857=CARTESIAN_POINT('Ctrl Pts',(39.4410297500782,-0.292247212632413,
-3.20947178351962));
#75858=CARTESIAN_POINT('Ctrl Pts',(39.4471795982934,-0.19272938941863,-3.21853365051929));
#75859=CARTESIAN_POINT('Ctrl Pts',(39.4533294465087,-0.0927776630986046,
-3.22296358295743));
#75860=CARTESIAN_POINT('Ctrl Pts',(39.4594792947239,0.00714400760919167,
-3.22274208177683));
#75861=CARTESIAN_POINT('Ctrl Pts',(39.465630103103,0.107081278894509,-3.22252054601369));
#75862=CARTESIAN_POINT('Ctrl Pts',(39.4717809114821,0.206988050831943,-3.21764613513559));
#75863=CARTESIAN_POINT('Ctrl Pts',(39.4779317198613,0.306401293621398,-3.20815146303399));
#75864=CARTESIAN_POINT('Ctrl Pts',(39.4840891062275,0.405920853984631,-3.19864663684755));
#75865=CARTESIAN_POINT('Ctrl Pts',(39.4902464925936,0.504945397976867,-3.18451172386564));
#75866=CARTESIAN_POINT('Ctrl Pts',(39.4964038789598,0.603018062348049,-3.16583113557593));
#75867=CARTESIAN_POINT('Ctrl Pts',(39.5025647016968,0.701145460013106,-3.14714012185183));
#75868=CARTESIAN_POINT('Ctrl Pts',(39.5087255244338,0.798319497638805,-3.12389848167956));
#75869=CARTESIAN_POINT('Ctrl Pts',(39.5148863471707,0.894096583169992,-3.09624108597243));
#75870=CARTESIAN_POINT('Ctrl Pts',(39.5210574700874,0.990033796858899,-3.06853745031347));
#75871=CARTESIAN_POINT('Ctrl Pts',(39.5272285930041,1.08456898182438,-3.03640345240416));
#75872=CARTESIAN_POINT('Ctrl Pts',(39.5333997159208,1.17727656341207,-3.00002290920264));
#75873=CARTESIAN_POINT('Ctrl Pts',(39.5380952378663,1.24781647806625,-2.97234145782015));
#75874=CARTESIAN_POINT('Ctrl Pts',(39.5427907598119,1.31729868019305,-2.94220249278023));
#75875=CARTESIAN_POINT('Ctrl Pts',(39.5474862817574,1.38554562870939,-2.90970460240628));
#75876=CARTESIAN_POINT('Ctrl Pts',(39.5536585298502,1.47525601718202,-2.86698623281809));
#75877=CARTESIAN_POINT('Ctrl Pts',(39.5598307779429,1.56314685124062,-2.82003993606994));
#75878=CARTESIAN_POINT('Ctrl Pts',(39.5660030260357,1.64879217280522,-2.7690435051469));
#75879=CARTESIAN_POINT('Ctrl Pts',(39.5721669146883,1.73432149985249,-2.71811614170219));
#75880=CARTESIAN_POINT('Ctrl Pts',(39.578330803341,1.81761098924881,-2.66314976706568));
#75881=CARTESIAN_POINT('Ctrl Pts',(39.5844946919936,1.89825647668429,-2.6043693883983));
#75882=CARTESIAN_POINT('Ctrl Pts',(39.5906520536521,1.97881656792768,-2.5456512527735));
#75883=CARTESIAN_POINT('Ctrl Pts',(39.5968094153107,2.05673787429803,-2.4831273968415));
#75884=CARTESIAN_POINT('Ctrl Pts',(39.6029667769692,2.13164342305119,-2.41706720623622));
#75885=CARTESIAN_POINT('Ctrl Pts',(39.6091196411155,2.20649425865922,-2.3510552678747));
#75886=CARTESIAN_POINT('Ctrl Pts',(39.6152725052618,2.27833339138376,-2.28151241680965));
#75887=CARTESIAN_POINT('Ctrl Pts',(39.6214253694081,2.34681602731882,-2.20874898900249));
#75888=CARTESIAN_POINT('Ctrl Pts',(39.6275759025447,2.41527271863851,-2.13601312758673));
#75889=CARTESIAN_POINT('Ctrl Pts',(39.6337264356812,2.48037514247187,-2.06005942975104));
#75890=CARTESIAN_POINT('Ctrl Pts',(39.6398769688177,2.54181521371162,-1.98123521618312));
#75891=CARTESIAN_POINT('Ctrl Pts',(39.6460268170329,2.60324844300542,-1.90241978045346));
#75892=CARTESIAN_POINT('Ctrl Pts',(39.6521766652481,2.66101986350874,-1.8207348071182));
#75893=CARTESIAN_POINT('Ctrl Pts',(39.6583265134633,2.7148622052112,-1.73656003904725));
#75894=CARTESIAN_POINT('Ctrl Pts',(39.6644773218425,2.76871295321453,-1.65237212893226));
#75895=CARTESIAN_POINT('Ctrl Pts',(39.6706281302216,2.81863316988512,-1.5656940179242));
#75896=CARTESIAN_POINT('Ctrl Pts',(39.6767789386008,2.8643999253652,-1.47693284548345));
#75897=CARTESIAN_POINT('Ctrl Pts',(39.6829363249669,2.91021562613935,-1.38807674733426));
#75898=CARTESIAN_POINT('Ctrl Pts',(39.6890937113331,2.95186879620757,-1.29713352603029));
#75899=CARTESIAN_POINT('Ctrl Pts',(39.6952510976993,2.98918341262852,-1.20453314116572));
#75900=CARTESIAN_POINT('Ctrl Pts',(39.7014119204363,3.02651885393352,-1.11188107702733));
#75901=CARTESIAN_POINT('Ctrl Pts',(39.7075727431732,3.05951077617051,-1.01757041753712));
#75902=CARTESIAN_POINT('Ctrl Pts',(39.7137335659102,3.08803277918776,-0.922047242369904));
#75903=CARTESIAN_POINT('Ctrl Pts',(39.7199046888269,3.1166024676798,-0.826364363553567));
#75904=CARTESIAN_POINT('Ctrl Pts',(39.7260758117436,3.1406872046676,-0.729465341565102));
#75905=CARTESIAN_POINT('Ctrl Pts',(39.7322469346602,3.16021150604174,-0.631807565308799));
#75906=CARTESIAN_POINT('Ctrl Pts',(39.7369424566059,3.17506727650892,-0.557501116099729));
#75907=CARTESIAN_POINT('Ctrl Pts',(39.7416379785515,3.18728384858711,-0.482755621299704));
#75908=CARTESIAN_POINT('Ctrl Pts',(39.7463335004971,3.19684815737126,-0.4077737377664));
#75909=CARTESIAN_POINT('Ctrl Pts',(39.7525057485899,3.20942040968641,-0.309210299454161));
#75910=CARTESIAN_POINT('Ctrl Pts',(39.7586779966826,3.21745224028383,-0.209891403028772));
#75911=CARTESIAN_POINT('Ctrl Pts',(39.7648502447754,3.22086289031212,-0.110271502711622));
#75912=CARTESIAN_POINT('Ctrl Pts',(39.771014133428,3.22426892109563,-0.0107865235091495));
#75913=CARTESIAN_POINT('Ctrl Pts',(39.7771780220807,3.22306619650828,0.0889982190027945));
#75914=CARTESIAN_POINT('Ctrl Pts',(39.7833419107333,3.21722545879891,0.188621074528142));
#75915=CARTESIAN_POINT('Ctrl Pts',(39.7894992723919,3.21139090589634,0.288138438565025));
#75916=CARTESIAN_POINT('Ctrl Pts',(39.7956566340504,3.20092812914673,0.38749382518187));
#75917=CARTESIAN_POINT('Ctrl Pts',(39.8018139957089,3.18585990512401,0.486224461975343));
#75918=CARTESIAN_POINT('Ctrl Pts',(39.8079668598553,3.17080268736108,0.584882983101115));
#75919=CARTESIAN_POINT('Ctrl Pts',(39.8141197240016,3.15114677577036,0.682917233567107));
#75920=CARTESIAN_POINT('Ctrl Pts',(39.8202725881479,3.12696679413358,0.779869367834104));
#75921=CARTESIAN_POINT('Ctrl Pts',(39.8264231212844,3.1027959730718,0.876784771829329));
#75922=CARTESIAN_POINT('Ctrl Pts',(39.832573654421,3.07410459255443,0.972618453214989));
#75923=CARTESIAN_POINT('Ctrl Pts',(39.8387241875575,3.041018237068,1.0669234482004));
#75924=CARTESIAN_POINT('Ctrl Pts',(39.8448740357727,3.00793556606715,1.16121794141284));
#75925=CARTESIAN_POINT('Ctrl Pts',(39.8510238839879,2.97045903694599,1.25398367679397));
#75926=CARTESIAN_POINT('Ctrl Pts',(39.8571737322032,2.92876357716053,1.34479049357059));
#75927=CARTESIAN_POINT('Ctrl Pts',(39.8633245405823,2.88706160754345,1.43561148784018));
#75928=CARTESIAN_POINT('Ctrl Pts',(39.8694753489614,2.84113958019999,1.52447256123594));
#75929=CARTESIAN_POINT('Ctrl Pts',(39.8756261573406,2.79121944401683,1.61096603869927));
#75930=CARTESIAN_POINT('Ctrl Pts',(39.8817835437068,2.74124592070318,1.69755201668283));
#75931=CARTESIAN_POINT('Ctrl Pts',(39.887940930073,2.68726596781312,1.78176496559147));
#75932=CARTESIAN_POINT('Ctrl Pts',(39.8940983164391,2.62954609378327,1.86322432980281));
#75933=CARTESIAN_POINT('Ctrl Pts',(39.9002591391761,2.57179400691569,1.94472915560474));
#75934=CARTESIAN_POINT('Ctrl Pts',(39.9064199619131,2.51029810961894,2.02347699393736));
#75935=CARTESIAN_POINT('Ctrl Pts',(39.91258078465,2.44536530223564,2.0991203160186));
#75936=CARTESIAN_POINT('Ctrl Pts',(39.9187519075667,2.38032393474356,2.17489010494463));
#75937=CARTESIAN_POINT('Ctrl Pts',(39.9249230304834,2.31183447757354,2.24754469375133));
#75938=CARTESIAN_POINT('Ctrl Pts',(39.9310941534001,2.24024087531824,2.31677326966913));
#75939=CARTESIAN_POINT('Ctrl Pts',(39.9357896753457,2.1857662950696,2.36944833413767));
#75940=CARTESIAN_POINT('Ctrl Pts',(39.9404851972912,2.12949534416398,2.42014067784178));
#75941=CARTESIAN_POINT('Ctrl Pts',(39.9451807192367,2.07159143502863,2.46872973182891));
#75942=CARTESIAN_POINT('Ctrl Pts',(39.9513534852644,1.99547055063582,2.5326052424212));
#75943=CARTESIAN_POINT('Ctrl Pts',(39.9575262512921,1.91625859641018,2.59306922074264));
#75944=CARTESIAN_POINT('Ctrl Pts',(39.9636990173197,1.83429428297196,2.6498079262385));
#75945=CARTESIAN_POINT('Ctrl Pts',(39.9648183560767,1.81943128114891,2.66009664150796));
#75946=CARTESIAN_POINT('Ctrl Pts',(39.9659376948337,1.80447787411704,2.67026295732891));
#75947=CARTESIAN_POINT('Ctrl Pts',(39.9670570335907,1.78943621037801,2.68030513402635));
#75948=CARTESIAN_POINT('Ctrl Pts',(38.7168453967856,1.78943621037806,2.68030513402632));
#75949=CARTESIAN_POINT('Ctrl Pts',(38.7230162077639,1.70636363716969,2.73576638308381));
#75950=CARTESIAN_POINT('Ctrl Pts',(38.7291870187422,1.6208043826183,2.78729911578586));
#75951=CARTESIAN_POINT('Ctrl Pts',(38.7353578297205,1.53317310434257,2.83469536187234));
#75952=CARTESIAN_POINT('Ctrl Pts',(38.7409376887467,1.45393389562647,2.87755267389499));
#75953=CARTESIAN_POINT('Ctrl Pts',(38.7465175477728,1.37300103670098,2.91702834418697));
#75954=CARTESIAN_POINT('Ctrl Pts',(38.7520974067989,1.29069388353065,2.95300302429858));
#75955=CARTESIAN_POINT('Ctrl Pts',(38.7582696548917,1.19964854227786,2.9927969778137));
#75956=CARTESIAN_POINT('Ctrl Pts',(38.7644419029845,1.10660086958338,3.02844643918464));
#75957=CARTESIAN_POINT('Ctrl Pts',(38.7706141510772,1.0119642434491,3.05974605686166));
#75958=CARTESIAN_POINT('Ctrl Pts',(38.7767780397299,0.917455789287036,3.09100328361784));
#75959=CARTESIAN_POINT('Ctrl Pts',(38.7829419283825,0.821363067822642,3.1179222409927));
#75960=CARTESIAN_POINT('Ctrl Pts',(38.7891058170351,0.724120851622665,3.14034497384368));
#75961=CARTESIAN_POINT('Ctrl Pts',(38.7952631786937,0.626981606031848,3.16274396307228));
#75962=CARTESIAN_POINT('Ctrl Pts',(38.8014205403522,0.528695706567802,3.18065609621248));
#75963=CARTESIAN_POINT('Ctrl Pts',(38.8075779020108,0.429713641743179,3.19397303504582));
#75964=CARTESIAN_POINT('Ctrl Pts',(38.8137307661571,0.330803876236448,3.20728024680794));
#75965=CARTESIAN_POINT('Ctrl Pts',(38.8198836303034,0.231199385550903,3.21599887973733));
#75966=CARTESIAN_POINT('Ctrl Pts',(38.8260364944497,0.131360516853901,3.22007173477733));
#75967=CARTESIAN_POINT('Ctrl Pts',(38.8321870275863,0.03155947206669,3.22414304681806));
#75968=CARTESIAN_POINT('Ctrl Pts',(38.8383375607228,-0.0684753407663051,
3.22357206049524));
#75969=CARTESIAN_POINT('Ctrl Pts',(38.8444880938593,-0.168279679590285,
3.21835354054476));
#75970=CARTESIAN_POINT('Ctrl Pts',(38.8506379420745,-0.26807290423622,3.21313560172693));
#75971=CARTESIAN_POINT('Ctrl Pts',(38.8567877902898,-0.367635272116785,
3.20327118092356));
#75972=CARTESIAN_POINT('Ctrl Pts',(38.862937638505,-0.466504783521725,3.18880712013934));
#75973=CARTESIAN_POINT('Ctrl Pts',(38.8690884468841,-0.565389731232556,
3.17434080110924));
#75974=CARTESIAN_POINT('Ctrl Pts',(38.8752392552632,-0.663581177764809,
3.15527347858415));
#75975=CARTESIAN_POINT('Ctrl Pts',(38.8813900636424,-0.760625472054809,
3.13170344281853));
#75976=CARTESIAN_POINT('Ctrl Pts',(38.8875474500086,-0.857773550444737,
3.10810820005887));
#75977=CARTESIAN_POINT('Ctrl Pts',(38.8937048363748,-0.953771603827205,
3.0800007308617));
#75978=CARTESIAN_POINT('Ctrl Pts',(38.8998622227409,-1.04817946896395,3.04752971492362));
#75979=CARTESIAN_POINT('Ctrl Pts',(38.9060230454779,-1.14264002210968,3.01504057726256));
#75980=CARTESIAN_POINT('Ctrl Pts',(38.9121838682149,-1.2355082158781,2.97818320333855));
#75981=CARTESIAN_POINT('Ctrl Pts',(38.9183446909518,-1.32636421616619,2.93715432495023));
#75982=CARTESIAN_POINT('Ctrl Pts',(38.9245158138685,-1.41737211712934,2.89605685104478));
#75983=CARTESIAN_POINT('Ctrl Pts',(38.9306869367852,-1.50636071750334,2.85077413887356));
#75984=CARTESIAN_POINT('Ctrl Pts',(38.9368580597019,-1.59293499430201,2.80154879779526));
#75985=CARTESIAN_POINT('Ctrl Pts',(38.9415535816474,-1.65880816230022,2.76409391763309));
#75986=CARTESIAN_POINT('Ctrl Pts',(38.946249103593,-1.72328407819148,2.72435741179683));
#75987=CARTESIAN_POINT('Ctrl Pts',(38.9509446255386,-1.78620106900576,2.68246217188289));
#75988=CARTESIAN_POINT('Ctrl Pts',(38.9570996536215,-1.86867450856015,2.6275446608586));
#75989=CARTESIAN_POINT('Ctrl Pts',(38.9632546817044,-1.94876206316078,2.56872070059939));
#75990=CARTESIAN_POINT('Ctrl Pts',(38.9694097097873,-2.02606874386555,2.5062248517703));
#75991=CARTESIAN_POINT('Ctrl Pts',(38.9755563907508,-2.10327058539179,2.44381375646308));
#75992=CARTESIAN_POINT('Ctrl Pts',(38.9817030717144,-2.17769871098348,2.37774094112655));
#75993=CARTESIAN_POINT('Ctrl Pts',(38.987849752678,-2.24898631620097,2.3082846687618));
#75994=CARTESIAN_POINT('Ctrl Pts',(38.9939899412545,-2.32019862440445,2.23890175907908));
#75995=CARTESIAN_POINT('Ctrl Pts',(39.0001301298311,-2.38827669489437,2.16614279976821));
#75996=CARTESIAN_POINT('Ctrl Pts',(39.0062703184076,-2.45288688390502,2.09032617006694));
#75997=CARTESIAN_POINT('Ctrl Pts',(39.0124060784873,-2.51745047401732,2.01456422170115));
#75998=CARTESIAN_POINT('Ctrl Pts',(39.0185418385669,-2.5785508720124,1.93574931853243));
#75999=CARTESIAN_POINT('Ctrl Pts',(39.0246775986465,-2.63589207408145,1.85423583621249));
#76000=CARTESIAN_POINT('Ctrl Pts',(39.0308110992547,-2.69321216045984,1.77275237093813));
#76001=CARTESIAN_POINT('Ctrl Pts',(39.0369445998628,-2.74677554998505,1.68857265798243));
#76002=CARTESIAN_POINT('Ctrl Pts',(39.043078100471,-2.79632782779313,1.6020824704146));
#76003=CARTESIAN_POINT('Ctrl Pts',(39.0492110074707,-2.84587530986541,1.51560065348296));
#76004=CARTESIAN_POINT('Ctrl Pts',(39.0553439144704,-2.89141223479319,1.42680918583746));
#76005=CARTESIAN_POINT('Ctrl Pts',(39.0614768214701,-2.93272921113104,1.33612010563375));
#76006=CARTESIAN_POINT('Ctrl Pts',(39.0676107997968,-2.97405340492551,1.24541518340671));
#76007=CARTESIAN_POINT('Ctrl Pts',(39.0737447781235,-3.01115600500093,1.15281238812868));
#76008=CARTESIAN_POINT('Ctrl Pts',(39.0798787564502,-3.04387542830063,1.05874451095988));
#76009=CARTESIAN_POINT('Ctrl Pts',(39.0860193054742,-3.07662990053854,0.96457586859163));
#76010=CARTESIAN_POINT('Ctrl Pts',(39.0921598544982,-3.10499167842174,0.868939424699028));
#76011=CARTESIAN_POINT('Ctrl Pts',(39.0983004035222,-3.12884888736368,0.772283757787963));
#76012=CARTESIAN_POINT('Ctrl Pts',(39.1044445273219,-3.15271998499353,0.67557182191448));
#76013=CARTESIAN_POINT('Ctrl Pts',(39.1105886511215,-3.17208120795575,0.577839910274741));
#76014=CARTESIAN_POINT('Ctrl Pts',(39.1167327749211,-3.186872104492,0.479545359805227));
#76015=CARTESIAN_POINT('Ctrl Pts',(39.1228868640422,-3.20168699078554,0.381091382731454));
#76016=CARTESIAN_POINT('Ctrl Pts',(39.1290409531633,-3.21191670436259,0.282073379134371));
#76017=CARTESIAN_POINT('Ctrl Pts',(39.1351950422844,-3.2175527969399,0.18295234735923));
#76018=CARTESIAN_POINT('Ctrl Pts',(39.1389878445938,-3.22102635484947,0.12186345657096));
#76019=CARTESIAN_POINT('Ctrl Pts',(39.1427806469031,-3.22275613433671,0.0607354334618325));
#76020=CARTESIAN_POINT('Ctrl Pts',(39.1465734492125,-3.22274998364956,-0.000324633233696488));
#76021=CARTESIAN_POINT('',(38.9000265507268,-3.22274891038197,-0.0026501192081339));
#76022=CARTESIAN_POINT('Ctrl Pts',(38.470402238185,1.78943621037805,2.68030513402632));
#76023=CARTESIAN_POINT('Ctrl Pts',(38.476552475551,1.70631879105963,2.73579632342613));
#76024=CARTESIAN_POINT('Ctrl Pts',(38.482702712917,1.62062405282665,2.78741343758364));
#76025=CARTESIAN_POINT('Ctrl Pts',(38.488852950283,1.53275302880884,2.83492252366398));
#76026=CARTESIAN_POINT('Ctrl Pts',(38.4952501026987,1.44135422578376,2.88433896838047));
#76027=CARTESIAN_POINT('Ctrl Pts',(38.5016472551144,1.3476011671571,2.92931035327353));
#76028=CARTESIAN_POINT('Ctrl Pts',(38.5080444075302,1.25197141895709,2.96962710261989));
#76029=CARTESIAN_POINT('Ctrl Pts',(38.5142038541353,1.15989508723702,3.00844575953955));
#76030=CARTESIAN_POINT('Ctrl Pts',(38.5203633007404,1.0660794941757,3.04294945474506));
#76031=CARTESIAN_POINT('Ctrl Pts',(38.5265227473455,0.970968081115809,3.07300155352292));
#76032=CARTESIAN_POINT('Ctrl Pts',(38.5326865903696,0.875788780523907,3.10307510254268));
#76033=CARTESIAN_POINT('Ctrl Pts',(38.5388504333938,0.779312237762846,3.12869061971578));
#76034=CARTESIAN_POINT('Ctrl Pts',(38.5450142764179,0.681993285611378,3.14976232768141));
#76035=CARTESIAN_POINT('Ctrl Pts',(38.5511872779008,0.584529733474962,3.17086534474549));
#76036=CARTESIAN_POINT('Ctrl Pts',(38.5573602793837,0.486221701546851,3.18741101349978));
#76037=CARTESIAN_POINT('Ctrl Pts',(38.5635332808666,0.387530032000321,3.19936525529641));
#76038=CARTESIAN_POINT('Ctrl Pts',(38.5642284470017,0.376415972384852,3.20071146979045));
#76039=CARTESIAN_POINT('Ctrl Pts',(38.5649236131368,0.365297047613253,3.20199951063944));
#76040=CARTESIAN_POINT('Ctrl Pts',(38.565618779272,0.354173915195078,3.20322937054083));
#76041=CARTESIAN_POINT('Ctrl Pts',(38.5717910273647,0.255413734879611,3.21414906303909));
#76042=CARTESIAN_POINT('Ctrl Pts',(38.5779632754575,0.155974247973943,3.22051631785057));
#76043=CARTESIAN_POINT('Ctrl Pts',(38.5841355235503,0.0563111975495212,
3.22225799890861));
#76044=CARTESIAN_POINT('Ctrl Pts',(38.5902994122029,-0.0432168733195461,
3.22399732110514));
#76045=CARTESIAN_POINT('Ctrl Pts',(38.5964633008555,-0.142967475403352,
3.22112351378161));
#76046=CARTESIAN_POINT('Ctrl Pts',(38.6026271895082,-0.242478533134772,
3.21361505527168));
#76047=CARTESIAN_POINT('Ctrl Pts',(38.6087845511667,-0.34188421776127,3.20611454753229));
#76048=CARTESIAN_POINT('Ctrl Pts',(38.6149419128253,-0.441050431570951,
3.19398917802298));
#76049=CARTESIAN_POINT('Ctrl Pts',(38.6210992744838,-0.539514848547188,
3.17726947089747));
#76050=CARTESIAN_POINT('Ctrl Pts',(38.6272521386301,-0.637907344310258,
3.16056197632201));
#76051=CARTESIAN_POINT('Ctrl Pts',(38.6334050027764,-0.735598635446793,
3.13926688860308));
#76052=CARTESIAN_POINT('Ctrl Pts',(38.6395578669228,-0.832132190479647,
3.1134664893118));
#76053=CARTESIAN_POINT('Ctrl Pts',(38.6457084000593,-0.928629173819252,
3.08767586449001));
#76054=CARTESIAN_POINT('Ctrl Pts',(38.6518589331958,-1.02396887338675,3.05738343160187));
#76055=CARTESIAN_POINT('Ctrl Pts',(38.6580094663324,-1.11770649144595,3.02272224352149));
#76056=CARTESIAN_POINT('Ctrl Pts',(38.6641593145476,-1.21143367091506,2.98806491529953));
#76057=CARTESIAN_POINT('Ctrl Pts',(38.6703091627628,-1.30355871616046,2.94903994977381));
#76058=CARTESIAN_POINT('Ctrl Pts',(38.676459010978,-1.39365445653052,2.90582945444027));
#76059=CARTESIAN_POINT('Ctrl Pts',(38.6826098193571,-1.48376426337474,2.86261221273544));
#76060=CARTESIAN_POINT('Ctrl Pts',(38.6887606277363,-1.57184374433822,2.81520833110536));
#76061=CARTESIAN_POINT('Ctrl Pts',(38.6949114361154,-1.65748899887154,2.76384655527759));
#76062=CARTESIAN_POINT('Ctrl Pts',(38.7010688224816,-1.74322584679221,2.71242985055675));
#76063=CARTESIAN_POINT('Ctrl Pts',(38.7072262088478,-1.8265228965419,2.657047023066));
#76064=CARTESIAN_POINT('Ctrl Pts',(38.713383595214,-1.90700410951207,2.59797091762092));
#76065=CARTESIAN_POINT('Ctrl Pts',(38.7195444179509,-1.98753023817731,2.53886184243992));
#76066=CARTESIAN_POINT('Ctrl Pts',(38.7257052406879,-2.06523706262828,2.47605565755229));
#76067=CARTESIAN_POINT('Ctrl Pts',(38.7318660634249,-2.13978224297069,2.40986504086169));
#76068=CARTESIAN_POINT('Ctrl Pts',(38.7380371863416,-2.21445205419244,2.34356376115138));
#76069=CARTESIAN_POINT('Ctrl Pts',(38.7442083092582,-2.28594935169415,2.27386705055432));
#76070=CARTESIAN_POINT('Ctrl Pts',(38.7503794321749,-2.35396912688206,2.20112401108755));
#76071=CARTESIAN_POINT('Ctrl Pts',(38.7550749541204,-2.40572443161908,2.14577483998694));
#76072=CARTESIAN_POINT('Ctrl Pts',(38.7597704760659,-2.45546720706799,2.08866275793249));
#76073=CARTESIAN_POINT('Ctrl Pts',(38.7644659980114,-2.50307963811206,2.02995317378722));
#76074=CARTESIAN_POINT('Ctrl Pts',(38.770617892004,-2.56545963162721,1.95303411298838));
#76075=CARTESIAN_POINT('Ctrl Pts',(38.7767697859965,-2.62440669444763,1.87309396875357));
#76076=CARTESIAN_POINT('Ctrl Pts',(38.7829216799891,-2.67961273722208,1.79047288195526));
#76077=CARTESIAN_POINT('Ctrl Pts',(38.7890655633465,-2.73474689392971,1.7079593794841));
#76078=CARTESIAN_POINT('Ctrl Pts',(38.795209446704,-2.78614946672464,1.6227722284766));
#76079=CARTESIAN_POINT('Ctrl Pts',(38.8013533300615,-2.83355202996752,1.53528513832675));
#76080=CARTESIAN_POINT('Ctrl Pts',(38.8074908818402,-2.88090574250036,1.44788820799485));
#76081=CARTESIAN_POINT('Ctrl Pts',(38.8136284336188,-2.92426742931672,1.3581964298393));
#76082=CARTESIAN_POINT('Ctrl Pts',(38.8197659853975,-2.96341207728283,1.26661218323301));
#76083=CARTESIAN_POINT('Ctrl Pts',(38.8258988786077,-3.00252701339788,1.1750974515575));
#76084=CARTESIAN_POINT('Ctrl Pts',(38.8320317718178,-3.03743110192722,1.081693507172));
#76085=CARTESIAN_POINT('Ctrl Pts',(38.838164665028,-3.06794586854737,0.986826078984108));
#76086=CARTESIAN_POINT('Ctrl Pts',(38.8442952427761,-3.09844911437588,0.891994467811846));
#76087=CARTESIAN_POINT('Ctrl Pts',(38.8504258205242,-3.12456619503217,0.795700885438159));
#76088=CARTESIAN_POINT('Ctrl Pts',(38.8565563982723,-3.14616759141027,0.698388895429812));
#76089=CARTESIAN_POINT('Ctrl Pts',(38.8626856552264,-3.16776433390495,0.601097870670672));
#76090=CARTESIAN_POINT('Ctrl Pts',(38.8688149121805,-3.18484723621972,0.502789302088776));
#76091=CARTESIAN_POINT('Ctrl Pts',(38.8749441691346,-3.19733754636273,0.403918527823539));
#76092=CARTESIAN_POINT('Ctrl Pts',(38.8810752541797,-3.20983158182246,0.305018264703097));
#76093=CARTESIAN_POINT('Ctrl Pts',(38.8872063392248,-3.21773023802526,0.205555895204617));
#76094=CARTESIAN_POINT('Ctrl Pts',(38.8933374242699,-3.22100653419584,0.105992778846848));
#76095=CARTESIAN_POINT('Ctrl Pts',(38.8955671330889,-3.22219803397303,0.0697843822980494));
#76096=CARTESIAN_POINT('Ctrl Pts',(38.8977968419078,-3.22277868876192,0.0335626825532226));
#76097=CARTESIAN_POINT('Ctrl Pts',(38.9000265507268,-3.22274891038197,-0.0026501192081339));
#76098=CARTESIAN_POINT('Ctrl Pts',(38.8985201488241,-3.22274882644913,-0.00275029466297132));
#76099=CARTESIAN_POINT('Ctrl Pts',(38.9060646964583,-3.22265200588648,-0.116202994426138));
#76100=CARTESIAN_POINT('Ctrl Pts',(38.9137273955404,-3.21656432972955,-0.229568442334264));
#76101=CARTESIAN_POINT('Ctrl Pts',(38.9342509370667,-3.18435131639635,-0.531072642175193));
#76102=CARTESIAN_POINT('Ctrl Pts',(38.9471159326192,-3.14756042191507,-0.717641260126694));
#76103=CARTESIAN_POINT('Ctrl Pts',(38.9608598654036,-3.08753583555694,-0.924052271636377));
#76104=CARTESIAN_POINT('Ctrl Pts',(38.9624543148532,-3.08023007553678,-0.948120726273012));
#76105=CARTESIAN_POINT('Ctrl Pts',(38.9644870520352,-3.07046149605965,-0.97899748198622));
#76106=CARTESIAN_POINT('Ctrl Pts',(38.9649397043297,-3.06825673625823,-0.98588562791305));
#76107=CARTESIAN_POINT('Ctrl Pts',(38.9656676598682,-3.06466302342795,-0.996984338830863));
#76108=CARTESIAN_POINT('Ctrl Pts',(38.9659438049694,-3.06328855223262,-1.00119951326819));
#76109=CARTESIAN_POINT('Ctrl Pts',(38.9664722423174,-3.06063669072522,-1.00927555579891));
#76110=CARTESIAN_POINT('Ctrl Pts',(38.9667246121572,-3.059360694359,-1.01313683286044));
#76111=CARTESIAN_POINT('Ctrl Pts',(38.9673084352517,-3.05638682379991,-1.02207917769647));
#76112=CARTESIAN_POINT('Ctrl Pts',(38.9676395701081,-3.05468357482492,-1.02715846920368));
#76113=CARTESIAN_POINT('Ctrl Pts',(38.9687082890737,-3.04913324897155,-1.04357429444997));
#76114=CARTESIAN_POINT('Ctrl Pts',(38.9694429366095,-3.04523561314486,-1.05489380931277));
#76115=CARTESIAN_POINT('Ctrl Pts',(38.9785458355029,-2.99592728416941,-1.1955441310358));
#76116=CARTESIAN_POINT('Ctrl Pts',(38.9864568303832,-2.94236691354503,-1.32188994192928));
#76117=CARTESIAN_POINT('Ctrl Pts',(39.0028115940323,-2.81287013402245,-1.58016675697157));
#76118=CARTESIAN_POINT('Ctrl Pts',(39.0112054661125,-2.73532043748411,-1.71090307810846));
#76119=CARTESIAN_POINT('Ctrl Pts',(39.0267281531353,-2.57809726251247,-1.93777140170975));
#76120=CARTESIAN_POINT('Ctrl Pts',(39.0337946066843,-2.50151456522588,-2.03567301473938));
#76121=CARTESIAN_POINT('Ctrl Pts',(39.0439903946623,-2.38644791646327,-2.16644504998062));
#76122=CARTESIAN_POINT('Ctrl Pts',(39.0469478315879,-2.35254913044546,-2.20320902624393));
#76123=CARTESIAN_POINT('Ctrl Pts',(39.0519244990418,-2.29478016659834,-2.26300689593011));
#76124=CARTESIAN_POINT('Ctrl Pts',(39.0539236213976,-2.27138455005892,-2.28648820800489));
#76125=CARTESIAN_POINT('Ctrl Pts',(39.0566366021057,-2.23940584424875,-2.31760884744372));
#76126=CARTESIAN_POINT('Ctrl Pts',(39.0573363451112,-2.23113750439746,-2.32556976591372));
#76127=CARTESIAN_POINT('Ctrl Pts',(39.0584497265335,-2.21795047446691,-2.33813143608706));
#76128=CARTESIAN_POINT('Ctrl Pts',(39.0588621018268,-2.21305953287834,-2.34276128157625));
#76129=CARTESIAN_POINT('Ctrl Pts',(39.0597184350409,-2.20288941492897,-2.35232821530745));
#76130=CARTESIAN_POINT('Ctrl Pts',(39.0601624911539,-2.19760807407725,-2.35726293788632));
#76131=CARTESIAN_POINT('Ctrl Pts',(39.0611779641854,-2.18551370124927,-2.36848757744297));
#76132=CARTESIAN_POINT('Ctrl Pts',(39.0617498705785,-2.17869005764982,-2.37476591955278));
#76133=CARTESIAN_POINT('Ctrl Pts',(39.0632399616886,-2.1608802763392,-2.39101108865657));
#76134=CARTESIAN_POINT('Ctrl Pts',(39.0641600961901,-2.14985234712002,-2.40093158346605));
#76135=CARTESIAN_POINT('Ctrl Pts',(39.0700523123043,-2.07904657484831,-2.46374801164275));
#76136=CARTESIAN_POINT('Ctrl Pts',(39.0751135767923,-2.01739402072552,-2.5144797611));
#76137=CARTESIAN_POINT('Ctrl Pts',(39.0816576877401,-1.93671581623818,-2.57598869790745));
#76138=CARTESIAN_POINT('Ctrl Pts',(39.0830598303985,-1.91937402482795,-2.58893592885779));
#76139=CARTESIAN_POINT('Ctrl Pts',(39.095158199764,-1.76925727623235,-2.69867447022444));
#76140=CARTESIAN_POINT('Ctrl Pts',(39.1061877187551,-1.62940319134005,-2.78534556118557));
#76141=CARTESIAN_POINT('Ctrl Pts',(39.1310554276237,-1.30307727624624,-2.95456318157637));
#76142=CARTESIAN_POINT('Ctrl Pts',(39.144890819654,-1.11411962683837,-3.0308754908564));
#76143=CARTESIAN_POINT('Ctrl Pts',(39.1595655495452,-0.894286465908746,
-3.09629550326156));
#76144=CARTESIAN_POINT('Ctrl Pts',(39.1612152681434,-0.869266249104422,
-3.10341270501232));
#76145=CARTESIAN_POINT('Ctrl Pts',(39.1633077428594,-0.837097675294885,
-3.11214373391211));
#76146=CARTESIAN_POINT('Ctrl Pts',(39.1637659048934,-0.830027083431778,
-3.11403695895987));
#76147=CARTESIAN_POINT('Ctrl Pts',(39.1645005750268,-0.818644567928665,
-3.11704322457693));
#76148=CARTESIAN_POINT('Ctrl Pts',(39.164777952878,-0.814336731143821,-3.11817143232451));
#76149=CARTESIAN_POINT('Ctrl Pts',(39.1653072340641,-0.806096638369069,
-3.12031124372292));
#76150=CARTESIAN_POINT('Ctrl Pts',(39.1655592207741,-0.802164820393485,
-3.12132434219196));
#76151=CARTESIAN_POINT('Ctrl Pts',(39.1661401310563,-0.793080681372778,
-3.12364672387928));
#76152=CARTESIAN_POINT('Ctrl Pts',(39.1664687462443,-0.787926995002609,
-3.1249506994953));
#76153=CARTESIAN_POINT('Ctrl Pts',(39.1675211914722,-0.771374672504296,
-3.12909518440884));
#76154=CARTESIAN_POINT('Ctrl Pts',(39.1682422086155,-0.75996356322609,-3.13188616506836));
#76155=CARTESIAN_POINT('Ctrl Pts',(39.1806045765768,-0.563140756821354,
-3.17888690149245));
#76156=CARTESIAN_POINT('Ctrl Pts',(39.1913569285077,-0.374150769360753,
-3.2066312026352));
#76157=CARTESIAN_POINT('Ctrl Pts',(39.2122694844599,-0.00121749177307916,
-3.2279340295954));
#76158=CARTESIAN_POINT('Ctrl Pts',(39.2224054714749,0.181903165602953,-3.22280421356543));
#76159=CARTESIAN_POINT('Ctrl Pts',(39.2372713190132,0.438304764730845,-3.19369061386641));
#76160=CARTESIAN_POINT('Ctrl Pts',(39.2416620380048,0.512688559534677,-3.18259643223032));
#76161=CARTESIAN_POINT('Ctrl Pts',(39.2479097065956,0.6160283649675,-3.16346669759801));
#76162=CARTESIAN_POINT('Ctrl Pts',(39.2497001187966,0.645365995493569,-3.15761225238062));
#76163=CARTESIAN_POINT('Ctrl Pts',(39.2528364200477,0.69624236187107,-3.14672102609189));
#76164=CARTESIAN_POINT('Ctrl Pts',(39.2541764172686,0.717818903528417,-3.14186928860523));
#76165=CARTESIAN_POINT('Ctrl Pts',(39.2561215146016,0.748897947416826,-3.13454395213167));
#76166=CARTESIAN_POINT('Ctrl Pts',(39.2567208830823,0.758442074818032,-3.13224832018168));
#76167=CARTESIAN_POINT('Ctrl Pts',(39.2577709951808,0.775105787075725,-3.12815960006328));
#76168=CARTESIAN_POINT('Ctrl Pts',(39.2582211157141,0.782230044702907,-3.12638571202832));
#76169=CARTESIAN_POINT('Ctrl Pts',(39.2590874270533,0.795905698927279,-3.12293090332341));
#76170=CARTESIAN_POINT('Ctrl Pts',(39.2595034963001,0.802457994069226,-3.12125367042773));
#76171=CARTESIAN_POINT('Ctrl Pts',(39.2604847552606,0.817873446638981,-3.11725592919275));
#76172=CARTESIAN_POINT('Ctrl Pts',(39.2610505002606,0.826732049784069,-3.11491823614743));
#76173=CARTESIAN_POINT('Ctrl Pts',(39.2627263144103,0.85288540520665,-3.10789721351607));
#76174=CARTESIAN_POINT('Ctrl Pts',(39.2638398349749,0.87015098637429,-3.10310744967131));
#76175=CARTESIAN_POINT('Ctrl Pts',(39.2784167370843,1.09468522842714,-3.03879660971757));
#76176=CARTESIAN_POINT('Ctrl Pts',(39.2925765874064,1.29547090309156,-2.95877390785682));
#76177=CARTESIAN_POINT('Ctrl Pts',(39.3236060632252,1.70446215143974,-2.7461154021794));
#76178=CARTESIAN_POINT('Ctrl Pts',(39.3404844841917,1.90855728384211,-2.60840224484998));
#76179=CARTESIAN_POINT('Ctrl Pts',(39.3580334495631,2.11659345332662,-2.43042249535349));
#76180=CARTESIAN_POINT('Ctrl Pts',(39.3598338094991,2.13789326882415,-2.41170766382542));
#76181=CARTESIAN_POINT('Ctrl Pts',(39.362088067794,2.16454501255764,-2.38765980814599));
#76182=CARTESIAN_POINT('Ctrl Pts',(39.3625603862631,2.17012814276729,-2.38258647639716));
#76183=CARTESIAN_POINT('Ctrl Pts',(39.3633123046844,2.17901559178365,-2.37445338808269));
#76184=CARTESIAN_POINT('Ctrl Pts',(39.3635928476753,2.18233135854243,-2.37140626707652));
#76185=CARTESIAN_POINT('Ctrl Pts',(39.3641244437186,2.18861425477795,-2.36560807787784));
#76186=CARTESIAN_POINT('Ctrl Pts',(39.364375592533,2.1915825543244,-2.36285840500009));
#76187=CARTESIAN_POINT('Ctrl Pts',(39.3649496923495,2.19836757908613,-2.35654933867806));
#76188=CARTESIAN_POINT('Ctrl Pts',(39.3652723563752,2.20218083717264,-2.35298626423987));
#76189=CARTESIAN_POINT('Ctrl Pts',(39.3662869752354,2.21417037657158,-2.34172866957656));
#76190=CARTESIAN_POINT('Ctrl Pts',(39.3669763940253,2.22231522198972,-2.33400057437667));
#76191=CARTESIAN_POINT('Ctrl Pts',(39.3731745779831,2.2955022818334,-2.26382786535447));
#76192=CARTESIAN_POINT('Ctrl Pts',(39.378486609106,2.35794427168836,-2.19871541235758));
#76193=CARTESIAN_POINT('Ctrl Pts',(39.4000428827543,2.60505184109672,-1.91838491640368));
#76194=CARTESIAN_POINT('Ctrl Pts',(39.4153219986218,2.76364748371816,-1.68189455695802));
#76195=CARTESIAN_POINT('Ctrl Pts',(39.4360117104762,2.92279468129681,-1.35982318984196));
#76196=CARTESIAN_POINT('Ctrl Pts',(39.4404311777144,2.95392593481961,-1.29080138369009));
#76197=CARTESIAN_POINT('Ctrl Pts',(39.4467170348712,2.99398351238235,-1.19293080652955));
#76198=CARTESIAN_POINT('Ctrl Pts',(39.4485159481675,3.00497999541645,-1.1649533547499));
#76199=CARTESIAN_POINT('Ctrl Pts',(39.4516768941388,3.02347859342186,-1.11588338236529));
#76200=CARTESIAN_POINT('Ctrl Pts',(39.4530330784389,3.03115539313289,-1.09485865373304));
#76201=CARTESIAN_POINT('Ctrl Pts',(39.4549986572776,3.04190535397881,-1.06443743835153));
#76202=CARTESIAN_POINT('Ctrl Pts',(39.4556021649113,3.04515536944266,-1.05510379359517));
#76203=CARTESIAN_POINT('Ctrl Pts',(39.4566550729737,3.05073726565942,-1.03883264459062));
#76204=CARTESIAN_POINT('Ctrl Pts',(39.4571038260695,3.05308855496693,-1.03190183722951));
#76205=CARTESIAN_POINT('Ctrl Pts',(39.4579707542821,3.05757739782353,-1.01852059176025));
#76206=CARTESIAN_POINT('Ctrl Pts',(39.4583888190526,3.05971820046875,-1.01207127817765));
#76207=CARTESIAN_POINT('Ctrl Pts',(39.4593798229488,3.06473633371996,-0.996792359630693));
#76208=CARTESIAN_POINT('Ctrl Pts',(39.4599533446228,3.06759591682979,-0.987957029224714));
#76209=CARTESIAN_POINT('Ctrl Pts',(39.4619682508713,3.07748604416483,-0.956942299578186));
#76210=CARTESIAN_POINT('Ctrl Pts',(39.4634162599488,3.08431441993459,-0.934699646918499));
#76211=CARTESIAN_POINT('Ctrl Pts',(39.4657510162797,3.0948771344825,-0.898916188733655));
#76212=CARTESIAN_POINT('Ctrl Pts',(39.4666327019952,3.09876491676096,-0.885421240144417));
#76213=CARTESIAN_POINT('Ctrl Pts',(39.483775701864,3.17240055600699,-0.623397018444148));
#76214=CARTESIAN_POINT('Ctrl Pts',(39.5010505570153,3.21211432778571,-0.367449694747811));
#76215=CARTESIAN_POINT('Ctrl Pts',(39.5311854738334,3.22725053041123,0.0774996261143986));
#76216=CARTESIAN_POINT('Ctrl Pts',(39.5438648346921,3.21730558876417,0.2647845740104));
#76217=CARTESIAN_POINT('Ctrl Pts',(39.5574298419839,3.18766600581436,0.474896824223559));
#76218=CARTESIAN_POINT('Ctrl Pts',(39.5590132968879,3.18388915199246,0.499591350544052));
#76219=CARTESIAN_POINT('Ctrl Pts',(39.5610341248735,3.17865181998118,0.531358843038604));
#76220=CARTESIAN_POINT('Ctrl Pts',(39.5614856595138,3.17745431937394,0.538473456559237));
#76221=CARTESIAN_POINT('Ctrl Pts',(39.5622122529664,3.1754830282558,0.549949744264628));
#76222=CARTESIAN_POINT('Ctrl Pts',(39.5624881480203,3.17472412741696,0.554313899627152));
#76223=CARTESIAN_POINT('Ctrl Pts',(39.5630164185219,3.17325101821033,0.562682936220123));
#76224=CARTESIAN_POINT('Ctrl Pts',(39.5632688703792,3.17253822659056,0.566688020208856));
#76225=CARTESIAN_POINT('Ctrl Pts',(39.5638533038773,3.17086766034932,0.575972772740443));
#76226=CARTESIAN_POINT('Ctrl Pts',(39.5641849650229,3.16990427541127,0.581251443099394));
#76227=CARTESIAN_POINT('Ctrl Pts',(39.5652571030804,3.16674036201778,0.598345626927872));
#76228=CARTESIAN_POINT('Ctrl Pts',(39.565994617083,3.16448688921343,0.610151414228941));
#76229=CARTESIAN_POINT('Ctrl Pts',(39.5757634998126,3.13361763792488,0.767100682506316));
#76230=CARTESIAN_POINT('Ctrl Pts',(39.5842616995361,3.09510262022304,0.910140041574776));
#76231=CARTESIAN_POINT('Ctrl Pts',(39.6047211540041,2.97697262499853,1.25291531162425));
#76232=CARTESIAN_POINT('Ctrl Pts',(39.6164973752005,2.88697295120931,1.44829215009111));
#76233=CARTESIAN_POINT('Ctrl Pts',(39.6335266825743,2.73659168282322,1.70409264763878));
#76234=CARTESIAN_POINT('Ctrl Pts',(39.6383081810283,2.69226987087226,1.77328712380675));
#76235=CARTESIAN_POINT('Ctrl Pts',(39.6460531284891,2.6177357392548,1.88040304191996));
#76236=CARTESIAN_POINT('Ctrl Pts',(39.648954254884,2.58922717117262,1.91946822815361));
#76237=CARTESIAN_POINT('Ctrl Pts',(39.6526951964302,2.55178911319659,1.96841713291518));
#76238=CARTESIAN_POINT('Ctrl Pts',(39.6535033561351,2.54366168844175,1.97890851074509));
#76239=CARTESIAN_POINT('Ctrl Pts',(39.6548045851885,2.53051358668526,1.99566605820484));
#76240=CARTESIAN_POINT('Ctrl Pts',(39.6552960212839,2.52553383161893,2.00196425836531));
#76241=CARTESIAN_POINT('Ctrl Pts',(39.6562310272417,2.51603296095574,2.01388872501931));
#76242=CARTESIAN_POINT('Ctrl Pts',(39.6566744135268,2.51151637221115,2.01951854860044));
#76243=CARTESIAN_POINT('Ctrl Pts',(39.6576837967055,2.50120905207499,2.03227832962638));
#76244=CARTESIAN_POINT('Ctrl Pts',(39.65825026175,2.49540669349987,2.0393987747592));
#76245=CARTESIAN_POINT('Ctrl Pts',(39.6597170765945,2.48033640508947,2.05773188190855));
#76246=CARTESIAN_POINT('Ctrl Pts',(39.6606192771946,2.4710229309074,2.0689066784153));
#76247=CARTESIAN_POINT('Ctrl Pts',(39.6662001699113,2.41314484376644,2.13740353205753));
#76248=CARTESIAN_POINT('Ctrl Pts',(39.6709576181331,2.3626672442439,2.19307178784247));
#76249=CARTESIAN_POINT('Ctrl Pts',(39.6776383145208,2.29030238348289,2.26747761828332));
#76250=CARTESIAN_POINT('Ctrl Pts',(39.679494840397,2.27003778255748,2.28776487958639));
#76251=CARTESIAN_POINT('Ctrl Pts',(39.682332450524,2.23882797620103,2.31818661798342));
#76252=CARTESIAN_POINT('Ctrl Pts',(39.6833060080094,2.2280783252365,2.32852031749382));
#76253=CARTESIAN_POINT('Ctrl Pts',(39.6909930169581,2.14286885525137,2.40930235810437));
#76254=CARTESIAN_POINT('Ctrl Pts',(39.6978264002758,2.06516308126227,2.47623172528963));
#76255=CARTESIAN_POINT('Ctrl Pts',(39.7101288006093,1.92114834567543,2.58877417296029));
#76256=CARTESIAN_POINT('Ctrl Pts',(39.7155639546189,1.85611072403138,2.63579163576638));
#76257=CARTESIAN_POINT('Ctrl Pts',(39.7209886430068,1.78943588752252,2.68030534957241));
#76258=CARTESIAN_POINT('Origin',(-1.72497344927317,0.,0.));
#76259=CARTESIAN_POINT('',(41.2170239499866,1.789436210378,2.68030513402635));
#76260=CARTESIAN_POINT('',(40.972917806056,1.78943621030417,2.68030513407564));
#76261=CARTESIAN_POINT('',(-1.72497344927317,1.78943621037804,2.68030513402633));
#76262=CARTESIAN_POINT('',(40.3965734492378,-3.22274866702434,0.00293115895939317));
#76263=CARTESIAN_POINT('Ctrl Pts',(40.3965734492731,-3.22274866702486,0.0029311583875785));
#76264=CARTESIAN_POINT('Ctrl Pts',(40.4026689406047,-3.22283856608011,-0.0959110132575726));
#76265=CARTESIAN_POINT('Ctrl Pts',(40.4087644319364,-3.21837696149856,-0.194856635371052));
#76266=CARTESIAN_POINT('Ctrl Pts',(40.414859923268,-3.20936208299301,-0.293449455182281));
#76267=CARTESIAN_POINT('Ctrl Pts',(40.4209523799394,-3.20035169257419,-0.391993190235922));
#76268=CARTESIAN_POINT('Ctrl Pts',(40.4270448366108,-3.18679257004819,-0.490184030980883));
#76269=CARTESIAN_POINT('Ctrl Pts',(40.4331372932821,-3.16873499236898,-0.587567962568068));
#76270=CARTESIAN_POINT('Ctrl Pts',(40.4392284227892,-3.15068134830373,-0.684930680302494));
#76271=CARTESIAN_POINT('Ctrl Pts',(40.4453195522962,-3.12813127669672,-0.781486402120908));
#76272=CARTESIAN_POINT('Ctrl Pts',(40.4514106818033,-3.10118648075366,-0.876789583703369));
#76273=CARTESIAN_POINT('Ctrl Pts',(40.4575021900668,-3.07424000933875,-0.972098691394826));
#76274=CARTESIAN_POINT('Ctrl Pts',(40.4635936983303,-3.04289839255802,-1.06615467758334));
#76275=CARTESIAN_POINT('Ctrl Pts',(40.4696852065938,-3.00731337428556,-1.15852657774571));
#76276=CARTESIAN_POINT('Ctrl Pts',(40.4757828570208,-2.97169247508056,-1.25099161794506));
#76277=CARTESIAN_POINT('Ctrl Pts',(40.4818805074477,-2.93181978869112,-1.34176876585871));
#76278=CARTESIAN_POINT('Ctrl Pts',(40.4879781578746,-2.88789538548396,-1.43044671519091));
#76279=CARTESIAN_POINT('Ctrl Pts',(40.4940788340213,-2.84394918651556,-1.5191686674752));
#76280=CARTESIAN_POINT('Ctrl Pts',(40.5001795101679,-2.79594748334401,-1.6057889593936));
#76281=CARTESIAN_POINT('Ctrl Pts',(40.5062801863146,-2.74413544236778,-1.68992255338551));
#76282=CARTESIAN_POINT('Ctrl Pts',(40.5123914223628,-2.69223371788128,-1.77420177754172));
#76283=CARTESIAN_POINT('Ctrl Pts',(40.518502658411,-2.63650873011724,-1.85598533823604));
#76284=CARTESIAN_POINT('Ctrl Pts',(40.5246138944592,-2.57724802975836,-1.93491864314928));
#76285=CARTESIAN_POINT('Ctrl Pts',(40.530316721458,-2.5219476749181,-2.00857689801266));
#76286=CARTESIAN_POINT('Ctrl Pts',(40.5360195484569,-2.46356899750457,-2.07975324295799));
#76287=CARTESIAN_POINT('Ctrl Pts',(40.5417223754557,-2.4023743985966,-2.14818872808411));
#76288=CARTESIAN_POINT('Ctrl Pts',(40.5478946235485,-2.33614264257929,-2.2222573948404));
#76289=CARTESIAN_POINT('Ctrl Pts',(40.5540668716413,-2.26636563631585,-2.29339052978325));
#76290=CARTESIAN_POINT('Ctrl Pts',(40.560239119734,-2.19333382918926,-2.36122939932442));
#76291=CARTESIAN_POINT('Ctrl Pts',(40.5664030083867,-2.1204009333524,-2.42897639067795));
#76292=CARTESIAN_POINT('Ctrl Pts',(40.5725668970393,-2.04422231382743,-2.4934376915636));
#76293=CARTESIAN_POINT('Ctrl Pts',(40.5787307856919,-1.96512759576635,-2.55428876497109));
#76294=CARTESIAN_POINT('Ctrl Pts',(40.5848881473505,-1.88611663177433,-2.61507540265988));
#76295=CARTESIAN_POINT('Ctrl Pts',(40.591045509009,-1.80419605062523,-2.67225914975049));
#76296=CARTESIAN_POINT('Ctrl Pts',(40.5972028706676,-1.71973041347598,-2.72555404779758));
#76297=CARTESIAN_POINT('Ctrl Pts',(40.6033557348139,-1.63532647243283,-2.77881001773382));
#76298=CARTESIAN_POINT('Ctrl Pts',(40.6095085989602,-1.54838153761617,-2.82818255498478));
#76299=CARTESIAN_POINT('Ctrl Pts',(40.6156614631065,-1.45929041340567,-2.8734281010393));
#76300=CARTESIAN_POINT('Ctrl Pts',(40.6218119962431,-1.37023304132688,-2.91865650583936));
#76301=CARTESIAN_POINT('Ctrl Pts',(40.6279625293796,-1.27903148230783,-2.95976082965567));
#76302=CARTESIAN_POINT('Ctrl Pts',(40.6341130625161,-1.18610570407999,-2.99654314523401));
#76303=CARTESIAN_POINT('Ctrl Pts',(40.6402629107313,-1.09319027403589,-3.03332136474592));
#76304=CARTESIAN_POINT('Ctrl Pts',(40.6464127589466,-0.99855141041053,-3.06577837304117));
#76305=CARTESIAN_POINT('Ctrl Pts',(40.6525626071618,-0.902628710776066,
-3.09376453095298));
#76306=CARTESIAN_POINT('Ctrl Pts',(40.6587134155409,-0.806691034915567,
-3.12175505828964));
#76307=CARTESIAN_POINT('Ctrl Pts',(40.66486422392,-0.709469541944053,-3.14527322711302));
#76308=CARTESIAN_POINT('Ctrl Pts',(40.6710150322992,-0.611417644943363,
-3.16421965513646));
#76309=CARTESIAN_POINT('Ctrl Pts',(40.6771724186654,-0.513260886261442,
-3.18318634543281));
#76310=CARTESIAN_POINT('Ctrl Pts',(40.6833298050316,-0.414272377471576,
-3.19757144902812));
#76311=CARTESIAN_POINT('Ctrl Pts',(40.6894871913978,-0.314914233430923,
-3.20732701608093));
#76312=CARTESIAN_POINT('Ctrl Pts',(40.6956480141347,-0.215500638684147,
-3.21708802761026));
#76313=CARTESIAN_POINT('Ctrl Pts',(40.7018088368717,-0.115717431681363,
-3.22221433491865));
#76314=CARTESIAN_POINT('Ctrl Pts',(40.7079696596087,-0.016028235548225,
-3.22271014181623));
#76315=CARTESIAN_POINT('Ctrl Pts',(40.7141407825253,0.0838276293370653,
-3.22320677764534));
#76316=CARTESIAN_POINT('Ctrl Pts',(40.720311905442,0.183588735197978,-3.21905746739879));
#76317=CARTESIAN_POINT('Ctrl Pts',(40.7264830283587,0.282794931016511,-3.21031845608677));
#76318=CARTESIAN_POINT('Ctrl Pts',(40.7311785503043,0.358279551220556,-3.20366906343137));
#76319=CARTESIAN_POINT('Ctrl Pts',(40.7358740722498,0.433442980414044,-3.19436355227302));
#76320=CARTESIAN_POINT('Ctrl Pts',(40.7405695941953,0.508087071587692,-3.18244640020621));
#76321=CARTESIAN_POINT('Ctrl Pts',(40.7467418422881,0.606206482960046,-3.16678134316491));
#76322=CARTESIAN_POINT('Ctrl Pts',(40.7529140903809,0.703773451911838,-3.14654671790471));
#76323=CARTESIAN_POINT('Ctrl Pts',(40.7590863384736,0.800329159595483,-3.12179288211137));
#76324=CARTESIAN_POINT('Ctrl Pts',(40.7652502271263,0.896754096181804,-3.09707257189976));
#76325=CARTESIAN_POINT('Ctrl Pts',(40.7714141157789,0.992170076689239,-3.06784532351005));
#76326=CARTESIAN_POINT('Ctrl Pts',(40.7775780044315,1.08612586599699,-3.03421294007396));
#76327=CARTESIAN_POINT('Ctrl Pts',(40.7837353660901,1.17998216472063,-3.00061617025464));
#76328=CARTESIAN_POINT('Ctrl Pts',(40.7898927277486,1.27238093954544,-2.96262368470892));
#76329=CARTESIAN_POINT('Ctrl Pts',(40.7960500894072,1.36288451772775,-2.92038753487238));
#76330=CARTESIAN_POINT('Ctrl Pts',(40.8022029535535,1.4533219895202,-2.87818223552202));
#76331=CARTESIAN_POINT('Ctrl Pts',(40.8083558176998,1.54186662447143,-2.83173961774241));
#76332=CARTESIAN_POINT('Ctrl Pts',(40.8145086818461,1.62810006422018,-2.78126009991627));
#76333=CARTESIAN_POINT('Ctrl Pts',(40.8206592149826,1.71430083446959,-2.73079970623244));
#76334=CARTESIAN_POINT('Ctrl Pts',(40.8268097481192,1.79819177486622,-2.67630567056568));
#76335=CARTESIAN_POINT('Ctrl Pts',(40.8329602812557,1.87937930638694,-2.61802425222238));
#76336=CARTESIAN_POINT('Ctrl Pts',(40.8391101294709,1.96055779689107,-2.5597493240785));
#76337=CARTESIAN_POINT('Ctrl Pts',(40.8452599776861,2.03903312418386,-2.49768810509254));
#76338=CARTESIAN_POINT('Ctrl Pts',(40.8514098259013,2.11444171555594,-2.43212947723119));
#76339=CARTESIAN_POINT('Ctrl Pts',(40.8575606342805,2.18986208032607,-2.3665606138276));
#76340=CARTESIAN_POINT('Ctrl Pts',(40.8637114426596,2.26221443030482,-2.2974935419846));
#76341=CARTESIAN_POINT('Ctrl Pts',(40.8698622510388,2.33116999913079,-2.2252559398084));
#76342=CARTESIAN_POINT('Ctrl Pts',(40.8760196374049,2.40019931254607,-2.15294108306965));
#76343=CARTESIAN_POINT('Ctrl Pts',(40.8821770237711,2.46582429018738,-2.07744923988472));
#76344=CARTESIAN_POINT('Ctrl Pts',(40.8883344101373,2.52775472598571,-1.99914321842056));
#76345=CARTESIAN_POINT('Ctrl Pts',(40.8944952328743,2.58971972449079,-1.9207934952123));
#76346=CARTESIAN_POINT('Ctrl Pts',(40.9006560556112,2.64798582162219,-1.83962681885158));
#76347=CARTESIAN_POINT('Ctrl Pts',(40.9068168783482,2.70230586789131,-1.75603546628768));
#76348=CARTESIAN_POINT('Ctrl Pts',(40.9129880012649,2.75671673096583,-1.67230435869557));
#76349=CARTESIAN_POINT('Ctrl Pts',(40.9191591241816,2.80716814561218,-1.58614085262557));
#76350=CARTESIAN_POINT('Ctrl Pts',(40.9253302470983,2.8534586172673,-1.49796244346878));
#76351=CARTESIAN_POINT('Ctrl Pts',(40.9300257690439,2.88868039593923,-1.4308687133789));
#76352=CARTESIAN_POINT('Ctrl Pts',(40.9347212909895,2.92149415278127,-1.36260898155911));
#76353=CARTESIAN_POINT('Ctrl Pts',(40.9394168129351,2.95183016262558,-1.29337398053071));
#76354=CARTESIAN_POINT('Ctrl Pts',(40.9455890610278,2.99170674739566,-1.20236480029458));
#76355=CARTESIAN_POINT('Ctrl Pts',(40.9517613091206,3.02744065937287,-1.10934952722247));
#76356=CARTESIAN_POINT('Ctrl Pts',(40.9579335572134,3.05882617184256,-1.01474135273526));
#76357=CARTESIAN_POINT('Ctrl Pts',(40.964097445866,3.09016917705901,-0.920261311686526));
#76358=CARTESIAN_POINT('Ctrl Pts',(40.9702613345186,3.11717535282186,-0.824193065864977));
#76359=CARTESIAN_POINT('Ctrl Pts',(40.9764252231712,3.13968634938288,-0.726971244272297));
#76360=CARTESIAN_POINT('Ctrl Pts',(40.9825825848298,3.16217350885833,-0.629852371692754));
#76361=CARTESIAN_POINT('Ctrl Pts',(40.9887399464883,3.18017485498476,-0.531582772707588));
#76362=CARTESIAN_POINT('Ctrl Pts',(40.9948973081469,3.19358164065124,-0.432612837298341));
#76363=CARTESIAN_POINT('Ctrl Pts',(41.0010501722932,3.20697863361983,-0.333715192347285));
#76364=CARTESIAN_POINT('Ctrl Pts',(41.0072030364395,3.21578768029252,-0.234118657158604));
#76365=CARTESIAN_POINT('Ctrl Pts',(41.0133559005858,3.2199511637498,-0.134283526786764));
#76366=CARTESIAN_POINT('Ctrl Pts',(41.0195064337223,3.22411306987328,-0.0344862189085126));
#76367=CARTESIAN_POINT('Ctrl Pts',(41.0256569668589,3.22363289175207,0.0655490710288874));
#76368=CARTESIAN_POINT('Ctrl Pts',(41.0318074999954,3.21850497270214,0.165358105914306));
#76369=CARTESIAN_POINT('Ctrl Pts',(41.0379573482106,3.21337762469559,0.265156026098697));
#76370=CARTESIAN_POINT('Ctrl Pts',(41.0441071964258,3.20360358705455,0.364727307520266));
#76371=CARTESIAN_POINT('Ctrl Pts',(41.050257044641,3.18922928237789,0.463609908137634));
#76372=CARTESIAN_POINT('Ctrl Pts',(41.0564078530202,3.17485273346878,0.562507947104669));
#76373=CARTESIAN_POINT('Ctrl Pts',(41.0625586613993,3.1558745534252,0.660716661802562));
#76374=CARTESIAN_POINT('Ctrl Pts',(41.0687094697784,3.13239262065319,0.757782312130238));
#76375=CARTESIAN_POINT('Ctrl Pts',(41.0748668561446,3.108885575109,0.854951769396925));
#76376=CARTESIAN_POINT('Ctrl Pts',(41.0810242425108,3.08086526103552,0.950975298165107));
#76377=CARTESIAN_POINT('Ctrl Pts',(41.087181628877,3.04847995850393,1.04541260041185));
#76378=CARTESIAN_POINT('Ctrl Pts',(41.0933424516139,3.01607658208504,1.13990260709622));
#76379=CARTESIAN_POINT('Ctrl Pts',(41.0995032743509,2.97930352571704,1.23280422038544));
#76380=CARTESIAN_POINT('Ctrl Pts',(41.1056640970879,2.93835714000737,1.32369742776349));
#76381=CARTESIAN_POINT('Ctrl Pts',(41.1118352200045,2.8973422966988,1.41474259802242));
#76382=CARTESIAN_POINT('Ctrl Pts',(41.1180063429212,2.85214038380119,1.50377226773134));
#76383=CARTESIAN_POINT('Ctrl Pts',(41.1241774658379,2.80299365198577,1.59039119383486));
#76384=CARTESIAN_POINT('Ctrl Pts',(41.1288729877835,2.76559858452276,1.65629833487081));
#76385=CARTESIAN_POINT('Ctrl Pts',(41.133568509729,2.72592062395105,1.72081029555234));
#76386=CARTESIAN_POINT('Ctrl Pts',(41.1382640316746,2.68408251505558,1.78376529141951));
#76387=CARTESIAN_POINT('Ctrl Pts',(41.1444372077828,2.62907819024535,1.86653186793366));
#76388=CARTESIAN_POINT('Ctrl Pts',(41.1506103838911,2.57014515438866,1.94689758370025));
#76389=CARTESIAN_POINT('Ctrl Pts',(41.1567835599993,2.50751985933295,2.02446578571999));
#76390=CARTESIAN_POINT('Ctrl Pts',(41.1629466708,2.44499667425195,2.10190751349096));
#76391=CARTESIAN_POINT('Ctrl Pts',(41.1691097816006,2.37879347784921,2.17656046723111));
#76392=CARTESIAN_POINT('Ctrl Pts',(41.1752728924013,2.3091901603766,2.2480565752934));
#76393=CARTESIAN_POINT('Ctrl Pts',(41.1814302037015,2.23965233977452,2.31948540536517));
#76394=CARTESIAN_POINT('Ctrl Pts',(41.1875875150018,2.16672105554266,2.38776298181445));
#76395=CARTESIAN_POINT('Ctrl Pts',(41.193744826302,2.09071637201169,2.45255430404757));
#76396=CARTESIAN_POINT('Ctrl Pts',(41.1998973678967,2.01477056482111,2.51729543626917));
#76397=CARTESIAN_POINT('Ctrl Pts',(41.2060499094915,1.93575642291291,2.57855540449767));
#76398=CARTESIAN_POINT('Ctrl Pts',(41.2122024510862,1.85402994020835,2.63603690097674));
#76399=CARTESIAN_POINT('Ctrl Pts',(41.2138096173864,1.83268135656855,2.6510522117391));
#76400=CARTESIAN_POINT('Ctrl Pts',(41.2154167836865,1.8111478745415,2.6658099045286));
#76401=CARTESIAN_POINT('Ctrl Pts',(41.2170239499866,1.789436210378,2.68030513402635));
#76402=CARTESIAN_POINT('Ctrl Pts',(39.9670570335907,1.78943621037801,2.68030513402635));
#76403=CARTESIAN_POINT('Ctrl Pts',(39.9732196010882,1.70662368603128,2.73559276820561));
#76404=CARTESIAN_POINT('Ctrl Pts',(39.9793821685857,1.62113340072966,2.78711433407194));
#76405=CARTESIAN_POINT('Ctrl Pts',(39.9855447360832,1.53334353057214,2.83460317853356));
#76406=CARTESIAN_POINT('Ctrl Pts',(39.9917011085207,1.44564191316245,2.88204428376277));
#76407=CARTESIAN_POINT('Ctrl Pts',(39.9978574809582,1.35564568716505,2.92546052205229));
#76408=CARTESIAN_POINT('Ctrl Pts',(40.0040138533957,1.26376118638599,2.9646290200098));
#76409=CARTESIAN_POINT('Ctrl Pts',(40.0101661718499,1.17193719172973,3.00377172543509));
#76410=CARTESIAN_POINT('Ctrl Pts',(40.0163184903041,1.07822779268038,3.03867208115502));
#76411=CARTESIAN_POINT('Ctrl Pts',(40.0224708087583,0.98306224853093,3.06915398408312));
#76412=CARTESIAN_POINT('Ctrl Pts',(40.0286210952501,0.887928135266615,3.0996258195735));
#76413=CARTESIAN_POINT('Ctrl Pts',(40.0347713817419,0.791339245884843,3.12568196966969));
#76414=CARTESIAN_POINT('Ctrl Pts',(40.0409216682336,0.693742194816822,3.1471954705151));
#76415=CARTESIAN_POINT('Ctrl Pts',(40.0470715685711,0.596151271515395,3.16870762060543));
#76416=CARTESIAN_POINT('Ctrl Pts',(40.0532214689085,0.497552736670877,3.18567759527323));
#76417=CARTESIAN_POINT('Ctrl Pts',(40.059371369246,0.398404664873244,3.19802928152749));
#76418=CARTESIAN_POINT('Ctrl Pts',(40.065522528474,0.299236297370409,3.21038349618375));
#76419=CARTESIAN_POINT('Ctrl Pts',(40.0716736877019,0.199518600493762,3.21811749073813));
#76420=CARTESIAN_POINT('Ctrl Pts',(40.0778248469298,0.0997150502907764,
3.22120698981694));
#76421=CARTESIAN_POINT('Ctrl Pts',(40.083982747012,-0.000197871358417603,
3.22429987457673));
#76422=CARTESIAN_POINT('Ctrl Pts',(40.0901406470941,-0.100196399287679,
3.22273808918772));
#76423=CARTESIAN_POINT('Ctrl Pts',(40.0962985471763,-0.199816923963555,
3.21654951141713));
#76424=CARTESIAN_POINT('Ctrl Pts',(40.1024601521362,-0.299497384959231,
3.21035721031163));
#76425=CARTESIAN_POINT('Ctrl Pts',(40.1086217570962,-0.398798958333763,
3.19953262122687));
#76426=CARTESIAN_POINT('Ctrl Pts',(40.1147833620561,-0.497265089790132,
3.1841553028984));
#76427=CARTESIAN_POINT('Ctrl Pts',(40.1209549333014,-0.595890488445507,
3.16875311203374));
#76428=CARTESIAN_POINT('Ctrl Pts',(40.1271265045467,-0.693677321720815,
3.14878357472114));
#76429=CARTESIAN_POINT('Ctrl Pts',(40.1332980757919,-0.790181112498599,
3.12437695740294));
#76430=CARTESIAN_POINT('Ctrl Pts',(40.1368746965201,-0.846108111430506,
3.11023255074612));
#76431=CARTESIAN_POINT('Ctrl Pts',(40.1404513172483,-0.90160449120352,3.09459884785688));
#76432=CARTESIAN_POINT('Ctrl Pts',(40.1440279379765,-0.956586756639631,
3.07750862541792));
#76433=CARTESIAN_POINT('Ctrl Pts',(40.1502001860692,-1.05147078510283,3.04801567638282));
#76434=CARTESIAN_POINT('Ctrl Pts',(40.156372434162,-1.1451565765698,3.01407858801189));
#76435=CARTESIAN_POINT('Ctrl Pts',(40.1625446822548,-1.23719717747275,2.97581261280906));
#76436=CARTESIAN_POINT('Ctrl Pts',(40.1687085709074,-1.32911312235386,2.93759846347648));
#76437=CARTESIAN_POINT('Ctrl Pts',(40.17487245956,-1.41938790786098,2.89506724569189));
#76438=CARTESIAN_POINT('Ctrl Pts',(40.1810363482126,-1.50758942075117,2.84838405081533));
#76439=CARTESIAN_POINT('Ctrl Pts',(40.1871937098712,-1.59569753630974,2.80175028917059));
#76440=CARTESIAN_POINT('Ctrl Pts',(40.1933510715297,-1.68173636212607,2.75097349329647));
#76441=CARTESIAN_POINT('Ctrl Pts',(40.1995084331883,-1.76529437220314,2.69626655617873));
#76442=CARTESIAN_POINT('Ctrl Pts',(40.2056612973346,-1.84879134913088,2.64159957856528));
#76443=CARTESIAN_POINT('Ctrl Pts',(40.2118141614809,-1.92981075068336,2.5830084043413));
#76444=CARTESIAN_POINT('Ctrl Pts',(40.2179670256272,-2.00796706315876,2.52075104597213));
#76445=CARTESIAN_POINT('Ctrl Pts',(40.2241175587638,-2.0860937661509,2.45851727377472));
#76446=CARTESIAN_POINT('Ctrl Pts',(40.2302680919003,-2.16135919593939,2.39262034757435));
#76447=CARTESIAN_POINT('Ctrl Pts',(40.2364186250368,-2.23340890014565,2.32336012000942));
#76448=CARTESIAN_POINT('Ctrl Pts',(40.242568473252,-2.30545058092077,2.25410760524044));
#76449=CARTESIAN_POINT('Ctrl Pts',(40.2487183214672,-2.37427693492087,2.18149283476765));
#76450=CARTESIAN_POINT('Ctrl Pts',(40.2548681696825,-2.43956928588356,2.10585357085282));
#76451=CARTESIAN_POINT('Ctrl Pts',(40.2610189780616,-2.50487183081491,2.03020249752581));
#76452=CARTESIAN_POINT('Ctrl Pts',(40.2671697864407,-2.56663899291463,1.95152632167501));
#76453=CARTESIAN_POINT('Ctrl Pts',(40.2733205948199,-2.62459207753573,1.87019624345593));
#76454=CARTESIAN_POINT('Ctrl Pts',(40.279477981186,-2.68260714013062,1.78877918671812));
#76455=CARTESIAN_POINT('Ctrl Pts',(40.2856353675522,-2.73679972740451,1.70470291442654));
#76456=CARTESIAN_POINT('Ctrl Pts',(40.2917927539184,-2.78693431929228,1.61836790083432));
#76457=CARTESIAN_POINT('Ctrl Pts',(40.2979535766554,-2.83709689075378,1.53198470460438));
#76458=CARTESIAN_POINT('Ctrl Pts',(40.3041143993923,-2.88319675624035,1.44334064203683));
#76459=CARTESIAN_POINT('Ctrl Pts',(40.3102752221293,-2.9250452135613,1.35285921703707));
#76460=CARTESIAN_POINT('Ctrl Pts',(40.316446345046,-2.96696363664015,1.26222651760853));
#76461=CARTESIAN_POINT('Ctrl Pts',(40.3226174679627,-3.00461628994125,1.16975072230248));
#76462=CARTESIAN_POINT('Ctrl Pts',(40.3287885908793,-3.03786325502638,1.07587378732849));
#76463=CARTESIAN_POINT('Ctrl Pts',(40.3334841128249,-3.06316041022609,1.0044441278805));
#76464=CARTESIAN_POINT('Ctrl Pts',(40.3381796347704,-3.08590791362778,0.932203663353661));
#76465=CARTESIAN_POINT('Ctrl Pts',(40.342875156716,-3.10606394303052,0.859351118173287));
#76466=CARTESIAN_POINT('Ctrl Pts',(40.350710863735,-3.13969955221256,0.737777583592601));
#76467=CARTESIAN_POINT('Ctrl Pts',(40.358546570754,-3.16621377910518,0.614154268083113));
#76468=CARTESIAN_POINT('Ctrl Pts',(40.366382277773,-3.18540180604714,0.489216615142617));
#76469=CARTESIAN_POINT('Ctrl Pts',(40.3740772191688,-3.20424512707252,0.366523421640472));
#76470=CARTESIAN_POINT('Ctrl Pts',(40.3817721605646,-3.21602311411887,0.242562533622061));
#76471=CARTESIAN_POINT('Ctrl Pts',(40.3894671019604,-3.22058710117146,0.118052048978578));
#76472=CARTESIAN_POINT('Ctrl Pts',(40.3918358843862,-3.2219920621407,0.0797231998450655));
#76473=CARTESIAN_POINT('Ctrl Pts',(40.394204666812,-3.22271373114598,0.041342434832041));
#76474=CARTESIAN_POINT('Ctrl Pts',(40.3965734492378,-3.22274866702434,0.00293115895943825));
#76475=CARTESIAN_POINT('Ctrl Pts',(39.7209886430068,1.78943588752252,2.68030534957241));
#76476=CARTESIAN_POINT('Ctrl Pts',(39.7321640893856,1.65207849352263,2.77200842746209));
#76477=CARTESIAN_POINT('Ctrl Pts',(39.7433052749528,1.50777340075562,2.85308531584831));
#76478=CARTESIAN_POINT('Ctrl Pts',(39.7551126764817,1.34071459180183,2.93069196149534));
#76479=CARTESIAN_POINT('Ctrl Pts',(39.7563102948743,1.32359539338073,2.93846324837295));
#76480=CARTESIAN_POINT('Ctrl Pts',(39.7583549276396,1.29404934284328,2.95156511911777));
#76481=CARTESIAN_POINT('Ctrl Pts',(39.7592059182603,1.28165533818344,2.95696803556938));
#76482=CARTESIAN_POINT('Ctrl Pts',(39.7604085383861,1.2639964284272,2.96453419246989));
#76483=CARTESIAN_POINT('Ctrl Pts',(39.7607639649647,1.25875943674085,2.96676164040834));
#76484=CARTESIAN_POINT('Ctrl Pts',(39.761374413209,1.24973325804424,2.97057253921833));
#76485=CARTESIAN_POINT('Ctrl Pts',(39.7616298392038,1.24594690659992,2.97216263580712));
#76486=CARTESIAN_POINT('Ctrl Pts',(39.7621216805988,1.23863729880266,2.97521591792621));
#76487=CARTESIAN_POINT('Ctrl Pts',(39.7623581571592,1.2351144887013,2.97668008298311));
#76488=CARTESIAN_POINT('Ctrl Pts',(39.7629221835489,1.22669241690849,2.98016297448509));
#76489=CARTESIAN_POINT('Ctrl Pts',(39.7632493804315,1.22179074068081,2.98217588802622));
#76490=CARTESIAN_POINT('Ctrl Pts',(39.7644165006735,1.20425030818957,2.98932850500378));
#76491=CARTESIAN_POINT('Ctrl Pts',(39.7652523952585,1.19158368682434,2.99440011491901));
#76492=CARTESIAN_POINT('Ctrl Pts',(39.7698296790476,1.12167643902437,3.02187655862792));
#76493=CARTESIAN_POINT('Ctrl Pts',(39.773484692314,1.06383198131068,3.04272223631978));
#76494=CARTESIAN_POINT('Ctrl Pts',(39.795127554147,0.711980781055297,3.15825797778673));
#76495=CARTESIAN_POINT('Ctrl Pts',(39.8116408571957,0.40619440215225,3.21193950109201));
#76496=CARTESIAN_POINT('Ctrl Pts',(39.8337766245109,0.0220881041297611,
3.22355534523597));
#76497=CARTESIAN_POINT('Ctrl Pts',(39.8381771210486,-0.0532913925965058,
3.223190309908));
#76498=CARTESIAN_POINT('Ctrl Pts',(39.845355665513,-0.173954576437729,3.21837210993128));
#76499=CARTESIAN_POINT('Ctrl Pts',(39.8480824355653,-0.219278834458008,
3.21560192051278));
#76500=CARTESIAN_POINT('Ctrl Pts',(39.8516275874507,-0.277465623360148,
3.21080969746222));
#76501=CARTESIAN_POINT('Ctrl Pts',(39.8524182724492,-0.290396750720803,
3.20966599585087));
#76502=CARTESIAN_POINT('Ctrl Pts',(39.8536980370717,-0.311249635632164,
3.20769460211176));
#76503=CARTESIAN_POINT('Ctrl Pts',(39.8541855793026,-0.319175939296277,
3.20691560756914));
#76504=CARTESIAN_POINT('Ctrl Pts',(39.8551175969417,-0.334293838818497,
3.20537322213585));
#76505=CARTESIAN_POINT('Ctrl Pts',(39.8555619068705,-0.341485921281881,
3.20461498905343));
#76506=CARTESIAN_POINT('Ctrl Pts',(39.8565795919936,-0.357924835355587,
3.20282593050606));
#76507=CARTESIAN_POINT('Ctrl Pts',(39.8571534643796,-0.367169845094468,
3.20177926016639));
#76508=CARTESIAN_POINT('Ctrl Pts',(39.8589214268339,-0.395574015047169,
3.19843885285245));
#76509=CARTESIAN_POINT('Ctrl Pts',(39.8601196768224,-0.414716941435674,
3.19601309903595));
#76510=CARTESIAN_POINT('Ctrl Pts',(39.8771109014239,-0.684604954247868,
3.15934787544266));
#76511=CARTESIAN_POINT('Ctrl Pts',(39.8938857735702,-0.930434109965115,
3.09586880912285));
#76512=CARTESIAN_POINT('Ctrl Pts',(39.9210651089218,-1.30517274953995,2.95039773149168));
#76513=CARTESIAN_POINT('Ctrl Pts',(39.9311970063851,-1.44018412841049,2.88690068275874));
#76514=CARTESIAN_POINT('Ctrl Pts',(39.9448108739191,-1.61990250625762,2.7866211036197));
#76515=CARTESIAN_POINT('Ctrl Pts',(39.9485234945605,-1.66874766446562,2.75764815298731));
#76516=CARTESIAN_POINT('Ctrl Pts',(39.9541595951937,-1.7430138315697,2.71090011792678));
#76517=CARTESIAN_POINT('Ctrl Pts',(39.9561288307718,-1.76898510473167,2.69402459828752));
#76518=CARTESIAN_POINT('Ctrl Pts',(39.9585628124718,-1.80116703696282,2.67244743629182));
#76519=CARTESIAN_POINT('Ctrl Pts',(39.959049661314,-1.80760827127583,2.66809488874902));
#76520=CARTESIAN_POINT('Ctrl Pts',(39.9598192718702,-1.81779825600206,2.66115535185934));
#76521=CARTESIAN_POINT('Ctrl Pts',(39.9601030542853,-1.82155732915326,2.65858368374509));
#76522=CARTESIAN_POINT('Ctrl Pts',(39.9606372087027,-1.82863632131726,2.65371872049736));
#76523=CARTESIAN_POINT('Ctrl Pts',(39.9608876910953,-1.83195734605558,2.65142718655085));
#76524=CARTESIAN_POINT('Ctrl Pts',(39.9614609800611,-1.83956148105148,2.64615916445889));
#76525=CARTESIAN_POINT('Ctrl Pts',(39.9617834979445,-1.84384166729123,2.64317851706781));
#76526=CARTESIAN_POINT('Ctrl Pts',(39.9627790960626,-1.85706067625363,2.63392529387039));
#76527=CARTESIAN_POINT('Ctrl Pts',(39.963449812422,-1.86597498209866,2.62761758693435));
#76528=CARTESIAN_POINT('Ctrl Pts',(39.9690104295967,-1.93993329092643,2.57471897120221));
#76529=CARTESIAN_POINT('Ctrl Pts',(39.9737457158652,-2.00325973037467,2.52576162974706));
#76530=CARTESIAN_POINT('Ctrl Pts',(39.9802377061916,-2.08921353965109,2.4540422427841));
#76531=CARTESIAN_POINT('Ctrl Pts',(39.9820734717929,-2.1134189107674,2.43322772275074));
#76532=CARTESIAN_POINT('Ctrl Pts',(39.984442657204,-2.14444990185094,2.40573131178357));
#76533=CARTESIAN_POINT('Ctrl Pts',(39.9849866120418,-2.15156012702867,2.39937440764058));
#76534=CARTESIAN_POINT('Ctrl Pts',(39.9935368542357,-2.26307276256311,2.29878214887312));
#76535=CARTESIAN_POINT('Ctrl Pts',(40.0013350345454,-2.36122813691671,2.19784031840064));
#76536=CARTESIAN_POINT('Ctrl Pts',(40.0160780481415,-2.53204057285876,1.99748041896476));
#76537=CARTESIAN_POINT('Ctrl Pts',(40.022991553198,-2.6062074553478,1.89969401693332));
#76538=CARTESIAN_POINT('Ctrl Pts',(40.0340514732086,-2.71290453514553,1.7409699015081));
#76539=CARTESIAN_POINT('Ctrl Pts',(40.0380717589711,-2.74935936884235,1.68280995410925));
#76540=CARTESIAN_POINT('Ctrl Pts',(40.0446805891996,-2.80527280392049,1.58693327420948));
#76541=CARTESIAN_POINT('Ctrl Pts',(40.0472276962569,-2.82589265080441,1.54991715612698));
#76542=CARTESIAN_POINT('Ctrl Pts',(40.0505702291102,-2.85171964725375,1.50132374843055));
#76543=CARTESIAN_POINT('Ctrl Pts',(40.0513417524742,-2.85759718966642,1.49010611655001));
#76544=CARTESIAN_POINT('Ctrl Pts',(40.0525979907795,-2.86703072503994,1.47184058141011));
#76545=CARTESIAN_POINT('Ctrl Pts',(40.0530812707732,-2.87062724589319,1.46481367033135));
#76546=CARTESIAN_POINT('Ctrl Pts',(40.0540102312467,-2.87747781722077,1.45130684268854));
#76547=CARTESIAN_POINT('Ctrl Pts',(40.0544557666593,-2.88073588992689,1.44482901111179));
#76548=CARTESIAN_POINT('Ctrl Pts',(40.0554738934587,-2.88811832588831,1.43002671483367));
#76549=CARTESIAN_POINT('Ctrl Pts',(40.0560469742298,-2.89222859688077,1.42169532951318));
#76550=CARTESIAN_POINT('Ctrl Pts',(40.0575625815878,-2.90297961901785,1.39966377663986));
#76551=CARTESIAN_POINT('Ctrl Pts',(40.0585072245931,-2.90955934924733,1.38593424680419));
#76552=CARTESIAN_POINT('Ctrl Pts',(40.0648607561466,-2.95300078443222,1.29361473809033));
#76553=CARTESIAN_POINT('Ctrl Pts',(40.0703755633625,-2.98676846181998,1.21361630870205));
#76554=CARTESIAN_POINT('Ctrl Pts',(40.0791170094146,-3.03423501618327,1.08713768970816));
#76555=CARTESIAN_POINT('Ctrl Pts',(40.0822723159697,-3.05018660176374,1.04154300420082));
#76556=CARTESIAN_POINT('Ctrl Pts',(40.0919197984805,-3.09543302362643,0.902246194701879));
#76557=CARTESIAN_POINT('Ctrl Pts',(40.0984903261723,-3.1214757690063,0.807552294098496));
#76558=CARTESIAN_POINT('Ctrl Pts',(40.1111536476425,-3.16294652745497,0.62443225562779));
#76559=CARTESIAN_POINT('Ctrl Pts',(40.1172324921037,-3.17908434152186,0.536254539451549));
#76560=CARTESIAN_POINT('Ctrl Pts',(40.1334068397218,-3.21233564652255,0.29912008265209));
#76561=CARTESIAN_POINT('Ctrl Pts',(40.1434412181666,-3.22277104870652,0.149431934785481));
#76562=CARTESIAN_POINT('Ctrl Pts',(40.1532596875225,-3.22274939918938,-0.00449845971419938));
#76563=CARTESIAN_POINT('Ctrl Pts',(40.1535173518547,-3.22274121395295,-0.00854367477969973));
#76564=CARTESIAN_POINT('Ctrl Pts',(40.1549633833723,-3.22265240666992,-0.0312781304336692));
#76565=CARTESIAN_POINT('Ctrl Pts',(40.1561442502217,-3.22241682628457,-0.0499669135980986));
#76566=CARTESIAN_POINT('Ctrl Pts',(40.1577369736299,-3.22187581434776,-0.0753576160558248));
#76567=CARTESIAN_POINT('Ctrl Pts',(40.1581564135566,-3.22171203037629,-0.0820617366684774));
#76568=CARTESIAN_POINT('Ctrl Pts',(40.1588170773794,-3.22142028134979,-0.0926500716955674));
#76569=CARTESIAN_POINT('Ctrl Pts',(40.159059073807,-3.22130621576293,-0.0965346028457733));
#76570=CARTESIAN_POINT('Ctrl Pts',(40.1595534136852,-3.22105844474806,-0.104482468912272));
#76571=CARTESIAN_POINT('Ctrl Pts',(40.1598057146607,-3.22092407735302,-0.108545745477598));
#76572=CARTESIAN_POINT('Ctrl Pts',(40.1603948283916,-3.22059180932549,-0.118049115324318));
#76573=CARTESIAN_POINT('Ctrl Pts',(40.1607312979975,-3.22038781238382,-0.123489006818093));
#76574=CARTESIAN_POINT('Ctrl Pts',(40.1618147005343,-3.21968499538193,-0.141042859973687));
#76575=CARTESIAN_POINT('Ctrl Pts',(40.1625586274475,-3.21913159162467,-0.153154707761682));
#76576=CARTESIAN_POINT('Ctrl Pts',(40.1734342361561,-3.20999858588507,-0.331020313197249));
#76577=CARTESIAN_POINT('Ctrl Pts',(40.1828943525046,-3.18869358329005,-0.495898031008083));
#76578=CARTESIAN_POINT('Ctrl Pts',(40.2052022722087,-3.10758913342228,-0.884504162717305));
#76579=CARTESIAN_POINT('Ctrl Pts',(40.2179033156276,-3.03624216669502,-1.10484698250114));
#76580=CARTESIAN_POINT('Ctrl Pts',(40.232463044738,-2.9340152452497,-1.33343571890868));
#76581=CARTESIAN_POINT('Ctrl Pts',(40.2335989802135,-2.92590993950567,-1.35112815118152));
#76582=CARTESIAN_POINT('Ctrl Pts',(40.2389444749062,-2.88717885999298,-1.43368806582139));
#76583=CARTESIAN_POINT('Ctrl Pts',(40.2432129677869,-2.85455491213075,-1.49759083614846));
#76584=CARTESIAN_POINT('Ctrl Pts',(40.2484251808164,-2.81288876547299,-1.57288898835381));
#76585=CARTESIAN_POINT('Ctrl Pts',(40.2492961739722,-2.80586606497999,-1.58538279026992));
#76586=CARTESIAN_POINT('Ctrl Pts',(40.2507262742465,-2.79423896158135,-1.60574884466103));
#76587=CARTESIAN_POINT('Ctrl Pts',(40.2512835952119,-2.78968401802936,-1.61364921944192));
#76588=CARTESIAN_POINT('Ctrl Pts',(40.2522837541382,-2.78146770122346,-1.62776133998531));
#76589=CARTESIAN_POINT('Ctrl Pts',(40.2527261338012,-2.77781888384923,-1.633980354866));
#76590=CARTESIAN_POINT('Ctrl Pts',(40.25366508845,-2.77004343205775,-1.64713145491186));
#76591=CARTESIAN_POINT('Ctrl Pts',(40.2541618517358,-2.76591158317992,-1.65406038504825));
#76592=CARTESIAN_POINT('Ctrl Pts',(40.2554889614952,-2.7548252883459,-1.67249392026445));
#76593=CARTESIAN_POINT('Ctrl Pts',(40.2563209911938,-2.74782485695075,-1.68397055477577));
#76594=CARTESIAN_POINT('Ctrl Pts',(40.2602726473932,-2.71434397937894,-1.73809504149306));
#76595=CARTESIAN_POINT('Ctrl Pts',(40.2634262196891,-2.6869424379776,-1.78016220835584));
#76596=CARTESIAN_POINT('Ctrl Pts',(40.2721129236422,-2.60967459658906,-1.89293414604569));
#76597=CARTESIAN_POINT('Ctrl Pts',(40.2777145263074,-2.5579287623426,-1.96229443688133));
#76598=CARTESIAN_POINT('Ctrl Pts',(40.2942306478675,-2.39978927835302,-2.15736650156583));
#76599=CARTESIAN_POINT('Ctrl Pts',(40.3053632637638,-2.28648053238194,-2.27710719947868));
#76600=CARTESIAN_POINT('Ctrl Pts',(40.3294825645016,-2.02244628362454,-2.51646754733987));
#76601=CARTESIAN_POINT('Ctrl Pts',(40.3424267680697,-1.86912696070829,-2.6323526470295));
#76602=CARTESIAN_POINT('Ctrl Pts',(40.3552784665909,-1.69644741089108,-2.74013160812073));
#76603=CARTESIAN_POINT('Ctrl Pts',(40.3560154855263,-1.68646652163516,-2.74628580616083));
#76604=CARTESIAN_POINT('Ctrl Pts',(40.357081318219,-1.67191536327321,-2.75514877966776));
#76605=CARTESIAN_POINT('Ctrl Pts',(40.3574129033277,-1.66737177568941,-2.75790085801732));
#76606=CARTESIAN_POINT('Ctrl Pts',(40.357996590674,-1.6593438713714,-2.76273631738093));
#76607=CARTESIAN_POINT('Ctrl Pts',(40.3582489983676,-1.6558623978749,-2.76482436383795));
#76608=CARTESIAN_POINT('Ctrl Pts',(40.3587774806738,-1.648552038456,-2.76919005964107));
#76609=CARTESIAN_POINT('Ctrl Pts',(40.3590534659245,-1.64472238179449,-2.77146634424997));
#76610=CARTESIAN_POINT('Ctrl Pts',(40.3597820659308,-1.63458070616443,-2.77746596409681));
#76611=CARTESIAN_POINT('Ctrl Pts',(40.3602338013023,-1.62826064141315,-2.78117575007049));
#76612=CARTESIAN_POINT('Ctrl Pts',(40.3622881471307,-1.59937541813454,-2.79799874389221));
#76613=CARTESIAN_POINT('Ctrl Pts',(40.3638749654213,-1.57666336613366,-2.81085955370472));
#76614=CARTESIAN_POINT('Ctrl Pts',(40.3777767152751,-1.37443104822405,-2.92215199374848));
#76615=CARTESIAN_POINT('Ctrl Pts',(40.3891730298433,-1.18604078291829,-3.0035585449422));
#76616=CARTESIAN_POINT('Ctrl Pts',(40.4151573245859,-0.743570310688917,
-3.14657508117909));
#76617=CARTESIAN_POINT('Ctrl Pts',(40.429741305321,-0.487223245393259,-3.19631363224641));
#76618=CARTESIAN_POINT('Ctrl Pts',(40.4466146206631,-0.208642366108974,
-3.21604586022124));
#76619=CARTESIAN_POINT('Ctrl Pts',(40.4477741550401,-0.189572546063888,
-3.21722626456615));
#76620=CARTESIAN_POINT('Ctrl Pts',(40.4495039975292,-0.161239837601685,
-3.21872725638837));
#76621=CARTESIAN_POINT('Ctrl Pts',(40.4500702290144,-0.151984011269613,
-3.21917758033607));
#76622=CARTESIAN_POINT('Ctrl Pts',(40.4510803128522,-0.135506213327811,
-3.21990805192836));
#76623=CARTESIAN_POINT('Ctrl Pts',(40.4515236708843,-0.128284970629541,
-3.22020383852983));
#76624=CARTESIAN_POINT('Ctrl Pts',(40.4524584301396,-0.11308432075495,-3.22077525537431));
#76625=CARTESIAN_POINT('Ctrl Pts',(40.4529499966037,-0.105104772061585,
-3.22104552813038));
#76626=CARTESIAN_POINT('Ctrl Pts',(40.4542487147636,-0.0840605483293663,
-3.221680028338));
#76627=CARTESIAN_POINT('Ctrl Pts',(40.4550574248883,-0.070994620734794,
-3.22199443458799));
#76628=CARTESIAN_POINT('Ctrl Pts',(40.4587415268159,-0.0116500550169357,
-3.22306129538118));
#76629=CARTESIAN_POINT('Ctrl Pts',(40.46164553474,0.0346376632234874,-3.22289616805717));
#76630=CARTESIAN_POINT('Ctrl Pts',(40.4694858358697,0.158237804464938,-3.21979233221754));
#76631=CARTESIAN_POINT('Ctrl Pts',(40.4744753989489,0.235471089690614,-3.21506666361623));
#76632=CARTESIAN_POINT('Ctrl Pts',(40.5005415847875,0.631841109465753,-3.17645556664471));
#76633=CARTESIAN_POINT('Ctrl Pts',(40.5228919993727,0.944731889723517,-3.09782676973865));
#76634=CARTESIAN_POINT('Ctrl Pts',(40.5472481070167,1.28957260569195,-2.95396507278737));
#76635=CARTESIAN_POINT('Ctrl Pts',(40.5506424418291,1.33781368246407,-2.93243286136286));
#76636=CARTESIAN_POINT('Ctrl Pts',(40.5545227692339,1.39343490157475,-2.90594801100087));
#76637=CARTESIAN_POINT('Ctrl Pts',(40.5550739861872,1.40134760085045,-2.90214051578807));
#76638=CARTESIAN_POINT('Ctrl Pts',(40.5559522194027,1.41397469943223,-2.89600082417691));
#76639=CARTESIAN_POINT('Ctrl Pts',(40.5562804905998,1.41869905510866,-2.89368937798069));
#76640=CARTESIAN_POINT('Ctrl Pts',(40.5568603756229,1.42705297517178,-2.88957674858487));
#76641=CARTESIAN_POINT('Ctrl Pts',(40.5571122818836,1.43068482412014,-2.88778027465099));
#76642=CARTESIAN_POINT('Ctrl Pts',(40.5576418889508,1.43832655203853,-2.88398238142146));
#76643=CARTESIAN_POINT('Ctrl Pts',(40.5579194924392,1.44233563624463,-2.88197945163579));
#76644=CARTESIAN_POINT('Ctrl Pts',(40.5586569867131,1.45299526787946,-2.87662610855585));
#76645=CARTESIAN_POINT('Ctrl Pts',(40.5591159592597,1.45963845143871,-2.87326097154096));
#76646=CARTESIAN_POINT('Ctrl Pts',(40.5612519216748,1.4905937985297,-2.85744532408666));
#76647=CARTESIAN_POINT('Ctrl Pts',(40.5629115443202,1.51475957980463,-2.84470862899866));
#76648=CARTESIAN_POINT('Ctrl Pts',(40.5674200810938,1.58060693933868,-2.8089263768702));
#76649=CARTESIAN_POINT('Ctrl Pts',(40.5702353299041,1.62194553998349,-2.78526100055333));
#76650=CARTESIAN_POINT('Ctrl Pts',(40.5798571320635,1.7632305747261,-2.70016579764916));
#76651=CARTESIAN_POINT('Ctrl Pts',(40.5864726965714,1.86034265937294,-2.63419938371192));
#76652=CARTESIAN_POINT('Ctrl Pts',(40.6086673725955,2.17542565024408,-2.39403485653286));
#76653=CARTESIAN_POINT('Ctrl Pts',(40.624065525291,2.37429938472125,-2.19694446055123));
#76654=CARTESIAN_POINT('Ctrl Pts',(40.6411699478432,2.54955873791154,-1.97127255671639));
#76655=CARTESIAN_POINT('Ctrl Pts',(40.6415839925144,2.5537768843949,-1.9658048922904));
#76656=CARTESIAN_POINT('Ctrl Pts',(40.6436440090588,2.57464216134981,-1.93857831450175));
#76657=CARTESIAN_POINT('Ctrl Pts',(40.6452997806274,2.59102854793722,-1.91662180239494));
#76658=CARTESIAN_POINT('Ctrl Pts',(40.6476387204415,2.61362797561477,-1.88552073956487));
#76659=CARTESIAN_POINT('Ctrl Pts',(40.6483127190886,2.6200772364769,-1.8765486735939));
#76660=CARTESIAN_POINT('Ctrl Pts',(40.6494036999365,2.63041413662276,-1.86201104154659));
#76661=CARTESIAN_POINT('Ctrl Pts',(40.649819570041,2.63433059014064,-1.85646599476481));
#76662=CARTESIAN_POINT('Ctrl Pts',(40.6506854709005,2.64243548212905,-1.84491352570061));
#76663=CARTESIAN_POINT('Ctrl Pts',(40.651135609418,2.64662101863044,-1.83890412389011));
#76664=CARTESIAN_POINT('Ctrl Pts',(40.6521967464161,2.65642227213904,-1.8247291544925));
#76665=CARTESIAN_POINT('Ctrl Pts',(40.6528083925193,2.66202085535789,-1.81655188125583));
#76666=CARTESIAN_POINT('Ctrl Pts',(40.6548154562938,2.68022499985389,-1.78969808206011));
#76667=CARTESIAN_POINT('Ctrl Pts',(40.6562168332792,2.69267219978799,-1.77091548575454));
#76668=CARTESIAN_POINT('Ctrl Pts',(40.6595210634323,2.72140099637895,-1.72656106798935));
#76669=CARTESIAN_POINT('Ctrl Pts',(40.6614297800688,2.73752054144332,-1.7008873239692));
#76670=CARTESIAN_POINT('Ctrl Pts',(40.6682079940824,2.79308561534073,-1.60955193073903));
#76671=CARTESIAN_POINT('Ctrl Pts',(40.6731468101554,2.83054765639472,-1.54271938521902));
#76672=CARTESIAN_POINT('Ctrl Pts',(40.6988518094608,3.0103220083431,-1.19336850452782));
#76673=CARTESIAN_POINT('Ctrl Pts',(40.7208555206752,3.11283674851488,-0.892396047288326));
#76674=CARTESIAN_POINT('Ctrl Pts',(40.7453280723297,3.18035920336323,-0.524219604486452));
#76675=CARTESIAN_POINT('Ctrl Pts',(40.7490690828834,3.18929075771276,-0.466815096782614));
#76676=CARTESIAN_POINT('Ctrl Pts',(40.7533537576054,3.19792481167503,-0.399365365385379));
#76677=CARTESIAN_POINT('Ctrl Pts',(40.7539758882693,3.19913792113715,-0.389528386398443));
#76678=CARTESIAN_POINT('Ctrl Pts',(40.7549131335055,3.2009042221205,-0.374640542904753));
#76679=CARTESIAN_POINT('Ctrl Pts',(40.7552300930692,3.20149086912764,-0.369593819368888));
#76680=CARTESIAN_POINT('Ctrl Pts',(40.7557967234085,3.20252048668558,-0.360549951750163));
#76681=CARTESIAN_POINT('Ctrl Pts',(40.7560466434655,3.20296791047684,-0.356553362634048));
#76682=CARTESIAN_POINT('Ctrl Pts',(40.7565840991829,3.20391564204478,-0.347942044669304));
#76683=CARTESIAN_POINT('Ctrl Pts',(40.7568714922465,3.20441345960861,-0.343327086484151));
#76684=CARTESIAN_POINT('Ctrl Pts',(40.757663008082,3.20575966164574,-0.33058925324667));
#76685=CARTESIAN_POINT('Ctrl Pts',(40.7581659618445,3.20658714953274,-0.322464135140428));
#76686=CARTESIAN_POINT('Ctrl Pts',(40.7608792923255,3.21089886576763,-0.278468745051941));
#76687=CARTESIAN_POINT('Ctrl Pts',(40.7630588437274,3.21381227257893,-0.242543404083277));
#76688=CARTESIAN_POINT('Ctrl Pts',(40.7694300811919,3.22064938085066,-0.136097907349347));
#76689=CARTESIAN_POINT('Ctrl Pts',(40.7735443335696,3.22285867264353,-0.0654860679921393));
#76690=CARTESIAN_POINT('Ctrl Pts',(40.7851490907652,3.22253574423974,0.136756083327457));
#76691=CARTESIAN_POINT('Ctrl Pts',(40.7924801727759,3.21426376028516,0.268236180175631));
#76692=CARTESIAN_POINT('Ctrl Pts',(40.8138452931435,3.16694963893702,0.647602796871585));
#76693=CARTESIAN_POINT('Ctrl Pts',(40.8279412604807,3.10701481029392,0.891849082088748));
#76694=CARTESIAN_POINT('Ctrl Pts',(40.8442509722197,3.01262235035659,1.14481404581125));
#76695=CARTESIAN_POINT('Ctrl Pts',(40.8454261461252,3.00568853246721,1.16289683368949));
#76696=CARTESIAN_POINT('Ctrl Pts',(40.8471748513558,2.99517789057144,1.18958555396114));
#76697=CARTESIAN_POINT('Ctrl Pts',(40.8477441738693,2.99172595483258,1.19824045778308));
#76698=CARTESIAN_POINT('Ctrl Pts',(40.8487577344429,2.98552762102993,1.21358753838897));
#76699=CARTESIAN_POINT('Ctrl Pts',(40.8492014656553,2.98279612303558,1.22028569454622));
#76700=CARTESIAN_POINT('Ctrl Pts',(40.8501349334438,2.97701255840337,1.23433265755208));
#76701=CARTESIAN_POINT('Ctrl Pts',(40.8506248276797,2.97395578238756,1.24167946144719));
#76702=CARTESIAN_POINT('Ctrl Pts',(40.851914411466,2.96585308455963,1.26095231278851));
#76703=CARTESIAN_POINT('Ctrl Pts',(40.8527156201121,2.96076247407987,1.27285930822398));
#76704=CARTESIAN_POINT('Ctrl Pts',(40.8563177057992,2.9376253775773,1.32608740641049));
#76705=CARTESIAN_POINT('Ctrl Pts',(40.8591456624544,2.91878537458856,1.3670560605923));
#76706=CARTESIAN_POINT('Ctrl Pts',(40.8667336472173,2.86648734871734,1.47476796981538));
#76707=CARTESIAN_POINT('Ctrl Pts',(40.8715428282265,2.83156072440399,1.54076368163563));
#76708=CARTESIAN_POINT('Ctrl Pts',(40.8957387757555,2.64712266128551,1.86178189951004));
#76709=CARTESIAN_POINT('Ctrl Pts',(40.9161944280046,2.46533852167192,2.09655829748027));
#76710=CARTESIAN_POINT('Ctrl Pts',(40.9410302121943,2.19677246649203,2.35939607506963));
#76711=CARTESIAN_POINT('Ctrl Pts',(40.9462462240171,2.13732942732533,2.41337615982134));
#76712=CARTESIAN_POINT('Ctrl Pts',(40.9519991343069,2.06756808855726,2.47212442934103));
#76713=CARTESIAN_POINT('Ctrl Pts',(40.9526856144752,2.05917295967253,2.47912156321815));
#76714=CARTESIAN_POINT('Ctrl Pts',(40.9536953277143,2.04671749650712,2.48939596549854));
#76715=CARTESIAN_POINT('Ctrl Pts',(40.9540209049078,2.04268464429904,2.49270620579504));
#76716=CARTESIAN_POINT('Ctrl Pts',(40.9545970136299,2.03551858507123,2.49855917164138));
#76717=CARTESIAN_POINT('Ctrl Pts',(40.9548478291248,2.03238862911907,2.50110581648721));
#76718=CARTESIAN_POINT('Ctrl Pts',(40.9553807672122,2.02571634491355,2.50651383145511));
#76719=CARTESIAN_POINT('Ctrl Pts',(40.9556627716094,2.02217274472622,2.50937356494077));
#76720=CARTESIAN_POINT('Ctrl Pts',(40.9564244830017,2.01256658522939,2.5170923039061));
#76721=CARTESIAN_POINT('Ctrl Pts',(40.9569031625239,2.00649244905026,2.52193695028403));
#76722=CARTESIAN_POINT('Ctrl Pts',(40.9592415913992,1.97663973137351,2.54557093536626));
#76723=CARTESIAN_POINT('Ctrl Pts',(40.9610798153957,1.95261350356946,2.56404693346831));
#76724=CARTESIAN_POINT('Ctrl Pts',(40.966215553248,1.88403615038903,2.61525932339684));
#76725=CARTESIAN_POINT('Ctrl Pts',(40.969466650066,1.83889666155041,2.64719348360908));
#76726=CARTESIAN_POINT('Ctrl Pts',(40.9727542574148,1.7917828152533,2.67873736985021));
#76727=CARTESIAN_POINT('Ctrl Pts',(40.9728360469865,1.79060976431233,2.67952164117767));
#76728=CARTESIAN_POINT('Ctrl Pts',(40.972917806056,1.78943621030417,2.68030513407564));
#76729=CARTESIAN_POINT('Origin',(-1.72497344927317,0.,0.));
#76730=CARTESIAN_POINT('',(42.4668644404635,1.78943621037806,2.68030513402632));
#76731=CARTESIAN_POINT('',(42.2181629331785,1.7894362082953,2.68030513541681));
#76732=CARTESIAN_POINT('',(-1.72497344927317,1.78943621037804,2.68030513402633));
#76733=CARTESIAN_POINT('',(41.6465734493189,-3.22274984877711,-0.000987272568188218));
#76734=CARTESIAN_POINT('Ctrl Pts',(41.6465734493189,-3.22274984877711,-0.000987272568138916));
#76735=CARTESIAN_POINT('Ctrl Pts',(41.6531888554372,-3.22271684721777,-0.108714129160543));
#76736=CARTESIAN_POINT('Ctrl Pts',(41.6598042615555,-3.21727816025484,-0.216286161899388));
#76737=CARTESIAN_POINT('Ctrl Pts',(41.6664196676738,-3.20650535883275,-0.323173244989212));
#76738=CARTESIAN_POINT('Ctrl Pts',(41.6730617404079,-3.19568913238853,-0.4304911885179));
#76739=CARTESIAN_POINT('Ctrl Pts',(41.6797038131421,-3.17949579627129,-0.537118334178048));
#76740=CARTESIAN_POINT('Ctrl Pts',(41.6863458858763,-3.15804844818564,-0.642532148154681));
#76741=CARTESIAN_POINT('Ctrl Pts',(41.6930019474588,-3.13655592990796,-0.748167973831837));
#76742=CARTESIAN_POINT('Ctrl Pts',(41.6996580090414,-3.10978738345449,-0.852585053181288));
#76743=CARTESIAN_POINT('Ctrl Pts',(41.7063140706239,-3.07791567669217,-0.955276216427788));
#76744=CARTESIAN_POINT('Ctrl Pts',(41.7129909883947,-3.04594410271754,-1.05828915347442));
#76745=CARTESIAN_POINT('Ctrl Pts',(41.7196679061655,-3.00883749347042,-1.15956505302346));
#76746=CARTESIAN_POINT('Ctrl Pts',(41.7263448239363,-2.9668173940531,-1.25861515676715));
#76747=CARTESIAN_POINT('Ctrl Pts',(41.729165111922,-2.94906836888673,-1.30045329633503));
#76748=CARTESIAN_POINT('Ctrl Pts',(41.7319853999078,-2.93044325601467,-1.34189462520743));
#76749=CARTESIAN_POINT('Ctrl Pts',(41.7348056878936,-2.91096115150686,-1.38290373378549));
#76750=CARTESIAN_POINT('Ctrl Pts',(41.7409779359863,-2.86832423534858,-1.47265286347875));
#76751=CARTESIAN_POINT('Ctrl Pts',(41.7471501840791,-2.82145774204699,-1.56058627746622));
#76752=CARTESIAN_POINT('Ctrl Pts',(41.7533224321719,-2.77053907784463,-1.64627785644946));
#76753=CARTESIAN_POINT('Ctrl Pts',(41.7594863208245,-2.71968937579647,-1.7318533782663));
#76754=CARTESIAN_POINT('Ctrl Pts',(41.7656502094771,-2.66479863097746,-1.81519272982256));
#76755=CARTESIAN_POINT('Ctrl Pts',(41.7718140981298,-2.60609148357015,-1.89589154272156));
#76756=CARTESIAN_POINT('Ctrl Pts',(41.7779714597883,-2.54744650166023,-1.97650490296165));
#76757=CARTESIAN_POINT('Ctrl Pts',(41.7841288214469,-2.48499340561815,-2.05448293411046));
#76758=CARTESIAN_POINT('Ctrl Pts',(41.7902861831054,-2.41900123876471,-2.12944841904067));
#76759=CARTESIAN_POINT('Ctrl Pts',(41.7964390472517,-2.35305727446859,-2.20435914704658));
#76760=CARTESIAN_POINT('Ctrl Pts',(41.802591911398,-2.28357966500936,-2.27626137864407));
#76761=CARTESIAN_POINT('Ctrl Pts',(41.8087447755444,-2.21087843322919,-2.34481003835748));
#76762=CARTESIAN_POINT('Ctrl Pts',(41.8148953086809,-2.13820474427747,-2.41333272844249));
#76763=CARTESIAN_POINT('Ctrl Pts',(41.8210458418174,-2.06231017534954,-2.47850407345808));
#76764=CARTESIAN_POINT('Ctrl Pts',(41.827196374954,-1.98354176732155,-2.54001567313883));
#76765=CARTESIAN_POINT('Ctrl Pts',(41.8333462231692,-1.90478213091737,-2.60152042290823));
#76766=CARTESIAN_POINT('Ctrl Pts',(41.8394960713844,-1.82314963403302,-2.65936597025777));
#76767=CARTESIAN_POINT('Ctrl Pts',(41.8456459195996,-1.73902377676392,-2.71328470057047));
#76768=CARTESIAN_POINT('Ctrl Pts',(41.8517967279787,-1.6548847850871,-2.76721184911045));
#76769=CARTESIAN_POINT('Ctrl Pts',(41.8579475363579,-1.56825202554976,-2.81721072845098));
#76770=CARTESIAN_POINT('Ctrl Pts',(41.864098344737,-1.47953243507694,-2.86305803923974));
#76771=CARTESIAN_POINT('Ctrl Pts',(41.8702557311032,-1.39071796336552,-2.90895438147252));
#76772=CARTESIAN_POINT('Ctrl Pts',(41.8764131174694,-1.2998125907652,-2.95069008932893));
#76773=CARTESIAN_POINT('Ctrl Pts',(41.8825705038356,-1.20724611690579,-2.98808874963845));
#76774=CARTESIAN_POINT('Ctrl Pts',(41.8887313265725,-1.11462798269791,-3.02550828173604));
#76775=CARTESIAN_POINT('Ctrl Pts',(41.8948921493095,-1.02034731093287,-3.05858580216776));
#76776=CARTESIAN_POINT('Ctrl Pts',(41.9010529720465,-0.924850066360242,
-3.08719450589908));
#76777=CARTESIAN_POINT('Ctrl Pts',(41.9072240949631,-0.829193161491493,
-3.1158510400587));
#76778=CARTESIAN_POINT('Ctrl Pts',(41.9133952178798,-0.732316042675764,
-3.14002372853251));
#76779=CARTESIAN_POINT('Ctrl Pts',(41.9195663407965,-0.634676030107168,
-3.15963667204117));
#76780=CARTESIAN_POINT('Ctrl Pts',(41.9242618627421,-0.560383097043063,
-3.17455988908045));
#76781=CARTESIAN_POINT('Ctrl Pts',(41.9289573846876,-0.485648722800563,
-3.18684430736783));
#76782=CARTESIAN_POINT('Ctrl Pts',(41.9336529066332,-0.410675552293991,
-3.19647667803912));
#76783=CARTESIAN_POINT('Ctrl Pts',(41.9398251547259,-0.312123567225377,
-3.20913839748034));
#76784=CARTESIAN_POINT('Ctrl Pts',(41.9459974028187,-0.212812002725103,
-3.21726038285199));
#76785=CARTESIAN_POINT('Ctrl Pts',(41.9521696509115,-0.113195239517363,
-3.22076146279892));
#76786=CARTESIAN_POINT('Ctrl Pts',(41.9583335395641,-0.0137133931755583,
-3.22425780102649));
#76787=CARTESIAN_POINT('Ctrl Pts',(41.9644974282167,0.0860724000127909,
-3.22314565789634));
#76788=CARTESIAN_POINT('Ctrl Pts',(41.9706613168693,0.185700516500948,-3.21739535660001));
#76789=CARTESIAN_POINT('Ctrl Pts',(41.9768186785279,0.285223135929762,-3.21165114434659));
#76790=CARTESIAN_POINT('Ctrl Pts',(41.9829760401864,0.384587979338632,-3.20127856311584));
#76791=CARTESIAN_POINT('Ctrl Pts',(41.9891334018449,0.48333225383915,-3.18629996938436));
#76792=CARTESIAN_POINT('Ctrl Pts',(41.9952862659912,0.582004402710598,-3.17133231644414));
#76793=CARTESIAN_POINT('Ctrl Pts',(42.0014391301375,0.680056455706556,-3.15176540488068));
#76794=CARTESIAN_POINT('Ctrl Pts',(42.0075919942838,0.777030499735695,-3.12767344282943));
#76795=CARTESIAN_POINT('Ctrl Pts',(42.0137425274204,0.873967805192531,-3.103590608007));
#76796=CARTESIAN_POINT('Ctrl Pts',(42.0198930605569,0.969827492085029,-3.0749862336431));
#76797=CARTESIAN_POINT('Ctrl Pts',(42.0260435936934,1.06416248280563,-3.04198549843502));
#76798=CARTESIAN_POINT('Ctrl Pts',(42.0321934419086,1.15848696841301,-3.00898843817785));
#76799=CARTESIAN_POINT('Ctrl Pts',(42.0383432901238,1.25128668540362,-2.97159613385995));
#76800=CARTESIAN_POINT('Ctrl Pts',(42.044493138339,1.34213131438872,-2.92998312238095));
#76801=CARTESIAN_POINT('Ctrl Pts',(42.0506439467182,1.43299012677032,-2.88836361394282));
#76802=CARTESIAN_POINT('Ctrl Pts',(42.0567947550973,1.5218928499006,-2.84252227037215));
#76803=CARTESIAN_POINT('Ctrl Pts',(42.0629455634764,1.6084316074118,-2.79268067039157));
#76804=CARTESIAN_POINT('Ctrl Pts',(42.0691029498426,1.69506291386803,-2.7427857672711));
#76805=CARTESIAN_POINT('Ctrl Pts',(42.0752603362088,1.77932482911819,-2.68888228207544));
#76806=CARTESIAN_POINT('Ctrl Pts',(42.0814177225749,1.86083655577004,-2.63123637767683));
#76807=CARTESIAN_POINT('Ctrl Pts',(42.0875785453119,1.94239377323541,-2.57355830172212));
#76808=CARTESIAN_POINT('Ctrl Pts',(42.0937393680488,2.02119740286241,-2.51213391418777));
#76809=CARTESIAN_POINT('Ctrl Pts',(42.0999001907858,2.0968996374192,-2.44726979981596));
#76810=CARTESIAN_POINT('Ctrl Pts',(42.1060713137025,2.17272843731557,-2.38229724018212));
#76811=CARTESIAN_POINT('Ctrl Pts',(42.1122424366191,2.24544516842659,-2.31387376442561));
#76812=CARTESIAN_POINT('Ctrl Pts',(42.1184135595358,2.31473870589036,-2.24234303485284));
#76813=CARTESIAN_POINT('Ctrl Pts',(42.1231090814815,2.36746319870094,-2.18791629355583));
#76814=CARTESIAN_POINT('Ctrl Pts',(42.1278046034272,2.41820660224388,-2.13169138250005));
#76815=CARTESIAN_POINT('Ctrl Pts',(42.1325001253728,2.46684819927642,-2.07383160459732));
#76816=CARTESIAN_POINT('Ctrl Pts',(42.1386723734656,2.53078741795934,-1.99777511759932));
#76817=CARTESIAN_POINT('Ctrl Pts',(42.1448446215584,2.59131848425128,-1.91862498491771));
#76818=CARTESIAN_POINT('Ctrl Pts',(42.1510168696512,2.64812742777466,-1.83671954548526));
#76819=CARTESIAN_POINT('Ctrl Pts',(42.1571807583038,2.70485943159059,-1.75492503542689));
#76820=CARTESIAN_POINT('Ctrl Pts',(42.1633446469565,2.75787908697984,-1.67038298951447));
#76821=CARTESIAN_POINT('Ctrl Pts',(42.1695085356091,2.80691182496822,-1.58346568303629));
#76822=CARTESIAN_POINT('Ctrl Pts',(42.1756658972677,2.85589264177358,-1.4966404140327));
#76823=CARTESIAN_POINT('Ctrl Pts',(42.1818232589263,2.90089472222778,-1.40744526112666));
#76824=CARTESIAN_POINT('Ctrl Pts',(42.1879806205848,2.94168663594483,-1.3162816181971));
#76825=CARTESIAN_POINT('Ctrl Pts',(42.1941334847312,2.98244875408687,-1.22518456378751));
#76826=CARTESIAN_POINT('Ctrl Pts',(42.2002863488775,3.01900664268743,-1.13212227332568));
#76827=CARTESIAN_POINT('Ctrl Pts',(42.2064392130238,3.05117512799439,-1.03752007248458));
#76828=CARTESIAN_POINT('Ctrl Pts',(42.2125897461604,3.08333142628539,-0.942953711644042));
#76829=CARTESIAN_POINT('Ctrl Pts',(42.2187402792969,3.11110148581676,-0.846849010418827));
#76830=CARTESIAN_POINT('Ctrl Pts',(42.2248908124335,3.13434886858439,-0.749649739881074));
#76831=CARTESIAN_POINT('Ctrl Pts',(42.2310406606487,3.15759366253118,-0.652461293421855));
#76832=CARTESIAN_POINT('Ctrl Pts',(42.2371905088639,3.17631667999076,-0.554178942447612));
#76833=CARTESIAN_POINT('Ctrl Pts',(42.2433403570792,3.1904320648593,-0.455259049352848));
#76834=CARTESIAN_POINT('Ctrl Pts',(42.2494911654583,3.20454965353562,-0.356323712086136));
#76835=CARTESIAN_POINT('Ctrl Pts',(42.2556419738375,3.21405811937742,-0.256751065050087));
#76836=CARTESIAN_POINT('Ctrl Pts',(42.2617927822167,3.21892331345298,-0.157004027365236));
#76837=CARTESIAN_POINT('Ctrl Pts',(42.2679501685829,3.22379371061431,-0.0571503151293831));
#76838=CARTESIAN_POINT('Ctrl Pts',(42.2741075549491,3.22401089871511,0.0428777254755896));
#76839=CARTESIAN_POINT('Ctrl Pts',(42.2802649413153,3.21959287528708,0.142615847298526));
#76840=CARTESIAN_POINT('Ctrl Pts',(42.2864257640523,3.21517238620793,0.242409631889109));
#76841=CARTESIAN_POINT('Ctrl Pts',(42.2925865867892,3.20611157329408,0.341912742874543));
#76842=CARTESIAN_POINT('Ctrl Pts',(42.2987474095262,3.19248027543204,0.440666828201722));
#76843=CARTESIAN_POINT('Ctrl Pts',(42.3049185324429,3.17882618762393,0.539586018884353));
#76844=CARTESIAN_POINT('Ctrl Pts',(42.3110896553596,3.16058643095412,0.637753255245494));
#76845=CARTESIAN_POINT('Ctrl Pts',(42.3172607782763,3.13788186881971,0.734720994549995));
#76846=CARTESIAN_POINT('Ctrl Pts',(42.3219563002217,3.12060628199354,0.808502404196861));
#76847=CARTESIAN_POINT('Ctrl Pts',(42.3266518221671,3.10074686348569,0.881589592692564));
#76848=CARTESIAN_POINT('Ctrl Pts',(42.3313473441125,3.07837571211205,0.953792712059928));
#76849=CARTESIAN_POINT('Ctrl Pts',(42.3375183118758,3.04897500744927,1.04868378640816));
#76850=CARTESIAN_POINT('Ctrl Pts',(42.343689279639,3.01513092331397,1.14238115422715));
#76851=CARTESIAN_POINT('Ctrl Pts',(42.3498602474023,2.9769582296873,1.23443803457164));
#76852=CARTESIAN_POINT('Ctrl Pts',(42.3560234343757,2.93883366687578,1.32637884313102));
#76853=CARTESIAN_POINT('Ctrl Pts',(42.3621866213491,2.89639150265972,1.41668287634627));
#76854=CARTESIAN_POINT('Ctrl Pts',(42.3683498083224,2.84979636673714,1.5049180145881));
#76855=CARTESIAN_POINT('Ctrl Pts',(42.3745068736213,2.80324751210626,1.59306551200454));
#76856=CARTESIAN_POINT('Ctrl Pts',(42.3806639389202,2.75255408509429,1.67914781649568));
#76857=CARTESIAN_POINT('Ctrl Pts',(42.3868210042191,2.69792855804005,1.76275326072934));
#76858=CARTESIAN_POINT('Ctrl Pts',(42.3929736012668,2.64334267334214,1.84629803155646));
#76859=CARTESIAN_POINT('Ctrl Pts',(42.3991261983146,2.58483059857675,1.92736915323287));
#76860=CARTESIAN_POINT('Ctrl Pts',(42.4052787953623,2.52264994534249,2.00558091728146));
#76861=CARTESIAN_POINT('Ctrl Pts',(42.4114292904071,2.4604905358059,2.08376596068651));
#76862=CARTESIAN_POINT('Ctrl Pts',(42.4175797854519,2.39466530625443,2.15909324642196));
#76863=CARTESIAN_POINT('Ctrl Pts',(42.4237302804968,2.32547376511001,2.23120804280665));
#76864=CARTESIAN_POINT('Ctrl Pts',(42.4298795872027,2.25629559248333,2.3033089058706));
#76865=CARTESIAN_POINT('Ctrl Pts',(42.4360288939086,2.18375270569772,2.37219820377838));
#76866=CARTESIAN_POINT('Ctrl Pts',(42.4421782006145,2.10818247187806,2.43755702041329));
#76867=CARTESIAN_POINT('Ctrl Pts',(42.4483294334061,2.03258856795084,2.50293630873582));
#76868=CARTESIAN_POINT('Ctrl Pts',(42.4544806661978,1.95396575454669,2.56478262620546));
#76869=CARTESIAN_POINT('Ctrl Pts',(42.4606318989895,1.87268504088621,2.62281686362983));
#76870=CARTESIAN_POINT('Ctrl Pts',(42.4627094128142,1.84523333940979,2.64241731359439));
#76871=CARTESIAN_POINT('Ctrl Pts',(42.4647869266388,1.81747871455803,2.66158328337868));
#76872=CARTESIAN_POINT('Ctrl Pts',(42.4668644404635,1.78943621037806,2.68030513402631));
#76873=CARTESIAN_POINT('Ctrl Pts',(41.2170239499866,1.789436210378,2.68030513402635));
#76874=CARTESIAN_POINT('Ctrl Pts',(41.2231741454125,1.70635148068182,2.73577449904767));
#76875=CARTESIAN_POINT('Ctrl Pts',(41.2293243408382,1.62065528784251,2.78739697266643));
#76876=CARTESIAN_POINT('Ctrl Pts',(41.235474536264,1.53274247640791,2.83492822898834));
#76877=CARTESIAN_POINT('Ctrl Pts',(41.2416244765792,1.44483331160414,2.88245751370973));
#76878=CARTESIAN_POINT('Ctrl Pts',(41.2477744168944,1.35470809335699,2.92589571228594));
#76879=CARTESIAN_POINT('Ctrl Pts',(41.2539243572096,1.26278658245949,2.96504428460357));
#76880=CARTESIAN_POINT('Ctrl Pts',(41.260075687455,1.17084429664666,3.00420170477702));
#76881=CARTESIAN_POINT('Ctrl Pts',(41.2662270177005,1.07710531129399,3.03906740251434));
#76882=CARTESIAN_POINT('Ctrl Pts',(41.2723783479459,0.982008744145685,3.0694912263959));
#76883=CARTESIAN_POINT('Ctrl Pts',(41.2785364887349,0.886806889313731,3.09994873450015));
#76884=CARTESIAN_POINT('Ctrl Pts',(41.2846946295239,0.79024486659597,3.12595441911275));
#76885=CARTESIAN_POINT('Ctrl Pts',(41.2908527703129,0.692776155103506,3.14740826100142));
#76886=CARTESIAN_POINT('Ctrl Pts',(41.2970147337812,0.595246939696369,3.16887542040912));
#76887=CARTESIAN_POINT('Ctrl Pts',(41.3031766972494,0.496810342641535,3.18578503802205));
#76888=CARTESIAN_POINT('Ctrl Pts',(41.3093386607177,0.397927170727749,3.19808873067909));
#76889=CARTESIAN_POINT('Ctrl Pts',(41.3155104475573,0.298886359756286,3.21041203782138));
#76890=CARTESIAN_POINT('Ctrl Pts',(41.3216822343969,0.199397985047641,3.21811472722107));
#76891=CARTESIAN_POINT('Ctrl Pts',(41.3278540212365,0.0999250258606228,
3.22120048300424));
#76892=CARTESIAN_POINT('Ctrl Pts',(41.3309397642958,0.0501909696836931,
3.2227432857189));
#76893=CARTESIAN_POINT('Ctrl Pts',(41.334025507355,0.000460725377187637,
3.2231327841228));
#76894=CARTESIAN_POINT('Ctrl Pts',(41.3371112504142,-0.0492083651102425,
3.22237429534546));
#76895=CARTESIAN_POINT('Ctrl Pts',(41.343283498507,-0.148558811063045,3.22085713049426));
#76896=CARTESIAN_POINT('Ctrl Pts',(41.3494557465998,-0.248013894267614,
3.21473831405031));
#76897=CARTESIAN_POINT('Ctrl Pts',(41.3556279946925,-0.347112303184287,
3.2040022801924));
#76898=CARTESIAN_POINT('Ctrl Pts',(41.3617918833451,-0.446076497272524,
3.19328078677927));
#76899=CARTESIAN_POINT('Ctrl Pts',(41.3679557719978,-0.544684549171801,
3.17795455158715));
#76900=CARTESIAN_POINT('Ctrl Pts',(41.3741196606504,-0.64247531955352,3.15806000992138));
#76901=CARTESIAN_POINT('Ctrl Pts',(41.3802770223089,-0.740162538457424,
3.13818653475485));
#76902=CARTESIAN_POINT('Ctrl Pts',(41.3864343839674,-0.837033773084093,
3.11375445647749));
#76903=CARTESIAN_POINT('Ctrl Pts',(41.392591745626,-0.93263414456588,3.08485187892221));
#76904=CARTESIAN_POINT('Ctrl Pts',(41.3987446097723,-1.02816468681501,3.05597041263231));
#76905=CARTESIAN_POINT('Ctrl Pts',(41.4048974739186,-1.12242579695264,3.02262506452357));
#76906=CARTESIAN_POINT('Ctrl Pts',(41.4110503380649,-1.21497481803341,2.98495456482083));
#76907=CARTESIAN_POINT('Ctrl Pts',(41.4172008712015,-1.30748877695991,2.94729833656965));
#76908=CARTESIAN_POINT('Ctrl Pts',(41.423351404338,-1.39829153376462,2.90532037615488));
#76909=CARTESIAN_POINT('Ctrl Pts',(41.4295019374746,-1.48695842267173,2.85920831905365));
#76910=CARTESIAN_POINT('Ctrl Pts',(41.4356517856898,-1.5756154376633,2.81310139697591));
#76911=CARTESIAN_POINT('Ctrl Pts',(41.441801633905,-1.66213667226087,2.76286149391629));
#76912=CARTESIAN_POINT('Ctrl Pts',(41.4479514821202,-1.74612108424166,2.70872271036862));
#76913=CARTESIAN_POINT('Ctrl Pts',(41.4541022904993,-1.83011860854692,2.65457547423696));
#76914=CARTESIAN_POINT('Ctrl Pts',(41.4602530988785,-1.91157815841264,2.59652838390418));
#76915=CARTESIAN_POINT('Ctrl Pts',(41.4664039072576,-1.99012761168494,2.5348589017358));
#76916=CARTESIAN_POINT('Ctrl Pts',(41.4725612936238,-2.06876106973406,2.47312346708945));
#76917=CARTESIAN_POINT('Ctrl Pts',(41.47871867999,-2.14447787411286,2.40775817345017));
#76918=CARTESIAN_POINT('Ctrl Pts',(41.4848760663562,-2.21693906097446,2.33908075158292));
#76919=CARTESIAN_POINT('Ctrl Pts',(41.4910368890932,-2.28944068764113,2.27036500158892));
#76920=CARTESIAN_POINT('Ctrl Pts',(41.4971977118301,-2.35868277737298,2.19833375534159));
#76921=CARTESIAN_POINT('Ctrl Pts',(41.5033585345671,-2.42436478206505,2.1233400495405));
#76922=CARTESIAN_POINT('Ctrl Pts',(41.5095296574838,-2.49015659943671,2.04822096297761));
#76923=CARTESIAN_POINT('Ctrl Pts',(41.5157007804005,-2.55237617192966,1.97012986350473));
#76924=CARTESIAN_POINT('Ctrl Pts',(41.5218719033172,-2.61076454491503,1.88945125724762));
#76925=CARTESIAN_POINT('Ctrl Pts',(41.5265674252627,-2.65519144913029,1.82806402329775));
#76926=CARTESIAN_POINT('Ctrl Pts',(41.5312629472083,-2.69740115169467,1.7651794096343));
#76927=CARTESIAN_POINT('Ctrl Pts',(41.5359584691539,-2.7372974487943,1.70097626065863));
#76928=CARTESIAN_POINT('Ctrl Pts',(41.5423065722644,-2.79123518152077,1.61417691983259));
#76929=CARTESIAN_POINT('Ctrl Pts',(41.5486546753748,-2.84112404934189,1.5246755827609));
#76930=CARTESIAN_POINT('Ctrl Pts',(41.5550027784852,-2.88669177993702,1.4328740803518));
#76931=CARTESIAN_POINT('Ctrl Pts',(41.561340685878,-2.93218632398999,1.3412200207589));
#76932=CARTESIAN_POINT('Ctrl Pts',(41.5676785932707,-2.97337336231237,1.24727350226578));
#76933=CARTESIAN_POINT('Ctrl Pts',(41.5740165006635,-3.01002462655561,1.15146398555436));
#76934=CARTESIAN_POINT('Ctrl Pts',(41.5803429132751,-3.04660941802866,1.05582823430831));
#76935=CARTESIAN_POINT('Ctrl Pts',(41.5866693258867,-3.07867467933153,0.958336587463989));
#76936=CARTESIAN_POINT('Ctrl Pts',(41.5929957384983,-3.10603918615133,0.859440595150354));
#76937=CARTESIAN_POINT('Ctrl Pts',(41.5993154040876,-3.13337450914324,0.760650073899592));
#76938=CARTESIAN_POINT('Ctrl Pts',(41.6056350696769,-3.15601894407938,0.660458570956468));
#76939=CARTESIAN_POINT('Ctrl Pts',(41.6119547352663,-3.17384021541428,0.559335185303994));
#76940=CARTESIAN_POINT('Ctrl Pts',(41.6182677003448,-3.19164259150543,0.458319017087579));
#76941=CARTESIAN_POINT('Ctrl Pts',(41.6245806654233,-3.20463191844682,0.356373327360609));
#76942=CARTESIAN_POINT('Ctrl Pts',(41.6308936305018,-3.21272660233886,0.253979017094328));
#76943=CARTESIAN_POINT('Ctrl Pts',(41.6361202367589,-3.21942832252161,0.169205105615897));
#76944=CARTESIAN_POINT('Ctrl Pts',(41.641346843016,-3.22277592216168,0.0841240354286471));
#76945=CARTESIAN_POINT('Ctrl Pts',(41.6465734492731,-3.22274984877734,-0.000987271822784419));
#76946=CARTESIAN_POINT('',(41.3996307778974,-3.22274865316434,0.00294635832935292));
#76947=CARTESIAN_POINT('Ctrl Pts',(40.972917806056,1.78943621030417,2.68030513407564));
#76948=CARTESIAN_POINT('Ctrl Pts',(40.980957584323,1.67403477442647,2.75734990985707));
#76949=CARTESIAN_POINT('Ctrl Pts',(40.9887073764522,1.55376902517541,2.82686727887822));
#76950=CARTESIAN_POINT('Ctrl Pts',(41.0100377824585,1.2116588987041,2.99616686366643));
#76951=CARTESIAN_POINT('Ctrl Pts',(41.0236188803539,0.982475836522961,3.0789374930667));
#76952=CARTESIAN_POINT('Ctrl Pts',(41.0386060427792,0.73872344541865,3.13695139008336));
#76953=CARTESIAN_POINT('Ctrl Pts',(41.0390654799045,0.731258067519423,3.13870004774921));
#76954=CARTESIAN_POINT('Ctrl Pts',(41.0412107982511,0.696432798931211,3.14672637711884));
#76955=CARTESIAN_POINT('Ctrl Pts',(41.0429068299818,0.668998518026038,3.1526729044838));
#76956=CARTESIAN_POINT('Ctrl Pts',(41.0452933938915,0.630551126726525,3.1604821547801));
#76957=CARTESIAN_POINT('Ctrl Pts',(41.0459742475717,0.619600188803281,3.16264727328437));
#76958=CARTESIAN_POINT('Ctrl Pts',(41.0470733980874,0.60195082073379,3.16604155829027));
#76959=CARTESIAN_POINT('Ctrl Pts',(41.0474905502978,0.59525929253796,3.16730647600172));
#76960=CARTESIAN_POINT('Ctrl Pts',(41.0483568385336,0.581377611438307,3.16988502302879));
#76961=CARTESIAN_POINT('Ctrl Pts',(41.0488060750347,0.57418690443771,3.17119541871411));
#76962=CARTESIAN_POINT('Ctrl Pts',(41.0498489833794,0.557512546622209,3.17417549139952));
#76963=CARTESIAN_POINT('Ctrl Pts',(41.0504432258945,0.548025782576076,3.17582714080104));
#76964=CARTESIAN_POINT('Ctrl Pts',(41.0523301981932,0.517947367657273,3.18092501939036));
#76965=CARTESIAN_POINT('Ctrl Pts',(41.053627922684,0.49732988106972,3.18421362521021));
#76966=CARTESIAN_POINT('Ctrl Pts',(41.0613795447484,0.374600617119166,3.20256860773854));
#76967=CARTESIAN_POINT('Ctrl Pts',(41.0679814821593,0.271854947992482,3.21292115242249));
#76968=CARTESIAN_POINT('Ctrl Pts',(41.0880760314614,-0.0355140691247797,
3.22904238198276));
#76969=CARTESIAN_POINT('Ctrl Pts',(41.1019533968349,-0.240364069228848,
3.2202769762283));
#76970=CARTESIAN_POINT('Ctrl Pts',(41.1237531475644,-0.559764665086802,
3.17595401467161));
#76971=CARTESIAN_POINT('Ctrl Pts',(41.1316822142413,-0.675586645266371,
3.15334851807387));
#76972=CARTESIAN_POINT('Ctrl Pts',(41.1431342486706,-0.845478873139643,
3.11039669788195));
#76973=CARTESIAN_POINT('Ctrl Pts',(41.1468245362911,-0.900661595518483,
3.09486862599111));
#76974=CARTESIAN_POINT('Ctrl Pts',(41.1510580198752,-0.964832172832273,
3.07494941137412));
#76975=CARTESIAN_POINT('Ctrl Pts',(41.1516776150025,-0.974246333396892,
3.07197966987172));
#76976=CARTESIAN_POINT('Ctrl Pts',(41.152611798047,-0.988476838320987,3.06741859354113));
#76977=CARTESIAN_POINT('Ctrl Pts',(41.1529282132672,-0.993303210872229,
3.06585909983028));
#76978=CARTESIAN_POINT('Ctrl Pts',(41.153494254275,-1.00194906352601,3.06304289943937));
#76979=CARTESIAN_POINT('Ctrl Pts',(41.1537441271462,-1.00576987568242,3.06179043820328));
#76980=CARTESIAN_POINT('Ctrl Pts',(41.1542819116748,-1.01400226186873,3.05907479110576));
#76981=CARTESIAN_POINT('Ctrl Pts',(41.1545696790777,-1.01841300119325,3.05760921706868));
#76982=CARTESIAN_POINT('Ctrl Pts',(41.1553632744113,-1.03059170051063,3.05353327537096));
#76983=CARTESIAN_POINT('Ctrl Pts',(41.1558679231591,-1.03835296452589,3.05090279121717));
#76984=CARTESIAN_POINT('Ctrl Pts',(41.1585620612214,-1.07987136539258,3.0366543936234));
#76985=CARTESIAN_POINT('Ctrl Pts',(41.1607213526855,-1.11344530574384,3.02450522801414));
#76986=CARTESIAN_POINT('Ctrl Pts',(41.1670299422431,-1.21212827182131,2.98692942218416));
#76987=CARTESIAN_POINT('Ctrl Pts',(41.1711033394766,-1.27662275848237,2.95993884921536));
#76988=CARTESIAN_POINT('Ctrl Pts',(41.1861593399872,-1.515140261821,2.85087248226606));
#76989=CARTESIAN_POINT('Ctrl Pts',(41.1967320934736,-1.68258141155163,2.75536772896923));
#76990=CARTESIAN_POINT('Ctrl Pts',(41.2182495554033,-1.99648878942316,2.53697753162626));
#76991=CARTESIAN_POINT('Ctrl Pts',(41.2291511645902,-2.14254158688703,2.41489603816608));
#76992=CARTESIAN_POINT('Ctrl Pts',(41.2417044789304,-2.28966783132644,2.26800796843223));
#76993=CARTESIAN_POINT('Ctrl Pts',(41.2427914679644,-2.3022479575006,2.25523684893812));
#76994=CARTESIAN_POINT('Ctrl Pts',(41.2444412126697,-2.3210970356885,2.23577952745254));
#76995=CARTESIAN_POINT('Ctrl Pts',(41.2450005084585,-2.32744522737459,2.22917030648221));
#76996=CARTESIAN_POINT('Ctrl Pts',(41.2459747616216,-2.33842991676013,2.2176358674692));
#76997=CARTESIAN_POINT('Ctrl Pts',(41.2463891588106,-2.34307928020381,2.21272293834061));
#76998=CARTESIAN_POINT('Ctrl Pts',(41.2472547157605,-2.35274243080177,2.20244739152366));
#76999=CARTESIAN_POINT('Ctrl Pts',(41.2477059919976,-2.3577534249839,2.19708221140661));
#77000=CARTESIAN_POINT('Ctrl Pts',(41.2486039153174,-2.3676700267056,2.18639169206184));
#77001=CARTESIAN_POINT('Ctrl Pts',(41.2490505382254,-2.37257610742014,2.18106684895383));
#77002=CARTESIAN_POINT('Ctrl Pts',(41.2500947522579,-2.3839848641791,2.16860024424316));
#77003=CARTESIAN_POINT('Ctrl Pts',(41.2506929374452,-2.39047343498167,2.16144572111962));
#77004=CARTESIAN_POINT('Ctrl Pts',(41.2541623315757,-2.42783340103523,2.1198773308669));
#77005=CARTESIAN_POINT('Ctrl Pts',(41.2570632236582,-2.45799225818394,2.08483299601679));
#77006=CARTESIAN_POINT('Ctrl Pts',(41.267586577498,-2.56350355193783,1.95675704569465));
#77007=CARTESIAN_POINT('Ctrl Pts',(41.275380692213,-2.63440570316206,1.86020148537382));
#77008=CARTESIAN_POINT('Ctrl Pts',(41.2894731125337,-2.75035948935685,1.68232664511113));
#77009=CARTESIAN_POINT('Ctrl Pts',(41.2957036281926,-2.797579231196,1.60257581120209));
#77010=CARTESIAN_POINT('Ctrl Pts',(41.3093819122003,-2.89308880458486,1.42414855275538));
#77011=CARTESIAN_POINT('Ctrl Pts',(41.3168340968007,-2.93990567010013,1.32480834142187));
#77012=CARTESIAN_POINT('Ctrl Pts',(41.3290186368766,-3.00884358159769,1.15678136266766));
#77013=CARTESIAN_POINT('Ctrl Pts',(41.3337979309899,-3.03389326108652,1.08939234692077));
#77014=CARTESIAN_POINT('Ctrl Pts',(41.3421564354891,-3.07444941986071,0.968001298429983));
#77015=CARTESIAN_POINT('Ctrl Pts',(41.3457674415938,-3.09083755589449,0.914324818958046));
#77016=CARTESIAN_POINT('Ctrl Pts',(41.349866403996,-3.108204256811,0.851624248774252));
#77017=CARTESIAN_POINT('Ctrl Pts',(41.3504279715182,-3.1105558867676,0.842994450106333));
#77018=CARTESIAN_POINT('Ctrl Pts',(41.3513195131313,-3.11424563056493,0.829228486384964));
#77019=CARTESIAN_POINT('Ctrl Pts',(41.3516508018782,-3.11560701659807,0.824098689000286));
#77020=CARTESIAN_POINT('Ctrl Pts',(41.3522341480687,-3.11798718013355,0.815039865022391));
#77021=CARTESIAN_POINT('Ctrl Pts',(41.3524865098037,-3.11901121464037,0.811112249157957));
#77022=CARTESIAN_POINT('Ctrl Pts',(41.3530150874122,-3.12114424586065,0.80286737818465));
#77023=CARTESIAN_POINT('Ctrl Pts',(41.3532912132257,-3.12225170423916,0.798549764493275));
#77024=CARTESIAN_POINT('Ctrl Pts',(41.3540205858157,-3.12515876960255,0.787117578492366));
#77025=CARTESIAN_POINT('Ctrl Pts',(41.3544729498594,-3.12694305218309,0.779999082360786));
#77026=CARTESIAN_POINT('Ctrl Pts',(41.3554609261163,-3.13079837503754,0.764392200885226));
#77027=CARTESIAN_POINT('Ctrl Pts',(41.3559959710274,-3.13285925014294,0.755901332660203));
#77028=CARTESIAN_POINT('Ctrl Pts',(41.3575855143787,-3.13889993420492,0.730564430291809));
#77029=CARTESIAN_POINT('Ctrl Pts',(41.3586346240465,-3.14277865087828,0.713694307322203));
#77030=CARTESIAN_POINT('Ctrl Pts',(41.3737299025313,-3.19697086577163,0.468977618165554));
#77031=CARTESIAN_POINT('Ctrl Pts',(41.3865738748205,-3.22253528388174,0.236331266495792));
#77032=CARTESIAN_POINT('Ctrl Pts',(41.3996307778974,-3.22274865316434,0.00294635832935292));
#77033=CARTESIAN_POINT('Ctrl Pts',(41.3996308389411,-3.22274865416171,0.00294526720681157));
#77034=CARTESIAN_POINT('Ctrl Pts',(41.4101609837527,-3.22292066871231,-0.185275231143605));
#77035=CARTESIAN_POINT('Ctrl Pts',(41.4207837320835,-3.2066040436147,-0.37313437457173));
#77036=CARTESIAN_POINT('Ctrl Pts',(41.4346359164017,-3.16606665841715,-0.603514064877092));
#77037=CARTESIAN_POINT('Ctrl Pts',(41.4373704933508,-3.15718789313295,-0.64836070533953));
#77038=CARTESIAN_POINT('Ctrl Pts',(41.4408847759572,-3.14469440171184,-0.705101543230631));
#77039=CARTESIAN_POINT('Ctrl Pts',(41.4416363749525,-3.14196047385066,-0.717185778268995));
#77040=CARTESIAN_POINT('Ctrl Pts',(41.4428973454155,-3.13727085922018,-0.737372763963564));
#77041=CARTESIAN_POINT('Ctrl Pts',(41.4434054936418,-3.13535328037617,-0.745484300528934));
#77042=CARTESIAN_POINT('Ctrl Pts',(41.444407091479,-3.13151926918105,-0.761426039385879));
#77043=CARTESIAN_POINT('Ctrl Pts',(41.4449004720729,-3.12960488149455,-0.769256674046396));
#77044=CARTESIAN_POINT('Ctrl Pts',(41.4458370319191,-3.12592227937388,-0.784078740958211));
#77045=CARTESIAN_POINT('Ctrl Pts',(41.4462800187235,-3.12415993567352,-0.791071592016112));
#77046=CARTESIAN_POINT('Ctrl Pts',(41.4472855542911,-3.1201133342246,-0.806903770923343));
#77047=CARTESIAN_POINT('Ctrl Pts',(41.4478485576607,-3.11781496360198,-0.815739397068185));
#77048=CARTESIAN_POINT('Ctrl Pts',(41.4495140121126,-3.11092007882728,-0.841790548517696));
#77049=CARTESIAN_POINT('Ctrl Pts',(41.4506198717715,-3.10621835348575,-0.858977639021715));
#77050=CARTESIAN_POINT('Ctrl Pts',(41.4585175222862,-3.07176975141496,-0.980921498774192));
#77051=CARTESIAN_POINT('Ctrl Pts',(41.4654770630248,-3.03687573875394,-1.0841391014907));
#77052=CARTESIAN_POINT('Ctrl Pts',(41.4734735641859,-2.99183893609184,-1.19799890577171));
#77053=CARTESIAN_POINT('Ctrl Pts',(41.4743617336352,-2.9867695885259,-1.21058209763802));
#77054=CARTESIAN_POINT('Ctrl Pts',(41.4817031482774,-2.94431356955439,-1.31407679577869));
#77055=CARTESIAN_POINT('Ctrl Pts',(41.4882639431685,-2.90286718693912,-1.40326049987602));
#77056=CARTESIAN_POINT('Ctrl Pts',(41.5020922428597,-2.80789815596172,-1.58533558153205));
#77057=CARTESIAN_POINT('Ctrl Pts',(41.5093625777834,-2.75368371772362,-1.67773850786885));
#77058=CARTESIAN_POINT('Ctrl Pts',(41.5259672062774,-2.61876733667292,-1.88347722767872));
#77059=CARTESIAN_POINT('Ctrl Pts',(41.5352563835041,-2.53511753338876,-1.99464686724353));
#77060=CARTESIAN_POINT('Ctrl Pts',(41.5457700151251,-2.42800741622158,-2.11932570617653));
#77061=CARTESIAN_POINT('Ctrl Pts',(41.5473792802327,-2.41124452241144,-2.13837821976389));
#77062=CARTESIAN_POINT('Ctrl Pts',(41.5494395006869,-2.38928045650573,-2.16275559232747));
#77063=CARTESIAN_POINT('Ctrl Pts',(41.5499049948148,-2.38428402200986,-2.16826256642882));
#77064=CARTESIAN_POINT('Ctrl Pts',(41.5506485994047,-2.3762473801383,-2.17705902833002));
#77065=CARTESIAN_POINT('Ctrl Pts',(41.5509276172846,-2.3732193337418,-2.18035951599411));
#77066=CARTESIAN_POINT('Ctrl Pts',(41.5514580732704,-2.36743847351322,-2.18663418522138));
#77067=CARTESIAN_POINT('Ctrl Pts',(41.5517096001292,-2.36468696367123,-2.18960945144182));
#77068=CARTESIAN_POINT('Ctrl Pts',(41.5522868689135,-2.35834832189242,-2.19643767659625));
#77069=CARTESIAN_POINT('Ctrl Pts',(41.5526123128179,-2.35475735989784,-2.20028703843058));
#77070=CARTESIAN_POINT('Ctrl Pts',(41.5536444961484,-2.34331332438144,-2.21249446392588));
#77071=CARTESIAN_POINT('Ctrl Pts',(41.5543485728151,-2.33542495362664,-2.22081952988898));
#77072=CARTESIAN_POINT('Ctrl Pts',(41.5675857807291,-2.18560464052134,-2.37725271909167));
#77073=CARTESIAN_POINT('Ctrl Pts',(41.579087259001,-2.02987112057745,-2.51154315726582));
#77074=CARTESIAN_POINT('Ctrl Pts',(41.5997845458028,-1.72777895193172,-2.72545559509027));
#77075=CARTESIAN_POINT('Ctrl Pts',(41.6089601979415,-1.58603893305355,-2.81030340594898));
#77076=CARTESIAN_POINT('Ctrl Pts',(41.6229182000108,-1.36892008311917,-2.91859723241247));
#77077=CARTESIAN_POINT('Ctrl Pts',(41.6274491850044,-1.29817890194282,-2.95074265819879));
#77078=CARTESIAN_POINT('Ctrl Pts',(41.6348135389141,-1.18355012062124,-2.99791070208356));
#77079=CARTESIAN_POINT('Ctrl Pts',(41.6375918017885,-1.14037854569827,-3.01459713826682));
#77080=CARTESIAN_POINT('Ctrl Pts',(41.6411924577925,-1.08461166028488,-3.03478251333899));
#77081=CARTESIAN_POINT('Ctrl Pts',(41.6419859981151,-1.07233244007331,-3.03914305143121));
#77082=CARTESIAN_POINT('Ctrl Pts',(41.6432728509826,-1.05243967530325,-3.04607170759743));
#77083=CARTESIAN_POINT('Ctrl Pts',(41.6437646240839,-1.04484229702476,-3.04868605967826));
#77084=CARTESIAN_POINT('Ctrl Pts',(41.6446998965571,-1.03040269125539,-3.05359459247757));
#77085=CARTESIAN_POINT('Ctrl Pts',(41.6451432108069,-1.02356236926262,-3.0558942580258));
#77086=CARTESIAN_POINT('Ctrl Pts',(41.646151913646,-1.00800754856697,-3.06106558788978));
#77087=CARTESIAN_POINT('Ctrl Pts',(41.6467177679957,-0.999288422945987,
-3.06392304020655));
#77088=CARTESIAN_POINT('Ctrl Pts',(41.6484372861928,-0.972814041576651,
-3.07247425876791));
#77089=CARTESIAN_POINT('Ctrl Pts',(41.6495947856717,-0.955021703470315,
-3.07805112897944));
#77090=CARTESIAN_POINT('Ctrl Pts',(41.6585337071672,-0.817858721331375,
-3.11974006437207));
#77091=CARTESIAN_POINT('Ctrl Pts',(41.6665367618616,-0.696545584555774,
-3.14904564045875));
#77092=CARTESIAN_POINT('Ctrl Pts',(41.6862708095288,-0.400982854423891,
-3.20252909398001));
#77093=CARTESIAN_POINT('Ctrl Pts',(41.6981667776634,-0.225858522660113,
-3.21962073225346));
#77094=CARTESIAN_POINT('Ctrl Pts',(41.7223526362528,0.131577845530588,-3.2251926589007));
#77095=CARTESIAN_POINT('Ctrl Pts',(41.734595686057,0.313324992523949,-3.21263508685753));
#77096=CARTESIAN_POINT('Ctrl Pts',(41.7469095899262,0.505780280299551,-3.18283985422686));
#77097=CARTESIAN_POINT('Ctrl Pts',(41.7477195238514,0.518488264655123,-3.18079442311357));
#77098=CARTESIAN_POINT('Ctrl Pts',(41.7488814112151,0.536795331804624,-3.17773515285817));
#77099=CARTESIAN_POINT('Ctrl Pts',(41.7492367301017,0.542404319754735,-3.17678256811051));
#77100=CARTESIAN_POINT('Ctrl Pts',(41.7498470515294,0.552057340823478,-3.17511686665986));
#77101=CARTESIAN_POINT('Ctrl Pts',(41.7501024579607,0.556102574271717,-3.17441086693698));
#77102=CARTESIAN_POINT('Ctrl Pts',(41.7505943059448,0.563903791934002,-3.17303397917033));
#77103=CARTESIAN_POINT('Ctrl Pts',(41.7508308085039,0.567659928901751,-3.1723641539092));
#77104=CARTESIAN_POINT('Ctrl Pts',(41.7513949599317,0.576631360882703,-3.1707478504196));
#77105=CARTESIAN_POINT('Ctrl Pts',(41.7517222554968,0.581845548407632,-3.16979516941375));
#77106=CARTESIAN_POINT('Ctrl Pts',(41.7527125496249,0.59764946688726,-3.16686733532586));
#77107=CARTESIAN_POINT('Ctrl Pts',(41.7533733071196,0.608231796460825,-3.16485192295055));
#77108=CARTESIAN_POINT('Ctrl Pts',(41.7622654608353,0.751112757138264,-3.13689701852716));
#77109=CARTESIAN_POINT('Ctrl Pts',(41.7700539637878,0.881685121248366,-3.10273012347454));
#77110=CARTESIAN_POINT('Ctrl Pts',(41.7918661125119,1.24735908910469,-2.98208278985948));
#77111=CARTESIAN_POINT('Ctrl Pts',(41.8055122053887,1.47502514175452,-2.87628677778942));
#77112=CARTESIAN_POINT('Ctrl Pts',(41.8239015214452,1.74573136360546,-2.70981674816123));
#77113=CARTESIAN_POINT('Ctrl Pts',(41.8278625908618,1.80216791083966,-2.67261570894969));
#77114=CARTESIAN_POINT('Ctrl Pts',(41.8335380702332,1.88003922898702,-2.61769710646741));
#77115=CARTESIAN_POINT('Ctrl Pts',(41.8351991518457,1.90248014290615,-2.60143323546238));
#77116=CARTESIAN_POINT('Ctrl Pts',(41.8381271469185,1.94140359901069,-2.57245076048246));
#77117=CARTESIAN_POINT('Ctrl Pts',(41.8393891926808,1.95797804895761,-2.55985796046748));
#77118=CARTESIAN_POINT('Ctrl Pts',(41.8412404050538,1.98198887004077,-2.54124559484091));
#77119=CARTESIAN_POINT('Ctrl Pts',(41.8418245826476,1.98952249646303,-2.53535190599361));
#77120=CARTESIAN_POINT('Ctrl Pts',(41.8428568653536,2.0027580013335,-2.52490221945136));
#77121=CARTESIAN_POINT('Ctrl Pts',(41.8433044092251,2.00847087481128,-2.52036020706156));
#77122=CARTESIAN_POINT('Ctrl Pts',(41.844172130646,2.01949800274255,-2.51153180223163));
#77123=CARTESIAN_POINT('Ctrl Pts',(41.8445922085786,2.0248141659362,-2.50724784753738));
#77124=CARTESIAN_POINT('Ctrl Pts',(41.8457065766934,2.03885755325565,-2.49585738914383));
#77125=CARTESIAN_POINT('Ctrl Pts',(41.8464020326518,2.04756117427818,-2.48872205395502));
#77126=CARTESIAN_POINT('Ctrl Pts',(41.8488722893242,2.07826061597207,-2.46328422448105));
#77127=CARTESIAN_POINT('Ctrl Pts',(41.8506571533664,2.10004934835103,-2.44473495655003));
#77128=CARTESIAN_POINT('Ctrl Pts',(41.8528744087912,2.12662757904884,-2.42149076634008));
#77129=CARTESIAN_POINT('Ctrl Pts',(41.8532955067176,2.13165373860917,-2.41706738197877));
#77130=CARTESIAN_POINT('Ctrl Pts',(41.8696681866981,2.32623850712508,-2.24473969602674));
#77131=CARTESIAN_POINT('Ctrl Pts',(41.8865940554169,2.49532658028293,-2.05512492662079));
#77132=CARTESIAN_POINT('Ctrl Pts',(41.9175801968807,2.75780891158807,-1.68003038129437));
#77133=CARTESIAN_POINT('Ctrl Pts',(41.9314665902514,2.8589310548206,-1.5015138538914));
#77134=CARTESIAN_POINT('Ctrl Pts',(41.9453847689313,2.94854310027333,-1.30093616725125));
#77135=CARTESIAN_POINT('Ctrl Pts',(41.9463272765626,2.95454989162051,-1.28723590835997));
#77136=CARTESIAN_POINT('Ctrl Pts',(41.9476354298151,2.96280383584513,-1.26804816076304));
#77137=CARTESIAN_POINT('Ctrl Pts',(41.9480058218087,2.96513145525455,-1.26259580314025));
#77138=CARTESIAN_POINT('Ctrl Pts',(41.9486340300147,2.96906344650798,-1.25331442491127));
#77139=CARTESIAN_POINT('Ctrl Pts',(41.9488923120766,2.97067548173606,-1.249488687402));
#77140=CARTESIAN_POINT('Ctrl Pts',(41.9493838139719,2.973734497994,-1.24218954103691));
#77141=CARTESIAN_POINT('Ctrl Pts',(41.9496171152882,2.97518279046933,-1.2387167085592));
#77142=CARTESIAN_POINT('Ctrl Pts',(41.9501655802575,2.97857864925566,-1.2305335317448));
#77143=CARTESIAN_POINT('Ctrl Pts',(41.9504804348797,2.98052113659516,-1.22582107083507));
#77144=CARTESIAN_POINT('Ctrl Pts',(41.9514088365538,2.98622793670706,-1.21188265099598));
#77145=CARTESIAN_POINT('Ctrl Pts',(41.9520205110591,2.98996069258822,-1.20264371806954));
#77146=CARTESIAN_POINT('Ctrl Pts',(41.9577860711542,3.0248788786772,-1.11505033344076));
#77147=CARTESIAN_POINT('Ctrl Pts',(41.9627674763962,3.05302338059868,-1.03550977188465));
#77148=CARTESIAN_POINT('Ctrl Pts',(41.9689647025155,3.0847621278938,-0.933208618793959));
#77149=CARTESIAN_POINT('Ctrl Pts',(41.9702741390275,3.09127670787651,-0.911396765009225));
#77150=CARTESIAN_POINT('Ctrl Pts',(41.9872816734895,3.17327016891815,-0.625871536357382));
#77151=CARTESIAN_POINT('Ctrl Pts',(42.0021201130746,3.21501338363019,-0.353639111426309));
#77152=CARTESIAN_POINT('Ctrl Pts',(42.0220536919655,3.22351668149749,-0.00859460259406048));
#77153=CARTESIAN_POINT('Ctrl Pts',(42.0261982704399,3.22292700887958,0.0622425999063536));
#77154=CARTESIAN_POINT('Ctrl Pts',(42.0329938607677,3.21821452912751,0.176334783075657));
#77155=CARTESIAN_POINT('Ctrl Pts',(42.0356003462993,3.21555004051634,0.219627806610689));
#77156=CARTESIAN_POINT('Ctrl Pts',(42.0390099496316,3.21097114394594,0.275581173165909));
#77157=CARTESIAN_POINT('Ctrl Pts',(42.0397879427736,3.20985384921835,0.288303537209825));
#77158=CARTESIAN_POINT('Ctrl Pts',(42.0410521228458,3.20792142860916,0.308901861826796));
#77159=CARTESIAN_POINT('Ctrl Pts',(42.0415368405485,3.20715283873196,0.316782132723543));
#77160=CARTESIAN_POINT('Ctrl Pts',(42.0424668050541,3.20562544513741,0.33186675951989));
#77161=CARTESIAN_POINT('Ctrl Pts',(42.0429118998262,3.20487137341624,0.339071554511315));
#77162=CARTESIAN_POINT('Ctrl Pts',(42.0439265889121,3.20310001200219,0.355462076680321));
#77163=CARTESIAN_POINT('Ctrl Pts',(42.0444966610165,3.20206749166539,0.364646062388857));
#77164=CARTESIAN_POINT('Ctrl Pts',(42.0462728769578,3.19873470559984,0.393184072532111));
#77165=CARTESIAN_POINT('Ctrl Pts',(42.0474833073904,3.1962983953354,0.412521481607143));
#77166=CARTESIAN_POINT('Ctrl Pts',(42.0639891261544,3.16084995727654,0.674684441067923));
#77167=CARTESIAN_POINT('Ctrl Pts',(42.0802000346239,3.10042847582344,0.912944539942265));
#77168=CARTESIAN_POINT('Ctrl Pts',(42.1072065135864,2.95879320926322,1.28670195239714));
#77169=CARTESIAN_POINT('Ctrl Pts',(42.1177387300236,2.89361241487982,1.42725938533381));
#77170=CARTESIAN_POINT('Ctrl Pts',(42.1318322435664,2.79039191269221,1.6134470581878));
#77171=CARTESIAN_POINT('Ctrl Pts',(42.1356370463925,2.76082646241958,1.66353134312558));
#77172=CARTESIAN_POINT('Ctrl Pts',(42.1413968535095,2.71318252853803,1.73946829539321));
#77173=CARTESIAN_POINT('Ctrl Pts',(42.1433999175532,2.69605396852741,1.76589992967303));
#77174=CARTESIAN_POINT('Ctrl Pts',(42.1458697087813,2.6741928749655,1.79857475317515));
#77175=CARTESIAN_POINT('Ctrl Pts',(42.1463593146701,2.66982212924108,1.80505636380382));
#77176=CARTESIAN_POINT('Ctrl Pts',(42.1471322803188,2.66286220585679,1.8152970190725));
#77177=CARTESIAN_POINT('Ctrl Pts',(42.1474166757966,2.66028858779679,1.81906652574608));
#77178=CARTESIAN_POINT('Ctrl Pts',(42.1479513333705,2.65542577391065,1.82615656165483));
#77179=CARTESIAN_POINT('Ctrl Pts',(42.1482017085895,2.65313837983643,1.82947822235146));
#77180=CARTESIAN_POINT('Ctrl Pts',(42.1487738901179,2.64788776658259,1.83707239168229));
#77181=CARTESIAN_POINT('Ctrl Pts',(42.1490954117769,2.64492044502432,1.84134202067219));
#77182=CARTESIAN_POINT('Ctrl Pts',(42.150084908614,2.63573676987695,1.85448825239833));
#77183=CARTESIAN_POINT('Ctrl Pts',(42.1507505615988,2.62948588847686,1.86334080846466));
#77184=CARTESIAN_POINT('Ctrl Pts',(42.1561584858292,2.57811911551218,1.93531365995502));
#77185=CARTESIAN_POINT('Ctrl Pts',(42.1607554418366,2.53077780660235,1.99682323705733));
#77186=CARTESIAN_POINT('Ctrl Pts',(42.1826618000868,2.29004689214005,2.28726594393112));
#77187=CARTESIAN_POINT('Ctrl Pts',(42.1987330626371,2.06759082090384,2.49018049204545));
#77188=CARTESIAN_POINT('Ctrl Pts',(42.2167267425001,1.81004140527699,2.66646240289804));
#77189=CARTESIAN_POINT('Ctrl Pts',(42.2174439808744,1.79975849288206,2.67341372982728));
#77190=CARTESIAN_POINT('Ctrl Pts',(42.2181629331785,1.7894362082953,2.68030513541681));
#77191=CARTESIAN_POINT('Origin',(-1.72497344927317,0.,0.));
#77192=CARTESIAN_POINT('',(43.716926315029,1.78943621037803,2.68030513402633));
#77193=CARTESIAN_POINT('',(43.4684957936438,1.78943612473158,2.68030519120596));
#77194=CARTESIAN_POINT('',(-1.72497344927317,1.78943621037804,2.68030513402633));
#77195=CARTESIAN_POINT('',(42.8965734492311,-3.22274897654346,-0.00256840185549188));
#77196=CARTESIAN_POINT('Ctrl Pts',(42.8965734492731,-3.22274897654292,-0.00256840253464825));
#77197=CARTESIAN_POINT('Ctrl Pts',(42.9070119662925,-3.22261461734424,-0.171158008007782));
#77198=CARTESIAN_POINT('Ctrl Pts',(42.9174504833119,-3.20924843949099,-0.339234248199928));
#77199=CARTESIAN_POINT('Ctrl Pts',(42.9278890003314,-3.18290631195516,-0.50519795309958));
#77200=CARTESIAN_POINT('Ctrl Pts',(42.9340612484241,-3.16733033060296,-0.603331544212998));
#77201=CARTESIAN_POINT('Ctrl Pts',(42.9402334965167,-3.14718428142756,-0.700916841221411));
#77202=CARTESIAN_POINT('Ctrl Pts',(42.9464057446094,-3.12251810559492,-0.797494979753408));
#77203=CARTESIAN_POINT('Ctrl Pts',(42.9525696332619,-3.09788533662103,-0.893942316808363));
#77204=CARTESIAN_POINT('Ctrl Pts',(42.9587335219145,-3.06874471543247,-0.989384789434819));
#77205=CARTESIAN_POINT('Ctrl Pts',(42.964897410567,-3.03519763550417,-1.08337107028473));
#77206=CARTESIAN_POINT('Ctrl Pts',(42.9710547722254,-3.00168607886396,-1.17725782826295));
#77207=CARTESIAN_POINT('Ctrl Pts',(42.9772121338839,-2.96377748522139,-1.26969105321386));
#77208=CARTESIAN_POINT('Ctrl Pts',(42.9833694955423,-2.92162350864595,-1.36023293454736));
#77209=CARTESIAN_POINT('Ctrl Pts',(42.9895223596885,-2.87950032253498,-1.45070868151334));
#77210=CARTESIAN_POINT('Ctrl Pts',(42.9956752238347,-2.83313810149224,-1.53929543890168));
#77211=CARTESIAN_POINT('Ctrl Pts',(43.0018280879809,-2.78273688404737,-1.62557466659096));
#77212=CARTESIAN_POINT('Ctrl Pts',(43.0079786211174,-2.73235476108069,-1.71182120743428));
#77213=CARTESIAN_POINT('Ctrl Pts',(43.0141291542538,-2.67793690101353,-1.79576158097013));
#77214=CARTESIAN_POINT('Ctrl Pts',(43.0202796873903,-2.61972920577409,-1.87700198479231));
#77215=CARTESIAN_POINT('Ctrl Pts',(43.0264295356054,-2.56152799252431,-1.95823334171003));
#77216=CARTESIAN_POINT('Ctrl Pts',(43.0325793838205,-2.49953803615927,-2.03676497358742));
#77217=CARTESIAN_POINT('Ctrl Pts',(43.0387292320356,-2.43404788848853,-2.11223304562837));
#77218=CARTESIAN_POINT('Ctrl Pts',(43.0448800404146,-2.36854751596743,-2.18771290035377));
#77219=CARTESIAN_POINT('Ctrl Pts',(43.0510308487937,-2.29954615141603,-2.26012791709842));
#77220=CARTESIAN_POINT('Ctrl Pts',(43.0571816571727,-2.22737117436342,-2.32914903218212));
#77221=CARTESIAN_POINT('Ctrl Pts',(43.0633390435388,-2.15511900972256,-2.3982439619538));
#77222=CARTESIAN_POINT('Ctrl Pts',(43.0694964299049,-2.07968676961233,-2.46393744130707));
#77223=CARTESIAN_POINT('Ctrl Pts',(43.075653816271,-2.00143699861166,-2.52593893494842));
#77224=CARTESIAN_POINT('Ctrl Pts',(43.0818146390078,-1.92314355725967,-2.58797503095313));
#77225=CARTESIAN_POINT('Ctrl Pts',(43.0879754617447,-1.84202980618773,-2.64631478423596));
#77226=CARTESIAN_POINT('Ctrl Pts',(43.0941362844816,-1.75848779783016,-2.70071068931539));
#77227=CARTESIAN_POINT('Ctrl Pts',(43.1003074073982,-1.67480611694209,-2.75519753802739));
#77228=CARTESIAN_POINT('Ctrl Pts',(43.1064785303148,-1.58868844433504,-2.80572714798561));
#77229=CARTESIAN_POINT('Ctrl Pts',(43.1126496532314,-1.50055209231866,-2.85209764572289));
#77230=CARTESIAN_POINT('Ctrl Pts',(43.1173451751779,-1.43349036290944,-2.88738031514006));
#77231=CARTESIAN_POINT('Ctrl Pts',(43.1220406971245,-1.36526044633556,-2.92025602217248));
#77232=CARTESIAN_POINT('Ctrl Pts',(43.1267362190711,-1.29605301174589,-2.95065486854095));
#77233=CARTESIAN_POINT('Ctrl Pts',(43.1329084671636,-1.20508006752428,-2.99061405170496));
#77234=CARTESIAN_POINT('Ctrl Pts',(43.1390807152562,-1.11209727072552,-3.02643238484143));
#77235=CARTESIAN_POINT('Ctrl Pts',(43.1452529633488,-1.01751762584899,-3.0579037662403));
#77236=CARTESIAN_POINT('Ctrl Pts',(43.1514168520012,-0.923066075771607,
-3.08933252408858));
#77237=CARTESIAN_POINT('Ctrl Pts',(43.1575807406536,-0.82702238475968,-3.11642589598497));
#77238=CARTESIAN_POINT('Ctrl Pts',(43.163744629306,-0.729821037891639,-3.1390251377061));
#77239=CARTESIAN_POINT('Ctrl Pts',(43.1699019909644,-0.632722618355907,
-3.16160044889809));
#77240=CARTESIAN_POINT('Ctrl Pts',(43.1760593526227,-0.534469400830379,
-3.1796909931772));
#77241=CARTESIAN_POINT('Ctrl Pts',(43.1822167142811,-0.435511676394324,
-3.19318761462965));
#77242=CARTESIAN_POINT('Ctrl Pts',(43.1883695784272,-0.33662623349731,-3.20667437776558));
#77243=CARTESIAN_POINT('Ctrl Pts',(43.1945224425733,-0.237037735879731,
-3.21557383092338));
#77244=CARTESIAN_POINT('Ctrl Pts',(43.2006753067194,-0.137206426103824,
-3.21982793936816));
#77245=CARTESIAN_POINT('Ctrl Pts',(43.2068258398557,-0.0374129373740154,
-3.2240804361459));
#77246=CARTESIAN_POINT('Ctrl Pts',(43.212976372992,0.0626227472322829,-3.22369106662332));
#77247=CARTESIAN_POINT('Ctrl Pts',(43.2191269061283,0.16243639593016,-3.21865375270115));
#77248=CARTESIAN_POINT('Ctrl Pts',(43.2252767543433,0.262238929413218,-3.21361699973259));
#77249=CARTESIAN_POINT('Ctrl Pts',(43.2314266025583,0.361819042322848,-3.20393335330992));
#77250=CARTESIAN_POINT('Ctrl Pts',(43.2375764507733,0.460714650667325,-3.18964881658788));
#77251=CARTESIAN_POINT('Ctrl Pts',(43.2437272591523,0.559625699392309,-3.17536204964869));
#77252=CARTESIAN_POINT('Ctrl Pts',(43.2498780675312,0.657851601325742,-3.15647302772775));
#77253=CARTESIAN_POINT('Ctrl Pts',(43.2560288759101,0.754938527703059,-3.13307921730197));
#77254=CARTESIAN_POINT('Ctrl Pts',(43.2621862622761,0.85212928377311,-3.10966038834652));
#77255=CARTESIAN_POINT('Ctrl Pts',(43.2683436486421,0.948178208798035,-3.08172725248936));
#77256=CARTESIAN_POINT('Ctrl Pts',(43.2745010350081,1.04264487033308,-3.04942769005401));
#77257=CARTESIAN_POINT('Ctrl Pts',(43.2806618577448,1.13716425269073,-3.01711010158202));
#77258=CARTESIAN_POINT('Ctrl Pts',(43.2868226804816,1.23009920894446,-2.98042139307577));
#77259=CARTESIAN_POINT('Ctrl Pts',(43.2929835032183,1.32102954851137,-2.93955753378971));
#77260=CARTESIAN_POINT('Ctrl Pts',(43.2991546261348,1.41211191304002,-2.89862535487926));
#77261=CARTESIAN_POINT('Ctrl Pts',(43.3053257490513,1.50118257871883,-2.85350427850703));
#77262=CARTESIAN_POINT('Ctrl Pts',(43.3114968719678,1.58784608274892,-2.80443619645712));
#77263=CARTESIAN_POINT('Ctrl Pts',(43.3161923939154,1.65378714254311,-2.76710097249347));
#77264=CARTESIAN_POINT('Ctrl Pts',(43.3208879158631,1.71833509488387,-2.72748158986566));
#77265=CARTESIAN_POINT('Ctrl Pts',(43.3255834378107,1.78132804395446,-2.68570064644617));
#77266=CARTESIAN_POINT('Ctrl Pts',(43.3317556859043,1.86413206747814,-2.63077973429977));
#77267=CARTESIAN_POINT('Ctrl Pts',(43.3379279339978,1.94453951891321,-2.57192911623941));
#77268=CARTESIAN_POINT('Ctrl Pts',(43.3441001820914,2.02215370790222,-2.50938477402676));
#77269=CARTESIAN_POINT('Ctrl Pts',(43.3502640707448,2.09966277941113,-2.44692513931068));
#77270=CARTESIAN_POINT('Ctrl Pts',(43.3564279593983,2.17438577251549,-2.38078199387189));
#77271=CARTESIAN_POINT('Ctrl Pts',(43.3625918480517,2.24595421962877,-2.31123499580457));
#77272=CARTESIAN_POINT('Ctrl Pts',(43.3687492097111,2.31744688230509,-2.24176164164463));
#77273=CARTESIAN_POINT('Ctrl Pts',(43.3749065713704,2.38579133017254,-2.16889190173063));
#77274=CARTESIAN_POINT('Ctrl Pts',(43.3810639330298,2.45065226330621,-2.09294554321228));
#77275=CARTESIAN_POINT('Ctrl Pts',(43.3872167971769,2.5154658201679,-2.01705465807619));
#77276=CARTESIAN_POINT('Ctrl Pts',(43.393369661324,2.57680063986894,-1.93809195156581));
#77277=CARTESIAN_POINT('Ctrl Pts',(43.3995225254711,2.63435904520707,-1.8564132038519));
#77278=CARTESIAN_POINT('Ctrl Pts',(43.4056730586084,2.69189564456962,-1.77476540009426));
#77279=CARTESIAN_POINT('Ctrl Pts',(43.4118235917457,2.74565842241112,-1.69040395436823));
#77280=CARTESIAN_POINT('Ctrl Pts',(43.4179741248831,2.79539125090078,-1.60371609609911));
#77281=CARTESIAN_POINT('Ctrl Pts',(43.4241239730991,2.84511854115916,-1.51703789136114));
#77282=CARTESIAN_POINT('Ctrl Pts',(43.4302738213151,2.89081655813809,-1.42803416592069));
#77283=CARTESIAN_POINT('Ctrl Pts',(43.4364236695311,2.9322741465557,-1.3371185033276));
#77284=CARTESIAN_POINT('Ctrl Pts',(43.442574477911,2.97373820766652,-1.24618864624771));
#77285=CARTESIAN_POINT('Ctrl Pts',(43.448725286291,3.01096034497466,-1.15334665436403));
#77286=CARTESIAN_POINT('Ctrl Pts',(43.4548760946709,3.04377715828944,-1.05902699360096));
#77287=CARTESIAN_POINT('Ctrl Pts',(43.4610334810379,3.07662906757199,-0.964606462599733));
#77288=CARTESIAN_POINT('Ctrl Pts',(43.4671908674048,3.10506610190875,-0.86870551808728));
#77289=CARTESIAN_POINT('Ctrl Pts',(43.4733482537718,3.1289745132135,-0.771774616167423));
#77290=CARTESIAN_POINT('Ctrl Pts',(43.4795090765095,3.15289626754413,-0.674789618159069));
#77291=CARTESIAN_POINT('Ctrl Pts',(43.4856698992473,3.1722842813181,-0.57677394415378));
#77292=CARTESIAN_POINT('Ctrl Pts',(43.491830721985,3.18707620426854,-0.478187024798082));
#77293=CARTESIAN_POINT('Ctrl Pts',(43.4980018449024,3.20189285759529,-0.379435279569272));
#77294=CARTESIAN_POINT('Ctrl Pts',(43.5041729678199,3.21209802686905,-0.280110813597029));
#77295=CARTESIAN_POINT('Ctrl Pts',(43.5103440907373,3.21768136283026,-0.180677087077551));
#77296=CARTESIAN_POINT('Ctrl Pts',(43.515039612675,3.22192964581572,-0.105019342050436));
#77297=CARTESIAN_POINT('Ctrl Pts',(43.5197351346127,3.22350320671854,-0.0292984234542198));
#77298=CARTESIAN_POINT('Ctrl Pts',(43.5244306565504,3.22241763723597,0.046283190583255));
#77299=CARTESIAN_POINT('Ctrl Pts',(43.5306030380365,3.22099062889376,0.145637120000158));
#77300=CARTESIAN_POINT('Ctrl Pts',(43.5367754195226,3.21496186675561,0.24509986855709));
#77301=CARTESIAN_POINT('Ctrl Pts',(43.5429478010087,3.20431536576978,0.34421010907832));
#77302=CARTESIAN_POINT('Ctrl Pts',(43.5491117885684,3.19368334314145,0.4431855679002));
#77303=CARTESIAN_POINT('Ctrl Pts',(43.555275776128,3.17844610962596,0.541809043401481));
#77304=CARTESIAN_POINT('Ctrl Pts',(43.5614397636877,3.15863968518723,0.639619341218158));
#77305=CARTESIAN_POINT('Ctrl Pts',(43.5679183699936,3.13782231250054,0.742422016609864));
#77306=CARTESIAN_POINT('Ctrl Pts',(43.5743969762995,3.11195693817601,0.844325818887086));
#77307=CARTESIAN_POINT('Ctrl Pts',(43.5808755826054,3.08114727120735,0.944801066696865));
#77308=CARTESIAN_POINT('Ctrl Pts',(43.5870281944349,3.05188790391388,1.04022053950578));
#77309=CARTESIAN_POINT('Ctrl Pts',(43.5931808062643,3.01816985646978,1.13435124988518));
#77310=CARTESIAN_POINT('Ctrl Pts',(43.5993334180938,2.98013405524829,1.2267512279388));
#77311=CARTESIAN_POINT('Ctrl Pts',(43.6054837360839,2.94211243467417,1.31911675709262));
#77312=CARTESIAN_POINT('Ctrl Pts',(43.611634054074,2.89977642460012,1.40975243503371));
#77313=CARTESIAN_POINT('Ctrl Pts',(43.6177843720641,2.85331575527376,1.49823454879619));
#77314=CARTESIAN_POINT('Ctrl Pts',(43.6239340422079,2.80685997990089,1.58670734225926));
#77315=CARTESIAN_POINT('Ctrl Pts',(43.6300837123518,2.75628061150776,1.67302663827981));
#77316=CARTESIAN_POINT('Ctrl Pts',(43.6362333824957,2.70181371112788,1.75679259813484));
#77317=CARTESIAN_POINT('Ctrl Pts',(43.6423840497997,2.64733797901842,1.84057214051983));
#77318=CARTESIAN_POINT('Ctrl Pts',(43.6485347171037,2.58897370006314,1.92179716055282));
#77319=CARTESIAN_POINT('Ctrl Pts',(43.6546853844077,2.52700013232355,2.00009697108334));
#77320=CARTESIAN_POINT('Ctrl Pts',(43.6608420666493,2.46496595861666,2.07847335354493));
#77321=CARTESIAN_POINT('Ctrl Pts',(43.6669987488909,2.39931572077314,2.15391847552512));
#77322=CARTESIAN_POINT('Ctrl Pts',(43.6731554311325,2.33036866048638,2.2260951167286));
#77323=CARTESIAN_POINT('Ctrl Pts',(43.6793156067755,2.26138247851965,2.29831271212862));
#77324=CARTESIAN_POINT('Ctrl Pts',(43.6854757824184,2.18909606308223,2.36725783414701));
#77325=CARTESIAN_POINT('Ctrl Pts',(43.6916359580614,2.11386373381855,2.43263184171931));
#77326=CARTESIAN_POINT('Ctrl Pts',(43.6978049516411,2.0385237138061,2.49809942842036));
#77327=CARTESIAN_POINT('Ctrl Pts',(43.7039739452209,1.96022970289234,2.55998542821244));
#77328=CARTESIAN_POINT('Ctrl Pts',(43.7101429388007,1.87936695546459,2.61803311843219));
#77329=CARTESIAN_POINT('Ctrl Pts',(43.7124040642101,1.84972827769303,2.63930937777946));
#77330=CARTESIAN_POINT('Ctrl Pts',(43.7146651896196,1.81974476091569,2.66007041629675));
#77331=CARTESIAN_POINT('Ctrl Pts',(43.716926315029,1.78943621037803,2.68030513402633));
#77332=CARTESIAN_POINT('Ctrl Pts',(42.4668644404635,1.78943621037806,2.68030513402631));
#77333=CARTESIAN_POINT('Ctrl Pts',(42.4730228196522,1.7063097483104,2.73580236058314));
#77334=CARTESIAN_POINT('Ctrl Pts',(42.4791811988409,1.62065192585895,2.78739362741565));
#77335=CARTESIAN_POINT('Ctrl Pts',(42.4853395780296,1.53287140170373,2.83485851998629));
#77336=CARTESIAN_POINT('Ctrl Pts',(42.4915018923073,1.44503478743852,2.88235374173382));
#77337=CARTESIAN_POINT('Ctrl Pts',(42.4976642065849,1.35507316197229,2.92571715166353));
#77338=CARTESIAN_POINT('Ctrl Pts',(42.5038265208625,1.26341635432497,2.96477599122163));
#77339=CARTESIAN_POINT('Ctrl Pts',(42.5099985241704,1.17161543432828,3.00389624314262));
#77340=CARTESIAN_POINT('Ctrl Pts',(42.5161705274784,1.07811441805955,3.03869826355687));
#77341=CARTESIAN_POINT('Ctrl Pts',(42.5223425307863,0.983359410082434,3.069058786192));
#77342=CARTESIAN_POINT('Ctrl Pts',(42.5249598748083,0.943176921300858,3.08193368733162));
#77343=CARTESIAN_POINT('Ctrl Pts',(42.5275772188302,0.902769061359369,3.09401048815375));
#77344=CARTESIAN_POINT('Ctrl Pts',(42.5301945628522,0.862170336031154,3.10528257557471));
#77345=CARTESIAN_POINT('Ctrl Pts',(42.5363668109449,0.766429996637244,3.13186453022073));
#77346=CARTESIAN_POINT('Ctrl Pts',(42.5425390590377,0.669290652049423,3.15406140438831));
#77347=CARTESIAN_POINT('Ctrl Pts',(42.5487113071304,0.571190470249088,3.17172807932783));
#77348=CARTESIAN_POINT('Ctrl Pts',(42.554875195783,0.473223151318917,3.18937082724607));
#77349=CARTESIAN_POINT('Ctrl Pts',(42.5610390844356,0.374298005424443,3.20249549464088));
#77350=CARTESIAN_POINT('Ctrl Pts',(42.5672029730882,0.274867710449411,3.2110068988173));
#77351=CARTESIAN_POINT('Ctrl Pts',(42.5733603347467,0.175542703058871,3.21950929019549));
#77352=CARTESIAN_POINT('Ctrl Pts',(42.5795176964052,0.0757140404387358,
3.22340809340008));
#77353=CARTESIAN_POINT('Ctrl Pts',(42.5856750580637,-0.0241570242698424,
3.22265946086124));
#77354=CARTESIAN_POINT('Ctrl Pts',(42.59182792221,-0.123955140309737,3.22191137514491));
#77355=CARTESIAN_POINT('Ctrl Pts',(42.5979807863562,-0.223795163807456,
3.21652260601525));
#77356=CARTESIAN_POINT('Ctrl Pts',(42.6041336505025,-0.323213279610985,
3.20650132362098));
#77357=CARTESIAN_POINT('Ctrl Pts',(42.610284183639,-0.422593730906763,3.19648383778497));
#77358=CARTESIAN_POINT('Ctrl Pts',(42.6164347167755,-0.521552160403222,
3.18183736942622));
#77359=CARTESIAN_POINT('Ctrl Pts',(42.622585249912,-0.619628211402932,3.1626220833564));
#77360=CARTESIAN_POINT('Ctrl Pts',(42.6287350981272,-0.717693340686126,
3.14340893709447));
#77361=CARTESIAN_POINT('Ctrl Pts',(42.6348849463424,-0.81487586055913,3.11962806817058));
#77362=CARTESIAN_POINT('Ctrl Pts',(42.6410347945575,-0.910724964878155,
3.09139088451261));
#77363=CARTESIAN_POINT('Ctrl Pts',(42.6471856029366,-1.00658903393289,3.06314929223765));
#77364=CARTESIAN_POINT('Ctrl Pts',(42.6533364113157,-1.10111885721787,3.03045012604058));
#77365=CARTESIAN_POINT('Ctrl Pts',(42.6594872196948,-1.19387913610439,2.99345455467001));
#77366=CARTESIAN_POINT('Ctrl Pts',(42.665644606061,-1.28673861754694,2.95641941835542));
#77367=CARTESIAN_POINT('Ctrl Pts',(42.6718019924271,-1.37782437132591,2.91507886276786));
#77368=CARTESIAN_POINT('Ctrl Pts',(42.6779593787933,-1.46672154529698,2.8696420458067));
#77369=CARTESIAN_POINT('Ctrl Pts',(42.6841202015302,-1.55566833181994,2.82417987104912));
#77370=CARTESIAN_POINT('Ctrl Pts',(42.6902810242672,-1.64242372891095,2.77461709770201));
#77371=CARTESIAN_POINT('Ctrl Pts',(42.6964418470041,-1.72659977509332,2.72120759574636));
#77372=CARTESIAN_POINT('Ctrl Pts',(42.7026129699207,-1.81091655384361,2.66770879930966));
#77373=CARTESIAN_POINT('Ctrl Pts',(42.7087840928374,-1.89264501213276,2.61035067762098));
#77374=CARTESIAN_POINT('Ctrl Pts',(42.714955215754,-1.97142821041354,2.54942902895642));
#77375=CARTESIAN_POINT('Ctrl Pts',(42.7196507377,-2.03137325469363,2.5030745903641));
#77376=CARTESIAN_POINT('Ctrl Pts',(42.7243462596459,-2.08961379107395,2.45465792433793));
#77377=CARTESIAN_POINT('Ctrl Pts',(42.7290417815918,-2.14600705485164,2.4043234564066));
#77378=CARTESIAN_POINT('Ctrl Pts',(42.7351222412986,-2.21903343447167,2.33914290616189));
#77379=CARTESIAN_POINT('Ctrl Pts',(42.7412027010054,-2.28923440967352,2.27050086199092));
#77380=CARTESIAN_POINT('Ctrl Pts',(42.7472831607122,-2.35625617205213,2.19867560457796));
#77381=CARTESIAN_POINT('Ctrl Pts',(42.7535035894005,-2.42482074011787,2.12519696755092));
#77382=CARTESIAN_POINT('Ctrl Pts',(42.7597240180888,-2.49005751577951,2.04838699778255));
#77383=CARTESIAN_POINT('Ctrl Pts',(42.7659444467771,-2.55162278540211,1.96858800248217));
#77384=CARTESIAN_POINT('Ctrl Pts',(42.7720094906818,-2.61165016968376,1.89078236651974));
#77385=CARTESIAN_POINT('Ctrl Pts',(42.7780745345866,-2.66818700987442,1.81013564901337));
#77386=CARTESIAN_POINT('Ctrl Pts',(42.7841395784913,-2.72095245481611,1.72700182429845));
#77387=CARTESIAN_POINT('Ctrl Pts',(42.7902008683294,-2.77368523964853,1.64391945674082));
#77388=CARTESIAN_POINT('Ctrl Pts',(42.7962621581675,-2.82265102483982,1.55835341620575));
#77389=CARTESIAN_POINT('Ctrl Pts',(42.8023234480056,-2.86761118870067,1.47068814945205));
#77390=CARTESIAN_POINT('Ctrl Pts',(42.8083827193884,-2.91255638048725,1.38305207589457));
#77391=CARTESIAN_POINT('Ctrl Pts',(42.8144419907712,-2.95349839674967,1.29331856370545));
#77392=CARTESIAN_POINT('Ctrl Pts',(42.8205012621539,-2.99024425283826,1.2018971964639));
#77393=CARTESIAN_POINT('Ctrl Pts',(42.826840611077,-3.02868861165756,1.10625006179073));
#77394=CARTESIAN_POINT('Ctrl Pts',(42.8331799600001,-3.0625393141137,1.00875575114826));
#77395=CARTESIAN_POINT('Ctrl Pts',(42.8395193089232,-3.09163202552679,0.909906028794799));
#77396=CARTESIAN_POINT('Ctrl Pts',(42.8455824738989,-3.11945726610376,0.815362853825724));
#77397=CARTESIAN_POINT('Ctrl Pts',(42.8516456388745,-3.14293034275207,0.719580363387587));
#77398=CARTESIAN_POINT('Ctrl Pts',(42.8577088038502,-3.16195921200763,0.623002009707894));
#77399=CARTESIAN_POINT('Ctrl Pts',(42.8637745881198,-3.18099630175592,0.526381934071794));
#77400=CARTESIAN_POINT('Ctrl Pts',(42.8698403723895,-3.19558529637308,0.428965753991759));
#77401=CARTESIAN_POINT('Ctrl Pts',(42.8759061566592,-3.205685835828,0.331203690305177));
#77402=CARTESIAN_POINT('Ctrl Pts',(42.8819788888794,-3.21579794477583,0.233329646708139));
#77403=CARTESIAN_POINT('Ctrl Pts',(42.8880516210995,-3.22141131975012,0.13510937576864));
#77404=CARTESIAN_POINT('Ctrl Pts',(42.8941243533197,-3.22253766425402,0.0369941206709852));
#77405=CARTESIAN_POINT('Ctrl Pts',(42.8949407186235,-3.22268908021306,0.0238043591057623));
#77406=CARTESIAN_POINT('Ctrl Pts',(42.8957570839273,-3.22275948437315,0.0106164887023605));
#77407=CARTESIAN_POINT('Ctrl Pts',(42.8965734492311,-3.22274897654346,-0.00256840185549149));
#77408=CARTESIAN_POINT('Ctrl Pts',(42.2181629331785,1.7894362082953,2.68030513541681));
#77409=CARTESIAN_POINT('Ctrl Pts',(42.2217196605947,1.73837085614481,2.71439759336871));
#77410=CARTESIAN_POINT('Ctrl Pts',(42.2253186739974,1.68634193990611,2.7470235475656));
#77411=CARTESIAN_POINT('Ctrl Pts',(42.2316293281462,1.59486245394465,2.80080902053283));
#77412=CARTESIAN_POINT('Ctrl Pts',(42.2343155408901,1.55584615997304,2.82266892187229));
#77413=CARTESIAN_POINT('Ctrl Pts',(42.2378150347013,1.50499593401331,2.84978446799692));
#77414=CARTESIAN_POINT('Ctrl Pts',(42.2386015006529,1.49356652458364,2.85579118712937));
#77415=CARTESIAN_POINT('Ctrl Pts',(42.239876084008,1.47504297060026,2.86538461347792));
#77416=CARTESIAN_POINT('Ctrl Pts',(42.2403626868135,1.46797103474877,2.8690140793695));
#77417=CARTESIAN_POINT('Ctrl Pts',(42.2412940102413,1.45443607947318,2.87589735746737));
#77418=CARTESIAN_POINT('Ctrl Pts',(42.2417385698248,1.4479753795481,2.87915564338288));
#77419=CARTESIAN_POINT('Ctrl Pts',(42.2427583876119,1.4331551821444,2.88656732437899));
#77420=CARTESIAN_POINT('Ctrl Pts',(42.2433341504346,1.42478853231344,2.89070619910277));
#77421=CARTESIAN_POINT('Ctrl Pts',(42.2451136447508,1.39893238610334,2.90335738122805));
#77422=CARTESIAN_POINT('Ctrl Pts',(42.2463216153317,1.38138396410044,2.91174762316685));
#77423=CARTESIAN_POINT('Ctrl Pts',(42.2629444337684,1.13998320979188,3.02449261211886));
#77424=CARTESIAN_POINT('Ctrl Pts',(42.2792904611879,0.904980560503523,3.1029146491541));
#77425=CARTESIAN_POINT('Ctrl Pts',(42.3063450856634,0.513217508158918,3.18532149947807));
#77426=CARTESIAN_POINT('Ctrl Pts',(42.3167876425959,0.360982577635473,3.2061440865308));
#77427=CARTESIAN_POINT('Ctrl Pts',(42.3307667904361,0.150215664862116,3.2197650826473));
#77428=CARTESIAN_POINT('Ctrl Pts',(42.3345445296417,0.0924984469676575,
3.22193991328354));
#77429=CARTESIAN_POINT('Ctrl Pts',(42.3402680615161,0.00341235853275508,
3.22290057495599));
#77430=CARTESIAN_POINT('Ctrl Pts',(42.3422612323528,-0.027930546787336,
3.22278137969128));
#77431=CARTESIAN_POINT('Ctrl Pts',(42.3447205573488,-0.067071557395471,
3.22206143381895));
#77432=CARTESIAN_POINT('Ctrl Pts',(42.3452093619568,-0.0748745683871715,
3.22188955104423));
#77433=CARTESIAN_POINT('Ctrl Pts',(42.3459813525845,-0.0872368952137637,
3.2215723014069));
#77434=CARTESIAN_POINT('Ctrl Pts',(42.3462655699483,-0.0917965970982968,
3.2214456001082));
#77435=CARTESIAN_POINT('Ctrl Pts',(42.3468000807563,-0.100387869615858,
3.22118861730599));
#77436=CARTESIAN_POINT('Ctrl Pts',(42.3470504865306,-0.104419417348497,
3.22106044930886));
#77437=CARTESIAN_POINT('Ctrl Pts',(42.3476229871091,-0.113651970450272,
3.22074958280677));
#77438=CARTESIAN_POINT('Ctrl Pts',(42.3479447960978,-0.118852771066763,
3.22056185552321));
#77439=CARTESIAN_POINT('Ctrl Pts',(42.3489360504688,-0.134905837682814,
3.21994346741317));
#77440=CARTESIAN_POINT('Ctrl Pts',(42.3496031616894,-0.145756536208583,
3.21947054007426));
#77441=CARTESIAN_POINT('Ctrl Pts',(42.3550547446546,-0.234790786360319,
3.21513893386138));
#77442=CARTESIAN_POINT('Ctrl Pts',(42.359691272036,-0.312819599756684,3.2084873756921));
#77443=CARTESIAN_POINT('Ctrl Pts',(42.3756697738247,-0.586054586034389,
3.17513070920855));
#77444=CARTESIAN_POINT('Ctrl Pts',(42.3865082030507,-0.778987479177579,
3.1333855714471));
#77445=CARTESIAN_POINT('Ctrl Pts',(42.4089683434236,-1.16096633016335,3.01324690163493));
#77446=CARTESIAN_POINT('Ctrl Pts',(42.420564748736,-1.34877744233324,2.93398744304411));
#77447=CARTESIAN_POINT('Ctrl Pts',(42.4342155460878,-1.54829430158038,2.82655997206818));
#77448=CARTESIAN_POINT('Ctrl Pts',(42.4356216765461,-1.56861509404701,2.81533357940513));
#77449=CARTESIAN_POINT('Ctrl Pts',(42.4376466466783,-1.59753977939494,2.79894352188412));
#77450=CARTESIAN_POINT('Ctrl Pts',(42.4382590881115,-1.60624391988547,2.79395752503463));
#77451=CARTESIAN_POINT('Ctrl Pts',(42.4393224896502,-1.62128032860834,2.785250724596));
#77452=CARTESIAN_POINT('Ctrl Pts',(42.4397727649262,-1.62762345191738,2.78154874128539));
#77453=CARTESIAN_POINT('Ctrl Pts',(42.4406390223109,-1.63978076027161,2.77439765022244));
#77454=CARTESIAN_POINT('Ctrl Pts',(42.4410548816434,-1.6455968617693,2.77095186366352));
#77455=CARTESIAN_POINT('Ctrl Pts',(42.4420351073943,-1.65925830404118,2.76279987344018));
#77456=CARTESIAN_POINT('Ctrl Pts',(42.4426000262205,-1.66709450135167,2.75807853060882));
#77457=CARTESIAN_POINT('Ctrl Pts',(42.4442717860968,-1.69017392681571,2.74403878397038));
#77458=CARTESIAN_POINT('Ctrl Pts',(42.4453820551361,-1.70535970015946,2.73462703547898));
#77459=CARTESIAN_POINT('Ctrl Pts',(42.4579106220937,-1.87511046551275,2.62745608363986));
#77460=CARTESIAN_POINT('Ctrl Pts',(42.4698207573752,-2.02113623095133,2.51685371930569));
#77461=CARTESIAN_POINT('Ctrl Pts',(42.4889853753387,-2.23408158038254,2.32503035665892));
#77462=CARTESIAN_POINT('Ctrl Pts',(42.4960085769168,-2.30778320620272,2.25189298094657));
#77463=CARTESIAN_POINT('Ctrl Pts',(42.5159684578198,-2.50683552729827,2.03431145885023));
#77464=CARTESIAN_POINT('Ctrl Pts',(42.5288838874211,-2.62306039654953,1.88207829401876));
#77465=CARTESIAN_POINT('Ctrl Pts',(42.5419386110903,-2.73306808475678,1.70782854072295));
#77466=CARTESIAN_POINT('Ctrl Pts',(42.5428771848956,-2.74093336154571,1.69517663037139));
#77467=CARTESIAN_POINT('Ctrl Pts',(42.5441808258271,-2.7518006091536,1.67742242694465));
#77468=CARTESIAN_POINT('Ctrl Pts',(42.5445505964582,-2.75487653368268,1.6723659517125));
#77469=CARTESIAN_POINT('Ctrl Pts',(42.5451780624932,-2.76008530663172,1.66374994548331));
#77470=CARTESIAN_POINT('Ctrl Pts',(42.5454362211682,-2.76222523229623,1.66019473186239));
#77471=CARTESIAN_POINT('Ctrl Pts',(42.5459277162155,-2.76629348073228,1.65340621543178));
#77472=CARTESIAN_POINT('Ctrl Pts',(42.5461611332657,-2.76822300702437,1.65017366313347));
#77473=CARTESIAN_POINT('Ctrl Pts',(42.5467101788511,-2.77275552353652,1.64254997686655));
#77474=CARTESIAN_POINT('Ctrl Pts',(42.5470254967309,-2.77535376322781,1.63815600892932));
#77475=CARTESIAN_POINT('Ctrl Pts',(42.547956174419,-2.78300793308283,1.62514131236917));
#77476=CARTESIAN_POINT('Ctrl Pts',(42.5485696487335,-2.78803427190687,1.61650312265316));
#77477=CARTESIAN_POINT('Ctrl Pts',(42.5544040706871,-2.83564307919883,1.53380071315588));
#77478=CARTESIAN_POINT('Ctrl Pts',(42.5594479812322,-2.87530902560953,1.45808682188049));
#77479=CARTESIAN_POINT('Ctrl Pts',(42.5665251897491,-2.92775120725039,1.34749959431129));
#77480=CARTESIAN_POINT('Ctrl Pts',(42.5686415274892,-2.9430054581154,1.31384980308687));
#77481=CARTESIAN_POINT('Ctrl Pts',(42.5807315369125,-3.02737965235529,1.11887904927416));
#77482=CARTESIAN_POINT('Ctrl Pts',(42.5904003789349,-3.08380983833858,0.952385771762098));
#77483=CARTESIAN_POINT('Ctrl Pts',(42.6106707814109,-3.17115166698426,0.603250921046015));
#77484=CARTESIAN_POINT('Ctrl Pts',(42.6212639353053,-3.20046041095039,0.420896165356633));
#77485=CARTESIAN_POINT('Ctrl Pts',(42.6336276446777,-3.21552799154996,0.216604768133396));
#77486=CARTESIAN_POINT('Ctrl Pts',(42.6348710084127,-3.21684084956794,0.196144866243502));
#77487=CARTESIAN_POINT('Ctrl Pts',(42.6367017223952,-3.2184782250612,0.166151807952567));
#77488=CARTESIAN_POINT('Ctrl Pts',(42.6372842637606,-3.21895579505952,0.156627248115719));
#77489=CARTESIAN_POINT('Ctrl Pts',(42.6383128620846,-3.2197226315505,0.139844560690493));
#77490=CARTESIAN_POINT('Ctrl Pts',(42.6387583583515,-3.22002964847593,0.132587280073419));
#77491=CARTESIAN_POINT('Ctrl Pts',(42.6396281597261,-3.22058021168594,0.118440638948911));
#77492=CARTESIAN_POINT('Ctrl Pts',(42.6400523858353,-3.22082619323022,0.111551408241236));
#77493=CARTESIAN_POINT('Ctrl Pts',(42.6410727838833,-3.22136379854938,0.0950061273349007));
#77494=CARTESIAN_POINT('Ctrl Pts',(42.6416696220326,-3.22163411133951,0.085349494596543));
#77495=CARTESIAN_POINT('Ctrl Pts',(42.6438489790326,-3.22246069900972,0.0501653940528284));
#77496=CARTESIAN_POINT('Ctrl Pts',(42.6454396267255,-3.22275699725731,0.0246333012112815));
#77497=CARTESIAN_POINT('Ctrl Pts',(42.6545039466654,-3.22271665035957,-0.119996792985065));
#77498=CARTESIAN_POINT('Ctrl Pts',(42.6621734231361,-3.21608164533105,-0.238987172216434));
#77499=CARTESIAN_POINT('Ctrl Pts',(42.6809218207046,-3.18449910205122,-0.522075959496533));
#77500=CARTESIAN_POINT('Ctrl Pts',(42.6921395575668,-3.15343606146854,-0.685149989314532));
#77501=CARTESIAN_POINT('Ctrl Pts',(42.716099656827,-3.06058909433109,-1.02682877364644));
#77502=CARTESIAN_POINT('Ctrl Pts',(42.7287972074266,-2.99536474041529,-1.2039064197207));
#77503=CARTESIAN_POINT('Ctrl Pts',(42.741434267157,-2.9100165621998,-1.38494036336811));
#77504=CARTESIAN_POINT('Ctrl Pts',(42.7421744035054,-2.90493707545927,-1.39556325549378));
#77505=CARTESIAN_POINT('Ctrl Pts',(42.7432438988451,-2.89747767967071,-1.41094612664779));
#77506=CARTESIAN_POINT('Ctrl Pts',(42.7435760556443,-2.89514409452615,-1.4157282752676));
#77507=CARTESIAN_POINT('Ctrl Pts',(42.7441604016862,-2.89100868095609,-1.42414987297785));
#77508=CARTESIAN_POINT('Ctrl Pts',(42.7444128986318,-2.88921180460668,-1.42779172252958));
#77509=CARTESIAN_POINT('Ctrl Pts',(42.744941199931,-2.88543120662733,-1.43541775191868));
#77510=CARTESIAN_POINT('Ctrl Pts',(42.7452169162615,-2.88344611896537,-1.43940121241359));
#77511=CARTESIAN_POINT('Ctrl Pts',(42.7459440381348,-2.87817943924847,-1.44991520235635));
#77512=CARTESIAN_POINT('Ctrl Pts',(42.746394570686,-2.8748838499502,-1.45643874923965));
#77513=CARTESIAN_POINT('Ctrl Pts',(42.7484356644581,-2.85980815460908,-1.48603020650837));
#77514=CARTESIAN_POINT('Ctrl Pts',(42.7500106817074,-2.84777200580747,-1.50896758028767));
#77515=CARTESIAN_POINT('Ctrl Pts',(42.7637103489831,-2.73967162466017,-1.70907379045854));
#77516=CARTESIAN_POINT('Ctrl Pts',(42.7749436684661,-2.62744734433604,-1.87703945943681));
#77517=CARTESIAN_POINT('Ctrl Pts',(42.7997413760648,-2.34745020904844,-2.2213152346494));
#77518=CARTESIAN_POINT('Ctrl Pts',(42.8132833097584,-2.17398290814975,-2.39134771558752));
#77519=CARTESIAN_POINT('Ctrl Pts',(42.8282270159554,-1.97704674604733,-2.54508607217044));
#77520=CARTESIAN_POINT('Ctrl Pts',(42.8286887813643,-1.97095521375683,-2.5498063641481));
#77521=CARTESIAN_POINT('Ctrl Pts',(42.8308362774878,-1.94259868566993,-2.57161733758292));
#77522=CARTESIAN_POINT('Ctrl Pts',(42.8325321482607,-1.92012847228508,-2.58843813106864));
#77523=CARTESIAN_POINT('Ctrl Pts',(42.834918521569,-1.88841924799229,-2.61153497156755));
#77524=CARTESIAN_POINT('Ctrl Pts',(42.8355993476656,-1.87936255676633,-2.61806007173481));
#77525=CARTESIAN_POINT('Ctrl Pts',(42.8366984652818,-1.86472634305043,-2.62848998547855));
#77526=CARTESIAN_POINT('Ctrl Pts',(42.837115612308,-1.85916796995023,-2.63242443321941));
#77527=CARTESIAN_POINT('Ctrl Pts',(42.8379818988246,-1.84761796599909,-2.64054517833469));
#77528=CARTESIAN_POINT('Ctrl Pts',(42.8384311388199,-1.84162448528395,-2.64472876509274));
#77529=CARTESIAN_POINT('Ctrl Pts',(42.8394861546221,-1.82754045376776,-2.65448865214723));
#77530=CARTESIAN_POINT('Ctrl Pts',(42.8400925568614,-1.81943856258134,-2.66004838830055));
#77531=CARTESIAN_POINT('Ctrl Pts',(42.842065277114,-1.79306142615782,-2.67797220656704));
#77532=CARTESIAN_POINT('Ctrl Pts',(42.8434372753487,-1.77468490897253,-2.69018546794621));
#77533=CARTESIAN_POINT('Ctrl Pts',(42.8466619423443,-1.73142804882892,-2.71829840987218));
#77534=CARTESIAN_POINT('Ctrl Pts',(42.8485201017628,-1.70645205698459,-2.73404656458143));
#77535=CARTESIAN_POINT('Ctrl Pts',(42.8550680211417,-1.6182841110775,-2.7879604890752));
#77536=CARTESIAN_POINT('Ctrl Pts',(42.8598220203931,-1.55400410220819,-2.82429407492053));
#77537=CARTESIAN_POINT('Ctrl Pts',(42.8842274045853,-1.22263479200983,-2.99685840271323));
#77538=CARTESIAN_POINT('Ctrl Pts',(42.9049902663269,-0.938762874228008,
-3.09752787809967));
#77539=CARTESIAN_POINT('Ctrl Pts',(42.9298908095668,-0.56917769571837,-3.17303627705564));
#77540=CARTESIAN_POINT('Ctrl Pts',(42.9349214925085,-0.492712588071752,
-3.18580586511337));
#77541=CARTESIAN_POINT('Ctrl Pts',(42.940493130576,-0.405111871963003,-3.19720491967623));
#77542=CARTESIAN_POINT('Ctrl Pts',(42.9411735877429,-0.394361781473908,
-3.19854868970525));
#77543=CARTESIAN_POINT('Ctrl Pts',(42.9421761538398,-0.378443101331638,
-3.20045706252447));
#77544=CARTESIAN_POINT('Ctrl Pts',(42.9425005599095,-0.373279729674426,
-3.20106339117617));
#77545=CARTESIAN_POINT('Ctrl Pts',(42.9430753654353,-0.364108272558035,
-3.20211789186341));
#77546=CARTESIAN_POINT('Ctrl Pts',(42.9433260441527,-0.360100798837707,
-3.20257103635188));
#77547=CARTESIAN_POINT('Ctrl Pts',(42.9438595260158,-0.351555734270683,
-3.20352102600854));
#77548=CARTESIAN_POINT('Ctrl Pts',(42.9441422078362,-0.347017950873448,
-3.20401575226539));
#77549=CARTESIAN_POINT('Ctrl Pts',(42.9449076545637,-0.334704164156703,
-3.20533178080819));
#77550=CARTESIAN_POINT('Ctrl Pts',(42.9453893746934,-0.326926136581007,
-3.20613443367199));
#77551=CARTESIAN_POINT('Ctrl Pts',(42.9478048923463,-0.28778572483437,-3.21002960943406));
#77552=CARTESIAN_POINT('Ctrl Pts',(42.9497153166246,-0.256380799457424,
-3.21269042673705));
#77553=CARTESIAN_POINT('Ctrl Pts',(42.9550937780551,-0.166881663234144,
-3.21895253256684));
#77554=CARTESIAN_POINT('Ctrl Pts',(42.9585101707497,-0.108719765296343,
-3.22144156265614));
#77555=CARTESIAN_POINT('Ctrl Pts',(42.9708375407736,0.104314046705968,-3.22478143352988));
#77556=CARTESIAN_POINT('Ctrl Pts',(42.979444100391,0.259130744852789,-3.21604635687948));
#77557=CARTESIAN_POINT('Ctrl Pts',(42.9916223030091,0.475209588365181,-3.18814405554449));
#77558=CARTESIAN_POINT('Ctrl Pts',(42.9951481626782,0.537440841841549,-3.17824539833281));
#77559=CARTESIAN_POINT('Ctrl Pts',(43.0089115203352,0.777321840479593,-3.13284220569045));
#77560=CARTESIAN_POINT('Ctrl Pts',(43.0193336093857,0.952120201069912,-3.08421512959863));
#77561=CARTESIAN_POINT('Ctrl Pts',(43.0313476415777,1.13863229861123,-3.01495485959217));
#77562=CARTESIAN_POINT('Ctrl Pts',(43.0324302602187,1.15531705586102,-3.00860080393486));
#77563=CARTESIAN_POINT('Ctrl Pts',(43.0340744758414,1.18046729977594,-2.99878277931221));
#77564=CARTESIAN_POINT('Ctrl Pts',(43.0346326458818,1.18897243355327,-2.99542079729703));
#77565=CARTESIAN_POINT('Ctrl Pts',(43.0356054873813,1.20373859651637,-2.98951110450956));
#77566=CARTESIAN_POINT('Ctrl Pts',(43.0360196027049,1.21000616407742,-2.9869798014919));
#77567=CARTESIAN_POINT('Ctrl Pts',(43.0368851072826,1.22306754248793,-2.98165680425003));
#77568=CARTESIAN_POINT('Ctrl Pts',(43.037336614726,1.22985985904333,-2.97886156736226));
#77569=CARTESIAN_POINT('Ctrl Pts',(43.03840683849,1.24590892381344,-2.9721926600866));
#77570=CARTESIAN_POINT('Ctrl Pts',(43.0390262339669,1.25515721206088,-2.96829894459281));
#77571=CARTESIAN_POINT('Ctrl Pts',(43.0410847805439,1.28575945236797,-2.95524619477804));
#77572=CARTESIAN_POINT('Ctrl Pts',(43.0425303224932,1.3070321456878,-2.94589958512677));
#77573=CARTESIAN_POINT('Ctrl Pts',(43.0570334638071,1.51826965226037,-2.85034951259255));
#77574=CARTESIAN_POINT('Ctrl Pts',(43.0707352894934,1.69950509787366,-2.7461405804526));
#77575=CARTESIAN_POINT('Ctrl Pts',(43.0942041431959,1.98360901088827,-2.54383160767006));
#77576=CARTESIAN_POINT('Ctrl Pts',(43.1037523944928,2.09240987631214,-2.45511801006155));
#77577=CARTESIAN_POINT('Ctrl Pts',(43.1182881902953,2.25092515153934,-2.30765463485599));
#77578=CARTESIAN_POINT('Ctrl Pts',(43.123363085877,2.30490626242056,-2.25373966361566));
#77579=CARTESIAN_POINT('Ctrl Pts',(43.1319348510027,2.39447514355486,-2.15769263017475));
#77580=CARTESIAN_POINT('Ctrl Pts',(43.1354764983054,2.43098872175777,-2.11646956249706));
#77581=CARTESIAN_POINT('Ctrl Pts',(43.1395055754905,2.47215445009682,-2.06752243513258));
#77582=CARTESIAN_POINT('Ctrl Pts',(43.1400638809961,2.47785021912557,-2.06069283030513));
#77583=CARTESIAN_POINT('Ctrl Pts',(43.1409512307291,2.4868904535251,-2.0497613136018));
#77584=CARTESIAN_POINT('Ctrl Pts',(43.1412815706574,2.4902531609399,-2.04567464811875));
#77585=CARTESIAN_POINT('Ctrl Pts',(43.1418638260637,2.49617564900892,-2.03844086204139));
#77586=CARTESIAN_POINT('Ctrl Pts',(43.1421160421045,2.49873957186375,-2.03529717031141));
#77587=CARTESIAN_POINT('Ctrl Pts',(43.1426449316822,2.50411293160897,-2.02868329777976));
#77588=CARTESIAN_POINT('Ctrl Pts',(43.1429215129071,2.50692108792429,-2.025212126282));
#77589=CARTESIAN_POINT('Ctrl Pts',(43.1436533885243,2.51434669713987,-2.01599419507258));
#77590=CARTESIAN_POINT('Ctrl Pts',(43.1441077893007,2.51895169414898,-2.01023736733903));
#77591=CARTESIAN_POINT('Ctrl Pts',(43.146191814602,2.54004427037647,-1.98368269920788));
#77592=CARTESIAN_POINT('Ctrl Pts',(43.1478050834613,2.55629486997702,-1.96269676496711));
#77593=CARTESIAN_POINT('Ctrl Pts',(43.1621705348721,2.700051774668,-1.77223500856972));
#77594=CARTESIAN_POINT('Ctrl Pts',(43.1739400141392,2.81081599430541,-1.59073431099035));
#77595=CARTESIAN_POINT('Ctrl Pts',(43.1998773356525,3.01238978044801,-1.172657197809));
#77596=CARTESIAN_POINT('Ctrl Pts',(43.2140405920445,3.09481465354932,-0.933657143999897));
#77597=CARTESIAN_POINT('Ctrl Pts',(43.2304272438378,3.15268440221548,-0.668634434885807));
#77598=CARTESIAN_POINT('Ctrl Pts',(43.2315998120293,3.15663669289056,-0.649719717576928));
#77599=CARTESIAN_POINT('Ctrl Pts',(43.2333453759244,3.16224066718501,-0.62164152931996));
#77600=CARTESIAN_POINT('Ctrl Pts',(43.2339141849805,3.16402317065066,-0.612504368060808));
#77601=CARTESIAN_POINT('Ctrl Pts',(43.2349271669012,3.16712013233677,-0.596254929518021));
#77602=CARTESIAN_POINT('Ctrl Pts',(43.2353708350004,3.16845028985694,-0.589145680607206));
#77603=CARTESIAN_POINT('Ctrl Pts',(43.2363045118478,3.17119439774743,-0.57420122237302));
#77604=CARTESIAN_POINT('Ctrl Pts',(43.2367946795013,3.17260326522033,-0.566365139971526));
#77605=CARTESIAN_POINT('Ctrl Pts',(43.2380857569203,3.17623072560392,-0.545750988381942));
#77606=CARTESIAN_POINT('Ctrl Pts',(43.2388881921863,3.17840122997594,-0.532964705187144));
#77607=CARTESIAN_POINT('Ctrl Pts',(43.2425035604747,3.18780338988673,-0.475476272433506));
#77608=CARTESIAN_POINT('Ctrl Pts',(43.2453438188681,3.19416927150867,-0.430639601260777));
#77609=CARTESIAN_POINT('Ctrl Pts',(43.2529724429511,3.20857414346446,-0.311138966819544));
#77610=CARTESIAN_POINT('Ctrl Pts',(43.2578106119749,3.21495152298744,-0.236306464384234));
#77611=CARTESIAN_POINT('Ctrl Pts',(43.2828154348829,3.23409932160388,0.145726984973295));
#77612=CARTESIAN_POINT('Ctrl Pts',(43.3041512721203,3.2054753472886,0.453343125383568));
#77613=CARTESIAN_POINT('Ctrl Pts',(43.3288565824333,3.11774957536298,0.818806655019639));
#77614=CARTESIAN_POINT('Ctrl Pts',(43.3332862104494,3.09964661718638,0.884872421551637));
#77615=CARTESIAN_POINT('Ctrl Pts',(43.3382658838135,3.07635558039444,0.960345809590095));
#77616=CARTESIAN_POINT('Ctrl Pts',(43.3389249598881,3.0732114819375,0.970360203999077));
#77617=CARTESIAN_POINT('Ctrl Pts',(43.3399021040513,3.06845728015622,0.985248101136925));
#77618=CARTESIAN_POINT('Ctrl Pts',(43.3402223060454,3.06688440909329,0.990133285507645));
#77619=CARTESIAN_POINT('Ctrl Pts',(43.3407924711809,3.06405680793869,0.998844156965081));
#77620=CARTESIAN_POINT('Ctrl Pts',(43.3410426966749,3.06280657591428,1.00267125786436));
#77621=CARTESIAN_POINT('Ctrl Pts',(43.3415783065097,3.06011044801472,1.01087231132271));
#77622=CARTESIAN_POINT('Ctrl Pts',(43.3418635578245,3.05866235007608,1.01524549381287));
#77623=CARTESIAN_POINT('Ctrl Pts',(43.3426432005881,3.05467112354348,1.02721274629916));
#77624=CARTESIAN_POINT('Ctrl Pts',(43.3431364803648,3.05210903634055,1.03480052796213));
#77625=CARTESIAN_POINT('Ctrl Pts',(43.3457092260153,3.03855482337168,1.07445389231433));
#77626=CARTESIAN_POINT('Ctrl Pts',(43.3477615208502,3.02708509764862,1.10635555288692));
#77627=CARTESIAN_POINT('Ctrl Pts',(43.353655367817,2.99229927086567,1.19851425675956));
#77628=CARTESIAN_POINT('Ctrl Pts',(43.3574325985022,2.96767104873109,1.25826109755009));
#77629=CARTESIAN_POINT('Ctrl Pts',(43.3783652969155,2.81913672199175,1.58992531565403));
#77630=CARTESIAN_POINT('Ctrl Pts',(43.3944258541196,2.65968341526877,1.84431575048016));
#77631=CARTESIAN_POINT('Ctrl Pts',(43.4129284517434,2.45445088831277,2.08858732932336));
#77632=CARTESIAN_POINT('Ctrl Pts',(43.4141054212306,2.44130217861829,2.1039415023352));
#77633=CARTESIAN_POINT('Ctrl Pts',(43.4197820489023,2.37746668483341,2.17708012124055));
#77634=CARTESIAN_POINT('Ctrl Pts',(43.4243485183919,2.32487120431583,2.23315878004042));
#77635=CARTESIAN_POINT('Ctrl Pts',(43.4298892953644,2.25992421593957,2.29762373585778));
#77636=CARTESIAN_POINT('Ctrl Pts',(43.4307796305721,2.24945381316668,2.30787560860098));
#77637=CARTESIAN_POINT('Ctrl Pts',(43.432235130183,2.23228381667067,2.3244593978631));
#77638=CARTESIAN_POINT('Ctrl Pts',(43.4327983989897,2.22562625427951,2.33083467967221));
#77639=CARTESIAN_POINT('Ctrl Pts',(43.4338051662157,2.21370439969849,2.34215339858362));
#77640=CARTESIAN_POINT('Ctrl Pts',(43.4342481823049,2.2084506497448,2.34710788802611));
#77641=CARTESIAN_POINT('Ctrl Pts',(43.4351842559037,2.19733384195525,2.35752109691249));
#77642=CARTESIAN_POINT('Ctrl Pts',(43.4356774861151,2.19146700204927,2.36297569019799));
#77643=CARTESIAN_POINT('Ctrl Pts',(43.4369852917782,2.17588708490755,2.37735292151821));
#77644=CARTESIAN_POINT('Ctrl Pts',(43.4378014651827,2.16613954165151,2.38623783338958));
#77645=CARTESIAN_POINT('Ctrl Pts',(43.4415690716463,2.12103424815053,2.42684731614712));
#77646=CARTESIAN_POINT('Ctrl Pts',(43.4445507319769,2.08503382315228,2.45784615978638));
#77647=CARTESIAN_POINT('Ctrl Pts',(43.4526513374431,1.98647656436327,2.5389868563962));
#77648=CARTESIAN_POINT('Ctrl Pts',(43.457827997611,1.92271544037624,2.58760641990464));
#77649=CARTESIAN_POINT('Ctrl Pts',(43.4648790302444,1.834809030872,2.64959333917145));
#77650=CARTESIAN_POINT('Ctrl Pts',(43.4666839122602,1.81221492822833,2.66509751486038));
#77651=CARTESIAN_POINT('Ctrl Pts',(43.4684957936438,1.78943612473158,2.68030519120596));
#77652=CARTESIAN_POINT('Origin',(-1.72497344927317,0.,0.));
#77653=CARTESIAN_POINT('',(44.9670777766272,1.78943621037802,2.68030513402634));
#77654=CARTESIAN_POINT('',(44.7203641905528,1.78943621037803,2.68030513402633));
#77655=CARTESIAN_POINT('',(-1.72497344927317,1.78943621037804,2.68030513402633));
#77656=CARTESIAN_POINT('',(44.1465734493244,-3.22274921673691,0.00224689155001823));
#77657=CARTESIAN_POINT('Ctrl Pts',(44.1465734493244,-3.22274921673691,0.0022468915499753));
#77658=CARTESIAN_POINT('Ctrl Pts',(44.1526529568098,-3.22281760930423,-0.095849562091568));
#77659=CARTESIAN_POINT('Ctrl Pts',(44.1587324642952,-3.21840290922743,-0.194120808494868));
#77660=CARTESIAN_POINT('Ctrl Pts',(44.1648119717806,-3.20948372755331,-0.292116013033343));
#77661=CARTESIAN_POINT('Ctrl Pts',(44.1708844563096,-3.20057484918487,-0.389998014972797));
#77662=CARTESIAN_POINT('Ctrl Pts',(44.1769569408386,-3.18717186664683,-0.487604165813532));
#77663=CARTESIAN_POINT('Ctrl Pts',(44.1830294253676,-3.16930542664221,-0.584483254812545));
#77664=CARTESIAN_POINT('Ctrl Pts',(44.1890968615674,-3.15145383981163,-0.681281803873583));
#77665=CARTESIAN_POINT('Ctrl Pts',(44.1951642977673,-3.12914624990319,-0.777354053550099));
#77666=CARTESIAN_POINT('Ctrl Pts',(44.2012317339671,-3.10246504238519,-0.872254677991387));
#77667=CARTESIAN_POINT('Ctrl Pts',(44.2072965624384,-3.07579530220618,-0.967114515012184));
#77668=CARTESIAN_POINT('Ctrl Pts',(44.2133613909097,-3.0447557976732,-1.06080329618506));
#77669=CARTESIAN_POINT('Ctrl Pts',(44.2194262193809,-3.00947962439654,-1.15288765837877));
#77670=CARTESIAN_POINT('Ctrl Pts',(44.2254901704919,-2.97420855430017,-1.24495869931171));
#77671=CARTESIAN_POINT('Ctrl Pts',(44.2315541216029,-2.93470219353686,-1.33542536435833));
#77672=CARTESIAN_POINT('Ctrl Pts',(44.2376180727139,-2.89114254196026,-1.42387231329482));
#77673=CARTESIAN_POINT('Ctrl Pts',(44.2436828756468,-2.84757677142465,-1.51233168664784));
#77674=CARTESIAN_POINT('Ctrl Pts',(44.2497476785798,-2.79995677867317,-1.59877037946745));
#77675=CARTESIAN_POINT('Ctrl Pts',(44.2558124815128,-2.74851092068858,-1.68279686277209));
#77676=CARTESIAN_POINT('Ctrl Pts',(44.2618835398218,-2.69701200027315,-1.76691001290734));
#77677=CARTESIAN_POINT('Ctrl Pts',(44.2679545981307,-2.64167957332646,-1.84860560559265));
#77678=CARTESIAN_POINT('Ctrl Pts',(44.2740256564397,-2.58278561195192,-1.92752069903131));
#77679=CARTESIAN_POINT('Ctrl Pts',(44.2801002125747,-2.52385771896009,-2.0064812592154));
#77680=CARTESIAN_POINT('Ctrl Pts',(44.2861747687096,-2.46136449333861,-2.08265778770013));
#77681=CARTESIAN_POINT('Ctrl Pts',(44.2922493248445,-2.39561708433311,-2.15572176955918));
#77682=CARTESIAN_POINT('Ctrl Pts',(44.29833346357,-2.3297659590251,-2.22890100958823));
#77683=CARTESIAN_POINT('Ctrl Pts',(44.3044176022955,-2.26065071977042,-2.29895758658903));
#77684=CARTESIAN_POINT('Ctrl Pts',(44.310501741021,-2.18861791905681,-2.36560122735922));
#77685=CARTESIAN_POINT('Ctrl Pts',(44.3136076711837,-2.1518454425353,-2.39962255779829));
#77686=CARTESIAN_POINT('Ctrl Pts',(44.3167136013464,-2.11431314330431,-2.43275512131571));
#77687=CARTESIAN_POINT('Ctrl Pts',(44.319819531509,-2.0760700651483,-2.46496463404552));
#77688=CARTESIAN_POINT('Ctrl Pts',(44.3259917795973,-2.00007165125118,-2.52897286763693));
#77689=CARTESIAN_POINT('Ctrl Pts',(44.3321640276855,-1.92097649915154,-2.58957575854878));
#77690=CARTESIAN_POINT('Ctrl Pts',(44.3383362757738,-1.83912266263081,-2.64645902940094));
#77691=CARTESIAN_POINT('Ctrl Pts',(44.3445001644218,-1.7573796855965,-2.70326525987893));
#77692=CARTESIAN_POINT('Ctrl Pts',(44.3506640530699,-1.67288580390756,-2.75636163758103));
#77693=CARTESIAN_POINT('Ctrl Pts',(44.3568279417179,-1.58601304345421,-2.80547325570805));
#77694=CARTESIAN_POINT('Ctrl Pts',(44.3629853033718,-1.49923227330649,-2.85453286912452));
#77695=CARTESIAN_POINT('Ctrl Pts',(44.3691426650256,-1.41007800848197,-2.89961589913159));
#77696=CARTESIAN_POINT('Ctrl Pts',(44.3753000266795,-1.31895143260922,-2.94049055106764));
#77697=CARTESIAN_POINT('Ctrl Pts',(44.381452890821,-1.22789141818314,-2.98133534699364));
#77698=CARTESIAN_POINT('Ctrl Pts',(44.3876057549626,-1.1348623520684,-3.01797769908814));
#77699=CARTESIAN_POINT('Ctrl Pts',(44.3937586191041,-1.04028939166791,-3.05023204757986));
#77700=CARTESIAN_POINT('Ctrl Pts',(44.3999091522358,-0.945752260191214,
-3.08247417652606));
#77701=CARTESIAN_POINT('Ctrl Pts',(44.4060596853675,-0.849672807295397,
-3.11033146497705));
#77702=CARTESIAN_POINT('Ctrl Pts',(44.4122102184992,-0.752494680015537,
-3.1336670721454));
#77703=CARTESIAN_POINT('Ctrl Pts',(44.4183600667095,-0.655327374460668,
-3.15700008066804));
#77704=CARTESIAN_POINT('Ctrl Pts',(44.4245099149198,-0.557062060136261,
-3.1758123075808));
#77705=CARTESIAN_POINT('Ctrl Pts',(44.4306597631301,-0.45815502131104,-3.19001748254574));
#77706=CARTESIAN_POINT('Ctrl Pts',(44.4368105715043,-0.359232540321682,
-3.2042248753371));
#77707=CARTESIAN_POINT('Ctrl Pts',(44.4429613798785,-0.259668565829818,
-3.21382372572693));
#77708=CARTESIAN_POINT('Ctrl Pts',(44.4491121882527,-0.159925985765453,
-3.21877946457612));
#77709=CARTESIAN_POINT('Ctrl Pts',(44.4552695746139,-0.0600767359176954,
-3.22374050334426));
#77710=CARTESIAN_POINT('Ctrl Pts',(44.4614269609751,0.0399510662436259,
-3.22404849322508));
#77711=CARTESIAN_POINT('Ctrl Pts',(44.4675843473363,0.139693157421742,-3.21972101031589));
#77712=CARTESIAN_POINT('Ctrl Pts',(44.4737451700682,0.239490913582315,-3.21539111228528));
#77713=CARTESIAN_POINT('Ctrl Pts',(44.4799059928002,0.339002208577645,-3.20642062847573));
#77714=CARTESIAN_POINT('Ctrl Pts',(44.4860668155321,0.437768627146858,-3.19287898166936));
#77715=CARTESIAN_POINT('Ctrl Pts',(44.4922379384438,0.536700171691406,-3.17931469480305));
#77716=CARTESIAN_POINT('Ctrl Pts',(44.4984090613555,0.634883924931221,-3.16116405837411));
#77717=CARTESIAN_POINT('Ctrl Pts',(44.5045801842671,0.731872234600702,-3.13854752946655));
#77718=CARTESIAN_POINT('Ctrl Pts',(44.5092757062609,0.805669296774438,-3.12133892571179));
#77719=CARTESIAN_POINT('Ctrl Pts',(44.5139712282547,0.878774483578418,-3.10154586109726));
#77720=CARTESIAN_POINT('Ctrl Pts',(44.5186667502485,0.950997881658948,-3.07924026207443));
#77721=CARTESIAN_POINT('Ctrl Pts',(44.5248389983783,1.04593529954678,-3.04991962593781));
#77722=CARTESIAN_POINT('Ctrl Pts',(44.531011246508,1.13968255083815,-3.01615268230944));
#77723=CARTESIAN_POINT('Ctrl Pts',(44.5371834946378,1.23179247345417,-2.97805387205162));
#77724=CARTESIAN_POINT('Ctrl Pts',(44.5433473833275,1.32377764616418,-2.94000666126174));
#77725=CARTESIAN_POINT('Ctrl Pts',(44.5495112720172,1.41412949992564,-2.89763940952146));
#77726=CARTESIAN_POINT('Ctrl Pts',(44.5556751607069,1.5024156224767,-2.85111642340995));
#77727=CARTESIAN_POINT('Ctrl Pts',(44.5618325224026,1.59060825810347,-2.80464270088319));
#77728=CARTESIAN_POINT('Ctrl Pts',(44.5679898840983,1.67673912915199,-2.75402219406405));
#77729=CARTESIAN_POINT('Ctrl Pts',(44.574147245794,1.76039632378757,-2.69946704845516));
#77730=CARTESIAN_POINT('Ctrl Pts',(44.5803001099774,1.84399241282648,-2.6449517514778));
#77731=CARTESIAN_POINT('Ctrl Pts',(44.5864529741608,1.92511805501856,-2.58650776621703));
#77732=CARTESIAN_POINT('Ctrl Pts',(44.5926058383442,2.00338726886607,-2.52439240480662));
#77733=CARTESIAN_POINT('Ctrl Pts',(44.5987563715178,2.08162683045724,-2.46230057577285));
#77734=CARTESIAN_POINT('Ctrl Pts',(44.6049069046914,2.15701177407305,-2.39654040402348));
#77735=CARTESIAN_POINT('Ctrl Pts',(44.611057437865,2.22918710352607,-2.32741109818894));
#77736=CARTESIAN_POINT('Ctrl Pts',(44.6172072861172,2.30135439555739,-2.25828949057188));
#77737=CARTESIAN_POINT('Ctrl Pts',(44.6233571343693,2.37031247033412,-2.18579979525279));
#77738=CARTESIAN_POINT('Ctrl Pts',(44.6295069826215,2.43574203890022,-2.11027919537539));
#77739=CARTESIAN_POINT('Ctrl Pts',(44.6356577910375,2.50118182285714,-2.03474680461415));
#77740=CARTESIAN_POINT('Ctrl Pts',(44.6418085994534,2.5630917219174,-1.95618289770892));
#77741=CARTESIAN_POINT('Ctrl Pts',(44.6479594078694,2.62119236796707,-1.87495816822967));
#77742=CARTESIAN_POINT('Ctrl Pts',(44.654116794272,2.67935514979558,-1.79364657290349));
#77743=CARTESIAN_POINT('Ctrl Pts',(44.6602741806746,2.73370029043168,-1.70966882658044));
#77744=CARTESIAN_POINT('Ctrl Pts',(44.6664315670772,2.78399154312429,-1.62342497526448));
#77745=CARTESIAN_POINT('Ctrl Pts',(44.6725923898503,2.83431086281969,-1.53713299219027));
#77746=CARTESIAN_POINT('Ctrl Pts',(44.6787532126235,2.8805715878488,-1.4485727705376));
#77747=CARTESIAN_POINT('Ctrl Pts',(44.6849140353966,2.92258424744677,-1.35816747092397));
#77748=CARTESIAN_POINT('Ctrl Pts',(44.6910851583489,2.96466714732472,-1.26761102416523));
#77749=CARTESIAN_POINT('Ctrl Pts',(44.6972562813011,3.00248763059313,-1.17520373993617));
#77750=CARTESIAN_POINT('Ctrl Pts',(44.7034274042533,3.03590497665852,-1.08138731969633));
#77751=CARTESIAN_POINT('Ctrl Pts',(44.7081229258316,3.06133177025094,-1.01000371106538));
#77752=CARTESIAN_POINT('Ctrl Pts',(44.7128184474099,3.08421038868229,-0.937804669863619));
#77753=CARTESIAN_POINT('Ctrl Pts',(44.7175139689882,3.10449864903982,-0.864988844211257));
#77754=CARTESIAN_POINT('Ctrl Pts',(44.7236862170209,3.13116750211432,-0.769272675274183));
#77755=CARTESIAN_POINT('Ctrl Pts',(44.7298584650537,3.15345254656793,-0.672153521110634));
#77756=CARTESIAN_POINT('Ctrl Pts',(44.7360307130864,3.17120826595635,-0.574069417779857));
#77757=CARTESIAN_POINT('Ctrl Pts',(44.7421946016792,3.18893993772539,-0.476118155542837));
#77758=CARTESIAN_POINT('Ctrl Pts',(44.7483584902719,3.20215440039602,-0.37720496538648));
#77759=CARTESIAN_POINT('Ctrl Pts',(44.7545223788646,3.21075606038626,-0.277782438597017));
#77760=CARTESIAN_POINT('Ctrl Pts',(44.7606797404634,3.21934861200581,-0.178465191164078));
#77761=CARTESIAN_POINT('Ctrl Pts',(44.7668371020623,3.22333803462936,-0.0786401097310378));
#77762=CARTESIAN_POINT('Ctrl Pts',(44.7729944636611,3.22268006199457,0.0212315925614776));
#77763=CARTESIAN_POINT('Ctrl Pts',(44.7791473277481,3.22202256996167,0.121030345726199));
#77764=CARTESIAN_POINT('Ctrl Pts',(44.7853001918352,3.21672443454802,0.220875218990439));
#77765=CARTESIAN_POINT('Ctrl Pts',(44.7914530559222,3.20679340486268,0.320302389983657));
#77766=CARTESIAN_POINT('Ctrl Pts',(44.7976035889998,3.19686613754291,0.419691893043447));
#77767=CARTESIAN_POINT('Ctrl Pts',(44.8037541220774,3.18230950658779,0.518663576521987));
#77768=CARTESIAN_POINT('Ctrl Pts',(44.809904655155,3.16318325888739,0.616757029302923));
#77769=CARTESIAN_POINT('Ctrl Pts',(44.8160545033117,3.14405914107842,0.714839558435483));
#77770=CARTESIAN_POINT('Ctrl Pts',(44.8222043514683,3.12036650136265,0.812043624962921));
#77771=CARTESIAN_POINT('Ctrl Pts',(44.828354199625,3.0922163383949,0.907918321801928));
#77772=CARTESIAN_POINT('Ctrl Pts',(44.834505007946,3.06406178039452,1.0038079873792));
#77773=CARTESIAN_POINT('Ctrl Pts',(44.840655816267,3.03144843920041,1.09836745419547));
#77774=CARTESIAN_POINT('Ctrl Pts',(44.846806624588,2.99453708834475,1.19116127750516));
#77775=CARTESIAN_POINT('Ctrl Pts',(44.8529640108972,2.95758626260795,1.28405433926215));
#77776=CARTESIAN_POINT('Ctrl Pts',(44.8591213972063,2.91632840931499,1.37517758243127));
#77777=CARTESIAN_POINT('Ctrl Pts',(44.8652787835154,2.87097230968958,1.46411596518024));
#77778=CARTESIAN_POINT('Ctrl Pts',(44.8714396061959,2.82559089731133,1.55310398348692));
#77779=CARTESIAN_POINT('Ctrl Pts',(44.8776004288763,2.77610689883539,1.63990433568739));
#77780=CARTESIAN_POINT('Ctrl Pts',(44.8837612515567,2.72277383195886,1.72412883001823));
#77781=CARTESIAN_POINT('Ctrl Pts',(44.8899323744182,2.66935159837899,1.80849413793698));
#77782=CARTESIAN_POINT('Ctrl Pts',(44.8961034972797,2.6120676916164,1.89027462987103));
#77783=CARTESIAN_POINT('Ctrl Pts',(44.9022746201413,2.55121758580642,1.96911309791288));
#77784=CARTESIAN_POINT('Ctrl Pts',(44.9069701426701,2.50491757701946,2.02910020417178));
#77785=CARTESIAN_POINT('Ctrl Pts',(44.911665665199,2.45655379384332,2.087384674831));
#77786=CARTESIAN_POINT('Ctrl Pts',(44.9163611877278,2.40627053220781,2.14382361408964));
#77787=CARTESIAN_POINT('Ctrl Pts',(44.9225333531327,2.34017424452021,2.21801141028038));
#77788=CARTESIAN_POINT('Ctrl Pts',(44.9287055185376,2.27052747811876,2.28927019455793));
#77789=CARTESIAN_POINT('Ctrl Pts',(44.9348776839424,2.19762001868556,2.35724072083707));
#77790=CARTESIAN_POINT('Ctrl Pts',(44.9410406362659,2.12482138691904,2.42510978872175));
#77791=CARTESIAN_POINT('Ctrl Pts',(44.9472035885894,2.04877205618219,2.4897000661279));
#77792=CARTESIAN_POINT('Ctrl Pts',(44.9533665409128,1.96980090855367,2.55068656309652));
#77793=CARTESIAN_POINT('Ctrl Pts',(44.9579369528176,1.91123633522698,2.59591381736485));
#77794=CARTESIAN_POINT('Ctrl Pts',(44.9625073647224,1.85106573411159,2.63915978083607));
#77795=CARTESIAN_POINT('Ctrl Pts',(44.9670777766272,1.78943621037802,2.68030513402634));
#77796=CARTESIAN_POINT('Ctrl Pts',(43.716926315029,1.78943621037803,2.68030513402633));
#77797=CARTESIAN_POINT('Ctrl Pts',(43.7190435017826,1.76105704067242,2.6992517506809));
#77798=CARTESIAN_POINT('Ctrl Pts',(43.7211606885363,1.73239290766513,2.71773692959355));
#77799=CARTESIAN_POINT('Ctrl Pts',(43.7232778752899,1.70346037892409,2.73575223657695));
#77800=CARTESIAN_POINT('Ctrl Pts',(43.7294501233816,1.61911319273265,2.78827237631396));
#77801=CARTESIAN_POINT('Ctrl Pts',(43.7356223714733,1.53218636313262,2.83698048428247));
#77802=CARTESIAN_POINT('Ctrl Pts',(43.741794619565,1.44305929443266,2.88161368598421));
#77803=CARTESIAN_POINT('Ctrl Pts',(43.7479585082166,1.35405293578609,2.92618643830464));
#77804=CARTESIAN_POINT('Ctrl Pts',(43.7541223968682,1.26285264592198,2.96669506096335));
#77805=CARTESIAN_POINT('Ctrl Pts',(43.7602862855197,1.16986584160716,3.00292049097887));
#77806=CARTESIAN_POINT('Ctrl Pts',(43.7664436471772,1.07697750180988,3.0391075615786));
#77807=CARTESIAN_POINT('Ctrl Pts',(43.7726010088347,0.98230681106408,3.07102029974576));
#77808=CARTESIAN_POINT('Ctrl Pts',(43.7787583704922,0.886283900001522,3.09848647102066));
#77809=CARTESIAN_POINT('Ctrl Pts',(43.7849112346374,0.790331126806957,3.12593258022211));
#77810=CARTESIAN_POINT('Ctrl Pts',(43.7910640987826,0.693028513380123,3.14893846081337));
#77811=CARTESIAN_POINT('Ctrl Pts',(43.7972169629278,0.594823328022513,3.16738105868874));
#77812=CARTESIAN_POINT('Ctrl Pts',(43.8033674960633,0.496655347654633,3.18581666959432));
#77813=CARTESIAN_POINT('Ctrl Pts',(43.8095180291987,0.397585901225343,3.19969235281176));
#77814=CARTESIAN_POINT('Ctrl Pts',(43.8156685623342,0.298073612445653,3.2089359114921));
#77815=CARTESIAN_POINT('Ctrl Pts',(43.8218184105483,0.198572405321534,3.21817844081279));
#77816=CARTESIAN_POINT('Ctrl Pts',(43.8279682587624,0.0986288864057926,
3.22278983096988));
#77817=CARTESIAN_POINT('Ctrl Pts',(43.8341181069765,-0.00129302174893185,
3.2227497406089));
#77818=CARTESIAN_POINT('Ctrl Pts',(43.8402689153546,-0.101230530518191,
3.2227096439887));
#77819=CARTESIAN_POINT('Ctrl Pts',(43.8464197237326,-0.201145987408588,
3.21801662455096));
#77820=CARTESIAN_POINT('Ctrl Pts',(43.8525705321106,-0.300576304171876,
3.20870245549044));
#77821=CARTESIAN_POINT('Ctrl Pts',(43.8587279184757,-0.400112956768798,
3.19937832538419));
#77822=CARTESIAN_POINT('Ctrl Pts',(43.8648853048408,-0.499162999856632,
3.1854232173993));
#77823=CARTESIAN_POINT('Ctrl Pts',(43.8710426912059,-0.597269417687098,
3.16692071343691));
#77824=CARTESIAN_POINT('Ctrl Pts',(43.8772035139418,-0.69543058764883,3.14840788342706));
#77825=CARTESIAN_POINT('Ctrl Pts',(43.8833643366776,-0.792646660926259,
3.12534270361975));
#77826=CARTESIAN_POINT('Ctrl Pts',(43.8895251594135,-0.888473801333701,
3.09785923935282));
#77827=CARTESIAN_POINT('Ctrl Pts',(43.8956962823291,-0.984461153585005,
3.07032982592715));
#77828=CARTESIAN_POINT('Ctrl Pts',(43.9018674052447,-1.07905452286466,3.03836751213368));
#77829=CARTESIAN_POINT('Ctrl Pts',(43.9080385281603,-1.17182800149522,3.00215534198544));
#77830=CARTESIAN_POINT('Ctrl Pts',(43.9127340501167,-1.24241805647297,2.97460200325804));
#77831=CARTESIAN_POINT('Ctrl Pts',(43.9174295720732,-1.31195486234312,2.94458923460663));
#77832=CARTESIAN_POINT('Ctrl Pts',(43.9221250940296,-1.38026069932417,2.91221530186234));
#77833=CARTESIAN_POINT('Ctrl Pts',(43.9282973421279,-1.4700484963608,2.86965987422987));
#77834=CARTESIAN_POINT('Ctrl Pts',(43.9344695902262,-1.55802441789106,2.82287322294944));
#77835=CARTESIAN_POINT('Ctrl Pts',(43.9406418383245,-1.64376218374863,2.77203236737559));
#77836=CARTESIAN_POINT('Ctrl Pts',(43.9468057269826,-1.72938382988641,2.721260368575));
#77837=CARTESIAN_POINT('Ctrl Pts',(43.9529696156408,-1.81277297499114,2.66644529874857));
#77838=CARTESIAN_POINT('Ctrl Pts',(43.9591335042989,-1.89352504691214,2.60781143091605));
#77839=CARTESIAN_POINT('Ctrl Pts',(43.965290865963,-1.97419160977797,2.54923965098443));
#77840=CARTESIAN_POINT('Ctrl Pts',(43.971448227627,-2.05222630149996,2.48685736622848));
#77841=CARTESIAN_POINT('Ctrl Pts',(43.9776055892911,-2.1272516608781,2.42093327743483));
#77842=CARTESIAN_POINT('Ctrl Pts',(43.9837584534429,-2.20222221959785,2.35505734147243));
#77843=CARTESIAN_POINT('Ctrl Pts',(43.9899113175947,-2.27418749085708,2.28564503079462));
#77844=CARTESIAN_POINT('Ctrl Pts',(43.9960641817466,-2.34280211789449,2.2130060548695));
#77845=CARTESIAN_POINT('Ctrl Pts',(44.0022147148886,-2.41139075031172,2.14039459818732));
#77846=CARTESIAN_POINT('Ctrl Pts',(44.0083652480306,-2.47663096283152,2.06455922062285));
#77847=CARTESIAN_POINT('Ctrl Pts',(44.0145157811727,-2.5382140402841,1.98584668295533));
#77848=CARTESIAN_POINT('Ctrl Pts',(44.0206656293934,-2.59979025986543,1.90714291069011));
#77849=CARTESIAN_POINT('Ctrl Pts',(44.0268154776141,-2.65770988640599,1.82556295743417));
#77850=CARTESIAN_POINT('Ctrl Pts',(44.0329653258347,-2.71170496090233,1.74148608019637));
#77851=CARTESIAN_POINT('Ctrl Pts',(44.0391161342193,-2.76570846554522,1.65739607619832));
#77852=CARTESIAN_POINT('Ctrl Pts',(44.0452669426039,-2.81578596635182,1.57080873942461));
#77853=CARTESIAN_POINT('Ctrl Pts',(44.0514177509885,-2.86171379465896,1.48213080393015));
#77854=CARTESIAN_POINT('Ctrl Pts',(44.0575751373601,-2.90769074051907,1.39335803174616));
#77855=CARTESIAN_POINT('Ctrl Pts',(44.0637325237317,-2.94950895175349,1.30249058266012));
#77856=CARTESIAN_POINT('Ctrl Pts',(44.0698899101033,-2.98699162510762,1.20995809598388));
#77857=CARTESIAN_POINT('Ctrl Pts',(44.0760507328456,-3.02449521713638,1.11737396792755));
#77858=CARTESIAN_POINT('Ctrl Pts',(44.0822115555879,-3.05765830847178,1.02312336147732));
#77859=CARTESIAN_POINT('Ctrl Pts',(44.0883723783302,-3.08635368930061,0.927652126090644));
#77860=CARTESIAN_POINT('Ctrl Pts',(44.0945435012522,-3.11509704547126,0.83202127389392));
#77861=CARTESIAN_POINT('Ctrl Pts',(44.1007146241741,-3.13935766546156,0.735166137980126));
#77862=CARTESIAN_POINT('Ctrl Pts',(44.1068857470961,-3.1590592348845,0.637543969456977));
#77863=CARTESIAN_POINT('Ctrl Pts',(44.1115812689871,-3.17404988596756,0.563264614605248));
#77864=CARTESIAN_POINT('Ctrl Pts',(44.1162767908782,-3.18640214017127,0.488541423362433));
#77865=CARTESIAN_POINT('Ctrl Pts',(44.1209723127692,-3.19610256468347,0.413577028525253));
#77866=CARTESIAN_POINT('Ctrl Pts',(44.1295060249372,-3.21373226221536,0.277335608886467));
#77867=CARTESIAN_POINT('Ctrl Pts',(44.1380397371051,-3.22265321509459,0.139943391985787));
#77868=CARTESIAN_POINT('Ctrl Pts',(44.146573449273,-3.22274921673633,0.00224689238003723));
#77869=CARTESIAN_POINT('',(43.9000265507268,-3.22274886258475,-0.00270762048436531));
#77870=CARTESIAN_POINT('Ctrl Pts',(43.4684957936438,1.78943612473158,2.68030519120596));
#77871=CARTESIAN_POINT('Ctrl Pts',(43.4877157978139,1.54780402775395,2.84162458298458));
#77872=CARTESIAN_POINT('Ctrl Pts',(43.5078864493151,1.28539961238176,2.96957769162189));
#77873=CARTESIAN_POINT('Ctrl Pts',(43.5301679120223,0.960501825768391,3.07671790198192));
#77874=CARTESIAN_POINT('Ctrl Pts',(43.5334674418493,0.911331458664287,3.0916391281324));
#77875=CARTESIAN_POINT('Ctrl Pts',(43.5372517817597,0.853432532566815,3.10770756046767));
#77876=CARTESIAN_POINT('Ctrl Pts',(43.5377982946381,0.845033415565883,3.11000191313858));
#77877=CARTESIAN_POINT('Ctrl Pts',(43.5386704724684,0.831566970626343,3.11362190513594));
#77878=CARTESIAN_POINT('Ctrl Pts',(43.538997365623,0.826505601174957,3.11496925938776));
#77879=CARTESIAN_POINT('Ctrl Pts',(43.5395756779191,0.8175259030862,3.11733625916046));
#77880=CARTESIAN_POINT('Ctrl Pts',(43.5398273840808,0.81360891454056,3.11836086586996));
#77881=CARTESIAN_POINT('Ctrl Pts',(43.5403124180941,0.806044098609917,3.12032444808976));
#77882=CARTESIAN_POINT('Ctrl Pts',(43.5405458039166,0.802396575251329,3.12126440511255));
#77883=CARTESIAN_POINT('Ctrl Pts',(43.5411886306378,0.792329537570116,3.12383984079869));
#77884=CARTESIAN_POINT('Ctrl Pts',(43.5415972985089,0.785906570775604,3.12546193560499));
#77885=CARTESIAN_POINT('Ctrl Pts',(43.5432213124402,0.760292952470528,3.13184660357921));
#77886=CARTESIAN_POINT('Ctrl Pts',(43.5444278781981,0.741063160271112,3.13645244820113));
#77887=CARTESIAN_POINT('Ctrl Pts',(43.5529605414526,0.603761799507086,3.16800505074666));
#77888=CARTESIAN_POINT('Ctrl Pts',(43.5599549918109,0.484282687136266,3.18845751385116));
#77889=CARTESIAN_POINT('Ctrl Pts',(43.5763624822714,0.196750469310036,3.22113560177844));
#77890=CARTESIAN_POINT('Ctrl Pts',(43.5856419666568,0.0283441807176981,
3.22701479711338));
#77891=CARTESIAN_POINT('Ctrl Pts',(43.6053741388683,-0.321396223821876,
3.2118340535394));
#77892=CARTESIAN_POINT('Ctrl Pts',(43.6158326678356,-0.502019122454991,
3.18859475684349));
#77893=CARTESIAN_POINT('Ctrl Pts',(43.6278876224103,-0.697163904403001,
3.14648995652153));
#77894=CARTESIAN_POINT('Ctrl Pts',(43.6289706431008,-0.714590646619772,
3.14257804103835));
#77895=CARTESIAN_POINT('Ctrl Pts',(43.6306153674344,-0.740891888532359,
3.13644391695774));
#77896=CARTESIAN_POINT('Ctrl Pts',(43.6311736411122,-0.749791112451979,
3.13432840010267));
#77897=CARTESIAN_POINT('Ctrl Pts',(43.6321466125339,-0.765251038963044,
3.13058366857307));
#77898=CARTESIAN_POINT('Ctrl Pts',(43.6325607537696,-0.771815876804614,
3.12897163773967));
#77899=CARTESIAN_POINT('Ctrl Pts',(43.6334262629721,-0.785502792908852,
3.12556504798225));
#77900=CARTESIAN_POINT('Ctrl Pts',(43.63387774897,-0.792623898416815,3.12376677443606));
#77901=CARTESIAN_POINT('Ctrl Pts',(43.6349478323443,-0.809457586498474,
3.11945454083183));
#77902=CARTESIAN_POINT('Ctrl Pts',(43.635567108389,-0.819164657128837,3.11691954941381));
#77903=CARTESIAN_POINT('Ctrl Pts',(43.637624854785,-0.851302745727447,3.1083662216641));
#77904=CARTESIAN_POINT('Ctrl Pts',(43.6390697091569,-0.873680134157912,
3.10215085231447));
#77905=CARTESIAN_POINT('Ctrl Pts',(43.6533941161485,-1.0936397264507,3.03848786729265));
#77906=CARTESIAN_POINT('Ctrl Pts',(43.6668993394536,-1.28532129224465,2.96249510637663));
#77907=CARTESIAN_POINT('Ctrl Pts',(43.6912165112321,-1.60716973328735,2.79775218404842));
#77908=CARTESIAN_POINT('Ctrl Pts',(43.7018439395147,-1.74057921387812,2.71676195556411));
#77909=CARTESIAN_POINT('Ctrl Pts',(43.7148563692884,-1.8990374942846,2.60408559597139));
#77910=CARTESIAN_POINT('Ctrl Pts',(43.7174238771067,-1.93006783092945,2.58117096241183));
#77911=CARTESIAN_POINT('Ctrl Pts',(43.7251496374181,-2.02291568918314,2.50999582096536));
#77912=CARTESIAN_POINT('Ctrl Pts',(43.7302423114258,-2.08339523886887,2.46002713359831));
#77913=CARTESIAN_POINT('Ctrl Pts',(43.7358746360664,-2.15011481775636,2.40067529942196));
#77914=CARTESIAN_POINT('Ctrl Pts',(43.7365571251502,-2.15819664580325,2.39341239003989));
#77915=CARTESIAN_POINT('Ctrl Pts',(43.7375621030969,-2.17009553626384,2.38260991746821));
#77916=CARTESIAN_POINT('Ctrl Pts',(43.7378869049005,-2.17394090111141,2.37910185042888));
#77917=CARTESIAN_POINT('Ctrl Pts',(43.7384621502992,-2.18075113466646,2.37285868138165));
#77918=CARTESIAN_POINT('Ctrl Pts',(43.7387128747457,-2.18371937848494,2.37012731933458));
#77919=CARTESIAN_POINT('Ctrl Pts',(43.7391974865555,-2.18945653070508,2.36482809582943));
#77920=CARTESIAN_POINT('Ctrl Pts',(43.7394314265268,-2.19222603677146,2.36226095652493));
#77921=CARTESIAN_POINT('Ctrl Pts',(43.739943215619,-2.19828460475079,2.35662525504995));
#77922=CARTESIAN_POINT('Ctrl Pts',(43.7402209091242,-2.20157177392333,2.35355465648566));
#77923=CARTESIAN_POINT('Ctrl Pts',(43.7413444792351,-2.21487059820334,2.34107976552734));
#77924=CARTESIAN_POINT('Ctrl Pts',(43.7421860612179,-2.22482869539563,2.33161822071004));
#77925=CARTESIAN_POINT('Ctrl Pts',(43.7495215986104,-2.31156148875756,2.24814867953351));
#77926=CARTESIAN_POINT('Ctrl Pts',(43.7557454985783,-2.38468822838401,2.17042763984898));
#77927=CARTESIAN_POINT('Ctrl Pts',(43.7668528465909,-2.51065228014839,2.02247983370302));
#77928=CARTESIAN_POINT('Ctrl Pts',(43.7717727701243,-2.56472727665808,1.95345198314072));
#77929=CARTESIAN_POINT('Ctrl Pts',(43.782435155217,-2.67604197552961,1.79875288049955));
#77930=CARTESIAN_POINT('Ctrl Pts',(43.7881660857676,-2.7321235398809,1.71237063152408));
#77931=CARTESIAN_POINT('Ctrl Pts',(43.8042176906825,-2.87557815923005,1.46636800151938));
#77932=CARTESIAN_POINT('Ctrl Pts',(43.8146779103869,-2.95370962208854,1.3018335267992));
#77933=CARTESIAN_POINT('Ctrl Pts',(43.8267347640332,-3.02381862247912,1.11488004083615));
#77934=CARTESIAN_POINT('Ctrl Pts',(43.8278178032251,-3.0299508139322,1.09810500974019));
#77935=CARTESIAN_POINT('Ctrl Pts',(43.8294625509683,-3.03901221997626,1.07266302397029));
#77936=CARTESIAN_POINT('Ctrl Pts',(43.8300208294152,-3.04204455743757,1.06403296190034));
#77937=CARTESIAN_POINT('Ctrl Pts',(43.8309938068158,-3.04725383077033,1.04900302654227));
#77938=CARTESIAN_POINT('Ctrl Pts',(43.8314079492444,-3.04944745833011,1.04260896630515));
#77939=CARTESIAN_POINT('Ctrl Pts',(43.8322734586615,-3.05398246321459,1.02925342893996));
#77940=CARTESIAN_POINT('Ctrl Pts',(43.8327249436739,-3.05632019000713,1.0222907616417));
#77941=CARTESIAN_POINT('Ctrl Pts',(43.8337950205934,-3.06179481757895,1.0057985434146));
#77942=CARTESIAN_POINT('Ctrl Pts',(43.8344142911464,-3.06491104690823,0.996262257530085));
#77943=CARTESIAN_POINT('Ctrl Pts',(43.8364720007518,-3.07509313055501,0.964603103829358));
#77944=CARTESIAN_POINT('Ctrl Pts',(43.8379168235111,-3.08196425050239,0.942418814861096));
#77945=CARTESIAN_POINT('Ctrl Pts',(43.8522329707281,-3.1473072543721,0.723090129842494));
#77946=CARTESIAN_POINT('Ctrl Pts',(43.8657291158139,-3.18701264822889,0.520888115878363));
#77947=CARTESIAN_POINT('Ctrl Pts',(43.8867175598491,-3.21764322098082,0.21031966200839));
#77948=CARTESIAN_POINT('Ctrl Pts',(43.8939471317267,-3.22283591521967,0.103872347831675));
#77949=CARTESIAN_POINT('Ctrl Pts',(43.901142110102,-3.22274892502026,-0.00263225773335575));
#77950=CARTESIAN_POINT('Ctrl Pts',(43.9000265507268,-3.22274886258475,-0.00270762048436531));
#77951=CARTESIAN_POINT('Ctrl Pts',(43.9096069044335,-3.22261879382433,-0.157522134600772));
#77952=CARTESIAN_POINT('Ctrl Pts',(43.9191872581401,-3.21133027161691,-0.311883592365834));
#77953=CARTESIAN_POINT('Ctrl Pts',(43.9287676118467,-3.18909511021841,-0.464531958514156));
#77954=CARTESIAN_POINT('Ctrl Pts',(43.9306763029786,-3.18466520536568,-0.494944048889516));
#77955=CARTESIAN_POINT('Ctrl Pts',(43.9325849941104,-3.17980092626336,-0.525288252370513));
#77956=CARTESIAN_POINT('Ctrl Pts',(43.9344936852422,-3.17450413358386,-0.555554739300273));
#77957=CARTESIAN_POINT('Ctrl Pts',(43.940665933334,-3.15737557990436,-0.653429279127569));
#77958=CARTESIAN_POINT('Ctrl Pts',(43.9468381814259,-3.13568621731844,-0.750683199551832));
#77959=CARTESIAN_POINT('Ctrl Pts',(43.9530104295177,-3.10949324956114,-0.846858484892082));
#77960=CARTESIAN_POINT('Ctrl Pts',(43.9591743181695,-3.08333575648705,-0.942903514363202));
#77961=CARTESIAN_POINT('Ctrl Pts',(43.9653382068212,-3.05268689480415,-1.03787239694889));
#77962=CARTESIAN_POINT('Ctrl Pts',(43.9715020954729,-3.01765519470704,-1.13131546809791));
#77963=CARTESIAN_POINT('Ctrl Pts',(43.9776594571306,-2.98266058997488,-1.22465959158478));
#77964=CARTESIAN_POINT('Ctrl Pts',(43.9838168187882,-2.94329252526662,-1.31648071129962));
#77965=CARTESIAN_POINT('Ctrl Pts',(43.9899741804459,-2.89970957094703,-1.40634347392739));
#77966=CARTESIAN_POINT('Ctrl Pts',(43.9961270445913,-2.85615845085793,-1.49614059823527));
#77967=CARTESIAN_POINT('Ctrl Pts',(44.0022799087367,-2.80839875107193,-1.58398181975867));
#77968=CARTESIAN_POINT('Ctrl Pts',(44.0084327728821,-2.75663711508082,-1.66945181968779));
#77969=CARTESIAN_POINT('Ctrl Pts',(44.0145833060178,-2.70489508896184,-1.75488943934654));
#77970=CARTESIAN_POINT('Ctrl Pts',(44.0207338391534,-2.6491543639489,-1.83795725126199));
#77971=CARTESIAN_POINT('Ctrl Pts',(44.0268843722891,-2.58966704930943,-1.91826539775417));
#77972=CARTESIAN_POINT('Ctrl Pts',(44.0330342205034,-2.53018635915748,-1.99856460115795));
#77973=CARTESIAN_POINT('Ctrl Pts',(44.0391840687177,-2.46696016742312,-2.07610440108029));
#77974=CARTESIAN_POINT('Ctrl Pts',(44.0453339169321,-2.40028275318897,-2.15052557930464));
#77975=CARTESIAN_POINT('Ctrl Pts',(44.0514847253103,-2.33359492873871,-2.22495837676405));
#77976=CARTESIAN_POINT('Ctrl Pts',(44.0576355336886,-2.26345510141153,-2.29627126185731));
#77977=CARTESIAN_POINT('Ctrl Pts',(44.0637863420669,-2.19019582233104,-2.36414039818782));
#77978=CARTESIAN_POINT('Ctrl Pts',(44.0699437284322,-2.11685819605443,-2.43208211722186));
#77979=CARTESIAN_POINT('Ctrl Pts',(44.0761011147976,-2.04039477544658,-2.49657243730347));
#77980=CARTESIAN_POINT('Ctrl Pts',(44.0822585011629,-1.9611726619434,-2.55732660263523));
#77981=CARTESIAN_POINT('Ctrl Pts',(44.088419323899,-1.88190633543491,-2.61811467421003));
#77982=CARTESIAN_POINT('Ctrl Pts',(44.0945801466351,-1.79987860656931,-2.67516219055248));
#77983=CARTESIAN_POINT('Ctrl Pts',(44.1007409693713,-1.71548539930341,-2.72822788770968));
#77984=CARTESIAN_POINT('Ctrl Pts',(44.1069120922871,-1.63095109640112,-2.7813823045465));
#77985=CARTESIAN_POINT('Ctrl Pts',(44.113083215203,-1.54404379375434,-2.83054139080731));
#77986=CARTESIAN_POINT('Ctrl Pts',(44.1192543381189,-1.45518394917245,-2.87550990896761));
#77987=CARTESIAN_POINT('Ctrl Pts',(44.1239498600732,-1.38757172417166,-2.90972583160524));
#77988=CARTESIAN_POINT('Ctrl Pts',(44.1286453820276,-1.3188295870886,-2.94151658870071));
#77989=CARTESIAN_POINT('Ctrl Pts',(44.1333409039819,-1.24914929040216,-2.97081531112046));
#77990=CARTESIAN_POINT('Ctrl Pts',(44.1395131520737,-1.1575547706802,-3.00932838491779));
#77991=CARTESIAN_POINT('Ctrl Pts',(44.1456854001654,-1.06401624545754,-3.04366929034211));
#77992=CARTESIAN_POINT('Ctrl Pts',(44.1518576482571,-0.968949932253002,
-3.07363849391676));
#77993=CARTESIAN_POINT('Ctrl Pts',(44.1580215369087,-0.874012372971452,
-3.10356710842891));
#77994=CARTESIAN_POINT('Ctrl Pts',(44.1641854255603,-0.777551549047892,
-3.12913565999139));
#77995=CARTESIAN_POINT('Ctrl Pts',(44.1703493142118,-0.680004405698589,
-3.15019230694421));
#77996=CARTESIAN_POINT('Ctrl Pts',(44.1765066758693,-0.582560555848621,
-3.17122665683458));
#77997=CARTESIAN_POINT('Ctrl Pts',(44.1826640375268,-0.484033095757913,
-3.18775850947409));
#77998=CARTESIAN_POINT('Ctrl Pts',(44.1888213991842,-0.3848739891357,-3.19968585567189));
#77999=CARTESIAN_POINT('Ctrl Pts',(44.1949742633295,-0.285787311148003,
-3.21160448979647));
#78000=CARTESIAN_POINT('Ctrl Pts',(44.2011271274747,-0.18607033388292,-3.21892525250218));
#78001=CARTESIAN_POINT('Ctrl Pts',(44.2072799916199,-0.0861841614773,-3.22159740700331));
#78002=CARTESIAN_POINT('Ctrl Pts',(44.2134305247554,0.0136641690974123,
-3.22426854915993));
#78003=CARTESIAN_POINT('Ctrl Pts',(44.2195810578908,0.113681133709421,-3.22229457085069));
#78004=CARTESIAN_POINT('Ctrl Pts',(44.2257315910263,0.213402462540845,-3.2156767485992));
#78005=CARTESIAN_POINT('Ctrl Pts',(44.2318814392404,0.313112686438066,-3.20905966330621));
#78006=CARTESIAN_POINT('Ctrl Pts',(44.2380312874545,0.412526906585908,-3.19779979097804));
#78007=CARTESIAN_POINT('Ctrl Pts',(44.2441811356686,0.511183825705347,-3.18195044883437));
#78008=CARTESIAN_POINT('Ctrl Pts',(44.2503319440466,0.609856147939027,-3.16609863216352));
#78009=CARTESIAN_POINT('Ctrl Pts',(44.2564827524247,0.707770505380661,-3.14565599133951));
#78010=CARTESIAN_POINT('Ctrl Pts',(44.2626335608027,0.804474670169112,-3.12072716967637));
#78011=CARTESIAN_POINT('Ctrl Pts',(44.2687909471678,0.901282255305708,-3.09577168786451));
#78012=CARTESIAN_POINT('Ctrl Pts',(44.2749483335329,0.996876641878205,-3.06632055324456));
#78013=CARTESIAN_POINT('Ctrl Pts',(44.2811057198979,1.09081979526626,-3.0325286044414));
#78014=CARTESIAN_POINT('Ctrl Pts',(44.2872665426338,1.1848153773127,-2.99871779671689));
#78015=CARTESIAN_POINT('Ctrl Pts',(44.2934273653697,1.27715748948332,-2.96056151619983));
#78016=CARTESIAN_POINT('Ctrl Pts',(44.2995881881055,1.36742909825289,-2.91826236376226));
#78017=CARTESIAN_POINT('Ctrl Pts',(44.3057593110211,1.45785163066296,-2.87589249205688));
#78018=CARTESIAN_POINT('Ctrl Pts',(44.3119304339367,1.54619636063744,-2.82936611566188));
#78019=CARTESIAN_POINT('Ctrl Pts',(44.3181015568523,1.63207170678766,-2.77893136050591));
#78020=CARTESIAN_POINT('Ctrl Pts',(44.3227970788087,1.69741306829971,-2.74055625382915));
#78021=CARTESIAN_POINT('Ctrl Pts',(44.3274926007651,1.76132531397057,-2.69991934319405));
#78022=CARTESIAN_POINT('Ctrl Pts',(44.3321881227215,1.82364851036005,-2.65714577567012));
#78023=CARTESIAN_POINT('Ctrl Pts',(44.3383603708198,1.90557214610582,-2.60092006247854));
#78024=CARTESIAN_POINT('Ctrl Pts',(44.3445326189181,1.98503726029677,-2.54080310036477));
#78025=CARTESIAN_POINT('Ctrl Pts',(44.3507048670164,2.06165095051911,-2.47703712542296));
#78026=CARTESIAN_POINT('Ctrl Pts',(44.3568687556746,2.13816087829606,-2.41335751250696));
#78027=CARTESIAN_POINT('Ctrl Pts',(44.3630326443327,2.21182672703464,-2.34603898510911));
#78028=CARTESIAN_POINT('Ctrl Pts',(44.3691965329909,2.28228450542419,-2.27536700310096));
#78029=CARTESIAN_POINT('Ctrl Pts',(44.3753538946549,2.3526676754735,-2.20476985625509));
#78030=CARTESIAN_POINT('Ctrl Pts',(44.381511256319,2.41984922384378,-2.1308266204447));
#78031=CARTESIAN_POINT('Ctrl Pts',(44.3876686179831,2.48349895808877,-2.05386233415777));
#78032=CARTESIAN_POINT('Ctrl Pts',(44.3938214821349,2.54710220075582,-1.97695426477664));
#78033=CARTESIAN_POINT('Ctrl Pts',(44.3999743462868,2.60717848226385,-1.89702986586594));
#78034=CARTESIAN_POINT('Ctrl Pts',(44.4061272104386,2.66343579864805,-1.81444958843722));
#78035=CARTESIAN_POINT('Ctrl Pts',(44.4122777435806,2.7196718019736,-1.73190059650896));
#78036=CARTESIAN_POINT('Ctrl Pts',(44.4184282767227,2.77209147069796,-1.64669808392377));
#78037=CARTESIAN_POINT('Ctrl Pts',(44.4245788098647,2.82044484319969,-1.55923328882123));
#78038=CARTESIAN_POINT('Ctrl Pts',(44.4307286580854,2.86879283108576,-1.4717782337695));
#78039=CARTESIAN_POINT('Ctrl Pts',(44.4368785063061,2.91307521286436,-1.38206177721953));
#78040=CARTESIAN_POINT('Ctrl Pts',(44.4430283545268,2.95308741129367,-1.2905007957219));
#78041=CARTESIAN_POINT('Ctrl Pts',(44.4491791629114,2.99310585675014,-1.1989255189853));
#78042=CARTESIAN_POINT('Ctrl Pts',(44.4553299712961,3.02885262067261,-1.10550554336071));
#78043=CARTESIAN_POINT('Ctrl Pts',(44.4614807796807,3.0601712057145,-1.01067786866827));
#78044=CARTESIAN_POINT('Ctrl Pts',(44.4676381660523,3.09152328444239,-0.915748780442773));
#78045=CARTESIAN_POINT('Ctrl Pts',(44.4737955524239,3.11843759105824,-0.819409400157921));
#78046=CARTESIAN_POINT('Ctrl Pts',(44.4799529387955,3.14080752738901,-0.722111929271725));
#78047=CARTESIAN_POINT('Ctrl Pts',(44.4861137615378,3.16318994813931,-0.624760157719311));
#78048=CARTESIAN_POINT('Ctrl Pts',(44.4922745842801,3.18102287033894,-0.526449658132515));
#78049=CARTESIAN_POINT('Ctrl Pts',(44.4984354070225,3.19425122935006,-0.427640791197048));
#78050=CARTESIAN_POINT('Ctrl Pts',(44.5046065299444,3.20750170464007,-0.328666727319451));
#78051=CARTESIAN_POINT('Ctrl Pts',(44.5107776528664,3.21613220207214,-0.229193064728275));
#78052=CARTESIAN_POINT('Ctrl Pts',(44.5169487757883,3.22013971532271,-0.129683369409323));
#78053=CARTESIAN_POINT('Ctrl Pts',(44.5216442976793,3.22318897660537,-0.0539678215838685));
#78054=CARTESIAN_POINT('Ctrl Pts',(44.5263398195703,3.22356285074246,0.0217685218144568));
#78055=CARTESIAN_POINT('Ctrl Pts',(44.5310353414613,3.22128013491466,0.0973234550568934));
#78056=CARTESIAN_POINT('Ctrl Pts',(44.5372077907022,3.21827941467403,0.196643403119909));
#78057=CARTESIAN_POINT('Ctrl Pts',(44.5433802399431,3.21067569309872,0.295999261434805));
#78058=CARTESIAN_POINT('Ctrl Pts',(44.549552689184,3.1984602949907,0.394929492274231));
#78059=CARTESIAN_POINT('Ctrl Pts',(44.5557167273029,3.18626154265824,0.493724912082246));
#78060=CARTESIAN_POINT('Ctrl Pts',(44.5618807654217,3.16946365769102,0.592095429893225));
#78061=CARTESIAN_POINT('Ctrl Pts',(44.5680448035406,3.14810996312968,0.689580468505031));
#78062=CARTESIAN_POINT('Ctrl Pts',(44.5743914446661,3.12612368830928,0.789953396648254));
#78063=CARTESIAN_POINT('Ctrl Pts',(44.5807380857916,3.09930744334619,0.889387094077229));
#78064=CARTESIAN_POINT('Ctrl Pts',(44.5870847269171,3.06776600361313,0.987385086769861));
#78065=CARTESIAN_POINT('Ctrl Pts',(44.5932373666891,3.03718870883173,1.08238751962989));
#78066=CARTESIAN_POINT('Ctrl Pts',(44.599390006461,3.00217104426191,1.17604029840144));
#78067=CARTESIAN_POINT('Ctrl Pts',(44.605542646233,2.96285985464771,1.26790340492364));
#78068=CARTESIAN_POINT('Ctrl Pts',(44.6116929325193,2.92356370220853,1.35973137230035));
#78069=CARTESIAN_POINT('Ctrl Pts',(44.6178432188056,2.87997745949126,1.44977062912724));
#78070=CARTESIAN_POINT('Ctrl Pts',(44.6239935050919,2.83229652355686,1.53760006671038));
#78071=CARTESIAN_POINT('Ctrl Pts',(44.6301430839192,2.78462107229512,1.62541940139375));
#78072=CARTESIAN_POINT('Ctrl Pts',(44.6362926627465,2.7328520721566,1.71102904090691));
#78073=CARTESIAN_POINT('Ctrl Pts',(44.6424422415738,2.67723092407883,1.79403236917732));
#78074=CARTESIAN_POINT('Ctrl Pts',(44.6485927579275,2.62160129634751,1.87704835161782));
#78075=CARTESIAN_POINT('Ctrl Pts',(44.6547432742813,2.56211859665406,1.95745687328124));
#78076=CARTESIAN_POINT('Ctrl Pts',(44.660893790635,2.49906702543883,2.03489104496145));
#78077=CARTESIAN_POINT('Ctrl Pts',(44.6670500122561,2.43595696709016,2.11239704518845));
#78078=CARTESIAN_POINT('Ctrl Pts',(44.6732062338773,2.36927170495756,2.1869228520603));
#78079=CARTESIAN_POINT('Ctrl Pts',(44.6793624554984,2.29933492787142,2.25813561416726));
#78080=CARTESIAN_POINT('Ctrl Pts',(44.6855221287894,2.22935893863781,2.32938830384087));
#78081=CARTESIAN_POINT('Ctrl Pts',(44.6916818020804,2.15612812223851,2.39732395465477));
#78082=CARTESIAN_POINT('Ctrl Pts',(44.6978414753715,2.08000072026934,2.46164874955364));
#78083=CARTESIAN_POINT('Ctrl Pts',(44.7040093662931,2.00377175660436,2.52605936027026));
#78084=CARTESIAN_POINT('Ctrl Pts',(44.7101772572147,1.92463883962987,2.5868492382469));
#78085=CARTESIAN_POINT('Ctrl Pts',(44.7163451481363,1.84299047136763,2.64376694981765));
#78086=CARTESIAN_POINT('Ctrl Pts',(44.7176848289418,1.82525624857537,2.65612961424445));
#78087=CARTESIAN_POINT('Ctrl Pts',(44.7190245097473,1.80740345041526,2.66830977218673));
#78088=CARTESIAN_POINT('Ctrl Pts',(44.7203641905528,1.78943621037803,2.68030513402633));
#78089=CARTESIAN_POINT('Origin',(-1.72497344927317,0.,0.));
#78090=CARTESIAN_POINT('',(46.216937227185,1.78943621037807,2.68030513402631));
#78091=CARTESIAN_POINT('',(45.9705987712989,1.78932308991453,2.68012452748162));
#78092=CARTESIAN_POINT('',(-1.72497344927317,1.78943621037804,2.68030513402633));
#78093=CARTESIAN_POINT('',(45.3965734492404,-3.22274967111447,0.00145596415035607));
#78094=CARTESIAN_POINT('Ctrl Pts',(45.396573449273,-3.22274967111471,0.00145596361978267));
#78095=CARTESIAN_POINT('Ctrl Pts',(45.4028312200437,-3.22279569093976,-0.100408103620474));
#78096=CARTESIAN_POINT('Ctrl Pts',(45.4090889908143,-3.21800781208672,-0.202255132764274));
#78097=CARTESIAN_POINT('Ctrl Pts',(45.415346761585,-3.2084172616612,-0.303605397801885));
#78098=CARTESIAN_POINT('Ctrl Pts',(45.4216072500032,-3.19882254621644,-0.40499967760246));
#78099=CARTESIAN_POINT('Ctrl Pts',(45.4278677384214,-3.1844210469915,-0.505896352872799));
#78100=CARTESIAN_POINT('Ctrl Pts',(45.4341282268395,-3.16529571634117,-0.605822243411565));
#78101=CARTESIAN_POINT('Ctrl Pts',(45.4406927782651,-3.14524149561597,-0.710601392157561));
#78102=CARTESIAN_POINT('Ctrl Pts',(45.4472573296907,-3.11999311937981,-0.814312578103785));
#78103=CARTESIAN_POINT('Ctrl Pts',(45.4538218811163,-3.08970564774613,-0.916425977799434));
#78104=CARTESIAN_POINT('Ctrl Pts',(45.4600966167591,-3.06075532571062,-1.01403121342577));
#78105=CARTESIAN_POINT('Ctrl Pts',(45.4663713524019,-3.02720158720057,-1.11017637426488));
#78106=CARTESIAN_POINT('Ctrl Pts',(45.4726460880447,-2.98922957059347,-1.20441858869314));
#78107=CARTESIAN_POINT('Ctrl Pts',(45.4789267294548,-2.95122181480891,-1.29874950368374));
#78108=CARTESIAN_POINT('Ctrl Pts',(45.4852073708648,-2.90878766842503,-1.39117353019518));
#78109=CARTESIAN_POINT('Ctrl Pts',(45.4914880122748,-2.86215862993982,-1.48127159547499));
#78110=CARTESIAN_POINT('Ctrl Pts',(45.4977796281942,-2.8154481139765,-1.57152709404916));
#78111=CARTESIAN_POINT('Ctrl Pts',(45.5040712441137,-2.7645282803184,-1.65944816268342));
#78112=CARTESIAN_POINT('Ctrl Pts',(45.5103628600331,-2.70967440190764,-1.74464385997443));
#78113=CARTESIAN_POINT('Ctrl Pts',(45.5112095213377,-2.70229272812937,-1.75610862532804));
#78114=CARTESIAN_POINT('Ctrl Pts',(45.5120561826423,-2.69483987223226,-1.76752408602211));
#78115=CARTESIAN_POINT('Ctrl Pts',(45.5129028439468,-2.68731655974303,-1.77888933613952));
#78116=CARTESIAN_POINT('Ctrl Pts',(45.5190750921054,-2.63247083642038,-1.8617431806827));
#78117=CARTESIAN_POINT('Ctrl Pts',(45.525247340264,-2.57369323324841,-1.942204021402));
#78118=CARTESIAN_POINT('Ctrl Pts',(45.5314195884226,-2.51121937177829,-2.01987495387845));
#78119=CARTESIAN_POINT('Ctrl Pts',(45.537583477137,-2.4488301223878,-2.0974406919749));
#78120=CARTESIAN_POINT('Ctrl Pts',(45.5437473658515,-2.38275483465068,-2.17222369659909));
#78121=CARTESIAN_POINT('Ctrl Pts',(45.549911254566,-2.31327283205333,-2.24385524644171));
#78122=CARTESIAN_POINT('Ctrl Pts',(45.5560686162824,-2.24386440458309,-2.315410944982));
#78123=CARTESIAN_POINT('Ctrl Pts',(45.5622259779988,-2.17105673487563,-2.38382151314611));
#78124=CARTESIAN_POINT('Ctrl Pts',(45.5683833397153,-2.09516928556608,-2.44875136086139));
#78125=CARTESIAN_POINT('Ctrl Pts',(45.5745362039133,-2.01933726668512,-2.5136337819031));
#78126=CARTESIAN_POINT('Ctrl Pts',(45.5806890681113,-1.94043026977323,-2.57504025571928));
#78127=CARTESIAN_POINT('Ctrl Pts',(45.5868419323094,-1.85880380462553,-2.63267278225184));
#78128=CARTESIAN_POINT('Ctrl Pts',(45.5929924654938,-1.77720826367673,-2.69028347469285));
#78129=CARTESIAN_POINT('Ctrl Pts',(45.5991429986783,-1.69289565608329,-2.74412281051767));
#78130=CARTESIAN_POINT('Ctrl Pts',(45.6052935318628,-1.60625297860078,-2.79393431047262));
#78131=CARTESIAN_POINT('Ctrl Pts',(45.6114433801222,-1.5196199496716,-2.84374026340469));
#78132=CARTESIAN_POINT('Ctrl Pts',(45.6175932283815,-1.43065774331018,-2.88951905573437));
#78133=CARTESIAN_POINT('Ctrl Pts',(45.6237430766409,-1.33977975121226,-2.93105915681373));
#78134=CARTESIAN_POINT('Ctrl Pts',(45.6298938850603,-1.24888757056588,-2.97260574344282));
#78135=CARTESIAN_POINT('Ctrl Pts',(45.6360446934797,-1.15607940517697,-3.00991214376555));
#78136=CARTESIAN_POINT('Ctrl Pts',(45.6421955018992,-1.06178957245985,-3.04281456324823));
#78137=CARTESIAN_POINT('Ctrl Pts',(45.6483528882995,-0.967398901498728,
-3.07575217021729));
#78138=CARTESIAN_POINT('Ctrl Pts',(45.6545102746998,-0.871523809911516,
-3.10427624789803));
#78139=CARTESIAN_POINT('Ctrl Pts',(45.6606676611002,-0.774614650359711,
-3.12827263932479));
#78140=CARTESIAN_POINT('Ctrl Pts',(45.6668284838679,-0.677651406906714,
-3.15228242286505));
#78141=CARTESIAN_POINT('Ctrl Pts',(45.6729893066357,-0.579653372255442,
-3.171759403286));
#78142=CARTESIAN_POINT('Ctrl Pts',(45.6791501294034,-0.481079920266214,
-3.18664081327291));
#78143=CARTESIAN_POINT('Ctrl Pts',(45.6853212523452,-0.382341665012466,
-3.20154710323407));
#78144=CARTESIAN_POINT('Ctrl Pts',(45.6914923752869,-0.283026503055811,
-3.21184243088581));
#78145=CARTESIAN_POINT('Ctrl Pts',(45.6976634982286,-0.183597885011521,
-3.21751602624125));
#78146=CARTESIAN_POINT('Ctrl Pts',(45.7023590197146,-0.107944034528595,
-3.22183298591709));
#78147=CARTESIAN_POINT('Ctrl Pts',(45.7070545412005,-0.0322245824695204,
-3.22347528245398));
#78148=CARTESIAN_POINT('Ctrl Pts',(45.7117500626865,0.0433579790249112,
-3.2224583237266));
#78149=CARTESIAN_POINT('Ctrl Pts',(45.7179223123319,0.142711041252509,-3.22112153437035));
#78150=CARTESIAN_POINT('Ctrl Pts',(45.7240945619773,0.242177094397714,-3.21518328861998));
#78151=CARTESIAN_POINT('Ctrl Pts',(45.7302668116227,0.341294855735243,-3.20462718330053));
#78152=CARTESIAN_POINT('Ctrl Pts',(45.7364307018349,0.440278376179301,-3.19408537472255));
#78153=CARTESIAN_POINT('Ctrl Pts',(45.7425945920472,0.538914114265246,-3.17893818314863));
#78154=CARTESIAN_POINT('Ctrl Pts',(45.7487584822594,0.636740865088272,-3.15922120675755));
#78155=CARTESIAN_POINT('Ctrl Pts',(45.7549158454823,0.734464026436455,-3.13952510881958));
#78156=CARTESIAN_POINT('Ctrl Pts',(45.7610732087053,0.831379480143805,-3.11526893176137));
#78157=CARTESIAN_POINT('Ctrl Pts',(45.7672305719282,0.927032187966362,-3.08653995356845));
#78158=CARTESIAN_POINT('Ctrl Pts',(45.7733834376398,1.02261502835973,-3.05783195982955));
#78159=CARTESIAN_POINT('Ctrl Pts',(45.7795363033514,1.11693654188626,-3.02465778500215));
#78160=CARTESIAN_POINT('Ctrl Pts',(45.7856891690631,1.20955382030329,-2.98715535556652));
#78161=CARTESIAN_POINT('Ctrl Pts',(45.791839703765,1.30213601071674,-2.94966713390508));
#78162=CARTESIAN_POINT('Ctrl Pts',(45.7979902384669,1.39301484674711,-2.90785407867085));
#78163=CARTESIAN_POINT('Ctrl Pts',(45.8041407731688,1.48176532251175,-2.86190305417595));
#78164=CARTESIAN_POINT('Ctrl Pts',(45.8102906229476,1.57050591503006,-2.8159571467837));
#78165=CARTESIAN_POINT('Ctrl Pts',(45.8164404727265,1.65711823276217,-2.76587438599479));
#78166=CARTESIAN_POINT('Ctrl Pts',(45.8225903225053,1.74120080898654,-2.7118881439478));
#78167=CARTESIAN_POINT('Ctrl Pts',(45.8287411324445,1.8252965128092,-2.65789347316645));
#78168=CARTESIAN_POINT('Ctrl Pts',(45.8348919423837,1.90686132507393,-2.59999434532863));
#78169=CARTESIAN_POINT('Ctrl Pts',(45.8410427523229,1.98552262035817,-2.53846754687667));
#78170=CARTESIAN_POINT('Ctrl Pts',(45.847200140234,2.06426803981365,-2.4768749487082));
#78171=CARTESIAN_POINT('Ctrl Pts',(45.8533575281451,2.14010339879176,-2.41164720089274));
#78172=CARTESIAN_POINT('Ctrl Pts',(45.8595149160562,2.21268915701501,-2.3431014184043));
#78173=CARTESIAN_POINT('Ctrl Pts',(45.865675740332,2.28531542448442,-2.27451738133197));
#78174=CARTESIAN_POINT('Ctrl Pts',(45.8718365646079,2.35468817790787,-2.20261193445683));
#78175=CARTESIAN_POINT('Ctrl Pts',(45.8779973888838,2.4205062285847,-2.12773756837695));
#78176=CARTESIAN_POINT('Ctrl Pts',(45.8841685133135,2.4864343190907,-2.05273802140265));
#78177=CARTESIAN_POINT('Ctrl Pts',(45.8903396377433,2.5487955644018,-1.97475997983011));
#78178=CARTESIAN_POINT('Ctrl Pts',(45.896510762173,2.6073303120889,-1.89418747914835));
#78179=CARTESIAN_POINT('Ctrl Pts',(45.9012062685907,2.65186843258084,-1.83288119723041));
#78180=CARTESIAN_POINT('Ctrl Pts',(45.9059017750084,2.69419208812412,-1.77007352280184));
#78181=CARTESIAN_POINT('Ctrl Pts',(45.9105972814261,2.73420475130028,-1.70594312345604));
#78182=CARTESIAN_POINT('Ctrl Pts',(45.9167695260658,2.78680140943208,-1.62164369366314));
#78183=CARTESIAN_POINT('Ctrl Pts',(45.9229417707054,2.83558838376867,-1.53476116288655));
#78184=CARTESIAN_POINT('Ctrl Pts',(45.9291140153451,2.88030245554016,-1.44567469615724));
#78185=CARTESIAN_POINT('Ctrl Pts',(45.9352779005448,2.92495596837081,-1.35670888455627));
#78186=CARTESIAN_POINT('Ctrl Pts',(45.9414417857445,2.9655473495035,-1.26554545466496));
#78187=CARTESIAN_POINT('Ctrl Pts',(45.9476056709442,3.00185716622106,-1.17259162375794));
#78188=CARTESIAN_POINT('Ctrl Pts',(45.9537630291543,3.03812853417031,-1.07973622243914));
#78189=CARTESIAN_POINT('Ctrl Pts',(45.9599203873645,3.07012719412026,-0.985094591646198));
#78190=CARTESIAN_POINT('Ctrl Pts',(45.9660777455747,3.0976805212264,-0.889096705040859));
#78191=CARTESIAN_POINT('Ctrl Pts',(45.9722306062933,3.12521372267929,-0.793168937741693));
#78192=CARTESIAN_POINT('Ctrl Pts',(45.9783834670119,3.14830792737386,-0.695887300459184));
#78193=CARTESIAN_POINT('Ctrl Pts',(45.9845363277305,3.16683967523579,-0.597698949181347));
#78194=CARTESIAN_POINT('Ctrl Pts',(45.990686857453,3.18536440239079,-0.499547796317951));
#78195=CARTESIAN_POINT('Ctrl Pts',(45.9968373871755,3.19933002671357,-0.400491038370601));
#78196=CARTESIAN_POINT('Ctrl Pts',(46.002987916898,3.20866393505546,-0.300987232909302));
#78197=CARTESIAN_POINT('Ctrl Pts',(46.0091377617167,3.21799680400246,-0.201494507881113));
#78198=CARTESIAN_POINT('Ctrl Pts',(46.0152876065354,3.22269894183314,-0.101555266790161));
#78199=CARTESIAN_POINT('Ctrl Pts',(46.0214374513541,3.22274958606181,-0.00163341312231848));
#78200=CARTESIAN_POINT('Ctrl Pts',(46.0275882563582,3.22280023819765,0.0983040415088446));
#78201=CARTESIAN_POINT('Ctrl Pts',(46.0337390613623,3.21819795400046,0.198223668908126));
#78202=CARTESIAN_POINT('Ctrl Pts',(46.0398898663665,3.20897408626979,0.297662352589265));
#78203=CARTESIAN_POINT('Ctrl Pts',(46.0460472494114,3.19974035398008,0.397207381980745));
#78204=CARTESIAN_POINT('Ctrl Pts',(46.0522046324564,3.1858752084948,0.49627000718771));
#78205=CARTESIAN_POINT('Ctrl Pts',(46.0583620155014,3.16746181681086,0.594393137195634));
#78206=CARTESIAN_POINT('Ctrl Pts',(46.0645228349418,3.14903814873278,0.692571029084221));
#78207=CARTESIAN_POINT('Ctrl Pts',(46.0706836543823,3.12606127926863,0.789807958837698));
#78208=CARTESIAN_POINT('Ctrl Pts',(46.0768444738227,3.09866487079108,0.885659969189805));
#78209=CARTESIAN_POINT('Ctrl Pts',(46.0830155935174,3.07122265834579,0.981672234211558));
#78210=CARTESIAN_POINT('Ctrl Pts',(46.0891867132122,3.03934628630086,1.07629454297083));
#78211=CARTESIAN_POINT('Ctrl Pts',(46.0953578329069,3.00321841195402,1.1691008222563));
#78212=CARTESIAN_POINT('Ctrl Pts',(46.1000533886598,2.97572900053088,1.23971637991233));
#78213=CARTESIAN_POINT('Ctrl Pts',(46.1047489444128,2.94577916859904,1.30928090671977));
#78214=CARTESIAN_POINT('Ctrl Pts',(46.1094445001657,2.91346702293576,1.37761658989933));
#78215=CARTESIAN_POINT('Ctrl Pts',(46.1156164258726,2.87099533844129,1.46743828128314));
#78216=CARTESIAN_POINT('Ctrl Pts',(46.1217883515795,2.82429123049196,1.55545212808397));
#78217=CARTESIAN_POINT('Ctrl Pts',(46.1279602772864,2.77353130235211,1.64123175614324));
#78218=CARTESIAN_POINT('Ctrl Pts',(46.1341242044575,2.72283715677691,1.72690021769508));
#78219=CARTESIAN_POINT('Ctrl Pts',(46.1402881316286,2.66809785467939,1.81033984354182));
#78220=CARTESIAN_POINT('Ctrl Pts',(46.1464520587997,2.60953730348872,1.89114584953166));
#78221=CARTESIAN_POINT('Ctrl Pts',(46.1526088291193,2.55104474615357,1.97185803277248));
#78222=CARTESIAN_POINT('Ctrl Pts',(46.1587655994388,2.48874001847481,2.04994232885636));
#78223=CARTESIAN_POINT('Ctrl Pts',(46.1649223697583,2.42289139691823,2.12502113901007));
#78224=CARTESIAN_POINT('Ctrl Pts',(46.1710749117893,2.35708799825572,2.200048387248));
#78225=CARTESIAN_POINT('Ctrl Pts',(46.1772274538203,2.28774582815966,2.27207392623162));
#78226=CARTESIAN_POINT('Ctrl Pts',(46.1833799958513,2.21517422701285,2.34075216682118));
#78227=CARTESIAN_POINT('Ctrl Pts',(46.1895307545825,2.14262366057298,2.40941050118514));
#78228=CARTESIAN_POINT('Ctrl Pts',(46.1956815133137,2.06684583405016,2.47472316248043));
#78229=CARTESIAN_POINT('Ctrl Pts',(46.201832272045,1.98818725954731,2.53638108009695));
#78230=CARTESIAN_POINT('Ctrl Pts',(46.2068672570917,1.92379768360679,2.58685399031425));
#78231=CARTESIAN_POINT('Ctrl Pts',(46.2119022421384,1.85747849723844,2.63487846584619));
#78232=CARTESIAN_POINT('Ctrl Pts',(46.216937227185,1.78943621037807,2.68030513402631));
#78233=CARTESIAN_POINT('Ctrl Pts',(44.9670777766272,1.78943621037802,2.68030513402634));
#78234=CARTESIAN_POINT('Ctrl Pts',(44.9732498862039,1.70620866293451,2.73586984761275));
#78235=CARTESIAN_POINT('Ctrl Pts',(44.9794219957806,1.62031946228957,2.78760190383352));
#78236=CARTESIAN_POINT('Ctrl Pts',(44.9855941053572,1.53215912380563,2.83524354894587));
#78237=CARTESIAN_POINT('Ctrl Pts',(44.9917450764698,1.44430072003734,2.88272202922903));
#78238=CARTESIAN_POINT('Ctrl Pts',(44.9978960475824,1.35418709224094,2.92613786024936));
#78239=CARTESIAN_POINT('Ctrl Pts',(45.004047018695,1.26223192229211,2.96528044826232));
#78240=CARTESIAN_POINT('Ctrl Pts',(45.010196885273,1.17029326480371,3.00441600741071));
#78241=CARTESIAN_POINT('Ctrl Pts',(45.0163467518509,1.07651412203582,3.03927967864055));
#78242=CARTESIAN_POINT('Ctrl Pts',(45.0224966184289,0.981329333323888,3.06970850441179));
#78243=CARTESIAN_POINT('Ctrl Pts',(45.028647025688,0.886136176199941,3.1001400054104));
#78244=CARTESIAN_POINT('Ctrl Pts',(45.0347974329471,0.789537541579017,3.12613575451336));
#78245=CARTESIAN_POINT('Ctrl Pts',(45.0409478402062,0.691983679373301,3.14758258827008));
#78246=CARTESIAN_POINT('Ctrl Pts',(45.047136220728,0.593827509339862,3.16916183703898));
#78247=CARTESIAN_POINT('Ctrl Pts',(45.0533246012498,0.494704708546602,3.1861357026898));
#78248=CARTESIAN_POINT('Ctrl Pts',(45.0595129817715,0.395083056032114,3.19844132998189));
#78249=CARTESIAN_POINT('Ctrl Pts',(45.0656728078821,0.295921077517692,3.21069017667682));
#78250=CARTESIAN_POINT('Ctrl Pts',(45.0718326339927,0.196265281299825,3.21831379667311));
#78251=CARTESIAN_POINT('Ctrl Pts',(45.0779924601033,0.0965794774239169,
3.22130252646977));
#78252=CARTESIAN_POINT('Ctrl Pts',(45.0841951178307,-0.00379947980933119,
3.22431203804289));
#78253=CARTESIAN_POINT('Ctrl Pts',(45.0903977755581,-0.104208416453509,
3.22262196846568));
#78254=CARTESIAN_POINT('Ctrl Pts',(45.0966004332855,-0.20417794773934,3.2162756300039));
#78255=CARTESIAN_POINT('Ctrl Pts',(45.1028030910128,-0.304147479025172,
3.20992929154211));
#78256=CARTESIAN_POINT('Ctrl Pts',(45.1090057487402,-0.403677171599521,
3.19892679497133));
#78257=CARTESIAN_POINT('Ctrl Pts',(45.1152084064676,-0.502308418893908,
3.18336360078586));
#78258=CARTESIAN_POINT('Ctrl Pts',(45.1213806548032,-0.600456112787606,
3.16787670732334));
#78259=CARTESIAN_POINT('Ctrl Pts',(45.1275529031388,-0.69805966120469,3.14781924985067));
#78260=CARTESIAN_POINT('Ctrl Pts',(45.1337251514744,-0.794660154599542,
3.12324075299869));
#78261=CARTESIAN_POINT('Ctrl Pts',(45.1398890403708,-0.891129816259442,
3.09869554425191));
#78262=CARTESIAN_POINT('Ctrl Pts',(45.1460529292671,-0.986598705801894,
3.06964157264494));
#78263=CARTESIAN_POINT('Ctrl Pts',(45.1522168181635,-1.08061540399782,3.03617982193786));
#78264=CARTESIAN_POINT('Ctrl Pts',(45.1583741800664,-1.17453254712581,3.00275350415844));
#78265=CARTESIAN_POINT('Ctrl Pts',(45.1645315419692,-1.26700014910275,2.96492883142535));
#78266=CARTESIAN_POINT('Ctrl Pts',(45.1706889038721,-1.35758026182949,2.92285706034198));
#78267=CARTESIAN_POINT('Ctrl Pts',(45.1768417682625,-1.44809421226379,2.88081601967767));
#78268=CARTESIAN_POINT('Ctrl Pts',(45.182994632653,-1.53672302172453,2.83453423079885));
#78269=CARTESIAN_POINT('Ctrl Pts',(45.1891474970435,-1.62304796865347,2.7842113522414));
#78270=CARTESIAN_POINT('Ctrl Pts',(45.195298030424,-1.70934021141462,2.73390753848412));
#78271=CARTESIAN_POINT('Ctrl Pts',(45.2014485638045,-1.79332995107658,2.67956589558555));
#78272=CARTESIAN_POINT('Ctrl Pts',(45.207599097185,-1.87462316215416,2.62143196791661));
#78273=CARTESIAN_POINT('Ctrl Pts',(45.2137489456438,-1.95590732044119,2.56330451402652));
#78274=CARTESIAN_POINT('Ctrl Pts',(45.2198987941025,-2.03449519382623,2.50138586764527));
#78275=CARTESIAN_POINT('Ctrl Pts',(45.2260486425613,-2.11002268570649,2.43596425021057));
#78276=CARTESIAN_POINT('Ctrl Pts',(45.2321994511833,-2.18556196953902,2.37053241863305));
#78277=CARTESIAN_POINT('Ctrl Pts',(45.2383502598052,-2.25803959445055,2.30159681411835));
#78278=CARTESIAN_POINT('Ctrl Pts',(45.2445010684272,-2.32712619969376,2.22948451737142));
#78279=CARTESIAN_POINT('Ctrl Pts',(45.2506584550336,-2.39628668963083,2.15729510010381));
#78280=CARTESIAN_POINT('Ctrl Pts',(45.2568158416399,-2.46204861701465,2.0819225207886));
#78281=CARTESIAN_POINT('Ctrl Pts',(45.2629732282463,-2.52412111754724,2.00372906014064));
#78282=CARTESIAN_POINT('Ctrl Pts',(45.2691340512224,-2.58622826005899,1.92549196058316));
#78283=CARTESIAN_POINT('Ctrl Pts',(45.2752948741984,-2.64464162123501,1.84443119691035));
#78284=CARTESIAN_POINT('Ctrl Pts',(45.2814556971745,-2.69911333978492,1.76093859674183));
#78285=CARTESIAN_POINT('Ctrl Pts',(45.287626820326,-2.75367612867754,1.67730640671066));
#78286=CARTESIAN_POINT('Ctrl Pts',(45.2937979434775,-2.8042838914251,1.59123463360137));
#78287=CARTESIAN_POINT('Ctrl Pts',(45.2999690666291,-2.85073437580245,1.50314040632212));
#78288=CARTESIAN_POINT('Ctrl Pts',(45.3046645861551,-2.88607788638083,1.43611076614776));
#78289=CARTESIAN_POINT('Ctrl Pts',(45.3093601056811,-2.9190154984685,1.36791075557459));
#78290=CARTESIAN_POINT('Ctrl Pts',(45.3140556252071,-2.94947714083506,1.29873097991518));
#78291=CARTESIAN_POINT('Ctrl Pts',(45.3209321105432,-2.99408754781707,1.19741871611951));
#78292=CARTESIAN_POINT('Ctrl Pts',(45.3278085958793,-3.03352293723517,1.09369460885342));
#78293=CARTESIAN_POINT('Ctrl Pts',(45.3346850812154,-3.06754223427876,0.98808005921386));
#78294=CARTESIAN_POINT('Ctrl Pts',(45.3414563185369,-3.10104084912839,0.88408199257659));
#78295=CARTESIAN_POINT('Ctrl Pts',(45.3482275558585,-3.12928783886883,0.778251211611842));
#78296=CARTESIAN_POINT('Ctrl Pts',(45.35499879318,-3.15209929248381,0.671109240603247));
#78297=CARTESIAN_POINT('Ctrl Pts',(45.3619279025234,-3.1754425972411,0.561469244671201));
#78298=CARTESIAN_POINT('Ctrl Pts',(45.3688570118668,-3.19309357957785,0.450456397961443));
#78299=CARTESIAN_POINT('Ctrl Pts',(45.3757861212102,-3.20490764928325,0.338651032872615));
#78300=CARTESIAN_POINT('Ctrl Pts',(45.3827152305536,-3.21672171898867,0.226845667783756));
#78301=CARTESIAN_POINT('Ctrl Pts',(45.389644339897,-3.22269871422779,0.11424808868431));
#78302=CARTESIAN_POINT('Ctrl Pts',(45.3965734492404,-3.22274967111447,0.00145596415041658));
#78303=CARTESIAN_POINT('',(45.1500265507268,-3.22274935820264,0.00203388900681504));
#78304=CARTESIAN_POINT('Ctrl Pts',(44.7203641905528,1.78943621037803,2.68030513402633));
#78305=CARTESIAN_POINT('Ctrl Pts',(44.7235369804355,1.74688407618643,2.70871396285133));
#78306=CARTESIAN_POINT('Ctrl Pts',(44.7267097703181,1.70368994908445,2.73608605417297));
#78307=CARTESIAN_POINT('Ctrl Pts',(44.7298825602008,1.65990979412347,2.76239335321257));
#78308=CARTESIAN_POINT('Ctrl Pts',(44.7360548082891,1.57474122395254,2.81357076558717));
#78309=CARTESIAN_POINT('Ctrl Pts',(44.7422270563773,1.48705372016049,2.86089576058143));
#78310=CARTESIAN_POINT('Ctrl Pts',(44.7483993044656,1.39723080362417,2.9041115067958));
#78311=CARTESIAN_POINT('Ctrl Pts',(44.7545631931136,1.30752953957013,2.94726872337204));
#78312=CARTESIAN_POINT('Ctrl Pts',(44.7607270817616,1.21569899915141,2.986327566344));
#78313=CARTESIAN_POINT('Ctrl Pts',(44.7668909704096,1.12215001817333,3.02107545407486));
#78314=CARTESIAN_POINT('Ctrl Pts',(44.7730483320635,1.02870009700774,3.05578654697153));
#78315=CARTESIAN_POINT('Ctrl Pts',(44.7792056937173,0.933535757908711,3.08619560967981));
#78316=CARTESIAN_POINT('Ctrl Pts',(44.7853630553712,0.837089805889483,3.11213724301739));
#78317=CARTESIAN_POINT('Ctrl Pts',(44.7915159195127,0.740714300740688,3.13805992784709));
#78318=CARTESIAN_POINT('Ctrl Pts',(44.7976687836542,0.643059462053335,3.15952155849571));
#78319=CARTESIAN_POINT('Ctrl Pts',(44.8038216477957,0.544574451297885,3.17640618144053));
#78320=CARTESIAN_POINT('Ctrl Pts',(44.8099721809274,0.446126751544787,3.19328440765349));
#78321=CARTESIAN_POINT('Ctrl Pts',(44.8161227140591,0.346849932307474,3.20558899828749));
#78322=CARTESIAN_POINT('Ctrl Pts',(44.8222732471908,0.247203703415233,3.21325503057535));
#78323=CARTESIAN_POINT('Ctrl Pts',(44.8284230954011,0.14756857109483,3.22092020917633));
#78324=CARTESIAN_POINT('Ctrl Pts',(44.8345729436113,0.047564544002484,3.22394782308566));
#78325=CARTESIAN_POINT('Ctrl Pts',(44.8407227918216,-0.0523441912946446,
3.22232488246262));
#78326=CARTESIAN_POINT('Ctrl Pts',(44.8468736001958,-0.15226852514893,3.220701688453));
#78327=CARTESIAN_POINT('Ctrl Pts',(44.85302440857,-0.252097103298146,3.2144265047803));
#78328=CARTESIAN_POINT('Ctrl Pts',(44.8591752169442,-0.351367398917399,
3.20353843639779));
#78329=CARTESIAN_POINT('Ctrl Pts',(44.8653326033054,-0.450743859234878,
3.19263872376172));
#78330=CARTESIAN_POINT('Ctrl Pts',(44.8714899896666,-0.549560412136144,
3.1771163226696));
#78331=CARTESIAN_POINT('Ctrl Pts',(44.8776473760278,-0.647361423232053,
3.1570620440864));
#78332=CARTESIAN_POINT('Ctrl Pts',(44.8838081987597,-0.745217016014586,
3.13699657342719));
#78333=CARTESIAN_POINT('Ctrl Pts',(44.8899690214916,-0.84205551727638,3.11239429538733));
#78334=CARTESIAN_POINT('Ctrl Pts',(44.8961298442235,-0.937435270241421,
3.08339628925758));
#78335=CARTESIAN_POINT('Ctrl Pts',(44.9023009671352,-1.03297448707043,3.0543498018311));
#78336=CARTESIAN_POINT('Ctrl Pts',(44.9084720900469,-1.12704967460522,3.02089305223879));
#78337=CARTESIAN_POINT('Ctrl Pts',(44.9146432129585,-1.21923787819585,2.98321580829689));
#78338=CARTESIAN_POINT('Ctrl Pts',(44.9193387349525,-1.28938260610739,2.95454771496364));
#78339=CARTESIAN_POINT('Ctrl Pts',(44.9240342569465,-1.35843525740968,2.92343718470311));
#78340=CARTESIAN_POINT('Ctrl Pts',(44.9287297789405,-1.42621969123783,2.88998528626453));
#78341=CARTESIAN_POINT('Ctrl Pts',(44.9349020270704,-1.51532210529602,2.84601287641504));
#78342=CARTESIAN_POINT('Ctrl Pts',(44.9410742752002,-1.60254584467215,2.79783847557569));
#78343=CARTESIAN_POINT('Ctrl Pts',(44.94724652333,-1.68746748683512,2.74564583356528));
#78344=CARTESIAN_POINT('Ctrl Pts',(44.9534104120199,-1.77227411460465,2.6935238791312));
#78345=CARTESIAN_POINT('Ctrl Pts',(44.9595743007097,-1.85478447545235,2.63739472582188));
#78346=CARTESIAN_POINT('Ctrl Pts',(44.9657381893995,-1.93459760068094,2.577489027317));
#78347=CARTESIAN_POINT('Ctrl Pts',(44.9718955510953,-2.01432621111425,2.5176467634644));
#78348=CARTESIAN_POINT('Ctrl Pts',(44.9780529127911,-2.09136291868725,2.45403616415223));
#78349=CARTESIAN_POINT('Ctrl Pts',(44.9842102744869,-2.1653345660287,2.38693187578978));
#78350=CARTESIAN_POINT('Ctrl Pts',(44.9903631386704,-2.23925218237269,2.31987660231025));
#78351=CARTESIAN_POINT('Ctrl Pts',(44.9965160028539,-2.31010886886649,2.24933300434687));
#78352=CARTESIAN_POINT('Ctrl Pts',(45.0026688670374,-2.37756421816483,2.17561622328072));
#78353=CARTESIAN_POINT('Ctrl Pts',(45.0088194002111,-2.44499401203456,2.10192736978378));
#78354=CARTESIAN_POINT('Ctrl Pts',(45.0149699333847,-2.50902473622744,2.02506804196943));
#78355=CARTESIAN_POINT('Ctrl Pts',(45.0211204665584,-2.5693532073192,1.94538984744409));
#78356=CARTESIAN_POINT('Ctrl Pts',(45.0272703148107,-2.62967496025157,1.8657205258572));
#78357=CARTESIAN_POINT('Ctrl Pts',(45.0334201630629,-2.68629501755139,1.78323330796266));
#78358=CARTESIAN_POINT('Ctrl Pts',(45.0395700113152,-2.73895146161718,1.69831164790362));
#78359=CARTESIAN_POINT('Ctrl Pts',(45.0457208197312,-2.79161612683074,1.61337672919166));
#78360=CARTESIAN_POINT('Ctrl Pts',(45.0518716281473,-2.84031572072484,1.52600698257051));
#78361=CARTESIAN_POINT('Ctrl Pts',(45.0580224365633,-2.88483304574274,1.43661263418177));
#78362=CARTESIAN_POINT('Ctrl Pts',(45.064179822966,-2.92939797984685,1.34712268294094));
#78363=CARTESIAN_POINT('Ctrl Pts',(45.0703372093687,-2.9697715194839,1.25560419581561));
#78364=CARTESIAN_POINT('Ctrl Pts',(45.0764945957713,-3.0057836894657,1.16248955893889));
#78365=CARTESIAN_POINT('Ctrl Pts',(45.0826554185446,-3.04181595744911,1.06932295579293));
#78366=CARTESIAN_POINT('Ctrl Pts',(45.0888162413179,-3.07348187076344,0.974558840888284));
#78367=CARTESIAN_POINT('Ctrl Pts',(45.0949770640911,-3.10066129822277,0.878645022863892));
#78368=CARTESIAN_POINT('Ctrl Pts',(45.1011481870434,-3.1278861665233,0.782570848092476));
#78369=CARTESIAN_POINT('Ctrl Pts',(45.1073193099957,-3.15060946728607,0.685343553900044));
#78370=CARTESIAN_POINT('Ctrl Pts',(45.113490432948,-3.16876213897789,0.587421542914688));
#78371=CARTESIAN_POINT('Ctrl Pts',(45.1181859545254,-3.18257425425655,0.512914047433577));
#78372=CARTESIAN_POINT('Ctrl Pts',(45.1228814761028,-3.19374127328364,0.43800456595355));
#78373=CARTESIAN_POINT('Ctrl Pts',(45.1275769976802,-3.202252974824,0.362895918592192));
#78374=CARTESIAN_POINT('Ctrl Pts',(45.135060182029,-3.2158179495982,0.243196361229775));
#78375=CARTESIAN_POINT('Ctrl Pts',(45.1425433663779,-3.22267319133973,0.122722239128668));
#78376=CARTESIAN_POINT('Ctrl Pts',(45.1500265507268,-3.22274935820264,0.00203388900681504));
#78377=CARTESIAN_POINT('Ctrl Pts',(45.1500283205554,-3.22644826576858,0.00200764693452582));
#78378=CARTESIAN_POINT('Ctrl Pts',(45.2088269525103,-3.21944509740503,-0.947386556412211));
#78379=CARTESIAN_POINT('Ctrl Pts',(45.3339079907115,-2.27377397144541,-2.97911589626085));
#78380=CARTESIAN_POINT('Ctrl Pts',(45.5252714351595,1.18232080972543,-3.62362621122949));
#78381=CARTESIAN_POINT('Ctrl Pts',(45.724118653899,3.68751965146775,-0.964753018247734));
#78382=CARTESIAN_POINT('Ctrl Pts',(45.8725610992789,3.02903273905734,1.68169936845078));
#78383=CARTESIAN_POINT('Ctrl Pts',(45.9547211384122,2.00465334780378,2.53949398247757));
#78384=CARTESIAN_POINT('Ctrl Pts',(45.9705987712989,1.78932308991422,2.68012452748182));
#78385=CARTESIAN_POINT('Origin',(-1.72497344927317,0.,0.));
#78386=CARTESIAN_POINT('',(47.4668462457454,1.78943621037804,2.68030513402633));
#78387=CARTESIAN_POINT('',(47.2204000228944,1.78943621037803,2.68030513402633));
#78388=CARTESIAN_POINT('',(-1.72497344927317,1.78943621037804,2.68030513402633));
#78389=CARTESIAN_POINT('',(46.64657344933,-3.22274878923343,-0.00279356304438793));
#78390=CARTESIAN_POINT('Ctrl Pts',(46.64657344933,-3.22274878923343,-0.00279356304438944));
#78391=CARTESIAN_POINT('Ctrl Pts',(46.6539949073187,-3.22264437215106,-0.123252640009857));
#78392=CARTESIAN_POINT('Ctrl Pts',(46.6614163653074,-3.21578244460685,-0.243415722663157));
#78393=CARTESIAN_POINT('Ctrl Pts',(46.668837823296,-3.20228492487645,-0.362613875091683));
#78394=CARTESIAN_POINT('Ctrl Pts',(46.6763621523232,-3.18860031200701,-0.483464268594949));
#78395=CARTESIAN_POINT('Ctrl Pts',(46.6838864813503,-3.16809494364444,-0.603322798527606));
#78396=CARTESIAN_POINT('Ctrl Pts',(46.6914108103774,-3.14094482293906,-0.721514505573045));
#78397=CARTESIAN_POINT('Ctrl Pts',(46.6962692590465,-3.123414028189,-0.797830724563636));
#78398=CARTESIAN_POINT('Ctrl Pts',(46.7011277077156,-3.10311384349577,-0.873452451264103));
#78399=CARTESIAN_POINT('Ctrl Pts',(46.7059861563847,-3.08010212327673,-0.948202759269441));
#78400=CARTESIAN_POINT('Ctrl Pts',(46.7121584215066,-3.05086759847718,-1.04316696500268));
#78401=CARTESIAN_POINT('Ctrl Pts',(46.7183306866286,-3.01718566831026,-1.13694503262286));
#78402=CARTESIAN_POINT('Ctrl Pts',(46.7245029517505,-2.97917036856004,-1.22908969469027));
#78403=CARTESIAN_POINT('Ctrl Pts',(46.7306668572702,-2.94120655603203,-1.32110955772356));
#78404=CARTESIAN_POINT('Ctrl Pts',(46.7368307627898,-2.89892120347925,-1.41150001429682));
#78405=CARTESIAN_POINT('Ctrl Pts',(46.7429946683095,-2.85247822575668,-1.49982850155744));
#78406=CARTESIAN_POINT('Ctrl Pts',(46.7491520466541,-2.80608442812754,-1.58806345469366));
#78407=CARTESIAN_POINT('Ctrl Pts',(46.7553094249986,-2.75554195926,-1.67424039715845));
#78408=CARTESIAN_POINT('Ctrl Pts',(46.7614668033431,-2.70106259151513,-1.75794722310358));
#78409=CARTESIAN_POINT('Ctrl Pts',(46.7676196838393,-2.64662301991724,-1.84159290279672));
#78410=CARTESIAN_POINT('Ctrl Pts',(46.7737725643356,-2.58825250331351,-1.92277169041361));
#78411=CARTESIAN_POINT('Ctrl Pts',(46.7799254448318,-2.5262080042061,-2.00109736944134));
#78412=CARTESIAN_POINT('Ctrl Pts',(46.7860759941076,-2.46418701269018,-2.07939337221908));
#78413=CARTESIAN_POINT('Ctrl Pts',(46.7922265433834,-2.3984950739998,-2.15483807422403));
#78414=CARTESIAN_POINT('Ctrl Pts',(46.7983770926592,-2.32943107527019,-2.22707620616483));
#78415=CARTESIAN_POINT('Ctrl Pts',(46.8045269567858,-2.26037477002374,-2.29930629103537));
#78416=CARTESIAN_POINT('Ctrl Pts',(46.8106768209123,-2.18794745172932,-2.36833020203992));
#78417=CARTESIAN_POINT('Ctrl Pts',(46.8168266850389,-2.11248601448805,-2.43382834256905));
#78418=CARTESIAN_POINT('Ctrl Pts',(46.822977509084,-2.0370127986402,-2.4993367065561));
#78419=CARTESIAN_POINT('Ctrl Pts',(46.829128333129,-1.95850485124619,-2.56131792221652));
#78420=CARTESIAN_POINT('Ctrl Pts',(46.8352791571741,-1.87733261314578,-2.61949228327156));
#78421=CARTESIAN_POINT('Ctrl Pts',(46.8414365587323,-1.7960735718044,-2.67772885430379));
#78422=CARTESIAN_POINT('Ctrl Pts',(46.8475939602905,-1.71214490411932,-2.73215018795683));
#78423=CARTESIAN_POINT('Ctrl Pts',(46.8537513618487,-1.62594644257923,-2.78251967259244));
#78424=CARTESIAN_POINT('Ctrl Pts',(46.8599121995386,-1.53969987807459,-2.83291726586816));
#78425=CARTESIAN_POINT('Ctrl Pts',(46.8660730372286,-1.45118138202589,-2.87925830564476));
#78426=CARTESIAN_POINT('Ctrl Pts',(46.8722338749185,-1.36081394415636,-2.92135293518082));
#78427=CARTESIAN_POINT('Ctrl Pts',(46.8784050122434,-1.27029543078865,-2.96351793815314));
#78428=CARTESIAN_POINT('Ctrl Pts',(46.8845761495683,-1.1779222033766,-3.00142218565318));
#78429=CARTESIAN_POINT('Ctrl Pts',(46.8907472868932,-1.08413583688106,-3.03492455420068));
#78430=CARTESIAN_POINT('Ctrl Pts',(46.8954426496369,-1.01277767582838,-3.06041511855229));
#78431=CARTESIAN_POINT('Ctrl Pts',(46.9001380123805,-0.940601824703771,
-3.08335842016347));
#78432=CARTESIAN_POINT('Ctrl Pts',(46.9048333751242,-0.86780687241381,-3.10371209919531));
#78433=CARTESIAN_POINT('Ctrl Pts',(46.911005680367,-0.772114017528194,-3.130468097966));
#78434=CARTESIAN_POINT('Ctrl Pts',(46.9171779856098,-0.675014195943398,
-3.15284147084316));
#78435=CARTESIAN_POINT('Ctrl Pts',(46.9233502908525,-0.57694532063497,-3.17068630733118));
#78436=CARTESIAN_POINT('Ctrl Pts',(46.9295142370435,-0.479009258395676,
-3.18850697684986));
#78437=CARTESIAN_POINT('Ctrl Pts',(46.9356781832346,-0.38010717450795,-3.20181122276752));
#78438=CARTESIAN_POINT('Ctrl Pts',(46.9418421294256,-0.280691581725667,
-3.21050304445399));
#78439=CARTESIAN_POINT('Ctrl Pts',(46.9479995489326,-0.181381254976336,
-3.21918566281971));
#78440=CARTESIAN_POINT('Ctrl Pts',(46.9541569684395,-0.0815589306455282,
-3.22326552890595));
#78441=CARTESIAN_POINT('Ctrl Pts',(46.9603143879465,0.0183142107331389,
-3.22269796167516));
#78442=CARTESIAN_POINT('Ctrl Pts',(46.9664673101688,0.118114406301845,-3.22213080898676));
#78443=CARTESIAN_POINT('Ctrl Pts',(46.9726202323911,0.217964912075569,-3.21692297412134));
#78444=CARTESIAN_POINT('Ctrl Pts',(46.9787731546133,0.31740189162692,-3.20708178905554));
#78445=CARTESIAN_POINT('Ctrl Pts',(46.9849237459473,0.416801201843157,-3.19724433208867));
#78446=CARTESIAN_POINT('Ctrl Pts',(46.9910743372813,0.515786865334471,-3.18277705529739));
#78447=CARTESIAN_POINT('Ctrl Pts',(46.9972249286153,0.613898410160742,-3.16373929148755));
#78448=CARTESIAN_POINT('Ctrl Pts',(47.003374835081,0.711999030267057,-3.14470364753259));
#78449=CARTESIAN_POINT('Ctrl Pts',(47.0095247415466,0.809225298807935,-3.12109861111653));
#78450=CARTESIAN_POINT('Ctrl Pts',(47.0156746480123,0.905126201654985,-3.0930347753586));
#78451=CARTESIAN_POINT('Ctrl Pts',(47.0218255146265,1.00104207694248,-3.06496655816007));
#78452=CARTESIAN_POINT('Ctrl Pts',(47.0279763812407,1.09563175861427,-3.03243828093851));
#78453=CARTESIAN_POINT('Ctrl Pts',(47.0341272478549,1.18845964986827,-2.99561032564901));
#78454=CARTESIAN_POINT('Ctrl Pts',(47.0402846920712,1.28138680923835,-2.95874298734984));
#78455=CARTESIAN_POINT('Ctrl Pts',(47.0464421362876,1.37254801145771,-2.91756694978181));
#78456=CARTESIAN_POINT('Ctrl Pts',(47.052599580504,1.46152801916254,-2.87229062103799));
#78457=CARTESIAN_POINT('Ctrl Pts',(47.0587604609681,1.55055768340403,-2.82698902520625));
#78458=CARTESIAN_POINT('Ctrl Pts',(47.0649213414323,1.63740335144169,-2.77758279601963));
#78459=CARTESIAN_POINT('Ctrl Pts',(47.0710822218965,1.72167659529636,-2.72432510242605));
#78460=CARTESIAN_POINT('Ctrl Pts',(47.0772534017357,1.80609072189543,-2.67097837594742));
#78461=CARTESIAN_POINT('Ctrl Pts',(47.0834245815749,1.88792347819824,-2.61376757307797));
#78462=CARTESIAN_POINT('Ctrl Pts',(47.0895957614142,1.96681738192434,-2.55298784733894));
#78463=CARTESIAN_POINT('Ctrl Pts',(47.0942907055641,2.02683872004956,-2.506747513201));
#78464=CARTESIAN_POINT('Ctrl Pts',(47.098985649714,2.08515970847106,-2.45844237546095));
#78465=CARTESIAN_POINT('Ctrl Pts',(47.1036805938639,2.14163737351416,-2.40821654401496));
#78466=CARTESIAN_POINT('Ctrl Pts',(47.1098526614097,2.2158840423445,-2.34218866075789));
#78467=CARTESIAN_POINT('Ctrl Pts',(47.1160247289555,2.28720506002567,-2.272607706105));
#78468=CARTESIAN_POINT('Ctrl Pts',(47.1221967965013,2.35524091165208,-2.19976312601614));
#78469=CARTESIAN_POINT('Ctrl Pts',(47.1283605043972,2.42318461329789,-2.12701720900684));
#78470=CARTESIAN_POINT('Ctrl Pts',(47.134524212293,2.48785169891878,-2.05101676717502));
#78471=CARTESIAN_POINT('Ctrl Pts',(47.1406879201888,2.54891674199184,-1.97209051640479));
#78472=CARTESIAN_POINT('Ctrl Pts',(47.1468451011119,2.60991712108668,-1.89324784349029));
#78473=CARTESIAN_POINT('Ctrl Pts',(47.153002282035,2.66732277651969,-1.81148586291148));
#78474=CARTESIAN_POINT('Ctrl Pts',(47.1591594629581,2.72084676406627,-1.7271683325519));
#78475=CARTESIAN_POINT('Ctrl Pts',(47.1653121471282,2.77433166162168,-1.64291238152653));
#78476=CARTESIAN_POINT('Ctrl Pts',(47.1714648312984,2.82394029540775,-1.55610495705118));
#78477=CARTESIAN_POINT('Ctrl Pts',(47.1776175154685,2.86942803792344,-1.4671401765608));
#78478=CARTESIAN_POINT('Ctrl Pts',(47.1837678691481,2.91489855076353,-1.37820909381452));
#78479=CARTESIAN_POINT('Ctrl Pts',(47.1899182228278,2.95625107627835,-1.28712266508161));
#78480=CARTESIAN_POINT('Ctrl Pts',(47.1960685765074,2.9932865491922,-1.19430029595786));
#78481=CARTESIAN_POINT('Ctrl Pts',(47.2022182459899,3.03031790208839,-1.1014882528748));
#78482=CARTESIAN_POINT('Ctrl Pts',(47.2083679154724,3.06303299620828,-1.00694105681462));
#78483=CARTESIAN_POINT('Ctrl Pts',(47.2145175849548,3.09128100061009,-0.911097874965736));
#78484=CARTESIAN_POINT('Ctrl Pts',(47.2206682155309,3.11953341971699,-0.815239714381489));
#78485=CARTESIAN_POINT('Ctrl Pts',(47.226818846107,3.14331723961166,-0.718085582430075));
#78486=CARTESIAN_POINT('Ctrl Pts',(47.2329694766831,3.16253184843985,-0.620088598591862));
#78487=CARTESIAN_POINT('Ctrl Pts',(47.239126687776,3.18176701484419,-0.521986768463238));
#78488=CARTESIAN_POINT('Ctrl Pts',(47.2452838988689,3.19642312447634,-0.423040712841666));
#78489=CARTESIAN_POINT('Ctrl Pts',(47.2514411099618,3.20645097407994,-0.323712392907326));
#78490=CARTESIAN_POINT('Ctrl Pts',(47.2576017585541,3.21648442211546,-0.224328619126176));
#78491=CARTESIAN_POINT('Ctrl Pts',(47.2637624071464,3.22188444084847,-0.124562589804339));
#78492=CARTESIAN_POINT('Ctrl Pts',(47.2699230557388,3.22265397643253,-0.0248779155799095));
#78493=CARTESIAN_POINT('Ctrl Pts',(47.2760940081682,3.22342479908389,0.0749734837283165));
#78494=CARTESIAN_POINT('Ctrl Pts',(47.2822649605977,3.21954968586724,0.174742821869841));
#78495=CARTESIAN_POINT('Ctrl Pts',(47.2884359130272,3.21108363338839,0.273969819296283));
#78496=CARTESIAN_POINT('Ctrl Pts',(47.293133212886,3.20463931420627,0.349500941327117));
#78497=CARTESIAN_POINT('Ctrl Pts',(47.2978305127448,3.19553599947028,0.424717890956712));
#78498=CARTESIAN_POINT('Ctrl Pts',(47.3025278126036,3.18381768600742,0.499422170879856));
#78499=CARTESIAN_POINT('Ctrl Pts',(47.3087009908281,3.16841751150901,0.597598324832455));
#78500=CARTESIAN_POINT('Ctrl Pts',(47.3148741690525,3.14844493899141,0.695234285421411));
#78501=CARTESIAN_POINT('Ctrl Pts',(47.321047347277,3.12394910720187,0.791870910005332));
#78502=CARTESIAN_POINT('Ctrl Pts',(47.3272102069154,3.09949422066611,0.888346004613346));
#78503=CARTESIAN_POINT('Ctrl Pts',(47.3333730665538,3.07053122456943,0.983824669490771));
#78504=CARTESIAN_POINT('Ctrl Pts',(47.3395359261922,3.03716064498571,1.07785563924396));
#78505=CARTESIAN_POINT('Ctrl Pts',(47.3456928862413,3.0038220104287,1.17179659492251));
#78506=CARTESIAN_POINT('Ctrl Pts',(47.3518498462903,2.96608431985286,1.2642922021938));
#78507=CARTESIAN_POINT('Ctrl Pts',(47.3580068063394,2.92409839401049,1.35490447805196));
#78508=CARTESIAN_POINT('Ctrl Pts',(47.3641595193605,2.88214142976529,1.44545425019778));
#78509=CARTESIAN_POINT('Ctrl Pts',(47.3703122323817,2.83594223626957,1.53412288007275));
#78510=CARTESIAN_POINT('Ctrl Pts',(47.3764649454029,2.78570006155276,1.6204915086371));
#78511=CARTESIAN_POINT('Ctrl Pts',(47.3826150599722,2.73547910542274,1.70682366146664));
#78512=CARTESIAN_POINT('Ctrl Pts',(47.3887651745415,2.68121878132588,1.79085736956817));
#78513=CARTESIAN_POINT('Ctrl Pts',(47.3949152891108,2.62316420412631,1.87219847256919));
#78514=CARTESIAN_POINT('Ctrl Pts',(47.4010666547556,2.56509781728333,1.95355612223142));
#78515=CARTESIAN_POINT('Ctrl Pts',(47.4072180204003,2.50323587876763,2.03221971234551));
#78516=CARTESIAN_POINT('Ctrl Pts',(47.4133693860451,2.43786647152331,2.10782462020029));
#78517=CARTESIAN_POINT('Ctrl Pts',(47.4195211257958,2.3724930887261,2.18343412609752));
#78518=CARTESIAN_POINT('Ctrl Pts',(47.4256728655465,2.30361210310448,2.25598425601033));
#78519=CARTESIAN_POINT('Ctrl Pts',(47.4318246052971,2.2315504287417,2.32514520976276));
#78520=CARTESIAN_POINT('Ctrl Pts',(47.4379822105324,2.15942004590611,2.39437210624486));
#78521=CARTESIAN_POINT('Ctrl Pts',(47.4441398157677,2.08410323496244,2.46020307499644));
#78522=CARTESIAN_POINT('Ctrl Pts',(47.450297421003,2.00596203592081,2.52234689782045));
#78523=CARTESIAN_POINT('Ctrl Pts',(47.4558136959171,1.93595944245132,2.57801828268711));
#78524=CARTESIAN_POINT('Ctrl Pts',(47.4613299708313,1.86369079257126,2.63073098797996));
#78525=CARTESIAN_POINT('Ctrl Pts',(47.4668462457454,1.78943621037804,2.68030513402633));
#78526=CARTESIAN_POINT('Ctrl Pts',(46.216937227185,1.78943621037807,2.68030513402631));
#78527=CARTESIAN_POINT('Ctrl Pts',(46.2230877404723,1.70631878588743,2.73579632687922));
#78528=CARTESIAN_POINT('Ctrl Pts',(46.2292382537596,1.62062966051722,2.78740969530876));
#78529=CARTESIAN_POINT('Ctrl Pts',(46.2353887670468,1.53277076357632,2.8349129349639));
#78530=CARTESIAN_POINT('Ctrl Pts',(46.2415456899858,1.4448203059963,2.88246567930366));
#78531=CARTESIAN_POINT('Ctrl Pts',(46.2477026129248,1.35469594328053,2.92589953232438));
#78532=CARTESIAN_POINT('Ctrl Pts',(46.2538595358637,1.26282357950996,2.96502852760874));
#78533=CARTESIAN_POINT('Ctrl Pts',(46.2600196269283,1.17090394160692,3.00417765723199));
#78534=CARTESIAN_POINT('Ctrl Pts',(46.2661797179928,1.07723491838889,3.03901736522023));
#78535=CARTESIAN_POINT('Ctrl Pts',(46.2723398090574,0.982259737026324,3.06941091604187));
#78536=CARTESIAN_POINT('Ctrl Pts',(46.2785105450889,0.887120433469441,3.09985698854531));
#78537=CARTESIAN_POINT('Ctrl Pts',(46.2846812811204,0.79067088188869,3.12584143853654));
#78538=CARTESIAN_POINT('Ctrl Pts',(46.2908520171519,0.693366991542634,3.14727815382421));
#78539=CARTESIAN_POINT('Ctrl Pts',(46.2966652510697,0.601700410310481,3.16747293119929));
#78540=CARTESIAN_POINT('Ctrl Pts',(46.3024784849875,0.50927600227785,3.18363207842856));
#78541=CARTESIAN_POINT('Ctrl Pts',(46.3082917189053,0.416478177357678,3.19572581588046));
#78542=CARTESIAN_POINT('Ctrl Pts',(46.3144639766131,0.317949183302638,3.20856645936026));
#78543=CARTESIAN_POINT('Ctrl Pts',(46.3206362343209,0.218652370678122,3.21686874010675));
#78544=CARTESIAN_POINT('Ctrl Pts',(46.3268084920286,0.119041973504201,3.22055066270416));
#78545=CARTESIAN_POINT('Ctrl Pts',(46.3329723903487,0.0195664835174384,
3.22422759869541));
#78546=CARTESIAN_POINT('Ctrl Pts',(46.3391362886688,-0.0802213166197347,
3.2232965982539));
#78547=CARTESIAN_POINT('Ctrl Pts',(46.3453001869889,-0.179859856710437,
3.21772714729576));
#78548=CARTESIAN_POINT('Ctrl Pts',(46.3514575583544,-0.279392889507493,
3.21216359383167));
#78549=CARTESIAN_POINT('Ctrl Pts',(46.3576149297198,-0.3787765451741,3.20197137879874));
#78550=CARTESIAN_POINT('Ctrl Pts',(46.3637723010853,-0.477547989810642,
3.18717201919316));
#78551=CARTESIAN_POINT('Ctrl Pts',(46.3699251749581,-0.576247289400351,
3.172383469397));
#78552=CARTESIAN_POINT('Ctrl Pts',(46.376078048831,-0.674334838734504,3.15299452973312));
#78553=CARTESIAN_POINT('Ctrl Pts',(46.3822309227038,-0.771352589650201,
3.12907857762312));
#78554=CARTESIAN_POINT('Ctrl Pts',(46.3883814655759,-0.868333585635746,
3.10517168601124));
#78555=CARTESIAN_POINT('Ctrl Pts',(46.394532008448,-0.964245167232633,3.07674129359341));
#78556=CARTESIAN_POINT('Ctrl Pts',(46.4006825513201,-1.05864002926922,3.04391176792772));
#78557=CARTESIAN_POINT('Ctrl Pts',(46.4068324092684,-1.15302437950546,3.01108589815402));
#78558=CARTESIAN_POINT('Ctrl Pts',(46.4129822672168,-1.245891935713,2.97386201178683));
#78559=CARTESIAN_POINT('Ctrl Pts',(46.4191321251652,-1.33681206134223,2.93241386491572));
#78560=CARTESIAN_POINT('Ctrl Pts',(46.4252829432638,-1.42774638192961,2.89095924692827));
#78561=CARTESIAN_POINT('Ctrl Pts',(46.4314337613623,-1.51673227275081,2.84527923866662));
#78562=CARTESIAN_POINT('Ctrl Pts',(46.4375845794609,-1.60336145485579,2.79559467870125));
#78563=CARTESIAN_POINT('Ctrl Pts',(46.4437419754652,-1.69008328131795,2.74585698428386));
#78564=CARTESIAN_POINT('Ctrl Pts',(46.4498993714694,-1.77444298865255,2.69210640275822));
#78565=CARTESIAN_POINT('Ctrl Pts',(46.4560567674737,-1.85605929590869,2.63460840592505));
#78566=CARTESIAN_POINT('Ctrl Pts',(46.4622175998187,-1.93772115187402,2.57707832041226));
#78567=CARTESIAN_POINT('Ctrl Pts',(46.4683784321636,-2.01663621561404,2.5157969210819));
#78568=CARTESIAN_POINT('Ctrl Pts',(46.4745392645086,-2.09245612288099,2.45107016144334));
#78569=CARTESIAN_POINT('Ctrl Pts',(46.4807103968838,-2.168402790185,2.3862351879234));
#78570=CARTESIAN_POINT('Ctrl Pts',(46.486881529259,-2.24124364776206,2.31794364560584));
#78571=CARTESIAN_POINT('Ctrl Pts',(46.4930526616342,-2.31066694634494,2.2465386321114));
#78572=CARTESIAN_POINT('Ctrl Pts',(46.4977480869711,-2.36348900481347,2.19220874755187));
#78573=CARTESIAN_POINT('Ctrl Pts',(46.502443512308,-2.41433332229022,2.13607717478546));
#78574=CARTESIAN_POINT('Ctrl Pts',(46.507138937645,-2.4630788926605,2.07830698671547));
#78575=CARTESIAN_POINT('Ctrl Pts',(46.5132722927928,-2.52675233510899,2.0028452223465));
#78576=CARTESIAN_POINT('Ctrl Pts',(46.5194056479406,-2.58707524734235,1.9243115331488));
#78577=CARTESIAN_POINT('Ctrl Pts',(46.5255390030883,-2.64373401534343,1.84303771491961));
#78578=CARTESIAN_POINT('Ctrl Pts',(46.5316645122836,-2.70032030392768,1.76186786434022));
#78579=CARTESIAN_POINT('Ctrl Pts',(46.5377900214788,-2.75325150827311,1.67796520329826));
#78580=CARTESIAN_POINT('Ctrl Pts',(46.5439155306741,-2.80225295442358,1.59169593262165));
#78581=CARTESIAN_POINT('Ctrl Pts',(46.550034892833,-2.85120522692009,1.50551323439539));
#78582=CARTESIAN_POINT('Ctrl Pts',(46.556154254992,-2.89623535952982,1.41696902467224));
#78583=CARTESIAN_POINT('Ctrl Pts',(46.5622736171509,-2.93711149370048,1.32645905932771));
#78584=CARTESIAN_POINT('Ctrl Pts',(46.5683885251004,-2.97795787462922,1.23601497508836));
#78585=CARTESIAN_POINT('Ctrl Pts',(46.5745034330499,-3.01465608571694,1.14360837851562));
#78586=CARTESIAN_POINT('Ctrl Pts',(46.5806183409994,-3.04702033759801,1.04965928984794));
#78587=CARTESIAN_POINT('Ctrl Pts',(46.5867314730216,-3.07937519006426,0.955737486422634));
#78588=CARTESIAN_POINT('Ctrl Pts',(46.5928446050439,-3.10739843466665,0.86027449432106));
#78589=CARTESIAN_POINT('Ctrl Pts',(46.5989577370661,-3.13095287065684,0.76370916206741));
#78590=CARTESIAN_POINT('Ctrl Pts',(46.6050697410841,-3.15450296034705,0.667161648194215));
#78591=CARTESIAN_POINT('Ctrl Pts',(46.611181745102,-3.17358578126501,0.569512627248587));
#78592=CARTESIAN_POINT('Ctrl Pts',(46.6172937491199,-3.18811468945743,0.47121363452872));
#78593=CARTESIAN_POINT('Ctrl Pts',(46.623408458521,-3.20265002864429,0.372871131294042));
#78594=CARTESIAN_POINT('Ctrl Pts',(46.6295231679221,-3.21262736756129,0.273878517798201));
#78595=CARTESIAN_POINT('Ctrl Pts',(46.6356378773232,-3.21801172049166,0.17469438822795));
#78596=CARTESIAN_POINT('Ctrl Pts',(46.6392830679732,-3.22122152028264,0.115567283730771));
#78597=CARTESIAN_POINT('Ctrl Pts',(46.6429282586231,-3.22280007565892,0.0563722112005146));
#78598=CARTESIAN_POINT('Ctrl Pts',(46.646573449273,-3.22274878923423,-0.00279356211900748));
#78599=CARTESIAN_POINT('',(46.4000265227372,-3.22266022380361,0.00169756151001587));
#78600=CARTESIAN_POINT('Ctrl Pts',(45.9705987712989,1.78932308991422,2.68012452748182));
#78601=CARTESIAN_POINT('Ctrl Pts',(46.0210035446588,1.10574053552164,3.12656706705717));
#78602=CARTESIAN_POINT('Ctrl Pts',(46.1376907242651,-0.881920472688252,
3.57354541826147));
#78603=CARTESIAN_POINT('Ctrl Pts',(46.2808328527696,-2.93975493458649,1.93617029787196));
#78604=CARTESIAN_POINT('Ctrl Pts',(46.3735702079145,-3.22033984576282,0.431640650872118));
#78605=CARTESIAN_POINT('Ctrl Pts',(46.4000251568126,-3.21830085460638,0.00171746357588361));
#78606=CARTESIAN_POINT('Ctrl Pts',(46.4000265507268,-3.22274955312531,0.00169715368999332));
#78607=CARTESIAN_POINT('Ctrl Pts',(46.4062581732079,-3.22280295769783,-0.0997135572294896));
#78608=CARTESIAN_POINT('Ctrl Pts',(46.4124897956889,-3.21806535961105,-0.201121896896725));
#78609=CARTESIAN_POINT('Ctrl Pts',(46.41872141817,-3.20856390007265,-0.302051753265169));
#78610=CARTESIAN_POINT('Ctrl Pts',(46.4249548901296,-3.19905962060328,-0.403011564529283));
#78611=CARTESIAN_POINT('Ctrl Pts',(46.4311883620892,-3.18478870581297,-0.503492193516223));
#78612=CARTESIAN_POINT('Ctrl Pts',(46.4374218340487,-3.16583008376198,-0.603023584321204));
#78613=CARTESIAN_POINT('Ctrl Pts',(46.4436586485661,-3.14686129558034,-0.70260834657482));
#78614=CARTESIAN_POINT('Ctrl Pts',(46.4498954630835,-3.12319987712051,-0.801242447405722));
#78615=CARTESIAN_POINT('Ctrl Pts',(46.4561322776009,-3.09497549546286,-0.89846772061352));
#78616=CARTESIAN_POINT('Ctrl Pts',(46.4623782356076,-3.0667097354172,-0.995835531047709));
#78617=CARTESIAN_POINT('Ctrl Pts',(46.4686241936143,-3.03386777351972,-1.09178998832456));
#78618=CARTESIAN_POINT('Ctrl Pts',(46.474870151621,-2.99662868287034,-1.18588958149517));
#78619=CARTESIAN_POINT('Ctrl Pts',(46.4811213541571,-2.95935832375774,-1.28006818705883));
#78620=CARTESIAN_POINT('Ctrl Pts',(46.4873725566932,-2.91768365327421,-1.37238844584609));
#78621=CARTESIAN_POINT('Ctrl Pts',(46.4936237592294,-2.87183040081695,-1.46243212199527));
#78622=CARTESIAN_POINT('Ctrl Pts',(46.4998860894401,-2.82589552565277,-1.552636083581));
#78623=CARTESIAN_POINT('Ctrl Pts',(46.5061484196508,-2.77576742312358,-1.64055500839909));
#78624=CARTESIAN_POINT('Ctrl Pts',(46.5124107498616,-2.72171601364334,-1.72579822215037));
#78625=CARTESIAN_POINT('Ctrl Pts',(46.5147763428602,-2.70129811303246,-1.75799881567537));
#78626=CARTESIAN_POINT('Ctrl Pts',(46.5171419358589,-2.68032079515301,-1.78981792885236));
#78627=CARTESIAN_POINT('Ctrl Pts',(46.5195075288576,-2.65880008360341,-1.82123575572481));
#78628=CARTESIAN_POINT('Ctrl Pts',(46.5256797784124,-2.60264874972824,-1.90321040987512));
#78629=CARTESIAN_POINT('Ctrl Pts',(46.5318520279673,-2.54260393550251,-1.98273007495402));
#78630=CARTESIAN_POINT('Ctrl Pts',(46.5380242775221,-2.47890752031201,-2.05940162868746));
#78631=CARTESIAN_POINT('Ctrl Pts',(46.544188167611,-2.41529737318388,-2.13596934131211));
#78632=CARTESIAN_POINT('Ctrl Pts',(46.5503520577,-2.3480457301317,-2.20969627837632));
#78633=CARTESIAN_POINT('Ctrl Pts',(46.5565159477889,-2.27743772054739,-2.28021818945642));
#78634=CARTESIAN_POINT('Ctrl Pts',(46.5626733108566,-2.20690447867853,-2.35066542399187));
#78635=CARTESIAN_POINT('Ctrl Pts',(46.5688306739243,-2.13302224180427,-2.41791407455335));
#78636=CARTESIAN_POINT('Ctrl Pts',(46.574988036992,-2.05611574860215,-2.48163365363428));
#78637=CARTESIAN_POINT('Ctrl Pts',(46.5811409025014,-1.97926543065437,-2.54530668965477));
#78638=CARTESIAN_POINT('Ctrl Pts',(46.5872937680108,-1.89939558177457,-2.60545550292683));
#78639=CARTESIAN_POINT('Ctrl Pts',(46.5934466335201,-1.81686638781891,-2.66178776225939));
#78640=CARTESIAN_POINT('Ctrl Pts',(46.5995971679912,-1.73436846038723,-2.71809867988421));
#78641=CARTESIAN_POINT('Ctrl Pts',(46.6057477024622,-1.64921354815239,-2.77059567198646));
#78642=CARTESIAN_POINT('Ctrl Pts',(46.6118982369332,-1.56179266225975,-2.81902842174598));
#78643=CARTESIAN_POINT('Ctrl Pts',(46.618048086453,-1.4743815119514,-2.86745577781595));
#78644=CARTESIAN_POINT('Ctrl Pts',(46.6241979359727,-1.38470526965231,-2.91181958089788));
#78645=CARTESIAN_POINT('Ctrl Pts',(46.6303477854925,-1.29318062611911,-2.95191487525135));
#78646=CARTESIAN_POINT('Ctrl Pts',(46.6364985951448,-1.20164169348925,-2.99201642940016));
#78647=CARTESIAN_POINT('Ctrl Pts',(46.6426494047972,-1.10825418434345,-3.02784797683744));
#78648=CARTESIAN_POINT('Ctrl Pts',(46.6488002144496,-1.01345495636064,-3.05925262342423));
#78649=CARTESIAN_POINT('Ctrl Pts',(46.654957602033,-0.918554346149848,-3.09069085544318));
#78650=CARTESIAN_POINT('Ctrl Pts',(46.6611149896164,-0.822239415427962,
-3.11769259581678));
#78651=CARTESIAN_POINT('Ctrl Pts',(46.6672723771998,-0.724962268816142,
-3.14015083575502));
#78652=CARTESIAN_POINT('Ctrl Pts',(46.6734332011249,-0.627630833351503,
-3.16262160928543));
#78653=CARTESIAN_POINT('Ctrl Pts',(46.6795940250499,-0.529336539917454,
-3.18054375473742));
#78654=CARTESIAN_POINT('Ctrl Pts',(46.685754848975,-0.430539699163005,-3.19386178942431));
#78655=CARTESIAN_POINT('Ctrl Pts',(46.69192597302,-0.331577682561036,-3.20720209018418));
#78656=CARTESIAN_POINT('Ctrl Pts',(46.698097097065,-0.232111873290175,-3.21592286671934));
#78657=CARTESIAN_POINT('Ctrl Pts',(46.70426822111,-0.13260583457467,-3.22002069172494));
#78658=CARTESIAN_POINT('Ctrl Pts',(46.7089637299391,-0.0568932934027771,
-3.2231386607292));
#78659=CARTESIAN_POINT('Ctrl Pts',(46.7136592387682,0.0188424719052745,
-3.22358127729843));
#78660=CARTESIAN_POINT('Ctrl Pts',(46.7183547475973,0.0943992403508688,
-3.221367154784));
#78661=CARTESIAN_POINT('Ctrl Pts',(46.7245270053207,0.193718795391608,-3.21845668537852));
#78662=CARTESIAN_POINT('Ctrl Pts',(46.7306992630441,0.293078432466108,-3.21094353465639));
#78663=CARTESIAN_POINT('Ctrl Pts',(46.7368715207675,0.392016665811267,-3.19881860945978));
#78664=CARTESIAN_POINT('Ctrl Pts',(46.7430354191033,0.490820902314827,-3.18671010563665));
#78665=CARTESIAN_POINT('Ctrl Pts',(46.7491993174392,0.58920444212071,-3.17000229422451));
#78666=CARTESIAN_POINT('Ctrl Pts',(46.755363215775,0.686706701132125,-3.14873807566146));
#78667=CARTESIAN_POINT('Ctrl Pts',(46.7615205871563,0.784105714960766,-3.12749637378833));
#78668=CARTESIAN_POINT('Ctrl Pts',(46.7676779585376,0.880624881204119,-3.10170794893263));
#78669=CARTESIAN_POINT('Ctrl Pts',(46.7738353299189,0.975810600396833,-3.07146727715813));
#78670=CARTESIAN_POINT('Ctrl Pts',(46.7799882038075,1.070926793643,-3.04124869390014));
#78671=CARTESIAN_POINT('Ctrl Pts',(46.7861410776961,1.16471106354602,-3.0065844604398));
#78672=CARTESIAN_POINT('Ctrl Pts',(46.7922939515848,1.25672274150975,-2.96761950281235));
#78673=CARTESIAN_POINT('Ctrl Pts',(46.7984444944727,1.3486995610814,-2.9286693069608));
#78674=CARTESIAN_POINT('Ctrl Pts',(46.8045950373605,1.43890472352187,-2.88542179358704));
#78675=CARTESIAN_POINT('Ctrl Pts',(46.8107455802484,1.52691623562123,-2.83807053680776));
#78676=CARTESIAN_POINT('Ctrl Pts',(46.8168954382126,1.61491794676929,-2.79072455305869));
#78677=CARTESIAN_POINT('Ctrl Pts',(46.8230452961768,1.7007261107242,-2.73927594027524));
#78678=CARTESIAN_POINT('Ctrl Pts',(46.829195154141,1.78394300724425,-2.68396440166489));
#78679=CARTESIAN_POINT('Ctrl Pts',(46.8353459722553,1.86717289605075,-2.62864422750834));
#78680=CARTESIAN_POINT('Ctrl Pts',(46.8414967903696,1.94781035206711,-2.56946017007818));
#78681=CARTESIAN_POINT('Ctrl Pts',(46.8476476084839,2.02548718047142,-2.50669488455335));
#78682=CARTESIAN_POINT('Ctrl Pts',(46.8538050045038,2.10324707926237,-2.44386247558073));
#78683=CARTESIAN_POINT('Ctrl Pts',(46.8599624005237,2.17803968934412,-2.37744146414566));
#78684=CARTESIAN_POINT('Ctrl Pts',(46.8661197965435,2.24953053573908,-2.30775430479015));
#78685=CARTESIAN_POINT('Ctrl Pts',(46.8722806289041,2.32106127999047,-2.23802825418604));
#78686=CARTESIAN_POINT('Ctrl Pts',(46.8784414612646,2.38928629431012,-2.16503274296757));
#78687=CARTESIAN_POINT('Ctrl Pts',(46.8846022936251,2.4539100108565,-2.089124989348));
#78688=CARTESIAN_POINT('Ctrl Pts',(46.8907734260156,2.51864176900815,-2.01309032882811));
#78689=CARTESIAN_POINT('Ctrl Pts',(46.8969445584061,2.57975993690463,-1.93413404417319));
#78690=CARTESIAN_POINT('Ctrl Pts',(46.9031156907966,2.63701097745493,-1.85264423656627));
#78691=CARTESIAN_POINT('Ctrl Pts',(46.9078111159767,2.68057153658342,-1.79064114372271));
#78692=CARTESIAN_POINT('Ctrl Pts',(46.9125065411568,2.72189420194264,-1.72717197777526));
#78693=CARTESIAN_POINT('Ctrl Pts',(46.9172019663369,2.76088529323415,-1.66241690321753));
#78694=CARTESIAN_POINT('Ctrl Pts',(46.9233741891572,2.81213980038256,-1.57729516586987));
#78695=CARTESIAN_POINT('Ctrl Pts',(46.9295464119775,2.85954421333119,-1.48965101133111));
#78696=CARTESIAN_POINT('Ctrl Pts',(46.9357186347978,2.90284135274562,-1.39986772349746));
#78697=CARTESIAN_POINT('Ctrl Pts',(46.9418824981635,2.94607985194526,-1.31020603518182));
#78698=CARTESIAN_POINT('Ctrl Pts',(46.9480463615292,2.98522194717725,-1.21841135983221));
#78699=CARTESIAN_POINT('Ctrl Pts',(46.9542102248949,3.02005468392615,-1.124894336636));
#78700=CARTESIAN_POINT('Ctrl Pts',(46.9603675612842,3.05485053594266,-1.03147633954845));
#78701=CARTESIAN_POINT('Ctrl Pts',(46.9665248976735,3.08534595080881,-0.936340025336802));
#78702=CARTESIAN_POINT('Ctrl Pts',(46.9726822340628,3.11137513641882,-0.839918045391802));
#78703=CARTESIAN_POINT('Ctrl Pts',(46.9788350730678,3.13738531003366,-0.74356649309076));
#78704=CARTESIAN_POINT('Ctrl Pts',(46.9849879120728,3.15893562729801,-0.645931560178757));
#78705=CARTESIAN_POINT('Ctrl Pts',(46.9911407510778,3.17590972684832,-0.547462299533217));
#78706=CARTESIAN_POINT('Ctrl Pts',(46.9972912591591,3.19287739597967,-0.449030342698692));
#78707=CARTESIAN_POINT('Ctrl Pts',(47.0034417672403,3.20527221842371,-0.349765113758991));
#78708=CARTESIAN_POINT('Ctrl Pts',(47.0095922753215,3.21302885395988,-0.250126260359202));
#78709=CARTESIAN_POINT('Ctrl Pts',(47.0157420985959,3.22078462586054,-0.150498500899773));
#78710=CARTESIAN_POINT('Ctrl Pts',(47.0218919218703,3.22390320386356,-0.0504976327562812));
#78711=CARTESIAN_POINT('Ctrl Pts',(47.0280417451446,3.22237117658844,0.0494121725088487));
#78712=CARTESIAN_POINT('Ctrl Pts',(47.0341925287261,3.22083891008423,0.149337578887788));
#78713=CARTESIAN_POINT('Ctrl Pts',(47.0403433123075,3.21465460253941,0.249171459775504));
#78714=CARTESIAN_POINT('Ctrl Pts',(47.0464940958889,3.20385693885345,0.348451256075473));
#78715=CARTESIAN_POINT('Ctrl Pts',(47.0526514578309,3.19304772689509,0.447837233690782));
#78716=CARTESIAN_POINT('Ctrl Pts',(47.0588088197729,3.17761535305071,0.546667510678373));
#78717=CARTESIAN_POINT('Ctrl Pts',(47.0649661817148,3.15765021446684,0.644486373461454));
#78718=CARTESIAN_POINT('Ctrl Pts',(47.0711269801964,3.13767393296305,0.742359830794476));
#78719=CARTESIAN_POINT('Ctrl Pts',(47.0772877786781,3.11315995519581,0.839220328634971));
#78720=CARTESIAN_POINT('Ctrl Pts',(47.0834485771597,3.08424895927587,0.934626085504626));
#78721=CARTESIAN_POINT('Ctrl Pts',(47.0896196763495,3.05528962486019,1.03019135852465));
#78722=CARTESIAN_POINT('Ctrl Pts',(47.0957907755393,3.02191873272581,1.12429662255493));
#78723=CARTESIAN_POINT('Ctrl Pts',(47.1019618747291,2.98432566643191,1.21651875414057));
#78724=CARTESIAN_POINT('Ctrl Pts',(47.1066576448449,2.95572000124364,1.28669327511375));
#78725=CARTESIAN_POINT('Ctrl Pts',(47.1113534149608,2.92467064979647,1.35577782472826));
#78726=CARTESIAN_POINT('Ctrl Pts',(47.1160491850767,2.89127853832094,1.42359614229062));
#78727=CARTESIAN_POINT('Ctrl Pts',(47.1222212498799,2.84738834121644,1.51273573824845));
#78728=CARTESIAN_POINT('Ctrl Pts',(47.128393314683,2.79929470480908,1.60000058535238));
#78729=CARTESIAN_POINT('Ctrl Pts',(47.1345653794862,2.74718097696689,1.68496713389052));
#78730=CARTESIAN_POINT('Ctrl Pts',(47.1407294212012,2.69513499193866,1.76982323412015));
#78731=CARTESIAN_POINT('Ctrl Pts',(47.1468934629161,2.63907952473299,1.85238660546671));
#78732=CARTESIAN_POINT('Ctrl Pts',(47.1530575046311,2.57924488033207,1.93225604146572));
#78733=CARTESIAN_POINT('Ctrl Pts',(47.1592142957543,2.5194806177684,2.01203152925628));
#78734=CARTESIAN_POINT('Ctrl Pts',(47.1653710868774,2.45594627986877,2.08911903954387));
#78735=CARTESIAN_POINT('Ctrl Pts',(47.1715278780006,2.38891609433598,2.16314526944506));
#78736=CARTESIAN_POINT('Ctrl Pts',(47.177680431001,2.32193205007221,2.23712054224145));
#78737=CARTESIAN_POINT('Ctrl Pts',(47.1838329840014,2.25145723131628,2.30803840181296));
#78738=CARTESIAN_POINT('Ctrl Pts',(47.1899855370018,2.17780641596424,2.37555820326192));
#78739=CARTESIAN_POINT('Ctrl Pts',(47.1961360151527,2.10418043816494,2.44305523474394));
#78740=CARTESIAN_POINT('Ctrl Pts',(47.2022864933035,2.02738090985673,2.50715618991461));
#78741=CARTESIAN_POINT('Ctrl Pts',(47.2084369714544,1.94775914652902,2.56755756889939));
#78742=CARTESIAN_POINT('Ctrl Pts',(47.2124246552677,1.89613610047936,2.60671901218419));
#78743=CARTESIAN_POINT('Ctrl Pts',(47.216412339081,1.8433274341045,2.64432605614692));
#78744=CARTESIAN_POINT('Ctrl Pts',(47.2204000228943,1.78943621037803,2.68030513402633));
#78745=CARTESIAN_POINT('Origin',(-1.72497344927317,0.,0.));
#78746=CARTESIAN_POINT('',(48.7170675950372,1.78943621037805,2.68030513402632));
#78747=CARTESIAN_POINT('',(48.4702430335869,1.79020435040141,2.68143717906909));
#78748=CARTESIAN_POINT('',(-1.72497344927317,1.78943621037804,2.68030513402633));
#78749=CARTESIAN_POINT('',(47.8965734492249,-3.22274998787281,-0.000279581503351442));
#78750=CARTESIAN_POINT('Ctrl Pts',(47.896573449273,-3.22274998787274,-0.000279582277973307));
#78751=CARTESIAN_POINT('Ctrl Pts',(47.8974054557895,-3.22274882591617,-0.0136734766987837));
#78752=CARTESIAN_POINT('Ctrl Pts',(47.8982374623059,-3.22266416599954,-0.0270669804709197));
#78753=CARTESIAN_POINT('Ctrl Pts',(47.8990694688224,-3.22249601981345,-0.0404594214793921));
#78754=CARTESIAN_POINT('Ctrl Pts',(47.9052431614043,-3.22124833383841,-0.139834621161703));
#78755=CARTESIAN_POINT('Ctrl Pts',(47.9114168539863,-3.2153973580358,-0.239326650631789));
#78756=CARTESIAN_POINT('Ctrl Pts',(47.9175905465683,-3.2049263431869,-0.338474071749408));
#78757=CARTESIAN_POINT('Ctrl Pts',(47.9237558739739,-3.19446951626273,-0.437487150955776));
#78758=CARTESIAN_POINT('Ctrl Pts',(47.9299212013795,-3.17940513810442,-0.536156121936185));
#78759=CARTESIAN_POINT('Ctrl Pts',(47.9360865287852,-3.15976846088399,-0.634019586529329));
#78760=CARTESIAN_POINT('Ctrl Pts',(47.9422453217225,-3.14015259606112,-0.731779328211086));
#78761=CARTESIAN_POINT('Ctrl Pts',(47.9484041146598,-3.11597415164381,-0.828734837495918));
#78762=CARTESIAN_POINT('Ctrl Pts',(47.9545629075971,-3.08732006438016,-0.924430842505624));
#78763=CARTESIAN_POINT('Ctrl Pts',(47.9607171861463,-3.05868698052973,-1.02005670245306));
#78764=CARTESIAN_POINT('Ctrl Pts',(47.9668714646954,-3.02558490060815,-1.11442447901149));
#78765=CARTESIAN_POINT('Ctrl Pts',(47.9730257432445,-2.98815141939414,-1.20709098964113));
#78766=CARTESIAN_POINT('Ctrl Pts',(47.9791776800203,-2.95073218204796,-1.29972223960337));
#78767=CARTESIAN_POINT('Ctrl Pts',(47.985329616796,-2.9089849807545,-1.39065310783238));
#78768=CARTESIAN_POINT('Ctrl Pts',(47.9914815535718,-2.8630963637999,-1.47945827048139));
#78769=CARTESIAN_POINT('Ctrl Pts',(47.9976327930992,-2.81721294776975,-1.56825336813013));
#78770=CARTESIAN_POINT('Ctrl Pts',(48.0037840326267,-2.76718924859587,-1.65492285348826));
#78771=CARTESIAN_POINT('Ctrl Pts',(48.0099352721542,-2.71325834445333,-1.73906489779834));
#78772=CARTESIAN_POINT('Ctrl Pts',(48.0160874579449,-2.65931914396168,-1.82321988592582));
#78773=CARTESIAN_POINT('Ctrl Pts',(48.0222396437356,-2.60147177895841,-1.90484629518602));
#78774=CARTESIAN_POINT('Ctrl Pts',(48.0283918295263,-2.5399927706897,-1.98357109460287));
#78775=CARTESIAN_POINT('Ctrl Pts',(48.0345505634188,-2.47844832701058,-2.06237968505191));
#78776=CARTESIAN_POINT('Ctrl Pts',(48.0407092973112,-2.41326478906135,-2.13828015568584));
#78777=CARTESIAN_POINT('Ctrl Pts',(48.0468680312037,-2.34475903942898,-2.21093252034433));
#78778=CARTESIAN_POINT('Ctrl Pts',(48.0530301869928,-2.27621522684409,-2.28362525188473));
#78779=CARTESIAN_POINT('Ctrl Pts',(48.0591923427819,-2.20434583869357,-2.35306598162725));
#78780=CARTESIAN_POINT('Ctrl Pts',(48.065354498571,-2.12950317605368,-2.41895303502926));
#78781=CARTESIAN_POINT('Ctrl Pts',(48.0715269170853,-2.05453586715217,-2.48494981962745));
#78782=CARTESIAN_POINT('Ctrl Pts',(48.0776993355997,-1.97658573163578,-2.54738083436659));
#78783=CARTESIAN_POINT('Ctrl Pts',(48.083871754114,-1.89603666061632,-2.60598590635079));
#78784=CARTESIAN_POINT('Ctrl Pts',(48.0885533985967,-1.83494195146005,-2.65043657204613));
#78785=CARTESIAN_POINT('Ctrl Pts',(48.0932350430794,-1.77235275676703,-2.69268707810716));
#78786=CARTESIAN_POINT('Ctrl Pts',(48.0979166875621,-1.7084460037503,-2.73264154523963));
#78787=CARTESIAN_POINT('Ctrl Pts',(48.1040905820961,-1.62416930256219,-2.78533129285944));
#78788=CARTESIAN_POINT('Ctrl Pts',(48.1102644766302,-1.53730524013941,-2.83421092951381));
#78789=CARTESIAN_POINT('Ctrl Pts',(48.1164383711642,-1.44823306185246,-2.87901694351691));
#78790=CARTESIAN_POINT('Ctrl Pts',(48.1226039262358,-1.35928119888294,-2.92376243525704));
#78791=CARTESIAN_POINT('Ctrl Pts',(48.1287694813075,-1.26812753288073,-2.96444504796746));
#78792=CARTESIAN_POINT('Ctrl Pts',(48.1349350363791,-1.1751793770992,-3.00084504667281));
#78793=CARTESIAN_POINT('Ctrl Pts',(48.141094082028,-1.08232935341321,-3.03720661526494));
#78794=CARTESIAN_POINT('Ctrl Pts',(48.1472531276769,-0.98768900859587,-3.06929440166731));
#78795=CARTESIAN_POINT('Ctrl Pts',(48.1534121733258,-0.891688432166575,
-3.09693546953118));
#78796=CARTESIAN_POINT('Ctrl Pts',(48.1595667407557,-0.795757657395764,
-3.12455643967844));
#78797=CARTESIAN_POINT('Ctrl Pts',(48.1657213081857,-0.698469033277891,
-3.1477369997403));
#78798=CARTESIAN_POINT('Ctrl Pts',(48.1718758756156,-0.600269856836845,
-3.16635336964671));
#78799=CARTESIAN_POINT('Ctrl Pts',(48.1780281233123,-0.502107692890165,
-3.18496272281112));
#78800=CARTESIAN_POINT('Ctrl Pts',(48.184180371009,-0.403036084600878,-3.19901122333952));
#78801=CARTESIAN_POINT('Ctrl Pts',(48.1903326187057,-0.30351375894017,-3.20842593192269));
#78802=CARTESIAN_POINT('Ctrl Pts',(48.1964841906779,-0.204002364191394,
-3.21783960645296));
#78803=CARTESIAN_POINT('Ctrl Pts',(48.2026357626501,-0.104040782666354,
-3.22262046003778));
#78804=CARTESIAN_POINT('Ctrl Pts',(48.2087873346222,-0.00409311987213795,
-3.22274740072344));
#78805=CARTESIAN_POINT('Ctrl Pts',(48.2149398738825,0.0958702589352058,
-3.22287436136957));
#78806=CARTESIAN_POINT('Ctrl Pts',(48.2210924131428,0.195819280525088,-3.21834595500233));
#78807=CARTESIAN_POINT('Ctrl Pts',(48.2272449524031,0.295290589862111,-3.20919320547064));
#78808=CARTESIAN_POINT('Ctrl Pts',(48.2334040698349,0.394868251927418,-3.20003067000277));
#78809=CARTESIAN_POINT('Ctrl Pts',(48.2395631872667,0.493966748688855,-3.18623395804791));
#78810=CARTESIAN_POINT('Ctrl Pts',(48.2457223046985,0.592128711458684,-3.16788591201866));
#78811=CARTESIAN_POINT('Ctrl Pts',(48.2518848613001,0.690345486570182,-3.14952762068318));
#78812=CARTESIAN_POINT('Ctrl Pts',(48.2580474179016,0.787624263677323,-3.12661303354869));
#78813=CARTESIAN_POINT('Ctrl Pts',(48.2642099745031,0.883520765206578,-3.09927549920119));
#78814=CARTESIAN_POINT('Ctrl Pts',(48.2703828176556,0.979577337354357,-3.07189233299057));
#78815=CARTESIAN_POINT('Ctrl Pts',(48.2765556608081,1.07424661348701,-3.04007161099999));
#78816=CARTESIAN_POINT('Ctrl Pts',(48.2827285039605,1.16710215795649,-3.00399569164027));
#78817=CARTESIAN_POINT('Ctrl Pts',(48.2874069714076,1.23747842240244,-2.97665334546702));
#78818=CARTESIAN_POINT('Ctrl Pts',(48.2920854388547,1.30681319972372,-2.94686770528887));
#78819=CARTESIAN_POINT('Ctrl Pts',(48.2967639063017,1.3749305652862,-2.91473558031287));
#78820=CARTESIAN_POINT('Ctrl Pts',(48.3029274850561,1.46467079580665,-2.87240358055557));
#78821=CARTESIAN_POINT('Ctrl Pts',(48.3090910638104,1.55261480753019,-2.82584747331742));
#78822=CARTESIAN_POINT('Ctrl Pts',(48.3152546425648,1.63833672151117,-2.77524239471943));
#78823=CARTESIAN_POINT('Ctrl Pts',(48.3214098424018,1.72394210305904,-2.7247061098833));
#78824=CARTESIAN_POINT('Ctrl Pts',(48.3275650422389,1.8073310187133,-2.67013201273159));
#78825=CARTESIAN_POINT('Ctrl Pts',(48.3337202420759,1.88809912584259,-2.61174257029525));
#78826=CARTESIAN_POINT('Ctrl Pts',(48.3398689064705,1.96878147534777,-2.55341512435771));
#78827=CARTESIAN_POINT('Ctrl Pts',(48.3460175708651,2.04684819710807,-2.49128064024699));
#78828=CARTESIAN_POINT('Ctrl Pts',(48.3521662352597,2.12192191323499,-2.42560610088142));
#78829=CARTESIAN_POINT('Ctrl Pts',(48.3583104241631,2.19694098468834,-2.3599793647145));
#78830=CARTESIAN_POINT('Ctrl Pts',(48.3644546130665,2.26897105447251,-2.2908179817846));
#78831=CARTESIAN_POINT('Ctrl Pts',(48.3705988019699,2.33766672511419,-2.21843004054531));
#78832=CARTESIAN_POINT('Ctrl Pts',(48.3767406757194,2.40633651096445,-2.14606937535913));
#78833=CARTESIAN_POINT('Ctrl Pts',(48.3828825494689,2.47167409433348,-2.07048488309211));
#78834=CARTESIAN_POINT('Ctrl Pts',(48.3890244232184,2.53337062315425,-1.99202179913752));
#78835=CARTESIAN_POINT('Ctrl Pts',(48.3951656376339,2.59506052881372,-1.91356713824448));
#78836=CARTESIAN_POINT('Ctrl Pts',(48.4013068520493,2.65310988762784,-1.83223484249483));
#78837=CARTESIAN_POINT('Ctrl Pts',(48.4074480664648,2.7072505307929,-1.74840273564805));
#78838=CARTESIAN_POINT('Ctrl Pts',(48.4135902763867,2.76139995029351,-1.66455703940415));
#78839=CARTESIAN_POINT('Ctrl Pts',(48.4197324863086,2.81163915926097,-1.57821109326239));
#78840=CARTESIAN_POINT('Ctrl Pts',(48.4258746962306,2.85774422714311,-1.48977028253695));
#78841=CARTESIAN_POINT('Ctrl Pts',(48.4320235914747,2.90389947683881,-1.40123321080424));
#78842=CARTESIAN_POINT('Ctrl Pts',(48.4381724867187,2.94591139838106,-1.31059710858022));
#78843=CARTESIAN_POINT('Ctrl Pts',(48.4443213819628,2.98360288606393,-1.21829035158743));
#78844=CARTESIAN_POINT('Ctrl Pts',(48.4504737595226,3.02131571963959,-1.1259313183312));
#78845=CARTESIAN_POINT('Ctrl Pts',(48.4566261370824,3.05470310140924,-1.03190015688265));
#78846=CARTESIAN_POINT('Ctrl Pts',(48.4627785146422,3.0836375016226,-0.936641511511598));
#78847=CARTESIAN_POINT('Ctrl Pts',(48.4689413557902,3.11262111169791,-0.841220856050377));
#78848=CARTESIAN_POINT('Ctrl Pts',(48.4751041969382,3.13713650586268,-0.744568969294602));
#78849=CARTESIAN_POINT('Ctrl Pts',(48.4812670380863,3.15710703715677,-0.64714196157814));
#78850=CARTESIAN_POINT('Ctrl Pts',(48.4860484004047,3.1726009211487,-0.571554450509453));
#78851=CARTESIAN_POINT('Ctrl Pts',(48.4908297627231,3.18536018203299,-0.495500621829391));
#78852=CARTESIAN_POINT('Ctrl Pts',(48.4956111250415,3.195370606819,-0.419194760913312));
#78853=CARTESIAN_POINT('Ctrl Pts',(48.5017953688468,3.20831815259115,-0.320500285102992));
#78854=CARTESIAN_POINT('Ctrl Pts',(48.5079796126521,3.21671131869511,-0.221034556122838));
#78855=CARTESIAN_POINT('Ctrl Pts',(48.5141638564573,3.22046816606932,-0.121253263189552));
#78856=CARTESIAN_POINT('Ctrl Pts',(48.5203397087429,3.2242199157049,-0.0216073654164394));
#78857=CARTESIAN_POINT('Ctrl Pts',(48.5265155610285,3.22334783589932,0.0783528166081075));
#78858=CARTESIAN_POINT('Ctrl Pts',(48.5326914133142,3.21782147504578,0.178164298427564));
#78859=CARTESIAN_POINT('Ctrl Pts',(48.5388606914528,3.21230099696058,0.277869531697386));
#78860=CARTESIAN_POINT('Ctrl Pts',(48.5450299695915,3.20213611239049,0.377425949919311));
#78861=CARTESIAN_POINT('Ctrl Pts',(48.5511992477301,3.18734840121872,0.476369322845732));
#78862=CARTESIAN_POINT('Ctrl Pts',(48.5573639095059,3.17257175543246,0.575238658177498));
#78863=CARTESIAN_POINT('Ctrl Pts',(48.5635285712817,3.15317922536676,0.673495433867807));
#78864=CARTESIAN_POINT('Ctrl Pts',(48.5696932330575,3.12924424947995,0.770680212277874));
#78865=CARTESIAN_POINT('Ctrl Pts',(48.5758554869797,3.10531862234906,0.867827031310971));
#78866=CARTESIAN_POINT('Ctrl Pts',(48.5820177409018,3.07685417855164,0.96390226561091));
#78867=CARTESIAN_POINT('Ctrl Pts',(48.588179994824,3.04397535096775,1.05845719100998));
#78868=CARTESIAN_POINT('Ctrl Pts',(48.5943414734557,3.01110065996157,1.15300022018815));
#78869=CARTESIAN_POINT('Ctrl Pts',(48.6005029520874,2.97381283155318,1.24602291223366));
#78870=CARTESIAN_POINT('Ctrl Pts',(48.6066644307191,2.93228570302068,1.33709315994082));
#78871=CARTESIAN_POINT('Ctrl Pts',(48.612826765544,2.89075280391723,1.42817606268444));
#78872=CARTESIAN_POINT('Ctrl Pts',(48.618989100369,2.84497961414036,1.51730558859858));
#78873=CARTESIAN_POINT('Ctrl Pts',(48.625151435194,2.795187086339,1.60407191698617));
#78874=CARTESIAN_POINT('Ctrl Pts',(48.6313201165647,2.74534327756,1.69092760541116));
#78875=CARTESIAN_POINT('Ctrl Pts',(48.6374887979355,2.69147208003589,1.77541486009589));
#78876=CARTESIAN_POINT('Ctrl Pts',(48.6436574793062,2.63383911875181,1.85715079060174));
#78877=CARTESIAN_POINT('Ctrl Pts',(48.6498294857358,2.57617509199692,1.93893077862445));
#78878=CARTESIAN_POINT('Ctrl Pts',(48.6560014921654,2.51474552811655,2.01795614685807));
#78879=CARTESIAN_POINT('Ctrl Pts',(48.662173498595,2.44985661502894,2.09387681784267));
#78880=CARTESIAN_POINT('Ctrl Pts',(48.6683555081248,2.38486253512,2.16992053504982));
#78881=CARTESIAN_POINT('Ctrl Pts',(48.6745375176546,2.31639820269218,2.24284918805124));
#78882=CARTESIAN_POINT('Ctrl Pts',(48.6807195271844,2.24480703191651,2.31234922794075));
#78883=CARTESIAN_POINT('Ctrl Pts',(48.6852991327166,2.19177260675709,2.36383455251585));
#78884=CARTESIAN_POINT('Ctrl Pts',(48.6898787382488,2.1370230110744,2.41343910677724));
#78885=CARTESIAN_POINT('Ctrl Pts',(48.694458343781,2.08070882147903,2.46105025603285));
#78886=CARTESIAN_POINT('Ctrl Pts',(48.7006391968184,2.0047045177545,2.52530852334874));
#78887=CARTESIAN_POINT('Ctrl Pts',(48.7068200498558,1.92559082778242,2.58615246483035));
#78888=CARTESIAN_POINT('Ctrl Pts',(48.7130009028932,1.84370708895466,2.64326724578472));
#78889=CARTESIAN_POINT('Ctrl Pts',(48.7143564669412,1.82574862079535,2.65579346881604));
#78890=CARTESIAN_POINT('Ctrl Pts',(48.7157120309892,1.80765705640678,2.66814045872364));
#78891=CARTESIAN_POINT('Ctrl Pts',(48.7170675950372,1.78943621037805,2.68030513402632));
#78892=CARTESIAN_POINT('Ctrl Pts',(47.4668462457454,1.78943621037804,2.68030513402633));
#78893=CARTESIAN_POINT('Ctrl Pts',(47.4730172821142,1.70636788358127,2.73576354807726));
#78894=CARTESIAN_POINT('Ctrl Pts',(47.479188318483,1.62081413773693,2.78729317563132));
#78895=CARTESIAN_POINT('Ctrl Pts',(47.4853593548518,1.53318972188769,2.83468637404527));
#78896=CARTESIAN_POINT('Ctrl Pts',(47.4906979136823,1.45738590693071,2.87568619365003));
#78897=CARTESIAN_POINT('Ctrl Pts',(47.4960364725128,1.38003294650229,2.913591009904));
#78898=CARTESIAN_POINT('Ctrl Pts',(47.5013750313432,1.30141033699827,2.94829589716739));
#78899=CARTESIAN_POINT('Ctrl Pts',(47.507547600212,1.21050500332719,2.98842251439108));
#78900=CARTESIAN_POINT('Ctrl Pts',(47.5137201690807,1.11758221817913,3.02441140884019));
#78901=CARTESIAN_POINT('Ctrl Pts',(47.5198927379495,1.02305466733697,3.05605574395168));
#78902=CARTESIAN_POINT('Ctrl Pts',(47.5260569501904,0.928655091019067,3.08765723791585));
#78903=CARTESIAN_POINT('Ctrl Pts',(47.5322211624313,0.832655475507946,3.1149257266562));
#78904=CARTESIAN_POINT('Ctrl Pts',(47.5383853746722,0.735490068682984,3.13770169413357));
#78905=CARTESIAN_POINT('Ctrl Pts',(47.5445430622812,0.638427508497301,3.16045355393943));
#78906=CARTESIAN_POINT('Ctrl Pts',(47.5507007498902,0.540202030756116,3.17872224771765));
#78907=CARTESIAN_POINT('Ctrl Pts',(47.5568584374992,0.441263775350576,3.19239782030112));
#78908=CARTESIAN_POINT('Ctrl Pts',(47.563011629791,0.342397748169423,3.20606340926076));
#78909=CARTESIAN_POINT('Ctrl Pts',(47.5691648220828,0.242820406811316,3.21514248435243));
#78910=CARTESIAN_POINT('Ctrl Pts',(47.5753180143746,0.142991932068644,3.21957619413849));
#78911=CARTESIAN_POINT('Ctrl Pts',(47.5814688768994,0.0432012551194085,
3.22400822520065));
#78912=CARTESIAN_POINT('Ctrl Pts',(47.5876197394241,-0.056839932864205,
3.22379836656984));
#78913=CARTESIAN_POINT('Ctrl Pts',(47.5937706019489,-0.156667370397694,
3.21893971635889));
#78914=CARTESIAN_POINT('Ctrl Pts',(47.5999207804033,-0.25648370558835,3.2140816065044));
#78915=CARTESIAN_POINT('Ctrl Pts',(47.6060709588578,-0.356085903782014,
3.20457575409293));
#78916=CARTESIAN_POINT('Ctrl Pts',(47.6122211373122,-0.455011758880625,
3.19046734222126));
#78917=CARTESIAN_POINT('Ctrl Pts',(47.6183722763906,-0.553953065651398,
3.17635672669357));
#78918=CARTESIAN_POINT('Ctrl Pts',(47.6245234154689,-0.652217389483371,
3.15764218511765));
#78919=CARTESIAN_POINT('Ctrl Pts',(47.6306745545473,-0.749350687482992,
3.13442037858178));
#78920=CARTESIAN_POINT('Ctrl Pts',(47.6368322702674,-0.846587837938679,
3.11117374387996));
#78921=CARTESIAN_POINT('Ctrl Pts',(47.6429899859875,-0.942691124543513,
3.08341032224836));
#78922=CARTESIAN_POINT('Ctrl Pts',(47.6491477017075,-1.03721981015267,3.05127721256638));
#78923=CARTESIAN_POINT('Ctrl Pts',(47.6553088535669,-1.13180124482361,3.01912617191057));
#78924=CARTESIAN_POINT('Ctrl Pts',(47.6614700054262,-1.22480592437142,2.98260074595528));
#78925=CARTESIAN_POINT('Ctrl Pts',(47.6676311572856,-1.31581326616096,2.94189615912847));
#78926=CARTESIAN_POINT('Ctrl Pts',(47.6738026054996,-1.40697269702269,2.90112354786843));
#78927=CARTESIAN_POINT('Ctrl Pts',(47.6799740537136,-1.49612773479907,2.85615802087152));
#78928=CARTESIAN_POINT('Ctrl Pts',(47.6861455019276,-1.58288244116645,2.80724076985693));
#78929=CARTESIAN_POINT('Ctrl Pts',(47.6908377513127,-1.64884341231761,2.77004821261049));
#78930=CARTESIAN_POINT('Ctrl Pts',(47.6955300006978,-1.71341731197272,2.73057219493661));
#78931=CARTESIAN_POINT('Ctrl Pts',(47.7002222500829,-1.77644236525286,2.6889347491962));
#78932=CARTESIAN_POINT('Ctrl Pts',(47.7063797254309,-1.85914794631434,2.63429538017306));
#78933=CARTESIAN_POINT('Ctrl Pts',(47.7125372007789,-1.93947937218019,2.57573816524997));
#78934=CARTESIAN_POINT('Ctrl Pts',(47.7186946761269,-2.01704061049959,2.51349651642796));
#78935=CARTESIAN_POINT('Ctrl Pts',(47.7248437993372,-2.09449664301502,2.45133929357497));
#78936=CARTESIAN_POINT('Ctrl Pts',(47.7309929225474,-2.1691896181193,2.38550783992295));
#78937=CARTESIAN_POINT('Ctrl Pts',(47.7371420457577,-2.24075154303061,2.31627936244874));
#78938=CARTESIAN_POINT('Ctrl Pts',(47.7432846684349,-2.31223781639796,2.24712406971926));
#78939=CARTESIAN_POINT('Ctrl Pts',(47.749427291112,-2.38059930729441,2.17457919390108));
#78940=CARTESIAN_POINT('Ctrl Pts',(47.7555699137891,-2.44550104646649,2.09896217074803));
#78941=CARTESIAN_POINT('Ctrl Pts',(47.7617080978264,-2.51035588784531,2.02339978821887));
#78942=CARTESIAN_POINT('Ctrl Pts',(47.7678462818636,-2.57175566375418,1.94477000179743));
#78943=CARTESIAN_POINT('Ctrl Pts',(47.7739844659008,-2.62940291799779,1.86342637561152));
#78944=CARTESIAN_POINT('Ctrl Pts',(47.7801203781277,-2.68702883634914,1.78211285560963));
#78945=CARTESIAN_POINT('Ctrl Pts',(47.7862562903545,-2.74090474014038,1.6980878473495));
#78946=CARTESIAN_POINT('Ctrl Pts',(47.7923922025813,-2.79077464818404,1.61173646281061));
#78947=CARTESIAN_POINT('Ctrl Pts',(47.7985275060852,-2.84063960880401,1.52539364489841));
#78948=CARTESIAN_POINT('Ctrl Pts',(47.804662809589,-2.8864991454356,1.43672528776936));
#78949=CARTESIAN_POINT('Ctrl Pts',(47.8107981130929,-2.92814220246344,1.34614293618938));
#78950=CARTESIAN_POINT('Ctrl Pts',(47.8169344700213,-2.96979240955621,1.25554503172396));
#78951=CARTESIAN_POINT('Ctrl Pts',(47.8230708269497,-3.00722451686743,1.16303287698175));
#78952=CARTESIAN_POINT('Ctrl Pts',(47.8292071838781,-3.04027519801814,1.06903895289917));
#78953=CARTESIAN_POINT('Ctrl Pts',(47.8353501327987,-3.07336138392101,0.974944055678911));
#78954=CARTESIAN_POINT('Ctrl Pts',(47.8414930817193,-3.10205660135938,0.879364623766396));
#78955=CARTESIAN_POINT('Ctrl Pts',(47.8476360306399,-3.12624716888796,0.782749130641511));
#78956=CARTESIAN_POINT('Ctrl Pts',(47.8537825320079,-3.15045172574311,0.686077765090956));
#78957=CARTESIAN_POINT('Ctrl Pts',(47.8599290333759,-3.17014635990226,0.588369573355306));
#78958=CARTESIAN_POINT('Ctrl Pts',(47.8660755347439,-3.1852687799006,0.490081995476812));
#78959=CARTESIAN_POINT('Ctrl Pts',(47.8722321041398,-3.20041597056705,0.391633421608901));
#78960=CARTESIAN_POINT('Ctrl Pts',(47.8783886735356,-3.21097594526943,0.29260400048704));
#78961=CARTESIAN_POINT('Ctrl Pts',(47.8845452429314,-3.21693840401225,0.19345507822518));
#78962=CARTESIAN_POINT('Ctrl Pts',(47.8885546450292,-3.22082139355637,0.128885368804992));
#78963=CARTESIAN_POINT('Ctrl Pts',(47.8925640471271,-3.22275558727389,0.0642649951616726));
#78964=CARTESIAN_POINT('Ctrl Pts',(47.8965734492249,-3.22274998787281,-0.000279581503348901));
#78965=CARTESIAN_POINT('',(47.6500265507268,-3.22274888240162,-0.00268392978501451));
#78966=CARTESIAN_POINT('Ctrl Pts',(47.2204000228943,1.78943621037803,2.68030513402633));
#78967=CARTESIAN_POINT('Ctrl Pts',(47.2265503217517,1.70631850415497,2.73579651497059));
#78968=CARTESIAN_POINT('Ctrl Pts',(47.232700620609,1.62062450475473,2.7874130976737));
#78969=CARTESIAN_POINT('Ctrl Pts',(47.2388509194664,1.5327554146123,2.83492123373414));
#78970=CARTESIAN_POINT('Ctrl Pts',(47.2451880431622,1.44221716497809,2.88387250289288));
#78971=CARTESIAN_POINT('Ctrl Pts',(47.251525166858,1.34936998556573,2.92846147270142));
#78972=CARTESIAN_POINT('Ctrl Pts',(47.2578622905538,1.25467812721937,2.96848452237455));
#78973=CARTESIAN_POINT('Ctrl Pts',(47.2640218596828,1.16263936082786,3.00738619970428));
#78974=CARTESIAN_POINT('Ctrl Pts',(47.2701814288117,1.06885835291513,3.04197433513195));
#78975=CARTESIAN_POINT('Ctrl Pts',(47.2763409979407,0.973778471150405,3.07211214828235));
#78976=CARTESIAN_POINT('Ctrl Pts',(47.2827668989199,0.874587457534403,3.10355308172772));
#78977=CARTESIAN_POINT('Ctrl Pts',(47.2891927998991,0.773983233015376,3.13015002880449));
#78978=CARTESIAN_POINT('Ctrl Pts',(47.2956187008784,0.672481183617758,3.15180688180289));
#78979=CARTESIAN_POINT('Ctrl Pts',(47.3020446018576,0.570979134220111,3.17346373480129));
#78980=CARTESIAN_POINT('Ctrl Pts',(47.3084705028369,0.468579793637156,3.19018048042091));
#78981=CARTESIAN_POINT('Ctrl Pts',(47.3148964038161,0.365802898924829,3.2019222041827));
#78982=CARTESIAN_POINT('Ctrl Pts',(47.3210687091399,0.267082053951235,3.21320054543299));
#78983=CARTESIAN_POINT('Ctrl Pts',(47.3272410144636,0.167665388864387,3.21992885365931));
#78984=CARTESIAN_POINT('Ctrl Pts',(47.3334133197873,0.06800838669313,3.22203234338816));
#78985=CARTESIAN_POINT('Ctrl Pts',(47.3395772660597,-0.0315136516439381,
3.22413298439557));
#78986=CARTESIAN_POINT('Ctrl Pts',(47.3457412123321,-0.131274949682221,
3.2216212468552));
#78987=CARTESIAN_POINT('Ctrl Pts',(47.3519051586046,-0.230813505313807,
3.21447393647308));
#78988=CARTESIAN_POINT('Ctrl Pts',(47.3580625781933,-0.330246664720032,
3.20733419400805));
#78989=CARTESIAN_POINT('Ctrl Pts',(47.364219997782,-0.429457119750578,3.19556866794352));
#78990=CARTESIAN_POINT('Ctrl Pts',(47.3703774173707,-0.527982429544278,
3.17920620856725));
#78991=CARTESIAN_POINT('Ctrl Pts',(47.3765303396749,-0.626435777967615,
3.16285570007955));
#78992=CARTESIAN_POINT('Ctrl Pts',(47.3826832619791,-0.724204548868616,
3.14191500457379));
#78993=CARTESIAN_POINT('Ctrl Pts',(47.3888361842832,-0.820831908505135,
3.11646475039905));
#78994=CARTESIAN_POINT('Ctrl Pts',(47.3949867756992,-0.917422663166053,
3.09102413744743));
#78995=CARTESIAN_POINT('Ctrl Pts',(47.4011373671152,-1.0128724461579,3.0610774707991));
#78996=CARTESIAN_POINT('Ctrl Pts',(47.4072879585312,-1.10673597347601,3.02675619228145));
#78997=CARTESIAN_POINT('Ctrl Pts',(47.4134378650789,-1.20058904909106,2.99243873543791));
#78998=CARTESIAN_POINT('Ctrl Pts',(47.4195877716266,-1.29285581224778,2.95374778434491));
#78999=CARTESIAN_POINT('Ctrl Pts',(47.4257376781743,-1.38310842808469,2.91086389902742));
#79000=CARTESIAN_POINT('Ctrl Pts',(47.4318885448703,-1.47337513452599,2.86797331850384));
#79001=CARTESIAN_POINT('Ctrl Pts',(47.4380394115664,-1.56162667668805,2.82088868994946));
#79002=CARTESIAN_POINT('Ctrl Pts',(47.4441902782624,-1.64745832048031,2.76983729572338));
#79003=CARTESIAN_POINT('Ctrl Pts',(47.45034772256,-1.73338175074464,2.71873130825915));
#79004=CARTESIAN_POINT('Ctrl Pts',(47.4565051668576,-1.81687974104749,2.66365030682196));
#79005=CARTESIAN_POINT('Ctrl Pts',(47.4626626111552,-1.89757525903276,2.60486577366412));
#79006=CARTESIAN_POINT('Ctrl Pts',(47.4688234917003,-1.97831581027566,2.54604843497887));
#79007=CARTESIAN_POINT('Ctrl Pts',(47.4749843722455,-2.05625043577832,2.48352372037595));
#79008=CARTESIAN_POINT('Ctrl Pts',(47.4811452527906,-2.13103565698307,2.41760306733068));
#79009=CARTESIAN_POINT('Ctrl Pts',(47.4873164327096,-2.20594589943208,2.35157221227046));
#79010=CARTESIAN_POINT('Ctrl Pts',(47.4934876126286,-2.2776959086766,2.28213438111367));
#79011=CARTESIAN_POINT('Ctrl Pts',(47.4996587925476,-2.34597940490285,2.20963757079564));
#79012=CARTESIAN_POINT('Ctrl Pts',(47.5043537358837,-2.39792848915891,2.15448305886163));
#79013=CARTESIAN_POINT('Ctrl Pts',(47.5090486792197,-2.44787194695625,2.09755878406992));
#79014=CARTESIAN_POINT('Ctrl Pts',(47.5137436225558,-2.49569140684989,2.03902966243152));
#79015=CARTESIAN_POINT('Ctrl Pts',(47.5198916750508,-2.55831123602816,1.96238547600402));
#79016=CARTESIAN_POINT('Ctrl Pts',(47.5260397275457,-2.61751393702052,1.88271087171108));
#79017=CARTESIAN_POINT('Ctrl Pts',(47.5321877800407,-2.67299039278759,1.8003443899891));
#79018=CARTESIAN_POINT('Ctrl Pts',(47.5383278548084,-2.72839486217701,1.71808478720483));
#79019=CARTESIAN_POINT('Ctrl Pts',(47.5444679295762,-2.78008244862477,1.63314060436496));
#79020=CARTESIAN_POINT('Ctrl Pts',(47.550608004344,-2.8277835636169,1.54588410944616));
#79021=CARTESIAN_POINT('Ctrl Pts',(47.5567417847098,-2.87543577855413,1.45871706416376));
#79022=CARTESIAN_POINT('Ctrl Pts',(47.5628755650755,-2.91910943321578,1.36924279815371));
#79023=CARTESIAN_POINT('Ctrl Pts',(47.5690093454413,-2.95857824073278,1.27786241667971));
#79024=CARTESIAN_POINT('Ctrl Pts',(47.5751385086787,-2.99801733858624,1.18655082067351));
#79025=CARTESIAN_POINT('Ctrl Pts',(47.5812676719161,-3.03325770759927,1.09333636151927));
#79026=CARTESIAN_POINT('Ctrl Pts',(47.5873968351535,-3.06411951315494,0.998643665980567));
#79027=CARTESIAN_POINT('Ctrl Pts',(47.5935237873491,-3.09497018558514,0.903985130000682));
#79028=CARTESIAN_POINT('Ctrl Pts',(47.5996507395447,-3.1214452944217,0.807849831755124));
#79029=CARTESIAN_POINT('Ctrl Pts',(47.6057776917403,-3.14341389342911,0.710680418399755));
#79030=CARTESIAN_POINT('Ctrl Pts',(47.6119033629361,-3.16537789932581,0.613531320853912));
#79031=CARTESIAN_POINT('Ctrl Pts',(47.6180290341319,-3.18283717672938,0.515348965925687));
#79032=CARTESIAN_POINT('Ctrl Pts',(47.6241547053277,-3.19571150870808,0.416587944629584));
#79033=CARTESIAN_POINT('Ctrl Pts',(47.6302823669541,-3.20859002397757,0.317794832653253));
#79034=CARTESIAN_POINT('Ctrl Pts',(47.6364100285805,-3.21688056513942,0.218423113421889));
#79035=CARTESIAN_POINT('Ctrl Pts',(47.6425376902069,-3.22055466709273,0.118933589734913));
#79036=CARTESIAN_POINT('Ctrl Pts',(47.6450339770468,-3.22205142277443,0.0784035468182273));
#79037=CARTESIAN_POINT('Ctrl Pts',(47.6475302638868,-3.22278264268373,0.0378539829513926));
#79038=CARTESIAN_POINT('Ctrl Pts',(47.6500265507268,-3.22274888240162,-0.00268392978501451));
#79039=CARTESIAN_POINT('Ctrl Pts',(47.6500278454515,-3.22023055859585,-0.00270284149074349));
#79040=CARTESIAN_POINT('Ctrl Pts',(47.6708821773994,-3.22287022505361,-0.341100026664383));
#79041=CARTESIAN_POINT('Ctrl Pts',(47.7580189155941,-3.01777852171772,-1.75191763288685));
#79042=CARTESIAN_POINT('Ctrl Pts',(47.9114380600351,-0.968103398024024,
-3.68661448347931));
#79043=CARTESIAN_POINT('Ctrl Pts',(48.1102852787748,2.57778134821769,-2.80783294777081));
#79044=CARTESIAN_POINT('Ctrl Pts',(48.296553603292,3.68122906515452,0.43159223718354));
#79045=CARTESIAN_POINT('Ctrl Pts',(48.4165395215627,2.50785121046015,2.19182082035424));
#79046=CARTESIAN_POINT('Ctrl Pts',(48.4702430335869,1.79020435040156,2.68143717906899));
#79047=CARTESIAN_POINT('Origin',(24.9384,0.,0.));
#79048=CARTESIAN_POINT('',(0.989963935465355,-3.93416568820139,0.00240681427912712));
#79049=CARTESIAN_POINT('',(0.585831332880558,1.74924991682375,3.52258622726146));
#79050=CARTESIAN_POINT('Ctrl Pts',(0.989963522034966,-3.93299925901829,
0.00241424140712914));
#79051=CARTESIAN_POINT('Ctrl Pts',(0.983684296778858,-3.93292343624727,
0.125935816900034));
#79052=CARTESIAN_POINT('Ctrl Pts',(0.977405071522742,-3.92702906700058,
0.249289462579013));
#79053=CARTESIAN_POINT('Ctrl Pts',(0.971125846266634,-3.91536025446055,
0.372079397159524));
#79054=CARTESIAN_POINT('Ctrl Pts',(0.965241985179104,-3.9044261552299,0.487138005276138));
#79055=CARTESIAN_POINT('Ctrl Pts',(0.959358124091569,-3.88839801893483,
0.601903673559196));
#79056=CARTESIAN_POINT('Ctrl Pts',(0.95347426300404,-3.86729751325782,0.715890315586026));
#79057=CARTESIAN_POINT('Ctrl Pts',(0.947598037826548,-3.84622439122579,
0.829729028943051));
#79058=CARTESIAN_POINT('Ctrl Pts',(0.941721812649061,-3.82009206596904,
0.942790325620221));
#79059=CARTESIAN_POINT('Ctrl Pts',(0.935845587471569,-3.7889740420547,1.05459220015874));
#79060=CARTESIAN_POINT('Ctrl Pts',(0.929975432826291,-3.75788816513285,
1.16627857591011));
#79061=CARTESIAN_POINT('Ctrl Pts',(0.924105278181015,-3.72182694485705,
1.27670772340426));
#79062=CARTESIAN_POINT('Ctrl Pts',(0.918235123535737,-3.68091499425547,
1.38540745092021));
#79063=CARTESIAN_POINT('Ctrl Pts',(0.912153602868706,-3.63852993148507,
1.49802111773744));
#79064=CARTESIAN_POINT('Ctrl Pts',(0.90607208220167,-3.59093831837406,1.60877803345252));
#79065=CARTESIAN_POINT('Ctrl Pts',(0.89999056153464,-3.53833547547697,1.71716949162893));
#79066=CARTESIAN_POINT('Ctrl Pts',(0.894127361297117,-3.48762102133713,
1.82166980629048));
#79067=CARTESIAN_POINT('Ctrl Pts',(0.888264161059598,-3.43224914112038,
1.92397117538651));
#79068=CARTESIAN_POINT('Ctrl Pts',(0.882400960822075,-3.37244370385505,
2.02363842232956));
#79069=CARTESIAN_POINT('Ctrl Pts',(0.876538733713052,-3.31264819263234,
2.12328912727597));
#79070=CARTESIAN_POINT('Ctrl Pts',(0.870676506604024,-3.24842079940996,
2.22030622661834));
#79071=CARTESIAN_POINT('Ctrl Pts',(0.864814279495,-3.18003049757982,2.31428067322489));
#79072=CARTESIAN_POINT('Ctrl Pts',(0.85895162032655,-3.1116351552294,2.40826204596119));
#79073=CARTESIAN_POINT('Ctrl Pts',(0.853088961158097,-3.03907653664482,
2.49919998737317));
#79074=CARTESIAN_POINT('Ctrl Pts',(0.847226301989647,-2.96266552858476,
2.58671644478779));
#79075=CARTESIAN_POINT('Ctrl Pts',(0.841361805614357,-2.8862305752769,2.67426032761286));
#79076=CARTESIAN_POINT('Ctrl Pts',(0.835497309239071,-2.80594110245673,
2.75838028438628));
#79077=CARTESIAN_POINT('Ctrl Pts',(0.829632812863782,-2.72214618334568,
2.83873372412711));
#79078=CARTESIAN_POINT('Ctrl Pts',(0.823761874740816,-2.63825922125414,
2.919175426619));
#79079=CARTESIAN_POINT('Ctrl Pts',(0.817890936617861,-2.55085942448793,
2.99584206890481));
#79080=CARTESIAN_POINT('Ctrl Pts',(0.812019998494897,-2.46033047483642,
3.06843004720512));
#79081=CARTESIAN_POINT('Ctrl Pts',(0.806145224363962,-2.36974237454065,
3.14106545371153));
#79082=CARTESIAN_POINT('Ctrl Pts',(0.800270450233023,-2.27602138115173,
3.20961664647278));
#79083=CARTESIAN_POINT('Ctrl Pts',(0.794395676102088,-2.17958039394005,
3.27382319411909));
#79084=CARTESIAN_POINT('Ctrl Pts',(0.788512509971539,-2.08300164266983,
3.33812145955931));
#79085=CARTESIAN_POINT('Ctrl Pts',(0.782629343840982,-1.98369549383543,
3.39806248092037));
#79086=CARTESIAN_POINT('Ctrl Pts',(0.776746177710432,-1.88209972512649,
3.45343157231743));
#79087=CARTESIAN_POINT('Ctrl Pts',(0.77525699431595,-1.85638317584779,3.46744693915331));
#79088=CARTESIAN_POINT('Ctrl Pts',(0.77376781092148,-1.83052002340702,3.48116961036836));
#79089=CARTESIAN_POINT('Ctrl Pts',(0.772278627526997,-1.80451755736747,
3.4945965983433));
#79090=CARTESIAN_POINT('Ctrl Pts',(0.766455262790914,-1.70283643176066,
3.5471020510463));
#79091=CARTESIAN_POINT('Ctrl Pts',(0.760631898054829,-1.59868024946819,
3.59525952156886));
#79092=CARTESIAN_POINT('Ctrl Pts',(0.754808533318744,-1.49246073302146,
3.6388253544776));
#79093=CARTESIAN_POINT('Ctrl Pts',(0.748992614587671,-1.38637703342419,
3.68233548223566));
#79094=CARTESIAN_POINT('Ctrl Pts',(0.7431766958566,-1.27823563018259,3.7212654856502));
#79095=CARTESIAN_POINT('Ctrl Pts',(0.737360777125527,-1.16847319636026,
3.75541733891024));
#79096=CARTESIAN_POINT('Ctrl Pts',(0.731550674180361,-1.05882052246498,
3.78953504109698));
#79097=CARTESIAN_POINT('Ctrl Pts',(0.725740571235197,-0.947550440725385,
3.81888396960525));
#79098=CARTESIAN_POINT('Ctrl Pts',(0.71993046829003,-0.835119262116037,
3.84331430123048));
#79099=CARTESIAN_POINT('Ctrl Pts',(0.714124405676074,-0.722766267870076,
3.86772764406356));
#79100=CARTESIAN_POINT('Ctrl Pts',(0.70831834306211,-0.609254192345964,
3.8872291026441));
#79101=CARTESIAN_POINT('Ctrl Pts',(0.702512280448154,-0.495053445997505,
3.90171899111225));
#79102=CARTESIAN_POINT('Ctrl Pts',(0.696708301752118,-0.380893688697493,
3.91620367885484));
#79103=CARTESIAN_POINT('Ctrl Pts',(0.690904323056092,-0.266046168834459,
3.92568031837934));
#79104=CARTESIAN_POINT('Ctrl Pts',(0.685100344360055,-0.150989718573033,
3.93010064818768));
#79105=CARTESIAN_POINT('Ctrl Pts',(0.679296985641433,-0.0359455585704462,
3.93452050581913));
#79106=CARTESIAN_POINT('Ctrl Pts',(0.673493626922802,0.0793070669081008,
3.93388511163517));
#79107=CARTESIAN_POINT('Ctrl Pts',(0.667690268204179,0.194286813897208,
3.92819826815624));
#79108=CARTESIAN_POINT('Ctrl Pts',(0.661886066318469,0.309283266236282,
3.92251059843866));
#79109=CARTESIAN_POINT('Ctrl Pts',(0.656081864432768,0.424006340962809,
3.91177004230581));
#79110=CARTESIAN_POINT('Ctrl Pts',(0.650277662547058,0.537978126806255,
3.8960324093978));
#79111=CARTESIAN_POINT('Ctrl Pts',(0.644467730218229,0.652062436102339,
3.88027923884792));
#79112=CARTESIAN_POINT('Ctrl Pts',(0.638657797889396,0.765393557871783,
3.85951919809204));
#79113=CARTESIAN_POINT('Ctrl Pts',(0.632847865560567,0.877502083968805,
3.83385955567368));
#79114=CARTESIAN_POINT('Ctrl Pts',(0.627034879167403,0.989669541329025,
3.80818642494008));
#79115=CARTESIAN_POINT('Ctrl Pts',(0.621221892774245,1.10061271792731,3.77760867621448));
#79116=CARTESIAN_POINT('Ctrl Pts',(0.615408906381081,1.20987750582488,3.74228345010088));
#79117=CARTESIAN_POINT('Ctrl Pts',(0.609587021543605,1.31930955484514,3.70690414858849));
#79118=CARTESIAN_POINT('Ctrl Pts',(0.603765136706121,1.42705769026697,3.66676300351413));
#79119=CARTESIAN_POINT('Ctrl Pts',(0.597943251868646,1.53268768508301,3.62206535832733));
#79120=CARTESIAN_POINT('Ctrl Pts',(0.593905945539284,1.60593898746127,3.59106885275259));
#79121=CARTESIAN_POINT('Ctrl Pts',(0.589868639209918,1.67817213107512,3.55788211578977));
#79122=CARTESIAN_POINT('Ctrl Pts',(0.585831332880556,1.74924991682375,3.52258622726146));
#79123=CARTESIAN_POINT('',(0.585799999999996,-1.74869447533084,3.52286199445102));
#79124=CARTESIAN_POINT('Origin',(0.585799999999996,0.,0.));
#79125=CARTESIAN_POINT('',(0.806636477965097,-3.93492227854593,0.00403485423253799));
#79126=CARTESIAN_POINT('Ctrl Pts',(0.585799999999983,-1.74869447533085,
3.52286199445101));
#79127=CARTESIAN_POINT('Ctrl Pts',(0.65208240624653,-2.92241244012897,2.94024646086725));
#79128=CARTESIAN_POINT('Ctrl Pts',(0.725694565568235,-3.86568596277398,
1.59600203772709));
#79129=CARTESIAN_POINT('Ctrl Pts',(0.79930672488994,-3.93806320532033,0.148344931151628));
#79130=CARTESIAN_POINT('Ctrl Pts',(0.806636477965097,-3.93698214742112,
0.00403696641419293));
#79131=CARTESIAN_POINT('',(2.05663644556805,-3.93145140809557,0.00214295819816745));
#79132=CARTESIAN_POINT('Ctrl Pts',(0.806636477965096,-3.93299793235017,
0.00403288101531948));
#79133=CARTESIAN_POINT('Ctrl Pts',(0.812372634790166,-3.93311361551045,
-0.108785133810083));
#79134=CARTESIAN_POINT('Ctrl Pts',(0.818108791615234,-3.92837095544938,
-0.221831062669951));
#79135=CARTESIAN_POINT('Ctrl Pts',(0.823844948440303,-3.91873779066641,
-0.334638802297222));
#79136=CARTESIAN_POINT('Ctrl Pts',(0.829573999063958,-3.90911655986839,
-0.447306790773436));
#79137=CARTESIAN_POINT('Ctrl Pts',(0.835303049687616,-3.89461689714465,
-0.559736749150826));
#79138=CARTESIAN_POINT('Ctrl Pts',(0.841032100311271,-3.87525862470365,
-0.671460789368933));
#79139=CARTESIAN_POINT('Ctrl Pts',(0.846968031026604,-3.85520131128005,
-0.78721926412103));
#79140=CARTESIAN_POINT('Ctrl Pts',(0.852903961741931,-3.82992782729007,
-0.902219406262141));
#79141=CARTESIAN_POINT('Ctrl Pts',(0.858839892457265,-3.7995192218675,-1.01594423206166));
#79142=CARTESIAN_POINT('Ctrl Pts',(0.864560073793223,-3.77021585807632,
-1.1255355762283));
#79143=CARTESIAN_POINT('Ctrl Pts',(0.870280255129183,-3.73614427695648,
-1.23394223546885));
#79144=CARTESIAN_POINT('Ctrl Pts',(0.876000436465141,-3.69742913017487,
-1.34071131394282));
#79145=CARTESIAN_POINT('Ctrl Pts',(0.88171906679873,-3.65872448083746,-1.44745144244409));
#79146=CARTESIAN_POINT('Ctrl Pts',(0.887437697132324,-3.61537891402056,
-1.5525544652223));
#79147=CARTESIAN_POINT('Ctrl Pts',(0.893156327465913,-3.56756658433904,
-1.65558378414006));
#79148=CARTESIAN_POINT('Ctrl Pts',(0.898874923668654,-3.51975454001874,
-1.75861248814167));
#79149=CARTESIAN_POINT('Ctrl Pts',(0.904593519871397,-3.46747596893911,
-1.85956712037717));
#79150=CARTESIAN_POINT('Ctrl Pts',(0.910312116074138,-3.4109522850809,-1.95803307145241));
#79151=CARTESIAN_POINT('Ctrl Pts',(0.916032194932967,-3.35441394637017,
-2.0565245517199));
#79152=CARTESIAN_POINT('Ctrl Pts',(0.921752273791793,-3.29362852544886,
-2.1525256944756));
#79153=CARTESIAN_POINT('Ctrl Pts',(0.927472352650621,-3.22886178257336,
-2.24564925779544));
#79154=CARTESIAN_POINT('Ctrl Pts',(0.933198659375992,-3.16402452342685,
-2.3388742115224));
#79155=CARTESIAN_POINT('Ctrl Pts',(0.938924966101368,-3.09519754230098,
-2.42921498008899));
#79156=CARTESIAN_POINT('Ctrl Pts',(0.944651272826739,-3.02268793654951,
-2.51631608472347));
#79157=CARTESIAN_POINT('Ctrl Pts',(0.950381294483434,-2.95013129032003,
-2.60347369604497));
#79158=CARTESIAN_POINT('Ctrl Pts',(0.956111316140125,-2.87388755933752,
-2.68738714521717));
#79159=CARTESIAN_POINT('Ctrl Pts',(0.96184133779682,-2.79430046944768,-2.76773804512719));
#79160=CARTESIAN_POINT('Ctrl Pts',(0.967579836774316,-2.71459563387847,
-2.84820782074067));
#79161=CARTESIAN_POINT('Ctrl Pts',(0.973318335751806,-2.63153789155595,
-2.92510424442966));
#79162=CARTESIAN_POINT('Ctrl Pts',(0.979056834729302,-2.54550357690634,
-2.99814951927969));
#79163=CARTESIAN_POINT('Ctrl Pts',(0.980536035645958,-2.5233266910007,-3.01697824747834));
#79164=CARTESIAN_POINT('Ctrl Pts',(0.982015236562617,-2.50095217360799,
-3.03555131633519));
#79165=CARTESIAN_POINT('Ctrl Pts',(0.983494437479273,-2.47838675880302,
-3.05386444915125));
#79166=CARTESIAN_POINT('Ctrl Pts',(0.989375340371957,-2.38867277086066,
-3.12667251365377));
#79167=CARTESIAN_POINT('Ctrl Pts',(0.995256243264646,-2.29559995768826,
-3.19564383824247));
#79168=CARTESIAN_POINT('Ctrl Pts',(1.00113714615733,-2.19953006256088,-3.26045341998485));
#79169=CARTESIAN_POINT('Ctrl Pts',(1.00701044555888,-2.10358437737356,-3.32517920862792));
#79170=CARTESIAN_POINT('Ctrl Pts',(1.01288374496043,-2.00464965514114,-3.38575372729037));
#79171=CARTESIAN_POINT('Ctrl Pts',(1.01875704436198,-1.90312105332842,-3.44189181357842));
#79172=CARTESIAN_POINT('Ctrl Pts',(1.02462430792401,-1.80169678986217,-3.49797220819148));
#79173=CARTESIAN_POINT('Ctrl Pts',(1.03049157148602,-1.69768430773464,-3.54962504138893));
#79174=CARTESIAN_POINT('Ctrl Pts',(1.03635883504804,-1.59150757477639,-3.59660849126359));
#79175=CARTESIAN_POINT('Ctrl Pts',(1.04244145259683,-1.48143369581434,-3.64531643725734));
#79176=CARTESIAN_POINT('Ctrl Pts',(1.04852407014562,-1.36903401549716,-3.68900539503127));
#79177=CARTESIAN_POINT('Ctrl Pts',(1.0546066876944,-1.25480907559537,-3.72745800563916));
#79178=CARTESIAN_POINT('Ctrl Pts',(1.06046709673469,-1.14475696972857,-3.7645058760702));
#79179=CARTESIAN_POINT('Ctrl Pts',(1.06632750577497,-1.03301105334662,-3.79669314223012));
#79180=CARTESIAN_POINT('Ctrl Pts',(1.07218791481525,-0.920038438947165,
-3.82387477185899));
#79181=CARTESIAN_POINT('Ctrl Pts',(1.07804739144925,-0.807083798783841,
-3.85105207682005));
#79182=CARTESIAN_POINT('Ctrl Pts',(1.08390686808325,-0.692903249131352,
-3.87322523260343));
#79183=CARTESIAN_POINT('Ctrl Pts',(1.08976634471724,-0.57797684805735,-3.89029970093689));
#79184=CARTESIAN_POINT('Ctrl Pts',(1.0956262962771,-0.463041131898891,-3.90737555320053));
#79185=CARTESIAN_POINT('Ctrl Pts',(1.10148624783695,-0.347359851667637,
-3.91935183596716));
#79186=CARTESIAN_POINT('Ctrl Pts',(1.10734619939681,-0.231420299174159,
-3.92618563559215));
#79187=CARTESIAN_POINT('Ctrl Pts',(1.11320803320733,-0.11544350621927,-3.9330216302735));
#79188=CARTESIAN_POINT('Ctrl Pts',(1.11906986701784,0.000791312908998643,
-3.93471183292274));
#79189=CARTESIAN_POINT('Ctrl Pts',(1.12493170082837,0.116795436012624,-3.93126542300652));
#79190=CARTESIAN_POINT('Ctrl Pts',(1.13080005434631,0.232928582382179,-3.92781517988979));
#79191=CARTESIAN_POINT('Ctrl Pts',(1.13666840786426,0.348830108527222,-3.91921693303263));
#79192=CARTESIAN_POINT('Ctrl Pts',(1.14253676138221,0.464014881146512,-3.90553187031864));
#79193=CARTESIAN_POINT('Ctrl Pts',(1.14840899313578,0.579275776256942,-3.89183776351798));
#79194=CARTESIAN_POINT('Ctrl Pts',(1.15428122488935,0.693818568909999,-3.87305021272871));
#79195=CARTESIAN_POINT('Ctrl Pts',(1.16015345664292,0.807168491414923,-3.84928149483341));
#79196=CARTESIAN_POINT('Ctrl Pts',(1.16603415994399,0.920681937652066,-3.82547848710911));
#79197=CARTESIAN_POINT('Ctrl Pts',(1.17191486324507,1.03299868141443,-3.7966800717954));
#79198=CARTESIAN_POINT('Ctrl Pts',(1.17779556654614,1.1436591919416,-3.76304831920711));
#79199=CARTESIAN_POINT('Ctrl Pts',(1.1793109297704,1.17217463634432,-3.75438195424523));
#79200=CARTESIAN_POINT('Ctrl Pts',(1.18082629299465,1.20058021115646,-3.74539489838777));
#79201=CARTESIAN_POINT('Ctrl Pts',(1.18234165621891,1.22886828704132,-3.73609043427807));
#79202=CARTESIAN_POINT('Ctrl Pts',(1.1882243843005,1.33868424120848,-3.69996996400009));
#79203=CARTESIAN_POINT('Ctrl Pts',(1.19410711238208,1.44708284648009,-3.65894555660818));
#79204=CARTESIAN_POINT('Ctrl Pts',(1.19998984046366,1.55359503319098,-3.61314703172239));
#79205=CARTESIAN_POINT('Ctrl Pts',(1.20586514879311,1.65997287848507,-3.56740627148223));
#79206=CARTESIAN_POINT('Ctrl Pts',(1.21174045712255,1.76446866236883,-3.51690353076491));
#79207=CARTESIAN_POINT('Ctrl Pts',(1.217615765452,1.86662890811831,-3.46181823892836));
#79208=CARTESIAN_POINT('Ctrl Pts',(1.22348521851548,1.96868734212001,-3.40678784447188));
#79209=CARTESIAN_POINT('Ctrl Pts',(1.22935467157896,2.0684145078154,-3.34718417793659));
#79210=CARTESIAN_POINT('Ctrl Pts',(1.23522412464244,2.16537794472313,-3.28323428291473));
#79211=CARTESIAN_POINT('Ctrl Pts',(1.24130598923895,2.26585042277286,-3.21697008448311));
#79212=CARTESIAN_POINT('Ctrl Pts',(1.24738785383545,2.36335493625515,-3.14603930720408));
#79213=CARTESIAN_POINT('Ctrl Pts',(1.25346971843196,2.45743907257205,-3.07074619670793));
#79214=CARTESIAN_POINT('Ctrl Pts',(1.2593327570952,2.54813805477908,-2.99816213783748));
#79215=CARTESIAN_POINT('Ctrl Pts',(1.26519579575845,2.63565820070237,-2.92152452934664));
#79216=CARTESIAN_POINT('Ctrl Pts',(1.27105883442169,2.71962534769648,-2.84114888173196));
#79217=CARTESIAN_POINT('Ctrl Pts',(1.27692109967458,2.80358141834184,-2.76078383670098));
#79218=CARTESIAN_POINT('Ctrl Pts',(1.28278336492747,2.88398512471447,-2.67668201764516));
#79219=CARTESIAN_POINT('Ctrl Pts',(1.28864563018036,2.96049787944984,-2.58919703880817));
#79220=CARTESIAN_POINT('Ctrl Pts',(1.29450852716744,3.03701887941485,-2.50170263234381));
#79221=CARTESIAN_POINT('Ctrl Pts',(1.30037142415452,3.10964782302408,-2.41082465108394));
#79222=CARTESIAN_POINT('Ctrl Pts',(1.3062343211416,3.178085723247,-2.31695061140578));
#79223=CARTESIAN_POINT('Ctrl Pts',(1.31209925511507,3.24654740131754,-2.22304395642814));
#79224=CARTESIAN_POINT('Ctrl Pts',(1.31796418908855,3.31081489785301,-2.12613950537412));
#79225=CARTESIAN_POINT('Ctrl Pts',(1.32382912306202,3.37063234323854,-2.02665404218734));
#79226=CARTESIAN_POINT('Ctrl Pts',(1.32970079216489,3.4305184813386,-1.92705433262179));
#79227=CARTESIAN_POINT('Ctrl Pts',(1.33557246126776,3.48594415583052,-1.8248680478289));
#79228=CARTESIAN_POINT('Ctrl Pts',(1.34144413037063,3.53669923705489,-1.72053698205396));
#79229=CARTESIAN_POINT('Ctrl Pts',(1.34731980744516,3.58748896344122,-1.61613470042075));
#79230=CARTESIAN_POINT('Ctrl Pts',(1.35319548451969,3.63360158470154,-1.50958509926003));
#79231=CARTESIAN_POINT('Ctrl Pts',(1.35907116159422,3.67487559543297,-1.40134876390253));
#79232=CARTESIAN_POINT('Ctrl Pts',(1.36495547492183,3.7162102719903,-1.29295333940975));
#79233=CARTESIAN_POINT('Ctrl Pts',(1.37083978824944,3.75269201467683,-1.18286662188127));
#79234=CARTESIAN_POINT('Ctrl Pts',(1.37672410157706,3.78420947000849,-1.07156319790203));
#79235=CARTESIAN_POINT('Ctrl Pts',(1.37821235937089,3.79218085017261,-1.04341238760437));
#79236=CARTESIAN_POINT('Ctrl Pts',(1.37970061716473,3.7998349301741,-1.01518378915294));
#79237=CARTESIAN_POINT('Ctrl Pts',(1.38118887495856,3.80717043128948,-0.986885153964277));
#79238=CARTESIAN_POINT('Ctrl Pts',(1.38705348940439,3.83607663691244,-0.875371822462174));
#79239=CARTESIAN_POINT('Ctrl Pts',(1.3929181038502,3.86012892210552,-0.762395905546755));
#79240=CARTESIAN_POINT('Ctrl Pts',(1.39878271829603,3.87918063792592,-0.648418520972878));
#79241=CARTESIAN_POINT('Ctrl Pts',(1.40463962831864,3.8982073252499,-0.534590870028694));
#79242=CARTESIAN_POINT('Ctrl Pts',(1.41049653834125,3.9122464385708,-0.419764772610415));
#79243=CARTESIAN_POINT('Ctrl Pts',(1.41635344836386,3.9212013774418,-0.304415435792203));
#79244=CARTESIAN_POINT('Ctrl Pts',(1.42220424217116,3.93014696490839,-0.189186555217397));
#79245=CARTESIAN_POINT('Ctrl Pts',(1.42805503597846,3.93401890569487,-0.0734359327945867));
#79246=CARTESIAN_POINT('Ctrl Pts',(1.43390582978577,3.93277195371724,0.0423528045715599));
#79247=CARTESIAN_POINT('Ctrl Pts',(1.43999459078212,3.93147428491951,0.162850974753455));
#79248=CARTESIAN_POINT('Ctrl Pts',(1.44608335177847,3.92463242110289,0.283389975391991));
#79249=CARTESIAN_POINT('Ctrl Pts',(1.45217211277483,3.91225522049489,0.403420487469947));
#79250=CARTESIAN_POINT('Ctrl Pts',(1.45801595739492,3.90037588457939,0.518622851739805));
#79251=CARTESIAN_POINT('Ctrl Pts',(1.463859802015,3.88339795179009,0.633356390142418));
#79252=CARTESIAN_POINT('Ctrl Pts',(1.4697036466351,3.86138234699156,0.747138119989815));
#79253=CARTESIAN_POINT('Ctrl Pts',(1.47554655267681,3.83937027811365,0.860901575382912));
#79254=CARTESIAN_POINT('Ctrl Pts',(1.48138945871854,3.81232222460642,0.973713119198366));
#79255=CARTESIAN_POINT('Ctrl Pts',(1.48723236476025,3.78035043649894,1.08509887902544));
#79256=CARTESIAN_POINT('Ctrl Pts',(1.4930757575243,3.7483759850963,1.19649391744383));
#79257=CARTESIAN_POINT('Ctrl Pts',(1.49891915028835,3.71147709824281,1.30646253723765));
#79258=CARTESIAN_POINT('Ctrl Pts',(1.5047625430524,3.66981600672843,1.41454567856955));
#79259=CARTESIAN_POINT('Ctrl Pts',(1.51060784785759,3.62814128311296,1.522664186241));
#79260=CARTESIAN_POINT('Ctrl Pts',(1.51645315266278,3.58170140563401,1.62889560209278));
#79261=CARTESIAN_POINT('Ctrl Pts',(1.52229845746796,3.53070659277404,1.73280118759825));
#79262=CARTESIAN_POINT('Ctrl Pts',(1.52815041052508,3.47965378013918,1.83682495180135));
#79263=CARTESIAN_POINT('Ctrl Pts',(1.5340023635822,3.42403587471379,1.9385172333325));
#79264=CARTESIAN_POINT('Ctrl Pts',(1.53985431663932,3.36410891449219,2.03746416199995));
#79265=CARTESIAN_POINT('Ctrl Pts',(1.54571020270278,3.30414167829566,2.13647759135431));
#79266=CARTESIAN_POINT('Ctrl Pts',(1.55156608876624,3.23985985082548,2.23274165019659));
#79267=CARTESIAN_POINT('Ctrl Pts',(1.5574219748297,3.17156160540978,2.32587316573594));
#79268=CARTESIAN_POINT('Ctrl Pts',(1.56328654009602,3.10316213290043,2.41914271458182));
#79269=CARTESIAN_POINT('Ctrl Pts',(1.56915110536234,3.03073462069176,2.50927013216155));
#79270=CARTESIAN_POINT('Ctrl Pts',(1.57501567062866,2.95461616807978,2.59590683563983));
#79271=CARTESIAN_POINT('Ctrl Pts',(1.57668914498518,2.93289549950179,2.62062892415276));
#79272=CARTESIAN_POINT('Ctrl Pts',(1.57836261934168,2.91087450860319,2.64506701647413));
#79273=CARTESIAN_POINT('Ctrl Pts',(1.5800360936982,2.88856153455991,2.6692136034909));
#79274=CARTESIAN_POINT('Ctrl Pts',(1.58591017028305,2.81024057442334,2.75397074413504));
#79275=CARTESIAN_POINT('Ctrl Pts',(1.59178424686792,2.72805535120082,2.83541916327497));
#79276=CARTESIAN_POINT('Ctrl Pts',(1.59765832345277,2.64231648922465,2.91318598286678));
#79277=CARTESIAN_POINT('Ctrl Pts',(1.60352479877662,2.55668857634133,2.99085216946804));
#79278=CARTESIAN_POINT('Ctrl Pts',(1.60939127410046,2.46751647285204,3.0648459558061));
#79279=CARTESIAN_POINT('Ctrl Pts',(1.61525774942431,2.37514960216785,3.13482908103806));
#79280=CARTESIAN_POINT('Ctrl Pts',(1.62111819982907,2.28287759303025,3.20474033301669));
#79281=CARTESIAN_POINT('Ctrl Pts',(1.62697865023383,2.18741767027199,3.27064886890375));
#79282=CARTESIAN_POINT('Ctrl Pts',(1.63283910063859,2.08915399344872,3.33225518105341));
#79283=CARTESIAN_POINT('Ctrl Pts',(1.63892427613023,1.98712229338737,3.39622385153625));
#79284=CARTESIAN_POINT('Ctrl Pts',(1.64500945162186,1.88206784372643,3.45555343979431));
#79285=CARTESIAN_POINT('Ctrl Pts',(1.6510946271135,1.77445623100745,3.50995642198572));
#79286=CARTESIAN_POINT('Ctrl Pts',(1.6569482966211,1.67093862220514,3.56228968310762));
#79287=CARTESIAN_POINT('Ctrl Pts',(1.6628019661287,1.56505526984246,3.61006414650832));
#79288=CARTESIAN_POINT('Ctrl Pts',(1.66865563563629,1.45724693615371,3.65306999208482));
#79289=CARTESIAN_POINT('Ctrl Pts',(1.67450841228232,1.34945504649512,3.69606927796973));
#79290=CARTESIAN_POINT('Ctrl Pts',(1.68036118892835,1.23973914291635,3.73430123926779));
#79291=CARTESIAN_POINT('Ctrl Pts',(1.68621396557439,1.12856000089635,3.76760418892123));
#79292=CARTESIAN_POINT('Ctrl Pts',(1.69206726446448,1.01737093834614,3.80091011020148));
#79293=CARTESIAN_POINT('Ctrl Pts',(1.69792056335458,0.904718773547644,3.82928602697692));
#79294=CARTESIAN_POINT('Ctrl Pts',(1.70377386224468,0.79107878826895,3.85262032268311));
#79295=CARTESIAN_POINT('Ctrl Pts',(1.70962909851816,0.677401189291951,3.87596234180775));
#79296=CARTESIAN_POINT('Ctrl Pts',(1.71548433479164,0.562735524128474,3.89425933861837));
#79297=CARTESIAN_POINT('Ctrl Pts',(1.72133957106511,0.447565888134444,3.90745105865428));
#79298=CARTESIAN_POINT('Ctrl Pts',(1.72720144344763,0.332265723118647,3.9206577296996));
#79299=CARTESIAN_POINT('Ctrl Pts',(1.73306331583015,0.216460857861962,3.9287475279576));
#79300=CARTESIAN_POINT('Ctrl Pts',(1.73892518821268,0.100639218276715,3.93171219034973));
#79301=CARTESIAN_POINT('Ctrl Pts',(1.7447909989767,-0.0152602377079235,
3.93467884459202));
#79302=CARTESIAN_POINT('Ctrl Pts',(1.75065680974071,-0.131176078438516,
3.93251351403517));
#79303=CARTESIAN_POINT('Ctrl Pts',(1.75652262050473,-0.246623416349175,
3.92525997744204));
#79304=CARTESIAN_POINT('Ctrl Pts',(1.76239704144614,-0.362240214561096,
3.91799579368701));
#79305=CARTESIAN_POINT('Ctrl Pts',(1.76827146238757,-0.47738672824052,3.9056285415912));
#79306=CARTESIAN_POINT('Ctrl Pts',(1.77414588332898,-0.591586112199691,
3.88825344748159));
#79307=CARTESIAN_POINT('Ctrl Pts',(1.77572502636527,-0.622284825098546,
3.88358273029232));
#79308=CARTESIAN_POINT('Ctrl Pts',(1.77730416940156,-0.652915171796896,
3.87855041553838));
#79309=CARTESIAN_POINT('Ctrl Pts',(1.77888331243784,-0.68346807235756,3.87315896834455));
#79310=CARTESIAN_POINT('Ctrl Pts',(1.78475698171083,-0.79711049049179,3.85310532089681));
#79311=CARTESIAN_POINT('Ctrl Pts',(1.79063065098381,-0.910058892662766,
3.82801245027434));
#79312=CARTESIAN_POINT('Ctrl Pts',(1.79650432025679,-1.02183170271352,3.79794009580583));
#79313=CARTESIAN_POINT('Ctrl Pts',(1.80237040603293,-1.13346020284273,3.76790656776668));
#79314=CARTESIAN_POINT('Ctrl Pts',(1.80823649180907,-1.2439157339494,3.73290644742008));
#79315=CARTESIAN_POINT('Ctrl Pts',(1.81410257758521,-1.35272486981782,3.69305082913522));
#79316=CARTESIAN_POINT('Ctrl Pts',(1.81996265661022,-1.46142258736996,3.65323602218342));
#79317=CARTESIAN_POINT('Ctrl Pts',(1.82582273563522,-1.56847687738249,3.60857574810993));
#79318=CARTESIAN_POINT('Ctrl Pts',(1.83168281466022,-1.67342814022944,3.55923127367248));
#79319=CARTESIAN_POINT('Ctrl Pts',(1.83776813618178,-1.7824133903927,3.50799015713077));
#79320=CARTESIAN_POINT('Ctrl Pts',(1.84385345770332,-1.8891302631675,3.45169764004533));
#79321=CARTESIAN_POINT('Ctrl Pts',(1.84993877922487,-1.99308510711857,3.39059003062626));
#79322=CARTESIAN_POINT('Ctrl Pts',(1.85579212552627,-2.09307714520534,3.33181187103131));
#79323=CARTESIAN_POINT('Ctrl Pts',(1.86164547182768,-2.19051349141098,3.26857923608651));
#79324=CARTESIAN_POINT('Ctrl Pts',(1.86749881812908,-2.28497940652602,3.20114949850081));
#79325=CARTESIAN_POINT('Ctrl Pts',(1.87335129001247,-2.37943120959433,3.1337298340892));
#79326=CARTESIAN_POINT('Ctrl Pts',(1.87920376189587,-2.47091312770396,3.06211455368878));
#79327=CARTESIAN_POINT('Ctrl Pts',(1.88505623377926,-2.55904010084445,2.98660388439278));
#79328=CARTESIAN_POINT('Ctrl Pts',(1.89090924677398,-2.64717522208095,2.91108623348647));
#79329=CARTESIAN_POINT('Ctrl Pts',(1.8967622597687,-2.73195446793767,2.83167274653416));
#79330=CARTESIAN_POINT('Ctrl Pts',(1.90261527276342,-2.81302706473549,2.74870291829903));
#79331=CARTESIAN_POINT('Ctrl Pts',(1.90847024244689,-2.89412676446951,2.66570535287465));
#79332=CARTESIAN_POINT('Ctrl Pts',(1.91432521213035,-2.97151706253956,2.57914937741913));
#79333=CARTESIAN_POINT('Ctrl Pts',(1.92018018181382,-3.04488563559911,2.48940966217338));
#79334=CARTESIAN_POINT('Ctrl Pts',(1.92604181781465,-3.1183377442224,2.39956777160393));
#79335=CARTESIAN_POINT('Ctrl Pts',(1.93190345381548,-3.18775872655857,2.30653522604996));
#79336=CARTESIAN_POINT('Ctrl Pts',(1.93776508981632,-3.25287793121025,2.21071802015664));
#79337=CARTESIAN_POINT('Ctrl Pts',(1.94363068151742,-3.3180410812818,2.11483615242715));
#79338=CARTESIAN_POINT('Ctrl Pts',(1.94949627321853,-3.3788964567285,2.01616623321353));
#79339=CARTESIAN_POINT('Ctrl Pts',(1.95536186491963,-3.43521883526877,1.91513982617841));
#79340=CARTESIAN_POINT('Ctrl Pts',(1.96123609408465,-3.49162415216157,1.81396465121162));
#79341=CARTESIAN_POINT('Ctrl Pts',(1.96711032324967,-3.54348296555399,1.71042643083464));
#79342=CARTESIAN_POINT('Ctrl Pts',(1.97298455241469,-3.59061768585969,1.60497776744466));
#79343=CARTESIAN_POINT('Ctrl Pts',(1.97456654533562,-3.6033115716035,1.57657931135477));
#79344=CARTESIAN_POINT('Ctrl Pts',(1.97614853825655,-3.61566310577279,1.548042382819));
#79345=CARTESIAN_POINT('Ctrl Pts',(1.97773053117749,-3.62766943983772,1.51937600193879));
#79346=CARTESIAN_POINT('Ctrl Pts',(1.98430602295599,-3.6775732983755,1.40022530960424));
#79347=CARTESIAN_POINT('Ctrl Pts',(1.9908815147345,-3.72165215810053,1.2784965980874));
#79348=CARTESIAN_POINT('Ctrl Pts',(1.99745700651301,-3.75966149616237,1.15474431554094));
#79349=CARTESIAN_POINT('Ctrl Pts',(2.00397687500376,-3.79734930628078,1.03203887618966));
#79350=CARTESIAN_POINT('Ctrl Pts',(2.0104967434945,-3.82906975507951,0.907344193337815));
#79351=CARTESIAN_POINT('Ctrl Pts',(2.01701661198525,-3.854630735699,0.781223970065293));
#79352=CARTESIAN_POINT('Ctrl Pts',(2.02361991540764,-3.88051882087186,0.65348978291872));
#79353=CARTESIAN_POINT('Ctrl Pts',(2.03022321883004,-3.90008851960739,0.524293517975706));
#79354=CARTESIAN_POINT('Ctrl Pts',(2.03682652225243,-3.91319083428004,0.394241670180517));
#79355=CARTESIAN_POINT('Ctrl Pts',(2.04342982567482,-3.92629314895268,0.26418982238533));
#79356=CARTESIAN_POINT('Ctrl Pts',(2.05003312909721,-3.93292792584975,0.133282638315857));
#79357=CARTESIAN_POINT('Ctrl Pts',(2.0566364325196,-3.9329994155864,0.00214406087016673));
#79358=CARTESIAN_POINT('',(3.30663650988561,-3.93223110072523,-0.00324727255823224));
#79359=CARTESIAN_POINT('Ctrl Pts',(2.0566364779651,-3.92760797316549,0.00214022045425887));
#79360=CARTESIAN_POINT('Ctrl Pts',(2.09661690194911,-3.92376833228284,-0.790766574382641));
#79361=CARTESIAN_POINT('Ctrl Pts',(2.20287973217967,-3.30533753684168,-2.90375943243531));
#79362=CARTESIAN_POINT('Ctrl Pts',(2.37542496865678,0.147023520660857,-4.64930955531007));
#79363=CARTESIAN_POINT('Ctrl Pts',(2.57427218739642,3.9905524730503,-2.3902958242871));
#79364=CARTESIAN_POINT('Ctrl Pts',(2.77311940613606,4.16846304929326,2.06445390521175));
#79365=CARTESIAN_POINT('Ctrl Pts',(2.97196662487571,0.517297643089777,4.62280760769746));
#79366=CARTESIAN_POINT('Ctrl Pts',(3.14980564881872,-3.17309355288368,3.11310308288762));
#79367=CARTESIAN_POINT('Ctrl Pts',(3.26136226651518,-3.9229062319681,0.893358099881881));
#79368=CARTESIAN_POINT('Ctrl Pts',(3.30663647796509,-3.92984741018714,-0.00324467181678128));
#79369=CARTESIAN_POINT('',(4.55663647792001,-3.93299992902536,-0.000747185703456276));
#79370=CARTESIAN_POINT('Ctrl Pts',(3.30663652016415,-3.93299865875662,-0.00324811000753884));
#79371=CARTESIAN_POINT('Ctrl Pts',(3.31356358509945,-3.93288527511355,-0.140539554911472));
#79372=CARTESIAN_POINT('Ctrl Pts',(3.32049065003477,-3.92557928781996,-0.27752307573409));
#79373=CARTESIAN_POINT('Ctrl Pts',(3.32741771497007,-3.91120026655955,-0.413523245857523));
#79374=CARTESIAN_POINT('Ctrl Pts',(3.33445827286756,-3.89658565955951,-0.55175164139948));
#79375=CARTESIAN_POINT('Ctrl Pts',(3.34149883076505,-3.87466438934153,-0.688964114611102));
#79376=CARTESIAN_POINT('Ctrl Pts',(3.34853938866253,-3.84561221477454,-0.824472979288515));
#79377=CARTESIAN_POINT('Ctrl Pts',(3.35557994656002,-3.81656004020754,-0.95998184396593));
#79378=CARTESIAN_POINT('Ctrl Pts',(3.36262050445751,-3.7803770898771,-1.09378708058283));
#79379=CARTESIAN_POINT('Ctrl Pts',(3.369661062355,-3.73728746254593,-1.22522300920975));
#79380=CARTESIAN_POINT('Ctrl Pts',(3.37553351744045,-3.70134685885581,-1.33485233102118));
#79381=CARTESIAN_POINT('Ctrl Pts',(3.3814059725259,-3.66051820663356,-1.44308243253663));
#79382=CARTESIAN_POINT('Ctrl Pts',(3.38727842761135,-3.61492857934629,-1.54944518012914));
#79383=CARTESIAN_POINT('Ctrl Pts',(3.39314327559298,-3.56939800828382,-1.65567014676781));
#79384=CARTESIAN_POINT('Ctrl Pts',(3.39900812357461,-3.51911888808148,-1.76003219348437));
#79385=CARTESIAN_POINT('Ctrl Pts',(3.40487297155624,-3.46426798301453,-1.862078500456));
#79386=CARTESIAN_POINT('Ctrl Pts',(3.41073179078696,-3.40947346175243,-1.96401990926685));
#79387=CARTESIAN_POINT('Ctrl Pts',(3.41659061001768,-3.35011669781919,-2.06364995128611));
#79388=CARTESIAN_POINT('Ctrl Pts',(3.4224494292484,-3.28642217370034,-2.16053657599466));
#79389=CARTESIAN_POINT('Ctrl Pts',(3.42853521474199,-3.2202601714881,-2.26117651587933));
#79390=CARTESIAN_POINT('Ctrl Pts',(3.43462100023558,-3.14941770805553,-2.35885576629735));
#79391=CARTESIAN_POINT('Ctrl Pts',(3.44070678572918,-3.0741986320021,-2.45311878452642));
#79392=CARTESIAN_POINT('Ctrl Pts',(3.44655882504513,-3.00186861136011,-2.54376129719758));
#79393=CARTESIAN_POINT('Ctrl Pts',(3.45241086436109,-2.92549225713851,-2.63124480923989));
#79394=CARTESIAN_POINT('Ctrl Pts',(3.45826290367704,-2.84538287023236,-2.71519526402582));
#79395=CARTESIAN_POINT('Ctrl Pts',(3.46411405332442,-2.76528566212415,-2.79913295606739));
#79396=CARTESIAN_POINT('Ctrl Pts',(3.46996520297179,-2.68145683503781,-2.87953835985712));
#79397=CARTESIAN_POINT('Ctrl Pts',(3.47581635261917,-2.59424791964966,-2.95607285623907));
#79398=CARTESIAN_POINT('Ctrl Pts',(3.4816680294769,-2.50703114641373,-3.03261424866392));
#79399=CARTESIAN_POINT('Ctrl Pts',(3.48751970633462,-2.41643399014157,-3.10528376766225));
#79400=CARTESIAN_POINT('Ctrl Pts',(3.49337138319235,-2.32284200753851,-3.17378228743159));
#79401=CARTESIAN_POINT('Ctrl Pts',(3.49922500417839,-2.22921893045997,-3.24230356476502));
#79402=CARTESIAN_POINT('Ctrl Pts',(3.50507862516442,-2.13259938197047,-3.30665084339127));
#79403=CARTESIAN_POINT('Ctrl Pts',(3.51093224615046,-2.03339830286724,-3.36656803613066));
#79404=CARTESIAN_POINT('Ctrl Pts',(3.5167925215223,-1.93408445215563,-3.42655334262703));
#79405=CARTESIAN_POINT('Ctrl Pts',(3.52265279689415,-1.83218356734116,-3.48209829748689));
#79406=CARTESIAN_POINT('Ctrl Pts',(3.52851307226599,-1.72813570276538,-3.53299249826936));
#79407=CARTESIAN_POINT('Ctrl Pts',(3.53437729470334,-1.62401775893387,-3.58392097777276));
#79408=CARTESIAN_POINT('Ctrl Pts',(3.54024151714069,-1.51775033401841,-3.63019230130826));
#79409=CARTESIAN_POINT('Ctrl Pts',(3.54610573957803,-1.4097923649181,-3.67164465707381));
#79410=CARTESIAN_POINT('Ctrl Pts',(3.55197859733777,-1.30167542301653,-3.7131580532347));
#79411=CARTESIAN_POINT('Ctrl Pts',(3.55785145509751,-1.19186335917039,-3.74983818867805));
#79412=CARTESIAN_POINT('Ctrl Pts',(3.56372431285725,-1.08082919488469,-3.78157338306225));
#79413=CARTESIAN_POINT('Ctrl Pts',(3.56531896893638,-1.05068010694269,-3.79019043505252));
#79414=CARTESIAN_POINT('Ctrl Pts',(3.56691362501551,-1.02044096452048,-3.79844319705715));
#79415=CARTESIAN_POINT('Ctrl Pts',(3.56850828109464,-0.990121329568143,
-3.80633008982855));
#79416=CARTESIAN_POINT('Ctrl Pts',(3.57438072828865,-0.878466874711392,
-3.83537419653658));
#79417=CARTESIAN_POINT('Ctrl Pts',(3.58025317548266,-0.765346438429972,
-3.85954987543601));
#79418=CARTESIAN_POINT('Ctrl Pts',(3.58612562267666,-0.651222527430752,
-3.87871089664681));
#79419=CARTESIAN_POINT('Ctrl Pts',(3.59199046272136,-0.537246452180766,
-3.89784709673202));
#79420=CARTESIAN_POINT('Ctrl Pts',(3.59785530276606,-0.422269891140721,
-3.91198148949371));
#79421=CARTESIAN_POINT('Ctrl Pts',(3.60372014281076,-0.306769337349473,
-3.92101792570018));
#79422=CARTESIAN_POINT('Ctrl Pts',(3.60957895406889,-0.191387512829826,
-3.93004507286471));
#79423=CARTESIAN_POINT('Ctrl Pts',(3.61543776532703,-0.0754831765679285,
-3.93398465499945));
#79424=CARTESIAN_POINT('Ctrl Pts',(3.62129657658517,0.040458847897597,-3.93279189401458));
#79425=CARTESIAN_POINT('Ctrl Pts',(3.62738236505388,0.160892602194006,-3.93155292407208));
#79426=CARTESIAN_POINT('Ctrl Pts',(3.63346815352259,0.281366575838322,-3.9247758271046));
#79427=CARTESIAN_POINT('Ctrl Pts',(3.63955394199131,0.401333266375885,-3.91246988605664));
#79428=CARTESIAN_POINT('Ctrl Pts',(3.64540597329665,0.516691996347188,-3.90063662030567));
#79429=CARTESIAN_POINT('Ctrl Pts',(3.651258004602,0.631581244978,-3.88369145141041));
#79430=CARTESIAN_POINT('Ctrl Pts',(3.65711003590734,0.745516948544496,-3.8616956741091));
#79431=CARTESIAN_POINT('Ctrl Pts',(3.66296117754383,0.859435330766979,-3.83970324076769));
#79432=CARTESIAN_POINT('Ctrl Pts',(3.66881231918033,0.972400050410675,-3.81266180405009));
#79433=CARTESIAN_POINT('Ctrl Pts',(3.67466346081681,1.08393618279765,-3.78068397933788));
#79434=CARTESIAN_POINT('Ctrl Pts',(3.68051512967199,1.19548236517773,-3.74870327325519));
#79435=CARTESIAN_POINT('Ctrl Pts',(3.68636679852716,1.30559930703886,-3.71178540889549));
#79436=CARTESIAN_POINT('Ctrl Pts',(3.69221846738233,1.41382690762245,-3.67009297910594));
#79437=CARTESIAN_POINT('Ctrl Pts',(3.69807208038277,1.52209046549996,-3.62838669751755));
#79438=CARTESIAN_POINT('Ctrl Pts',(3.7039256933832,1.62846304841473,-3.58190284477065));
#79439=CARTESIAN_POINT('Ctrl Pts',(3.70977930638364,1.73250487179925,-3.53085200329777));
#79440=CARTESIAN_POINT('Ctrl Pts',(3.7156395738357,1.83666497107257,-3.47974312666698));
#79441=CARTESIAN_POINT('Ctrl Pts',(3.72149984128775,1.93848865092629,-3.42405708083812));
#79442=CARTESIAN_POINT('Ctrl Pts',(3.72736010873981,2.03756097805657,-3.36405027618512));
#79443=CARTESIAN_POINT('Ctrl Pts',(3.73322432328592,2.13670003384666,-3.30400305486108));
#79444=CARTESIAN_POINT('Ctrl Pts',(3.73908853783204,2.2330837040564,-3.23962950897484));
#79445=CARTESIAN_POINT('Ctrl Pts',(3.74495275237815,2.32632772029525,-3.17122820651336));
#79446=CARTESIAN_POINT('Ctrl Pts',(3.75082560235005,2.41970904422912,-3.10272617881978));
#79447=CARTESIAN_POINT('Ctrl Pts',(3.75669845232195,2.50994116598464,-3.03018481522649));
#79448=CARTESIAN_POINT('Ctrl Pts',(3.76257130229385,2.59667437253834,-2.95394163838804));
#79449=CARTESIAN_POINT('Ctrl Pts',(3.76416603480732,2.62022618556797,-2.93323832166502));
#79450=CARTESIAN_POINT('Ctrl Pts',(3.7657607673208,2.64352022341602,-2.91226224876372));
#79451=CARTESIAN_POINT('Ctrl Pts',(3.76735549983428,2.66654998642768,-2.89102061042161));
#79452=CARTESIAN_POINT('Ctrl Pts',(3.77322794292317,2.75135478691542,-2.81280040030813));
#79453=CARTESIAN_POINT('Ctrl Pts',(3.77910038601206,2.83285690181505,-2.73071458870866));
#79454=CARTESIAN_POINT('Ctrl Pts',(3.78497282910096,2.91068323909851,-2.6450731713189));
#79455=CARTESIAN_POINT('Ctrl Pts',(3.79083766495501,2.98840875918961,-2.55954269487216));
#79456=CARTESIAN_POINT('Ctrl Pts',(3.79670250080907,3.06246769545385,-2.47046607537385));
#79457=CARTESIAN_POINT('Ctrl Pts',(3.80256733666312,3.13252152151712,-2.37819215313482));
#79458=CARTESIAN_POINT('Ctrl Pts',(3.80842614365053,3.20250333445235,-2.28601308558327));
#79459=CARTESIAN_POINT('Ctrl Pts',(3.81428495063794,3.26848797793113,-2.19064358002084));
#79460=CARTESIAN_POINT('Ctrl Pts',(3.82014375762535,3.33017563498916,-2.0924672614224));
#79461=CARTESIAN_POINT('Ctrl Pts',(3.82622954766487,3.39425320738438,-1.9904873765879));
#79462=CARTESIAN_POINT('Ctrl Pts',(3.8323153377044,3.45369380440183,-1.88547913208565));
#79463=CARTESIAN_POINT('Ctrl Pts',(3.83840112774392,3.50820919364773,-1.77790811168787));
#79464=CARTESIAN_POINT('Ctrl Pts',(3.84425315460459,3.56063057527853,-1.67446903529696));
#79465=CARTESIAN_POINT('Ctrl Pts',(3.85010518146526,3.60849793277353,-1.5686608332186));
#79466=CARTESIAN_POINT('Ctrl Pts',(3.85595720832593,3.65160108937571,-1.46092384608854));
#79467=CARTESIAN_POINT('Ctrl Pts',(3.86180834546086,3.69469769269496,-1.35320323898755));
#79468=CARTESIAN_POINT('Ctrl Pts',(3.86765948259579,3.73303138183604,-1.24355481358343));
#79469=CARTESIAN_POINT('Ctrl Pts',(3.87351061973073,3.76644009297464,-1.13243897232177));
#79470=CARTESIAN_POINT('Ctrl Pts',(3.87936228403202,3.79985181411765,-1.02131311992348));
#79471=CARTESIAN_POINT('Ctrl Pts',(3.88521394833331,3.82833755615214,-0.908719984724476));
#79472=CARTESIAN_POINT('Ctrl Pts',(3.89106561263461,3.85178531217261,-0.795134522537734));
#79473=CARTESIAN_POINT('Ctrl Pts',(3.89691922103335,3.87524085823717,-0.681511323871822));
#79474=CARTESIAN_POINT('Ctrl Pts',(3.9027728294321,3.89365500657552,-0.566895547275909));
#79475=CARTESIAN_POINT('Ctrl Pts',(3.90862643783084,3.90696710471404,-0.451771006907689));
#79476=CARTESIAN_POINT('Ctrl Pts',(3.91448670063306,3.9202943360945,-0.336515592540206));
#79477=CARTESIAN_POINT('Ctrl Pts',(3.92034696343528,3.92850789310142,-0.220750670868103));
#79478=CARTESIAN_POINT('Ctrl Pts',(3.9262072262375,3.93159911146462,-0.104963930617245));
#79479=CARTESIAN_POINT('Ctrl Pts',(3.93207143609996,3.93469241185476,0.0109007954259721));
#79480=CARTESIAN_POINT('Ctrl Pts',(3.93793564596241,3.9326565111082,0.126786957026716));
#79481=CARTESIAN_POINT('Ctrl Pts',(3.94379985582487,3.92553478914966,0.242209865975237));
#79482=CARTESIAN_POINT('Ctrl Pts',(3.94967270109944,3.91840258001458,0.357802742303846));
#79483=CARTESIAN_POINT('Ctrl Pts',(3.95554554637401,3.906169646254,0.472930595011592));
#79484=CARTESIAN_POINT('Ctrl Pts',(3.96141839164858,3.88893082125202,0.587116740960479));
#79485=CARTESIAN_POINT('Ctrl Pts',(3.96301316729036,3.88424960509175,0.618124076532006));
#79486=CARTESIAN_POINT('Ctrl Pts',(3.96460794293215,3.87919954224919,0.649062047781664));
#79487=CARTESIAN_POINT('Ctrl Pts',(3.96620271857393,3.87378316741701,0.679921298266663));
#79488=CARTESIAN_POINT('Ctrl Pts',(3.97207516613946,3.85383843264438,0.793554417331757));
#79489=CARTESIAN_POINT('Ctrl Pts',(3.977947613705,3.82885611548635,0.906499453759549));
#79490=CARTESIAN_POINT('Ctrl Pts',(3.98382006127053,3.79889525322836,1.01827494076947));
#79491=CARTESIAN_POINT('Ctrl Pts',(3.989684901662,3.76897320229934,1.12990563370905));
#79492=CARTESIAN_POINT('Ctrl Pts',(3.99554974205346,3.73408553749332,1.24036939451578));
#79493=CARTESIAN_POINT('Ctrl Pts',(4.00141458244493,3.69434266252296,1.34919282975518));
#79494=CARTESIAN_POINT('Ctrl Pts',(4.00727339402476,3.65464064157266,1.45790439903596));
#79495=CARTESIAN_POINT('Ctrl Pts',(4.0131322056046,3.6100934786871,1.56497861072361));
#79496=CARTESIAN_POINT('Ctrl Pts',(4.01899101718443,3.56086176930219,1.66995582573974));
#79497=CARTESIAN_POINT('Ctrl Pts',(4.02507680552314,3.50972276973085,1.77899997270889));
#79498=CARTESIAN_POINT('Ctrl Pts',(4.03116259386185,3.45352903145065,1.88578091814643));
#79499=CARTESIAN_POINT('Ctrl Pts',(4.03724838220057,3.39251635754362,1.98980445365844));
#79500=CARTESIAN_POINT('Ctrl Pts',(4.04310041376238,3.33384719695139,2.08983241702266));
#79501=CARTESIAN_POINT('Ctrl Pts',(4.04895244532419,3.2707226938025,2.18731049930099));
#79502=CARTESIAN_POINT('Ctrl Pts',(4.054804476886,3.20339962252632,2.28182380090976));
#79503=CARTESIAN_POINT('Ctrl Pts',(4.0606556187543,3.13608678648191,2.37632273351351));
#79504=CARTESIAN_POINT('Ctrl Pts',(4.0665067606226,3.06457689124168,2.46785744508208));
#79505=CARTESIAN_POINT('Ctrl Pts',(4.07235790249091,2.98916960253729,2.55604266147243));
#79506=CARTESIAN_POINT('Ctrl Pts',(4.07820957155287,2.91375551956173,2.64423582343785));
#79507=CARTESIAN_POINT('Ctrl Pts',(4.08406124061483,2.83444361370559,2.72907857610939));
#79508=CARTESIAN_POINT('Ctrl Pts',(4.0899129096768,2.75157285938732,2.81021988454339));
#79509=CARTESIAN_POINT('Ctrl Pts',(4.09576652285861,2.66867457263748,2.8913881508293));
#79510=CARTESIAN_POINT('Ctrl Pts',(4.10162013604041,2.5822153815549,2.96885223857184));
#79511=CARTESIAN_POINT('Ctrl Pts',(4.10747374922222,2.49256948012377,3.04229952285365));
#79512=CARTESIAN_POINT('Ctrl Pts',(4.11333401681674,2.40282166884527,3.11583030232498));
#79513=CARTESIAN_POINT('Ctrl Pts',(4.11919428441125,2.30988023643114,3.18533490199171));
#79514=CARTESIAN_POINT('Ctrl Pts',(4.12505455200577,2.21415074672552,3.25054233486888));
#79515=CARTESIAN_POINT('Ctrl Pts',(4.13091876667184,2.11835678024655,3.31579368696972));
#79516=CARTESIAN_POINT('Ctrl Pts',(4.13678298133791,2.01977136804527,3.37674189236581));
#79517=CARTESIAN_POINT('Ctrl Pts',(4.14264719600398,1.91882569072704,3.43316136652588));
#79518=CARTESIAN_POINT('Ctrl Pts',(4.14852004606164,1.81773136512377,3.48966392158946));
#79519=CARTESIAN_POINT('Ctrl Pts',(4.1543928961193,1.71427020574622,3.5416242509723));
#79520=CARTESIAN_POINT('Ctrl Pts',(4.16026574617696,1.60889448067025,3.58886438167686));
#79521=CARTESIAN_POINT('Ctrl Pts',(4.16186047655583,1.58028045710011,3.60169210089267));
#79522=CARTESIAN_POINT('Ctrl Pts',(4.1634552069347,1.55152535239075,3.61417205672211));
#79523=CARTESIAN_POINT('Ctrl Pts',(4.16504993731357,1.52263840700106,3.62630132249449));
#79524=CARTESIAN_POINT('Ctrl Pts',(4.17092238347021,1.41626491987186,3.67096621451127));
#79525=CARTESIAN_POINT('Ctrl Pts',(4.17679482962686,1.30774638193382,3.71102139669462));
#79526=CARTESIAN_POINT('Ctrl Pts',(4.18266727578351,1.19751972912854,3.74625619763891));
#79527=CARTESIAN_POINT('Ctrl Pts',(4.18853211475511,1.08743586427276,3.78144535531226));
#79528=CARTESIAN_POINT('Ctrl Pts',(4.19439695372671,0.975648674918339,3.81182642481333));
#79529=CARTESIAN_POINT('Ctrl Pts',(4.20026179269831,0.862616080010135,3.83723630996424));
#79530=CARTESIAN_POINT('Ctrl Pts',(4.20612060284905,0.749699678107125,3.86262007476535));
#79531=CARTESIAN_POINT('Ctrl Pts',(4.2119794129998,0.635540817963619,3.88304272952699));
#79532=CARTESIAN_POINT('Ctrl Pts',(4.21783822315054,0.520612987435137,3.89839083691128));
#79533=CARTESIAN_POINT('Ctrl Pts',(4.22392401202149,0.401232687682143,3.91433355202));
#79534=CARTESIAN_POINT('Ctrl Pts',(4.23000980089243,0.281023063252718,3.92480043865746));
#79535=CARTESIAN_POINT('Ctrl Pts',(4.23609558976338,0.160527348097331,3.92972263277103));
#79536=CARTESIAN_POINT('Ctrl Pts',(4.24194761988218,0.0446599446712767,
3.9344557624957));
#79537=CARTESIAN_POINT('Ctrl Pts',(4.24779965000098,-0.0714715258643642,
3.9340622739106));
#79538=CARTESIAN_POINT('Ctrl Pts',(4.25365168011978,-0.187379205918145,
3.9285338274208));
#79539=CARTESIAN_POINT('Ctrl Pts',(4.25950282054239,-0.303269264288719,
3.92300622143209));
#79540=CARTESIAN_POINT('Ctrl Pts',(4.265353960965,-0.418935187051956,3.91234522946963));
#79541=CARTESIAN_POINT('Ctrl Pts',(4.27120510138761,-0.533890846026035,
3.89659461126374));
#79542=CARTESIAN_POINT('Ctrl Pts',(4.27705676900275,-0.648856862598774,
3.8808425739143));
#79543=CARTESIAN_POINT('Ctrl Pts',(4.28290843661789,-0.763112078610132,
3.86000005482292));
#79544=CARTESIAN_POINT('Ctrl Pts',(4.28876010423303,-0.876177913582972,
3.8341623940242));
#79545=CARTESIAN_POINT('Ctrl Pts',(4.29461371596842,-0.9892813128185,3.80831614908795));
#79546=CARTESIAN_POINT('Ctrl Pts',(4.3004673277038,-1.10119414252346,3.77747155456045));
#79547=CARTESIAN_POINT('Ctrl Pts',(4.30632093943919,-1.21145108949488,3.74177434618413));
#79548=CARTESIAN_POINT('Ctrl Pts',(4.31218120559523,-1.32183337721955,3.70603655700896));
#79549=CARTESIAN_POINT('Ctrl Pts',(4.31804147175126,-1.43055563147713,3.66543527067302));
#79550=CARTESIAN_POINT('Ctrl Pts',(4.3239017379073,-1.53717060325931,3.62016512558135));
#79551=CARTESIAN_POINT('Ctrl Pts',(4.32976595113772,-1.64385738359312,3.5748644896168));
#79552=CARTESIAN_POINT('Ctrl Pts',(4.33563016436815,-1.74843368325179,3.52488891111368));
#79553=CARTESIAN_POINT('Ctrl Pts',(4.34149437759857,-1.85047659493403,3.4704791270949));
#79554=CARTESIAN_POINT('Ctrl Pts',(4.34736722623593,-1.95266977094539,3.41598922139439));
#79555=CARTESIAN_POINT('Ctrl Pts',(4.35324007487329,-2.05232175906285,3.35705228796));
#79556=CARTESIAN_POINT('Ctrl Pts',(4.35911292351064,-2.14903830102412,3.29395254682446));
#79557=CARTESIAN_POINT('Ctrl Pts',(4.3607076676915,-2.17530121907452,3.27681811152685));
#79558=CARTESIAN_POINT('Ctrl Pts',(4.36230241187236,-2.20134787576329,3.25937695296744));
#79559=CARTESIAN_POINT('Ctrl Pts',(4.36389715605321,-2.22717081254393,3.24163526198621));
#79560=CARTESIAN_POINT('Ctrl Pts',(4.36974003646156,-2.32178180608944,3.17663262401477));
#79561=CARTESIAN_POINT('Ctrl Pts',(4.37558291686992,-2.41371090712612,3.10737017371693));
#79562=CARTESIAN_POINT('Ctrl Pts',(4.38142579727827,-2.50254700172264,3.03409747769729));
#79563=CARTESIAN_POINT('Ctrl Pts',(4.38726109196053,-2.59126776171811,2.96091991054617));
#79564=CARTESIAN_POINT('Ctrl Pts',(4.39309638664279,-2.67690317974983,2.88374271258626));
#79565=CARTESIAN_POINT('Ctrl Pts',(4.39893168132505,-2.75907060592688,2.80285896746702));
#79566=CARTESIAN_POINT('Ctrl Pts',(4.40476100216875,-2.84115391382613,2.72205802646686));
#79567=CARTESIAN_POINT('Ctrl Pts',(4.41059032301245,-2.91977599414055,2.6375583757563));
#79568=CARTESIAN_POINT('Ctrl Pts',(4.41641964385614,-2.99458740595752,2.54969317136016));
#79569=CARTESIAN_POINT('Ctrl Pts',(4.42226201194214,-3.06956626140006,2.46163130621363));
#79570=CARTESIAN_POINT('Ctrl Pts',(4.42810438002813,-3.1407170507501,2.37018908122731));
#79571=CARTESIAN_POINT('Ctrl Pts',(4.43394674811412,-3.20772511407505,2.27573913103681));
#79572=CARTESIAN_POINT('Ctrl Pts',(4.43976956158102,-3.27450889896778,2.1816053082749));
#79573=CARTESIAN_POINT('Ctrl Pts',(4.44559237504791,-3.33717740148251,2.08448420439446));
#79574=CARTESIAN_POINT('Ctrl Pts',(4.4514151885148,-3.39546011366069,1.98477696896638));
#79575=CARTESIAN_POINT('Ctrl Pts',(4.4572371989607,-3.45373478810213,1.88508348410822));
#79576=CARTESIAN_POINT('Ctrl Pts',(4.4630592094066,-3.50762466383906,1.78280493759554));
#79577=CARTESIAN_POINT('Ctrl Pts',(4.46888121985249,-3.55690388340501,1.6783693765731));
#79578=CARTESIAN_POINT('Ctrl Pts',(4.47470387391394,-3.60618855072346,1.57392227033761));
#79579=CARTESIAN_POINT('Ctrl Pts',(4.48052652797539,-3.65086137070472,1.46731805383295));
#79580=CARTESIAN_POINT('Ctrl Pts',(4.48634918203684,-3.69074389137489,1.35900644894677));
#79581=CARTESIAN_POINT('Ctrl Pts',(4.49220645669377,-3.73086354731027,1.25005084010303));
#79582=CARTESIAN_POINT('Ctrl Pts',(4.4980637313507,-3.76613559788889,1.13936787157651));
#79583=CARTESIAN_POINT('Ctrl Pts',(4.50392100600763,-3.79642909718072,1.02743131647794));
#79584=CARTESIAN_POINT('Ctrl Pts',(4.50975234755442,-3.82658847186685,0.915990360985462));
#79585=CARTESIAN_POINT('Ctrl Pts',(4.5155836891012,-3.85181325390274,0.803307319074836));
#79586=CARTESIAN_POINT('Ctrl Pts',(4.52141503064799,-3.87202571242438,0.689859320676657));
#79587=CARTESIAN_POINT('Ctrl Pts',(4.52728527185999,-3.89237300404805,0.57565453430403));
#79588=CARTESIAN_POINT('Ctrl Pts',(4.53315551307199,-3.90764080592582,0.460674975547904));
#79589=CARTESIAN_POINT('Ctrl Pts',(4.539025754284,-3.91780300444119,0.345410796576432));
#79590=CARTESIAN_POINT('Ctrl Pts',(4.544895995496,-3.92796520295657,0.230146617604964));
#79591=CARTESIAN_POINT('Ctrl Pts',(4.550766236708,-3.93302184218556,0.114598245955288));
#79592=CARTESIAN_POINT('Ctrl Pts',(4.55663647792001,-3.93299992902536,-0.000747185703453174));
#79593=CARTESIAN_POINT('',(5.8066364641403,-3.93299833356548,0.00362052083856629));
#79594=CARTESIAN_POINT('Ctrl Pts',(4.5566364779651,-3.9329999290252,-0.000747186589495274));
#79595=CARTESIAN_POINT('Ctrl Pts',(4.55867244357435,-3.93299232891272,-0.0407522432060994));
#79596=CARTESIAN_POINT('Ctrl Pts',(4.5607084091836,-3.93237437087316,-0.0807508249110428));
#79597=CARTESIAN_POINT('Ctrl Pts',(4.56274437479285,-3.93114654101444,-0.120730580509577));
#79598=CARTESIAN_POINT('Ctrl Pts',(4.56861682114895,-3.92760504456334,-0.236046364340019));
#79599=CARTESIAN_POINT('Ctrl Pts',(4.57448926750506,-3.91897932797847,-0.351399251435818));
#79600=CARTESIAN_POINT('Ctrl Pts',(4.58036171386116,-3.90525918752465,-0.466304276470143));
#79601=CARTESIAN_POINT('Ctrl Pts',(4.58622655303069,-3.89155682018647,-0.581060453152324));
#79602=CARTESIAN_POINT('Ctrl Pts',(4.59209139220022,-3.8727732012637,-0.695369514851362));
#79603=CARTESIAN_POINT('Ctrl Pts',(4.59795623136976,-3.84895011973601,-0.808747164312879));
#79604=CARTESIAN_POINT('Ctrl Pts',(4.60381504171668,-3.82515152739351,-0.922008266036873));
#79605=CARTESIAN_POINT('Ctrl Pts',(4.6096738520636,-3.79632386097098,-1.03433945785894));
#79606=CARTESIAN_POINT('Ctrl Pts',(4.61553266241053,-3.76256054934362,-1.1452629010507));
#79607=CARTESIAN_POINT('Ctrl Pts',(4.62161845120728,-3.72748920013178,-1.26048367248725));
#79608=CARTESIAN_POINT('Ctrl Pts',(4.62770424000403,-3.68709209753127,-1.37418496181102));
#79609=CARTESIAN_POINT('Ctrl Pts',(4.63379002880078,-3.64153218184008,-1.48584399202038));
#79610=CARTESIAN_POINT('Ctrl Pts',(4.63964205911007,-3.59772224751303,-1.59321413760295));
#79611=CARTESIAN_POINT('Ctrl Pts',(4.64549408941937,-3.54913896763112,-1.69869560053916));
#79612=CARTESIAN_POINT('Ctrl Pts',(4.65134611972866,-3.4959773457879,-1.80184111334428));
#79613=CARTESIAN_POINT('Ctrl Pts',(4.65719726033934,-3.44282380623736,-1.90497094468233));
#79614=CARTESIAN_POINT('Ctrl Pts',(4.66304840095001,-3.38509349803426,-2.00576516469815));
#79615=CARTESIAN_POINT('Ctrl Pts',(4.66889954156068,-3.32302810139414,-2.10379971417074));
#79616=CARTESIAN_POINT('Ctrl Pts',(4.67475120936123,-3.26095711263941,-2.20184309659157));
#79617=CARTESIAN_POINT('Ctrl Pts',(4.68060287716179,-3.19455048010673,-2.2971259649112));
#79618=CARTESIAN_POINT('Ctrl Pts',(4.68645454496234,-3.12409367234671,-2.38925254554709));
#79619=CARTESIAN_POINT('Ctrl Pts',(4.69230815688027,-3.05361345650737,-2.48140973367678));
#79620=CARTESIAN_POINT('Ctrl Pts',(4.69816176879819,-2.97908064076982,-2.57040822083238));
#79621=CARTESIAN_POINT('Ctrl Pts',(4.70401538071611,-2.90082102925586,-2.65588523024377));
#79622=CARTESIAN_POINT('Ctrl Pts',(4.70987564704947,-2.82247245182242,-2.74145941034881));
#79623=CARTESIAN_POINT('Ctrl Pts',(4.71573591338282,-2.74038890171791,-2.82350381733387));
#79624=CARTESIAN_POINT('Ctrl Pts',(4.72159617971618,-2.65493316841876,-2.90169241499335));
#79625=CARTESIAN_POINT('Ctrl Pts',(4.72746039312111,-2.56941987802637,-2.97993367510427));
#79626=CARTESIAN_POINT('Ctrl Pts',(4.73332460652603,-2.4805301981218,-3.05431369010774));
#79627=CARTESIAN_POINT('Ctrl Pts',(4.73918881993096,-2.38865874586569,-3.12454771059738));
#79628=CARTESIAN_POINT('Ctrl Pts',(4.74506166873729,-2.29665200745726,-3.1948851548401));
#79629=CARTESIAN_POINT('Ctrl Pts',(4.75093451754363,-2.20165507135535,-3.26106418437028));
#79630=CARTESIAN_POINT('Ctrl Pts',(4.75680736634997,-2.10409021430103,-3.32284416879315));
#79631=CARTESIAN_POINT('Ctrl Pts',(4.75840210874414,-2.07759697075655,-3.33962021113981));
#79632=CARTESIAN_POINT('Ctrl Pts',(4.75999685113832,-2.05091450706119,-3.35607214973232));
#79633=CARTESIAN_POINT('Ctrl Pts',(4.76159159353249,-2.02405155226804,-3.3721957703789));
#79634=CARTESIAN_POINT('Ctrl Pts',(4.76746403965121,-1.92513196802138,-3.43156905463566));
#79635=CARTESIAN_POINT('Ctrl Pts',(4.77333648576992,-1.82343208240723,-3.48668551016047));
#79636=CARTESIAN_POINT('Ctrl Pts',(4.77920893188864,-1.71935433526915,-3.53727432775452));
#79637=CARTESIAN_POINT('Ctrl Pts',(4.7850737708186,-1.61541141083544,-3.58779761240434));
#79638=CARTESIAN_POINT('Ctrl Pts',(4.79093860974857,-1.50909711881973,-3.63380474372197));
#79639=CARTESIAN_POINT('Ctrl Pts',(4.79680344867854,-1.4008414500738,-3.67506901047519));
#79640=CARTESIAN_POINT('Ctrl Pts',(4.80266225878403,-1.29269706391098,-3.71629085918004));
#79641=CARTESIAN_POINT('Ctrl Pts',(4.80852106888951,-1.18261565442301,-3.75277939457094));
#79642=CARTESIAN_POINT('Ctrl Pts',(4.814379878995,-1.07104970171551,-3.78435483754564));
#79643=CARTESIAN_POINT('Ctrl Pts',(4.82046566788155,-0.955161522566597,
-3.81715355887017));
#79644=CARTESIAN_POINT('Ctrl Pts',(4.82655145676809,-0.83767185572949,-3.84465060929839));
#79645=CARTESIAN_POINT('Ctrl Pts',(4.83263724565464,-0.71910856941166,-3.8667003847465));
#79646=CARTESIAN_POINT('Ctrl Pts',(4.83848927571933,-0.605099370434301,
-3.88790321502003));
#79647=CARTESIAN_POINT('Ctrl Pts',(4.84434130578403,-0.490097951290665,
-3.90406943482824));
#79648=CARTESIAN_POINT('Ctrl Pts',(4.85019333584872,-0.374585997779909,
-3.91512124081327));
#79649=CARTESIAN_POINT('Ctrl Pts',(4.85604447621404,-0.259091605852325,
-3.92617136656345));
#79650=CARTESIAN_POINT('Ctrl Pts',(4.86189561657936,-0.143087245252928,
-3.93210858517045));
#79651=CARTESIAN_POINT('Ctrl Pts',(4.86774675694468,-0.0270603173116924,
-3.93290690701255));
#79652=CARTESIAN_POINT('Ctrl Pts',(4.87359842449938,0.0889770646881643,
-3.93370530078366));
#79653=CARTESIAN_POINT('Ctrl Pts',(4.87945009205407,0.205036604699887,-3.92936387451259));
#79654=CARTESIAN_POINT('Ctrl Pts',(4.88530175960877,0.320631018722372,-3.91990876804972));
#79655=CARTESIAN_POINT('Ctrl Pts',(4.89115537128061,0.436263837025392,-3.91045052028833));
#79656=CARTESIAN_POINT('Ctrl Pts',(4.89700898295247,0.551430810302264,-3.89587524779013));
#79657=CARTESIAN_POINT('Ctrl Pts',(4.90286259462431,0.665650601907628,-3.87626086276195));
#79658=CARTESIAN_POINT('Ctrl Pts',(4.90872286071249,0.780000239168845,-3.85662417999839));
#79659=CARTESIAN_POINT('Ctrl Pts',(4.91458312680066,0.893400137945136,-3.8319370208324));
#79660=CARTESIAN_POINT('Ctrl Pts',(4.92044339288884,1.00537986972123,-3.80232827588036));
#79661=CARTESIAN_POINT('Ctrl Pts',(4.92630760604881,1.11743502333547,-3.77269958851612));
#79662=CARTESIAN_POINT('Ctrl Pts',(4.93217181920878,1.22806771172037,-3.73814283779098));
#79663=CARTESIAN_POINT('Ctrl Pts',(4.93803603236875,1.33682502762982,-3.69883601224798));
#79664=CARTESIAN_POINT('Ctrl Pts',(4.94390888093235,1.4457424951736,-3.65947130505998));
#79665=CARTESIAN_POINT('Ctrl Pts',(4.94978172949596,1.5527786979277,-3.61534271984959));
#79666=CARTESIAN_POINT('Ctrl Pts',(4.95565457805957,1.65750288613398,-3.56667536824667));
#79667=CARTESIAN_POINT('Ctrl Pts',(4.95724932279709,1.68594025280957,-3.5534599750661));
#79668=CARTESIAN_POINT('Ctrl Pts',(4.95884406753462,1.71420729329543,-3.53991016100368));
#79669=CARTESIAN_POINT('Ctrl Pts',(4.96043881227214,1.74229574265083,-3.52603099038292));
#79670=CARTESIAN_POINT('Ctrl Pts',(4.96631125835394,1.84572790986844,-3.47492269749273));
#79671=CARTESIAN_POINT('Ctrl Pts',(4.97218370443574,1.94708253229897,-3.41917387948225));
#79672=CARTESIAN_POINT('Ctrl Pts',(4.97805615051755,2.04591419948807,-3.3589766430169));
#79673=CARTESIAN_POINT('Ctrl Pts',(4.98392098940941,2.14461783974361,-3.29885738629036));
#79674=CARTESIAN_POINT('Ctrl Pts',(4.98978582830127,2.24080467436438,-3.23430138371258));
#79675=CARTESIAN_POINT('Ctrl Pts',(4.99565066719313,2.33405149138522,-3.16554776232525));
#79676=CARTESIAN_POINT('Ctrl Pts',(5.00150947725937,2.4272024543152,-3.09686481697902));
#79677=CARTESIAN_POINT('Ctrl Pts',(5.0073682873256,2.51741908031261,-3.02399307940692));
#79678=CARTESIAN_POINT('Ctrl Pts',(5.01322709739184,2.60430547696755,-2.94721597149528));
#79679=CARTESIAN_POINT('Ctrl Pts',(5.01931288629267,2.69455797916813,-2.86746440660682));
#79680=CARTESIAN_POINT('Ctrl Pts',(5.0253986751935,2.78121660935734,-2.78349898821209));
#79681=CARTESIAN_POINT('Ctrl Pts',(5.03148446409433,2.86387346032466,-2.69568503413289));
#79682=CARTESIAN_POINT('Ctrl Pts',(5.03733649411715,2.94335541103549,-2.61124406779842));
#79683=CARTESIAN_POINT('Ctrl Pts',(5.04318852413997,3.01913702380235,-2.52324509018783));
#79684=CARTESIAN_POINT('Ctrl Pts',(5.04904055416279,3.09089239730181,-2.43205123060799));
#79685=CARTESIAN_POINT('Ctrl Pts',(5.05489169448533,3.16263686163381,-2.3408712354823));
#79686=CARTESIAN_POINT('Ctrl Pts',(5.06074283480786,3.23035604825503,-2.24649764893359));
#79687=CARTESIAN_POINT('Ctrl Pts',(5.06659397513041,3.29376455157214,-2.1493264244425));
#79688=CARTESIAN_POINT('Ctrl Pts',(5.07244564264147,3.35717876800379,-2.05214644481121));
#79689=CARTESIAN_POINT('Ctrl Pts',(5.07829731015253,3.41628130313462,-1.95216867234492));
#79690=CARTESIAN_POINT('Ctrl Pts',(5.08414897766359,3.47083066658839,-1.84981714876623));
#79691=CARTESIAN_POINT('Ctrl Pts',(5.09000258929098,3.52539815313408,-1.74743162064646));
#79692=CARTESIAN_POINT('Ctrl Pts',(5.09585620091836,3.5754092657523,-1.64267113784546));
#79693=CARTESIAN_POINT('Ctrl Pts',(5.10170981254575,3.62066928123041,-1.53598273296104));
#79694=CARTESIAN_POINT('Ctrl Pts',(5.10757007858847,3.66598074852326,-1.42917304415781));
#79695=CARTESIAN_POINT('Ctrl Pts',(5.1134303446312,3.70653017679169,-1.32043143952382));
#79696=CARTESIAN_POINT('Ctrl Pts',(5.11929061067393,3.74217162445302,-1.21022334018918));
#79697=CARTESIAN_POINT('Ctrl Pts',(5.1251548237878,3.77783707773611,-1.09994101227738));
#79698=CARTESIAN_POINT('Ctrl Pts',(5.13101903690168,3.80858785874347,-0.988190620465026));
#79699=CARTESIAN_POINT('Ctrl Pts',(5.13688325001556,3.83432880143551,-0.875449394586642));
#79700=CARTESIAN_POINT('Ctrl Pts',(5.14275609853249,3.86010764919865,-0.762542150538906));
#79701=CARTESIAN_POINT('Ctrl Pts',(5.14862894704941,3.88086186123423,-0.648641565558515));
#79702=CARTESIAN_POINT('Ctrl Pts',(5.15450179556634,3.89654789264389,-0.534231710339649));
#79703=CARTESIAN_POINT('Ctrl Pts',(5.15609654071482,3.9008073627149,-0.503164237541329));
#79704=CARTESIAN_POINT('Ctrl Pts',(5.15769128586329,3.9046934176504,-0.472059219835393));
#79705=CARTESIAN_POINT('Ctrl Pts',(5.15928603101177,3.9082058486662,-0.440926348102861));
#79706=CARTESIAN_POINT('Ctrl Pts',(5.1651584771793,3.92113992912232,-0.326283507856984));
#79707=CARTESIAN_POINT('Ctrl Pts',(5.17103092334683,3.92904700856901,-0.210879137396811));
#79708=CARTESIAN_POINT('Ctrl Pts',(5.17690336951435,3.93184785086485,-0.0951917940235433));
#79709=CARTESIAN_POINT('Ctrl Pts',(5.18276820849321,3.93464506493914,0.020345687533596));
#79710=CARTESIAN_POINT('Ctrl Pts',(5.18863304747207,3.93234918611412,0.136165003611755));
#79711=CARTESIAN_POINT('Ctrl Pts',(5.19449788645093,3.92493253515872,0.251780846079617));
#79712=CARTESIAN_POINT('Ctrl Pts',(5.20035669660532,3.91752350822963,0.36727783999562));
#79713=CARTESIAN_POINT('Ctrl Pts',(5.20621550675971,3.9050042057642,0.482571366305245));
#79714=CARTESIAN_POINT('Ctrl Pts',(5.2120743169141,3.88739898171281,0.597175147656201));
#79715=CARTESIAN_POINT('Ctrl Pts',(5.21816010578232,3.869111706015,0.716218843973764));
#79716=CARTESIAN_POINT('Ctrl Pts',(5.22424589465055,3.84533645586416,0.834517816800412));
#79717=CARTESIAN_POINT('Ctrl Pts',(5.23033168351877,3.8161599802714,0.951531399889123));
#79718=CARTESIAN_POINT('Ctrl Pts',(5.23618371363209,3.78810419038673,1.06405042194691));
#79719=CARTESIAN_POINT('Ctrl Pts',(5.24203574374541,3.75505455895332,1.17538053978761));
#79720=CARTESIAN_POINT('Ctrl Pts',(5.24788777385873,3.71714033540991,1.28505125456875));
#79721=CARTESIAN_POINT('Ctrl Pts',(5.25373891427248,3.67923187606583,1.39470529582209));
#79722=CARTESIAN_POINT('Ctrl Pts',(5.25959005468625,3.63646043015309,1.50270004507394));
#79723=CARTESIAN_POINT('Ctrl Pts',(5.2654411951,3.58900475555364,1.60858132048503));
#79724=CARTESIAN_POINT('Ctrl Pts',(5.2712928627029,3.54154480518665,1.71447213582416));
#79725=CARTESIAN_POINT('Ctrl Pts',(5.27714453030579,3.48939995620785,1.81824872155039));
#79726=CARTESIAN_POINT('Ctrl Pts',(5.28299619790869,3.43279633998593,1.91947865009726));
#79727=CARTESIAN_POINT('Ctrl Pts',(5.28884980962844,3.37617391817692,2.02074221056314));
#79728=CARTESIAN_POINT('Ctrl Pts',(5.2947034213482,3.31508998518154,2.11945707086956));
#79729=CARTESIAN_POINT('Ctrl Pts',(5.30055703306796,3.24981529998154,2.21521771300383));
#79730=CARTESIAN_POINT('Ctrl Pts',(5.30641729920336,3.1844664101866,2.3110872163243));
#79731=CARTESIAN_POINT('Ctrl Pts',(5.31227756533877,3.11491749222178,2.4039954565216));
#79732=CARTESIAN_POINT('Ctrl Pts',(5.31813783147417,3.04148115039268,2.49356800825765));
#79733=CARTESIAN_POINT('Ctrl Pts',(5.32400204468104,2.96799534690394,2.58320088989244));
#79734=CARTESIAN_POINT('Ctrl Pts',(5.3298662578879,2.89061718127177,2.6694933024567));
#79735=CARTESIAN_POINT('Ctrl Pts',(5.33573047109477,2.80969664624507,2.75210714836454));
#79736=CARTESIAN_POINT('Ctrl Pts',(5.3416033197044,2.72865695091712,2.83484264807464));
#79737=CARTESIAN_POINT('Ctrl Pts',(5.34747616831404,2.64406477628405,2.91388848890184));
#79738=CARTESIAN_POINT('Ctrl Pts',(5.35334901692367,2.55630378176638,2.98894629850168));
#79739=CARTESIAN_POINT('Ctrl Pts',(5.35494376119959,2.53247269859723,3.009327891861));
#79740=CARTESIAN_POINT('Ctrl Pts',(5.35653850547551,2.5084081231882,3.02941566631621));
#79741=CARTESIAN_POINT('Ctrl Pts',(5.35813324975143,2.48411809468964,3.04920420628654));
#79742=CARTESIAN_POINT('Ctrl Pts',(5.36400569588059,2.39467310593038,3.12207302714088));
#79743=CARTESIAN_POINT('Ctrl Pts',(5.36987814200974,2.30186936027663,3.19112485718943));
#79744=CARTESIAN_POINT('Ctrl Pts',(5.3757505881389,2.20606658059504,3.25603428145063));
#79745=CARTESIAN_POINT('Ctrl Pts',(5.381615427079,2.11038790419881,3.32085962179663));
#79746=CARTESIAN_POINT('Ctrl Pts',(5.3874802660191,2.01171825863209,3.38155299787701));
#79747=CARTESIAN_POINT('Ctrl Pts',(5.39334510495919,1.91045092296981,3.43782871459935));
#79748=CARTESIAN_POINT('Ctrl Pts',(5.39920391507448,1.80928768616376,3.4940465820882));
#79749=CARTESIAN_POINT('Ctrl Pts',(5.40506272518976,1.70553242982779,3.54585562329428));
#79750=CARTESIAN_POINT('Ctrl Pts',(5.41092153530505,1.59960738322865,3.59301338983316));
#79751=CARTESIAN_POINT('Ctrl Pts',(5.4170073241878,1.48957864730563,3.64199811637156));
#79752=CARTESIAN_POINT('Ctrl Pts',(5.42309311307055,1.37720897540698,3.68596363024611));
#79753=CARTESIAN_POINT('Ctrl Pts',(5.4291789019533,1.26300008688424,3.72469056171521));
#79754=CARTESIAN_POINT('Ctrl Pts',(5.4350309320269,1.15317803042048,3.76192996846788));
#79755=CARTESIAN_POINT('Ctrl Pts',(5.44088296210051,1.04165586952818,3.79432565857732));
#79756=CARTESIAN_POINT('Ctrl Pts',(5.44673499217412,0.928899278516613,3.82173195428085));
#79757=CARTESIAN_POINT('Ctrl Pts',(5.452586132548,0.816159830189972,3.84913408333223));
#79758=CARTESIAN_POINT('Ctrl Pts',(5.45843727292188,0.702186726453746,3.87154822862387));
#79759=CARTESIAN_POINT('Ctrl Pts',(5.46428841329576,0.587458685331134,3.88887918210749));
#79760=CARTESIAN_POINT('Ctrl Pts',(5.47014008085867,0.472720307186906,3.90621169711381));
#79761=CARTESIAN_POINT('Ctrl Pts',(5.47599174842159,0.357227265183229,3.91846004811158));
#79762=CARTESIAN_POINT('Ctrl Pts',(5.4818434159845,0.241465592784657,3.92558064080986));
#79763=CARTESIAN_POINT('Ctrl Pts',(5.48769702766419,0.125665460544065,3.93270359920367));
#79764=CARTESIAN_POINT('Ctrl Pts',(5.49355063934388,0.00959693280344369,
3.93469538640835));
#79765=CARTESIAN_POINT('Ctrl Pts',(5.49940425102358,-0.106252462921666,
3.93156449955016));
#79766=CARTESIAN_POINT('Ctrl Pts',(5.50526451711901,-0.222233556833263,
3.92843005348375));
#79767=CARTESIAN_POINT('Ctrl Pts',(5.51112478321445,-0.337994608063186,
3.92016132105254));
#79768=CARTESIAN_POINT('Ctrl Pts',(5.51698504930989,-0.453051618335803,
3.90681881216973));
#79769=CARTESIAN_POINT('Ctrl Pts',(5.52284926247678,-0.568186123082922,
3.89346731669226));
#79770=CARTESIAN_POINT('Ctrl Pts',(5.52871347564367,-0.682615235559708,
3.87503530571441));
#79771=CARTESIAN_POINT('Ctrl Pts',(5.53457768881057,-0.795865300405437,
3.85163438342875));
#79772=CARTESIAN_POINT('Ctrl Pts',(5.54045053738055,-0.909282132715467,
3.82819900189155));
#79773=CARTESIAN_POINT('Ctrl Pts',(5.54632338595054,-1.02151605304674,3.79978020681874));
#79774=CARTESIAN_POINT('Ctrl Pts',(5.55219623452053,-1.1321086193517,3.76653940295194));
#79775=CARTESIAN_POINT('Ctrl Pts',(5.55379097917738,-1.16213951527903,3.75751301759154));
#79776=CARTESIAN_POINT('Ctrl Pts',(5.55538572383423,-1.19204949971307,3.74813134541748));
#79777=CARTESIAN_POINT('Ctrl Pts',(5.55698046849108,-1.22182967016167,3.73839822077753));
#79778=CARTESIAN_POINT('Ctrl Pts',(5.5628529146185,-1.33149139304234,3.70255721648003));
#79779=CARTESIAN_POINT('Ctrl Pts',(5.56872536074592,-1.43975834348045,3.66182690993442));
#79780=CARTESIAN_POINT('Ctrl Pts',(5.57459780687335,-1.54616227365557,3.61633394800926));
#79781=CARTESIAN_POINT('Ctrl Pts',(5.58046264581158,-1.65242836777232,3.57089991784108));
#79782=CARTESIAN_POINT('Ctrl Pts',(5.58632748474981,-1.75683586437637,3.52071566236118));
#79783=CARTESIAN_POINT('Ctrl Pts',(5.59219232368805,-1.85893178418655,3.46595753317045));
#79784=CARTESIAN_POINT('Ctrl Pts',(5.59805113380136,-1.96092275338637,3.41125569319375));
#79785=CARTESIAN_POINT('Ctrl Pts',(5.60390994391467,-2.06060651012118,3.35198952577101));
#79786=CARTESIAN_POINT('Ctrl Pts',(5.60976875402798,-2.15755080096085,3.28838311960045));
#79787=CARTESIAN_POINT('Ctrl Pts',(5.61585454291143,-2.25825085371823,3.2223125093396));
#79788=CARTESIAN_POINT('Ctrl Pts',(5.62194033179488,-2.35599446809467,3.15155874318567));
#79789=CARTESIAN_POINT('Ctrl Pts',(5.62802612067832,-2.45032582351664,3.07642525646366));
#79790=CARTESIAN_POINT('Ctrl Pts',(5.63387815074965,-2.5410338548287,3.00417769216567));
#79791=CARTESIAN_POINT('Ctrl Pts',(5.63973018082097,-2.62858657239987,2.92788093768364));
#79792=CARTESIAN_POINT('Ctrl Pts',(5.6455822108923,-2.7126096359302,2.84784795293896));
#79793=CARTESIAN_POINT('Ctrl Pts',(5.6514333512638,-2.79661992520883,2.76782713582359));
#79794=CARTESIAN_POINT('Ctrl Pts',(5.6572844916353,-2.87710132820144,2.68407150288923));
#79795=CARTESIAN_POINT('Ctrl Pts',(5.6631356320068,-2.95371490731195,2.59693227603709));
#79796=CARTESIAN_POINT('Ctrl Pts',(5.66898729956722,-3.03033538932134,2.50978519792309));
#79797=CARTESIAN_POINT('Ctrl Pts',(5.67483896712764,-3.10308708172622,2.41925423030597));
#79798=CARTESIAN_POINT('Ctrl Pts',(5.68069063468806,-3.1716705093492,2.32572465698857));
#79799=CARTESIAN_POINT('Ctrl Pts',(5.68654424636516,-3.24027672264545,2.23216401006677));
#79800=CARTESIAN_POINT('Ctrl Pts',(5.69239785804226,-3.30471167319672,2.13560310965609));
#79801=CARTESIAN_POINT('Ctrl Pts',(5.69825146971936,-3.36471889774139,2.03645666273111));
#79802=CARTESIAN_POINT('Ctrl Pts',(5.70411173581206,-3.42479433880496,1.93719750561965));
#79803=CARTESIAN_POINT('Ctrl Pts',(5.70997200190475,-3.48043179308373,1.83534728916393));
#79804=CARTESIAN_POINT('Ctrl Pts',(5.71583226799745,-3.53142045923226,1.73134587535703));
#79805=CARTESIAN_POINT('Ctrl Pts',(5.72169648116154,-3.58244346783244,1.62727441336501));
#79806=CARTESIAN_POINT('Ctrl Pts',(5.72756069432563,-3.6288112886858,1.52104924688573));
#79807=CARTESIAN_POINT('Ctrl Pts',(5.73342490748972,-3.67036169393012,1.41312916456012));
#79808=CARTESIAN_POINT('Ctrl Pts',(5.73929775605678,-3.71197328461965,1.30505016348884));
#79809=CARTESIAN_POINT('Ctrl Pts',(5.74517060462384,-3.74875317080466,1.19527165579196));
#79810=CARTESIAN_POINT('Ctrl Pts',(5.7510434531909,-3.7805892432829,1.08426656020261));
#79811=CARTESIAN_POINT('Ctrl Pts',(5.75263819787084,-3.78923418051141,1.05412364341946));
#79812=CARTESIAN_POINT('Ctrl Pts',(5.75423294255078,-3.79751486921203,1.02389033124141));
#79813=CARTESIAN_POINT('Ctrl Pts',(5.75582768723071,-3.80542972120358,0.993576185795752));
#79814=CARTESIAN_POINT('Ctrl Pts',(5.76345579314931,-3.84328865253039,0.848575224074156));
#79815=CARTESIAN_POINT('Ctrl Pts',(5.7710838990679,-3.87287613987567,0.70133166860417));
#79816=CARTESIAN_POINT('Ctrl Pts',(5.7787120049865,-3.89397603459136,0.552665940716588));
#79817=CARTESIAN_POINT('Ctrl Pts',(5.78618099959784,-3.91463581588087,0.407101165878184));
#79818=CARTESIAN_POINT('Ctrl Pts',(5.79364999420918,-3.92715842132982,0.260172687026572));
#79819=CARTESIAN_POINT('Ctrl Pts',(5.80111898882052,-3.9313857410616,0.112672778334271));
#79820=CARTESIAN_POINT('Ctrl Pts',(5.80295814726045,-3.93242667242753,0.0763525349714642));
#79821=CARTESIAN_POINT('Ctrl Pts',(5.80479730570037,-3.93296484650485,0.0399977603377867));
#79822=CARTESIAN_POINT('Ctrl Pts',(5.8066364641403,-3.93299833356548,0.00362052083856629));
#79823=CARTESIAN_POINT('',(7.05663650576764,-3.93060739270548,-0.000901275032790407));
#79824=CARTESIAN_POINT('Ctrl Pts',(5.80663647796509,-3.93210781031187,0.00361942768470874));
#79825=CARTESIAN_POINT('Ctrl Pts',(5.85598262063352,-3.92329404442754,-0.972199952904983));
#79826=CARTESIAN_POINT('Ctrl Pts',(5.97161116954849,-3.06253954822306,-3.27263336896532));
#79827=CARTESIAN_POINT('Ctrl Pts',(6.15352212470999,0.80000188434543,-4.58235619056535));
#79828=CARTESIAN_POINT('Ctrl Pts',(6.35236934344966,4.28728808542873,-1.80475819528463));
#79829=CARTESIAN_POINT('Ctrl Pts',(6.55121656218928,3.83635924797249,2.63065371934916));
#79830=CARTESIAN_POINT('Ctrl Pts',(6.75006378092894,-0.138570632095021,
4.64960099912353));
#79831=CARTESIAN_POINT('Ctrl Pts',(6.91853708618754,-3.39848507636798,2.74152539667428));
#79832=CARTESIAN_POINT('Ctrl Pts',(7.02072798519958,-3.92523164958614,0.711663097972118));
#79833=CARTESIAN_POINT('Ctrl Pts',(7.05663647796509,-3.92668421635667,-0.000899823416283008));
#79834=CARTESIAN_POINT('',(8.3066364779651,-3.93344384724419,-0.00329189189212218));
#79835=CARTESIAN_POINT('Ctrl Pts',(7.05663652272271,-3.93299989653023,-0.000902160284366488));
#79836=CARTESIAN_POINT('Ctrl Pts',(7.06288361214318,-3.93297141513468,-0.125067818755675));
#79837=CARTESIAN_POINT('Ctrl Pts',(7.06913070156365,-3.92705879239068,-0.249078431000784));
#79838=CARTESIAN_POINT('Ctrl Pts',(7.07537779098412,-3.91533128588655,-0.372384105136066));
#79839=CARTESIAN_POINT('Ctrl Pts',(7.08164686886942,-3.90356250098108,-0.496123789783527));
#79840=CARTESIAN_POINT('Ctrl Pts',(7.08791594675472,-3.88593791112278,-0.619153250419358));
#79841=CARTESIAN_POINT('Ctrl Pts',(7.09418502464002,-3.86257841551443,-0.740929810442296));
#79842=CARTESIAN_POINT('Ctrl Pts',(7.10046521277651,-3.83917752149492,-0.862922186602119));
#79843=CARTESIAN_POINT('Ctrl Pts',(7.106745400913,-3.81002150458914,-0.983656917383635));
#79844=CARTESIAN_POINT('Ctrl Pts',(7.11302558904949,-3.77528127951279,-1.10260612213077));
#79845=CARTESIAN_POINT('Ctrl Pts',(7.1193249248549,-3.74043513494592,-1.22191799117091));
#79846=CARTESIAN_POINT('Ctrl Pts',(7.12562426066031,-3.69997082401521,-1.33943313800122));
#79847=CARTESIAN_POINT('Ctrl Pts',(7.13192359646571,-3.65410841841374,-1.45464107823127));
#79848=CARTESIAN_POINT('Ctrl Pts',(7.13720180377988,-3.61568035358776,-1.55117369874183));
#79849=CARTESIAN_POINT('Ctrl Pts',(7.14248001109405,-3.57346331290171,-1.64608680048987));
#79850=CARTESIAN_POINT('Ctrl Pts',(7.14775821840821,-3.52761112971304,-1.73909422330265));
#79851=CARTESIAN_POINT('Ctrl Pts',(7.15363066454209,-3.47659674928628,-1.8425727431882));
#79852=CARTESIAN_POINT('Ctrl Pts',(7.15950311067597,-3.4209399596555,-1.94397793156341));
#79853=CARTESIAN_POINT('Ctrl Pts',(7.16537555680985,-3.36083246309158,-2.04286420376632));
#79854=CARTESIAN_POINT('Ctrl Pts',(7.17124039575466,-3.30080283000746,-2.14162237831588));
#79855=CARTESIAN_POINT('Ctrl Pts',(7.17710523469946,-3.23633416817014,-2.2378677757007));
#79856=CARTESIAN_POINT('Ctrl Pts',(7.18297007364427,-3.16766522035791,-2.33117696705652));
#79857=CARTESIAN_POINT('Ctrl Pts',(7.18882888376425,-3.09906686153566,-2.42439024021667));
#79858=CARTESIAN_POINT('Ctrl Pts',(7.19468769388423,-3.02627704847413,-2.51467297999974));
#79859=CARTESIAN_POINT('Ctrl Pts',(7.20054650400421,-2.94957884357713,-2.60162903687712));
#79860=CARTESIAN_POINT('Ctrl Pts',(7.20663229288519,-2.86990923951165,-2.6919538969155));
#79861=CARTESIAN_POINT('Ctrl Pts',(7.21271808176618,-2.78602252134734,-2.77868871160012));
#79862=CARTESIAN_POINT('Ctrl Pts',(7.21880387064716,-2.69828363646979,-2.86142524228038));
#79863=CARTESIAN_POINT('Ctrl Pts',(7.22465590072539,-2.61391485480897,-2.94098381317034));
#79864=CARTESIAN_POINT('Ctrl Pts',(7.23050793080362,-2.52598470426606,-3.01684527738739));
#79865=CARTESIAN_POINT('Ctrl Pts',(7.23635996088185,-2.43485601816631,-3.08868340410592));
#79866=CARTESIAN_POINT('Ctrl Pts',(7.24221110126033,-2.34374118660395,-3.16051060908229));
#79867=CARTESIAN_POINT('Ctrl Pts',(7.2480622416388,-2.24942911090274,-3.22831543694416));
#79868=CARTESIAN_POINT('Ctrl Pts',(7.25391338201728,-2.15231548530825,-3.29181212278318));
#79869=CARTESIAN_POINT('Ctrl Pts',(7.25976504958474,-2.05519310975554,-3.35531452968703));
#79870=CARTESIAN_POINT('Ctrl Pts',(7.26561671715221,-1.95526902851059,-3.41450779671165));
#79871=CARTESIAN_POINT('Ctrl Pts',(7.27146838471967,-1.85296706391351,-3.4691500486505));
#79872=CARTESIAN_POINT('Ctrl Pts',(7.27732199640388,-1.75063111123349,-3.52381045454561));
#79873=CARTESIAN_POINT('Ctrl Pts',(7.28317560808809,-1.64591606872578,-3.57391664419774));
#79874=CARTESIAN_POINT('Ctrl Pts',(7.2890292197723,-1.5392687920494,-3.6192734886746));
#79875=CARTESIAN_POINT('Ctrl Pts',(7.29488948587215,-1.43250027820454,-3.66468189504376));
#79876=CARTESIAN_POINT('Ctrl Pts',(7.30074975197199,-1.32379552651248,-3.70533001798262));
#79877=CARTESIAN_POINT('Ctrl Pts',(7.30661001807184,-1.21361982543884,-3.74107149347641));
#79878=CARTESIAN_POINT('Ctrl Pts',(7.31247423124311,-1.10336991760511,-3.77683704196516));
#79879=CARTESIAN_POINT('Ctrl Pts',(7.31833844441438,-0.991647485115964,
-3.80768925276693));
#79880=CARTESIAN_POINT('Ctrl Pts',(7.32420265758565,-0.878929671228565,
-3.83353252666963));
#79881=CARTESIAN_POINT('Ctrl Pts',(7.3300755061599,-0.766045873650185,-3.85941385633159));
#79882=CARTESIAN_POINT('Ctrl Pts',(7.33594835473416,-0.652164174375472,
-3.88027145396397));
#79883=CARTESIAN_POINT('Ctrl Pts',(7.34182120330841,-0.537768604378055,
-3.89606133526479));
#79884=CARTESIAN_POINT('Ctrl Pts',(7.34341594792156,-0.506705021397034,
-3.90034900381751));
#79885=CARTESIAN_POINT('Ctrl Pts',(7.34501069253471,-0.475603554578537,
-3.90426329172176));
#79886=CARTESIAN_POINT('Ctrl Pts',(7.34660543714786,-0.444473894600172,
-3.90780398139658));
#79887=CARTESIAN_POINT('Ctrl Pts',(7.35247788328177,-0.329842843406956,
-3.92084212507229));
#79888=CARTESIAN_POINT('Ctrl Pts',(7.35835032941567,-0.214445698971003,
-3.92885396116556));
#79889=CARTESIAN_POINT('Ctrl Pts',(7.36422277554958,-0.0987609464627275,
-3.93175981914636));
#79890=CARTESIAN_POINT('Ctrl Pts',(7.37008761449442,0.0167739475768885,
-3.93466191286766));
#79891=CARTESIAN_POINT('Ctrl Pts',(7.37595245343926,0.132595299365251,-3.93247117168982));
#79892=CARTESIAN_POINT('Ctrl Pts',(7.3818172923841,0.248217826102488,-3.92515947584362));
#79893=CARTESIAN_POINT('Ctrl Pts',(7.38767610250411,0.363721497408917,-3.91785529613449));
#79894=CARTESIAN_POINT('Ctrl Pts',(7.39353491262413,0.47902634013968,-3.90544065835273));
#79895=CARTESIAN_POINT('Ctrl Pts',(7.39939372274414,0.593646055039921,-3.88793947500929));
#79896=CARTESIAN_POINT('Ctrl Pts',(7.40547951162512,0.712706303143439,-3.86976027056101));
#79897=CARTESIAN_POINT('Ctrl Pts',(7.41156530050609,0.831026809866332,-3.84609241785892));
#79898=CARTESIAN_POINT('Ctrl Pts',(7.41765108938706,0.948066830428479,-3.81702217507854));
#79899=CARTESIAN_POINT('Ctrl Pts',(7.42350311946532,1.06061127357061,-3.78906853776704));
#79900=CARTESIAN_POINT('Ctrl Pts',(7.42935514954358,1.17197134624308,-3.75611998177188));
#79901=CARTESIAN_POINT('Ctrl Pts',(7.43520717962184,1.28167643247323,-3.71830532937287));
#79902=CARTESIAN_POINT('Ctrl Pts',(7.44105832000035,1.3913648399463,-3.6804964260364));
#79903=CARTESIAN_POINT('Ctrl Pts',(7.44690946037885,1.49939837057773,-3.63782303193787));
#79904=CARTESIAN_POINT('Ctrl Pts',(7.45276060075736,1.60532268044908,-3.59046349259198));
#79905=CARTESIAN_POINT('Ctrl Pts',(7.45861226832485,1.71125653412312,-3.54309968614159));
#79906=CARTESIAN_POINT('Ctrl Pts',(7.46446393589234,1.81508041187348,-3.4910490638332));
#79907=CARTESIAN_POINT('Ctrl Pts',(7.47031560345983,1.91636168104144,-3.43453736439655));
#79908=CARTESIAN_POINT('Ctrl Pts',(7.47616921514406,2.01767659918357,-3.37800688991166));
#79909=CARTESIAN_POINT('Ctrl Pts',(7.48202282682829,2.116446868255,-3.31701259250204));
#79910=CARTESIAN_POINT('Ctrl Pts',(7.48787643851252,2.21226672462819,-3.25182486291972));
#79911=CARTESIAN_POINT('Ctrl Pts',(7.4937367046124,2.30819550950339,-3.18656302759355));
#79912=CARTESIAN_POINT('Ctrl Pts',(7.49959697071228,2.40116684515268,-3.11709847773811));
#79913=CARTESIAN_POINT('Ctrl Pts',(7.50545723681217,2.49080602262458,-3.04374347763689));
#79914=CARTESIAN_POINT('Ctrl Pts',(7.51132144998346,2.58050557486939,-2.9703390706625));
#79915=CARTESIAN_POINT('Ctrl Pts',(7.51718566315476,2.66686819281238,-2.89303927082564));
#79916=CARTESIAN_POINT('Ctrl Pts',(7.52304987632606,2.74955546129944,-2.81219376381472));
#79917=CARTESIAN_POINT('Ctrl Pts',(7.52892272490034,2.83236449171167,-2.73122920698205));
#79918=CARTESIAN_POINT('Ctrl Pts',(7.53479557347462,2.91148708962327,-2.64670882299955));
#79919=CARTESIAN_POINT('Ctrl Pts',(7.54066842204891,2.9866245345438,-2.55901600027452));
#79920=CARTESIAN_POINT('Ctrl Pts',(7.54226316666178,3.00702775693175,-2.53520342365873));
#79921=CARTESIAN_POINT('Ctrl Pts',(7.54385791127464,3.02713737236875,-2.51115708808148));
#79922=CARTESIAN_POINT('Ctrl Pts',(7.54545265588751,3.04694795797518,-2.48688502777891));
#79923=CARTESIAN_POINT('Ctrl Pts',(7.55132510202144,3.11989794377009,-2.39750622346376));
#79924=CARTESIAN_POINT('Ctrl Pts',(7.55719754815538,3.18903398928196,-2.30476519870854));
#79925=CARTESIAN_POINT('Ctrl Pts',(7.56306999428931,3.25403035311977,-2.20902138083252));
#79926=CARTESIAN_POINT('Ctrl Pts',(7.56893483323417,3.31894252042051,-2.11340158986255));
#79927=CARTESIAN_POINT('Ctrl Pts',(7.57479967217902,3.37972544024367,-2.01478708010426));
#79928=CARTESIAN_POINT('Ctrl Pts',(7.58066451112388,3.43609306060994,-1.91357087112765));
#79929=CARTESIAN_POINT('Ctrl Pts',(7.58652332124391,3.49240273726927,-1.81245870845122));
#79930=CARTESIAN_POINT('Ctrl Pts',(7.59238213136395,3.54430594239584,-1.70875052513813));
#79931=CARTESIAN_POINT('Ctrl Pts',(7.59824094148399,3.59155984442061,-1.60286833019602));
#79932=CARTESIAN_POINT('Ctrl Pts',(7.60432673036495,3.64064443081831,-1.49288410618655));
#79933=CARTESIAN_POINT('Ctrl Pts',(7.61041251924591,3.68471193163949,-1.38055439091041));
#79934=CARTESIAN_POINT('Ctrl Pts',(7.61649830812688,3.72354252179092,-1.26638070437564));
#79935=CARTESIAN_POINT('Ctrl Pts',(7.62235033820516,3.7608816056744,-1.15659249765038));
#79936=CARTESIAN_POINT('Ctrl Pts',(7.62820236828344,3.79337851819582,-1.04509979024559));
#79937=CARTESIAN_POINT('Ctrl Pts',(7.63405439836172,3.82088715893014,-0.93236812403833));
#79938=CARTESIAN_POINT('Ctrl Pts',(7.63990553874025,3.84839161745238,-0.819653596727187));
#79939=CARTESIAN_POINT('Ctrl Pts',(7.64575667911878,3.87090921412992,-0.705700886603481));
#79940=CARTESIAN_POINT('Ctrl Pts',(7.65160781949731,3.8883443063907,-0.590988625067398));
#79941=CARTESIAN_POINT('Ctrl Pts',(7.65745948706482,3.90578096955697,-0.476266027932311));
#79942=CARTESIAN_POINT('Ctrl Pts',(7.66331115463233,3.91813415585814,-0.360784152029154));
#79943=CARTESIAN_POINT('Ctrl Pts',(7.66916282219984,3.92535982981755,-0.245028991049561));
#79944=CARTESIAN_POINT('Ctrl Pts',(7.6750164338841,3.93258790438388,-0.129235372392126));
#79945=CARTESIAN_POINT('Ctrl Pts',(7.68087004556835,3.93468505350706,-0.0131687004549297));
#79946=CARTESIAN_POINT('Ctrl Pts',(7.6867236572526,3.93165933174991,0.1026834897333));
#79947=CARTESIAN_POINT('Ctrl Pts',(7.6925839233525,3.92863017033682,0.218667381282902));
#79948=CARTESIAN_POINT('Ctrl Pts',(7.6984441894524,3.92046652491974,0.334435890958983));
#79949=CARTESIAN_POINT('Ctrl Pts',(7.70430445555231,3.90722846603072,0.449504965755925));
#79950=CARTESIAN_POINT('Ctrl Pts',(7.71016866872363,3.89398149089746,0.56465154315226));
#79951=CARTESIAN_POINT('Ctrl Pts',(7.71603288189495,3.87565336201966,0.679097340474461));
#79952=CARTESIAN_POINT('Ctrl Pts',(7.72189709506627,3.85235525357663,0.792368601245983));
#79953=CARTESIAN_POINT('Ctrl Pts',(7.72776994364057,3.82902283728201,0.905806660691923));
#79954=CARTESIAN_POINT('Ctrl Pts',(7.73364279221488,3.80070593569257,1.01806633240571));
#79955=CARTESIAN_POINT('Ctrl Pts',(7.73951564078919,3.76756553732628,1.12868902801052));
#79956=CARTESIAN_POINT('Ctrl Pts',(7.74111038540184,3.75856641686759,1.15872810455419));
#79957=CARTESIAN_POINT('Ctrl Pts',(7.74270513001449,3.74921190000219,1.18864659217748));
#79958=CARTESIAN_POINT('Ctrl Pts',(7.74429987462715,3.73950581299458,1.21843558491194));
#79959=CARTESIAN_POINT('Ctrl Pts',(7.75017232076106,3.70376437033916,1.32812979790921));
#79960=CARTESIAN_POINT('Ctrl Pts',(7.75604476689497,3.66313236131554,1.43643367736083));
#79961=CARTESIAN_POINT('Ctrl Pts',(7.76191721302888,3.61773600768323,1.5428788606732));
#79962=CARTESIAN_POINT('Ctrl Pts',(7.76778205197371,3.57239846066019,1.64918615448997));
#79963=CARTESIAN_POINT('Ctrl Pts',(7.77364689091855,3.52230900310579,1.75363916363233));
#79964=CARTESIAN_POINT('Ctrl Pts',(7.77951172986338,3.46764357535158,1.85578474891968));
#79965=CARTESIAN_POINT('Ctrl Pts',(7.7853705399834,3.4130343415169,1.95782533254445));
#79966=CARTESIAN_POINT('Ctrl Pts',(7.79122935010342,3.35385868770488,2.05756284797543));
#79967=CARTESIAN_POINT('Ctrl Pts',(7.79708816022343,3.29034031013881,2.15456483854063));
#79968=CARTESIAN_POINT('Ctrl Pts',(7.80317394910441,3.22436113894012,2.25532482623803));
#79969=CARTESIAN_POINT('Ctrl Pts',(7.80925973798537,3.15369613003769,2.35313262796932));
#79970=CARTESIAN_POINT('Ctrl Pts',(7.81534552686635,3.07864830485412,2.44753214790303));
#79971=CARTESIAN_POINT('Ctrl Pts',(7.82119755694461,3.00648311166854,2.53830572563136));
#79972=CARTESIAN_POINT('Ctrl Pts',(7.82704958702288,2.93026586568177,2.62592766661633));
#79973=CARTESIAN_POINT('Ctrl Pts',(7.83290161710114,2.85030918687491,2.71002334661834));
#79974=CARTESIAN_POINT('Ctrl Pts',(7.83875275747964,2.77036466409535,2.79410624132966));
#79975=CARTESIAN_POINT('Ctrl Pts',(7.84460389785815,2.68668212363562,2.87466364152844));
#79976=CARTESIAN_POINT('Ctrl Pts',(7.85045503823666,2.59961247957813,2.95135629093162));
#79977=CARTESIAN_POINT('Ctrl Pts',(7.85630670580415,2.51253499052731,3.02805585035871));
#79978=CARTESIAN_POINT('Ctrl Pts',(7.86215837337164,2.42207010141677,3.10088969353643));
#79979=CARTESIAN_POINT('Ctrl Pts',(7.86801004093913,2.32860282403901,3.16955799566399));
#79980=CARTESIAN_POINT('Ctrl Pts',(7.87386365262336,2.23510449375257,3.2382491116637));
#79981=CARTESIAN_POINT('Ctrl Pts',(7.87971726430759,2.13860212468947,3.30277169014711));
#79982=CARTESIAN_POINT('Ctrl Pts',(7.88557087599182,2.03951019084641,3.36286889150226));
#79983=CARTESIAN_POINT('Ctrl Pts',(7.89143114209171,1.940305608787,3.42303441166277));
#79984=CARTESIAN_POINT('Ctrl Pts',(7.89729140819159,1.83850593980556,3.47876429892532));
#79985=CARTESIAN_POINT('Ctrl Pts',(7.90315167429147,1.73455085435709,3.5298473527405));
#79986=CARTESIAN_POINT('Ctrl Pts',(7.90901588746277,1.6305257519266,3.58096481258059));
#79987=CARTESIAN_POINT('Ctrl Pts',(7.91488010063406,1.52434272008469,3.62742904163521));
#79988=CARTESIAN_POINT('Ctrl Pts',(7.92074431380535,1.41646040001964,3.66907739563725));
#79989=CARTESIAN_POINT('Ctrl Pts',(7.92661716237964,1.30841921681614,3.71078707931985));
#79990=CARTESIAN_POINT('Ctrl Pts',(7.93249001095393,1.19867414164117,3.74766660322759));
#79991=CARTESIAN_POINT('Ctrl Pts',(7.93836285952821,1.08769799126529,3.77960342890593));
#79992=CARTESIAN_POINT('Ctrl Pts',(7.93995760414107,1.05756293572458,3.78827572482132));
#79993=CARTESIAN_POINT('Ctrl Pts',(7.94155234875394,1.02733715418253,3.79658385444725));
#79994=CARTESIAN_POINT('Ctrl Pts',(7.9431470933668,0.997030207319577,3.80452622092321));
#79995=CARTESIAN_POINT('Ctrl Pts',(7.94901953950072,0.88542869350939,3.83377298490644));
#79996=CARTESIAN_POINT('Ctrl Pts',(7.95489198563463,0.772352361360635,3.85815399328153));
#79997=CARTESIAN_POINT('Ctrl Pts',(7.96076443176855,0.658263451059872,3.87752217646769));
#79998=CARTESIAN_POINT('Ctrl Pts',(7.96662927071339,0.544322331967745,3.89686527003564));
#79999=CARTESIAN_POINT('Ctrl Pts',(7.97249410965824,0.429371646992982,3.91120838339557));
#80000=CARTESIAN_POINT('Ctrl Pts',(7.97835894860308,0.31388771359242,3.920454502128));
#80001=CARTESIAN_POINT('Ctrl Pts',(7.9842177587231,0.198522493154094,3.92969111621237));
#80002=CARTESIAN_POINT('Ctrl Pts',(7.99007656884313,0.0826255241719993,
3.93384112455213));
#80003=CARTESIAN_POINT('Ctrl Pts',(7.99593537896315,-0.0333184521080177,
3.93285886865384));
#80004=CARTESIAN_POINT('Ctrl Pts',(8.00202116784412,-0.153754265388441,
3.9318385587442));
#80005=CARTESIAN_POINT('Ctrl Pts',(8.00810695672509,-0.274240353943659,
3.92528020320809));
#80006=CARTESIAN_POINT('Ctrl Pts',(8.01419274560606,-0.394229199108612,
3.91319209068124));
#80007=CARTESIAN_POINT('Ctrl Pts',(8.02004477568432,-0.50960920073134,3.90156828981002));
#80008=CARTESIAN_POINT('Ctrl Pts',(8.0258968057626,-0.624529003870829,3.8848317437445));
#80009=CARTESIAN_POINT('Ctrl Pts',(8.03174883584087,-0.738504434452509,
3.86304286803732));
#80010=CARTESIAN_POINT('Ctrl Pts',(8.03759997621938,-0.852462537045229,
3.84125730495107));
#80011=CARTESIAN_POINT('Ctrl Pts',(8.04345111659789,-0.965476146661259,
3.81442101708987));
#80012=CARTESIAN_POINT('Ctrl Pts',(8.0493022569764,-1.07707013505366,3.78264575716198));
#80013=CARTESIAN_POINT('Ctrl Pts',(8.0551539245439,-1.18867417808802,3.75086763427644));
#80014=CARTESIAN_POINT('Ctrl Pts',(8.0610055921114,-1.29885794805044,3.71414976790702));
#80015=CARTESIAN_POINT('Ctrl Pts',(8.0668572596789,-1.40716104982742,3.67265391506586));
#80016=CARTESIAN_POINT('Ctrl Pts',(8.07271087136315,-1.51550013346278,3.63114427593534));
#80017=CARTESIAN_POINT('Ctrl Pts',(8.0785644830474,-1.62195692070602,3.58485364168991));
#80018=CARTESIAN_POINT('Ctrl Pts',(8.08441809473164,-1.72609124545215,3.53399179574224));
#80019=CARTESIAN_POINT('Ctrl Pts',(8.09027836083153,-1.83034395063028,3.48307212978844));
#80020=CARTESIAN_POINT('Ctrl Pts',(8.09613862693142,-1.93226855194517,3.42757106145758));
#80021=CARTESIAN_POINT('Ctrl Pts',(8.10199889303131,-2.0314496512951,3.3677442471561));
#80022=CARTESIAN_POINT('Ctrl Pts',(8.10786310620262,-2.13069755219898,3.30787713763518));
#80023=CARTESIAN_POINT('Ctrl Pts',(8.11372731937392,-2.22719792841481,3.24367870912619));
#80024=CARTESIAN_POINT('Ctrl Pts',(8.11959153254523,-2.32056597014865,3.17544683126455));
#80025=CARTESIAN_POINT('Ctrl Pts',(8.12546438111952,-2.41407150188209,3.10711447790095));
#80026=CARTESIAN_POINT('Ctrl Pts',(8.13133722969382,-2.50443517199168,3.03473707857497));
#80027=CARTESIAN_POINT('Ctrl Pts',(8.13721007826811,-2.59130665525716,2.95865152027405));
#80028=CARTESIAN_POINT('Ctrl Pts',(8.13880482288089,-2.61489620097573,2.93799084212519));
#80029=CARTESIAN_POINT('Ctrl Pts',(8.14039956749366,-2.63822846324328,2.91705693601381));
#80030=CARTESIAN_POINT('Ctrl Pts',(8.14199431210644,-2.66129692920873,2.89585698103069));
#80031=CARTESIAN_POINT('Ctrl Pts',(8.14777911715162,-2.74497589399877,2.81895588629643));
#80032=CARTESIAN_POINT('Ctrl Pts',(8.15356392219681,-2.82547909158505,2.73827726983921));
#80033=CARTESIAN_POINT('Ctrl Pts',(8.15934872724199,-2.90243816768425,2.65411787281004));
#80034=CARTESIAN_POINT('Ctrl Pts',(8.1651259627185,-2.97929654081986,2.57006860055269));
#80035=CARTESIAN_POINT('Ctrl Pts',(8.17090319819501,-3.05261972432337,2.48254791182106));
#80036=CARTESIAN_POINT('Ctrl Pts',(8.17668043367151,-3.12207335630604,2.39189192018451));
#80037=CARTESIAN_POINT('Ctrl Pts',(8.18245105966144,-3.19144752937611,2.30133964416816));
#80038=CARTESIAN_POINT('Ctrl Pts',(8.18822168565136,-3.25696069928966,2.20765953720203));
#80039=CARTESIAN_POINT('Ctrl Pts',(8.19399231164128,-3.3183169287146,2.11122281169139));
#80040=CARTESIAN_POINT('Ctrl Pts',(8.19975929030372,-3.37963437789929,2.01484703906882));
#80041=CARTESIAN_POINT('Ctrl Pts',(8.20552626896615,-3.43679987836929,1.91571846826686));
#80042=CARTESIAN_POINT('Ctrl Pts',(8.21129324762859,-3.48955952594087,1.81423904569253));
#80043=CARTESIAN_POINT('Ctrl Pts',(8.21705807448063,-3.54229948750974,1.71279748774162));
#80044=CARTESIAN_POINT('Ctrl Pts',(8.22282290133268,-3.59063666711438,1.60900719962662));
#80045=CARTESIAN_POINT('Ctrl Pts',(8.22858772818473,-3.63436248685362,1.50329581724661));
#80046=CARTESIAN_POINT('Ctrl Pts',(8.23435189644263,-3.67808331120104,1.39759651170765));
#80047=CARTESIAN_POINT('Ctrl Pts',(8.24011606470054,-3.7171936615783,1.28997694314073));
#80048=CARTESIAN_POINT('Ctrl Pts',(8.24588023295844,-3.75153295765055,1.18088503575145));
#80049=CARTESIAN_POINT('Ctrl Pts',(8.25164770053762,-3.78589190900785,1.07173068583187));
#80050=CARTESIAN_POINT('Ctrl Pts',(8.2574151681168,-3.81547422276402,0.961102721236819));
#80051=CARTESIAN_POINT('Ctrl Pts',(8.26318263569598,-3.84016919586695,0.849464270652149));
#80052=CARTESIAN_POINT('Ctrl Pts',(8.26895192380287,-3.86487196405191,0.737790580876233));
#80053=CARTESIAN_POINT('Ctrl Pts',(8.27472121190976,-3.88468424346046,0.625106189909439));
#80054=CARTESIAN_POINT('Ctrl Pts',(8.28049050001665,-3.89954676236548,0.511882846093653));
#80055=CARTESIAN_POINT('Ctrl Pts',(8.28626624305139,-3.91442591009634,0.398532823127594));
#80056=CARTESIAN_POINT('Ctrl Pts',(8.29204198608612,-3.92434420267456,0.284643068235318));
#80057=CARTESIAN_POINT('Ctrl Pts',(8.29781772912086,-3.92929438452151,0.170688721852677));
#80058=CARTESIAN_POINT('Ctrl Pts',(8.30075731206894,-3.93181379545439,0.11269129165692));
#80059=CARTESIAN_POINT('Ctrl Pts',(8.30369689501702,-3.93304713651331,0.0546771189250599));
#80060=CARTESIAN_POINT('Ctrl Pts',(8.3066364779651,-3.93299862266704,-0.00329151928449545));
#80061=CARTESIAN_POINT('',(9.55663647796509,-3.93447037223625,0.00250579399543049));
#80062=CARTESIAN_POINT('Ctrl Pts',(8.3066364779651,-3.93541974394845,-0.00329354551642644));
#80063=CARTESIAN_POINT('Ctrl Pts',(8.31803816225876,-3.93743804138694,-0.228275259319388));
#80064=CARTESIAN_POINT('Ctrl Pts',(8.39572225279899,-3.81735299180208,-1.75900887235532));
#80065=CARTESIAN_POINT('Ctrl Pts',(8.53968874958569,-1.80864929602783,-4.28564802508547));
#80066=CARTESIAN_POINT('Ctrl Pts',(8.73853596832538,2.62717012805726,-3.83874567914929));
#80067=CARTESIAN_POINT('Ctrl Pts',(8.93738318706501,4.64972487276848,0.134349836257429));
#80068=CARTESIAN_POINT('Ctrl Pts',(9.13623040580465,2.40113756831285,3.98403434334837));
#80069=CARTESIAN_POINT('Ctrl Pts',(9.3350776245443,-2.05308553492218,4.17406648931669));
#80070=CARTESIAN_POINT('Ctrl Pts',(9.47521298193112,-3.86306683227914,1.60587142326164));
#80071=CARTESIAN_POINT('Ctrl Pts',(9.54906593307138,-3.93857895538214,0.151689483416833));
#80072=CARTESIAN_POINT('Ctrl Pts',(9.55663647796509,-3.93747221447367,0.00250770581520343));
#80073=CARTESIAN_POINT('',(10.8066364494697,-3.93103660093039,0.00204695750207211));
#80074=CARTESIAN_POINT('Ctrl Pts',(9.55663647796509,-3.9329992023507,0.00250485703357371));
#80075=CARTESIAN_POINT('Ctrl Pts',(9.56242578790064,-3.93307177594825,-0.111446517220179));
#80076=CARTESIAN_POINT('Ctrl Pts',(9.56821509783619,-3.92818786930245,-0.225594949222398));
#80077=CARTESIAN_POINT('Ctrl Pts',(9.57400440777174,-3.91832254996172,-0.339466337744191));
#80078=CARTESIAN_POINT('Ctrl Pts',(9.57978709579029,-3.90846851475097,-0.453207478120546));
#80079=CARTESIAN_POINT('Ctrl Pts',(9.58556978380884,-3.89364442876225,-0.566671784410446));
#80080=CARTESIAN_POINT('Ctrl Pts',(9.5913524718274,-3.87387738108328,-0.679384306803833));
#80081=CARTESIAN_POINT('Ctrl Pts',(9.59724495475224,-3.85373501985801,-0.794236882541554));
#80082=CARTESIAN_POINT('Ctrl Pts',(9.60313743767708,-3.828460061154,-0.908308387270493));
#80083=CARTESIAN_POINT('Ctrl Pts',(9.60902992060192,-3.79813674705107,-1.02110050959752));
#80084=CARTESIAN_POINT('Ctrl Pts',(9.61480474556086,-3.76841891276068,-1.13164045879956));
#80085=CARTESIAN_POINT('Ctrl Pts',(9.6205795705198,-3.73385256954763,-1.24095121187066));
#80086=CARTESIAN_POINT('Ctrl Pts',(9.62635439547874,-3.69456856339101,-1.34857411008921));
#80087=CARTESIAN_POINT('Ctrl Pts',(9.63212798143693,-3.65529298569989,-1.45617391759037));
#80088=CARTESIAN_POINT('Ctrl Pts',(9.63790156739512,-3.61130190230417,-1.56208619036244));
#80089=CARTESIAN_POINT('Ctrl Pts',(9.64367515335332,-3.56277550140972,-1.66586906044704));
#80090=CARTESIAN_POINT('Ctrl Pts',(9.64944898682857,-3.51424702015963,-1.76965637976495));
#80091=CARTESIAN_POINT('Ctrl Pts',(9.65522282030383,-3.46118301601565,-1.87131372986746));
#80092=CARTESIAN_POINT('Ctrl Pts',(9.66099665377908,-3.40381076254495,-1.97042160280056));
#80093=CARTESIAN_POINT('Ctrl Pts',(9.66697793779946,-3.34437715671481,-2.07309036510705));
#80094=CARTESIAN_POINT('Ctrl Pts',(9.67295922181983,-3.28032013107761,-2.17302257094501));
#80095=CARTESIAN_POINT('Ctrl Pts',(9.67894050584021,-3.21194202257755,-2.26978356756772));
#80096=CARTESIAN_POINT('Ctrl Pts',(9.68472252244736,-3.14584194146343,-2.36332095644473));
#80097=CARTESIAN_POINT('Ctrl Pts',(9.69050453905452,-3.07570442656063,-2.45389477069358));
#80098=CARTESIAN_POINT('Ctrl Pts',(9.69628655566168,-3.00184350990193,-2.54114630473329));
#80099=CARTESIAN_POINT('Ctrl Pts',(9.70236747338866,-2.92416435607779,-2.63290830337435));
#80100=CARTESIAN_POINT('Ctrl Pts',(9.70844839111565,-2.84236692233796,-2.72099494731911));
#80101=CARTESIAN_POINT('Ctrl Pts',(9.71452930884263,-2.75685898198012,-2.80503432304767));
#80102=CARTESIAN_POINT('Ctrl Pts',(9.72061022656961,-2.6713510416223,-2.88907369877623));
#80103=CARTESIAN_POINT('Ctrl Pts',(9.7266911442966,-2.58213304953528,-2.96906550752146));
#80104=CARTESIAN_POINT('Ctrl Pts',(9.73277206202358,-2.48964991172429,-3.04468919876089));
#80105=CARTESIAN_POINT('Ctrl Pts',(9.7386445081575,-2.40033736557993,-3.11772028932825));
#80106=CARTESIAN_POINT('Ctrl Pts',(9.74451695429143,-2.30765913822446,-3.18694049328549));
#80107=CARTESIAN_POINT('Ctrl Pts',(9.75038940042535,-2.21197436113287,-3.25202374310072));
#80108=CARTESIAN_POINT('Ctrl Pts',(9.7562542393702,-2.11641353446579,-3.31702268382638));
#80109=CARTESIAN_POINT('Ctrl Pts',(9.76211907831504,-2.01785424186353,-3.37789509727265));
#80110=CARTESIAN_POINT('Ctrl Pts',(9.76798391725989,-1.91668924306658,-3.4343545748092));
#80111=CARTESIAN_POINT('Ctrl Pts',(9.77384272737991,-1.81562823792765,-3.49075601421329));
#80112=CARTESIAN_POINT('Ctrl Pts',(9.77970153749994,-1.71196721318701,-3.54275334047334));
#80113=CARTESIAN_POINT('Ctrl Pts',(9.78556034761997,-1.60612795724475,-3.59010333903591));
#80114=CARTESIAN_POINT('Ctrl Pts',(9.79164613650094,-1.49618833575372,-3.63928774489011));
#80115=CARTESIAN_POINT('Ctrl Pts',(9.79773192538191,-1.38389866963451,-3.68345719638661));
#80116=CARTESIAN_POINT('Ctrl Pts',(9.80381771426288,-1.26976027913928,-3.72239141326112));
#80117=CARTESIAN_POINT('Ctrl Pts',(9.80966974434114,-1.16000601271181,-3.75983014350298));
#80118=CARTESIAN_POINT('Ctrl Pts',(9.81552177441941,-1.04854285075996,-3.7924282516616));
#80119=CARTESIAN_POINT('Ctrl Pts',(9.82137380449768,-0.935836202344345,
-3.82003921477015));
#80120=CARTESIAN_POINT('Ctrl Pts',(9.8272249448762,-0.823146689021302,-3.84764598011028));
#80121=CARTESIAN_POINT('Ctrl Pts',(9.83307608525471,-0.709214466503963,
-3.87026700963775));
#80122=CARTESIAN_POINT('Ctrl Pts',(9.83892722563323,-0.594518079174452,
-3.88780622633571));
#80123=CARTESIAN_POINT('Ctrl Pts',(9.84477889320072,-0.479811357676326,
-3.90534702332079));
#80124=CARTESIAN_POINT('Ctrl Pts',(9.85063056076822,-0.364340743127473,
-3.91780503478093));
#80125=CARTESIAN_POINT('Ctrl Pts',(9.85648222833571,-0.248592189045484,
-3.92513578409022));
#80126=CARTESIAN_POINT('Ctrl Pts',(9.86233584001997,-0.132805179480328,
-3.93246896891596));
#80127=CARTESIAN_POINT('Ctrl Pts',(9.86818945170422,-0.0167404590803251,
-3.93467147828041));
#80128=CARTESIAN_POINT('Ctrl Pts',(9.87404306338847,0.0991144300150325,
-3.9317509241765));
#80129=CARTESIAN_POINT('Ctrl Pts',(9.87990332948836,0.215101023539559,-3.92882704997179));
#80130=CARTESIAN_POINT('Ctrl Pts',(9.88576359558825,0.33087689617723,-3.92076849836277));
#80131=CARTESIAN_POINT('Ctrl Pts',(9.89162386168814,0.445957940592019,-3.90763490045103));
#80132=CARTESIAN_POINT('Ctrl Pts',(9.89748807485944,0.561116495668119,-3.89449245665277));
#80133=CARTESIAN_POINT('Ctrl Pts',(9.90335228803074,0.675578883445476,-3.87626822506084));
#80134=CARTESIAN_POINT('Ctrl Pts',(9.90921650120204,0.788871246722858,-3.85307294974984));
#80135=CARTESIAN_POINT('Ctrl Pts',(9.91508934977633,0.902330439749382,-3.82984351801515));
#80136=CARTESIAN_POINT('Ctrl Pts',(9.92096219835063,1.01461577026381,-3.80162853334182));
#80137=CARTESIAN_POINT('Ctrl Pts',(9.92683504692492,1.12526850393877,-3.76858856789162));
#80138=CARTESIAN_POINT('Ctrl Pts',(9.92842979153769,1.15531573718245,-3.75961671952173));
#80139=CARTESIAN_POINT('Ctrl Pts',(9.93002453615046,1.18524270417137,-3.75028936542526));
#80140=CARTESIAN_POINT('Ctrl Pts',(9.93161928076323,1.21504049546738,-3.74061032378065));
#80141=CARTESIAN_POINT('Ctrl Pts',(9.93749172689715,1.32476710805129,-3.70496847226986));
#80142=CARTESIAN_POINT('Ctrl Pts',(9.94336417303108,1.43310782714073,-3.66443479431161));
#80143=CARTESIAN_POINT('Ctrl Pts',(9.949236619165,1.53959417575555,-3.61913508645085));
#80144=CARTESIAN_POINT('Ctrl Pts',(9.95510145810985,1.64594258154894,-3.57389406000412));
#80145=CARTESIAN_POINT('Ctrl Pts',(9.96096629705469,1.75044101704354,-3.52389944173168));
#80146=CARTESIAN_POINT('Ctrl Pts',(9.96683113599954,1.85263618353321,-3.4693267605493));
#80147=CARTESIAN_POINT('Ctrl Pts',(9.97268994611955,1.9547262973925,-3.41481017794675));
#80148=CARTESIAN_POINT('Ctrl Pts',(9.97854875623955,2.05451748923695,-3.35572508660673));
#80149=CARTESIAN_POINT('Ctrl Pts',(9.98440756635956,2.15157709950946,-3.29229479009193));
#80150=CARTESIAN_POINT('Ctrl Pts',(9.99049335524053,2.25239693918485,-3.22640711233154));
#80151=CARTESIAN_POINT('Ctrl Pts',(9.9965791441215,2.35026884774362,-3.15583091891095));
#80152=CARTESIAN_POINT('Ctrl Pts',(10.0026649330025,2.44473645447035,-3.08086881710074));
#80153=CARTESIAN_POINT('Ctrl Pts',(10.0085169630807,2.53557550373734,-3.00878605460214));
#80154=CARTESIAN_POINT('Ctrl Pts',(10.014368993159,2.6232665958657,-2.93264838003059));
#80155=CARTESIAN_POINT('Ctrl Pts',(10.0202210232373,2.70743482298513,-2.85276807316814));
#80156=CARTESIAN_POINT('Ctrl Pts',(10.0260721636158,2.79159025378436,-2.77289991072193));
#80157=CARTESIAN_POINT('Ctrl Pts',(10.0319233039943,2.87222358476016,-2.68929053181993));
#80158=CARTESIAN_POINT('Ctrl Pts',(10.0377744443728,2.94899524122218,-2.60229054243544));
#80159=CARTESIAN_POINT('Ctrl Pts',(10.0436261119403,3.02577381482653,-2.51528271433368));
#80160=CARTESIAN_POINT('Ctrl Pts',(10.0494777795078,3.09868974873285,-2.42488397841122));
#80161=CARTESIAN_POINT('Ctrl Pts',(10.0553294470753,3.16744286876422,-2.33147907413184));
#80162=CARTESIAN_POINT('Ctrl Pts',(10.0611830587595,3.23621883084693,-2.23804313766632));
#80163=CARTESIAN_POINT('Ctrl Pts',(10.0670366704437,3.30082898408807,-2.14159937961505));
#80164=CARTESIAN_POINT('Ctrl Pts',(10.072890282128,3.36101611273705,-2.04256204065431));
#80165=CARTESIAN_POINT('Ctrl Pts',(10.0787505482279,3.42127166242138,-1.94341211554066));
#80166=CARTESIAN_POINT('Ctrl Pts',(10.0846108143278,3.47709393676087,-1.8416630780679));
#80167=CARTESIAN_POINT('Ctrl Pts',(10.0904710804276,3.52827133617625,-1.73775440678971));
#80168=CARTESIAN_POINT('Ctrl Pts',(10.0963352935989,3.57948320516119,-1.633775749791));
#80169=CARTESIAN_POINT('Ctrl Pts',(10.1021995067702,3.62604380416773,-1.52763494023623));
#80170=CARTESIAN_POINT('Ctrl Pts',(10.1080637199415,3.66779007265798,-1.41979047148216));
#80171=CARTESIAN_POINT('Ctrl Pts',(10.1139365685158,3.70959781501364,-1.31178719532815));
#80172=CARTESIAN_POINT('Ctrl Pts',(10.1198094170901,3.74657694631575,-1.20207564326126));
#80173=CARTESIAN_POINT('Ctrl Pts',(10.1256822656644,3.77861449895025,-1.09112852969892));
#80174=CARTESIAN_POINT('Ctrl Pts',(10.1272770102772,3.78731414680017,-1.06100135896997));
#80175=CARTESIAN_POINT('Ctrl Pts',(10.12887175489,3.79564971086845,-1.03078313170016));
#80176=CARTESIAN_POINT('Ctrl Pts',(10.1304664995029,3.80361958561641,-1.0004834071164));
#80177=CARTESIAN_POINT('Ctrl Pts',(10.1363389456368,3.83296764534644,-0.888908488437121));
#80178=CARTESIAN_POINT('Ctrl Pts',(10.1422113917707,3.85745129025957,-0.775854335070879));
#80179=CARTESIAN_POINT('Ctrl Pts',(10.1480838379046,3.8769230312308,-0.661783053509366));
#80180=CARTESIAN_POINT('Ctrl Pts',(10.1539486768494,3.89636954843464,-0.547859540320254));
#80181=CARTESIAN_POINT('Ctrl Pts',(10.1598135157943,3.91081700393777,-0.432921922864211));
#80182=CARTESIAN_POINT('Ctrl Pts',(10.1656783547391,3.92016795097699,-0.317446430335651));
#80183=CARTESIAN_POINT('Ctrl Pts',(10.1715371648591,3.92950928560874,-0.202089642092598));
#80184=CARTESIAN_POINT('Ctrl Pts',(10.1773959749791,3.93376449929369,-0.0861964880890872));
#80185=CARTESIAN_POINT('Ctrl Pts',(10.1832547850991,3.9328874935267,0.0297483320758639));
#80186=CARTESIAN_POINT('Ctrl Pts',(10.1893405739801,3.93197651129038,0.150185021934936));
#80187=CARTESIAN_POINT('Ctrl Pts',(10.1954263628611,3.92552753134741,0.270677014284574));
#80188=CARTESIAN_POINT('Ctrl Pts',(10.2015121517421,3.91354834531258,0.390676783161187));
#80189=CARTESIAN_POINT('Ctrl Pts',(10.2073641818203,3.90202928700147,0.50606728890923));
#80190=CARTESIAN_POINT('Ctrl Pts',(10.2132162118986,3.88539706785114,0.621002237527868));
#80191=CARTESIAN_POINT('Ctrl Pts',(10.2190682419769,3.86371166387371,0.73499740029896));
#80192=CARTESIAN_POINT('Ctrl Pts',(10.2249193823554,3.84202955678616,0.848975232081036));
#80193=CARTESIAN_POINT('Ctrl Pts',(10.2307705227339,3.81529586962827,0.962013156139898));
#80194=CARTESIAN_POINT('Ctrl Pts',(10.2366216631124,3.78362192375809,1.07363594297933));
#80195=CARTESIAN_POINT('Ctrl Pts',(10.2424733306799,3.75194512405866,1.18526878705557));
#80196=CARTESIAN_POINT('Ctrl Pts',(10.2483249982474,3.71532729363835,1.2954858427646));
#80197=CARTESIAN_POINT('Ctrl Pts',(10.2541766658149,3.6739297715127,1.40382656834547));
#80198=CARTESIAN_POINT('Ctrl Pts',(10.2600302774992,3.63251849576636,1.5122032882847));
#80199=CARTESIAN_POINT('Ctrl Pts',(10.2658838891834,3.5863245181947,1.61870205262089));
#80200=CARTESIAN_POINT('Ctrl Pts',(10.2717375008677,3.5355572225572,1.72288250499667));
#80201=CARTESIAN_POINT('Ctrl Pts',(10.2775977669676,3.48473221439894,1.82718139024236));
#80202=CARTESIAN_POINT('Ctrl Pts',(10.2834580330675,3.42932369238321,1.92915633141456));
#80203=CARTESIAN_POINT('Ctrl Pts',(10.2893182991673,3.3695869357278,2.0283916985071));
#80204=CARTESIAN_POINT('Ctrl Pts',(10.2951825123387,3.30980994450955,2.12769390370464));
#80205=CARTESIAN_POINT('Ctrl Pts',(10.30104672551,3.24569914198479,2.22425251716007));
#80206=CARTESIAN_POINT('Ctrl Pts',(10.3069109386813,3.17755204834987,2.31768245884278));
#80207=CARTESIAN_POINT('Ctrl Pts',(10.3127837872556,3.10930460406272,2.41124998167659));
#80208=CARTESIAN_POINT('Ctrl Pts',(10.3186566358299,3.03700926341205,2.50167931612669));
#80209=CARTESIAN_POINT('Ctrl Pts',(10.3245294844042,2.961002595234,2.58861983130345));
#80210=CARTESIAN_POINT('Ctrl Pts',(10.326124229017,2.94036333932942,2.61222812231557));
#80211=CARTESIAN_POINT('Ctrl Pts',(10.3277189736297,2.91945062202231,2.6355793780091));
#80212=CARTESIAN_POINT('Ctrl Pts',(10.3293137182425,2.89827161648838,2.6586670790187));
#80213=CARTESIAN_POINT('Ctrl Pts',(10.3351861643765,2.82028259669823,2.74368462944437));
#80214=CARTESIAN_POINT('Ctrl Pts',(10.3410586105104,2.73841899260408,2.82541002810544));
#80215=CARTESIAN_POINT('Ctrl Pts',(10.3469310566443,2.65298978342595,2.90346934012356));
#80216=CARTESIAN_POINT('Ctrl Pts',(10.3527958955891,2.56767123957049,2.98142753381183));
#80217=CARTESIAN_POINT('Ctrl Pts',(10.358660734534,2.47879657831782,3.05572880879589));
#80218=CARTESIAN_POINT('Ctrl Pts',(10.3645255734788,2.38671371744883,3.12603368998826));
#80219=CARTESIAN_POINT('Ctrl Pts',(10.3703843835989,2.29472551415571,3.19626630051523));
#80220=CARTESIAN_POINT('Ctrl Pts',(10.3762431937189,2.19953599752989,3.26251043922199));
#80221=CARTESIAN_POINT('Ctrl Pts',(10.3821020038389,2.10152797526098,3.32446524559898));
#80222=CARTESIAN_POINT('Ctrl Pts',(10.3881877927199,1.99972298073973,3.38882027060366));
#80223=CARTESIAN_POINT('Ctrl Pts',(10.3942735816008,1.89487701320576,3.44854658519396));
#80224=CARTESIAN_POINT('Ctrl Pts',(10.4003593704818,1.78745486938629,3.50335469085094));
#80225=CARTESIAN_POINT('Ctrl Pts',(10.4062114005601,1.68415887456965,3.55605758428199));
#80226=CARTESIAN_POINT('Ctrl Pts',(10.4120634306383,1.57848136005072,3.60421291683126));
#80227=CARTESIAN_POINT('Ctrl Pts',(10.4179154607166,1.47086209298752,3.64760931342878));
#80228=CARTESIAN_POINT('Ctrl Pts',(10.4237666010951,1.36325918756878,3.69099911235628));
#80229=CARTESIAN_POINT('Ctrl Pts',(10.4296177414736,1.25371549983707,3.72963125936829));
#80230=CARTESIAN_POINT('Ctrl Pts',(10.4354688818521,1.14269098967903,3.76334243752895));
#80231=CARTESIAN_POINT('Ctrl Pts',(10.4413205494197,1.03165647618905,3.79705665307392));
#80232=CARTESIAN_POINT('Ctrl Pts',(10.4471722169872,0.919141270591103,3.82584889826477));
#80233=CARTESIAN_POINT('Ctrl Pts',(10.4530238845547,0.805620022377508,3.84960587327384));
#80234=CARTESIAN_POINT('Ctrl Pts',(10.4588774962389,0.692061058666013,3.87337074113254));
#80235=CARTESIAN_POINT('Ctrl Pts',(10.4647311079231,0.577495792100148,3.89209692775887));
#80236=CARTESIAN_POINT('Ctrl Pts',(10.4705847196073,0.462407870315806,3.90572246344642));
#80237=CARTESIAN_POINT('Ctrl Pts',(10.4764449857072,0.347189115993989,3.91936348871256));
#80238=CARTESIAN_POINT('Ctrl Pts',(10.4823052518071,0.231446931268476,3.92789224090785));
#80239=CARTESIAN_POINT('Ctrl Pts',(10.488165517907,0.115668979892364,3.93129872778585));
#80240=CARTESIAN_POINT('Ctrl Pts',(10.4940297310783,-0.000186951534076524,
3.93470750903869));
#80241=CARTESIAN_POINT('Ctrl Pts',(10.4998939442496,-0.116078285278519,
3.93298716144111));
#80242=CARTESIAN_POINT('Ctrl Pts',(10.5057581574209,-0.23152021637001,3.92617974491897));
#80243=CARTESIAN_POINT('Ctrl Pts',(10.5116310059952,-0.347132142576803,
3.91936230407078));
#80244=CARTESIAN_POINT('Ctrl Pts',(10.5175038545695,-0.462292935751987,
3.90744288612649));
#80245=CARTESIAN_POINT('Ctrl Pts',(10.5233767031438,-0.576525655849704,
3.89051502607908));
#80246=CARTESIAN_POINT('Ctrl Pts',(10.5249714477566,-0.607545017693227,
3.88591834471144));
#80247=CARTESIAN_POINT('Ctrl Pts',(10.5265661923694,-0.638496022515862,
3.88095264354574));
#80248=CARTESIAN_POINT('Ctrl Pts',(10.5281609369822,-0.669369307559842,
3.87562043163373));
#80249=CARTESIAN_POINT('Ctrl Pts',(10.5340333831161,-0.783056290381801,
3.85598523300877));
#80250=CARTESIAN_POINT('Ctrl Pts',(10.53990582925,-0.89606891319852,3.83131059936058));
#80251=CARTESIAN_POINT('Ctrl Pts',(10.5457782753839,-1.00792555042906,3.80165425634582));
#80252=CARTESIAN_POINT('Ctrl Pts',(10.5516431143287,-1.11963728814594,3.77203633027068));
#80253=CARTESIAN_POINT('Ctrl Pts',(10.5575079532736,-1.23019562233906,3.73744963315401));
#80254=CARTESIAN_POINT('Ctrl Pts',(10.5633727922184,-1.33912686083216,3.69800327887872));
#80255=CARTESIAN_POINT('Ctrl Pts',(10.5692316023384,-1.44794612227647,3.65859747391141));
#80256=CARTESIAN_POINT('Ctrl Pts',(10.5750904124584,-1.55514122856975,3.61434208807975));
#80257=CARTESIAN_POINT('Ctrl Pts',(10.5809492225784,-1.66025210513203,3.56539646426658));
#80258=CARTESIAN_POINT('Ctrl Pts',(10.5870350114594,-1.76943512877518,3.51455461633608));
#80259=CARTESIAN_POINT('Ctrl Pts',(10.5931208003404,-1.87636872520191,3.45865188368426));
#80260=CARTESIAN_POINT('Ctrl Pts',(10.5992065892213,-1.98055804532792,3.39792272264789));
#80261=CARTESIAN_POINT('Ctrl Pts',(10.6050586192996,-2.08074539114887,3.33952620512759));
#80262=CARTESIAN_POINT('Ctrl Pts',(10.6109106493779,-2.17839500030641,3.27666741927234));
#80263=CARTESIAN_POINT('Ctrl Pts',(10.6167626794561,-2.27309127560223,3.20960200847099));
#80264=CARTESIAN_POINT('Ctrl Pts',(10.6226138198347,-2.36777315397059,3.14254679380303));
#80265=CARTESIAN_POINT('Ctrl Pts',(10.6284649602132,-2.45950225400597,3.07128646464774));
#80266=CARTESIAN_POINT('Ctrl Pts',(10.6343161005917,-2.54789248702578,2.99611963622242));
#80267=CARTESIAN_POINT('Ctrl Pts',(10.6401677681592,-2.6362906840246,2.9209460352497));
#80268=CARTESIAN_POINT('Ctrl Pts',(10.6460194357267,-2.72134910107028,2.84186550310911));
#80269=CARTESIAN_POINT('Ctrl Pts',(10.6518711032943,-2.80271578149733,2.75921605680777));
#80270=CARTESIAN_POINT('Ctrl Pts',(10.6577247149785,-2.88410949461566,2.67653915163807));
#80271=CARTESIAN_POINT('Ctrl Pts',(10.6635783266627,-2.96180874242292,2.59029126900251));
#80272=CARTESIAN_POINT('Ctrl Pts',(10.669431938347,-3.03549988222078,2.50084574994893));
#80273=CARTESIAN_POINT('Ctrl Pts',(10.6752922044469,-3.10927479448281,2.41129854877237));
#80274=CARTESIAN_POINT('Ctrl Pts',(10.6811524705468,-3.17903224124492,2.31854677487927));
#80275=CARTESIAN_POINT('Ctrl Pts',(10.6870127366467,-3.24450013215575,2.22299525245587));
#80276=CARTESIAN_POINT('Ctrl Pts',(10.692876949818,-3.31001211772647,2.12737937311147));
#80277=CARTESIAN_POINT('Ctrl Pts',(10.6987411629893,-3.37122857678235,2.02896034053399));
#80278=CARTESIAN_POINT('Ctrl Pts',(10.7046053761606,-3.42792275149611,1.92816871921918));
#80279=CARTESIAN_POINT('Ctrl Pts',(10.7104782247349,-3.48470041175713,1.82722867624189));
#80280=CARTESIAN_POINT('Ctrl Pts',(10.7163510733092,-3.53694231115576,1.7239094391362));
#80281=CARTESIAN_POINT('Ctrl Pts',(10.7222239218835,-3.58446924579559,1.61866278944863));
#80282=CARTESIAN_POINT('Ctrl Pts',(10.7238186664962,-3.5973749630162,1.59008355307292));
#80283=CARTESIAN_POINT('Ctrl Pts',(10.725413411109,-3.60993329615207,1.56136228644923));
#80284=CARTESIAN_POINT('Ctrl Pts',(10.7270081557218,-3.6221412933009,1.53250822228284));
#80285=CARTESIAN_POINT('Ctrl Pts',(10.7336438455333,-3.67293844392245,1.41244723065286));
#80286=CARTESIAN_POINT('Ctrl Pts',(10.7402795353448,-3.71781296604215,1.28973834100993));
#80287=CARTESIAN_POINT('Ctrl Pts',(10.7469152251562,-3.75651119405273,1.16495177967011));
#80288=CARTESIAN_POINT('Ctrl Pts',(10.753420604165,-3.79444947135759,1.04261576038941));
#80289=CARTESIAN_POINT('Ctrl Pts',(10.7599259831737,-3.82645164497718,0.918283160435526));
#80290=CARTESIAN_POINT('Ctrl Pts',(10.7664313621825,-3.85232520642628,0.79251467111511));
#80291=CARTESIAN_POINT('Ctrl Pts',(10.7731322073953,-3.87897618712105,0.662967233763629));
#80292=CARTESIAN_POINT('Ctrl Pts',(10.7798330526081,-3.89912430388189,0.531896459975942));
#80293=CARTESIAN_POINT('Ctrl Pts',(10.7865338978209,-3.91261283787805,0.399937221163387));
#80294=CARTESIAN_POINT('Ctrl Pts',(10.7932347430338,-3.92610137187421,0.267977982350833));
#80295=CARTESIAN_POINT('Ctrl Pts',(10.7999355882466,-3.93293015768591,0.13513055279225));
#80296=CARTESIAN_POINT('Ctrl Pts',(10.8066364334594,-3.93299946662572,0.00204829729017384));
#80297=CARTESIAN_POINT('',(12.0566365093898,-3.93228720468563,-0.00328288393016922));
#80298=CARTESIAN_POINT('Ctrl Pts',(10.8066364779651,-3.92754306292935,0.00204457292697976));
#80299=CARTESIAN_POINT('Ctrl Pts',(10.8463761101305,-3.92384443896021,-0.786112286478094));
#80300=CARTESIAN_POINT('Ctrl Pts',(10.9523981485427,-3.31103251769868,-2.89414287706054));
#80301=CARTESIAN_POINT('Ctrl Pts',(11.124702593201,0.130128929703057,-4.64984491489734));
#80302=CARTESIAN_POINT('Ctrl Pts',(11.3235498119408,3.98185303646486,-2.40475314054045));
#80303=CARTESIAN_POINT('Ctrl Pts',(11.5223970306803,4.1759284859373,2.04929562320325));
#80304=CARTESIAN_POINT('Ctrl Pts',(11.7212442494201,0.534081544591076,4.62090339378258));
#80305=CARTESIAN_POINT('Ctrl Pts',(11.8993240651815,-3.16677355483953,3.122576578027));
#80306=CARTESIAN_POINT('Ctrl Pts',(12.0111214746966,-3.92290114994221,0.898019261252334));
#80307=CARTESIAN_POINT('Ctrl Pts',(12.0566364779651,-3.92997078819238,-0.00328032767339696));
#80308=CARTESIAN_POINT('',(13.3066364779246,-3.93299994461018,-0.000660072963464881));
#80309=CARTESIAN_POINT('Ctrl Pts',(12.056636519041,-3.93299862922908,-0.00328366901515391));
#80310=CARTESIAN_POINT('Ctrl Pts',(12.0635891360599,-3.93288359427993,-0.141066221162596));
#80311=CARTESIAN_POINT('Ctrl Pts',(12.0705417530788,-3.92552444896857,-0.278537064495642));
#80312=CARTESIAN_POINT('Ctrl Pts',(12.0774943700977,-3.9110422068447,-0.415015489204126));
#80313=CARTESIAN_POINT('Ctrl Pts',(12.0845298037661,-3.89638745834408,-0.55311958750304));
#80314=CARTESIAN_POINT('Ctrl Pts',(12.0915652374345,-3.87443898224943,-0.69020742892668));
#80315=CARTESIAN_POINT('Ctrl Pts',(12.0986006711029,-3.84537148345569,-0.825595030402807));
#80316=CARTESIAN_POINT('Ctrl Pts',(12.1053800097017,-3.81736206344984,-0.956054421499278));
#80317=CARTESIAN_POINT('Ctrl Pts',(12.1121593483005,-3.78274283410755,-1.08493521447258));
#80318=CARTESIAN_POINT('Ctrl Pts',(12.1189386868992,-3.741711752173,-1.21164440478651));
#80319=CARTESIAN_POINT('Ctrl Pts',(12.1248111330331,-3.70616952117716,-1.321403326538));
#80320=CARTESIAN_POINT('Ctrl Pts',(12.130683579167,-3.66573420768565,-1.42978079598826));
#80321=CARTESIAN_POINT('Ctrl Pts',(12.136556025301,-3.62053118292523,-1.53630822215661));
#80322=CARTESIAN_POINT('Ctrl Pts',(12.1424208642458,-3.57538671433511,-1.64269765229173));
#80323=CARTESIAN_POINT('Ctrl Pts',(12.1482857031906,-3.52548697654204,-1.74724142802812));
#80324=CARTESIAN_POINT('Ctrl Pts',(12.1541505421355,-3.47100708690141,-1.84948609150764));
#80325=CARTESIAN_POINT('Ctrl Pts',(12.1600093522555,-3.41658320045438,-1.95162565147609));
#80326=CARTESIAN_POINT('Ctrl Pts',(12.1658681623755,-3.35758872027433,-2.05147043750303));
#80327=CARTESIAN_POINT('Ctrl Pts',(12.1717269724956,-3.29424655707933,-2.14858758750277));
#80328=CARTESIAN_POINT('Ctrl Pts',(12.1778127613765,-3.22845042705099,-2.24946719607712));
#80329=CARTESIAN_POINT('Ctrl Pts',(12.1838985502575,-3.15796310726952,-2.34740313081352));
#80330=CARTESIAN_POINT('Ctrl Pts',(12.1899843391385,-3.08308679060405,-2.44193874648871));
#80331=CARTESIAN_POINT('Ctrl Pts',(12.1958363692168,-3.01108651819134,-2.53284319243957));
#80332=CARTESIAN_POINT('Ctrl Pts',(12.201688399295,-2.93502847777535,-2.62060336345059));
#80333=CARTESIAN_POINT('Ctrl Pts',(12.2075404293733,-2.8552246086817,-2.70484406832971));
#80334=CARTESIAN_POINT('Ctrl Pts',(12.2133915697518,-2.7754328723833,-2.7890719658696));
#80335=CARTESIAN_POINT('Ctrl Pts',(12.2192427101303,-2.69189672393637,-2.86978116117752));
#80336=CARTESIAN_POINT('Ctrl Pts',(12.2250938505088,-2.60496646091622,-2.9466317614357));
#80337=CARTESIAN_POINT('Ctrl Pts',(12.2309455180763,-2.51802836546109,-3.02348928594911));
#80338=CARTESIAN_POINT('Ctrl Pts',(12.2367971856438,-2.42769585721846,-3.09648725049883));
#80339=CARTESIAN_POINT('Ctrl Pts',(12.2426488532113,-2.33435340300642,-3.1653251317791));
#80340=CARTESIAN_POINT('Ctrl Pts',(12.2485024648956,-2.24097993735587,-3.23418588327142));
#80341=CARTESIAN_POINT('Ctrl Pts',(12.2543560765798,-2.14459486978902,-3.29888355802961));
#80342=CARTESIAN_POINT('Ctrl Pts',(12.2602096882641,-2.04561220732036,-3.35916056437645));
#80343=CARTESIAN_POINT('Ctrl Pts',(12.266069954364,-1.94651702085566,-3.41950609393184));
#80344=CARTESIAN_POINT('Ctrl Pts',(12.2719302204639,-1.84481869873655,-3.47542070934868));
#80345=CARTESIAN_POINT('Ctrl Pts',(12.2777904865638,-1.74095652725323,-3.52669241219225));
#80346=CARTESIAN_POINT('Ctrl Pts',(12.2836546997351,-1.63702440136828,-3.57799864812175));
#80347=CARTESIAN_POINT('Ctrl Pts',(12.2895189129064,-1.53092590156432,-3.62465557871271));
#80348=CARTESIAN_POINT('Ctrl Pts',(12.2953831260777,-1.42311937298879,-3.66649972729087));
#80349=CARTESIAN_POINT('Ctrl Pts',(12.301255974652,-1.31515409288238,-3.70840549386871));
#80350=CARTESIAN_POINT('Ctrl Pts',(12.3071288232263,-1.20547615432937,-3.74548420209323));
#80351=CARTESIAN_POINT('Ctrl Pts',(12.3130016718006,-1.0945581690045,-3.77762245528395));
#80352=CARTESIAN_POINT('Ctrl Pts',(12.3145964164134,-1.06443890791312,-3.78634944789959));
#80353=CARTESIAN_POINT('Ctrl Pts',(12.3161911610262,-1.03422825981636,-3.79471243954144));
#80354=CARTESIAN_POINT('Ctrl Pts',(12.317785905639,-1.00393578247977,-3.80270981599395));
#80355=CARTESIAN_POINT('Ctrl Pts',(12.3236583517729,-0.892387550872972,
-3.83215914728696));
#80356=CARTESIAN_POINT('Ctrl Pts',(12.3295307979068,-0.779355669449756,
-3.85674540856278));
#80357=CARTESIAN_POINT('Ctrl Pts',(12.3354032440407,-0.665302110626149,
-3.87632069127367));
#80358=CARTESIAN_POINT('Ctrl Pts',(12.3412680829856,-0.551396297216714,
-3.89587061608884));
#80359=CARTESIAN_POINT('Ctrl Pts',(12.3471329219304,-0.436471841991697,
-3.91042240182997));
#80360=CARTESIAN_POINT('Ctrl Pts',(12.3529977608753,-0.321004885490681,
-3.91987816947046));
#80361=CARTESIAN_POINT('Ctrl Pts',(12.3588565709953,-0.205656624500349,
-3.92932421695202));
#80362=CARTESIAN_POINT('Ctrl Pts',(12.3647153811153,-0.0897673809748686,
-3.93368463247566));
#80363=CARTESIAN_POINT('Ctrl Pts',(12.3705741912353,0.0261781875330107,
-3.93291287756257));
#80364=CARTESIAN_POINT('Ctrl Pts',(12.3766599801163,0.14661565472656,-3.93211122375015));
#80365=CARTESIAN_POINT('Ctrl Pts',(12.3827457689973,0.267113451580874,-3.92577162471444));
#80366=CARTESIAN_POINT('Ctrl Pts',(12.3888315578782,0.387124045285005,-3.91390137504283));
#80367=CARTESIAN_POINT('Ctrl Pts',(12.3946835879565,0.502524960072433,-3.90248706878387));
#80368=CARTESIAN_POINT('Ctrl Pts',(12.4005356180348,0.617474959459671,-3.88595919025421));
#80369=CARTESIAN_POINT('Ctrl Pts',(12.406387648113,0.731489760484053,-3.86437727587602));
#80370=CARTESIAN_POINT('Ctrl Pts',(12.4122387884915,0.845487227533909,-3.84279864265388));
#80371=CARTESIAN_POINT('Ctrl Pts',(12.41808992887,0.95854937288855,-3.81616757822868));
#80372=CARTESIAN_POINT('Ctrl Pts',(12.4239410692485,1.07020086619408,-3.78459497251654));
#80373=CARTESIAN_POINT('Ctrl Pts',(12.429792736816,1.18186241932278,-3.75301952210593));
#80374=CARTESIAN_POINT('Ctrl Pts',(12.4356444043835,1.29211266995565,-3.71650175780903));
#80375=CARTESIAN_POINT('Ctrl Pts',(12.441496071951,1.40049093006382,-3.67520260051184));
#80376=CARTESIAN_POINT('Ctrl Pts',(12.4473496836353,1.50890519700026,-3.63388972227409));
#80377=CARTESIAN_POINT('Ctrl Pts',(12.4532032953195,1.61544585067027,-3.58779243944179));
#80378=CARTESIAN_POINT('Ctrl Pts',(12.4590569070037,1.71967234482693,-3.53711973594865));
#80379=CARTESIAN_POINT('Ctrl Pts',(12.4649171731036,1.82401732419438,-3.48638942746741));
#80380=CARTESIAN_POINT('Ctrl Pts',(12.4707774392035,1.92604252119309,-3.43107349742524));
#80381=CARTESIAN_POINT('Ctrl Pts',(12.4766377053034,2.02533207425494,-3.37142684764095));
#80382=CARTESIAN_POINT('Ctrl Pts',(12.4825019184747,2.12468850191775,-3.31174002398357));
#80383=CARTESIAN_POINT('Ctrl Pts',(12.488366131646,2.22130527304521,-3.24771690027245));
#80384=CARTESIAN_POINT('Ctrl Pts',(12.4942303448173,2.31479703768735,-3.17965464701969));
#80385=CARTESIAN_POINT('Ctrl Pts',(12.5001031933916,2.40842647451834,-3.11149216804737));
#80386=CARTESIAN_POINT('Ctrl Pts',(12.5059760419659,2.49892139879179,-3.03927894564602));
#80387=CARTESIAN_POINT('Ctrl Pts',(12.5118488905401,2.58593087423756,-2.96335123022314));
#80388=CARTESIAN_POINT('Ctrl Pts',(12.5134436351529,2.60955789108877,-2.94273341357065));
#80389=CARTESIAN_POINT('Ctrl Pts',(12.5150383797657,2.6329281209656,-2.92184190230099));
#80390=CARTESIAN_POINT('Ctrl Pts',(12.5166331243785,2.65603503799387,-2.90068386366886));
#80391=CARTESIAN_POINT('Ctrl Pts',(12.5225055705125,2.74112334898775,-2.822772051853));
#80392=CARTESIAN_POINT('Ctrl Pts',(12.5283780166464,2.82292302678023,-2.74098266883384));
#80393=CARTESIAN_POINT('Ctrl Pts',(12.5342504627803,2.9010598561669,-2.65562435425963));
#80394=CARTESIAN_POINT('Ctrl Pts',(12.5401153017251,2.97909546680741,-2.57037661317097));
#80395=CARTESIAN_POINT('Ctrl Pts',(12.54598014067,3.05347738836451,-2.48156943653244));
#80396=CARTESIAN_POINT('Ctrl Pts',(12.5518449796148,3.12386583006348,-2.38955043381842));
#80397=CARTESIAN_POINT('Ctrl Pts',(12.5577037897349,3.19418191520013,-2.2976260230366));
#80398=CARTESIAN_POINT('Ctrl Pts',(12.5635625998549,3.26051243619574,-2.20249667965134));
#80399=CARTESIAN_POINT('Ctrl Pts',(12.5694214099749,3.32255618516582,-2.10454493808433));
#80400=CARTESIAN_POINT('Ctrl Pts',(12.5755071988559,3.38700359852803,-2.00279840466059));
#80401=CARTESIAN_POINT('Ctrl Pts',(12.5815929877368,3.44682506386771,-1.89800669770205));
#80402=CARTESIAN_POINT('Ctrl Pts',(12.5876787766178,3.50173066085964,-1.79063435094816));
#80403=CARTESIAN_POINT('Ctrl Pts',(12.5935308066961,3.55452730092494,-1.68738624046198));
#80404=CARTESIAN_POINT('Ctrl Pts',(12.5993828367744,3.60277854383915,-1.58175248314428));
#80405=CARTESIAN_POINT('Ctrl Pts',(12.6052348668526,3.64627261541475,-1.4741726540933));
#80406=CARTESIAN_POINT('Ctrl Pts',(12.6110860072312,3.68976007447055,-1.36660918069089));
#80407=CARTESIAN_POINT('Ctrl Pts',(12.6169371476097,3.72849164534272,-1.2571006069517));
#80408=CARTESIAN_POINT('Ctrl Pts',(12.6227882879882,3.76230359362784,-1.14610674431968));
#80409=CARTESIAN_POINT('Ctrl Pts',(12.6286399555557,3.79611858837664,-1.03510288111719));
#80410=CARTESIAN_POINT('Ctrl Pts',(12.6344916231232,3.82501295891772,-0.922613858431041));
#80411=CARTESIAN_POINT('Ctrl Pts',(12.6403432906907,3.84887297460058,-0.809114222708547));
#80412=CARTESIAN_POINT('Ctrl Pts',(12.6461969023749,3.87274091736668,-0.695576878668005));
#80413=CARTESIAN_POINT('Ctrl Pts',(12.6520505140592,3.89157109446155,-0.581028658256058));
#80414=CARTESIAN_POINT('Ctrl Pts',(12.6579041257434,3.90530109716657,-0.465953152655482));
#80415=CARTESIAN_POINT('Ctrl Pts',(12.6637643918433,3.91904670820877,-0.350746828632537));
#80416=CARTESIAN_POINT('Ctrl Pts',(12.6696246579432,3.92768052343756,-0.235012433685925));
#80417=CARTESIAN_POINT('Ctrl Pts',(12.6754849240431,3.93119210792718,-0.119237622297209));
#80418=CARTESIAN_POINT('Ctrl Pts',(12.6813491372144,3.93470605757812,-0.00338483297355624));
#80419=CARTESIAN_POINT('Ctrl Pts',(12.6872133503857,3.93309091262892,0.112508014690212));
#80420=CARTESIAN_POINT('Ctrl Pts',(12.693077563557,3.92638829289976,0.227956077742426));
#80421=CARTESIAN_POINT('Ctrl Pts',(12.6989504121313,3.91967580316405,0.343574144939991));
#80422=CARTESIAN_POINT('Ctrl Pts',(12.7048232607056,3.90786092891218,0.458745710681152));
#80423=CARTESIAN_POINT('Ctrl Pts',(12.7106961092799,3.89103677214975,0.57299375020889));
#80424=CARTESIAN_POINT('Ctrl Pts',(12.7122908538927,3.88646825092499,0.604017271972283));
#80425=CARTESIAN_POINT('Ctrl Pts',(12.7138855985055,3.88153064800218,0.634972771725714));
#80426=CARTESIAN_POINT('Ctrl Pts',(12.7154803431183,3.87622646393288,0.665850884437639));
#80427=CARTESIAN_POINT('Ctrl Pts',(12.7213527892522,3.85669447430789,0.77955564453807));
#80428=CARTESIAN_POINT('Ctrl Pts',(12.7272252353861,3.83212243957652,0.892590619527022));
#80429=CARTESIAN_POINT('Ctrl Pts',(12.73309768152,3.80256764816943,1.00447413162073));
#80430=CARTESIAN_POINT('Ctrl Pts',(12.7389625204649,3.77305114215161,1.11621270938705));
#80431=CARTESIAN_POINT('Ctrl Pts',(12.7448273594097,3.73856482012168,1.22680239457453));
#80432=CARTESIAN_POINT('Ctrl Pts',(12.7506921983545,3.69921736591707,1.33576939615249));
#80433=CARTESIAN_POINT('Ctrl Pts',(12.7565510084746,3.6599103593549,1.44462438391895));
#80434=CARTESIAN_POINT('Ctrl Pts',(12.7624098185946,3.61575229957747,1.55185961947675));
#80435=CARTESIAN_POINT('Ctrl Pts',(12.7682686287146,3.56690211176297,1.65701488378979));
#80436=CARTESIAN_POINT('Ctrl Pts',(12.7743544175956,3.51615939715971,1.76624401482874));
#80437=CARTESIAN_POINT('Ctrl Pts',(12.7804402064765,3.46035375797207,1.87322831366523));
#80438=CARTESIAN_POINT('Ctrl Pts',(12.7865259953575,3.3997192012342,1.97747271858791));
#80439=CARTESIAN_POINT('Ctrl Pts',(12.7923780254358,3.3414136542045,2.07771303336549));
#80440=CARTESIAN_POINT('Ctrl Pts',(12.798230055514,3.27864353701332,2.17541966321022));
#80441=CARTESIAN_POINT('Ctrl Pts',(12.8040820855923,3.21166411568012,2.27017677903124));
#80442=CARTESIAN_POINT('Ctrl Pts',(12.8099332259708,3.14469487740713,2.36491948867501));
#80443=CARTESIAN_POINT('Ctrl Pts',(12.8157843663493,3.07351784595457,2.45671323845246));
#80444=CARTESIAN_POINT('Ctrl Pts',(12.8216355067278,2.99843128593945,2.54517166876804));
#80445=CARTESIAN_POINT('Ctrl Pts',(12.8274871742953,2.92333796060942,2.63363806920687));
#80446=CARTESIAN_POINT('Ctrl Pts',(12.8333388418628,2.84433467399043,2.71876823763874));
#80447=CARTESIAN_POINT('Ctrl Pts',(12.8391905094303,2.76175912345691,2.80020991070357));
#80448=CARTESIAN_POINT('Ctrl Pts',(12.8450441211145,2.67915613860523,2.88167864137512));
#80449=CARTESIAN_POINT('Ctrl Pts',(12.8508977327988,2.5929788240577,2.95945614986129));
#80450=CARTESIAN_POINT('Ctrl Pts',(12.856751344483,2.50360023599489,3.03322845468757));
#80451=CARTESIAN_POINT('Ctrl Pts',(12.8626116105829,2.41412004189673,3.10708462424671));
#80452=CARTESIAN_POINT('Ctrl Pts',(12.8684718766828,2.32143162949325,3.17692623895583));
#80453=CARTESIAN_POINT('Ctrl Pts',(12.8743321427826,2.22593957581017,3.24248084109098));
#80454=CARTESIAN_POINT('Ctrl Pts',(12.8801963559539,2.13038320526011,3.30807959628874));
#80455=CARTESIAN_POINT('Ctrl Pts',(12.8860605691252,2.03201978330911,3.36938537134209));
#80456=CARTESIAN_POINT('Ctrl Pts',(12.8919247822965,1.93127966843302,3.4261710176664));
#80457=CARTESIAN_POINT('Ctrl Pts',(12.8977976308708,1.83039120774077,3.48304028423534));
#80458=CARTESIAN_POINT('Ctrl Pts',(12.9036704794451,1.72711943650159,3.53537595155666));
#80459=CARTESIAN_POINT('Ctrl Pts',(12.9095433280194,1.62191597340105,3.5829984056969));
#80460=CARTESIAN_POINT('Ctrl Pts',(12.9111380726322,1.59334846414105,3.59593006079208));
#80461=CARTESIAN_POINT('Ctrl Pts',(12.912732817245,1.56463860934895,3.60851446087554));
#80462=CARTESIAN_POINT('Ctrl Pts',(12.9143275618578,1.53579563904659,3.62074864566507));
#80463=CARTESIAN_POINT('Ctrl Pts',(12.9202000079918,1.42958503448824,3.66579948991424));
#80464=CARTESIAN_POINT('Ctrl Pts',(12.9260724541257,1.32121265514115,3.70624844362442));
#80465=CARTESIAN_POINT('Ctrl Pts',(12.9319449002596,1.21111466909181,3.7418832502245));
#80466=CARTESIAN_POINT('Ctrl Pts',(12.9378097392044,1.10115930439256,3.7774718953605));
#80467=CARTESIAN_POINT('Ctrl Pts',(12.9436745781493,0.989483167967315,3.80825866898438));
#80468=CARTESIAN_POINT('Ctrl Pts',(12.9495394170941,0.87654358351824,3.83407881324745));
#80469=CARTESIAN_POINT('Ctrl Pts',(12.9553982272142,0.763720096540402,3.85987241541308));
#80470=CARTESIAN_POINT('Ctrl Pts',(12.9612570373342,0.649636145414761,3.88070945176689));
#80471=CARTESIAN_POINT('Ctrl Pts',(12.9671158474542,0.53476480296806,3.89647476644037));
#80472=CARTESIAN_POINT('Ctrl Pts',(12.9732016363352,0.41544317890391,3.91285085216074));
#80473=CARTESIAN_POINT('Ctrl Pts',(12.9792874252162,0.295272352536118,3.92375415683198));
#80474=CARTESIAN_POINT('Ctrl Pts',(12.9853732140971,0.174795304188719,3.92911384432082));
#80475=CARTESIAN_POINT('Ctrl Pts',(12.9912252441754,0.058945851560767,3.93426766299713));
#80476=CARTESIAN_POINT('Ctrl Pts',(12.9970772742537,-0.0571862815160144,
3.9342958560697));
#80477=CARTESIAN_POINT('Ctrl Pts',(13.0029293043319,-0.1731132709532,3.92918831254241));
#80478=CARTESIAN_POINT('Ctrl Pts',(13.0087804447104,-0.289022635700781,
3.9240815455286));
#80479=CARTESIAN_POINT('Ctrl Pts',(13.014631585089,-0.404726505978026,3.91384061258856));
#80480=CARTESIAN_POINT('Ctrl Pts',(13.0204827254675,-0.519738597916684,
3.89850750798759));
#80481=CARTESIAN_POINT('Ctrl Pts',(13.026334393035,-0.634761052469176,3.88317302187064));
#80482=CARTESIAN_POINT('Ctrl Pts',(13.0321860606025,-0.749091195021596,
3.86274550665698));
#80483=CARTESIAN_POINT('Ctrl Pts',(13.03803772817,-0.862250102067256,3.83731856398254));
#80484=CARTESIAN_POINT('Ctrl Pts',(13.0438913398542,-0.975446604229726,
3.81188317364008));
#80485=CARTESIAN_POINT('Ctrl Pts',(13.0497449515385,-1.08747069405064,3.7814451436646));
#80486=CARTESIAN_POINT('Ctrl Pts',(13.0555985632227,-1.19785653221811,3.74614851924245));
#80487=CARTESIAN_POINT('Ctrl Pts',(13.0614588293226,-1.30836785756999,3.71081176943746));
#80488=CARTESIAN_POINT('Ctrl Pts',(13.0673190954225,-1.41723682008301,3.67060552688228));
#80489=CARTESIAN_POINT('Ctrl Pts',(13.0731793615224,-1.52401546695074,3.62572280469632));
#80490=CARTESIAN_POINT('Ctrl Pts',(13.0790435746937,-1.63086603255683,3.58080985260158));
#80491=CARTESIAN_POINT('Ctrl Pts',(13.084907787865,-1.73562310643167,3.53121432552517));
#80492=CARTESIAN_POINT('Ctrl Pts',(13.0907720010363,-1.83786290992666,3.47717542328769));
#80493=CARTESIAN_POINT('Ctrl Pts',(13.0966448496106,-1.9402532676185,3.42305694554979));
#80494=CARTESIAN_POINT('Ctrl Pts',(13.1025176981849,-2.04011860162605,3.36448224220103));
#80495=CARTESIAN_POINT('Ctrl Pts',(13.1083905467592,-2.13706362425989,3.30173409981258));
#80496=CARTESIAN_POINT('Ctrl Pts',(13.109985291372,-2.16338859256551,3.28469513468848));
#80497=CARTESIAN_POINT('Ctrl Pts',(13.1115800359848,-2.18949841454651,3.26734866289345));
#80498=CARTESIAN_POINT('Ctrl Pts',(13.1131747805975,-2.2153856092198,3.24970084814923));
#80499=CARTESIAN_POINT('Ctrl Pts',(13.1190208234721,-2.31028334315751,3.18500717819714));
#80500=CARTESIAN_POINT('Ctrl Pts',(13.1248668663467,-2.40251085169915,3.1160400027466));
#80501=CARTESIAN_POINT('Ctrl Pts',(13.1307129092213,-2.4916558632707,3.04304782397989));
#80502=CARTESIAN_POINT('Ctrl Pts',(13.1365513636227,-2.58068515989634,2.9701503929267));
#80503=CARTESIAN_POINT('Ctrl Pts',(13.142389818024,-2.6666395950843,2.89323860850244));
#80504=CARTESIAN_POINT('Ctrl Pts',(13.1482282724254,-2.749135225128,2.81260457831534));
#80505=CARTESIAN_POINT('Ctrl Pts',(13.1540607468928,-2.83154636047867,2.73205313611047));
#80506=CARTESIAN_POINT('Ctrl Pts',(13.1598932213603,-2.9105054390927,2.64778731995767));
#80507=CARTESIAN_POINT('Ctrl Pts',(13.1657256958278,-2.98566159569659,2.56013941729401));
#80508=CARTESIAN_POINT('Ctrl Pts',(13.1715969784151,-3.06131782635182,2.47190832299632));
#80509=CARTESIAN_POINT('Ctrl Pts',(13.1774682610025,-3.13312000555237,2.38025023652073));
#80510=CARTESIAN_POINT('Ctrl Pts',(13.1833395435899,-3.20074780223883,2.28554205965747));
#80511=CARTESIAN_POINT('Ctrl Pts',(13.1891654831846,-3.26785332008022,2.1915652991593));
#80512=CARTESIAN_POINT('Ctrl Pts',(13.1949914227793,-3.33084846868497,2.09458574588242));
#80513=CARTESIAN_POINT('Ctrl Pts',(13.200817362374,-3.38946127116969,1.99500408301356));
#80514=CARTESIAN_POINT('Ctrl Pts',(13.2066424913309,-3.44806591810223,1.89543627622071));
#80515=CARTESIAN_POINT('Ctrl Pts',(13.2124676202878,-3.50228921951273,1.79326743942917));
#80516=CARTESIAN_POINT('Ctrl Pts',(13.2182927492447,-3.55190376447066,1.68892529377092));
#80517=CARTESIAN_POINT('Ctrl Pts',(13.2241185112485,-3.60152370129814,1.58457180871131));
#80518=CARTESIAN_POINT('Ctrl Pts',(13.2299442732523,-3.64653370711372,1.47804492253806));
#80519=CARTESIAN_POINT('Ctrl Pts',(13.2357700352561,-3.68675370574358,1.36979418643313));
#80520=CARTESIAN_POINT('Ctrl Pts',(13.2416755721452,-3.72752445563517,1.26006112234401));
#80521=CARTESIAN_POINT('Ctrl Pts',(13.2475811090342,-3.76337287285803,1.14855705555912));
#80522=CARTESIAN_POINT('Ctrl Pts',(13.2534866459232,-3.79416341890537,1.03576684183282));
#80523=CARTESIAN_POINT('Ctrl Pts',(13.2593211256594,-3.8245834840667,0.924333753058107));
#80524=CARTESIAN_POINT('Ctrl Pts',(13.2651556053955,-3.85006669718843,0.811645722880928));
#80525=CARTESIAN_POINT('Ctrl Pts',(13.2709900851316,-3.87053400840513,0.69818012702979));
#80526=CARTESIAN_POINT('Ctrl Pts',(13.2769311505971,-3.89137522156222,0.58264171340562));
#80527=CARTESIAN_POINT('Ctrl Pts',(13.2828722160626,-3.90701541620972,0.466297498712091));
#80528=CARTESIAN_POINT('Ctrl Pts',(13.2888132815281,-3.917426483295,0.349655184401622));
#80529=CARTESIAN_POINT('Ctrl Pts',(13.2947543469936,-3.92783755038029,0.233012870091152));
#80530=CARTESIAN_POINT('Ctrl Pts',(13.3006954124591,-3.9330195358347,0.116072908435258));
#80531=CARTESIAN_POINT('Ctrl Pts',(13.3066364779246,-3.93299994461018,-0.000660072963477499));
#80532=CARTESIAN_POINT('',(14.5566364620208,-3.93299834093028,0.00361251154098325));
#80533=CARTESIAN_POINT('Ctrl Pts',(13.3066364779651,-3.93299994461005,-0.0006600737587242));
#80534=CARTESIAN_POINT('Ctrl Pts',(13.3084316517558,-3.93299402484778,-0.0359325328708672));
#80535=CARTESIAN_POINT('Ctrl Pts',(13.3102268255465,-3.93251361331012,-0.0712005153535426));
#80536=CARTESIAN_POINT('Ctrl Pts',(13.3120219993372,-3.93155900442503,-0.106455599779701));
#80537=CARTESIAN_POINT('Ctrl Pts',(13.3178944454711,-3.92843624868645,-0.221783477956529));
#80538=CARTESIAN_POINT('Ctrl Pts',(13.3237668916051,-3.92022944147405,-0.337166920342933));
#80539=CARTESIAN_POINT('Ctrl Pts',(13.329639337739,-3.90692661815479,-0.45212100189397));
#80540=CARTESIAN_POINT('Ctrl Pts',(13.3355041766838,-3.89364102736347,-0.566926171490323));
#80541=CARTESIAN_POINT('Ctrl Pts',(13.3413690156287,-3.87527259537927,-0.681302679495434));
#80542=CARTESIAN_POINT('Ctrl Pts',(13.3472338545736,-3.851861352367,-0.794766080140218));
#80543=CARTESIAN_POINT('Ctrl Pts',(13.3530926646936,-3.82847417519594,-0.908112844851515));
#80544=CARTESIAN_POINT('Ctrl Pts',(13.3589514748136,-3.80005458091169,-1.02054796680724));
#80545=CARTESIAN_POINT('Ctrl Pts',(13.3648102849337,-3.76669426268574,-1.13159327121115));
#80546=CARTESIAN_POINT('Ctrl Pts',(13.3708960738146,-3.73204151757779,-1.24694063099592));
#80547=CARTESIAN_POINT('Ctrl Pts',(13.3769818626956,-3.69205753667132,-1.36078785684508));
#80548=CARTESIAN_POINT('Ctrl Pts',(13.3830676515766,-3.64690336095326,-1.47261158350319));
#80549=CARTESIAN_POINT('Ctrl Pts',(13.3889196816548,-3.60348358421941,-1.58014009372028));
#80550=CARTESIAN_POINT('Ctrl Pts',(13.3947717117331,-3.55528363581229,-1.68579726622336));
#80551=CARTESIAN_POINT('Ctrl Pts',(13.4006237418113,-3.50249689396205,-1.78913512843112));
#80552=CARTESIAN_POINT('Ctrl Pts',(13.4064748821899,-3.44971817742105,-1.89245727990787));
#80553=CARTESIAN_POINT('Ctrl Pts',(13.4123260225684,-3.39235424196728,-1.99346045418398));
#80554=CARTESIAN_POINT('Ctrl Pts',(13.4181771629469,-3.33064522641628,-2.09171971730211));
#80555=CARTESIAN_POINT('Ctrl Pts',(13.4240288305143,-3.26893065086997,-2.18998783360057));
#80556=CARTESIAN_POINT('Ctrl Pts',(13.4298804980818,-3.20287043682752,-2.28551119720595));
#80557=CARTESIAN_POINT('Ctrl Pts',(13.4357321656493,-3.13274861385817,-2.37789300061414));
#80558=CARTESIAN_POINT('Ctrl Pts',(13.4415857773335,-3.06260349410916,-2.47030549630081));
#80559=CARTESIAN_POINT('Ctrl Pts',(13.4474393890177,-2.98839433201654,-2.55957402732073));
#80560=CARTESIAN_POINT('Ctrl Pts',(13.453293000702,-2.91044561226842,-2.6453346363036));
#80561=CARTESIAN_POINT('Ctrl Pts',(13.4591532668018,-2.83240828001768,-2.73119273838465));
#80562=CARTESIAN_POINT('Ctrl Pts',(13.4650135329017,-2.75062318314964,-2.8135346527984));
#80563=CARTESIAN_POINT('Ctrl Pts',(13.4708737990016,-2.66545192487042,-2.89203302820085));
#80564=CARTESIAN_POINT('Ctrl Pts',(13.4767380121729,-2.58022330110081,-2.97058427469961));
#80565=CARTESIAN_POINT('Ctrl Pts',(13.4826022253441,-2.49160428989289,-3.04528656171485));
#80566=CARTESIAN_POINT('Ctrl Pts',(13.4884664385154,-2.39998847184148,-3.11585370886183));
#80567=CARTESIAN_POINT('Ctrl Pts',(13.4943392870897,-2.30823774404417,-3.18652477033379));
#80568=CARTESIAN_POINT('Ctrl Pts',(13.500212135664,-2.21348173901715,-3.2530483024118));
#80569=CARTESIAN_POINT('Ctrl Pts',(13.5060849842382,-2.11614185695144,-3.3151821429988));
#80570=CARTESIAN_POINT('Ctrl Pts',(13.5076797288511,-2.08970966640956,-3.3320542973372));
#80571=CARTESIAN_POINT('Ctrl Pts',(13.5092744734639,-2.06308707959257,-3.34860303622743));
#80572=CARTESIAN_POINT('Ctrl Pts',(13.5108692180768,-2.03628281023104,-3.36482411379221));
#80573=CARTESIAN_POINT('Ctrl Pts',(13.5167416642107,-1.93757946505785,-3.42455618842418));
#80574=CARTESIAN_POINT('Ctrl Pts',(13.5226141103446,-1.83608038008772,-3.48004155777348));
#80575=CARTESIAN_POINT('Ctrl Pts',(13.5284865564785,-1.73218700919155,-3.53100795314709));
#80576=CARTESIAN_POINT('Ctrl Pts',(13.5343513954233,-1.6284282221635,-3.58190832645814));
#80577=CARTESIAN_POINT('Ctrl Pts',(13.5402162343682,-1.52228168480992,-3.62830118673706));
#80578=CARTESIAN_POINT('Ctrl Pts',(13.546081073313,-1.41417656195017,-3.66995826292763));
#80579=CARTESIAN_POINT('Ctrl Pts',(13.551939883433,-1.3061825669243,-3.7115725172748));
#80580=CARTESIAN_POINT('Ctrl Pts',(13.5577986935531,-1.19623437444989,-3.74846052291427));
#80581=CARTESIAN_POINT('Ctrl Pts',(13.5636575036731,-1.08478380886473,-3.78044085895083));
#80582=CARTESIAN_POINT('Ctrl Pts',(13.569743292554,-0.969015487495461,-3.81366015936748));
#80583=CARTESIAN_POINT('Ctrl Pts',(13.575829081435,-0.851626438381354,-3.84158363892788));
#80584=CARTESIAN_POINT('Ctrl Pts',(13.581914870316,-0.733143997551199,-3.86406377779335));
#80585=CARTESIAN_POINT('Ctrl Pts',(13.5877669003943,-0.619212538368887,
-3.88568044103577));
#80586=CARTESIAN_POINT('Ctrl Pts',(13.5936189304725,-0.504270577384078,
-3.90226412979255));
#80587=CARTESIAN_POINT('Ctrl Pts',(13.5994709605508,-0.388799514714528,
-3.91373529219309));
#80588=CARTESIAN_POINT('Ctrl Pts',(13.6053221009293,-0.273346007418829,
-3.9252047106022));
#80589=CARTESIAN_POINT('Ctrl Pts',(13.6111732413078,-0.157363969600864,
-3.93156310727175));
#80590=CARTESIAN_POINT('Ctrl Pts',(13.6170243816864,-0.0413407050098623,
-3.93278272297228));
#80591=CARTESIAN_POINT('Ctrl Pts',(13.6228760492539,0.0746930133017308,
-3.93400244856045));
#80592=CARTESIAN_POINT('Ctrl Pts',(13.6287277168214,0.190767552411546,-3.93008246842282));
#80593=CARTESIAN_POINT('Ctrl Pts',(13.6345793843889,0.306395536613611,-3.92104715288445));
#80594=CARTESIAN_POINT('Ctrl Pts',(13.6404329960731,0.422061936241297,-3.9120088355166));
#80595=CARTESIAN_POINT('Ctrl Pts',(13.6462866077574,0.537281074073332,-3.89785183561486));
#80596=CARTESIAN_POINT('Ctrl Pts',(13.6521402194416,0.651571333732123,-3.87865231711461));
#80597=CARTESIAN_POINT('Ctrl Pts',(13.6580004855415,0.765991519141649,-3.8594309725037));
#80598=CARTESIAN_POINT('Ctrl Pts',(13.6638607516414,0.879480310844347,-3.83515573621396));
#80599=CARTESIAN_POINT('Ctrl Pts',(13.6697210177413,0.991566815415545,-3.80595378986223));
#80600=CARTESIAN_POINT('Ctrl Pts',(13.6755852309126,1.10372881373231,-3.77673217509175));
#80601=CARTESIAN_POINT('Ctrl Pts',(13.6814494440839,1.21448625022413,-3.74257736438277));
#80602=CARTESIAN_POINT('Ctrl Pts',(13.6873136572552,1.32338557434277,-3.70366570057578));
#80603=CARTESIAN_POINT('Ctrl Pts',(13.6931865058295,1.43244525919888,-3.66469673702744));
#80604=CARTESIAN_POINT('Ctrl Pts',(13.6990593544038,1.53964098952691,-3.62095709587331));
#80605=CARTESIAN_POINT('Ctrl Pts',(13.7049322029781,1.64454120101405,-3.57267032318506));
#80606=CARTESIAN_POINT('Ctrl Pts',(13.7065269475909,1.67302636371384,-3.55955827548971));
#80607=CARTESIAN_POINT('Ctrl Pts',(13.7081216922037,1.70134241567111,-3.54611119070619));
#80608=CARTESIAN_POINT('Ctrl Pts',(13.7097164368165,1.72948107361273,-3.53233410311303));
#80609=CARTESIAN_POINT('Ctrl Pts',(13.7155888829504,1.83309813663172,-3.48160171366076));
#80610=CARTESIAN_POINT('Ctrl Pts',(13.7214613290843,1.93465451844559,-3.42622128594048));
#80611=CARTESIAN_POINT('Ctrl Pts',(13.7273337752182,2.03370411398415,-3.36638330805687));
#80612=CARTESIAN_POINT('Ctrl Pts',(13.7331986141631,2.13262540029965,-3.30662284451758));
#80613=CARTESIAN_POINT('Ctrl Pts',(13.7390634531079,2.22904600752161,-3.2424165256699));
#80614=CARTESIAN_POINT('Ctrl Pts',(13.7449282920528,2.32254185819059,-3.1740019402881));
#80615=CARTESIAN_POINT('Ctrl Pts',(13.7507871021728,2.41594159878554,-3.10565768242157));
#80616=CARTESIAN_POINT('Ctrl Pts',(13.7566459122928,2.50642223140701,-3.03311400517208));
#80617=CARTESIAN_POINT('Ctrl Pts',(13.7625047224128,2.59358683713495,-2.95665289106454));
#80618=CARTESIAN_POINT('Ctrl Pts',(13.7685905112938,2.68412832550653,-2.8772295630287));
#80619=CARTESIAN_POINT('Ctrl Pts',(13.7746763001748,2.77109126625278,-2.79357935980456));
#80620=CARTESIAN_POINT('Ctrl Pts',(13.7807620890557,2.8540664283801,-2.70606611567302));
#80621=CARTESIAN_POINT('Ctrl Pts',(13.786614119134,2.93385446474073,-2.62191430776104));
#80622=CARTESIAN_POINT('Ctrl Pts',(13.7924661492123,3.00995510677078,-2.53419107588701));
#80623=CARTESIAN_POINT('Ctrl Pts',(13.7983181792905,3.08204113675473,-2.44325836361028));
#80624=CARTESIAN_POINT('Ctrl Pts',(13.804169319669,3.15411620730715,-2.3523394760765));
#80625=CARTESIAN_POINT('Ctrl Pts',(13.8100204600475,3.22217762267703,-2.25821240216862));
#80626=CARTESIAN_POINT('Ctrl Pts',(13.815871600426,3.28593854142631,-2.1612720564448));
#80627=CARTESIAN_POINT('Ctrl Pts',(13.8217232679935,3.34970520504785,-2.06432297637532));
#80628=CARTESIAN_POINT('Ctrl Pts',(13.827574935561,3.40917037462039,-1.96456046597406));
#80629=CARTESIAN_POINT('Ctrl Pts',(13.8334266031285,3.46409102164404,-1.8624076873137));
#80630=CARTESIAN_POINT('Ctrl Pts',(13.8392802148128,3.51902991511588,-1.76022097013505));
#80631=CARTESIAN_POINT('Ctrl Pts',(13.845133826497,3.56942108817908,-1.65564276950856));
#80632=CARTESIAN_POINT('Ctrl Pts',(13.8509874381812,3.61506819570829,-1.54911940804395));
#80633=CARTESIAN_POINT('Ctrl Pts',(13.8568477042811,3.66076719510241,-1.4424749502781));
#80634=CARTESIAN_POINT('Ctrl Pts',(13.862707970381,3.70171120165123,-1.33388129822243));
#80635=CARTESIAN_POINT('Ctrl Pts',(13.8685682364809,3.73775258476823,-1.22380334002585));
#80636=CARTESIAN_POINT('Ctrl Pts',(13.8744324496522,3.77381824287729,-1.11365124090209));
#80637=CARTESIAN_POINT('Ctrl Pts',(13.8802966628235,3.80497459162737,-1.00201324214997));
#80638=CARTESIAN_POINT('Ctrl Pts',(13.8861608759948,3.83112473276239,-0.889366224913153));
#80639=CARTESIAN_POINT('Ctrl Pts',(13.8920337245691,3.85731338153694,-0.776553328237669));
#80640=CARTESIAN_POINT('Ctrl Pts',(13.8979065731434,3.87848103448428,-0.662728852497358));
#80641=CARTESIAN_POINT('Ctrl Pts',(13.9037794217177,3.89458238930981,-0.548376707089073));
#80642=CARTESIAN_POINT('Ctrl Pts',(13.9053741663305,3.89895463704307,-0.517324915859616));
#80643=CARTESIAN_POINT('Ctrl Pts',(13.9069689109433,3.90295360868116,-0.486234224110163));
#80644=CARTESIAN_POINT('Ctrl Pts',(13.908563655556,3.90657906025345,-0.455114321889844));
#80645=CARTESIAN_POINT('Ctrl Pts',(13.91443610169,3.91992932894139,-0.340519202385656));
#80646=CARTESIAN_POINT('Ctrl Pts',(13.9203085478239,3.92825539497768,-0.225144304396692));
#80647=CARTESIAN_POINT('Ctrl Pts',(13.9261809939578,3.93147628507484,-0.109467894353272));
#80648=CARTESIAN_POINT('Ctrl Pts',(13.9320458329026,3.9346930028187,0.0060586680283022));
#80649=CARTESIAN_POINT('Ctrl Pts',(13.9379106718475,3.93281768465536,0.121885556352266));
#80650=CARTESIAN_POINT('Ctrl Pts',(13.9437755107923,3.92582088935509,0.237527566196477));
#80651=CARTESIAN_POINT('Ctrl Pts',(13.9496343209124,3.91883128648645,0.353050700582037));
#80652=CARTESIAN_POINT('Ctrl Pts',(13.9554931310324,3.90673070302807,0.468388924378064));
#80653=CARTESIAN_POINT('Ctrl Pts',(13.9613519411524,3.88954172706935,0.583055875012324));
#80654=CARTESIAN_POINT('Ctrl Pts',(13.9674377300334,3.87168682537056,0.70216518883016));
#80655=CARTESIAN_POINT('Ctrl Pts',(13.9735235189143,3.84834128124193,0.820549711180056));
#80656=CARTESIAN_POINT('Ctrl Pts',(13.9796093077953,3.81958987993541,0.937668464381209));
#80657=CARTESIAN_POINT('Ctrl Pts',(13.9854613378736,3.79194283720538,1.05028861599465));
#80658=CARTESIAN_POINT('Ctrl Pts',(13.9913133679519,3.7592976689318,1.16173800413208));
#80659=CARTESIAN_POINT('Ctrl Pts',(13.9971653980301,3.72178191529397,1.27154566374581));
#80660=CARTESIAN_POINT('Ctrl Pts',(14.0030165384086,3.6842718652763,1.38133662900793));
#80661=CARTESIAN_POINT('Ctrl Pts',(14.0088676787872,3.64189283582871,1.48948597097399));
#80662=CARTESIAN_POINT('Ctrl Pts',(14.0147188191657,3.59482193449524,1.59553886172413));
#80663=CARTESIAN_POINT('Ctrl Pts',(14.0205704867332,3.5477467920636,1.70160130786216));
#80664=CARTESIAN_POINT('Ctrl Pts',(14.0264221543007,3.49597910508139,1.80556654944974));
#80665=CARTESIAN_POINT('Ctrl Pts',(14.0322738218682,3.43974343325799,1.90700134068085));
#80666=CARTESIAN_POINT('Ctrl Pts',(14.0381274335524,3.38348907809181,2.00846983189121));
#80667=CARTESIAN_POINT('Ctrl Pts',(14.0439810452367,3.32276398674131,2.10740583974196));
#80668=CARTESIAN_POINT('Ctrl Pts',(14.0498346569209,3.25783744394467,2.20340286575833));
#80669=CARTESIAN_POINT('Ctrl Pts',(14.0556949230208,3.19283709232267,2.29950902168405));
#80670=CARTESIAN_POINT('Ctrl Pts',(14.0615551891207,3.12362598776988,2.39266918455233));
#80671=CARTESIAN_POINT('Ctrl Pts',(14.0674154552206,3.05051537297152,2.48250779641563));
#80672=CARTESIAN_POINT('Ctrl Pts',(14.0732796683919,2.97735551590106,2.57240691737713));
#80673=CARTESIAN_POINT('Ctrl Pts',(14.0791438815632,2.90029119297989,2.65897972468709));
#80674=CARTESIAN_POINT('Ctrl Pts',(14.0850080947345,2.81967116699783,2.74188685215147));
#80675=CARTESIAN_POINT('Ctrl Pts',(14.0908809433088,2.73893242322828,2.82491606529642));
#80676=CARTESIAN_POINT('Ctrl Pts',(14.0967537918831,2.65462782627727,2.9042685431518));
#80677=CARTESIAN_POINT('Ctrl Pts',(14.1026266404574,2.56713994962853,2.97964452225785));
#80678=CARTESIAN_POINT('Ctrl Pts',(14.1042213850702,2.54338302516427,3.00011251748914));
#80679=CARTESIAN_POINT('Ctrl Pts',(14.105816129683,2.51939154302913,3.02028754345122));
#80680=CARTESIAN_POINT('Ctrl Pts',(14.1074108742958,2.49517352266139,3.04016415540503));
#80681=CARTESIAN_POINT('Ctrl Pts',(14.1132833204297,2.4059937135938,3.11335727491005));
#80682=CARTESIAN_POINT('Ctrl Pts',(14.1191557665636,2.3134413100962,3.18274562456913));
#80683=CARTESIAN_POINT('Ctrl Pts',(14.1250282126975,2.21787485106744,3.24800248537506));
#80684=CARTESIAN_POINT('Ctrl Pts',(14.1308930516423,2.12243218919344,3.31317481219513));
#80685=CARTESIAN_POINT('Ctrl Pts',(14.1367578905872,2.02398357450615,3.37422606233112));
#80686=CARTESIAN_POINT('Ctrl Pts',(14.142622729532,1.92292124611626,3.43086911455897));
#80687=CARTESIAN_POINT('Ctrl Pts',(14.148481539652,1.82196280584332,3.48745393994674));
#80688=CARTESIAN_POINT('Ctrl Pts',(14.1543403497721,1.71839635446936,3.53963937985336));
#80689=CARTESIAN_POINT('Ctrl Pts',(14.1601991598921,1.61264323813689,3.58718145435819));
#80690=CARTESIAN_POINT('Ctrl Pts',(14.166284948773,1.50279309342829,3.63656537745399));
#80691=CARTESIAN_POINT('Ctrl Pts',(14.172370737654,1.3905838031818,3.68093862102548));
#80692=CARTESIAN_POINT('Ctrl Pts',(14.178456526535,1.2765162868987,3.72007999501118));
#80693=CARTESIAN_POINT('Ctrl Pts',(14.1843085566132,1.16683017236244,3.75771792533524));
#80694=CARTESIAN_POINT('Ctrl Pts',(14.1901605866915,1.05542637684033,3.79051834409894));
#80695=CARTESIAN_POINT('Ctrl Pts',(14.1960126167698,0.942770042609576,3.81833388361441));
#80696=CARTESIAN_POINT('Ctrl Pts',(14.2018637571483,0.830130835822037,3.84614519425917));
#80697=CARTESIAN_POINT('Ctrl Pts',(14.2077148975268,0.716239870152568,3.86897303347964));
#80698=CARTESIAN_POINT('Ctrl Pts',(14.2135660379053,0.601575514764253,3.88672045560729));
#80699=CARTESIAN_POINT('Ctrl Pts',(14.2194177054728,0.486900828093242,3.90446947678143));
#80700=CARTESIAN_POINT('Ctrl Pts',(14.2252693730403,0.371453021698423,3.91713710767553));
#80701=CARTESIAN_POINT('Ctrl Pts',(14.2311210406078,0.255717967548004,3.92467798947546));
#80702=CARTESIAN_POINT('Ctrl Pts',(14.236974652292,0.139944462400024,3.93222137660473));
#80703=CARTESIAN_POINT('Ctrl Pts',(14.2428282639762,0.0238839319974031,
3.93463460091986));
#80704=CARTESIAN_POINT('Ctrl Pts',(14.2486818756605,-0.0919760685040969,
3.93192438925554));
#80705=CARTESIAN_POINT('Ctrl Pts',(14.2545421417604,-0.207967779245849,
3.92921109660875));
#80706=CARTESIAN_POINT('Ctrl Pts',(14.2604024078602,-0.323758091591143,
3.9213627524506));
#80707=CARTESIAN_POINT('Ctrl Pts',(14.2662626739601,-0.438862790739952,
3.90843810887469));
#80708=CARTESIAN_POINT('Ctrl Pts',(14.2721268871314,-0.554045016482335,
3.89550476014949));
#80709=CARTESIAN_POINT('Ctrl Pts',(14.2779911003027,-0.668540302193927,
3.87748836809554));
#80710=CARTESIAN_POINT('Ctrl Pts',(14.283855313474,-0.781874590395646,3.85449881630461));
#80711=CARTESIAN_POINT('Ctrl Pts',(14.2897281620483,-0.89537577008339,3.83147541103013));
#80712=CARTESIAN_POINT('Ctrl Pts',(14.2956010106226,-1.00771214059734,3.80346432985501));
#80713=CARTESIAN_POINT('Ctrl Pts',(14.3014738591969,-1.11842467684313,3.77062531183202));
#80714=CARTESIAN_POINT('Ctrl Pts',(14.3030686038097,-1.14848814919649,3.76170802979764));
#80715=CARTESIAN_POINT('Ctrl Pts',(14.3046633484225,-1.17843200092335,3.75243502427599));
#80716=CARTESIAN_POINT('Ctrl Pts',(14.3062580930353,-1.20824731566829,3.74281009726387));
#80717=CARTESIAN_POINT('Ctrl Pts',(14.3121305391693,-1.31803845614238,3.70736751607094));
#80718=CARTESIAN_POINT('Ctrl Pts',(14.3180029853032,-1.42645258664682,3.66703060036621));
#80719=CARTESIAN_POINT('Ctrl Pts',(14.3238754314371,-1.53302100258657,3.62192429595491));
#80720=CARTESIAN_POINT('Ctrl Pts',(14.3297402703819,-1.63945136939473,3.57687642242201));
#80721=CARTESIAN_POINT('Ctrl Pts',(14.3356051093268,-1.74404039922512,3.52707160622746));
#80722=CARTESIAN_POINT('Ctrl Pts',(14.3414699482716,-1.84633447544124,3.47268455302193));
#80723=CARTESIAN_POINT('Ctrl Pts',(14.3473287583917,-1.94852339735197,3.41835340757776));
#80724=CARTESIAN_POINT('Ctrl Pts',(14.3531875685117,-2.04842169528549,3.35944958717139));
#80725=CARTESIAN_POINT('Ctrl Pts',(14.3590463786317,-2.14559630498422,3.29619560949256));
#80726=CARTESIAN_POINT('Ctrl Pts',(14.3651321675127,-2.24653559932926,3.23049108141458));
#80727=CARTESIAN_POINT('Ctrl Pts',(14.3712179563937,-2.34453547954069,3.16009269335622));
#80728=CARTESIAN_POINT('Ctrl Pts',(14.3773037452746,-2.43913902626371,3.08530222353618));
#80729=CARTESIAN_POINT('Ctrl Pts',(14.3831557753529,-2.53010879399015,3.01338450054002));
#80730=CARTESIAN_POINT('Ctrl Pts',(14.3890078054312,-2.61793797156652,2.93740615695396));
#80731=CARTESIAN_POINT('Ctrl Pts',(14.3948598355095,-2.70225108478815,2.85767879139018));
#80732=CARTESIAN_POINT('Ctrl Pts',(14.400710975888,-2.7865513796621,2.77796354699063));
#80733=CARTESIAN_POINT('Ctrl Pts',(14.4065621162665,-2.86733637279507,2.69450069783535));
#80734=CARTESIAN_POINT('Ctrl Pts',(14.412413256645,-2.94426585352191,2.60764023281297));
#80735=CARTESIAN_POINT('Ctrl Pts',(14.4182649242125,-3.02120226561124,2.52077194164431));
#80736=CARTESIAN_POINT('Ctrl Pts',(14.42411659178,-3.09428220065159,2.43050573551848));
#80737=CARTESIAN_POINT('Ctrl Pts',(14.4299682593475,-3.16320478645603,2.33722580829103));
#80738=CARTESIAN_POINT('Ctrl Pts',(14.4358218710318,-3.23215027061418,2.24391489039856));
#80739=CARTESIAN_POINT('Ctrl Pts',(14.441675482716,-3.29693541357618,2.14758859274089));
#80740=CARTESIAN_POINT('Ctrl Pts',(14.4475290944003,-3.35730224795042,2.04866068832958));
#80741=CARTESIAN_POINT('Ctrl Pts',(14.4533893605002,-3.41773770765006,1.94962032217166));
#80742=CARTESIAN_POINT('Ctrl Pts',(14.4592496266001,-3.47374461806866,1.8479727992091));
#80743=CARTESIAN_POINT('Ctrl Pts',(14.4651098927,-3.52511058209074,1.74415721310663));
#80744=CARTESIAN_POINT('Ctrl Pts',(14.4709741058713,-3.57651114268652,1.64027170397937));
#80745=CARTESIAN_POINT('Ctrl Pts',(14.4768383190426,-3.62326436641486,1.53421560135532));
#80746=CARTESIAN_POINT('Ctrl Pts',(14.4827025322139,-3.66520636059976,1.42644710179489));
#80747=CARTESIAN_POINT('Ctrl Pts',(14.4885753807881,-3.70721011686793,1.31851990670335));
#80748=CARTESIAN_POINT('Ctrl Pts',(14.4944482293624,-3.74438837146067,1.20887567204276));
#80749=CARTESIAN_POINT('Ctrl Pts',(14.5003210779367,-3.77662729872452,1.09798690635577));
#80750=CARTESIAN_POINT('Ctrl Pts',(14.5019158225495,-3.78538162891455,1.06787557972124));
#80751=CARTESIAN_POINT('Ctrl Pts',(14.5035105671623,-3.79377204123858,1.03767253569214));
#80752=CARTESIAN_POINT('Ctrl Pts',(14.505105311775,-3.80179691280552,1.00738733056476));
#80753=CARTESIAN_POINT('Ctrl Pts',(14.5126879630412,-3.83995336874241,0.863388004800826));
#80754=CARTESIAN_POINT('Ctrl Pts',(14.5202706143073,-3.869945230132,0.717141104295974));
#80755=CARTESIAN_POINT('Ctrl Pts',(14.5278532655734,-3.89155635414203,0.569454249731109));
#80756=CARTESIAN_POINT('Ctrl Pts',(14.5352847910977,-3.91273675846922,0.424710862388383));
#80757=CARTESIAN_POINT('Ctrl Pts',(14.5427163166219,-3.92586718729728,0.278584130433398));
#80758=CARTESIAN_POINT('Ctrl Pts',(14.5501478421462,-3.93078909684648,0.131856270661835));
#80759=CARTESIAN_POINT('Ctrl Pts',(14.5523107154377,-3.93222157079446,0.0891525528335636));
#80760=CARTESIAN_POINT('Ctrl Pts',(14.5544735887293,-3.93295904182085,0.0463980723529652));
#80761=CARTESIAN_POINT('Ctrl Pts',(14.5566364620208,-3.93299834093028,0.00361251154098325));
#80762=CARTESIAN_POINT('',(15.8066365080151,-3.93062432271256,-0.000977886178903984));
#80763=CARTESIAN_POINT('Ctrl Pts',(14.5566364779651,-3.93196599139969,0.00361124798914868));
#80764=CARTESIAN_POINT('Ctrl Pts',(14.605741828815,-3.9232411870099,-0.967535612376183));
#80765=CARTESIAN_POINT('Ctrl Pts',(14.7211295859113,-3.06929600653939,-3.26324377639959));
#80766=CARTESIAN_POINT('Ctrl Pts',(14.9027997492544,0.783357859407177,-4.58523082680123));
#80767=CARTESIAN_POINT('Ctrl Pts',(15.1016469679939,4.28070666041439,-1.82031364287207));
#80768=CARTESIAN_POINT('Ctrl Pts',(15.3004941867337,3.84588598521871,2.6167063762759));
#80769=CARTESIAN_POINT('Ctrl Pts',(15.4993414054732,-0.121686798380474,
4.65007350415478));
#80770=CARTESIAN_POINT('Ctrl Pts',(15.6680555025504,-3.39317719519555,2.75113718683392));
#80771=CARTESIAN_POINT('Ctrl Pts',(15.770487193381,-3.92513071241371,0.716349405360537));
#80772=CARTESIAN_POINT('Ctrl Pts',(15.8066364779651,-3.92671809469238,-0.000976317707402457));
#80773=CARTESIAN_POINT('',(17.0566364779651,-3.93351353754304,-0.00325536527871665));
#80774=CARTESIAN_POINT('Ctrl Pts',(15.8066365262899,-3.93299987819377,-0.000978840037985765));
#80775=CARTESIAN_POINT('Ctrl Pts',(15.8128950481088,-3.93296892038583,-0.125367964021516));
#80776=CARTESIAN_POINT('Ctrl Pts',(15.8191535699278,-3.92703264506812,-0.249598067531602));
#80777=CARTESIAN_POINT('Ctrl Pts',(15.8254120917467,-3.91526147166832,-0.37311741914522));
#80778=CARTESIAN_POINT('Ctrl Pts',(15.8316932505353,-3.90344772212963,-0.497083538204289));
#80779=CARTESIAN_POINT('Ctrl Pts',(15.8379744093238,-3.88575687475537,-0.620333443228178));
#80780=CARTESIAN_POINT('Ctrl Pts',(15.8442555681124,-3.86231098173614,-0.742322625520993));
#80781=CARTESIAN_POINT('Ctrl Pts',(15.8505482106162,-3.83882222306597,-0.864534838163019));
#80782=CARTESIAN_POINT('Ctrl Pts',(15.8568408531201,-3.80955748416183,-0.985481417500003));
#80783=CARTESIAN_POINT('Ctrl Pts',(15.8631334956239,-3.77468881186758,-1.10463268716877));
#80784=CARTESIAN_POINT('Ctrl Pts',(15.8694454887733,-3.7397129141401,-1.22415036156907));
#80785=CARTESIAN_POINT('Ctrl Pts',(15.8757574819227,-3.69909870924959,-1.34186137941075));
#80786=CARTESIAN_POINT('Ctrl Pts',(15.8820694750721,-3.65306737819782,-1.45725348870637));
#80787=CARTESIAN_POINT('Ctrl Pts',(15.8870582643656,-3.61668574626613,-1.5484555711205));
#80788=CARTESIAN_POINT('Ctrl Pts',(15.8920470536591,-3.57692111262724,-1.63820947314562));
#80789=CARTESIAN_POINT('Ctrl Pts',(15.8970358429526,-3.5339026077732,-1.72627383655484));
#80790=CARTESIAN_POINT('Ctrl Pts',(15.9029082890865,-3.48326429902636,-1.82993690990061));
#80791=CARTESIAN_POINT('Ctrl Pts',(15.9087807352204,-3.42797608331511,-1.93154352221046));
#80792=CARTESIAN_POINT('Ctrl Pts',(15.9146531813543,-3.36822804370767,-2.03064739567982));
#80793=CARTESIAN_POINT('Ctrl Pts',(15.9205180202992,-3.30855740193817,-2.12962288961424));
#80794=CARTESIAN_POINT('Ctrl Pts',(15.926382859244,-3.24443863666649,-2.22610174127127));
#80795=CARTESIAN_POINT('Ctrl Pts',(15.9322476981889,-3.17610895160689,-2.31965965769174));
#80796=CARTESIAN_POINT('Ctrl Pts',(15.9381065083089,-3.10784950678848,-2.41312140023685));
#80797=CARTESIAN_POINT('Ctrl Pts',(15.9439653184289,-3.03538799445726,-2.50366784809147));
#80798=CARTESIAN_POINT('Ctrl Pts',(15.9498241285489,-2.9590060367134,-2.59090182652559));
#80799=CARTESIAN_POINT('Ctrl Pts',(15.9559099174299,-2.87966493167289,-2.68151537520228));
#80800=CARTESIAN_POINT('Ctrl Pts',(15.9619957063108,-2.79609370471019,-2.76855421473168));
#80801=CARTESIAN_POINT('Ctrl Pts',(15.9680814951918,-2.70865581847126,-2.85160878401329));
#80802=CARTESIAN_POINT('Ctrl Pts',(15.9739335252701,-2.62457647390999,-2.9314731774518));
#80803=CARTESIAN_POINT('Ctrl Pts',(15.9797855553483,-2.53692235957565,-3.00765342008782));
#80804=CARTESIAN_POINT('Ctrl Pts',(15.9856375854266,-2.4460551218421,-3.07982196578147));
#80805=CARTESIAN_POINT('Ctrl Pts',(15.9914887258051,-2.35520169889724,-3.15197953949849));
#80806=CARTESIAN_POINT('Ctrl Pts',(15.9973398661836,-2.26113644744985,-3.22012637196162));
#80807=CARTESIAN_POINT('Ctrl Pts',(16.0031910065621,-2.16425402151115,-3.2839752633619));
#80808=CARTESIAN_POINT('Ctrl Pts',(16.0090426741296,-2.06736286644548,-3.34782990756073));
#80809=CARTESIAN_POINT('Ctrl Pts',(16.0148943416971,-1.96765437746729,-3.40738561341262));
#80810=CARTESIAN_POINT('Ctrl Pts',(16.0207460092646,-1.8655514958625,-3.46239896838669));
#80811=CARTESIAN_POINT('Ctrl Pts',(16.0265996209488,-1.76341469231684,-3.51743060060959));
#80812=CARTESIAN_POINT('Ctrl Pts',(16.0324532326331,-1.65888227805341,-3.56791668519934));
#80813=CARTESIAN_POINT('Ctrl Pts',(16.0383068443173,-1.55240039726309,-3.61366047195602));
#80814=CARTESIAN_POINT('Ctrl Pts',(16.0441671104172,-1.44579746732689,-3.6594562604831));
#80815=CARTESIAN_POINT('Ctrl Pts',(16.0500273765171,-1.33724102749432,-3.70049882753172));
#80816=CARTESIAN_POINT('Ctrl Pts',(16.055887642617,-1.2271958317091,-3.73664012056765));
#80817=CARTESIAN_POINT('Ctrl Pts',(16.0617518557883,-1.1170765170631,-3.77280575588811));
#80818=CARTESIAN_POINT('Ctrl Pts',(16.0676160689596,-1.00546684690839,-3.80406343271795));
#80819=CARTESIAN_POINT('Ctrl Pts',(16.0734802821309,-0.892843614231449,
-3.83031581994568));
#80820=CARTESIAN_POINT('Ctrl Pts',(16.0793531307052,-0.780054537140163,
-3.85660686537635));
#80821=CARTESIAN_POINT('Ctrl Pts',(16.0852259792795,-0.666249323523363,
-3.87787783532325));
#80822=CARTESIAN_POINT('Ctrl Pts',(16.0910988278538,-0.551911841454746,
-3.8940829882351));
#80823=CARTESIAN_POINT('Ctrl Pts',(16.0926935724666,-0.520864031986637,
-3.89848342185412));
#80824=CARTESIAN_POINT('Ctrl Pts',(16.0942883170793,-0.489776983168089,
-3.90251061484425));
#80825=CARTESIAN_POINT('Ctrl Pts',(16.0958830616921,-0.458660384822775,
-3.90616431443868));
#80826=CARTESIAN_POINT('Ctrl Pts',(16.1017555078261,-0.344077431422402,
-3.91961860290947));
#80827=CARTESIAN_POINT('Ctrl Pts',(16.10762795396,-0.228710139070021,-3.92804939865324));
#80828=CARTESIAN_POINT('Ctrl Pts',(16.1135004000939,-0.113036700494293,
-3.93137529426298));
#80829=CARTESIAN_POINT('Ctrl Pts',(16.1193652390387,0.00248689426889545,
-3.93469688149489));
#80830=CARTESIAN_POINT('Ctrl Pts',(16.1252300779836,0.11831543721581,-3.93292670754258));
#80831=CARTESIAN_POINT('Ctrl Pts',(16.1310949169284,0.233963750849901,-3.9260348907375));
#80832=CARTESIAN_POINT('Ctrl Pts',(16.1369537270484,0.349493182545274,-3.91915015845029));
#80833=CARTESIAN_POINT('Ctrl Pts',(16.1428125371685,0.464842343289673,-3.90715427982403));
#80834=CARTESIAN_POINT('Ctrl Pts',(16.1486713472885,0.579524850206603,-3.89006940143656));
#80835=CARTESIAN_POINT('Ctrl Pts',(16.1547571361695,0.698650322979956,-3.8723226301992));
#80836=CARTESIAN_POINT('Ctrl Pts',(16.1608429250504,0.817055988789581,-3.8490845608549));
#80837=CARTESIAN_POINT('Ctrl Pts',(16.1669287139314,0.934200793212602,-3.82043948754079));
#80838=CARTESIAN_POINT('Ctrl Pts',(16.1727807440097,1.04684599540481,-3.7928946886812));
#80839=CARTESIAN_POINT('Ctrl Pts',(16.1786327740879,1.15832497172005,-3.76035070356085));
#80840=CARTESIAN_POINT('Ctrl Pts',(16.1844848041662,1.26816664152833,-3.72293464478155));
#80841=CARTESIAN_POINT('Ctrl Pts',(16.1903359445447,1.37799161181431,-3.68552427446556));
#80842=CARTESIAN_POINT('Ctrl Pts',(16.1961870849232,1.48617937936311,-3.64324343651981));
#80843=CARTESIAN_POINT('Ctrl Pts',(16.2020382253018,1.59227495567051,-3.59626882553911));
#80844=CARTESIAN_POINT('Ctrl Pts',(16.2078898928693,1.69838009121176,-3.54928998213604));
#80845=CARTESIAN_POINT('Ctrl Pts',(16.2137415604367,1.80239228278799,-3.49761669234978));
#80846=CARTESIAN_POINT('Ctrl Pts',(16.2195932280042,1.90387808092456,-3.44147312251237));
#80847=CARTESIAN_POINT('Ctrl Pts',(16.2254468396885,2.00539759598659,-3.38531089993147));
#80848=CARTESIAN_POINT('Ctrl Pts',(16.2313004513727,2.10438868710423,-3.32467564411195));
#80849=CARTESIAN_POINT('Ctrl Pts',(16.237154063057,2.20044461152328,-3.25983627067651));
#80850=CARTESIAN_POINT('Ctrl Pts',(16.2430143291569,2.29660973280769,-3.19492318751027));
#80851=CARTESIAN_POINT('Ctrl Pts',(16.2488745952568,2.38983268461691,-3.12579667888275));
#80852=CARTESIAN_POINT('Ctrl Pts',(16.2547348613566,2.47973762662331,-3.05276764643308));
#80853=CARTESIAN_POINT('Ctrl Pts',(16.2605990745279,2.56970312240332,-2.97968942665957));
#80854=CARTESIAN_POINT('Ctrl Pts',(16.2664632876993,2.65634585023443,-2.90270372313745));
#80855=CARTESIAN_POINT('Ctrl Pts',(16.2723275008706,2.73932612746827,-2.82215899044857));
#80856=CARTESIAN_POINT('Ctrl Pts',(16.2782003494449,2.82242859810006,-2.74149565084606));
#80857=CARTESIAN_POINT('Ctrl Pts',(16.2840731980191,2.90185757190905,-2.65726312192466));
#80858=CARTESIAN_POINT('Ctrl Pts',(16.2899460465934,2.97731293827268,-2.5698437048961));
#80859=CARTESIAN_POINT('Ctrl Pts',(16.2915407912062,2.99780249074346,-2.54610537032173));
#80860=CARTESIAN_POINT('Ctrl Pts',(16.293135535819,3.01799928698865,-2.52213221222626));
#80861=CARTESIAN_POINT('Ctrl Pts',(16.2947302804318,3.03789787499169,-2.49793224510213));
#80862=CARTESIAN_POINT('Ctrl Pts',(16.3006027265658,3.11117191852845,-2.40881891483113));
#80863=CARTESIAN_POINT('Ctrl Pts',(16.3064751726997,3.18064425530551,-2.31632953768794));
#80864=CARTESIAN_POINT('Ctrl Pts',(16.3123476188336,3.2459878409817,-2.22082235584005));
#80865=CARTESIAN_POINT('Ctrl Pts',(16.3182124577784,3.3112467803283,-2.12543889435905));
#80866=CARTESIAN_POINT('Ctrl Pts',(16.3240772967233,3.37238737338344,-2.02704574033967));
#80867=CARTESIAN_POINT('Ctrl Pts',(16.3299421356681,3.42912214298098,-1.92603487209279));
#80868=CARTESIAN_POINT('Ctrl Pts',(16.3358009457881,3.48579859145661,-1.82512783906379));
#80869=CARTESIAN_POINT('Ctrl Pts',(16.3416597559082,3.53807802372136,-1.72160880240612));
#80870=CARTESIAN_POINT('Ctrl Pts',(16.3475185660282,3.58571607747243,-1.61589888661257));
#80871=CARTESIAN_POINT('Ctrl Pts',(16.3536043549092,3.63519969818896,-1.50609361609421));
#80872=CARTESIAN_POINT('Ctrl Pts',(16.3596901437901,3.67967478299223,-1.39392465249725));
#80873=CARTESIAN_POINT('Ctrl Pts',(16.3657759326711,3.71891968719538,-1.27989271432829));
#80874=CARTESIAN_POINT('Ctrl Pts',(16.3716279627494,3.75665717107912,-1.17024081132944));
#80875=CARTESIAN_POINT('Ctrl Pts',(16.3774799928276,3.78955870464399,-1.05886683673531));
#80876=CARTESIAN_POINT('Ctrl Pts',(16.3833320229059,3.8174764980236,-0.946235798856451));
#80877=CARTESIAN_POINT('Ctrl Pts',(16.3891831632844,3.84539004698656,-0.833621884574917));
#80878=CARTESIAN_POINT('Ctrl Pts',(16.3950343036629,3.86832126287971,-0.719751688113013));
#80879=CARTESIAN_POINT('Ctrl Pts',(16.4008854440414,3.88617276582833,-0.605103490432974));
#80880=CARTESIAN_POINT('Ctrl Pts',(16.4067371116089,3.90402587720114,-0.490444962926106));
#80881=CARTESIAN_POINT('Ctrl Pts',(16.4125887791764,3.91679830219751,-0.375008703312604));
#80882=CARTESIAN_POINT('Ctrl Pts',(16.4184404467439,3.92444424096509,-0.259280542185409));
#80883=CARTESIAN_POINT('Ctrl Pts',(16.4242940584281,3.9320927199654,-0.14351393235063));
#80884=CARTESIAN_POINT('Ctrl Pts',(16.4301476701124,3.93461129881638,-0.0274556404041727));
#80885=CARTESIAN_POINT('Ctrl Pts',(16.4360012817966,3.93200626176507,0.0884067725927054));
#80886=CARTESIAN_POINT('Ctrl Pts',(16.4418615478965,3.92939826329435,0.204400898572298));
#80887=CARTESIAN_POINT('Ctrl Pts',(16.4477218139964,3.92165503260585,0.320198287651489));
#80888=CARTESIAN_POINT('Ctrl Pts',(16.4535820800963,3.90883488221637,0.435314671896743));
#80889=CARTESIAN_POINT('Ctrl Pts',(16.4594462932676,3.89600609705702,0.550508590605755));
#80890=CARTESIAN_POINT('Ctrl Pts',(16.4653105064389,3.87809364708405,0.66502018376895));
#80891=CARTESIAN_POINT('Ctrl Pts',(16.4711747196102,3.8552069855118,0.778375294354234));
#80892=CARTESIAN_POINT('Ctrl Pts',(16.4770475681845,3.83228662196796,0.891897327087797));
#80893=CARTESIAN_POINT('Ctrl Pts',(16.4829204167588,3.80437752720706,1.00425907875835));
#80894=CARTESIAN_POINT('Ctrl Pts',(16.488793265333,3.77163902352979,1.11500137945533));
#80895=CARTESIAN_POINT('Ctrl Pts',(16.4903880099458,3.76274903569678,1.14507293420628));
#80896=CARTESIAN_POINT('Ctrl Pts',(16.4919827545586,3.75350321593581,1.17502519129287));
#80897=CARTESIAN_POINT('Ctrl Pts',(16.4935774991715,3.74390535814819,1.20484923091203));
#80898=CARTESIAN_POINT('Ctrl Pts',(16.4994499453054,3.70856245596412,1.31467249963693));
#80899=CARTESIAN_POINT('Ctrl Pts',(16.5053223914393,3.6683239712852,1.42312320185847));
#80900=CARTESIAN_POINT('Ctrl Pts',(16.5111948375732,3.62331442439222,1.52973251975346));
#80901=CARTESIAN_POINT('Ctrl Pts',(16.517059676518,3.57836318303758,1.63620373553232));
#80902=CARTESIAN_POINT('Ctrl Pts',(16.5229245154629,3.52865332948246,1.74083793327168));
#80903=CARTESIAN_POINT('Ctrl Pts',(16.5287893544077,3.47435915752887,1.84318133793051));
#80904=CARTESIAN_POINT('Ctrl Pts',(16.5346481645278,3.4201207978584,1.94541953757613));
#80905=CARTESIAN_POINT('Ctrl Pts',(16.5405069746478,3.36130768576459,2.04537126509643));
#80906=CARTESIAN_POINT('Ctrl Pts',(16.5463657847678,3.29814194572552,2.14260325441877));
#80907=CARTESIAN_POINT('Ctrl Pts',(16.5524515736488,3.23252907374073,2.24360215135699));
#80908=CARTESIAN_POINT('Ctrl Pts',(16.5585373625298,3.16221967541623,2.34166589628814));
#80909=CARTESIAN_POINT('Ctrl Pts',(16.5646231514107,3.0875151140716,2.43633729610237));
#80910=CARTESIAN_POINT('Ctrl Pts',(16.570475181489,3.01567999975477,2.52737231064207));
#80911=CARTESIAN_POINT('Ctrl Pts',(16.5763272115673,2.93978141560752,2.61527042240941));
#80912=CARTESIAN_POINT('Ctrl Pts',(16.5821792416455,2.86013061927182,2.69965587449656));
#80913=CARTESIAN_POINT('Ctrl Pts',(16.5880303820241,2.78049193245931,2.78402849723817));
#80914=CARTESIAN_POINT('Ctrl Pts',(16.5938815224026,2.69710245137203,2.86488922162652));
#80915=CARTESIAN_POINT('Ctrl Pts',(16.5997326627811,2.61031185592353,2.94189751942944));
#80916=CARTESIAN_POINT('Ctrl Pts',(16.6055843303486,2.52351344062408,3.01891275569622));
#80917=CARTESIAN_POINT('Ctrl Pts',(16.6114359979161,2.43331361099781,3.09207460100663));
#80918=CARTESIAN_POINT('Ctrl Pts',(16.6172876654836,2.34009628762112,3.16108183454049));
#80919=CARTESIAN_POINT('Ctrl Pts',(16.6231412771678,2.24684799437861,3.23011199455073));
#80920=CARTESIAN_POINT('Ctrl Pts',(16.6289948888521,2.15058054600681,3.2949845523311));
#80921=CARTESIAN_POINT('Ctrl Pts',(16.6348485005363,2.05170748117339,3.35544116498817));
#80922=CARTESIAN_POINT('Ctrl Pts',(16.6407087666362,1.95272201693505,3.41596650503118));
#80923=CARTESIAN_POINT('Ctrl Pts',(16.6465690327361,1.85112537689023,3.47206566429996));
#80924=CARTESIAN_POINT('Ctrl Pts',(16.652429298836,1.74735646171636,3.52352584717327));
#80925=CARTESIAN_POINT('Ctrl Pts',(16.6582935120073,1.64351765495195,3.57502069007963));
#80926=CARTESIAN_POINT('Ctrl Pts',(16.6641577251786,1.53750403690162,3.6218701684192));
#80927=CARTESIAN_POINT('Ctrl Pts',(16.6700219383499,1.42977365516118,3.66390997364933));
#80928=CARTESIAN_POINT('Ctrl Pts',(16.6758947869242,1.32188463402051,3.70601168499526));
#80929=CARTESIAN_POINT('Ctrl Pts',(16.6817676354985,1.21227419360324,3.74328945532005));
#80930=CARTESIAN_POINT('Ctrl Pts',(16.6876404840728,1.10141473893056,3.77562903009108));
#80931=CARTESIAN_POINT('Ctrl Pts',(16.6892352286856,1.07131137156472,3.78441069064193));
#80932=CARTESIAN_POINT('Ctrl Pts',(16.6908299732984,1.0411159564907,3.79282851673441));
#80933=CARTESIAN_POINT('Ctrl Pts',(16.6924247179112,1.01083804852762,3.80088087680328));
#80934=CARTESIAN_POINT('Ctrl Pts',(16.6982971640451,0.899343466802657,3.830532678337));
#80935=CARTESIAN_POINT('Ctrl Pts',(16.704169610179,0.786356408673737,3.85532411147381));
#80936=CARTESIAN_POINT('Ctrl Pts',(16.7100420563129,0.672338577263635,3.87510642918657));
#80937=CARTESIAN_POINT('Ctrl Pts',(16.7159068952577,0.558468444986268,3.89486312080969));
#80938=CARTESIAN_POINT('Ctrl Pts',(16.7217717342026,0.443570598317961,3.90962353096729));
#80939=CARTESIAN_POINT('Ctrl Pts',(16.7276365731474,0.32812099931161,3.91928891634832));
#80940=CARTESIAN_POINT('Ctrl Pts',(16.7334953832675,0.212790077973007,3.92894436609158));
#80941=CARTESIAN_POINT('Ctrl Pts',(16.7393541933875,0.0969089418910236,
3.93351517442654));
#80942=CARTESIAN_POINT('Ctrl Pts',(16.7452130035075,-0.0190378366721754,
3.93295392304243));
#80943=CARTESIAN_POINT('Ctrl Pts',(16.7512987923885,-0.139476560800132,
3.93237092796956));
#80944=CARTESIAN_POINT('Ctrl Pts',(16.7573845812695,-0.259985668775966,
3.92625010633041));
#80945=CARTESIAN_POINT('Ctrl Pts',(16.7634703701504,-0.380017615447589,
3.91459775864003));
#80946=CARTESIAN_POINT('Ctrl Pts',(16.7693224002287,-0.49543906302227,3.90339298461643));
#80947=CARTESIAN_POINT('Ctrl Pts',(16.775174430307,-0.610418879766082,3.88707382810077));
#80948=CARTESIAN_POINT('Ctrl Pts',(16.7810264603852,-0.72447267542454,3.86569894618854));
#80949=CARTESIAN_POINT('Ctrl Pts',(16.7868776007637,-0.838509131179923,
3.84432731395668));
#80950=CARTESIAN_POINT('Ctrl Pts',(16.7927287411422,-0.95161943960452,3.81790156074716));
#80951=CARTESIAN_POINT('Ctrl Pts',(16.7985798815207,-1.06332806980422,3.78653171331846));
#80952=CARTESIAN_POINT('Ctrl Pts',(16.8044315490882,-1.17504676497526,3.75515903945984));
#80953=CARTESIAN_POINT('Ctrl Pts',(16.8102832166557,-1.28536313287844,3.71884149760305));
#80954=CARTESIAN_POINT('Ctrl Pts',(16.8161348842232,-1.39381619408798,3.67773917197755));
#80955=CARTESIAN_POINT('Ctrl Pts',(16.8219884959075,-1.50230528697723,3.63662319080544));
#80956=CARTESIAN_POINT('Ctrl Pts',(16.8278421075917,-1.60892945590143,3.59071941132919));
#80957=CARTESIAN_POINT('Ctrl Pts',(16.833695719276,-1.71324777592382,3.54023601731468));
#80958=CARTESIAN_POINT('Ctrl Pts',(16.8395559853758,-1.81768468554497,3.48969523352012));
#80959=CARTESIAN_POINT('Ctrl Pts',(16.8454162514757,-1.9198101419382,3.4345646240956));
#80960=CARTESIAN_POINT('Ctrl Pts',(16.8512765175756,-2.01920782143974,3.37509833543211));
#80961=CARTESIAN_POINT('Ctrl Pts',(16.8571407307469,-2.11867244836869,3.3155919943744));
#80962=CARTESIAN_POINT('Ctrl Pts',(16.8630049439182,-2.21540529594528,3.25174438649032));
#80963=CARTESIAN_POINT('Ctrl Pts',(16.8688691570895,-2.30902047533366,3.18385198218917));
#80964=CARTESIAN_POINT('Ctrl Pts',(16.8747420056638,-2.40277350864656,3.11585960228109));
#80965=CARTESIAN_POINT('Ctrl Pts',(16.8806148542381,-2.49339938880002,3.04381079482913));
#80966=CARTESIAN_POINT('Ctrl Pts',(16.8864877028124,-2.58054656963073,2.96804117255254));
#80967=CARTESIAN_POINT('Ctrl Pts',(16.8880824474251,-2.60421097973624,2.94746628535595));
#80968=CARTESIAN_POINT('Ctrl Pts',(16.8896771920379,-2.62761910019042,2.9266172377897));
#80969=CARTESIAN_POINT('Ctrl Pts',(16.8912719366507,-2.65076439211749,2.90550118524877));
#80970=CARTESIAN_POINT('Ctrl Pts',(16.8970566991093,-2.73472141869071,2.82890500361985));
#80971=CARTESIAN_POINT('Ctrl Pts',(16.9028414615679,-2.8155164682209,2.74851984382134));
#80972=CARTESIAN_POINT('Ctrl Pts',(16.9086262240266,-2.89278011612591,2.66464110148938));
#80973=CARTESIAN_POINT('Ctrl Pts',(16.9144034208435,-2.96994271423334,2.58087206055212));
#80974=CARTESIAN_POINT('Ctrl Pts',(16.9201806176604,-3.04358280363557,2.49361882875862));
#80975=CARTESIAN_POINT('Ctrl Pts',(16.9259578144773,-3.11336480779858,2.40321629770633));
#80976=CARTESIAN_POINT('Ctrl Pts',(16.9317284140713,-3.18306712496895,2.3129170010898));
#80977=CARTESIAN_POINT('Ctrl Pts',(16.9374990136653,-3.24891986163083,2.21947589476493));
#80978=CARTESIAN_POINT('Ctrl Pts',(16.9432696132592,-3.31062573586229,2.12326311064981));
#80979=CARTESIAN_POINT('Ctrl Pts',(16.9490365710708,-3.37229266797669,2.02711104570523));
#80980=CARTESIAN_POINT('Ctrl Pts',(16.9548035288824,-3.4298177075269,1.92819113610653));
#80981=CARTESIAN_POINT('Ctrl Pts',(16.960570486694,-3.48294549312191,1.82690440142383));
#80982=CARTESIAN_POINT('Ctrl Pts',(16.9663352982464,-3.53605350642034,1.72565536210779));
#80983=CARTESIAN_POINT('Ctrl Pts',(16.9721001097988,-3.58476732048757,1.62204162590005));
#80984=CARTESIAN_POINT('Ctrl Pts',(16.9778649213511,-3.62887680623236,1.51649006761958));
#80985=CARTESIAN_POINT('Ctrl Pts',(16.9836290798747,-3.67298129532408,1.41095046605338));
#80986=CARTESIAN_POINT('Ctrl Pts',(16.9893932383983,-3.71248233006194,1.30347387312784));
#80987=CARTESIAN_POINT('Ctrl Pts',(16.9951573969219,-3.7472177048882,1.194507627507));
#80988=CARTESIAN_POINT('Ctrl Pts',(17.0009249127067,-3.78197331089375,1.08547791587602));
#80989=CARTESIAN_POINT('Ctrl Pts',(17.0066924284914,-3.81195758242033,0.974957225464982));
#80990=CARTESIAN_POINT('Ctrl Pts',(17.0124599442761,-3.83705813313859,0.863408294444193));
#80991=CARTESIAN_POINT('Ctrl Pts',(17.0182292829875,-3.86216661733521,0.751824106386962));
#80992=CARTESIAN_POINT('Ctrl Pts',(17.0239986216988,-3.88238822930771,0.639211450260981));
#80993=CARTESIAN_POINT('Ctrl Pts',(17.0297679604102,-3.89766198503899,0.526041871320081));
#80994=CARTESIAN_POINT('Ctrl Pts',(17.0355438875975,-3.91295318311102,0.412743054856122));
#80995=CARTESIAN_POINT('Ctrl Pts',(17.0413198147847,-3.92328520357892,0.298886470476205));
#80996=CARTESIAN_POINT('Ctrl Pts',(17.047095741972,-3.92864906866525,0.184947277016033));
#80997=CARTESIAN_POINT('Ctrl Pts',(17.050275987303,-3.9316024311894,0.122211966082349));
#80998=CARTESIAN_POINT('Ctrl Pts',(17.0534562326341,-3.93305054888195,0.0594516086523946));
#80999=CARTESIAN_POINT('Ctrl Pts',(17.0566364779651,-3.93299865311076,-0.00325493916173806));
#81000=CARTESIAN_POINT('',(18.3066364779651,-3.93441244414383,0.00256739835708875));
#81001=CARTESIAN_POINT('Ctrl Pts',(17.0566364779651,-3.93555909411355,-0.00325705817586157));
#81002=CARTESIAN_POINT('Ctrl Pts',(17.0677973704402,-3.93752172051231,-0.223467208643121));
#81003=CARTESIAN_POINT('Ctrl Pts',(17.1452406691619,-3.82037057107914,-1.74937440102309));
#81004=CARTESIAN_POINT('Ctrl Pts',(17.28896637413,-1.82419876275297,-4.2790524821404));
#81005=CARTESIAN_POINT('Ctrl Pts',(17.4878135928696,2.61321414266571,-3.84825975156499));
#81006=CARTESIAN_POINT('Ctrl Pts',(17.6866608116094,4.650182051095,0.117465580568825));
#81007=CARTESIAN_POINT('Ctrl Pts',(17.8855080303489,2.41558795570895,3.97528943589974));
#81008=CARTESIAN_POINT('Ctrl Pts',(18.0843552490887,-2.03791576839781,4.18149382300865));
#81009=CARTESIAN_POINT('Ctrl Pts',(18.224731398294,-3.86033642911773,1.61548625749645));
#81010=CARTESIAN_POINT('Ctrl Pts',(18.2988251412528,-3.93851969709005,0.156507900232432));
#81011=CARTESIAN_POINT('Ctrl Pts',(18.3066364779651,-3.93735639800032,0.00256931943232003));
#81012=CARTESIAN_POINT('',(19.5566364501327,-3.93099991098921,0.0019806725685321));
#81013=CARTESIAN_POINT('Ctrl Pts',(18.3066364779651,-3.9329991626239,0.00256647612112477));
#81014=CARTESIAN_POINT('Ctrl Pts',(18.3124243982231,-3.93307351157268,-0.111369652441173));
#81015=CARTESIAN_POINT('Ctrl Pts',(18.3182123184812,-3.9281927071081,-0.225501921867932));
#81016=CARTESIAN_POINT('Ctrl Pts',(18.3240002387392,-3.91833207797461,-0.339356341793069));
#81017=CARTESIAN_POINT('Ctrl Pts',(18.3297815910592,-3.90848263835275,-0.453081563536361));
#81018=CARTESIAN_POINT('Ctrl Pts',(18.3355629433793,-3.89366464276368,-0.566529141787071));
#81019=CARTESIAN_POINT('Ctrl Pts',(18.3413442956993,-3.87390544353728,-0.679224274104115));
#81020=CARTESIAN_POINT('Ctrl Pts',(18.3472070203188,-3.85386813438285,-0.793505585839553));
#81021=CARTESIAN_POINT('Ctrl Pts',(18.3530697449383,-3.8287494430815,-0.907012664087174));
#81022=CARTESIAN_POINT('Ctrl Pts',(18.3589324695578,-3.79863253644424,-1.01925455754055));
#81023=CARTESIAN_POINT('Ctrl Pts',(18.3647060952287,-3.76897333247794,-1.12979065115714));
#81024=CARTESIAN_POINT('Ctrl Pts',(18.3704797208996,-3.73446689042605,-1.23909932194822));
#81025=CARTESIAN_POINT('Ctrl Pts',(18.3762533465705,-3.69524406185396,-1.34672206610461));
#81026=CARTESIAN_POINT('Ctrl Pts',(18.3820257767339,-3.65602935490084,-1.4543225255112));
#81027=CARTESIAN_POINT('Ctrl Pts',(18.3877982068972,-3.61210034781823,-1.56023735225455));
#81028=CARTESIAN_POINT('Ctrl Pts',(18.3935706370606,-3.56363722976075,-1.66402484797046));
#81029=CARTESIAN_POINT('Ctrl Pts',(18.3993433590193,-3.51517166190038,-1.76781759012774));
#81030=CARTESIAN_POINT('Ctrl Pts',(18.4051160809781,-3.46217170848123,-1.86948240220678));
#81031=CARTESIAN_POINT('Ctrl Pts',(18.4108888029369,-3.40486463611714,-1.96859996183046));
#81032=CARTESIAN_POINT('Ctrl Pts',(18.4168188765728,-3.34599549926883,-2.07041924766809));
#81033=CARTESIAN_POINT('Ctrl Pts',(18.4227489502087,-3.28258128171833,-2.16954999672107));
#81034=CARTESIAN_POINT('Ctrl Pts',(18.4286790238446,-3.21491656800035,-2.26556846305665));
#81035=CARTESIAN_POINT('Ctrl Pts',(18.4344599653401,-3.14895351672432,-2.35917221411569));
#81036=CARTESIAN_POINT('Ctrl Pts',(18.4402409068357,-3.0789515343617,-2.44981806250247));
#81037=CARTESIAN_POINT('Ctrl Pts',(18.4460218483312,-3.00522427957689,-2.53714722265807));
#81038=CARTESIAN_POINT('Ctrl Pts',(18.4520264880373,-2.92864408898966,-2.62785565535448));
#81039=CARTESIAN_POINT('Ctrl Pts',(18.4580311277434,-2.84804485615273,-2.71498515999039));
#81040=CARTESIAN_POINT('Ctrl Pts',(18.4640357674495,-2.76381877789818,-2.79817704281509));
#81041=CARTESIAN_POINT('Ctrl Pts',(18.4700404071556,-2.67959269964363,-2.88136892563979));
#81042=CARTESIAN_POINT('Ctrl Pts',(18.4760450468618,-2.5917402031067,-2.96062290501553));
#81043=CARTESIAN_POINT('Ctrl Pts',(18.4820496865679,-2.50068890915906,-3.03562909124433));
#81044=CARTESIAN_POINT('Ctrl Pts',(18.4879221327018,-2.41164213111716,-3.10898399843243));
#81045=CARTESIAN_POINT('Ctrl Pts',(18.4937945788357,-2.31921585654286,-3.17854026507982));
#81046=CARTESIAN_POINT('Ctrl Pts',(18.4996670249696,-2.22376803057712,-3.24397052178086));
#81047=CARTESIAN_POINT('Ctrl Pts',(18.5055318639145,-2.12844384808832,-3.30931601987839));
#81048=CARTESIAN_POINT('Ctrl Pts',(18.5113967028593,-2.03010623581613,-3.37054590547077));
#81049=CARTESIAN_POINT('Ctrl Pts',(18.5172615418042,-1.92914691094862,-3.42737234568662));
#81050=CARTESIAN_POINT('Ctrl Pts',(18.5231203519242,-1.82829136831464,-3.48414037054661));
#81051=CARTESIAN_POINT('Ctrl Pts',(18.5289791620442,-1.72481983167672,-3.53651375208932));
#81052=CARTESIAN_POINT('Ctrl Pts',(18.5348379721642,-1.61915320353093,-3.58424774583113));
#81053=CARTESIAN_POINT('Ctrl Pts',(18.5409237610452,-1.50939289768618,-3.63383102339216));
#81054=CARTESIAN_POINT('Ctrl Pts',(18.5470095499262,-1.39726435316989,-3.67840791277819));
#81055=CARTESIAN_POINT('Ctrl Pts',(18.5530953388071,-1.28326808708139,-3.71775631485961));
#81056=CARTESIAN_POINT('Ctrl Pts',(18.5589473688854,-1.1736504859769,-3.75559332120603));
#81057=CARTESIAN_POINT('Ctrl Pts',(18.5647993989637,-1.06230642408677,-3.78859594246006));
#81058=CARTESIAN_POINT('Ctrl Pts',(18.5706514290419,-0.949700775371681,
-3.81661596669857));
#81059=CARTESIAN_POINT('Ctrl Pts',(18.5765025694205,-0.837112246394062,
-3.84463173097796));
#81060=CARTESIAN_POINT('Ctrl Pts',(18.582353709799,-0.723262912972853,-3.86766630464765));
#81061=CARTESIAN_POINT('Ctrl Pts',(18.5882048501775,-0.608630967475324,
-3.88562187370697));
#81062=CARTESIAN_POINT('Ctrl Pts',(18.594056517745,-0.493988693615218,-3.90357906056686));
#81063=CARTESIAN_POINT('Ctrl Pts',(18.5999081853125,-0.378564075906531,
-3.91645626914058));
#81064=CARTESIAN_POINT('Ctrl Pts',(18.60575985288,-0.262842903166594,-3.92420725857529));
#81065=CARTESIAN_POINT('Ctrl Pts',(18.6116134645642,-0.14708328404066,-3.93196082314403));
#81066=CARTESIAN_POINT('Ctrl Pts',(18.6174670762485,-0.0310273261863687,
-3.93458475445545));
#81067=CARTESIAN_POINT('Ctrl Pts',(18.6233206879327,0.0848374038312977,
-3.9320848941638));
#81068=CARTESIAN_POINT('Ctrl Pts',(18.6291809540326,0.200833849465549,-3.92958219201821));
#81069=CARTESIAN_POINT('Ctrl Pts',(18.6350412201325,0.316638219857573,-3.92194408118004));
#81070=CARTESIAN_POINT('Ctrl Pts',(18.6409014862324,0.431766194339378,-3.90922843454123));
#81071=CARTESIAN_POINT('Ctrl Pts',(18.6467656994037,0.546971711091178,-3.8965042235191));
#81072=CARTESIAN_POINT('Ctrl Pts',(18.652629912575,0.66149951734439,-3.87869573038758));
#81073=CARTESIAN_POINT('Ctrl Pts',(18.6584941257463,0.774875356904638,-3.85591197789341));
#81074=CARTESIAN_POINT('Ctrl Pts',(18.6643669743206,0.888418149137797,-3.83309467496741));
#81075=CARTESIAN_POINT('Ctrl Pts',(18.6702398228949,1.00080518937484,-3.80528758961883));
#81076=CARTESIAN_POINT('Ctrl Pts',(18.6761126714692,1.11157716326739,-3.77264962726496));
#81077=CARTESIAN_POINT('Ctrl Pts',(18.677707416082,1.1416567756359,-3.76378694095899));
#81078=CARTESIAN_POINT('Ctrl Pts',(18.6793021606948,1.17161741340048,-3.7545683145776));
#81079=CARTESIAN_POINT('Ctrl Pts',(18.6808969053076,1.2014501533178,-3.74499753392344));
#81080=CARTESIAN_POINT('Ctrl Pts',(18.6867693514415,1.31130545979526,-3.70975433987203));
#81081=CARTESIAN_POINT('Ctrl Pts',(18.6926417975754,1.41979264436669,-3.66961431937687));
#81082=CARTESIAN_POINT('Ctrl Pts',(18.6985142437093,1.52644277636708,-3.62470156709166));
#81083=CARTESIAN_POINT('Ctrl Pts',(18.7043790826541,1.63295475338068,-3.57984699495666));
#81084=CARTESIAN_POINT('Ctrl Pts',(18.710243921599,1.73763403280681,-3.53023214500362));
#81085=CARTESIAN_POINT('Ctrl Pts',(18.7161087605438,1.84002668157384,-3.47603089904223));
#81086=CARTESIAN_POINT('Ctrl Pts',(18.7219675706639,1.94231407470667,-3.42188536983969));
#81087=CARTESIAN_POINT('Ctrl Pts',(18.7278263807839,2.04231914945018,-3.3631630145224));
#81088=CARTESIAN_POINT('Ctrl Pts',(18.7336851909039,2.13960843827371,-3.30008556417374));
#81089=CARTESIAN_POINT('Ctrl Pts',(18.7397709797849,2.24066685457846,-3.23456440234945));
#81090=CARTESIAN_POINT('Ctrl Pts',(18.7458567686658,2.33879438342135,-3.16434405169622));
#81091=CARTESIAN_POINT('Ctrl Pts',(18.7519425575468,2.43353355831423,-3.08972546038616));
#81092=CARTESIAN_POINT('Ctrl Pts',(18.7577945876251,2.52463374465121,-3.01797301394323));
#81093=CARTESIAN_POINT('Ctrl Pts',(18.7636466177034,2.61260071817849,-2.94215425177779));
#81094=CARTESIAN_POINT('Ctrl Pts',(18.7694986477816,2.69705843959465,-2.86258009030512));
#81095=CARTESIAN_POINT('Ctrl Pts',(18.7753497881601,2.78150332067783,-2.78301802670477));
#81096=CARTESIAN_POINT('Ctrl Pts',(18.7812009285386,2.8624397096894,-2.6997019824014));
#81097=CARTESIAN_POINT('Ctrl Pts',(18.7870520689171,2.93952676111078,-2.61298132804533));
#81098=CARTESIAN_POINT('Ctrl Pts',(18.7929037364846,3.01662075809179,-2.52625286013998));
#81099=CARTESIAN_POINT('Ctrl Pts',(18.7987554040521,3.08986445338437,-2.43611948134101));
#81100=CARTESIAN_POINT('Ctrl Pts',(18.8046070716196,3.15895627778329,-2.34296483862936));
#81101=CARTESIAN_POINT('Ctrl Pts',(18.8104606833039,3.22807105676253,-2.2497792468764));
#81102=CARTESIAN_POINT('Ctrl Pts',(18.8163142949881,3.29303097590415,-2.15357072711794));
#81103=CARTESIAN_POINT('Ctrl Pts',(18.8221679066724,3.35357731702582,-2.05475258333696));
#81104=CARTESIAN_POINT('Ctrl Pts',(18.8280281727722,3.41419248753713,-1.95582210258571));
#81105=CARTESIAN_POINT('Ctrl Pts',(18.8338884388721,3.47038384942836,-1.85427642917784));
#81106=CARTESIAN_POINT('Ctrl Pts',(18.839748704972,3.52193820874784,-1.7505542704418));
#81107=CARTESIAN_POINT('Ctrl Pts',(18.8456129181433,3.57352729153124,-1.64676225160697));
#81108=CARTESIAN_POINT('Ctrl Pts',(18.8514771313146,3.62047298587642,-1.5407912054892));
#81109=CARTESIAN_POINT('Ctrl Pts',(18.8573413444859,3.66261056750948,-1.43309903034226));
#81110=CARTESIAN_POINT('Ctrl Pts',(18.8632141930602,3.70481019923985,-1.32524827205673));
#81111=CARTESIAN_POINT('Ctrl Pts',(18.8690870416345,3.74218745457847,-1.21567171620558));
#81112=CARTESIAN_POINT('Ctrl Pts',(18.8749598902088,3.77462765020768,-1.10484166389924));
#81113=CARTESIAN_POINT('Ctrl Pts',(18.8765546348216,3.78343663388278,-1.07474628060885));
#81114=CARTESIAN_POINT('Ctrl Pts',(18.8781493794344,3.79188186680698,-1.0445585193725));
#81115=CARTESIAN_POINT('Ctrl Pts',(18.8797441240472,3.7999617087422,-1.01428793352432));
#81116=CARTESIAN_POINT('Ctrl Pts',(18.8856165701811,3.82971470878677,-0.902820314564572));
#81117=CARTESIAN_POINT('Ctrl Pts',(18.891489016315,3.85460869725281,-0.789855807750062));
#81118=CARTESIAN_POINT('Ctrl Pts',(18.8973614624489,3.87449450805717,-0.675855980986188));
#81119=CARTESIAN_POINT('Ctrl Pts',(18.9032263013937,3.89435455870654,-0.562003830031724));
#81120=CARTESIAN_POINT('Ctrl Pts',(18.9090911403386,3.90921926287072,-0.447119429667083));
#81121=CARTESIAN_POINT('Ctrl Pts',(18.9149559792834,3.91898944521827,-0.331678652113463));
#81122=CARTESIAN_POINT('Ctrl Pts',(18.9208147894035,3.92874958420086,-0.216356543159836));
#81123=CARTESIAN_POINT('Ctrl Pts',(18.9266735995235,3.93342558333507,-0.100479604036908));
#81124=CARTESIAN_POINT('Ctrl Pts',(18.9325324096435,3.9329695844526,0.0154676362374262));
#81125=CARTESIAN_POINT('Ctrl Pts',(18.9386181985245,3.93249591951521,0.135906839964299));
#81126=CARTESIAN_POINT('Ctrl Pts',(18.9447039874054,3.92648449418511,0.256421454547686));
#81127=CARTESIAN_POINT('Ctrl Pts',(18.9507897762864,3.91494111193318,0.37646392934171));
#81128=CARTESIAN_POINT('Ctrl Pts',(18.9566418063647,3.90384111792017,0.491895500647184));
#81129=CARTESIAN_POINT('Ctrl Pts',(18.9624938364429,3.8876263426259,0.606890083954243));
#81130=CARTESIAN_POINT('Ctrl Pts',(18.9683458665212,3.86635500340985,0.720963235961203));
#81131=CARTESIAN_POINT('Ctrl Pts',(18.9741970068997,3.84508689813226,0.835019045122419));
#81132=CARTESIAN_POINT('Ctrl Pts',(18.9800481472782,3.81876383323651,0.948153295281717));
#81133=CARTESIAN_POINT('Ctrl Pts',(18.9858992876567,3.78749540376611,1.05989035586263));
#81134=CARTESIAN_POINT('Ctrl Pts',(18.9917509552242,3.75622415700368,1.17163748397603));
#81135=CARTESIAN_POINT('Ctrl Pts',(18.9976026227917,3.72000677129877,1.28198677417077));
#81136=CARTESIAN_POINT('Ctrl Pts',(19.0034542903592,3.67900291235452,1.39047710189235));
#81137=CARTESIAN_POINT('Ctrl Pts',(19.0093079020435,3.63798543057736,1.4990034736753));
#81138=CARTESIAN_POINT('Ctrl Pts',(19.0151615137277,3.59217845955852,1.60566926845081));
#81139=CARTESIAN_POINT('Ctrl Pts',(19.021015125412,3.54178978272248,1.71003337248215));
#81140=CARTESIAN_POINT('Ctrl Pts',(19.0268753915119,3.4913438237814,1.81451611815967));
#81141=CARTESIAN_POINT('Ctrl Pts',(19.0327356576117,3.43630594284824,1.91669157803847));
#81142=CARTESIAN_POINT('Ctrl Pts',(19.0385959237116,3.37692990828578,2.01614319792147));
#81143=CARTESIAN_POINT('Ctrl Pts',(19.0444601368829,3.31751388211816,2.1156618015622));
#81144=CARTESIAN_POINT('Ctrl Pts',(19.0503243500542,3.25375411110288,2.21245256782033));
#81145=CARTESIAN_POINT('Ctrl Pts',(19.0561885632255,3.18594671523122,2.30612933889395));
#81146=CARTESIAN_POINT('Ctrl Pts',(19.0620614117998,3.11803946893254,2.39994405458956));
#81147=CARTESIAN_POINT('Ctrl Pts',(19.0679342603741,3.04607295804537,2.49063530069165));
#81148=CARTESIAN_POINT('Ctrl Pts',(19.0738071089484,2.97038247602983,2.5778512265247));
#81149=CARTESIAN_POINT('Ctrl Pts',(19.0754018535612,2.94982907900116,2.60153430401523));
#81150=CARTESIAN_POINT('Ctrl Pts',(19.076996598174,2.92900128906535,2.62496134083283));
#81151=CARTESIAN_POINT('Ctrl Pts',(19.0785913427869,2.90790625567867,2.64812579160901));
#81152=CARTESIAN_POINT('Ctrl Pts',(19.0844637889208,2.83022645274341,2.73342596337996));
#81153=CARTESIAN_POINT('Ctrl Pts',(19.0903362350547,2.74866013708834,2.81544807388718));
#81154=CARTESIAN_POINT('Ctrl Pts',(19.0962086811886,2.66351492812146,2.89381706879929));
#81155=CARTESIAN_POINT('Ctrl Pts',(19.1020735201335,2.57848001658223,2.97208454421722));
#81156=CARTESIAN_POINT('Ctrl Pts',(19.1079383590783,2.48987573264462,3.0467080374681));
#81157=CARTESIAN_POINT('Ctrl Pts',(19.1138031980232,2.39804875914592,3.11734681239651));
#81158=CARTESIAN_POINT('Ctrl Pts',(19.1196620081432,2.30631618018096,3.1879129734298));
#81159=CARTESIAN_POINT('Ctrl Pts',(19.1255208182632,2.21136782665817,3.25450231305547));
#81160=CARTESIAN_POINT('Ctrl Pts',(19.1313796283832,2.11358541130495,3.31681258275455));
#81161=CARTESIAN_POINT('Ctrl Pts',(19.1374654172642,2.01201476403699,3.38153684224348));
#81162=CARTESIAN_POINT('Ctrl Pts',(19.1435512061452,1.90738635673773,3.44164346374798));
#81163=CARTESIAN_POINT('Ctrl Pts',(19.1496369950261,1.80016393188753,3.49684126295879));
#81164=CARTESIAN_POINT('Ctrl Pts',(19.1554890251044,1.69705998471473,3.54991888158042));
#81165=CARTESIAN_POINT('Ctrl Pts',(19.1613410551827,1.59155802113151,3.59845761670925));
#81166=CARTESIAN_POINT('Ctrl Pts',(19.1671930852609,1.48409703788399,3.64224449785348));
#81167=CARTESIAN_POINT('Ctrl Pts',(19.1730442256394,1.37665239221657,3.68602472196131));
#81168=CARTESIAN_POINT('Ctrl Pts',(19.178895366018,1.26724970177216,3.72505437258937));
#81169=CARTESIAN_POINT('Ctrl Pts',(19.1847465063965,1.15634833039371,3.75916846374244));
#81170=CARTESIAN_POINT('Ctrl Pts',(19.1905981739639,1.04543696677868,3.7932856285822));
#81171=CARTESIAN_POINT('Ctrl Pts',(19.1964498415314,0.933027048910614,3.82248623197764));
#81172=CARTESIAN_POINT('Ctrl Pts',(19.2023015090989,0.819592811755834,3.84665525137335));
#81173=CARTESIAN_POINT('Ctrl Pts',(19.2081551207831,0.706120888010383,3.87083230051355));
#81174=CARTESIAN_POINT('Ctrl Pts',(19.2140087324674,0.591624372355505,3.88997435557079));
#81175=CARTESIAN_POINT('Ctrl Pts',(19.2198623441516,0.476586684223825,3.90401769109984));
#81176=CARTESIAN_POINT('Ctrl Pts',(19.2257226102515,0.361418220660793,3.91807699116444));
#81177=CARTESIAN_POINT('Ctrl Pts',(19.2315828763514,0.245707767240356,3.92702595246014));
#81178=CARTESIAN_POINT('Ctrl Pts',(19.2374431424512,0.129942948218467,3.93085281207632));
#81179=CARTESIAN_POINT('Ctrl Pts',(19.2433073556225,0.0141001579920049,
3.93468224920142));
#81180=CARTESIAN_POINT('Ctrl Pts',(19.2491715687938,-0.101796658427518,
3.93338271983628));
#81181=CARTESIAN_POINT('Ctrl Pts',(19.2550357819651,-0.217262546543552,
3.92699452327978));
#81182=CARTESIAN_POINT('Ctrl Pts',(19.2609086305394,-0.332898465053581,
3.92059691972356));
#81183=CARTESIAN_POINT('Ctrl Pts',(19.2667814791137,-0.448101779025144,
3.9090957346196));
#81184=CARTESIAN_POINT('Ctrl Pts',(19.272654327688,-0.562395211926534,3.89258277055249));
#81185=CARTESIAN_POINT('Ctrl Pts',(19.2742490723008,-0.59343106004965,3.88809875225118));
#81186=CARTESIAN_POINT('Ctrl Pts',(19.2758438169136,-0.624399891530775,
3.8832454683769));
#81187=CARTESIAN_POINT('Ctrl Pts',(19.2774385615265,-0.655292334563368,
3.87802539396824));
#81188=CARTESIAN_POINT('Ctrl Pts',(19.2833110076604,-0.769049864260871,
3.85880312757318));
#81189=CARTESIAN_POINT('Ctrl Pts',(19.2891834537943,-0.882151336824631,
3.83453901074328));
#81190=CARTESIAN_POINT('Ctrl Pts',(19.2950558999282,-0.994114920244128,
3.80528901994947));
#81191=CARTESIAN_POINT('Ctrl Pts',(19.3009207388731,-1.10593346561165,3.77607691970503));
#81192=CARTESIAN_POINT('Ctrl Pts',(19.3067855778179,-1.21661665690062,3.741891893112));
#81193=CARTESIAN_POINT('Ctrl Pts',(19.3126504167628,-1.32569040885986,3.70284133333538));
#81194=CARTESIAN_POINT('Ctrl Pts',(19.3185092268828,-1.43465203727234,3.66383091600539));
#81195=CARTESIAN_POINT('Ctrl Pts',(19.3243680370029,-1.54200713029718,3.61996505239691));
#81196=CARTESIAN_POINT('Ctrl Pts',(19.3302268471229,-1.64729503780582,3.57140141378987));
#81197=CARTESIAN_POINT('Ctrl Pts',(19.3363126360039,-1.75666195082899,3.52095634972411));
#81198=CARTESIAN_POINT('Ctrl Pts',(19.3423984248848,-1.86379782777535,3.46544226652362));
#81199=CARTESIAN_POINT('Ctrl Pts',(19.3484842137658,-1.96820697150083,3.40509182215921));
#81200=CARTESIAN_POINT('Ctrl Pts',(19.3543362438441,-2.06860569736493,3.34705947457623));
#81201=CARTESIAN_POINT('Ctrl Pts',(19.3601882739223,-2.16648290600157,3.28455567343344));
#81202=CARTESIAN_POINT('Ctrl Pts',(19.3660403040006,-2.26142207469899,3.21783455138143));
#81203=CARTESIAN_POINT('Ctrl Pts',(19.3718914443791,-2.35634680954133,3.15112357311959));
#81204=CARTESIAN_POINT('Ctrl Pts',(19.3777425847576,-2.44833405448497,3.08019678641447));
#81205=CARTESIAN_POINT('Ctrl Pts',(19.3835937251362,-2.53699663910662,3.00535140260864));
#81206=CARTESIAN_POINT('Ctrl Pts',(19.3894453927037,-2.62566721224589,2.9304992752179));
#81207=CARTESIAN_POINT('Ctrl Pts',(19.3952970602712,-2.71101221369989,2.85172811551655));
#81208=CARTESIAN_POINT('Ctrl Pts',(19.4011487278387,-2.79267846176761,2.7693746603122));
#81209=CARTESIAN_POINT('Ctrl Pts',(19.4070023395229,-2.87437184205344,2.68699384457688));
#81210=CARTESIAN_POINT('Ctrl Pts',(19.4128559512072,-2.95238374777046,2.60102866013899));
#81211=CARTESIAN_POINT('Ctrl Pts',(19.4187095628915,-3.02639918266904,2.51185130673378));
#81212=CARTESIAN_POINT('Ctrl Pts',(19.4245698289913,-3.10049875869173,2.42257257605811));
#81213=CARTESIAN_POINT('Ctrl Pts',(19.4304300950912,-3.17059253165322,2.33007470618488));
#81214=CARTESIAN_POINT('Ctrl Pts',(19.4362903611911,-3.23640694306014,2.23476153065873));
#81215=CARTESIAN_POINT('Ctrl Pts',(19.4421545743625,-3.30226568251972,2.13938415874498));
#81216=CARTESIAN_POINT('Ctrl Pts',(19.4480187875338,-3.36383910216311,2.04118805481818));
#81217=CARTESIAN_POINT('Ctrl Pts',(19.4538830007052,-3.42089888225791,1.94060295716732));
#81218=CARTESIAN_POINT('Ctrl Pts',(19.4597558492795,-3.47804268627537,1.83986974197289));
#81219=CARTESIAN_POINT('Ctrl Pts',(19.4656286978538,-3.53065939829735,1.73674087877304));
#81220=CARTESIAN_POINT('Ctrl Pts',(19.4715015464281,-3.57856817516872,1.63166749543821));
#81221=CARTESIAN_POINT('Ctrl Pts',(19.4730962910408,-3.5915775798639,1.60313530873337));
#81222=CARTESIAN_POINT('Ctrl Pts',(19.4746910356535,-3.60424011848294,1.57445983134891));
#81223=CARTESIAN_POINT('Ctrl Pts',(19.4762857802662,-3.61655280561863,1.54565028521073));
#81224=CARTESIAN_POINT('Ctrl Pts',(19.482981668108,-3.66825034479546,1.42468703618701));
#81225=CARTESIAN_POINT('Ctrl Pts',(19.4896775559498,-3.71392777890546,1.30100391030865));
#81226=CARTESIAN_POINT('Ctrl Pts',(19.4963734437916,-3.75332172710987,1.1751872245753));
#81227=CARTESIAN_POINT('Ctrl Pts',(19.5028625956307,-3.791499384424,1.05325513776327));
#81228=CARTESIAN_POINT('Ctrl Pts',(19.5093517474698,-3.82377565411695,0.929319551209696));
#81229=CARTESIAN_POINT('Ctrl Pts',(19.5158408993089,-3.84995753952759,0.803937773608565));
#81230=CARTESIAN_POINT('Ctrl Pts',(19.522640155152,-3.87739060655682,0.672564243580846));
#81231=CARTESIAN_POINT('Ctrl Pts',(19.5294394109952,-3.89813228339126,0.539603086248654));
#81232=CARTESIAN_POINT('Ctrl Pts',(19.5362386668384,-3.91201753782734,0.405718848134176));
#81233=CARTESIAN_POINT('Ctrl Pts',(19.5426799998392,-3.92517185201789,0.278882473516147));
#81234=CARTESIAN_POINT('Ctrl Pts',(19.54912133284,-3.93217292772303,0.151218048903424));
#81235=CARTESIAN_POINT('Ctrl Pts',(19.5555626658407,-3.93293094111045,0.0233069186303194));
#81236=CARTESIAN_POINT('Ctrl Pts',(19.5559205886831,-3.93297306132162,0.0161993346382784));
#81237=CARTESIAN_POINT('Ctrl Pts',(19.5562785115256,-3.93299591809394,0.00909099241931421));
#81238=CARTESIAN_POINT('Ctrl Pts',(19.556636434368,-3.932999500598,0.00198199291543827));
#81239=CARTESIAN_POINT('',(20.8066365087508,-3.93233693810469,-0.00331674980543856));
#81240=CARTESIAN_POINT('Ctrl Pts',(19.5566364779651,-3.92746964905172,0.00197834150499453));
#81241=CARTESIAN_POINT('Ctrl Pts',(19.596135318312,-3.92391641524205,-0.78143951356653));
#81242=CARTESIAN_POINT('Ctrl Pts',(19.7019165649055,-3.31671944988108,-2.88457228488614));
#81243=CARTESIAN_POINT('Ctrl Pts',(19.8739802177454,0.113244265961148,-4.65028676612202));
#81244=CARTESIAN_POINT('Ctrl Pts',(20.072827436485,3.9730950150831,-2.41919558367359));
#81245=CARTESIAN_POINT('Ctrl Pts',(20.2716746552246,4.18334204600648,2.03411912066562));
#81246=CARTESIAN_POINT('Ctrl Pts',(20.4705218739644,0.550856741649847,4.61893365628057));
#81247=CARTESIAN_POINT('Ctrl Pts',(20.6488424815444,-3.16042591545766,3.13204690802899));
#81248=CARTESIAN_POINT('Ctrl Pts',(20.7608806828781,-3.92289919341051,0.902680882788246));
#81249=CARTESIAN_POINT('Ctrl Pts',(20.8066364779651,-3.93009567427408,-0.00331424972451248));
#81250=CARTESIAN_POINT('',(22.0566364779294,-3.93299995833283,-0.000572497990083963));
#81251=CARTESIAN_POINT('Ctrl Pts',(20.8066365178393,-3.93299860084824,-0.00331748787579959));
#81252=CARTESIAN_POINT('Ctrl Pts',(20.8136152576822,-3.93288195755667,-0.1416022140626));
#81253=CARTESIAN_POINT('Ctrl Pts',(20.8205939975251,-3.92546834619834,-0.279571453062378));
#81254=CARTESIAN_POINT('Ctrl Pts',(20.827572737368,-3.91088023639587,-0.416539045670631));
#81255=CARTESIAN_POINT('Ctrl Pts',(20.8346373446069,-3.89611263243974,-0.555191906791886));
#81256=CARTESIAN_POINT('Ctrl Pts',(20.8417019518459,-3.87399296404665,-0.692818279067035));
#81257=CARTESIAN_POINT('Ctrl Pts',(20.8487665590848,-3.84469752196738,-0.828727919511514));
#81258=CARTESIAN_POINT('Ctrl Pts',(20.8552498098711,-3.81781284296527,-0.953453364744746));
#81259=CARTESIAN_POINT('Ctrl Pts',(20.8617330606573,-3.78488542051725,-1.07673324297054));
#81260=CARTESIAN_POINT('Ctrl Pts',(20.8682163114436,-3.74608662368957,-1.19805008568676));
#81261=CARTESIAN_POINT('Ctrl Pts',(20.8740887575775,-3.71094316681251,-1.30793733939193));
#81262=CARTESIAN_POINT('Ctrl Pts',(20.8799612037114,-3.67090164357798,-1.41646091691581));
#81263=CARTESIAN_POINT('Ctrl Pts',(20.8858336498453,-3.62608572291032,-1.52315177513797));
#81264=CARTESIAN_POINT('Ctrl Pts',(20.8916984887901,-3.58132785695687,-1.6297044256163));
#81265=CARTESIAN_POINT('Ctrl Pts',(20.897563327735,-3.53180805149049,-1.73442870046945));
#81266=CARTESIAN_POINT('Ctrl Pts',(20.9034281666798,-3.47769977618529,-1.8368705089692));
#81267=CARTESIAN_POINT('Ctrl Pts',(20.9092869767998,-3.42364712206868,-1.93920701130059));
#81268=CARTESIAN_POINT('Ctrl Pts',(20.9151457869198,-3.3650155719174,-2.03926535085938));
#81269=CARTESIAN_POINT('Ctrl Pts',(20.9210045970398,-3.30202646323742,-2.13661185901413));
#81270=CARTESIAN_POINT('Ctrl Pts',(20.9270903859208,-3.23659706556539,-2.23772971140984));
#81271=CARTESIAN_POINT('Ctrl Pts',(20.9331761748018,-3.16646582044746,-2.33592094330405));
#81272=CARTESIAN_POINT('Ctrl Pts',(20.9392619636827,-3.09193326066032,-2.4307278152073));
#81273=CARTESIAN_POINT('Ctrl Pts',(20.945113993761,-3.02026354121814,-2.52189309827153));
#81274=CARTESIAN_POINT('Ctrl Pts',(20.9509660238393,-2.94452466351218,-2.6099288610706));
#81275=CARTESIAN_POINT('Ctrl Pts',(20.9568180539175,-2.86502720247481,-2.69445878221942));
#81276=CARTESIAN_POINT('Ctrl Pts',(20.962669194296,-2.78554182764865,-2.77897585205869));
#81277=CARTESIAN_POINT('Ctrl Pts',(20.9685203346745,-2.70229928878462,-2.85998783899913));
#81278=CARTESIAN_POINT('Ctrl Pts',(20.974371475053,-2.61564864698193,-2.93715358051662));
#81279=CARTESIAN_POINT('Ctrl Pts',(20.9802231426205,-2.52899019793825,-3.01432627468359));
#81280=CARTESIAN_POINT('Ctrl Pts',(20.986074810188,-2.43892334423997,-3.08765175960288));
#81281=CARTESIAN_POINT('Ctrl Pts',(20.9919264777555,-2.34583145895638,-3.15682811793271));
#81282=CARTESIAN_POINT('Ctrl Pts',(20.9977800894397,-2.25270864548165,-3.22602745892775));
#81283=CARTESIAN_POINT('Ctrl Pts',(21.0036337011239,-2.15655913361623,-3.29107468590123));
#81284=CARTESIAN_POINT('Ctrl Pts',(21.0094873128082,-2.05779599231784,-3.35171070559508));
#81285=CARTESIAN_POINT('Ctrl Pts',(21.015347578908,-1.95892057657606,-3.41241565662577));
#81286=CARTESIAN_POINT('Ctrl Pts',(21.0212078450079,-1.85742595348252,-3.46869917483589));
#81287=CARTESIAN_POINT('Ctrl Pts',(21.0270681111078,-1.75375063665521,-3.52034766811908));
#81288=CARTESIAN_POINT('Ctrl Pts',(21.0329323242791,-1.65000549127859,-3.57203094826832));
#81289=CARTESIAN_POINT('Ctrl Pts',(21.0387965374504,-1.5440771044176,-3.61907281993428));
#81290=CARTESIAN_POINT('Ctrl Pts',(21.0446607506217,-1.43642322460665,-3.66130814324752));
#81291=CARTESIAN_POINT('Ctrl Pts',(21.050533599196,-1.32861081804929,-3.70360566058851));
#81292=CARTESIAN_POINT('Ctrl Pts',(21.0564064477703,-1.2190682370594,-3.74108237014096));
#81293=CARTESIAN_POINT('Ctrl Pts',(21.0622792963446,-1.10826767844745,-3.77362315989669));
#81294=CARTESIAN_POINT('Ctrl Pts',(21.0638740409575,-1.07818030402943,-3.78245945943799));
#81295=CARTESIAN_POINT('Ctrl Pts',(21.0654687855704,-1.04800022150378,-3.79093209223556));
#81296=CARTESIAN_POINT('Ctrl Pts',(21.0670635301833,-1.01773698271176,-3.79903940937979));
#81297=CARTESIAN_POINT('Ctrl Pts',(21.0729359763172,-0.906296418370578,
-3.82889358341765));
#81298=CARTESIAN_POINT('Ctrl Pts',(21.0788084224511,-0.793354555957315,
-3.85389010669937));
#81299=CARTESIAN_POINT('Ctrl Pts',(21.084680868585,-0.679372827779649,-3.87387939420869));
#81300=CARTESIAN_POINT('Ctrl Pts',(21.0905457075299,-0.56553875196647,-3.89384278751889));
#81301=CARTESIAN_POINT('Ctrl Pts',(21.0964105464747,-0.450667892574487,
-3.90881177344058));
#81302=CARTESIAN_POINT('Ctrl Pts',(21.1022753854195,-0.335236031601066,
-3.91868674470369));
#81303=CARTESIAN_POINT('Ctrl Pts',(21.1081341955395,-0.219922830061613,
-3.92855156488293));
#81304=CARTESIAN_POINT('Ctrl Pts',(21.1139930056596,-0.104050183384135,
-3.93333275096322));
#81305=CARTESIAN_POINT('Ctrl Pts',(21.1198518157796,0.0118974230570147,
-3.93298200495815));
#81306=CARTESIAN_POINT('Ctrl Pts',(21.1259376046605,0.132337007136651,-3.93261767054655));
#81307=CARTESIAN_POINT('Ctrl Pts',(21.1320233935415,0.252857029019293,-3.92671564647913));
#81308=CARTESIAN_POINT('Ctrl Pts',(21.1381091824225,0.372909933016485,-3.9152812391778));
#81309=CARTESIAN_POINT('Ctrl Pts',(21.1439612125007,0.488351532933007,-3.90428603432216));
#81310=CARTESIAN_POINT('Ctrl Pts',(21.149813242579,0.603360788043665,-3.88817565361085));
#81311=CARTESIAN_POINT('Ctrl Pts',(21.1556652726573,0.717453202398772,-3.86700787461931));
#81312=CARTESIAN_POINT('Ctrl Pts',(21.1615164130358,0.831528270979573,-3.84584331382172));
#81313=CARTESIAN_POINT('Ctrl Pts',(21.1673675534143,0.94468636964673,-3.81962295893095));
#81314=CARTESIAN_POINT('Ctrl Pts',(21.1732186937928,1.05645176853335,-3.78845597318522));
#81315=CARTESIAN_POINT('Ctrl Pts',(21.1790703613603,1.16822723750603,-3.75728617928748));
#81316=CARTESIAN_POINT('Ctrl Pts',(21.1849220289277,1.27860935906109,-3.72116897957871));
#81317=CARTESIAN_POINT('Ctrl Pts',(21.1907736964952,1.38713686389532,-3.68026362110415));
#81318=CARTESIAN_POINT('Ctrl Pts',(21.1966273081795,1.4957004251418,-3.639344672522));
#81319=CARTESIAN_POINT('Ctrl Pts',(21.2024809198637,1.60240775787166,-3.5936345477074));
#81320=CARTESIAN_POINT('Ctrl Pts',(21.2083345315479,1.70681755991168,-3.5433406295722));
#81321=CARTESIAN_POINT('Ctrl Pts',(21.2141947976478,1.81134605554794,-3.49298953705399));
#81322=CARTESIAN_POINT('Ctrl Pts',(21.2200550637477,1.91357143471598,-3.43804442996549));
#81323=CARTESIAN_POINT('Ctrl Pts',(21.2259153298475,2.01307691302864,-3.37875869843217));
#81324=CARTESIAN_POINT('Ctrl Pts',(21.2317795430188,2.11264941137453,-3.3194330361155));
#81325=CARTESIAN_POINT('Ctrl Pts',(21.2376437561901,2.20949801655538,-3.25576115450926));
#81326=CARTESIAN_POINT('Ctrl Pts',(21.2435079693614,2.30323630212144,-3.18803882294272));
#81327=CARTESIAN_POINT('Ctrl Pts',(21.2493808179357,2.39711262289315,-3.12021676621148));
#81328=CARTESIAN_POINT('Ctrl Pts',(21.25525366651,2.48786916021109,-3.04833261119209));
#81329=CARTESIAN_POINT('Ctrl Pts',(21.2611265150842,2.57515375917751,-2.97272133180928));
#81330=CARTESIAN_POINT('Ctrl Pts',(21.2627212596971,2.59885548453773,-2.95218944188497));
#81331=CARTESIAN_POINT('Ctrl Pts',(21.26431600431,2.6223014184144,-2.93138292674213));
#81332=CARTESIAN_POINT('Ctrl Pts',(21.2659107489229,2.64548500895171,-2.91030892989246));
#81333=CARTESIAN_POINT('Ctrl Pts',(21.2717831950568,2.7308556604786,-2.83270659135749));
#81334=CARTESIAN_POINT('Ctrl Pts',(21.2776556411907,2.81295178012734,-2.75121476599919));
#81335=CARTESIAN_POINT('Ctrl Pts',(21.2835280873247,2.89139803447535,-2.66614073263811));
#81336=CARTESIAN_POINT('Ctrl Pts',(21.2893929262695,2.9697426692469,-2.58117690450365));
#81337=CARTESIAN_POINT('Ctrl Pts',(21.2952577652144,3.04444656349929,-2.49264039756693));
#81338=CARTESIAN_POINT('Ctrl Pts',(21.3011226041592,3.11516866651142,-2.4008775852145));
#81339=CARTESIAN_POINT('Ctrl Pts',(21.3069814142792,3.18581806997047,-2.30920910144061));
#81340=CARTESIAN_POINT('Ctrl Pts',(21.3128402243992,3.25249357282365,-2.21432123441996));
#81341=CARTESIAN_POINT('Ctrl Pts',(21.3186990345193,3.3148925801716,-2.11659542235244));
#81342=CARTESIAN_POINT('Ctrl Pts',(21.3247848234002,3.37970901513408,-2.01508357126305));
#81343=CARTESIAN_POINT('Ctrl Pts',(21.3308706122812,3.43991058973808,-1.91050976967832));
#81344=CARTESIAN_POINT('Ctrl Pts',(21.3369564011622,3.49520569882572,-1.803337495561));
#81345=CARTESIAN_POINT('Ctrl Pts',(21.3428084312404,3.54837688959339,-1.7002817728014));
#81346=CARTESIAN_POINT('Ctrl Pts',(21.3486604613187,3.59701137557048,-1.59482391438598));
#81347=CARTESIAN_POINT('Ctrl Pts',(21.354512491397,3.64089578784765,-1.48740272355311));
#81348=CARTESIAN_POINT('Ctrl Pts',(21.3603636317755,3.68477352826048,-1.37999786425063));
#81349=CARTESIAN_POINT('Ctrl Pts',(21.366214772154,3.72390247459274,-1.27063064858002));
#81350=CARTESIAN_POINT('Ctrl Pts',(21.3720659125325,3.75811722392336,-1.15976029042667));
#81351=CARTESIAN_POINT('Ctrl Pts',(21.3779175801,3.79233505601014,-1.04887994283061));
#81352=CARTESIAN_POINT('Ctrl Pts',(21.3837692476675,3.82163768901133,-0.936496578523215));
#81353=CARTESIAN_POINT('Ctrl Pts',(21.389620915235,3.84590966992567,-0.823084327862094));
#81354=CARTESIAN_POINT('Ctrl Pts',(21.3954745269192,3.87018971479168,-0.709634397915104));
#81355=CARTESIAN_POINT('Ctrl Pts',(21.4013281386035,3.8894356977365,-0.595155305896249));
#81356=CARTESIAN_POINT('Ctrl Pts',(21.4071817502877,3.90358345451057,-0.480130413191341));
#81357=CARTESIAN_POINT('Ctrl Pts',(21.4130420163876,3.91774729452678,-0.364974759601082));
#81358=CARTESIAN_POINT('Ctrl Pts',(21.4189022824875,3.92680128987833,-0.249272477396976));
#81359=CARTESIAN_POINT('Ctrl Pts',(21.4247625485874,3.93073323501185,-0.13351117995613));
#81360=CARTESIAN_POINT('Ctrl Pts',(21.4306267617587,3.93466782843266,-0.0176719136824199));
#81361=CARTESIAN_POINT('Ctrl Pts',(21.43649097493,3.93347350651945,0.0982260346514063));
#81362=CARTESIAN_POINT('Ctrl Pts',(21.4423551881013,3.92719012833042,0.213697674166369));
#81363=CARTESIAN_POINT('Ctrl Pts',(21.4482280366756,3.92089749749296,0.329339352544417));
#81364=CARTESIAN_POINT('Ctrl Pts',(21.4541008852499,3.90950089450785,0.444553059408025));
#81365=CARTESIAN_POINT('Ctrl Pts',(21.4599737338241,3.89309168866756,0.558861435087084));
#81366=CARTESIAN_POINT('Ctrl Pts',(21.4615684784369,3.88863584542845,0.589901340850946));
#81367=CARTESIAN_POINT('Ctrl Pts',(21.4631632230497,3.88381067593326,0.620874565206294));
#81368=CARTESIAN_POINT('Ctrl Pts',(21.4647579676625,3.87861864671218,0.6517717341037));
#81369=CARTESIAN_POINT('Ctrl Pts',(21.4706304137965,3.85949965318686,0.765546666205749));
#81370=CARTESIAN_POINT('Ctrl Pts',(21.4765028599304,3.83533821575921,0.878670118252889));
#81371=CARTESIAN_POINT('Ctrl Pts',(21.4823753060643,3.80618987348751,0.990660207619714));
#81372=CARTESIAN_POINT('Ctrl Pts',(21.4882401450091,3.77707929008933,1.10250522459853));
#81373=CARTESIAN_POINT('Ctrl Pts',(21.494104983954,3.74299475175835,1.21321940220833));
#81374=CARTESIAN_POINT('Ctrl Pts',(21.4999698228988,3.70404322125797,1.32232855790567));
#81375=CARTESIAN_POINT('Ctrl Pts',(21.5058286330189,3.66513173140596,1.43132555366265));
#81376=CARTESIAN_POINT('Ctrl Pts',(21.5116874431389,3.62136333892159,1.53872042229152));
#81377=CARTESIAN_POINT('Ctrl Pts',(21.5175462532589,3.57289529685836,1.64405237072527));
#81378=CARTESIAN_POINT('Ctrl Pts',(21.5236320421399,3.52254953288448,1.7534650308826));
#81379=CARTESIAN_POINT('Ctrl Pts',(21.5297178310209,3.46713272661096,1.86065125735366));
#81380=CARTESIAN_POINT('Ctrl Pts',(21.5358036199018,3.4068770859369,1.96511514200011));
#81381=CARTESIAN_POINT('Ctrl Pts',(21.5416556499801,3.34893590057752,2.06556650615375));
#81382=CARTESIAN_POINT('Ctrl Pts',(21.5475076800584,3.28652097455898,2.1635004131418));
#81383=CARTESIAN_POINT('Ctrl Pts',(21.5533597101366,3.21988606232296,2.25850010973175));
#81384=CARTESIAN_POINT('Ctrl Pts',(21.5592108505152,3.15326128077052,2.35348536326424));
#81385=CARTESIAN_POINT('Ctrl Pts',(21.5650619908937,3.08241802596525,2.44553695506596));
#81386=CARTESIAN_POINT('Ctrl Pts',(21.5709131312722,3.00765315766804,2.53426744507549));
#81387=CARTESIAN_POINT('Ctrl Pts',(21.5767647988397,2.93288155304041,2.6230059297209));
#81388=CARTESIAN_POINT('Ctrl Pts',(21.5826164664072,2.85418789888381,2.70842240160628));
#81389=CARTESIAN_POINT('Ctrl Pts',(21.5884681339747,2.7719086112616,2.79016337349872));
#81390=CARTESIAN_POINT('Ctrl Pts',(21.594321745659,2.68960198774951,2.87193150243483));
#81391=CARTESIAN_POINT('Ctrl Pts',(21.6001753573432,2.60370765510291,2.95002141207857));
#81392=CARTESIAN_POINT('Ctrl Pts',(21.6060289690274,2.51459752696156,3.02411776844071));
#81393=CARTESIAN_POINT('Ctrl Pts',(21.6118892351273,2.42538609797146,3.09829835791917));
#81394=CARTESIAN_POINT('Ctrl Pts',(21.6177495012272,2.33295189478774,3.1684760682044));
#81395=CARTESIAN_POINT('Ctrl Pts',(21.6236097673271,2.23769850246221,3.23437697433035));
#81396=CARTESIAN_POINT('Ctrl Pts',(21.6294739804984,2.14238095401548,3.30032226676547));
#81397=CARTESIAN_POINT('Ctrl Pts',(21.6353381936698,2.04424078465955,3.36198479989251));
#81398=CARTESIAN_POINT('Ctrl Pts',(21.6412024068411,1.943707525246,3.41913586397237));
#81399=CARTESIAN_POINT('Ctrl Pts',(21.6470752554154,1.84302622462333,3.47637108639622));
#81400=CARTESIAN_POINT('Ctrl Pts',(21.6529481039897,1.73994516745276,3.52908139337201));
#81401=CARTESIAN_POINT('Ctrl Pts',(21.658820952564,1.63491531725601,3.57708553230164));
#81402=CARTESIAN_POINT('Ctrl Pts',(21.6604156971767,1.60639495177096,3.59012083211882));
#81403=CARTESIAN_POINT('Ctrl Pts',(21.6620104417894,1.57773098079289,3.60280939607684));
#81404=CARTESIAN_POINT('Ctrl Pts',(21.6636051864022,1.54893262353388,3.61514823039837));
#81405=CARTESIAN_POINT('Ctrl Pts',(21.6694776325361,1.44288630088227,3.66058443336778));
#81406=CARTESIAN_POINT('Ctrl Pts',(21.67535007867,1.33466150801162,3.70142662564121));
#81407=CARTESIAN_POINT('Ctrl Pts',(21.6812225248039,1.2246936394195,3.73746096829993));
#81408=CARTESIAN_POINT('Ctrl Pts',(21.6870873637488,1.11486822362282,3.77344863193404));
#81409=CARTESIAN_POINT('Ctrl Pts',(21.6929522026936,1.00330461162231,3.80464070391446));
#81410=CARTESIAN_POINT('Ctrl Pts',(21.6988170416385,0.890459525861827,3.83087076691474));
#81411=CARTESIAN_POINT('Ctrl Pts',(21.7046758517585,0.777730440431554,3.85707386643718));
#81412=CARTESIAN_POINT('Ctrl Pts',(21.7105346618785,0.663722901638883,3.87832500962752));
#81413=CARTESIAN_POINT('Ctrl Pts',(21.7163934719985,0.548909561055544,3.89450732362668));
#81414=CARTESIAN_POINT('Ctrl Pts',(21.7224792608795,0.429648185930714,3.91131656382851));
#81415=CARTESIAN_POINT('Ctrl Pts',(21.7285650497605,0.309517742174652,3.92265614255285));
#81416=CARTESIAN_POINT('Ctrl Pts',(21.7346508386414,0.189060949322586,3.92845325254625));
#81417=CARTESIAN_POINT('Ctrl Pts',(21.7405028687197,0.0732309741642367,
3.93402769206625));
#81418=CARTESIAN_POINT('Ctrl Pts',(21.746354898798,-0.0429002909674251,
3.93447756619805));
#81419=CARTESIAN_POINT('Ctrl Pts',(21.7522069288763,-0.158845061913345,
3.92979099269996));
#81420=CARTESIAN_POINT('Ctrl Pts',(21.7580580692548,-0.27477220546626,3.92510513171415));
#81421=CARTESIAN_POINT('Ctrl Pts',(21.7639092096333,-0.390512498301815,
3.91528439248784));
#81422=CARTESIAN_POINT('Ctrl Pts',(21.7697603500118,-0.505579507274324,
3.90036900328985));
#81423=CARTESIAN_POINT('Ctrl Pts',(21.7756120175793,-0.620656883808554,
3.88545227021215));
#81424=CARTESIAN_POINT('Ctrl Pts',(21.7814636851468,-0.735060445935161,
3.86544002779491));
#81425=CARTESIAN_POINT('Ctrl Pts',(21.7873153527143,-0.848310933432702,
3.84042413806321));
#81426=CARTESIAN_POINT('Ctrl Pts',(21.7931689643985,-0.961599046472934,
3.81539993722886));
#81427=CARTESIAN_POINT('Ctrl Pts',(21.7990225760827,-1.07373291972062,3.78536887265583));
#81428=CARTESIAN_POINT('Ctrl Pts',(21.804876187767,-1.18424619389995,3.75047329709645));
#81429=CARTESIAN_POINT('Ctrl Pts',(21.8107364538669,-1.29488510013388,3.71553805206851));
#81430=CARTESIAN_POINT('Ctrl Pts',(21.8165967199668,-1.40389933571341,3.6757273828946));
#81431=CARTESIAN_POINT('Ctrl Pts',(21.8224569860666,-1.51084024994538,3.63123267488397));
#81432=CARTESIAN_POINT('Ctrl Pts',(21.8283211992379,-1.6178531922078,3.58670799830419));
#81433=CARTESIAN_POINT('Ctrl Pts',(21.8341854124092,-1.72278965919017,3.53749317604446));
#81434=CARTESIAN_POINT('Ctrl Pts',(21.8400496255805,-1.8252250064917,3.4838258675883));
#81435=CARTESIAN_POINT('Ctrl Pts',(21.8459224741548,-1.92781119594008,3.43007953082564));
#81436=CARTESIAN_POINT('Ctrl Pts',(21.8517953227291,-2.02788855911491,3.37186782934882));
#81437=CARTESIAN_POINT('Ctrl Pts',(21.8576681713034,-2.12506078412123,3.30947211255663));
#81438=CARTESIAN_POINT('Ctrl Pts',(21.8592629159162,-2.15144744817087,3.29252884695759));
#81439=CARTESIAN_POINT('Ctrl Pts',(21.8608576605291,-2.17762008388537,3.27527729550833));
#81440=CARTESIAN_POINT('Ctrl Pts',(21.8624524051419,-2.20357118795022,3.25772359472618));
#81441=CARTESIAN_POINT('Ctrl Pts',(21.8683016986376,-2.2987560990595,3.19333914910054));
#81442=CARTESIAN_POINT('Ctrl Pts',(21.8741509921333,-2.39128240582993,3.12466742122805));
#81443=CARTESIAN_POINT('Ctrl Pts',(21.880000285629,-2.48073667426204,3.05195585698275));
#81444=CARTESIAN_POINT('Ctrl Pts',(21.8858419879227,-2.57007484911417,2.97933865766768));
#81445=CARTESIAN_POINT('Ctrl Pts',(21.8916836902164,-2.6563485922422,2.90269230695721));
#81446=CARTESIAN_POINT('Ctrl Pts',(21.8975253925101,-2.73917266184636,2.82230794361522));
#81447=CARTESIAN_POINT('Ctrl Pts',(21.9033611086428,-2.82191185923516,2.74200595245112));
#81448=CARTESIAN_POINT('Ctrl Pts',(21.9091968247755,-2.90120811580661,2.6579738550509));
#81449=CARTESIAN_POINT('Ctrl Pts',(21.9150325409082,-2.9767091378659,2.5705430765785));
#81450=CARTESIAN_POINT('Ctrl Pts',(21.9209327049507,-3.05304397071259,2.48214673864408));
#81451=CARTESIAN_POINT('Ctrl Pts',(21.9268328689933,-3.12549889273747,2.39027646314334));
#81452=CARTESIAN_POINT('Ctrl Pts',(21.9327330330358,-3.19374784495553,2.29531342148342));
#81453=CARTESIAN_POINT('Ctrl Pts',(21.9385621855732,-3.2611753859737,2.20149330881303));
#81454=CARTESIAN_POINT('Ctrl Pts',(21.9443913381105,-3.32449740350828,2.10465482189322));
#81455=CARTESIAN_POINT('Ctrl Pts',(21.9502204906479,-3.38344044542388,2.00519818279137));
#81456=CARTESIAN_POINT('Ctrl Pts',(21.956048824259,-3.4423752065467,1.90575551615842));
#81457=CARTESIAN_POINT('Ctrl Pts',(21.9618771578701,-3.49693200260813,1.80369578730248));
#81458=CARTESIAN_POINT('Ctrl Pts',(21.9677054914812,-3.54688186239486,1.69944639639336));
#81459=CARTESIAN_POINT('Ctrl Pts',(21.9735344467611,-3.59683704999491,1.5951858859076));
#81460=CARTESIAN_POINT('Ctrl Pts',(21.9793634020411,-3.64218414461965,1.48873562533101));
#81461=CARTESIAN_POINT('Ctrl Pts',(21.9851923573211,-3.6827414384427,1.38054500019992));
#81462=CARTESIAN_POINT('Ctrl Pts',(21.9911460340385,-3.72416653168075,1.27003943360337));
#81463=CARTESIAN_POINT('Ctrl Pts',(21.9970997107558,-3.76059434010847,1.1577185980051));
#81464=CARTESIAN_POINT('Ctrl Pts',(22.0030533874732,-3.7918846222398,1.04407854667229));
#81465=CARTESIAN_POINT('Ctrl Pts',(22.0088910875013,-3.82256537457987,0.93265218572669));
#81466=CARTESIAN_POINT('Ctrl Pts',(22.0147287875294,-3.84830690806666,0.819957963166135));
#81467=CARTESIAN_POINT('Ctrl Pts',(22.0205664875576,-3.86902884222337,0.706473508380677));
#81468=CARTESIAN_POINT('Ctrl Pts',(22.0265781526195,-3.89036829560161,0.58960718626344));
#81469=CARTESIAN_POINT('Ctrl Pts',(22.0325898176815,-3.90638422816247,0.47190327475391));
#81470=CARTESIAN_POINT('Ctrl Pts',(22.0386014827435,-3.91704643023887,0.353887359696457));
#81471=CARTESIAN_POINT('Ctrl Pts',(22.0446131478055,-3.92770863231527,0.235871444638986));
#81472=CARTESIAN_POINT('Ctrl Pts',(22.0506248128675,-3.93301715168668,0.117544003992333));
#81473=CARTESIAN_POINT('Ctrl Pts',(22.0566364779294,-3.93299995833283,-0.000572497990078241));
#81474=CARTESIAN_POINT('',(23.3066364599429,-3.93299834994999,0.00360267826161876));
#81475=CARTESIAN_POINT('Ctrl Pts',(22.0566364779651,-3.93299995833273,-0.000572498690872157));
#81476=CARTESIAN_POINT('Ctrl Pts',(22.0581908599372,-3.93299551279697,-0.0311128164560471));
#81477=CARTESIAN_POINT('Ctrl Pts',(22.0597452419094,-3.93263534867649,-0.0616502033595227));
#81478=CARTESIAN_POINT('Ctrl Pts',(22.0612996238815,-3.93191963181071,-0.0921792220707062));
#81479=CARTESIAN_POINT('Ctrl Pts',(22.0671720700154,-3.92921565761587,-0.207517678848141));
#81480=CARTESIAN_POINT('Ctrl Pts',(22.0730445161493,-3.92142786721891,-0.322930159899214));
#81481=CARTESIAN_POINT('Ctrl Pts',(22.0789169622832,-3.90854253527997,-0.437931786819878));
#81482=CARTESIAN_POINT('Ctrl Pts',(22.0847818012281,-3.89567389504906,-0.552784440195304));
#81483=CARTESIAN_POINT('Ctrl Pts',(22.0906466401729,-3.87772089064231,-0.667226890841104));
#81484=CARTESIAN_POINT('Ctrl Pts',(22.0965114791178,-3.85472179291523,-0.780774550830383));
#81485=CARTESIAN_POINT('Ctrl Pts',(22.1023702892378,-3.83174633736018,-0.89420548827065));
#81486=CARTESIAN_POINT('Ctrl Pts',(22.1082290993578,-3.80373518764924,-1.0067430619087));
#81487=CARTESIAN_POINT('Ctrl Pts',(22.1140879094778,-3.77077830007421,-1.11790876715833));
#81488=CARTESIAN_POINT('Ctrl Pts',(22.1201736983588,-3.73654461510292,-1.23338119229143));
#81489=CARTESIAN_POINT('Ctrl Pts',(22.1262594872398,-3.69697428242109,-1.34737285134649));
#81490=CARTESIAN_POINT('Ctrl Pts',(22.1323452761207,-3.65222644159015,-1.45935979777085));
#81491=CARTESIAN_POINT('Ctrl Pts',(22.138197306199,-3.60919739217649,-1.56704525838521));
#81492=CARTESIAN_POINT('Ctrl Pts',(22.1440493362773,-3.56138140768638,-1.6728767506504));
#81493=CARTESIAN_POINT('Ctrl Pts',(22.1499013663556,-3.5089702384656,-1.77640560277282));
#81494=CARTESIAN_POINT('Ctrl Pts',(22.1557525067341,-3.45656703745475,-1.87991871512755));
#81495=CARTESIAN_POINT('Ctrl Pts',(22.1616036471126,-3.39957022744269,-1.98112951471479));
#81496=CARTESIAN_POINT('Ctrl Pts',(22.1674547874911,-3.3382184027067,-2.07961219842314));
#81497=CARTESIAN_POINT('Ctrl Pts',(22.1733064550586,-3.27686105015837,-2.17810375544204));
#81498=CARTESIAN_POINT('Ctrl Pts',(22.1791581226261,-3.21114812143522,-2.27386635708007));
#81499=CARTESIAN_POINT('Ctrl Pts',(22.1850097901936,-3.14136220340735,-2.36650216712425));
#81500=CARTESIAN_POINT('Ctrl Pts',(22.1908634018779,-3.07155310019859,-2.45916875383616));
#81501=CARTESIAN_POINT('Ctrl Pts',(22.1967170135621,-2.99766856555371,-2.54870615333636));
#81502=CARTESIAN_POINT('Ctrl Pts',(22.2025706252463,-2.92003176047537,-2.63474923243467));
#81503=CARTESIAN_POINT('Ctrl Pts',(22.2084308913462,-2.84230669748049,-2.72089012574476));
#81504=CARTESIAN_POINT('Ctrl Pts',(22.2142911574461,-2.76082112713157,-2.80352846287704));
#81505=CARTESIAN_POINT('Ctrl Pts',(22.220151423546,-2.67593546162276,-2.88233558164725));
#81506=CARTESIAN_POINT('Ctrl Pts',(22.2260156367173,-2.59099262297914,-2.96119577946206));
#81507=CARTESIAN_POINT('Ctrl Pts',(22.2318798498886,-2.50264544349439,-3.03621935382319));
#81508=CARTESIAN_POINT('Ctrl Pts',(22.23774406306,-2.41128646203427,-3.10711869712283));
#81509=CARTESIAN_POINT('Ctrl Pts',(22.2436169116343,-2.31979294903535,-3.17812244392611));
#81510=CARTESIAN_POINT('Ctrl Pts',(22.2494897602086,-2.22527911874374,-3.24498960098023));
#81511=CARTESIAN_POINT('Ctrl Pts',(22.2553626087829,-2.1281654892705,-3.30747647766058));
#81512=CARTESIAN_POINT('Ctrl Pts',(22.2569573533956,-2.10179473656521,-3.3244444973011));
#81513=CARTESIAN_POINT('Ctrl Pts',(22.2585520980084,-2.07523241450326,-3.34108979496335));
#81514=CARTESIAN_POINT('Ctrl Pts',(22.2601468426212,-2.04848722134078,-3.3574080931581));
#81515=CARTESIAN_POINT('Ctrl Pts',(22.2660192887551,-1.9500014168234,-3.41749817051523));
#81516=CARTESIAN_POINT('Ctrl Pts',(22.271891734889,-1.84870447095246,-3.47335172204802));
#81517=CARTESIAN_POINT('Ctrl Pts',(22.2777641810229,-1.74499684633191,-3.5246950231604));
#81518=CARTESIAN_POINT('Ctrl Pts',(22.2836290199677,-1.64142356496303,-3.5759718139651));
#81519=CARTESIAN_POINT('Ctrl Pts',(22.2894938589126,-1.53544618201719,-3.62274979148631));
#81520=CARTESIAN_POINT('Ctrl Pts',(22.2953586978574,-1.42749303062162,-3.66479912785499));
#81521=CARTESIAN_POINT('Ctrl Pts',(22.3012175079775,-1.31965085083926,-3.70680523915214));
#81522=CARTESIAN_POINT('Ctrl Pts',(22.3070763180975,-1.20983732525929,-3.7440922286813));
#81523=CARTESIAN_POINT('Ctrl Pts',(22.3129351282175,-1.09850361649316,-3.77647703614777));
#81524=CARTESIAN_POINT('Ctrl Pts',(22.3190209170985,-0.982856679144769,
-3.81011647780135));
#81525=CARTESIAN_POINT('Ctrl Pts',(22.3251067059794,-0.865569795360856,
-3.83846601844896));
#81526=CARTESIAN_POINT('Ctrl Pts',(22.3311924948604,-0.747169762042387,
-3.86137622444246));
#81527=CARTESIAN_POINT('Ctrl Pts',(22.3370445249387,-0.633317545049769,
-3.88340643567645));
#81528=CARTESIAN_POINT('Ctrl Pts',(22.3428965550169,-0.518436557948746,
-3.90040737478319));
#81529=CARTESIAN_POINT('Ctrl Pts',(22.3487485850952,-0.40300790882696,-3.91229774243001));
#81530=CARTESIAN_POINT('Ctrl Pts',(22.3545997254737,-0.2875968086308,-3.92418630235249));
#81531=CARTESIAN_POINT('Ctrl Pts',(22.3604508658522,-0.17163862303592,-3.93096579334788));
#81532=CARTESIAN_POINT('Ctrl Pts',(22.3663020062307,-0.0556205517840449,
-3.93260668694687));
#81533=CARTESIAN_POINT('Ctrl Pts',(22.3721536737982,0.0604079727206123,
-3.93424772839072));
#81534=CARTESIAN_POINT('Ctrl Pts',(22.3780053413657,0.17649598026796,-3.93074924621335));
#81535=CARTESIAN_POINT('Ctrl Pts',(22.3838570089332,0.292156009875148,-3.92213384089501));
#81536=CARTESIAN_POINT('Ctrl Pts',(22.3897106206175,0.407854465554346,-3.91351557325521));
#81537=CARTESIAN_POINT('Ctrl Pts',(22.3955642323017,0.523124248563739,-3.89977703279664));
#81538=CARTESIAN_POINT('Ctrl Pts',(22.4014178439859,0.637483469145844,-3.88099263418082));
#81539=CARTESIAN_POINT('Ctrl Pts',(22.4072781100858,0.751972693873832,-3.86218688136474));
#81540=CARTESIAN_POINT('Ctrl Pts',(22.4131383761857,0.865548881953724,-3.83832388825205));
#81541=CARTESIAN_POINT('Ctrl Pts',(22.4189986422856,0.97774068126266,-3.80952912578497));
#81542=CARTESIAN_POINT('Ctrl Pts',(22.4248628554569,1.09000804523644,-3.78071496915015));
#81543=CARTESIAN_POINT('Ctrl Pts',(22.4307270686282,1.20088876931135,-3.74696254906766));
#81544=CARTESIAN_POINT('Ctrl Pts',(22.4365912817995,1.3099286656199,-3.70844656035209));
#81545=CARTESIAN_POINT('Ctrl Pts',(22.4424641303738,1.41912912966684,-3.66987385455031));
#81546=CARTESIAN_POINT('Ctrl Pts',(22.4483369789481,1.52648297402847,-3.62652373448567));
#81547=CARTESIAN_POINT('Ctrl Pts',(22.4542098275224,1.63155782553067,-3.57861817772581));
#81548=CARTESIAN_POINT('Ctrl Pts',(22.4558045721352,1.6600904109113,-3.56560964743607));
#81549=CARTESIAN_POINT('Ctrl Pts',(22.457399316748,1.68845510319967,-3.55226546821775));
#81550=CARTESIAN_POINT('Ctrl Pts',(22.4589940613608,1.71664360089758,-3.53859064423923));
#81551=CARTESIAN_POINT('Ctrl Pts',(22.4648665074947,1.82044419254028,-3.48823482766493));
#81552=CARTESIAN_POINT('Ctrl Pts',(22.4707389536286,1.9222009938083,-3.43322352103325));
#81553=CARTESIAN_POINT('Ctrl Pts',(22.4766113997625,2.02146721090104,-3.37374559136459));
#81554=CARTESIAN_POINT('Ctrl Pts',(22.4824762387074,2.12060483815836,-3.31434470963238));
#81555=CARTESIAN_POINT('Ctrl Pts',(22.4883410776522,2.21725794591733,-3.25048892181649));
#81556=CARTESIAN_POINT('Ctrl Pts',(22.4942059165971,2.3110015968181,-3.18241427527972));
#81557=CARTESIAN_POINT('Ctrl Pts',(22.5000647267171,2.40464888291587,-3.11440960681443));
#81558=CARTESIAN_POINT('Ctrl Pts',(22.5059235368371,2.49539232857328,-3.04219494723135));
#81559=CARTESIAN_POINT('Ctrl Pts',(22.5117823469572,2.58283399359506,-2.96605083596519));
#81560=CARTESIAN_POINT('Ctrl Pts',(22.5178681358381,2.67366327493734,-2.88695679191847));
#81561=CARTESIAN_POINT('Ctrl Pts',(22.5239539247191,2.76092938022794,-2.80362290667319));
#81562=CARTESIAN_POINT('Ctrl Pts',(22.5300397136001,2.84422176007164,-2.71641152617474));
#81563=CARTESIAN_POINT('Ctrl Pts',(22.5358917436784,2.92431482962595,-2.63254998713243));
#81564=CARTESIAN_POINT('Ctrl Pts',(22.5417437737566,3.00073349716659,-2.54510365856938));
#81565=CARTESIAN_POINT('Ctrl Pts',(22.5475958038349,3.07314923290107,-2.45443329351596));
#81566=CARTESIAN_POINT('Ctrl Pts',(22.5534469442134,3.14555395907795,-2.36377671332015));
#81567=CARTESIAN_POINT('Ctrl Pts',(22.5592980845919,3.21395670560722,-2.26989739412847));
#81568=CARTESIAN_POINT('Ctrl Pts',(22.5651492249705,3.2780691989884,-2.1731892063609));
#81569=CARTESIAN_POINT('Ctrl Pts',(22.571000892538,3.3421874689188,-2.07647230516516));
#81570=CARTESIAN_POINT('Ctrl Pts',(22.5768525601055,3.40201448885485,-1.97692637325704));
#81571=CARTESIAN_POINT('Ctrl Pts',(22.582704227673,3.45730569537737,-1.87497368747169));
#81572=CARTESIAN_POINT('Ctrl Pts',(22.5885578393572,3.51261527146017,-1.77298712964547));
#81573=CARTESIAN_POINT('Ctrl Pts',(22.5944114510415,3.56338584070317,-1.66859259114971));
#81574=CARTESIAN_POINT('Ctrl Pts',(22.6002650627257,3.60941943865695,-1.56223567871347));
#81575=CARTESIAN_POINT('Ctrl Pts',(22.6061253288256,3.65550536783994,-1.4557578591961));
#81576=CARTESIAN_POINT('Ctrl Pts',(22.6119855949255,3.69684341314009,-1.34731359263554));
#81577=CARTESIAN_POINT('Ctrl Pts',(22.6178458610254,3.73328425691335,-1.23736722806243));
#81578=CARTESIAN_POINT('Ctrl Pts',(22.6237100741968,3.76974964472785,-1.12734681119453));
#81579=CARTESIAN_POINT('Ctrl Pts',(22.6295742873681,3.8013111509184,-1.0158226785602));
#81580=CARTESIAN_POINT('Ctrl Pts',(22.6354385005394,3.82787014628981,-0.903271356317258));
#81581=CARTESIAN_POINT('Ctrl Pts',(22.6413113491137,3.85446825136294,-0.790554295552259));
#81582=CARTESIAN_POINT('Ctrl Pts',(22.647184197688,3.87604906679985,-0.676807430918695));
#81583=CARTESIAN_POINT('Ctrl Pts',(22.6530570462623,3.89256553350679,-0.56251450412859));
#81584=CARTESIAN_POINT('Ctrl Pts',(22.654651790875,3.8970505029333,-0.531478793439604));
#81585=CARTESIAN_POINT('Ctrl Pts',(22.6562465354877,3.90116233997505,-0.500402827103983));
#81586=CARTESIAN_POINT('Ctrl Pts',(22.6578412801005,3.90490076547796,-0.469296294221111));
#81587=CARTESIAN_POINT('Ctrl Pts',(22.6637137262344,3.91866704643364,-0.354750405613924));
#81588=CARTESIAN_POINT('Ctrl Pts',(22.6695861723683,3.92741198927103,-0.239406500546002));
#81589=CARTESIAN_POINT('Ctrl Pts',(22.6754586185022,3.93105288462848,-0.12374254827698));
#81590=CARTESIAN_POINT('Ctrl Pts',(22.681323457447,3.93468906355624,-0.00822842753193724));
#81591=CARTESIAN_POINT('Ctrl Pts',(22.6871882963919,3.93323433064254,0.107604506597884));
#81592=CARTESIAN_POINT('Ctrl Pts',(22.6930531353367,3.92665748305163,0.223271159791434));
#81593=CARTESIAN_POINT('Ctrl Pts',(22.6989119454567,3.92008739620257,0.338818912193898));
#81594=CARTESIAN_POINT('Ctrl Pts',(22.7047707555767,3.9084056910377,0.454200313437066));
#81595=CARTESIAN_POINT('Ctrl Pts',(22.7106295656967,3.89163318949212,0.568928922136524));
#81596=CARTESIAN_POINT('Ctrl Pts',(22.7167153545777,3.87421089702634,0.688102282742312));
#81597=CARTESIAN_POINT('Ctrl Pts',(22.7228011434587,3.85129536657459,0.80657079343946));
#81598=CARTESIAN_POINT('Ctrl Pts',(22.7288869323396,3.82296941851443,0.923793172254195));
#81599=CARTESIAN_POINT('Ctrl Pts',(22.7347389624179,3.79573148711634,1.03651296915895));
#81600=CARTESIAN_POINT('Ctrl Pts',(22.7405909924961,3.7634912120264,1.14808015873495));
#81601=CARTESIAN_POINT('Ctrl Pts',(22.7464430225744,3.72637442248686,1.25802331593485));
#81602=CARTESIAN_POINT('Ctrl Pts',(22.7522941629529,3.68926327591191,1.3679497581831));
#81603=CARTESIAN_POINT('Ctrl Pts',(22.7581453033314,3.64727722119318,1.47625226745097));
#81604=CARTESIAN_POINT('Ctrl Pts',(22.7639964437099,3.60059171320558,1.58247537573111));
#81605=CARTESIAN_POINT('Ctrl Pts',(22.7698481112774,3.55390199884383,1.68870805473579));
#81606=CARTESIAN_POINT('Ctrl Pts',(22.7756997788449,3.50251215581756,1.79286058186567));
#81607=CARTESIAN_POINT('Ctrl Pts',(22.7815514464124,3.44664516921986,1.89449889878391));
#81608=CARTESIAN_POINT('Ctrl Pts',(22.7874050580966,3.3907596217688,1.99617098329925));
#81609=CARTESIAN_POINT('Ctrl Pts',(22.7932586697808,3.3303941720394,2.09532683460348));
#81610=CARTESIAN_POINT('Ctrl Pts',(22.799112281465,3.26581662697953,2.19155897911601));
#81611=CARTESIAN_POINT('Ctrl Pts',(22.8049725475649,3.20116566983665,2.28790052082187));
#81612=CARTESIAN_POINT('Ctrl Pts',(22.8108328136648,3.1322932904819,2.38131137833333));
#81613=CARTESIAN_POINT('Ctrl Pts',(22.8166930797647,3.05950936588006,2.47141486604175));
#81614=CARTESIAN_POINT('Ctrl Pts',(22.822557292936,2.98667641904217,2.56157904125045));
#81615=CARTESIAN_POINT('Ctrl Pts',(22.8284215061072,2.90992695409135,2.64843110203499));
#81616=CARTESIAN_POINT('Ctrl Pts',(22.8342857192785,2.82960849926366,2.73163041806443));
#81617=CARTESIAN_POINT('Ctrl Pts',(22.8401585678528,2.74917177072991,2.81495225003954));
#81618=CARTESIAN_POINT('Ctrl Pts',(22.8460314164271,2.66515586212278,2.894610318744));
#81619=CARTESIAN_POINT('Ctrl Pts',(22.8519042650014,2.57794225594872,2.97030347355182));
#81620=CARTESIAN_POINT('Ctrl Pts',(22.8534990096143,2.55425980834995,2.99085759636546));
#81621=CARTESIAN_POINT('Ctrl Pts',(22.8550937542271,2.53034174084131,3.01111960353115));
#81622=CARTESIAN_POINT('Ctrl Pts',(22.85668849884,2.50619605303813,3.03108402122675));
#81623=CARTESIAN_POINT('Ctrl Pts',(22.8625609449739,2.41728259953259,3.10460047430989));
#81624=CARTESIAN_POINT('Ctrl Pts',(22.8684333911079,2.32498275853158,3.1743244286784));
#81625=CARTESIAN_POINT('Ctrl Pts',(22.8743058372418,2.22965388023827,3.23992786560726));
#81626=CARTESIAN_POINT('Ctrl Pts',(22.8801706761866,2.13444849133673,3.30544631959424));
#81627=CARTESIAN_POINT('Ctrl Pts',(22.8860355151315,2.03622220561441,3.36685463882064));
#81628=CARTESIAN_POINT('Ctrl Pts',(22.8919003540763,1.93536621704558,3.42386427971651));
#81629=CARTESIAN_POINT('Ctrl Pts',(22.8977591641963,1.83461390448438,3.48081531693353));
#81630=CARTESIAN_POINT('Ctrl Pts',(22.9036179743163,1.731237623639,3.53337646748249));
#81631=CARTESIAN_POINT('Ctrl Pts',(22.9094767844364,1.62565783197171,3.58130222312346));
#81632=CARTESIAN_POINT('Ctrl Pts',(22.9155625733173,1.51598772677603,3.63108469171641));
#81633=CARTESIAN_POINT('Ctrl Pts',(22.9216483621983,1.40394029758123,3.67586507998539));
#81634=CARTESIAN_POINT('Ctrl Pts',(22.9277341510793,1.29001565743486,3.71542038046476));
#81635=CARTESIAN_POINT('Ctrl Pts',(22.9335861811576,1.18046693107724,3.75345633811747));
#81636=CARTESIAN_POINT('Ctrl Pts',(22.9394382112358,1.06918296982486,3.78666105308058));
#81637=CARTESIAN_POINT('Ctrl Pts',(22.9452902413141,0.956628377789582,3.8148854696842));
#81638=CARTESIAN_POINT('Ctrl Pts',(22.9511413816926,0.844090897729359,3.84310559525444));
#81639=CARTESIAN_POINT('Ctrl Pts',(22.9569925220711,0.730283571819675,3.86634682744824));
#81640=CARTESIAN_POINT('Ctrl Pts',(22.9628436624496,0.615684414055787,3.88451048425523));
#81641=CARTESIAN_POINT('Ctrl Pts',(22.9686953300171,0.501074930883504,3.90267577761154));
#81642=CARTESIAN_POINT('Ctrl Pts',(22.9745469975846,0.385673882316584,3.91576252141985));
#81643=CARTESIAN_POINT('Ctrl Pts',(22.9803986651521,0.269966972420246,3.92372359294105));
#81644=CARTESIAN_POINT('Ctrl Pts',(22.9862522768364,0.154221620876628,3.93168730939248));
#81645=CARTESIAN_POINT('Ctrl Pts',(22.9921058885206,0.0381706181077041,
3.9345219390514));
#81646=CARTESIAN_POINT('Ctrl Pts',(22.9979595002049,-0.0776984595194039,
3.93223243837242));
#81647=CARTESIAN_POINT('Ctrl Pts',(23.0038197663047,-0.193699257705575,
3.92994033497738));
#81648=CARTESIAN_POINT('Ctrl Pts',(23.0096800324046,-0.30951730443686,3.92251248263557));
#81649=CARTESIAN_POINT('Ctrl Pts',(23.0155402985045,-0.424668174773692,
3.91000587484653));
#81650=CARTESIAN_POINT('Ctrl Pts',(23.0214045116758,-0.539896602801737,
3.89749084346831));
#81651=CARTESIAN_POINT('Ctrl Pts',(23.0272687248471,-0.654456552097231,
3.87989030795856));
#81652=CARTESIAN_POINT('Ctrl Pts',(23.0331329380184,-0.767873569313706,
3.85731242985961));
#81653=CARTESIAN_POINT('Ctrl Pts',(23.0390057865927,-0.881457599839678,
3.83470130449111));
#81654=CARTESIAN_POINT('Ctrl Pts',(23.044878635167,-0.993894939356715,3.80709830662511));
#81655=CARTESIAN_POINT('Ctrl Pts',(23.0507514837413,-1.10472598577643,3.77466150751962));
#81656=CARTESIAN_POINT('Ctrl Pts',(23.0523462283541,-1.13482163901424,3.76585344615452));
#81657=CARTESIAN_POINT('Ctrl Pts',(23.0539409729669,-1.16479896406286,3.75668922929904));
#81658=CARTESIAN_POINT('Ctrl Pts',(23.0555357175798,-1.19464903082042,3.74717262654923));
#81659=CARTESIAN_POINT('Ctrl Pts',(23.0614081637137,-1.30456814120325,3.71212893580567));
#81660=CARTESIAN_POINT('Ctrl Pts',(23.0672806098476,-1.41312802225318,3.67218594282703));
#81661=CARTESIAN_POINT('Ctrl Pts',(23.0731530559815,-1.5198595187809,3.62746689070639));
#81662=CARTESIAN_POINT('Ctrl Pts',(23.0790178949264,-1.62645275492183,3.58280576781606));
#81663=CARTESIAN_POINT('Ctrl Pts',(23.0848827338713,-1.73122193890643,3.53338104764182));
#81664=CARTESIAN_POINT('Ctrl Pts',(23.0907475728161,-1.83371282272411,3.47936578757928));
#81665=CARTESIAN_POINT('Ctrl Pts',(23.0966063829362,-1.93609834992588,3.42540605308931));
#81666=CARTESIAN_POINT('Ctrl Pts',(23.1024651930562,-2.03620987184902,3.36686535641789));
#81667=CARTESIAN_POINT('Ctrl Pts',(23.1083240031762,-2.13361351911859,3.30396464131116));
#81668=CARTESIAN_POINT('Ctrl Pts',(23.1144097920572,-2.23479072428027,3.23862706170743));
#81669=CARTESIAN_POINT('Ctrl Pts',(23.1204955809382,-2.33304557831242,3.16858497991537));
#81670=CARTESIAN_POINT('Ctrl Pts',(23.1265813698191,-2.42792006910148,3.09413851306859));
#81671=CARTESIAN_POINT('Ctrl Pts',(23.1324333998974,-2.51915037377007,3.02255157968484));
#81672=CARTESIAN_POINT('Ctrl Pts',(23.1382854299757,-2.60725485329683,2.94689264884913));
#81673=CARTESIAN_POINT('Ctrl Pts',(23.144137460054,-2.69185690452306,2.867471953755));
#81674=CARTESIAN_POINT('Ctrl Pts',(23.1499886004325,-2.77644609347362,2.78806333320114));
#81675=CARTESIAN_POINT('Ctrl Pts',(23.155839740811,-2.85753361158639,2.70489436837059));
#81676=CARTESIAN_POINT('Ctrl Pts',(23.1616908811895,-2.93477797961284,2.61831381052378));
#81677=CARTESIAN_POINT('Ctrl Pts',(23.1675425487571,-3.01202930737322,2.53172545175037));
#81678=CARTESIAN_POINT('Ctrl Pts',(23.1733942163246,-3.0854365214968,2.44172519736995));
#81679=CARTESIAN_POINT('Ctrl Pts',(23.1792458838921,-3.15469735675409,2.34869614622427));
#81680=CARTESIAN_POINT('Ctrl Pts',(23.1850994955763,-3.22398120274239,2.25563618776331));
#81681=CARTESIAN_POINT('Ctrl Pts',(23.1909531072606,-3.28911568394661,2.15954576302053));
#81682=CARTESIAN_POINT('Ctrl Pts',(23.1968067189448,-3.34984133224644,2.06083770558804));
#81683=CARTESIAN_POINT('Ctrl Pts',(23.2026669850447,-3.4106360137734,1.96201743633174));
#81684=CARTESIAN_POINT('Ctrl Pts',(23.2085272511446,-3.46701164192267,1.86057394718685));
#81685=CARTESIAN_POINT('Ctrl Pts',(23.2143875172445,-3.51875422660916,1.75694555769955));
#81686=CARTESIAN_POINT('Ctrl Pts',(23.2202517304159,-3.57053166153517,1.65324737127));
#81687=CARTESIAN_POINT('Ctrl Pts',(23.2261159435872,-3.61766967175745,1.54736173095373));
#81688=CARTESIAN_POINT('Ctrl Pts',(23.2319801567585,-3.66000270194713,1.43974623518858));
#81689=CARTESIAN_POINT('Ctrl Pts',(23.2378530053328,-3.7023980700438,1.33197226919968));
#81690=CARTESIAN_POINT('Ctrl Pts',(23.2437258539071,-3.73997420292759,1.22246375333706));
#81691=CARTESIAN_POINT('Ctrl Pts',(23.2495987024814,-3.77261555999464,1.11169277972213));
#81692=CARTESIAN_POINT('Ctrl Pts',(23.2511934470941,-3.78147916811835,1.08161343897699));
#81693=CARTESIAN_POINT('Ctrl Pts',(23.2527881917068,-3.78997919380532,1.051441060039));
#81694=CARTESIAN_POINT('Ctrl Pts',(23.2543829363194,-3.79811397947583,1.02118519324866));
#81695=CARTESIAN_POINT('Ctrl Pts',(23.2619216566848,-3.83656896086636,0.8781588319525));
#81696=CARTESIAN_POINT('Ctrl Pts',(23.2694603770502,-3.866962272519,0.73287961600431));
#81697=CARTESIAN_POINT('Ctrl Pts',(23.2769990974156,-3.88907771444612,0.586142927107849));
#81698=CARTESIAN_POINT('Ctrl Pts',(23.2843940960392,-3.9107715370956,0.442203696068143));
#81699=CARTESIAN_POINT('Ctrl Pts',(23.2917890946628,-3.92450013026313,0.296861841860589));
#81700=CARTESIAN_POINT('Ctrl Pts',(23.2991840932864,-3.9301044830118,0.150889869144963));
#81701=CARTESIAN_POINT('Ctrl Pts',(23.3016682155052,-3.93198709285311,0.101855076954787));
#81702=CARTESIAN_POINT('Ctrl Pts',(23.3041523377241,-3.93295333092603,0.0527493780525428));
#81703=CARTESIAN_POINT('Ctrl Pts',(23.3066364599429,-3.93299834994999,0.00360267826161876));
#81704=CARTESIAN_POINT('',(24.5566365102202,-3.9306426375169,-0.00105404585137062));
#81705=CARTESIAN_POINT('Ctrl Pts',(23.3066364779651,-3.93182490893431,0.00360124692383467));
#81706=CARTESIAN_POINT('Ctrl Pts',(23.3555010369964,-3.92319230971691,-0.962871716430977));
#81707=CARTESIAN_POINT('Ctrl Pts',(23.4706480022741,-3.07602472218424,-3.25384824264235));
#81708=CARTESIAN_POINT('Ctrl Pts',(23.6520773737987,0.766703506199793,-4.5880450089923));
#81709=CARTESIAN_POINT('Ctrl Pts',(23.8509245925382,4.27406879625159,-1.83584509037353));
#81710=CARTESIAN_POINT('Ctrl Pts',(24.049771811278,3.85536201618789,2.60272453307588));
#81711=CARTESIAN_POINT('Ctrl Pts',(24.2486190300175,-0.104801360273113,
4.65048470009646));
#81712=CARTESIAN_POINT('Ctrl Pts',(24.4175739189133,-3.38784425822317,2.76074661215668));
#81713=CARTESIAN_POINT('Ctrl Pts',(24.5202464015625,-3.9250314248909,0.721034683795631));
#81714=CARTESIAN_POINT('Ctrl Pts',(24.5566364779651,-3.92675474403147,-0.00105236284854396));
#81715=CARTESIAN_POINT('',(25.8066364779651,-3.9335827204154,-0.00321703522350915));
#81716=CARTESIAN_POINT('Ctrl Pts',(24.5566365297764,-3.932999858484,-0.00105506625215207));
#81717=CARTESIAN_POINT('Ctrl Pts',(24.5629066911867,-3.93296642890169,-0.125671451479569));
#81718=CARTESIAN_POINT('Ctrl Pts',(24.569176852597,-3.92700610699965,-0.250124843395846));
#81719=CARTESIAN_POINT('Ctrl Pts',(24.5754470140074,-3.91519047823295,-0.373861631026793));
#81720=CARTESIAN_POINT('Ctrl Pts',(24.5817404834431,-3.9033309273154,-0.498058384518136));
#81721=CARTESIAN_POINT('Ctrl Pts',(24.5880339528788,-3.88557254366928,-0.621532888384749));
#81722=CARTESIAN_POINT('Ctrl Pts',(24.5943274223145,-3.86203853726118,-0.743738755686087));
#81723=CARTESIAN_POINT('Ctrl Pts',(24.6006327607509,-3.83846014752159,-0.866175093882362));
#81724=CARTESIAN_POINT('Ctrl Pts',(24.6069380991874,-3.80908445827578,-0.987337713059643));
#81725=CARTESIAN_POINT('Ctrl Pts',(24.6132434376239,-3.77408465406791,-1.10669509076761));
#81726=CARTESIAN_POINT('Ctrl Pts',(24.6195683362665,-3.7389762746595,-1.22642273486743));
#81727=CARTESIAN_POINT('Ctrl Pts',(24.6258932349091,-3.69820897668527,-1.34433363505084));
#81728=CARTESIAN_POINT('Ctrl Pts',(24.6322181335517,-3.65200505726233,-1.45991371722112));
#81729=CARTESIAN_POINT('Ctrl Pts',(24.6369165782001,-3.61768252180174,-1.54577226598434));
#81730=CARTESIAN_POINT('Ctrl Pts',(24.6416150228484,-3.58036092298856,-1.63034505658126));
#81731=CARTESIAN_POINT('Ctrl Pts',(24.6463134674968,-3.54014749293069,-1.71343068966812));
#81732=CARTESIAN_POINT('Ctrl Pts',(24.6521859136307,-3.48988592350725,-1.81727694972292));
#81733=CARTESIAN_POINT('Ctrl Pts',(24.6580583597647,-3.43496701066595,-1.91908364632974));
#81734=CARTESIAN_POINT('Ctrl Pts',(24.6639308058986,-3.37557921576622,-2.01840381442542));
#81735=CARTESIAN_POINT('Ctrl Pts',(24.6697956448435,-3.31626835204206,-2.11759532279731));
#81736=CARTESIAN_POINT('Ctrl Pts',(24.6756604837883,-3.25250032871324,-2.21430635669629));
#81737=CARTESIAN_POINT('Ctrl Pts',(24.6815253227332,-3.18451080730261,-2.30811176466238));
#81738=CARTESIAN_POINT('Ctrl Pts',(24.6873841328532,-3.11659117645802,-2.40182074434181));
#81739=CARTESIAN_POINT('Ctrl Pts',(24.6932429429733,-3.04445892022942,-2.49262970645418));
#81740=CARTESIAN_POINT('Ctrl Pts',(24.6991017530933,-2.96839421670032,-2.58014045630468));
#81741=CARTESIAN_POINT('Ctrl Pts',(24.7051875419743,-2.88938265676124,-2.67104149892138));
#81742=CARTESIAN_POINT('Ctrl Pts',(24.7112733308552,-2.80612802284882,-2.75838321572819));
#81743=CARTESIAN_POINT('Ctrl Pts',(24.7173591197362,-2.71899228807735,-2.84175472857457));
#81744=CARTESIAN_POINT('Ctrl Pts',(24.7232111498145,-2.63520348916414,-2.92192389158554));
#81745=CARTESIAN_POINT('Ctrl Pts',(24.7290631798928,-2.54782656671861,-2.99842190823836));
#81746=CARTESIAN_POINT('Ctrl Pts',(24.7349152099711,-2.45722197539512,-3.07091992139738));
#81747=CARTESIAN_POINT('Ctrl Pts',(24.7407663503496,-2.36663115892949,-3.14340691248995));
#81748=CARTESIAN_POINT('Ctrl Pts',(24.7466174907281,-2.27281397194419,-3.21189485106909));
#81749=CARTESIAN_POINT('Ctrl Pts',(24.7524686311066,-2.17616402301271,-3.27609510621184));
#81750=CARTESIAN_POINT('Ctrl Pts',(24.7583202986742,-2.07950536590031,-3.3403011458112));
#81751=CARTESIAN_POINT('Ctrl Pts',(24.7641719662417,-1.9800137838004,-3.40021850527551));
#81752=CARTESIAN_POINT('Ctrl Pts',(24.7700236338092,-1.87811133136837,-3.45560223795878));
#81753=CARTESIAN_POINT('Ctrl Pts',(24.7758772454935,-1.77617502358462,-3.51100437094258));
#81754=CARTESIAN_POINT('Ctrl Pts',(24.7817308571777,-1.67182661577805,-3.56186968483403));
#81755=CARTESIAN_POINT('Ctrl Pts',(24.787584468862,-1.56551153478921,-3.60799981075968));
#81756=CARTESIAN_POINT('Ctrl Pts',(24.7934447349619,-1.45907559427354,-3.654182377648));
#81757=CARTESIAN_POINT('Ctrl Pts',(24.7993050010618,-1.35066889756852,-3.6956188476788));
#81758=CARTESIAN_POINT('Ctrl Pts',(24.8051652671617,-1.24075565796832,-3.73215948175042));
#81759=CARTESIAN_POINT('Ctrl Pts',(24.811029480333,-1.13076838838416,-3.76872472707511));
#81760=CARTESIAN_POINT('Ctrl Pts',(24.8168936935043,-1.01927295208768,-3.80038745781482));
#81761=CARTESIAN_POINT('Ctrl Pts',(24.8227579066756,-0.90674578550836,-3.82704861224192));
#81762=CARTESIAN_POINT('Ctrl Pts',(24.8286307552499,-0.794052915977578,
-3.85374902680604));
#81763=CARTESIAN_POINT('Ctrl Pts',(24.8345036038242,-0.680325688489406,
-3.87543308861966));
#81764=CARTESIAN_POINT('Ctrl Pts',(24.8403764523985,-0.566047801838025,
-3.89205329948529));
#81765=CARTESIAN_POINT('Ctrl Pts',(24.8419711970112,-0.535016175229567,
-3.89656644015361));
#81766=CARTESIAN_POINT('Ctrl Pts',(24.8435659416239,-0.50394395427505,-3.90070648513353));
#81767=CARTESIAN_POINT('Ctrl Pts',(24.8451606862366,-0.472840827816458,
-3.9044731464757));
#81768=CARTESIAN_POINT('Ctrl Pts',(24.8510331323705,-0.358307482933332,
-3.91834340235286));
#81769=CARTESIAN_POINT('Ctrl Pts',(24.8569055785044,-0.242971563730075,
-3.92719304659092));
#81770=CARTESIAN_POINT('Ctrl Pts',(24.8627780246383,-0.127310964188841,
-3.9309389359792));
#81771=CARTESIAN_POINT('Ctrl Pts',(24.8686428635831,-0.0118001918284861,
-3.93467997292811));
#81772=CARTESIAN_POINT('Ctrl Pts',(24.874507702528,0.104034015129978,-3.93333038954029));
#81773=CARTESIAN_POINT('Ctrl Pts',(24.8803725414728,0.219706590890167,-3.92685854264187));
#81774=CARTESIAN_POINT('Ctrl Pts',(24.8862313515928,0.33526025977114,-3.92039334854868));
#81775=CARTESIAN_POINT('Ctrl Pts',(24.8920901617129,0.450652217702628,-3.90881638723821));
#81776=CARTESIAN_POINT('Ctrl Pts',(24.8979489718329,0.565396004599239,-3.89214803906316));
#81777=CARTESIAN_POINT('Ctrl Pts',(24.9040347607139,0.684585131427196,-3.87483393501988));
#81778=CARTESIAN_POINT('Ctrl Pts',(24.9101205495948,0.803074395198658,-3.85202595541681));
#81779=CARTESIAN_POINT('Ctrl Pts',(24.9162063384758,0.920322438981543,-3.82380642924129));
#81780=CARTESIAN_POINT('Ctrl Pts',(24.9220583685541,1.03306691504787,-3.79667083199935));
#81781=CARTESIAN_POINT('Ctrl Pts',(24.9279103986323,1.14466332520609,-3.76453184683155));
#81782=CARTESIAN_POINT('Ctrl Pts',(24.9337624287106,1.25464013037985,-3.7275148749858));
#81783=CARTESIAN_POINT('Ctrl Pts',(24.9396135690891,1.36460021548638,-3.69050353092909));
#81784=CARTESIAN_POINT('Ctrl Pts',(24.9454647094676,1.47294079354598,-3.6486158065898));
#81785=CARTESIAN_POINT('Ctrl Pts',(24.9513158498461,1.57920623746743,-3.60202674331326));
#81786=CARTESIAN_POINT('Ctrl Pts',(24.9571675174136,1.68548125592786,-3.55543348235227));
#81787=CARTESIAN_POINT('Ctrl Pts',(24.9630191849811,1.78968038997646,-3.50413820637703));
#81788=CARTESIAN_POINT('Ctrl Pts',(24.9688708525486,1.89136937903747,-3.44836350636637));
#81789=CARTESIAN_POINT('Ctrl Pts',(24.9747244642329,1.9930921525307,-3.39257027616293));
#81790=CARTESIAN_POINT('Ctrl Pts',(24.9805780759171,2.09230276054195,-3.33229486138188));
#81791=CARTESIAN_POINT('Ctrl Pts',(24.9864316876013,2.1885934865531,-3.26780469897106));
#81792=CARTESIAN_POINT('Ctrl Pts',(24.9922919537012,2.28499367635317,-3.20324122381437));
#81793=CARTESIAN_POINT('Ctrl Pts',(24.9981522198011,2.37846701521994,-3.13445366781653));
#81794=CARTESIAN_POINT('Ctrl Pts',(25.004012485901,2.46863653640493,-3.06175156587315));
#81795=CARTESIAN_POINT('Ctrl Pts',(25.0098766990723,2.55886678956589,-2.98900049680374));
#81796=CARTESIAN_POINT('Ctrl Pts',(25.0157409122436,2.64578848494008,-2.91232990461799));
#81797=CARTESIAN_POINT('Ctrl Pts',(25.0216051254149,2.72906067686341,-2.83208700819693));
#81798=CARTESIAN_POINT('Ctrl Pts',(25.0274779739892,2.81245549204637,-2.75172594933419));
#81799=CARTESIAN_POINT('Ctrl Pts',(25.0333508225635,2.89218979451776,-2.66778238604164));
#81800=CARTESIAN_POINT('Ctrl Pts',(25.0392236711378,2.9679620874797,-2.58063752729497));
#81801=CARTESIAN_POINT('Ctrl Pts',(25.0408184157506,2.98853769988835,-2.55697374774065));
#81802=CARTESIAN_POINT('Ctrl Pts',(25.0424131603633,3.00882141065661,-2.5330740832016));
#81803=CARTESIAN_POINT('Ctrl Pts',(25.0440079049761,3.02880773870287,-2.50894652832092));
#81804=CARTESIAN_POINT('Ctrl Pts',(25.04988035111,3.10240487389666,-2.42009984701261));
#81805=CARTESIAN_POINT('Ctrl Pts',(25.055752797244,3.17221258597784,-2.32786333691163));
#81806=CARTESIAN_POINT('Ctrl Pts',(25.0616252433779,3.23790253196703,-2.23259405031042));
#81807=CARTESIAN_POINT('Ctrl Pts',(25.0674900823227,3.30350738295017,-2.13744817590568));
#81808=CARTESIAN_POINT('Ctrl Pts',(25.0733549212676,3.36500484312648,-2.0392776748939));
#81809=CARTESIAN_POINT('Ctrl Pts',(25.0792197602124,3.42210601393322,-1.93847347915882));
#81810=CARTESIAN_POINT('Ctrl Pts',(25.0850785703324,3.47914848697196,-1.83777290619033));
#81811=CARTESIAN_POINT('Ctrl Pts',(25.0909373804525,3.53180345709436,-1.73444438103925));
#81812=CARTESIAN_POINT('Ctrl Pts',(25.0967961905725,3.57982503448564,-1.62890813813115));
#81813=CARTESIAN_POINT('Ctrl Pts',(25.1028819794535,3.62970703710172,-1.51928326883669));
#81814=CARTESIAN_POINT('Ctrl Pts',(25.1089677683344,3.67458911950307,-1.40727653581594));
#81815=CARTESIAN_POINT('Ctrl Pts',(25.1150535572154,3.71424782033151,-1.29338784947233));
#81816=CARTESIAN_POINT('Ctrl Pts',(25.1209055872937,3.7523832066639,-1.18387369591013));
#81817=CARTESIAN_POINT('Ctrl Pts',(25.126757617372,3.7856889274804,-1.07261992254162));
#81818=CARTESIAN_POINT('Ctrl Pts',(25.1326096474502,3.81401550542179,-0.960090997979949));
#81819=CARTESIAN_POINT('Ctrl Pts',(25.1384607878287,3.84233777679793,-0.847579181491054));
#81820=CARTESIAN_POINT('Ctrl Pts',(25.1443119282073,3.86568230956893,-0.733793000017495));
#81821=CARTESIAN_POINT('Ctrl Pts',(25.1501630685858,3.88394998784131,-0.619210377777634));
#81822=CARTESIAN_POINT('Ctrl Pts',(25.1560147361533,3.90221931203536,-0.504617431619288));
#81823=CARTESIAN_POINT('Ctrl Pts',(25.1618664037208,3.91541080732815,-0.389228310269791));
#81824=CARTESIAN_POINT('Ctrl Pts',(25.1677180712883,3.92347691009548,-0.273528674817936));
#81825=CARTESIAN_POINT('Ctrl Pts',(25.1735716829725,3.93154569268787,-0.157790600135666));
#81826=CARTESIAN_POINT('Ctrl Pts',(25.1794252946568,3.93448566806009,-0.0417422183555004));
#81827=CARTESIAN_POINT('Ctrl Pts',(25.185278906341,3.93230135006062,0.0741288898570414));
#81828=CARTESIAN_POINT('Ctrl Pts',(25.1911391724409,3.93011454891729,0.190131720937063));
#81829=CARTESIAN_POINT('Ctrl Pts',(25.1969994385408,3.92279183504807,0.305956462683684));
#81830=CARTESIAN_POINT('Ctrl Pts',(25.2028597046407,3.91038976218568,0.421118638620297));
#81831=CARTESIAN_POINT('Ctrl Pts',(25.208723917812,3.89797933614163,0.536358379862815));
#81832=CARTESIAN_POINT('Ctrl Pts',(25.2145881309833,3.88048280124066,0.650934259083974));
#81833=CARTESIAN_POINT('Ctrl Pts',(25.2204523441546,3.85800788828905,0.764371724947675));
#81834=CARTESIAN_POINT('Ctrl Pts',(25.2263251927289,3.8354998796902,0.877976234232687));
#81835=CARTESIAN_POINT('Ctrl Pts',(25.2321980413032,3.80799895972618,0.990438584421596));
#81836=CARTESIAN_POINT('Ctrl Pts',(25.2380708898775,3.77566278237978,1.10129903012404));
#81837=CARTESIAN_POINT('Ctrl Pts',(25.2396656344903,3.76688204438392,1.13140266659876));
#81838=CARTESIAN_POINT('Ctrl Pts',(25.241260379103,3.75774504363042,1.16138829823806));
#81839=CARTESIAN_POINT('Ctrl Pts',(25.2428551237158,3.74825554160734,1.19124699152184));
#81840=CARTESIAN_POINT('Ctrl Pts',(25.2487275698497,3.71331164587487,1.30119786800404));
#81841=CARTESIAN_POINT('Ctrl Pts',(25.2546000159836,3.67346721606696,1.40979396312183));
#81842=CARTESIAN_POINT('Ctrl Pts',(25.2604724621175,3.62884506934392,1.51656601000362));
#81843=CARTESIAN_POINT('Ctrl Pts',(25.2663373010624,3.58428072631959,1.62319974396949));
#81844=CARTESIAN_POINT('Ctrl Pts',(25.2722021400072,3.53495113216584,1.72801375075103));
#81845=CARTESIAN_POINT('Ctrl Pts',(25.278066978952,3.48102893185714,1.83055362542962));
#81846=CARTESIAN_POINT('Ctrl Pts',(25.283925789072,3.42716216145924,1.93298809313159));
#81847=CARTESIAN_POINT('Ctrl Pts',(25.289784599192,3.36871236650804,2.03315271492282));
#81848=CARTESIAN_POINT('Ctrl Pts',(25.2956434093121,3.3059000968078,2.13061342104244));
#81849=CARTESIAN_POINT('Ctrl Pts',(25.301729198193,3.2406543891129,2.23184989559695));
#81850=CARTESIAN_POINT('Ctrl Pts',(25.307814987074,3.17070152836388,2.33016829080207));
#81851=CARTESIAN_POINT('Ctrl Pts',(25.313900775955,3.09634121580394,2.42511032229747));
#81852=CARTESIAN_POINT('Ctrl Pts',(25.3197528060332,3.02483712746957,2.51640557339288));
#81853=CARTESIAN_POINT('Ctrl Pts',(25.3256048361115,2.94925820585057,2.60457869704562));
#81854=CARTESIAN_POINT('Ctrl Pts',(25.3314568661898,2.86991434214601,2.68925280863377));
#81855=CARTESIAN_POINT('Ctrl Pts',(25.3373080065683,2.79058254130082,2.77391404699073));
#81856=CARTESIAN_POINT('Ctrl Pts',(25.3431591469468,2.70748721903882,2.85507702945651));
#81857=CARTESIAN_POINT('Ctrl Pts',(25.3490102873253,2.62097681649429,2.93239996033956));
#81858=CARTESIAN_POINT('Ctrl Pts',(25.3548619548928,2.53445861934421,3.00972985803502));
#81859=CARTESIAN_POINT('Ctrl Pts',(25.3607136224603,2.44452503844631,3.08321874087236));
#81860=CARTESIAN_POINT('Ctrl Pts',(25.3665652900278,2.3515588980991,3.15256399598342));
#81861=CARTESIAN_POINT('Ctrl Pts',(25.372418901712,2.25856187133742,3.22193228987271));
#81862=CARTESIAN_POINT('Ctrl Pts',(25.3782725133962,2.16253061290004,3.28715397163468));
#81863=CARTESIAN_POINT('Ctrl Pts',(25.3841261250804,2.06387772067324,3.34796919850058));
#81864=CARTESIAN_POINT('Ctrl Pts',(25.3899863911803,1.96511267933486,3.40885356042689));
#81865=CARTESIAN_POINT('Ctrl Pts',(25.3958466572802,1.86372040773272,3.46532125205994));
#81866=CARTESIAN_POINT('Ctrl Pts',(25.4017069233801,1.76013903097998,3.51715788551223));
#81867=CARTESIAN_POINT('Ctrl Pts',(25.4075711365514,1.65648788894963,3.56902943254877));
#81868=CARTESIAN_POINT('Ctrl Pts',(25.4134353497227,1.55064508243277,3.61626354248425));
#81869=CARTESIAN_POINT('Ctrl Pts',(25.419299562894,1.44306805939358,3.65869424466681));
#81870=CARTESIAN_POINT('Ctrl Pts',(25.4251724114682,1.33533262278401,3.70118742858419));
#81871=CARTESIAN_POINT('Ctrl Pts',(25.4310452600425,1.22585826228886,3.73886295383567));
#81872=CARTESIAN_POINT('Ctrl Pts',(25.4369181086168,1.1151169649515,3.77160485131692));
#81873=CARTESIAN_POINT('Ctrl Pts',(25.4385128532297,1.08504568265685,3.78049576072195));
#81874=CARTESIAN_POINT('Ctrl Pts',(25.4401075978425,1.05488103216075,3.78902317229664));
#81875=CARTESIAN_POINT('Ctrl Pts',(25.4417023424554,1.02463256229506,3.79718541979249));
#81876=CARTESIAN_POINT('Ctrl Pts',(25.4475747885893,0.913246382660954,3.82724186793112));
#81877=CARTESIAN_POINT('Ctrl Pts',(25.4534472347232,0.800350088235134,3.85244339896585));
#81878=CARTESIAN_POINT('Ctrl Pts',(25.4593196808571,0.686404838989232,3.87263959038434));
#81879=CARTESIAN_POINT('Ctrl Pts',(25.465184519802,0.572607194852999,3.89280961957957));
#81880=CARTESIAN_POINT('Ctrl Pts',(25.4710493587468,0.457763701367477,3.90798713192554));
#81881=CARTESIAN_POINT('Ctrl Pts',(25.4769141976916,0.342349958906268,3.91807165652147));
#81882=CARTESIAN_POINT('Ctrl Pts',(25.4827730078117,0.227054857253721,3.92814581462094));
#81883=CARTESIAN_POINT('Ctrl Pts',(25.4886318179317,0.111191081912517,3.93313736268711));
#81884=CARTESIAN_POINT('Ctrl Pts',(25.4944906280517,-0.004756970227735,
3.93299712321713));
#81885=CARTESIAN_POINT('Ctrl Pts',(25.5005764169327,-0.125197017273399,
3.93285145066766));
#81886=CARTESIAN_POINT('Ctrl Pts',(25.5066622058136,-0.245727555812056,
3.92716824362582));
#81887=CARTESIAN_POINT('Ctrl Pts',(25.5127479946946,-0.365801021423707,
3.9159518144029));
#81888=CARTESIAN_POINT('Ctrl Pts',(25.5186000247729,-0.481262393170798,
3.90516621495688));
#81889=CARTESIAN_POINT('Ctrl Pts',(25.5244520548511,-0.596300707562093,
3.88926466315186));
#81890=CARTESIAN_POINT('Ctrl Pts',(25.5303040849294,-0.710431364549665,
3.86830405685283));
#81891=CARTESIAN_POINT('Ctrl Pts',(25.5361552253079,-0.824544669948839,
3.84734663725073));
#81892=CARTESIAN_POINT('Ctrl Pts',(25.5420063656864,-0.937750185873964,
3.82133176710452));
#81893=CARTESIAN_POINT('Ctrl Pts',(25.5478575060649,-1.04957198505342,3.7903677457723));
#81894=CARTESIAN_POINT('Ctrl Pts',(25.5537091736324,-1.16140385940057,3.75940093457524));
#81895=CARTESIAN_POINT('Ctrl Pts',(25.5595608411999,-1.271851370773,3.72348419606158));
#81896=CARTESIAN_POINT('Ctrl Pts',(25.5654125087674,-1.38045296151046,3.68277593956746));
#81897=CARTESIAN_POINT('Ctrl Pts',(25.5712661204516,-1.48909063327404,3.64205415844948));
#81898=CARTESIAN_POINT('Ctrl Pts',(25.5771197321358,-1.59588077808782,3.59653783896309));
#81899=CARTESIAN_POINT('Ctrl Pts',(25.5829733438201,-1.70038171799668,3.54643356248255));
#81900=CARTESIAN_POINT('Ctrl Pts',(25.58883360992,-1.80500145510774,3.49627232720461));
#81901=CARTESIAN_POINT('Ctrl Pts',(25.5946938760198,-1.90732642010164,3.44151290355854));
#81902=CARTESIAN_POINT('Ctrl Pts',(25.6005541421197,-2.00693936924165,3.38240792456911));
#81903=CARTESIAN_POINT('Ctrl Pts',(25.606418355291,-2.10661941079979,3.3232631365388));
#81904=CARTESIAN_POINT('Ctrl Pts',(25.6122825684623,-2.20358345435853,3.25976719108145));
#81905=CARTESIAN_POINT('Ctrl Pts',(25.6181467816336,-2.2974445371279,3.19221515547138));
#81906=CARTESIAN_POINT('Ctrl Pts',(25.6240196302079,-2.39144383592908,3.12456364546759));
#81907=CARTESIAN_POINT('Ctrl Pts',(25.6298924787822,-2.48233073126536,3.0528443798206));
#81908=CARTESIAN_POINT('Ctrl Pts',(25.6357653273565,-2.56975246066532,2.97739169255652));
#81909=CARTESIAN_POINT('Ctrl Pts',(25.6373600719693,-2.59349142315416,2.956902867582));
#81910=CARTESIAN_POINT('Ctrl Pts',(25.6389548165822,-2.61697509317041,2.93613895344535));
#81911=CARTESIAN_POINT('Ctrl Pts',(25.640549561195,-2.64019690589979,2.9151070817514));
#81912=CARTESIAN_POINT('Ctrl Pts',(25.6463343613492,-2.72443205225064,2.83881575984568));
#81913=CARTESIAN_POINT('Ctrl Pts',(25.6521191615033,-2.80551894687543,2.7587239653442));
#81914=CARTESIAN_POINT('Ctrl Pts',(25.6579039616575,-2.88308709437247,2.67512575522402));
#81915=CARTESIAN_POINT('Ctrl Pts',(25.6636811997646,-2.96055384269176,2.59163682694235));
#81916=CARTESIAN_POINT('Ctrl Pts',(25.6694584378717,-3.03451069836479,2.50465090261323));
#81917=CARTESIAN_POINT('Ctrl Pts',(25.6752356759788,-3.10462086965447,2.41450165783872));
#81918=CARTESIAN_POINT('Ctrl Pts',(25.6810063285583,-3.17465112170482,2.32445517503063));
#81919=CARTESIAN_POINT('Ctrl Pts',(25.6867769811377,-3.24084315136317,2.23125287937215));
#81920=CARTESIAN_POINT('Ctrl Pts',(25.6925476337171,-3.30289833132539,2.13526382747612));
#81921=CARTESIAN_POINT('Ctrl Pts',(25.6983146496206,-3.36491440399852,2.03933526805798));
#81922=CARTESIAN_POINT('Ctrl Pts',(25.7040816655241,-3.42279857562265,1.94062379863746));
#81923=CARTESIAN_POINT('Ctrl Pts',(25.7098486814276,-3.47629402636826,1.83952951654394));
#81924=CARTESIAN_POINT('Ctrl Pts',(25.715613556132,-3.52976961512355,1.73847276911222));
#81925=CARTESIAN_POINT('Ctrl Pts',(25.7213784308363,-3.57885952230643,1.63503534409878));
#81926=CARTESIAN_POINT('Ctrl Pts',(25.7271433055407,-3.62335206581951,1.52964335945392));
#81927=CARTESIAN_POINT('Ctrl Pts',(25.7329075322382,-3.66783960810145,1.42426322150593));
#81928=CARTESIAN_POINT('Ctrl Pts',(25.7386717589358,-3.70773064965458,1.31692935439913));
#81929=CARTESIAN_POINT('Ctrl Pts',(25.7444359856333,-3.7428613571943,1.20808851530905));
#81930=CARTESIAN_POINT('Ctrl Pts',(25.7502036269295,-3.7780128753776,1.09918320134592));
#81931=CARTESIAN_POINT('Ctrl Pts',(25.7559712682257,-3.80839829491612,0.988769538700377));
#81932=CARTESIAN_POINT('Ctrl Pts',(25.7617389095219,-3.83390354286085,0.877309879141372));
#81933=CARTESIAN_POINT('Ctrl Pts',(25.7675083756034,-3.85941686023952,0.765814955609947));
#81934=CARTESIAN_POINT('Ctrl Pts',(25.7732778416849,-3.88004685222984,0.65327379560468));
#81935=CARTESIAN_POINT('Ctrl Pts',(25.7790473077664,-3.89573081843034,0.540157745785523));
#81936=CARTESIAN_POINT('Ctrl Pts',(25.7848234966307,-3.9114330601346,0.426909889204726));
#81937=CARTESIAN_POINT('Ctrl Pts',(25.790599685495,-3.9221777268169,0.313086229874658));
#81938=CARTESIAN_POINT('Ctrl Pts',(25.7963758743593,-3.92795411346371,0.1991619504914));
#81939=CARTESIAN_POINT('Ctrl Pts',(25.7997960755613,-3.93137443177674,0.131705022328782));
#81940=CARTESIAN_POINT('Ctrl Pts',(25.8032162767632,-3.93305383103106,0.0642128260551774));
#81941=CARTESIAN_POINT('Ctrl Pts',(25.8066364779651,-3.93299868468798,-0.00321655757663048));
#81942=CARTESIAN_POINT('',(27.0566364779651,-3.93435343806616,0.00262747460303034));
#81943=CARTESIAN_POINT('Ctrl Pts',(25.8066364779651,-3.93569742829264,-0.00321876471293834));
#81944=CARTESIAN_POINT('Ctrl Pts',(25.8175565786217,-3.93760386311818,-0.218658353487745));
#81945=CARTESIAN_POINT('Ctrl Pts',(25.8947590855247,-3.82336855807856,-1.73974115160522));
#81946=CARTESIAN_POINT('Ctrl Pts',(26.0382439986743,-1.83972417824563,-4.27240052182587));
#81947=CARTESIAN_POINT('Ctrl Pts',(26.237091217414,2.59922370323215,-3.85772308642246));
#81948=CARTESIAN_POINT('Ctrl Pts',(26.4359384361537,4.65057791887957,0.100579776150997));
#81949=CARTESIAN_POINT('Ctrl Pts',(26.6347856548932,2.43000649467348,3.9664921160622));
#81950=CARTESIAN_POINT('Ctrl Pts',(26.8336328736329,-2.02271913287657,4.18886602560103));
#81951=CARTESIAN_POINT('Ctrl Pts',(26.9742498146569,-3.85758709369341,1.62510249400492));
#81952=CARTESIAN_POINT('Ctrl Pts',(27.0485843494343,-3.93845870985197,0.161325734877928));
#81953=CARTESIAN_POINT('Ctrl Pts',(27.0566364779651,-3.93723842550275,0.00262940128077819));
#81954=CARTESIAN_POINT('',(28.3066364508351,-3.93096447206993,0.00191346378281269));
#81955=CARTESIAN_POINT('Ctrl Pts',(27.0566364779651,-3.93299912295048,0.00262657015236832));
#81956=CARTESIAN_POINT('Ctrl Pts',(27.0624230850425,-3.93307520374763,-0.111296032760114));
#81957=CARTESIAN_POINT('Ctrl Pts',(27.0682096921198,-3.92819730815862,-0.225413803237607));
#81958=CARTESIAN_POINT('Ctrl Pts',(27.0739962991972,-3.91834103977739,-0.339252849650841));
#81959=CARTESIAN_POINT('Ctrl Pts',(27.0797763934189,-3.90849586467629,-0.452963769639129));
#81960=CARTESIAN_POINT('Ctrl Pts',(27.0855564876406,-3.89368349056366,-0.566396168206476));
#81961=CARTESIAN_POINT('Ctrl Pts',(27.0913365818623,-3.87393154667742,-0.679075379952401));
#81962=CARTESIAN_POINT('Ctrl Pts',(27.0971695289144,-3.85399899221638,-0.792784923564359));
#81963=CARTESIAN_POINT('Ctrl Pts',(27.1030024759665,-3.82903606102631,-0.905726996853392));
#81964=CARTESIAN_POINT('Ctrl Pts',(27.1088354230185,-3.79912486104711,-1.01741795255133));
#81965=CARTESIAN_POINT('Ctrl Pts',(27.1146079286819,-3.76952360292889,-1.12795155907285));
#81966=CARTESIAN_POINT('Ctrl Pts',(27.1203804343453,-3.73507626101903,-1.23725943527664));
#81967=CARTESIAN_POINT('Ctrl Pts',(27.1261529400087,-3.6959137047072,-1.3448832244316));
#81968=CARTESIAN_POINT('Ctrl Pts',(27.1319242944339,-3.65675895876952,-1.45248554966436));
#81969=CARTESIAN_POINT('Ctrl Pts',(27.1376956488591,-3.61289101273658,-1.55840405530356));
#81970=CARTESIAN_POINT('Ctrl Pts',(27.1434670032844,-3.56449006855692,-1.66219720585709));
#81971=CARTESIAN_POINT('Ctrl Pts',(27.1492386945002,-3.5160862999131,-1.76599641331795));
#81972=CARTESIAN_POINT('Ctrl Pts',(27.1550103857161,-3.46314918823332,-1.86766963364983));
#81973=CARTESIAN_POINT('Ctrl Pts',(27.1607820769319,-3.40590600456802,-1.96679772423285));
#81974=CARTESIAN_POINT('Ctrl Pts',(27.1666608464469,-3.34760082667656,-2.0677648715054));
#81975=CARTESIAN_POINT('Ctrl Pts',(27.172539615962,-3.28482842684045,-2.1660911070396));
#81976=CARTESIAN_POINT('Ctrl Pts',(27.178418385477,-3.21787575663264,-2.26136344157146));
#81977=CARTESIAN_POINT('Ctrl Pts',(27.1841983330029,-3.1520485593716,-2.35503425020812));
#81978=CARTESIAN_POINT('Ctrl Pts',(27.1899782805287,-3.0821808544064,-2.44575273197191));
#81979=CARTESIAN_POINT('Ctrl Pts',(27.1957582280546,-3.00858593618571,-2.53316001559032));
#81980=CARTESIAN_POINT('Ctrl Pts',(27.2016864085642,-2.93310359696907,-2.62280895320181));
#81981=CARTESIAN_POINT('Ctrl Pts',(27.2076145890738,-2.85370060363789,-2.70897419680968));
#81982=CARTESIAN_POINT('Ctrl Pts',(27.2135427695834,-2.77075394578029,-2.79131001000301));
#81983=CARTESIAN_POINT('Ctrl Pts',(27.219470950093,-2.68780728792268,-2.87364582319633));
#81984=CARTESIAN_POINT('Ctrl Pts',(27.2253991306026,-2.60131736618754,-2.95215194076755));
#81985=CARTESIAN_POINT('Ctrl Pts',(27.2313273111122,-2.51169493614476,-3.02652896033472));
#81986=CARTESIAN_POINT('Ctrl Pts',(27.2371997572461,-2.4229151002466,-3.10020671699247));
#81987=CARTESIAN_POINT('Ctrl Pts',(27.24307220338,-2.3307419970519,-3.17009812926226));
#81988=CARTESIAN_POINT('Ctrl Pts',(27.2489446495139,-2.23553238064819,-3.2358745301809));
#81989=CARTESIAN_POINT('Ctrl Pts',(27.2548094884588,-2.14044609914401,-3.30156572409939));
#81990=CARTESIAN_POINT('Ctrl Pts',(27.2606743274036,-2.04233146373895,-3.36315227454946));
#81991=CARTESIAN_POINT('Ctrl Pts',(27.2665391663485,-1.94157914390406,-3.42034492821364));
#81992=CARTESIAN_POINT('Ctrl Pts',(27.2723979764685,-1.84093039350915,-3.47747879006915));
#81993=CARTESIAN_POINT('Ctrl Pts',(27.2782567865885,-1.73764970919876,-3.53022753637549));
#81994=CARTESIAN_POINT('Ctrl Pts',(27.2841155967086,-1.6321571020155,-3.57834489594566));
#81995=CARTESIAN_POINT('Ctrl Pts',(27.2902013855895,-1.52257755895691,-3.62832639148047));
#81996=CARTESIAN_POINT('Ctrl Pts',(27.2962871744705,-1.4106116144076,-3.6733101310299));
#81997=CARTESIAN_POINT('Ctrl Pts',(27.3023729633515,-1.29675897571493,-3.71307219952734));
#81998=CARTESIAN_POINT('Ctrl Pts',(27.3082249934298,-1.18727948519185,-3.75130698311451));
#81999=CARTESIAN_POINT('Ctrl Pts',(27.314077023508,-1.07605599138446,-3.78471368233932));
#82000=CARTESIAN_POINT('Ctrl Pts',(27.3199290535863,-0.963552827024398,
-3.81314239827643));
#82001=CARTESIAN_POINT('Ctrl Pts',(27.3257801939648,-0.851066766820581,
-3.84156679212));
#82002=CARTESIAN_POINT('Ctrl Pts',(27.3316313343433,-0.737301823547027,
-3.86501460623153));
#82003=CARTESIAN_POINT('Ctrl Pts',(27.3374824747218,-0.622735831251369,
-3.88338629091617));
#82004=CARTESIAN_POINT('Ctrl Pts',(27.3433341422893,-0.508159516535937,
-3.90175963089343));
#82005=CARTESIAN_POINT('Ctrl Pts',(27.3491858098568,-0.392782417488927,
-3.9150558668005));
#82006=CARTESIAN_POINT('Ctrl Pts',(27.3550374774243,-0.277090151822499,
-3.9232269941673));
#82007=CARTESIAN_POINT('Ctrl Pts',(27.3608910891085,-0.161359449374253,
-3.93140083625178));
#82008=CARTESIAN_POINT('Ctrl Pts',(27.3667447007928,-0.0453137842112288,
-3.9344461549148));
#82009=CARTESIAN_POINT('Ctrl Pts',(27.372598312477,0.0705592591044405,-3.93236702139496));
#82010=CARTESIAN_POINT('Ctrl Pts',(27.3784585785769,0.186564027487612,-3.9302855243055));
#82011=CARTESIAN_POINT('Ctrl Pts',(27.3843188446767,0.302395368805617,-3.92306795494325));
#82012=CARTESIAN_POINT('Ctrl Pts',(27.3901791107766,0.417568755444039,-3.91077042722747));
#82013=CARTESIAN_POINT('Ctrl Pts',(27.3960433239479,0.532819714939232,-3.89846461674443));
#82014=CARTESIAN_POINT('Ctrl Pts',(27.4019075371192,0.64741142967131,-3.88107209687023));
#82015=CARTESIAN_POINT('Ctrl Pts',(27.4077717502905,0.760869250705581,-3.85870016758632));
#82016=CARTESIAN_POINT('Ctrl Pts',(27.4136445988648,0.874494145135491,-3.83629529430474));
#82017=CARTESIAN_POINT('Ctrl Pts',(27.4195174474391,0.986981413323301,-3.80889647490465));
#82018=CARTESIAN_POINT('Ctrl Pts',(27.4253902960134,1.09787116695553,-3.77666094596374));
#82019=CARTESIAN_POINT('Ctrl Pts',(27.4269850406262,1.12798276186274,-3.76790753857221));
#82020=CARTESIAN_POINT('Ctrl Pts',(27.4285797852391,1.15797667538553,-3.75879776144932));
#82021=CARTESIAN_POINT('Ctrl Pts',(27.4301745298519,1.18784397059293,-3.74933536797204));
#82022=CARTESIAN_POINT('Ctrl Pts',(27.4360469759858,1.29782652257194,-3.7144912960454));
#82023=CARTESIAN_POINT('Ctrl Pts',(27.4419194221197,1.40645874227142,-3.67474546224114));
#82024=CARTESIAN_POINT('Ctrl Pts',(27.4477918682536,1.51327125152412,-3.63022025768556));
#82025=CARTESIAN_POINT('Ctrl Pts',(27.4536567071985,1.61994539544582,-3.58575273124942));
#82026=CARTESIAN_POINT('Ctrl Pts',(27.4595215461433,1.72480413865467,-3.53651830376502));
#82027=CARTESIAN_POINT('Ctrl Pts',(27.4653863850882,1.82739291969843,-3.48268920764343));
#82028=CARTESIAN_POINT('Ctrl Pts',(27.4712451952082,1.92987624349184,-3.42891544572514));
#82029=CARTESIAN_POINT('Ctrl Pts',(27.4771040053283,2.03009388261276,-3.3705566006582));
#82030=CARTESIAN_POINT('Ctrl Pts',(27.4829628154483,2.1276115672721,-3.30783282812326));
#82031=CARTESIAN_POINT('Ctrl Pts',(27.4890486043293,2.22890722779675,-3.24267904610188));
#82032=CARTESIAN_POINT('Ctrl Pts',(27.4951343932102,2.32728908315672,-3.17281546403948));
#82033=CARTESIAN_POINT('Ctrl Pts',(27.5012201820912,2.42229857712262,-3.09854136704187));
#82034=CARTESIAN_POINT('Ctrl Pts',(27.5070722121695,2.51365869941481,-3.02712018267815));
#82035=CARTESIAN_POINT('Ctrl Pts',(27.5129242422478,2.60190039453619,-2.95162133255492));
#82036=CARTESIAN_POINT('Ctrl Pts',(27.518776272326,2.68664649671219,-2.87235436562137));
#82037=CARTESIAN_POINT('Ctrl Pts',(27.5246274127046,2.7713797147121,-2.79309944985634));
#82038=CARTESIAN_POINT('Ctrl Pts',(27.5304785530831,2.85261809465008,-2.71007783863559));
#82039=CARTESIAN_POINT('Ctrl Pts',(27.5363296934616,2.93001952467321,-2.62363766268015));
#82040=CARTESIAN_POINT('Ctrl Pts',(27.5421813610291,3.00742792858161,-2.53718969844651));
#82041=CARTESIAN_POINT('Ctrl Pts',(27.5480330285966,3.08099841957563,-2.44732286513857));
#82042=CARTESIAN_POINT('Ctrl Pts',(27.5538846961641,3.1504280373978,-2.35441971219616));
#82043=CARTESIAN_POINT('Ctrl Pts',(27.5597383078484,3.21988072202623,-2.26148569376584));
#82044=CARTESIAN_POINT('Ctrl Pts',(27.5655919195326,3.28518955060098,-2.16551368076623));
#82045=CARTESIAN_POINT('Ctrl Pts',(27.5714455312169,3.34609430591902,-2.06691603503778));
#82046=CARTESIAN_POINT('Ctrl Pts',(27.5773057973168,3.40706829807387,-1.96820630300226));
#82047=CARTESIAN_POINT('Ctrl Pts',(27.5831660634167,3.46362800665929,-1.86686533249271));
#82048=CARTESIAN_POINT('Ctrl Pts',(27.5890263295166,3.51555864616209,-1.76333105382824));
#82049=CARTESIAN_POINT('Ctrl Pts',(27.5948905426879,3.56752426256507,-1.65972704160829));
#82050=CARTESIAN_POINT('Ctrl Pts',(27.6007547558592,3.61485443329103,-1.55392715610801));
#82051=CARTESIAN_POINT('Ctrl Pts',(27.6066189690305,3.65738277250184,-1.446388694441));
#82052=CARTESIAN_POINT('Ctrl Pts',(27.6124918176048,3.69997373722392,-1.33869187598726));
#82053=CARTESIAN_POINT('Ctrl Pts',(27.6183646661791,3.73774862379689,-1.229251761069));
#82054=CARTESIAN_POINT('Ctrl Pts',(27.6242375147534,3.77059103471154,-1.11854023126259));
#82055=CARTESIAN_POINT('Ctrl Pts',(27.6258322593661,3.77950923806932,-1.0884770322048));
#82056=CARTESIAN_POINT('Ctrl Pts',(27.6274270039788,3.78806402850286,-1.05832013501393));
#82057=CARTESIAN_POINT('Ctrl Pts',(27.6290217485916,3.79625373109626,-1.02807908700534));
#82058=CARTESIAN_POINT('Ctrl Pts',(27.6348941947255,3.82641127917549,-0.916720237415284));
#82059=CARTESIAN_POINT('Ctrl Pts',(27.6407666408594,3.85171528297846,-0.803846866538452));
#82060=CARTESIAN_POINT('Ctrl Pts',(27.6466390869933,3.87201490143052,-0.689919997608392));
#82061=CARTESIAN_POINT('Ctrl Pts',(27.6525039259381,3.89228822367954,-0.576140709978197));
#82062=CARTESIAN_POINT('Ctrl Pts',(27.6583687648829,3.90756998052033,-0.461311041404331));
#82063=CARTESIAN_POINT('Ctrl Pts',(27.6642336038278,3.91775926936079,-0.345906500860604));
#82064=CARTESIAN_POINT('Ctrl Pts',(27.6700924139478,3.92793808401126,-0.230620591666161));
#82065=CARTESIAN_POINT('Ctrl Pts',(27.6759512240678,3.93303480694386,-0.114761395208751));
#82066=CARTESIAN_POINT('Ctrl Pts',(27.6818100341878,3.93299982095811,0.00118673646314422));
#82067=CARTESIAN_POINT('Ctrl Pts',(27.6878958230688,3.93296347956478,0.121626866121606));
#82068=CARTESIAN_POINT('Ctrl Pts',(27.6939816119497,3.92738968810554,0.24216251400827));
#82069=CARTESIAN_POINT('Ctrl Pts',(27.7000674008307,3.9162822618308,0.362246112014192));
#82070=CARTESIAN_POINT('Ctrl Pts',(27.705919430909,3.90560147846434,0.477717226964077));
#82071=CARTESIAN_POINT('Ctrl Pts',(27.7117714609872,3.88980436081067,0.592769928808034));
#82072=CARTESIAN_POINT('Ctrl Pts',(27.7176234910655,3.86894736680903,0.706919566047993));
#82073=CARTESIAN_POINT('Ctrl Pts',(27.723474631444,3.84809354375188,0.821051848813789));
#82074=CARTESIAN_POINT('Ctrl Pts',(27.7293257718224,3.82218144817613,0.934280933449317));
#82075=CARTESIAN_POINT('Ctrl Pts',(27.7351769122009,3.79131894736579,1.04613079456882));
#82076=CARTESIAN_POINT('Ctrl Pts',(27.7410285797684,3.76045366583752,1.15799073338472));
#82077=CARTESIAN_POINT('Ctrl Pts',(27.7468802473359,3.72463720235774,1.26847080316033));
#82078=CARTESIAN_POINT('Ctrl Pts',(27.7527319149034,3.68402754721204,1.37710930262737));
#82079=CARTESIAN_POINT('Ctrl Pts',(27.7585855265876,3.64340440020117,1.48578389538262));
#82080=CARTESIAN_POINT('Ctrl Pts',(27.7644391382719,3.59798503967955,1.5926153142569));
#82081=CARTESIAN_POINT('Ctrl Pts',(27.7702927499561,3.54797564599711,1.69716169395004));
#82082=CARTESIAN_POINT('Ctrl Pts',(27.776153016056,3.49790940138059,1.80182692250145));
#82083=CARTESIAN_POINT('Ctrl Pts',(27.7820132821558,3.44324288717978,1.90420155394945));
#82084=CARTESIAN_POINT('Ctrl Pts',(27.7878735482557,3.38422835755668,2.00386811539812));
#82085=CARTESIAN_POINT('Ctrl Pts',(27.793737761427,3.32517407981299,2.10360180537477));
#82086=CARTESIAN_POINT('Ctrl Pts',(27.7996019745983,3.26176618095077,2.20062344829359));
#82087=CARTESIAN_POINT('Ctrl Pts',(27.8054661877696,3.19429937685201,2.29454581367269));
#82088=CARTESIAN_POINT('Ctrl Pts',(27.8113390363439,3.12673322386795,2.38860648532596));
#82089=CARTESIAN_POINT('Ctrl Pts',(27.8172118849182,3.05509649158996,2.47955844735739));
#82090=CARTESIAN_POINT('Ctrl Pts',(27.8230847334924,2.97972319368144,2.56704863394461));
#82091=CARTESIAN_POINT('Ctrl Pts',(27.8246794781053,2.95925592651549,2.59080618566342));
#82092=CARTESIAN_POINT('Ctrl Pts',(27.8262742227182,2.93851333855551,2.61430869473074));
#82093=CARTESIAN_POINT('Ctrl Pts',(27.8278689673311,2.91750255544411,2.63754958986122));
#82094=CARTESIAN_POINT('Ctrl Pts',(27.833741413465,2.84013299353676,2.72313125833334));
#82095=CARTESIAN_POINT('Ctrl Pts',(27.8396138595989,2.75886504173572,2.80544899926235));
#82096=CARTESIAN_POINT('Ctrl Pts',(27.8454863057328,2.67400495558111,2.88412664380877));
#82097=CARTESIAN_POINT('Ctrl Pts',(27.8513511446777,2.58925479750527,2.96270236903483));
#82098=CARTESIAN_POINT('Ctrl Pts',(27.8572159836225,2.50092205909048,3.03764709667529));
#82099=CARTESIAN_POINT('Ctrl Pts',(27.8630808225673,2.40935218365957,3.10861883399925));
#82100=CARTESIAN_POINT('Ctrl Pts',(27.8689396326873,2.31787643847565,3.17951761515577));
#82101=CARTESIAN_POINT('Ctrl Pts',(27.8747984428073,2.22317049990736,3.24645127774988));
#82102=CARTESIAN_POINT('Ctrl Pts',(27.8806572529273,2.12561498068711,3.30911618923823));
#82103=CARTESIAN_POINT('Ctrl Pts',(27.8867430418083,2.0242800198353,3.37420882985159));
#82104=CARTESIAN_POINT('Ctrl Pts',(27.8928288306893,1.91987055224875,3.43469496579195));
#82105=CARTESIAN_POINT('Ctrl Pts',(27.8989146195703,1.81284926004676,3.4902817307988));
#82106=CARTESIAN_POINT('Ctrl Pts',(27.9047666496485,1.70993871989666,3.54373337480676));
#82107=CARTESIAN_POINT('Ctrl Pts',(27.9106186797268,1.60461369824476,3.59265487255402));
#82108=CARTESIAN_POINT('Ctrl Pts',(27.916470709805,1.49731241563733,3.63683166093487));
#82109=CARTESIAN_POINT('Ctrl Pts',(27.9223218501836,1.39002744633031,3.68100173300067));
#82110=CARTESIAN_POINT('Ctrl Pts',(27.9281729905621,1.28076719559822,3.7204283726566));
#82111=CARTESIAN_POINT('Ctrl Pts',(27.9340241309406,1.16999042518382,3.75494492702332));
#82112=CARTESIAN_POINT('Ctrl Pts',(27.9398757985081,1.05920367375901,3.78946459133888));
#82113=CARTESIAN_POINT('Ctrl Pts',(27.9457274660756,0.946900525693874,3.81907316794247));
#82114=CARTESIAN_POINT('Ctrl Pts',(27.9515791336431,0.833554795176103,3.84365391306748));
#82115=CARTESIAN_POINT('Ctrl Pts',(27.9574327453273,0.720171407472755,3.86824282472576));
#82116=CARTESIAN_POINT('Ctrl Pts',(27.9632863570115,0.605745152313695,3.88780049583462));
#82117=CARTESIAN_POINT('Ctrl Pts',(27.9691399686957,0.490759214554631,3.90226144605019));
#82118=CARTESIAN_POINT('Ctrl Pts',(27.9750002347956,0.375642560194304,3.91673883554781));
#82119=CARTESIAN_POINT('Ctrl Pts',(27.9808605008955,0.259965363668743,3.92610788795599));
#82120=CARTESIAN_POINT('Ctrl Pts',(27.9867207669954,0.14421520330767,3.930355069855));
#82121=CARTESIAN_POINT('Ctrl Pts',(27.9925849801667,0.0283870816149384,
3.93460511236307));
#82122=CARTESIAN_POINT('Ctrl Pts',(27.998449193338,-0.0875136894336054,
3.93372641836407));
#82123=CARTESIAN_POINT('Ctrl Pts',(28.0043134065093,-0.203002012209708,
3.92775752599862));
#82124=CARTESIAN_POINT('Ctrl Pts',(28.0101862550836,-0.318660398416178,
3.92177984408383));
#82125=CARTESIAN_POINT('Ctrl Pts',(28.0160591036579,-0.433904714281006,
3.91069704345804));
#82126=CARTESIAN_POINT('Ctrl Pts',(28.0219319522322,-0.548257353079323,
3.89459919308707));
#82127=CARTESIAN_POINT('Ctrl Pts',(28.023526696845,-0.579309278287869,3.89022789697191));
#82128=CARTESIAN_POINT('Ctrl Pts',(28.0251214414579,-0.610295528116905,
3.88548709437747));
#82129=CARTESIAN_POINT('Ctrl Pts',(28.0267161860708,-0.641206721834683,
3.88037922629658));
#82130=CARTESIAN_POINT('Ctrl Pts',(28.0325886322047,-0.755033298566156,
3.86157014556832));
#82131=CARTESIAN_POINT('Ctrl Pts',(28.0384610783386,-0.868222129685195,
3.83771686546812));
#82132=CARTESIAN_POINT('Ctrl Pts',(28.0443335244725,-0.980291183104439,
3.80887361254318));
#82133=CARTESIAN_POINT('Ctrl Pts',(28.0501983634174,-1.09221506184536,3.78006772327784));
#82134=CARTESIAN_POINT('Ctrl Pts',(28.0560632023622,-1.2030216509221,3.74628481792268));
#82135=CARTESIAN_POINT('Ctrl Pts',(28.0619280413071,-1.31223647825913,3.70763056750886));
#82136=CARTESIAN_POINT('Ctrl Pts',(28.0677868514271,-1.42133903702995,3.66901605215096));
#82137=CARTESIAN_POINT('Ctrl Pts',(28.0736456615472,-1.52885270135796,3.62554028911732));
#82138=CARTESIAN_POINT('Ctrl Pts',(28.0795044716673,-1.63431625163951,3.57735927600611));
#82139=CARTESIAN_POINT('Ctrl Pts',(28.0855902605482,-1.74386561208965,3.52731166090041));
#82140=CARTESIAN_POINT('Ctrl Pts',(28.0916760494292,-1.85120235701782,3.47218695907927));
#82141=CARTESIAN_POINT('Ctrl Pts',(28.0977618383102,-1.95582994775565,3.41221602708007));
#82142=CARTESIAN_POINT('Ctrl Pts',(28.1036138683884,-2.05643872995143,3.35454861456454));
#82143=CARTESIAN_POINT('Ctrl Pts',(28.1094658984667,-2.15454224760076,3.29240062221843));
#82144=CARTESIAN_POINT('Ctrl Pts',(28.115317928545,-2.24972305797007,3.22602466860342));
#82145=CARTESIAN_POINT('Ctrl Pts',(28.1211690689235,-2.34488939774674,3.15965880630179));
#82146=CARTESIAN_POINT('Ctrl Pts',(28.127020209302,-2.43713357478847,3.08906649718448));
#82147=CARTESIAN_POINT('Ctrl Pts',(28.1328713496805,-2.52606734203592,3.0145435448007));
#82148=CARTESIAN_POINT('Ctrl Pts',(28.138723017248,-2.61500912223483,2.94001387788297));
#82149=CARTESIAN_POINT('Ctrl Pts',(28.1445746848156,-2.70063958286243,2.86155312918251));
#82150=CARTESIAN_POINT('Ctrl Pts',(28.1504263523831,-2.78260432183879,2.7794967508677));
#82151=CARTESIAN_POINT('Ctrl Pts',(28.1562799640673,-2.86459629220127,2.69741311072115));
#82152=CARTESIAN_POINT('Ctrl Pts',(28.1621335757515,-2.94291982727585,2.61173175789363));
#82153=CARTESIAN_POINT('Ctrl Pts',(28.1679871874358,-3.01725858141465,2.52282374590054));
#82154=CARTESIAN_POINT('Ctrl Pts',(28.1738474535357,-3.09168184422896,2.43381466282518));
#82155=CARTESIAN_POINT('Ctrl Pts',(28.1797077196356,-3.16211101923544,2.34157191651411));
#82156=CARTESIAN_POINT('Ctrl Pts',(28.1855679857355,-3.2282710834055,2.24649834454599));
#82157=CARTESIAN_POINT('Ctrl Pts',(28.1914321989068,-3.29447570843561,2.15136073757143));
#82158=CARTESIAN_POINT('Ctrl Pts',(28.1972964120781,-3.35640527684828,2.05338885696761));
#82159=CARTESIAN_POINT('Ctrl Pts',(28.2031606252494,-3.4138299100163,1.95301160915087));
#82160=CARTESIAN_POINT('Ctrl Pts',(28.2090334738237,-3.47133910437526,1.85248654986108));
#82161=CARTESIAN_POINT('Ctrl Pts',(28.214906322398,-3.52432993529329,1.74954942027436));
#82162=CARTESIAN_POINT('Ctrl Pts',(28.2207791709723,-3.5726199227409,1.64465068863719));
#82163=CARTESIAN_POINT('Ctrl Pts',(28.222373915585,-3.58573284338834,1.61616592778553));
#82164=CARTESIAN_POINT('Ctrl Pts',(28.2239686601977,-3.59849942054148,1.58753661771179));
#82165=CARTESIAN_POINT('Ctrl Pts',(28.2255634048104,-3.61091663532755,1.55877196944093));
#82166=CARTESIAN_POINT('Ctrl Pts',(28.2323194906888,-3.66352177899585,1.43691143300609));
#82167=CARTESIAN_POINT('Ctrl Pts',(28.2390755765672,-3.71000883784057,1.31225778602846));
#82168=CARTESIAN_POINT('Ctrl Pts',(28.2458316624456,-3.75010443956021,1.18541372203582));
#82169=CARTESIAN_POINT('Ctrl Pts',(28.2523049043881,-3.78852143653605,1.06387999230453));
#82170=CARTESIAN_POINT('Ctrl Pts',(28.2587781463305,-3.82107110275934,0.940335813861802));
#82171=CARTESIAN_POINT('Ctrl Pts',(28.265251388273,-3.84755994505957,0.815335188234384));
#82172=CARTESIAN_POINT('Ctrl Pts',(28.2717062130248,-3.87397342325884,0.690690205170065));
#82173=CARTESIAN_POINT('Ctrl Pts',(28.2781610377765,-3.8943603892922,0.564597288335471));
#82174=CARTESIAN_POINT('Ctrl Pts',(28.2846158625283,-3.90857683972787,0.437625511074123));
#82175=CARTESIAN_POINT('Ctrl Pts',(28.2910434986928,-3.9227334085682,0.311188555962646));
#82176=CARTESIAN_POINT('Ctrl Pts',(28.2974711348572,-3.93077123230382,0.183880379132744));
#82177=CARTESIAN_POINT('Ctrl Pts',(28.3038987710217,-3.93259732066487,0.0562788903539033));
#82178=CARTESIAN_POINT('Ctrl Pts',(28.3048113257982,-3.93285657704056,0.0381628450309305));
#82179=CARTESIAN_POINT('Ctrl Pts',(28.3057238805747,-3.93299070927667,0.0200409103137733));
#82180=CARTESIAN_POINT('Ctrl Pts',(28.3066364353512,-3.93299953390383,0.00191476166166355));
#82181=CARTESIAN_POINT('',(29.5566365080617,-3.9323872535115,-0.00334900090502091));
#82182=CARTESIAN_POINT('Ctrl Pts',(28.3066364779651,-3.92739873788489,0.00191118970400611));
#82183=CARTESIAN_POINT('Ctrl Pts',(28.3458945264934,-3.92399062950395,-0.776765967029143));
#82184=CARTESIAN_POINT('Ctrl Pts',(28.4514349812685,-3.32238059726958,-2.87499851905737));
#82185=CARTESIAN_POINT('Ctrl Pts',(28.6232578422896,0.0963581091439014,
-4.65066730542375));
#82186=CARTESIAN_POINT('Ctrl Pts',(28.8221050610294,3.9642846102464,-2.43360613081016));
#82187=CARTESIAN_POINT('Ctrl Pts',(29.0209522797691,4.19070045060739,2.01891579919035));
#82188=CARTESIAN_POINT('Ctrl Pts',(29.2197994985086,0.567624675912214,4.61690302023292));
#82189=CARTESIAN_POINT('Ctrl Pts',(29.3983608979072,-3.15405118804572,3.14151233710411));
#82190=CARTESIAN_POINT('Ctrl Pts',(29.5106398910595,-3.92290060823451,0.907342439014413));
#82191=CARTESIAN_POINT('Ctrl Pts',(29.5566364779651,-3.93022207073951,-0.0033465609634104));
#82192=CARTESIAN_POINT('',(30.8066364779651,-3.93544205199766,-0.000484814710531748));
#82193=CARTESIAN_POINT('Ctrl Pts',(29.5566365165592,-3.93299857355406,-0.00334968980077072));
#82194=CARTESIAN_POINT('Ctrl Pts',(29.5636420149798,-3.93288035987524,-0.14214887951555));
#82195=CARTESIAN_POINT('Ctrl Pts',(29.5706475134005,-3.92541082729009,-0.280628809344632));
#82196=CARTESIAN_POINT('Ctrl Pts',(29.5776530118211,-3.91071391485967,-0.41809768729681));
#82197=CARTESIAN_POINT('Ctrl Pts',(29.5847475963944,-3.89583010760655,-0.557314702600614));
#82198=CARTESIAN_POINT('Ctrl Pts',(29.5918421809678,-3.87353400600672,-0.695494759666681));
#82199=CARTESIAN_POINT('Ctrl Pts',(29.5989367655412,-3.84400351079835,-0.83194110907562));
#82200=CARTESIAN_POINT('Ctrl Pts',(29.6051224890234,-3.81825605853182,-0.950907819371501));
#82201=CARTESIAN_POINT('Ctrl Pts',(29.6113082125057,-3.78700982382328,-1.06855691050145));
#82202=CARTESIAN_POINT('Ctrl Pts',(29.617493935988,-3.75041210475301,-1.18443997083941));
#82203=CARTESIAN_POINT('Ctrl Pts',(29.6233663821219,-3.71566788534505,-1.29445410768542));
#82204=CARTESIAN_POINT('Ctrl Pts',(29.6292388282558,-3.67602068029653,-1.40312236244948));
#82205=CARTESIAN_POINT('Ctrl Pts',(29.6351112743898,-3.63159245459888,-1.50997524605554));
#82206=CARTESIAN_POINT('Ctrl Pts',(29.6409761133346,-3.58722178139388,-1.61668971202953));
#82207=CARTESIAN_POINT('Ctrl Pts',(29.6468409522795,-3.5380825611499,-1.72159310525812));
#82208=CARTESIAN_POINT('Ctrl Pts',(29.6527057912243,-3.48434661357268,-1.82423070813003));
#82209=CARTESIAN_POINT('Ctrl Pts',(29.6585646013444,-3.4306659044457,-1.92676280356466));
#82210=CARTESIAN_POINT('Ctrl Pts',(29.6644234114644,-3.37239805735304,-2.0270333774321));
#82211=CARTESIAN_POINT('Ctrl Pts',(29.6702822215844,-3.30976283367029,-2.12460796027286));
#82212=CARTESIAN_POINT('Ctrl Pts',(29.6763680104654,-3.24470103101146,-2.2259627232966));
#82213=CARTESIAN_POINT('Ctrl Pts',(29.6824537993464,-3.17492678520572,-2.32440795774144));
#82214=CARTESIAN_POINT('Ctrl Pts',(29.6885395882273,-3.10073896497493,-2.41948483588681));
#82215=CARTESIAN_POINT('Ctrl Pts',(29.6943916183056,-3.02940074343561,-2.51090975409172));
#82216=CARTESIAN_POINT('Ctrl Pts',(29.7002436483839,-2.95398202702203,-2.59921994796741));
#82217=CARTESIAN_POINT('Ctrl Pts',(29.7060956784621,-2.87479202217847,-2.6840379708974));
#82218=CARTESIAN_POINT('Ctrl Pts',(29.7119468188406,-2.79561405680271,-2.76884309871697));
#82219=CARTESIAN_POINT('Ctrl Pts',(29.7177979592192,-2.71266622503623,-2.85015680918375));
#82220=CARTESIAN_POINT('Ctrl Pts',(29.7236490995977,-2.62629634689994,-2.92763667456535));
#82221=CARTESIAN_POINT('Ctrl Pts',(29.7295007671652,-2.53991868681935,-3.00512352089921));
#82222=CARTESIAN_POINT('Ctrl Pts',(29.7353524347327,-2.45011867515528,-3.07877555942503));
#82223=CARTESIAN_POINT('Ctrl Pts',(29.7412041023002,-2.35727858617364,-3.1482894827457));
#82224=CARTESIAN_POINT('Ctrl Pts',(29.7470577139844,-2.26440765265608,-3.21782650088165));
#82225=CARTESIAN_POINT('Ctrl Pts',(29.7529113256686,-2.16849496417907,-3.2832224224523));
#82226=CARTESIAN_POINT('Ctrl Pts',(29.7587649373529,-2.06995264619744,-3.34421665603475));
#82227=CARTESIAN_POINT('Ctrl Pts',(29.7646252034527,-1.97129830480545,-3.40528022817344));
#82228=CARTESIAN_POINT('Ctrl Pts',(29.7704854695526,-1.87000871889741,-3.4619319071041));
#82229=CARTESIAN_POINT('Ctrl Pts',(29.7763457356525,-1.7665216236375,-3.51395650986479));
#82230=CARTESIAN_POINT('Ctrl Pts',(29.7822099488238,-1.66296482660153,-3.56601615281288));
#82231=CARTESIAN_POINT('Ctrl Pts',(29.7880741619951,-1.55720794930092,-3.61344234532776));
#82232=CARTESIAN_POINT('Ctrl Pts',(29.7939383751664,-1.44970813762182,-3.65606828652216));
#82233=CARTESIAN_POINT('Ctrl Pts',(29.7998112237407,-1.3420500260706,-3.69875699695247));
#82234=CARTESIAN_POINT('Ctrl Pts',(29.805684072315,-1.23264424691249,-3.73663121371915));
#82235=CARTESIAN_POINT('Ctrl Pts',(29.8115569208893,-1.12196257586798,-3.76957411100401));
#82236=CARTESIAN_POINT('Ctrl Pts',(29.813151665502,-1.09190748481735,-3.77851960096657));
#82237=CARTESIAN_POINT('Ctrl Pts',(29.8147464101148,-1.06175836577921,-3.78710176321037));
#82238=CARTESIAN_POINT('Ctrl Pts',(29.8163411547275,-1.03152476454455,-3.7953189141535));
#82239=CARTESIAN_POINT('Ctrl Pts',(29.8222136008614,-0.920193336761872,
-3.8255775373226));
#82240=CARTESIAN_POINT('Ctrl Pts',(29.8280860469953,-0.807342982445388,
-3.85098399304252));
#82241=CARTESIAN_POINT('Ctrl Pts',(29.8339584931293,-0.693434587710648,
-3.87138702180066));
#82242=CARTESIAN_POINT('Ctrl Pts',(29.8398233320741,-0.579673750344011,
-3.89176362039768));
#82243=CARTESIAN_POINT('Ctrl Pts',(29.8456881710189,-0.464858001304861,
-3.90714960914067));
#82244=CARTESIAN_POINT('Ctrl Pts',(29.8515530099638,-0.349462757775396,
-3.91744365382937));
#82245=CARTESIAN_POINT('Ctrl Pts',(29.8574118200838,-0.234186136038471,
-3.92772711664315));
#82246=CARTESIAN_POINT('Ctrl Pts',(29.8632706302038,-0.118331613936684,
-3.93292901024229));
#82247=CARTESIAN_POINT('Ctrl Pts',(29.8691294403239,-0.0023834982782619,
-3.93299927776957));
#82248=CARTESIAN_POINT('Ctrl Pts',(29.8752152292048,0.118056614746108,-3.93307226756228));
#82249=CARTESIAN_POINT('Ctrl Pts',(29.8813010180858,0.238597272655179,-3.9276078962786));
#82250=CARTESIAN_POINT('Ctrl Pts',(29.8873868069668,0.358690904102268,-3.91660948210494));
#82251=CARTESIAN_POINT('Ctrl Pts',(29.8932388370451,0.474171667103122,-3.9060335236193));
#82252=CARTESIAN_POINT('Ctrl Pts',(29.8990908671233,0.589238661592703,-3.89034085313425));
#82253=CARTESIAN_POINT('Ctrl Pts',(29.9049428972016,0.703407185022154,-3.86958748861674));
#82254=CARTESIAN_POINT('Ctrl Pts',(29.9107940375801,0.817558351106234,-3.84883727928864));
#82255=CARTESIAN_POINT('Ctrl Pts',(29.9166451779586,0.930810911148064,-3.82302797963558));
#82256=CARTESIAN_POINT('Ctrl Pts',(29.9224963183372,1.04268874204003,-3.79226702477858));
#82257=CARTESIAN_POINT('Ctrl Pts',(29.9283479859047,1.15457665314818,-3.76150329835305));
#82258=CARTESIAN_POINT('Ctrl Pts',(29.9341996534722,1.26508919028757,-3.72578713942102));
#82259=CARTESIAN_POINT('Ctrl Pts',(29.9400513210397,1.37376450896226,-3.68527611908737));
#82260=CARTESIAN_POINT('Ctrl Pts',(29.9459049327239,1.48247593315799,-3.64475163965818));
#82261=CARTESIAN_POINT('Ctrl Pts',(29.9517585444082,1.58934853806043,-3.59942927552809));
#82262=CARTESIAN_POINT('Ctrl Pts',(29.9576121560924,1.69394027138842,-3.54951480585284));
#82263=CARTESIAN_POINT('Ctrl Pts',(29.9634724221923,1.79865090513289,-3.49954359315361));
#82264=CARTESIAN_POINT('Ctrl Pts',(29.9693326882922,1.90107511867518,-3.44497003344469));
#82265=CARTESIAN_POINT('Ctrl Pts',(29.9751929543921,2.00079521030422,-3.38604600181741));
#82266=CARTESIAN_POINT('Ctrl Pts',(29.9810571675634,2.10058246651529,-3.32708228302288));
#82267=CARTESIAN_POINT('Ctrl Pts',(29.9869213807347,2.19766162884491,-3.26376248300584));
#82268=CARTESIAN_POINT('Ctrl Pts',(29.992785593906,2.29164519943838,-3.19638096601313));
#82269=CARTESIAN_POINT('Ctrl Pts',(29.9986584424803,2.38576716643431,-3.12890022572548));
#82270=CARTESIAN_POINT('Ctrl Pts',(30.0045312910546,2.47678412021313,-3.05734608584746));
#82271=CARTESIAN_POINT('Ctrl Pts',(30.0104041396289,2.56434269189248,-2.98205223940454));
#82272=CARTESIAN_POINT('Ctrl Pts',(30.0119988842417,2.58811881326234,-2.96160654691442));
#82273=CARTESIAN_POINT('Ctrl Pts',(30.0135936288545,2.61164014201203,-2.94088530222528));
#82274=CARTESIAN_POINT('Ctrl Pts',(30.0151883734673,2.6349001003905,-2.91989562501164));
#82275=CARTESIAN_POINT('Ctrl Pts',(30.0210608196012,2.7205519668771,-2.84260378290915));
#82276=CARTESIAN_POINT('Ctrl Pts',(30.0269332657351,2.80294344598199,-2.76141058964439));
#82277=CARTESIAN_POINT('Ctrl Pts',(30.032805711869,2.88169809101305,-2.67662195915893));
#82278=CARTESIAN_POINT('Ctrl Pts',(30.0386705508139,2.96035071697719,-2.5919431641881));
#82279=CARTESIAN_POINT('Ctrl Pts',(30.0445353897587,3.03537559898794,-2.50367849426677));
#82280=CARTESIAN_POINT('Ctrl Pts',(30.0504002287036,3.10643043087439,-2.41217308212689));
#82281=CARTESIAN_POINT('Ctrl Pts',(30.0562590388236,3.17741222117548,-2.32076173396823));
#82282=CARTESIAN_POINT('Ctrl Pts',(30.0621178489436,3.24443182679994,-2.2261165943656));
#82283=CARTESIAN_POINT('Ctrl Pts',(30.0679766590636,3.30718526982313,-2.128618000268));
#82284=CARTESIAN_POINT('Ctrl Pts',(30.0740624479446,3.37236987181047,-2.02734216990075));
#82285=CARTESIAN_POINT('Ctrl Pts',(30.0801482368256,3.43295076194822,-1.92298765244804));
#82286=CARTESIAN_POINT('Ctrl Pts',(30.0862340257065,3.48863465409053,-1.8160168639852));
#82287=CARTESIAN_POINT('Ctrl Pts',(30.0920860557848,3.54217969452251,-1.7131548876951));
#82288=CARTESIAN_POINT('Ctrl Pts',(30.0979380858631,3.5911967823388,-1.60787431859592));
#82289=CARTESIAN_POINT('Ctrl Pts',(30.1037901159414,3.63547095672144,-1.50061318228079));
#82290=CARTESIAN_POINT('Ctrl Pts',(30.1096412563199,3.67973839998318,-1.39336835316249));
#82291=CARTESIAN_POINT('Ctrl Pts',(30.1154923966984,3.71926420587809,-1.28414393751746));
#82292=CARTESIAN_POINT('Ctrl Pts',(30.1213435370769,3.75388130514824,-1.17339854561805));
#82293=CARTESIAN_POINT('Ctrl Pts',(30.1271952046444,3.78850152342635,-1.06264317553542));
#82294=CARTESIAN_POINT('Ctrl Pts',(30.1330468722119,3.81821203254567,-0.950366951330369));
#82295=CARTESIAN_POINT('Ctrl Pts',(30.1388985397794,3.84289565867639,-0.837043581019613));
#82296=CARTESIAN_POINT('Ctrl Pts',(30.1447521514636,3.86758748552087,-0.723682560952003));
#82297=CARTESIAN_POINT('Ctrl Pts',(30.1506057631479,3.88724902056602,-0.6092741066811));
#82298=CARTESIAN_POINT('Ctrl Pts',(30.1564593748321,3.90181434487731,-0.494301343422853));
#82299=CARTESIAN_POINT('Ctrl Pts',(30.162319640932,3.91639622712365,-0.379197878540295));
#82300=CARTESIAN_POINT('Ctrl Pts',(30.1681799070319,3.92587028322505,-0.263529234560758));
#82301=CARTESIAN_POINT('Ctrl Pts',(30.1740401731318,3.93022253716149,-0.14778297732793));
#82302=CARTESIAN_POINT('Ctrl Pts',(30.1799043863031,3.93457772247626,-0.0319587613922855));
#82303=CARTESIAN_POINT('Ctrl Pts',(30.1857685994744,3.93380423934554,0.0839427595497822));
#82304=CARTESIAN_POINT('Ctrl Pts',(30.1916328126457,3.92794018554004,0.199436453086367));
#82305=CARTESIAN_POINT('Ctrl Pts',(30.19750566122,3.92206749656623,0.315100217961935));
#82306=CARTESIAN_POINT('Ctrl Pts',(30.2033785097943,3.91108931510681,0.430354546907637));
#82307=CARTESIAN_POINT('Ctrl Pts',(30.2092513583686,3.89509527653647,0.544721751634045));
#82308=CARTESIAN_POINT('Ctrl Pts',(30.2108461029814,3.89075217003141,0.575777632150334));
#82309=CARTESIAN_POINT('Ctrl Pts',(30.2124408475941,3.88603949758164,0.606768172738725));
#82310=CARTESIAN_POINT('Ctrl Pts',(30.2140355922069,3.88095969166349,0.637683990455502));
#82311=CARTESIAN_POINT('Ctrl Pts',(30.2199080383408,3.86225394631316,0.751527594487761));
#82312=CARTESIAN_POINT('Ctrl Pts',(30.2257804844747,3.83850342474694,0.864738032111168));
#82313=CARTESIAN_POINT('Ctrl Pts',(30.2316529306086,3.80976191591847,0.976833222212087));
#82314=CARTESIAN_POINT('Ctrl Pts',(30.2375177695534,3.78105763894991,1.08878320377716));
#82315=CARTESIAN_POINT('Ctrl Pts',(30.2433826084983,3.74737533370723,1.19962041409267));
#82316=CARTESIAN_POINT('Ctrl Pts',(30.2492474474431,3.70882024046955,1.30887028535427));
#82317=CARTESIAN_POINT('Ctrl Pts',(30.2551062575631,3.67030478035827,1.4180078520254));
#82318=CARTESIAN_POINT('Ctrl Pts',(30.2609650676831,3.62692663223362,1.52556093777231));
#82319=CARTESIAN_POINT('Ctrl Pts',(30.2668238778031,3.57884137495112,1.63106818157243));
#82320=CARTESIAN_POINT('Ctrl Pts',(30.2729096666841,3.52889322539274,1.740662928292));
#82321=CARTESIAN_POINT('Ctrl Pts',(30.2789954555651,3.47386598267881,1.848049669196));
#82322=CARTESIAN_POINT('Ctrl Pts',(30.2850812444461,3.41399005251188,1.95273165625744));
#82323=CARTESIAN_POINT('Ctrl Pts',(30.2909332745243,3.35641399275139,2.05339274538111));
#82324=CARTESIAN_POINT('Ctrl Pts',(30.2967853046026,3.29435508081834,2.15155263829803));
#82325=CARTESIAN_POINT('Ctrl Pts',(30.3026373346808,3.22806555623097,2.24679366312869));
#82326=CARTESIAN_POINT('Ctrl Pts',(30.3084884750593,3.16178610981697,2.34202020821212));
#82327=CARTESIAN_POINT('Ctrl Pts',(30.3143396154379,3.09127756569557,2.43432842837938));
#82328=CARTESIAN_POINT('Ctrl Pts',(30.3201907558164,3.01683537485756,2.52332980821138));
#82329=CARTESIAN_POINT('Ctrl Pts',(30.3260424233839,2.94238647676238,2.61233920708655));
#82330=CARTESIAN_POINT('Ctrl Pts',(30.3318940909514,2.86400349260866,2.69804085624789));
#82331=CARTESIAN_POINT('Ctrl Pts',(30.3377457585188,2.78202155271323,2.78008004925022));
#82332=CARTESIAN_POINT('Ctrl Pts',(30.3435993702031,2.70001237571666,2.86214649837504));
#82333=CARTESIAN_POINT('Ctrl Pts',(30.3494529818873,2.61440215744926,2.94054777959619));
#82334=CARTESIAN_POINT('Ctrl Pts',(30.3553065935715,2.52556166410646,3.01496721056727));
#82335=CARTESIAN_POINT('Ctrl Pts',(30.3611668596714,2.43662017643716,3.08947124192751));
#82336=CARTESIAN_POINT('Ctrl Pts',(30.3670271257713,2.34444140117678,3.15998412252751));
#82337=CARTESIAN_POINT('Ctrl Pts',(30.3728873918712,2.24942792608211,3.22623046377067));
#82338=CARTESIAN_POINT('Ctrl Pts',(30.3787516050425,2.15435045645802,3.29252142398425));
#82339=CARTESIAN_POINT('Ctrl Pts',(30.3846158182138,2.05643483363147,3.35453990219237));
#82340=CARTESIAN_POINT('Ctrl Pts',(30.3904800313851,1.95610975516662,3.41205563051689));
#82341=CARTESIAN_POINT('Ctrl Pts',(30.3963528799594,1.85563694205142,3.46965605417525));
#82342=CARTESIAN_POINT('Ctrl Pts',(30.4022257285336,1.75274795802705,3.52274030584411));
#82343=CARTESIAN_POINT('Ctrl Pts',(30.4080985771079,1.64789310550567,3.57112549665044));
#82344=CARTESIAN_POINT('Ctrl Pts',(30.4096933217208,1.61942025981996,3.58426426932691));
#82345=CARTESIAN_POINT('Ctrl Pts',(30.4112880663337,1.59080255057366,3.59705682986824));
#82346=CARTESIAN_POINT('Ctrl Pts',(30.4128828109465,1.56204918604753,3.60950015104145));
#82347=CARTESIAN_POINT('Ctrl Pts',(30.4187552570804,1.45616854347534,3.65532111367539));
#82348=CARTESIAN_POINT('Ctrl Pts',(30.4246277032144,1.34809276397599,3.6965560060263));
#82349=CARTESIAN_POINT('Ctrl Pts',(30.4305001493483,1.23825646271758,3.7329894096472));
#82350=CARTESIAN_POINT('Ctrl Pts',(30.4363649882931,1.12856244382185,3.76937561729839));
#82351=CARTESIAN_POINT('Ctrl Pts',(30.4422298272379,1.01711282716177,3.80097257638203));
#82352=CARTESIAN_POINT('Ctrl Pts',(30.4480946661828,0.904363727901238,3.82761221228804));
#82353=CARTESIAN_POINT('Ctrl Pts',(30.4539534763028,0.791730530300531,3.85422446369131));
#82354=CARTESIAN_POINT('Ctrl Pts',(30.4598122864228,0.677800906978657,3.8758894335315));
#82355=CARTESIAN_POINT('Ctrl Pts',(30.4656710965428,0.563047082020645,3.89248853349988));
#82356=CARTESIAN_POINT('Ctrl Pts',(30.4717568854238,0.443847528242206,3.90973070656102));
#82357=CARTESIAN_POINT('Ctrl Pts',(30.4778426743048,0.323759050963221,3.92150640983129));
#82358=CARTESIAN_POINT('Ctrl Pts',(30.4839284631858,0.203324101774599,3.92774086589703));
#82359=CARTESIAN_POINT('Ctrl Pts',(30.489780493264,0.0875151312516204,3.93373585276428));
#82360=CARTESIAN_POINT('Ctrl Pts',(30.4956325233423,-0.0286137347967784,
3.93460740202397));
#82361=CARTESIAN_POINT('Ctrl Pts',(30.5014845534205,-0.14457475857213,3.93034186034546));
#82362=CARTESIAN_POINT('Ctrl Pts',(30.507335693799,-0.260518152483535,3.92607696716864));
#82363=CARTESIAN_POINT('Ctrl Pts',(30.5131868341776,-0.376293341894099,
3.91667655113809));
#82364=CARTESIAN_POINT('Ctrl Pts',(30.5190379745561,-0.491413750794095,
3.90217907399577));
#82365=CARTESIAN_POINT('Ctrl Pts',(30.5248896421236,-0.606544532067361,
3.88768029062768));
#82366=CARTESIAN_POINT('Ctrl Pts',(30.5307413096911,-0.721020005409382,
3.86808358485917));
#82367=CARTESIAN_POINT('Ctrl Pts',(30.5365929772586,-0.834360580202792,
3.84347907789332));
#82368=CARTESIAN_POINT('Ctrl Pts',(30.5424465889428,-0.947738810468877,
3.81886639649971));
#82369=CARTESIAN_POINT('Ctrl Pts',(30.548300200627,-1.05998098870953,3.78924269327498));
#82370=CARTESIAN_POINT('Ctrl Pts',(30.5541538123112,-1.17062024183378,3.75474862666052));
#82371=CARTESIAN_POINT('Ctrl Pts',(30.5600140784111,-1.28138527022589,3.720215347015));
#82372=CARTESIAN_POINT('Ctrl Pts',(30.565874344511,-1.39054334156857,3.68080077610797));
#82373=CARTESIAN_POINT('Ctrl Pts',(30.5717346106109,-1.49764511319724,3.63669466891523));
#82374=CARTESIAN_POINT('Ctrl Pts',(30.5775988237822,-1.60481902119897,3.592558854888));
#82375=CARTESIAN_POINT('Ctrl Pts',(30.5834630369535,-1.70993349774922,3.54372538632));
#82376=CARTESIAN_POINT('Ctrl Pts',(30.5893272501248,-1.8125630382938,3.4904303792242));
#82377=CARTESIAN_POINT('Ctrl Pts',(30.5952000986991,-1.91534370694621,3.43705689205787));
#82378=CARTESIAN_POINT('Ctrl Pts',(30.6010729472734,-2.01563177981354,3.37920895994793));
#82379=CARTESIAN_POINT('Ctrl Pts',(30.6069457958477,-2.11302992602051,3.31716649141127));
#82380=CARTESIAN_POINT('Ctrl Pts',(30.6085405404605,-2.13947793791766,3.30031914872675));
#82381=CARTESIAN_POINT('Ctrl Pts',(30.6101352850733,-2.16571304229105,3.28316274507734));
#82382=CARTESIAN_POINT('Ctrl Pts',(30.6117300296861,-2.19172771359365,3.26570338969502));
#82383=CARTESIAN_POINT('Ctrl Pts',(30.6175826628863,-2.28720025993826,3.2016284261294));
#82384=CARTESIAN_POINT('Ctrl Pts',(30.6234352960864,-2.38002577654119,3.13325231778851));
#82385=CARTESIAN_POINT('Ctrl Pts',(30.6292879292865,-2.46978966200441,3.0608214625254));
#82386=CARTESIAN_POINT('Ctrl Pts',(30.6351329685946,-2.55943707728573,2.98848458754003));
#82387=CARTESIAN_POINT('Ctrl Pts',(30.6409780079027,-2.64603043913017,2.91210368561626));
#82388=CARTESIAN_POINT('Ctrl Pts',(30.6468230472108,-2.72918320320198,2.83196893403868));
#82389=CARTESIAN_POINT('Ctrl Pts',(30.6526620940125,-2.81225071661165,2.75191633896797));
#82390=CARTESIAN_POINT('Ctrl Pts',(30.6585011408142,-2.8918843493997,2.66811783541977));
#82391=CARTESIAN_POINT('Ctrl Pts',(30.6643401876159,-2.9677303752455,2.58090399276013));
#82392=CARTESIAN_POINT('Ctrl Pts',(30.6702691997138,-3.04474500110615,2.49234640009262));
#82393=CARTESIAN_POINT('Ctrl Pts',(30.6761982118117,-3.11785398546651,2.40026761360309));
#82394=CARTESIAN_POINT('Ctrl Pts',(30.6821272239096,-3.18672548496361,2.30505307606646));
#82395=CARTESIAN_POINT('Ctrl Pts',(30.6879596771534,-3.25447535526495,2.21138918583592));
#82396=CARTESIAN_POINT('Ctrl Pts',(30.6937921303972,-3.31812447955412,2.11469126848677));
#82397=CARTESIAN_POINT('Ctrl Pts',(30.699624583641,-3.37739792399084,2.01535909034156));
#82398=CARTESIAN_POINT('Ctrl Pts',(30.705456208986,-3.43666295474479,1.91604101209293));
#82399=CARTESIAN_POINT('Ctrl Pts',(30.711287834331,-3.49155332717248,1.81408977406003));
#82400=CARTESIAN_POINT('Ctrl Pts',(30.717119459676,-3.54183850283713,1.709932460602));
#82401=CARTESIAN_POINT('Ctrl Pts',(30.7229516944836,-3.59212893380038,1.60576426167373));
#82402=CARTESIAN_POINT('Ctrl Pts',(30.7287839292912,-3.63781303043699,1.49938990421546));
#82403=CARTESIAN_POINT('Ctrl Pts',(30.7346161640988,-3.67870744569314,1.3912586132714));
#82404=CARTESIAN_POINT('Ctrl Pts',(30.740617856921,-3.72079006523903,1.27998552257424));
#82405=CARTESIAN_POINT('Ctrl Pts',(30.7466195497432,-3.75780023394118,1.16685227392636));
#82406=CARTESIAN_POINT('Ctrl Pts',(30.7526212425654,-3.78959289579709,1.05236623098816));
#82407=CARTESIAN_POINT('Ctrl Pts',(30.7584622457792,-3.82053433941606,0.940945442795381));
#82408=CARTESIAN_POINT('Ctrl Pts',(30.764303248993,-3.84653408883727,0.828243806335129));
#82409=CARTESIAN_POINT('Ctrl Pts',(30.7701442522068,-3.86751042118617,0.714739212591838));
#82410=CARTESIAN_POINT('Ctrl Pts',(30.7762262898332,-3.88935236133569,0.596550746562568));
#82411=CARTESIAN_POINT('Ctrl Pts',(30.7823083274596,-3.90574732588091,0.477492137902916));
#82412=CARTESIAN_POINT('Ctrl Pts',(30.788390365086,-3.91666289591793,0.358107190293335));
#82413=CARTESIAN_POINT('Ctrl Pts',(30.7944724027123,-3.92757846595495,0.238722242683717));
#82414=CARTESIAN_POINT('Ctrl Pts',(30.8005544403387,-3.9330146910959,0.119011460734204));
#82415=CARTESIAN_POINT('Ctrl Pts',(30.8066364779651,-3.9329999701559,-0.000484513865750852));
#82416=CARTESIAN_POINT('',(32.0566364779651,-3.93299836096378,0.0035906345187518));
#82417=CARTESIAN_POINT('Ctrl Pts',(30.8066364779651,-3.93943799754381,-0.000485306978784902));
#82418=CARTESIAN_POINT('Ctrl Pts',(30.8079500681187,-3.9394828345648,-0.026336136481718));
#82419=CARTESIAN_POINT('Ctrl Pts',(30.8092636582722,-3.93925047646468,-0.0521861383401698));
#82420=CARTESIAN_POINT('Ctrl Pts',(30.8768596546724,-3.91290316029452,-1.38211552106476));
#82421=CARTESIAN_POINT('Ctrl Pts',(31.0094244671653,-2.43720376157095,-3.96207383771694));
#82422=CARTESIAN_POINT('Ctrl Pts',(31.2082716859051,2.01511080184506,-4.19253142233196));
#82423=CARTESIAN_POINT('Ctrl Pts',(31.4071189046448,4.61638584894327,-0.571815498755066));
#82424=CARTESIAN_POINT('Ctrl Pts',(31.6059661233843,2.97714339143227,3.57415843210569));
#82425=CARTESIAN_POINT('Ctrl Pts',(31.8048133421241,-1.39684201829475,4.43698362030694));
#82426=CARTESIAN_POINT('Ctrl Pts',(31.9550365843866,-3.73190738848403,2.00973408201049));
#82427=CARTESIAN_POINT('Ctrl Pts',(32.0389774204028,-3.93478407738548,0.352892674307761));
#82428=CARTESIAN_POINT('Ctrl Pts',(32.0566358501724,-3.93168473390337,0.00360185313312367));
#82429=CARTESIAN_POINT('',(33.3066367910396,-3.93066234985505,-0.00113524685437975));
#82430=CARTESIAN_POINT('Ctrl Pts',(32.0566364779651,-3.93299836096378,0.0035906345187518));
#82431=CARTESIAN_POINT('Ctrl Pts',(32.0627144488667,-3.93310815591637,-0.116673170205319));
#82432=CARTESIAN_POINT('Ctrl Pts',(32.0687924197683,-3.92769665718947,-0.237065644027127));
#82433=CARTESIAN_POINT('Ctrl Pts',(32.0748703906699,-3.91676081377956,-0.357034630870517));
#82434=CARTESIAN_POINT('Ctrl Pts',(32.0806648687197,-3.90633504741434,-0.471407942650909));
#82435=CARTESIAN_POINT('Ctrl Pts',(32.0864593467694,-3.89088869568617,-0.585395908830107));
#82436=CARTESIAN_POINT('Ctrl Pts',(32.0922538248192,-3.8704724238071,-0.698521450313995));
#82437=CARTESIAN_POINT('Ctrl Pts',(32.0980469710849,-3.85006084433813,-0.811620991388227));
#82438=CARTESIAN_POINT('Ctrl Pts',(32.1038401173505,-3.82468168979032,-0.923858086228779));
#82439=CARTESIAN_POINT('Ctrl Pts',(32.1096332636162,-3.79443712046992,-1.03476371157863));
#82440=CARTESIAN_POINT('Ctrl Pts',(32.1154265492162,-3.76419182371933,-1.14567200438586));
#82441=CARTESIAN_POINT('Ctrl Pts',(32.1212198348163,-3.72908099129357,-1.25524835663895));
#82442=CARTESIAN_POINT('Ctrl Pts',(32.1270131204164,-3.68925702660706,-1.36303763397436));
#82443=CARTESIAN_POINT('Ctrl Pts',(32.1328080163116,-3.64942199249616,-1.47085687229595));
#82444=CARTESIAN_POINT('Ctrl Pts',(32.1386029122068,-3.60487136932325,-1.57688765259656));
#82445=CARTESIAN_POINT('Ctrl Pts',(32.144397808102,-3.55580587480623,-1.68069437456473));
#82446=CARTESIAN_POINT('Ctrl Pts',(32.1501990994925,-3.50668622950756,-1.78461566207819));
#82447=CARTESIAN_POINT('Ctrl Pts',(32.1560003908831,-3.45304194941713,-1.88630761058477));
#82448=CARTESIAN_POINT('Ctrl Pts',(32.1618016822737,-3.39511992355919,-1.98535883523645));
#82449=CARTESIAN_POINT('Ctrl Pts',(32.1676067205749,-3.33716048729706,-2.08447403462477));
#82450=CARTESIAN_POINT('Ctrl Pts',(32.1734117588761,-3.27491803530903,-2.18094476193633));
#82451=CARTESIAN_POINT('Ctrl Pts',(32.1792167971773,-3.20868197266625,-2.27438980790158));
#82452=CARTESIAN_POINT('Ctrl Pts',(32.1850305171287,-3.14234685153438,-2.36797460439998));
#82453=CARTESIAN_POINT('Ctrl Pts',(32.1908442370801,-3.07200646015585,-2.45852435822425));
#82454=CARTESIAN_POINT('Ctrl Pts',(32.1966579570314,-2.99798951063316,-2.54569202656832));
#82455=CARTESIAN_POINT('Ctrl Pts',(32.1986078978887,-2.9731639815029,-2.57492835018944));
#82456=CARTESIAN_POINT('Ctrl Pts',(32.200557838746,-2.94792515245973,-2.60378452284406));
#82457=CARTESIAN_POINT('Ctrl Pts',(32.2025077796034,-2.9222862884835,-2.63224843966927));
#82458=CARTESIAN_POINT('Ctrl Pts',(32.2083802257373,-2.84507222987714,-2.71797043359014));
#82459=CARTESIAN_POINT('Ctrl Pts',(32.2142526718712,-2.76395386205481,-2.80043558297738));
#82460=CARTESIAN_POINT('Ctrl Pts',(32.2201251180051,-2.6792367571074,-2.87926716359643));
#82461=CARTESIAN_POINT('Ctrl Pts',(32.22598995695,-2.5946293950203,-2.95799662548579));
#82462=CARTESIAN_POINT('Ctrl Pts',(32.2318547958948,-2.50643286632609,-3.03310160004337));
#82463=CARTESIAN_POINT('Ctrl Pts',(32.2377196348396,-2.41499199288139,-3.10423946794038));
#82464=CARTESIAN_POINT('Ctrl Pts',(32.2435784449597,-2.32364511707433,-3.17530420889451));
#82465=CARTESIAN_POINT('Ctrl Pts',(32.2494372550797,-2.22906085442845,-3.2424097023228));
#82466=CARTESIAN_POINT('Ctrl Pts',(32.2552960651997,-2.13161926579595,-3.30525162516979));
#82467=CARTESIAN_POINT('Ctrl Pts',(32.2613818540807,-2.03040264936802,-3.37052813481688));
#82468=CARTESIAN_POINT('Ctrl Pts',(32.2674676429617,-1.92610316804087,-3.43120372923139));
#82469=CARTESIAN_POINT('Ctrl Pts',(32.2735534318426,-1.81918297146479,-3.48698470262382));
#82470=CARTESIAN_POINT('Ctrl Pts',(32.2794054619209,-1.71636964379681,-3.5406230953568));
#82471=CARTESIAN_POINT('Ctrl Pts',(32.2852574919992,-1.61113361400549,-3.58973573285033));
#82472=CARTESIAN_POINT('Ctrl Pts',(32.2911095220774,-1.50391271236987,-3.63410725675128));
#82473=CARTESIAN_POINT('Ctrl Pts',(32.296960662456,-1.39670811181402,-3.67847203473106));
#82474=CARTESIAN_POINT('Ctrl Pts',(32.3028118028345,-1.28751962126107,-3.71809697429432));
#82475=CARTESIAN_POINT('Ctrl Pts',(32.308662943213,-1.17680569913497,-3.75281458994226));
#82476=CARTESIAN_POINT('Ctrl Pts',(32.3145146107805,-1.06608180166135,-3.78753533365462));
#82477=CARTESIAN_POINT('Ctrl Pts',(32.320366278348,-0.953832593836438,-3.81734775080719));
#82478=CARTESIAN_POINT('Ctrl Pts',(32.3262179459154,-0.840531677115653,
-3.84213423760352));
#82479=CARTESIAN_POINT('Ctrl Pts',(32.3320715575997,-0.727193118097655,
-3.86692895928734));
#82480=CARTESIAN_POINT('Ctrl Pts',(32.3379251692839,-0.612802558991906,
-3.88669434206711));
#82481=CARTESIAN_POINT('Ctrl Pts',(32.3437787809681,-0.497843064976492,
-3.90136402847194));
#82482=CARTESIAN_POINT('Ctrl Pts',(32.349639047068,-0.382752884421308,-3.91605039145118));
#82483=CARTESIAN_POINT('Ctrl Pts',(32.3554993131679,-0.267092888303129,
-3.92562944343905));
#82484=CARTESIAN_POINT('Ctrl Pts',(32.3613595792678,-0.151350629577838,
-3.93008676582673));
#82485=CARTESIAN_POINT('Ctrl Pts',(32.3672237924391,-0.0355304148425893,
-3.93454709035962));
#82486=CARTESIAN_POINT('Ctrl Pts',(32.3730880056104,0.0803717604859929,
-3.93387881873478));
#82487=CARTESIAN_POINT('Ctrl Pts',(32.3789522187817,0.195870729612114,-3.92811960832167));
#82488=CARTESIAN_POINT('Ctrl Pts',(32.384825067356,0.311539777845725,-3.9223519171284));
#82489=CARTESIAN_POINT('Ctrl Pts',(32.3906979159303,0.426804024898627,-3.911478363882));
#82490=CARTESIAN_POINT('Ctrl Pts',(32.3965707645046,0.541185701310483,-3.89558815029221));
#82491=CARTESIAN_POINT('Ctrl Pts',(32.3981655091174,0.572245511545825,-3.89127323697584));
#82492=CARTESIAN_POINT('Ctrl Pts',(32.3997602537302,0.603240317358721,-3.88658869855381));
#82493=CARTESIAN_POINT('Ctrl Pts',(32.401354998343,0.634160733601198,-3.88153695898395));
#82494=CARTESIAN_POINT('Ctrl Pts',(32.4072274444769,0.748021271123717,-3.86293456442569));
#82495=CARTESIAN_POINT('Ctrl Pts',(32.4130998906108,0.8612532219627,-3.83928682096459));
#82496=CARTESIAN_POINT('Ctrl Pts',(32.4189723367447,0.973374456375479,-3.81064707991645));
#82497=CARTESIAN_POINT('Ctrl Pts',(32.4248371756896,1.08535044851462,-3.78204443889782));
#82498=CARTESIAN_POINT('Ctrl Pts',(32.4307020146344,1.19621818873576,-3.74846276152279));
#82499=CARTESIAN_POINT('Ctrl Pts',(32.4365668535793,1.30550301389679,-3.71000685723172));
#82500=CARTESIAN_POINT('Ctrl Pts',(32.4424256636993,1.41467549853607,-3.67159048410471));
#82501=CARTESIAN_POINT('Ctrl Pts',(32.4482844738193,1.52226791707535,-3.62830998663364));
#82502=CARTESIAN_POINT('Ctrl Pts',(32.4541432839394,1.62781876745331,-3.58032052480316));
#82503=CARTESIAN_POINT('Ctrl Pts',(32.4602290728203,1.73745881013218,-3.53047188195104));
#82504=CARTESIAN_POINT('Ctrl Pts',(32.4663148617013,1.84489545852133,-3.47554214368864));
#82505=CARTESIAN_POINT('Ctrl Pts',(32.4724006505823,1.94963175564452,-3.41576126469378));
#82506=CARTESIAN_POINT('Ctrl Pts',(32.4782526806605,2.05034506874808,-3.3582766051327));
#82507=CARTESIAN_POINT('Ctrl Pts',(32.4841047107388,2.14856125604564,-3.29630682475106));
#82508=CARTESIAN_POINT('Ctrl Pts',(32.4899567408171,2.24386241685593,-3.23010378381585));
#82509=CARTESIAN_POINT('Ctrl Pts',(32.4958078811956,2.33914908877641,-3.16391080790563));
#82510=CARTESIAN_POINT('Ctrl Pts',(32.5016590215741,2.43152127600425,-3.09348608688119));
#82511=CARTESIAN_POINT('Ctrl Pts',(32.5075101619526,2.52059019508077,-3.01912471893141));
#82512=CARTESIAN_POINT('Ctrl Pts',(32.5133618295201,2.60966713928554,-2.94475665100682));
#82513=CARTESIAN_POINT('Ctrl Pts',(32.5192134970876,2.69543990635964,-2.86645149598967));
#82514=CARTESIAN_POINT('Ctrl Pts',(32.5250651646551,2.77755348578489,-2.78454406206908));
#82515=CARTESIAN_POINT('Ctrl Pts',(32.5309187763394,2.8596943460465,-2.70260941580047));
#82516=CARTESIAN_POINT('Ctrl Pts',(32.5367723880236,2.93817330880889,-2.61707040263851));
#82517=CARTESIAN_POINT('Ctrl Pts',(32.5426259997078,3.01267335528806,-2.52829750115318));
#82518=CARTESIAN_POINT('Ctrl Pts',(32.5484862658077,3.08725809380044,-2.43942368218017));
#82519=CARTESIAN_POINT('Ctrl Pts',(32.5543465319076,3.15785462188899,-2.34730895392833));
#82520=CARTESIAN_POINT('Ctrl Pts',(32.5602067980075,3.22418718561602,-2.25235565400082));
#82521=CARTESIAN_POINT('Ctrl Pts',(32.5660710111788,3.29056442638678,-2.15733840007403));
#82522=CARTESIAN_POINT('Ctrl Pts',(32.5719352243501,3.35267176328473,-2.05947911571031));
#82523=CARTESIAN_POINT('Ctrl Pts',(32.5777994375214,3.41027853937052,-1.9592062892684));
#82524=CARTESIAN_POINT('Ctrl Pts',(32.5836722860957,3.46797014486351,-1.85878580512019));
#82525=CARTESIAN_POINT('Ctrl Pts',(32.58954513467,3.52114777353984,-1.75594505144156));
#82526=CARTESIAN_POINT('Ctrl Pts',(32.5954179832442,3.56962812783369,-1.65113416443927));
#82527=CARTESIAN_POINT('Ctrl Pts',(32.597012727857,3.5827927417104,-1.62267325738612));
#82528=CARTESIAN_POINT('Ctrl Pts',(32.5986074724699,3.59561127509653,-1.5940671725533));
#82529=CARTESIAN_POINT('Ctrl Pts',(32.6002022170827,3.60808069240139,-1.56532511546973));
#82530=CARTESIAN_POINT('Ctrl Pts',(32.6060746632166,3.65399775075439,-1.45948611112614));
#82531=CARTESIAN_POINT('Ctrl Pts',(32.6119471093505,3.69533073337939,-1.35144780769194));
#82532=CARTESIAN_POINT('Ctrl Pts',(32.6178195554844,3.73186382739031,-1.24164462460713));
#82533=CARTESIAN_POINT('Ctrl Pts',(32.6236843944293,3.76834959629215,-1.13198368098376));
#82534=CARTESIAN_POINT('Ctrl Pts',(32.6295492333741,3.80004771226752,-1.02056279281366));
#82535=CARTESIAN_POINT('Ctrl Pts',(32.6354140723189,3.82678968673084,-0.907837922500752));
#82536=CARTESIAN_POINT('Ctrl Pts',(32.641272882439,3.85350417149142,-0.795228928941078));
#82537=CARTESIAN_POINT('Ctrl Pts',(32.647131692559,3.87527255357542,-0.681319019232035));
#82538=CARTESIAN_POINT('Ctrl Pts',(32.652990502679,3.8919758160551,-0.566580309613941));
#82539=CARTESIAN_POINT('Ctrl Pts',(32.65907629156,3.90932618703355,-0.447396456765771));
#82540=CARTESIAN_POINT('Ctrl Pts',(32.665162080441,3.92121089740585,-0.327318718520768));
#82541=CARTESIAN_POINT('Ctrl Pts',(32.6712478693219,3.92755467737133,-0.206889478366118));
#82542=CARTESIAN_POINT('Ctrl Pts',(32.6770998994002,3.93365478894175,-0.0910859975893578));
#82543=CARTESIAN_POINT('Ctrl Pts',(32.6829519294785,3.93463175540505,0.0250420294514206));
#82544=CARTESIAN_POINT('Ctrl Pts',(32.6888039595567,3.9304714806856,0.141006877552701));
#82545=CARTESIAN_POINT('Ctrl Pts',(32.6946550999352,3.92631183846382,0.256954095208426));
#82546=CARTESIAN_POINT('Ctrl Pts',(32.7005062403138,3.91701652281431,0.372737770273564));
#82547=CARTESIAN_POINT('Ctrl Pts',(32.7063573806923,3.90262355376715,0.487871292024686));
#82548=CARTESIAN_POINT('Ctrl Pts',(32.7122090482598,3.88822928791041,0.603015187330697));
#82549=CARTESIAN_POINT('Ctrl Pts',(32.7180607158273,3.86873650688895,0.717508402684074));
#82550=CARTESIAN_POINT('Ctrl Pts',(32.7239123833948,3.84423489651378,0.83087126585631));
#82551=CARTESIAN_POINT('Ctrl Pts',(32.729765995079,3.81972514589652,0.944271791906046));
#82552=CARTESIAN_POINT('Ctrl Pts',(32.7356196067633,3.79020334424603,1.05654081522187));
#82553=CARTESIAN_POINT('Ctrl Pts',(32.7414732184475,3.75580972613532,1.16721133522054));
#82554=CARTESIAN_POINT('Ctrl Pts',(32.7473334845474,3.72137700918388,1.27800766603159));
#82555=CARTESIAN_POINT('Ctrl Pts',(32.7531937506473,3.68206154424488,1.38720147151405));
#82556=CARTESIAN_POINT('Ctrl Pts',(32.7590540167472,3.63805267831903,1.4943432369358));
#82557=CARTESIAN_POINT('Ctrl Pts',(32.7649182299185,3.59401417105377,1.60155716566751));
#82558=CARTESIAN_POINT('Ctrl Pts',(32.7707824430898,3.54527614170624,1.70671592815627));
#82559=CARTESIAN_POINT('Ctrl Pts',(32.7766466562611,3.49207431993456,1.80939380568565));
#82560=CARTESIAN_POINT('Ctrl Pts',(32.7825195048354,3.43879415531324,1.91222288250206));
#82561=CARTESIAN_POINT('Ctrl Pts',(32.7883923534097,3.38103728490401,2.01256342629882));
#82562=CARTESIAN_POINT('Ctrl Pts',(32.794265201984,3.3190832564259,2.11001785227359));
#82563=CARTESIAN_POINT('Ctrl Pts',(32.7958599465968,3.30225992922728,2.13648114667755));
#82564=CARTESIAN_POINT('Ctrl Pts',(32.7974546912095,3.28512734792143,2.1627318141998));
#82565=CARTESIAN_POINT('Ctrl Pts',(32.7990494358223,3.2676916149064,2.18876232375066));
#82566=CARTESIAN_POINT('Ctrl Pts',(32.8049218819562,3.20348672459517,2.2846163959034));
#82567=CARTESIAN_POINT('Ctrl Pts',(32.81079432809,3.13495310760068,2.37780348622807));
#82568=CARTESIAN_POINT('Ctrl Pts',(32.8166667742239,3.06233950919108,2.46790715596178));
#82569=CARTESIAN_POINT('Ctrl Pts',(32.8225316131688,2.98981997471313,2.55789410505891));
#82570=CARTESIAN_POINT('Ctrl Pts',(32.8283964521136,2.91323122623499,2.64480525787337));
#82571=CARTESIAN_POINT('Ctrl Pts',(32.8342612910584,2.83286571989194,2.72825233676453));
#82572=CARTESIAN_POINT('Ctrl Pts',(32.8401201011784,2.75258282614324,2.8116136353254));
#82573=CARTESIAN_POINT('Ctrl Pts',(32.8459789112984,2.66853118177182,2.89151764690684));
#82574=CARTESIAN_POINT('Ctrl Pts',(32.8518377214184,2.58104358149604,2.96760897532308));
#82575=CARTESIAN_POINT('Ctrl Pts',(32.8579235102994,2.4901665853012,3.04664819163654));
#82576=CARTESIAN_POINT('Ctrl Pts',(32.8640092991804,2.39558230608856,3.12157297851322));
#82577=CARTESIAN_POINT('Ctrl Pts',(32.8700950880614,2.29770630253051,3.19202674602071));
#82578=CARTESIAN_POINT('Ctrl Pts',(32.8759471181396,2.20358977500006,3.25977434204214));
#82579=CARTESIAN_POINT('Ctrl Pts',(32.8817991482179,2.10643009924294,3.32338778821915));
#82580=CARTESIAN_POINT('Ctrl Pts',(32.8876511782961,2.00662993215558,3.38259150879578));
#82581=CARTESIAN_POINT('Ctrl Pts',(32.8935023186746,1.90684493795386,3.44178622847283));
#82582=CARTESIAN_POINT('Ctrl Pts',(32.8993534590531,1.80442060602961,3.49657234472912));
#82583=CARTESIAN_POINT('Ctrl Pts',(32.9052045994316,1.69978683548065,3.54671872495222));
#82584=CARTESIAN_POINT('Ctrl Pts',(32.9110562669991,1.59514363740686,3.59686962337476));
#82585=CARTESIAN_POINT('Ctrl Pts',(32.9169079345666,1.48829097775519,3.64237977607909));
#82586=CARTESIAN_POINT('Ctrl Pts',(32.9227596021341,1.37968085511645,3.68306526388349));
#82587=CARTESIAN_POINT('Ctrl Pts',(32.9286132138183,1.27103464861707,3.72376426874721));
#82588=CARTESIAN_POINT('Ctrl Pts',(32.9344668255026,1.16063020499076,3.7596352764898));
#82589=CARTESIAN_POINT('Ctrl Pts',(32.9403204371868,1.04893619556056,3.79054374168706));
#82590=CARTESIAN_POINT('Ctrl Pts',(32.9461807032867,0.93711521181,3.82148734378541));
#82591=CARTESIAN_POINT('Ctrl Pts',(32.9520409693866,0.824002134818662,3.84745703289744));
#82592=CARTESIAN_POINT('Ctrl Pts',(32.9579012354864,0.710077482248281,3.86836903218966));
#82593=CARTESIAN_POINT('Ctrl Pts',(32.9637654486577,0.596076097882421,3.88929511636356));
#82594=CARTESIAN_POINT('Ctrl Pts',(32.969629661829,0.481262457970925,3.90515667123887));
#82595=CARTESIAN_POINT('Ctrl Pts',(32.9754938750003,0.36612214233278,3.91592180423635));
#82596=CARTESIAN_POINT('Ctrl Pts',(32.9813667235746,0.250812275725717,3.92670278953299));
#82597=CARTESIAN_POINT('Ctrl Pts',(32.9872395721489,0.135175184620491,3.9323723547306));
#82598=CARTESIAN_POINT('Ctrl Pts',(32.9931124207232,0.0196964752109615,
3.93295067968876));
#82599=CARTESIAN_POINT('Ctrl Pts',(32.9947071653361,-0.0116612292154589,
3.93310772113123));
#82600=CARTESIAN_POINT('Ctrl Pts',(32.996301909949,-0.0430072868758966,
3.93288964572984));
#82601=CARTESIAN_POINT('Ctrl Pts',(32.9978966545618,-0.0743320629214669,
3.93229751473891));
#82602=CARTESIAN_POINT('Ctrl Pts',(33.0037691006957,-0.189681604470987,
3.93011706696041));
#82603=CARTESIAN_POINT('Ctrl Pts',(33.0096415468297,-0.305128243973245,
3.92285319132686));
#82604=CARTESIAN_POINT('Ctrl Pts',(33.0155139929636,-0.420187170315274,
3.9104899618721));
#82605=CARTESIAN_POINT('Ctrl Pts',(33.0213788319084,-0.535097048886176,
3.89814274779183));
#82606=CARTESIAN_POINT('Ctrl Pts',(33.0272436708533,-0.649619805881446,
3.88070936007733));
#82607=CARTESIAN_POINT('Ctrl Pts',(33.0331085097981,-0.763270684661763,
3.85822586974065));
#82608=CARTESIAN_POINT('Ctrl Pts',(33.0389673199181,-0.876804734788063,
3.83576549155181));
#82609=CARTESIAN_POINT('Ctrl Pts',(33.0448261300381,-0.989468286339254,
3.80826541627433));
#82610=CARTESIAN_POINT('Ctrl Pts',(33.0506849401581,-1.10078243136404,3.77581342743524));
#82611=CARTESIAN_POINT('Ctrl Pts',(33.0567707290391,-1.21640904704381,3.74210420170561));
#82612=CARTESIAN_POINT('Ctrl Pts',(33.0628565179201,-1.33057913389214,3.70305166232924));
#82613=CARTESIAN_POINT('Ctrl Pts',(33.0689423068011,-1.44276802845002,3.65881256913803));
#82614=CARTESIAN_POINT('Ctrl Pts',(33.0747943368793,-1.55064768024876,3.61627272606205));
#82615=CARTESIAN_POINT('Ctrl Pts',(33.0806463669576,-1.65669510975156,3.56893758241947));
#82616=CARTESIAN_POINT('Ctrl Pts',(33.0864983970359,-1.76046077946921,3.51699685014796));
#82617=CARTESIAN_POINT('Ctrl Pts',(33.0923495374144,-1.86421067341505,3.46506401456465));
#82618=CARTESIAN_POINT('Ctrl Pts',(33.0982006777929,-1.96567912779575,3.40852716755154));
#82619=CARTESIAN_POINT('Ctrl Pts',(33.1040518181714,-2.06443926095335,3.34762296829174));
#82620=CARTESIAN_POINT('Ctrl Pts',(33.1099034857389,-2.16320829241994,3.28671328155064));
#82621=CARTESIAN_POINT('Ctrl Pts',(33.1157551533064,-2.2592681657184,3.22143567730739));
#82622=CARTESIAN_POINT('Ctrl Pts',(33.1216068208739,-2.35221976612745,3.15207093382102));
#82623=CARTESIAN_POINT('Ctrl Pts',(33.1274604325581,-2.44520224811983,3.0826831450821));
#82624=CARTESIAN_POINT('Ctrl Pts',(33.1333140442423,-2.53507407271398,3.00920576412062));
#82625=CARTESIAN_POINT('Ctrl Pts',(33.1391676559265,-2.62146864371653,2.93196029134281));
#82626=CARTESIAN_POINT('Ctrl Pts',(33.1450279220264,-2.70796142850888,2.85462700551682));
#82627=CARTESIAN_POINT('Ctrl Pts',(33.1508881881263,-2.79096876140429,2.77351735365818));
#82628=CARTESIAN_POINT('Ctrl Pts',(33.1567484542262,-2.87016034776382,2.68899025251566));
#82629=CARTESIAN_POINT('Ctrl Pts',(33.1626126673975,-2.94940527211877,2.60440621974265));
#82630=CARTESIAN_POINT('Ctrl Pts',(33.1684768805688,-3.02482906417223,2.51640046751559));
#82631=CARTESIAN_POINT('Ctrl Pts',(33.1743410937401,-3.09614233762215,2.42536422526259));
#82632=CARTESIAN_POINT('Ctrl Pts',(33.1802139423144,-3.1675606241126,2.33419392672339));
#82633=CARTESIAN_POINT('Ctrl Pts',(33.1860867908887,-3.2348560720885,2.23998456683498));
#82634=CARTESIAN_POINT('Ctrl Pts',(33.1919596394629,-3.29778308478639,2.14315555331309));
#82635=CARTESIAN_POINT('Ctrl Pts',(33.1935543840758,-3.31487062130878,2.11686208673897));
#82636=CARTESIAN_POINT('Ctrl Pts',(33.1951491286887,-3.33163630867265,2.09037558800984));
#82637=CARTESIAN_POINT('Ctrl Pts',(33.1967438733015,-3.34807582995316,2.06370473587755));
#82638=CARTESIAN_POINT('Ctrl Pts',(33.2027912381652,-3.41041545635189,1.96256730436164));
#82639=CARTESIAN_POINT('Ctrl Pts',(33.2088386030289,-3.46825976736853,1.85845523200901));
#82640=CARTESIAN_POINT('Ctrl Pts',(33.2148859678926,-3.52132262059677,1.75179222560025));
#82641=CARTESIAN_POINT('Ctrl Pts',(33.2209239767828,-3.57430337944903,1.64529423920869));
#82642=CARTESIAN_POINT('Ctrl Pts',(33.226961985673,-3.62251723791411,1.53625351206916));
#82643=CARTESIAN_POINT('Ctrl Pts',(33.2329999945633,-3.66572201704252,1.42512143123654));
#82644=CARTESIAN_POINT('Ctrl Pts',(33.2391363681801,-3.70963064181988,1.31217890644078));
#82645=CARTESIAN_POINT('Ctrl Pts',(33.2452727417969,-3.74836531030906,1.19707660729187));
#82646=CARTESIAN_POINT('Ctrl Pts',(33.2514091154137,-3.78172039376651,1.08031470570869));
#82647=CARTESIAN_POINT('Ctrl Pts',(33.2574297674202,-3.81444645685911,0.965754735774939));
#82648=CARTESIAN_POINT('Ctrl Pts',(33.2634504194266,-3.84199391261333,0.849597585619082));
#82649=CARTESIAN_POINT('Ctrl Pts',(33.2694710714331,-3.86421710185485,0.732335435256624));
#82650=CARTESIAN_POINT('Ctrl Pts',(33.2756653058551,-3.88708101154747,0.611692480408314));
#82651=CARTESIAN_POINT('Ctrl Pts',(33.2818595402771,-3.90430882981542,0.489880217607703));
#82652=CARTESIAN_POINT('Ctrl Pts',(33.2880537746991,-3.91579739769619,0.367450323439404));
#82653=CARTESIAN_POINT('Ctrl Pts',(33.2942480091211,-3.92728596557697,0.245020429271104));
#82654=CARTESIAN_POINT('Ctrl Pts',(33.3004422435431,-3.93303519759643,0.121973337018079));
#82655=CARTESIAN_POINT('Ctrl Pts',(33.3066364779651,-3.93299983775287,-0.00112970610199267));
#82656=CARTESIAN_POINT('',(34.5566364779651,-3.93583466796628,-0.0031786779811645));
#82657=CARTESIAN_POINT('Ctrl Pts',(33.3066373091263,-3.9267941936085,-0.00114441588407893));
#82658=CARTESIAN_POINT('Ctrl Pts',(33.3362885700978,-3.92829771108111,-0.589498635609008));
#82659=CARTESIAN_POINT('Ctrl Pts',(33.4322222373162,-3.52779483796851,-2.49110991178401));
#82660=CARTESIAN_POINT('Ctrl Pts',(33.5944383107807,-0.576005850405059,
-4.61586487358942));
#82661=CARTESIAN_POINT('Ctrl Pts',(33.7932855295205,3.57145441695431,-2.98038665588391));
#82662=CARTESIAN_POINT('Ctrl Pts',(33.99213274826,4.43824979459357,1.39281371034701));
#82663=CARTESIAN_POINT('Ctrl Pts',(34.1909799669998,1.22815979920724,4.48660392485808));
#82664=CARTESIAN_POINT('Ctrl Pts',(34.3791478769013,-2.87710201293364,3.51427533050346));
#82665=CARTESIAN_POINT('Ctrl Pts',(34.5010333805565,-3.9262035401934,1.09370000885035));
#82666=CARTESIAN_POINT('Ctrl Pts',(34.5566364779651,-3.93583466796628,-0.0031786779811645));
#82667=CARTESIAN_POINT('',(35.8066364779651,-3.93429339661999,0.00268599589076086));
#82668=CARTESIAN_POINT('Ctrl Pts',(34.5566364779651,-3.93583466796628,-0.0031786779811645));
#82669=CARTESIAN_POINT('Ctrl Pts',(34.5673157868031,-3.93768445318938,-0.213848708976004));
#82670=CARTESIAN_POINT('Ctrl Pts',(34.6442775018874,-3.82634700125658,-1.7301091391965));
#82671=CARTESIAN_POINT('Ctrl Pts',(34.7875216232188,-1.85522533780729,-4.26569223184847));
#82672=CARTESIAN_POINT('Ctrl Pts',(34.9863688419583,2.58519899421029,-3.86713555895036));
#82673=CARTESIAN_POINT('Ctrl Pts',(35.1852160606979,4.65091247090342,0.0836926456322418));
#82674=CARTESIAN_POINT('Ctrl Pts',(35.3840632794377,2.44439299510388,3.95764249982663));
#82675=CARTESIAN_POINT('Ctrl Pts',(35.5829104981772,-2.00749582872452,4.19618299989382));
#82676=CARTESIAN_POINT('Ctrl Pts',(35.7237682310197,-3.85481877961169,1.63472012191788));
#82677=CARTESIAN_POINT('Ctrl Pts',(35.7983435576157,-3.93839600529667,0.166142970595259));
#82678=CARTESIAN_POINT('Ctrl Pts',(35.8066364779651,-3.93711838212695,0.00268792454698923));
#82679=CARTESIAN_POINT('',(37.056636451576,-3.93093029693069,0.00184536342784963));
#82680=CARTESIAN_POINT('Ctrl Pts',(35.8066364779651,-3.93299908341869,0.00268511224544268));
#82681=CARTESIAN_POINT('Ctrl Pts',(35.8124218483503,-3.93307685187136,-0.111225676248522));
#82682=CARTESIAN_POINT('Ctrl Pts',(35.8182072187354,-3.9282016719798,-0.225330603230136));
#82683=CARTESIAN_POINT('Ctrl Pts',(35.8239925891206,-3.91834943567708,-0.339155863769318));
#82684=CARTESIAN_POINT('Ctrl Pts',(35.8297715028224,-3.90850819482782,-0.452854091184537));
#82685=CARTESIAN_POINT('Ctrl Pts',(35.8355504165241,-3.89370097473932,-0.566272851449055));
#82686=CARTESIAN_POINT('Ctrl Pts',(35.8413293302259,-3.87395569505401,-0.67893760593928));
#82687=CARTESIAN_POINT('Ctrl Pts',(35.8471324804521,-3.85412760448416,-0.79207487173984));
#82688=CARTESIAN_POINT('Ctrl Pts',(35.8529356306784,-3.82931993226872,-0.904451358442189));
#82689=CARTESIAN_POINT('Ctrl Pts',(35.8587387809047,-3.79961374328103,-1.0155906664941));
#82690=CARTESIAN_POINT('Ctrl Pts',(35.8645102457723,-3.77006975089651,-1.12612315088873));
#82691=CARTESIAN_POINT('Ctrl Pts',(35.8702817106398,-3.73568071269343,-1.23543151752743));
#82692=CARTESIAN_POINT('Ctrl Pts',(35.8760531755074,-3.69657752796805,-1.34305754892396));
#82693=CARTESIAN_POINT('Ctrl Pts',(35.8818235341759,-3.65748183803049,-1.45066295196821));
#82694=CARTESIAN_POINT('Ctrl Pts',(35.8875938928444,-3.61367394256633,-1.55658626034691));
#82695=CARTESIAN_POINT('Ctrl Pts',(35.893364251513,-3.56533406801193,-1.66038609470011));
#82696=CARTESIAN_POINT('Ctrl Pts',(35.8991349926789,-3.51699098917224,-1.76419280959005));
#82697=CARTESIAN_POINT('Ctrl Pts',(35.9049057338448,-3.46411551493796,-1.86587538495103));
#82698=CARTESIAN_POINT('Ctrl Pts',(35.9106764750107,-3.40693493204139,-1.96501485206503));
#82699=CARTESIAN_POINT('Ctrl Pts',(35.9165038467312,-3.3491932135771,-2.06512721379367));
#82700=CARTESIAN_POINT('Ctrl Pts',(35.9223312184517,-3.28706164524794,-2.16264589458816));
#82701=CARTESIAN_POINT('Ctrl Pts',(35.9281585901722,-3.22081966464825,-2.25716851116951));
#82702=CARTESIAN_POINT('Ctrl Pts',(35.933937624766,-3.15512715079951,-2.35090707759782));
#82703=CARTESIAN_POINT('Ctrl Pts',(35.9397166593598,-3.08539247285777,-2.44169879756162));
#82704=CARTESIAN_POINT('Ctrl Pts',(35.9454956939537,-3.01192857010563,-2.52918470827685));
#82705=CARTESIAN_POINT('Ctrl Pts',(35.9513472342375,-2.93754296479728,-2.61776824632357));
#82706=CARTESIAN_POINT('Ctrl Pts',(35.9571987745213,-2.85933422874015,-2.70296212788809));
#82707=CARTESIAN_POINT('Ctrl Pts',(35.9630503148051,-2.77766451117824,-2.78443331098824));
#82708=CARTESIAN_POINT('Ctrl Pts',(35.9689018550889,-2.69599479361635,-2.86590449408837));
#82709=CARTESIAN_POINT('Ctrl Pts',(35.9747533953728,-2.61086446994547,-2.94365272926105));
#82710=CARTESIAN_POINT('Ctrl Pts',(35.9806049356566,-2.52266784757149,-3.01738892601352));
#82711=CARTESIAN_POINT('Ctrl Pts',(35.9864773817905,-2.43415612433894,-3.0913885607331));
#82712=CARTESIAN_POINT('Ctrl Pts',(35.9923498279244,-2.34223740778439,-3.16161419713871));
#82713=CARTESIAN_POINT('Ctrl Pts',(35.9982222740583,-2.2472672562383,-3.22773587504294));
#82714=CARTESIAN_POINT('Ctrl Pts',(36.0040871130032,-2.15242012938801,-3.29377189867393));
#82715=CARTESIAN_POINT('Ctrl Pts',(36.009951951948,-2.05452976444679,-3.35571430199108));
#82716=CARTESIAN_POINT('Ctrl Pts',(36.0158167908928,-1.9539857780179,-3.41327241504451));
#82717=CARTESIAN_POINT('Ctrl Pts',(36.0216756010129,-1.85354514687046,-3.47077136061129));
#82718=CARTESIAN_POINT('Ctrl Pts',(36.0275344111329,-1.75045667659687,-3.52389477621279));
#82719=CARTESIAN_POINT('Ctrl Pts',(36.033393221253,-1.64513948124863,-3.57239486720561));
#82720=CARTESIAN_POINT('Ctrl Pts',(36.0394790101339,-1.53574214573281,-3.62277392173081));
#82721=CARTESIAN_POINT('Ctrl Pts',(36.0455647990149,-1.42394027737069,-3.66816391835342));
#82722=CARTESIAN_POINT('Ctrl Pts',(36.0516505878958,-1.3102327671693,-3.70833912902203));
#82723=CARTESIAN_POINT('Ctrl Pts',(36.0575026179741,-1.20089283066499,-3.7469711857417));
#82724=CARTESIAN_POINT('Ctrl Pts',(36.0633546480524,-1.08979137137159,-3.78078152248512));
#82725=CARTESIAN_POINT('Ctrl Pts',(36.0692066781307,-0.977392174669665,
-3.80961855530111));
#82726=CARTESIAN_POINT('Ctrl Pts',(36.0750578185092,-0.86501006631765,-3.83845120394602));
#82727=CARTESIAN_POINT('Ctrl Pts',(36.0809089588877,-0.751331013131233,
-3.86231194935055));
#82728=CARTESIAN_POINT('Ctrl Pts',(36.0867600992662,-0.636832484538411,
-3.88109950743815));
#82729=CARTESIAN_POINT('Ctrl Pts',(36.0926117668337,-0.522323639604124,
-3.89988875828868));
#82730=CARTESIAN_POINT('Ctrl Pts',(36.0984634344012,-0.406995580413226,
-3.9136038462243));
#82731=CARTESIAN_POINT('Ctrl Pts',(36.1043151019687,-0.291333747170069,
-3.92219500379059));
#82732=CARTESIAN_POINT('Ctrl Pts',(36.1101687136529,-0.175633487255264,
-3.93078901562247));
#82733=CARTESIAN_POINT('Ctrl Pts',(36.1160223253372,-0.0595996447918956,
-3.93425568148592));
#82734=CARTESIAN_POINT('Ctrl Pts',(36.1218759370214,0.0562801840893303,
-3.93259730215018));
#82735=CARTESIAN_POINT('Ctrl Pts',(36.1277362031213,0.172291745751625,-3.93093703756034));
#82736=CARTESIAN_POINT('Ctrl Pts',(36.1335964692212,0.288148530812364,-3.92414010483423));
#82737=CARTESIAN_POINT('Ctrl Pts',(36.1394567353211,0.403365811098988,-3.91226085817861));
#82738=CARTESIAN_POINT('Ctrl Pts',(36.1453209484924,0.518660693805935,-3.90037361048105));
#82739=CARTESIAN_POINT('Ctrl Pts',(36.1511851616637,0.633314806177066,-3.88339729317651));
#82740=CARTESIAN_POINT('Ctrl Pts',(36.157049374835,0.746853112795433,-3.86143748206646));
#82741=CARTESIAN_POINT('Ctrl Pts',(36.1629222234093,0.860558611328997,-3.83944533382733));
#82742=CARTESIAN_POINT('Ctrl Pts',(36.1687950719836,0.973144624373589,-3.81245514161668));
#82743=CARTESIAN_POINT('Ctrl Pts',(36.1746679205579,1.08415069571401,-3.78062247109955));
#82744=CARTESIAN_POINT('Ctrl Pts',(36.1762626651707,1.11429387615108,-3.77197845803247));
#82745=CARTESIAN_POINT('Ctrl Pts',(36.1778574097834,1.14432066997479,-3.76297765027667));
#82746=CARTESIAN_POINT('Ctrl Pts',(36.1794521543962,1.17422212668442,-3.75362376873398));
#82747=CARTESIAN_POINT('Ctrl Pts',(36.1853246005301,1.28433047409437,-3.71917927833557));
#82748=CARTESIAN_POINT('Ctrl Pts',(36.191197046664,1.3931062966548,-3.67982815525321));
#82749=CARTESIAN_POINT('Ctrl Pts',(36.1970694927979,1.50007977488483,-3.63569108547213));
#82750=CARTESIAN_POINT('Ctrl Pts',(36.2029343317427,1.60691467926409,-3.59161119101919));
#82751=CARTESIAN_POINT('Ctrl Pts',(36.2087991706876,1.71195150374035,-3.54275783513725));
#82752=CARTESIAN_POINT('Ctrl Pts',(36.2146640096324,1.81473506447399,-3.48930159856791));
#82753=CARTESIAN_POINT('Ctrl Pts',(36.2205228197524,1.91741296773092,-3.43590031291708));
#82754=CARTESIAN_POINT('Ctrl Pts',(36.2263816298724,2.0178418499043,-3.37790574753603));
#82755=CARTESIAN_POINT('Ctrl Pts',(36.2322404399924,2.11558664467219,-3.31553647980001));
#82756=CARTESIAN_POINT('Ctrl Pts',(36.2383262288734,2.21711821387963,-3.25075093660465));
#82757=CARTESIAN_POINT('Ctrl Pts',(36.2444120177543,2.31575309863678,-3.18124504425275));
#82758=CARTESIAN_POINT('Ctrl Pts',(36.2504978066353,2.41103165901885,-3.10731642083789));
#82759=CARTESIAN_POINT('Ctrl Pts',(36.2563498367136,2.50265051272435,-3.03622744020958));
#82760=CARTESIAN_POINT('Ctrl Pts',(36.2622018667918,2.59116576601304,-2.96104949754691));
#82761=CARTESIAN_POINT('Ctrl Pts',(36.2680538968701,2.67619913160987,-2.88209077025179));
#82762=CARTESIAN_POINT('Ctrl Pts',(36.2739050372486,2.76121956935729,-2.80314404726261));
#82763=CARTESIAN_POINT('Ctrl Pts',(36.2797561776271,2.84275886913032,-2.7204179637272));
#82764=CARTESIAN_POINT('Ctrl Pts',(36.2856073180056,2.92047365725232,-2.63425940584736));
#82765=CARTESIAN_POINT('Ctrl Pts',(36.2914589855731,2.99819544749306,-2.54809308506333));
#82766=CARTESIAN_POINT('Ctrl Pts',(36.2973106531406,3.07209176419466,-2.45849398210059));
#82767=CARTESIAN_POINT('Ctrl Pts',(36.3031623207081,3.14185826004183,-2.36584354381412));
#82768=CARTESIAN_POINT('Ctrl Pts',(36.3090159323923,3.211647934617,-2.27316232400017));
#82769=CARTESIAN_POINT('Ctrl Pts',(36.3148695440765,3.27730481155736,-2.17742808310776));
#82770=CARTESIAN_POINT('Ctrl Pts',(36.3207231557607,3.33856717807005,-2.07905223539799));
#82771=CARTESIAN_POINT('Ctrl Pts',(36.3265834218606,3.39989918795403,-1.98056455352187));
#82772=CARTESIAN_POINT('Ctrl Pts',(36.3324436879605,3.45682649751959,-1.87942962204603));
#82773=CARTESIAN_POINT('Ctrl Pts',(36.3383039540603,3.50913273252388,-1.77608458850628));
#82774=CARTESIAN_POINT('Ctrl Pts',(36.3441681672316,3.56147419740369,-1.67266994887332));
#82775=CARTESIAN_POINT('Ctrl Pts',(36.3500323804029,3.60918822048394,-1.56704261891427));
#82776=CARTESIAN_POINT('Ctrl Pts',(36.3558965935742,3.65210675655598,-1.45965928857324));
#82777=CARTESIAN_POINT('Ctrl Pts',(36.3617694421485,3.69508849272728,-1.3521178298859));
#82778=CARTESIAN_POINT('Ctrl Pts',(36.3676422907228,3.73326051248998,-1.24281559881976));
#82779=CARTESIAN_POINT('Ctrl Pts',(36.3735151392971,3.76650470567798,-1.13222405119554));
#82780=CARTESIAN_POINT('Ctrl Pts',(36.37510988391,3.77553201113743,-1.10219343273561));
#82781=CARTESIAN_POINT('Ctrl Pts',(36.3767046285229,3.7841962462906,-1.07206779719081));
#82782=CARTESIAN_POINT('Ctrl Pts',(36.3782993731358,3.79249570156589,-1.04185668573188));
#82783=CARTESIAN_POINT('Ctrl Pts',(36.3841718192697,3.8230574000663,-0.930608073727307));
#82784=CARTESIAN_POINT('Ctrl Pts',(36.3900442654036,3.84877108558446,-0.817827326972223));
#82785=CARTESIAN_POINT('Ctrl Pts',(36.3959167115375,3.86948424404304,-0.703974917949945));
#82786=CARTESIAN_POINT('Ctrl Pts',(36.4017815504824,3.89017057059735,-0.59026999377152));
#82787=CARTESIAN_POINT('Ctrl Pts',(36.4076463894272,3.90586917863183,-0.475496570964712));
#82788=CARTESIAN_POINT('Ctrl Pts',(36.4135112283721,3.91647743962409,-0.36012978898659));
#82789=CARTESIAN_POINT('Ctrl Pts',(36.4193700384921,3.92707479573938,-0.244881599543646));
#82790=CARTESIAN_POINT('Ctrl Pts',(36.4252288486121,3.93259217527238,-0.129041673302607));
#82791=CARTESIAN_POINT('Ctrl Pts',(36.4310876587321,3.93297820264459,-0.0130941789565775));
#82792=CARTESIAN_POINT('Ctrl Pts',(36.4371734476131,3.93337918527441,0.107345288684975));
#82793=CARTESIAN_POINT('Ctrl Pts',(36.4432592364941,3.9282431011739,0.227900380667051));
#82794=CARTESIAN_POINT('Ctrl Pts',(36.449345025375,3.91757177732272,0.348023518637074));
#82795=CARTESIAN_POINT('Ctrl Pts',(36.4551970554533,3.90731034542402,0.463532654797463));
#82796=CARTESIAN_POINT('Ctrl Pts',(36.4610490855316,3.89193109368867,0.578641958261));
#82797=CARTESIAN_POINT('Ctrl Pts',(36.4669011156098,3.87148871989132,0.692866575723123));
#82798=CARTESIAN_POINT('Ctrl Pts',(36.4727522559883,3.85104945400259,0.807073827311895));
#82799=CARTESIAN_POINT('Ctrl Pts',(36.4786033963668,3.8255486693858,0.920396253550279));
#82800=CARTESIAN_POINT('Ctrl Pts',(36.4844545367454,3.79509250414324,1.03235744051942));
#82801=CARTESIAN_POINT('Ctrl Pts',(36.4903062043129,3.76463359479376,1.14432871521516));
#82802=CARTESIAN_POINT('Ctrl Pts',(36.4961578718804,3.72921852576281,1.25493810794196));
#82803=CARTESIAN_POINT('Ctrl Pts',(36.5020095394479,3.68900360983545,1.363723346805));
#82804=CARTESIAN_POINT('Ctrl Pts',(36.5078631511321,3.64877533318805,1.47254472770855));
#82805=CARTESIAN_POINT('Ctrl Pts',(36.5137167628164,3.6037441819966,1.57954036215897));
#82806=CARTESIAN_POINT('Ctrl Pts',(36.5195703745006,3.55411473081814,1.68426763911841));
#82807=CARTESIAN_POINT('Ctrl Pts',(36.5254306406005,3.50442886062639,1.78911397058059));
#82808=CARTESIAN_POINT('Ctrl Pts',(36.5312909067004,3.4501344339106,1.89168642383512));
#82809=CARTESIAN_POINT('Ctrl Pts',(36.5371511728003,3.39148218730608,1.99156661279144));
#82810=CARTESIAN_POINT('Ctrl Pts',(36.5430153859716,3.33279043658988,2.09151407416047));
#82811=CARTESIAN_POINT('Ctrl Pts',(36.5488795991429,3.26973524588477,2.18876531455354));
#82812=CARTESIAN_POINT('Ctrl Pts',(36.5547438123142,3.2026099230778,2.28293203591426));
#82813=CARTESIAN_POINT('Ctrl Pts',(36.5606166608885,3.13538575423729,2.37723742337755));
#82814=CARTESIAN_POINT('Ctrl Pts',(36.5664895094628,3.06407974506618,2.4684489021776));
#82815=CARTESIAN_POINT('Ctrl Pts',(36.572362358037,2.98902462502732,2.55621219600023));
#82816=CARTESIAN_POINT('Ctrl Pts',(36.5739571026498,2.96864375757753,2.58004390871256));
#82817=CARTESIAN_POINT('Ctrl Pts',(36.5755518472626,2.94798664507684,2.60362158015751));
#82818=CARTESIAN_POINT('Ctrl Pts',(36.5771465918754,2.92706038926025,2.62693861321951));
#82819=CARTESIAN_POINT('Ctrl Pts',(36.5830190380094,2.8500020884632,2.71280065003746));
#82820=CARTESIAN_POINT('Ctrl Pts',(36.5888914841433,2.76903357199705,2.79541293606631));
#82821=CARTESIAN_POINT('Ctrl Pts',(36.5947639302772,2.68445972749625,2.87439819291809));
#82822=CARTESIAN_POINT('Ctrl Pts',(36.6006287692221,2.59999544027558,2.95328113196745));
#82823=CARTESIAN_POINT('Ctrl Pts',(36.6064936081669,2.51193541201003,3.02854610588567));
#82824=CARTESIAN_POINT('Ctrl Pts',(36.6123584471118,2.42062384195347,3.09984986987538));
#82825=CARTESIAN_POINT('Ctrl Pts',(36.6182172572318,2.32940613661575,3.17108033638751));
#82826=CARTESIAN_POINT('Ctrl Pts',(36.6240760673519,2.23494386165567,3.23835743946063));
#82827=CARTESIAN_POINT('Ctrl Pts',(36.6299348774719,2.13761652479249,3.30137616653027));
#82828=CARTESIAN_POINT('Ctrl Pts',(36.6360206663529,2.03651858641248,3.36683633005071));
#82829=CARTESIAN_POINT('Ctrl Pts',(36.6421064552338,1.9323294351303,3.42770118294426));
#82830=CARTESIAN_POINT('Ctrl Pts',(36.6481922441148,1.82551068660393,3.48367618086051));
#82831=CARTESIAN_POINT('Ctrl Pts',(36.6540442741931,1.7227949103051,3.53750114551896));
#82832=CARTESIAN_POINT('Ctrl Pts',(36.6598963042713,1.61764821924696,3.58680476087673));
#82833=CARTESIAN_POINT('Ctrl Pts',(36.6657483343496,1.51050805199816,3.63137087404313));
#82834=CARTESIAN_POINT('Ctrl Pts',(36.6715994747282,1.40338417355473,3.67593021170447));
#82835=CARTESIAN_POINT('Ctrl Pts',(36.6774506151067,1.29426780308131,3.71575332056582));
#82836=CARTESIAN_POINT('Ctrl Pts',(36.6833017554852,1.18361709417196,3.75067188306094));
#82837=CARTESIAN_POINT('Ctrl Pts',(36.6891534230527,1.07295641561064,3.78559359172583));
#82838=CARTESIAN_POINT('Ctrl Pts',(36.6950050906202,0.960761518014698,3.81560975116161));
#82839=CARTESIAN_POINT('Ctrl Pts',(36.7008567581877,0.847505788546212,3.84060189792963));
#82840=CARTESIAN_POINT('Ctrl Pts',(36.706710369872,0.734212431792843,3.86560234791224));
#82841=CARTESIAN_POINT('Ctrl Pts',(36.7125639815563,0.61985794578722,3.88557537721353));
#82842=CARTESIAN_POINT('Ctrl Pts',(36.7184175932405,0.504925274437549,3.90045375145433));
#82843=CARTESIAN_POINT('Ctrl Pts',(36.7242778593404,0.389861947040513,3.9153490395069));
#82844=CARTESIAN_POINT('Ctrl Pts',(36.7301381254403,0.274219532560922,3.92513805950056));
#82845=CARTESIAN_POINT('Ctrl Pts',(36.7359983915402,0.15848555697376,3.92980550768492));
#82846=CARTESIAN_POINT('Ctrl Pts',(36.7418626047115,0.0426736309558888,
3.93447609954074));
#82847=CARTESIAN_POINT('Ctrl Pts',(36.7477268178829,-0.0732295666226823,
3.93401825249274));
#82848=CARTESIAN_POINT('Ctrl Pts',(36.7535910310542,-0.188738801397796,
3.92846874301514));
#82849=CARTESIAN_POINT('Ctrl Pts',(36.7594638796285,-0.304418130397105,
3.92291106155448));
#82850=CARTESIAN_POINT('Ctrl Pts',(36.7653367282028,-0.419701928710933,
3.91224679152824));
#82851=CARTESIAN_POINT('Ctrl Pts',(36.7712095767771,-0.534112265718246,
3.89656426709599));
#82852=CARTESIAN_POINT('Ctrl Pts',(36.7728043213897,-0.565179858602923,
3.89230575080096));
#82853=CARTESIAN_POINT('Ctrl Pts',(36.7743990660025,-0.596183118236474,
3.88767749199223));
#82854=CARTESIAN_POINT('Ctrl Pts',(36.7759938106151,-0.627112655085652,
3.88268189758464));
#82855=CARTESIAN_POINT('Ctrl Pts',(36.7818662567491,-0.741006778099209,
3.86428625051241));
#82856=CARTESIAN_POINT('Ctrl Pts',(36.787738702883,-0.854281475430034,3.84084412163663));
#82857=CARTESIAN_POINT('Ctrl Pts',(36.7936111490169,-0.966454521269314,
3.81240798686579));
#82858=CARTESIAN_POINT('Ctrl Pts',(36.7994759879617,-1.07848225771788,3.78400868837222));
#82859=CARTESIAN_POINT('Ctrl Pts',(36.8053408269066,-1.18941078364758,3.7506283496673));
#82860=CARTESIAN_POINT('Ctrl Pts',(36.8112056658514,-1.29876524641428,3.71237091825513));
#82861=CARTESIAN_POINT('Ctrl Pts',(36.8170644759715,-1.40800729707499,3.6741528139845));
#82862=CARTESIAN_POINT('Ctrl Pts',(36.8229232860915,-1.51567811518661,3.63106772473424));
#82863=CARTESIAN_POINT('Ctrl Pts',(36.8287820962115,-1.62131591775133,3.58326997236409));
#82864=CARTESIAN_POINT('Ctrl Pts',(36.8348678850925,-1.73104628126997,3.5336204660736));
#82865=CARTESIAN_POINT('Ctrl Pts',(36.8409536739735,-1.83858247899382,3.47888587242603));
#82866=CARTESIAN_POINT('Ctrl Pts',(36.8470394628544,-1.94342713727684,3.41929524348161));
#82867=CARTESIAN_POINT('Ctrl Pts',(36.8528914929327,-2.04424464932306,3.36199352635236));
#82868=CARTESIAN_POINT('Ctrl Pts',(36.858743523011,-2.14257318253464,3.30020216219617));
#82869=CARTESIAN_POINT('Ctrl Pts',(36.8645955530892,-2.23799437965998,3.23417225215515));
#82870=CARTESIAN_POINT('Ctrl Pts',(36.8704466934677,-2.33340106964617,3.16815238081751));
#82871=CARTESIAN_POINT('Ctrl Pts',(36.8762978338463,-2.42590096258857,3.09789548001554));
#82872=CARTESIAN_POINT('Ctrl Pts',(36.8821489742248,-2.51510473991064,3.02369594160508));
#82873=CARTESIAN_POINT('Ctrl Pts',(36.8880006417923,-2.60431655451206,2.9494897178004));
#82874=CARTESIAN_POINT('Ctrl Pts',(36.8938523093598,-2.6902313453144,2.87134041457043));
#82875=CARTESIAN_POINT('Ctrl Pts',(36.8997039769273,-2.77249349453142,2.78958219502149));
#82876=CARTESIAN_POINT('Ctrl Pts',(36.9055575886117,-2.85478297394511,2.70779681269794));
#82877=CARTESIAN_POINT('Ctrl Pts',(36.911411200296,-2.93341710571831,2.62240042114911));
#82878=CARTESIAN_POINT('Ctrl Pts',(36.9172648119803,-3.00807819897582,2.53376292277837));
#82879=CARTESIAN_POINT('Ctrl Pts',(36.9231250780802,-3.08282416734458,2.44502466084783));
#82880=CARTESIAN_POINT('Ctrl Pts',(36.9289853441801,-3.15358781581915,2.35303825427781));
#82881=CARTESIAN_POINT('Ctrl Pts',(36.93484561028,-3.22009266046172,2.25820553936982));
#82882=CARTESIAN_POINT('Ctrl Pts',(36.9407098234513,-3.28664229818494,2.16330895167979));
#82883=CARTESIAN_POINT('Ctrl Pts',(36.9465740366226,-3.34892719885407,2.06556258611286));
#82884=CARTESIAN_POINT('Ctrl Pts',(36.9524382497939,-3.40671592797793,1.96539451155778));
#82885=CARTESIAN_POINT('Ctrl Pts',(36.9583110983682,-3.46458975444535,1.86507893355034));
#82886=CARTESIAN_POINT('Ctrl Pts',(36.9641839469425,-3.51795400559901,1.76233489475654));
#82887=CARTESIAN_POINT('Ctrl Pts',(36.9700567955168,-3.56662456694096,1.65761219785968));
#82888=CARTESIAN_POINT('Ctrl Pts',(36.9716515401294,-3.57984083065237,1.62917523842059));
#82889=CARTESIAN_POINT('Ctrl Pts',(36.9732462847421,-3.59271127801773,1.6005924731228));
#82890=CARTESIAN_POINT('Ctrl Pts',(36.9748410293548,-3.60523285673848,1.57187310196888));
#82891=CARTESIAN_POINT('Ctrl Pts',(36.9816573132758,-3.65875279656022,1.44912028859335));
#82892=CARTESIAN_POINT('Ctrl Pts',(36.9884735971968,-3.70605617844956,1.32349986733078));
#82893=CARTESIAN_POINT('Ctrl Pts',(36.9952898811179,-3.74685935742616,1.19563119550639));
#82894=CARTESIAN_POINT('Ctrl Pts',(37.0017475223055,-3.78551565346634,1.07449040804119));
#82895=CARTESIAN_POINT('Ctrl Pts',(37.0082051634932,-3.81833803639176,0.951332193712651));
#82896=CARTESIAN_POINT('Ctrl Pts',(37.0146628046808,-3.84513250844753,0.826707319720848));
#82897=CARTESIAN_POINT('Ctrl Pts',(37.0211026152414,-3.87185299648597,0.702426555843145));
#82898=CARTESIAN_POINT('Ctrl Pts',(37.027542425802,-3.89257868793019,0.576687462732061));
#82899=CARTESIAN_POINT('Ctrl Pts',(37.0339822363626,-3.90716502540595,0.450056067889892));
#82900=CARTESIAN_POINT('Ctrl Pts',(37.0403956793402,-3.92169163962408,0.32394316094311));
#82901=CARTESIAN_POINT('Ctrl Pts',(37.0468091223177,-3.93012896942495,0.196945499472617));
#82902=CARTESIAN_POINT('Ctrl Pts',(37.0532225652953,-3.93238344128207,0.0696381413490412));
#82903=CARTESIAN_POINT('Ctrl Pts',(37.0543605223326,-3.93278345920136,0.0470496027761474));
#82904=CARTESIAN_POINT('Ctrl Pts',(37.05549847937,-3.93298895303553,0.024451349141318));
#82905=CARTESIAN_POINT('Ctrl Pts',(37.0566364364073,-3.93299956648052,0.00184663587889645));
#82906=CARTESIAN_POINT('',(38.3066365073438,-3.93243957318768,-0.00337961949426096));
#82907=CARTESIAN_POINT('Ctrl Pts',(37.0566364779651,-3.92733035500781,0.00184314972404838));
#82908=CARTESIAN_POINT('Ctrl Pts',(37.0956537346748,-3.92406703883986,-0.772091625719316));
#82909=CARTESIAN_POINT('Ctrl Pts',(37.2009533976313,-3.32801601167788,-2.86542164041253));
#82910=CARTESIAN_POINT('Ctrl Pts',(37.372535466834,0.0794706818914165,-4.65098652778712));
#82911=CARTESIAN_POINT('Ctrl Pts',(37.5713826855737,3.95542193811241,-2.44798459195364));
#82912=CARTESIAN_POINT('Ctrl Pts',(37.7702299043133,4.19800360272441,2.00368585922314));
#82913=CARTESIAN_POINT('Ctrl Pts',(37.969077123053,0.58438512629953,4.61481151241442));
#82914=CARTESIAN_POINT('Ctrl Pts',(38.1478793142703,-3.14764932441101,3.15097279315654));
#82915=CARTESIAN_POINT('Ctrl Pts',(38.2603990992409,-3.92290543832594,0.912003963472055));
#82916=CARTESIAN_POINT('Ctrl Pts',(38.3066364779651,-3.930349927301,-0.00337724190769125));
#82917=CARTESIAN_POINT('',(39.5566364779651,-3.93546570744218,-0.000396427527168986));
#82918=CARTESIAN_POINT('Ctrl Pts',(38.3066365152026,-3.93299854740284,-0.00338025549177386));
#82919=CARTESIAN_POINT('Ctrl Pts',(38.3136694315384,-3.93287880190695,-0.142706665141453));
#82920=CARTESIAN_POINT('Ctrl Pts',(38.3207023478743,-3.92535182945411,-0.281710047409065));
#82921=CARTESIAN_POINT('Ctrl Pts',(38.3277352642102,-3.9105430525726,-0.419692785232426));
#82922=CARTESIAN_POINT('Ctrl Pts',(38.3348606654883,-3.89553953586925,-0.559490037110306));
#82923=CARTESIAN_POINT('Ctrl Pts',(38.3419860667664,-3.87306150665475,-0.698239609978886));
#82924=CARTESIAN_POINT('Ctrl Pts',(38.3491114680445,-3.84328850131442,-0.835237987440902));
#82925=CARTESIAN_POINT('Ctrl Pts',(38.3549981655405,-3.81869133560515,-0.948420105061101));
#82926=CARTESIAN_POINT('Ctrl Pts',(38.3608848630364,-3.78911601011755,-1.06040738142393));
#82927=CARTESIAN_POINT('Ctrl Pts',(38.3667715605323,-3.75468813833344,-1.17081423968885));
#82928=CARTESIAN_POINT('Ctrl Pts',(38.3726440066662,-3.72034361448153,-1.28095380918857));
#82929=CARTESIAN_POINT('Ctrl Pts',(38.3785164528001,-3.68109125034966,-1.38976530845056));
#82930=CARTESIAN_POINT('Ctrl Pts',(38.384388898934,-3.6370513053883,-1.49677880863316));
#82931=CARTESIAN_POINT('Ctrl Pts',(38.3902537378789,-3.59306840993928,-1.60365368312023));
#82932=CARTESIAN_POINT('Ctrl Pts',(38.3961185768237,-3.54431042279645,-1.70873481161991));
#82933=CARTESIAN_POINT('Ctrl Pts',(38.4019834157685,-3.49094751143177,-1.81156685563309));
#82934=CARTESIAN_POINT('Ctrl Pts',(38.4078422258886,-3.43763945505075,-1.91429319233101));
#82935=CARTESIAN_POINT('Ctrl Pts',(38.4137010360086,-3.37973607925242,-2.01477467848436));
#82936=CARTESIAN_POINT('Ctrl Pts',(38.4195598461286,-3.31745556638457,-2.11257604953385));
#82937=CARTESIAN_POINT('Ctrl Pts',(38.4256456350095,-3.25276221654935,-2.21416638686929));
#82938=CARTESIAN_POINT('Ctrl Pts',(38.4317314238905,-3.18334588999762,-2.31286432590927));
#82939=CARTESIAN_POINT('Ctrl Pts',(38.4378172127715,-3.10950378745594,-2.40820995675153));
#82940=CARTESIAN_POINT('Ctrl Pts',(38.4436692428497,-3.038498004382,-2.49989330470076));
#82941=CARTESIAN_POINT('Ctrl Pts',(38.449521272928,-2.9634004436228,-2.588476765323));
#82942=CARTESIAN_POINT('Ctrl Pts',(38.4553733030063,-2.88451893905781,-2.67358177174681));
#82943=CARTESIAN_POINT('Ctrl Pts',(38.4612244433848,-2.80564942705857,-2.75867383942926));
#82944=CARTESIAN_POINT('Ctrl Pts',(38.4670755837633,-2.72299739601975,-2.84028820133775));
#82945=CARTESIAN_POINT('Ctrl Pts',(38.4729267241418,-2.63690942029811,-2.91808116904638));
#82946=CARTESIAN_POINT('Ctrl Pts',(38.4787783917093,-2.55081368803153,-2.99588114591796));
#82947=CARTESIAN_POINT('Ctrl Pts',(38.4846300592768,-2.46128170237478,-3.06985876698141));
#82948=CARTESIAN_POINT('Ctrl Pts',(38.4904817268443,-2.36869463375025,-3.13970933878325));
#82949=CARTESIAN_POINT('Ctrl Pts',(38.4963353385285,-2.27607680465157,-3.20958311724603));
#82950=CARTESIAN_POINT('Ctrl Pts',(38.5021889502127,-2.18040220412883,-3.27532687119829));
#82951=CARTESIAN_POINT('Ctrl Pts',(38.5080425618969,-2.0820820087003,-3.3366785144881));
#82952=CARTESIAN_POINT('Ctrl Pts',(38.5139028279968,-1.9836500423715,-3.39809990263931));
#82953=CARTESIAN_POINT('Ctrl Pts',(38.5197630940967,-1.88256682910686,-3.45511899536387));
#82954=CARTESIAN_POINT('Ctrl Pts',(38.5256233601966,-1.77926931984543,-3.50751902168139));
#82955=CARTESIAN_POINT('Ctrl Pts',(38.5314875733679,-1.67590223650006,-3.55995434104572));
#82956=CARTESIAN_POINT('Ctrl Pts',(38.5373517865392,-1.57031826311682,-3.6077642291169));
#82957=CARTESIAN_POINT('Ctrl Pts',(38.5432159997104,-1.46297393690635,-3.65078022618902));
#82958=CARTESIAN_POINT('Ctrl Pts',(38.5490888482847,-1.35547153978527,-3.69385956687759));
#82959=CARTESIAN_POINT('Ctrl Pts',(38.554961696859,-1.24620400492513,-3.7321307915044));
#82960=CARTESIAN_POINT('Ctrl Pts',(38.5608345454333,-1.13564268073632,-3.76547536198154));
#82961=CARTESIAN_POINT('Ctrl Pts',(38.5624292900462,-1.10562026931021,-3.77452992442493));
#82962=CARTESIAN_POINT('Ctrl Pts',(38.564024034659,-1.07550251125637,-3.78322150296472));
#82963=CARTESIAN_POINT('Ctrl Pts',(38.5656187792719,-1.04529894618971,-3.79154837936887));
#82964=CARTESIAN_POINT('Ctrl Pts',(38.5714912254058,-0.93407812282038,-3.82221105272282));
#82965=CARTESIAN_POINT('Ctrl Pts',(38.5773636715397,-0.82132076448187,-3.84802710590822));
#82966=CARTESIAN_POINT('Ctrl Pts',(38.5832361176736,-0.707487205021032,
-3.86884360691041));
#82967=CARTESIAN_POINT('Ctrl Pts',(38.5891009566184,-0.593801105986399,
-3.88963314213796));
#82968=CARTESIAN_POINT('Ctrl Pts',(38.5949657955633,-0.479041981094081,
-3.90543593084494));
#82969=CARTESIAN_POINT('Ctrl Pts',(38.6008306345081,-0.363684876442936,
-3.91614891323692));
#82970=CARTESIAN_POINT('Ctrl Pts',(38.6066894446281,-0.248446354379057,
-3.92685088310242));
#82971=CARTESIAN_POINT('Ctrl Pts',(38.6125482547481,-0.132611484342829,
-3.93247341563584));
#82972=CARTESIAN_POINT('Ctrl Pts',(38.6184070648681,-0.0166643881909874,
-3.93296469576911));
#82973=CARTESIAN_POINT('Ctrl Pts',(38.6244928537491,0.10377466582988,-3.93347500880389));
#82974=CARTESIAN_POINT('Ctrl Pts',(38.6305786426301,0.224334370491517,-3.92844836234927));
#82975=CARTESIAN_POINT('Ctrl Pts',(38.6366644315111,0.344467146008484,-3.91788608631246));
#82976=CARTESIAN_POINT('Ctrl Pts',(38.6425164615893,0.459985549531777,-3.90772951363615));
#82977=CARTESIAN_POINT('Ctrl Pts',(38.6483684916676,0.575108766293744,-3.89245476027826));
#82978=CARTESIAN_POINT('Ctrl Pts',(38.6542205217458,0.689351893536949,-3.87211608385867));
#82979=CARTESIAN_POINT('Ctrl Pts',(38.6600716621243,0.803577652092602,-3.85178049958234));
#82980=CARTESIAN_POINT('Ctrl Pts',(38.6659228025028,0.916923180325123,-3.82638259545112));
#82981=CARTESIAN_POINT('Ctrl Pts',(38.6717739428814,1.02891196816364,-3.79602807705233));
#82982=CARTESIAN_POINT('Ctrl Pts',(38.6776256104488,1.14091084621557,-3.76567082370504));
#82983=CARTESIAN_POINT('Ctrl Pts',(38.6834772780163,1.25155234188126,-3.73035617645139));
#82984=CARTESIAN_POINT('Ctrl Pts',(38.6893289455838,1.3603740415613,-3.69024002837839));
#82985=CARTESIAN_POINT('Ctrl Pts',(38.6951825572681,1.46923189539491,-3.65011055239946));
#82986=CARTESIAN_POINT('Ctrl Pts',(38.7010361689523,1.57626836340257,-3.60517654650915));
#82987=CARTESIAN_POINT('Ctrl Pts',(38.7068897806365,1.68104064902344,-3.555642183394));
#82988=CARTESIAN_POINT('Ctrl Pts',(38.7127500467364,1.78593204031363,-3.50605150936191));
#82989=CARTESIAN_POINT('Ctrl Pts',(38.7186103128363,1.88855373781312,-3.45185021656064));
#82990=CARTESIAN_POINT('Ctrl Pts',(38.7244705789361,1.98848712799414,-3.3932886617265));
#82991=CARTESIAN_POINT('Ctrl Pts',(38.7303347921074,2.08848782642049,-3.33468766386443));
#82992=CARTESIAN_POINT('Ctrl Pts',(38.7361990052788,2.18579626595397,-3.27172078027991));
#82993=CARTESIAN_POINT('Ctrl Pts',(38.7420632184501,2.28002388244395,-3.20468096625627));
#82994=CARTESIAN_POINT('Ctrl Pts',(38.7479360670243,2.37439025470839,-3.13754243211574));
#82995=CARTESIAN_POINT('Ctrl Pts',(38.7538089155986,2.46566642493059,-3.06631925078858));
#82996=CARTESIAN_POINT('Ctrl Pts',(38.7596817641729,2.55349781490262,-2.99134383000141));
#82997=CARTESIAN_POINT('Ctrl Pts',(38.7612765087858,2.57734801880756,-2.97098460451037));
#82998=CARTESIAN_POINT('Ctrl Pts',(38.7628712533987,2.60094443231498,-2.95034890347279));
#82999=CARTESIAN_POINT('Ctrl Pts',(38.7644659980115,2.62428045186533,-2.92944382263213));
#83000=CARTESIAN_POINT('Ctrl Pts',(38.7703384441454,2.71021240403054,-2.8524634960201));
#83001=CARTESIAN_POINT('Ctrl Pts',(38.7762108902794,2.79289815629724,-2.77157000534445));
#83002=CARTESIAN_POINT('Ctrl Pts',(38.7820833364133,2.87196015366701,-2.68706789563438));
#83003=CARTESIAN_POINT('Ctrl Pts',(38.7879481753581,2.95091973382448,-2.60267525027884));
#83004=CARTESIAN_POINT('Ctrl Pts',(38.793813014303,3.02626461442448,-2.51468358110271));
#83005=CARTESIAN_POINT('Ctrl Pts',(38.7996778532478,3.09765123835948,-2.42343677563289));
#83006=CARTESIAN_POINT('Ctrl Pts',(38.8055366633678,3.1689644796399,-2.33228376830675));
#83007=CARTESIAN_POINT('Ctrl Pts',(38.8113954734878,3.23632730441255,-2.23788260397548));
#83008=CARTESIAN_POINT('Ctrl Pts',(38.8172542836079,3.29943435573531,-2.14061251332266));
#83009=CARTESIAN_POINT('Ctrl Pts',(38.8233400724888,3.36498626531822,-2.03957403895337));
#83010=CARTESIAN_POINT('Ctrl Pts',(38.8294258613698,3.42594567225829,-1.9354401814996));
#83011=CARTESIAN_POINT('Ctrl Pts',(38.8355116502508,3.48201761328852,-1.82867228905251));
#83012=CARTESIAN_POINT('Ctrl Pts',(38.841363680329,3.53593579741771,-1.72600541542057));
#83013=CARTESIAN_POINT('Ctrl Pts',(38.8472157104073,3.58533484080514,-1.62090352371436));
#83014=CARTESIAN_POINT('Ctrl Pts',(38.8530677404856,3.62999819355835,-1.51380385610658));
#83015=CARTESIAN_POINT('Ctrl Pts',(38.8589188808641,3.67465475602281,-1.40672047114714));
#83016=CARTESIAN_POINT('Ctrl Pts',(38.8647700212426,3.71457690035054,-1.29764029560235));
#83017=CARTESIAN_POINT('Ctrl Pts',(38.8706211616211,3.74959589314948,-1.18702133008491));
#83018=CARTESIAN_POINT('Ctrl Pts',(38.8764728291886,3.78461804116707,-1.0763923977753));
#83019=CARTESIAN_POINT('Ctrl Pts',(38.8823244967561,3.81473603468499,-0.964224793983947));
#83020=CARTESIAN_POINT('Ctrl Pts',(38.8881761643236,3.83983098058972,-0.850991798141068));
#83021=CARTESIAN_POINT('Ctrl Pts',(38.8940297760078,3.8649342638622,-0.737721182566711));
#83022=CARTESIAN_POINT('Ctrl Pts',(38.8998833876921,3.88501109177934,-0.623384874467584));
#83023=CARTESIAN_POINT('Ctrl Pts',(38.9057369993763,3.89999379159077,-0.508465756519987));
#83024=CARTESIAN_POINT('Ctrl Pts',(38.9115972654762,3.91499352381185,-0.393415997932268));
#83025=CARTESIAN_POINT('Ctrl Pts',(38.9174575315761,3.92488751575212,-0.277782517216073));
#83026=CARTESIAN_POINT('Ctrl Pts',(38.9233177976759,3.92966002110912,-0.162052826253335));
#83027=CARTESIAN_POINT('Ctrl Pts',(38.9291820108472,3.93443574089685,-0.0462451877456786));
#83028=CARTESIAN_POINT('Ctrl Pts',(38.9350462240186,3.9340831067468,0.0696583776954723));
#83029=CARTESIAN_POINT('Ctrl Pts',(38.9409104371899,3.9286384546399,0.185172602521538));
#83030=CARTESIAN_POINT('Ctrl Pts',(38.9467832857641,3.92318578495866,0.300856928920133));
#83031=CARTESIAN_POINT('Ctrl Pts',(38.9526561343384,3.91262616976747,0.416150360371662));
#83032=CARTESIAN_POINT('Ctrl Pts',(38.9585289829127,3.89704750934145,0.530574886265481));
#83033=CARTESIAN_POINT('Ctrl Pts',(38.9601237275255,3.89281719683212,0.561646332078223));
#83034=CARTESIAN_POINT('Ctrl Pts',(38.9617184721383,3.88821708356199,0.592653780305154));
#83035=CARTESIAN_POINT('Ctrl Pts',(38.9633132167512,3.88324956792143,0.623587839231974));
#83036=CARTESIAN_POINT('Ctrl Pts',(38.9691856628851,3.86495731737279,0.737498614218898));
#83037=CARTESIAN_POINT('Ctrl Pts',(38.975058109019,3.8416180248077,0.850794544791016));
#83038=CARTESIAN_POINT('Ctrl Pts',(38.9809305551529,3.813283728366,0.962993357702474));
#83039=CARTESIAN_POINT('Ctrl Pts',(38.9867953940978,3.78498613627976,1.07504682784463));
#83040=CARTESIAN_POINT('Ctrl Pts',(38.9926602330426,3.75170650821108,1.18600560952804));
#83041=CARTESIAN_POINT('Ctrl Pts',(38.9985250719875,3.71354836056725,1.29539475594441));
#83042=CARTESIAN_POINT('Ctrl Pts',(39.0043838821075,3.67542943800527,1.40467145460097));
#83043=CARTESIAN_POINT('Ctrl Pts',(39.0102426922275,3.63244210616119,1.51238133942785));
#83044=CARTESIAN_POINT('Ctrl Pts',(39.0161015023476,3.58474026764131,1.61806248752972));
#83045=CARTESIAN_POINT('Ctrl Pts',(39.0221872912285,3.53519039104206,1.7278378758543));
#83046=CARTESIAN_POINT('Ctrl Pts',(39.0282730801095,3.48055343739693,1.83542371534555));
#83047=CARTESIAN_POINT('Ctrl Pts',(39.0343588689905,3.42105800717408,1.94032242463723));
#83048=CARTESIAN_POINT('Ctrl Pts',(39.0402108990688,3.3638478321263,2.04119191156059));
#83049=CARTESIAN_POINT('Ctrl Pts',(39.046062929147,3.30214575249688,2.13957649621314));
#83050=CARTESIAN_POINT('Ctrl Pts',(39.0519149592253,3.23620248955498,2.2350575935752));
#83051=CARTESIAN_POINT('Ctrl Pts',(39.0577660996038,3.17026925214336,2.33052417469116));
#83052=CARTESIAN_POINT('Ctrl Pts',(39.0636172399824,3.10009634832847,2.42308780618229));
#83053=CARTESIAN_POINT('Ctrl Pts',(39.0694683803609,3.02597781643561,2.51235890239423));
#83054=CARTESIAN_POINT('Ctrl Pts',(39.0753200479284,2.95185260644735,2.60163804195083));
#83055=CARTESIAN_POINT('Ctrl Pts',(39.0811717154959,2.8737813257401,2.68762373845095));
#83056=CARTESIAN_POINT('Ctrl Pts',(39.0870233830634,2.79209781446559,2.76996007091374));
#83057=CARTESIAN_POINT('Ctrl Pts',(39.0928769947477,2.71038716523769,2.85232375821863));
#83058=CARTESIAN_POINT('Ctrl Pts',(39.0987306064319,2.6250621900807,2.93103537733209));
#83059=CARTESIAN_POINT('Ctrl Pts',(39.1045842181162,2.53649250285734,3.00577690172583));
#83060=CARTESIAN_POINT('Ctrl Pts',(39.1104444842161,2.44782212916132,3.08060339266612));
#83061=CARTESIAN_POINT('Ctrl Pts',(39.116304750316,2.35589999715888,3.15145051390063));
#83062=CARTESIAN_POINT('Ctrl Pts',(39.1221650164159,2.26112769200391,3.21804141683308));
#83063=CARTESIAN_POINT('Ctrl Pts',(39.1280292295872,2.16629155475493,3.28467717080899));
#83064=CARTESIAN_POINT('Ctrl Pts',(39.1338934427585,2.06860176942996,3.34705077641272));
#83065=CARTESIAN_POINT('Ctrl Pts',(39.1397576559298,1.96848619465356,3.4049304106631));
#83066=CARTESIAN_POINT('Ctrl Pts',(39.1456305045041,1.86822319373349,3.46289527612043));
#83067=CARTESIAN_POINT('Ctrl Pts',(39.1515033530784,1.7655276393991,3.51635277259045));
#83068=CARTESIAN_POINT('Ctrl Pts',(39.1573762016527,1.66084916701591,3.56511837733652));
#83069=CARTESIAN_POINT('Ctrl Pts',(39.1589709462654,1.63242421653601,3.57836044964108));
#83070=CARTESIAN_POINT('Ctrl Pts',(39.1605656908781,1.60385314633796,3.59125683809931));
#83071=CARTESIAN_POINT('Ctrl Pts',(39.1621604354908,1.57514515364979,3.60380448206248));
#83072=CARTESIAN_POINT('Ctrl Pts',(39.1680328816248,1.46943158714517,3.65000960023234));
#83073=CARTESIAN_POINT('Ctrl Pts',(39.1739053277587,1.36150624594712,3.69163664899737));
#83074=CARTESIAN_POINT('Ctrl Pts',(39.1797777738926,1.25180296016412,3.72846863322254));
#83075=CARTESIAN_POINT('Ctrl Pts',(39.1856426128374,1.14224178443512,3.76525290515514));
#83076=CARTESIAN_POINT('Ctrl Pts',(39.1915074517823,1.03090763252803,3.7972543347504));
#83077=CARTESIAN_POINT('Ctrl Pts',(39.1973722907271,0.918256006313075,3.82430319233059));
#83078=CARTESIAN_POINT('Ctrl Pts',(39.2032311008471,0.8057201815594,3.85132424474419));
#83079=CARTESIAN_POINT('Ctrl Pts',(39.2090899109672,0.691869975818573,3.8734027555914));
#83080=CARTESIAN_POINT('Ctrl Pts',(39.2149487210872,0.57717717946286,3.89041842267735));
#83081=CARTESIAN_POINT('Ctrl Pts',(39.2210345099681,0.458041018623016,3.90809330126746));
#83082=CARTESIAN_POINT('Ctrl Pts',(39.2271202988491,0.337996091133369,3.92030497382628));
#83083=CARTESIAN_POINT('Ctrl Pts',(39.2332060877301,0.217584573488528,3.92697669376581));
#83084=CARTESIAN_POINT('Ctrl Pts',(39.2390581178084,0.101798134489563,3.93339214893908));
#83085=CARTESIAN_POINT('Ctrl Pts',(39.2449101478866,-0.0143268013692517,
3.9346853618356));
#83086=CARTESIAN_POINT('Ctrl Pts',(39.2507621779649,-0.13030254908064,3.93084090821583));
#83087=CARTESIAN_POINT('Ctrl Pts',(39.2566133183434,-0.246260664689525,
3.92699703907861));
#83088=CARTESIAN_POINT('Ctrl Pts',(39.2624644587219,-0.362069224231788,
3.91801707018397));
#83089=CARTESIAN_POINT('Ctrl Pts',(39.2683155991004,-0.477241515248946,
3.9039376962399));
#83090=CARTESIAN_POINT('Ctrl Pts',(39.2741672666679,-0.592424183313889,
3.88985705374126));
#83091=CARTESIAN_POINT('Ctrl Pts',(39.2800189342354,-0.706970058563911,
3.87067614299513));
#83092=CARTESIAN_POINT('Ctrl Pts',(39.2858706018029,-0.820399226308901,
3.84648334319437));
#83093=CARTESIAN_POINT('Ctrl Pts',(39.2917242134871,-0.933866078960063,
3.82228250574855));
#83094=CARTESIAN_POINT('Ctrl Pts',(39.2975778251714,-1.04621508233125,3.79306655444722));
#83095=CARTESIAN_POINT('Ctrl Pts',(39.3034314368556,-1.15697885567182,3.75897445156632));
#83096=CARTESIAN_POINT('Ctrl Pts',(39.3092917029555,-1.26786854583558,3.72484359260877));
#83097=CARTESIAN_POINT('Ctrl Pts',(39.3151519690554,-1.37716901374189,3.68582563963176));
#83098=CARTESIAN_POINT('Ctrl Pts',(39.3210122351553,-1.48443023067911,3.64210871477582));
#83099=CARTESIAN_POINT('Ctrl Pts',(39.3268764483266,-1.59176369138076,3.59836234521179));
#83100=CARTESIAN_POINT('Ctrl Pts',(39.3327406614979,-1.69705479161216,3.54991087418261));
#83101=CARTESIAN_POINT('Ctrl Pts',(39.3386048746692,-1.7998771722758,3.49698887111762));
#83102=CARTESIAN_POINT('Ctrl Pts',(39.3444777232435,-1.90285096501586,3.44398893725272));
#83103=CARTESIAN_POINT('Ctrl Pts',(39.3503505718177,-2.00334842532305,3.38650553720828));
#83104=CARTESIAN_POINT('Ctrl Pts',(39.356223420392,-2.10097120858039,3.32481713492882));
#83105=CARTESIAN_POINT('Ctrl Pts',(39.3578181650048,-2.12748021961938,3.30806593728376));
#83106=CARTESIAN_POINT('Ctrl Pts',(39.3594129096176,-2.15377744675309,3.291004907634));
#83107=CARTESIAN_POINT('Ctrl Pts',(39.3610076542304,-2.17985534230117,3.27364012784561));
#83108=CARTESIAN_POINT('Ctrl Pts',(39.3668637167746,-2.27561599646785,3.20987491071258));
#83109=CARTESIAN_POINT('Ctrl Pts',(39.3727197793188,-2.3687411492821,3.14179459873242));
#83110=CARTESIAN_POINT('Ctrl Pts',(39.378575841863,-2.45881502679421,3.06964455010852));
#83111=CARTESIAN_POINT('Ctrl Pts',(39.384424307879,-2.54877205979722,2.99758809506854));
#83112=CARTESIAN_POINT('Ctrl Pts',(39.390272773895,-2.63568536628193,2.92147265832977));
#83113=CARTESIAN_POINT('Ctrl Pts',(39.3961212399109,-2.71916709477171,2.8415874631464));
#83114=CARTESIAN_POINT('Ctrl Pts',(39.4019637069651,-2.80256319333762,2.76178420880572));
#83115=CARTESIAN_POINT('Ctrl Pts',(39.4078061740193,-2.88253441563955,2.67821917217045));
#83116=CARTESIAN_POINT('Ctrl Pts',(39.4136486410735,-2.95872559837939,2.5912220733651));
#83117=CARTESIAN_POINT('Ctrl Pts',(39.4196064676106,-3.03642117564412,2.5025072172758));
#83118=CARTESIAN_POINT('Ctrl Pts',(39.4255642941478,-3.11018551207959,2.41022360207101));
#83119=CARTESIAN_POINT('Ctrl Pts',(39.4315221206849,-3.17968092376429,2.31476094295922));
#83120=CARTESIAN_POINT('Ctrl Pts',(39.4373579629526,-3.2477534428941,2.22125284607863));
#83121=CARTESIAN_POINT('Ctrl Pts',(39.4431938052203,-3.31172992496697,2.1246949964004));
#83122=CARTESIAN_POINT('Ctrl Pts',(39.4490296474881,-3.37133394785222,2.02548670991917));
#83123=CARTESIAN_POINT('Ctrl Pts',(39.4548646521831,-3.43092941623973,1.92629266202487));
#83124=CARTESIAN_POINT('Ctrl Pts',(39.4606996568782,-3.48615345896569,1.82444929010516));
#83125=CARTESIAN_POINT('Ctrl Pts',(39.4665346615733,-3.53677396329765,1.72038336789792));
#83126=CARTESIAN_POINT('Ctrl Pts',(39.4723702626728,-3.58739964162599,1.61630680895937));
#83127=CARTESIAN_POINT('Ctrl Pts',(39.4782058637723,-3.63342066444593,1.51000762231545));
#83128=CARTESIAN_POINT('Ctrl Pts',(39.4840414648718,-3.67465203776792,1.40193487770584));
#83129=CARTESIAN_POINT('Ctrl Pts',(39.4900910492962,-3.71739530784309,1.28989925680764));
#83130=CARTESIAN_POINT('Ctrl Pts',(39.4961406337207,-3.75499075718299,1.17595796659253));
#83131=CARTESIAN_POINT('Ctrl Pts',(39.5021902181451,-3.78728840254579,1.06062979212455));
#83132=CARTESIAN_POINT('Ctrl Pts',(39.5080346078133,-3.81849054993651,0.949213413078005));
#83133=CARTESIAN_POINT('Ctrl Pts',(39.5138789974814,-3.8447484187838,0.83650313148381));
#83134=CARTESIAN_POINT('Ctrl Pts',(39.5197233871496,-3.86597893184856,0.722977107869293));
#83135=CARTESIAN_POINT('Ctrl Pts',(39.5258755689522,-3.88832754026671,0.603472287647107));
#83136=CARTESIAN_POINT('Ctrl Pts',(39.5320277507548,-3.90510478510686,0.483064001120986));
#83137=CARTESIAN_POINT('Ctrl Pts',(39.5381799325573,-3.91627592610257,0.3623146017337));
#83138=CARTESIAN_POINT('Ctrl Pts',(39.5443321143599,-3.92744706709828,0.241565202346451));
#83139=CARTESIAN_POINT('Ctrl Pts',(39.5504842961625,-3.93301215567005,0.120475222334223));
#83140=CARTESIAN_POINT('Ctrl Pts',(39.5566364779651,-3.93299998004603,-0.000396179149394312));
#83141=CARTESIAN_POINT('',(40.806636477965,-3.93299837325538,0.00357714558460698));
#83142=CARTESIAN_POINT('Ctrl Pts',(39.5566364779651,-3.93946210749301,-0.000396830092737622));
#83143=CARTESIAN_POINT('Ctrl Pts',(39.5577092763001,-3.93949232068474,-0.0215086434630096));
#83144=CARTESIAN_POINT('Ctrl Pts',(39.5587820746351,-3.93933734594436,-0.0426200010628439));
#83145=CARTESIAN_POINT('Ctrl Pts',(39.6261372792166,-3.91789589192311,-1.36789847410651));
#83146=CARTESIAN_POINT('Ctrl Pts',(39.7587020917098,-2.45157417157785,-3.95319811699279));
#83147=CARTESIAN_POINT('Ctrl Pts',(39.9575493104495,1.99987423861761,-4.19982074625295));
#83148=CARTESIAN_POINT('Ctrl Pts',(40.156396529189,4.61427912745781,-0.588574043643822));
#83149=CARTESIAN_POINT('Ctrl Pts',(40.3552437479286,2.99010170290171,3.56332472239632));
#83150=CARTESIAN_POINT('Ctrl Pts',(40.5540909666685,-1.38072191342157,4.44202636965956));
#83151=CARTESIAN_POINT('Ctrl Pts',(40.7045549800519,-3.72834198752477,2.01939489233835));
#83152=CARTESIAN_POINT('Ctrl Pts',(40.7887365871891,-3.93466605613737,0.357674737801762));
#83153=CARTESIAN_POINT('Ctrl Pts',(40.8066357880796,-3.9315453160497,0.00358947132840354));
#83154=CARTESIAN_POINT('',(42.0566368090547,-3.93068341693143,-0.00121071286382613));
#83155=CARTESIAN_POINT('Ctrl Pts',(40.806636477965,-3.93299837325538,0.00357714558460698));
#83156=CARTESIAN_POINT('Ctrl Pts',(40.8126843498893,-3.93310722773962,-0.116106132406968));
#83157=CARTESIAN_POINT('Ctrl Pts',(40.8187322218136,-3.92774801925936,-0.235913693313374));
#83158=CARTESIAN_POINT('Ctrl Pts',(40.8247800937378,-3.91691839487931,-0.355301685692745));
#83159=CARTESIAN_POINT('Ctrl Pts',(40.8305766403865,-3.90653880620868,-0.469728392439114));
#83160=CARTESIAN_POINT('Ctrl Pts',(40.8363731870352,-3.89113439964223,-0.583769238264932));
#83161=CARTESIAN_POINT('Ctrl Pts',(40.8421697336839,-3.87075626857845,-0.696946848232061));
#83162=CARTESIAN_POINT('Ctrl Pts',(40.8479650293874,-3.85038253529231,-0.810100033488199));
#83163=CARTESIAN_POINT('Ctrl Pts',(40.853760325091,-3.82503728550107,-0.922389937950088));
#83164=CARTESIAN_POINT('Ctrl Pts',(40.8595556207946,-3.79482309977436,-1.03334729951693));
#83165=CARTESIAN_POINT('Ctrl Pts',(40.8653511347839,-3.7646077759996,-1.14430884040567));
#83166=CARTESIAN_POINT('Ctrl Pts',(40.8711466487731,-3.72952326321698,-1.25393733151824));
#83167=CARTESIAN_POINT('Ctrl Pts',(40.8769421627624,-3.68972237107758,-1.36177745038228));
#83168=CARTESIAN_POINT('Ctrl Pts',(40.8827393641702,-3.64990989053348,-1.46964896791285));
#83169=CARTESIAN_POINT('Ctrl Pts',(40.888536565578,-3.60537844794011,-1.57573068271518));
#83170=CARTESIAN_POINT('Ctrl Pts',(40.8943337669858,-3.55632914848002,-1.67958685029127));
#83171=CARTESIAN_POINT('Ctrl Pts',(40.90013741641,-3.50722529326646,-1.7835585333087));
#83172=CARTESIAN_POINT('Ctrl Pts',(40.9059410658343,-3.45359373354725,-1.88529934734926));
#83173=CARTESIAN_POINT('Ctrl Pts',(40.9117447152585,-3.39568172111523,-1.98439780509955));
#83174=CARTESIAN_POINT('Ctrl Pts',(40.9175521771462,-3.33773166582208,-2.08356136141415));
#83175=CARTESIAN_POINT('Ctrl Pts',(40.9233596390339,-3.27549579008755,-2.18007875340368));
#83176=CARTESIAN_POINT('Ctrl Pts',(40.9291671009215,-3.20926383555447,-2.27356870004014));
#83177=CARTESIAN_POINT('Ctrl Pts',(40.9349831988458,-3.14293339021857,-2.36719767171316));
#83178=CARTESIAN_POINT('Ctrl Pts',(40.9407992967701,-3.07259526719338,-2.45778988360377));
#83179=CARTESIAN_POINT('Ctrl Pts',(40.9466153946944,-2.99857846943249,-2.54499826378249));
#83180=CARTESIAN_POINT('Ctrl Pts',(40.9483387311788,-2.97664695285533,-2.57083850671945));
#83181=CARTESIAN_POINT('Ctrl Pts',(40.9500620676632,-2.9543926983173,-2.59638191712149));
#83182=CARTESIAN_POINT('Ctrl Pts',(40.9517854041476,-2.9318248420384,-2.62162012801369));
#83183=CARTESIAN_POINT('Ctrl Pts',(40.9576578502815,-2.85492255304568,-2.70762192471537));
#83184=CARTESIAN_POINT('Ctrl Pts',(40.9635302964155,-2.77410415481936,-2.79038107508411));
#83185=CARTESIAN_POINT('Ctrl Pts',(40.9694027425494,-2.68967384953248,-2.86951974782212));
#83186=CARTESIAN_POINT('Ctrl Pts',(40.9752675814942,-2.60535291558434,-2.94855590402233));
#83187=CARTESIAN_POINT('Ctrl Pts',(40.9811324204391,-2.51742967800563,-3.02398062921735));
#83188=CARTESIAN_POINT('Ctrl Pts',(40.9869972593839,-2.42624771231289,-3.09545005427264));
#83189=CARTESIAN_POINT('Ctrl Pts',(40.992856069504,-2.33515947811122,-3.1668460115569));
#83190=CARTESIAN_POINT('Ctrl Pts',(40.998714879624,-2.24081950219823,-3.23429450251988));
#83191=CARTESIAN_POINT('Ctrl Pts',(41.004573689744,-2.14360673790931,-3.29748982609345));
#83192=CARTESIAN_POINT('Ctrl Pts',(41.010659478625,-2.04262781081007,-3.36313342772154));
#83193=CARTESIAN_POINT('Ctrl Pts',(41.0167452675059,-1.93854933299478,-3.42418733847521));
#83194=CARTESIAN_POINT('Ctrl Pts',(41.0228310563869,-1.83183238460756,-3.48035617641399));
#83195=CARTESIAN_POINT('Ctrl Pts',(41.0286830864652,-1.72921449824348,-3.53436753558338));
#83196=CARTESIAN_POINT('Ctrl Pts',(41.0345351165435,-1.62415749249673,-3.58386196629385));
#83197=CARTESIAN_POINT('Ctrl Pts',(41.0403871466217,-1.51709841278372,-3.62862252182961));
#83198=CARTESIAN_POINT('Ctrl Pts',(41.0462382870002,-1.41005560954835,-3.67337627229866));
#83199=CARTESIAN_POINT('Ctrl Pts',(41.0520894273788,-1.30101171881765,-3.71339741919552));
#83200=CARTESIAN_POINT('Ctrl Pts',(41.0579405677573,-1.19042458784561,-3.74851681344137));
#83201=CARTESIAN_POINT('Ctrl Pts',(41.0637922353248,-1.07982749294963,-3.78363937195207));
#83202=CARTESIAN_POINT('Ctrl Pts',(41.0696439028923,-0.967687275392694,
-3.81385917473373));
#83203=CARTESIAN_POINT('Ctrl Pts',(41.0754955704598,-0.854477106483174,
-3.83905689909594));
#83204=CARTESIAN_POINT('Ctrl Pts',(41.081349182144,-0.741229325426693,-3.86426299497214));
#83205=CARTESIAN_POINT('Ctrl Pts',(41.0872027938282,-0.626911289451086,
-3.88444360496097));
#83206=CARTESIAN_POINT('Ctrl Pts',(41.0930564055124,-0.512005819602848,
-3.89953061799658));
#83207=CARTESIAN_POINT('Ctrl Pts',(41.0989166716123,-0.396969724629124,
-3.91463478202574));
#83208=CARTESIAN_POINT('Ctrl Pts',(41.1047769377122,-0.281345272962014,
-3.92463373775944));
#83209=CARTESIAN_POINT('Ctrl Pts',(41.1106372038121,-0.165619961988667,
-3.92951129635619));
#83210=CARTESIAN_POINT('Ctrl Pts',(41.1165014169834,-0.049816706420237,
-3.93439214014029));
#83211=CARTESIAN_POINT('Ctrl Pts',(41.1223656301548,0.0660871313754274,
-3.93414471917854));
#83212=CARTESIAN_POINT('Ctrl Pts',(41.1282298433261,0.181606251065211,-3.92880492892865));
#83213=CARTESIAN_POINT('Ctrl Pts',(41.1341026919004,0.297295479535092,-3.92345727551976));
#83214=CARTESIAN_POINT('Ctrl Pts',(41.1399755404747,0.412598449118441,-3.91300232386485));
#83215=CARTESIAN_POINT('Ctrl Pts',(41.145848389049,0.527037069608885,-3.89752754028218));
#83216=CARTESIAN_POINT('Ctrl Pts',(41.1474431336617,0.558112342742973,-3.89332543504479));
#83217=CARTESIAN_POINT('Ctrl Pts',(41.1490378782745,0.58912395400931,-3.8887534711043));
#83218=CARTESIAN_POINT('Ctrl Pts',(41.1506326228873,0.620062509520288,-3.88381403832462));
#83219=CARTESIAN_POINT('Ctrl Pts',(41.1565050690212,0.73398984261351,-3.8656251993731));
#83220=CARTESIAN_POINT('Ctrl Pts',(41.1623775151551,0.84730691306653,-3.84238876235125));
#83221=CARTESIAN_POINT('Ctrl Pts',(41.168249961289,0.959531400593865,-3.81415632758732));
#83222=CARTESIAN_POINT('Ctrl Pts',(41.1741148002338,1.0716105120929,-3.78596046522684));
#83223=CARTESIAN_POINT('Ctrl Pts',(41.1799796391787,1.18259945809538,-3.75278157521827));
#83224=CARTESIAN_POINT('Ctrl Pts',(41.1858444781235,1.29202319802029,-3.71472274278679));
#83225=CARTESIAN_POINT('Ctrl Pts',(41.1917032882435,1.40133445462451,-3.67670303334505));
#83226=CARTESIAN_POINT('Ctrl Pts',(41.1975620983635,1.50908331740957,-3.63381349433048));
#83227=CARTESIAN_POINT('Ctrl Pts',(41.2034209084835,1.6148077239633,-3.58620760896918));
#83228=CARTESIAN_POINT('Ctrl Pts',(41.2095066973645,1.7246280466353,-3.53675740289205));
#83229=CARTESIAN_POINT('Ctrl Pts',(41.2155924862454,1.83226343923973,-3.48221813427216));
#83230=CARTESIAN_POINT('Ctrl Pts',(41.2216782751264,1.93721611310014,-3.4228179517972));
#83231=CARTESIAN_POINT('Ctrl Pts',(41.2275303052047,2.03813749178024,-3.36569936597445));
#83232=CARTESIAN_POINT('Ctrl Pts',(41.2333823352829,2.13657804680104,-3.3040866217169));
#83233=CARTESIAN_POINT('Ctrl Pts',(41.2392343653612,2.23211896571971,-3.23823006021413));
#83234=CARTESIAN_POINT('Ctrl Pts',(41.2450855057397,2.32764535929759,-3.17238351106008));
#83235=CARTESIAN_POINT('Ctrl Pts',(41.2509366461182,2.42027265306176,-3.10229466205746));
#83236=CARTESIAN_POINT('Ctrl Pts',(41.2567877864967,2.50961099460106,-3.02825719775871));
#83237=CARTESIAN_POINT('Ctrl Pts',(41.2626394540642,2.59895738554353,-2.95421306266904));
#83238=CARTESIAN_POINT('Ctrl Pts',(41.2684911216317,2.68501391688605,-2.87621986881838));
#83239=CARTESIAN_POINT('Ctrl Pts',(41.2743427891991,2.76742436474649,-2.79461113312881));
#83240=CARTESIAN_POINT('Ctrl Pts',(41.2801964008834,2.84986219207291,-2.71297528432845));
#83241=CARTESIAN_POINT('Ctrl Pts',(41.2860500125676,2.92865123366631,-2.62772179587343));
#83242=CARTESIAN_POINT('Ctrl Pts',(41.2919036242519,3.00347312760742,-2.53921999278127));
#83243=CARTESIAN_POINT('Ctrl Pts',(41.2977638903517,3.07838007945944,-2.45061758038765));
#83244=CARTESIAN_POINT('Ctrl Pts',(41.3036241564516,3.14931061507326,-2.35875979870026));
#83245=CARTESIAN_POINT('Ctrl Pts',(41.3094844225515,3.21598752142227,-2.26404798139444));
#83246=CARTESIAN_POINT('Ctrl Pts',(41.3153486357228,3.28270933674064,-2.16927237273514));
#83247=CARTESIAN_POINT('Ctrl Pts',(41.321212848894,3.34517159588094,-2.07163924815229));
#83248=CARTESIAN_POINT('Ctrl Pts',(41.3270770620653,3.403142087563,-1.97157625565368));
#83249=CARTESIAN_POINT('Ctrl Pts',(41.3329499106396,3.46119794424507,-1.8713659144418));
#83250=CARTESIAN_POINT('Ctrl Pts',(41.3388227592139,3.51474864198052,-1.76871892919217));
#83251=CARTESIAN_POINT('Ctrl Pts',(41.3446956077882,3.56360924994612,-1.664084767582));
#83252=CARTESIAN_POINT('Ctrl Pts',(41.3462903524011,3.57687711993312,-1.63567184948201));
#83253=CARTESIAN_POINT('Ctrl Pts',(41.347885097014,3.5897994388583,-1.6071124979248));
#83254=CARTESIAN_POINT('Ctrl Pts',(41.3494798416269,3.60237313772528,-1.57841590735628));
#83255=CARTESIAN_POINT('Ctrl Pts',(41.3553522877608,3.64867419979032,-1.47274432773401));
#83256=CARTESIAN_POINT('Ctrl Pts',(41.3612247338948,3.69039920210543,-1.36485681852462));
#83257=CARTESIAN_POINT('Ctrl Pts',(41.3670971800287,3.72733075580979,-1.25518701267757));
#83258=CARTESIAN_POINT('Ctrl Pts',(41.3729620189735,3.764214468239,-1.14565927351416));
#83259=CARTESIAN_POINT('Ctrl Pts',(41.3788268579184,3.79631694974478,-1.03435421721276));
#83260=CARTESIAN_POINT('Ctrl Pts',(41.3846916968632,3.82346805723129,-0.921727191381479));
#83261=CARTESIAN_POINT('Ctrl Pts',(41.3905505069833,3.85059125444227,-0.809215941723395));
#83262=CARTESIAN_POINT('Ctrl Pts',(41.3964093171033,3.87277310527054,-0.695385824960153));
#83263=CARTESIAN_POINT('Ctrl Pts',(41.4022681272233,3.88989287929663,-0.580708522063683));
#83264=CARTESIAN_POINT('Ctrl Pts',(41.4083539161043,3.90767589807999,-0.461588454922284));
#83265=CARTESIAN_POINT('Ctrl Pts',(41.4144397049853,3.91999653802832,-0.341554662205697));
#83266=CARTESIAN_POINT('Ctrl Pts',(41.4205254938662,3.92677756041714,-0.221149250517372));
#83267=CARTESIAN_POINT('Ctrl Pts',(41.4263775239445,3.93329811966705,-0.105368682941397));
#83268=CARTESIAN_POINT('Ctrl Pts',(41.4322295540228,3.9346967460258,0.0107550311402793));
#83269=CARTESIAN_POINT('Ctrl Pts',(41.438081584101,3.93095757255749,0.126734220922879));
#83270=CARTESIAN_POINT('Ctrl Pts',(41.4439327244795,3.9272189675657,0.242695778079594));
#83271=CARTESIAN_POINT('Ctrl Pts',(41.449783864858,3.91834412917111,0.358512441595939));
#83272=CARTESIAN_POINT('Ctrl Pts',(41.4556350052365,3.9043693102467,0.473697465903849));
#83273=CARTESIAN_POINT('Ctrl Pts',(41.461486672804,3.89039323218815,0.58889286840678));
#83274=CARTESIAN_POINT('Ctrl Pts',(41.4673383403715,3.87131630992616,0.703456108195251));
#83275=CARTESIAN_POINT('Ctrl Pts',(41.473190007939,3.84722648696806,0.816907190549473));
#83276=CARTESIAN_POINT('Ctrl Pts',(41.4790436196232,3.82312866057726,0.930395965090257));
#83277=CARTESIAN_POINT('Ctrl Pts',(41.4848972313074,3.79401470765438,1.04277144334969));
#83278=CARTESIAN_POINT('Ctrl Pts',(41.4907508429916,3.76002316614685,1.15356611862479));
#83279=CARTESIAN_POINT('Ctrl Pts',(41.4966111090915,3.7259929828812,1.26448674585297));
#83280=CARTESIAN_POINT('Ctrl Pts',(41.5024713751914,3.68707426497149,1.37382258780479));
#83281=CARTESIAN_POINT('Ctrl Pts',(41.5083316412913,3.64345472596101,1.48112344518355));
#83282=CARTESIAN_POINT('Ctrl Pts',(41.5141958544626,3.59980580783481,1.5884965730259));
#83283=CARTESIAN_POINT('Ctrl Pts',(41.5200600676339,3.55144993620144,1.69383161235954));
#83284=CARTESIAN_POINT('Ctrl Pts',(41.5259242808052,3.49862129336033,1.79670199132903));
#83285=CARTESIAN_POINT('Ctrl Pts',(41.5317971293795,3.44571485719775,1.8997238530554));
#83286=CARTESIAN_POINT('Ctrl Pts',(41.5376699779538,3.38832270877834,2.00027345329677));
#83287=CARTESIAN_POINT('Ctrl Pts',(41.5435428265281,3.32672295032909,2.09795219482087));
#83288=CARTESIAN_POINT('Ctrl Pts',(41.5451375711409,3.30999582350222,2.12447640106608));
#83289=CARTESIAN_POINT('Ctrl Pts',(41.5467323157537,3.29295867254856,2.1507891047475));
#83290=CARTESIAN_POINT('Ctrl Pts',(41.5483270603665,3.27561757248019,2.17688275266699));
#83291=CARTESIAN_POINT('Ctrl Pts',(41.5541995065005,3.2117611560756,2.27296932390479));
#83292=CARTESIAN_POINT('Ctrl Pts',(41.5600719526344,3.14356635758723,2.36640464870643));
#83293=CARTESIAN_POINT('Ctrl Pts',(41.5659443987683,3.07128040853467,2.45677138784852));
#83294=CARTESIAN_POINT('Ctrl Pts',(41.5718092377132,2.99908809897565,2.54702106557277));
#83295=CARTESIAN_POINT('Ctrl Pts',(41.577674076658,2.92281543388061,2.63420974279851));
#83296=CARTESIAN_POINT('Ctrl Pts',(41.5835389156029,2.8427534576025,2.71794808252274));
#83297=CARTESIAN_POINT('Ctrl Pts',(41.5893977257229,2.76277378190151,2.80160034251215));
#83298=CARTESIAN_POINT('Ctrl Pts',(41.5952565358429,2.67901282685052,2.8818090228245));
#83299=CARTESIAN_POINT('Ctrl Pts',(41.601115345963,2.59180209451376,2.95821752122357));
#83300=CARTESIAN_POINT('Ctrl Pts',(41.6072011348439,2.50121269252215,3.03758619514228));
#83301=CARTESIAN_POINT('Ctrl Pts',(41.6132869237249,2.4069010922651,3.1128539280669));
#83302=CARTESIAN_POINT('Ctrl Pts',(41.6193727126059,2.30928155488068,3.18366262350266));
#83303=CARTESIAN_POINT('Ctrl Pts',(41.6252247426841,2.21541164250376,3.25175151445801));
#83304=CARTESIAN_POINT('Ctrl Pts',(41.6310767727624,2.11848359066862,3.31571733263689));
#83305=CARTESIAN_POINT('Ctrl Pts',(41.6369288028407,2.0188990529887,3.37528304203386));
#83306=CARTESIAN_POINT('Ctrl Pts',(41.6427799432192,1.91932965541181,3.43483969549706));
#83307=CARTESIAN_POINT('Ctrl Pts',(41.6486310835977,1.81710492966494,3.48999735816178));
#83308=CARTESIAN_POINT('Ctrl Pts',(41.6544822239763,1.71265393275851,3.5405233379554));
#83309=CARTESIAN_POINT('Ctrl Pts',(41.6603338915438,1.60819352479486,3.59105387015062));
#83310=CARTESIAN_POINT('Ctrl Pts',(41.6661855591113,1.50150681905239,3.63695170987969));
#83311=CARTESIAN_POINT('Ctrl Pts',(41.6720372266788,1.39304514332302,3.67803129794516));
#83312=CARTESIAN_POINT('Ctrl Pts',(41.6778908383631,1.28454743305186,3.71912453400308));
#83313=CARTESIAN_POINT('Ctrl Pts',(41.6837444500474,1.17427396655959,3.75539618900909));
#83314=CARTESIAN_POINT('Ctrl Pts',(41.6895980617316,1.06269292353887,3.78671001665831));
#83315=CARTESIAN_POINT('Ctrl Pts',(41.6954583278315,0.950985034619151,3.81805944202657));
#83316=CARTESIAN_POINT('Ctrl Pts',(41.7013185939314,0.837967000464165,3.84443967884929));
#83317=CARTESIAN_POINT('Ctrl Pts',(41.7071788600313,0.724119031370313,3.865765206063));
#83318=CARTESIAN_POINT('Ctrl Pts',(41.7130430732026,0.610194382129835,3.88710509668228));
#83319=CARTESIAN_POINT('Ctrl Pts',(41.7189072863739,0.495439093153907,3.90338344072787));
#83320=CARTESIAN_POINT('Ctrl Pts',(41.7247714995453,0.380338625256995,3.91456658266756));
#83321=CARTESIAN_POINT('Ctrl Pts',(41.7306443481196,0.265068665068968,3.92576619244952));
#83322=CARTESIAN_POINT('Ctrl Pts',(41.7365171966939,0.149452922732807,3.93185560399583));
#83323=CARTESIAN_POINT('Ctrl Pts',(41.7423900452682,0.0339770745151441,
3.9328532337741));
#83324=CARTESIAN_POINT('Ctrl Pts',(41.7439847898808,0.00262014703646743,
3.9331241354829));
#83325=CARTESIAN_POINT('Ctrl Pts',(41.7455795344935,-0.0287264958199402,
3.93301988053087));
#83326=CARTESIAN_POINT('Ctrl Pts',(41.7471742791062,-0.0600532154152404,
3.93254149518073));
#83327=CARTESIAN_POINT('Ctrl Pts',(41.7530467252401,-0.175409913857684,
3.93077990139472));
#83328=CARTESIAN_POINT('Ctrl Pts',(41.758919171374,-0.290882167778746,3.92393526583223));
#83329=CARTESIAN_POINT('Ctrl Pts',(41.7647916175079,-0.405985227089397,
3.91198990226012));
#83330=CARTESIAN_POINT('Ctrl Pts',(41.7706564564528,-0.520939181459127,
3.90006001275743));
#83331=CARTESIAN_POINT('Ctrl Pts',(41.7765212953976,-0.635524484941258,
3.88304257749326));
#83332=CARTESIAN_POINT('Ctrl Pts',(41.7823861343425,-0.749256253116583,
3.86097190706766));
#83333=CARTESIAN_POINT('Ctrl Pts',(41.7882449444625,-0.862871109487015,
3.83892392442716));
#83334=CARTESIAN_POINT('Ctrl Pts',(41.7941037545825,-0.975633772398393,
3.8118331170997));
#83335=CARTESIAN_POINT('Ctrl Pts',(41.7999625647026,-1.08706501831039,3.7797855290963));
#83336=CARTESIAN_POINT('Ctrl Pts',(41.8060483535835,-1.20281327153411,3.74649637127466));
#83337=CARTESIAN_POINT('Ctrl Pts',(41.8121341424645,-1.31712440735174,3.70785864630608));
#83338=CARTESIAN_POINT('Ctrl Pts',(41.8182199313455,-1.42947319656069,3.66402720791134));
#83339=CARTESIAN_POINT('Ctrl Pts',(41.8240719614238,-1.53750660136114,3.62187936136642));
#83340=CARTESIAN_POINT('Ctrl Pts',(41.829923991502,-1.64372520790638,3.57492959298137));
#83341=CARTESIAN_POINT('Ctrl Pts',(41.8357760215803,-1.7476787928177,3.52336598115144));
#83342=CARTESIAN_POINT('Ctrl Pts',(41.8416271619588,-1.85161657338814,3.471810208675));
#83343=CARTESIAN_POINT('Ctrl Pts',(41.8474783023374,-1.95328964681564,3.41564217110512));
#83344=CARTESIAN_POINT('Ctrl Pts',(41.8533294427159,-2.05227027493576,3.35509697603737));
#83345=CARTESIAN_POINT('Ctrl Pts',(41.8591811102834,-2.15125982123112,3.29454632583492));
#83346=CARTESIAN_POINT('Ctrl Pts',(41.8650327778509,-2.24755608733207,3.22961794984392));
#83347=CARTESIAN_POINT('Ctrl Pts',(41.8708844454184,-2.34075894162928,3.16059117526809));
#83348=CARTESIAN_POINT('Ctrl Pts',(41.8767380571026,-2.43399276098545,3.09154146772353));
#83349=CARTESIAN_POINT('Ctrl Pts',(41.8825916687869,-2.52413079295164,3.01839089997251));
#83350=CARTESIAN_POINT('Ctrl Pts',(41.8884452804711,-2.61080527636804,2.94145963917385));
#83351=CARTESIAN_POINT('Ctrl Pts',(41.894305546571,-2.69757829177952,2.86444092252531));
#83352=CARTESIAN_POINT('Ctrl Pts',(41.9001658126709,-2.78087959043404,2.78363320889896));
#83353=CARTESIAN_POINT('Ctrl Pts',(41.9060260787708,-2.86037757662643,2.69939421336208));
#83354=CARTESIAN_POINT('Ctrl Pts',(41.9118902919421,-2.93992910718403,2.61509848024282));
#83355=CARTESIAN_POINT('Ctrl Pts',(41.9177545051134,-3.01567195505458,2.52736717551507));
#83356=CARTESIAN_POINT('Ctrl Pts',(41.9236187182847,-3.08731531527128,2.43659047525254));
#83357=CARTESIAN_POINT('Ctrl Pts',(41.9294915668589,-3.15906417460091,2.34568010089484));
#83358=CARTESIAN_POINT('Ctrl Pts',(41.9353644154332,-3.22670125756978,2.2517157150014));
#83359=CARTESIAN_POINT('Ctrl Pts',(41.9412372640075,-3.28997944614429,2.15511583074973));
#83360=CARTESIAN_POINT('Ctrl Pts',(41.9428320086203,-3.30716234283552,2.12888458316073));
#83361=CARTESIAN_POINT('Ctrl Pts',(41.9444267532331,-3.32402409339884,2.10245913603982));
#83362=CARTESIAN_POINT('Ctrl Pts',(41.9460214978459,-3.3405603494249,2.07584815240666));
#83363=CARTESIAN_POINT('Ctrl Pts',(41.9520612572671,-3.4031879371436,1.9750646552753));
#83364=CARTESIAN_POINT('Ctrl Pts',(41.9581010166883,-3.46134306028622,1.8712965097234));
#83365=CARTESIAN_POINT('Ctrl Pts',(41.9641407761096,-3.51473849071923,1.76496525230859));
#83366=CARTESIAN_POINT('Ctrl Pts',(41.9701712777305,-3.56805207613178,1.65879698045018));
#83367=CARTESIAN_POINT('Ctrl Pts',(41.9762017793514,-3.61662032103247,1.55007375489776));
#83368=CARTESIAN_POINT('Ctrl Pts',(41.9822322809723,-3.66019984270016,1.43924497966738));
#83369=CARTESIAN_POINT('Ctrl Pts',(41.9884326307217,-3.70500677473279,1.32529472943574));
#83370=CARTESIAN_POINT('Ctrl Pts',(41.9946329804711,-3.74453955918482,1.20911888860736));
#83371=CARTESIAN_POINT('Ctrl Pts',(42.0008333302205,-3.77858418078361,1.09123351704934));
#83372=CARTESIAN_POINT('Ctrl Pts',(42.006846728243,-3.81160229564376,0.976902602042955));
#83373=CARTESIAN_POINT('Ctrl Pts',(42.0128601262655,-3.83945829879576,0.860964158620311));
#83374=CARTESIAN_POINT('Ctrl Pts',(42.018873524288,-3.86200575857607,0.743908946528562));
#83375=CARTESIAN_POINT('Ctrl Pts',(42.0251673499008,-3.8856046920475,0.621395005288603));
#83376=CARTESIAN_POINT('Ctrl Pts',(42.0314611755136,-3.9033878463458,0.497658012167005));
#83377=CARTESIAN_POINT('Ctrl Pts',(42.0377550011265,-3.91524622943359,0.373277327072032));
#83378=CARTESIAN_POINT('Ctrl Pts',(42.0440488267393,-3.92710461252138,0.248896641977059));
#83379=CARTESIAN_POINT('Ctrl Pts',(42.0503426523522,-3.9330381322875,0.123872739030405));
#83380=CARTESIAN_POINT('Ctrl Pts',(42.056636477965,-3.93299981544993,-0.00120485302445938));
#83381=CARTESIAN_POINT('',(43.306636477965,-3.93597073404585,-0.00313681186104915));
#83382=CARTESIAN_POINT('Ctrl Pts',(42.0566373589272,-3.9268363506648,-0.00122044486381472));
#83383=CARTESIAN_POINT('Ctrl Pts',(42.08604781148,-3.92842785028224,-0.584780799616886));
#83384=CARTESIAN_POINT('Ctrl Pts',(42.1817406702796,-3.53244649474052,-2.48145397176705));
#83385=CARTESIAN_POINT('Ctrl Pts',(42.343715935325,-0.592762475981856,-4.61374294017385));
#83386=CARTESIAN_POINT('Ctrl Pts',(42.5425631540648,3.56060894862422,-2.99333512756587));
#83387=CARTESIAN_POINT('Ctrl Pts',(42.7414103728044,4.44327790862288,1.37668903448674));
#83388=CARTESIAN_POINT('Ctrl Pts',(42.9402575915441,1.2444427730145,4.48211484186561));
#83389=CARTESIAN_POINT('Ctrl Pts',(43.1286662932643,-2.86958038868927,3.52347388524056));
#83390=CARTESIAN_POINT('Ctrl Pts',(43.2507925887379,-3.9263799435556,1.09839315991139));
#83391=CARTESIAN_POINT('Ctrl Pts',(43.306636477965,-3.93597073404585,-0.00313681186104915));
#83392=CARTESIAN_POINT('',(44.556636477965,-3.93423236178689,0.00274293657858196));
#83393=CARTESIAN_POINT('Ctrl Pts',(43.306636477965,-3.93597073404585,-0.00313681186104915));
#83394=CARTESIAN_POINT('Ctrl Pts',(43.3170749949845,-3.93776347504488,-0.209038290373662));
#83395=CARTESIAN_POINT('Ctrl Pts',(43.39379591825,-3.82930594892105,-1.72047837853632));
#83396=CARTESIAN_POINT('Ctrl Pts',(43.5367992477632,-1.87070203706735,-4.25892770068468));
#83397=CARTESIAN_POINT('Ctrl Pts',(43.7356464665026,2.57114020051616,-3.8764970450033));
#83398=CARTESIAN_POINT('Ctrl Pts',(43.9344936852423,4.65118570275307,0.0668044115854355));
#83399=CARTESIAN_POINT('Ctrl Pts',(44.133340903982,2.4587472673275,3.94874070401929));
#83400=CARTESIAN_POINT('Ctrl Pts',(44.3321881227215,-1.99224605665835,4.20344464912718));
#83401=CARTESIAN_POINT('Ctrl Pts',(44.4732866473825,-3.8520314402992,1.64433913035412));
#83402=CARTESIAN_POINT('Ctrl Pts',(44.5481027657971,-3.93833159539374,0.170959590838341));
#83403=CARTESIAN_POINT('Ctrl Pts',(44.556636477965,-3.93699635256031,0.00274486362576644));
#83404=CARTESIAN_POINT('',(45.8066364523549,-3.93089729110193,0.00177639705978037));
#83405=CARTESIAN_POINT('Ctrl Pts',(44.556636477965,-3.93299904411574,0.00274207671270665));
#83406=CARTESIAN_POINT('Ctrl Pts',(44.5624206881413,-3.93307845537151,-0.111158599951776));
#83407=CARTESIAN_POINT('Ctrl Pts',(44.5682048983176,-3.92820579813593,-0.225252330880906));
#83408=CARTESIAN_POINT('Ctrl Pts',(44.5739891084939,-3.91835726600955,-0.339065385892148));
#83409=CARTESIAN_POINT('Ctrl Pts',(44.5797669192364,-3.90851962993069,-0.452752522396843));
#83410=CARTESIAN_POINT('Ctrl Pts',(44.5855447299789,-3.89371709785247,-0.566159178932715));
#83411=CARTESIAN_POINT('Ctrl Pts',(44.5913225407214,-3.87397789315147,-0.67881093345179));
#83412=CARTESIAN_POINT('Ctrl Pts',(44.5970958748664,-3.85425398221473,-0.791375406370457));
#83413=CARTESIAN_POINT('Ctrl Pts',(44.6028692090114,-3.82960107394074,-0.903185721844889));
#83414=CARTESIAN_POINT('Ctrl Pts',(44.6086425431563,-3.80009920536556,-1.01377267145058));
#83415=CARTESIAN_POINT('Ctrl Pts',(44.6144130463777,-3.7706118028743,-1.12430539533532));
#83416=CARTESIAN_POINT('Ctrl Pts',(44.6201835495991,-3.73628027642083,-1.23361553491909));
#83417=CARTESIAN_POINT('Ctrl Pts',(44.6259540528205,-3.69723556713716,-1.34124500412712));
#83418=CARTESIAN_POINT('Ctrl Pts',(44.6317234956459,-3.65819803276486,-1.44885469519065));
#83419=CARTESIAN_POINT('Ctrl Pts',(44.6374929384714,-3.61444918202758,-1.55478392921504));
#83420=CARTESIAN_POINT('Ctrl Pts',(44.6432623812969,-3.5661692773945,-1.65859147621335));
#83421=CARTESIAN_POINT('Ctrl Pts',(44.6490322530335,-3.51788578354319,-1.76240674045847));
#83422=CARTESIAN_POINT('Ctrl Pts',(44.6548021247701,-3.46507074697258,-1.86409961824766));
#83423=CARTESIAN_POINT('Ctrl Pts',(44.6605719965068,-3.40795148119965,-1.96325130887237));
#83424=CARTESIAN_POINT('Ctrl Pts',(44.6663478768146,-3.35077273313811,-2.0625062530911));
#83425=CARTESIAN_POINT('Ctrl Pts',(44.6721237571224,-3.28928101433859,-2.15921435327852));
#83426=CARTESIAN_POINT('Ctrl Pts',(44.6778996374303,-3.22374836692943,-2.2529836809706));
#83427=CARTESIAN_POINT('Ctrl Pts',(44.6836778400347,-3.15818937094041,-2.34679071030784));
#83428=CARTESIAN_POINT('Ctrl Pts',(44.6894560426391,-3.08858647423604,-2.4376562789466));
#83429=CARTESIAN_POINT('Ctrl Pts',(44.6952342452436,-3.01525226988168,-2.52522132673027));
#83430=CARTESIAN_POINT('Ctrl Pts',(44.7010220474629,-2.94179623177173,-2.61293185067644));
#83431=CARTESIAN_POINT('Ctrl Pts',(44.7068098496823,-2.86459678953794,-2.69733058461385));
#83432=CARTESIAN_POINT('Ctrl Pts',(44.7125976519017,-2.78400402223915,-2.77809477954879));
#83433=CARTESIAN_POINT('Ctrl Pts',(44.7183592880014,-2.70377560740306,-2.85849384701251));
#83434=CARTESIAN_POINT('Ctrl Pts',(44.7241209241011,-2.62018485274011,-2.93529096204368));
#83435=CARTESIAN_POINT('Ctrl Pts',(44.7298825602008,-2.53360749863687,-3.00820910889702));
#83436=CARTESIAN_POINT('Ctrl Pts',(44.7357550063304,-2.44536505513321,-3.082529645956));
#83437=CARTESIAN_POINT('Ctrl Pts',(44.7416274524601,-2.35370193720534,-3.15308858054237));
#83438=CARTESIAN_POINT('Ctrl Pts',(44.7474998985897,-2.25897250273774,-3.21955466359476));
#83439=CARTESIAN_POINT('Ctrl Pts',(44.7533647375302,-2.16436578114149,-3.28593464622922));
#83440=CARTESIAN_POINT('Ctrl Pts',(44.7592295764707,-2.06670097739061,-3.34823208568584));
#83441=CARTESIAN_POINT('Ctrl Pts',(44.7650944154112,-1.96636665008259,-3.40615489921451));
#83442=CARTESIAN_POINT('Ctrl Pts',(44.7709532255268,-1.86613546253602,-3.46401817035793));
#83443=CARTESIAN_POINT('Ctrl Pts',(44.7768120356424,-1.76324056556485,-3.51751555481816));
#83444=CARTESIAN_POINT('Ctrl Pts',(44.782670845758,-1.65810017070269,-3.56639773776225));
#83445=CARTESIAN_POINT('Ctrl Pts',(44.7887566346406,-1.54888648506683,-3.61717368708458));
#83446=CARTESIAN_POINT('Ctrl Pts',(44.7948424235232,-1.43725016692758,-3.66296934236462));
#83447=CARTESIAN_POINT('Ctrl Pts',(44.8009282124058,-1.32368928437454,-3.70355716554126));
#83448=CARTESIAN_POINT('Ctrl Pts',(44.8067802424795,-1.21449034357772,-3.74258598603381));
#83449=CARTESIAN_POINT('Ctrl Pts',(44.8126322725532,-1.10351238371233,-3.77679951451677));
#83450=CARTESIAN_POINT('Ctrl Pts',(44.8184843026268,-0.991218636692286,
-3.80604448401144));
#83451=CARTESIAN_POINT('Ctrl Pts',(44.8243354430007,-0.878941961991345,
-3.83528500731507));
#83452=CARTESIAN_POINT('Ctrl Pts',(44.8301865833746,-0.765350297790627,
-3.85955836943044));
#83453=CARTESIAN_POINT('Ctrl Pts',(44.8360377237485,-0.650920742602548,
-3.87876155323445));
#83454=CARTESIAN_POINT('Ctrl Pts',(44.8418893913113,-0.536480877287995,
-3.89796646724928));
#83455=CARTESIAN_POINT('Ctrl Pts',(44.8477410588741,-0.421203378591719,
-3.91210022641299));
#83456=CARTESIAN_POINT('Ctrl Pts',(44.8535927264369,-0.305573502809252,
-3.92111130094274));
#83457=CARTESIAN_POINT('Ctrl Pts',(44.8594463381164,-0.189905210974066,
-3.93012536924821));
#83458=CARTESIAN_POINT('Ctrl Pts',(44.8652999497959,-0.0738847211529398,
-3.93401333664791));
#83459=CARTESIAN_POINT('Ctrl Pts',(44.8711535614754,0.0420003653842455,
-3.93277573341115));
#83460=CARTESIAN_POINT('Ctrl Pts',(44.8770138275706,0.158017190679275,-3.9315367232607));
#83461=CARTESIAN_POINT('Ctrl Pts',(44.8828740936657,0.273897891879422,-3.9251605168428));
#83462=CARTESIAN_POINT('Ctrl Pts',(44.8887343597608,0.389157546645517,-3.91369970793479));
#83463=CARTESIAN_POINT('Ctrl Pts',(44.8945985729274,0.504494832372195,-3.90223117981569));
#83464=CARTESIAN_POINT('Ctrl Pts',(44.9004627860939,0.619209830641658,-3.88567128897828));
#83465=CARTESIAN_POINT('Ctrl Pts',(44.9063269992604,0.732827125818421,-3.86412388565179));
#83466=CARTESIAN_POINT('Ctrl Pts',(44.9121998478299,0.846611729225945,-3.8425447524912));
#83467=CARTESIAN_POINT('Ctrl Pts',(44.9180726963994,0.959295002661169,-3.81596354341015));
#83468=CARTESIAN_POINT('Ctrl Pts',(44.9239455449689,1.07041592807867,-3.78453415110968));
#83469=CARTESIAN_POINT('Ctrl Pts',(44.9255402896261,1.10059029746953,-3.77599964611486));
#83470=CARTESIAN_POINT('Ctrl Pts',(44.9271350342834,1.1306495765463,-3.76710792615816));
#83471=CARTESIAN_POINT('Ctrl Pts',(44.9287297789406,1.16058480135576,-3.7578626796175));
#83472=CARTESIAN_POINT('Ctrl Pts',(44.9346022251097,1.27081749312859,-3.72381822467294));
#83473=CARTESIAN_POINT('Ctrl Pts',(44.9404746712788,1.37973548501979,-3.68486233087554));
#83474=CARTESIAN_POINT('Ctrl Pts',(44.9463471174479,1.48686852242519,-3.64111397748287));
#83475=CARTESIAN_POINT('Ctrl Pts',(44.952211956428,1.59386277928895,-3.59742229587257));
#83476=CARTESIAN_POINT('Ctrl Pts',(44.9580767954082,1.69907630073164,-3.54895065533863));
#83477=CARTESIAN_POINT('Ctrl Pts',(44.9639416343883,1.80205328652408,-3.4958679827087));
#83478=CARTESIAN_POINT('Ctrl Pts',(44.9698004445437,1.90492441600864,-3.44283987698702));
#83479=CARTESIAN_POINT('Ctrl Pts',(44.9756592546991,2.00556321761252,-3.38521035546842));
#83480=CARTESIAN_POINT('Ctrl Pts',(44.9815180648545,2.1035338342139,-3.32319641434529));
#83481=CARTESIAN_POINT('Ctrl Pts',(44.9876038537222,2.20529997308246,-3.25877996415797));
#83482=CARTESIAN_POINT('Ctrl Pts',(44.99368964259,2.30418658640912,-3.18963267796784));
#83483=CARTESIAN_POINT('Ctrl Pts',(44.9997754314577,2.39973295664176,-3.11605050292953));
#83484=CARTESIAN_POINT('Ctrl Pts',(45.0056274615712,2.4916093342146,-3.0452946628072));
#83485=CARTESIAN_POINT('Ctrl Pts',(45.0114794916848,2.58039697900309,-2.9704386182479));
#83486=CARTESIAN_POINT('Ctrl Pts',(45.0173315217983,2.66571648721625,-2.89178917104679));
#83487=CARTESIAN_POINT('Ctrl Pts',(45.023182662212,2.75102302407562,-2.81315168113219));
#83488=CARTESIAN_POINT('Ctrl Pts',(45.0290338026257,2.83286216890139,-2.73072221537499));
#83489=CARTESIAN_POINT('Ctrl Pts',(45.0348849430394,2.91088929071739,-2.64484641088794));
#83490=CARTESIAN_POINT('Ctrl Pts',(45.040736610642,2.98892344279184,-2.55896286897464));
#83491=CARTESIAN_POINT('Ctrl Pts',(45.0465882782445,3.06314461109269,-2.46963267700669));
#83492=CARTESIAN_POINT('Ctrl Pts',(45.0524399458471,3.13324706525646,-2.37723617422875));
#83493=CARTESIAN_POINT('Ctrl Pts',(45.0582935575662,3.20337280976299,-2.28480897429129));
#83494=CARTESIAN_POINT('Ctrl Pts',(45.0641471692853,3.26937686949293,-2.1893137669915));
#83495=CARTESIAN_POINT('Ctrl Pts',(45.0700007810045,3.3309960395111,-2.09116101359062));
#83496=CARTESIAN_POINT('Ctrl Pts',(45.0758610471389,3.39268525851159,-1.99289667964614));
#83497=CARTESIAN_POINT('Ctrl Pts',(45.0817213132733,3.44997941846655,-1.8919691198558));
#83498=CARTESIAN_POINT('Ctrl Pts',(45.0875815794076,3.50266055925314,-1.78881469321238));
#83499=CARTESIAN_POINT('Ctrl Pts',(45.0934457926132,3.55537718242393,-1.6855907888594));
#83500=CARTESIAN_POINT('Ctrl Pts',(45.0993100058188,3.60347442862843,-1.5801374062886));
#83501=CARTESIAN_POINT('Ctrl Pts',(45.1051742190244,3.64678259549991,-1.47291062225748));
#83502=CARTESIAN_POINT('Ctrl Pts',(45.1110470676325,3.69015453622069,-1.36552594041497));
#83503=CARTESIAN_POINT('Ctrl Pts',(45.1169199162405,3.72872318563004,-1.25636303347945));
#83504=CARTESIAN_POINT('Ctrl Pts',(45.1227927648485,3.76236872245895,-1.14589292530437));
#83505=CARTESIAN_POINT('Ctrl Pts',(45.1243875091257,3.77150500893467,-1.11589528964697));
#83506=CARTESIAN_POINT('Ctrl Pts',(45.1259822534029,3.78027857266151,-1.08580131924658));
#83507=CARTESIAN_POINT('Ctrl Pts',(45.1275769976801,3.78868766943574,-1.05562054899741));
#83508=CARTESIAN_POINT('Ctrl Pts',(45.1334494437569,3.81965311516091,-0.944483642360871));
#83509=CARTESIAN_POINT('Ctrl Pts',(45.1393218898338,3.84577614321039,-0.831797007719057));
#83510=CARTESIAN_POINT('Ctrl Pts',(45.1451943359106,3.86690256851341,-0.718020560725395));
#83511=CARTESIAN_POINT('Ctrl Pts',(45.1510591747984,3.88800162656469,-0.604391500174129));
#83512=CARTESIAN_POINT('Ctrl Pts',(45.1569240136862,3.90411687883725,-0.489675837397397));
#83513=CARTESIAN_POINT('Ctrl Pts',(45.1627888525741,3.91514397222974,-0.374348336062974));
#83514=CARTESIAN_POINT('Ctrl Pts',(45.1686476626372,3.92615973020211,-0.259139386883065));
#83515=CARTESIAN_POINT('Ctrl Pts',(45.1745064727003,3.93209769379473,-0.143320259163626));
#83516=CARTESIAN_POINT('Ctrl Pts',(45.1803652827635,3.93290472972664,-0.0273749318511684));
#83517=CARTESIAN_POINT('Ctrl Pts',(45.1864510716658,3.93374303140654,0.0930622863947814));
#83518=CARTESIAN_POINT('Ctrl Pts',(45.1925368605682,3.92904472264376,0.213635233589722));
#83519=CARTESIAN_POINT('Ctrl Pts',(45.1986226494705,3.91880964212148,0.333796328343629));
#83520=CARTESIAN_POINT('Ctrl Pts',(45.2044746794926,3.90896769731263,0.449341961830767));
#83521=CARTESIAN_POINT('Ctrl Pts',(45.2103267095148,3.89400651467889,0.564506348318379));
#83522=CARTESIAN_POINT('Ctrl Pts',(45.2161787395369,3.87397903110801,0.678804439095266));
#83523=CARTESIAN_POINT('Ctrl Pts',(45.2220298798596,3.85395459236771,0.793085152835175));
#83524=CARTESIAN_POINT('Ctrl Pts',(45.2278810201823,3.82886545550704,0.90649942569439));
#83525=CARTESIAN_POINT('Ctrl Pts',(45.233732160505,3.79881602804613,1.01857046150957));
#83526=CARTESIAN_POINT('Ctrl Pts',(45.2395838280172,3.7687638931234,1.13065159495643));
#83527=CARTESIAN_POINT('Ctrl Pts',(45.2454354955293,3.73375068621552,1.2413888514924));
#83528=CARTESIAN_POINT('Ctrl Pts',(45.2512871630414,3.69393104054491,1.35031939469845));
#83529=CARTESIAN_POINT('Ctrl Pts',(45.2571407746707,3.65409816547271,1.45928612822909));
#83530=CARTESIAN_POINT('Ctrl Pts',(45.2629943863,3.60945581822659,1.56644456684418));
#83531=CARTESIAN_POINT('Ctrl Pts',(45.2688479979294,3.5602069648722,1.67135135961158));
#83532=CARTESIAN_POINT('Ctrl Pts',(45.2747082639753,3.51090212516121,1.77637741097504));
#83533=CARTESIAN_POINT('Ctrl Pts',(45.2805685300213,3.45698050282509,1.87914633305179));
#83534=CARTESIAN_POINT('Ctrl Pts',(45.2864287960673,3.39869131366523,1.97923883208079));
#83535=CARTESIAN_POINT('Ctrl Pts',(45.2922930091851,3.34036286491889,2.07939874652897));
#83536=CARTESIAN_POINT('Ctrl Pts',(45.298157222303,3.27766121491813,2.17687830168419));
#83537=CARTESIAN_POINT('Ctrl Pts',(45.3040214354209,3.2108782596862,2.27128813704349));
#83538=CARTESIAN_POINT('Ctrl Pts',(45.3098942839429,3.14399696256334,2.36583699652503));
#83539=CARTESIAN_POINT('Ctrl Pts',(45.3157671324649,3.07302261796205,2.45730678915368));
#83540=CARTESIAN_POINT('Ctrl Pts',(45.3216399809869,2.99828666675576,2.54534203280318));
#83541=CARTESIAN_POINT('Ctrl Pts',(45.3232347261312,2.97799246116798,2.56924760040159));
#83542=CARTESIAN_POINT('Ctrl Pts',(45.3248294712755,2.95742108973002,2.592900131298));
#83543=CARTESIAN_POINT('Ctrl Pts',(45.3264242164198,2.93657963018286,2.61629300262702));
#83544=CARTESIAN_POINT('Ctrl Pts',(45.332296662543,2.8598336066834,2.70243427544308));
#83545=CARTESIAN_POINT('Ctrl Pts',(45.3381691086663,2.779165593308,2.78534001710213));
#83546=CARTESIAN_POINT('Ctrl Pts',(45.3440415547895,2.69487910576092,2.86463184464134));
#83547=CARTESIAN_POINT('Ctrl Pts',(45.3499063937232,2.61070180325834,2.94382095723808));
#83548=CARTESIAN_POINT('Ctrl Pts',(45.3557712326568,2.52291564642326,3.0194051848909));
#83549=CARTESIAN_POINT('Ctrl Pts',(45.3616360715904,2.4318635858981,3.09104003526043));
#83550=CARTESIAN_POINT('Ctrl Pts',(45.3674948816987,2.34090512333472,3.16260124780181));
#83551=CARTESIAN_POINT('Ctrl Pts',(45.373353691807,2.24668775769553,3.23022090418208));
#83552=CARTESIAN_POINT('Ctrl Pts',(45.3792125019153,2.14958988667897,3.29359261583571));
#83553=CARTESIAN_POINT('Ctrl Pts',(45.3852982908005,2.04873030371198,3.35941943924977));
#83554=CARTESIAN_POINT('Ctrl Pts',(45.3913840796857,1.94476284241733,3.42066220667751));
#83555=CARTESIAN_POINT('Ctrl Pts',(45.3974698685708,1.8381480459053,3.47702469955773));
#83556=CARTESIAN_POINT('Ctrl Pts',(45.4033218986362,1.73562838799901,3.53122227510883));
#83557=CARTESIAN_POINT('Ctrl Pts',(45.4091739287015,1.63066141412722,3.58090735796026));
#83558=CARTESIAN_POINT('Ctrl Pts',(45.4150259587668,1.52368377511028,3.62586220828449));
#83559=CARTESIAN_POINT('Ctrl Pts',(45.420877099132,1.41672240019707,3.67081022399959));
#83560=CARTESIAN_POINT('Ctrl Pts',(45.4267282394971,1.30775134891695,3.71102927699763));
#83561=CARTESIAN_POINT('Ctrl Pts',(45.4325793798623,1.19722816067176,3.7463493872428));
#83562=CARTESIAN_POINT('Ctrl Pts',(45.438431047416,1.08669501427171,3.7816726798349));
#83563=CARTESIAN_POINT('Ctrl Pts',(45.4442827149697,0.974609846665904,3.81209602638497));
#83564=CARTESIAN_POINT('Ctrl Pts',(45.4501343825235,0.861445611746805,3.83749924534223));
#83565=CARTESIAN_POINT('Ctrl Pts',(45.4559879941936,0.748243779948002,3.86291090408409));
#83566=CARTESIAN_POINT('Ctrl Pts',(45.4618416058637,0.633962571083644,3.88329902832254));
#83567=CARTESIAN_POINT('Ctrl Pts',(45.4676952175337,0.519084681744792,3.89859463052751));
#83568=CARTESIAN_POINT('Ctrl Pts',(45.473555483619,0.404076198644307,3.91390762084989));
#83569=CARTESIAN_POINT('Ctrl Pts',(45.4794157497042,0.288470091169484,3.92411647949205));
#83570=CARTESIAN_POINT('Ctrl Pts',(45.4852760157895,0.172753826510763,3.92920413257264));
#83571=CARTESIAN_POINT('Ctrl Pts',(45.4911402289458,0.0569596233558427,
3.9342952123455));
#83572=CARTESIAN_POINT('Ctrl Pts',(45.4970044421022,-0.0589444723727581,
3.9342582184567));
#83573=CARTESIAN_POINT('Ctrl Pts',(45.5028686552585,-0.174473095974319,
3.92912816522713));
#83574=CARTESIAN_POINT('Ctrl Pts',(45.5087415038176,-0.290171842345175,
3.92399055768907));
#83575=CARTESIAN_POINT('Ctrl Pts',(45.5146143523766,-0.405493602914874,
3.91374495908021));
#83576=CARTESIAN_POINT('Ctrl Pts',(45.5204872009356,-0.519960129469059,
3.89847796758716));
#83577=CARTESIAN_POINT('Ctrl Pts',(45.5220819456768,-0.551042982949431,
3.89433228697686));
#83578=CARTESIAN_POINT('Ctrl Pts',(45.5236766904181,-0.582062846145865,
3.88981663263307));
#83579=CARTESIAN_POINT('Ctrl Pts',(45.5252714351593,-0.613010320845078,
3.8849333773615));
#83580=CARTESIAN_POINT('Ctrl Pts',(45.5311438815243,-0.726970493028684,
3.86695140574754));
#83581=CARTESIAN_POINT('Ctrl Pts',(45.5370163278893,-0.8403295674727,3.84392073604923));
#83582=CARTESIAN_POINT('Ctrl Pts',(45.5428887742542,-0.952605130974747,
3.81589209287168));
#83583=CARTESIAN_POINT('Ctrl Pts',(45.5487536134309,-1.06473525230577,3.78789975809987));
#83584=CARTESIAN_POINT('Ctrl Pts',(45.5546184526076,-1.17578425657252,3.75492242430939));
#83585=CARTESIAN_POINT('Ctrl Pts',(45.5604832917843,-1.28527691679575,3.71706231413357));
#83586=CARTESIAN_POINT('Ctrl Pts',(45.5663421021367,-1.39465702286518,3.67924112266385));
#83587=CARTESIAN_POINT('Ctrl Pts',(45.5722009124892,-1.5024835787848,3.63654727274737));
#83588=CARTESIAN_POINT('Ctrl Pts',(45.5780597228416,-1.60829424422621,3.58913340849694));
#83589=CARTESIAN_POINT('Ctrl Pts',(45.5841455116356,-1.71820416165022,3.53988266536269));
#83590=CARTESIAN_POINT('Ctrl Pts',(45.5902313004297,-1.82593839191682,3.48553890149408));
#83591=CARTESIAN_POINT('Ctrl Pts',(45.5963170892237,-1.9309987330142,3.42632936144463));
#83592=CARTESIAN_POINT('Ctrl Pts',(45.6021691195343,-2.0320236488207,3.36939409228447));
#83593=CARTESIAN_POINT('Ctrl Pts',(45.6080211498448,-2.13057590408607,3.30796016780319));
#83594=CARTESIAN_POINT('Ctrl Pts',(45.6138731801553,-2.2262362325335,3.24227716843502));
#83595=CARTESIAN_POINT('Ctrl Pts',(45.6197243207657,-2.32188201747935,3.17660415503305));
#83596=CARTESIAN_POINT('Ctrl Pts',(45.625575461376,-2.41463640914046,3.10668358511262));
#83597=CARTESIAN_POINT('Ctrl Pts',(45.6314266019864,-2.50410902253351,3.03280843497677));
#83598=CARTESIAN_POINT('Ctrl Pts',(45.637278269785,-2.59358969741732,2.95892662868305));
#83599=CARTESIAN_POINT('Ctrl Pts',(45.6431299375837,-2.67978768746533,2.88108979706325));
#83600=CARTESIAN_POINT('Ctrl Pts',(45.6489816053823,-2.76234616385116,2.79963080977774));
#83601=CARTESIAN_POINT('Ctrl Pts',(45.6548352172968,-2.84493206886839,2.71814475914715));
#83602=CARTESIAN_POINT('Ctrl Pts',(45.6606888292112,-2.9238757617867,2.63303445013365));
#83603=CARTESIAN_POINT('Ctrl Pts',(45.6665424411257,-2.99885821066938,2.54466862917372));
#83604=CARTESIAN_POINT('Ctrl Pts',(45.6724027074533,-3.07392589994712,2.45620235353938));
#83605=CARTESIAN_POINT('Ctrl Pts',(45.6782629737809,-3.14502308942954,2.36447349448886));
#83606=CARTESIAN_POINT('Ctrl Pts',(45.6841232401084,-3.2118718378919,2.26988288177098));
#83607=CARTESIAN_POINT('Ctrl Pts',(45.6899874535062,-3.2787656110491,2.17522855935663));
#83608=CARTESIAN_POINT('Ctrl Pts',(45.695851666904,-3.34140502260285,2.07770899221613));
#83609=CARTESIAN_POINT('Ctrl Pts',(45.7017158803018,-3.39955708522553,1.97775140609049));
#83610=CARTESIAN_POINT('Ctrl Pts',(45.7075887290991,-3.45779478018413,1.87764662653426));
#83611=CARTESIAN_POINT('Ctrl Pts',(45.7134615778964,-3.51153174705241,1.77509702757215));
#83612=CARTESIAN_POINT('Ctrl Pts',(45.7193344266936,-3.56058223926699,1.67055174041885));
#83613=CARTESIAN_POINT('Ctrl Pts',(45.7209291690954,-3.57390165246216,1.64216299620176));
#83614=CARTESIAN_POINT('Ctrl Pts',(45.7225239114972,-3.5868757819742,1.61362719182157));
#83615=CARTESIAN_POINT('Ctrl Pts',(45.724118653899,-3.59950154213154,1.5849535160984));
#83616=CARTESIAN_POINT('Ctrl Pts',(45.7305881397463,-3.65072121030955,1.46863131943987));
#83617=CARTESIAN_POINT('Ctrl Pts',(45.7370576255936,-3.69635132197521,1.34970412641326));
#83618=CARTESIAN_POINT('Ctrl Pts',(45.743527111441,-3.7361454474959,1.22870101943298));
#83619=CARTESIAN_POINT('Ctrl Pts',(45.7499705088804,-3.77577910193737,1.10818586133743));
#83620=CARTESIAN_POINT('Ctrl Pts',(45.7564139063199,-3.80962360872221,0.985611738784826));
#83621=CARTESIAN_POINT('Ctrl Pts',(45.7628573037594,-3.83748139162275,0.8615251412171));
#83622=CARTESIAN_POINT('Ctrl Pts',(45.7692834923951,-3.86526477291706,0.737769949856485));
#83623=CARTESIAN_POINT('Ctrl Pts',(45.7757096810308,-3.88709323586644,0.612510597555861));
#83624=CARTESIAN_POINT('Ctrl Pts',(45.7821358696666,-3.90281850505353,0.486309280820051));
#83625=CARTESIAN_POINT('Ctrl Pts',(45.7885361949728,-3.91848048512147,0.360615883540352));
#83626=CARTESIAN_POINT('Ctrl Pts',(45.794936520279,-3.92808819621711,0.233988347893363));
#83627=CARTESIAN_POINT('Ctrl Pts',(45.8013368455852,-3.93154427294153,0.106998270549759));
#83628=CARTESIAN_POINT('Ctrl Pts',(45.8031033762349,-3.932498172184,0.0719481983906104));
#83629=CARTESIAN_POINT('Ctrl Pts',(45.8048699068845,-3.93298373692229,0.0368705902930527));
#83630=CARTESIAN_POINT('Ctrl Pts',(45.8066364375341,-3.93299959826995,0.00177764125482606));
#83631=CARTESIAN_POINT('',(47.0566365067525,-3.9325046759356,-0.00340936713855836));
#83632=CARTESIAN_POINT('Ctrl Pts',(45.806636477965,-3.92726452529281,0.00177424710315623));
#83633=CARTESIAN_POINT('Ctrl Pts',(45.8454129428563,-3.92414560096597,-0.76741648345805));
#83634=CARTESIAN_POINT('Ctrl Pts',(45.9504718139941,-3.33362574617699,-2.85584174047811));
#83635=CARTESIAN_POINT('Ctrl Pts',(46.1218130913783,0.0625822105554463,
-4.65124432931964));
#83636=CARTESIAN_POINT('Ctrl Pts',(46.320660310118,3.94650710844973,-2.46233096823187));
#83637=CARTESIAN_POINT('Ctrl Pts',(46.5195075288577,4.20525141962489,1.98842986640301));
#83638=CARTESIAN_POINT('Ctrl Pts',(46.7183547475972,0.601137845897373,4.61265846243321));
#83639=CARTESIAN_POINT('Ctrl Pts',(46.897397730633,-3.14122023442404,3.16042933645599));
#83640=CARTESIAN_POINT('Ctrl Pts',(47.0101583074223,-3.92291374881594,0.916664918939353));
#83641=CARTESIAN_POINT('Ctrl Pts',(47.056636477965,-3.93047922134086,-0.00340704118923197));
#83642=CARTESIAN_POINT('',(48.3066364779243,-3.93299998520013,-0.000341197588748887));
#83643=CARTESIAN_POINT('Ctrl Pts',(47.0566365137715,-3.93299852178314,-0.00340993425095843));
#83644=CARTESIAN_POINT('Ctrl Pts',(47.063697492587,-3.93287725698335,-0.14327605577757));
#83645=CARTESIAN_POINT('Ctrl Pts',(47.0707584714024,-3.92529131289588,-0.282815375072087));
#83646=CARTESIAN_POINT('Ctrl Pts',(47.0778194502179,-3.9103676131021,-0.421324258027222));
#83647=CARTESIAN_POINT('Ctrl Pts',(47.0849765080332,-3.8952408459734,-0.561717836474329));
#83648=CARTESIAN_POINT('Ctrl Pts',(47.0921335658485,-3.87257533825972,-0.701052745607565));
#83649=CARTESIAN_POINT('Ctrl Pts',(47.0992906236638,-3.84255229214712,-0.838618436546029));
#83650=CARTESIAN_POINT('Ctrl Pts',(47.1048768108013,-3.81911887043196,-0.94599044794049));
#83651=CARTESIAN_POINT('Ctrl Pts',(47.1104629979389,-3.79120420303399,-1.05228509905202));
#83652=CARTESIAN_POINT('Ctrl Pts',(47.1160491850765,-3.75891448323585,-1.15717367223755));
#83653=CARTESIAN_POINT('Ctrl Pts',(47.1219216474124,-3.72497001294099,-1.26743746761962));
#83654=CARTESIAN_POINT('Ctrl Pts',(47.1277941097484,-3.6861128910397,-1.37639101302529));
#83655=CARTESIAN_POINT('Ctrl Pts',(47.1336665720844,-3.64246167079225,-1.48356394429405));
#83656=CARTESIAN_POINT('Ctrl Pts',(47.1395314270849,-3.59886699743339,-1.59059804105212));
#83657=CARTESIAN_POINT('Ctrl Pts',(47.1453962820855,-3.55049073048167,-1.69585573149472));
#83658=CARTESIAN_POINT('Ctrl Pts',(47.151261137086,-3.49750138385289,-1.79888106053377));
#83659=CARTESIAN_POINT('Ctrl Pts',(47.1571199630991,-3.44456650951828,-1.90180048100088));
#83660=CARTESIAN_POINT('Ctrl Pts',(47.1629787891122,-3.38702817588962,-2.00249173924161));
#83661=CARTESIAN_POINT('Ctrl Pts',(47.1688376151253,-3.32510298432286,-2.10051877964639));
#83662=CARTESIAN_POINT('Ctrl Pts',(47.1749233979874,-3.26077895955596,-2.20234315217217));
#83663=CARTESIAN_POINT('Ctrl Pts',(47.1810091808495,-3.19172150231696,-2.30129230103316));
#83664=CARTESIAN_POINT('Ctrl Pts',(47.1870949637116,-3.11822613909831,-2.39690524331773));
#83665=CARTESIAN_POINT('Ctrl Pts',(47.1929470091838,-3.04755352108066,-2.48884596789811));
#83666=CARTESIAN_POINT('Ctrl Pts',(47.1987990546561,-2.97277787900469,-2.57770166929477));
#83667=CARTESIAN_POINT('Ctrl Pts',(47.2046511001283,-2.89420567089331,-2.66309266353408));
#83668=CARTESIAN_POINT('Ctrl Pts',(47.2105022556919,-2.81564541109725,-2.74847067253917));
#83669=CARTESIAN_POINT('Ctrl Pts',(47.2163534112555,-2.73329001301056,-2.83038471788304));
#83670=CARTESIAN_POINT('Ctrl Pts',(47.2222045668191,-2.64748480158604,-2.90848985306308));
#83671=CARTESIAN_POINT('Ctrl Pts',(47.2280562493478,-2.56167186239736,-2.98660202252525));
#83672=CARTESIAN_POINT('Ctrl Pts',(47.2339079318765,-2.47240879793387,-3.06090432163304));
#83673=CARTESIAN_POINT('Ctrl Pts',(47.2397596144052,-2.38007567067358,-3.13109067289143));
#83674=CARTESIAN_POINT('Ctrl Pts',(47.2456132408115,-2.28771187115799,-3.20130033944032));
#83675=CARTESIAN_POINT('Ctrl Pts',(47.2514668672179,-2.19227630984071,-3.26739108937189));
#83676=CARTESIAN_POINT('Ctrl Pts',(47.2573204936242,-2.09417920993768,-3.32909934316547));
#83677=CARTESIAN_POINT('Ctrl Pts',(47.2631807740199,-1.99597060017408,-3.39087774254729));
#83678=CARTESIAN_POINT('Ctrl Pts',(47.2690410544157,-1.89509476322088,-3.44826348223305));
#83679=CARTESIAN_POINT('Ctrl Pts',(47.2749013348114,-1.79198786121663,-3.50103820391212));
#83680=CARTESIAN_POINT('Ctrl Pts',(47.2807655620484,-1.68881151772795,-3.55384846884721));
#83681=CARTESIAN_POINT('Ctrl Pts',(47.2866297892853,-1.58340149221702,-3.60204136069649));
#83682=CARTESIAN_POINT('Ctrl Pts',(47.2924940165223,-1.47621370860026,-3.64544676089786));
#83683=CARTESIAN_POINT('Ctrl Pts',(47.2983668787172,-1.36886809310394,-3.68891607468774));
#83684=CARTESIAN_POINT('Ctrl Pts',(47.3042397409121,-1.25973988321992,-3.72758368992329));
#83685=CARTESIAN_POINT('Ctrl Pts',(47.310112603107,-1.14929999544176,-3.7613293554909));
#83686=CARTESIAN_POINT('Ctrl Pts',(47.3117072033434,-1.1193133440762,-3.77049198258907));
#83687=CARTESIAN_POINT('Ctrl Pts',(47.3133018035798,-1.08923004604906,-3.77929203982554));
#83688=CARTESIAN_POINT('Ctrl Pts',(47.3148964038162,-1.05905963205316,-3.78772777476886));
#83689=CARTESIAN_POINT('Ctrl Pts',(47.3207689043242,-0.947949795571908,
-3.81879440614748));
#83690=CARTESIAN_POINT('Ctrl Pts',(47.3266414048322,-0.835285833085913,
-3.84501992627515));
#83691=CARTESIAN_POINT('Ctrl Pts',(47.3325139053402,-0.721527529778128,
-3.86624973634299));
#83692=CARTESIAN_POINT('Ctrl Pts',(47.3383787990124,-0.607916581201406,
-3.88745204676587));
#83693=CARTESIAN_POINT('Ctrl Pts',(47.3442436926846,-0.493214513363632,
-3.90367144072259));
#83694=CARTESIAN_POINT('Ctrl Pts',(47.3501085863568,-0.377896003926385,
-3.91480313811774));
#83695=CARTESIAN_POINT('Ctrl Pts',(47.35596745149,-0.262696030676819,-3.92592339321296));
#83696=CARTESIAN_POINT('Ctrl Pts',(47.3618263166231,-0.146881285142962,
-3.93196631434662));
#83697=CARTESIAN_POINT('Ctrl Pts',(47.3676851817563,-0.0309357060821324,
-3.93287833298835));
#83698=CARTESIAN_POINT('Ctrl Pts',(47.3737709501229,0.0895002352245635,
-3.93382567245998));
#83699=CARTESIAN_POINT('Ctrl Pts',(47.3798567184896,0.210076902211475,-3.92923656982957));
#83700=CARTESIAN_POINT('Ctrl Pts',(47.3859424868562,0.330246726315724,-3.91911037095892));
#83701=CARTESIAN_POINT('Ctrl Pts',(47.3917945723126,0.445802238383835,-3.90937300049571));
#83702=CARTESIAN_POINT('Ctrl Pts',(47.397646657769,0.560981125584535,-3.89451596011917));
#83703=CARTESIAN_POINT('Ctrl Pts',(47.4034987432254,0.675298284084939,-3.87459174978628));
#83704=CARTESIAN_POINT('Ctrl Pts',(47.4093499390223,0.789598063595361,-3.85467056841823));
#83705=CARTESIAN_POINT('Ctrl Pts',(47.4152011348193,0.903035967785185,-3.82968381972095));
#83706=CARTESIAN_POINT('Ctrl Pts',(47.4210523306163,1.01513509889997,-3.79973548171203));
#83707=CARTESIAN_POINT('Ctrl Pts',(47.4269040535837,1.12724432971841,-3.76978444547221));
#83708=CARTESIAN_POINT('Ctrl Pts',(47.4327557765511,1.23801414831716,-3.73487103798001));
#83709=CARTESIAN_POINT('Ctrl Pts',(47.4386074995184,1.3469815712235,-3.69514947556716));
#83710=CARTESIAN_POINT('Ctrl Pts',(47.444461166525,1.45598519490961,-3.65541471699444));
#83711=CARTESIAN_POINT('Ctrl Pts',(47.4503148335315,1.56318484410882,-3.61086876875883));
#83712=CARTESIAN_POINT('Ctrl Pts',(47.456168500538,1.66813697697349,-3.56171419769382));
#83713=CARTESIAN_POINT('Ctrl Pts',(47.4620288215649,1.77320841174416,-3.51250375130874));
#83714=CARTESIAN_POINT('Ctrl Pts',(47.4678891425918,1.87602685631187,-3.458674401153));
#83715=CARTESIAN_POINT('Ctrl Pts',(47.4737494636186,1.97617278397272,-3.40047498562855));
#83716=CARTESIAN_POINT('Ctrl Pts',(47.4796137315547,2.07638615962443,-3.34223637296711));
#83717=CARTESIAN_POINT('Ctrl Pts',(47.4854779994908,2.17392308734801,-3.27962205713108));
#83718=CARTESIAN_POINT('Ctrl Pts',(47.4913422674268,2.26839393475696,-3.21292358402092));
#83719=CARTESIAN_POINT('Ctrl Pts',(47.4972151701021,2.36300388412054,-3.14612690190518));
#83720=CARTESIAN_POINT('Ctrl Pts',(47.5030880727774,2.45453841736447,-3.07523431262208));
#83721=CARTESIAN_POINT('Ctrl Pts',(47.5089609754527,2.54264174438561,-3.00057693780841));
#83722=CARTESIAN_POINT('Ctrl Pts',(47.5105551911537,2.56655763658064,-2.9803109865898));
#83723=CARTESIAN_POINT('Ctrl Pts',(47.5121494068548,2.59022091086395,-2.95976782459626));
#83724=CARTESIAN_POINT('Ctrl Pts',(47.5137436225559,2.61362494454484,-2.93895451636343));
#83725=CARTESIAN_POINT('Ctrl Pts',(47.5196158969124,2.69983342105921,-2.8622889458707));
#83726=CARTESIAN_POINT('Ctrl Pts',(47.525488171269,2.78281016550265,-2.78169862677287));
#83727=CARTESIAN_POINT('Ctrl Pts',(47.5313604456256,2.86217652834462,-2.69748670443306));
#83728=CARTESIAN_POINT('Ctrl Pts',(47.5372251125981,2.94144007405476,-2.61338387652585));
#83729=CARTESIAN_POINT('Ctrl Pts',(47.5430897795706,3.01710225844809,-2.52566907353751));
#83730=CARTESIAN_POINT('Ctrl Pts',(47.5489544465431,3.08881828540358,-2.43468490769473));
#83731=CARTESIAN_POINT('Ctrl Pts',(47.5548130846949,3.16046058897979,-2.3437942726909));
#83732=CARTESIAN_POINT('Ctrl Pts',(47.5606717228466,3.22816454956605,-2.24964128248949));
#83733=CARTESIAN_POINT('Ctrl Pts',(47.5665303609984,3.29162344160212,-2.15260403202619));
#83734=CARTESIAN_POINT('Ctrl Pts',(47.5726162143441,3.35754345584558,-2.05180339199845));
#83735=CARTESIAN_POINT('Ctrl Pts',(47.5787020676899,3.41888215100117,-1.94789057282718));
#83736=CARTESIAN_POINT('Ctrl Pts',(47.5847879210356,3.47534286242914,-1.84132587788334));
#83737=CARTESIAN_POINT('Ctrl Pts',(47.5906397802171,3.52963272348791,-1.73885847469354));
#83738=CARTESIAN_POINT('Ctrl Pts',(47.5964916393985,3.57941256880411,-1.63393975254393));
#83739=CARTESIAN_POINT('Ctrl Pts',(47.60234349858,3.62446426942557,-1.52700614263904));
#83740=CARTESIAN_POINT('Ctrl Pts',(47.6081944687424,3.66950912575675,-1.42008877817344));
#83741=CARTESIAN_POINT('Ctrl Pts',(47.6140454389048,3.70982710515734,-1.31115751543514));
#83742=CARTESIAN_POINT('Ctrl Pts',(47.6198964090671,3.74524781942878,-1.20066971772589));
#83743=CARTESIAN_POINT('Ctrl Pts',(47.625747907276,3.78067173039812,-1.09017194856016));
#83744=CARTESIAN_POINT('Ctrl Pts',(47.6315994054849,3.81119737142664,-0.978117758842683));
#83745=CARTESIAN_POINT('Ctrl Pts',(47.6374509036937,3.83670413885191,-0.864979971396215));
#83746=CARTESIAN_POINT('Ctrl Pts',(47.6433043470545,3.8622193852233,-0.751804574746371));
#83747=CARTESIAN_POINT('Ctrl Pts',(47.6491577904153,3.88271234967359,-0.637545267163114));
#83748=CARTESIAN_POINT('Ctrl Pts',(47.6550112337761,3.89811361379941,-0.522684660107483));
#83749=CARTESIAN_POINT('Ctrl Pts',(47.6608713339294,3.91353239291821,-0.407693428532405));
#83750=CARTESIAN_POINT('Ctrl Pts',(47.6667314340827,3.92384785909345,-0.292099942553816));
#83751=CARTESIAN_POINT('Ctrl Pts',(47.672591534236,3.92904250328329,-0.176391630735043));
#83752=CARTESIAN_POINT('Ctrl Pts',(47.6784555826383,3.93424064737041,-0.0606053603129594));
#83753=CARTESIAN_POINT('Ctrl Pts',(47.6843196310405,3.93431109927501,0.0552954776255242));
#83754=CARTESIAN_POINT('Ctrl Pts',(47.6901836794428,3.92928844000814,0.17082551102922));
#83755=CARTESIAN_POINT('Ctrl Pts',(47.6960563662491,3.92425838179826,0.286525733189095));
#83756=CARTESIAN_POINT('Ctrl Pts',(47.7019290530553,3.91412027454157,0.401853650390887));
#83757=CARTESIAN_POINT('Ctrl Pts',(47.7078017398616,3.89896028938375,0.516330961504905));
#83758=CARTESIAN_POINT('Ctrl Pts',(47.7093981070062,3.89483936432548,0.547449225478263));
#83759=CARTESIAN_POINT('Ctrl Pts',(47.7109944741509,3.89034765612506,0.578504709157234));
#83760=CARTESIAN_POINT('Ctrl Pts',(47.7125908412955,3.88548753675185,0.60948798326632));
#83761=CARTESIAN_POINT('Ctrl Pts',(47.7184634438457,3.86760847332902,0.723467060796133));
#83762=CARTESIAN_POINT('Ctrl Pts',(47.7243360463959,3.8446799400168,0.836849554227666));
#83763=CARTESIAN_POINT('Ctrl Pts',(47.7302086489461,3.81675223316005,0.949152985913109));
#83764=CARTESIAN_POINT('Ctrl Pts',(47.7360736434181,3.78886070722584,1.06131092617733));
#83765=CARTESIAN_POINT('Ctrl Pts',(47.7419386378901,3.75598298611239,1.17239218729747));
#83766=CARTESIAN_POINT('Ctrl Pts',(47.747803632362,3.71822087056931,1.28192143193832));
#83767=CARTESIAN_POINT('Ctrl Pts',(47.7536625969548,3.68049757876209,1.3913380680984));
#83768=CARTESIAN_POINT('Ctrl Pts',(47.7595215615475,3.63790001490782,1.49920547319908));
#83769=CARTESIAN_POINT('Ctrl Pts',(47.7653805261403,3.59058041276574,1.60506115131575));
#83770=CARTESIAN_POINT('Ctrl Pts',(47.7714662567192,3.54142934773005,1.71501387881092));
#83771=CARTESIAN_POINT('Ctrl Pts',(47.7775519872982,3.48718344368452,1.82279556769424));
#83772=CARTESIAN_POINT('Ctrl Pts',(47.7836377178771,3.42806947800816,1.9279078437386));
#83773=CARTESIAN_POINT('Ctrl Pts',(47.7894898988744,3.37122410470161,2.02898626915768));
#83774=CARTESIAN_POINT('Ctrl Pts',(47.7953420798716,3.30987764434753,2.12759599818236));
#83775=CARTESIAN_POINT('Ctrl Pts',(47.8011942608689,3.24427930421203,2.22331752034241));
#83776=CARTESIAN_POINT('Ctrl Pts',(47.8070455506096,3.17869095436124,2.31902446461439));
#83777=CARTESIAN_POINT('Ctrl Pts',(47.8128968403502,3.10885224584378,2.41184373574585));
#83778=CARTESIAN_POINT('Ctrl Pts',(47.8187481300908,3.0350558082925,2.50138466465075));
#83779=CARTESIAN_POINT('Ctrl Pts',(47.8245999453131,2.96125274336959,2.59093363487894));
#83780=CARTESIAN_POINT('Ctrl Pts',(47.8304517605354,2.8834915057514,2.67720335862645));
#83781=CARTESIAN_POINT('Ctrl Pts',(47.8363035757576,2.80210464943293,2.75983668604256));
#83782=CARTESIAN_POINT('Ctrl Pts',(47.8421573332373,2.72069078026094,2.84249744002445));
#83783=CARTESIAN_POINT('Ctrl Pts',(47.8480110907171,2.63564918945304,2.92151910340916));
#83784=CARTESIAN_POINT('Ctrl Pts',(47.8538648481968,2.54734834294464,2.99658228982573));
#83785=CARTESIAN_POINT('Ctrl Pts',(47.8597252566187,2.45894717047799,3.07173076179056));
#83786=CARTESIAN_POINT('Ctrl Pts',(47.8655856650406,2.36727966612812,3.14291151194314));
#83787=CARTESIAN_POINT('Ctrl Pts',(47.8714460734626,2.27274641734158,3.20984621476809));
#83788=CARTESIAN_POINT('Ctrl Pts',(47.8773104271116,2.17814952876956,3.27682597803667));
#83789=CARTESIAN_POINT('Ctrl Pts',(47.8831747807606,2.0806834010134,3.33955377909172));
#83790=CARTESIAN_POINT('Ctrl Pts',(47.8890391344097,1.98077505993792,3.39779622136583));
#83791=CARTESIAN_POINT('Ctrl Pts',(47.8949121196797,1.88071966583925,3.45612438948748));
#83792=CARTESIAN_POINT('Ctrl Pts',(47.9007851049497,1.7782152487932,3.50995383127813));
#83793=CARTESIAN_POINT('Ctrl Pts',(47.9066580902197,1.67371078463081,3.55909837029135));
#83794=CARTESIAN_POINT('Ctrl Pts',(47.9082514134915,1.64535903724794,3.57243113618339));
#83795=CARTESIAN_POINT('Ctrl Pts',(47.9098447367633,1.61686017759492,3.58541936430235));
#83796=CARTESIAN_POINT('Ctrl Pts',(47.9114380600352,1.58822336681766,3.59805996852392));
#83797=CARTESIAN_POINT('Ctrl Pts',(47.9173108113641,1.48267236437856,3.64465134552468));
#83798=CARTESIAN_POINT('Ctrl Pts',(47.9231835626931,1.37489288537159,3.68667213053081));
#83799=CARTESIAN_POINT('Ctrl Pts',(47.9290563140221,1.26531802826798,3.72390376988182));
#83800=CARTESIAN_POINT('Ctrl Pts',(47.9349214607175,1.15588505979396,3.76108719793304));
#83801=CARTESIAN_POINT('Ctrl Pts',(47.9407866074129,1.04466172424185,3.79349368113952));
#83802=CARTESIAN_POINT('Ctrl Pts',(47.9466517541083,0.932102958880354,3.82095185445283));
#83803=CARTESIAN_POINT('Ctrl Pts',(47.9525108741465,0.819659851852007,3.84838181346806));
#83804=CARTESIAN_POINT('Ctrl Pts',(47.9583699941848,0.705884443535285,3.8708734787474));
#83805=CARTESIAN_POINT('Ctrl Pts',(47.964229114223,0.591248135025886,3.88830485466719));
#83806=CARTESIAN_POINT('Ctrl Pts',(47.970314787746,0.472179206088296,3.90641024629804));
#83807=CARTESIAN_POINT('Ctrl Pts',(47.976400461269,0.352181886539044,3.91905597209619));
#83808=CARTESIAN_POINT('Ctrl Pts',(47.982486134792,0.231798005776437,3.92616335428342));
#83809=CARTESIAN_POINT('Ctrl Pts',(47.9883384782184,0.116029749301907,3.93299823316174));
#83810=CARTESIAN_POINT('Ctrl Pts',(47.9941908216448,-9.55212978881598E-5,
3.93471161259046));
#83811=CARTESIAN_POINT('Ctrl Pts',(48.0000431650713,-0.116090136285115,
3.93128631369649));
#83812=CARTESIAN_POINT('Ctrl Pts',(48.0058946195261,-0.232067131677432,
3.92786153510579));
#83813=CARTESIAN_POINT('Ctrl Pts',(48.0117460739809,-0.34791309790432,3.91929964241296));
#83814=CARTESIAN_POINT('Ctrl Pts',(48.0175975284357,-0.463141150386326,
3.9056355788551));
#83815=CARTESIAN_POINT('Ctrl Pts',(48.0234495104708,-0.578379592089053,
3.8919702833145));
#83816=CARTESIAN_POINT('Ctrl Pts',(48.029301492506,-0.692999598839239,3.87320195109583));
#83817=CARTESIAN_POINT('Ctrl Pts',(48.0351534745411,-0.806520897288482,
3.84941723410661));
#83818=CARTESIAN_POINT('Ctrl Pts',(48.0410074007474,-0.920079910283162,
3.82562461525403));
#83819=CARTESIAN_POINT('Ctrl Pts',(48.0468613269538,-1.03253908484983,3.7968123824681));
#83820=CARTESIAN_POINT('Ctrl Pts',(48.0527152531602,-1.14343049832214,3.76311781578876));
#83821=CARTESIAN_POINT('Ctrl Pts',(48.058575832263,-1.25444793816839,3.72938495575625));
#83822=CARTESIAN_POINT('Ctrl Pts',(48.0644364113658,-1.36389366494346,3.69075880703968));
#83823=CARTESIAN_POINT('Ctrl Pts',(48.0702969904686,-1.47131692950533,3.6474258721667));
#83824=CARTESIAN_POINT('Ctrl Pts',(48.0761615161443,-1.57881253397215,3.60406375646029));
#83825=CARTESIAN_POINT('Ctrl Pts',(48.0820260418199,-1.68428258914526,3.55598871427612));
#83826=CARTESIAN_POINT('Ctrl Pts',(48.0878905674956,-1.78729984590362,3.50343378142543));
#83827=CARTESIAN_POINT('Ctrl Pts',(48.0937637254089,-1.89046873802004,3.45080149079692));
#83828=CARTESIAN_POINT('Ctrl Pts',(48.0996368833223,-1.99117726797664,3.39367635205968));
#83829=CARTESIAN_POINT('Ctrl Pts',(48.1055100412357,-2.0890260407125,3.33233539746902));
#83830=CARTESIAN_POINT('Ctrl Pts',(48.107101787082,-2.11554505822753,3.31571074491902));
#83831=CARTESIAN_POINT('Ctrl Pts',(48.1086935329284,-2.14185420489738,3.29877666346379));
#83832=CARTESIAN_POINT('Ctrl Pts',(48.1102852787747,-2.16794595377746,3.2815391726292));
#83833=CARTESIAN_POINT('Ctrl Pts',(48.1161436697141,-2.26397614954072,3.21809690868127));
#83834=CARTESIAN_POINT('Ctrl Pts',(48.1220020606534,-2.35738380061524,3.15032696055728));
#83835=CARTESIAN_POINT('Ctrl Pts',(48.1278604515928,-2.44775204026117,3.07847347713072));
#83836=CARTESIAN_POINT('Ctrl Pts',(48.1337112415304,-2.53800303113575,3.00671322040284));
#83837=CARTESIAN_POINT('Ctrl Pts',(48.1395620314681,-2.62522212975228,2.93088021971269));
#83838=CARTESIAN_POINT('Ctrl Pts',(48.1454128214058,-2.70902024659567,2.85126258060087));
#83839=CARTESIAN_POINT('Ctrl Pts',(48.1512576052132,-2.79273234045464,2.77172667300267));
#83840=CARTESIAN_POINT('Ctrl Pts',(48.1571023890205,-2.8730301375782,2.68841413843918));
#83841=CARTESIAN_POINT('Ctrl Pts',(48.1629471728279,-2.94955709858846,2.60165368989926));
#83842=CARTESIAN_POINT('Ctrl Pts',(48.1689342272069,-3.02794683756462,2.51278136536532));
#83843=CARTESIAN_POINT('Ctrl Pts',(48.1749212815859,-3.10237944058315,2.42029137357435));
#83844=CARTESIAN_POINT('Ctrl Pts',(48.1809083359649,-3.17251110960001,2.3245778669394));
#83845=CARTESIAN_POINT('Ctrl Pts',(48.1867464677607,-3.24089831654017,2.23124514754212));
#83846=CARTESIAN_POINT('Ctrl Pts',(48.1925845995565,-3.30519578873378,2.13484775451402));
#83847=CARTESIAN_POINT('Ctrl Pts',(48.1984227313523,-3.365125676473,2.03578441430868));
#83848=CARTESIAN_POINT('Ctrl Pts',(48.2042600189846,-3.42504689866194,1.93673539814745));
#83849=CARTESIAN_POINT('Ctrl Pts',(48.2100973066169,-3.48060157694486,1.83502155671701));
#83850=CARTESIAN_POINT('Ctrl Pts',(48.2159345942492,-3.53155608365004,1.7310692152639));
#83851=CARTESIAN_POINT('Ctrl Pts',(48.2217724692948,-3.58251571796839,1.62710641296191));
#83852=CARTESIAN_POINT('Ctrl Pts',(48.2276103443403,-3.62887407771079,1.52090503610112));
#83853=CARTESIAN_POINT('Ctrl Pts',(48.2334482193859,-3.67044458102268,1.41291386065862));
#83854=CARTESIAN_POINT('Ctrl Pts',(48.2395472409308,-3.71387466360447,1.30009190052059));
#83855=CARTESIAN_POINT('Ctrl Pts',(48.2456462624756,-3.75207840010692,1.18531675855074));
#83856=CARTESIAN_POINT('Ctrl Pts',(48.2517452840205,-3.78490063685083,1.06911934280799));
#83857=CARTESIAN_POINT('Ctrl Pts',(48.2575919867618,-3.81636500537843,0.957729057636036));
#83858=CARTESIAN_POINT('Ctrl Pts',(48.2634386895031,-3.84288423206317,0.845032258677021));
#83859=CARTESIAN_POINT('Ctrl Pts',(48.2692853922444,-3.86437396766523,0.731507237169474));
#83860=CARTESIAN_POINT('Ctrl Pts',(48.2751361942627,-3.88587877028598,0.617902620284232));
#83861=CARTESIAN_POINT('Ctrl Pts',(48.280986996281,-3.90234700273276,0.503469034870847));
#83862=CARTESIAN_POINT('Ctrl Pts',(48.2868377982993,-3.91374618334939,0.388689866497759));
#83863=CARTESIAN_POINT('Ctrl Pts',(48.2926969889661,-3.92516170766029,0.273746132293219));
#83864=CARTESIAN_POINT('Ctrl Pts',(48.2985561796329,-3.93149365780932,0.158456239440373));
#83865=CARTESIAN_POINT('Ctrl Pts',(48.3044153702997,-3.93276160057252,0.0433034994225827));
#83866=CARTESIAN_POINT('Ctrl Pts',(48.3051557395079,-3.93292181822595,0.0287527623332245));
#83867=CARTESIAN_POINT('Ctrl Pts',(48.3058961087161,-3.93300124705041,0.0142042075055692));
#83868=CARTESIAN_POINT('Ctrl Pts',(48.3066364779243,-3.93299998520013,-0.000341197588803423));
#83869=CARTESIAN_POINT('',(49.2909686583561,-0.918523134026603,3.82423904224853));
#83870=CARTESIAN_POINT('Ctrl Pts',(48.306636477965,-3.93299998520006,-0.000341198387843754));
#83871=CARTESIAN_POINT('Ctrl Pts',(48.3074684844815,-3.93299856716416,-0.0166869238569671));
#83872=CARTESIAN_POINT('Ctrl Pts',(48.308300490998,-3.93289524936037,-0.033032172584711));
#83873=CARTESIAN_POINT('Ctrl Pts',(48.3091324975144,-3.93269004605578,-0.0493761243297054));
#83874=CARTESIAN_POINT('Ctrl Pts',(48.315006317975,-3.93124134662219,-0.164761564550813));
#83875=CARTESIAN_POINT('Ctrl Pts',(48.3208801384356,-3.92470779553677,-0.280276028324374));
#83876=CARTESIAN_POINT('Ctrl Pts',(48.3267539588961,-3.91307046304444,-0.395434635874443));
#83877=CARTESIAN_POINT('Ctrl Pts',(48.3326201670137,-3.90144821228079,-0.510444000384883));
#83878=CARTESIAN_POINT('Ctrl Pts',(48.3384863751313,-3.88473537506585,-0.625098018529042));
#83879=CARTESIAN_POINT('Ctrl Pts',(48.3443525832488,-3.86296501795712,-0.738911544123905));
#83880=CARTESIAN_POINT('Ctrl Pts',(48.3502127558905,-3.84121705938312,-0.852607972135366));
#83881=CARTESIAN_POINT('Ctrl Pts',(48.3560729285321,-3.81442200812411,-0.965465224274634));
#83882=CARTESIAN_POINT('Ctrl Pts',(48.3619331011737,-3.78266467860207,-1.07700368117117));
#83883=CARTESIAN_POINT('Ctrl Pts',(48.3680183768021,-3.74968747550933,-1.1928265920106));
#83884=CARTESIAN_POINT('Ctrl Pts',(48.3741036524304,-3.71135916735355,-1.30722690779745));
#83885=CARTESIAN_POINT('Ctrl Pts',(48.3801889280588,-3.66783310645094,-1.4196792959054));
#83886=CARTESIAN_POINT('Ctrl Pts',(48.3860422958279,-3.62596580946009,-1.52784616036806));
#83887=CARTESIAN_POINT('Ctrl Pts',(48.391895663597,-3.57928984325164,-1.63421042976855));
#83888=CARTESIAN_POINT('Ctrl Pts',(48.3977490313661,-3.52799211720192,-1.73832120764866));
#83889=CARTESIAN_POINT('Ctrl Pts',(48.4036014980707,-3.47670228789798,-1.84241595876874));
#83890=CARTESIAN_POINT('Ctrl Pts',(48.4094539647754,-3.42079229597198,-1.9442575376294));
#83891=CARTESIAN_POINT('Ctrl Pts',(48.41530643148,-3.3604961422573,-2.04341740177425));
#83892=CARTESIAN_POINT('Ctrl Pts',(48.4211594126556,-3.30019468810806,-2.14258598273332));
#83893=CARTESIAN_POINT('Ctrl Pts',(48.4270123938311,-3.23550652036474,-2.23907202731734));
#83894=CARTESIAN_POINT('Ctrl Pts',(48.4328653750067,-3.16670993754481,-2.33247447391283));
#83895=CARTESIAN_POINT('Ctrl Pts',(48.4387202862167,-3.0978906688882,-2.42590772018707));
#83896=CARTESIAN_POINT('Ctrl Pts',(48.4445751974267,-3.02496053617689,-2.51625501408668));
#83897=CARTESIAN_POINT('Ctrl Pts',(48.4504301086367,-2.94823877130806,-2.60314754621322));
#83898=CARTESIAN_POINT('Ctrl Pts',(48.4562916469597,-2.87143016587333,-2.6901384310911));
#83899=CARTESIAN_POINT('Ctrl Pts',(48.4621531852827,-2.79082163576131,-2.77366643923067));
#83900=CARTESIAN_POINT('Ctrl Pts',(48.4680147236056,-2.70677006513171,-2.85339881799002));
#83901=CARTESIAN_POINT('Ctrl Pts',(48.4738801946845,-2.62266210072131,-2.93318469260029));
#83902=CARTESIAN_POINT('Ctrl Pts',(48.4797456657633,-2.53510680715101,-3.0091695967008));
#83903=CARTESIAN_POINT('Ctrl Pts',(48.4856111368422,-2.44449365213772,-3.08106147044462));
#83904=CARTESIAN_POINT('Ctrl Pts',(48.4914852126711,-2.35374756601887,-3.15305881084233));
#83905=CARTESIAN_POINT('Ctrl Pts',(48.4973592885,-2.25993499882691,-3.22095089561564));
#83906=CARTESIAN_POINT('Ctrl Pts',(48.503233364329,-2.16347388609934,-3.28448926686726));
#83907=CARTESIAN_POINT('Ctrl Pts',(48.5048154816374,-2.13749315304893,-3.30160262390066));
#83908=CARTESIAN_POINT('Ctrl Pts',(48.5063975989457,-2.111320418004,-3.31840040821361));
#83909=CARTESIAN_POINT('Ctrl Pts',(48.5079797162541,-2.08496412466013,-3.33487834843795));
#83910=CARTESIAN_POINT('Ctrl Pts',(48.5138537288573,-1.987109687154,-3.39605688939871));
#83911=CARTESIAN_POINT('Ctrl Pts',(48.5197277414606,-1.88639724144626,-3.45302671887418));
#83912=CARTESIAN_POINT('Ctrl Pts',(48.5256017540639,-1.7832245806399,-3.50550981955573));
#83913=CARTESIAN_POINT('Ctrl Pts',(48.5314681776143,-1.68018521590145,-3.55792511360229));
#83914=CARTESIAN_POINT('Ctrl Pts',(48.5373346011647,-1.57469232194212,-3.60586502106239));
#83915=CARTESIAN_POINT('Ctrl Pts',(48.5432010247151,-1.46717201477847,-3.64909513154301));
#83916=CARTESIAN_POINT('Ctrl Pts',(48.5490614355031,-1.35976191003179,-3.69228093353171));
#83917=CARTESIAN_POINT('Ctrl Pts',(48.5549218462911,-1.25032890636376,-3.73076638722925));
#83918=CARTESIAN_POINT('Ctrl Pts',(48.5607822570791,-1.13932243459314,-3.76436361023118));
#83919=CARTESIAN_POINT('Ctrl Pts',(48.5668674519923,-1.02405815675097,-3.79924950098197));
#83920=CARTESIAN_POINT('Ctrl Pts',(48.5729526469054,-0.907097692538037,
-3.82886445470895));
#83921=CARTESIAN_POINT('Ctrl Pts',(48.5790378418185,-0.788965889178756,
-3.85305357161205));
#83922=CARTESIAN_POINT('Ctrl Pts',(48.5848915022426,-0.675328861601405,
-3.87632232114794));
#83923=CARTESIAN_POINT('Ctrl Pts',(48.5907451626667,-0.56060844454005,-3.89457049495094));
#83924=CARTESIAN_POINT('Ctrl Pts',(48.5965988230908,-0.445285078524572,
-3.90771163199683));
#83925=CARTESIAN_POINT('Ctrl Pts',(48.6024516019306,-0.329979080662889,
-3.92085078993566));
#83926=CARTESIAN_POINT('Ctrl Pts',(48.6083043807704,-0.214070724731052,
-3.92888439368455));
#83927=CARTESIAN_POINT('Ctrl Pts',(48.6141571596102,-0.0980470935696117,
-3.93177768540422));
#83928=CARTESIAN_POINT('Ctrl Pts',(48.6200104719687,0.0179871138977239,
-3.93467124086618));
#83929=CARTESIAN_POINT('Ctrl Pts',(48.6258637843272,0.134136204493536,-3.93242354250173));
#83930=CARTESIAN_POINT('Ctrl Pts',(48.6317170966857,0.249912275789835,-3.92505195563187));
#83931=CARTESIAN_POINT('Ctrl Pts',(48.637572357708,0.36572689084317,-3.91767791463958));
#83932=CARTESIAN_POINT('Ctrl Pts',(48.6434276187304,0.481167827619029,-3.90517661938991));
#83933=CARTESIAN_POINT('Ctrl Pts',(48.6492828797528,0.595752196064166,-3.8876173063825));
#83934=CARTESIAN_POINT('Ctrl Pts',(48.6551447934754,0.710466754340802,-3.87003804262584));
#83935=CARTESIAN_POINT('Ctrl Pts',(48.6610067071979,0.824322393184345,-3.84738935310329));
#83936=CARTESIAN_POINT('Ctrl Pts',(48.6668686209204,0.936846206648068,-3.81979164158061));
#83937=CARTESIAN_POINT('Ctrl Pts',(48.6727344827349,1.04944580668567,-3.79217534256131));
#83938=CARTESIAN_POINT('Ctrl Pts',(48.6786003445494,1.16071139970324,-3.75960350004611));
#83939=CARTESIAN_POINT('Ctrl Pts',(48.6844662063638,1.27018670565374,-3.72224592588675));
#83940=CARTESIAN_POINT('Ctrl Pts',(48.6903406921989,1.37982296277079,-3.68483342842675));
#83941=CARTESIAN_POINT('Ctrl Pts',(48.6962151780341,1.48766329643573,-3.64262130679637));
#83942=CARTESIAN_POINT('Ctrl Pts',(48.7020896638692,1.59327272284702,-3.59582689108244));
#83943=CARTESIAN_POINT('Ctrl Pts',(48.7036687542441,1.62166105051042,-3.5832483244597));
#83944=CARTESIAN_POINT('Ctrl Pts',(48.7052478446189,1.64988832874966,-3.57033891094029));
#83945=CARTESIAN_POINT('Ctrl Pts',(48.7068269349938,1.6779464473734,-3.55710341707223));
#83946=CARTESIAN_POINT('Ctrl Pts',(48.7126911328813,1.78214463804094,-3.50795135053006));
#83947=CARTESIAN_POINT('Ctrl Pts',(48.7185553307689,1.8843586773044,-3.45413329509077));
#83948=CARTESIAN_POINT('Ctrl Pts',(48.7244195286564,1.98414050183357,-3.39583207314255));
#83949=CARTESIAN_POINT('Ctrl Pts',(48.7302761014818,2.08379258268181,-3.33760665873918));
#83950=CARTESIAN_POINT('Ctrl Pts',(48.7361326743071,2.18101838292689,-3.27490987674335));
#83951=CARTESIAN_POINT('Ctrl Pts',(48.7419892471324,2.27539109351899,-3.20797200292248));
#83952=CARTESIAN_POINT('Ctrl Pts',(48.7478397827625,2.3696665208539,-3.14110313140485));
#83953=CARTESIAN_POINT('Ctrl Pts',(48.7536903183926,2.46109437200237,-3.07000210183485));
#83954=CARTESIAN_POINT('Ctrl Pts',(48.7595408540227,2.54927428133677,-2.99494401258436));
#83955=CARTESIAN_POINT('Ctrl Pts',(48.7656297415106,2.64104665579661,-2.91682804348288));
#83956=CARTESIAN_POINT('Ctrl Pts',(48.7717186289986,2.7293004301247,-2.83442597610796));
#83957=CARTESIAN_POINT('Ctrl Pts',(48.7778075164865,2.81361940131041,-2.7480965893814));
#83958=CARTESIAN_POINT('Ctrl Pts',(48.7836513016526,2.89454419323814,-2.66524230926087));
#83959=CARTESIAN_POINT('Ctrl Pts',(48.7894950868186,2.97184451333193,-2.57877109368838));
#83960=CARTESIAN_POINT('Ctrl Pts',(48.7953388719847,3.04518851884893,-2.48903914888269));
#83961=CARTESIAN_POINT('Ctrl Pts',(48.8011817918658,3.11852166437307,-2.39932049061995));
#83962=CARTESIAN_POINT('Ctrl Pts',(48.8070247117469,3.18789939764433,-2.30634238397281));
#83963=CARTESIAN_POINT('Ctrl Pts',(48.812867631628,3.25302975996991,-2.21049460093213));
#83964=CARTESIAN_POINT('Ctrl Pts',(48.8187111115083,3.31816636454202,-2.11463763161534));
#83965=CARTESIAN_POINT('Ctrl Pts',(48.8245545913885,3.37905455588627,-2.01591078213367));
#83966=CARTESIAN_POINT('Ctrl Pts',(48.8303980712687,3.43544577510909,-1.91473270361298));
#83967=CARTESIAN_POINT('Ctrl Pts',(48.8362435365058,3.49185615358228,-1.81352024924149));
#83968=CARTESIAN_POINT('Ctrl Pts',(48.8420890017429,3.54376632027041,-1.70985527188832));
#83969=CARTESIAN_POINT('Ctrl Pts',(48.84793446698,3.5909740674939,-1.6041802413028));
#83970=CARTESIAN_POINT('Ctrl Pts',(48.8537866884761,3.63823637799919,-1.49838307024645));
#83971=CARTESIAN_POINT('Ctrl Pts',(48.8596389099722,3.68078525174441,-1.39057158772529));
#83972=CARTESIAN_POINT('Ctrl Pts',(48.8654911314683,3.71846693036184,-1.2812075116098));
#83973=CARTESIAN_POINT('Ctrl Pts',(48.8713473490879,3.75617433948887,-1.1717687574674));
#83974=CARTESIAN_POINT('Ctrl Pts',(48.8772035667075,3.78900781907255,-1.06077569549521));
#83975=CARTESIAN_POINT('Ctrl Pts',(48.8830597843271,3.81686417808038,-0.948702717444605));
#83976=CARTESIAN_POINT('Ctrl Pts',(48.8889247714818,3.8447622512685,-0.836461912995315));
#83977=CARTESIAN_POINT('Ctrl Pts',(48.8947897586364,3.86766824756651,-0.723138369865339));
#83978=CARTESIAN_POINT('Ctrl Pts',(48.9006547457911,3.88553047299015,-0.609214201627749));
#83979=CARTESIAN_POINT('Ctrl Pts',(48.9023278817718,3.89062612473906,-0.576714450149148));
#83980=CARTESIAN_POINT('Ctrl Pts',(48.9040010177526,3.89531162915813,-0.544165831869741));
#83981=CARTESIAN_POINT('Ctrl Pts',(48.9056741537333,3.89958656322034,-0.511579549973744));
#83982=CARTESIAN_POINT('Ctrl Pts',(48.9115580129171,3.91462007533889,-0.396984504377214));
#83983=CARTESIAN_POINT('Ctrl Pts',(48.9174418721009,3.92462275728447,-0.281537550039955));
#83984=CARTESIAN_POINT('Ctrl Pts',(48.9233257312847,3.92950719094621,-0.165717338567898));
#83985=CARTESIAN_POINT('Ctrl Pts',(48.9292019545742,3.93438528573783,-0.0500474350596651));
#83986=CARTESIAN_POINT('Ctrl Pts',(48.9350781778637,3.93415832535556,0.0659943546379723));
#83987=CARTESIAN_POINT('Ctrl Pts',(48.9409544011532,3.92879033102886,0.181921782132266));
#83988=CARTESIAN_POINT('Ctrl Pts',(48.9468245539282,3.9234278821837,0.297729449177621));
#83989=CARTESIAN_POINT('Ctrl Pts',(48.9526947067031,3.91293498308656,0.413422580262193));
#83990=CARTESIAN_POINT('Ctrl Pts',(48.958564859478,3.89732766435233,0.528513080892061));
#83991=CARTESIAN_POINT('Ctrl Pts',(48.9646463808528,3.88115836755125,0.64774768456467));
#83992=CARTESIAN_POINT('Ctrl Pts',(48.9707279022276,3.85949937841456,0.766334992409335));
#83993=CARTESIAN_POINT('Ctrl Pts',(48.9768094236024,3.83242749655273,0.883735528122851));
#83994=CARTESIAN_POINT('Ctrl Pts',(48.9826726220244,3.80632747893706,0.996921455346187));
#83995=CARTESIAN_POINT('Ctrl Pts',(48.9885358204463,3.77519662446219,1.10900391808571));
#83996=CARTESIAN_POINT('Ctrl Pts',(48.9943990188683,3.73915597887939,1.2195087394564));
#83997=CARTESIAN_POINT('Ctrl Pts',(49.000261244185,3.70312131490247,1.32999522052602));
#83998=CARTESIAN_POINT('Ctrl Pts',(49.0061234695017,3.66217860787634,1.43890418969773));
#83999=CARTESIAN_POINT('Ctrl Pts',(49.0119856948184,3.61649870358219,1.54577686843487));
#84000=CARTESIAN_POINT('Ctrl Pts',(49.0178483522195,3.57081543237963,1.65265742438907));
#84001=CARTESIAN_POINT('Ctrl Pts',(49.0237110096207,3.52039443167278,1.7575010130483));
#84002=CARTESIAN_POINT('Ctrl Pts',(49.0295736670218,3.46545432315126,1.85986970891841));
#84003=CARTESIAN_POINT('Ctrl Pts',(49.0354381616566,3.4104969975541,1.96227048498689));
#84004=CARTESIAN_POINT('Ctrl Pts',(49.0413026562914,3.35101794255593,2.06219446346489));
#84005=CARTESIAN_POINT('Ctrl Pts',(49.0471671509262,3.2872809204378,2.15922975853095));
#84006=CARTESIAN_POINT('Ctrl Pts',(49.0530380873566,3.22347388702324,2.25637164104934));
#84007=CARTESIAN_POINT('Ctrl Pts',(49.0589090237871,3.15539977696748,2.35061816239508));
#84008=CARTESIAN_POINT('Ctrl Pts',(49.0647799602175,3.08336479279709,2.44158771182593));
#84009=CARTESIAN_POINT('Ctrl Pts',(49.0706547326819,3.01128274140875,2.53261670020381));
#84010=CARTESIAN_POINT('Ctrl Pts',(49.0765295051462,2.93523493088686,2.62036414215503));
#84011=CARTESIAN_POINT('Ctrl Pts',(49.0824042776106,2.85556568354273,2.70448398534233));
#84012=CARTESIAN_POINT('Ctrl Pts',(49.0882874421249,2.77578262952704,2.78872399282997));
#84013=CARTESIAN_POINT('Ctrl Pts',(49.0941706066392,2.69236810858523,2.86932577381937));
#84014=CARTESIAN_POINT('Ctrl Pts',(49.1000537711535,2.60570090784886,2.94598231135823));
#84015=CARTESIAN_POINT('Ctrl Pts',(49.1015429715933,2.5837629128906,2.96538631563848));
#84016=CARTESIAN_POINT('Ctrl Pts',(49.1030321720331,2.56161665519144,2.98453774370936));
#84017=CARTESIAN_POINT('Ctrl Pts',(49.104521372473,2.53926857338398,3.00343205553655));
#84018=CARTESIAN_POINT('Ctrl Pts',(49.1103447293239,2.45187882260223,3.07731621329097));
#84019=CARTESIAN_POINT('Ctrl Pts',(49.1161680861748,2.3611056470291,3.14751483806536));
#84020=CARTESIAN_POINT('Ctrl Pts',(49.1219914430257,2.2672959664739,3.21369849245557));
#84021=CARTESIAN_POINT('Ctrl Pts',(49.1278073538278,2.17360623588712,3.27979752096061));
#84022=CARTESIAN_POINT('Ctrl Pts',(49.1336232646298,2.07688805952106,3.34189154446061));
#84023=CARTESIAN_POINT('Ctrl Pts',(49.1394391754318,1.97752286652601,3.39969003180684));
#84024=CARTESIAN_POINT('Ctrl Pts',(49.1452492704114,1.87825703721406,3.45743072154399));
#84025=CARTESIAN_POINT('Ctrl Pts',(49.151059365391,1.77634981625796,3.51088420597852));
#84026=CARTESIAN_POINT('Ctrl Pts',(49.1568694603706,1.67221253818103,3.55980255451762));
#84027=CARTESIAN_POINT('Ctrl Pts',(49.1626755149881,1.56814767756246,3.60868688505151));
#84028=CARTESIAN_POINT('Ctrl Pts',(49.1684815696055,1.46185622341962,3.65304217281303));
#84029=CARTESIAN_POINT('Ctrl Pts',(49.174287624223,1.35377444905346,3.69266621035398));
#84030=CARTESIAN_POINT('Ctrl Pts',(49.1800915949038,1.24573146791119,3.73227602584714));
#84031=CARTESIAN_POINT('Ctrl Pts',(49.1858955655846,1.13589983829548,3.76715782131109));
#84032=CARTESIAN_POINT('Ctrl Pts',(49.1916995362654,1.02473552523914,3.79715763477273));
#84033=CARTESIAN_POINT('Ctrl Pts',(49.1975028869562,0.913583086942417,3.82715424360365));
#84034=CARTESIAN_POINT('Ctrl Pts',(49.2033062376471,0.801098654615878,3.852269797829));
#84035=CARTESIAN_POINT('Ctrl Pts',(49.2091095883379,0.687752267144868,3.87240052409834));
#84036=CARTESIAN_POINT('Ctrl Pts',(49.2149137821895,0.574389411733869,3.89253417513308));
#84037=CARTESIAN_POINT('Ctrl Pts',(49.2207179760412,0.460164766805947,3.90768148593855));
#84038=CARTESIAN_POINT('Ctrl Pts',(49.2265221698928,0.345556637970963,3.91779014368486));
#84039=CARTESIAN_POINT('Ctrl Pts',(49.232332094217,0.230835356689904,3.92790878169488));
#84040=CARTESIAN_POINT('Ctrl Pts',(49.2381420185411,0.115730255415686,3.93297879649116));
#84041=CARTESIAN_POINT('Ctrl Pts',(49.2439519428653,0.000722841650785665,
3.93299993357487));
#84042=CARTESIAN_POINT('Ctrl Pts',(49.2497649212577,-0.114345027376021,
3.93302108176958));
#84043=CARTESIAN_POINT('Ctrl Pts',(49.2555778996502,-0.229314686452266,
3.92798808630921));
#84044=CARTESIAN_POINT('Ctrl Pts',(49.2613908780426,-0.343708406002381,
3.91795272197653));
#84045=CARTESIAN_POINT('Ctrl Pts',(49.2672127549553,-0.458277239711371,
3.90790199548594));
#84046=CARTESIAN_POINT('Ctrl Pts',(49.2730346318679,-0.572267956320908,
3.89283366289546));
#84047=CARTESIAN_POINT('Ctrl Pts',(49.2788565087805,-0.68521144197363,3.87285092403367));
#84048=CARTESIAN_POINT('Ctrl Pts',(49.2828938919724,-0.763536033415078,
3.85899319821454));
#84049=CARTESIAN_POINT('Ctrl Pts',(49.2869312751642,-0.841357213550516,
3.84277310414495));
#84050=CARTESIAN_POINT('Ctrl Pts',(49.2909686583561,-0.918523134026603,
3.82423904224853));
#84051=CARTESIAN_POINT('',(49.291,2.49116634986212,3.04344857313454));
#84052=CARTESIAN_POINT('Origin',(49.291,0.,0.));
#84053=CARTESIAN_POINT('',(48.4899635220349,-3.93640077382959,-0.000934446622206373));
#84054=CARTESIAN_POINT('Ctrl Pts',(49.291,2.49116634986212,3.04344857313454));
#84055=CARTESIAN_POINT('Ctrl Pts',(49.2247175937535,3.50515732392066,2.213462413376));
#84056=CARTESIAN_POINT('Ctrl Pts',(49.0921527812602,4.62042791627047,-0.525508407013305));
#84057=CARTESIAN_POINT('Ctrl Pts',(48.8933055625208,2.05138932172835,-4.17834256249585));
#84058=CARTESIAN_POINT('Ctrl Pts',(48.694458343781,-2.40332474549236,-3.98116326218143));
#84059=CARTESIAN_POINT('Ctrl Pts',(48.5600109969525,-3.92216493045881,-1.37922589845858));
#84060=CARTESIAN_POINT('Ctrl Pts',(48.4918460563704,-3.93942359247251,-0.0379796677341524));
#84061=CARTESIAN_POINT('Ctrl Pts',(48.4899635220349,-3.93933315937227,-0.000935142729620586));
#84062=CARTESIAN_POINT('',(47.2399635542899,-3.93231350106613,-0.00327549983485499));
#84063=CARTESIAN_POINT('Ctrl Pts',(48.4899635220349,-3.93299988918353,-0.000933639299641673));
#84064=CARTESIAN_POINT('Ctrl Pts',(48.4841266678079,-3.93302711093771,0.113739292968427));
#84065=CARTESIAN_POINT('Ctrl Pts',(48.478289813581,-3.92803487061338,0.228617479894471));
#84066=CARTESIAN_POINT('Ctrl Pts',(48.472452959354,-3.91799539673541,0.34322160648788));
#84067=CARTESIAN_POINT('Ctrl Pts',(48.4666237055437,-3.90796899568411,0.457676502165316));
#84068=CARTESIAN_POINT('Ctrl Pts',(48.4607944517333,-3.89290846354109,0.571857633777924));
#84069=CARTESIAN_POINT('Ctrl Pts',(48.4549651979229,-3.87283801159206,0.685284419761366));
#84070=CARTESIAN_POINT('Ctrl Pts',(48.4491419268033,-3.85278815838713,0.798594793351819));
#84071=CARTESIAN_POINT('Ctrl Pts',(48.4433186556837,-3.82773868257875,0.911151950930715));
#84072=CARTESIAN_POINT('Ctrl Pts',(48.4374953845641,-3.79776563490822,1.02247991780288));
#84073=CARTESIAN_POINT('Ctrl Pts',(48.4316315729698,-3.76758392074174,1.13458292820758));
#84074=CARTESIAN_POINT('Ctrl Pts',(48.4257677613755,-3.73240984801752,1.24543913760885));
#84075=CARTESIAN_POINT('Ctrl Pts',(48.4199039497813,-3.69237365308898,1.3545721855901));
#84076=CARTESIAN_POINT('Ctrl Pts',(48.4140871743393,-3.65265860568199,1.46282983050319));
#84077=CARTESIAN_POINT('Ctrl Pts',(48.4082703988973,-3.60815931243622,1.56939146215388));
#84078=CARTESIAN_POINT('Ctrl Pts',(48.4024536234553,-3.55905282173006,1.67380763892846));
#84079=CARTESIAN_POINT('Ctrl Pts',(48.396637633795,-3.50995296476548,1.7782097102371));
#84080=CARTESIAN_POINT('Ctrl Pts',(48.3908216441348,-3.45624732587386,1.88046652385039));
#84081=CARTESIAN_POINT('Ctrl Pts',(48.3850056544745,-3.39816041180273,1.98015020027692));
#84082=CARTESIAN_POINT('Ctrl Pts',(48.3791889988926,-3.34006684687096,2.07984529032817));
#84083=CARTESIAN_POINT('Ctrl Pts',(48.3733723433106,-3.27759122087877,2.17696629582394));
#84084=CARTESIAN_POINT('Ctrl Pts',(48.3675556877287,-3.21100274889135,2.27111213871359));
#84085=CARTESIAN_POINT('Ctrl Pts',(48.3616563726098,-3.14346799906705,2.36659587271112));
#84086=CARTESIAN_POINT('Ctrl Pts',(48.3557570574909,-3.07170285443242,2.45901886339764));
#84087=CARTESIAN_POINT('Ctrl Pts',(48.349857742372,-2.9960312515734,2.5479964167156));
#84088=CARTESIAN_POINT('Ctrl Pts',(48.3440322443374,-2.92130651406732,2.63586060968115));
#84089=CARTESIAN_POINT('Ctrl Pts',(48.3382067463029,-2.84277285759069,2.72036483345076));
#84090=CARTESIAN_POINT('Ctrl Pts',(48.3323812482684,-2.76077939831325,2.80117584486393));
#84091=CARTESIAN_POINT('Ctrl Pts',(48.3264450246073,-2.6772274839308,2.88352283651732));
#84092=CARTESIAN_POINT('Ctrl Pts',(48.3205088009462,-2.59008325111016,2.96203448838341));
#84093=CARTESIAN_POINT('Ctrl Pts',(48.3145725772851,-2.49975036241423,3.03640200329435));
#84094=CARTESIAN_POINT('Ctrl Pts',(48.308636353624,-2.40941747371832,3.11076951820526));
#84095=CARTESIAN_POINT('Ctrl Pts',(48.3027001299629,-2.3158963318695,3.18099267867581));
#84096=CARTESIAN_POINT('Ctrl Pts',(48.2967639063018,-2.21961939102252,3.24681055175642));
#84097=CARTESIAN_POINT('Ctrl Pts',(48.2908898279569,-2.12435035709865,3.3119393887152));
#84098=CARTESIAN_POINT('Ctrl Pts',(48.2850157496119,-2.02605343213304,3.37298018509058));
#84099=CARTESIAN_POINT('Ctrl Pts',(48.2791416712669,-1.92511465841178,3.42963883695763));
#84100=CARTESIAN_POINT('Ctrl Pts',(48.273275194168,-1.82430650270457,3.48622417071002));
#84101=CARTESIAN_POINT('Ctrl Pts',(48.267408717069,-1.72086365371022,3.53843843664275));
#84102=CARTESIAN_POINT('Ctrl Pts',(48.26154223997,-1.61520224345694,3.58602993751191));
#84103=CARTESIAN_POINT('Ctrl Pts',(48.2556817877773,-1.50964934809005,3.63357256163129));
#84104=CARTESIAN_POINT('Ctrl Pts',(48.2498213355846,-1.40188279793812,3.67650169542959));
#84105=CARTESIAN_POINT('Ctrl Pts',(48.243960883392,-1.29234393088991,3.71461117269251));
#84106=CARTESIAN_POINT('Ctrl Pts',(48.2378757085657,-1.17860472880421,3.75418198123374));
#84107=CARTESIAN_POINT('Ctrl Pts',(48.2317905337395,-1.06295496255167,3.78855588415592));
#84108=CARTESIAN_POINT('Ctrl Pts',(48.2257053589132,-0.945912664613604,
3.8175565786146));
#84109=CARTESIAN_POINT('Ctrl Pts',(48.219851687597,-0.833323106912179,3.84545397485219));
#84110=CARTESIAN_POINT('Ctrl Pts',(48.2139980162808,-0.719445474591379,
3.86837942247393));
#84111=CARTESIAN_POINT('Ctrl Pts',(48.2081443449646,-0.60475625264573,3.88622681722077));
#84112=CARTESIAN_POINT('Ctrl Pts',(48.2022915665054,-0.49008452417913,3.90407148971507));
#84113=CARTESIAN_POINT('Ctrl Pts',(48.1964387880463,-0.374601860298475,
3.91683958592564));
#84114=CARTESIAN_POINT('Ctrl Pts',(48.1905860095871,-0.258793506260321,
3.92447638814626));
#84115=CARTESIAN_POINT('Ctrl Pts',(48.1847327088812,-0.142974818578138,
3.932113871803));
#84116=CARTESIAN_POINT('Ctrl Pts',(48.1788794081753,-0.0268307951890033,
3.93461912408343));
#84117=CARTESIAN_POINT('Ctrl Pts',(48.1730261074695,0.0891503589144591,
3.9319894727104));
#84118=CARTESIAN_POINT('Ctrl Pts',(48.1671708693795,0.205169901621544,3.92935895094904));
#84119=CARTESIAN_POINT('Ctrl Pts',(48.1613156312896,0.3210260550782,3.92159015529858));
#84120=CARTESIAN_POINT('Ctrl Pts',(48.1554603931996,0.436233491927892,3.90873244678123));
#84121=CARTESIAN_POINT('Ctrl Pts',(48.1495985190088,0.551571500440835,3.89586016583321));
#84122=CARTESIAN_POINT('Ctrl Pts',(48.1437366448179,0.666258914056482,3.87788750592427));
#84123=CARTESIAN_POINT('Ctrl Pts',(48.1378747706271,0.779818280783277,3.85491536210021));
#84124=CARTESIAN_POINT('Ctrl Pts',(48.1320089580572,0.893453943896832,3.83192778413259));
#84125=CARTESIAN_POINT('Ctrl Pts',(48.1261431454874,1.0059596510704,3.80393413323241));
#84126=CARTESIAN_POINT('Ctrl Pts',(48.1202773329176,1.11687253241484,3.7710853538918));
#84127=CARTESIAN_POINT('Ctrl Pts',(48.1144029101881,1.22794821773791,3.73818835732065));
#84128=CARTESIAN_POINT('Ctrl Pts',(48.1085284874585,1.3374260218931,3.70042214311632));
#84129=CARTESIAN_POINT('Ctrl Pts',(48.102654064729,1.44486240208544,3.65798600858996));
#84130=CARTESIAN_POINT('Ctrl Pts',(48.1010749390067,1.47374278051279,3.64657859127079));
#84131=CARTESIAN_POINT('Ctrl Pts',(48.0994958132844,1.50247578059378,3.6348339790261));
#84132=CARTESIAN_POINT('Ctrl Pts',(48.0979166875621,1.53105310235788,3.62275660205876));
#84133=CARTESIAN_POINT('Ctrl Pts',(48.0920430178542,1.63734846998385,3.57783394501977));
#84134=CARTESIAN_POINT('Ctrl Pts',(48.0861693481464,1.7418421306723,3.52815426272047));
#84135=CARTESIAN_POINT('Ctrl Pts',(48.0802956784385,1.84407800639631,3.47388331789158));
#84136=CARTESIAN_POINT('Ctrl Pts',(48.074429592217,1.94618188552957,3.41968244220078));
#84137=CARTESIAN_POINT('Ctrl Pts',(48.0685635059956,2.04603341512508,3.3609022843018));
#84138=CARTESIAN_POINT('Ctrl Pts',(48.0626974197741,2.14319592845312,3.29775684553334));
#84139=CARTESIAN_POINT('Ctrl Pts',(48.056837340294,2.24025894953682,3.23467606628434));
#84140=CARTESIAN_POINT('Ctrl Pts',(48.0509772608139,2.33463808690553,3.16723912104829));
#84141=CARTESIAN_POINT('Ctrl Pts',(48.0451171813337,2.42592135437328,3.09570582943466));
#84142=CARTESIAN_POINT('Ctrl Pts',(48.0390318599791,2.52071324563104,3.0214230371108));
#84143=CARTESIAN_POINT('Ctrl Pts',(48.0329465386245,2.61216609972045,2.94272289146592));
#84144=CARTESIAN_POINT('Ctrl Pts',(48.0268612172698,2.69985149461221,2.85994596225876));
#84145=CARTESIAN_POINT('Ctrl Pts',(48.0210078704915,2.78419429161251,2.7803245185161));
#84146=CARTESIAN_POINT('Ctrl Pts',(48.0151545237132,2.86505127847718,2.6969317292472));
#84147=CARTESIAN_POINT('Ctrl Pts',(48.0093011769348,2.94207565639376,2.61011107657418));
#84148=CARTESIAN_POINT('Ctrl Pts',(48.0034487045672,3.01908852791185,2.52330339373037));
#84149=CARTESIAN_POINT('Ctrl Pts',(47.9975962321996,3.0922696547716,2.43306917464447));
#84150=CARTESIAN_POINT('Ctrl Pts',(47.991743759832,3.16131073701573,2.33978704672649));
#84151=CARTESIAN_POINT('Ctrl Pts',(47.9858907463462,3.230358202781,2.24649629396638));
#84152=CARTESIAN_POINT('Ctrl Pts',(47.9800377328605,3.29526461715692,2.15015740425872));
#84153=CARTESIAN_POINT('Ctrl Pts',(47.9741847193747,3.35576386897012,2.05117962541429));
#84154=CARTESIAN_POINT('Ctrl Pts',(47.9683297491939,3.41628334602088,1.95216875774593));
#84155=CARTESIAN_POINT('Ctrl Pts',(47.9624747790131,3.47239251545957,1.85051759905071));
#84156=CARTESIAN_POINT('Ctrl Pts',(47.9566198088323,3.52387060001388,1.7466610988849));
#84157=CARTESIAN_POINT('Ctrl Pts',(47.950758172327,3.57540729624365,1.64268635027346));
#84158=CARTESIAN_POINT('Ctrl Pts',(47.9448965358218,3.62230219956516,1.53650161880801));
#84159=CARTESIAN_POINT('Ctrl Pts',(47.9390348993165,3.66438214697297,1.42856308259236));
#84160=CARTESIAN_POINT('Ctrl Pts',(47.9331693071063,3.7064904918869,1.32055170443102));
#84161=CARTESIAN_POINT('Ctrl Pts',(47.9273037148961,3.74377727813839,1.21078455505471));
#84162=CARTESIAN_POINT('Ctrl Pts',(47.9214381226858,3.77611933416747,1.09973259209983));
#84163=CARTESIAN_POINT('Ctrl Pts',(47.9155638930086,3.80850901598256,0.988517097889588));
#84164=CARTESIAN_POINT('Ctrl Pts',(47.9096896633315,3.83593933774177,0.876013413978493));
#84165=CARTESIAN_POINT('Ctrl Pts',(47.9038154336543,3.85833825570205,0.762702369595143));
#84166=CARTESIAN_POINT('Ctrl Pts',(47.902233445377,3.86437050632624,0.732186582206608));
#84167=CARTESIAN_POINT('Ctrl Pts',(47.9006514570997,3.87003813163025,0.701612262918697));
#84168=CARTESIAN_POINT('Ctrl Pts',(47.8990694688225,3.87534036911817,0.670988840058476));
#84169=CARTESIAN_POINT('Ctrl Pts',(47.8931981591211,3.8950188198683,0.557334647856081));
#84170=CARTESIAN_POINT('Ctrl Pts',(47.8873268494198,3.909726305003,0.442623035810078));
#84171=CARTESIAN_POINT('Ctrl Pts',(47.8814555397185,3.9193553223701,0.327326835149767));
#84172=CARTESIAN_POINT('Ctrl Pts',(47.87559185214,3.92897183936552,0.212180311793679));
#84173=CARTESIAN_POINT('Ctrl Pts',(47.8697281645615,3.93352296520263,0.0964511172989043));
#84174=CARTESIAN_POINT('Ctrl Pts',(47.8638644769831,3.93295226119242,-0.019378110884881));
#84175=CARTESIAN_POINT('Ctrl Pts',(47.8580068317063,3.93238214527045,-0.13508798156012));
#84176=CARTESIAN_POINT('Ctrl Pts',(47.8521491864295,3.92670069934096,-0.250897269853491));
#84177=CARTESIAN_POINT('Ctrl Pts',(47.8462915411528,3.91590336792172,-0.366319277542559));
#84178=CARTESIAN_POINT('Ctrl Pts',(47.8402053206915,3.90468470644504,-0.486245246371798));
#84179=CARTESIAN_POINT('Ctrl Pts',(47.8341191002303,3.88794272894013,-0.605752641170845));
#84180=CARTESIAN_POINT('Ctrl Pts',(47.828032879769,3.86573198890414,-0.724296341260414));
#84181=CARTESIAN_POINT('Ctrl Pts',(47.822182040935,3.84438023847664,-0.83825542119042));
#84182=CARTESIAN_POINT('Ctrl Pts',(47.8163312021009,3.81797495370962,-0.951323518056299));
#84183=CARTESIAN_POINT('Ctrl Pts',(47.8104803632669,3.78661724024109,-1.06302345971712));
#84184=CARTESIAN_POINT('Ctrl Pts',(47.8046304218782,3.75526433665275,-1.17470626800698));
#84185=CARTESIAN_POINT('Ctrl Pts',(47.7987804804895,3.71896062650313,-1.28502094031307));
#84186=CARTESIAN_POINT('Ctrl Pts',(47.7929305391008,3.67785760393822,-1.39350365810566));
#84187=CARTESIAN_POINT('Ctrl Pts',(47.7870800770231,3.63675092289358,-1.5019960316802));
#84188=CARTESIAN_POINT('Ctrl Pts',(47.7812296149454,3.59084422679533,-1.60865573986473));
#84189=CARTESIAN_POINT('Ctrl Pts',(47.7753791528677,3.54033758856154,-1.71303787436771));
#84190=CARTESIAN_POINT('Ctrl Pts',(47.7695267519312,3.48981421229293,-1.8174546013889));
#84191=CARTESIAN_POINT('Ctrl Pts',(47.7636743509948,3.43468804270889,-1.91959188182632));
#84192=CARTESIAN_POINT('Ctrl Pts',(47.7578219500583,3.37520529466236,-2.01902902873712));
#84193=CARTESIAN_POINT('Ctrl Pts',(47.751962896438,3.31565492993703,-2.1185792102646));
#84194=CARTESIAN_POINT('Ctrl Pts',(47.7461038428178,3.25173831453506,-2.21542277683459));
#84195=CARTESIAN_POINT('Ctrl Pts',(47.7402447891975,3.18374527432843,-2.30916760504546));
#84196=CARTESIAN_POINT('Ctrl Pts',(47.7343817910201,3.11570645839669,-2.40297554614955));
#84197=CARTESIAN_POINT('Ctrl Pts',(47.7285187928428,3.04358600977531,-2.49368027200128));
#84198=CARTESIAN_POINT('Ctrl Pts',(47.7226557946655,2.96771322403652,-2.58092371446324));
#84199=CARTESIAN_POINT('Ctrl Pts',(47.7167841553799,2.89172861412003,-2.66829573960631));
#84200=CARTESIAN_POINT('Ctrl Pts',(47.7109125160944,2.81198091350175,-2.75219600145978));
#84201=CARTESIAN_POINT('Ctrl Pts',(47.7050408768089,2.72883537233496,-2.8323040992615));
#84202=CARTESIAN_POINT('Ctrl Pts',(47.7034346679002,2.70609059827031,-2.85421796932213));
#84203=CARTESIAN_POINT('Ctrl Pts',(47.7018284589915,2.68309174140948,-2.87584830433206));
#84204=CARTESIAN_POINT('Ctrl Pts',(47.7002222500828,2.65984667742076,-2.89718909507367));
#84205=CARTESIAN_POINT('Ctrl Pts',(47.6943494954793,2.5748561411265,-2.97521706913959));
#84206=CARTESIAN_POINT('Ctrl Pts',(47.6884767408758,2.4862870283832,-3.04963254301817));
#84207=CARTESIAN_POINT('Ctrl Pts',(47.6826039862723,2.39447927651606,-3.12008942088766));
#84208=CARTESIAN_POINT('Ctrl Pts',(47.6767388368527,2.3027904151666,-3.19045505750015));
#84209=CARTESIAN_POINT('Ctrl Pts',(47.670873687433,2.20787157999033,-3.25687204332534));
#84210=CARTESIAN_POINT('Ctrl Pts',(47.6650085380134,2.11009854825462,-3.31903195475032));
#84211=CARTESIAN_POINT('Ctrl Pts',(47.6591494157994,2.01242599105466,-3.38112798876318));
#84212=CARTESIAN_POINT('Ctrl Pts',(47.6532902935853,1.91190541802128,-3.43897542950064));
#84213=CARTESIAN_POINT('Ctrl Pts',(47.6474311713713,1.80894405682423,-3.49230731741642));
#84214=CARTESIAN_POINT('Ctrl Pts',(47.6413454988701,1.70200156584504,-3.5477013494691));
#84215=CARTESIAN_POINT('Ctrl Pts',(47.635259826369,1.59242608449288,-3.59822330392868));
#84216=CARTESIAN_POINT('Ctrl Pts',(47.6291741538678,1.48070545057497,-3.6436246196113));
#84217=CARTESIAN_POINT('Ctrl Pts',(47.6233218096457,1.3732682517648,-3.68728522202805));
#84218=CARTESIAN_POINT('Ctrl Pts',(47.6174694654236,1.26384778289763,-3.72621044297521));
#84219=CARTESIAN_POINT('Ctrl Pts',(47.6116171212014,1.15290034873803,-3.76022735826967));
#84220=CARTESIAN_POINT('Ctrl Pts',(47.6057656664612,1.04196977717749,-3.79423910342561));
#84221=CARTESIAN_POINT('Ctrl Pts',(47.599914211721,0.929513096818536,-3.82334390510347));
#84222=CARTESIAN_POINT('Ctrl Pts',(47.5940627569807,0.816002612318447,-3.84741845094727));
#84223=CARTESIAN_POINT('Ctrl Pts',(47.5882107751708,0.702481903362645,-3.87149516530553));
#84224=CARTESIAN_POINT('Ctrl Pts',(47.5823587933608,0.587907605908124,-3.89054063735023));
#84225=CARTESIAN_POINT('Ctrl Pts',(47.5765068115509,0.47276237440816,-3.90448264656714));
#84226=CARTESIAN_POINT('Ctrl Pts',(47.570652886081,0.3575788989112,-3.9184292864418));
#84227=CARTESIAN_POINT('Ctrl Pts',(47.5647989606111,0.241824522396646,-3.92726904332349));
#84228=CARTESIAN_POINT('Ctrl Pts',(47.5589450351412,0.125986466751967,-3.93098160898717));
#84229=CARTESIAN_POINT('Ctrl Pts',(47.5530844575288,0.0100167778548999,
-3.93469839344657));
#84230=CARTESIAN_POINT('Ctrl Pts',(47.5472238799164,-0.10603636662833,-3.9332763443045));
#84231=CARTESIAN_POINT('Ctrl Pts',(47.5413633023041,-0.221686196205895,
-3.92674728374666));
#84232=CARTESIAN_POINT('Ctrl Pts',(47.5354987785597,-0.337413896861429,
-3.92021382694383));
#84233=CARTESIAN_POINT('Ctrl Pts',(47.5296342548153,-0.45273733165556,-3.9085665529287));
#84234=CARTESIAN_POINT('Ctrl Pts',(47.5237697310709,-0.567177036468162,
-3.89188889991778));
#84235=CARTESIAN_POINT('Ctrl Pts',(47.5178965757204,-0.681785177541864,
-3.87518670016827));
#84236=CARTESIAN_POINT('Ctrl Pts',(47.51202342037,-0.795506588259925,-3.85343942207063));
#84237=CARTESIAN_POINT('Ctrl Pts',(47.5061502650195,-0.907874049112982,
-3.82678111615326));
#84238=CARTESIAN_POINT('Ctrl Pts',(47.5045585204607,-0.938327916534902,
-3.81955617302527));
#84239=CARTESIAN_POINT('Ctrl Pts',(47.502966775902,-0.968682433722741,-3.81197078341857));
#84240=CARTESIAN_POINT('Ctrl Pts',(47.5013750313433,-0.998928538987354,
-3.80402822991583));
#84241=CARTESIAN_POINT('Ctrl Pts',(47.4955024488879,-1.1105185212781,-3.77472497262171));
#84242=CARTESIAN_POINT('Ctrl Pts',(47.4896298664325,-1.22100472439362,-3.74045833527711));
#84243=CARTESIAN_POINT('Ctrl Pts',(47.4837572839771,-1.32991222295747,-3.70132712405001));
#84244=CARTESIAN_POINT('Ctrl Pts',(47.4778923057512,-1.43867870049359,-3.66224658264544));
#84245=CARTESIAN_POINT('Ctrl Pts',(47.4720273275254,-1.54587015329953,-3.61831413230468));
#84246=CARTESIAN_POINT('Ctrl Pts',(47.4661623492995,-1.65102396609546,-3.56967909809529));
#84247=CARTESIAN_POINT('Ctrl Pts',(47.4603033971205,-1.75606973726155,-3.52109403457383));
#84248=CARTESIAN_POINT('Ctrl Pts',(47.4544444449415,-1.85908165980543,-3.46781617024461));
#84249=CARTESIAN_POINT('Ctrl Pts',(47.4485854927625,-1.95961499212944,-3.41004370684915));
#84250=CARTESIAN_POINT('Ctrl Pts',(47.4424997560892,-2.06403970301986,-3.35003502467343));
#84251=CARTESIAN_POINT('Ctrl Pts',(47.4364140194159,-2.16578963941227,-3.2851769178553));
#84252=CARTESIAN_POINT('Ctrl Pts',(47.4303282827426,-2.26439189659742,-3.21574537838802));
#84253=CARTESIAN_POINT('Ctrl Pts',(47.4244761045323,-2.35920999536975,-3.14897848323712));
#84254=CARTESIAN_POINT('Ctrl Pts',(47.4186239263219,-2.45111719634862,-3.07798298423056));
#84255=CARTESIAN_POINT('Ctrl Pts',(47.4127717481116,-2.53972132550726,-3.00304921517508));
#84256=CARTESIAN_POINT('Ctrl Pts',(47.4069204576031,-2.62831201453301,-2.92812681263064));
#84257=CARTESIAN_POINT('Ctrl Pts',(47.4010691670946,-2.71360031244272,-2.84926759467338));
#84258=CARTESIAN_POINT('Ctrl Pts',(47.3952178765862,-2.79522712830017,-2.76680217963171));
#84259=CARTESIAN_POINT('Ctrl Pts',(47.3893660570423,-2.87686132432127,-2.68432930860573));
#84260=CARTESIAN_POINT('Ctrl Pts',(47.3835142374983,-2.95483308940464,-2.59824988611721));
#84261=CARTESIAN_POINT('Ctrl Pts',(47.3776624179544,-3.02882071597627,-2.50893086203525));
#84262=CARTESIAN_POINT('Ctrl Pts',(47.3718086525974,-3.10283294448411,-2.41958213810977));
#84263=CARTESIAN_POINT('Ctrl Pts',(47.3659548872403,-3.17285813669213,-2.32699198875545));
#84264=CARTESIAN_POINT('Ctrl Pts',(47.3601011218833,-3.23861578526996,-2.23155927445368));
#84265=CARTESIAN_POINT('Ctrl Pts',(47.3542407003537,-3.30444820525265,-2.13601804595969));
#84266=CARTESIAN_POINT('Ctrl Pts',(47.3483802788241,-3.36600316147584,-2.03762814169207));
#84267=CARTESIAN_POINT('Ctrl Pts',(47.3425198572944,-3.42304424395122,-1.93681622875079));
#84268=CARTESIAN_POINT('Ctrl Pts',(47.3366554874771,-3.48012375618902,-1.83593639672915));
#84269=CARTESIAN_POINT('Ctrl Pts',(47.3307911176597,-3.5326831522767,-1.73263167436644));
#84270=CARTESIAN_POINT('Ctrl Pts',(47.3249267478423,-3.5805333936393,-1.62735048991723));
#84271=CARTESIAN_POINT('Ctrl Pts',(47.3190537420387,-3.62845410020758,-1.52191426632704));
#84272=CARTESIAN_POINT('Ctrl Pts',(47.3131807362351,-3.67165165794374,-1.41449615376108));
#84273=CARTESIAN_POINT('Ctrl Pts',(47.3073077304315,-3.70998622524951,-1.30556164483295));
#84274=CARTESIAN_POINT('Ctrl Pts',(47.3057144244889,-3.72038612879807,-1.27600846435938));
#84275=CARTESIAN_POINT('Ctrl Pts',(47.3041211185462,-3.73042840543479,-1.24634374364339));
#84276=CARTESIAN_POINT('Ctrl Pts',(47.3025278126036,-3.74011091092013,-1.21657690838526));
#84277=CARTESIAN_POINT('Ctrl Pts',(47.295489133608,-3.78288489811189,-1.0850772431386));
#84278=CARTESIAN_POINT('Ctrl Pts',(47.2884504546125,-3.8187501841302,-0.951226593623726));
#84279=CARTESIAN_POINT('Ctrl Pts',(47.2814117756169,-3.8474848584014,-0.815689441130601));
#84280=CARTESIAN_POINT('Ctrl Pts',(47.2744513536712,-3.87590005641323,-0.681659210277727));
#84281=CARTESIAN_POINT('Ctrl Pts',(47.2674909317255,-3.89734228445253,-0.54597981908715));
#84282=CARTESIAN_POINT('Ctrl Pts',(47.2605305097797,-3.91164293126658,-0.40931476674097));
#84283=CARTESIAN_POINT('Ctrl Pts',(47.253674861034,-3.92572831461808,-0.274706893539193));
#84284=CARTESIAN_POINT('Ctrl Pts',(47.2468192122883,-3.93288545623893,-0.139142876403734));
#84285=CARTESIAN_POINT('Ctrl Pts',(47.2399635635426,-3.93299863541307,-0.00327625379142282));
#84286=CARTESIAN_POINT('',(45.9899634930907,-3.93107654104103,0.00207074533378259));
#84287=CARTESIAN_POINT('Ctrl Pts',(47.2399635220349,-3.92992510810637,-0.00327287152616401));
#84288=CARTESIAN_POINT('Ctrl Pts',(47.1945358793113,-3.92290211273228,0.896324194432669));
#84289=CARTESIAN_POINT('Ctrl Pts',(47.082825830341,-3.16907068698517,3.11914721721579));
#84290=CARTESIAN_POINT('Ctrl Pts',(46.9048333751243,0.527994240069298,4.62159797093886));
#84291=CARTESIAN_POINT('Ctrl Pts',(46.7059861563847,4.17322476015174,2.0547975509789));
#84292=CARTESIAN_POINT('Ctrl Pts',(46.5071389376449,3.98501756744227,-2.39950675661282));
#84293=CARTESIAN_POINT('Ctrl Pts',(46.3082917189054,0.136254273817925,-4.64966862412523));
#84294=CARTESIAN_POINT('Ctrl Pts',(46.1358999137019,-3.30896276145751,-2.89761448064259));
#84295=CARTESIAN_POINT('Ctrl Pts',(46.0297905147452,-3.9238187618561,-0.787807482198896));
#84296=CARTESIAN_POINT('Ctrl Pts',(45.9899635220349,-3.92757019263908,0.00206832399879703));
#84297=CARTESIAN_POINT('',(44.7399635220349,-3.93446379439651,0.0024830546121077));
#84298=CARTESIAN_POINT('Ctrl Pts',(45.9899634772174,-3.93299945417141,0.00207207321575638));
#84299=CARTESIAN_POINT('Ctrl Pts',(45.9833496275681,-3.9329302526653,0.133423361231383));
#84300=CARTESIAN_POINT('Ctrl Pts',(45.9767357779188,-3.92627640942975,0.26454482366088));
#84301=CARTESIAN_POINT('Ctrl Pts',(45.9701219282695,-3.91313366715487,0.394808691620507));
#84302=CARTESIAN_POINT('Ctrl Pts',(45.9636237689115,-3.90022081938343,0.522793967592652));
#84303=CARTESIAN_POINT('Ctrl Pts',(45.9571256095534,-3.88104439224054,0.64995119918622));
#84304=CARTESIAN_POINT('Ctrl Pts',(45.9506274501953,-3.85574587958801,0.775701432279254));
#84305=CARTESIAN_POINT('Ctrl Pts',(45.9439557554004,-3.82977176201388,0.904809865814193));
#84306=CARTESIAN_POINT('Ctrl Pts',(45.9372840606055,-3.79734414290077,1.03243481741227));
#84307=CARTESIAN_POINT('Ctrl Pts',(45.9306123658106,-3.75866883754653,1.15797131642222));
#84308=CARTESIAN_POINT('Ctrl Pts',(45.9239406710158,-3.7199935321923,1.28350781543213));
#84309=CARTESIAN_POINT('Ctrl Pts',(45.9172689762209,-3.67507071678868,1.40695563122873));
#84310=CARTESIAN_POINT('Ctrl Pts',(45.910597281426,-3.62415700711541,1.5277352479328));
#84311=CARTESIAN_POINT('Ctrl Pts',(45.9047248338578,-3.57934259342467,1.63404586138289));
#84312=CARTESIAN_POINT('Ctrl Pts',(45.8988523862897,-3.52977142964467,1.73856091847256));
#84313=CARTESIAN_POINT('Ctrl Pts',(45.8929799387215,-3.47560856965179,1.84082429106177));
#84314=CARTESIAN_POINT('Ctrl Pts',(45.8871150983274,-3.42151587227798,1.94295519158326));
#84315=CARTESIAN_POINT('Ctrl Pts',(45.8812502579333,-3.36284349900859,2.04283984623267));
#84316=CARTESIAN_POINT('Ctrl Pts',(45.8753854175392,-3.2998047705344,2.14004146603714));
#84317=CARTESIAN_POINT('Ctrl Pts',(45.8695266059567,-3.23683084324713,2.23714316662551));
#84318=CARTESIAN_POINT('Ctrl Pts',(45.8636677943742,-3.16949971205812,2.33156697355163));
#84319=CARTESIAN_POINT('Ctrl Pts',(45.8578089827917,-3.09807055090966,2.422900712284));
#84320=CARTESIAN_POINT('Ctrl Pts',(45.8517231944539,-3.02387414609812,2.51777281973958));
#84321=CARTESIAN_POINT('Ctrl Pts',(45.8456374061162,-2.94525597783488,2.6093101899429));
#84322=CARTESIAN_POINT('Ctrl Pts',(45.8395516177785,-2.86255624786836,2.69708374504571));
#84323=CARTESIAN_POINT('Ctrl Pts',(45.833699586214,-2.7830330368584,2.78148589419858));
#84324=CARTESIAN_POINT('Ctrl Pts',(45.8278475546495,-2.69973633784404,2.86240770440601));
#84325=CARTESIAN_POINT('Ctrl Pts',(45.8219955230849,-2.61300908549438,2.93950208693987));
#84326=CARTESIAN_POINT('Ctrl Pts',(45.8161443812139,-2.52629501842428,3.0165847486944));
#84327=CARTESIAN_POINT('Ctrl Pts',(45.8102932393429,-2.43615174389131,3.08984086521073));
#84328=CARTESIAN_POINT('Ctrl Pts',(45.8044420974718,-2.3429573898478,3.15896180245307));
#84329=CARTESIAN_POINT('Ctrl Pts',(45.7985904284071,-2.24975463890086,3.2280889675602));
#84330=CARTESIAN_POINT('Ctrl Pts',(45.7927387593424,-2.15350059398267,3.29307996647261));
#84331=CARTESIAN_POINT('Ctrl Pts',(45.7868870902777,-2.05460405395717,3.35366831715105));
#84332=CARTESIAN_POINT('Ctrl Pts',(45.7810334770931,-1.95567465719872,3.41427679730276));
#84333=CARTESIAN_POINT('Ctrl Pts',(45.7751798639086,-1.85410137191503,3.47047950489353));
#84334=CARTESIAN_POINT('Ctrl Pts',(45.769326250724,-1.75031875069544,3.52205526233816));
#84335=CARTESIAN_POINT('Ctrl Pts',(45.7634659831268,-1.64641814894475,3.57368965132615));
#84336=CARTESIAN_POINT('Ctrl Pts',(45.7576057155295,-1.54030356860845,3.62068640744339));
#84337=CARTESIAN_POINT('Ctrl Pts',(45.7517454479322,-1.43243084273132,3.6628719443617));
#84338=CARTESIAN_POINT('Ctrl Pts',(45.7458812332634,-1.32448546123561,3.70508589454439));
#84339=CARTESIAN_POINT('Ctrl Pts',(45.7400170185946,-1.2147799665808,3.74248203998889));
#84340=CARTESIAN_POINT('Ctrl Pts',(45.7341528039258,-1.10378502384003,3.77493677048324));
#84341=CARTESIAN_POINT('Ctrl Pts',(45.7282799538654,-0.992626634696376,
3.80743929242489));
#84342=CARTESIAN_POINT('Ctrl Pts',(45.722407103805,-0.880175407843266,3.83498577895984));
#84343=CARTESIAN_POINT('Ctrl Pts',(45.7165342537446,-0.766911932180097,
3.85750373794761));
#84344=CARTESIAN_POINT('Ctrl Pts',(45.7149395233919,-0.7361560469392,3.86361832836109));
#84345=CARTESIAN_POINT('Ctrl Pts',(45.7133447930392,-0.705340295015743,
3.86936243364421));
#84346=CARTESIAN_POINT('Ctrl Pts',(45.7117500626865,-0.674474337062625,
3.87473526433019));
#84347=CARTESIAN_POINT('Ctrl Pts',(45.70587761653,-0.560813318546454,3.89452021346446));
#84348=CARTESIAN_POINT('Ctrl Pts',(45.7000051703735,-0.446090714275419,
3.90933286902292));
#84349=CARTESIAN_POINT('Ctrl Pts',(45.694132724217,-0.33077946938094,3.91906544250489));
#84350=CARTESIAN_POINT('Ctrl Pts',(45.6882678852455,-0.2156175990323,3.92878540838086));
#84351=CARTESIAN_POINT('Ctrl Pts',(45.6824030462741,-0.099869012550308,
3.93343834451574));
#84352=CARTESIAN_POINT('Ctrl Pts',(45.6765382073026,0.0159835148301993,
3.93296752176441));
#84353=CARTESIAN_POINT('Ctrl Pts',(45.670679397152,0.131716950427295,3.93249718300011));
#84354=CARTESIAN_POINT('Ctrl Pts',(45.6648205870014,0.247553703526219,3.92691356341085));
#84355=CARTESIAN_POINT('Ctrl Pts',(45.6589617768508,0.363006911437183,3.91621181529406));
#84356=CARTESIAN_POINT('Ctrl Pts',(45.6528759879798,0.482932942451069,3.90509546608403));
#84357=CARTESIAN_POINT('Ctrl Pts',(45.6467901991088,0.602444656298446,3.88845636229384));
#84358=CARTESIAN_POINT('Ctrl Pts',(45.6407044102378,0.72099715796601,3.86634867778437));
#84359=CARTESIAN_POINT('Ctrl Pts',(45.6348523801191,0.834995987880806,3.84509016252104));
#84360=CARTESIAN_POINT('Ctrl Pts',(45.6290003500004,0.948107490242205,3.81877550282313));
#84361=CARTESIAN_POINT('Ctrl Pts',(45.6231483198818,1.05985426280836,3.7875055038385));
#84362=CARTESIAN_POINT('Ctrl Pts',(45.6172971794593,1.17158404628275,3.75624025889616));
#84363=CARTESIAN_POINT('Ctrl Pts',(45.6114460390368,1.28194911454815,3.72002128397307));
#84364=CARTESIAN_POINT('Ctrl Pts',(45.6055948986143,1.39048538441558,3.67899978196882));
#84365=CARTESIAN_POINT('Ctrl Pts',(45.5997432309993,1.49903143348947,3.63797458389379));
#84366=CARTESIAN_POINT('Ctrl Pts',(45.5938915633842,1.6057479699206,3.59214614469524));
#84367=CARTESIAN_POINT('Ctrl Pts',(45.5880398957692,1.71018978507401,3.54171425993522));
#84368=CARTESIAN_POINT('Ctrl Pts',(45.5821862840339,1.81466629930169,3.49126562001147));
#84369=CARTESIAN_POINT('Ctrl Pts',(45.5763326722987,1.91686621747538,3.43621067301501));
#84370=CARTESIAN_POINT('Ctrl Pts',(45.5704790605634,2.01636851616535,3.37679537535474));
#84371=CARTESIAN_POINT('Ctrl Pts',(45.5646187944075,2.11598392966051,3.31731253403057));
#84372=CARTESIAN_POINT('Ctrl Pts',(45.5587585282515,2.21289524759174,3.25345966033542));
#84373=CARTESIAN_POINT('Ctrl Pts',(45.5528982620956,2.30670997415815,3.18552634506753));
#84374=CARTESIAN_POINT('Ctrl Pts',(45.5470340488652,2.40058788790678,3.11754727456559));
#84375=CARTESIAN_POINT('Ctrl Pts',(45.5411698356349,2.49136473438587,3.04548254644141));
#84376=CARTESIAN_POINT('Ctrl Pts',(45.5353056224046,2.5786820383223,2.96966125092307));
#84377=CARTESIAN_POINT('Ctrl Pts',(45.5294327737673,2.66612792224426,2.89372830398352));
#84378=CARTESIAN_POINT('Ctrl Pts',(45.5235599251301,2.75010379755439,2.81402803281994));
#84379=CARTESIAN_POINT('Ctrl Pts',(45.5176870764928,2.83028882404551,2.73092551573328));
#84380=CARTESIAN_POINT('Ctrl Pts',(45.5160923323108,2.85206268752807,2.70835942152238));
#84381=CARTESIAN_POINT('Ctrl Pts',(45.5144975881288,2.87355726132222,2.68554263745087));
#84382=CARTESIAN_POINT('Ctrl Pts',(45.5129028439468,2.89476665755451,2.66248286347737));
#84383=CARTESIAN_POINT('Ctrl Pts',(45.5070303982175,2.97286760297757,2.57756813375818));
#84384=CARTESIAN_POINT('Ctrl Pts',(45.5011579524883,3.04735982192094,2.48907181891898));
#84385=CARTESIAN_POINT('Ctrl Pts',(45.4952855067591,3.11789691544379,2.39733348215598));
#84386=CARTESIAN_POINT('Ctrl Pts',(45.4894206682254,3.1883426348642,2.30571398369154));
#84387=CARTESIAN_POINT('Ctrl Pts',(45.4835558296916,3.25484316802578,2.21086113974441));
#84388=CARTESIAN_POINT('Ctrl Pts',(45.4776909911579,3.31708975232654,2.11315039100633));
#84389=CARTESIAN_POINT('Ctrl Pts',(45.4718321814548,3.37927234950895,2.01554008519721));
#84390=CARTESIAN_POINT('Ctrl Pts',(45.4659733717518,3.43720947500505,1.91507806460877));
#84391=CARTESIAN_POINT('Ctrl Pts',(45.4601145620487,3.49063379920915,1.81217126117228));
#84392=CARTESIAN_POINT('Ctrl Pts',(45.4540287730136,3.54612786420274,1.70527768931592));
#84393=CARTESIAN_POINT('Ctrl Pts',(45.4479429839786,3.59675211319836,1.59574643428041));
#84394=CARTESIAN_POINT('Ctrl Pts',(45.4418571949435,3.64225748729813,1.48406515902122));
#84395=CARTESIAN_POINT('Ctrl Pts',(45.4360051652942,3.68601496835745,1.37667363915109));
#84396=CARTESIAN_POINT('Ctrl Pts',(45.430153135645,3.72503938938397,1.26729463805309));
#84397=CARTESIAN_POINT('Ctrl Pts',(45.4243011059957,3.75915741224881,1.15638425704212));
#84398=CARTESIAN_POINT('Ctrl Pts',(45.4184499660499,3.79327024803743,1.04549073810435));
#84399=CARTESIAN_POINT('Ctrl Pts',(45.4125988261041,3.82247804732586,0.933066697155677));
#84400=CARTESIAN_POINT('Ctrl Pts',(45.4067476861584,3.84665706876898,0.819584281992779));
#84401=CARTESIAN_POINT('Ctrl Pts',(45.4008960190269,3.87083826873363,0.706091642103263));
#84402=CARTESIAN_POINT('Ctrl Pts',(45.3950443518954,3.88998970400641,0.591540842741068));
#84403=CARTESIAN_POINT('Ctrl Pts',(45.3891926847639,3.90403871548622,0.476414428816662));
#84404=CARTESIAN_POINT('Ctrl Pts',(45.3833390735185,3.918092394504,0.361249766157874));
#84405=CARTESIAN_POINT('Ctrl Pts',(45.3774854622732,3.92704022890058,0.245509518768089));
#84406=CARTESIAN_POINT('Ctrl Pts',(45.3716318510278,3.9308614676783,0.129680846395937));
#84407=CARTESIAN_POINT('Ctrl Pts',(45.3657715853688,3.93468705045878,0.0137204994277308));
#84408=CARTESIAN_POINT('Ctrl Pts',(45.3599113197098,3.93337439161206,-0.102328059785022));
#84409=CARTESIAN_POINT('Ctrl Pts',(45.3540510540507,3.92695487095885,-0.217978075623614));
#84410=CARTESIAN_POINT('Ctrl Pts',(45.348186841322,3.92053102656046,-0.333705985315314));
#84411=CARTESIAN_POINT('Ctrl Pts',(45.3423226285933,3.90899351240924,-0.449034406834267));
#84412=CARTESIAN_POINT('Ctrl Pts',(45.3364584158646,3.89242533084684,-0.563483845182683));
#84413=CARTESIAN_POINT('Ctrl Pts',(45.3305855677321,3.87583275164646,-0.678101817172088));
#84414=CARTESIAN_POINT('Ctrl Pts',(45.3247127195995,3.85419479718883,-0.791837818170126));
#84415=CARTESIAN_POINT('Ctrl Pts',(45.3188398714669,3.82764509296975,-0.904224553009133));
#84416=CARTESIAN_POINT('Ctrl Pts',(45.3172451227137,3.82043562547685,-0.934742727704025));
#84417=CARTESIAN_POINT('Ctrl Pts',(45.3156503739604,3.81286425855215,-0.965161511444319));
#84418=CARTESIAN_POINT('Ctrl Pts',(45.3140556252071,3.80493428586479,-0.995471787772322));
#84419=CARTESIAN_POINT('Ctrl Pts',(45.3081831788506,3.77573323515354,-1.10708527637067));
#84420=CARTESIAN_POINT('Ctrl Pts',(45.3023107324941,3.74156804667851,-1.21759967111882));
#84421=CARTESIAN_POINT('Ctrl Pts',(45.2964382861375,3.70253706269697,-1.32653997276949));
#84422=CARTESIAN_POINT('Ctrl Pts',(45.2905734469675,3.66355663958204,-1.43533915279066));
#84423=CARTESIAN_POINT('Ctrl Pts',(45.2847086077975,3.61972309385321,-1.54256790918217));
#84424=CARTESIAN_POINT('Ctrl Pts',(45.2788437686276,3.57118529858779,-1.64776350340407));
#84425=CARTESIAN_POINT('Ctrl Pts',(45.2729849582802,3.52269739825527,-1.75285096071767));
#84426=CARTESIAN_POINT('Ctrl Pts',(45.2671261479328,3.46951503916198,-1.85590903992961));
#84427=CARTESIAN_POINT('Ctrl Pts',(45.2612673375854,3.4118359883381,-1.95649282868121));
#84428=CARTESIAN_POINT('Ctrl Pts',(45.2551815487888,3.35192237098437,-2.06097337309331));
#84429=CARTESIAN_POINT('Ctrl Pts',(45.2490957599922,3.28715675230539,-2.16278360700214));
#84430=CARTESIAN_POINT('Ctrl Pts',(45.2430099711957,3.21781469002824,-2.26145033565597));
#84431=CARTESIAN_POINT('Ctrl Pts',(45.2371579408859,3.15113609440967,-2.35632722112586));
#84432=CARTESIAN_POINT('Ctrl Pts',(45.2313059105761,3.08022639715495,-2.44829726485992));
#84433=CARTESIAN_POINT('Ctrl Pts',(45.2254538802664,3.00537554915616,-2.53696803459057));
#84434=CARTESIAN_POINT('Ctrl Pts',(45.2196027396553,2.93053608091667,-2.62562532348507));
#84435=CARTESIAN_POINT('Ctrl Pts',(45.2137515990441,2.85175691986575,-2.71098401993632));
#84436=CARTESIAN_POINT('Ctrl Pts',(45.207900458433,2.76936833282354,-2.79268473644165));
#84437=CARTESIAN_POINT('Ctrl Pts',(45.2020487906319,2.68697232254,-2.87439281421092));
#84438=CARTESIAN_POINT('Ctrl Pts',(45.1961971228309,2.60096653330443,-2.95244196577199));
#84439=CARTESIAN_POINT('Ctrl Pts',(45.1903454550299,2.51171759877025,-3.02651015263915));
#84440=CARTESIAN_POINT('Ctrl Pts',(45.1844918431115,2.42243901279127,-3.10060294740515));
#84441=CARTESIAN_POINT('Ctrl Pts',(45.1786382311931,2.32991545692717,-3.17071188371098));
#84442=CARTESIAN_POINT('Ctrl Pts',(45.1727846192748,2.23454551411417,-3.23655609334247));
#84443=CARTESIAN_POINT('Ctrl Pts',(45.1669243529409,2.13906715427116,-3.30247515500219));
#84444=CARTESIAN_POINT('Ctrl Pts',(45.1610640866071,2.04073628931843,-3.36411957822822));
#84445=CARTESIAN_POINT('Ctrl Pts',(45.1552038202733,1.93997934989935,-3.4212525662342));
#84446=CARTESIAN_POINT('Ctrl Pts',(45.1493396068679,1.83915454754894,-3.47842403508392));
#84447=CARTESIAN_POINT('Ctrl Pts',(45.1434753934625,1.73590078437729,-3.53107783094257));
#84448=CARTESIAN_POINT('Ctrl Pts',(45.1376111800571,1.63066629615307,-3.5790245082411));
#84449=CARTESIAN_POINT('Ctrl Pts',(45.1317383312503,1.52527684391502,-3.62704178986041));
#84450=CARTESIAN_POINT('Ctrl Pts',(45.1258654824435,1.41790122732476,-3.67033796500544));
#84451=CARTESIAN_POINT('Ctrl Pts',(45.1199926336367,1.3090047920021,-3.7087727693289));
#84452=CARTESIAN_POINT('Ctrl Pts',(45.1183978912469,1.27943451576739,-3.71920954604711));
#84453=CARTESIAN_POINT('Ctrl Pts',(45.1168031488572,1.24975216627677,-3.7292881508894));
#84454=CARTESIAN_POINT('Ctrl Pts',(45.1152084064674,1.21996719318159,-3.73900642518312));
#84455=CARTESIAN_POINT('Ctrl Pts',(45.1093359603488,1.11028762940305,-3.77479279577373));
#84456=CARTESIAN_POINT('Ctrl Pts',(45.1034635142301,0.998848473062372,-3.80580899859355));
#84457=CARTESIAN_POINT('Ctrl Pts',(45.0975910681115,0.886102472380609,-3.83188092305084));
#84458=CARTESIAN_POINT('Ctrl Pts',(45.0917262291816,0.77350252329128,-3.85791907383934));
#84459=CARTESIAN_POINT('Ctrl Pts',(45.0858613902516,0.659599495435837,-3.87902559093735));
#84460=CARTESIAN_POINT('Ctrl Pts',(45.0799965513217,0.544863145754668,-3.89507550021798));
#84461=CARTESIAN_POINT('Ctrl Pts',(45.0741377412163,0.430244740542621,-3.91110891082112));
#84462=CARTESIAN_POINT('Ctrl Pts',(45.0682789311109,0.314795124286692,-3.9220959957818));
#84463=CARTESIAN_POINT('Ctrl Pts',(45.0624201210054,0.198995495849135,-3.92796254980006));
#84464=CARTESIAN_POINT('Ctrl Pts',(45.0563343321189,0.0787096222447494,
-3.93405638260983));
#84465=CARTESIAN_POINT('Ctrl Pts',(45.0502485432323,-0.0419534893208762,
-3.93462480424674));
#84466=CARTESIAN_POINT('Ctrl Pts',(45.0441627543457,-0.162446786266555,
-3.92964375505359));
#84467=CARTESIAN_POINT('Ctrl Pts',(45.0383107242811,-0.278311862997924,
-3.92485403096439));
#84468=CARTESIAN_POINT('Ctrl Pts',(45.0324586942165,-0.394019478645874,
-3.91493330776742));
#84469=CARTESIAN_POINT('Ctrl Pts',(45.0266066641519,-0.509082736305069,
-3.89991330257432));
#84470=CARTESIAN_POINT('Ctrl Pts',(45.0207555237866,-0.624128500597504,
-3.88489558091173));
#84471=CARTESIAN_POINT('Ctrl Pts',(45.0149043834213,-0.738529691916645,
-3.86478017220676));
#84472=CARTESIAN_POINT('Ctrl Pts',(45.0090532430561,-0.851805411671151,
-3.83965057533205));
#84473=CARTESIAN_POINT('Ctrl Pts',(45.0032015755014,-0.965091337599584,
-3.81451871427366));
#84474=CARTESIAN_POINT('Ctrl Pts',(44.9973499079468,-1.07725118680878,-3.78437185647899));
#84475=CARTESIAN_POINT('Ctrl Pts',(44.9914982403922,-1.1878158151131,-3.74934428792118));
#84476=CARTESIAN_POINT('Ctrl Pts',(44.9856446287204,-1.29841717663714,-3.7143050820487));
#84477=CARTESIAN_POINT('Ctrl Pts',(44.9797910170486,-1.40742186956713,-3.67438206586608));
#84478=CARTESIAN_POINT('Ctrl Pts',(44.9739374053768,-1.51437810721186,-3.6297586625556));
#84479=CARTESIAN_POINT('Ctrl Pts',(44.9680771392887,-1.62145593326642,-3.58508453112707));
#84480=CARTESIAN_POINT('Ctrl Pts',(44.9622168732006,-1.72648027432731,-3.53569950652833));
#84481=CARTESIAN_POINT('Ctrl Pts',(44.9563566071124,-1.82902135944053,-3.48183426755357));
#84482=CARTESIAN_POINT('Ctrl Pts',(44.9504923939525,-1.93163150916946,-3.42793274866207));
#84483=CARTESIAN_POINT('Ctrl Pts',(44.9446281807926,-2.03175471636381,-3.36954521454028));
#84484=CARTESIAN_POINT('Ctrl Pts',(44.9387639676327,-2.1289892520815,-3.306946289936));
#84485=CARTESIAN_POINT('Ctrl Pts',(44.9328911190691,-2.22636697145233,-3.24425518468169));
#84486=CARTESIAN_POINT('Ctrl Pts',(44.9270182705056,-2.32084719367175,-3.17734054994632));
#84487=CARTESIAN_POINT('Ctrl Pts',(44.921145421942,-2.41206031000855,-3.10651799622688));
#84488=CARTESIAN_POINT('Ctrl Pts',(44.919550677204,-2.43682880790952,-3.08728646085576));
#84489=CARTESIAN_POINT('Ctrl Pts',(44.9179559324659,-2.46135660688793,-3.06776698041003));
#84490=CARTESIAN_POINT('Ctrl Pts',(44.9163611877279,-2.48563678149518,-3.04796633683482));
#84491=CARTESIAN_POINT('Ctrl Pts',(44.9105671096081,-2.57385229654257,-2.9760259986984));
#84492=CARTESIAN_POINT('Ctrl Pts',(44.9047730314883,-2.65910878842539,-2.90011648010944));
#84493=CARTESIAN_POINT('Ctrl Pts',(44.8989789533686,-2.74102038004823,-2.82051347739383));
#84494=CARTESIAN_POINT('Ctrl Pts',(44.8931924170807,-2.82282535186984,-2.7410140895166));
#84495=CARTESIAN_POINT('Ctrl Pts',(44.8874058807929,-2.90129377484753,-2.65783106623817));
#84496=CARTESIAN_POINT('Ctrl Pts',(44.881619344505,-2.97607141756385,-2.5712813765824));
#84497=CARTESIAN_POINT('Ctrl Pts',(44.8757170185688,-3.0523453745741,-2.4829998118225));
#84498=CARTESIAN_POINT('Ctrl Pts',(44.8698146926325,-3.12477889579652,-2.39121565963971));
#84499=CARTESIAN_POINT('Ctrl Pts',(44.8639123666963,-3.19303385795157,-2.29630655226494));
#84500=CARTESIAN_POINT('Ctrl Pts',(44.8581359753042,-3.25983250311532,-2.20342246609502));
#84501=CARTESIAN_POINT('Ctrl Pts',(44.8523595839122,-3.32262885091409,-2.10754580369962));
#84502=CARTESIAN_POINT('Ctrl Pts',(44.8465831925201,-3.38114599827894,-2.00906464264402));
#84503=CARTESIAN_POINT('Ctrl Pts',(44.8408088880004,-3.43964200479542,-1.91061906048086));
#84504=CARTESIAN_POINT('Ctrl Pts',(44.8350345834807,-3.49386166611185,-1.80957121479011));
#84505=CARTESIAN_POINT('Ctrl Pts',(44.8292602789609,-3.54357187614594,-1.70633741053391));
#84506=CARTESIAN_POINT('Ctrl Pts',(44.8234865745486,-3.5932769199365,-1.60311433507914));
#84507=CARTESIAN_POINT('Ctrl Pts',(44.8177128701362,-3.63847326039928,-1.4977061362803));
#84508=CARTESIAN_POINT('Ctrl Pts',(44.8119391657238,-3.67897455680063,-1.39055212430661));
#84509=CARTESIAN_POINT('Ctrl Pts',(44.8059411954164,-3.72104903028886,-1.27923596812068));
#84510=CARTESIAN_POINT('Ctrl Pts',(44.799943225109,-3.75805613309071,-1.16603607841502));
#84511=CARTESIAN_POINT('Ctrl Pts',(44.7939452548016,-3.78984315864233,-1.0514646132381));
#84512=CARTESIAN_POINT('Ctrl Pts',(44.7881654491639,-3.82047399208656,-0.941060465432645));
#84513=CARTESIAN_POINT('Ctrl Pts',(44.7823856435261,-3.84625782289911,-0.829383217623024));
#84514=CARTESIAN_POINT('Ctrl Pts',(44.7766058378884,-3.86711003596097,-0.716902343258804));
#84515=CARTESIAN_POINT('Ctrl Pts',(44.7708228221345,-3.88797383038574,-0.604358996780819));
#84516=CARTESIAN_POINT('Ctrl Pts',(44.7650398063806,-3.90390049724624,-0.491011555797396));
#84517=CARTESIAN_POINT('Ctrl Pts',(44.7592567906267,-3.91485726408778,-0.377334866953882));
#84518=CARTESIAN_POINT('Ctrl Pts',(44.75346655778,-3.92582770476428,-0.26351631178214));
#84519=CARTESIAN_POINT('Ctrl Pts',(44.7476763249333,-3.93181585334791,-0.149368112098914));
#84520=CARTESIAN_POINT('Ctrl Pts',(44.7418860920866,-3.93284099725113,-0.0353651006038775));
#84521=CARTESIAN_POINT('Ctrl Pts',(44.7412452354027,-3.93295445906514,-0.0227473710867152));
#84522=CARTESIAN_POINT('Ctrl Pts',(44.7406043787188,-3.93300717721392,-0.010131414475007));
#84523=CARTESIAN_POINT('Ctrl Pts',(44.7399635220349,-3.93299921675928,0.0024821303117587));
#84524=CARTESIAN_POINT('',(43.4899635220349,-3.93339113294996,-0.0033046727686965));
#84525=CARTESIAN_POINT('Ctrl Pts',(44.7399635220349,-3.93751357002608,0.00248497933675672));
#84526=CARTESIAN_POINT('Ctrl Pts',(44.732480337686,-3.9385999113406,0.149941192123029));
#84527=CARTESIAN_POINT('Ctrl Pts',(44.6587147470908,-3.86405265430505,1.60238341515768));
#84528=CARTESIAN_POINT('Ctrl Pts',(44.5186667502484,-2.0585824653155,4.17135808064711));
#84529=CARTESIAN_POINT('Ctrl Pts',(44.3198195315091,2.39588698568534,3.98719394825372));
#84530=CARTESIAN_POINT('Ctrl Pts',(44.1209723127691,4.64954371604161,0.140475102657688));
#84531=CARTESIAN_POINT('Ctrl Pts',(43.9221250940297,2.63222480384985,-3.83528129358985));
#84532=CARTESIAN_POINT('Ctrl Pts',(43.7232778752899,-1.80300190926075,-4.2880268350132));
#84533=CARTESIAN_POINT('Ctrl Pts',(43.5792240179585,-3.81625323490381,-1.76250455766419));
#84534=CARTESIAN_POINT('Ctrl Pts',(43.5014525668734,-3.9374071917899,-0.230019437054218));
#84535=CARTESIAN_POINT('Ctrl Pts',(43.4899635220349,-3.9353688373681,-0.00330633435426386));
#84536=CARTESIAN_POINT('',(42.2399635491998,-3.93062879302141,-0.000873385175346215));
#84537=CARTESIAN_POINT('Ctrl Pts',(43.4899635220349,-3.932998611914,-0.00330434298873431));
#84538=CARTESIAN_POINT('Ctrl Pts',(43.4841873072457,-3.93309431636171,0.110608002457005));
#84539=CARTESIAN_POINT('Ctrl Pts',(43.4784110924565,-3.92823694115193,0.224695840362946));
#84540=CARTESIAN_POINT('Ctrl Pts',(43.4726348776673,-3.91840740930241,0.33848541286737));
#84541=CARTESIAN_POINT('Ctrl Pts',(43.4668642751708,-3.90858742803428,0.452164425012327));
#84542=CARTESIAN_POINT('Ctrl Pts',(43.4610936726743,-3.89380493005363,0.56554532515269));
#84543=CARTESIAN_POINT('Ctrl Pts',(43.4553230701777,-3.87409289134661,0.678154310771268));
#84544=CARTESIAN_POINT('Ctrl Pts',(43.4495561597942,-3.85439346468033,0.79069124757057));
#84545=CARTESIAN_POINT('Ctrl Pts',(43.4437892494106,-3.82977083967027,0.902456832394481));
#84546=CARTESIAN_POINT('Ctrl Pts',(43.4380223390271,-3.80030974732204,1.01298313135467));
#84547=CARTESIAN_POINT('Ctrl Pts',(43.4322572654583,-3.77085803860671,1.123474226657));
#84548=CARTESIAN_POINT('Ctrl Pts',(43.4264921918896,-3.73657103413654,1.23272640831967));
#84549=CARTESIAN_POINT('Ctrl Pts',(43.4207271183208,-3.69758424204237,1.3402834674053));
#84550=CARTESIAN_POINT('Ctrl Pts',(43.4149623885826,-3.65859977513147,1.44783411175759));
#84551=CARTESIAN_POINT('Ctrl Pts',(43.4091976588445,-3.61491622361328,1.55368943336535));
#84552=CARTESIAN_POINT('Ctrl Pts',(43.4034329291063,-3.5667181905589,1.65741073640068));
#84553=CARTESIAN_POINT('Ctrl Pts',(43.3976670507409,-3.51851055400567,1.76115270599336));
#84554=CARTESIAN_POINT('Ctrl Pts',(43.3919011723755,-3.4657868293721,1.86275942558409));
#84555=CARTESIAN_POINT('Ctrl Pts',(43.38613529401,-3.40877835683801,1.96181525989395));
#84556=CARTESIAN_POINT('Ctrl Pts',(43.3803634192129,-3.3517105963015,2.06097411086577));
#84557=CARTESIAN_POINT('Ctrl Pts',(43.3745915444158,-3.290349407056,2.15757641132062));
#84558=CARTESIAN_POINT('Ctrl Pts',(43.3688196696187,-3.22497035933261,2.2512341462909));
#84559=CARTESIAN_POINT('Ctrl Pts',(43.363044419501,-3.15955307875467,2.34494665114055));
#84560=CARTESIAN_POINT('Ctrl Pts',(43.3572691693832,-3.09011352346045,2.43571082598991));
#84561=CARTESIAN_POINT('Ctrl Pts',(43.3514939192655,-3.01696736764411,2.52317199226897));
#84562=CARTESIAN_POINT('Ctrl Pts',(43.34570992324,-2.94371044094894,2.61076560775393));
#84563=CARTESIAN_POINT('Ctrl Pts',(43.3399259272145,-2.86673599811686,2.69504591777783));
#84564=CARTESIAN_POINT('Ctrl Pts',(43.334141931189,-2.78639634865771,2.7756952981527));
#84565=CARTESIAN_POINT('Ctrl Pts',(43.3312891000629,-2.74677055160925,2.81547386328625));
#84566=CARTESIAN_POINT('Ctrl Pts',(43.3284362689368,-2.70632659616591,2.85436973667235));
#84567=CARTESIAN_POINT('Ctrl Pts',(43.3255834378107,-2.66510952229929,2.89234856719408));
#84568=CARTESIAN_POINT('Ctrl Pts',(43.319710991677,-2.58026571789122,2.97052656883632));
#84569=CARTESIAN_POINT('Ctrl Pts',(43.3138385455433,-2.49183705363632,3.0450990959405));
#84570=CARTESIAN_POINT('Ctrl Pts',(43.3079660994096,-2.4001627782383,3.11571944147085));
#84571=CARTESIAN_POINT('Ctrl Pts',(43.302101260465,-2.30860725804554,3.18624830513682));
#84572=CARTESIAN_POINT('Ctrl Pts',(43.2962364215203,-2.21381481216261,3.25283491850321));
#84573=CARTESIAN_POINT('Ctrl Pts',(43.2903715825757,-2.11616060093259,3.31517017829562));
#84574=CARTESIAN_POINT('Ctrl Pts',(43.2845127724559,-2.01860677440873,3.37744135988128));
#84575=CARTESIAN_POINT('Ctrl Pts',(43.2786539623361,-1.91819738023632,3.43546965943753));
#84576=CARTESIAN_POINT('Ctrl Pts',(43.2727951522163,-1.81533910759,3.48898737808757));
#84577=CARTESIAN_POINT('Ctrl Pts',(43.2667093633352,-1.70849595698518,3.54457845041107));
#84578=CARTESIAN_POINT('Ctrl Pts',(43.2606235744542,-1.59901070407391,3.59530210325724));
#84579=CARTESIAN_POINT('Ctrl Pts',(43.2545377855731,-1.48737078546669,3.64090883524158));
#84580=CARTESIAN_POINT('Ctrl Pts',(43.2486857554951,-1.38001902312814,3.68476378528186));
#84581=CARTESIAN_POINT('Ctrl Pts',(43.242833725417,-1.27067548382995,3.72388748066768));
#84582=CARTESIAN_POINT('Ctrl Pts',(43.236981695339,-1.15979611141858,3.75810616932762));
#84583=CARTESIAN_POINT('Ctrl Pts',(43.2311305549607,-1.04893359629425,3.79231965562897));
#84584=CARTESIAN_POINT('Ctrl Pts',(43.2252794145824,-0.936536107192468,
3.82162949608052));
#84585=CARTESIAN_POINT('Ctrl Pts',(43.2194282742041,-0.823075679452457,
3.84591152080932));
#84586=CARTESIAN_POINT('Ctrl Pts',(43.2135766066368,-0.709605028903685,
3.87019573335374));
#84587=CARTESIAN_POINT('Ctrl Pts',(43.2077249390695,-0.595071653561087,
3.88945114312864));
#84588=CARTESIAN_POINT('Ctrl Pts',(43.2018732715022,-0.479958032240053,
3.90360465304675));
#84589=CARTESIAN_POINT('Ctrl Pts',(43.1960196598182,-0.364806166382434,
3.91776286522704));
#84590=CARTESIAN_POINT('Ctrl Pts',(43.1901660481342,-0.249074081271785,
3.92681575669156));
#84591=CARTESIAN_POINT('Ctrl Pts',(43.1843124364502,-0.13324891767699,3.93074213424614));
#84592=CARTESIAN_POINT('Ctrl Pts',(43.1784521703505,-0.0172920834444121,
3.93467297532679));
#84593=CARTESIAN_POINT('Ctrl Pts',(43.1725919042509,0.0987576271060678,
3.93346565629663));
#84594=CARTESIAN_POINT('Ctrl Pts',(43.1667316381512,0.214413430015104,3.92715111512521));
#84595=CARTESIAN_POINT('Ctrl Pts',(43.1608674249801,0.330147130703012,3.92083232091399));
#84596=CARTESIAN_POINT('Ctrl Pts',(43.155003211809,0.445485985130819,3.90939949575695));
#84597=CARTESIAN_POINT('Ctrl Pts',(43.1491389986379,0.559950423097398,3.89293520671396));
#84598=CARTESIAN_POINT('Ctrl Pts',(43.1432661500639,0.674583416763201,3.87644667302519));
#84599=CARTESIAN_POINT('Ctrl Pts',(43.1373933014898,0.788339019499037,3.85491196489894));
#84600=CARTESIAN_POINT('Ctrl Pts',(43.1315204529157,0.90074981497593,3.82846428360261));
#84601=CARTESIAN_POINT('Ctrl Pts',(43.1299257083008,0.931274441735608,3.82128253920871));
#84602=CARTESIAN_POINT('Ctrl Pts',(43.128330963686,0.961700006603048,3.81373880719636));
#84603=CARTESIAN_POINT('Ctrl Pts',(43.1267362190711,0.992017390206271,3.80583637293149));
#84604=CARTESIAN_POINT('Ctrl Pts',(43.1208637729372,1.10365733585567,3.77673665432205));
#84605=CARTESIAN_POINT('Ctrl Pts',(43.1149913268034,1.21420269460918,3.74267180265341));
#84606=CARTESIAN_POINT('Ctrl Pts',(43.1091188806696,1.32317837816996,3.70373972891502));
#84607=CARTESIAN_POINT('Ctrl Pts',(43.1032540417248,1.43201289421539,3.66485808793317));
#84608=CARTESIAN_POINT('Ctrl Pts',(43.0973892027801,1.53928139303118,3.62112190110369));
#84609=CARTESIAN_POINT('Ctrl Pts',(43.0915243638353,1.64452100114867,3.572679621346));
#84610=CARTESIAN_POINT('Ctrl Pts',(43.0856655537154,1.74965242706913,3.52428713835538));
#84611=CARTESIAN_POINT('Ctrl Pts',(43.0798067435955,1.85275873747101,3.47119835664669));
#84612=CARTESIAN_POINT('Ctrl Pts',(43.0739479334756,1.95339484067194,3.41361063925519));
#84613=CARTESIAN_POINT('Ctrl Pts',(43.0678621445946,2.05792973177641,3.35379189056561));
#84614=CARTESIAN_POINT('Ctrl Pts',(43.0617763557135,2.15979871799785,3.289118718314));
#84615=CARTESIAN_POINT('Ctrl Pts',(43.0556905668325,2.25852835458129,3.21986625056886));
#84616=CARTESIAN_POINT('Ctrl Pts',(43.0498385367544,2.3534657265786,3.15327381166631));
#84617=CARTESIAN_POINT('Ctrl Pts',(43.0439865066762,2.44550009918171,3.08244763439425));
#84618=CARTESIAN_POINT('Ctrl Pts',(43.038134476598,2.53423877709297,3.00767731325658));
#84619=CARTESIAN_POINT('Ctrl Pts',(43.0322833362196,2.62296396382608,2.93291835965049));
#84620=CARTESIAN_POINT('Ctrl Pts',(43.0264321958412,2.70839413610495,2.85421672073105));
#84621=CARTESIAN_POINT('Ctrl Pts',(43.0205810554628,2.7901696067844,2.77190233691171));
#84622=CARTESIAN_POINT('Ctrl Pts',(43.0147293878954,2.87195244545116,2.68958053654886));
#84623=CARTESIAN_POINT('Ctrl Pts',(43.008877720328,2.95007963657812,2.60364563746764));
#84624=CARTESIAN_POINT('Ctrl Pts',(43.0030260527606,3.02422880900815,2.51446398080489));
#84625=CARTESIAN_POINT('Ctrl Pts',(42.9971724410765,3.0984026162358,2.42525269505807));
#84626=CARTESIAN_POINT('Ctrl Pts',(42.9913188293923,3.16859551265873,2.33279282451787));
#84627=CARTESIAN_POINT('Ctrl Pts',(42.9854652177082,3.23452626837141,2.23748269696445));
#84628=CARTESIAN_POINT('Ctrl Pts',(42.9796049516084,3.30053197450387,2.14206422037132));
#84629=CARTESIAN_POINT('Ctrl Pts',(42.9737446855086,3.36226563372475,2.04378935960896));
#84630=CARTESIAN_POINT('Ctrl Pts',(42.9678844194089,3.4194900622587,1.94308433016017));
#84631=CARTESIAN_POINT('Ctrl Pts',(42.9620202062376,3.47675303322451,1.84231147274288));
#84632=CARTESIAN_POINT('Ctrl Pts',(42.9561559930664,3.52950053835556,1.73910555462318));
#84633=CARTESIAN_POINT('Ctrl Pts',(42.9502917798952,3.57754272528043,1.63391463938392));
#84634=CARTESIAN_POINT('Ctrl Pts',(42.944418931321,3.62565565718538,1.52856882426019));
#84635=CARTESIAN_POINT('Ctrl Pts',(42.9385460827468,3.66904928791142,1.42123256002071));
#84636=CARTESIAN_POINT('Ctrl Pts',(42.9326732341727,3.70758293075699,1.31237106473719));
#84637=CARTESIAN_POINT('Ctrl Pts',(42.9310784895589,3.71804656158268,1.2828102338979));
#84638=CARTESIAN_POINT('Ctrl Pts',(42.9294837449452,3.72815212141798,1.25313700439382));
#84639=CARTESIAN_POINT('Ctrl Pts',(42.9278890003315,3.73789744300419,1.22336082395291));
#84640=CARTESIAN_POINT('Ctrl Pts',(42.9220165541974,3.77378336202907,1.11371379068472));
#84641=CARTESIAN_POINT('Ctrl Pts',(42.9161441080634,3.80490071252197,1.00230283538655));
#84642=CARTESIAN_POINT('Ctrl Pts',(42.9102716619294,3.83107497297339,0.889580548043272));
#84643=CARTESIAN_POINT('Ctrl Pts',(42.9044068229844,3.85721532718824,0.777004281579848));
#84644=CARTESIAN_POINT('Ctrl Pts',(42.8985419840394,3.87842523261075,0.663120460123252));
#84645=CARTESIAN_POINT('Ctrl Pts',(42.8926771450945,3.8945792887361,0.548398726975031));
#84646=CARTESIAN_POINT('Ctrl Pts',(42.8868183349743,3.91071673912421,0.433794923276933));
#84647=CARTESIAN_POINT('Ctrl Pts',(42.8809595248542,3.92180862047035,0.318355328002071));
#84648=CARTESIAN_POINT('Ctrl Pts',(42.875100714734,3.9277802906891,0.202561072455336));
#84649=CARTESIAN_POINT('Ctrl Pts',(42.8690149258531,3.93398331203176,0.0822807803089556));
#84650=CARTESIAN_POINT('Ctrl Pts',(42.8629291369722,3.93466126693419,-0.0383817654108247));
#84651=CARTESIAN_POINT('Ctrl Pts',(42.8568433480912,3.92978959915348,-0.15887953419208));
#84652=CARTESIAN_POINT('Ctrl Pts',(42.8509913180129,3.92510505505535,-0.274748911372842));
#84653=CARTESIAN_POINT('Ctrl Pts',(42.8451392879345,3.91528937100348,-0.390465485271834));
#84654=CARTESIAN_POINT('Ctrl Pts',(42.8392872578561,3.90037382210772,-0.505542330390647));
#84655=CARTESIAN_POINT('Ctrl Pts',(42.8334361174774,3.88546054086267,-0.620601680069629));
#84656=CARTESIAN_POINT('Ctrl Pts',(42.8275849770988,3.86544898953233,-0.735021084536224));
#84657=CARTESIAN_POINT('Ctrl Pts',(42.8217338367201,3.84042223041134,-0.848319569597698));
#84658=CARTESIAN_POINT('Ctrl Pts',(42.8158821691525,3.81539321637405,-0.961628262876645));
#84659=CARTESIAN_POINT('Ctrl Pts',(42.8100305015849,3.78534818543122,-1.07381543233026));
#84660=CARTESIAN_POINT('Ctrl Pts',(42.8041788340173,3.75042099762731,-1.18441181206375));
#84661=CARTESIAN_POINT('Ctrl Pts',(42.7983252223329,3.71548220586098,-1.29504493555809));
#84662=CARTESIAN_POINT('Ctrl Pts',(42.7924716106485,3.67565815637435,-1.4040858244576));
#84663=CARTESIAN_POINT('Ctrl Pts',(42.7866179989641,3.63113186215738,-1.5110825257495));
#84664=CARTESIAN_POINT('Ctrl Pts',(42.7807577328641,3.58655495022188,-1.61820086143755));
#84665=CARTESIAN_POINT('Ctrl Pts',(42.7748974667641,3.53726528295333,-1.72326998934912));
#84666=CARTESIAN_POINT('Ctrl Pts',(42.7690372006641,3.4834931489193,-1.82585992930244));
#84667=CARTESIAN_POINT('Ctrl Pts',(42.7631729874927,3.42968479768131,-1.92851896676967));
#84668=CARTESIAN_POINT('Ctrl Pts',(42.7573087743213,3.37138817547999,-2.02869513495938));
#84669=CARTESIAN_POINT('Ctrl Pts',(42.7514445611499,3.30887754227419,-2.12598645579729));
#84670=CARTESIAN_POINT('Ctrl Pts',(42.7455717125754,3.24627485843956,-2.22342104389715));
#84671=CARTESIAN_POINT('Ctrl Pts',(42.739698864001,3.17944601659607,-2.31796196999404));
#84672=CARTESIAN_POINT('Ctrl Pts',(42.7338260154266,3.10870629159263,-2.40923933900565));
#84673=CARTESIAN_POINT('Ctrl Pts',(42.732231270815,3.08949724953285,-2.43402528241107));
#84674=CARTESIAN_POINT('Ctrl Pts',(42.7306365262034,3.07000004406421,-2.45857078841704));
#84675=CARTESIAN_POINT('Ctrl Pts',(42.7290417815917,3.0502214508407,-2.48286892542301));
#84676=CARTESIAN_POINT('Ctrl Pts',(42.7231693354579,2.97738927290907,-2.57234375398275));
#84677=CARTESIAN_POINT('Ctrl Pts',(42.717296889324,2.90049485421054,-2.65876099088872));
#84678=CARTESIAN_POINT('Ctrl Pts',(42.7114244431901,2.81982455190766,-2.74172910705247));
#84679=CARTESIAN_POINT('Ctrl Pts',(42.7055596042453,2.73925875022137,-2.82458974600282));
#84680=CARTESIAN_POINT('Ctrl Pts',(42.6996947653005,2.65492707747333,-2.90400985585174));
#84681=CARTESIAN_POINT('Ctrl Pts',(42.6938299263556,2.56715679645829,-2.97963000763484));
#84682=CARTESIAN_POINT('Ctrl Pts',(42.6879711162357,2.47947673985589,-3.05517242486246));
#84683=CARTESIAN_POINT('Ctrl Pts',(42.6821123061157,2.38836541708526,-3.12692238549876));
#84684=CARTESIAN_POINT('Ctrl Pts',(42.6762534959957,2.29418720034906,-3.19455694733316));
#84685=CARTESIAN_POINT('Ctrl Pts',(42.6701677071147,2.1963603835543,-3.26481176972059));
#84686=CARTESIAN_POINT('Ctrl Pts',(42.6640819182337,2.09522455164948,-3.3306255453884));
#84687=CARTESIAN_POINT('Ctrl Pts',(42.6579961293527,1.99122659376556,-3.39168183240716));
#84688=CARTESIAN_POINT('Ctrl Pts',(42.6521440992745,1.89122325984881,-3.45039291080419));
#84689=CARTESIAN_POINT('Ctrl Pts',(42.6462920691963,1.78857400550308,-3.50470500623368));
#84690=CARTESIAN_POINT('Ctrl Pts',(42.640440039118,1.68370534757026,-3.5543811419941));
#84691=CARTESIAN_POINT('Ctrl Pts',(42.6345888987396,1.57885263309941,-3.60404972535902));
#84692=CARTESIAN_POINT('Ctrl Pts',(42.6287377583611,1.47178155940849,-3.64908357355293));
#84693=CARTESIAN_POINT('Ctrl Pts',(42.6228866179826,1.36294163890904,-3.68929249164768));
#84694=CARTESIAN_POINT('Ctrl Pts',(42.6170349504151,1.25409191190956,-3.72950503257452));
#84695=CARTESIAN_POINT('Ctrl Pts',(42.6111832828477,1.14347340904853,-3.76489163595134));
#84696=CARTESIAN_POINT('Ctrl Pts',(42.6053316152802,1.03155326047639,-3.79531116916657));
#84697=CARTESIAN_POINT('Ctrl Pts',(42.599478003596,0.919595928344136,-3.82574080875278));
#84698=CARTESIAN_POINT('Ctrl Pts',(42.5936243919118,0.806336489275951,-3.85119998844847));
#84699=CARTESIAN_POINT('Ctrl Pts',(42.5877707802276,0.692254087172466,-3.87159828479054));
#84700=CARTESIAN_POINT('Ctrl Pts',(42.5819105141277,0.578041995611775,-3.89201977002003));
#84701=CARTESIAN_POINT('Ctrl Pts',(42.5760502480279,0.463005480836088,-3.90736881582649));
#84702=CARTESIAN_POINT('Ctrl Pts',(42.570189981928,0.347630765393659,-3.91760664831882));
#84703=CARTESIAN_POINT('Ctrl Pts',(42.5643257687568,0.232178341493546,-3.92785137630961));
#84704=CARTESIAN_POINT('Ctrl Pts',(42.5584615555855,0.11638767529605,-3.93297801791629));
#84705=CARTESIAN_POINT('Ctrl Pts',(42.5525973424143,0.000745209508502876,
-3.9329999294003));
#84706=CARTESIAN_POINT('Ctrl Pts',(42.54672449384,-0.115067546694507,-3.93302187315028));
#84707=CARTESIAN_POINT('Ctrl Pts',(42.5408516452657,-0.230731255534072,
-3.9279241024371));
#84708=CARTESIAN_POINT('Ctrl Pts',(42.5349787966914,-0.345764285630725,
-3.91777182321562));
#84709=CARTESIAN_POINT('Ctrl Pts',(42.5333840520783,-0.377000967924689,
-3.91501501918869));
#84710=CARTESIAN_POINT('Ctrl Pts',(42.5317893074653,-0.408191205040602,
-3.91188580256903));
#84711=CARTESIAN_POINT('Ctrl Pts',(42.5301945628522,-0.439325502388764,
-3.90838612510981));
#84712=CARTESIAN_POINT('Ctrl Pts',(42.5243221167183,-0.553973630115394,
-3.89549900375098));
#84713=CARTESIAN_POINT('Ctrl Pts',(42.5184496705844,-0.668246179663863,
-3.87754141813316));
#84714=CARTESIAN_POINT('Ctrl Pts',(42.5125772244505,-0.781658957024931,
-3.85454255066703));
#84715=CARTESIAN_POINT('Ctrl Pts',(42.5067123855056,-0.894924819042929,
-3.83157347602127));
#84716=CARTESIAN_POINT('Ctrl Pts',(42.5008475465607,-1.00733272235404,-3.80357618775543));
#84717=CARTESIAN_POINT('Ctrl Pts',(42.4949827076159,-1.11840335776539,-3.77063163532837));
#84718=CARTESIAN_POINT('Ctrl Pts',(42.4891238974959,-1.22935981691158,-3.73772094861154));
#84719=CARTESIAN_POINT('Ctrl Pts',(42.4832650873759,-1.33898134851726,-3.69987323009655));
#84720=CARTESIAN_POINT('Ctrl Pts',(42.4774062772559,-1.44679927093527,-3.65722037476841));
#84721=CARTESIAN_POINT('Ctrl Pts',(42.4713204883749,-1.55879421529793,-3.61291508625743));
#84722=CARTESIAN_POINT('Ctrl Pts',(42.465234699494,-1.66884252992364,-3.5634249053048));
#84723=CARTESIAN_POINT('Ctrl Pts',(42.459148910613,-1.77643638351166,-3.50895465563977));
#84724=CARTESIAN_POINT('Ctrl Pts',(42.4532968805348,-1.87989749262114,-3.45657664094951));
#84725=CARTESIAN_POINT('Ctrl Pts',(42.4474448504565,-1.98108881431325,-3.39959427927564));
#84726=CARTESIAN_POINT('Ctrl Pts',(42.4415928203783,-2.07958037965062,-3.33823822465866));
#84727=CARTESIAN_POINT('Ctrl Pts',(42.4357416799998,-2.17805697105231,-3.27689149816649));
#84728=CARTESIAN_POINT('Ctrl Pts',(42.4298905396213,-2.273834271458,-3.21117261936068));
#84729=CARTESIAN_POINT('Ctrl Pts',(42.4240393992428,-2.36650923123514,-3.14135688174376));
#84730=CARTESIAN_POINT('Ctrl Pts',(42.4181877316753,-2.45919254104573,-3.07153485371413));
#84731=CARTESIAN_POINT('Ctrl Pts',(42.4123360641078,-2.54877262438937,-2.99761548181562));
#84732=CARTESIAN_POINT('Ctrl Pts',(42.4064843965404,-2.63487817719977,-2.91991540824669));
#84733=CARTESIAN_POINT('Ctrl Pts',(42.4006307848562,-2.72101233711132,-2.8421895201537));
#84734=CARTESIAN_POINT('Ctrl Pts',(42.394777173172,-2.80366936440841,-2.76068070954268));
#84735=CARTESIAN_POINT('Ctrl Pts',(42.3889235614878,-2.8825141160547,-2.67574314364167));
#84736=CARTESIAN_POINT('Ctrl Pts',(42.3830632953879,-2.96144849881741,-2.59070902028187));
#84737=CARTESIAN_POINT('Ctrl Pts',(42.377203029288,-3.0365616743948,-2.50223866483081));
#84738=CARTESIAN_POINT('Ctrl Pts',(42.3713427631882,-3.1075581203337,-2.41072012659041));
#84739=CARTESIAN_POINT('Ctrl Pts',(42.3654785500169,-3.1786023845863,-2.31913994776909));
#84740=CARTESIAN_POINT('Ctrl Pts',(42.3596143368456,-3.24552416002274,-2.22450783479905));
#84741=CARTESIAN_POINT('Ctrl Pts',(42.3537501236743,-3.30807165749659,-2.12724020948922));
#84742=CARTESIAN_POINT('Ctrl Pts',(42.3478772751,-3.37071125988378,-2.02982935181101));
#84743=CARTESIAN_POINT('Ctrl Pts',(42.3420044265258,-3.42896352139119,-1.92977559207154));
#84744=CARTESIAN_POINT('Ctrl Pts',(42.3361315779515,-3.48262287083093,-1.82751934040801));
#84745=CARTESIAN_POINT('Ctrl Pts',(42.3345368333385,-3.49719381666281,-1.79975213265173));
#84746=CARTESIAN_POINT('Ctrl Pts',(42.3329420887256,-3.51142637231868,-1.77182262769116));
#84747=CARTESIAN_POINT('Ctrl Pts',(42.3313473441126,-3.52531704580881,-1.74373986779274));
#84748=CARTESIAN_POINT('Ctrl Pts',(42.3250482766907,-3.5801836922543,-1.63281602672377));
#84749=CARTESIAN_POINT('Ctrl Pts',(42.3187492092687,-3.62987581658613,-1.5191699993202));
#84750=CARTESIAN_POINT('Ctrl Pts',(42.3124501418468,-3.67413461259416,-1.40329036501273));
#84751=CARTESIAN_POINT('Ctrl Pts',(42.3061711023168,-3.71825268771015,-1.28777917013381));
#84752=CARTESIAN_POINT('Ctrl Pts',(42.2998920627869,-3.7569717656237,-1.17004882670027));
#84753=CARTESIAN_POINT('Ctrl Pts',(42.2936130232569,-3.7900804902256,-1.05060881283725));
#84754=CARTESIAN_POINT('Ctrl Pts',(42.2873460973,-3.82312534121277,-0.931399223598544));
#84755=CARTESIAN_POINT('Ctrl Pts',(42.281079171343,-3.85058131694735,-0.810486841434601));
#84756=CARTESIAN_POINT('Ctrl Pts',(42.274812245386,-3.87228552257363,-0.688399470995369));
#84757=CARTESIAN_POINT('Ctrl Pts',(42.2685636294963,-3.89392631505821,-0.566668803024465));
#84758=CARTESIAN_POINT('Ctrl Pts',(42.2623150136065,-3.90984878548117,-0.443770304983643));
#84759=CARTESIAN_POINT('Ctrl Pts',(42.2560663977168,-3.91994041182175,-0.320243919172191));
#84760=CARTESIAN_POINT('Ctrl Pts',(42.2506987869713,-3.9286091991085,-0.214133771336548));
#84761=CARTESIAN_POINT('Ctrl Pts',(42.2453311762258,-3.932976188352,-0.107560690645611));
#84762=CARTESIAN_POINT('Ctrl Pts',(42.2399635654804,-3.93299990283659,-0.000874235302823624));
#84763=CARTESIAN_POINT('',(40.9899634959417,-3.93299833106861,0.00362323219413291));
#84764=CARTESIAN_POINT('Ctrl Pts',(42.2399635220349,-3.92667249913085,-0.00087196670281342));
#84765=CARTESIAN_POINT('Ctrl Pts',(42.2041423898142,-3.92526855652312,0.709962603038024));
#84766=CARTESIAN_POINT('Ctrl Pts',(42.1020388513469,-3.40040452164114,2.73803753544301));
#84767=CARTESIAN_POINT('Ctrl Pts',(41.9336529066332,-0.144695732084588,
4.64941428208763));
#84768=CARTESIAN_POINT('Ctrl Pts',(41.7348056878936,3.83289027569088,2.63570524829183));
#84769=CARTESIAN_POINT('Ctrl Pts',(41.5359584691537,4.28966176770655,-1.79910865154202));
#84770=CARTESIAN_POINT('Ctrl Pts',(41.3371112504143,0.806037805343487,-4.58129818694668));
#84771=CARTESIAN_POINT('Ctrl Pts',(41.155112934708,-3.06008131386444,-3.27603838467406));
#84772=CARTESIAN_POINT('Ctrl Pts',(41.0393970252482,-3.92331410043244,-0.973892289700984));
#84773=CARTESIAN_POINT('Ctrl Pts',(40.9899635220349,-3.93215931941742,0.00362194329329435));
#84774=CARTESIAN_POINT('',(39.7399635219896,-3.93299992292088,-0.000778655457619776));
#84775=CARTESIAN_POINT('Ctrl Pts',(40.9899634959417,-3.93299833106861,0.00362323219413291));
#84776=CARTESIAN_POINT('Ctrl Pts',(40.9824898564729,-3.93286215684296,0.151439594361313));
#84777=CARTESIAN_POINT('Ctrl Pts',(40.975016217004,-3.92438925053041,0.298883036488164));
#84778=CARTESIAN_POINT('Ctrl Pts',(40.9675425775351,-3.90772648188647,0.445154740245648));
#84779=CARTESIAN_POINT('Ctrl Pts',(40.9599054571219,-3.89069922614583,0.5946260412473));
#84780=CARTESIAN_POINT('Ctrl Pts',(40.9522683367088,-3.86511989035994,0.742874037455968));
#84781=CARTESIAN_POINT('Ctrl Pts',(40.9446312162956,-3.83119322941646,0.889071110133193));
#84782=CARTESIAN_POINT('Ctrl Pts',(40.9428930818421,-3.82347185079602,0.92234414437671));
#84783=CARTESIAN_POINT('Ctrl Pts',(40.9411549473885,-3.81531829668762,0.955511036363426));
#84784=CARTESIAN_POINT('Ctrl Pts',(40.939416812935,-3.80673532218173,0.98856218158188));
#84785=CARTESIAN_POINT('Ctrl Pts',(40.9335443668011,-3.77773695824565,1.10022849690089));
#84786=CARTESIAN_POINT('Ctrl Pts',(40.9276719206673,-3.74377246966985,1.21080473294224));
#84787=CARTESIAN_POINT('Ctrl Pts',(40.9217994745335,-3.70493933613558,1.31981571272478));
#84788=CARTESIAN_POINT('Ctrl Pts',(40.9159346355887,-3.66615650719029,1.42868547926923));
#84789=CARTESIAN_POINT('Ctrl Pts',(40.9100697966439,-3.62251771282398,1.53599363600944));
#84790=CARTESIAN_POINT('Ctrl Pts',(40.9042049576991,-3.57417098571519,1.6412771749073));
#84791=CARTESIAN_POINT('Ctrl Pts',(40.8983461475792,-3.52587395714903,1.74645248644917));
#84792=CARTESIAN_POINT('Ctrl Pts',(40.8924873374592,-3.47287879347344,1.84960694643604));
#84793=CARTESIAN_POINT('Ctrl Pts',(40.8866285273392,-3.41538245360437,1.95029528420991));
#84794=CARTESIAN_POINT('Ctrl Pts',(40.8805427384583,-3.3556586225349,2.05488443352908));
#84795=CARTESIAN_POINT('Ctrl Pts',(40.8744569495773,-3.29107794989201,2.15681208573282));
#84796=CARTESIAN_POINT('Ctrl Pts',(40.8683711606963,-3.22191513385494,2.25560454650999));
#84797=CARTESIAN_POINT('Ctrl Pts',(40.8625191306181,-3.15540890308403,2.35060232958681));
#84798=CARTESIAN_POINT('Ctrl Pts',(40.8566671005399,-3.08466630045064,2.44270095769923));
#84799=CARTESIAN_POINT('Ctrl Pts',(40.8508150704616,-3.00997656386486,2.53150747282805));
#84800=CARTESIAN_POINT('Ctrl Pts',(40.8449639300832,-2.93529818255913,2.6203004864653));
#84801=CARTESIAN_POINT('Ctrl Pts',(40.8391127897047,-2.85667412647018,2.70580206603224));
#84802=CARTESIAN_POINT('Ctrl Pts',(40.8332616493263,-2.77443400936456,2.787652225024));
#84803=CARTESIAN_POINT('Ctrl Pts',(40.8274099817588,-2.69218648240703,2.86950975873237));
#84804=CARTESIAN_POINT('Ctrl Pts',(40.8215583141914,-2.60632253975584,2.94771492624675));
#84805=CARTESIAN_POINT('Ctrl Pts',(40.815706646624,-2.5172082297601,3.02194502399167));
#84806=CARTESIAN_POINT('Ctrl Pts',(40.8098530349398,-2.42806431305464,3.09619978342063));
#84807=CARTESIAN_POINT('Ctrl Pts',(40.8039994232556,-2.33566819916816,3.16647658263216));
#84808=CARTESIAN_POINT('Ctrl Pts',(40.7981458115714,-2.2404179604264,3.23249383024915));
#84809=CARTESIAN_POINT('Ctrl Pts',(40.7922855454716,-2.14505944072703,3.29858612661021));
#84810=CARTESIAN_POINT('Ctrl Pts',(40.7864252793717,-2.04684066002644,3.36040897074151));
#84811=CARTESIAN_POINT('Ctrl Pts',(40.7805650132719,-1.94618761832499,3.41772479206247));
#84812=CARTESIAN_POINT('Ctrl Pts',(40.7747008001006,-1.84546678367061,3.47507921737108));
#84813=CARTESIAN_POINT('Ctrl Pts',(40.7688365869294,-1.74230879034057,3.52792038734939));
#84814=CARTESIAN_POINT('Ctrl Pts',(40.7629723737581,-1.63716152939203,3.57605804296837));
#84815=CARTESIAN_POINT('Ctrl Pts',(40.7570995251839,-1.53185943284241,3.62426658415084));
#84816=CARTESIAN_POINT('Ctrl Pts',(40.7512266766097,-1.42456260398709,3.66775763295613));
#84817=CARTESIAN_POINT('Ctrl Pts',(40.7453538280354,-1.31573613299586,3.70639008043259));
#84818=CARTESIAN_POINT('Ctrl Pts',(40.7437590834221,-1.28618481284678,3.71688054119201));
#84819=CARTESIAN_POINT('Ctrl Pts',(40.7421643388087,-1.25652076903543,3.72701303314016));
#84820=CARTESIAN_POINT('Ctrl Pts',(40.7405695941953,-1.22675344731855,3.73678538044294));
#84821=CARTESIAN_POINT('Ctrl Pts',(40.7346971480614,-1.11713903516171,3.77277081827219));
#84822=CARTESIAN_POINT('Ctrl Pts',(40.7288247019275,-1.0057563729685,3.80398929075869));
#84823=CARTESIAN_POINT('Ctrl Pts',(40.7229522557935,-0.893057892113009,
3.83026586562012));
#84824=CARTESIAN_POINT('Ctrl Pts',(40.7170874168487,-0.780505401298543,
3.85650840170647));
#84825=CARTESIAN_POINT('Ctrl Pts',(40.7112225779038,-0.666640880347451,
3.877821677983));
#84826=CARTESIAN_POINT('Ctrl Pts',(40.705357738959,-0.551933858533738,3.89407986767144));
#84827=CARTESIAN_POINT('Ctrl Pts',(40.6994989288389,-0.437344751047511,
3.91032134457742));
#84828=CARTESIAN_POINT('Ctrl Pts',(40.6936401187189,-0.321915272144686,
3.92151801322171));
#84829=CARTESIAN_POINT('Ctrl Pts',(40.6877813085989,-0.206126485174543,
3.92759479479612));
#84830=CARTESIAN_POINT('Ctrl Pts',(40.6816955197179,-0.085851873462126,
3.93390699966024));
#84831=CARTESIAN_POINT('Ctrl Pts',(40.6756097308369,0.0348100071207318,
3.93469448735638));
#84832=CARTESIAN_POINT('Ctrl Pts',(40.669523941956,0.155312148578736,3.92993220507732));
#84833=CARTESIAN_POINT('Ctrl Pts',(40.6636719118777,0.271185730476043,3.92535284491819));
#84834=CARTESIAN_POINT('Ctrl Pts',(40.6578198817994,0.386911167016915,3.91564220821036));
#84835=CARTESIAN_POINT('Ctrl Pts',(40.6519678517212,0.502001504513165,3.90083112803753));
#84836=CARTESIAN_POINT('Ctrl Pts',(40.6461167113426,0.617074344518227,3.88602229963274));
#84837=CARTESIAN_POINT('Ctrl Pts',(40.6402655709641,0.731511867598882,3.86611462232444));
#84838=CARTESIAN_POINT('Ctrl Pts',(40.6344144305856,0.844833024359663,3.84119072176211));
#84839=CARTESIAN_POINT('Ctrl Pts',(40.6285627630181,0.958164391380532,3.81626457555109));
#84840=CARTESIAN_POINT('Ctrl Pts',(40.6227110954506,1.07037878839605,3.78632139642283));
#84841=CARTESIAN_POINT('Ctrl Pts',(40.6168594278831,1.18100682819149,3.75149461838413));
#84842=CARTESIAN_POINT('Ctrl Pts',(40.6110058161989,1.29167162226623,3.71665626974244));
#84843=CARTESIAN_POINT('Ctrl Pts',(40.6051522045146,1.40074861706163,3.67693122002077));
#84844=CARTESIAN_POINT('Ctrl Pts',(40.5992985928304,1.50778569361863,3.63250207186713));
#84845=CARTESIAN_POINT('Ctrl Pts',(40.5934383267305,1.61494445047091,3.58802241643096));
#84846=CARTESIAN_POINT('Ctrl Pts',(40.5875780606306,1.72005827845911,3.53882814740728));
#84847=CARTESIAN_POINT('Ctrl Pts',(40.5817177945307,1.82269698853103,3.4851491629484));
#84848=CARTESIAN_POINT('Ctrl Pts',(40.5758535813594,1.92540482896517,3.43143402402463));
#84849=CARTESIAN_POINT('Ctrl Pts',(40.5699893681881,2.02563387543411,3.37322836212841));
#84850=CARTESIAN_POINT('Ctrl Pts',(40.5641251550168,2.12298190106599,3.31080607220451));
#84851=CARTESIAN_POINT('Ctrl Pts',(40.5582523064425,2.22047327746065,3.24829186174274));
#84852=CARTESIAN_POINT('Ctrl Pts',(40.5523794578682,2.31507482939733,3.18154886825232));
#84853=CARTESIAN_POINT('Ctrl Pts',(40.5465066092939,2.4064163757511,3.11089203067495));
#84854=CARTESIAN_POINT('Ctrl Pts',(40.5449118646811,2.43121974623194,3.09170549629499));
#84855=CARTESIAN_POINT('Ctrl Pts',(40.5433171200684,2.45578294099633,3.07223058036415));
#84856=CARTESIAN_POINT('Ctrl Pts',(40.5417223754557,2.48009902229586,3.05247405224141));
#84857=CARTESIAN_POINT('Ctrl Pts',(40.5358499293217,2.56963992839446,2.97972312631378));
#84858=CARTESIAN_POINT('Ctrl Pts',(40.5299774831878,2.65612693165349,2.90290718572238));
#84859=CARTESIAN_POINT('Ctrl Pts',(40.5241050370539,2.73916824320118,2.8223122320959));
#84860=CARTESIAN_POINT('Ctrl Pts',(40.518240198109,2.82210198271784,2.74182168147909));
#84861=CARTESIAN_POINT('Ctrl Pts',(40.5123753591642,2.90159861307141,2.65756213816487));
#84862=CARTESIAN_POINT('Ctrl Pts',(40.5065105202193,2.97729840836829,2.56986053853661));
#84863=CARTESIAN_POINT('Ctrl Pts',(40.5006517100993,3.05292038723931,2.48224909271918));
#84864=CARTESIAN_POINT('Ctrl Pts',(40.4947928999793,3.12475302586017,2.39120293949301));
#84865=CARTESIAN_POINT('Ctrl Pts',(40.4889340898592,3.19247305138952,2.29708615775545));
#84866=CARTESIAN_POINT('Ctrl Pts',(40.4828483009783,3.26281664845811,2.19932315604083));
#84867=CARTESIAN_POINT('Ctrl Pts',(40.4767625120973,3.32872220444049,2.0982471091588));
#84868=CARTESIAN_POINT('Ctrl Pts',(40.4706767232163,3.38987287186793,1.99430461880173));
#84869=CARTESIAN_POINT('Ctrl Pts',(40.464824693138,3.44867470546611,1.89435462186979));
#84870=CARTESIAN_POINT('Ctrl Pts',(40.4589726630598,3.50307995977951,1.79175471236219));
#84871=CARTESIAN_POINT('Ctrl Pts',(40.4531206329815,3.55285127102775,1.68693119182629));
#84872=CARTESIAN_POINT('Ctrl Pts',(40.4472694926029,3.60261501541071,1.58212360788999));
#84873=CARTESIAN_POINT('Ctrl Pts',(40.4414183522244,3.64774604027802,1.47509345840352));
#84874=CARTESIAN_POINT('Ctrl Pts',(40.4355672118459,3.68805374272889,1.36629008294119));
#84875=CARTESIAN_POINT('Ctrl Pts',(40.4297155442784,3.72836507691226,1.25747690427175));
#84876=CARTESIAN_POINT('Ctrl Pts',(40.4238638767109,3.76385208116434,1.14689056965885));
#84877=CARTESIAN_POINT('Ctrl Pts',(40.4180122091434,3.79437319888796,1.03499808094545));
#84878=CARTESIAN_POINT('Ctrl Pts',(40.4121585974591,3.82490445673235,0.923068417861169));
#84879=CARTESIAN_POINT('Ctrl Pts',(40.4063049857749,3.8504664387394,0.809832136374644));
#84880=CARTESIAN_POINT('Ctrl Pts',(40.4004513740906,3.87096828653383,0.695768298105991));
#84881=CARTESIAN_POINT('Ctrl Pts',(40.3945911079907,3.89149344093353,0.581574791483559));
#84882=CARTESIAN_POINT('Ctrl Pts',(40.3887308418908,3.90694690638146,0.466552257409715));
#84883=CARTESIAN_POINT('Ctrl Pts',(40.3828705757909,3.91728946762736,0.351186883034859));
#84884=CARTESIAN_POINT('Ctrl Pts',(40.3770063626196,3.92763899490981,0.235743806493633));
#84885=CARTESIAN_POINT('Ctrl Pts',(40.3711421494482,3.93287074496085,0.119957841781663));
#84886=CARTESIAN_POINT('Ctrl Pts',(40.3652779362769,3.93299763246142,0.00431544353016689));
#84887=CARTESIAN_POINT('Ctrl Pts',(40.3594050877026,3.93312470681139,-0.111497245036857));
#84888=CARTESIAN_POINT('Ctrl Pts',(40.3535322391283,3.92813193350777,-0.227165533792494));
#84889=CARTESIAN_POINT('Ctrl Pts',(40.347659390554,3.91808408127113,-0.342207732364104));
#84890=CARTESIAN_POINT('Ctrl Pts',(40.3460646459413,3.91535563390519,-0.373446904305652));
#84891=CARTESIAN_POINT('Ctrl Pts',(40.3444699013287,3.91225473193894,-0.404639969150923));
#84892=CARTESIAN_POINT('Ctrl Pts',(40.342875156716,3.90878331850588,-0.435777430542405));
#84893=CARTESIAN_POINT('Ctrl Pts',(40.3370027105821,3.89600027585911,-0.550437209492545));
#84894=CARTESIAN_POINT('Ctrl Pts',(40.3311302644482,3.87814643010622,-0.66472601320237));
#84895=CARTESIAN_POINT('Ctrl Pts',(40.3252578183143,3.85525052411216,-0.778159621371421));
#84896=CARTESIAN_POINT('Ctrl Pts',(40.3193929793694,3.83238427756186,-0.891446287212729));
#84897=CARTESIAN_POINT('Ctrl Pts',(40.3135281404246,3.80448904063948,-1.00387955913017));
#84898=CARTESIAN_POINT('Ctrl Pts',(40.3076633014797,3.77164532767107,-1.11498005464538));
#84899=CARTESIAN_POINT('Ctrl Pts',(40.3018044913597,3.73883537675374,-1.22596634320083));
#84900=CARTESIAN_POINT('Ctrl Pts',(40.2959456812397,3.70108718427368,-1.33562218642375));
#84901=CARTESIAN_POINT('Ctrl Pts',(40.2900868711197,3.65853221970939,-1.44347878313062));
#84902=CARTESIAN_POINT('Ctrl Pts',(40.2840010822387,3.61432861439189,-1.55551390007959));
#84903=CARTESIAN_POINT('Ctrl Pts',(40.2779152933577,3.5649383516893,-1.66560709475051));
#84904=CARTESIAN_POINT('Ctrl Pts',(40.2718295044768,3.51056579425569,-1.77325035012035));
#84905=CARTESIAN_POINT('Ctrl Pts',(40.2659774743985,3.45828171937946,-1.87675896345987));
#84906=CARTESIAN_POINT('Ctrl Pts',(40.2601254443202,3.40139123898617,-1.97800196997601));
#84907=CARTESIAN_POINT('Ctrl Pts',(40.254273414242,3.34012461671111,-2.07654919152918));
#84908=CARTESIAN_POINT('Ctrl Pts',(40.2484222738635,3.27886730896415,-2.17508143068523));
#84909=CARTESIAN_POINT('Ctrl Pts',(40.2425711334849,3.21323540038668,-2.27091834883834));
#84910=CARTESIAN_POINT('Ctrl Pts',(40.2367199931064,3.143503818494,-2.36365664662058));
#84911=CARTESIAN_POINT('Ctrl Pts',(40.2308683255389,3.07376595377106,-2.45640330014304));
#84912=CARTESIAN_POINT('Ctrl Pts',(40.2250166579714,2.99992792987121,-2.54605044789692));
#84913=CARTESIAN_POINT('Ctrl Pts',(40.2191649904039,2.92230605180612,-2.63222649853262));
#84914=CARTESIAN_POINT('Ctrl Pts',(40.2133113787197,2.84465838519605,-2.71843117969123));
#84915=CARTESIAN_POINT('Ctrl Pts',(40.2074577670355,2.76322464121197,-2.80116216366751));
#84916=CARTESIAN_POINT('Ctrl Pts',(40.2016041553512,2.67835868270532,-2.88008398606308));
#84917=CARTESIAN_POINT('Ctrl Pts',(40.1957438892513,2.59339624814367,-2.95909552718937));
#84918=CARTESIAN_POINT('Ctrl Pts',(40.1898836231515,2.50499411415356,-3.03428898199129));
#84919=CARTESIAN_POINT('Ctrl Pts',(40.1840233570516,2.41354006161249,-3.10536847588037));
#84920=CARTESIAN_POINT('Ctrl Pts',(40.1781591438803,2.32202441192372,-3.17649584401845));
#84921=CARTESIAN_POINT('Ctrl Pts',(40.172294930709,2.22745308709818,-3.24350349547377));
#84922=CARTESIAN_POINT('Ctrl Pts',(40.1664307175377,2.1302422802082,-3.30613926319104));
#84923=CARTESIAN_POINT('Ctrl Pts',(40.1605578689634,2.03288832461819,-3.36886726580493));
#84924=CARTESIAN_POINT('Ctrl Pts',(40.1546850203891,1.93288748538726,-3.42721032847708));
#84925=CARTESIAN_POINT('Ctrl Pts',(40.1488121718148,1.83067998586112,-3.48096248031597));
#84926=CARTESIAN_POINT('Ctrl Pts',(40.147217427202,1.80292601652283,-3.49555862620468));
#84927=CARTESIAN_POINT('Ctrl Pts',(40.1456226825891,1.77500944286886,-3.50981652938437));
#84928=CARTESIAN_POINT('Ctrl Pts',(40.1440279379763,1.746939303992,-3.5237326896585));
#84929=CARTESIAN_POINT('Ctrl Pts',(40.1381554918424,1.64357455379922,-3.57497719673732));
#84930=CARTESIAN_POINT('Ctrl Pts',(40.1322830457085,1.53778003612507,-3.62175550893053));
#84931=CARTESIAN_POINT('Ctrl Pts',(40.1264105995746,1.42997862296408,-3.66382998211786));
#84932=CARTESIAN_POINT('Ctrl Pts',(40.1205457606298,1.32231685616405,-3.70584995187246));
#84933=CARTESIAN_POINT('Ctrl Pts',(40.114680921685,1.212653745353,-3.74317805126427));
#84934=CARTESIAN_POINT('Ctrl Pts',(40.1088160827401,1.10143608626553,-3.77562280264754));
#84935=CARTESIAN_POINT('Ctrl Pts',(40.1029572726201,0.990332754577357,-3.80803420209663));
#84936=CARTESIAN_POINT('Ctrl Pts',(40.0970984625001,0.877678447586047,-3.83557212330901));
#84937=CARTESIAN_POINT('Ctrl Pts',(40.0912396523801,0.763938611919312,-3.85809367398185));
#84938=CARTESIAN_POINT('Ctrl Pts',(40.0851538634991,0.645792330840744,-3.88148774203657));
#84939=CARTESIAN_POINT('Ctrl Pts',(40.0790680746182,0.526475133337671,-3.8994687304049));
#84940=CARTESIAN_POINT('Ctrl Pts',(40.0729822857372,0.406524868837962,-3.91193386076711));
#84941=CARTESIAN_POINT('Ctrl Pts',(40.0671302556589,0.291181965974274,-3.92392019799237));
#84942=CARTESIAN_POINT('Ctrl Pts',(40.0612782255807,0.175254181137358,-3.93080654902714));
#84943=CARTESIAN_POINT('Ctrl Pts',(40.0554261955024,0.0592278899181963,
-3.9325540119693));
#84944=CARTESIAN_POINT('Ctrl Pts',(40.0495750551239,-0.0567807615142353,
-3.93430120924));
#84945=CARTESIAN_POINT('Ctrl Pts',(40.0437239147454,-0.172887476354015,
-3.93091106563208));
#84946=CARTESIAN_POINT('Ctrl Pts',(40.0378727743669,-0.288604339455222,
-3.92239678452443));
#84947=CARTESIAN_POINT('Ctrl Pts',(40.0320211067994,-0.404331628670237,
-3.91388173627826));
#84948=CARTESIAN_POINT('Ctrl Pts',(40.0261694392319,-0.519668584052631,
-3.90024166307759));
#84949=CARTESIAN_POINT('Ctrl Pts',(40.0203177716645,-0.634131590288176,
-3.88154172027026));
#84950=CARTESIAN_POINT('Ctrl Pts',(40.0144641599802,-0.748632624905172,
-3.86283556472589));
#84951=CARTESIAN_POINT('Ctrl Pts',(40.008610548296,-0.862258725289931,-3.83906626351055));
#84952=CARTESIAN_POINT('Ctrl Pts',(40.0027569366118,-0.974536358533108,
-3.81035010017413));
#84953=CARTESIAN_POINT('Ctrl Pts',(39.9968966705119,-1.08694162956307,-3.78160129215661));
#84954=CARTESIAN_POINT('Ctrl Pts',(39.991036404412,-1.1979949730428,-3.74789449994818));
#84955=CARTESIAN_POINT('Ctrl Pts',(39.9851761383122,-1.30723781953995,-3.70939594586025));
#84956=CARTESIAN_POINT('Ctrl Pts',(39.9793119251409,-1.41655424449064,-3.67087146179919));
#84957=CARTESIAN_POINT('Ctrl Pts',(39.9734477119696,-1.52405736187819,-3.62754894358141));
#84958=CARTESIAN_POINT('Ctrl Pts',(39.9675834987983,-1.62931000667219,-3.57964214722057));
#84959=CARTESIAN_POINT('Ctrl Pts',(39.961710650224,-1.73471764225125,-3.53166480525024));
#84960=CARTESIAN_POINT('Ctrl Pts',(39.9558378016497,-1.83786782434999,-3.47908989924171));
#84961=CARTESIAN_POINT('Ctrl Pts',(39.9499649530754,-1.93834925514787,-3.42217637842758));
#84962=CARTESIAN_POINT('Ctrl Pts',(39.9483702084626,-1.96563451858214,-3.40672177755203));
#84963=CARTESIAN_POINT('Ctrl Pts',(39.9467754638497,-1.99272317105285,-3.39094750118053));
#84964=CARTESIAN_POINT('Ctrl Pts',(39.9451807192368,-2.01960738063346,-3.3748592604864));
#84965=CARTESIAN_POINT('Ctrl Pts',(39.9393082731029,-2.11860509559063,-3.31561634089736));
#84966=CARTESIAN_POINT('Ctrl Pts',(39.933435826969,-2.21515960775382,-3.25191456193877));
#84967=CARTESIAN_POINT('Ctrl Pts',(39.9275633808351,-2.30884235755335,-3.18398115069287));
#84968=CARTESIAN_POINT('Ctrl Pts',(39.9216985418903,-2.40240375036212,-3.11613574064653));
#84969=CARTESIAN_POINT('Ctrl Pts',(39.9158337029454,-2.49310044719666,-3.0440698398317));
#84970=CARTESIAN_POINT('Ctrl Pts',(39.9099688640006,-2.580529788326,-2.96805576287949));
#84971=CARTESIAN_POINT('Ctrl Pts',(39.9041100538806,-2.66786925551552,-2.89211982542243));
#84972=CARTESIAN_POINT('Ctrl Pts',(39.8982512437606,-2.75194773759665,-2.81224405413166));
#84973=CARTESIAN_POINT('Ctrl Pts',(39.8923924336406,-2.83239336053307,-2.72874272352822));
#84974=CARTESIAN_POINT('Ctrl Pts',(39.8863066447596,-2.91595556302168,-2.64200643084679));
#84975=CARTESIAN_POINT('Ctrl Pts',(39.8802208558787,-2.99559736112515,-2.55135824521931));
#84976=CARTESIAN_POINT('Ctrl Pts',(39.8741350669977,-3.07094147611195,-2.45719503708911));
#84977=CARTESIAN_POINT('Ctrl Pts',(39.8682830369194,-3.14339157843153,-2.36664869428625));
#84978=CARTESIAN_POINT('Ctrl Pts',(39.8624310068412,-3.21186777857737,-2.2728527288008));
#84979=CARTESIAN_POINT('Ctrl Pts',(39.8565789767629,-3.27607436366046,-2.17619524945872));
#84980=CARTESIAN_POINT('Ctrl Pts',(39.8507278363844,-3.34027118724505,-2.0795524652112));
#84981=CARTESIAN_POINT('Ctrl Pts',(39.8448766960059,-3.40019945777604,-1.98004937633592));
#84982=CARTESIAN_POINT('Ctrl Pts',(39.8390255556274,-3.4556064613382,-1.87810356060514));
#84983=CARTESIAN_POINT('Ctrl Pts',(39.8331738880599,-3.51101845708308,-1.77614855953483));
#84984=CARTESIAN_POINT('Ctrl Pts',(39.8273222204924,-3.56190817865106,-1.67175075729493));
#84985=CARTESIAN_POINT('Ctrl Pts',(39.8214705529249,-3.60806893954932,-1.56535220556252));
#84986=CARTESIAN_POINT('Ctrl Pts',(39.8156169412407,-3.65424503657302,-1.45891830472615));
#84987=CARTESIAN_POINT('Ctrl Pts',(39.8097633295565,-3.69568888442674,-1.35048271165834));
#84988=CARTESIAN_POINT('Ctrl Pts',(39.8039097178723,-3.73224225777654,-1.24050664216967));
#84989=CARTESIAN_POINT('Ctrl Pts',(39.7980494517724,-3.76883718518785,-1.13040555132353));
#84990=CARTESIAN_POINT('Ctrl Pts',(39.7921891856725,-3.80053041103256,-1.0187608811661));
#84991=CARTESIAN_POINT('Ctrl Pts',(39.7863289195726,-3.82721380981329,-0.906048262497335));
#84992=CARTESIAN_POINT('Ctrl Pts',(39.7804647064014,-3.85391518069266,-0.793259728375754));
#84993=CARTESIAN_POINT('Ctrl Pts',(39.7746004932301,-3.87559992850287,-0.679402218543763));
#84994=CARTESIAN_POINT('Ctrl Pts',(39.7687362800588,-3.8922114870999,-0.56495906018719));
#84995=CARTESIAN_POINT('Ctrl Pts',(39.7628634314845,-3.90884750720583,-0.450347377467224));
#84996=CARTESIAN_POINT('Ctrl Pts',(39.7569905829102,-3.92039538724821,-0.335148734787296));
#84997=CARTESIAN_POINT('Ctrl Pts',(39.7511177343359,-3.92685056468687,-0.219849136041925));
#84998=CARTESIAN_POINT('Ctrl Pts',(39.749522989723,-3.92860343798432,-0.188540068279316));
#84999=CARTESIAN_POINT('Ctrl Pts',(39.7479282451101,-3.92998108784378,-0.157223539597995));
#85000=CARTESIAN_POINT('Ctrl Pts',(39.7463335004972,-3.93098408375229,-0.125909226374263));
#85001=CARTESIAN_POINT('Ctrl Pts',(39.7442101743431,-3.93231952481774,-0.0842157165003056));
#85002=CARTESIAN_POINT('Ctrl Pts',(39.742086848189,-3.93299166275049,-0.0425008473423755));
#85003=CARTESIAN_POINT('Ctrl Pts',(39.7399635220349,-3.93299992292071,-0.000778656347341876));
#85004=CARTESIAN_POINT('',(38.4899635541443,-3.93221249083461,-0.00323415915035297));
#85005=CARTESIAN_POINT('Ctrl Pts',(39.7399635219896,-3.93299992292088,-0.000778655457617156));
#85006=CARTESIAN_POINT('Ctrl Pts',(39.7341222016867,-3.93302264681791,0.114000075487013));
#85007=CARTESIAN_POINT('Ctrl Pts',(39.7282808813837,-3.92801663955931,0.228980042591623));
#85008=CARTESIAN_POINT('Ctrl Pts',(39.7224395610808,-3.91795511212009,0.343681159524406));
#85009=CARTESIAN_POINT('Ctrl Pts',(39.7166057401983,-3.90790650224411,0.458235016616241));
#85010=CARTESIAN_POINT('Ctrl Pts',(39.7107719193158,-3.8928153129585,0.572510322663808));
#85011=CARTESIAN_POINT('Ctrl Pts',(39.7049380984333,-3.87270674435775,0.686025853890374));
#85012=CARTESIAN_POINT('Ctrl Pts',(39.6991101642807,-3.85261846669758,0.799426840071701));
#85013=CARTESIAN_POINT('Ctrl Pts',(39.6932822301281,-3.82752295049738,0.912069166749725));
#85014=CARTESIAN_POINT('Ctrl Pts',(39.6874542959755,-3.79749722697163,1.02347633638633));
#85015=CARTESIAN_POINT('Ctrl Pts',(39.6816222953831,-3.7674505530035,1.13496124035252));
#85016=CARTESIAN_POINT('Ctrl Pts',(39.6757902947907,-3.7324668492666,1.24520884713989));
#85017=CARTESIAN_POINT('Ctrl Pts',(39.6699582941983,-3.69267473507464,1.35375119609972));
#85018=CARTESIAN_POINT('Ctrl Pts',(39.6641366491117,-3.6529532771636,1.46210081343785));
#85019=CARTESIAN_POINT('Ctrl Pts',(39.6583150040252,-3.60844060355128,1.56875082642146));
#85020=CARTESIAN_POINT('Ctrl Pts',(39.6524933589386,-3.55931438831396,1.67325135145357));
#85021=CARTESIAN_POINT('Ctrl Pts',(39.6466724354933,-3.5101942626788,1.77773892277819));
#85022=CARTESIAN_POINT('Ctrl Pts',(39.640851512048,-3.45646191029779,1.88007715749181));
#85023=CARTESIAN_POINT('Ctrl Pts',(39.6350305886027,-3.39834244097618,1.97983778473391));
#85024=CARTESIAN_POINT('Ctrl Pts',(39.6292089391354,-3.34021572263118,2.07961085474481));
#85025=CARTESIAN_POINT('Ctrl Pts',(39.6233872896681,-3.27770101050125,2.17680531706256));
#85026=CARTESIAN_POINT('Ctrl Pts',(39.6175656402009,-3.21106809880611,2.2710197411801));
#85027=CARTESIAN_POINT('Ctrl Pts',(39.6117256936639,-3.14422576415691,2.36553027517054));
#85028=CARTESIAN_POINT('Ctrl Pts',(39.605885747127,-3.07323954689038,2.45704166411266));
#85029=CARTESIAN_POINT('Ctrl Pts',(39.60004580059,-2.9984232303731,2.54518115888809));
#85030=CARTESIAN_POINT('Ctrl Pts',(39.5942152834158,-2.92372771465095,2.63317834084265));
#85031=CARTESIAN_POINT('Ctrl Pts',(39.5883847662415,-2.84521477321636,2.71781422872262));
#85032=CARTESIAN_POINT('Ctrl Pts',(39.5825542490673,-2.76323366118692,2.79875485415988));
#85033=CARTESIAN_POINT('Ctrl Pts',(39.576709587849,-2.68105367409605,2.87989183057919));
#85034=CARTESIAN_POINT('Ctrl Pts',(39.5708649266307,-2.59538899735307,2.95731532969188));
#85035=CARTESIAN_POINT('Ctrl Pts',(39.5650202654124,-2.5066238357333,3.03073026614604));
#85036=CARTESIAN_POINT('Ctrl Pts',(39.5591756041941,-2.41785867411354,3.10414520260021));
#85037=CARTESIAN_POINT('Ctrl Pts',(39.5533309429757,-2.32599339744468,3.17355137528231));
#85038=CARTESIAN_POINT('Ctrl Pts',(39.5474862817574,-2.231439307828,3.23869844466571));
#85039=CARTESIAN_POINT('Ctrl Pts',(39.5416138356235,-2.13643571783778,3.30415521648654));
#85040=CARTESIAN_POINT('Ctrl Pts',(39.5357413894896,-2.03839047734439,3.36553779771454));
#85041=CARTESIAN_POINT('Ctrl Pts',(39.5298689433557,-1.93768826068458,3.4225506869008));
#85042=CARTESIAN_POINT('Ctrl Pts',(39.5240041044108,-1.83711649405956,3.47948972137339));
#85043=CARTESIAN_POINT('Ctrl Pts',(39.518139265466,-1.73389495229055,3.53207011878397));
#85044=CARTESIAN_POINT('Ctrl Pts',(39.5122744265212,-1.6284385705889,3.58003866205637));
#85045=CARTESIAN_POINT('Ctrl Pts',(39.5064156164011,-1.52309059391863,3.62795789554443));
#85046=CARTESIAN_POINT('Ctrl Pts',(39.5005568062811,-1.41551272082882,3.67127453449536));
#85047=CARTESIAN_POINT('Ctrl Pts',(39.4946979961611,-1.30614527324796,3.70978079206468));
#85048=CARTESIAN_POINT('Ctrl Pts',(39.4886122072801,-1.19254077288174,3.74977883763395));
#85049=CARTESIAN_POINT('Ctrl Pts',(39.4825264183991,-1.07700562759994,3.78458601745905));
#85050=CARTESIAN_POINT('Ctrl Pts',(39.4764406295182,-0.960057541266778,
3.81402392722657));
#85051=CARTESIAN_POINT('Ctrl Pts',(39.4705885994399,-0.847601501104463,
3.84233110921568));
#85052=CARTESIAN_POINT('Ctrl Pts',(39.4647365693616,-0.73383949939955,3.86567377607085));
#85053=CARTESIAN_POINT('Ctrl Pts',(39.4588845392834,-0.619247398138756,
3.88394408557826));
#85054=CARTESIAN_POINT('Ctrl Pts',(39.4530333989049,-0.504672718621039,
3.90221161740175));
#85055=CARTESIAN_POINT('Ctrl Pts',(39.4471822585263,-0.389268598568526,
3.91540826013805));
#85056=CARTESIAN_POINT('Ctrl Pts',(39.4413311181478,-0.273519851921076,
3.92347752518159));
#85057=CARTESIAN_POINT('Ctrl Pts',(39.4354794505803,-0.157760676287066,
3.93154751726762));
#85058=CARTESIAN_POINT('Ctrl Pts',(39.4296277830128,-0.0416572247126819,
3.93448918454312));
#85059=CARTESIAN_POINT('Ctrl Pts',(39.4237761154453,0.074302538509432,3.93229807272682));
#85060=CARTESIAN_POINT('Ctrl Pts',(39.4179225037611,0.190300827385199,3.93010623295099));
#85061=CARTESIAN_POINT('Ctrl Pts',(39.4120688920769,0.306154919920153,3.92277823104649));
#85062=CARTESIAN_POINT('Ctrl Pts',(39.4062152803926,0.421379542415999,3.91036165606626));
#85063=CARTESIAN_POINT('Ctrl Pts',(39.4003550142927,0.536735152850913,3.89793096586021));
#85064=CARTESIAN_POINT('Ctrl Pts',(39.3944947481928,0.651459453743064,3.88040020079199));
#85065=CARTESIAN_POINT('Ctrl Pts',(39.3886344820929,0.765074862772757,3.85786851180198));
#85066=CARTESIAN_POINT('Ctrl Pts',(39.3827702689216,0.878766795312571,3.83532164701896));
#85067=CARTESIAN_POINT('Ctrl Pts',(39.3769060557504,0.991347948291256,3.80776724942484));
#85068=CARTESIAN_POINT('Ctrl Pts',(39.3710418425791,1.10235514877109,3.77535456957063));
#85069=CARTESIAN_POINT('Ctrl Pts',(39.3651689940048,1.21352581396196,3.7428941601158));
#85070=CARTESIAN_POINT('Ctrl Pts',(39.3592961454305,1.32311751110444,3.70556132301106));
#85071=CARTESIAN_POINT('Ctrl Pts',(39.3534232968562,1.43068622752751,3.66355372805738));
#85072=CARTESIAN_POINT('Ctrl Pts',(39.3518285522434,1.45989601028432,3.65214676176146));
#85073=CARTESIAN_POINT('Ctrl Pts',(39.3502338076306,1.48895676312913,3.64039535624159));
#85074=CARTESIAN_POINT('Ctrl Pts',(39.3486390630179,1.51785991994509,3.62830404781963));
#85075=CARTESIAN_POINT('Ctrl Pts',(39.3427666168839,1.62429215376019,3.58377932779368));
#85076=CARTESIAN_POINT('Ctrl Pts',(39.33689417075,1.72894179370186,3.53449298768078));
#85077=CARTESIAN_POINT('Ctrl Pts',(39.3310217246161,1.83135226396449,3.48060883830288));
#85078=CARTESIAN_POINT('Ctrl Pts',(39.3251568856712,1.93363007131431,3.4267944906571));
#85079=CARTESIAN_POINT('Ctrl Pts',(39.3192920467263,2.03367411486602,3.36839436885132));
#85080=CARTESIAN_POINT('Ctrl Pts',(39.3134272077815,2.13104702644055,3.30562060301828));
#85081=CARTESIAN_POINT('Ctrl Pts',(39.3075683976614,2.2283198424741,3.24291136615893));
#85082=CARTESIAN_POINT('Ctrl Pts',(39.3017095875414,2.32292664278129,3.17583765056074));
#85083=CARTESIAN_POINT('Ctrl Pts',(39.2958507774214,2.41445454864099,3.10465750648068));
#85084=CARTESIAN_POINT('Ctrl Pts',(39.2897649885404,2.50952837768939,3.03071974087418));
#85085=CARTESIAN_POINT('Ctrl Pts',(39.2836791996594,2.60127952367582,2.95235114529647));
#85086=CARTESIAN_POINT('Ctrl Pts',(39.2775934107785,2.68927798352129,2.86989075181402));
#85087=CARTESIAN_POINT('Ctrl Pts',(39.2717413807002,2.77389636972064,2.79059771152558));
#85088=CARTESIAN_POINT('Ctrl Pts',(39.2658893506219,2.85504470831304,2.70752172058038));
#85089=CARTESIAN_POINT('Ctrl Pts',(39.2600373205436,2.93237497801825,2.62100476693433));
#85090=CARTESIAN_POINT('Ctrl Pts',(39.2541861801651,3.00969349099628,2.53450096669151));
#85091=CARTESIAN_POINT('Ctrl Pts',(39.2483350397866,3.08319481386154,2.44455755202576));
#85092=CARTESIAN_POINT('Ctrl Pts',(39.2424838994081,3.15256928403407,2.35155180877754));
#85093=CARTESIAN_POINT('Ctrl Pts',(39.2366322318405,3.22195000486086,2.25853768569241));
#85094=CARTESIAN_POINT('Ctrl Pts',(39.230780564273,3.28720288666852,2.16246101688231));
#85095=CARTESIAN_POINT('Ctrl Pts',(39.2249288967055,3.34806033518655,2.06372987378448));
#85096=CARTESIAN_POINT('Ctrl Pts',(39.2190752850213,3.4089380025537,1.96496592894859));
#85097=CARTESIAN_POINT('Ctrl Pts',(39.2132216733371,3.46541711611587,1.86354610790681));
#85098=CARTESIAN_POINT('Ctrl Pts',(39.2073680616529,3.51727531575113,1.75990435910813));
#85099=CARTESIAN_POINT('Ctrl Pts',(39.2015077955529,3.56919246805268,1.65614478983991));
#85100=CARTESIAN_POINT('Ctrl Pts',(39.1956475294531,3.61647803638353,1.55015862108794));
#85101=CARTESIAN_POINT('Ctrl Pts',(39.1897872633532,3.65895719374826,1.4424012112855));
#85102=CARTESIAN_POINT('Ctrl Pts',(39.1839230501818,3.70146496214628,1.33457122351704));
#85103=CARTESIAN_POINT('Ctrl Pts',(39.1780588370105,3.73915973942352,1.22496800915292));
#85104=CARTESIAN_POINT('Ctrl Pts',(39.1721946238392,3.771916634124,1.11406189469826));
#85105=CARTESIAN_POINT('Ctrl Pts',(39.1663217752649,3.80472176530183,1.00299246438819));
#85106=CARTESIAN_POINT('Ctrl Pts',(39.1604489266906,3.83257440271595,0.890616704555471));
#85107=CARTESIAN_POINT('Ctrl Pts',(39.1545760781162,3.85540074576738,0.777415004702317));
#85108=CARTESIAN_POINT('Ctrl Pts',(39.1529813335035,3.86159913265726,0.746675611594062));
#85109=CARTESIAN_POINT('Ctrl Pts',(39.1513865888908,3.86742719220224,0.715875341961086));
#85110=CARTESIAN_POINT('Ctrl Pts',(39.1497918442781,3.87288410860961,0.68502385453292));
#85111=CARTESIAN_POINT('Ctrl Pts',(39.1439193981442,3.89297851582945,0.571417138681087));
#85112=CARTESIAN_POINT('Ctrl Pts',(39.1380469520103,3.90810353902675,0.45673529994965));
#85113=CARTESIAN_POINT('Ctrl Pts',(39.1321745058764,3.91815010211211,0.341450988164994));
#85114=CARTESIAN_POINT('Ctrl Pts',(39.1263096669316,3.92818365084143,0.226316016116477));
#85115=CARTESIAN_POINT('Ctrl Pts',(39.1204448279867,3.93315178651159,0.110580531044016));
#85116=CARTESIAN_POINT('Ctrl Pts',(39.1145799890419,3.93299646542847,-0.00527284810658881));
#85117=CARTESIAN_POINT('Ctrl Pts',(39.1087211789219,3.93284130400935,-0.121007134518799));
#85118=CARTESIAN_POINT('Ctrl Pts',(39.1028623688019,3.9275731621685,-0.23685866307964));
#85119=CARTESIAN_POINT('Ctrl Pts',(39.0970035586819,3.91718586633032,-0.352340586112312));
#85120=CARTESIAN_POINT('Ctrl Pts',(39.0909177698009,3.90639615165778,-0.472296445536227));
#85121=CARTESIAN_POINT('Ctrl Pts',(39.08483198092,3.89008257456317,-0.591853029483201));
#85122=CARTESIAN_POINT('Ctrl Pts',(39.078746192039,3.86829782477532,-0.710465297420283));
#85123=CARTESIAN_POINT('Ctrl Pts',(39.0728941619607,3.84734984029886,-0.824521596972113));
#85124=CARTESIAN_POINT('Ctrl Pts',(39.0670421318825,3.82134331373662,-0.937704341699031));
#85125=CARTESIAN_POINT('Ctrl Pts',(39.0611901018042,3.79037774973595,-1.04953585660834));
#85126=CARTESIAN_POINT('Ctrl Pts',(39.0553389614257,3.75941689351263,-1.16135036947396));
#85127=CARTESIAN_POINT('Ctrl Pts',(39.0494878210472,3.72349860919663,-1.27181366272718));
#85128=CARTESIAN_POINT('Ctrl Pts',(39.0436366806687,3.68277283527244,-1.38046124312832));
#85129=CARTESIAN_POINT('Ctrl Pts',(39.0377850131013,3.64204339194754,-1.48911861269909));
#85130=CARTESIAN_POINT('Ctrl Pts',(39.0319333455338,3.59650574303546,-1.59595955712241));
#85131=CARTESIAN_POINT('Ctrl Pts',(39.0260816779663,3.54635847090481,-1.7005383253081));
#85132=CARTESIAN_POINT('Ctrl Pts',(39.0202280662821,3.49619453819819,-1.80515183800608));
#85133=CARTESIAN_POINT('Ctrl Pts',(39.0143744545979,3.44141811567231,-1.90750130749258));
#85134=CARTESIAN_POINT('Ctrl Pts',(39.0085208429137,3.382274012236,-2.00716504208125));
#85135=CARTESIAN_POINT('Ctrl Pts',(39.0026605768138,3.32306267348093,-2.10694207491223));
#85136=CARTESIAN_POINT('Ctrl Pts',(38.9968003107139,3.25947395451529,-2.20402692315999));
#85137=CARTESIAN_POINT('Ctrl Pts',(38.9909400446141,3.19179637616573,-2.29802630383016));
#85138=CARTESIAN_POINT('Ctrl Pts',(38.9850758314428,3.12407321486295,-2.3920889960058));
#85139=CARTESIAN_POINT('Ctrl Pts',(38.9792116182715,3.05225596596096,-2.48306175892373));
#85140=CARTESIAN_POINT('Ctrl Pts',(38.9733474051002,2.97667274221939,-2.57058522242078));
#85141=CARTESIAN_POINT('Ctrl Pts',(38.9674745565259,2.90097821768147,-2.65823756942801));
#85142=CARTESIAN_POINT('Ctrl Pts',(38.9616017079516,2.82150693301668,-2.7424301802827));
#85143=CARTESIAN_POINT('Ctrl Pts',(38.9557288593774,2.73862309141705,-2.82284122174049));
#85144=CARTESIAN_POINT('Ctrl Pts',(38.9541341147644,2.71611637117436,-2.84467646464894));
#85145=CARTESIAN_POINT('Ctrl Pts',(38.9525393701515,2.69335820126911,-2.86623310145387));
#85146=CARTESIAN_POINT('Ctrl Pts',(38.9509446255386,2.6703562656032,-2.88750522332926));
#85147=CARTESIAN_POINT('Ctrl Pts',(38.9450721794047,2.58565453525737,-2.9658371323104));
#85148=CARTESIAN_POINT('Ctrl Pts',(38.9391997332708,2.4973614051379,-3.04057008110341));
#85149=CARTESIAN_POINT('Ctrl Pts',(38.9333272871369,2.40581549393361,-3.11135674732889));
#85150=CARTESIAN_POINT('Ctrl Pts',(38.927462448192,2.31438817165108,-3.18205171623755));
#85151=CARTESIAN_POINT('Ctrl Pts',(38.9215976092472,2.21971677175287,-3.24881031806787));
#85152=CARTESIAN_POINT('Ctrl Pts',(38.9157327703023,2.12217589277859,-3.31132276894135));
#85153=CARTESIAN_POINT('Ctrl Pts',(38.9098739601823,2.02473528200919,-3.37377095946267));
#85154=CARTESIAN_POINT('Ctrl Pts',(38.9040151500623,1.92443140523235,-3.43198145930564));
#85155=CARTESIAN_POINT('Ctrl Pts',(38.8981563399423,1.8216704649381,-3.48568583167964));
#85156=CARTESIAN_POINT('Ctrl Pts',(38.8920705510613,1.71492841748643,-3.54147078895906));
#85157=CARTESIAN_POINT('Ctrl Pts',(38.8859847621803,1.60553543515362,-3.59239313158994));
#85158=CARTESIAN_POINT('Ctrl Pts',(38.8798989732994,1.49397850077039,-3.6382024736449));
#85159=CARTESIAN_POINT('Ctrl Pts',(38.8740469432211,1.38670653517688,-3.6822522513835));
#85160=CARTESIAN_POINT('Ctrl Pts',(38.8681949131429,1.27743420618785,-3.72157439838867));
#85161=CARTESIAN_POINT('Ctrl Pts',(38.8623428830646,1.16661714144689,-3.7559943350972));
#85162=CARTESIAN_POINT('Ctrl Pts',(38.8564917426861,1.05581692451981,-3.79040903885096));
#85163=CARTESIAN_POINT('Ctrl Pts',(38.8506406023076,0.9434728334458,-3.81992289162211));
#85164=CARTESIAN_POINT('Ctrl Pts',(38.844789461929,0.830056677352447,-3.84441086674963));
#85165=CARTESIAN_POINT('Ctrl Pts',(38.8389377943615,0.716630302439545,-3.86890104824886));
#85166=CARTESIAN_POINT('Ctrl Pts',(38.833086126794,0.602132074559348,-3.88836436467114));
#85167=CARTESIAN_POINT('Ctrl Pts',(38.8272344592265,0.487044339022436,-3.90272684309653));
#85168=CARTESIAN_POINT('Ctrl Pts',(38.8213808475423,0.371918367548383,-3.9170940932104));
#85169=CARTESIAN_POINT('Ctrl Pts',(38.8155272358581,0.256202908932304,-3.92635708442548));
#85170=CARTESIAN_POINT('Ctrl Pts',(38.8096736241738,0.140385064663461,-3.93049373916553));
#85171=CARTESIAN_POINT('Ctrl Pts',(38.8038133580739,0.0244355580779736,
-3.93463509647581));
#85172=CARTESIAN_POINT('Ctrl Pts',(38.797953091974,-0.0916161531383416,
-3.93363847076239));
#85173=CARTESIAN_POINT('Ctrl Pts',(38.7920928258741,-0.20728322965967,-3.92753391617461));
#85174=CARTESIAN_POINT('Ctrl Pts',(38.7862286127029,-0.3230282115524,-3.92142524997956));
#85175=CARTESIAN_POINT('Ctrl Pts',(38.7803643995316,-0.438387632494599,
-3.91020184441281));
#85176=CARTESIAN_POINT('Ctrl Pts',(38.7745001863604,-0.552881773172785,
-3.89394539572569));
#85177=CARTESIAN_POINT('Ctrl Pts',(38.7686273377861,-0.667544513289531,
-3.87766500845006));
#85178=CARTESIAN_POINT('Ctrl Pts',(38.7627544892118,-0.781339025385813,
-3.85633686212652));
#85179=CARTESIAN_POINT('Ctrl Pts',(38.7568816406375,-0.893797652072539,
-3.83009330919622));
#85180=CARTESIAN_POINT('Ctrl Pts',(38.7552868960246,-0.924335267134304,
-3.82296699491646));
#85181=CARTESIAN_POINT('Ctrl Pts',(38.7536921514118,-0.954774477665476,
-3.81547851376626));
#85182=CARTESIAN_POINT('Ctrl Pts',(38.7520974067989,-0.98510615834445,-3.80763113454965));
#85183=CARTESIAN_POINT('Ctrl Pts',(38.746224960665,-1.09679875131735,-3.77873414918237));
#85184=CARTESIAN_POINT('Ctrl Pts',(38.7403525145311,-1.20740577352903,-3.74487005168703));
#85185=CARTESIAN_POINT('Ctrl Pts',(38.7344800683971,-1.31645195970563,-3.70613589035632));
#85186=CARTESIAN_POINT('Ctrl Pts',(38.7286152294523,-1.42535688703736,-3.66745190540571));
#85187=CARTESIAN_POINT('Ctrl Pts',(38.7227503905074,-1.53270461327704,-3.62391053946211));
#85188=CARTESIAN_POINT('Ctrl Pts',(38.7168855515626,-1.63803199619866,-3.57565940484122));
#85189=CARTESIAN_POINT('Ctrl Pts',(38.7110267414425,-1.74325110669441,-3.52745787049758));
#85190=CARTESIAN_POINT('Ctrl Pts',(38.7051679313225,-1.84645363126394,-3.47455636852455));
#85191=CARTESIAN_POINT('Ctrl Pts',(38.6993091212024,-1.94719412064057,-3.41715145355642));
#85192=CARTESIAN_POINT('Ctrl Pts',(38.6932233323215,-2.05183744198914,-3.35752258932152));
#85193=CARTESIAN_POINT('Ctrl Pts',(38.6871375434405,-2.15382367618305,-3.29303446950404));
#85194=CARTESIAN_POINT('Ctrl Pts',(38.6810517545595,-2.25267887974533,-3.22396136216756));
#85195=CARTESIAN_POINT('Ctrl Pts',(38.6751997244813,-2.34773699562076,-3.15754139433116));
#85196=CARTESIAN_POINT('Ctrl Pts',(38.669347694403,-2.43989980335057,-3.08688242463019));
#85197=CARTESIAN_POINT('Ctrl Pts',(38.6634956643247,-2.52877408251778,-3.01227333414256));
#85198=CARTESIAN_POINT('Ctrl Pts',(38.6576445239462,-2.61763484989107,-2.93767558667415));
#85199=CARTESIAN_POINT('Ctrl Pts',(38.6517933835677,-2.70320776629022,-2.85912917820392));
#85200=CARTESIAN_POINT('Ctrl Pts',(38.6459422431892,-2.78513254614726,-2.77696339558001));
#85201=CARTESIAN_POINT('Ctrl Pts',(38.6400905756216,-2.86706470744469,-2.69479020980131));
#85202=CARTESIAN_POINT('Ctrl Pts',(38.6342389080541,-2.9453477869035,-2.60899729433365));
#85203=CARTESIAN_POINT('Ctrl Pts',(38.6283872404865,-3.01965874879582,-2.51995040443673));
#85204=CARTESIAN_POINT('Ctrl Pts',(38.6225336288023,-3.09399439923746,-2.43087393022981));
#85205=CARTESIAN_POINT('Ctrl Pts',(38.616680017118,-3.16435504332694,-2.33854164913412));
#85206=CARTESIAN_POINT('Ctrl Pts',(38.6108264054338,-3.23045872844755,-2.24335137769299));
#85207=CARTESIAN_POINT('Ctrl Pts',(38.6049661393339,-3.29663756057493,-2.14805289346525));
#85208=CARTESIAN_POINT('Ctrl Pts',(38.599105873234,-3.35854953867246,-2.04989027376121));
#85209=CARTESIAN_POINT('Ctrl Pts',(38.5932456071341,-3.41595670555015,-1.94928930274778));
#85210=CARTESIAN_POINT('Ctrl Pts',(38.5873813939628,-3.47340253793976,-1.84862057385229));
#85211=CARTESIAN_POINT('Ctrl Pts',(38.5815171807914,-3.52633732922251,-1.74551059031613));
#85212=CARTESIAN_POINT('Ctrl Pts',(38.5756529676201,-3.57457041386852,-1.64040707030171));
#85213=CARTESIAN_POINT('Ctrl Pts',(38.5697801190458,-3.62287452460275,-1.53514877909776));
#85214=CARTESIAN_POINT('Ctrl Pts',(38.5639072704715,-3.66646295564883,-1.4278914740419));
#85215=CARTESIAN_POINT('Ctrl Pts',(38.5580344218972,-3.70519417592132,-1.31910011701869));
#85216=CARTESIAN_POINT('Ctrl Pts',(38.5564396772845,-3.71571145796756,-1.28955833191726));
#85217=CARTESIAN_POINT('Ctrl Pts',(38.5548449326719,-3.72587087367678,-1.25990349824903));
#85218=CARTESIAN_POINT('Ctrl Pts',(38.5532501880592,-3.73567023864127,-1.23014505979169));
#85219=CARTESIAN_POINT('Ctrl Pts',(38.5462392868433,-3.77875072889645,-1.0993194274556));
#85220=CARTESIAN_POINT('Ctrl Pts',(38.5392283856274,-3.81498593538232,-0.966134731394327));
#85221=CARTESIAN_POINT('Ctrl Pts',(38.5322174844115,-3.84415332338129,-0.831248594787745));
#85222=CARTESIAN_POINT('Ctrl Pts',(38.5251751644464,-3.87345142251401,-0.695757977593311));
#85223=CARTESIAN_POINT('Ctrl Pts',(38.5181328444814,-3.89561804847248,-0.558550643918599));
#85224=CARTESIAN_POINT('Ctrl Pts',(38.5110905245163,-3.91047620229872,-0.420315204644498));
#85225=CARTESIAN_POINT('Ctrl Pts',(38.5040482045513,-3.92533435612497,-0.282079765370396));
#85226=CARTESIAN_POINT('Ctrl Pts',(38.4970058845862,-3.93288385965473,-0.142816253941332));
#85227=CARTESIAN_POINT('Ctrl Pts',(38.4899635646211,-3.93299866955088,-0.00323501329192832));
#85228=CARTESIAN_POINT('',(37.2399634924685,-3.93111579142054,0.00213576531572005));
#85229=CARTESIAN_POINT('Ctrl Pts',(38.4899635220349,-3.92980300012612,-0.00323154136619402));
#85230=CARTESIAN_POINT('Ctrl Pts',(38.4447766711298,-3.92290905173679,0.891666188285667));
#85231=CARTESIAN_POINT('Ctrl Pts',(38.3333074139783,-3.17538053464665,3.10966251113421));
#85232=CARTESIAN_POINT('Ctrl Pts',(38.1555557505799,0.511208908507071,4.62348953424194));
#85233=CARTESIAN_POINT('Ctrl Pts',(37.9567085318404,4.16573650181501,2.06993464119223));
#85234=CARTESIAN_POINT('Ctrl Pts',(37.7578613131006,3.99370385220429,-2.38501982428893));
#85235=CARTESIAN_POINT('Ctrl Pts',(37.5590140943612,0.153136628653335,-4.64914392058655));
#85236=CARTESIAN_POINT('Ctrl Pts',(37.386381497339,-3.30324063369252,-2.90718042645609));
#85237=CARTESIAN_POINT('Ctrl Pts',(37.2800313065638,-3.92374991679303,-0.792479136698486));
#85238=CARTESIAN_POINT('Ctrl Pts',(37.2399635220349,-3.92764697970144,0.00213329408759316));
#85239=CARTESIAN_POINT('',(35.9899635220349,-3.93452019141862,0.00241941282782897));
#85240=CARTESIAN_POINT('Ctrl Pts',(37.2399634764134,-3.932999419371,0.00213710723760822));
#85241=CARTESIAN_POINT('Ctrl Pts',(37.2334098247858,-3.93292870039597,0.132283916372161));
#85242=CARTESIAN_POINT('Ctrl Pts',(37.2268561731581,-3.92639368087127,0.262202170396104));
#85243=CARTESIAN_POINT('Ctrl Pts',(37.2203025215305,-3.91348782244965,0.391282587829128));
#85244=CARTESIAN_POINT('Ctrl Pts',(37.2137879833111,-3.90065898858428,0.519592629395078));
#85245=CARTESIAN_POINT('Ctrl Pts',(37.2072734450916,-3.88153532829353,0.64707459334773));
#85246=CARTESIAN_POINT('Ctrl Pts',(37.2007589068722,-3.85625898977929,0.7731465603276));
#85247=CARTESIAN_POINT('Ctrl Pts',(37.1941856985404,-3.83075501185786,0.900353934946174));
#85248=CARTESIAN_POINT('Ctrl Pts',(37.1876124902087,-3.79898711375405,1.02612555331995));
#85249=CARTESIAN_POINT('Ctrl Pts',(37.181039281877,-3.76115085212069,1.14988402353968));
#85250=CARTESIAN_POINT('Ctrl Pts',(37.1744660735452,-3.72331459048733,1.27364249375941));
#85251=CARTESIAN_POINT('Ctrl Pts',(37.1678928652135,-3.67941012507819,1.39538760983665));
#85252=CARTESIAN_POINT('Ctrl Pts',(37.1613196568818,-3.62968041094891,1.51456565205135));
#85253=CARTESIAN_POINT('Ctrl Pts',(37.1554472107479,-3.58525232458046,1.62103825993672));
#85254=CARTESIAN_POINT('Ctrl Pts',(37.149574764614,-3.536061001913,1.72573259710872));
#85255=CARTESIAN_POINT('Ctrl Pts',(37.14370231848,-3.4822698392381,1.82819193924835));
#85256=CARTESIAN_POINT('Ctrl Pts',(37.1378374795352,-3.42854835784009,1.93051855516616));
#85257=CARTESIAN_POINT('Ctrl Pts',(37.1319726405903,-3.37023907644195,2.03061557100527));
#85258=CARTESIAN_POINT('Ctrl Pts',(37.1261078016455,-3.30755372806207,2.12804542620281));
#85259=CARTESIAN_POINT('Ctrl Pts',(37.1202489915254,-3.24493281776612,2.22537512732371));
#85260=CARTESIAN_POINT('Ctrl Pts',(37.1143901814054,-3.17794501041741,2.32004277573182));
#85261=CARTESIAN_POINT('Ctrl Pts',(37.1085313712854,-3.1068479813703,2.41163525862749));
#85262=CARTESIAN_POINT('Ctrl Pts',(37.1024455824044,-3.03299655079306,2.5067761665195));
#85263=CARTESIAN_POINT('Ctrl Pts',(37.0963597935234,-2.95471127585929,2.59859841486491));
#85264=CARTESIAN_POINT('Ctrl Pts',(37.0902740046425,-2.87233079815463,2.68667169300091));
#85265=CARTESIAN_POINT('Ctrl Pts',(37.0844219745642,-2.79311460403095,2.7713620236754));
#85266=CARTESIAN_POINT('Ctrl Pts',(37.0785699444859,-2.71011231082609,2.85258574219773));
#85267=CARTESIAN_POINT('Ctrl Pts',(37.0727179144076,-2.62366559043396,2.92999451698681));
#85268=CARTESIAN_POINT('Ctrl Pts',(37.0668667740291,-2.5372320127675,3.00739152311324));
#85269=CARTESIAN_POINT('Ctrl Pts',(37.0610156336506,-2.44735535698887,3.08097446305657));
#85270=CARTESIAN_POINT('Ctrl Pts',(37.0551644932721,-2.35441262768268,3.15043333187807));
#85271=CARTESIAN_POINT('Ctrl Pts',(37.0493128257046,-2.26146152421694,3.21989845895832));
#85272=CARTESIAN_POINT('Ctrl Pts',(37.043461158137,-2.16544412918584,3.28523852878785));
#85273=CARTESIAN_POINT('Ctrl Pts',(37.0376094905695,-2.06676827094617,3.34618557677398));
#85274=CARTESIAN_POINT('Ctrl Pts',(37.0317558788853,-1.96805962933559,3.4071528733773));
#85275=CARTESIAN_POINT('Ctrl Pts',(37.025902267201,-1.86669111976615,3.46372402889574));
#85276=CARTESIAN_POINT('Ctrl Pts',(37.0200486555168,-1.7630964886576,3.51567628937638));
#85277=CARTESIAN_POINT('Ctrl Pts',(37.0141883894169,-1.6593840906435,3.56768760945197));
#85278=CARTESIAN_POINT('Ctrl Pts',(37.008328123317,-1.55344088967951,3.61506936869121));
#85279=CARTESIAN_POINT('Ctrl Pts',(37.0024678572171,-1.44572208530969,3.65764632681289));
#85280=CARTESIAN_POINT('Ctrl Pts',(36.9966036440458,-1.33793072897609,3.70025196183959));
#85281=CARTESIAN_POINT('Ctrl Pts',(36.9907394308744,-1.22836177771908,3.73804621739922));
#85282=CARTESIAN_POINT('Ctrl Pts',(36.9848752177031,-1.11748544447807,3.77090377514193));
#85283=CARTESIAN_POINT('Ctrl Pts',(36.9790023691288,-1.00644583923602,3.80380971759439));
#85284=CARTESIAN_POINT('Ctrl Pts',(36.9731295205545,-0.894095409315755,
3.83176435416209));
#85285=CARTESIAN_POINT('Ctrl Pts',(36.9672566719802,-0.780914477028074,
3.85469344819636));
#85286=CARTESIAN_POINT('Ctrl Pts',(36.9656619273675,-0.75018072325557,3.86091973663587));
#85287=CARTESIAN_POINT('Ctrl Pts',(36.9640671827548,-0.719385756813729,
3.86677575314457));
#85288=CARTESIAN_POINT('Ctrl Pts',(36.9624724381421,-0.688539235687553,
3.87226067316223));
#85289=CARTESIAN_POINT('Ctrl Pts',(36.9565999920082,-0.574950807615644,
3.89245820014941));
#85290=CARTESIAN_POINT('Ctrl Pts',(36.9507275458743,-0.460282746080942,
3.90768732111895));
#85291=CARTESIAN_POINT('Ctrl Pts',(36.9448550997404,-0.345007601699793,
3.91783853097207));
#85292=CARTESIAN_POINT('Ctrl Pts',(36.9389902607955,-0.229881785179329,
3.92797659090931));
#85293=CARTESIAN_POINT('Ctrl Pts',(36.9331254218507,-0.114150857684523,
3.93304978499831));
#85294=CARTESIAN_POINT('Ctrl Pts',(36.9272605829058,0.00170261472762606,
3.93299963146491));
#85295=CARTESIAN_POINT('Ctrl Pts',(36.9214017727858,0.117436994305847,3.93294952948738));
#85296=CARTESIAN_POINT('Ctrl Pts',(36.9155429626657,0.233293257362139,3.92778655562286));
#85297=CARTESIAN_POINT('Ctrl Pts',(36.9096841525457,0.348784562024424,3.91750409435567));
#85298=CARTESIAN_POINT('Ctrl Pts',(36.9035983636647,0.468750166535014,3.90682327569679));
#85299=CARTESIAN_POINT('Ctrl Pts',(36.8975125747838,0.58832151009465,3.89061823444403));
#85300=CARTESIAN_POINT('Ctrl Pts',(36.8914267859028,0.70695350456514,3.86894116553652));
#85301=CARTESIAN_POINT('Ctrl Pts',(36.8855747558245,0.821028772942941,3.84809672585305));
#85302=CARTESIAN_POINT('Ctrl Pts',(36.8797227257462,0.934235078816343,3.82219295318668));
#85303=CARTESIAN_POINT('Ctrl Pts',(36.873870695668,1.04609465706276,3.79132891852774));
#85304=CARTESIAN_POINT('Ctrl Pts',(36.8680195552894,1.15793722899886,3.76046957621039));
#85305=CARTESIAN_POINT('Ctrl Pts',(36.8621684149109,1.26843308205228,3.72465158125484));
#85306=CARTESIAN_POINT('Ctrl Pts',(36.8563172745324,1.377117587066,3.68402445043373));
#85307=CARTESIAN_POINT('Ctrl Pts',(36.8504656069649,1.48581188457658,3.64339365909954));
#85308=CARTESIAN_POINT('Ctrl Pts',(36.8446139393974,1.5926941224023,3.59795301527448));
#85309=CARTESIAN_POINT('Ctrl Pts',(36.8387622718299,1.69731836937081,3.54790069660869));
#85310=CARTESIAN_POINT('Ctrl Pts',(36.8329086601456,1.80197737596095,3.49783174891369));
#85311=CARTESIAN_POINT('Ctrl Pts',(36.8270550484614,1.90437652732299,3.44314825808369));
#85312=CARTESIAN_POINT('Ctrl Pts',(36.8212014367771,2.00409390971568,3.3840946501303));
#85313=CARTESIAN_POINT('Ctrl Pts',(36.8153411706772,2.10392465133778,3.32497390973388));
#85314=CARTESIAN_POINT('Ctrl Pts',(36.8094809045773,2.20106718311247,3.26147334706311));
#85315=CARTESIAN_POINT('Ctrl Pts',(36.8036206384774,2.29512796029872,3.19388112581778));
#85316=CARTESIAN_POINT('Ctrl Pts',(36.7977564253061,2.38925209034279,3.12624337910996));
#85317=CARTESIAN_POINT('Ctrl Pts',(36.7918922121348,2.48029000886613,3.05450874156429));
#85318=CARTESIAN_POINT('Ctrl Pts',(36.7860279989635,2.56788204800477,2.97900499958204));
#85319=CARTESIAN_POINT('Ctrl Pts',(36.7801551503892,2.65560307163525,2.90339007384512));
#85320=CARTESIAN_POINT('Ctrl Pts',(36.7742823018149,2.73986778894419,2.8239952489147));
#85321=CARTESIAN_POINT('Ctrl Pts',(36.7684094532406,2.82035403620938,2.74118443568422));
#85322=CARTESIAN_POINT('Ctrl Pts',(36.7668147086279,2.84220970090093,2.71869754595714));
#85323=CARTESIAN_POINT('Ctrl Pts',(36.7652199640151,2.86378698786068,2.69595895376266));
#85324=CARTESIAN_POINT('Ctrl Pts',(36.7636252194024,2.88507998128988,2.67297633763571));
#85325=CARTESIAN_POINT('Ctrl Pts',(36.7577527732685,2.96348874714819,2.58834574904788));
#85326=CARTESIAN_POINT('Ctrl Pts',(36.7518803271346,3.03830181444336,2.50012049516091));
#85327=CARTESIAN_POINT('Ctrl Pts',(36.7460078810007,3.10917155355338,2.4086388792375));
#85328=CARTESIAN_POINT('Ctrl Pts',(36.7401430420559,3.17994948773362,2.31727576894753));
#85329=CARTESIAN_POINT('Ctrl Pts',(36.7342782031111,3.24679400131313,2.22266500908758));
#85330=CARTESIAN_POINT('Ctrl Pts',(36.7284133641662,3.30939497049408,2.12518091683237));
#85331=CARTESIAN_POINT('Ctrl Pts',(36.7225545540462,3.37193158832961,2.02779703440739));
#85332=CARTESIAN_POINT('Ctrl Pts',(36.7166957439262,3.43023311640159,1.92754604033316));
#85333=CARTESIAN_POINT('Ctrl Pts',(36.7108369338062,3.48403074929415,1.82483389325517));
#85334=CARTESIAN_POINT('Ctrl Pts',(36.7047511449252,3.53991258013931,1.71814252933926));
#85335=CARTESIAN_POINT('Ctrl Pts',(36.6986653560443,3.59093420476172,1.60879581752963));
#85336=CARTESIAN_POINT('Ctrl Pts',(36.6925795671633,3.63684479527185,1.49728051316513));
#85337=CARTESIAN_POINT('Ctrl Pts',(36.686727537085,3.68099193245167,1.39004857855646));
#85338=CARTESIAN_POINT('Ctrl Pts',(36.6808755070068,3.7204132567031,1.28081198980515));
#85339=CARTESIAN_POINT('Ctrl Pts',(36.6750234769285,3.75493377493265,1.17002621589008));
#85340=CARTESIAN_POINT('Ctrl Pts',(36.66917233655,3.78944904491566,1.05925728503194));
#85341=CARTESIAN_POINT('Ctrl Pts',(36.6633211961715,3.81906486740816,0.946940031848625));
#85342=CARTESIAN_POINT('Ctrl Pts',(36.657470055793,3.84365578750946,0.83354615177868));
#85343=CARTESIAN_POINT('Ctrl Pts',(36.6516183882256,3.86824892325786,0.720142054896152));
#85344=CARTESIAN_POINT('Ctrl Pts',(36.6457667206581,3.88781616898965,0.605661542282593));
#85345=CARTESIAN_POINT('Ctrl Pts',(36.6399150530906,3.90228311395982,0.490586891899909));
#85346=CARTESIAN_POINT('Ctrl Pts',(36.6340614414064,3.91675486532571,0.375474009927441));
#85347=CARTESIAN_POINT('Ctrl Pts',(36.6282078297221,3.92612289501087,0.25976700759516));
#85348=CARTESIAN_POINT('Ctrl Pts',(36.6223542180379,3.93036468327514,0.143952966150416));
#85349=CARTESIAN_POINT('Ctrl Pts',(36.616493951938,3.93461129362597,0.0280072667119841));
#85350=CARTESIAN_POINT('Ctrl Pts',(36.6106336858382,3.93372001584771,-0.0880453013893719));
#85351=CARTESIAN_POINT('Ctrl Pts',(36.6047734197383,3.92772046214228,-0.203717871746349));
#85352=CARTESIAN_POINT('Ctrl Pts',(36.598909206567,3.9217168675509,-0.31946835117574));
#85353=CARTESIAN_POINT('Ctrl Pts',(36.5930449933957,3.9105981856969,-0.43483791278791));
#85354=CARTESIAN_POINT('Ctrl Pts',(36.5871807802244,3.89444567732624,-0.549346763306142));
#85355=CARTESIAN_POINT('Ctrl Pts',(36.5813079316501,3.87826938342547,-0.664024234923348));
#85356=CARTESIAN_POINT('Ctrl Pts',(36.5754350830758,3.85704454441074,-0.777838061049976));
#85357=CARTESIAN_POINT('Ctrl Pts',(36.5695622345016,3.83090308814628,-0.890320464344874));
#85358=CARTESIAN_POINT('Ctrl Pts',(36.5679674898887,3.8238044977393,-0.920864535834475));
#85359=CARTESIAN_POINT('Ctrl Pts',(36.5663727452758,3.81634365128301,-0.95131053159593));
#85360=CARTESIAN_POINT('Ctrl Pts',(36.5647780006629,3.80852380929646,-0.981649323344114));
#85361=CARTESIAN_POINT('Ctrl Pts',(36.558905554529,3.77972822631074,-1.09336810193003));
#85362=CARTESIAN_POINT('Ctrl Pts',(36.553033108395,3.74596454780185,-1.20400581916583));
#85363=CARTESIAN_POINT('Ctrl Pts',(36.5471606622611,3.70732939059398,-1.31308712187657));
#85364=CARTESIAN_POINT('Ctrl Pts',(36.5412958233163,3.66874428151579,-1.42202712025262));
#85365=CARTESIAN_POINT('Ctrl Pts',(36.5354309843714,3.62530037987541,-1.52941432753211));
#85366=CARTESIAN_POINT('Ctrl Pts',(36.5295661454266,3.57714487750403,-1.63478546768274));
#85367=CARTESIAN_POINT('Ctrl Pts',(36.5237073353066,3.52903887710375,-1.74004829042668));
#85368=CARTESIAN_POINT('Ctrl Pts',(36.5178485251865,3.47623108042718,-1.84329879453504));
#85369=CARTESIAN_POINT('Ctrl Pts',(36.5119897150665,3.41891763766497,-1.94409135249952));
#85370=CARTESIAN_POINT('Ctrl Pts',(36.5059039261855,3.35938378940106,-2.04878875964854));
#85371=CARTESIAN_POINT('Ctrl Pts',(36.4998181373046,3.29498827554955,-2.15083349179325));
#85372=CARTESIAN_POINT('Ctrl Pts',(36.4937323484236,3.22600493383233,-2.24975135668133));
#85373=CARTESIAN_POINT('Ctrl Pts',(36.4878803183453,3.15967128366404,-2.34486972702322));
#85374=CARTESIAN_POINT('Ctrl Pts',(36.482028288267,3.08909600512226,-2.4370966384242));
#85375=CARTESIAN_POINT('Ctrl Pts',(36.4761762581888,3.01456762221467,-2.52603860839359));
#85376=CARTESIAN_POINT('Ctrl Pts',(36.4703251178103,2.94005057005607,-2.61496705627786));
#85377=CARTESIAN_POINT('Ctrl Pts',(36.4644739774317,2.86158187393101,-2.70061123899355));
#85378=CARTESIAN_POINT('Ctrl Pts',(36.4586228370532,2.77949049349779,-2.78261057220651));
#85379=CARTESIAN_POINT('Ctrl Pts',(36.4527711694857,2.69739171661382,-2.86461729357673));
#85380=CARTESIAN_POINT('Ctrl Pts',(36.4469195019182,2.61166989902848,-2.94297822047091));
#85381=CARTESIAN_POINT('Ctrl Pts',(36.4410678343507,2.5226905026107,-3.01736998527489));
#85382=CARTESIAN_POINT('Ctrl Pts',(36.4352142226665,2.43368154430616,-3.09178646547384));
#85383=CARTESIAN_POINT('Ctrl Pts',(36.4293606109823,2.34141317208805,-3.16223089646156));
#85384=CARTESIAN_POINT('Ctrl Pts',(36.423506999298,2.24628294638947,-3.2284209646141));
#85385=CARTESIAN_POINT('Ctrl Pts',(36.4176467331981,2.15104457616456,-3.2946862779741));
#85386=CARTESIAN_POINT('Ctrl Pts',(36.4117864670982,2.05293819834845,-3.35668733902035));
#85387=CARTESIAN_POINT('Ctrl Pts',(36.4059262009983,1.95238938092377,-3.41418580414952));
#85388=CARTESIAN_POINT('Ctrl Pts',(36.400061987827,1.85177284074446,-3.47172299628259));
#85389=CARTESIAN_POINT('Ctrl Pts',(36.3941977746557,1.74871095197124,-3.52475136524969));
#85390=CARTESIAN_POINT('Ctrl Pts',(36.3883335614844,1.64365125950279,-3.57307983917725));
#85391=CARTESIAN_POINT('Ctrl Pts',(36.3824607129101,1.53843686038308,-3.6214794796596));
#85392=CARTESIAN_POINT('Ctrl Pts',(36.3765878643359,1.43121916751251,-3.66516525702887));
#85393=CARTESIAN_POINT('Ctrl Pts',(36.3707150157616,1.32246301410729,-3.70399521818242));
#85394=CARTESIAN_POINT('Ctrl Pts',(36.3691202711488,1.29293078838095,-3.71453931285502));
#85395=CARTESIAN_POINT('Ctrl Pts',(36.367525526536,1.26328518927632,-3.72472564395935));
#85396=CARTESIAN_POINT('Ctrl Pts',(36.3659307819232,1.23353565858427,-3.73455201851588));
#85397=CARTESIAN_POINT('Ctrl Pts',(36.3600583357892,1.12398675959701,-3.77073640491336));
#85398=CARTESIAN_POINT('Ctrl Pts',(36.3541858896553,1.01266095893547,-3.80215704412923));
#85399=CARTESIAN_POINT('Ctrl Pts',(36.3483134435214,0.900010369633905,-3.82863818276831));
#85400=CARTESIAN_POINT('Ctrl Pts',(36.3424486045765,0.78750570833446,-3.85508501763962));
#85401=CARTESIAN_POINT('Ctrl Pts',(36.3365837656316,0.673680069858687,-3.8766049828504));
#85402=CARTESIAN_POINT('Ctrl Pts',(36.3307189266868,0.559002754264918,-3.8930713993869));
#85403=CARTESIAN_POINT('Ctrl Pts',(36.3248601165668,0.444443322461914,-3.90952088909186));
#85404=CARTESIAN_POINT('Ctrl Pts',(36.3190013064467,0.329034361644007,-3.92092710456594));
#85405=CARTESIAN_POINT('Ctrl Pts',(36.3131424963267,0.213256798060077,-3.92721409374141));
#85406=CARTESIAN_POINT('Ctrl Pts',(36.3070567074457,0.0929938445441312,
-3.93374464995247));
#85407=CARTESIAN_POINT('Ctrl Pts',(36.3009709185648,-0.0276664074746646,
-3.93475120119759));
#85408=CARTESIAN_POINT('Ctrl Pts',(36.2948851296838,-0.14817699638656,-3.9302077016033));
#85409=CARTESIAN_POINT('Ctrl Pts',(36.2890330996055,-0.264058701266171,
-3.92583872055473));
#85410=CARTESIAN_POINT('Ctrl Pts',(36.2831810695272,-0.37980157700227,-3.91633820245232));
#85411=CARTESIAN_POINT('Ctrl Pts',(36.277329039449,-0.49491861473092,-3.90173609625162));
#85412=CARTESIAN_POINT('Ctrl Pts',(36.2714778990704,-0.610018150909,-3.8871362100481));
#85413=CARTESIAN_POINT('Ctrl Pts',(36.2656267586919,-0.724491628305239,
-3.86743632990958));
#85414=CARTESIAN_POINT('Ctrl Pts',(36.2597756183134,-0.837857848307911,
-3.84271820799143));
#85415=CARTESIAN_POINT('Ctrl Pts',(36.2539239507459,-0.951234282630988,
-3.81799785896526));
#85416=CARTESIAN_POINT('Ctrl Pts',(36.2480722831784,-1.06350285734598,-3.78825845740157));
#85417=CARTESIAN_POINT('Ctrl Pts',(36.2422206156109,-1.17419394375876,-3.75363258490229));
#85418=CARTESIAN_POINT('Ctrl Pts',(36.2363670039266,-1.28492180539675,-3.71899520854755));
#85419=CARTESIAN_POINT('Ctrl Pts',(36.2305133922424,-1.39407074230773,-3.67946825647472));
#85420=CARTESIAN_POINT('Ctrl Pts',(36.2246597805581,-1.50118830475779,-3.63523351019689));
#85421=CARTESIAN_POINT('Ctrl Pts',(36.2187995144582,-1.60842763900001,-3.59094847763355));
#85422=CARTESIAN_POINT('Ctrl Pts',(36.2129392483583,-1.71363060725445,-3.54194512663007));
#85423=CARTESIAN_POINT('Ctrl Pts',(36.2070789822584,-1.81636660379168,-3.48845257394024));
#85424=CARTESIAN_POINT('Ctrl Pts',(36.2012147690871,-1.91917179621669,-3.43492399235306));
#85425=CARTESIAN_POINT('Ctrl Pts',(36.1953505559158,-2.01950635142536,-3.37690039487789));
#85426=CARTESIAN_POINT('Ctrl Pts',(36.1894863427445,-2.11696754594518,-3.31465494575451));
#85427=CARTESIAN_POINT('Ctrl Pts',(36.1836134941702,-2.21457225787572,-3.25231783650188));
#85428=CARTESIAN_POINT('Ctrl Pts',(36.1777406455959,-2.30929482757873,-3.1857467046369));
#85429=CARTESIAN_POINT('Ctrl Pts',(36.1718677970216,-2.40076450275936,-3.11525581650859));
#85430=CARTESIAN_POINT('Ctrl Pts',(36.1702730524089,-2.42560266602413,-3.09611434492741));
#85431=CARTESIAN_POINT('Ctrl Pts',(36.1686783077962,-2.45020117753265,-3.07668405622527));
#85432=CARTESIAN_POINT('Ctrl Pts',(36.1670835631835,-2.47455308725801,-3.0569717071543));
#85433=CARTESIAN_POINT('Ctrl Pts',(36.1612882209238,-2.5630485431541,-2.9853365320287));
#85434=CARTESIAN_POINT('Ctrl Pts',(36.155492878664,-2.64859779005247,-2.90971999295362));
#85435=CARTESIAN_POINT('Ctrl Pts',(36.1496975364043,-2.73081386313657,-2.83039655258784));
#85436=CARTESIAN_POINT('Ctrl Pts',(36.1439097363987,-2.81292293744588,-2.75117634642691));
#85437=CARTESIAN_POINT('Ctrl Pts',(36.1381219363931,-2.89170715676281,-2.66825911971025));
#85438=CARTESIAN_POINT('Ctrl Pts',(36.1323341363876,-2.96681105847508,-2.58196071684098));
#85439=CARTESIAN_POINT('Ctrl Pts',(36.1264020274562,-3.04378754793543,-2.49351061042225));
#85440=CARTESIAN_POINT('Ctrl Pts',(36.1204699185248,-3.1168973971269,-2.40150874837553));
#85441=CARTESIAN_POINT('Ctrl Pts',(36.1145378095935,-3.18579619034485,-2.30633727663243));
#85442=CARTESIAN_POINT('Ctrl Pts',(36.1087601655715,-3.25290094269537,-2.21364395438578));
#85443=CARTESIAN_POINT('Ctrl Pts',(36.1029825215496,-3.31601096819452,-2.1179444200756));
#85444=CARTESIAN_POINT('Ctrl Pts',(36.0972048775276,-3.37484808622337,-2.0196260532372));
#85445=CARTESIAN_POINT('Ctrl Pts',(36.0914293147106,-3.43366401012889,-1.92134310233455));
#85446=CARTESIAN_POINT('Ctrl Pts',(36.0856537518936,-3.48820986723053,-1.82044355797122));
#85447=CARTESIAN_POINT('Ctrl Pts',(36.0798781890765,-3.53825118769959,-1.71734316103173));
#85448=CARTESIAN_POINT('Ctrl Pts',(36.0741032215919,-3.58828735001918,-1.61425339145483));
#85449=CARTESIAN_POINT('Ctrl Pts',(36.0683282541072,-3.63381971388977,-1.508963603127));
#85450=CARTESIAN_POINT('Ctrl Pts',(36.0625532866225,-3.67466050355064,-1.40191268759684));
#85451=CARTESIAN_POINT('Ctrl Pts',(36.0565041395735,-3.71744030151651,-1.28977928918629));
#85452=CARTESIAN_POINT('Ctrl Pts',(36.0504549925246,-3.75507186446882,-1.17571388591425));
#85453=CARTESIAN_POINT('Ctrl Pts',(36.0444058454756,-3.78739718369451,-1.06024128053141));
#85454=CARTESIAN_POINT('Ctrl Pts',(36.0386247027133,-3.81829034660931,-0.949884628354775));
#85455=CARTESIAN_POINT('Ctrl Pts',(36.0328435599511,-3.84433734512878,-0.838243238474594));
#85456=CARTESIAN_POINT('Ctrl Pts',(36.0270624171888,-3.8654524764882,-0.725786574697586));
#85457=CARTESIAN_POINT('Ctrl Pts',(36.0212780528597,-3.88657937434611,-0.613267243957136));
#85458=CARTESIAN_POINT('Ctrl Pts',(36.0154936885306,-3.90276887576901,-0.499932155174765));
#85459=CARTESIAN_POINT('Ctrl Pts',(36.0097093242014,-3.91398711034839,-0.38625626211963));
#85460=CARTESIAN_POINT('Ctrl Pts',(36.0039176492429,-3.9252195232109,-0.272436698597958));
#85461=CARTESIAN_POINT('Ctrl Pts',(35.9981259742844,-3.93146811458794,-0.158275894357944));
#85462=CARTESIAN_POINT('Ctrl Pts',(35.992334299326,-3.93275107682362,-0.0442489292822916));
#85463=CARTESIAN_POINT('Ctrl Pts',(35.9915440402289,-3.93292613370875,-0.0286902442554935));
#85464=CARTESIAN_POINT('Ctrl Pts',(35.9907537811319,-3.93300881996226,-0.0131340427485895));
#85465=CARTESIAN_POINT('Ctrl Pts',(35.9899635220349,-3.93299925641567,0.00241847757537678));
#85466=CARTESIAN_POINT('',(34.739963522035,-3.93332081374984,-0.00333872239636136));
#85467=CARTESIAN_POINT('Ctrl Pts',(35.9899635220349,-3.93762631029128,0.0024213228406085));
#85468=CARTESIAN_POINT('Ctrl Pts',(35.9827211295046,-3.9386567952212,0.145122008460187));
#85469=CARTESIAN_POINT('Ctrl Pts',(35.9091963307278,-3.86675733052379,1.59277050702035));
#85470=CARTESIAN_POINT('Ctrl Pts',(35.7693891257042,-2.07371529249546,4.1638557740525));
#85471=CARTESIAN_POINT('Ctrl Pts',(35.5705419069645,2.38139350245334,3.99586724101343));
#85472=CARTESIAN_POINT('Ctrl Pts',(35.371694688225,4.6490029931939,0.157356889391723));
#85473=CARTESIAN_POINT('Ctrl Pts',(35.1728474694854,2.64613353856358,-3.82569827841376));
#85474=CARTESIAN_POINT('Ctrl Pts',(34.9740002507456,-1.78741999599338,-4.29454535187287));
#85475=CARTESIAN_POINT('Ctrl Pts',(34.8297056015956,-3.81320887697328,-1.77214066905022));
#85476=CARTESIAN_POINT('Ctrl Pts',(34.751693358692,-3.93732144507338,-0.234826367187542));
#85477=CARTESIAN_POINT('Ctrl Pts',(34.739963522035,-3.93522822798615,-0.00334034146760698));
#85478=CARTESIAN_POINT('',(33.4899635468833,-3.93061375975798,-0.000796215185199833));
#85479=CARTESIAN_POINT('Ctrl Pts',(34.739963522035,-3.93299858311176,-0.00333844887719042));
#85480=CARTESIAN_POINT('Ctrl Pts',(34.7341874476538,-3.93309528539993,0.110585704628955));
#85481=CARTESIAN_POINT('Ctrl Pts',(34.7284113732727,-3.92823788115257,0.224683591804017));
#85482=CARTESIAN_POINT('Ctrl Pts',(34.7226352988915,-3.91840775789089,0.338481377479638));
#85483=CARTESIAN_POINT('Ctrl Pts',(34.7168647659296,-3.90858706540015,0.452169988445717));
#85484=CARTESIAN_POINT('Ctrl Pts',(34.7110942329677,-3.89380317397632,0.565558647516841));
#85485=CARTESIAN_POINT('Ctrl Pts',(34.7053237000058,-3.87408952563053,0.678173537820377));
#85486=CARTESIAN_POINT('Ctrl Pts',(34.6995567654491,-3.85438817037686,0.790718203414797));
#85487=CARTESIAN_POINT('Ctrl Pts',(34.6937898308923,-3.82976324162912,0.902489640128141));
#85488=CARTESIAN_POINT('Ctrl Pts',(34.6880228963355,-3.8002999313102,1.0130199564094));
#85489=CARTESIAN_POINT('Ctrl Pts',(34.6822577349691,-3.77084568023356,1.12351628734061));
#85490=CARTESIAN_POINT('Ctrl Pts',(34.6764925736027,-3.73655611310215,1.23277184402113));
#85491=CARTESIAN_POINT('Ctrl Pts',(34.6707274122363,-3.69756718542943,1.34033052238448));
#85492=CARTESIAN_POINT('Ctrl Pts',(34.6649625312168,-3.65858015370136,1.44788397040904));
#85493=CARTESIAN_POINT('Ctrl Pts',(34.6591976501973,-3.6148943615961,1.55374030305034));
#85494=CARTESIAN_POINT('Ctrl Pts',(34.6534327691778,-3.56669483819284,1.65746098934742));
#85495=CARTESIAN_POINT('Ctrl Pts',(34.6476666761293,-3.51848518115074,1.76120348224966));
#85496=CARTESIAN_POINT('Ctrl Pts',(34.6419005830808,-3.4657600879619,1.86280905011959));
#85497=CARTESIAN_POINT('Ctrl Pts',(34.6361344900323,-3.40875129601817,1.96186227903348));
#85498=CARTESIAN_POINT('Ctrl Pts',(34.6303623658268,-3.3516828746216,2.06101911459542));
#85499=CARTESIAN_POINT('Ctrl Pts',(34.6245902416213,-3.29032202516318,2.15761791282369));
#85500=CARTESIAN_POINT('Ctrl Pts',(34.6188181174158,-3.22494467578866,2.25127093840399));
#85501=CARTESIAN_POINT('Ctrl Pts',(34.6130425610421,-3.15952845232737,2.3449796510973));
#85502=CARTESIAN_POINT('Ctrl Pts',(34.6072670046685,-3.09009123587556,2.43573876783277));
#85503=CARTESIAN_POINT('Ctrl Pts',(34.6014914482948,-3.01694901452852,2.52319393700432));
#85504=CARTESIAN_POINT('Ctrl Pts',(34.5957072109202,-2.94369685612108,2.61078055643865));
#85505=CARTESIAN_POINT('Ctrl Pts',(34.5899229735457,-2.86672886659721,2.69505300422099));
#85506=CARTESIAN_POINT('Ctrl Pts',(34.5841387361711,-2.7863975975899,2.77569404440497));
#85507=CARTESIAN_POINT('Ctrl Pts',(34.5815277618695,-2.75013648563879,2.81209498543454));
#85508=CARTESIAN_POINT('Ctrl Pts',(34.5789167875679,-2.71319052644958,2.84775655000578));
#85509=CARTESIAN_POINT('Ctrl Pts',(34.5763058132664,-2.6755942070439,2.88265236184197));
#85510=CARTESIAN_POINT('Ctrl Pts',(34.5704333671324,-2.59103482995219,2.96113791996639));
#85511=CARTESIAN_POINT('Ctrl Pts',(34.5645609209985,-2.50287752499796,3.0360310441156));
#85512=CARTESIAN_POINT('Ctrl Pts',(34.5586884748646,-2.41146027973897,3.10698379771142));
#85513=CARTESIAN_POINT('Ctrl Pts',(34.5528236359197,-2.32016145672751,3.17784463884011));
#85514=CARTESIAN_POINT('Ctrl Pts',(34.5469587969749,-2.22561141486791,3.2447750090869));
#85515=CARTESIAN_POINT('Ctrl Pts',(34.5410939580301,-2.12818418966159,3.30746444499022));
#85516=CARTESIAN_POINT('Ctrl Pts',(34.53523514791,-2.03085711582818,3.37008943860792));
#85517=CARTESIAN_POINT('Ctrl Pts',(34.52937633779,-1.93065908706628,3.42848194686668));
#85518=CARTESIAN_POINT('Ctrl Pts',(34.52351752767,-1.82799581784233,3.48237279594689));
#85519=CARTESIAN_POINT('Ctrl Pts',(34.517431738789,-1.72135522537966,3.53835145430905));
#85520=CARTESIAN_POINT('Ctrl Pts',(34.511345949908,-1.61205487419881,3.58947231887924));
#85521=CARTESIAN_POINT('Ctrl Pts',(34.5052601610271,-1.50058129174565,3.63548412001249));
#85522=CARTESIAN_POINT('Ctrl Pts',(34.4994081309488,-1.39338947648432,3.67972858025478));
#85523=CARTESIAN_POINT('Ctrl Pts',(34.4935561008705,-1.28418871798513,3.71924904926795));
#85524=CARTESIAN_POINT('Ctrl Pts',(34.4877040707923,-1.17343432618692,3.7538701205724));
#85525=CARTESIAN_POINT('Ctrl Pts',(34.4818529304137,-1.06269677267447,3.78848592834298));
#85526=CARTESIAN_POINT('Ctrl Pts',(34.4760017900352,-0.950406449934469,
3.81820369615239));
#85527=CARTESIAN_POINT('Ctrl Pts',(34.4701506496567,-0.837034939327708,
3.84289754096367));
#85528=CARTESIAN_POINT('Ctrl Pts',(34.4642989820892,-0.723653213923857,
3.8675936106956));
#85529=CARTESIAN_POINT('Ctrl Pts',(34.4584473145217,-0.609190510912237,
3.88726476961269));
#85530=CARTESIAN_POINT('Ctrl Pts',(34.4525956469542,-0.494129040508674,
3.90183616920623));
#85531=CARTESIAN_POINT('Ctrl Pts',(34.44674203527,-0.379029342894668,3.91641240989868));
#85532=CARTESIAN_POINT('Ctrl Pts',(34.4408884235858,-0.263330892192644,
3.9258854703341));
#85533=CARTESIAN_POINT('Ctrl Pts',(34.4350348119016,-0.147520749006666,
3.93023238862698));
#85534=CARTESIAN_POINT('Ctrl Pts',(34.4291745458017,-0.0315789522580382,
3.93458424851878));
#85535=CARTESIAN_POINT('Ctrl Pts',(34.4233142797018,0.0844743770975343,
3.93379831940984));
#85536=CARTESIAN_POINT('Ctrl Pts',(34.4174540136019,0.200152345972468,3.92790377153027));
#85537=CARTESIAN_POINT('Ctrl Pts',(34.4115898004306,0.315908227555552,3.92200525348945));
#85538=CARTESIAN_POINT('Ctrl Pts',(34.4057255872593,0.431287834768613,3.91099130451018));
#85539=CARTESIAN_POINT('Ctrl Pts',(34.399861374088,0.545811300767073,3.89494274976603));
#85540=CARTESIAN_POINT('Ctrl Pts',(34.3939885255137,0.660503409386893,3.87887056256963));
#85541=CARTESIAN_POINT('Ctrl Pts',(34.3881156769395,0.774336455757687,3.85774904835337));
#85542=CARTESIAN_POINT('Ctrl Pts',(34.3822428283652,0.886842542971706,3.83170971029585));
#85543=CARTESIAN_POINT('Ctrl Pts',(34.3806480837524,0.917393045717129,3.82463884961164));
#85544=CARTESIAN_POINT('Ctrl Pts',(34.3790533391396,0.947845801617697,3.81720564399785));
#85545=CARTESIAN_POINT('Ctrl Pts',(34.3774585945268,0.978191679432268,3.80941334568585));
#85546=CARTESIAN_POINT('Ctrl Pts',(34.3715861483928,1.08993655157172,3.78071918881001));
#85547=CARTESIAN_POINT('Ctrl Pts',(34.3657137022589,1.20060487266298,3.74705595710973));
#85548=CARTESIAN_POINT('Ctrl Pts',(34.359841256125,1.30972120202169,3.70851983586105));
#85549=CARTESIAN_POINT('Ctrl Pts',(34.3539764171801,1.41869618167212,3.67003363445047));
#85550=CARTESIAN_POINT('Ctrl Pts',(34.3481115782352,1.52612278150101,3.62668723291229));
#85551=CARTESIAN_POINT('Ctrl Pts',(34.3422467392904,1.63153759205154,3.57862740247188));
#85552=CARTESIAN_POINT('Ctrl Pts',(34.3363879291703,1.73684404030358,3.53061697565574));
#85553=CARTESIAN_POINT('Ctrl Pts',(34.3305291190503,1.84014243886888,3.47790292779082));
#85554=CARTESIAN_POINT('Ctrl Pts',(34.3246703089303,1.94098698236471,3.42068100446252));
#85555=CARTESIAN_POINT('Ctrl Pts',(34.3185845200493,2.04573838903953,3.36124222122756));
#85556=CARTESIAN_POINT('Ctrl Pts',(34.3124987311684,2.14784153504624,3.29693936640616));
#85557=CARTESIAN_POINT('Ctrl Pts',(34.3064129422874,2.24682197974801,3.22804584715292));
#85558=CARTESIAN_POINT('Ctrl Pts',(34.3005609122091,2.34200052617568,3.16179856931368));
#85559=CARTESIAN_POINT('Ctrl Pts',(34.2947088821308,2.43429146524979,3.09130704008724));
#85560=CARTESIAN_POINT('Ctrl Pts',(34.2888568520526,2.52330105273017,3.01685942617332));
#85561=CARTESIAN_POINT('Ctrl Pts',(34.283005711674,2.61229710784553,2.94242313072873));
#85562=CARTESIAN_POINT('Ctrl Pts',(34.2771545712955,2.6980124863042,2.86403221160928));
#85563=CARTESIAN_POINT('Ctrl Pts',(34.2713034309169,2.78008630530296,2.78201530101237));
#85564=CARTESIAN_POINT('Ctrl Pts',(34.2654517633494,2.86216751916993,2.6999910006747));
#85565=CARTESIAN_POINT('Ctrl Pts',(34.2596000957819,2.94060622892761,2.61434035160873));
#85566=CARTESIAN_POINT('Ctrl Pts',(34.2537484282144,3.0150787353421,2.52542852199145));
#85567=CARTESIAN_POINT('Ctrl Pts',(34.2478948165302,3.08957598397633,2.43648715293561));
#85568=CARTESIAN_POINT('Ctrl Pts',(34.242041204846,3.16010414381335,2.34428276562728));
#85569=CARTESIAN_POINT('Ctrl Pts',(34.2361875931617,3.22638054045464,2.24921266406171));
#85570=CARTESIAN_POINT('Ctrl Pts',(34.2303273270618,3.29273228044229,2.1540344863189));
#85571=CARTESIAN_POINT('Ctrl Pts',(34.2244670609619,3.35482237334615,2.05598443123333));
#85572=CARTESIAN_POINT('Ctrl Pts',(34.218606794862,3.41241208934595,1.95548785025261));
#85573=CARTESIAN_POINT('Ctrl Pts',(34.2127425816907,3.47004059381008,1.85492358169993));
#85574=CARTESIAN_POINT('Ctrl Pts',(34.2068783685194,3.52316249676447,1.75190987261508));
#85575=CARTESIAN_POINT('Ctrl Pts',(34.2010141553481,3.57158632014928,1.64689409426426));
#85576=CARTESIAN_POINT('Ctrl Pts',(34.1951413067738,3.6200814504965,1.54172367392868));
#85577=CARTESIAN_POINT('Ctrl Pts',(34.1892684581995,3.66386453819004,1.43454568159406));
#85578=CARTESIAN_POINT('Ctrl Pts',(34.1833956096252,3.7027932082271,1.32582482142524));
#85579=CARTESIAN_POINT('Ctrl Pts',(34.1818008650125,3.71336410683561,1.29630217941409));
#85580=CARTESIAN_POINT('Ctrl Pts',(34.1802061203997,3.72357734493953,1.26666583930661));
#85581=CARTESIAN_POINT('Ctrl Pts',(34.178611375787,3.73343072098931,1.23692524089908));
#85582=CARTESIAN_POINT('Ctrl Pts',(34.1727389296531,3.76971453698585,1.12740923391896));
#85583=CARTESIAN_POINT('Ctrl Pts',(34.1668664835192,3.80123622077032,1.01611200164018));
#85584=CARTESIAN_POINT('Ctrl Pts',(34.1609940373853,3.82781960860819,0.903485497368166));
#85585=CARTESIAN_POINT('Ctrl Pts',(34.1551291984405,3.85436856022431,0.791004889898326));
#85586=CARTESIAN_POINT('Ctrl Pts',(34.1492643594956,3.87599184334496,0.677198833363267));
#85587=CARTESIAN_POINT('Ctrl Pts',(34.1433995205508,3.89256235299504,0.562536512633344));
#85588=CARTESIAN_POINT('Ctrl Pts',(34.1375407104308,3.90911582880992,0.447992060280275));
#85589=CARTESIAN_POINT('Ctrl Pts',(34.1316819003108,3.92062680364344,0.332593501161323));
#85590=CARTESIAN_POINT('Ctrl Pts',(34.1258230901908,3.92701888889182,0.216821692380688));
#85591=CARTESIAN_POINT('Ctrl Pts',(34.1197373013099,3.93365861274941,0.0965647166165378));
#85592=CARTESIAN_POINT('Ctrl Pts',(34.1136515124289,3.93477469457016,-0.0240945719776713));
#85593=CARTESIAN_POINT('Ctrl Pts',(34.1075657235479,3.93034059197947,-0.144609235661027));
#85594=CARTESIAN_POINT('Ctrl Pts',(34.1017136934697,3.92607680592999,-0.260494858796975));
#85595=CARTESIAN_POINT('Ctrl Pts',(34.0958616633914,3.91668135891694,-0.376246311069399));
#85596=CARTESIAN_POINT('Ctrl Pts',(34.0900096333132,3.9021837577946,-0.491376556628453));
#85597=CARTESIAN_POINT('Ctrl Pts',(34.0841584929347,3.88768836078124,-0.606489298629065));
#85598=CARTESIAN_POINT('Ctrl Pts',(34.0783073525562,3.86809240362079,-0.720980611694875));
#85599=CARTESIAN_POINT('Ctrl Pts',(34.0724562121776,3.84347720162034,-0.834369223200796));
#85600=CARTESIAN_POINT('Ctrl Pts',(34.0666045446102,3.81885978178503,-0.947768051044381));
#85601=CARTESIAN_POINT('Ctrl Pts',(34.0607528770427,3.78922230580551,-1.06006357584979));
#85602=CARTESIAN_POINT('Ctrl Pts',(34.0549012094752,3.75469692891723,-1.17078604876362));
#85603=CARTESIAN_POINT('Ctrl Pts',(34.049047597791,3.72016008156113,-1.2815453073313));
#85604=CARTESIAN_POINT('Ctrl Pts',(34.0431939861067,3.68073222721102,-1.39073008040158));
#85605=CARTESIAN_POINT('Ctrl Pts',(34.0373403744225,3.63659473658771,-1.49788775341231));
#85606=CARTESIAN_POINT('Ctrl Pts',(34.0314801083226,3.5924070702399,-1.60516724381235));
#85607=CARTESIAN_POINT('Ctrl Pts',(34.0256198422227,3.54349923885702,-1.71041465218157));
#85608=CARTESIAN_POINT('Ctrl Pts',(34.0197595761228,3.4900999682102,-1.81319916498413));
#85609=CARTESIAN_POINT('Ctrl Pts',(34.0138953629515,3.43666473149438,-1.91605290635171));
#85610=CARTESIAN_POINT('Ctrl Pts',(34.0080311497802,3.37873223798797,-2.01644009193294));
#85611=CARTESIAN_POINT('Ctrl Pts',(34.0021669366089,3.31657528624049,-2.11395775045265));
#85612=CARTESIAN_POINT('Ctrl Pts',(33.9962940880347,3.25432680468145,-2.21161900952961));
#85613=CARTESIAN_POINT('Ctrl Pts',(33.9904212394604,3.18784168595066,-2.30640197105836));
#85614=CARTESIAN_POINT('Ctrl Pts',(33.9845483908861,3.11743385971219,-2.39793559761724));
#85615=CARTESIAN_POINT('Ctrl Pts',(33.9829536462732,3.09831494319716,-2.42279112658315));
#85616=CARTESIAN_POINT('Ctrl Pts',(33.9813589016604,3.07890699213294,-2.44740726606919));
#85617=CARTESIAN_POINT('Ctrl Pts',(33.9797641570475,3.05921675695992,-2.47177705991775));
#85618=CARTESIAN_POINT('Ctrl Pts',(33.9738917109136,2.98670994647429,-2.56151575570399));
#85619=CARTESIAN_POINT('Ctrl Pts',(33.9680192647797,2.91012981974181,-2.64821163018046));
#85620=CARTESIAN_POINT('Ctrl Pts',(33.9621468186458,2.82976131037675,-2.73147211706341));
#85621=CARTESIAN_POINT('Ctrl Pts',(33.9562819797009,2.74949691068483,-2.81462474799453));
#85622=CARTESIAN_POINT('Ctrl Pts',(33.9504171407561,2.66545417203359,-2.8943505465603));
#85623=CARTESIAN_POINT('Ctrl Pts',(33.9445523018113,2.57795904995689,-2.97028889785916));
#85624=CARTESIAN_POINT('Ctrl Pts',(33.9386934916913,2.49055386944009,-3.046149187506));
#85625=CARTESIAN_POINT('Ctrl Pts',(33.9328346815713,2.3997036747864,-3.11822950465146));
#85626=CARTESIAN_POINT('Ctrl Pts',(33.9269758714512,2.30577166317804,-3.18620558616125));
#85627=CARTESIAN_POINT('Ctrl Pts',(33.9208900825703,2.20820058985354,-3.25681515918901));
#85628=CARTESIAN_POINT('Ctrl Pts',(33.9148042936893,2.10730439758311,-3.32299572996346));
#85629=CARTESIAN_POINT('Ctrl Pts',(33.9087185048083,2.00352882353616,-3.38442923596577));
#85630=CARTESIAN_POINT('Ctrl Pts',(33.90286647473,1.90373933155899,-3.44350304413928));
#85631=CARTESIAN_POINT('Ctrl Pts',(33.8970144446518,1.8012879636811,-3.49818750580618));
#85632=CARTESIAN_POINT('Ctrl Pts',(33.8911624145735,1.69660037345911,-3.54824409712444));
#85633=CARTESIAN_POINT('Ctrl Pts',(33.885311274195,1.59192869917097,-3.59829307820546));
#85634=CARTESIAN_POINT('Ctrl Pts',(33.8794601338165,1.48502185134508,-3.64371540963567));
#85635=CARTESIAN_POINT('Ctrl Pts',(33.873608993438,1.37632864882293,-3.68431926554));
#85636=CARTESIAN_POINT('Ctrl Pts',(33.8677573258705,1.2676256530206,-3.72492677986021));
#85637=CARTESIAN_POINT('Ctrl Pts',(33.861905658303,1.15713636981042,-3.76071481095275));
#85638=CARTESIAN_POINT('Ctrl Pts',(33.8560539907355,1.04532741380425,-3.79154053096486));
#85639=CARTESIAN_POINT('Ctrl Pts',(33.8502003790513,0.933481311179146,-3.82237649229677));
#85640=CARTESIAN_POINT('Ctrl Pts',(33.844346767367,0.820315062227955,-3.84824675451633));
#85641=CARTESIAN_POINT('Ctrl Pts',(33.8384931556828,0.706307479360857,-3.86905915496247));
#85642=CARTESIAN_POINT('Ctrl Pts',(33.8326328895829,0.592170292091333,-3.88989521505172));
#85643=CARTESIAN_POINT('Ctrl Pts',(33.826772623483,0.477190268775185,-3.90566186267629));
#85644=CARTESIAN_POINT('Ctrl Pts',(33.8209123573831,0.361853487965521,-3.91631855870372));
#85645=CARTESIAN_POINT('Ctrl Pts',(33.8150481442118,0.246439024248364,-3.92698243234722));
#85646=CARTESIAN_POINT('Ctrl Pts',(33.8091839310405,0.130667736450913,-3.93252948152007));
#85647=CARTESIAN_POINT('Ctrl Pts',(33.8033197178692,0.0150261125709177,
-3.9329712960993));
#85648=CARTESIAN_POINT('Ctrl Pts',(33.7974468692949,-0.100785800484037,
-3.9334137612768));
#85649=CARTESIAN_POINT('Ctrl Pts',(33.7915740207206,-0.216467257082468,
-3.92873600454368));
#85650=CARTESIAN_POINT('Ctrl Pts',(33.7857011721463,-0.33153639225403,-3.91900148259875));
#85651=CARTESIAN_POINT('Ctrl Pts',(33.7841064275335,-0.362782878707366,
-3.91635811861041));
#85652=CARTESIAN_POINT('Ctrl Pts',(33.7825116829207,-0.393984272536504,
-3.91334217583988));
#85653=CARTESIAN_POINT('Ctrl Pts',(33.7809169383078,-0.425131072127442,
-3.90995557155216));
#85654=CARTESIAN_POINT('Ctrl Pts',(33.7750444921739,-0.539825237807404,
-3.89748482790048));
#85655=CARTESIAN_POINT('Ctrl Pts',(33.76917204604,-0.65416223887964,-3.87994228967359));
#85656=CARTESIAN_POINT('Ctrl Pts',(33.7632995999061,-0.767657778564146,
-3.85735538095856));
#85657=CARTESIAN_POINT('Ctrl Pts',(33.7574347609612,-0.881006295694552,
-3.83479773141105));
#85658=CARTESIAN_POINT('Ctrl Pts',(33.7515699220164,-0.993515117454448,
-3.80720878610233));
#85659=CARTESIAN_POINT('Ctrl Pts',(33.7457050830715,-1.10470464387939,-3.77466775356339));
#85660=CARTESIAN_POINT('Ctrl Pts',(33.7398462729515,-1.21577987182446,-3.74216017193186));
#85661=CARTESIAN_POINT('Ctrl Pts',(33.7339874628314,-1.32553810762419,-3.7047107438636));
#85662=CARTESIAN_POINT('Ctrl Pts',(33.7281286527114,-1.4335101938042,-3.66244966166901));
#85663=CARTESIAN_POINT('Ctrl Pts',(33.7220428638304,-1.54566527445485,-3.61855132414855));
#85664=CARTESIAN_POINT('Ctrl Pts',(33.7159570749495,-1.65589256478992,-3.56946106006242));
#85665=CARTESIAN_POINT('Ctrl Pts',(33.7098712860685,-1.76368349313182,-3.51538184783024));
#85666=CARTESIAN_POINT('Ctrl Pts',(33.7040192559902,-1.86733410723615,-3.46337985059013));
#85667=CARTESIAN_POINT('Ctrl Pts',(33.698167225912,-1.96873166748688,-3.40676529501449));
#85668=CARTESIAN_POINT('Ctrl Pts',(33.6923151958337,-2.06744537026547,-3.3457672723858));
#85669=CARTESIAN_POINT('Ctrl Pts',(33.6864640554552,-2.16614406533622,-3.28477852344936));
#85670=CARTESIAN_POINT('Ctrl Pts',(33.6806129150767,-2.2621593626964,-3.21940784976893));
#85671=CARTESIAN_POINT('Ctrl Pts',(33.6747617746981,-2.35508721576678,-3.14992907954003));
#85672=CARTESIAN_POINT('Ctrl Pts',(33.6689101071306,-2.44802344165643,-3.08044404925919));
#85673=CARTESIAN_POINT('Ctrl Pts',(33.6630584395631,-2.53787133918501,-3.00685043415877));
#85674=CARTESIAN_POINT('Ctrl Pts',(33.6572067719956,-2.62425845699118,-2.92946352612731));
#85675=CARTESIAN_POINT('Ctrl Pts',(33.6513531603114,-2.71067427544373,-2.85205090761565));
#85676=CARTESIAN_POINT('Ctrl Pts',(33.6454995486272,-2.79362672017384,-2.77084276589168));
#85677=CARTESIAN_POINT('Ctrl Pts',(33.6396459369429,-2.8727793643566,-2.68619204892854));
#85678=CARTESIAN_POINT('Ctrl Pts',(33.633785670843,-2.95202198966969,-2.60144510059783));
#85679=CARTESIAN_POINT('Ctrl Pts',(33.6279254047431,-3.02745591010843,-2.51324806784514));
#85680=CARTESIAN_POINT('Ctrl Pts',(33.6220651386432,-3.0987841961425,-2.42198792435831));
#85681=CARTESIAN_POINT('Ctrl Pts',(33.6162009254719,-3.17016052399471,-2.33066631432769));
#85682=CARTESIAN_POINT('Ctrl Pts',(33.6103367123006,-3.23742547192394,-2.23627782131645));
#85683=CARTESIAN_POINT('Ctrl Pts',(33.6044724991293,-3.30032574039641,-2.13923795013011));
#85684=CARTESIAN_POINT('Ctrl Pts',(33.598599650555,-3.36331863325876,-2.04205518195652));
#85685=CARTESIAN_POINT('Ctrl Pts',(33.5927268019806,-3.42193381066567,-1.94221359850298));
#85686=CARTESIAN_POINT('Ctrl Pts',(33.5868539534063,-3.47596410363447,-1.84015286056474));
#85687=CARTESIAN_POINT('Ctrl Pts',(33.5852592087936,-3.49063577744745,-1.81243874365247));
#85688=CARTESIAN_POINT('Ctrl Pts',(33.5836644641809,-3.50496965262407,-1.78456110189523));
#85689=CARTESIAN_POINT('Ctrl Pts',(33.5820697195682,-3.51896220436475,-1.75652896482021));
#85690=CARTESIAN_POINT('Ctrl Pts',(33.5757828686536,-3.57412406915894,-1.64601981796256));
#85691=CARTESIAN_POINT('Ctrl Pts',(33.5694960177391,-3.62414209049564,-1.53277880180385));
#85692=CARTESIAN_POINT('Ctrl Pts',(33.5632091668245,-3.66875642446101,-1.41729153598547));
#85693=CARTESIAN_POINT('Ctrl Pts',(33.5569419548774,-3.71323139144215,-1.30216503117198));
#85694=CARTESIAN_POINT('Ctrl Pts',(33.5506747429303,-3.75233621169791,-1.18480656813154));
#85695=CARTESIAN_POINT('Ctrl Pts',(33.5444075309832,-3.78585837643043,-1.06572292534765));
#85696=CARTESIAN_POINT('Ctrl Pts',(33.5381521325137,-3.81931735304266,-0.946863751108828));
#85697=CARTESIAN_POINT('Ctrl Pts',(33.5318967340443,-3.84721455081169,-0.82628618464541));
#85698=CARTESIAN_POINT('Ctrl Pts',(33.5256413355748,-3.86938585152948,-0.704515529980335));
#85699=CARTESIAN_POINT('Ctrl Pts',(33.5194037340276,-3.89149407378478,-0.58309131893491));
#85700=CARTESIAN_POINT('Ctrl Pts',(33.5131661324805,-3.9079088197401,-0.460481103916105));
#85701=CARTESIAN_POINT('Ctrl Pts',(33.5069285309334,-3.91851629497949,-0.337222546666419));
#85702=CARTESIAN_POINT('Ctrl Pts',(33.5012735412267,-3.92813299826519,-0.225476731027766));
#85703=CARTESIAN_POINT('Ctrl Pts',(33.4956185515199,-3.93297714188587,-0.113198403560563));
#85704=CARTESIAN_POINT('Ctrl Pts',(33.4899635618132,-3.93299991924726,-0.00079699499911527));
#85705=CARTESIAN_POINT('',(32.2399635002821,-3.93299832602929,0.00362869822633291));
#85706=CARTESIAN_POINT('Ctrl Pts',(33.489963522035,-3.92664241618237,-0.000794917321835231));
#85707=CARTESIAN_POINT('Ctrl Pts',(33.4543831816328,-3.92537167507928,0.70527486915122));
#85708=CARTESIAN_POINT('Ctrl Pts',(33.3525204349843,-3.40567834183995,2.72842261129244));
#85709=CARTESIAN_POINT('Ctrl Pts',(33.1843752820887,-0.161577020458298,
4.64885823486118));
#85710=CARTESIAN_POINT('Ctrl Pts',(32.9855280633493,3.82329463833261,2.64960527812334));
#85711=CARTESIAN_POINT('Ctrl Pts',(32.7866808446095,4.29616613733598,-1.78352082740046));
#85712=CARTESIAN_POINT('Ctrl Pts',(32.5878336258701,0.822667401222829,-4.5783412245405));
#85713=CARTESIAN_POINT('Ctrl Pts',(32.4055945183451,-3.05328697462271,-3.28541975544593));
#85714=CARTESIAN_POINT('Ctrl Pts',(32.2896378170668,-3.92337245183106,-0.978557300575992));
#85715=CARTESIAN_POINT('Ctrl Pts',(32.239963522035,-3.93230204247149,0.00362762571011338));
#85716=CARTESIAN_POINT('',(30.9899635219853,-3.93299990487155,-0.000865032002295244));
#85717=CARTESIAN_POINT('Ctrl Pts',(32.2399635002821,-3.93299832602929,0.00362869822633291));
#85718=CARTESIAN_POINT('Ctrl Pts',(32.2324495091862,-3.93286122768884,0.152224009785864));
#85719=CARTESIAN_POINT('Ctrl Pts',(32.2249355180902,-3.92429936199548,0.300442608336801));
#85720=CARTESIAN_POINT('Ctrl Pts',(32.2174215269942,-3.90746138941711,0.447475686730029));
#85721=CARTESIAN_POINT('Ctrl Pts',(32.2097357398829,-3.89023844212168,0.597870453562282));
#85722=CARTESIAN_POINT('Ctrl Pts',(32.2020499527715,-3.86435660804196,0.747025156214954));
#85723=CARTESIAN_POINT('Ctrl Pts',(32.1943641656602,-3.83002292530235,0.894099206832475));
#85724=CARTESIAN_POINT('Ctrl Pts',(32.1929558399037,-3.82373170112221,0.921048713837953));
#85725=CARTESIAN_POINT('Ctrl Pts',(32.1915475141471,-3.81715682519089,0.947928419918569));
#85726=CARTESIAN_POINT('Ctrl Pts',(32.1901391883906,-3.81029974298554,0.974733229455291));
#85727=CARTESIAN_POINT('Ctrl Pts',(32.1842667422567,-3.78170703586469,1.08650410306624));
#85728=CARTESIAN_POINT('Ctrl Pts',(32.1783942961228,-3.74814427871285,1.19720293681802));
#85729=CARTESIAN_POINT('Ctrl Pts',(32.1725218499888,-3.70970722517867,1.30635420290868));
#85730=CARTESIAN_POINT('Ctrl Pts',(32.166657011044,-3.67131996314989,1.41536407403392));
#85731=CARTESIAN_POINT('Ctrl Pts',(32.1607921720991,-3.62807109743308,1.52282997788857));
#85732=CARTESIAN_POINT('Ctrl Pts',(32.1549273331542,-3.58010697852691,1.62828837197314));
#85733=CARTESIAN_POINT('Ctrl Pts',(32.1490685230342,-3.5321921648571,1.73363835895746));
#85734=CARTESIAN_POINT('Ctrl Pts',(32.1432097129142,-3.47957190924197,1.83698456685857));
#85735=CARTESIAN_POINT('Ctrl Pts',(32.1373509027941,-3.42244155250033,1.93788101278668));
#85736=CARTESIAN_POINT('Ctrl Pts',(32.1312651139132,-3.36309788327394,2.04268633266862));
#85737=CARTESIAN_POINT('Ctrl Pts',(32.1251793250322,-3.29888774047044,2.14484780840094));
#85738=CARTESIAN_POINT('Ctrl Pts',(32.1190935361512,-3.23008410045181,2.2438907513532));
#85739=CARTESIAN_POINT('Ctrl Pts',(32.113241506073,-3.16392324953187,2.33912939543602));
#85740=CARTESIAN_POINT('Ctrl Pts',(32.1073894759947,-3.09351552770848,2.43148428613212));
#85741=CARTESIAN_POINT('Ctrl Pts',(32.1015374459164,-3.0191487441359,2.52056141777633));
#85742=CARTESIAN_POINT('Ctrl Pts',(32.0956863055379,-2.94479326674391,2.60962500678647));
#85743=CARTESIAN_POINT('Ctrl Pts',(32.0898351651594,-2.86648018922745,2.69541151035522));
#85744=CARTESIAN_POINT('Ctrl Pts',(32.0839840247809,-2.78453781605224,2.7775597475077));
#85745=CARTESIAN_POINT('Ctrl Pts',(32.0781323572134,-2.70258805985182,2.85971538623378));
#85746=CARTESIAN_POINT('Ctrl Pts',(32.0722806896459,-2.61700864988439,2.93823181421886));
#85747=CARTESIAN_POINT('Ctrl Pts',(32.0664290220784,-2.52816446033411,3.01278500087602));
#85748=CARTESIAN_POINT('Ctrl Pts',(32.0605754103941,-2.43929075381722,3.08736295655783));
#85749=CARTESIAN_POINT('Ctrl Pts',(32.0547217987099,-2.34715042739772,3.15797478712707));
#85750=CARTESIAN_POINT('Ctrl Pts',(32.0488681870256,-2.25214052830562,3.22433745764355));
#85751=CARTESIAN_POINT('Ctrl Pts',(32.0430079209257,-2.15702262147515,3.29077556958269));
#85752=CARTESIAN_POINT('Ctrl Pts',(32.0371476548258,-2.0590289699169,3.35295464317976));
#85753=CARTESIAN_POINT('Ctrl Pts',(32.0312873887259,-1.95858470819298,3.41063556259425));
#85754=CARTESIAN_POINT('Ctrl Pts',(32.0254231755546,-1.85807279413596,3.46835533190128));
#85755=CARTESIAN_POINT('Ctrl Pts',(32.0195589623833,-1.75510734962699,3.52157072506845));
#85756=CARTESIAN_POINT('Ctrl Pts',(32.013694749212,-1.65013557193111,3.57008985800744));
#85757=CARTESIAN_POINT('Ctrl Pts',(32.0078219006377,-1.54500921704376,3.61868043825796));
#85758=CARTESIAN_POINT('Ctrl Pts',(32.0019490520634,-1.4378710135635,3.66256080019713));
#85759=CARTESIAN_POINT('Ctrl Pts',(31.9960762034891,-1.32918553622086,3.70158814703922));
#85760=CARTESIAN_POINT('Ctrl Pts',(31.9944814588765,-1.29967250225172,3.71218584087319));
#85761=CARTESIAN_POINT('Ctrl Pts',(31.9928867142638,-1.2700454455619,3.72242597756096));
#85762=CARTESIAN_POINT('Ctrl Pts',(31.9912919696511,-1.2403138039453,3.73230634698476));
#85763=CARTESIAN_POINT('Ctrl Pts',(31.9854195235172,-1.13083077921645,3.76868956268156));
#85764=CARTESIAN_POINT('Ctrl Pts',(31.9795470773833,-1.01956220703233,3.80031226505993));
#85765=CARTESIAN_POINT('Ctrl Pts',(31.9736746312493,-0.906959880597128,
3.82699788019111));
#85766=CARTESIAN_POINT('Ctrl Pts',(31.9678097923045,-0.794503419644181,
3.85364892667488));
#85767=CARTESIAN_POINT('Ctrl Pts',(31.9619449533597,-0.680717038829331,
3.8753755098871));
#85768=CARTESIAN_POINT('Ctrl Pts',(31.9560801144148,-0.566069807448353,
3.89205009899608));
#85769=CARTESIAN_POINT('Ctrl Pts',(31.9502213042948,-0.451540428932859,
3.90870754728025));
#85770=CARTESIAN_POINT('Ctrl Pts',(31.9443624941748,-0.336152366604314,
3.92032327198773));
#85771=CARTESIAN_POINT('Ctrl Pts',(31.9385036840548,-0.220386408026008,
3.92682044804157));
#85772=CARTESIAN_POINT('Ctrl Pts',(31.9324178951738,-0.100135509109817,
3.9335693340741));
#85773=CARTESIAN_POINT('Ctrl Pts',(31.9263321062928,0.0205227166320908,
3.9347949455506));
#85774=CARTESIAN_POINT('Ctrl Pts',(31.9202463174118,0.141041355778371,3.93047024361719));
#85775=CARTESIAN_POINT('Ctrl Pts',(31.9143942873336,0.256930801677664,3.92631165608009));
#85776=CARTESIAN_POINT('Ctrl Pts',(31.9085422572553,0.372690735103975,3.91702128789831));
#85777=CARTESIAN_POINT('Ctrl Pts',(31.902690227177,0.487834093622869,3.9026282038005));
#85778=CARTESIAN_POINT('Ctrl Pts',(31.8968390867985,0.602959946589611,3.8882373079217));
#85779=CARTESIAN_POINT('Ctrl Pts',(31.89098794642,0.717469000980662,3.86874528988671));
#85780=CARTESIAN_POINT('Ctrl Pts',(31.8851368060415,0.830879910554138,3.84423302808734));
#85781=CARTESIAN_POINT('Ctrl Pts',(31.879285138474,0.944301038474486,3.81971855772801));
#85782=CARTESIAN_POINT('Ctrl Pts',(31.8734334709065,1.05662342083569,3.7901830317544));
#85783=CARTESIAN_POINT('Ctrl Pts',(31.867581803339,1.16737718901218,3.7557581789266));
#85784=CARTESIAN_POINT('Ctrl Pts',(31.8617281916547,1.27816775323912,3.72132188902859));
#85785=CARTESIAN_POINT('Ctrl Pts',(31.8558745799705,1.38738827249572,3.68199316489111));
#85786=CARTESIAN_POINT('Ctrl Pts',(31.8500209682862,1.49458596776459,3.63795296629316));
#85787=CARTESIAN_POINT('Ctrl Pts',(31.8441607021864,1.60190552592078,3.59386270257257));
#85788=CARTESIAN_POINT('Ctrl Pts',(31.8383004360865,1.70719728767763,3.5450504311115));
#85789=CARTESIAN_POINT('Ctrl Pts',(31.8324401699866,1.81003023204784,3.49174448650998));
#85790=CARTESIAN_POINT('Ctrl Pts',(31.8265759568153,1.91293243760318,3.43840263869747));
#85791=CARTESIAN_POINT('Ctrl Pts',(31.8207117436439,2.01337217083464,3.38056129689765));
#85792=CARTESIAN_POINT('Ctrl Pts',(31.8148475304726,2.11094621299648,3.31849289374496));
#85793=CARTESIAN_POINT('Ctrl Pts',(31.8089746818983,2.20866393874395,3.25633309117372));
#85794=CARTESIAN_POINT('Ctrl Pts',(31.8031018333241,2.3035072139943,3.18993404036242));
#85795=CARTESIAN_POINT('Ctrl Pts',(31.7972289847498,2.39510471650483,3.11960933403148));
#85796=CARTESIAN_POINT('Ctrl Pts',(31.795634240137,2.41997759068629,3.10051298833999));
#85797=CARTESIAN_POINT('Ctrl Pts',(31.7940394955241,2.44461133786158,3.08112739090936));
#85798=CARTESIAN_POINT('Ctrl Pts',(31.7924447509113,2.46899899574816,3.06145928586263));
#85799=CARTESIAN_POINT('Ctrl Pts',(31.7865723047774,2.55880347360716,2.98903396677659));
#85800=CARTESIAN_POINT('Ctrl Pts',(31.7806998586435,2.64556882901847,2.91253257095941));
#85801=CARTESIAN_POINT('Ctrl Pts',(31.7748274125096,2.72890223720773,2.83223967555055));
#85802=CARTESIAN_POINT('Ctrl Pts',(31.7689625735647,2.81212769498282,2.75205079186402));
#85803=CARTESIAN_POINT('Ctrl Pts',(31.7630977346199,2.89192975164321,2.66808046002105));
#85804=CARTESIAN_POINT('Ctrl Pts',(31.757232895675,2.96794749654531,2.58065430806809));
#85805=CARTESIAN_POINT('Ctrl Pts',(31.751374085555,3.04388709818183,2.49331802677652));
#85806=CARTESIAN_POINT('Ctrl Pts',(31.745515275435,3.11604985613295,2.40253330144581));
#85807=CARTESIAN_POINT('Ctrl Pts',(31.7396564653149,3.18411117770079,2.30866303475429));
#85808=CARTESIAN_POINT('Ctrl Pts',(31.733570676434,3.25480929310917,2.21115609843426));
#85809=CARTESIAN_POINT('Ctrl Pts',(31.727484887553,3.32108142651117,2.11032002405109));
#85810=CARTESIAN_POINT('Ctrl Pts',(31.721399098672,3.38260911089501,2.00660025986494));
#85811=CARTESIAN_POINT('Ctrl Pts',(31.7155470685938,3.44177348000197,1.90686443405825));
#85812=CARTESIAN_POINT('Ctrl Pts',(31.7096950385155,3.49655092076498,1.80446274895838));
#85813=CARTESIAN_POINT('Ctrl Pts',(31.7038430084372,3.54670252304745,1.69982064142333));
#85814=CARTESIAN_POINT('Ctrl Pts',(31.6979918680587,3.59684650064796,1.59519444290721));
#85815=CARTESIAN_POINT('Ctrl Pts',(31.6921407276802,3.64236585951319,1.48832887186991));
#85816=CARTESIAN_POINT('Ctrl Pts',(31.6862895873017,3.68306836642569,1.37967257283546));
#85817=CARTESIAN_POINT('Ctrl Pts',(31.6804379197342,3.72377454064267,1.27100648384548));
#85818=CARTESIAN_POINT('Ctrl Pts',(31.6745862521667,3.75966285514443,1.16054973323197));
#85819=CARTESIAN_POINT('Ctrl Pts',(31.6687345845992,3.79059005856127,1.04876880576058));
#85820=CARTESIAN_POINT('Ctrl Pts',(31.662880972915,3.82152753701391,0.936950740982704));
#85821=CARTESIAN_POINT('Ctrl Pts',(31.6570273612307,3.84750051678102,0.823808022741547));
#85822=CARTESIAN_POINT('Ctrl Pts',(31.6511737495465,3.86841640059097,0.709819379588075));
#85823=CARTESIAN_POINT('Ctrl Pts',(31.6453134834466,3.88935606168445,0.595701153562978));
#85824=CARTESIAN_POINT('Ctrl Pts',(31.6394532173467,3.90522707749785,0.480735490010174));
#85825=CARTESIAN_POINT('Ctrl Pts',(31.6335929512468,3.915988467671,0.365408430482562));
#85826=CARTESIAN_POINT('Ctrl Pts',(31.6277287380755,3.926757105975,0.250003694594859));
#85827=CARTESIAN_POINT('Ctrl Pts',(31.6218645249042,3.93240924582848,0.13423748990664));
#85828=CARTESIAN_POINT('Ctrl Pts',(31.6160003117329,3.93295603548759,0.0185963147360922));
#85829=CARTESIAN_POINT('Ctrl Pts',(31.6101274631586,3.93350363032702,-0.0972151489489237));
#85830=CARTESIAN_POINT('Ctrl Pts',(31.6042546145843,3.92893088694179,-0.212900804182463));
#85831=CARTESIAN_POINT('Ctrl Pts',(31.59838176601,3.91930082458506,-0.327978728589047));
#85832=CARTESIAN_POINT('Ctrl Pts',(31.5967870213972,3.91668582611037,-0.359227601716395));
#85833=CARTESIAN_POINT('Ctrl Pts',(31.5951922767845,3.91369820807359,-0.390431720451608));
#85834=CARTESIAN_POINT('Ctrl Pts',(31.5935975321717,3.91033987911371,-0.421581581444166));
#85835=CARTESIAN_POINT('Ctrl Pts',(31.5877250860378,3.89797325579415,-0.536287020355445));
#85836=CARTESIAN_POINT('Ctrl Pts',(31.5818526399039,3.88053451576804,-0.650639898796893));
#85837=CARTESIAN_POINT('Ctrl Pts',(31.57598019377,3.85805064348412,-0.764155895293471));
#85838=CARTESIAN_POINT('Ctrl Pts',(31.5701153548252,3.83559589689393,-0.877524842736153));
#85839=CARTESIAN_POINT('Ctrl Pts',(31.5642505158803,3.80810909437062,-0.990058662381687));
#85840=CARTESIAN_POINT('Ctrl Pts',(31.5583856769355,3.77566900904911,-1.10127768256061));
#85841=CARTESIAN_POINT('Ctrl Pts',(31.5525268668155,3.74326227086528,-1.21238237394107));
#85842=CARTESIAN_POINT('Ctrl Pts',(31.5466680566955,3.7059124927633,-1.32217455974736));
#85843=CARTESIAN_POINT('Ctrl Pts',(31.5408092465755,3.66374944111582,-1.43018496451457));
#85844=CARTESIAN_POINT('Ctrl Pts',(31.5347234576945,3.61995293198713,-1.54237984827041));
#85845=CARTESIAN_POINT('Ctrl Pts',(31.5286376688135,3.57096274845395,-1.65265165554713));
#85846=CARTESIAN_POINT('Ctrl Pts',(31.5225518799326,3.5169814071894,-1.76049163062028));
#85847=CARTESIAN_POINT('Ctrl Pts',(31.5166998498543,3.46507352163452,-1.8641894075411));
#85848=CARTESIAN_POINT('Ctrl Pts',(31.510847819776,3.40855103440419,-1.96563831864943));
#85849=CARTESIAN_POINT('Ctrl Pts',(31.5049957896978,3.34764264561864,-2.06440735254344));
#85850=CARTESIAN_POINT('Ctrl Pts',(31.4991446493193,3.28674351689803,-2.16316137031758));
#85851=CARTESIAN_POINT('Ctrl Pts',(31.4932935089408,3.22146002934798,-2.25923596923873));
#85852=CARTESIAN_POINT('Ctrl Pts',(31.4874423685623,3.15206564427238,-2.35222685432289));
#85853=CARTESIAN_POINT('Ctrl Pts',(31.4815907009948,3.08266500674803,-2.44522611790543));
#85854=CARTESIAN_POINT('Ctrl Pts',(31.4757390334273,3.00915298262472,-2.53514078402328));
#85855=CARTESIAN_POINT('Ctrl Pts',(31.4698873658598,2.93184452556327,-2.62159811525808));
#85856=CARTESIAN_POINT('Ctrl Pts',(31.4640337541756,2.85451038408561,-2.70808417046646));
#85857=CARTESIAN_POINT('Ctrl Pts',(31.4581801424913,2.77337757703474,-2.79111029881737));
#85858=CARTESIAN_POINT('Ctrl Pts',(31.4523265308071,2.68879874684229,-2.87033975323119));
#85859=CARTESIAN_POINT('Ctrl Pts',(31.4464662647072,2.60412376700378,-2.94965927609339));
#85860=CARTESIAN_POINT('Ctrl Pts',(31.4406059986074,2.51599524676099,-3.02517322751174));
#85861=CARTESIAN_POINT('Ctrl Pts',(31.4347457325075,2.42479989010049,-3.09658432679762));
#85862=CARTESIAN_POINT('Ctrl Pts',(31.4288815193362,2.33354311053194,-3.1680435236791));
#85863=CARTESIAN_POINT('Ctrl Pts',(31.4230173061649,2.23921571708517,-3.23539412633645));
#85864=CARTESIAN_POINT('Ctrl Pts',(31.4171530929936,2.14223298445839,-3.29838245816014));
#85865=CARTESIAN_POINT('Ctrl Pts',(31.4112802444193,2.04510743898454,-3.36146354405205));
#85866=CARTESIAN_POINT('Ctrl Pts',(31.405407395845,1.9453191053953,-3.42016932986814));
#85867=CARTESIAN_POINT('Ctrl Pts',(31.3995345472707,1.8433074562443,-3.47429224760298));
#85868=CARTESIAN_POINT('Ctrl Pts',(31.3979398026579,1.81560666915988,-3.48898907324042));
#85869=CARTESIAN_POINT('Ctrl Pts',(31.396345058045,1.7877420506565,-3.50334824882253));
#85870=CARTESIAN_POINT('Ctrl Pts',(31.3947503134321,1.75972262705796,-3.51736624135449));
#85871=CARTESIAN_POINT('Ctrl Pts',(31.3888778672982,1.65654462949257,-3.56898573289212));
#85872=CARTESIAN_POINT('Ctrl Pts',(31.3830054211642,1.5509206634995,-3.61614788158668));
#85873=CARTESIAN_POINT('Ctrl Pts',(31.3771329750303,1.44327273538859,-3.65861350941636));
#85874=CARTESIAN_POINT('Ctrl Pts',(31.3712681360855,1.33576425481336,-3.70102412711018));
#85875=CARTESIAN_POINT('Ctrl Pts',(31.3654032971406,1.22623740701823,-3.73875017234563));
#85876=CARTESIAN_POINT('Ctrl Pts',(31.3595384581958,1.11513828952806,-3.77159854640289));
#85877=CARTESIAN_POINT('Ctrl Pts',(31.3536796480758,1.00415337758109,-3.80441315361765));
#85878=CARTESIAN_POINT('Ctrl Pts',(31.3478208379557,0.891599804726413,-3.83235994638736));
#85879=CARTESIAN_POINT('Ctrl Pts',(31.3419620278357,0.777942495674706,-3.85529434329253));
#85880=CARTESIAN_POINT('Ctrl Pts',(31.3358762389548,0.659881938411699,-3.87911725183847));
#85881=CARTESIAN_POINT('Ctrl Pts',(31.3297904500738,0.540630817295887,-3.89753136803522));
#85882=CARTESIAN_POINT('Ctrl Pts',(31.3237046611928,0.420726605016576,-3.91043196128397));
#85883=CARTESIAN_POINT('Ctrl Pts',(31.3178526311145,0.305427985479641,-3.92283703500502));
#85884=CARTESIAN_POINT('Ctrl Pts',(31.3120006010363,0.189525969535115,-3.93014427989007));
#85885=CARTESIAN_POINT('Ctrl Pts',(31.306148570958,0.0735067883130117,-3.93231302824075));
#85886=CARTESIAN_POINT('Ctrl Pts',(31.3002974305795,-0.0424947542032381,
-3.93448144687082));
#85887=CARTESIAN_POINT('Ctrl Pts',(31.294446290201,-0.158613013407076,-3.93151291456186));
#85888=CARTESIAN_POINT('Ctrl Pts',(31.2885951498225,-0.274360029426959,
-3.92341886296287));
#85889=CARTESIAN_POINT('Ctrl Pts',(31.282743482255,-0.390117474277434,-3.91532408208811));
#85890=CARTESIAN_POINT('Ctrl Pts',(31.2768918146875,-0.505503197075474,
-3.90210289272387));
#85891=CARTESIAN_POINT('Ctrl Pts',(31.27104014712,-0.620033349112839,-3.88381869375849));
#85892=CARTESIAN_POINT('Ctrl Pts',(31.2651865354358,-0.734601551839591,
-3.8655284201799));
#85893=CARTESIAN_POINT('Ctrl Pts',(31.2593329237516,-0.84831321062232,-3.84217185738055));
#85894=CARTESIAN_POINT('Ctrl Pts',(31.2534793120673,-0.96069437344229,-3.8138635687235));
#85895=CARTESIAN_POINT('Ctrl Pts',(31.2476190459675,-1.07320329174214,-3.78552309905931));
#85896=CARTESIAN_POINT('Ctrl Pts',(31.2417587798676,-1.18437829407815,-3.75221976897599));
#85897=CARTESIAN_POINT('Ctrl Pts',(31.2358985137677,-1.29376021047995,-3.71411813460192));
#85898=CARTESIAN_POINT('Ctrl Pts',(31.2300343005964,-1.40321579900311,-3.67599083759253));
#85899=CARTESIAN_POINT('Ctrl Pts',(31.2241700874251,-1.51087551380498,-3.63305895385118));
#85900=CARTESIAN_POINT('Ctrl Pts',(31.2183058742538,-1.61630141657886,-3.5855346506156));
#85901=CARTESIAN_POINT('Ctrl Pts',(31.2124330256795,-1.72188256527054,-3.53794036501441));
#85902=CARTESIAN_POINT('Ctrl Pts',(31.2065601771052,-1.82522296933522,-3.48574034876349));
#85903=CARTESIAN_POINT('Ctrl Pts',(31.2006873285309,-1.92591039340687,-3.42919205594662));
#85904=CARTESIAN_POINT('Ctrl Pts',(31.1990925839181,-1.95325159335207,-3.41383663102915));
#85905=CARTESIAN_POINT('Ctrl Pts',(31.1974978393053,-1.98039734438661,-3.39816081881947));
#85906=CARTESIAN_POINT('Ctrl Pts',(31.1959030946925,-2.00733979389806,-3.38217030201516));
#85907=CARTESIAN_POINT('Ctrl Pts',(31.1900306485585,-2.10655197006687,-3.32328723833731));
#85908=CARTESIAN_POINT('Ctrl Pts',(31.1841582024246,-2.20333714987633,-3.25993647329951));
#85909=CARTESIAN_POINT('Ctrl Pts',(31.1782857562907,-2.2972659515097,-3.19234367636604));
#85910=CARTESIAN_POINT('Ctrl Pts',(31.1724209173458,-2.39107307741595,-3.12483843939897));
#85911=CARTESIAN_POINT('Ctrl Pts',(31.166556078401,-2.48203085103357,-3.05310233764));
#85912=CARTESIAN_POINT('Ctrl Pts',(31.1606912394561,-2.56973562649878,-2.97740622184863));
#85913=CARTESIAN_POINT('Ctrl Pts',(31.1548324293361,-2.65735024488843,-2.9017879187008));
#85914=CARTESIAN_POINT('Ctrl Pts',(31.1489736192161,-2.74171820538918,-2.82221796690118));
#85915=CARTESIAN_POINT('Ctrl Pts',(31.1431148090961,-2.82246649527063,-2.73900928860688));
#85916=CARTESIAN_POINT('Ctrl Pts',(31.1370290202151,-2.9063430904582,-2.65257698600789));
#85917=CARTESIAN_POINT('Ctrl Pts',(31.1309432313341,-2.98631351137256,-2.56221858107816));
#85918=CARTESIAN_POINT('Ctrl Pts',(31.1248574424532,-3.06199904071403,-2.46832957172789));
#85919=CARTESIAN_POINT('Ctrl Pts',(31.1190054123749,-3.13477744345842,-2.37804689556482));
#85920=CARTESIAN_POINT('Ctrl Pts',(31.1131533822966,-3.2035937697591,-2.28450018871559));
#85921=CARTESIAN_POINT('Ctrl Pts',(31.1073013522183,-3.26815089943506,-2.18807648370019));
#85922=CARTESIAN_POINT('Ctrl Pts',(31.1014502118398,-3.33269821431826,-2.09166743823808));
#85923=CARTESIAN_POINT('Ctrl Pts',(31.0955990714613,-3.39298739018811,-1.99238260768692));
#85924=CARTESIAN_POINT('Ctrl Pts',(31.0897479310828,-3.4487641985508,-1.89063864945004));
#85925=CARTESIAN_POINT('Ctrl Pts',(31.0838962635153,-3.50454603241568,-1.78888552406107));
#85926=CARTESIAN_POINT('Ctrl Pts',(31.0780445959478,-3.55581449184181,-1.68467319301558));
#85927=CARTESIAN_POINT('Ctrl Pts',(31.0721929283803,-3.60236128658844,-1.57844295458813));
#85928=CARTESIAN_POINT('Ctrl Pts',(31.066339316696,-3.64892354571373,-1.4721774229758));
#85929=CARTESIAN_POINT('Ctrl Pts',(31.0604857050118,-3.69076085510404,-1.3638930293081));
#85930=CARTESIAN_POINT('Ctrl Pts',(31.0546320933275,-3.72771331577219,-1.25405041183149));
#85931=CARTESIAN_POINT('Ctrl Pts',(31.0487718272276,-3.76470778418629,-1.1440829247065));
#85932=CARTESIAN_POINT('Ctrl Pts',(31.0429115611277,-3.79680618815631,-1.03255407013663));
#85933=CARTESIAN_POINT('Ctrl Pts',(31.0370512950278,-3.8238986758598,-0.919939083177609));
#85934=CARTESIAN_POINT('Ctrl Pts',(31.0311870818565,-3.85100941119605,-0.807248246523758));
#85935=CARTESIAN_POINT('Ctrl Pts',(31.0253228686852,-3.87310743803521,-0.693470225611817));
#85936=CARTESIAN_POINT('Ctrl Pts',(31.0194586555139,-3.89013443562237,-0.579088139047071));
#85937=CARTESIAN_POINT('Ctrl Pts',(31.0135858069396,-3.90718650647712,-0.46453761805056));
#85938=CARTESIAN_POINT('Ctrl Pts',(31.0077129583653,-3.91915260208994,-0.349381665687266));
#85939=CARTESIAN_POINT('Ctrl Pts',(31.001840109791,-3.92602639524769,-0.234106266081031));
#85940=CARTESIAN_POINT('Ctrl Pts',(31.0002453651783,-3.92789294168911,-0.202803769485678));
#85941=CARTESIAN_POINT('Ctrl Pts',(30.9986506205656,-3.92938429425715,-0.171492449566823));
#85942=CARTESIAN_POINT('Ctrl Pts',(30.9970558759528,-3.93050098729974,-0.140181984704809));
#85943=CARTESIAN_POINT('Ctrl Pts',(30.9946917579802,-3.93215642107315,-0.093766005543916));
#85944=CARTESIAN_POINT('Ctrl Pts',(30.9923276400076,-3.9329896873435,-0.0473205289319825));
#85945=CARTESIAN_POINT('Ctrl Pts',(30.9899635220349,-3.93299990487134,-0.000865032977774666));
#85946=CARTESIAN_POINT('',(29.7399635545323,-3.9321542581735,-0.00319654787924418));
#85947=CARTESIAN_POINT('Ctrl Pts',(30.9899635219853,-3.93299990487155,-0.000865032002347642));
#85948=CARTESIAN_POINT('Ctrl Pts',(30.9841253417436,-3.93302513698879,0.113856636603515));
#85949=CARTESIAN_POINT('Ctrl Pts',(30.9782871615019,-3.92802663704679,0.228780085806603));
#85950=CARTESIAN_POINT('Ctrl Pts',(30.9724489812603,-3.91797751735153,0.343425644831478));
#85951=CARTESIAN_POINT('Ctrl Pts',(30.9666182781553,-3.90794126787233,0.457924373769877));
#85952=CARTESIAN_POINT('Ctrl Pts',(30.9607875750502,-3.89286729525467,0.572145506995858));
#85953=CARTESIAN_POINT('Ctrl Pts',(30.9549568719452,-3.87278070147756,0.685608225054937));
#85954=CARTESIAN_POINT('Ctrl Pts',(30.9491320302226,-3.85271429998339,0.798956883391825));
#85955=CARTESIAN_POINT('Ctrl Pts',(30.9433071884999,-3.82764537044766,0.911548232901897));
#85956=CARTESIAN_POINT('Ctrl Pts',(30.9374823467773,-3.79765084705022,1.02290617551112));
#85957=CARTESIAN_POINT('Ctrl Pts',(30.9316615817414,-3.76767731620202,1.13418618098947));
#85958=CARTESIAN_POINT('Ctrl Pts',(30.9258408167055,-3.73278515561282,1.24423409336451));
#85959=CARTESIAN_POINT('Ctrl Pts',(30.9200200516697,-3.69310231239223,1.35258430798347));
#85960=CARTESIAN_POINT('Ctrl Pts',(30.9142014303861,-3.65343408412109,1.46089461787837));
#85961=CARTESIAN_POINT('Ctrl Pts',(30.9083828091025,-3.60897882362711,1.56750808008232));
#85962=CARTESIAN_POINT('Ctrl Pts',(30.902564187819,-3.55991403820347,1.67197519138348));
#85963=CARTESIAN_POINT('Ctrl Pts',(30.8967462590075,-3.51085509196278,1.77642987009029));
#85964=CARTESIAN_POINT('Ctrl Pts',(30.890928330196,-3.45718788940113,1.87873832685015));
#85965=CARTESIAN_POINT('Ctrl Pts',(30.8851104013845,-3.39913737069582,1.97847267737998));
#85966=CARTESIAN_POINT('Ctrl Pts',(30.879291714612,-3.34107928915678,2.07822002132187));
#85967=CARTESIAN_POINT('Ctrl Pts',(30.8734730278396,-3.27863696731716,2.17539223080068));
#85968=CARTESIAN_POINT('Ctrl Pts',(30.8676543410671,-3.21208002246922,2.2695882730694));
#85969=CARTESIAN_POINT('Ctrl Pts',(30.8618296959027,-3.14545492266097,2.36388077300362));
#85970=CARTESIAN_POINT('Ctrl Pts',(30.8560050507382,-3.07470702598918,2.45519067578944));
#85971=CARTESIAN_POINT('Ctrl Pts',(30.8501804055738,-3.00014789455701,2.5431479726483));
#85972=CARTESIAN_POINT('Ctrl Pts',(30.8443528158915,-2.92555107143917,2.63114973433288));
#85973=CARTESIAN_POINT('Ctrl Pts',(30.8385252262092,-2.84713946084802,2.7157952074665));
#85974=CARTESIAN_POINT('Ctrl Pts',(30.8326976365269,-2.76526202818392,2.79675077822178));
#85975=CARTESIAN_POINT('Ctrl Pts',(30.8268603130383,-2.68324783587989,2.87784156883371));
#85976=CARTESIAN_POINT('Ctrl Pts',(30.8210229895497,-2.59775656565234,2.95522986146392));
#85977=CARTESIAN_POINT('Ctrl Pts',(30.8151856660612,-2.50917122701455,3.02862159298951));
#85978=CARTESIAN_POINT('Ctrl Pts',(30.8095266631118,-2.42329202336917,3.09977132898978));
#85979=CARTESIAN_POINT('Ctrl Pts',(30.8038676601625,-2.33450535955606,3.16716498088228));
#85980=CARTESIAN_POINT('Ctrl Pts',(30.7982086572131,-2.24318446416675,3.23057463305229));
#85981=CARTESIAN_POINT('Ctrl Pts',(30.7923362110792,-2.14841917708794,3.29637593587396));
#85982=CARTESIAN_POINT('Ctrl Pts',(30.7864637649453,-2.05059746597944,3.35811411933725));
#85983=CARTESIAN_POINT('Ctrl Pts',(30.7805913188114,-1.9501029296624,3.41549228717064));
#85984=CARTESIAN_POINT('Ctrl Pts',(30.7747264798666,-1.84973857435013,3.47279612710707));
#85985=CARTESIAN_POINT('Ctrl Pts',(30.7688616409218,-1.74670863494545,3.5257509801732));
#85986=CARTESIAN_POINT('Ctrl Pts',(30.7629968019769,-1.6414271244812,3.57410212431282));
#85987=CARTESIAN_POINT('Ctrl Pts',(30.7571379918569,-1.53625383928816,3.62240356536911));
#85988=CARTESIAN_POINT('Ctrl Pts',(30.7512791817369,-1.42883396013813,3.66611053908882));
#85989=CARTESIAN_POINT('Ctrl Pts',(30.745420371617,-1.31960705157309,3.70501366116761));
#85990=CARTESIAN_POINT('Ctrl Pts',(30.739334582736,-1.2061485349061,3.74542394635063));
#85991=CARTESIAN_POINT('Ctrl Pts',(30.733248793855,-1.09074053777285,3.78065041027169));
#85992=CARTESIAN_POINT('Ctrl Pts',(30.727163004974,-0.973900112830244,3.81051276998638));
#85993=CARTESIAN_POINT('Ctrl Pts',(30.7213109748958,-0.861547598720272,
3.83922809854539));
#85994=CARTESIAN_POINT('Ctrl Pts',(30.7154589448175,-0.747871105288671,
3.86298368670579));
#85995=CARTESIAN_POINT('Ctrl Pts',(30.7096069147393,-0.633346099804996,
3.88166996508742));
#85996=CARTESIAN_POINT('Ctrl Pts',(30.7037557743608,-0.518838505863574,
3.90035340254428));
#85997=CARTESIAN_POINT('Ctrl Pts',(30.6979046339823,-0.40348306421814,3.91396899608031));
#85998=CARTESIAN_POINT('Ctrl Pts',(30.6920534936038,-0.287764380499728,
3.92245849708007));
#85999=CARTESIAN_POINT('Ctrl Pts',(30.6862018260363,-0.172035270503619,
3.93094876298565));
#86000=CARTESIAN_POINT('Ctrl Pts',(30.6803501584688,-0.055943265647758,
3.93431198797021));
#86001=CARTESIAN_POINT('Ctrl Pts',(30.6744984909013,0.0600236891657086,
3.93254194596052));
#86002=CARTESIAN_POINT('Ctrl Pts',(30.6686448792171,0.176029172022672,3.93077131588455));
#86003=CARTESIAN_POINT('Ctrl Pts',(30.6627912675328,0.291909109136011,3.92386403395518));
#86004=CARTESIAN_POINT('Ctrl Pts',(30.6569376558486,0.407178057208399,3.91186592685997));
#86005=CARTESIAN_POINT('Ctrl Pts',(30.6510773897487,0.522578043609061,3.8998541802554));
#86006=CARTESIAN_POINT('Ctrl Pts',(30.6452171236488,0.637365243240775,3.88274010009507));
#86007=CARTESIAN_POINT('Ctrl Pts',(30.6393568575489,0.75106171691046,3.86062110254186));
#86008=CARTESIAN_POINT('Ctrl Pts',(30.6334926443776,0.864834768690114,3.83848720715608));
#86009=CARTESIAN_POINT('Ctrl Pts',(30.6276284312063,0.9775152308187,3.81134177867732));
#86010=CARTESIAN_POINT('Ctrl Pts',(30.621764218035,1.08863939147607,3.77933238486993));
#86011=CARTESIAN_POINT('Ctrl Pts',(30.6158913694607,1.19992718907508,3.74727585532468));
#86012=CARTESIAN_POINT('Ctrl Pts',(30.6100185208864,1.309653721049,3.71034119694256));
#86013=CARTESIAN_POINT('Ctrl Pts',(30.6041456723121,1.41737425990548,3.66872446599052));
#86014=CARTESIAN_POINT('Ctrl Pts',(30.6025509276993,1.44662526933686,3.65742363698888));
#86015=CARTESIAN_POINT('Ctrl Pts',(30.6009561830864,1.47572850051372,3.64577782989925));
#86016=CARTESIAN_POINT('Ctrl Pts',(30.5993614384736,1.50467537090407,3.63379154990964));
#86017=CARTESIAN_POINT('Ctrl Pts',(30.5934889923397,1.61126857444412,3.58965358385694));
#86018=CARTESIAN_POINT('Ctrl Pts',(30.5876165462057,1.71609648552891,3.54074755642489));
#86019=CARTESIAN_POINT('Ctrl Pts',(30.5817441000718,1.81870193655789,3.48723561950731));
#86020=CARTESIAN_POINT('Ctrl Pts',(30.575879261127,1.92117447209504,3.43379300215652));
#86021=CARTESIAN_POINT('Ctrl Pts',(30.5700144221821,2.02142990972165,3.37575652997487));
#86022=CARTESIAN_POINT('Ctrl Pts',(30.5641495832373,2.1190301138874,3.31333674359223));
#86023=CARTESIAN_POINT('Ctrl Pts',(30.5582907731173,2.21652998886429,3.25098112230627));
#86024=CARTESIAN_POINT('Ctrl Pts',(30.5524319629973,2.31137971331781,3.18425137062467));
#86025=CARTESIAN_POINT('Ctrl Pts',(30.5465731528773,2.40316547425604,3.11340403792116));
#86026=CARTESIAN_POINT('Ctrl Pts',(30.5404873639963,2.49850714806143,3.03981197728392));
#86027=CARTESIAN_POINT('Ctrl Pts',(30.5344015751153,2.59054224926123,2.96177705106598));
#86028=CARTESIAN_POINT('Ctrl Pts',(30.5283157862343,2.6788395465697,2.87963672773742));
#86029=CARTESIAN_POINT('Ctrl Pts',(30.5224637561561,2.76374529170566,2.80065146351629));
#86030=CARTESIAN_POINT('Ctrl Pts',(30.5166117260778,2.8451947481822,2.71787067367035));
#86031=CARTESIAN_POINT('Ctrl Pts',(30.5107596959995,2.92283865523893,2.63163508021934));
#86032=CARTESIAN_POINT('Ctrl Pts',(30.504908555621,3.00047075788517,2.54541259739586));
#86033=CARTESIAN_POINT('Ctrl Pts',(30.4990574152425,3.07429818498459,2.45573666242723));
#86034=CARTESIAN_POINT('Ctrl Pts',(30.493206274864,3.14400990605597,2.36298343426735));
#86035=CARTESIAN_POINT('Ctrl Pts',(30.4873546072965,3.21372790816818,2.27022184902196));
#86036=CARTESIAN_POINT('Ctrl Pts',(30.481502939729,3.27932921872088,2.17438274986283));
#86037=CARTESIAN_POINT('Ctrl Pts',(30.4756512721615,3.34054476348101,2.07587323388969));
#86038=CARTESIAN_POINT('Ctrl Pts',(30.4697976604772,3.40178064606174,1.97733098981012));
#86039=CARTESIAN_POINT('Ctrl Pts',(30.463944048793,3.45862764744553,1.87611691567687));
#86040=CARTESIAN_POINT('Ctrl Pts',(30.4580904371087,3.51086183328906,1.77266414967816));
#86041=CARTESIAN_POINT('Ctrl Pts',(30.4522301710089,3.56315539922169,1.66909377804698));
#86042=CARTESIAN_POINT('Ctrl Pts',(30.446369904909,3.6108254966039,1.56328000411087));
#86043=CARTESIAN_POINT('Ctrl Pts',(30.4405096388091,3.65369564616487,1.45567754849619));
#86044=CARTESIAN_POINT('Ctrl Pts',(30.4346454256378,3.69659467010448,1.3480026192821));
#86045=CARTESIAN_POINT('Ctrl Pts',(30.4287812124665,3.73468717332118,1.23853699896449));
#86046=CARTESIAN_POINT('Ctrl Pts',(30.4229169992952,3.76784655740463,1.12775055746123));
#86047=CARTESIAN_POINT('Ctrl Pts',(30.4170441507209,3.80105477065506,1.01680097632789));
#86048=CARTESIAN_POINT('Ctrl Pts',(30.4111713021466,3.82931526613401,0.904527091545456));
#86049=CARTESIAN_POINT('Ctrl Pts',(30.4052984535723,3.85255249941213,0.791409021475846));
#86050=CARTESIAN_POINT('Ctrl Pts',(30.4037037089595,3.85886246162522,0.760692337642873));
#86051=CARTESIAN_POINT('Ctrl Pts',(30.4021089643467,3.86480231998018,0.72991343301046));
#86052=CARTESIAN_POINT('Ctrl Pts',(30.4005142197339,3.8703712236184,0.699081963282273));
#86053=CARTESIAN_POINT('Ctrl Pts',(30.3946417735999,3.89087800970672,0.585548960095529));
#86054=CARTESIAN_POINT('Ctrl Pts',(30.388769327466,3.9064193483538,0.470922797049242));
#86055=CARTESIAN_POINT('Ctrl Pts',(30.3828968813321,3.91688444797553,0.355675724793542));
#86056=CARTESIAN_POINT('Ctrl Pts',(30.3770320423872,3.92733599106737,0.240577944034012));
#86057=CARTESIAN_POINT('Ctrl Pts',(30.3711672034424,3.9327243349837,0.12486126145588));
#86058=CARTESIAN_POINT('Ctrl Pts',(30.3653023644975,3.9329896840009,0.00900808206402624));
#86059=CARTESIAN_POINT('Ctrl Pts',(30.3594435543775,3.93325476024971,-0.106726004795038));
#86060=CARTESIAN_POINT('Ctrl Pts',(30.3535847442575,3.92840731549468,-0.222595898502569));
#86061=CARTESIAN_POINT('Ctrl Pts',(30.3477259341375,3.91843940843405,-0.338114777007737));
#86062=CARTESIAN_POINT('Ctrl Pts',(30.3416401452565,3.90808533026572,-0.458109023611916));
#86063=CARTESIAN_POINT('Ctrl Pts',(30.3355543563755,3.8922059763021,-0.577724054775901));
#86064=CARTESIAN_POINT('Ctrl Pts',(30.3294685674946,3.87085205685679,-0.696414642240932));
#86065=CARTESIAN_POINT('Ctrl Pts',(30.3236165374163,3.85031835427077,-0.81054625302127));
#86066=CARTESIAN_POINT('Ctrl Pts',(30.317764507338,3.82472297102752,-0.923822682539965));
#86067=CARTESIAN_POINT('Ctrl Pts',(30.3119124772597,3.79416367665801,-1.03576589764723));
#86068=CARTESIAN_POINT('Ctrl Pts',(30.3060613368812,3.76360902829963,-1.14769209372857));
#86069=CARTESIAN_POINT('Ctrl Pts',(30.3002101965027,3.7280920781872,-1.25828507976001));
#86070=CARTESIAN_POINT('Ctrl Pts',(30.2943590561242,3.68776107721996,-1.36707982113023));
#86071=CARTESIAN_POINT('Ctrl Pts',(30.2885073885567,3.647426442421,-1.47588436492967));
#86072=CARTESIAN_POINT('Ctrl Pts',(30.2826557209892,3.60227703820654,-1.58288995437695));
#86073=CARTESIAN_POINT('Ctrl Pts',(30.2768040534217,3.55250982709289,-1.68765012025847));
#86074=CARTESIAN_POINT('Ctrl Pts',(30.2709504417374,3.50272608167206,-1.79244509091858));
#86075=CARTESIAN_POINT('Ctrl Pts',(30.2650968300531,3.44832165599115,-1.89499278146015));
#86076=CARTESIAN_POINT('Ctrl Pts',(30.2592432183689,3.3895398261628,-1.99487061406404));
#86077=CARTESIAN_POINT('Ctrl Pts',(30.253382952269,3.33069117285034,-2.09486198829771));
#86078=CARTESIAN_POINT('Ctrl Pts',(30.2475226861691,3.26745539273513,-2.19217709016946));
#86079=CARTESIAN_POINT('Ctrl Pts',(30.2416624200692,3.20011957671275,-2.28642159164486));
#86080=CARTESIAN_POINT('Ctrl Pts',(30.2357982068979,3.13273840792464,-2.38072956972229));
#86081=CARTESIAN_POINT('Ctrl Pts',(30.2299339937265,3.06125195884796,-2.47196250473654));
#86082=CARTESIAN_POINT('Ctrl Pts',(30.2240697805552,2.98598703518934,-2.55975983750062));
#86083=CARTESIAN_POINT('Ctrl Pts',(30.2181969319809,2.91061127945028,-2.64768645706356));
#86084=CARTESIAN_POINT('Ctrl Pts',(30.2123240834066,2.83144622601685,-2.73216707687537));
#86085=CARTESIAN_POINT('Ctrl Pts',(30.2064512348323,2.74885490708845,-2.81287854337434));
#86086=CARTESIAN_POINT('Ctrl Pts',(30.2048564902196,2.72642762001491,-2.83479536529685));
#86087=CARTESIAN_POINT('Ctrl Pts',(30.2032617456069,2.70374787330462,-2.85643449597814));
#86088=CARTESIAN_POINT('Ctrl Pts',(30.2016670009942,2.68082332935361,-2.87778999873053));
#86089=CARTESIAN_POINT('Ctrl Pts',(30.1957945548603,2.59640658423568,-2.95642894729872));
#86090=CARTESIAN_POINT('Ctrl Pts',(30.1899221087264,2.50838539502564,-3.03148199994583));
#86091=CARTESIAN_POINT('Ctrl Pts',(30.1840496625925,2.41709711703613,-3.10260060704172));
#86092=CARTESIAN_POINT('Ctrl Pts',(30.1781848236476,2.3259270942293,-3.17362708682334));
#86093=CARTESIAN_POINT('Ctrl Pts',(30.1723199847028,2.23149872205837,-3.24072900487486));
#86094=CARTESIAN_POINT('Ctrl Pts',(30.1664551457579,2.13418547175362,-3.30359521917498));
#86095=CARTESIAN_POINT('Ctrl Pts',(30.1605963356379,2.03697225566015,-3.36639680946816));
#86096=CARTESIAN_POINT('Ctrl Pts',(30.1547375255179,1.93688040518021,-3.42497113367271));
#86097=CARTESIAN_POINT('Ctrl Pts',(30.1488787153978,1.83431514541938,-3.47904828182724));
#86098=CARTESIAN_POINT('Ctrl Pts',(30.1427929265169,1.72777635944791,-3.53522045675878));
#86099=CARTESIAN_POINT('Ctrl Pts',(30.1367071376359,1.61856899968815,-3.58653967476689));
#86100=CARTESIAN_POINT('Ctrl Pts',(30.1306213487549,1.50717913659744,-3.6327537833172));
#86101=CARTESIAN_POINT('Ctrl Pts',(30.1247693186766,1.40006782498762,-3.67719278022727));
#86102=CARTESIAN_POINT('Ctrl Pts',(30.1189172885984,1.29093899691935,-3.71691144098346));
#86103=CARTESIAN_POINT('Ctrl Pts',(30.1130652585201,1.18024764312597,-3.75173353276797));
#86104=CARTESIAN_POINT('Ctrl Pts',(30.1072141181416,1.06957311803465,-3.78655033045688));
#86105=CARTESIAN_POINT('Ctrl Pts',(30.1013629777631,0.957336933753299,-3.8164719153507));
#86106=CARTESIAN_POINT('Ctrl Pts',(30.0955118373846,0.84401044232151,-3.84137154845144));
#86107=CARTESIAN_POINT('Ctrl Pts',(30.0896601698171,0.73067374014865,-3.86627342501445));
#86108=CARTESIAN_POINT('Ctrl Pts',(30.0838085022495,0.616246939290572,-3.88615236158756));
#86109=CARTESIAN_POINT('Ctrl Pts',(30.077956834682,0.501212113278957,-3.90093263431996));
#86110=CARTESIAN_POINT('Ctrl Pts',(30.0721032229978,0.386139068907821,-3.91571781754596));
#86111=CARTESIAN_POINT('Ctrl Pts',(30.0662496113135,0.27045800747624,-3.92540091597733));
#86112=CARTESIAN_POINT('Ctrl Pts',(30.0603959996292,0.154655947097649,-3.92995808349495));
#86113=CARTESIAN_POINT('Ctrl Pts',(30.0545357335293,0.0387222423464035,
-3.93452043162384));
#86114=CARTESIAN_POINT('Ctrl Pts',(30.0486754674294,-0.0773323226202726,
-3.93394520170984));
#86115=CARTESIAN_POINT('Ctrl Pts',(30.0428152013295,-0.193020802557902,
-3.92826067996765));
#86116=CARTESIAN_POINT('Ctrl Pts',(30.0369509881582,-0.308787202283246,
-3.92257232952335));
#86117=CARTESIAN_POINT('Ctrl Pts',(30.0310867749869,-0.424186615459352,
-3.91176787343508));
#86118=CARTESIAN_POINT('Ctrl Pts',(30.0252225618156,-0.538739029292221,
-3.89592726553221));
#86119=CARTESIAN_POINT('Ctrl Pts',(30.0193497132413,-0.653460128374264,
-3.88006333139114));
#86120=CARTESIAN_POINT('Ctrl Pts',(30.013476864667,-0.767331333810295,-3.85914851890151));
#86121=CARTESIAN_POINT('Ctrl Pts',(30.0076040160927,-0.879884510716179,
-3.83331348154593));
#86122=CARTESIAN_POINT('Ctrl Pts',(30.00600927148,-0.91044780044609,-3.82629809776389));
#86123=CARTESIAN_POINT('Ctrl Pts',(30.0044145268673,-0.940914001339077,
-3.81892019218749));
#86124=CARTESIAN_POINT('Ctrl Pts',(30.0028197822545,-0.971273976264554,
-3.81118300046472));
#86125=CARTESIAN_POINT('Ctrl Pts',(29.9969473361206,-1.08307075924357,-3.78269176666031));
#86126=CARTESIAN_POINT('Ctrl Pts',(29.9910748899867,-1.19380001443587,-3.74922951171389));
#86127=CARTESIAN_POINT('Ctrl Pts',(29.9852024438528,-1.30298612731375,-3.71089155756779));
#86128=CARTESIAN_POINT('Ctrl Pts',(29.979337604908,-1.41203080008544,-3.67260326655341));
#86129=CARTESIAN_POINT('Ctrl Pts',(29.9734727659631,-1.51953591940979,-3.62945197229674));
#86130=CARTESIAN_POINT('Ctrl Pts',(29.9676079270183,-1.62503781012665,-3.58158360444913));
#86131=CARTESIAN_POINT('Ctrl Pts',(29.9617491168983,-1.73043124903029,-3.5337644434096));
#86132=CARTESIAN_POINT('Ctrl Pts',(29.9558903067783,-1.83382518110547,-3.48123802340571));
#86133=CARTESIAN_POINT('Ctrl Pts',(29.9500314966583,-1.93477344632288,-3.42419928032874));
#86134=CARTESIAN_POINT('Ctrl Pts',(29.9439457077773,-2.03963259304888,-3.36495077401223));
#86135=CARTESIAN_POINT('Ctrl Pts',(29.9378599188964,-2.14185231432237,-3.30083339613807));
#86136=CARTESIAN_POINT('Ctrl Pts',(29.9317741300154,-2.24095767391047,-3.23211969205068));
#86137=CARTESIAN_POINT('Ctrl Pts',(29.9259220999371,-2.33625633716823,-3.16604532256921));
#86138=CARTESIAN_POINT('Ctrl Pts',(29.9200700698589,-2.42867510338249,-3.0957214661676));
#86139=CARTESIAN_POINT('Ctrl Pts',(29.9142180397806,-2.51781970578769,-3.02143557421753));
#86140=CARTESIAN_POINT('Ctrl Pts',(29.9083668994021,-2.60695075530109,-2.94716097614985));
#86141=CARTESIAN_POINT('Ctrl Pts',(29.9025157590236,-2.69280831328885,-2.8689258047693));
#86142=CARTESIAN_POINT('Ctrl Pts',(29.8966646186451,-2.77503090090207,-2.78705803653936));
#86143=CARTESIAN_POINT('Ctrl Pts',(29.8908129510777,-2.85726089678748,-2.70518289200653));
#86144=CARTESIAN_POINT('Ctrl Pts',(29.8849612835102,-2.93585497829912,-2.61967479165901));
#86145=CARTESIAN_POINT('Ctrl Pts',(29.8791096159427,-3.01048878376404,-2.53089831538743));
#86146=CARTESIAN_POINT('Ctrl Pts',(29.8732560042585,-3.08514738503834,-2.44209234464522));
#86147=CARTESIAN_POINT('Ctrl Pts',(29.8674023925742,-3.15584282815298,-2.35001615504212));
#86148=CARTESIAN_POINT('Ctrl Pts',(29.86154878089,-3.22229171785936,-2.25506653671571));
#86149=CARTESIAN_POINT('Ctrl Pts',(29.8556885147901,-3.28881614700269,-2.16000897917859));
#86150=CARTESIAN_POINT('Ctrl Pts',(29.8498282486902,-3.35108415005529,-2.06207181189839));
#86151=CARTESIAN_POINT('Ctrl Pts',(29.8439679825904,-3.40885622535348,-1.96167995220138));
#86152=CARTESIAN_POINT('Ctrl Pts',(29.8381037694191,-3.46666721194057,-1.8612204754656));
#86153=CARTESIAN_POINT('Ctrl Pts',(29.8322395562478,-3.51997605146945,-1.75830338037986));
#86154=CARTESIAN_POINT('Ctrl Pts',(29.8263753430765,-3.56859045398145,-1.65337568983956));
#86155=CARTESIAN_POINT('Ctrl Pts',(29.8205024945022,-3.61727644409519,-1.54829348702854));
#86156=CARTESIAN_POINT('Ctrl Pts',(29.8146296459279,-3.66125404412129,-1.44119516068858));
#86157=CARTESIAN_POINT('Ctrl Pts',(29.8087567973536,-3.70038003560882,-1.33254515573307));
#86158=CARTESIAN_POINT('Ctrl Pts',(29.8071620527407,-3.71100451593692,-1.30304175412173));
#86159=CARTESIAN_POINT('Ctrl Pts',(29.8055673081279,-3.72127154277174,-1.2734240052593));
#86160=CARTESIAN_POINT('Ctrl Pts',(29.803972563515,-3.73117889742914,-1.2437013449295));
#86161=CARTESIAN_POINT('Ctrl Pts',(29.7969890545378,-3.77456396337151,-1.11354353560678));
#86162=CARTESIAN_POINT('Ctrl Pts',(29.7900055455606,-3.8111662578302,-0.981018558808337));
#86163=CARTESIAN_POINT('Ctrl Pts',(29.7830220365834,-3.84076258079052,-0.846777301301432));
#86164=CARTESIAN_POINT('Ctrl Pts',(29.7758456247582,-3.87117643187473,-0.708827947908951));
#86165=CARTESIAN_POINT('Ctrl Pts',(29.7686692129329,-3.89419154278163,-0.569066121117047));
#86166=CARTESIAN_POINT('Ctrl Pts',(29.7614928011076,-3.90961824669457,-0.428222097880171));
#86167=CARTESIAN_POINT('Ctrl Pts',(29.7543163892823,-3.9250449506075,-0.287378074643332));
#86168=CARTESIAN_POINT('Ctrl Pts',(29.747139977457,-3.93288305006062,-0.145451907656713));
#86169=CARTESIAN_POINT('Ctrl Pts',(29.7399635656318,-3.93299870026503,-0.00319745422851603));
#86170=CARTESIAN_POINT('',(28.489963522035,-3.92772619981674,0.00219722477549311));
#86171=CARTESIAN_POINT('Ctrl Pts',(29.739963522035,-3.92968187761009,-0.00319389424515149));
#86172=CARTESIAN_POINT('Ctrl Pts',(29.6950174629484,-3.92291879964284,0.887004282061398));
#86173=CARTESIAN_POINT('Ctrl Pts',(29.5837889976154,-3.18166436252796,3.10018088548878));
#86174=CARTESIAN_POINT('Ctrl Pts',(29.4062781260356,0.494417430209507,4.62531527855905));
#86175=CARTESIAN_POINT('Ctrl Pts',(29.2074309072962,4.15819300996308,2.08504698106617));
#86176=CARTESIAN_POINT('Ctrl Pts',(29.0085836885562,4.00233764393561,-2.37050277479532));
#86177=CARTESIAN_POINT('Ctrl Pts',(28.8097364698168,0.170016879685549,-4.64855722584818));
#86178=CARTESIAN_POINT('Ctrl Pts',(28.6368630809762,-3.29749257198293,-2.91674327551318));
#86179=CARTESIAN_POINT('Ctrl Pts',(28.5302720983823,-3.92368339933592,-0.797150168107896));
#86180=CARTESIAN_POINT('Ctrl Pts',(28.489963522035,-3.92772619981674,0.00219722477549311));
#86181=CARTESIAN_POINT('',(27.239963522035,-3.93773669167115,0.00235620308681454));
#86182=CARTESIAN_POINT('Ctrl Pts',(28.489963522035,-3.92772619981674,0.00219722477549311));
#86183=CARTESIAN_POINT('Ctrl Pts',(28.4639896921358,-3.93033127847545,0.51727652289259));
#86184=CARTESIAN_POINT('Ctrl Pts',(28.3717334559901,-3.59630940642058,2.34353714429184));
#86185=CARTESIAN_POINT('Ctrl Pts',(28.2131948135979,-0.830978145420823,
4.57684010461503));
#86186=CARTESIAN_POINT('Ctrl Pts',(28.0143475948581,3.4007603027884,3.17377053114104));
#86187=CARTESIAN_POINT('Ctrl Pts',(27.8155003761186,4.50862997901059,-1.14465965847099));
#86188=CARTESIAN_POINT('Ctrl Pts',(27.6166531573788,1.474964486074,-4.41162892661981));
#86189=CARTESIAN_POINT('Ctrl Pts',(27.4248075393512,-2.759048571294,-3.6538230993727));
#86190=CARTESIAN_POINT('Ctrl Pts',(27.2992443275697,-3.92947964173005,-1.16559882579688));
#86191=CARTESIAN_POINT('Ctrl Pts',(27.239963522035,-3.93773669167115,0.00235620308681454));
#86192=CARTESIAN_POINT('',(25.989963522035,-3.93325007891365,-0.00337094196644616));
#86193=CARTESIAN_POINT('Ctrl Pts',(27.239963522035,-3.93773669167115,0.00235620308681454));
#86194=CARTESIAN_POINT('Ctrl Pts',(27.2329619213232,-3.93871192414688,0.140302283404259));
#86195=CARTESIAN_POINT('Ctrl Pts',(27.1596779143649,-3.86944318367108,1.5831590277253));
#86196=CARTESIAN_POINT('Ctrl Pts',(27.0201115011599,-2.08882077843383,4.15629856686949));
#86197=CARTESIAN_POINT('Ctrl Pts',(26.8212642824203,2.36686862149651,4.004487851141));
#86198=CARTESIAN_POINT('Ctrl Pts',(26.6224170636807,4.64840097541825,0.174236600890457));
#86199=CARTESIAN_POINT('Ctrl Pts',(26.423569844941,2.66000738516909,-3.81606482285398));
#86200=CARTESIAN_POINT('Ctrl Pts',(26.2247226262013,-1.77181451638399,-4.30100724724962));
#86201=CARTESIAN_POINT('Ctrl Pts',(26.0801871852327,-3.81014481169265,-1.78177796532842));
#86202=CARTESIAN_POINT('Ctrl Pts',(26.0019341505106,-3.9372342010039,-0.239632457677508));
#86203=CARTESIAN_POINT('Ctrl Pts',(25.989963522035,-3.93508678583485,-0.00337251609275779));
#86204=CARTESIAN_POINT('',(24.7399635445061,-3.9306001245949,-0.000718677470833023));
#86205=CARTESIAN_POINT('Ctrl Pts',(25.989963522035,-3.93299855558116,-0.00337072640157237));
#86206=CARTESIAN_POINT('Ctrl Pts',(25.9841875105398,-3.93309620432813,0.110566845214765));
#86207=CARTESIAN_POINT('Ctrl Pts',(25.9784114990446,-3.92823857947925,0.224676345046821));
#86208=CARTESIAN_POINT('Ctrl Pts',(25.9726354875494,-3.9184075443469,0.338483849548717));
#86209=CARTESIAN_POINT('Ctrl Pts',(25.9665685167649,-3.90808128322736,0.458024263455157));
#86210=CARTESIAN_POINT('Ctrl Pts',(25.9605015459804,-3.89226740998787,0.577230993667277));
#86211=CARTESIAN_POINT('Ctrl Pts',(25.9544345751959,-3.87100689880111,0.695553441105879));
#86212=CARTESIAN_POINT('Ctrl Pts',(25.9486676611254,-3.85079787761639,0.808023965728239));
#86213=CARTESIAN_POINT('Ctrl Pts',(25.9429007470548,-3.82566814695001,0.919695102139139));
#86214=CARTESIAN_POINT('Ctrl Pts',(25.9371338329842,-3.79570600900335,1.03009945792426));
#86215=CARTESIAN_POINT('Ctrl Pts',(25.9313685509217,-3.76575235019257,1.14047256982631));
#86216=CARTESIAN_POINT('Ctrl Pts',(25.9256032688591,-3.73096911289362,1.24957920184213));
#86217=CARTESIAN_POINT('Ctrl Pts',(25.9198379867965,-3.69149527863074,1.35696411442859));
#86218=CARTESIAN_POINT('Ctrl Pts',(25.9140728441454,-3.65202239889297,1.46434643031783));
#86219=CARTESIAN_POINT('Ctrl Pts',(25.9083077014943,-3.60785929551641,1.5700067091801));
#86220=CARTESIAN_POINT('Ctrl Pts',(25.9025425588432,-3.55919389605387,1.67350763675965));
#86221=CARTESIAN_POINT('Ctrl Pts',(25.8967760633438,-3.51051707676943,1.7770328518653));
#86222=CARTESIAN_POINT('Ctrl Pts',(25.8910095678444,-3.45733604460149,1.87839732321322));
#86223=CARTESIAN_POINT('Ctrl Pts',(25.8852430723451,-3.39988526660132,1.97718718738192));
#86224=CARTESIAN_POINT('Ctrl Pts',(25.8794704699136,-3.34237364610159,2.07608167367198));
#86225=CARTESIAN_POINT('Ctrl Pts',(25.8736978674821,-3.28058347096434,2.17239574252534));
#86226=CARTESIAN_POINT('Ctrl Pts',(25.8679252650506,-3.21479318612327,2.2657435358962));
#86227=CARTESIAN_POINT('Ctrl Pts',(25.8621491040677,-3.14896234451134,2.35914887401055));
#86228=CARTESIAN_POINT('Ctrl Pts',(25.8563729430848,-3.0791267473614,2.44958396172238));
#86229=CARTESIAN_POINT('Ctrl Pts',(25.8505967821018,-3.0056046509437,2.53669660823395));
#86230=CARTESIAN_POINT('Ctrl Pts',(25.8448120833999,-2.93197388182711,2.62393801557886));
#86231=CARTESIAN_POINT('Ctrl Pts',(25.8390273846979,-2.85464602973347,2.70784687121573));
#86232=CARTESIAN_POINT('Ctrl Pts',(25.8332426859959,-2.77397558729295,2.78810839837742));
#86233=CARTESIAN_POINT('Ctrl Pts',(25.8311711869046,-2.74508752296738,2.81685003024867));
#86234=CARTESIAN_POINT('Ctrl Pts',(25.8290996878134,-2.71577112039666,2.84512432816432));
#86235=CARTESIAN_POINT('Ctrl Pts',(25.8270281887221,-2.6860436152956,2.87291815002268));
#86236=CARTESIAN_POINT('Ctrl Pts',(25.8211557425882,-2.60176978040093,2.95171022982959));
#86237=CARTESIAN_POINT('Ctrl Pts',(25.8152832964543,-2.5138849970653,3.02692296358918));
#86238=CARTESIAN_POINT('Ctrl Pts',(25.8094108503204,-2.42272598724428,3.09820718976818));
#86239=CARTESIAN_POINT('Ctrl Pts',(25.8035460113756,-2.33168506515144,3.16939907408935));
#86240=CARTESIAN_POINT('Ctrl Pts',(25.7976811724307,-2.23737867391849,3.23667231876815));
#86241=CARTESIAN_POINT('Ctrl Pts',(25.7918163334859,-2.14017971927364,3.29971510424912));
#86242=CARTESIAN_POINT('Ctrl Pts',(25.7859575233659,-2.0430806813487,3.36269308421483));
#86243=CARTESIAN_POINT('Ctrl Pts',(25.7800987132459,-1.9430953390677,3.4214490312959));
#86244=CARTESIAN_POINT('Ctrl Pts',(25.7742399031258,-1.84062842683969,3.47571230027884));
#86245=CARTESIAN_POINT('Ctrl Pts',(25.7681541142449,-1.73419179852608,3.53207780662852));
#86246=CARTESIAN_POINT('Ctrl Pts',(25.7620683253639,-1.62507779015006,3.58359520891931));
#86247=CARTESIAN_POINT('Ctrl Pts',(25.7559825364829,-1.51377201357829,3.63001147255861));
#86248=CARTESIAN_POINT('Ctrl Pts',(25.7501305064047,-1.40674155867399,3.67464485965931));
#86249=CARTESIAN_POINT('Ctrl Pts',(25.7442784763264,-1.29768502074069,3.71456158124025));
#86250=CARTESIAN_POINT('Ctrl Pts',(25.7384264462481,-1.1870570698065,3.74958457872634));
#86251=CARTESIAN_POINT('Ctrl Pts',(25.7325753058696,-1.07644593793511,3.78460225157261));
#86252=CARTESIAN_POINT('Ctrl Pts',(25.7267241654911,-0.964264262058645,
3.81472755492515));
#86253=CARTESIAN_POINT('Ctrl Pts',(25.7208730251126,-0.85098316334188,3.83983289424275));
#86254=CARTESIAN_POINT('Ctrl Pts',(25.7150213575452,-0.737691857974338,
3.86494049555669));
#86255=CARTESIAN_POINT('Ctrl Pts',(25.7091696899777,-0.623301336437284,
3.88502714426204));
#86256=CARTESIAN_POINT('Ctrl Pts',(25.7033180224102,-0.508293533989227,
3.90001624141551));
#86257=CARTESIAN_POINT('Ctrl Pts',(25.697464410726,-0.393247522160508,3.91501031844083));
#86258=CARTESIAN_POINT('Ctrl Pts',(25.6916107990418,-0.277584231303043,
3.92490342295136));
#86259=CARTESIAN_POINT('Ctrl Pts',(25.6857571873576,-0.161790635434357,
3.92967082467295));
#86260=CARTESIAN_POINT('Ctrl Pts',(25.6798969212577,-0.045865404814469,
3.93444364600116));
#86261=CARTESIAN_POINT('Ctrl Pts',(25.6740366551578,0.0701900132309724,
3.93407911717854));
#86262=CARTESIAN_POINT('Ctrl Pts',(25.6681763890579,0.185888622905629,3.92860464031114));
#86263=CARTESIAN_POINT('Ctrl Pts',(25.6623121758866,0.301665159191289,3.92312647621336));
#86264=CARTESIAN_POINT('Ctrl Pts',(25.6564479627153,0.417083997958116,3.91253154862948));
#86265=CARTESIAN_POINT('Ctrl Pts',(25.650583749544,0.531664982044918,3.89689893978111));
#86266=CARTESIAN_POINT('Ctrl Pts',(25.6447109009698,0.64641469345154,3.88124331098565));
#86267=CARTESIAN_POINT('Ctrl Pts',(25.6388380523955,0.760323682616542,3.8605352691614));
#86268=CARTESIAN_POINT('Ctrl Pts',(25.6329652038212,0.872923578222459,3.83490461766434));
#86269=CARTESIAN_POINT('Ctrl Pts',(25.6313704592083,0.903499554200888,3.82794473390718));
#86270=CARTESIAN_POINT('Ctrl Pts',(25.6297757145954,0.933979099670331,3.82062215268567));
#86271=CARTESIAN_POINT('Ctrl Pts',(25.6281809699825,0.96435307164083,3.81294009305377));
#86272=CARTESIAN_POINT('Ctrl Pts',(25.6223085238485,1.07620139696237,3.78465187623174));
#86273=CARTESIAN_POINT('Ctrl Pts',(25.6164360777146,1.18699122127737,3.75139070833524));
#86274=CARTESIAN_POINT('Ctrl Pts',(25.6105636315807,1.29624675778246,3.7132510476587));
#86275=CARTESIAN_POINT('Ctrl Pts',(25.6046987926359,1.40536076424958,3.67516079324382));
#86276=CARTESIAN_POINT('Ctrl Pts',(25.598833953691,1.5129440487181,3.63220474850107));
#86277=CARTESIAN_POINT('Ctrl Pts',(25.5929691147462,1.61853267185289,3.58452800102674));
#86278=CARTESIAN_POINT('Ctrl Pts',(25.5871103046262,1.72401275401673,3.53690026338234));
#86279=CARTESIAN_POINT('Ctrl Pts',(25.5812514945062,1.82750187880104,3.48456164437377));
#86280=CARTESIAN_POINT('Ctrl Pts',(25.5753926843862,1.92855353300051,3.42770626955567));
#86281=CARTESIAN_POINT('Ctrl Pts',(25.5693068955052,2.03352007414724,3.36864823544891));
#86282=CARTESIAN_POINT('Ctrl Pts',(25.5632211066242,2.13585603375695,3.30471654586177));
#86283=CARTESIAN_POINT('Ctrl Pts',(25.5571353177433,2.23508598156619,3.23618288343016));
#86284=CARTESIAN_POINT('Ctrl Pts',(25.551283287665,2.33050444753691,3.17028164009632));
#86285=CARTESIAN_POINT('Ctrl Pts',(25.5454312575867,2.42305073626668,3.10012568831626));
#86286=CARTESIAN_POINT('Ctrl Pts',(25.5395792275085,2.51233005976414,3.02600176318612));
#86287=CARTESIAN_POINT('Ctrl Pts',(25.5337280871299,2.60159580988775,2.95188910731417));
#86288=CARTESIAN_POINT('Ctrl Pts',(25.5278769467514,2.68759526440664,2.87380994154586));
#86289=CARTESIAN_POINT('Ctrl Pts',(25.5220258063729,2.76996634961764,2.79209158552974));
#86290=CARTESIAN_POINT('Ctrl Pts',(25.5161741388054,2.85234485648086,2.71036586667242));
#86291=CARTESIAN_POINT('Ctrl Pts',(25.5103224712379,2.93109405069021,2.62500059688869));
#86292=CARTESIAN_POINT('Ctrl Pts',(25.5044708036704,3.00588890920285,2.53635976658109));
#86293=CARTESIAN_POINT('Ctrl Pts',(25.4986171919862,3.08070861703143,2.44768948686959));
#86294=CARTESIAN_POINT('Ctrl Pts',(25.4927635803019,3.15157111040107,2.35574179846793));
#86295=CARTESIAN_POINT('Ctrl Pts',(25.4869099686177,3.21819227414718,2.26091297634814));
#86296=CARTESIAN_POINT('Ctrl Pts',(25.4810497025178,3.28488917317232,2.1659763523393));
#86297=CARTESIAN_POINT('Ctrl Pts',(25.4751894364179,3.34733488112954,2.06815239567862));
#86298=CARTESIAN_POINT('Ctrl Pts',(25.469329170318,3.40528912530119,1.96786558817046));
#86299=CARTESIAN_POINT('Ctrl Pts',(25.4634649571468,3.46328240345805,1.8675112343796));
#86300=CARTESIAN_POINT('Ctrl Pts',(25.4576007439755,3.51677800384791,1.76469109252163));
#86301=CARTESIAN_POINT('Ctrl Pts',(25.4517365308042,3.56558282524708,1.6598518356477));
#86302=CARTESIAN_POINT('Ctrl Pts',(25.4458636822299,3.6144595146511,1.55485819672696));
#86303=CARTESIAN_POINT('Ctrl Pts',(25.4399908336556,3.65863148205304,1.44783988939282));
#86304=CARTESIAN_POINT('Ctrl Pts',(25.4341179850813,3.69795466602593,1.33926109777634));
#86305=CARTESIAN_POINT('Ctrl Pts',(25.4325232404685,3.70863269305282,1.30977703381479));
#86306=CARTESIAN_POINT('Ctrl Pts',(25.4309284958556,3.718953474776,1.28017797382429));
#86307=CARTESIAN_POINT('Ctrl Pts',(25.4293337512428,3.7289147753841,1.25047334954495));
#86308=CARTESIAN_POINT('Ctrl Pts',(25.4234613051088,3.76559600996759,1.14108981276867));
#86309=CARTESIAN_POINT('Ctrl Pts',(25.4175888589749,3.79752161144521,1.02990777090968));
#86310=CARTESIAN_POINT('Ctrl Pts',(25.411716412841,3.82451377617999,0.917378534635202));
#86311=CARTESIAN_POINT('Ctrl Pts',(25.4058515738961,3.85147097516186,0.804995069161654));
#86312=CARTESIAN_POINT('Ctrl Pts',(25.3999867349513,3.87350735088755,0.691268278026297));
#86313=CARTESIAN_POINT('Ctrl Pts',(25.3941218960064,3.89049409558753,0.576666881482352));
#86314=CARTESIAN_POINT('Ctrl Pts',(25.3882630858864,3.90746337857897,0.462183290687546));
#86315=CARTESIAN_POINT('Ctrl Pts',(25.3824042757664,3.91939329513246,0.346827289198799));
#86316=CARTESIAN_POINT('Ctrl Pts',(25.3765454656464,3.92620571113299,0.231079453579754));
#86317=CARTESIAN_POINT('Ctrl Pts',(25.3704596767654,3.93328204996276,0.110847379732617));
#86318=CARTESIAN_POINT('Ctrl Pts',(25.3643738878845,3.9348362439859,-0.00980706089680983));
#86319=CARTESIAN_POINT('Ctrl Pts',(25.3582880990035,3.93083976504607,-0.130337030549801));
#86320=CARTESIAN_POINT('Ctrl Pts',(25.3524360689252,3.92699679326041,-0.246237371744446));
#86321=CARTESIAN_POINT('Ctrl Pts',(25.3465840388469,3.91802170715974,-0.362022176262712));
#86322=CARTESIAN_POINT('Ctrl Pts',(25.3407320087687,3.90394224495369,-0.477204304324647));
#86323=CARTESIAN_POINT('Ctrl Pts',(25.3348808683901,3.88986492328586,-0.592368920940156));
#86324=CARTESIAN_POINT('Ctrl Pts',(25.3290297280116,3.87068481865748,-0.706930633091622));
#86325=CARTESIAN_POINT('Ctrl Pts',(25.3231785876331,3.84648149831601,-0.820407876066914));
#86326=CARTESIAN_POINT('Ctrl Pts',(25.3173269200656,3.8222759972503,-0.933895343365568));
#86327=CARTESIAN_POINT('Ctrl Pts',(25.3114752524981,3.79304646698865,-1.04629774295961));
#86328=CARTESIAN_POINT('Ctrl Pts',(25.3056235849306,3.7589233562151,-1.15714484923049));
#86329=CARTESIAN_POINT('Ctrl Pts',(25.2997699732464,3.72478890861983,-1.26802878256231));
#86330=CARTESIAN_POINT('Ctrl Pts',(25.2939163615621,3.68575776924242,-1.37735600025294));
#86331=CARTESIAN_POINT('Ctrl Pts',(25.2880627498779,3.6420096641432,-1.48467323215835));
#86332=CARTESIAN_POINT('Ctrl Pts',(25.282202483778,3.59821182597481,-1.59211246284075));
#86333=CARTESIAN_POINT('Ctrl Pts',(25.2763422176781,3.54968647530237,-1.69753676402993));
#86334=CARTESIAN_POINT('Ctrl Pts',(25.2704819515782,3.49666077208495,-1.80051449451602));
#86335=CARTESIAN_POINT('Ctrl Pts',(25.2646177384068,3.44359935440785,-1.90356158370516));
#86336=CARTESIAN_POINT('Ctrl Pts',(25.2587535252355,3.38603175340706,-2.00415846311935));
#86337=CARTESIAN_POINT('Ctrl Pts',(25.2528893120642,3.32422930262604,-2.10190117359557));
#86338=CARTESIAN_POINT('Ctrl Pts',(25.2470164634899,3.26233584405733,-2.19978781603129));
#86339=CARTESIAN_POINT('Ctrl Pts',(25.2411436149156,3.19619532501196,-2.29481156332244));
#86340=CARTESIAN_POINT('Ctrl Pts',(25.2352707663413,3.12612032583015,-2.38660024059992));
#86341=CARTESIAN_POINT('Ctrl Pts',(25.2336760217286,3.1070917869502,-2.4115250273956));
#86342=CARTESIAN_POINT('Ctrl Pts',(25.2320812771159,3.08777334619203,-2.43621147578762));
#86343=CARTESIAN_POINT('Ctrl Pts',(25.2304865325032,3.06817172869338,-2.46065260515309));
#86344=CARTESIAN_POINT('Ctrl Pts',(25.2246140863693,2.99599124162355,-2.55065398500134));
#86345=CARTESIAN_POINT('Ctrl Pts',(25.2187416402353,2.91972641653179,-2.63762735400208));
#86346=CARTESIAN_POINT('Ctrl Pts',(25.2128691941014,2.83966075972733,-2.72117911385208));
#86347=CARTESIAN_POINT('Ctrl Pts',(25.2070043551566,2.75969882027951,-2.80462264043429));
#86348=CARTESIAN_POINT('Ctrl Pts',(25.2011395162117,2.67594612379049,-2.88465307656847));
#86349=CARTESIAN_POINT('Ctrl Pts',(25.1952746772669,2.58872731423561,-2.96090862617043));
#86350=CARTESIAN_POINT('Ctrl Pts',(25.1894158671469,2.50159816220215,-3.03708578805298));
#86351=CARTESIAN_POINT('Ctrl Pts',(25.1835570570268,2.41101029348404,-3.10949551136133));
#86352=CARTESIAN_POINT('Ctrl Pts',(25.1776982469068,2.31732572545454,-3.17781221631276));
#86353=CARTESIAN_POINT('Ctrl Pts',(25.1716124580258,2.22001168203069,-3.24877560902566));
#86354=CARTESIAN_POINT('Ctrl Pts',(25.1655266691449,2.11935645966524,-3.31532210234597));
#86355=CARTESIAN_POINT('Ctrl Pts',(25.1594408802639,2.01580463768916,-3.37713201735894));
#86356=CARTESIAN_POINT('Ctrl Pts',(25.1535888501856,1.91623030333138,-3.43656777644727));
#86357=CARTESIAN_POINT('Ctrl Pts',(25.1477368201074,1.8139781726968,-3.49162388336151));
#86358=CARTESIAN_POINT('Ctrl Pts',(25.1418847900291,1.70947303044468,-3.54206027026394));
#86359=CARTESIAN_POINT('Ctrl Pts',(25.1360336496506,1.60498377638853,-3.59248898918773));
#86360=CARTESIAN_POINT('Ctrl Pts',(25.1301825092721,1.4982425639467,-3.63829920498125));
#86361=CARTESIAN_POINT('Ctrl Pts',(25.1243313688935,1.38969751247317,-3.67929746335165));
#86362=CARTESIAN_POINT('Ctrl Pts',(25.118479701326,1.28114268106726,-3.7202994156739));
#86363=CARTESIAN_POINT('Ctrl Pts',(25.1126280337585,1.17078407425861,-3.7564884026335));
#86364=CARTESIAN_POINT('Ctrl Pts',(25.106776366191,1.05908778496831,-3.78771990301961));
#86365=CARTESIAN_POINT('Ctrl Pts',(25.1009227545068,0.947354386491927,-3.81896177953878));
#86366=CARTESIAN_POINT('Ctrl Pts',(25.0950691428226,0.83428281970488,-3.8452427831944));
#86367=CARTESIAN_POINT('Ctrl Pts',(25.0892155311384,0.720351559213901,-3.86646901334255));
#86368=CARTESIAN_POINT('Ctrl Pts',(25.0833552650385,0.606290781083612,-3.88771937357763));
#86369=CARTESIAN_POINT('Ctrl Pts',(25.0774949989386,0.491368765187452,-3.90390341514437));
#86370=CARTESIAN_POINT('Ctrl Pts',(25.0716347328387,0.376071439674704,-3.91497883420345));
#86371=CARTESIAN_POINT('Ctrl Pts',(25.0657705196674,0.260696457828296,-3.92606171290163));
#86372=CARTESIAN_POINT('Ctrl Pts',(25.0599063064961,0.14494607482321,-3.93202909650567));
#86373=CARTESIAN_POINT('Ctrl Pts',(25.0540420933247,0.0293068175335294,
-3.93289080835536));
#86374=CARTESIAN_POINT('Ctrl Pts',(25.0481692447504,-0.086502725446165,
-3.93375378912704));
#86375=CARTESIAN_POINT('Ctrl Pts',(25.0422963961761,-0.202200404596252,
-3.92949610804844));
#86376=CARTESIAN_POINT('Ctrl Pts',(25.0364235476018,-0.317304127708729,
-3.92017947172563));
#86377=CARTESIAN_POINT('Ctrl Pts',(25.0348288029891,-0.348560006354695,
-3.91764958262716));
#86378=CARTESIAN_POINT('Ctrl Pts',(25.0332340583763,-0.379772145524845,
-3.91474695346925));
#86379=CARTESIAN_POINT('Ctrl Pts',(25.0316393137635,-0.410931036706119,
-3.9114734670034));
#86380=CARTESIAN_POINT('Ctrl Pts',(25.0257668676296,-0.525669728147831,
-3.89941926548007));
#86381=CARTESIAN_POINT('Ctrl Pts',(25.0198944214957,-0.640069673261343,
-3.88229200593471));
#86382=CARTESIAN_POINT('Ctrl Pts',(25.0140219753618,-0.753646478881124,
-3.86011735376919));
#86383=CARTESIAN_POINT('Ctrl Pts',(25.008157136417,-0.867076156674893,-3.83797142673244));
#86384=CARTESIAN_POINT('Ctrl Pts',(25.0022922974721,-0.979684413505547,
-3.81079118812873));
#86385=CARTESIAN_POINT('Ctrl Pts',(24.9964274585273,-1.0909913649604,-3.77865410451682));
#86386=CARTESIAN_POINT('Ctrl Pts',(24.9905686484073,-1.20218389722635,-3.74655005656884));
#86387=CARTESIAN_POINT('Ctrl Pts',(24.9847098382873,-1.31207739010615,-3.70949941270171));
#86388=CARTESIAN_POINT('Ctrl Pts',(24.9788510281673,-1.42020221648381,-3.66763066083466));
#86389=CARTESIAN_POINT('Ctrl Pts',(24.9727652392864,-1.5325159547089,-3.62413985308453));
#86390=CARTESIAN_POINT('Ctrl Pts',(24.9666794504054,-1.64292076745683,-3.57545015309787));
#86391=CARTESIAN_POINT('Ctrl Pts',(24.9605936615244,-1.75090734937847,-3.52176269130849));
#86392=CARTESIAN_POINT('Ctrl Pts',(24.9547416314462,-1.85474610189072,-3.47013739714183));
#86393=CARTESIAN_POINT('Ctrl Pts',(24.9488896013679,-1.95634856381872,-3.41389139410223));
#86394=CARTESIAN_POINT('Ctrl Pts',(24.9430375712896,-2.05528310254263,-3.35325220769371));
#86395=CARTESIAN_POINT('Ctrl Pts',(24.9371864309111,-2.15420259998476,-3.29262224042243));
#86396=CARTESIAN_POINT('Ctrl Pts',(24.9313352905326,-2.25045462838112,-3.22760063375053));
#86397=CARTESIAN_POINT('Ctrl Pts',(24.9254841501541,-2.34363414953303,-3.15845974695619));
#86398=CARTESIAN_POINT('Ctrl Pts',(24.9196324825866,-2.43682206617908,-3.08931263055365));
#86399=CARTESIAN_POINT('Ctrl Pts',(24.9137808150191,-2.52693659328818,-3.01604574255075));
#86400=CARTESIAN_POINT('Ctrl Pts',(24.9079291474517,-2.61360413711462,-2.93897302036908));
#86401=CARTESIAN_POINT('Ctrl Pts',(24.9020755357674,-2.70030047475459,-2.86187469208975));
#86402=CARTESIAN_POINT('Ctrl Pts',(24.8962219240832,-2.78354724322715,-2.78096828994615));
#86403=CARTESIAN_POINT('Ctrl Pts',(24.890368312399,-2.86300673635456,-2.69660553800299));
#86404=CARTESIAN_POINT('Ctrl Pts',(24.8845080462991,-2.94255655943915,-2.61214688205301));
#86405=CARTESIAN_POINT('Ctrl Pts',(24.8786477801992,-3.01831023017652,-2.5242243348382));
#86406=CARTESIAN_POINT('Ctrl Pts',(24.8727875140994,-3.08996941587409,-2.43322378933027));
#86407=CARTESIAN_POINT('Ctrl Pts',(24.8669233009281,-3.16167686626099,-2.34216195212588));
#86408=CARTESIAN_POINT('Ctrl Pts',(24.8610590877568,-3.22928409982488,-2.24801832354449));
#86409=CARTESIAN_POINT('Ctrl Pts',(24.8551948745856,-3.29253630998429,-2.15120748590996));
#86410=CARTESIAN_POINT('Ctrl Pts',(24.8493220260113,-3.3558816627889,-2.05425408855334));
#86411=CARTESIAN_POINT('Ctrl Pts',(24.843449177437,-3.41485898328074,-1.95462599775342));
#86412=CARTESIAN_POINT('Ctrl Pts',(24.8375763288627,-3.46925950741377,-1.85276211916672));
#86413=CARTESIAN_POINT('Ctrl Pts',(24.8359815842498,-3.484031715773,-1.82510145848849));
#86414=CARTESIAN_POINT('Ctrl Pts',(24.8343868396368,-3.49846672148907,-1.79727604748046));
#86415=CARTESIAN_POINT('Ctrl Pts',(24.8327920950239,-3.51256096699897,-1.76929490281164));
#86416=CARTESIAN_POINT('Ctrl Pts',(24.8265172351429,-3.5680177561215,-1.65919717262696));
#86417=CARTESIAN_POINT('Ctrl Pts',(24.8202423752619,-3.61836096930805,-1.54635787322841));
#86418=CARTESIAN_POINT('Ctrl Pts',(24.8139675153808,-3.66332972147213,-1.43125970801211));
#86419=CARTESIAN_POINT('Ctrl Pts',(24.8077119179017,-3.70816042972878,-1.31651486815399));
#86420=CARTESIAN_POINT('Ctrl Pts',(24.8014563204226,-3.74764945383605,-1.1995252913079));
#86421=CARTESIAN_POINT('Ctrl Pts',(24.7952007229434,-3.78158312857588,-1.08079509698659));
#86422=CARTESIAN_POINT('Ctrl Pts',(24.7889566520863,-3.81545427681164,-0.962283676023485));
#86423=CARTESIAN_POINT('Ctrl Pts',(24.7827125812291,-3.84379037820219,-0.842038338564769));
#86424=CARTESIAN_POINT('Ctrl Pts',(24.776468510372,-3.86642608699356,-0.720581927205831));
#86425=CARTESIAN_POINT('Ctrl Pts',(24.7702417352015,-3.88899909628404,-0.599461942527479));
#86426=CARTESIAN_POINT('Ctrl Pts',(24.764014960031,-3.90590313373206,-0.477137891634039));
#86427=CARTESIAN_POINT('Ctrl Pts',(24.7577881848605,-3.91702312745135,-0.354145194815961));
#86428=CARTESIAN_POINT('Ctrl Pts',(24.7518466425865,-3.92763374224968,-0.236786483841156));
#86429=CARTESIAN_POINT('Ctrl Pts',(24.7459051003125,-3.93297833254885,-0.118819332281221));
#86430=CARTESIAN_POINT('Ctrl Pts',(24.7399635580385,-3.93299993420865,-0.000719384965967845));
#86431=CARTESIAN_POINT('',(23.4899635046889,-3.93299832268712,0.00363231885978147));
#86432=CARTESIAN_POINT('Ctrl Pts',(24.739963522035,-3.92661513087914,-0.000717502642775814));
#86433=CARTESIAN_POINT('Ctrl Pts',(24.7046239734514,-3.92547634547242,0.700586071088623));
#86434=CARTESIAN_POINT('Ctrl Pts',(24.6030020186211,-3.41092723159537,2.71880545169115));
#86435=CARTESIAN_POINT('Ctrl Pts',(24.4350976575446,-0.178456178513938,
4.64824089454367));
#86436=CARTESIAN_POINT('Ctrl Pts',(24.236250438805,3.81364859256515,2.66347037411458));
#86437=CARTESIAN_POINT('Ctrl Pts',(24.0374032200652,4.30261386396493,-1.76790948834883));
#86438=CARTESIAN_POINT('Ctrl Pts',(23.8385560013257,0.839286150601286,-4.57532389878272));
#86439=CARTESIAN_POINT('Ctrl Pts',(23.6560761019823,-3.0464647852414,-3.29479500069049));
#86440=CARTESIAN_POINT('Ctrl Pts',(23.5398786088853,-3.9234348859021,-0.983222851819869));
#86441=CARTESIAN_POINT('Ctrl Pts',(23.489963522035,-3.93244535509981,0.00363146522480512));
#86442=CARTESIAN_POINT('',(22.2399631348525,-3.93532363914096,-0.000943749275237955));
#86443=CARTESIAN_POINT('Ctrl Pts',(23.4899635046889,-3.93299832268712,0.00363231885978147));
#86444=CARTESIAN_POINT('Ctrl Pts',(23.4824079195757,-3.93286034573355,0.15303085679816));
#86445=CARTESIAN_POINT('Ctrl Pts',(23.4748523344626,-3.9242063378758,0.30204887539334));
#86446=CARTESIAN_POINT('Ctrl Pts',(23.4672967493495,-3.90718678259729,0.449867142495451));
#86447=CARTESIAN_POINT('Ctrl Pts',(23.4595604189944,-3.88976008431239,0.601221528649032));
#86448=CARTESIAN_POINT('Ctrl Pts',(23.4518240886393,-3.86356278656303,0.751318393200962));
#86449=CARTESIAN_POINT('Ctrl Pts',(23.4440877582841,-3.82880428901931,0.899303461789901));
#86450=CARTESIAN_POINT('Ctrl Pts',(23.4430123601382,-3.82397264118408,0.919874308829396));
#86451=CARTESIAN_POINT('Ctrl Pts',(23.4419369619923,-3.81897564221488,0.940404384476784));
#86452=CARTESIAN_POINT('Ctrl Pts',(23.4408615638464,-3.81381392671508,0.960891425913532));
#86453=CARTESIAN_POINT('Ctrl Pts',(23.4349891177125,-3.78562725339186,1.07276538416606));
#86454=CARTESIAN_POINT('Ctrl Pts',(23.4291166715786,-3.7524666701744,1.18358535611239));
#86455=CARTESIAN_POINT('Ctrl Pts',(23.4232442254447,-3.71442620341627,1.29287546939936));
#86456=CARTESIAN_POINT('Ctrl Pts',(23.4173793864999,-3.67643501442353,1.40202400785769));
#86457=CARTESIAN_POINT('Ctrl Pts',(23.4115145475551,-3.63357664757394,1.50964624193568));
#86458=CARTESIAN_POINT('Ctrl Pts',(23.4056497086102,-3.58599576925675,1.61527810078411));
#86459=CARTESIAN_POINT('Ctrl Pts',(23.3997908984902,-3.53846380221969,1.72080137421707));
#86460=CARTESIAN_POINT('Ctrl Pts',(23.3939320883702,-3.48621914844071,1.82433796745765));
#86461=CARTESIAN_POINT('Ctrl Pts',(23.3880732782502,-3.42945552806597,1.92544119126442));
#86462=CARTESIAN_POINT('Ctrl Pts',(23.3819874893693,-3.3704928031022,2.03046129989939));
#86463=CARTESIAN_POINT('Ctrl Pts',(23.3759017004883,-3.30665403671978,2.13285525220847));
#86464=CARTESIAN_POINT('Ctrl Pts',(23.3698159116073,-3.23821047986439,2.23214737150046));
#86465=CARTESIAN_POINT('Ctrl Pts',(23.3639638815291,-3.1723958810977,2.32762562090973));
#86466=CARTESIAN_POINT('Ctrl Pts',(23.3581118514508,-3.10232396837973,2.42023555653111));
#86467=CARTESIAN_POINT('Ctrl Pts',(23.3522598213725,-3.02828111831431,2.50958213024819));
#86468=CARTESIAN_POINT('Ctrl Pts',(23.346408680994,-2.95424952518105,2.59891512036715));
#86469=CARTESIAN_POINT('Ctrl Pts',(23.3405575406155,-2.87624845876133,2.68498541688066));
#86470=CARTESIAN_POINT('Ctrl Pts',(23.334706400237,-2.79460490989147,2.76743064910587));
#86471=CARTESIAN_POINT('Ctrl Pts',(23.3288547326696,-2.71295400492076,2.84988330966375));
#86472=CARTESIAN_POINT('Ctrl Pts',(23.3230030651021,-2.62766025596515,2.92870996291517));
#86473=CARTESIAN_POINT('Ctrl Pts',(23.3171513975346,-2.53908735823309,3.00358525553394));
#86474=CARTESIAN_POINT('Ctrl Pts',(23.3112977858504,-2.45048503366638,3.07848542419168));
#86475=CARTESIAN_POINT('Ctrl Pts',(23.3054441741662,-2.35860170954444,3.14943135513341));
#86476=CARTESIAN_POINT('Ctrl Pts',(23.299590562482,-2.26383340276663,3.2161385735876));
#86477=CARTESIAN_POINT('Ctrl Pts',(23.2937302963821,-2.16895736289373,3.28292162514837));
#86478=CARTESIAN_POINT('Ctrl Pts',(23.2878700302822,-2.07119013248194,3.3454561084084));
#86479=CARTESIAN_POINT('Ctrl Pts',(23.2820097641823,-1.97095597504987,3.40350136541992));
#86480=CARTESIAN_POINT('Ctrl Pts',(23.276145551011,-1.87065430679648,3.46158571771665));
#86481=CARTESIAN_POINT('Ctrl Pts',(23.2702813378397,-1.76788276866357,3.51517463245229));
#86482=CARTESIAN_POINT('Ctrl Pts',(23.2644171246684,-1.66308785822796,3.56407460300914));
#86483=CARTESIAN_POINT('Ctrl Pts',(23.2585442760942,-1.55813863104833,3.61304658168363));
#86484=CARTESIAN_POINT('Ctrl Pts',(23.2526714275199,-1.4511604655139,3.65731567821485));
#86485=CARTESIAN_POINT('Ctrl Pts',(23.2467985789456,-1.34261741479074,3.69673740986571));
#86486=CARTESIAN_POINT('Ctrl Pts',(23.2452038343326,-1.31314305609978,3.70744219705526));
#86487=CARTESIAN_POINT('Ctrl Pts',(23.2436090897197,-1.28355337713294,3.71778984347746));
#86488=CARTESIAN_POINT('Ctrl Pts',(23.2420143451067,-1.25385780759683,3.72777810476005));
#86489=CARTESIAN_POINT('Ctrl Pts',(23.2361418989728,-1.14450761378008,3.76455861862816));
#86490=CARTESIAN_POINT('Ctrl Pts',(23.2302694528389,-1.03335459863079,3.79658513396738));
#86491=CARTESIAN_POINT('Ctrl Pts',(23.224397006705,-0.920849911226558,3.82367943753056));
#86492=CARTESIAN_POINT('Ctrl Pts',(23.2185321677601,-0.808490962822574,
3.85073864302979));
#86493=CARTESIAN_POINT('Ctrl Pts',(23.2126673288153,-0.694784222365801,
3.87287824672256));
#86494=CARTESIAN_POINT('Ctrl Pts',(23.2068024898704,-0.58019829298932,3.88996901540517));
#86495=CARTESIAN_POINT('Ctrl Pts',(23.2009436797504,-0.465730153462115,
3.9070422154467));
#86496=CARTESIAN_POINT('Ctrl Pts',(23.1950848696304,-0.350385029046763,
3.91907684306931));
#86497=CARTESIAN_POINT('Ctrl Pts',(23.1892260595104,-0.234643425181591,
3.92599432794025));
#86498=CARTESIAN_POINT('Ctrl Pts',(23.1831402706294,-0.114417824515235,
3.93317980616016));
#86499=CARTESIAN_POINT('Ctrl Pts',(23.1770544817485,0.00623515556169527,
3.93484352525785));
#86500=CARTESIAN_POINT('Ctrl Pts',(23.1709686928675,0.126768703412605,3.93095646068932));
#86501=CARTESIAN_POINT('Ctrl Pts',(23.1651166627892,0.242672485364009,3.92721870060331));
#86502=CARTESIAN_POINT('Ctrl Pts',(23.159264632711,0.358465389433446,3.91834872343684));
#86503=CARTESIAN_POINT('Ctrl Pts',(23.1534126026327,0.473660250861932,3.90437382518035));
#86504=CARTESIAN_POINT('Ctrl Pts',(23.1475614622542,0.588837598908159,3.89040105156493));
#86505=CARTESIAN_POINT('Ctrl Pts',(23.1417103218757,0.703416674859619,3.87132494979667));
#86506=CARTESIAN_POINT('Ctrl Pts',(23.1358591814972,0.816915841974344,3.8472246499433));
#86507=CARTESIAN_POINT('Ctrl Pts',(23.1300075139297,0.930425235387965,3.82312217864783));
#86508=CARTESIAN_POINT('Ctrl Pts',(23.1241558463622,1.0428541221751,3.7939946952414));
#86509=CARTESIAN_POINT('Ctrl Pts',(23.1183041787948,1.15373215849437,3.75997222150057));
#86510=CARTESIAN_POINT('Ctrl Pts',(23.1124505671105,1.26464703215,3.72593844437315));
#86511=CARTESIAN_POINT('Ctrl Pts',(23.1065969554263,1.37400963584463,3.68700656435129));
#86512=CARTESIAN_POINT('Ctrl Pts',(23.1007433437421,1.48136653647223,3.64335589595915));
#86513=CARTESIAN_POINT('Ctrl Pts',(23.0948830776422,1.58884548097268,3.59965560526427));
#86514=CARTESIAN_POINT('Ctrl Pts',(23.0890228115423,1.6943137882741,3.55122597493344));
#86515=CARTESIAN_POINT('Ctrl Pts',(23.0831625454425,1.79733961113691,3.49829377300395));
#86516=CARTESIAN_POINT('Ctrl Pts',(23.0772983322712,1.90043482509449,3.4453259195908));
#86517=CARTESIAN_POINT('Ctrl Pts',(23.0714341190999,2.00108392083609,3.38784966049926));
#86518=CARTESIAN_POINT('Ctrl Pts',(23.0655699059286,2.09888269305838,3.32613596246155));
#86519=CARTESIAN_POINT('Ctrl Pts',(23.0596970573543,2.19682547979467,3.2643313873297));
#86520=CARTESIAN_POINT('Ctrl Pts',(23.05382420878,2.29190922789305,3.19827715463894));
#86521=CARTESIAN_POINT('Ctrl Pts',(23.0479513602057,2.38376147888872,3.12828550675386));
#86522=CARTESIAN_POINT('Ctrl Pts',(23.0463566155929,2.40870352883323,3.10927960152754));
#86523=CARTESIAN_POINT('Ctrl Pts',(23.04476187098,2.43340750363462,3.08998357818745));
#86524=CARTESIAN_POINT('Ctrl Pts',(23.0431671263671,2.45786641656803,3.07040415553181));
#86525=CARTESIAN_POINT('Ctrl Pts',(23.0372946802332,2.54793328215618,2.99830539818229));
#86526=CARTESIAN_POINT('Ctrl Pts',(23.0314222340993,2.63497584575797,2.9221195557755));
#86527=CARTESIAN_POINT('Ctrl Pts',(23.0255497879654,2.71860025187564,2.84212977720964));
#86528=CARTESIAN_POINT('Ctrl Pts',(23.0196849490205,2.80211633061937,2.76224361770735));
#86529=CARTESIAN_POINT('Ctrl Pts',(23.0138201100757,2.88222276143276,2.67856360444628));
#86530=CARTESIAN_POINT('Ctrl Pts',(23.0079552711308,2.95855745368066,2.59141405284269));
#86531=CARTESIAN_POINT('Ctrl Pts',(23.0020964610108,3.03481367685349,2.5043540875662));
#86532=CARTESIAN_POINT('Ctrl Pts',(22.9962376508908,3.10730560270164,2.41383198708636));
#86533=CARTESIAN_POINT('Ctrl Pts',(22.9903788407708,3.17570732295032,2.32020947307775));
#86534=CARTESIAN_POINT('Ctrl Pts',(22.9842930518898,3.24675902457591,2.222959887737));
#86535=CARTESIAN_POINT('Ctrl Pts',(22.9782072630088,3.31339686162952,2.12236511533057));
#86536=CARTESIAN_POINT('Ctrl Pts',(22.9721214741278,3.37530075175515,2.01886944481338));
#86537=CARTESIAN_POINT('Ctrl Pts',(22.9662694440496,3.43482687631556,1.91934910510346));
#86538=CARTESIAN_POINT('Ctrl Pts',(22.9604174139713,3.4899757813125,1.817146994531));
#86539=CARTESIAN_POINT('Ctrl Pts',(22.954565383893,3.5405070134031,1.71268767965543));
#86540=CARTESIAN_POINT('Ctrl Pts',(22.9487142435145,3.59103056309559,1.60824424600833));
#86541=CARTESIAN_POINT('Ctrl Pts',(22.942863103136,3.63693765580665,1.50154466239417));
#86542=CARTESIAN_POINT('Ctrl Pts',(22.9370119627575,3.6780344305367,1.39303687237151));
#86543=CARTESIAN_POINT('Ctrl Pts',(22.93116029519,3.71913490809483,1.28451930577405));
#86544=CARTESIAN_POINT('Ctrl Pts',(22.9253086276225,3.75542405967508,1.17419359548204));
#86545=CARTESIAN_POINT('Ctrl Pts',(22.919456960055,3.78675694102397,1.06252570303348));
#86546=CARTESIAN_POINT('Ctrl Pts',(22.9136033483708,3.81810023218825,0.950820710832328));
#86547=CARTESIAN_POINT('Ctrl Pts',(22.9077497366865,3.84448386727344,0.837773047571822));
#86548=CARTESIAN_POINT('Ctrl Pts',(22.9018961250023,3.86581351133244,0.72386110242196));
#86549=CARTESIAN_POINT('Ctrl Pts',(22.8960358589024,3.88716740303973,0.609819661591173));
#86550=CARTESIAN_POINT('Ctrl Pts',(22.8901755928025,3.90345575996642,0.494912384329474));
#86551=CARTESIAN_POINT('Ctrl Pts',(22.8843153267026,3.91463583718272,0.379625160184026));
#86552=CARTESIAN_POINT('Ctrl Pts',(22.8784511135313,3.92582344452861,0.264260286508817));
#86553=CARTESIAN_POINT('Ctrl Pts',(22.87258690036,3.93189589966359,0.148515368169132));
#86554=CARTESIAN_POINT('Ctrl Pts',(22.8667226871887,3.93286258427199,0.0328769407558719));
#86555=CARTESIAN_POINT('Ctrl Pts',(22.8608498386144,3.93383069238102,-0.0829317711256017));
#86556=CARTESIAN_POINT('Ctrl Pts',(22.8549769900401,3.92967803920366,-0.198633267574225));
#86557=CARTESIAN_POINT('Ctrl Pts',(22.8491041414658,3.92046589369477,-0.313745400565606));
#86558=CARTESIAN_POINT('Ctrl Pts',(22.847509396853,3.91796437858899,-0.345003562875146));
#86559=CARTESIAN_POINT('Ctrl Pts',(22.8459146522402,3.91509008387223,-0.376218324086762));
#86560=CARTESIAN_POINT('Ctrl Pts',(22.8443199076274,3.91184488366374,-0.407380173982224));
#86561=CARTESIAN_POINT('Ctrl Pts',(22.8384474614935,3.8998948427197,-0.522129760516045));
#86562=CARTESIAN_POINT('Ctrl Pts',(22.8325750153596,3.88287143834218,-0.636545205998862));
#86563=CARTESIAN_POINT('Ctrl Pts',(22.8267025692257,3.86079989620795,-0.750142094166606));
#86564=CARTESIAN_POINT('Ctrl Pts',(22.8208377302808,3.83875694563342,-0.863591828493058));
#86565=CARTESIAN_POINT('Ctrl Pts',(22.814972891336,3.81167893991004,-0.976224712159847));
#86566=CARTESIAN_POINT('Ctrl Pts',(22.8091080523911,3.77964290994305,-1.08756079063067));
#86567=CARTESIAN_POINT('Ctrl Pts',(22.8032492422711,3.74763981176064,-1.19878241997172));
#86568=CARTESIAN_POINT('Ctrl Pts',(22.7973904321511,3.71068894047635,-1.30870950080175));
#86569=CARTESIAN_POINT('Ctrl Pts',(22.791531622031,3.66891835764608,-1.41687228956162));
#86570=CARTESIAN_POINT('Ctrl Pts',(22.7854458331501,3.62552952214327,-1.52922546088548));
#86571=CARTESIAN_POINT('Ctrl Pts',(22.7793600442691,3.57694006369284,-1.63967442688406));
#86572=CARTESIAN_POINT('Ctrl Pts',(22.7732742553881,3.52335065031684,-1.74770969983917));
#86573=CARTESIAN_POINT('Ctrl Pts',(22.7674222253098,3.47181963846494,-1.8515952731335));
#86574=CARTESIAN_POINT('Ctrl Pts',(22.7615701952316,3.4156658896206,-1.95324875127649));
#86575=CARTESIAN_POINT('Ctrl Pts',(22.7557181651533,3.3551165373737,-2.05223829528676));
#86576=CARTESIAN_POINT('Ctrl Pts',(22.7498670247748,3.29457639060643,-2.15121278965245));
#86577=CARTESIAN_POINT('Ctrl Pts',(22.7440158843962,3.22964218481652,-2.24752380264201));
#86578=CARTESIAN_POINT('Ctrl Pts',(22.7381647440177,3.16058591149103,-2.34076604898577));
#86579=CARTESIAN_POINT('Ctrl Pts',(22.7323130764502,3.09152341618074,-2.43401669647558));
#86580=CARTESIAN_POINT('Ctrl Pts',(22.7264614088827,3.01833836105618,-2.5241976954736));
#86581=CARTESIAN_POINT('Ctrl Pts',(22.7206097413152,2.94134434427477,-2.61093516740704));
#86582=CARTESIAN_POINT('Ctrl Pts',(22.714756129631,2.86432474754457,-2.69770145638605));
#86583=CARTESIAN_POINT('Ctrl Pts',(22.7089025179467,2.78349394712559,-2.78102163444996));
#86584=CARTESIAN_POINT('Ctrl Pts',(22.7030489062625,2.69920336038026,-2.86055767627781));
#86585=CARTESIAN_POINT('Ctrl Pts',(22.6971886401626,2.61481695166547,-2.94018413508418));
#86586=CARTESIAN_POINT('Ctrl Pts',(22.6913283740627,2.52696320710391,-3.01601758750192));
#86587=CARTESIAN_POINT('Ctrl Pts',(22.6854681079628,2.4360277486927,-3.08775935066176));
#86588=CARTESIAN_POINT('Ctrl Pts',(22.6796038947915,2.34503104242302,-3.1595494341296));
#86589=CARTESIAN_POINT('Ctrl Pts',(22.6737396816202,2.25094882401828,-3.22724210000187));
#86590=CARTESIAN_POINT('Ctrl Pts',(22.6678754684489,2.15419544432737,-3.29058216545936));
#86591=CARTESIAN_POINT('Ctrl Pts',(22.6620026198746,2.05729958952528,-3.35401550293377));
#86592=CARTESIAN_POINT('Ctrl Pts',(22.6561297713003,1.95772507724096,-3.41308323788457));
#86593=CARTESIAN_POINT('Ctrl Pts',(22.650256922726,1.85591062344171,-3.46757620792913));
#86594=CARTESIAN_POINT('Ctrl Pts',(22.6486621781132,1.82826338383714,-3.48237351954225));
#86595=CARTESIAN_POINT('Ctrl Pts',(22.6470674335005,1.80045108787041,-3.49683377820558));
#86596=CARTESIAN_POINT('Ctrl Pts',(22.6454726888878,1.77248274897734,-3.51095341817258));
#86597=CARTESIAN_POINT('Ctrl Pts',(22.6396002427538,1.66949286439449,-3.56294721358935));
#86598=CARTESIAN_POINT('Ctrl Pts',(22.6337277966199,1.56404084268664,-3.61049257697362));
#86599=CARTESIAN_POINT('Ctrl Pts',(22.627855350486,1.456547818915,-3.65334879955555));
#86600=CARTESIAN_POINT('Ctrl Pts',(22.6219905115412,1.34919404201552,-3.69614950602361));
#86601=CARTESIAN_POINT('Ctrl Pts',(22.6161256725963,1.23980490129853,-3.73427299970174));
#86602=CARTESIAN_POINT('Ctrl Pts',(22.6102608336515,1.12882579019753,-3.76752456334194));
#86603=CARTESIAN_POINT('Ctrl Pts',(22.6044020235314,1.01796076127777,-3.80074194567657));
#86604=CARTESIAN_POINT('Ctrl Pts',(22.5985432134114,0.905509406527807,-3.82909724153774));
#86605=CARTESIAN_POINT('Ctrl Pts',(22.5926844032914,0.791936122611474,-3.85244418229559));
#86606=CARTESIAN_POINT('Ctrl Pts',(22.5865986144104,0.673962845738983,-3.87669561723851));
#86607=CARTESIAN_POINT('Ctrl Pts',(22.5805128255295,0.554779373282434,-3.8955426184819));
#86608=CARTESIAN_POINT('Ctrl Pts',(22.5744270366485,0.434922794106225,-3.90887850452874));
#86609=CARTESIAN_POINT('Ctrl Pts',(22.5685750065702,0.319669978056154,-3.92170215119032));
#86610=CARTESIAN_POINT('Ctrl Pts',(22.5627229764919,0.20379525911963,-3.92943019358294));
#86611=CARTESIAN_POINT('Ctrl Pts',(22.5568709464137,0.0877847175549696,
-3.93202019874819));
#86612=CARTESIAN_POINT('Ctrl Pts',(22.5510198060352,-0.0282081866174044,
-3.93460981014805));
#86613=CARTESIAN_POINT('Ctrl Pts',(22.5451686656566,-0.144336459218755,
-3.93206292827684));
#86614=CARTESIAN_POINT('Ctrl Pts',(22.5393175252781,-0.260112102085443,
-3.92438921290291));
#86615=CARTESIAN_POINT('Ctrl Pts',(22.5334658577106,-0.375898176362008,
-3.9167148061256));
#86616=CARTESIAN_POINT('Ctrl Pts',(22.5276141901431,-0.491331145267315,
-3.90391267491319));
#86617=CARTESIAN_POINT('Ctrl Pts',(22.5217625225756,-0.605926933078434,
-3.88604446085865));
#86618=CARTESIAN_POINT('Ctrl Pts',(22.5159089108914,-0.720560793385398,
-3.86817031039476));
#86619=CARTESIAN_POINT('Ctrl Pts',(22.5100552992071,-0.834356511329692,
-3.84522679395706));
#86620=CARTESIAN_POINT('Ctrl Pts',(22.5042016875229,-0.946839722032035,
-3.81732675321124));
#86621=CARTESIAN_POINT('Ctrl Pts',(22.498341421423,-1.05945080422265,-3.78939499555665));
#86622=CARTESIAN_POINT('Ctrl Pts',(22.4924811553231,-1.17074599962289,-3.75649556668775));
#86623=CARTESIAN_POINT('Ctrl Pts',(22.4866208892232,-1.28026554377832,-3.71879135438034));
#86624=CARTESIAN_POINT('Ctrl Pts',(22.4807566760519,-1.38985885275179,-3.68106174711369));
#86625=CARTESIAN_POINT('Ctrl Pts',(22.4748924628806,-1.49767374552357,-3.63852106388615));
#86626=CARTESIAN_POINT('Ctrl Pts',(22.4690282497093,-1.60327151628474,-3.59137988036215));
#86627=CARTESIAN_POINT('Ctrl Pts',(22.463155401135,-1.7090247860494,-3.54416927863918));
#86628=CARTESIAN_POINT('Ctrl Pts',(22.4572825525607,-1.81255404958358,-3.49234484037944));
#86629=CARTESIAN_POINT('Ctrl Pts',(22.4514097039864,-1.91344613941091,-3.43616252112345));
#86630=CARTESIAN_POINT('Ctrl Pts',(22.4498149593737,-1.94084291538542,-3.42090647461853));
#86631=CARTESIAN_POINT('Ctrl Pts',(22.4482202147609,-1.96804540707908,-3.40532933324931));
#86632=CARTESIAN_POINT('Ctrl Pts',(22.4466254701481,-1.9950457412971,-3.38943675116269));
#86633=CARTESIAN_POINT('Ctrl Pts',(22.4407530240142,-2.09447107060941,-3.33091431974292));
#86634=CARTESIAN_POINT('Ctrl Pts',(22.4348805778803,-2.19148564199589,-3.26791540387743));
#86635=CARTESIAN_POINT('Ctrl Pts',(22.4290081317464,-2.28565925705394,-3.20066411243723));
#86636=CARTESIAN_POINT('Ctrl Pts',(22.4231432928016,-2.37971087925262,-3.13349993857594));
#86637=CARTESIAN_POINT('Ctrl Pts',(22.4172784538568,-2.47092853041574,-3.06209458168142));
#86638=CARTESIAN_POINT('Ctrl Pts',(22.411413614912,-2.5589075838686,-2.9867174250705));
#86639=CARTESIAN_POINT('Ctrl Pts',(22.405554804792,-2.64679619829897,-2.91141775322549));
#86640=CARTESIAN_POINT('Ctrl Pts',(22.399695994672,-2.73145252486569,-2.83215467001134));
#86641=CARTESIAN_POINT('Ctrl Pts',(22.3938371845519,-2.81250241706229,-2.74923974109549));
#86642=CARTESIAN_POINT('Ctrl Pts',(22.387751395671,-2.89669229907429,-2.66311256814963));
#86643=CARTESIAN_POINT('Ctrl Pts',(22.38166560679,-2.97699028842615,-2.57304513525218));
#86644=CARTESIAN_POINT('Ctrl Pts',(22.375579817909,-3.05301623424322,-2.47943156256577));
#86645=CARTESIAN_POINT('Ctrl Pts',(22.3697277878308,-3.12612197786177,-2.38941374337947));
#86646=CARTESIAN_POINT('Ctrl Pts',(22.3638757577525,-3.1952775230049,-2.29611752853822));
#86647=CARTESIAN_POINT('Ctrl Pts',(22.3580237276743,-3.26018434611698,-2.19992886915322));
#86648=CARTESIAN_POINT('Ctrl Pts',(22.3521725872958,-3.32508130127155,-2.10375483358679));
#86649=CARTESIAN_POINT('Ctrl Pts',(22.3463214469173,-3.38573058759472,-2.00468957038597));
#86650=CARTESIAN_POINT('Ctrl Pts',(22.3404703065388,-3.44187646536597,-1.90314881109173));
#86651=CARTESIAN_POINT('Ctrl Pts',(22.3346186389713,-3.49802740189262,-1.80159890295372));
#86652=CARTESIAN_POINT('Ctrl Pts',(22.3287669714038,-3.54967392322551,-1.69757341709578));
#86653=CARTESIAN_POINT('Ctrl Pts',(22.3229153038363,-3.59660613812219,-1.59151289257164));
#86654=CARTESIAN_POINT('Ctrl Pts',(22.3170616921521,-3.64355394544678,-1.48541713124725));
#86655=CARTESIAN_POINT('Ctrl Pts',(22.3112080804679,-3.6857841647678,-1.37728536466135));
#86656=CARTESIAN_POINT('Ctrl Pts',(22.3053544687837,-3.723135225553,-1.267577647423));
#86657=CARTESIAN_POINT('Ctrl Pts',(22.2994942026838,-3.76052874721483,-1.15774521389146));
#86658=CARTESIAN_POINT('Ctrl Pts',(22.2936339365839,-3.79303190610754,-1.04633364536741));
#86659=CARTESIAN_POINT('Ctrl Pts',(22.287773670484,-3.820533125532,-0.933817774896539));
#86660=CARTESIAN_POINT('Ctrl Pts',(22.2819094573127,-3.84805286788273,-0.821226121488842));
#86661=CARTESIAN_POINT('Ctrl Pts',(22.2760452441415,-3.8705638823988,-0.707529089609426));
#86662=CARTESIAN_POINT('Ctrl Pts',(22.2701810309702,-3.88800609448337,-0.593209582913304));
#86663=CARTESIAN_POINT('Ctrl Pts',(22.2643081823959,-3.90547399126356,-0.478721733938183));
#86664=CARTESIAN_POINT('Ctrl Pts',(22.2584353338216,-3.9178581446798,-0.363609990171793));
#86665=CARTESIAN_POINT('Ctrl Pts',(22.2525624852473,-3.92515046292946,-0.248360309559825));
#86666=CARTESIAN_POINT('Ctrl Pts',(22.2509677406344,-3.92713065790591,-0.217064796833616));
#86667=CARTESIAN_POINT('Ctrl Pts',(22.2493729960215,-3.9287356935202,-0.185759098495439));
#86668=CARTESIAN_POINT('Ctrl Pts',(22.2477782514086,-3.92996606897404,-0.154452894802086));
#86669=CARTESIAN_POINT('Ctrl Pts',(22.2451733416174,-3.93197580585645,-0.103316282791359));
#86670=CARTESIAN_POINT('Ctrl Pts',(22.2425684318262,-3.93298750996713,-0.052140189329702));
#86671=CARTESIAN_POINT('Ctrl Pts',(22.239963522035,-3.93299988507042,-0.000950808129968768));
#86672=CARTESIAN_POINT('',(20.9899638959796,-3.93207325480824,-0.00316412887844202));
#86673=CARTESIAN_POINT('Ctrl Pts',(22.2399624835488,-3.93923257004676,-0.000931875137709155));
#86674=CARTESIAN_POINT('Ctrl Pts',(22.1762853332555,-3.93515111789854,1.25237922762071));
#86675=CARTESIAN_POINT('Ctrl Pts',(22.0463257767155,-2.60887796690492,3.81768824482034));
#86676=CARTESIAN_POINT('Ctrl Pts',(21.8500838139293,1.76400300349318,4.3042169351731));
#86677=CARTESIAN_POINT('Ctrl Pts',(21.6512365951896,4.57456014021278,0.843439117503365));
#86678=CARTESIAN_POINT('Ctrl Pts',(21.4523893764499,3.18302001183926,-3.39210460121854));
#86679=CARTESIAN_POINT('Ctrl Pts',(21.2535421577102,-1.13237711623261,-4.51173049815657));
#86680=CARTESIAN_POINT('Ctrl Pts',(21.0994006690304,-3.67124635021135,-2.1670127640921));
#86681=CARTESIAN_POINT('Ctrl Pts',(21.0115415865969,-3.93275998093503,-0.430560889368484));
#86682=CARTESIAN_POINT('Ctrl Pts',(20.9899649104101,-3.92956263409438,-0.00318220646910175));
#86683=CARTESIAN_POINT('',(19.7399630144492,-3.93119624677767,0.0022721441981891));
#86684=CARTESIAN_POINT('Ctrl Pts',(20.989963522035,-3.93299873257221,-0.00315746502512106));
#86685=CARTESIAN_POINT('Ctrl Pts',(20.9841232485646,-3.93309168334435,0.112623791810322));
#86686=CARTESIAN_POINT('Ctrl Pts',(20.9782829750942,-3.92806771476633,0.228472972992468));
#86687=CARTESIAN_POINT('Ctrl Pts',(20.9724427016238,-3.91793560031064,0.343903521090631));
#86688=CARTESIAN_POINT('Ctrl Pts',(20.9666036388637,-3.90780558627987,0.459310140007778));
#86689=CARTESIAN_POINT('Ctrl Pts',(20.9607645761037,-3.89256956762769,0.574297885362371));
#86690=CARTESIAN_POINT('Ctrl Pts',(20.9549255133436,-3.8722883276806,0.688383691925197));
#86691=CARTESIAN_POINT('Ctrl Pts',(20.9490862357527,-3.8520063415458,0.802473695934891));
#86692=CARTESIAN_POINT('Ctrl Pts',(20.9432469581617,-3.82667883766087,0.915661286759442));
#86693=CARTESIAN_POINT('Ctrl Pts',(20.9374076805708,-3.79641789498912,1.02747270844844));
#86694=CARTESIAN_POINT('Ctrl Pts',(20.9315667627835,-3.76614845231261,1.13931553687937));
#86695=CARTESIAN_POINT('Ctrl Pts',(20.9257258449962,-3.73094292380567,1.24978102730664));
#86696=CARTESIAN_POINT('Ctrl Pts',(20.919884927209,-3.69096330339389,1.35841042877315));
#86697=CARTESIAN_POINT('Ctrl Pts',(20.914037239955,-3.65093734767691,1.46716572879546));
#86698=CARTESIAN_POINT('Ctrl Pts',(20.908189552701,-3.60612639588913,1.57408030124601));
#86699=CARTESIAN_POINT('Ctrl Pts',(20.9023418654471,-3.55674074244052,1.67871507143518));
#86700=CARTESIAN_POINT('Ctrl Pts',(20.8964904987089,-3.50732401453099,1.78341567995696));
#86701=CARTESIAN_POINT('Ctrl Pts',(20.8906391319708,-3.45332704621566,1.88583326332586));
#86702=CARTESIAN_POINT('Ctrl Pts',(20.8847877652327,-3.39500537267214,1.98555471330491));
#86703=CARTESIAN_POINT('Ctrl Pts',(20.8789267994929,-3.33658802407192,2.08543975350351));
#86704=CARTESIAN_POINT('Ctrl Pts',(20.8730658337531,-3.27383202684813,2.18261947962998));
#86705=CARTESIAN_POINT('Ctrl Pts',(20.8672048680132,-3.20703557374272,2.2767107477123));
#86706=CARTESIAN_POINT('Ctrl Pts',(20.8634191520858,-3.16389039807688,2.33748619463052));
#86707=CARTESIAN_POINT('Ctrl Pts',(20.8596334361584,-3.11906032460714,2.39697376210787));
#86708=CARTESIAN_POINT('Ctrl Pts',(20.855847720231,-3.07263405224841,2.45507820261667));
#86709=CARTESIAN_POINT('Ctrl Pts',(20.8499752740971,-3.00061708403131,2.54521047972609));
#86710=CARTESIAN_POINT('Ctrl Pts',(20.8441028279632,-2.92451028708953,2.63232216620249));
#86711=CARTESIAN_POINT('Ctrl Pts',(20.8382303818293,-2.84459645267688,2.7160191496781));
#86712=CARTESIAN_POINT('Ctrl Pts',(20.8323655428845,-2.76478613894951,2.79960771176272));
#86713=CARTESIAN_POINT('Ctrl Pts',(20.8265007039396,-2.68117887787208,2.87979007124439));
#86714=CARTESIAN_POINT('Ctrl Pts',(20.8206358649948,-2.59409865603453,2.95620384323542));
#86715=CARTESIAN_POINT('Ctrl Pts',(20.8147770548748,-2.50710794925554,3.03253906486069));
#86716=CARTESIAN_POINT('Ctrl Pts',(20.8089182447548,-2.41665169160741,3.10511313351274));
#86717=CARTESIAN_POINT('Ctrl Pts',(20.8030594346348,-2.32309130876799,3.17359981269325));
#86718=CARTESIAN_POINT('Ctrl Pts',(20.7969736457538,-2.22590626164745,3.24473976468245));
#86719=CARTESIAN_POINT('Ctrl Pts',(20.7908878568728,-2.1253720220937,3.31146889055746));
#86720=CARTESIAN_POINT('Ctrl Pts',(20.7848020679919,-2.02193258831947,3.37346670478481));
#86721=CARTESIAN_POINT('Ctrl Pts',(20.7789500379136,-1.92246632526592,3.43308314576557));
#86722=CARTESIAN_POINT('Ctrl Pts',(20.7730980078354,-1.82031431897399,3.48832480340048));
#86723=CARTESIAN_POINT('Ctrl Pts',(20.7672459777571,-1.71590091755337,3.53895083903966));
#86724=CARTESIAN_POINT('Ctrl Pts',(20.7613948373786,-1.61150339038099,3.58956917786744));
#86725=CARTESIAN_POINT('Ctrl Pts',(20.7555436970001,-1.50484552351931,3.63557310966683));
#86726=CARTESIAN_POINT('Ctrl Pts',(20.7496925566217,-1.39637508436237,3.67676836689123));
#86727=CARTESIAN_POINT('Ctrl Pts',(20.7438408890542,-1.28789487199603,3.71796733581697));
#86728=CARTESIAN_POINT('Ctrl Pts',(20.7379892214867,-1.17760214913332,3.75435662211436));
#86729=CARTESIAN_POINT('Ctrl Pts',(20.7321375539193,-1.06596274554514,3.78579085860667));
#86730=CARTESIAN_POINT('Ctrl Pts',(20.726283942235,-0.95428625166892,3.81723553858801));
#86731=CARTESIAN_POINT('Ctrl Pts',(20.7204303305508,-0.841262585091059,
3.84372178336171));
#86732=CARTESIAN_POINT('Ctrl Pts',(20.7145767188666,-0.727370049150624,
3.86515482375527));
#86733=CARTESIAN_POINT('Ctrl Pts',(20.7087164527667,-0.613348039593898,
3.88661222933856));
#86734=CARTESIAN_POINT('Ctrl Pts',(20.7028561866668,-0.498455595654684,
3.90300488820321));
#86735=CARTESIAN_POINT('Ctrl Pts',(20.696995920567,-0.38317856787765,3.91428961436417));
#86736=CARTESIAN_POINT('Ctrl Pts',(20.6911317073957,-0.267823897438149,
3.92558194113908));
#86737=CARTESIAN_POINT('Ctrl Pts',(20.6852674942244,-0.152084539141536,
3.93175946280133));
#86738=CARTESIAN_POINT('Ctrl Pts',(20.6794032810531,-0.0364470368946023,
3.9328311193721));
#86739=CARTESIAN_POINT('Ctrl Pts',(20.6735304324788,0.0793607484578857,
3.93390435402096));
#86740=CARTESIAN_POINT('Ctrl Pts',(20.6676575839045,0.195065966862631,3.92985673216703));
#86741=CARTESIAN_POINT('Ctrl Pts',(20.6617847353302,0.310186414876173,3.9207490850635));
#86742=CARTESIAN_POINT('Ctrl Pts',(20.6601899907173,0.34144683509439,3.91827594601159));
#86743=CARTESIAN_POINT('Ctrl Pts',(20.6585952461043,0.372664192628336,3.91542998810426));
#86744=CARTESIAN_POINT('Ctrl Pts',(20.6570005014914,0.403828975562439,3.912213076827));
#86745=CARTESIAN_POINT('Ctrl Pts',(20.6511280553575,0.518589362630107,3.90036720630957));
#86746=CARTESIAN_POINT('Ctrl Pts',(20.6452556092236,0.633020214199333,3.88344767112789));
#86747=CARTESIAN_POINT('Ctrl Pts',(20.6393831630896,0.746637091306685,3.86147925721285));
#86748=CARTESIAN_POINT('Ctrl Pts',(20.6335183241448,0.860106788678741,3.83953930126486));
#86749=CARTESIAN_POINT('Ctrl Pts',(20.6276534852,0.972764206367716,3.81256355073526));
#86750=CARTESIAN_POINT('Ctrl Pts',(20.6217886462551,1.08412932010921,3.78062860081224));
#86751=CARTESIAN_POINT('Ctrl Pts',(20.6159298361351,1.19537995487396,3.74872647876743));
#86752=CARTESIAN_POINT('Ctrl Pts',(20.6100710260151,1.30534053306963,3.71187541051525));
#86753=CARTESIAN_POINT('Ctrl Pts',(20.6042122158951,1.41354119508099,3.67020303114269));
#86754=CARTESIAN_POINT('Ctrl Pts',(20.5981264270141,1.52593370692096,3.62691620364123));
#86755=CARTESIAN_POINT('Ctrl Pts',(20.5920406381331,1.63642673515667,3.57842702676651));
#86756=CARTESIAN_POINT('Ctrl Pts',(20.5859548492521,1.7445106101207,3.52493570596349));
#86757=CARTESIAN_POINT('Ctrl Pts',(20.5801028191739,1.84844291859143,3.47349901889008));
#86758=CARTESIAN_POINT('Ctrl Pts',(20.5742507890956,1.95014732918308,3.41743757051405));
#86759=CARTESIAN_POINT('Ctrl Pts',(20.5683987590174,2.04919179690856,3.35697810232397));
#86760=CARTESIAN_POINT('Ctrl Pts',(20.5625476186388,2.14822120663928,3.2965278259482));
#86761=CARTESIAN_POINT('Ctrl Pts',(20.5566964782603,2.24459112485832,3.23168107454867));
#86762=CARTESIAN_POINT('Ctrl Pts',(20.5508453378818,2.33789601955901,3.16270947159712));
#86763=CARTESIAN_POINT('Ctrl Pts',(20.5449936703143,2.43120932105043,3.09373165428957));
#86764=CARTESIAN_POINT('Ctrl Pts',(20.5391420027468,2.52145671762473,3.020628492351));
#86765=CARTESIAN_POINT('Ctrl Pts',(20.5332903351793,2.60826404619016,2.94371324441626));
#86766=CARTESIAN_POINT('Ctrl Pts',(20.5274367234951,2.69510021501009,2.86677244270213));
#86767=CARTESIAN_POINT('Ctrl Pts',(20.5215831118108,2.7784937340069,2.78601731061528));
#86768=CARTESIAN_POINT('Ctrl Pts',(20.5157295001266,2.85810625899502,2.70179895852624));
#86769=CARTESIAN_POINT('Ctrl Pts',(20.5098692340267,2.93780928790779,2.61748486658481));
#86770=CARTESIAN_POINT('Ctrl Pts',(20.5040089679268,3.01372245951614,2.52969999707192));
#86771=CARTESIAN_POINT('Ctrl Pts',(20.4981487018269,3.08554674102027,2.43882970069236));
#86772=CARTESIAN_POINT('Ctrl Pts',(20.4922844886556,3.15741939841086,2.34789820034322));
#86773=CARTESIAN_POINT('Ctrl Pts',(20.4864202754844,3.22519744080989,2.25387746964359));
#86774=CARTESIAN_POINT('Ctrl Pts',(20.4805560623131,3.28862530937061,2.15718162762597));
#86775=CARTESIAN_POINT('Ctrl Pts',(20.4746832137388,3.35214657924372,2.06034339522458));
#86776=CARTESIAN_POINT('Ctrl Pts',(20.4688103651645,3.4113046799798,1.96082254350937));
#86777=CARTESIAN_POINT('Ctrl Pts',(20.4629375165902,3.46589005103204,1.85905759839686));
#86778=CARTESIAN_POINT('Ctrl Pts',(20.4613427719774,3.48071245370826,1.83142380264347));
#86779=CARTESIAN_POINT('Ctrl Pts',(20.4597480273646,3.49519795340568,1.80362464463149));
#86780=CARTESIAN_POINT('Ctrl Pts',(20.4581532827518,3.50934297619718,1.77566913455619));
#86781=CARTESIAN_POINT('Ctrl Pts',(20.4522808366178,3.56143024066478,1.67272649048393));
#86782=CARTESIAN_POINT('Ctrl Pts',(20.4464083904839,3.60907130997126,1.56731767217624));
#86783=CARTESIAN_POINT('Ctrl Pts',(20.4405359443499,3.65202509315485,1.45986359601413));
#86784=CARTESIAN_POINT('Ctrl Pts',(20.4346711054051,3.69492323384417,1.35254871627138));
#86785=CARTESIAN_POINT('Ctrl Pts',(20.4288062664602,3.7331460112999,1.243194227746));
#86786=CARTESIAN_POINT('Ctrl Pts',(20.4229414275154,3.76649830404232,1.13224534693074));
#86787=CARTESIAN_POINT('Ctrl Pts',(20.4170826173953,3.79981631193363,1.02141051722102));
#86788=CARTESIAN_POINT('Ctrl Pts',(20.4112238072753,3.82827367536364,0.908984948709361));
#86789=CARTESIAN_POINT('Ctrl Pts',(20.4053649971552,3.85172370420032,0.795432905090898));
#86790=CARTESIAN_POINT('Ctrl Pts',(20.3992792082743,3.87608222100296,0.677481691396547));
#86791=CARTESIAN_POINT('Ctrl Pts',(20.3931934193933,3.89503740490437,0.558315376668335));
#86792=CARTESIAN_POINT('Ctrl Pts',(20.3871076305123,3.90848208690171,0.438470952707787));
#86793=CARTESIAN_POINT('Ctrl Pts',(20.3812556004341,3.92141035059607,0.323229824983995));
#86794=CARTESIAN_POINT('Ctrl Pts',(20.3754035703558,3.92924357666178,0.207362169025676));
#86795=CARTESIAN_POINT('Ctrl Pts',(20.3695515402775,3.93193889091192,0.0913540263717977));
#86796=CARTESIAN_POINT('Ctrl Pts',(20.363700399899,3.93463379538624,-0.0246364792546189));
#86797=CARTESIAN_POINT('Ctrl Pts',(20.3578492595204,3.93219233158833,-0.140767015976084));
#86798=CARTESIAN_POINT('Ctrl Pts',(20.3519981191419,3.92462371629558,-0.256549577061237));
#86799=CARTESIAN_POINT('Ctrl Pts',(20.3461464515744,3.91705441906898,-0.3723425701796));
#86800=CARTESIAN_POINT('Ctrl Pts',(20.3402947840069,3.90435707898377,-0.487787112834));
#86801=CARTESIAN_POINT('Ctrl Pts',(20.3344431164393,3.88659289818115,-0.602399073544966));
#86802=CARTESIAN_POINT('Ctrl Pts',(20.3285895047551,3.86882281553248,-0.717049112124836));
#86803=CARTESIAN_POINT('Ctrl Pts',(20.3227358930708,3.84598260816349,-0.830865610473498));
#86804=CARTESIAN_POINT('Ctrl Pts',(20.3168822813866,3.8181846870822,-0.94337410147354));
#86805=CARTESIAN_POINT('Ctrl Pts',(20.3110220152867,3.79035516518226,-1.05601049270072));
#86806=CARTESIAN_POINT('Ctrl Pts',(20.3051617491868,3.75755677960058,-1.167335507151));
#86807=CARTESIAN_POINT('Ctrl Pts',(20.2993014830869,3.71995200068839,-1.27688923269579));
#86808=CARTESIAN_POINT('Ctrl Pts',(20.2934372699155,3.68232189378844,-1.38651674608085));
#86809=CARTESIAN_POINT('Ctrl Pts',(20.2875730567442,3.63987909852825,-1.49437021131679));
#86810=CARTESIAN_POINT('Ctrl Pts',(20.2817088435729,3.59283379224433,-1.60001073162253));
#86811=CARTESIAN_POINT('Ctrl Pts',(20.2758359949986,3.54571920894637,-1.70580681388301));
#86812=CARTESIAN_POINT('Ctrl Pts',(20.2699631464243,3.49398877214061,-1.8093830791024));
#86813=CARTESIAN_POINT('Ctrl Pts',(20.26409029785,3.4378980622037,-1.91032612762743));
#86814=CARTESIAN_POINT('Ctrl Pts',(20.2624955532373,3.42266689178285,-1.93773674119633));
#86815=CARTESIAN_POINT('Ctrl Pts',(20.2609008086247,3.40711445026582,-1.9649533620427));
#86816=CARTESIAN_POINT('Ctrl Pts',(20.259306064012,3.39124638465022,-1.99196811184236));
#86817=CARTESIAN_POINT('Ctrl Pts',(20.2534336178781,3.33281423204201,-2.09144652472551));
#86818=CARTESIAN_POINT('Ctrl Pts',(20.2475611717442,3.26990340843406,-2.18851824426593));
#86819=CARTESIAN_POINT('Ctrl Pts',(20.2416887256103,3.20273763208658,-2.28275286880039));
#86820=CARTESIAN_POINT('Ctrl Pts',(20.2358238866655,3.13565886254135,-2.37686542144368));
#86821=CARTESIAN_POINT('Ctrl Pts',(20.2299590477206,3.06433633913443,-2.46814785421082));
#86822=CARTESIAN_POINT('Ctrl Pts',(20.2240942087758,2.98903907776629,-2.55619529605742));
#86823=CARTESIAN_POINT('Ctrl Pts',(20.2182353986558,2.91381921903475,-2.64415222858108));
#86824=CARTESIAN_POINT('Ctrl Pts',(20.2123765885357,2.83463301641362,-2.72888047241358));
#86825=CARTESIAN_POINT('Ctrl Pts',(20.2065177784157,2.75179169580537,-2.8100055983746));
#86826=CARTESIAN_POINT('Ctrl Pts',(20.2004319895347,2.6657409828596,-2.89427362881527));
#86827=CARTESIAN_POINT('Ctrl Pts',(20.1943462006538,2.57574647866703,-2.97465334502407));
#86828=CARTESIAN_POINT('Ctrl Pts',(20.1882604117728,2.48220195814077,-3.05076423851502));
#86829=CARTESIAN_POINT('Ctrl Pts',(20.1824083816945,2.39225053877939,-3.12395166691658));
#86830=CARTESIAN_POINT('Ctrl Pts',(20.1765563516163,2.29901713926724,-3.19319187447863));
#86831=CARTESIAN_POINT('Ctrl Pts',(20.170704321538,2.20288743956765,-3.25818598741617));
#86832=CARTESIAN_POINT('Ctrl Pts',(20.1648531811595,2.10677235472292,-3.32317021912522));
#86833=CARTESIAN_POINT('Ctrl Pts',(20.159002040781,2.00776218755567,-3.38390940830432));
#86834=CARTESIAN_POINT('Ctrl Pts',(20.1531509004025,1.90627243728438,-3.44014743795231));
#86835=CARTESIAN_POINT('Ctrl Pts',(20.147299232835,1.80477354276511,-3.49639053465868));
#86836=CARTESIAN_POINT('Ctrl Pts',(20.1414475652675,1.70079498260152,-3.54813146526662));
#86837=CARTESIAN_POINT('Ctrl Pts',(20.1355958977,1.59477710513419,-3.5951599387148));
#86838=CARTESIAN_POINT('Ctrl Pts',(20.1297422860157,1.48872400503487,-3.64220403657137));
#86839=CARTESIAN_POINT('Ctrl Pts',(20.1238886743314,1.38063061805801,-3.68453239657957));
#86840=CARTESIAN_POINT('Ctrl Pts',(20.1180350626471,1.27095685195525,-3.72198303065288));
#86841=CARTESIAN_POINT('Ctrl Pts',(20.1121747965473,1.16115840815582,-3.75947623879801));
#86842=CARTESIAN_POINT('Ctrl Pts',(20.1063145304474,1.04977639072099,-3.79208051967024));
#86843=CARTESIAN_POINT('Ctrl Pts',(20.1004542643475,0.937285531215521,-3.81968386558024));
#86844=CARTESIAN_POINT('Ctrl Pts',(20.0945900511762,0.824718905618889,-3.84730580320189));
#86845=CARTESIAN_POINT('Ctrl Pts',(20.0887258380049,0.711042355264937,-3.86992001847493));
#86846=CARTESIAN_POINT('Ctrl Pts',(20.0828616248336,0.596738729076179,-3.88746599846488));
#86847=CARTESIAN_POINT('Ctrl Pts',(20.0769887762593,0.482266783993507,-3.90503781595486));
#86848=CARTESIAN_POINT('Ctrl Pts',(20.071115927685,0.367166329539215,-3.91752645852448));
#86849=CARTESIAN_POINT('Ctrl Pts',(20.0652430791107,0.251923316113332,-3.92492339323947));
#86850=CARTESIAN_POINT('Ctrl Pts',(20.063648334498,0.220629613833267,-3.9269319963285));
#86851=CARTESIAN_POINT('Ctrl Pts',(20.0620535898852,0.189325385389403,-3.92856544945613));
#86852=CARTESIAN_POINT('Ctrl Pts',(20.0604588452725,0.158020311487698,-3.92982424303649));
#86853=CARTESIAN_POINT('Ctrl Pts',(20.0545863991385,0.0427433205923004,
-3.934459591816));
#86854=CARTESIAN_POINT('Ctrl Pts',(20.0487139530046,-0.072930801677193,
-3.93402611889401));
#86855=CARTESIAN_POINT('Ctrl Pts',(20.0428415068707,-0.188519030851017,
-3.92847929547898));
#86856=CARTESIAN_POINT('Ctrl Pts',(20.0369766679259,-0.303957526592885,
-3.9229396574401));
#86857=CARTESIAN_POINT('Ctrl Pts',(20.031111828981,-0.41930994143253,-3.91229986102818));
#86858=CARTESIAN_POINT('Ctrl Pts',(20.0252469900362,-0.534090234586468,
-3.89656728689745));
#86859=CARTESIAN_POINT('Ctrl Pts',(20.0193881799161,-0.648752538092979,
-3.88085088523696));
#86860=CARTESIAN_POINT('Ctrl Pts',(20.0135293697961,-0.762843482644825,
-3.8600521747055));
#86861=CARTESIAN_POINT('Ctrl Pts',(20.0076705596761,-0.875879812045625,
-3.83423050361489));
#86862=CARTESIAN_POINT('Ctrl Pts',(20.0015847707951,-0.993295332009472,
-3.807408463714));
#86863=CARTESIAN_POINT('Ctrl Pts',(19.9954989819141,-1.10957241568892,-3.77516642014239));
#86864=CARTESIAN_POINT('Ctrl Pts',(19.9894131930332,-1.22417805782623,-3.73762987503268));
#86865=CARTESIAN_POINT('Ctrl Pts',(19.9835611629549,-1.33438162847987,-3.70153513114445));
#86866=CARTESIAN_POINT('Ctrl Pts',(19.9777091328766,-1.44303936204964,-3.66054525357306));
#86867=CARTESIAN_POINT('Ctrl Pts',(19.9718571027983,-1.54969130213815,-3.61482307562588));
#86868=CARTESIAN_POINT('Ctrl Pts',(19.9660059624198,-1.65632702764745,-3.5691078489435));
#86869=CARTESIAN_POINT('Ctrl Pts',(19.9601548220413,-1.76095718619479,-3.51866191524246));
#86870=CARTESIAN_POINT('Ctrl Pts',(19.9543036816628,-1.86314166519393,-3.46369631108421));
#86871=CARTESIAN_POINT('Ctrl Pts',(19.9484520140953,-1.96533535103594,-3.40872575451357));
#86872=CARTESIAN_POINT('Ctrl Pts',(19.9426003465278,-2.06508255522672,-3.34923491379087));
#86873=CARTESIAN_POINT('Ctrl Pts',(19.9367486789603,-2.16196827819438,-3.28548050733545));
#86874=CARTESIAN_POINT('Ctrl Pts',(19.9308950672761,-2.25888618979084,-3.221704919566));
#86875=CARTESIAN_POINT('Ctrl Pts',(19.9250414555919,-2.3529403846782,-3.15366317654784));
#86876=CARTESIAN_POINT('Ctrl Pts',(19.9191878439077,-2.44374592020367,-3.0816545681643));
#86877=CARTESIAN_POINT('Ctrl Pts',(19.9133275778078,-2.53465468392592,-3.00956410002681));
#86878=CARTESIAN_POINT('Ctrl Pts',(19.9074673117079,-2.62230709292485,-2.93349802259585));
#86879=CARTESIAN_POINT('Ctrl Pts',(19.901607045608,-2.7063522331158,-2.85379512059102));
#86880=CARTESIAN_POINT('Ctrl Pts',(19.8957428324367,-2.79045398032162,-2.77403853620375));
#86881=CARTESIAN_POINT('Ctrl Pts',(19.8898786192654,-2.87094333452931,-2.6906405464676));
#86882=CARTESIAN_POINT('Ctrl Pts',(19.8840144060941,-2.94750831036257,-2.60397460823711));
#86883=CARTESIAN_POINT('Ctrl Pts',(19.8781415575198,-3.02418603268067,-2.51718104925334));
#86884=CARTESIAN_POINT('Ctrl Pts',(19.8722687089455,-3.09692758439631,-2.42711025785644));
#86885=CARTESIAN_POINT('Ctrl Pts',(19.8663958603712,-3.16546302917209,-2.33416640600979));
#86886=CARTESIAN_POINT('Ctrl Pts',(19.8648011157584,-3.18407350924169,-2.30892793695128));
#86887=CARTESIAN_POINT('Ctrl Pts',(19.8632063711456,-3.20237410142416,-2.28347776576456));
#86888=CARTESIAN_POINT('Ctrl Pts',(19.8616116265327,-3.22035998380339,-2.25782430111775));
#86889=CARTESIAN_POINT('Ctrl Pts',(19.8556714388557,-3.28735473394137,-2.16226894175588));
#86890=CARTESIAN_POINT('Ctrl Pts',(19.8497312511786,-3.35020127333526,-2.06357478088844));
#86891=CARTESIAN_POINT('Ctrl Pts',(19.8437910635016,-3.408595750654,-1.96213251556145));
#86892=CARTESIAN_POINT('Ctrl Pts',(19.8378589838667,-3.4669105225975,-1.86082871356512));
#86893=CARTESIAN_POINT('Ctrl Pts',(19.8319269042319,-3.52078512172335,-1.75678461211711));
#86894=CARTESIAN_POINT('Ctrl Pts',(19.8259948245971,-3.56995767443358,-1.65042152274891));
#86895=CARTESIAN_POINT('Ctrl Pts',(19.8200695201429,-3.61907406590691,-1.54417991340013));
#86896=CARTESIAN_POINT('Ctrl Pts',(19.8141442156888,-3.66349892815091,-1.43562494691014));
#86897=CARTESIAN_POINT('Ctrl Pts',(19.8082189112347,-3.7030155051032,-1.32520382166869));
#86898=CARTESIAN_POINT('Ctrl Pts',(19.8022998744631,-3.74249028211675,-1.21489949794766));
#86899=CARTESIAN_POINT('Ctrl Pts',(19.7963808376916,-3.77706697789933,-1.10273332201382));
#86900=CARTESIAN_POINT('Ctrl Pts',(19.7904618009201,-3.80657661320366,-0.989173133385114));
#86901=CARTESIAN_POINT('Ctrl Pts',(19.7845464878454,-3.83606768384311,-0.875684386061103));
#86902=CARTESIAN_POINT('Ctrl Pts',(19.7786311747707,-3.86049793596701,-0.7608037578258));
#86903=CARTESIAN_POINT('Ctrl Pts',(19.772715861696,-3.87974806231536,-0.645014707553379));
#86904=CARTESIAN_POINT('Ctrl Pts',(19.7668024441909,-3.89899201993626,-0.529262762029275));
#86905=CARTESIAN_POINT('Ctrl Pts',(19.7608890266857,-3.91305908525392,-0.412603368035265));
#86906=CARTESIAN_POINT('Ctrl Pts',(19.7549756091806,-3.92188103807962,-0.295530240671769));
#86907=CARTESIAN_POINT('Ctrl Pts',(19.7499715801321,-3.92934631651909,-0.196461076415751));
#86908=CARTESIAN_POINT('Ctrl Pts',(19.7449675510835,-3.93305652182695,-0.0970959558208752));
#86909=CARTESIAN_POINT('Ctrl Pts',(19.739963522035,-3.93299934888168,0.00226311650535728));
#86910=CARTESIAN_POINT('',(18.4899641225863,-3.93462928533228,0.00227594938782067));
#86911=CARTESIAN_POINT('Ctrl Pts',(19.7399620606286,-3.9278079804333,0.00228910842207941));
#86912=CARTESIAN_POINT('Ctrl Pts',(19.7142295096835,-3.93046244247961,0.512557092329908));
#86913=CARTESIAN_POINT('Ctrl Pts',(19.6222145524918,-3.60059902134384,2.33387743482087));
#86914=CARTESIAN_POINT('Ctrl Pts',(19.4639171890534,-0.847591389378432,
4.57379261204712));
#86915=CARTESIAN_POINT('Ctrl Pts',(19.2650699703139,3.38921377376182,3.18609792961681));
#86916=CARTESIAN_POINT('Ctrl Pts',(19.0662227515741,4.51275657002401,-1.1282810647494));
#86917=CARTESIAN_POINT('Ctrl Pts',(18.8673755328346,1.49097359512779,-4.40624417843557));
#86918=CARTESIAN_POINT('Ctrl Pts',(18.6752897180372,-2.75106770730041,-3.66288770573472));
#86919=CARTESIAN_POINT('Ctrl Pts',(18.5494863094863,-3.92972806296831,-1.17034855638654));
#86920=CARTESIAN_POINT('Ctrl Pts',(18.489965307182,-3.93784438422833,0.00225448157776348));
#86921=CARTESIAN_POINT('',(17.2399634336168,-3.93317891120594,-0.00339957664883343));
#86922=CARTESIAN_POINT('Ctrl Pts',(18.489963522035,-3.93299933516336,0.00228683286660641));
#86923=CARTESIAN_POINT('Ctrl Pts',(18.4832027131417,-3.9329219864051,0.135314750767533));
#86924=CARTESIAN_POINT('Ctrl Pts',(18.4764419042485,-3.9260959776598,0.268144188695659));
#86925=CARTESIAN_POINT('Ctrl Pts',(18.4696810953553,-3.91257804618956,0.400277444375149));
#86926=CARTESIAN_POINT('Ctrl Pts',(18.4638086492214,-3.90083635586009,0.515048537410222));
#86927=CARTESIAN_POINT('Ctrl Pts',(18.4579362030875,-3.88402070381646,0.629494700770946));
#86928=CARTESIAN_POINT('Ctrl Pts',(18.4520637569536,-3.86215543622327,0.743131473193722));
#86929=CARTESIAN_POINT('Ctrl Pts',(18.4461989180087,-3.84031849298093,0.856621040109026));
#86930=CARTESIAN_POINT('Ctrl Pts',(18.4403340790639,-3.81344501987382,0.969302898987156));
#86931=CARTESIAN_POINT('Ctrl Pts',(18.4344692401191,-3.78161117631,1.08069695623115));
#86932=CARTESIAN_POINT('Ctrl Pts',(18.428610429999,-3.74981005669104,1.1919765047455));
#86933=CARTESIAN_POINT('Ctrl Pts',(18.422751619879,-3.7130588218373,1.30197048969573));
#86934=CARTESIAN_POINT('Ctrl Pts',(18.416892809759,-3.6714846802617,1.4102089357977));
#86935=CARTESIAN_POINT('Ctrl Pts',(18.410807020878,-3.62829989643136,1.52264069553817));
#86936=CARTESIAN_POINT('Ctrl Pts',(18.404721231997,-3.57991104108909,1.63317769496063));
#86937=CARTESIAN_POINT('Ctrl Pts',(18.3986354431161,-3.52651785693774,1.74131008286843));
#86938=CARTESIAN_POINT('Ctrl Pts',(18.3927834130378,-3.47517553702818,1.84528904087194));
#86939=CARTESIAN_POINT('Ctrl Pts',(18.3869313829595,-3.41920643531677,1.94704430010447));
#86940=CARTESIAN_POINT('Ctrl Pts',(18.3810793528812,-3.35883690100393,2.04614360992926));
#86941=CARTESIAN_POINT('Ctrl Pts',(18.3752282125027,-3.2984765448325,2.14522785342151));
#86942=CARTESIAN_POINT('Ctrl Pts',(18.3693770721242,-3.23371730125901,2.24165659745801));
#86943=CARTESIAN_POINT('Ctrl Pts',(18.3635259317456,-3.16483042551607,2.33502406362927));
#86944=CARTESIAN_POINT('Ctrl Pts',(18.3576742641781,-3.09593734305105,2.42839994222899));
#86945=CARTESIAN_POINT('Ctrl Pts',(18.3518225966106,-3.0229161345377,2.51871366201266));
#86946=CARTESIAN_POINT('Ctrl Pts',(18.3459709290431,-2.94607971883014,2.6055907756779));
#86947=CARTESIAN_POINT('Ctrl Pts',(18.3401173173588,-2.86921777553405,2.69249675278229));
#86948=CARTESIAN_POINT('Ctrl Pts',(18.3342637056745,-2.78853837832446,2.77596354399245));
#86949=CARTESIAN_POINT('Ctrl Pts',(18.3284100939903,-2.70439233029071,2.85565248653697));
#86950=CARTESIAN_POINT('Ctrl Pts',(18.3225498278904,-2.62015062459991,2.93543201987826));
#86951=CARTESIAN_POINT('Ctrl Pts',(18.3166895617905,-2.53243470247297,3.0114248481223));
#86952=CARTESIAN_POINT('Ctrl Pts',(18.3108292956905,-2.44162964300481,3.08333158878512));
#86953=CARTESIAN_POINT('Ctrl Pts',(18.3049650825192,-2.35076342350592,3.15528676087341));
#86954=CARTESIAN_POINT('Ctrl Pts',(18.2991008693479,-2.2568042579867,3.22315012394814));
#86955=CARTESIAN_POINT('Ctrl Pts',(18.2932366561766,-2.16016603332199,3.28666574334567));
#86956=CARTESIAN_POINT('Ctrl Pts',(18.2873638076022,-2.06338550311883,3.35027489327369));
#86957=CARTESIAN_POINT('Ctrl Pts',(18.2814909590279,-1.96391839398079,3.40952331104666));
#86958=CARTESIAN_POINT('Ctrl Pts',(18.2756181104536,-1.8622030414123,3.46420103812622));
#86959=CARTESIAN_POINT('Ctrl Pts',(18.2740233658409,-1.83458271228516,3.47904851964917));
#86960=CARTESIAN_POINT('Ctrl Pts',(18.2724286212283,-1.80679671513932,3.49355924844205));
#86961=CARTESIAN_POINT('Ctrl Pts',(18.2708338766156,-1.77885405692203,3.50772964240005));
#86962=CARTESIAN_POINT('Ctrl Pts',(18.2649614304817,-1.6759587381894,3.55991033299644));
#86963=CARTESIAN_POINT('Ctrl Pts',(18.2590889843477,-1.57059321014312,3.60764706896696));
#86964=CARTESIAN_POINT('Ctrl Pts',(18.2532165382138,-1.46317817013717,3.65069837735659));
#86965=CARTESIAN_POINT('Ctrl Pts',(18.247351699269,-1.35590227598285,3.69369391691749));
#86966=CARTESIAN_POINT('Ctrl Pts',(18.2414868603241,-1.24658252976148,3.73201594665387));
#86967=CARTESIAN_POINT('Ctrl Pts',(18.2356220213793,-1.13566397065819,3.76546894101503));
#86968=CARTESIAN_POINT('Ctrl Pts',(18.2297632112593,-1.02485943149117,3.79888754700769));
#86969=CARTESIAN_POINT('Ctrl Pts',(18.2239044011392,-0.912459741861291,
3.82744695455661));
#86970=CARTESIAN_POINT('Ctrl Pts',(18.2180455910192,-0.798929032112439,
3.85100005214852));
#86971=CARTESIAN_POINT('Ctrl Pts',(18.2119598021382,-0.680999978791925,
3.87546563073887));
#86972=CARTESIAN_POINT('Ctrl Pts',(18.2058740132573,-0.561850919989012,
3.89452898167878));
#86973=CARTESIAN_POINT('Ctrl Pts',(18.1997882243763,-0.442018749999848,
3.90808244854795));
#86974=CARTESIAN_POINT('Ctrl Pts',(18.193936194298,-0.326789405565467,3.9211153186219));
#86975=CARTESIAN_POINT('Ctrl Pts',(18.1880841642198,-0.21092890806477,3.92905372190601));
#86976=CARTESIAN_POINT('Ctrl Pts',(18.1822321341415,-0.0949232599168263,
3.93185434302019));
#86977=CARTESIAN_POINT('Ctrl Pts',(18.176380993763,0.0210647515827713,3.93465453834848));
#86978=CARTESIAN_POINT('Ctrl Pts',(18.1705298533845,0.137197456728115,3.93231849463597));
#86979=CARTESIAN_POINT('Ctrl Pts',(18.164678713006,0.252986840622257,3.9248549856615));
#86980=CARTESIAN_POINT('Ctrl Pts',(18.1588270454385,0.368786657164403,3.9173908042233));
#86981=CARTESIAN_POINT('Ctrl Pts',(18.152975377871,0.484242678437045,3.90479826572867));
#86982=CARTESIAN_POINT('Ctrl Pts',(18.1471237103035,0.598870717603099,3.88713813281668));
#86983=CARTESIAN_POINT('Ctrl Pts',(18.1412700986193,0.713536839979979,3.86947213262675));
#86984=CARTESIAN_POINT('Ctrl Pts',(18.135416486935,0.827374024943987,3.84673525314798));
#86985=CARTESIAN_POINT('Ctrl Pts',(18.1295628752508,0.939907703530585,3.81903947463807));
#86986=CARTESIAN_POINT('Ctrl Pts',(18.1237026091509,1.05256931097761,3.79131221142574));
#86987=CARTESIAN_POINT('Ctrl Pts',(18.117842343051,1.16392405274187,3.75861489615878));
#86988=CARTESIAN_POINT('Ctrl Pts',(18.1119820769512,1.27351186939958,3.72110958162997));
#86989=CARTESIAN_POINT('Ctrl Pts',(18.1061178637799,1.38317349685899,3.68357900610576));
#86990=CARTESIAN_POINT('Ctrl Pts',(18.1002536506086,1.49106544568376,3.64123413378783));
#86991=CARTESIAN_POINT('Ctrl Pts',(18.0943894374372,1.59674862848231,3.59428474351155));
#86992=CARTESIAN_POINT('Ctrl Pts',(18.088516588863,1.70258743605868,3.54726621746326));
#86993=CARTESIAN_POINT('Ctrl Pts',(18.0826437402887,1.80621061761258,3.49562982473978));
#86994=CARTESIAN_POINT('Ctrl Pts',(18.0767708917144,1.90720454165451,3.4396307703433));
#86995=CARTESIAN_POINT('Ctrl Pts',(18.0751761471016,1.93462897023533,3.42442448855497));
#86996=CARTESIAN_POINT('Ctrl Pts',(18.0735814024888,1.96185969781174,3.40889675970325));
#86997=CARTESIAN_POINT('Ctrl Pts',(18.071986657876,1.98888884093666,3.39305322363173));
#86998=CARTESIAN_POINT('Ctrl Pts',(18.0661142117421,2.08842025541688,3.33471139798524));
#86999=CARTESIAN_POINT('Ctrl Pts',(18.0602417656082,2.18554904312068,3.27188871847559));
#87000=CARTESIAN_POINT('Ctrl Pts',(18.0543693194743,2.27984459947886,3.2048085125678));
#87001=CARTESIAN_POINT('Ctrl Pts',(18.0485044805294,2.37401800501449,3.13781520261403));
#87002=CARTESIAN_POINT('Ctrl Pts',(18.0426396415846,2.4653651441655,3.06657557146715));
#87003=CARTESIAN_POINT('Ctrl Pts',(18.0367748026397,2.55348090185147,2.99135826738955));
#87004=CARTESIAN_POINT('Ctrl Pts',(18.0309159925197,2.64150607998831,2.91621828375575));
#87005=CARTESIAN_POINT('Ctrl Pts',(18.0250571823997,2.72630617126706,2.83710902698035));
#87006=CARTESIAN_POINT('Ctrl Pts',(18.0191983722797,2.80750646414212,2.75434138294443));
#87007=CARTESIAN_POINT('Ctrl Pts',(18.0131125833987,2.89185257357177,2.66836720090754));
#87008=CARTESIAN_POINT('Ctrl Pts',(18.0070267945177,2.97231395040191,2.57844569957846));
#87009=CARTESIAN_POINT('Ctrl Pts',(18.0009410056368,3.04850972884881,2.48497030829629));
#87010=CARTESIAN_POINT('Ctrl Pts',(17.9950889755585,3.12177878172414,2.39508536288336));
#87011=CARTESIAN_POINT('Ctrl Pts',(17.9892369454802,3.19110359464856,2.30191485552831));
#87012=CARTESIAN_POINT('Ctrl Pts',(17.983384915402,3.25618494385395,2.20584419472882));
#87013=CARTESIAN_POINT('Ctrl Pts',(17.9775337750235,3.32125639856811,2.10978813980833));
#87014=CARTESIAN_POINT('Ctrl Pts',(17.9716826346449,3.38208544055183,2.01083315026287));
#87015=CARTESIAN_POINT('Ctrl Pts',(17.9658314942664,3.43841557573441,1.90939449264603));
#87016=CARTESIAN_POINT('Ctrl Pts',(17.9599798266989,3.49475078627407,1.8079466953847));
#87017=CARTESIAN_POINT('Ctrl Pts',(17.9541281591314,3.5465860835206,1.70401514659803));
#87018=CARTESIAN_POINT('Ctrl Pts',(17.9482764915639,3.59371077676712,1.59804000355057));
#87019=CARTESIAN_POINT('Ctrl Pts',(17.9424228798797,3.64085112638916,1.49202965206942));
#87020=CARTESIAN_POINT('Ctrl Pts',(17.9365692681955,3.68327759220414,1.383974733776));
#87021=CARTESIAN_POINT('Ctrl Pts',(17.9307156565112,3.7208277687047,1.27433500918558));
#87022=CARTESIAN_POINT('Ctrl Pts',(17.9248553904113,3.75842063243765,1.16457064559638));
#87023=CARTESIAN_POINT('Ctrl Pts',(17.9189951243115,3.79112600842261,1.05321827103378));
#87024=CARTESIAN_POINT('Ctrl Pts',(17.9131348582116,3.81883145807233,0.940752515190457));
#87025=CARTESIAN_POINT('Ctrl Pts',(17.9072706450403,3.84655556820376,0.828211010163995));
#87026=CARTESIAN_POINT('Ctrl Pts',(17.901406431869,3.86927296559918,0.714555035009219));
#87027=CARTESIAN_POINT('Ctrl Pts',(17.8955422186977,3.88692269903637,0.600267383518262));
#87028=CARTESIAN_POINT('Ctrl Pts',(17.8896693701234,3.90459842275671,0.485811436657047));
#87029=CARTESIAN_POINT('Ctrl Pts',(17.8837965215491,3.917191544189,0.370722366361768));
#87030=CARTESIAN_POINT('Ctrl Pts',(17.8779236729748,3.92469308927438,0.255486115086346));
#87031=CARTESIAN_POINT('Ctrl Pts',(17.876328928362,3.92673009882118,0.224194249035622));
#87032=CARTESIAN_POINT('Ctrl Pts',(17.8747341837492,3.92839196811639,0.192891516277938));
#87033=CARTESIAN_POINT('Ctrl Pts',(17.8731394391363,3.92967917878615,0.161587597960445));
#87034=CARTESIAN_POINT('Ctrl Pts',(17.8672669930024,3.93441916991728,0.0463148623622432));
#87035=CARTESIAN_POINT('Ctrl Pts',(17.8613945468685,3.93409070193677,-0.0693596057384894));
#87036=CARTESIAN_POINT('Ctrl Pts',(17.8555221007346,3.92864880759938,-0.184952822492626));
#87037=CARTESIAN_POINT('Ctrl Pts',(17.8496572617897,3.92321396271262,-0.300396299353858));
#87038=CARTESIAN_POINT('Ctrl Pts',(17.8437924228449,3.91267888341305,-0.415758325086691));
#87039=CARTESIAN_POINT('Ctrl Pts',(17.8379275839,3.89705050914172,-0.530552852408001));
#87040=CARTESIAN_POINT('Ctrl Pts',(17.83206877378,3.88143820022727,-0.645229375449533));
#87041=CARTESIAN_POINT('Ctrl Pts',(17.82620996366,3.86074306587699,-0.759339153307035));
#87042=CARTESIAN_POINT('Ctrl Pts',(17.82035115354,3.83502401569583,-0.872398876109003));
#87043=CARTESIAN_POINT('Ctrl Pts',(17.814265364659,3.8083085723865,-0.989838695768315));
#87044=CARTESIAN_POINT('Ctrl Pts',(17.808179575778,3.77617209420852,-1.10614499969457));
#87045=CARTESIAN_POINT('Ctrl Pts',(17.802093786897,3.7387395994,-1.22078466892337));
#87046=CARTESIAN_POINT('Ctrl Pts',(17.7962417568188,3.70274490917848,-1.33102095966742));
#87047=CARTESIAN_POINT('Ctrl Pts',(17.7903897267405,3.66185368403598,-1.43971585758892));
#87048=CARTESIAN_POINT('Ctrl Pts',(17.7845376966622,3.61622833968109,-1.54640925866582));
#87049=CARTESIAN_POINT('Ctrl Pts',(17.7786865562837,3.57060993186908,-1.65308643886017));
#87050=CARTESIAN_POINT('Ctrl Pts',(17.7728354159052,3.52025899840678,-1.75776234728274));
#87051=CARTESIAN_POINT('Ctrl Pts',(17.7669842755267,3.46538617625046,-1.8599966799573));
#87052=CARTESIAN_POINT('Ctrl Pts',(17.7611326079592,3.41050841004128,-1.96224022396685));
#87053=CARTESIAN_POINT('Ctrl Pts',(17.7552809403917,3.35110814071534,-2.06204139068277));
#87054=CARTESIAN_POINT('Ctrl Pts',(17.7494292728242,3.2874417098647,-2.15898494766449));
#87055=CARTESIAN_POINT('Ctrl Pts',(17.74357566114,3.22375412692838,-2.25596071248945));
#87056=CARTESIAN_POINT('Ctrl Pts',(17.7377220494557,3.15579779092312,-2.35007663444583));
#87057=CARTESIAN_POINT('Ctrl Pts',(17.7318684377715,3.08387164217203,-2.44094749935496));
#87058=CARTESIAN_POINT('Ctrl Pts',(17.7260081716716,3.01186372740773,-2.53192166672735));
#87059=CARTESIAN_POINT('Ctrl Pts',(17.7201479055717,2.93587724898755,-2.61964308963168));
#87060=CARTESIAN_POINT('Ctrl Pts',(17.7142876394718,2.85625067294446,-2.70376054659142));
#87061=CARTESIAN_POINT('Ctrl Pts',(17.7084234263005,2.7765704659268,-2.78793465927364));
#87062=CARTESIAN_POINT('Ctrl Pts',(17.7025592131292,2.69324557586156,-2.86849968598149));
#87063=CARTESIAN_POINT('Ctrl Pts',(17.6966949999579,2.6066491762404,-2.94514330245665));
#87064=CARTESIAN_POINT('Ctrl Pts',(17.6908221513836,2.5199252582658,-3.02189978121959));
#87065=CARTESIAN_POINT('Ctrl Pts',(17.6849493028093,2.42992053611577,-3.09472306595429));
#87066=CARTESIAN_POINT('Ctrl Pts',(17.679076454235,2.33703893654878,-3.16334285354195));
#87067=CARTESIAN_POINT('Ctrl Pts',(17.6774817096222,2.31181737180677,-3.18197623650794));
#87068=CARTESIAN_POINT('Ctrl Pts',(17.6758869650094,2.28638382371883,-3.20029992388997));
#87069=CARTESIAN_POINT('Ctrl Pts',(17.6742922203967,2.26074669657243,-3.21830908614087));
#87070=CARTESIAN_POINT('Ctrl Pts',(17.6684197742627,2.16634120556882,-3.28462555737223));
#87071=CARTESIAN_POINT('Ctrl Pts',(17.6625473281288,2.06885720586434,-3.34689561649549));
#87072=CARTESIAN_POINT('Ctrl Pts',(17.6566748819949,1.96867667352833,-3.40482028235052));
#87073=CARTESIAN_POINT('Ctrl Pts',(17.6508100430501,1.86862591543521,-3.46266991237292));
#87074=CARTESIAN_POINT('Ctrl Pts',(17.6449452041052,1.76588592578803,-3.51618513828397));
#87075=CARTESIAN_POINT('Ctrl Pts',(17.6390803651604,1.66086932412086,-3.56510898686061));
#87076=CARTESIAN_POINT('Ctrl Pts',(17.6332215550404,1.55596067540873,-3.61398254363633));
#87077=CARTESIAN_POINT('Ctrl Pts',(17.6273627449204,1.44878044204021,-3.6582739374224));
#87078=CARTESIAN_POINT('Ctrl Pts',(17.6215039348003,1.33976704161409,-3.69777139290744));
#87079=CARTESIAN_POINT('Ctrl Pts',(17.6154181459194,1.22653030470003,-3.73879903683058));
#87080=CARTESIAN_POINT('Ctrl Pts',(17.6093323570384,1.11131588226435,-3.77465355433522));
#87081=CARTESIAN_POINT('Ctrl Pts',(17.6032465681574,0.994639837373666,-3.8051518489949));
#87082=CARTESIAN_POINT('Ctrl Pts',(17.5973945380792,0.882445389378838,-3.83447868585616));
#87083=CARTESIAN_POINT('Ctrl Pts',(17.5915425080009,0.768899968198137,-3.85885306701172));
#87084=CARTESIAN_POINT('Ctrl Pts',(17.5856904779226,0.654478437272971,-3.87816283504764));
#87085=CARTESIAN_POINT('Ctrl Pts',(17.5798393375441,0.540074302158601,-3.89746966736797));
#87086=CARTESIAN_POINT('Ctrl Pts',(17.5739881971656,0.424794729621852,-3.91171334878648));
#87087=CARTESIAN_POINT('Ctrl Pts',(17.5681370567871,0.309124000851478,-3.92083299212012));
#87088=CARTESIAN_POINT('Ctrl Pts',(17.5622853892196,0.193442850123971,-3.92995345713555));
#87089=CARTESIAN_POINT('Ctrl Pts',(17.5564337216521,0.0773708852054871,
-3.93394893380431));
#87090=CARTESIAN_POINT('Ctrl Pts',(17.5505820540846,-0.0386039901499777,
-3.93281053852642));
#87091=CARTESIAN_POINT('Ctrl Pts',(17.5447284424004,-0.154617396179694,
-3.93167176503613));
#87092=CARTESIAN_POINT('Ctrl Pts',(17.5388748307161,-0.27053323538834,-3.92539573209044));
#87093=CARTESIAN_POINT('Ctrl Pts',(17.5330212190319,-0.385865822081359,
-3.91402562170324));
#87094=CARTESIAN_POINT('Ctrl Pts',(17.527160952932,-0.50132951944777,-3.90264258571651));
#87095=CARTESIAN_POINT('Ctrl Pts',(17.5213006868321,-0.616208229278308,
-3.8861539542776));
#87096=CARTESIAN_POINT('Ctrl Pts',(17.5154404207322,-0.730023488886417,
-3.86465453898199));
#87097=CARTESIAN_POINT('Ctrl Pts',(17.5095762075609,-0.843915406610444,
-3.84314064316176));
#87098=CARTESIAN_POINT('Ctrl Pts',(17.5037119943896,-0.956742046483424,
-3.81660933773218));
#87099=CARTESIAN_POINT('Ctrl Pts',(17.4978477812183,-1.06803889982722,-3.78520566263656));
#87100=CARTESIAN_POINT('Ctrl Pts',(17.491974932644,-1.17949964441291,-3.75375574375994));
#87101=CARTESIAN_POINT('Ctrl Pts',(17.4861020840697,-1.2894257155315,-3.71741926488159));
#87102=CARTESIAN_POINT('Ctrl Pts',(17.4802292354954,-1.39737132445573,-3.67638985712735));
#87103=CARTESIAN_POINT('Ctrl Pts',(17.4786344908827,-1.426683450612,-3.66524851299863));
#87104=CARTESIAN_POINT('Ctrl Pts',(17.4770397462699,-1.45584967964805,-3.65376139101638));
#87105=CARTESIAN_POINT('Ctrl Pts',(17.4754450016571,-1.48486140462146,-3.64193294955654));
#87106=CARTESIAN_POINT('Ctrl Pts',(17.4695725555232,-1.591693426998,-3.59837620400363));
#87107=CARTESIAN_POINT('Ctrl Pts',(17.4637001093892,-1.69678615261499,-3.55004185303041));
#87108=CARTESIAN_POINT('Ctrl Pts',(17.4578276632553,-1.79968153748353,-3.49708955613678));
#87109=CARTESIAN_POINT('Ctrl Pts',(17.4519628243105,-1.90244363127891,-3.44420585385007));
#87110=CARTESIAN_POINT('Ctrl Pts',(17.4460979853656,-2.00301368073523,-3.38671628932404));
#87111=CARTESIAN_POINT('Ctrl Pts',(17.4402331464208,-2.10095241007959,-3.32482901373601));
#87112=CARTESIAN_POINT('Ctrl Pts',(17.4343743363008,-2.19879046224462,-3.26300535584431));
#87113=CARTESIAN_POINT('Ctrl Pts',(17.4285155261807,-2.29400222713966,-3.19679319824423));
#87114=CARTESIAN_POINT('Ctrl Pts',(17.4226567160607,-2.38617250060025,-3.12644683264871));
#87115=CARTESIAN_POINT('Ctrl Pts',(17.4165709271797,-2.48191358349775,-3.05337514730866));
#87116=CARTESIAN_POINT('Ctrl Pts',(17.4104851382988,-2.5743723411495,-2.9758426528553));
#87117=CARTESIAN_POINT('Ctrl Pts',(17.4043993494178,-2.66311571062527,-2.89418446402797));
#87118=CARTESIAN_POINT('Ctrl Pts',(17.3985473193395,-2.7484503940289,-2.81566281523259));
#87119=CARTESIAN_POINT('Ctrl Pts',(17.3926952892613,-2.83034951258053,-2.73332687224123));
#87120=CARTESIAN_POINT('Ctrl Pts',(17.386843259183,-2.90846195493877,-2.64751544975167));
#87121=CARTESIAN_POINT('Ctrl Pts',(17.3809921188045,-2.98656252165387,-2.56171707340174));
#87122=CARTESIAN_POINT('Ctrl Pts',(17.375140978426,-3.0608772786748,-2.4724445737531));
#87123=CARTESIAN_POINT('Ctrl Pts',(17.3692898380475,-3.13109315136304,-2.38007241013535));
#87124=CARTESIAN_POINT('Ctrl Pts',(17.36343817048,-3.20131535051627,-2.28769192376609));
#87125=CARTESIAN_POINT('Ctrl Pts',(17.3575865029125,-3.26743768102214,-2.19221154734077));
#87126=CARTESIAN_POINT('Ctrl Pts',(17.351734835345,-3.32918885536161,-2.09403690639302));
#87127=CARTESIAN_POINT('Ctrl Pts',(17.3458812236607,-3.39096054547549,-1.99582964859534));
#87128=CARTESIAN_POINT('Ctrl Pts',(17.3400276119765,-3.44835797176212,-1.8949266960883));
#87129=CARTESIAN_POINT('Ctrl Pts',(17.3341740002923,-3.50115484408842,-1.79175996096468));
#87130=CARTESIAN_POINT('Ctrl Pts',(17.3283137341924,-3.55401173616876,-1.68847594536982));
#87131=CARTESIAN_POINT('Ctrl Pts',(17.3224534680925,-3.60225744709231,-1.58292337876656));
#87132=CARTESIAN_POINT('Ctrl Pts',(17.3165932019926,-3.64571302354465,-1.4755560138324));
#87133=CARTESIAN_POINT('Ctrl Pts',(17.3107289888213,-3.68919786867878,-1.36811633363985));
#87134=CARTESIAN_POINT('Ctrl Pts',(17.30486477565,-3.72788601748201,-1.25885980992159));
#87135=CARTESIAN_POINT('Ctrl Pts',(17.2990005624787,-3.76164831424909,-1.14825561610079));
#87136=CARTESIAN_POINT('Ctrl Pts',(17.2931277139044,-3.79546032800798,-1.03748855102045));
#87137=CARTESIAN_POINT('Ctrl Pts',(17.2872548653301,-3.82433191027645,-0.925370253913503));
#87138=CARTESIAN_POINT('Ctrl Pts',(17.2813820167558,-3.84818490275428,-0.812380424563512));
#87139=CARTESIAN_POINT('Ctrl Pts',(17.279787272143,-3.85466207150327,-0.781698563899738));
#87140=CARTESIAN_POINT('Ctrl Pts',(17.2781925275302,-3.86076948077279,-0.750952467568144));
#87141=CARTESIAN_POINT('Ctrl Pts',(17.2765977829174,-3.86650622712652,-0.720151786494933));
#87142=CARTESIAN_POINT('Ctrl Pts',(17.2677944531138,-3.89817428842386,-0.550125469122141));
#87143=CARTESIAN_POINT('Ctrl Pts',(17.2589911233102,-3.9186344127923,-0.377951252578233));
#87144=CARTESIAN_POINT('Ctrl Pts',(17.2501877935066,-3.927662822198,-0.204826158299304));
#87145=CARTESIAN_POINT('Ctrl Pts',(17.2467797030161,-3.93115804922311,-0.137803111264485));
#87146=CARTESIAN_POINT('Ctrl Pts',(17.2433716125255,-3.93294038466564,-0.0706378330955611));
#87147=CARTESIAN_POINT('Ctrl Pts',(17.239963522035,-3.9329985293756,-0.00340116588511312));
#87148=CARTESIAN_POINT('',(15.989963522035,-3.92659065282687,-0.000639758371446531));
#87149=CARTESIAN_POINT('Ctrl Pts',(17.2399625682156,-3.93494441549702,-0.00338402184785404));
#87150=CARTESIAN_POINT('Ctrl Pts',(17.185891900203,-3.92519397476945,1.06388872901601));
#87151=CARTESIAN_POINT('Ctrl Pts',(17.0655388259439,-2.92427844162612,3.45556040462417));
#87152=CARTESIAN_POINT('Ctrl Pts',(16.8789033454381,1.12418408352393,4.5137789232215));
#87153=CARTESIAN_POINT('Ctrl Pts',(16.6800561266984,4.40488891136011,1.49497280909776));
#87154=CARTESIAN_POINT('Ctrl Pts',(16.4812089079589,3.63935299032934,-2.89708471280141));
#87155=CARTESIAN_POINT('Ctrl Pts',(16.2823616892191,-0.46921805946625,-4.62793954520115));
#87156=CARTESIAN_POINT('Ctrl Pts',(16.1186132272446,-3.49764510045685,-2.5525207092964));
#87157=CARTESIAN_POINT('Ctrl Pts',(16.0211471715165,-3.92748632721169,-0.619480281848567));
#87158=CARTESIAN_POINT('Ctrl Pts',(15.989963522035,-3.92659065282687,-0.000639758371446531));
#87159=CARTESIAN_POINT('',(14.7399635092212,-3.9329983210553,0.00363408533045304));
#87160=CARTESIAN_POINT('Ctrl Pts',(15.989963522035,-3.92659065282687,-0.000639758371446531));
#87161=CARTESIAN_POINT('Ctrl Pts',(15.95486476527,-3.92558252652043,0.69589619463605));
#87162=CARTESIAN_POINT('Ctrl Pts',(15.8534836022582,-3.41615124407677,2.70918611068639));
#87163=CARTESIAN_POINT('Ctrl Pts',(15.6858200330004,-0.195332983705196,
4.64756226928094));
#87164=CARTESIAN_POINT('Ctrl Pts',(15.4869728142606,3.80395226557352,2.67730035345362));
#87165=CARTESIAN_POINT('Ctrl Pts',(15.2881255955209,4.30900486257963,-1.75227484020969));
#87166=CARTESIAN_POINT('Ctrl Pts',(15.0892783767814,0.855893834375464,-4.57224624945369));
#87167=CARTESIAN_POINT('Ctrl Pts',(14.9065576856193,-3.03961470054979,-3.30416404160057));
#87168=CARTESIAN_POINT('Ctrl Pts',(14.7901194007039,-3.92350144596277,-0.987888984853184));
#87169=CARTESIAN_POINT('Ctrl Pts',(14.739963522035,-3.93258919388794,0.00363345398641773));
#87170=CARTESIAN_POINT('',(13.4899631080426,-3.93529776951097,-0.00102838428343817));
#87171=CARTESIAN_POINT('Ctrl Pts',(14.7399635092212,-3.9329983210553,0.00363408533045304));
#87172=CARTESIAN_POINT('Ctrl Pts',(14.7323650281588,-3.93285951130317,0.15386130138135));
#87173=CARTESIAN_POINT('Ctrl Pts',(14.7247665470964,-3.92410999965482,0.30370417608665));
#87174=CARTESIAN_POINT('Ctrl Pts',(14.717168066034,-3.90690212688664,0.452332588842152));
#87175=CARTESIAN_POINT('Ctrl Pts',(14.7093791901893,-3.8892630772605,0.604685176739965));
#87176=CARTESIAN_POINT('Ctrl Pts',(14.7015903143445,-3.86273644131324,0.755762030018039));
#87177=CARTESIAN_POINT('Ctrl Pts',(14.6938014384998,-3.82753406574427,0.904694410045241));
#87178=CARTESIAN_POINT('Ctrl Pts',(14.6930622721006,-3.82419335089489,0.91882813271221));
#87179=CARTESIAN_POINT('Ctrl Pts',(14.6923231057013,-3.82077453694752,0.932942558131614));
#87180=CARTESIAN_POINT('Ctrl Pts',(14.6915839393021,-3.8172778270376,0.947036953453815));
#87181=CARTESIAN_POINT('Ctrl Pts',(14.6857114931682,-3.78949755914025,1.05901252134163));
#87182=CARTESIAN_POINT('Ctrl Pts',(14.6798390470342,-3.75673958706406,1.16995217037249));
#87183=CARTESIAN_POINT('Ctrl Pts',(14.6739666009003,-3.71909620862784,1.27937968991619));
#87184=CARTESIAN_POINT('Ctrl Pts',(14.6681017619555,-3.6815015935673,1.38866545663461));
#87185=CARTESIAN_POINT('Ctrl Pts',(14.6622369230106,-3.63903429065255,1.49644260198653));
#87186=CARTESIAN_POINT('Ctrl Pts',(14.6563720840658,-3.59183728025604,1.60224653289153));
#87187=CARTESIAN_POINT('Ctrl Pts',(14.6505132739458,-3.54468878653844,1.70794170149779));
#87188=CARTESIAN_POINT('Ctrl Pts',(14.6446544638257,-3.49282042341684,1.8116673149959));
#87189=CARTESIAN_POINT('Ctrl Pts',(14.6387956537057,-3.4364242878107,1.91297598368216));
#87190=CARTESIAN_POINT('Ctrl Pts',(14.6327098648247,-3.37784328450623,2.01820949642721));
#87191=CARTESIAN_POINT('Ctrl Pts',(14.6266240759438,-3.31437673623003,2.12083457529475));
#87192=CARTESIAN_POINT('Ctrl Pts',(14.6205382870628,-3.24629416493512,2.22037456180442));
#87193=CARTESIAN_POINT('Ctrl Pts',(14.6146862569845,-3.18082668605661,2.31609115770327));
#87194=CARTESIAN_POINT('Ctrl Pts',(14.6088342269062,-3.11109150630972,2.40895491723037));
#87195=CARTESIAN_POINT('Ctrl Pts',(14.602982196828,-3.03737356597209,2.49856975502667));
#87196=CARTESIAN_POINT('Ctrl Pts',(14.5971310564494,-2.96366683316973,2.58817096843992));
#87197=CARTESIAN_POINT('Ctrl Pts',(14.5912799160709,-2.8859788062546,2.67452392310072));
#87198=CARTESIAN_POINT('Ctrl Pts',(14.5854287756924,-2.80463515812238,2.75726506339595));
#87199=CARTESIAN_POINT('Ctrl Pts',(14.5795771081249,-2.72328418091027,2.8400136586854));
#87200=CARTESIAN_POINT('Ctrl Pts',(14.5737254405574,-2.63827721752455,2.91914949791004));
#87201=CARTESIAN_POINT('Ctrl Pts',(14.5678737729899,-2.54997677940284,2.9943459092941));
#87202=CARTESIAN_POINT('Ctrl Pts',(14.5620201613056,-2.46164700496657,3.06956730340333));
#87203=CARTESIAN_POINT('Ctrl Pts',(14.5561665496214,-2.37002189458091,3.14084639932784));
#87204=CARTESIAN_POINT('Ctrl Pts',(14.5503129379371,-2.27549642959328,3.20789728621542));
#87205=CARTESIAN_POINT('Ctrl Pts',(14.5444526718372,-2.18086350757442,3.27502439689356));
#87206=CARTESIAN_POINT('Ctrl Pts',(14.5385924057373,-2.08332398732458,3.33791346532767));
#87207=CARTESIAN_POINT('Ctrl Pts',(14.5327321396374,-1.98330125572515,3.39632229463563));
#87208=CARTESIAN_POINT('Ctrl Pts',(14.5268679264661,-1.88321115570634,3.45477046410603));
#87209=CARTESIAN_POINT('Ctrl Pts',(14.5210037132948,-1.78063487894454,3.50873219386432));
#87210=CARTESIAN_POINT('Ctrl Pts',(14.5151395001235,-1.67601821744151,3.55801235731471));
#87211=CARTESIAN_POINT('Ctrl Pts',(14.5092666515492,-1.57124750167656,3.60736508873945));
#87212=CARTESIAN_POINT('Ctrl Pts',(14.5033938029749,-1.46443078454555,3.6520223361943));
#87213=CARTESIAN_POINT('Ctrl Pts',(14.4975209544006,-1.35603159153177,3.69183793289573));
#87214=CARTESIAN_POINT('Ctrl Pts',(14.4959262097878,-1.32659629673441,3.70264967229946));
#87215=CARTESIAN_POINT('Ctrl Pts',(14.4943314651751,-1.29704438562647,3.71310469202366));
#87216=CARTESIAN_POINT('Ctrl Pts',(14.4927367205623,-1.26738527970299,3.72320071347116));
#87217=CARTESIAN_POINT('Ctrl Pts',(14.4868642744284,-1.15816935853068,3.76037804057635));
#87218=CARTESIAN_POINT('Ctrl Pts',(14.4809918282945,-1.04713336591795,3.79280794662146));
#87219=CARTESIAN_POINT('Ctrl Pts',(14.4751193821606,-0.934727800867599,
3.82031058139063));
#87220=CARTESIAN_POINT('Ctrl Pts',(14.4692545432157,-0.822467846414021,
3.84777758914205));
#87221=CARTESIAN_POINT('Ctrl Pts',(14.4633897042709,-0.70884224548679,3.87032992141478));
#87222=CARTESIAN_POINT('Ctrl Pts',(14.457524865326,-0.594319128877981,3.88783664433702));
#87223=CARTESIAN_POINT('Ctrl Pts',(14.451666055206,-0.479913737549473,3.90532537103348));
#87224=CARTESIAN_POINT('Ctrl Pts',(14.445807245086,-0.364613071820371,3.91777874290011));
#87225=CARTESIAN_POINT('Ctrl Pts',(14.439948434966,-0.248897348668801,3.92511644538422));
#87226=CARTESIAN_POINT('Ctrl Pts',(14.433862646085,-0.12869863137231,3.93273842105418));
#87227=CARTESIAN_POINT('Ctrl Pts',(14.4277768572041,-0.00805248771519723,
3.93484022583765));
#87228=CARTESIAN_POINT('Ctrl Pts',(14.4216910683231,0.11249437966016,3.93139084988314));
#87229=CARTESIAN_POINT('Ctrl Pts',(14.4158390382448,0.228410969525238,3.92807396652885));
#87230=CARTESIAN_POINT('Ctrl Pts',(14.4099870081666,0.344235317561232,3.91962449732425));
#87231=CARTESIAN_POINT('Ctrl Pts',(14.4041349780883,0.459480163107657,3.90606796916164));
#87232=CARTESIAN_POINT('Ctrl Pts',(14.3982838377098,0.574707487672586,3.8925135020342));
#87233=CARTESIAN_POINT('Ctrl Pts',(14.3924326973313,0.68935507451161,3.87385356804228));
#87234=CARTESIAN_POINT('Ctrl Pts',(14.3865815569528,0.802941002732841,3.85016554788627));
#87235=CARTESIAN_POINT('Ctrl Pts',(14.3807298893853,0.916537165070234,3.82647539343463));
#87236=CARTESIAN_POINT('Ctrl Pts',(14.3748782218178,1.02907107395979,3.79775633662782));
#87237=CARTESIAN_POINT('Ctrl Pts',(14.3690265542503,1.14007191654556,3.76413669054461));
#87238=CARTESIAN_POINT('Ctrl Pts',(14.3631729425661,1.25110963726782,3.73050587490748));
#87239=CARTESIAN_POINT('Ctrl Pts',(14.3573193308819,1.36061288350438,3.6919713523002));
#87240=CARTESIAN_POINT('Ctrl Pts',(14.3514657191977,1.46812757403888,3.64871078962785));
#87241=CARTESIAN_POINT('Ctrl Pts',(14.3456054530978,1.57576448782272,3.60540104812691));
#87242=CARTESIAN_POINT('Ctrl Pts',(14.3397451869979,1.68140795011717,3.55735469744872));
#87243=CARTESIAN_POINT('Ctrl Pts',(14.333884920898,1.78462529312407,3.50479693607801));
#87244=CARTESIAN_POINT('Ctrl Pts',(14.3280207077267,1.88791215622052,3.45220377542099));
#87245=CARTESIAN_POINT('Ctrl Pts',(14.3221564945554,1.98876928745983,3.39509335683575));
#87246=CARTESIAN_POINT('Ctrl Pts',(14.3162922813841,2.08679150031032,3.33373517757974));
#87247=CARTESIAN_POINT('Ctrl Pts',(14.3104194328098,2.18495805670444,3.27228664475215));
#87248=CARTESIAN_POINT('Ctrl Pts',(14.3045465842355,2.28028102401497,3.20657810107659));
#87249=CARTESIAN_POINT('Ctrl Pts',(14.2986737356612,2.37238681246571,3.13692043444503));
#87250=CARTESIAN_POINT('Ctrl Pts',(14.2970789910484,2.39739770932159,3.11800522026959));
#87251=CARTESIAN_POINT('Ctrl Pts',(14.2954842464356,2.42217158603637,3.09879902543088));
#87252=CARTESIAN_POINT('Ctrl Pts',(14.2938895018228,2.44670143153496,3.07930854331371));
#87253=CARTESIAN_POINT('Ctrl Pts',(14.2880170556889,2.53702949736151,3.00753729829005));
#87254=CARTESIAN_POINT('Ctrl Pts',(14.2821446095549,2.62434812153707,2.93166801376936));
#87255=CARTESIAN_POINT('Ctrl Pts',(14.276272163421,2.70826242303331,2.85198240667535));
#87256=CARTESIAN_POINT('Ctrl Pts',(14.2704073244762,2.79206802162401,2.77240002462006));
#87257=CARTESIAN_POINT('Ctrl Pts',(14.2645424855313,2.87247777042338,2.68901143322388));
#87258=CARTESIAN_POINT('Ctrl Pts',(14.2586776465865,2.94912840357876,2.60213963099696));
#87259=CARTESIAN_POINT('Ctrl Pts',(14.2528188364665,3.02570024288419,2.51535712958161));
#87260=CARTESIAN_POINT('Ctrl Pts',(14.2469600263465,3.09852038085622,2.42509884744537));
#87261=CARTESIAN_POINT('Ctrl Pts',(14.2411012162264,3.16726159794009,2.33172532048995));
#87262=CARTESIAN_POINT('Ctrl Pts',(14.2350154273455,3.23866594899831,2.23473436832026));
#87263=CARTESIAN_POINT('Ctrl Pts',(14.2289296384645,3.30566861111373,2.13438222418711));
#87264=CARTESIAN_POINT('Ctrl Pts',(14.2228438495835,3.36794789080634,2.03111201188244));
#87265=CARTESIAN_POINT('Ctrl Pts',(14.2169918195052,3.42783498599518,1.93180847039984));
#87266=CARTESIAN_POINT('Ctrl Pts',(14.211139789427,3.4833546281127,1.82980728184328));
#87267=CARTESIAN_POINT('Ctrl Pts',(14.2052877593487,3.53426482377998,1.72553213687589));
#87268=CARTESIAN_POINT('Ctrl Pts',(14.1994366189702,3.58516727943433,1.6212728451371));
#87269=CARTESIAN_POINT('Ctrl Pts',(14.1935854785917,3.631461500727,1.51474065573167));
#87270=CARTESIAN_POINT('Ctrl Pts',(14.1877343382131,3.67295200143222,1.40638280534676));
#87271=CARTESIAN_POINT('Ctrl Pts',(14.1818826706456,3.71444624044032,1.29801519189666));
#87272=CARTESIAN_POINT('Ctrl Pts',(14.1760310030781,3.75113575064304,1.18782197652054));
#87273=CARTESIAN_POINT('Ctrl Pts',(14.1701793355106,3.78287389681412,1.07626859138524));
#87274=CARTESIAN_POINT('Ctrl Pts',(14.1643257238264,3.8146225874429,0.964678144540481));
#87275=CARTESIAN_POINT('Ctrl Pts',(14.1584721121422,3.84141652998987,0.85172702674279));
#87276=CARTESIAN_POINT('Ctrl Pts',(14.1526185004579,3.86315965307619,0.737893281473863));
#87277=CARTESIAN_POINT('Ctrl Pts',(14.146758234358,3.88492749385586,0.623930129422035));
#87278=CARTESIAN_POINT('Ctrl Pts',(14.1408979682581,3.9016329771412,0.509082753451748));
#87279=CARTESIAN_POINT('Ctrl Pts',(14.1350377021582,3.91323159399635,0.393836884698193));
#87280=CARTESIAN_POINT('Ctrl Pts',(14.1291734889869,3.92483802288055,0.278513394269038));
#87281=CARTESIAN_POINT('Ctrl Pts',(14.1233092758156,3.93133071323441,0.16279128832216));
#87282=CARTESIAN_POINT('Ctrl Pts',(14.1174450626443,3.93271728004675,0.0471571333064215));
#87283=CARTESIAN_POINT('Ctrl Pts',(14.11157221407,3.93410588866127,-0.0686472998861706));
#87284=CARTESIAN_POINT('Ctrl Pts',(14.1056993654957,3.93037338044257,-0.184363112078128));
#87285=CARTESIAN_POINT('Ctrl Pts',(14.0998265169215,3.92157927323944,-0.299507935953051));
#87286=CARTESIAN_POINT('Ctrl Pts',(14.0982317723086,3.91919127448394,-0.330774975319696));
#87287=CARTESIAN_POINT('Ctrl Pts',(14.0966370276958,3.91643034098348,-0.361999967454853));
#87288=CARTESIAN_POINT('Ctrl Pts',(14.095042283083,3.91329831231293,-0.393173395397972));
#87289=CARTESIAN_POINT('Ctrl Pts',(14.0891698369491,3.90176501130031,-0.507965616632582));
#87290=CARTESIAN_POINT('Ctrl Pts',(14.0832973908152,3.88515716701732,-0.622442120640527));
#87291=CARTESIAN_POINT('Ctrl Pts',(14.0774249446813,3.86349824603618,-0.736118402755522));
#87292=CARTESIAN_POINT('Ctrl Pts',(14.0715601057364,3.84186738210372,-0.849647428182004));
#87293=CARTESIAN_POINT('Ctrl Pts',(14.0656952667916,3.81519853019166,-0.962377890856129));
#87294=CARTESIAN_POINT('Ctrl Pts',(14.0598304278468,3.7835669779599,-1.07382955970274));
#87295=CARTESIAN_POINT('Ctrl Pts',(14.0539716177267,3.75196794172543,-1.18516666059724));
#87296=CARTESIAN_POINT('Ctrl Pts',(14.0481128076067,3.71541646443954,-1.29522718711191));
#87297=CARTESIAN_POINT('Ctrl Pts',(14.0422539974867,3.67403890115292,-1.40354093378676));
#87298=CARTESIAN_POINT('Ctrl Pts',(14.0361682086057,3.63105831133817,-1.51605091135319));
#87299=CARTESIAN_POINT('Ctrl Pts',(14.0300824197247,3.58287021860048,-1.62667557985427));
#87300=CARTESIAN_POINT('Ctrl Pts',(14.0239966308438,3.52967343966517,-1.73490472629544));
#87301=CARTESIAN_POINT('Ctrl Pts',(14.0181446007655,3.47851998092954,-1.8389767262788));
#87302=CARTESIAN_POINT('Ctrl Pts',(14.0122925706873,3.4227357108332,-1.94083343120115));
#87303=CARTESIAN_POINT('Ctrl Pts',(14.006440540609,3.362546193441,-2.04004218019516));
#87304=CARTESIAN_POINT('Ctrl Pts',(14.0005894002305,3.3023658268218,-2.13923584621824));
#87305=CARTESIAN_POINT('Ctrl Pts',(13.994738259852,3.23778175892049,-2.23578200345887));
#87306=CARTESIAN_POINT('Ctrl Pts',(13.9888871194734,3.16906450782115,-2.32927438170523));
#87307=CARTESIAN_POINT('Ctrl Pts',(13.983035451906,3.10034106528297,-2.42277518363463));
#87308=CARTESIAN_POINT('Ctrl Pts',(13.9771837843385,3.0274839440693,-2.51322132651705));
#87309=CARTESIAN_POINT('Ctrl Pts',(13.971332116771,2.95080538269953,-2.60023779555476));
#87310=CARTESIAN_POINT('Ctrl Pts',(13.9654785050867,2.87410134618564,-2.68728317433008));
#87311=CARTESIAN_POINT('Ctrl Pts',(13.9596248934025,2.79357361811643,-2.77089630356811));
#87312=CARTESIAN_POINT('Ctrl Pts',(13.9537712817183,2.70957238615181,-2.85073788416326));
#87313=CARTESIAN_POINT('Ctrl Pts',(13.9479110156184,2.62547566115773,-2.93067022907494));
#87314=CARTESIAN_POINT('Ctrl Pts',(13.9420507495185,2.53789785058966,-3.0068221826623));
#87315=CARTESIAN_POINT('Ctrl Pts',(13.9361904834186,2.44722348937104,-3.07889366381346));
#87316=CARTESIAN_POINT('Ctrl Pts',(13.9303262702473,2.35648805615109,-3.15101368734784));
#87317=CARTESIAN_POINT('Ctrl Pts',(13.924462057076,2.26265225322036,-3.21904752393788));
#87318=CARTESIAN_POINT('Ctrl Pts',(13.9185978439047,2.16612950211537,-3.2827384879191));
#87319=CARTESIAN_POINT('Ctrl Pts',(13.9127249953304,2.06946461551345,-3.34652324063628));
#87320=CARTESIAN_POINT('Ctrl Pts',(13.9068521467561,1.97010523737935,-3.40595214594057));
#87321=CARTESIAN_POINT('Ctrl Pts',(13.9009792981818,1.86848932130979,-3.46081444982988));
#87322=CARTESIAN_POINT('Ctrl Pts',(13.899384553569,1.84089599369804,-3.47571205232472));
#87323=CARTESIAN_POINT('Ctrl Pts',(13.8977898089563,1.81313638695708,-3.49027320341912));
#87324=CARTESIAN_POINT('Ctrl Pts',(13.8961950643435,1.78521950151592,-3.50449430466184));
#87325=CARTESIAN_POINT('Ctrl Pts',(13.8903226182096,1.68241908779071,-3.55686171844305));
#87326=CARTESIAN_POINT('Ctrl Pts',(13.8844501720757,1.57714040070536,-3.60478966965293));
#87327=CARTESIAN_POINT('Ctrl Pts',(13.8785777259417,1.46980369851994,-3.64803592194719));
#87328=CARTESIAN_POINT('Ctrl Pts',(13.8727128869969,1.36260604070707,-3.69122615288163));
#87329=CARTESIAN_POINT('Ctrl Pts',(13.8668480480521,1.25335604931443,-3.7297465923615));
#87330=CARTESIAN_POINT('Ctrl Pts',(13.8609832091072,1.14249840781187,-3.76340090717789));
#87331=CARTESIAN_POINT('Ctrl Pts',(13.8551243989872,1.0317547236246,-3.79702062667624));
#87332=CARTESIAN_POINT('Ctrl Pts',(13.8492655888672,0.919407069599642,-3.82578405177716));
#87333=CARTESIAN_POINT('Ctrl Pts',(13.8434067787472,0.8059193082311,-3.84954322856885));
#87334=CARTESIAN_POINT('Ctrl Pts',(13.8373209898662,0.688034867173198,-3.87422287016465));
#87335=CARTESIAN_POINT('Ctrl Pts',(13.8312352009852,0.568920614755863,-3.89350250796558));
#87336=CARTESIAN_POINT('Ctrl Pts',(13.8251494121042,0.449113248937317,-3.90727351098294));
#87337=CARTESIAN_POINT('Ctrl Pts',(13.819297382026,0.333907755930442,-3.92051556151109));
#87338=CARTESIAN_POINT('Ctrl Pts',(13.8134453519477,0.218061861757758,-3.92866429952059));
#87339=CARTESIAN_POINT('Ctrl Pts',(13.8075933218694,0.102061489397147,-3.93167552735243));
#87340=CARTESIAN_POINT('Ctrl Pts',(13.8017421814909,-0.0139212471172105,
-3.93468629737927));
#87341=CARTESIAN_POINT('Ctrl Pts',(13.7958910411124,-0.130058002017154,
-3.93256109952536));
#87342=CARTESIAN_POINT('Ctrl Pts',(13.7900399007339,-0.245860745280993,
-3.92530782155105));
#87343=CARTESIAN_POINT('Ctrl Pts',(13.7841882331664,-0.361673922396517,
-3.91805389005486));
#87344=CARTESIAN_POINT('Ctrl Pts',(13.7783365655989,-0.477152615477489,
-3.90567098578471));
#87345=CARTESIAN_POINT('Ctrl Pts',(13.7724848980314,-0.591812528168616,
-3.88821899222545));
#87346=CARTESIAN_POINT('Ctrl Pts',(13.7666312863472,-0.706510534659967,
-3.870761200539));
#87347=CARTESIAN_POINT('Ctrl Pts',(13.7607776746629,-0.820388811420534,
-3.848231032963));
#87348=CARTESIAN_POINT('Ctrl Pts',(13.7549240629787,-0.932972586964773,
-3.82073960797805));
#87349=CARTESIAN_POINT('Ctrl Pts',(13.7490637968788,-1.04568434831993,-3.7932169306008));
#87350=CARTESIAN_POINT('Ctrl Pts',(13.7432035307789,-1.15709826940755,-3.76072183671057));
#87351=CARTESIAN_POINT('Ctrl Pts',(13.737343264679,-1.26675399735092,-3.723415543583));
#87352=CARTESIAN_POINT('Ctrl Pts',(13.7314790515077,-1.3764835818362,-3.68608412350716));
#87353=CARTESIAN_POINT('Ctrl Pts',(13.7256148383364,-1.48445223108702,-3.64393520167339));
#87354=CARTESIAN_POINT('Ctrl Pts',(13.7197506251651,-1.59022047757638,-3.59717775939649));
#87355=CARTESIAN_POINT('Ctrl Pts',(13.7138777765908,-1.69614447410502,-3.55035146400239));
#87356=CARTESIAN_POINT('Ctrl Pts',(13.7080049280165,-1.79986123212222,-3.49890328701583));
#87357=CARTESIAN_POINT('Ctrl Pts',(13.7021320794423,-1.9009566574887,-3.44308768205943));
#87358=CARTESIAN_POINT('Ctrl Pts',(13.7005373348294,-1.92840864828039,-3.4279312151101));
#87359=CARTESIAN_POINT('Ctrl Pts',(13.6989425902166,-1.95566752198257,-3.41245294995782));
#87360=CARTESIAN_POINT('Ctrl Pts',(13.6973478456038,-1.98272538492187,-3.39665851212429));
#87361=CARTESIAN_POINT('Ctrl Pts',(13.6914753994699,-2.0823625565004,-3.33849748455399));
#87362=CARTESIAN_POINT('Ctrl Pts',(13.685602953336,-2.17960524037133,-3.27585124847258));
#87363=CARTESIAN_POINT('Ctrl Pts',(13.6797305072021,-2.27402242721818,-3.20894234920304));
#87364=CARTESIAN_POINT('Ctrl Pts',(13.6738656682572,-2.36831730568186,-3.14212012397626));
#87365=CARTESIAN_POINT('Ctrl Pts',(13.6680008293124,-2.45979363172764,-3.07104645339295));
#87366=CARTESIAN_POINT('Ctrl Pts',(13.6621359903676,-2.5480458032047,-2.99598924977559));
#87367=CARTESIAN_POINT('Ctrl Pts',(13.6562771802475,-2.63620725490464,-2.92100920202499));
#87368=CARTESIAN_POINT('Ctrl Pts',(13.6504183701275,-2.72115083138239,-2.84205403244364));
#87369=CARTESIAN_POINT('Ctrl Pts',(13.6445595600075,-2.80250125728835,-2.75943394610149));
#87370=CARTESIAN_POINT('Ctrl Pts',(13.6384737711265,-2.8870033161192,-2.67361303835645));
#87371=CARTESIAN_POINT('Ctrl Pts',(13.6323879822455,-2.96762781521578,-2.58383776498953));
#87372=CARTESIAN_POINT('Ctrl Pts',(13.6263021933646,-3.04399317514067,-2.49050086321949));
#87373=CARTESIAN_POINT('Ctrl Pts',(13.6204501632863,-3.11742529576768,-2.4007490878534));
#87374=CARTESIAN_POINT('Ctrl Pts',(13.614598133208,-3.18691914796908,-2.3077045950877));
#87375=CARTESIAN_POINT('Ctrl Pts',(13.6087461031298,-3.25217480875052,-2.21175224953622));
#87376=CARTESIAN_POINT('Ctrl Pts',(13.6028949627513,-3.31742054853965,-2.11581449187598));
#87377=CARTESIAN_POINT('Ctrl Pts',(13.5970438223727,-3.37842914568288,-2.01697010215551));
#87378=CARTESIAN_POINT('Ctrl Pts',(13.5911926819942,-3.43494335260479,-1.91563388057221));
#87379=CARTESIAN_POINT('Ctrl Pts',(13.5853410144267,-3.49146265146869,-1.81428852857393));
#87380=CARTESIAN_POINT('Ctrl Pts',(13.5794893468592,-3.54348655377244,-1.71045125943168));
#87381=CARTESIAN_POINT('Ctrl Pts',(13.5736376792917,-3.5908035700392,-1.60456184717003));
#87382=CARTESIAN_POINT('Ctrl Pts',(13.5677840676075,-3.63813630657747,-1.49863725495746));
#87383=CARTESIAN_POINT('Ctrl Pts',(13.5619304559233,-3.6807588790428,-1.39065954112105));
#87384=CARTESIAN_POINT('Ctrl Pts',(13.5560768442391,-3.7185080474881,-1.28108817056683));
#87385=CARTESIAN_POINT('Ctrl Pts',(13.5502165781392,-3.75630012938088,-1.17139223871892));
#87386=CARTESIAN_POINT('Ctrl Pts',(13.5443563120393,-3.78920761465667,-1.06009942515104));
#87387=CARTESIAN_POINT('Ctrl Pts',(13.5384960459394,-3.81711720321073,-0.947684154638398));
#87388=CARTESIAN_POINT('Ctrl Pts',(13.5326318327681,-3.84504558974039,-0.835193168946053));
#87389=CARTESIAN_POINT('Ctrl Pts',(13.5267676195968,-3.86796929513556,-0.721578625142255));
#87390=CARTESIAN_POINT('Ctrl Pts',(13.5209034064255,-3.88582649174952,-0.607323205564899));
#87391=CARTESIAN_POINT('Ctrl Pts',(13.5150305578512,-3.90370998414853,-0.492899538080586));
#87392=CARTESIAN_POINT('Ctrl Pts',(13.5091577092769,-3.91651203208837,-0.377833520606281));
#87393=CARTESIAN_POINT('Ctrl Pts',(13.5032848607027,-3.92422277928354,-0.262611078502395));
#87394=CARTESIAN_POINT('Ctrl Pts',(13.5016901160898,-3.9263165966866,-0.231322962267526));
#87395=CARTESIAN_POINT('Ctrl Pts',(13.500095371477,-3.92803529418511,-0.200023298266526));
#87396=CARTESIAN_POINT('Ctrl Pts',(13.4985006268642,-3.92937933582806,-0.168721768504988));
#87397=CARTESIAN_POINT('Ctrl Pts',(13.4956549252544,-3.93177767687659,-0.112866546977301));
#87398=CARTESIAN_POINT('Ctrl Pts',(13.4928092236447,-3.93298513356625,-0.056959824101717));
#87399=CARTESIAN_POINT('Ctrl Pts',(13.489963522035,-3.93299986357157,-0.00103592761850977));
#87400=CARTESIAN_POINT('',(12.239963913861,-3.93201440718328,-0.00312379772517306));
#87401=CARTESIAN_POINT('Ctrl Pts',(13.4899624084639,-3.93918085105486,-0.001015637292931));
#87402=CARTESIAN_POINT('Ctrl Pts',(13.4265260750175,-3.93478655511187,1.24759946057853));
#87403=CARTESIAN_POINT('Ctrl Pts',(13.2968073353243,-2.61735902960304,3.80880663961671));
#87404=CARTESIAN_POINT('Ctrl Pts',(13.1008061893849,1.74836256028053,4.31059373859052));
#87405=CARTESIAN_POINT('Ctrl Pts',(12.9019589706453,4.57146741630123,0.860044000654414));
#87406=CARTESIAN_POINT('Ctrl Pts',(12.7031117519055,3.19531592007835,-3.38052454395175));
#87407=CARTESIAN_POINT('Ctrl Pts',(12.504264533166,-1.11598734534858,-4.51581247024143));
#87408=CARTESIAN_POINT('Ctrl Pts',(12.3498822614166,-3.66733284149021,-2.17668070861014));
#87409=CARTESIAN_POINT('Ctrl Pts',(12.2617823959138,-3.93262971169265,-0.435322618273008));
#87410=CARTESIAN_POINT('Ctrl Pts',(12.2399649366575,-3.92944490519375,-0.00314202184111889));
#87411=CARTESIAN_POINT('',(10.9899630120657,-3.93123823607095,0.00233406685951829));
#87412=CARTESIAN_POINT('Ctrl Pts',(12.239963522035,-3.93299876499558,-0.00311681619685484));
#87413=CARTESIAN_POINT('Ctrl Pts',(12.2341198337128,-3.93309058247703,0.11274437622992));
#87414=CARTESIAN_POINT('Ctrl Pts',(12.2282761453906,-3.9280584152009,0.228670229510765));
#87415=CARTESIAN_POINT('Ctrl Pts',(12.2224324570685,-3.91791188187092,0.344173627540887));
#87416=CARTESIAN_POINT('Ctrl Pts',(12.216589862448,-3.90776724756089,0.459655408014585));
#87417=CARTESIAN_POINT('Ctrl Pts',(12.2107472678275,-3.89251018623907,0.574714478005286));
#87418=CARTESIAN_POINT('Ctrl Pts',(12.204904673207,-3.87220232072403,0.688867322043548));
#87419=CARTESIAN_POINT('Ctrl Pts',(12.1990617509642,-3.85189331644964,0.803026567178875));
#87420=CARTESIAN_POINT('Ctrl Pts',(12.1932188287215,-3.82653301736519,0.916279077516074));
#87421=CARTESIAN_POINT('Ctrl Pts',(12.1873759064787,-3.79623432426462,1.02815074540416));
#87422=CARTESIAN_POINT('Ctrl Pts',(12.181531235386,-3.76592656243685,1.14005589769482));
#87423=CARTESIAN_POINT('Ctrl Pts',(12.1756865642933,-3.73067757563759,1.25057898607222));
#87424=CARTESIAN_POINT('Ctrl Pts',(12.1698418932006,-3.69065015226566,1.35926099538736));
#87425=CARTESIAN_POINT('Ctrl Pts',(12.1639903674728,-3.65057578469843,1.46807046705312));
#87426=CARTESIAN_POINT('Ctrl Pts',(12.158138841745,-3.60571193471527,1.57503415949148));
#87427=CARTESIAN_POINT('Ctrl Pts',(12.1522873160171,-3.55626965542888,1.67971281410715));
#87428=CARTESIAN_POINT('Ctrl Pts',(12.1464320218302,-3.50679553466756,1.78445888314635));
#87429=CARTESIAN_POINT('Ctrl Pts',(12.1405767276432,-3.45273730610917,1.8869166182753));
#87430=CARTESIAN_POINT('Ctrl Pts',(12.1347214334563,-3.39435122124357,1.98667279309962));
#87431=CARTESIAN_POINT('Ctrl Pts',(12.1288565851549,-3.33586986749531,2.08659174060062));
#87432=CARTESIAN_POINT('Ctrl Pts',(12.1229917368535,-3.2730467801339,2.18379997792449));
#87433=CARTESIAN_POINT('Ctrl Pts',(12.1171268885522,-3.20618080333904,2.27791432154509));
#87434=CARTESIAN_POINT('Ctrl Pts',(12.113607957597,-3.16606096672959,2.3343832803438));
#87435=CARTESIAN_POINT('Ctrl Pts',(12.1100890266418,-3.12448644944354,2.38973906388321));
#87436=CARTESIAN_POINT('Ctrl Pts',(12.1065700956867,-3.08152830119491,2.44390513910315));
#87437=CARTESIAN_POINT('Ctrl Pts',(12.1006976495528,-3.00983908227655,2.53429831903999));
#87438=CARTESIAN_POINT('Ctrl Pts',(12.0948252034189,-2.93404909368788,2.62168577861705));
#87439=CARTESIAN_POINT('Ctrl Pts',(12.0889527572849,-2.85443969377792,2.70567238123632));
#87440=CARTESIAN_POINT('Ctrl Pts',(12.0830879183401,-2.77493342018747,2.78955018729103));
#87441=CARTESIAN_POINT('Ctrl Pts',(12.0772230793952,-2.69161785619536,2.87003560009203));
#87442=CARTESIAN_POINT('Ctrl Pts',(12.0713582404504,-2.60481567041912,2.94676506072999));
#87443=CARTESIAN_POINT('Ctrl Pts',(12.0654994303303,-2.5181027138914,3.0234156464865));
#87444=CARTESIAN_POINT('Ctrl Pts',(12.0596406202103,-2.42791057241676,3.09631768764274));
#87445=CARTESIAN_POINT('Ctrl Pts',(12.0537818100903,-2.33459948471038,3.16514363749736));
#87446=CARTESIAN_POINT('Ctrl Pts',(12.0476960212093,-2.23767339077667,3.23663600399595));
#87447=CARTESIAN_POINT('Ctrl Pts',(12.0416102323283,-2.13738211057119,3.30372973453318));
#87448=CARTESIAN_POINT('Ctrl Pts',(12.0355244434474,-2.03416847568164,3.36610273350993));
#87449=CARTESIAN_POINT('Ctrl Pts',(12.0296724133691,-1.93491933844161,3.42607994816902));
#87450=CARTESIAN_POINT('Ctrl Pts',(12.0238203832908,-1.83296859062397,3.48169216038219));
#87451=CARTESIAN_POINT('Ctrl Pts',(12.0179683532126,-1.7287397030445,3.53269699225926));
#87452=CARTESIAN_POINT('Ctrl Pts',(12.0121172128341,-1.62452666166115,3.58369406973552));
#87453=CARTESIAN_POINT('Ctrl Pts',(12.0062660724556,-1.51803654036001,3.63008497800266));
#87454=CARTESIAN_POINT('Ctrl Pts',(12.000414932077,-1.4097163981887,3.67167382493024));
#87455=CARTESIAN_POINT('Ctrl Pts',(11.9945632645096,-1.30138649634974,3.7132664190217));
#87456=CARTESIAN_POINT('Ctrl Pts',(11.9887115969421,-1.19122663177882,3.75005594350249));
#87457=CARTESIAN_POINT('Ctrl Pts',(11.9828599293746,-1.07970210334088,3.78189534070435));
#87458=CARTESIAN_POINT('Ctrl Pts',(11.9770063176903,-0.968140522780236,
3.81374531600296));
#87459=CARTESIAN_POINT('Ctrl Pts',(11.9711527060061,-0.855213774087097,
3.84064178042879));
#87460=CARTESIAN_POINT('Ctrl Pts',(11.9652990943218,-0.741399813336094,
3.86248822869212));
#87461=CARTESIAN_POINT('Ctrl Pts',(11.9594388282219,-0.627456468293577,
3.88435951210934));
#87462=CARTESIAN_POINT('Ctrl Pts',(11.953578562122,-0.512624304272825,3.90116924278434));
#87463=CARTESIAN_POINT('Ctrl Pts',(11.9477182960222,-0.39738901180531,3.91287247087052));
#87464=CARTESIAN_POINT('Ctrl Pts',(11.9418540828509,-0.282076104785633,
3.92458358144468));
#87465=CARTESIAN_POINT('Ctrl Pts',(11.9359898696795,-0.166359940346541,
3.93118131744411));
#87466=CARTESIAN_POINT('Ctrl Pts',(11.9301256565082,-0.0507270916490356,
3.93267285216719));
#87467=CARTESIAN_POINT('Ctrl Pts',(11.9242528079339,0.0650760333018407,
3.93416658326394));
#87468=CARTESIAN_POINT('Ctrl Pts',(11.9183799593596,0.180795186052275,3.93053911919053));
#87469=CARTESIAN_POINT('Ctrl Pts',(11.9125071107853,0.295947945456476,3.9218495398957));
#87470=CARTESIAN_POINT('Ctrl Pts',(11.9109123661726,0.327217139678331,3.91948992520577));
#87471=CARTESIAN_POINT('Ctrl Pts',(11.9093176215598,0.358444625222629,3.91675733775559));
#87472=CARTESIAN_POINT('Ctrl Pts',(11.907722876947,0.38962088346284,3.91365360848014));
#87473=CARTESIAN_POINT('Ctrl Pts',(11.9018504308131,0.504423526912368,3.90222451642464));
#87474=CARTESIAN_POINT('Ctrl Pts',(11.8959779846792,0.618915059751209,3.88572059659295));
#87475=CARTESIAN_POINT('Ctrl Pts',(11.8901055385453,0.732610956210603,3.86416487573191));
#87476=CARTESIAN_POINT('Ctrl Pts',(11.8842406996004,0.84615957057305,3.84263707823369));
#87477=CARTESIAN_POINT('Ctrl Pts',(11.8783758606556,0.958914195814496,3.8160705699254));
#87478=CARTESIAN_POINT('Ctrl Pts',(11.8725110217107,1.07039453271425,3.78454020249956));
#87479=CARTESIAN_POINT('Ctrl Pts',(11.8666522115907,1.18176027219244,3.75304224705694));
#87480=CARTESIAN_POINT('Ctrl Pts',(11.8607934014707,1.29185393346273,3.71659069377557));
#87481=CARTESIAN_POINT('Ctrl Pts',(11.8549345913506,1.4002051965583,3.67531147081865));
#87482=CARTESIAN_POINT('Ctrl Pts',(11.8488488024697,1.51275414398552,3.63243303117999));
#87483=CARTESIAN_POINT('Ctrl Pts',(11.8427630135887,1.62342251030598,3.58434537934897));
#87484=CARTESIAN_POINT('Ctrl Pts',(11.8366772247077,1.73169990225679,3.53124686881615));
#87485=CARTESIAN_POINT('Ctrl Pts',(11.8308251946295,1.83581829461074,3.48018790393473));
#87486=CARTESIAN_POINT('Ctrl Pts',(11.8249731645512,1.93772559649863,3.42449611863627));
#87487=CARTESIAN_POINT('Ctrl Pts',(11.8191211344729,2.03698894247253,3.36439668413887));
#87488=CARTESIAN_POINT('Ctrl Pts',(11.8132699940944,2.13623719717497,3.30430638671893));
#87489=CARTESIAN_POINT('Ctrl Pts',(11.8074188537159,2.23284194170572,3.23980998651906));
#87490=CARTESIAN_POINT('Ctrl Pts',(11.8015677133374,2.32639666045386,3.17117763271456));
#87491=CARTESIAN_POINT('Ctrl Pts',(11.7957160457699,2.41995980850207,3.10253909512038));
#87492=CARTESIAN_POINT('Ctrl Pts',(11.7898643782024,2.51047205116509,3.02976410764543));
#87493=CARTESIAN_POINT('Ctrl Pts',(11.7840127106349,2.59755809036092,2.95316456825565));
#87494=CARTESIAN_POINT('Ctrl Pts',(11.7781590989506,2.68467306240772,2.87653957997556));
#87495=CARTESIAN_POINT('Ctrl Pts',(11.7723054872664,2.76835925733957,2.79608778604424));
#87496=CARTESIAN_POINT('Ctrl Pts',(11.7664518755822,2.84827705830305,2.71215906597392));
#87497=CARTESIAN_POINT('Ctrl Pts',(11.7605916094823,2.92828571023082,2.62813493530599));
#87498=CARTESIAN_POINT('Ctrl Pts',(11.7547313433824,3.00451713239478,2.54062628879651));
#87499=CARTESIAN_POINT('Ctrl Pts',(11.7488710772825,3.07667089473987,2.45001738880779));
#87500=CARTESIAN_POINT('Ctrl Pts',(11.7430068641112,3.14887325488722,2.35934746090782));
#87501=CARTESIAN_POINT('Ctrl Pts',(11.7371426509399,3.2169922441767,2.2655734552825));
#87502=CARTESIAN_POINT('Ctrl Pts',(11.7312784377686,3.28077080176058,2.16910856028813));
#87503=CARTESIAN_POINT('Ctrl Pts',(11.7254055891943,3.34464327706713,2.07250161499349));
#87504=CARTESIAN_POINT('Ctrl Pts',(11.71953274062,3.40416235271693,1.97319622519693));
#87505=CARTESIAN_POINT('Ctrl Pts',(11.7136598920457,3.45911687723639,1.87163015299989));
#87506=CARTESIAN_POINT('Ctrl Pts',(11.7120651474329,3.47403952181282,1.844050360259));
#87507=CARTESIAN_POINT('Ctrl Pts',(11.7104704028201,3.48862586606958,1.81630398303906));
#87508=CARTESIAN_POINT('Ctrl Pts',(11.7088756582074,3.50287230338666,1.78840001849884));
#87509=CARTESIAN_POINT('Ctrl Pts',(11.7030032120734,3.55533301406993,1.68564718436352));
#87510=CARTESIAN_POINT('Ctrl Pts',(11.6971307659395,3.60335651369744,1.58041204790642));
#87511=CARTESIAN_POINT('Ctrl Pts',(11.6912583198056,3.64670018452956,1.47311464732112));
#87512=CARTESIAN_POINT('Ctrl Pts',(11.6853934808608,3.68998770780535,1.36595624019734));
#87513=CARTESIAN_POINT('Ctrl Pts',(11.6795286419159,3.72860730458444,1.25674126127248));
#87514=CARTESIAN_POINT('Ctrl Pts',(11.6736638029711,3.76236223807134,1.14591421560903));
#87515=CARTESIAN_POINT('Ctrl Pts',(11.6678049928511,3.7960824728083,1.03520109580903));
#87516=CARTESIAN_POINT('Ctrl Pts',(11.6619461827311,3.82494787117419,0.922879598464706));
#87517=CARTESIAN_POINT('Ctrl Pts',(11.656087372611,3.84881005824067,0.809413451571847));
#87518=CARTESIAN_POINT('Ctrl Pts',(11.6500015837301,3.87359670087795,0.691551462365815));
#87519=CARTESIAN_POINT('Ctrl Pts',(11.6439157948491,3.89298445832331,0.572454760379923));
#87520=CARTESIAN_POINT('Ctrl Pts',(11.6378300059681,3.9068642124379,0.452659944740006));
#87521=CARTESIAN_POINT('Ctrl Pts',(11.6319779758899,3.92021083686836,0.337466519851978));
#87522=CARTESIAN_POINT('Ctrl Pts',(11.6261259458116,3.92846473221161,0.221628070538059));
#87523=CARTESIAN_POINT('Ctrl Pts',(11.6202739157333,3.93158125972364,0.105630479454896));
#87524=CARTESIAN_POINT('Ctrl Pts',(11.6144227753548,3.93469731342168,-0.0103494762050065));
#87525=CARTESIAN_POINT('Ctrl Pts',(11.6085716349763,3.93267754116737,-0.126488112431964));
#87526=CARTESIAN_POINT('Ctrl Pts',(11.6027204945978,3.92552938770189,-0.242297392245137));
#87527=CARTESIAN_POINT('Ctrl Pts',(11.5968688270303,3.91838059018629,-0.358117106498744));
#87528=CARTESIAN_POINT('Ctrl Pts',(11.5910171594628,3.90610251837752,-0.473606992750635));
#87529=CARTESIAN_POINT('Ctrl Pts',(11.5851654918953,3.88875461610913,-0.588282700485007));
#87530=CARTESIAN_POINT('Ctrl Pts',(11.5793118802111,3.87140095029613,-0.702996507267154));
#87531=CARTESIAN_POINT('Ctrl Pts',(11.5734582685269,3.84897416656266,-0.81689518917469));
#87532=CARTESIAN_POINT('Ctrl Pts',(11.5676046568427,3.82158495236323,-0.929503874048374));
#87533=CARTESIAN_POINT('Ctrl Pts',(11.5617443907428,3.79416460196518,-1.0422405730503));
#87534=CARTESIAN_POINT('Ctrl Pts',(11.5558841246429,3.76177065897067,-1.15368394609837));
#87535=CARTESIAN_POINT('Ctrl Pts',(11.550023858543,3.72456392269728,-1.26337349415834));
#87536=CARTESIAN_POINT('Ctrl Pts',(11.5441596453717,3.68733212653026,-1.37313692153916));
#87537=CARTESIAN_POINT('Ctrl Pts',(11.5382954322004,3.6452812320772,-1.48114378756401));
#87538=CARTESIAN_POINT('Ctrl Pts',(11.5324312190291,3.59861982163417,-1.58695443518132));
#87539=CARTESIAN_POINT('Ctrl Pts',(11.5265583704548,3.55188969948653,-1.69292089527609));
#87540=CARTESIAN_POINT('Ctrl Pts',(11.5206855218805,3.50053569399984,-1.79668431334494));
#87541=CARTESIAN_POINT('Ctrl Pts',(11.5148126733062,3.44481188279228,-1.89783036443543));
#87542=CARTESIAN_POINT('Ctrl Pts',(11.5132179286934,3.42968034200677,-1.92529610240638));
#87543=CARTESIAN_POINT('Ctrl Pts',(11.5116231840806,3.41422682784621,-1.9525690154841));
#87544=CARTESIAN_POINT('Ctrl Pts',(11.5100284394677,3.3984569586644,-1.97964120489182));
#87545=CARTESIAN_POINT('Ctrl Pts',(11.5041559933338,3.34038640205949,-2.07933113188455));
#87546=CARTESIAN_POINT('Ctrl Pts',(11.4982835471999,3.27782846516256,-2.17663064366548));
#87547=CARTESIAN_POINT('Ctrl Pts',(11.492411101066,3.21100530195031,-2.27110852907716));
#87548=CARTESIAN_POINT('Ctrl Pts',(11.4865462621211,3.14426870171793,-2.3654640274766));
#87549=CARTESIAN_POINT('Ctrl Pts',(11.4806814231763,3.07327809930128,-2.45700483392695));
#87550=CARTESIAN_POINT('Ctrl Pts',(11.4748165842314,2.99830103872154,-2.54532510324346));
#87551=CARTESIAN_POINT('Ctrl Pts',(11.4689577741114,2.9234010516246,-2.633554582781));
#87552=CARTESIAN_POINT('Ctrl Pts',(11.4630989639914,2.84452302326456,-2.71856979689325));
#87553=CARTESIAN_POINT('Ctrl Pts',(11.4572401538713,2.76197681792224,-2.79999518879232));
#87554=CARTESIAN_POINT('Ctrl Pts',(11.4511543649904,2.67623265343389,-2.8845751179068));
#87555=CARTESIAN_POINT('Ctrl Pts',(11.4450685761094,2.58653060504518,-2.96528107851399));
#87556=CARTESIAN_POINT('Ctrl Pts',(11.4389827872284,2.4932630634291,-3.04173113482111));
#87557=CARTESIAN_POINT('Ctrl Pts',(11.4331307571501,2.40357798405176,-3.11524469859156));
#87558=CARTESIAN_POINT('Ctrl Pts',(11.4272787270719,2.31059661361456,-3.18482298456818));
#87559=CARTESIAN_POINT('Ctrl Pts',(11.4214266969936,2.21470354431358,-3.25016572051409));
#87560=CARTESIAN_POINT('Ctrl Pts',(11.4155755566151,2.11882505389179,-3.3154985222295));
#87561=CARTESIAN_POINT('Ctrl Pts',(11.4097244162366,2.0200360862833,-3.37659682157969));
#87562=CARTESIAN_POINT('Ctrl Pts',(11.403873275858,1.91875120799459,-3.43320299455469));
#87563=CARTESIAN_POINT('Ctrl Pts',(11.3980216082905,1.81745720391705,-3.48981426775777));
#87564=CARTESIAN_POINT('Ctrl Pts',(11.392169940723,1.71366720296469,-3.54193240832468));
#87565=CARTESIAN_POINT('Ctrl Pts',(11.3863182731555,1.60782078699842,-3.58934552765484));
#87566=CARTESIAN_POINT('Ctrl Pts',(11.3804646614713,1.50193920536598,-3.63677439918511));
#87567=CARTESIAN_POINT('Ctrl Pts',(11.3746110497871,1.39400022723991,-3.67949497233228));
#87568=CARTESIAN_POINT('Ctrl Pts',(11.3687574381028,1.28446316915365,-3.71734359013096));
#87569=CARTESIAN_POINT('Ctrl Pts',(11.362897172003,1.17480158878038,-3.75523523443164));
#87570=CARTESIAN_POINT('Ctrl Pts',(11.3570369059031,1.06353869328584,-3.78824373371904));
#87571=CARTESIAN_POINT('Ctrl Pts',(11.3511766398032,0.951148804400062,-3.81625535726952));
#87572=CARTESIAN_POINT('Ctrl Pts',(11.3453124266319,0.838683217429767,-3.84428584751939));
#87573=CARTESIAN_POINT('Ctrl Pts',(11.3394482134606,0.72508952974335,-3.86731267862198));
#87574=CARTESIAN_POINT('Ctrl Pts',(11.3335840002893,0.610850367354952,-3.88527358479455));
#87575=CARTESIAN_POINT('Ctrl Pts',(11.327711151715,0.496442980999267,-3.90326093947068));
#87576=CARTESIAN_POINT('Ctrl Pts',(11.3218383031407,0.381388632167704,-3.91616743488324));
#87577=CARTESIAN_POINT('Ctrl Pts',(11.3159654545664,0.266173237073291,-3.92398277364541));
#87578=CARTESIAN_POINT('Ctrl Pts',(11.3143707099536,0.234887034422116,-3.92610499240012));
#87579=CARTESIAN_POINT('Ctrl Pts',(11.3127759653408,0.203588943489356,-3.92785210188751));
#87580=CARTESIAN_POINT('Ctrl Pts',(11.3111812207281,0.172288646697863,-3.9292245573674));
#87581=CARTESIAN_POINT('Ctrl Pts',(11.3053087745941,0.0570292469096958,
-3.93427845177297));
#87582=CARTESIAN_POINT('Ctrl Pts',(11.2994363284602,-0.0586456867649011,
-3.93426499989482));
#87583=CARTESIAN_POINT('Ctrl Pts',(11.2935638823263,-0.174253294726548,
-3.92913791935037));
#87584=CARTESIAN_POINT('Ctrl Pts',(11.2876990433815,-0.289711144153209,
-3.92401748044555));
#87585=CARTESIAN_POINT('Ctrl Pts',(11.2818342044366,-0.405101432160393,
-3.91379660422549));
#87586=CARTESIAN_POINT('Ctrl Pts',(11.2759693654918,-0.519938094369209,
-3.89848090645879));
#87587=CARTESIAN_POINT('Ctrl Pts',(11.2701105553717,-0.634656708984688,
-3.88318095262984));
#87588=CARTESIAN_POINT('Ctrl Pts',(11.2642517452517,-0.748822422514947,
-3.86279664880266));
#87589=CARTESIAN_POINT('Ctrl Pts',(11.2583929351317,-0.861951766452858,
-3.83738558817182));
#87590=CARTESIAN_POINT('Ctrl Pts',(11.2523071462508,-0.979463904471754,
-3.81099006637249));
#87591=CARTESIAN_POINT('Ctrl Pts',(11.2462213573698,-1.09585729399974,-3.77917044291681));
#87592=CARTESIAN_POINT('Ctrl Pts',(11.2401355684888,-1.21059847758865,-3.74205028374286));
#87593=CARTESIAN_POINT('Ctrl Pts',(11.2342835384106,-1.32093238346523,-3.70635593215681));
#87594=CARTESIAN_POINT('Ctrl Pts',(11.2284315083323,-1.4297382369095,-3.6657608661504));
#87595=CARTESIAN_POINT('Ctrl Pts',(11.222579478254,-1.53655549330081,-3.62042624783424));
#87596=CARTESIAN_POINT('Ctrl Pts',(11.2167283378755,-1.64335650997958,-3.57509852186108));
#87597=CARTESIAN_POINT('Ctrl Pts',(11.210877197497,-1.74816915033764,-3.52503283774727));
#87598=CARTESIAN_POINT('Ctrl Pts',(11.2050260571185,-1.8505525384064,-3.47043863259353));
#87599=CARTESIAN_POINT('Ctrl Pts',(11.199174389551,-1.95294515123991,-3.41583950849044));
#87600=CARTESIAN_POINT('Ctrl Pts',(11.1933227219835,-2.05290771191474,-3.35671124674412));
#87601=CARTESIAN_POINT('Ctrl Pts',(11.187471054416,-2.15002429143809,-3.29330905719857));
#87602=CARTESIAN_POINT('Ctrl Pts',(11.1816174427318,-2.24717313628831,-3.2298858033571));
#87603=CARTESIAN_POINT('Ctrl Pts',(11.1757638310476,-2.34147377391848,-3.16218602410032));
#87604=CARTESIAN_POINT('Ctrl Pts',(11.1699102193634,-2.43254017747779,-3.09050760959366));
#87605=CARTESIAN_POINT('Ctrl Pts',(11.1640499532635,-2.52371010579004,-3.0187477106991));
#87606=CARTESIAN_POINT('Ctrl Pts',(11.1581896871636,-2.61163813647035,-2.94300040474197));
#87607=CARTESIAN_POINT('Ctrl Pts',(11.1523294210637,-2.69597212760409,-2.86360320002298));
#87608=CARTESIAN_POINT('Ctrl Pts',(11.1464652078924,-2.78036292030289,-2.78415251881808));
#87609=CARTESIAN_POINT('Ctrl Pts',(11.1406009947211,-2.86115456593174,-2.70104733950031));
#87610=CARTESIAN_POINT('Ctrl Pts',(11.1347367815498,-2.93803372513164,-2.61465998362867));
#87611=CARTESIAN_POINT('Ctrl Pts',(11.1288639329755,-3.01502609346969,-2.5281454172333));
#87612=CARTESIAN_POINT('Ctrl Pts',(11.1229910844012,-3.08809421693889,-2.43833934760837));
#87613=CARTESIAN_POINT('Ctrl Pts',(11.117118235827,-3.15696669341386,-2.34564496390131));
#87614=CARTESIAN_POINT('Ctrl Pts',(11.1155234912141,-3.17566869286801,-2.32047423675136));
#87615=CARTESIAN_POINT('Ctrl Pts',(11.1139287466013,-3.19406157517828,-2.2950906836513));
#87616=CARTESIAN_POINT('Ctrl Pts',(11.1123340019885,-3.21214048792809,-2.26950269570518));
#87617=CARTESIAN_POINT('Ctrl Pts',(11.1063993270745,-3.27941926667771,-2.1742796807209));
#87618=CARTESIAN_POINT('Ctrl Pts',(11.1004646521605,-3.34256962426546,-2.07590768305915));
#87619=CARTESIAN_POINT('Ctrl Pts',(11.0945299772465,-3.40128662071416,-1.97477551224204));
#87620=CARTESIAN_POINT('Ctrl Pts',(11.0886033536864,-3.45992395798658,-1.87378054369873));
#87621=CARTESIAN_POINT('Ctrl Pts',(11.0826767301263,-3.5141396972636,-1.77003319406172));
#87622=CARTESIAN_POINT('Ctrl Pts',(11.0767501065661,-3.56367074985205,-1.66395306023004));
#87623=CARTESIAN_POINT('Ctrl Pts',(11.0708301927134,-3.61314572685761,-1.55799302288384));
#87624=CARTESIAN_POINT('Ctrl Pts',(11.0649102788607,-3.6579463995249,-1.44970581711695));
#87625=CARTESIAN_POINT('Ctrl Pts',(11.0589903650079,-3.69785469604635,-1.33953710173625));
#87626=CARTESIAN_POINT('Ctrl Pts',(11.0530765800023,-3.73772167577604,-1.22948244328781));
#87627=CARTESIAN_POINT('Ctrl Pts',(11.0471627949967,-3.7727062283439,-1.11755053000092));
#87628=CARTESIAN_POINT('Ctrl Pts',(11.0412490099911,-3.80263797799915,-1.00420785113367));
#87629=CARTESIAN_POINT('Ctrl Pts',(11.0353388793976,-3.83255123138704,-0.890935212157697));
#87630=CARTESIAN_POINT('Ctrl Pts',(11.0294287488041,-3.85741779186855,-0.776253929583021));
#87631=CARTESIAN_POINT('Ctrl Pts',(11.0235186182106,-3.8771169050801,-0.660646277778147));
#87632=CARTESIAN_POINT('Ctrl Pts',(11.0176101824024,-3.89681036938656,-0.545071777549431));
#87633=CARTESIAN_POINT('Ctrl Pts',(11.0117017465942,-3.91133926234982,-0.42857183151326));
#87634=CARTESIAN_POINT('Ctrl Pts',(11.0057933107859,-3.92063388177004,-0.31163915850992));
#87635=CARTESIAN_POINT('Ctrl Pts',(11.0005167145356,-3.92893454806693,-0.207211096001756));
#87636=CARTESIAN_POINT('Ctrl Pts',(10.9952401182853,-3.9330612436711,-0.102438247546336));
#87637=CARTESIAN_POINT('Ctrl Pts',(10.989963522035,-3.93299931278836,0.00232499597257397));
#87638=CARTESIAN_POINT('',(9.73996412712546,-3.93468200878748,0.00220793234553757));
#87639=CARTESIAN_POINT('Ctrl Pts',(10.9899620430679,-3.92789199627619,0.00235130254412344));
#87640=CARTESIAN_POINT('Ctrl Pts',(10.9644702897948,-3.93059709637408,0.50781727451283));
#87641=CARTESIAN_POINT('Ctrl Pts',(10.8726961302754,-3.60487430294788,2.32421058671237));
#87642=CARTESIAN_POINT('Ctrl Pts',(10.714639564509,-0.864193458227065,4.57068481609948));
#87643=CARTESIAN_POINT('Ctrl Pts',(10.5157923457696,3.37762255948928,3.19838332083506));
#87644=CARTESIAN_POINT('Ctrl Pts',(10.3169451270298,4.51682366238826,-1.11188759515321));
#87645=CARTESIAN_POINT('Ctrl Pts',(10.1180979082903,1.50696304637114,-4.40080133592016));
#87646=CARTESIAN_POINT('Ctrl Pts',(9.92577130003029,-2.74307050786764,-3.67194027927687));
#87647=CARTESIAN_POINT('Ctrl Pts',(9.79972709801699,-3.92999336875819,-1.17507727859808));
#87648=CARTESIAN_POINT('Ctrl Pts',(9.73996530225019,-3.93794979387841,0.00218662693770836));
#87649=CARTESIAN_POINT('',(8.489963468396,-3.93310746533601,-0.00342879478566001));
#87650=CARTESIAN_POINT('Ctrl Pts',(9.73996352203497,-3.93299937407447,0.00221890284016636));
#87651=CARTESIAN_POINT('Ctrl Pts',(9.7334435049603,-3.93292700297544,0.130496483113836));
#87652=CARTESIAN_POINT('Ctrl Pts',(9.72692348788562,-3.92657937860584,0.25859433429193));
#87653=CARTESIAN_POINT('Ctrl Pts',(9.72040347081094,-3.91400567965978,0.386068050466482));
#87654=CARTESIAN_POINT('Ctrl Pts',(9.714531024677,-3.90268080597933,0.50088102152982));
#87655=CARTESIAN_POINT('Ctrl Pts',(9.70865857854307,-3.88628082419871,0.615387488854809));
#87656=CARTESIAN_POINT('Ctrl Pts',(9.70278613240914,-3.86482832122034,0.729102905969475));
#87657=CARTESIAN_POINT('Ctrl Pts',(9.69692129346427,-3.84340360789598,0.842671015700072));
#87658=CARTESIAN_POINT('Ctrl Pts',(9.69105645451941,-3.81693946508308,0.955449710595288));
#87659=CARTESIAN_POINT('Ctrl Pts',(9.68519161557455,-3.7855103084452,1.06695862368468));
#87660=CARTESIAN_POINT('Ctrl Pts',(9.67933280545452,-3.75411345974988,1.17835290997703));
#87661=CARTESIAN_POINT('Ctrl Pts',(9.67347399533448,-3.71776186051044,1.28847961528162));
#87662=CARTESIAN_POINT('Ctrl Pts',(9.66761518521445,-3.67658101189881,1.39686830551242));
#87663=CARTESIAN_POINT('Ctrl Pts',(9.66152939633348,-3.63380475776958,1.5094561300561));
#87664=CARTESIAN_POINT('Ctrl Pts',(9.65544360745251,-3.58581758647112,1.62016810300132));
#87665=CARTESIAN_POINT('Ctrl Pts',(9.64935781857155,-3.53281738809582,1.72849365123735));
#87666=CARTESIAN_POINT('Ctrl Pts',(9.64350578849328,-3.48185295914286,1.83265835016494));
#87667=CARTESIAN_POINT('Ctrl Pts',(9.63765375841501,-3.42625370453409,1.93461616504343));
#87668=CARTESIAN_POINT('Ctrl Pts',(9.63180172833674,-3.36624440245535,2.03393402620096));
#87669=CARTESIAN_POINT('Ctrl Pts',(9.62595058795822,-3.30624422375095,2.13323678779901));
#87670=CARTESIAN_POINT('Ctrl Pts',(9.6200994475797,-3.24183554439956,2.22990004001445));
#87671=CARTESIAN_POINT('Ctrl Pts',(9.61424830720118,-3.17328814444511,2.32351702217224));
#87672=CARTESIAN_POINT('Ctrl Pts',(9.60839663963368,-3.10473456835549,2.41714243923982));
#87673=CARTESIAN_POINT('Ctrl Pts',(9.60254497206618,-3.03204177458839,2.50772070709806));
#87674=CARTESIAN_POINT('Ctrl Pts',(9.59669330449868,-2.95552132029931,2.59487624468995));
#87675=CARTESIAN_POINT('Ctrl Pts',(9.59083969281444,-2.87897544339443,2.68206073822267));
#87676=CARTESIAN_POINT('Ctrl Pts',(9.5849860811302,-2.79859964989581,2.76581992988817));
#87677=CARTESIAN_POINT('Ctrl Pts',(9.57913246944596,-2.71474351087968,2.84581388536508));
#87678=CARTESIAN_POINT('Ctrl Pts',(9.57327220334606,-2.63079204377651,2.92589877837906));
#87679=CARTESIAN_POINT('Ctrl Pts',(9.56741193724617,-2.54335263343562,3.00220960630231));
#87680=CARTESIAN_POINT('Ctrl Pts',(9.56155167114628,-2.45280926934149,3.07444559038414));
#87681=CARTESIAN_POINT('Ctrl Pts',(9.55568745797496,-2.36220492147658,3.14673022764712));
#87682=CARTESIAN_POINT('Ctrl Pts',(9.54982324480365,-2.26849279042965,3.21493431350354));
#87683=CARTESIAN_POINT('Ctrl Pts',(9.54395903163234,-2.17208583103624,3.27880041213423));
#87684=CARTESIAN_POINT('Ctrl Pts',(9.53808618305805,-2.07553690665617,3.34276055739701));
#87685=CARTESIAN_POINT('Ctrl Pts',(9.53221333448375,-1.97628558702804,3.40236975434652));
#87686=CARTESIAN_POINT('Ctrl Pts',(9.52634048590945,-1.87476944239729,3.45741645421163));
#87687=CARTESIAN_POINT('Ctrl Pts',(9.52474574129675,-1.84720320725529,3.47236412857212));
#87688=CARTESIAN_POINT('Ctrl Pts',(9.52315099668404,-1.81947008242169,3.48697565397087));
#87689=CARTESIAN_POINT('Ctrl Pts',(9.52155625207134,-1.79157906177759,3.50124741562206));
#87690=CARTESIAN_POINT('Ctrl Pts',(9.51568380593743,-1.68887389190436,3.55380137997778));
#87691=CARTESIAN_POINT('Ctrl Pts',(9.50981135980352,-1.58368239279322,3.60192038844979));
#87692=CARTESIAN_POINT('Ctrl Pts',(9.50393891366961,-1.47642438222513,3.64536144210298));
#87693=CARTESIAN_POINT('Ctrl Pts',(9.49807407472477,-1.36930531409211,3.68874622204996));
#87694=CARTESIAN_POINT('Ctrl Pts',(9.49220923577993,-1.26012543763137,3.72746494430459));
#87695=CARTESIAN_POINT('Ctrl Pts',(9.48634439683508,-1.14932907913176,3.7613204686469));
#87696=CARTESIAN_POINT('Ctrl Pts',(9.48048558671507,-1.03864661495097,3.79514119083564));
#87697=CARTESIAN_POINT('Ctrl Pts',(9.47462677659505,-0.926351366844571,
3.82410853868028));
#87698=CARTESIAN_POINT('Ctrl Pts',(9.46876796647504,-0.812906927927939,
3.84807371635819));
#87699=CARTESIAN_POINT('Ctrl Pts',(9.46268217759406,-0.695067487696164,
3.87296733961191));
#87700=CARTESIAN_POINT('Ctrl Pts',(9.45659638871309,-0.575988434281552,
3.89246320072552));
#87701=CARTESIAN_POINT('Ctrl Pts',(9.45051059983211,-0.456206267535364,
3.90645169449994));
#87702=CARTESIAN_POINT('Ctrl Pts',(9.44465856975385,-0.341025005689439,
3.91990288183466));
#87703=CARTESIAN_POINT('Ctrl Pts',(9.43880653967558,-0.225194096689067,
3.92826192771017));
#87704=CARTESIAN_POINT('Ctrl Pts',(9.43295450959732,-0.109199382469267,
3.93148375233427));
#87705=CARTESIAN_POINT('Ctrl Pts',(9.4271033692188,0.00677769676451066,
3.93470508713577));
#87706=CARTESIAN_POINT('Ctrl Pts',(9.42125222884029,0.122918118616052,3.93279074214541));
#87707=CARTESIAN_POINT('Ctrl Pts',(9.41540108846178,0.238733839547532,3.92574771907912));
#87708=CARTESIAN_POINT('Ctrl Pts',(9.40954942089428,0.354559995499951,3.91870406143495));
#87709=CARTESIAN_POINT('Ctrl Pts',(9.40369775332678,0.470060979755278,3.90653083220509));
#87710=CARTESIAN_POINT('Ctrl Pts',(9.39784608575928,0.58475238803632,3.88928703552281));
#87711=CARTESIAN_POINT('Ctrl Pts',(9.39199247407505,0.699481900581413,3.87203750988322));
#87712=CARTESIAN_POINT('Ctrl Pts',(9.38613886239082,0.813400893779758,3.84971412847263));
#87713=CARTESIAN_POINT('Ctrl Pts',(9.38028525070659,0.926034395189715,3.82242714762827));
#87714=CARTESIAN_POINT('Ctrl Pts',(9.3744249846067,1.03879593893931,3.79510914680474));
#87715=CARTESIAN_POINT('Ctrl Pts',(9.36856471850681,1.15026867211446,3.76281638139967));
#87716=CARTESIAN_POINT('Ctrl Pts',(9.36270445240692,1.2599919499029,3.72570923264013));
#87717=CARTESIAN_POINT('Ctrl Pts',(9.35684023923562,1.36978912973027,3.68857709106222));
#87718=CARTESIAN_POINT('Ctrl Pts',(9.35097602606431,1.47783412352762,3.64662425864128));
#87719=CARTESIAN_POINT('Ctrl Pts',(9.345111812893,1.58368708508111,3.60005891848276));
#87720=CARTESIAN_POINT('Ctrl Pts',(9.33923896431871,1.6896959214218,3.55342500808888));
#87721=CARTESIAN_POINT('Ctrl Pts',(9.33336611574442,1.79350591403744,3.50216521641961));
#87722=CARTESIAN_POINT('Ctrl Pts',(9.32749326717013,1.89470250750391,3.44653324487932));
#87723=CARTESIAN_POINT('Ctrl Pts',(9.3258985225573,1.92218197002126,3.43142664272661));
#87724=CARTESIAN_POINT('Ctrl Pts',(9.32430377794448,1.94946890000054,3.41599789229209));
#87725=CARTESIAN_POINT('Ctrl Pts',(9.32270903333165,1.97655539356812,3.400252604757));
#87726=CARTESIAN_POINT('Ctrl Pts',(9.31683658719773,2.07629799382696,3.34227256696972));
#87727=CARTESIAN_POINT('Ctrl Pts',(9.31096414106382,2.17365425333958,3.27980298080728));
#87728=CARTESIAN_POINT('Ctrl Pts',(9.3050916949299,2.2681927594629,3.21306560871702));
#87729=CARTESIAN_POINT('Ctrl Pts',(9.29922685598505,2.3626088000456,3.14641468847256));
#87730=CARTESIAN_POINT('Ctrl Pts',(9.29336201704021,2.45421401146745,3.07550721272152));
#87731=CARTESIAN_POINT('Ctrl Pts',(9.28749717809536,2.54260230584417,3.00061035696338));
#87732=CARTESIAN_POINT('Ctrl Pts',(9.28163836797534,2.63089974051472,2.9257904922407));
#87733=CARTESIAN_POINT('Ctrl Pts',(9.27577955785533,2.71598652220557,2.84698967010068));
#87734=CARTESIAN_POINT('Ctrl Pts',(9.26992074773531,2.79748681300003,2.76451741377965));
#87735=CARTESIAN_POINT('Ctrl Pts',(9.26383495885434,2.88214454270148,2.67885006320415));
#87736=CARTESIAN_POINT('Ctrl Pts',(9.25774916997336,2.96293189831491,2.58922131371123));
#87737=CARTESIAN_POINT('Ctrl Pts',(9.25166338109239,3.03946658800689,2.49602320910479));
#87738=CARTESIAN_POINT('Ctrl Pts',(9.24581135101413,3.11306153434305,2.40640489961994));
#87739=CARTESIAN_POINT('Ctrl Pts',(9.23995932093587,3.18272419675997,2.31348672813126));
#87740=CARTESIAN_POINT('Ctrl Pts',(9.2341072908576,3.24815395402568,2.21765301410012));
#87741=CARTESIAN_POINT('Ctrl Pts',(9.22825615047909,3.31357376383076,2.12183386992431));
#87742=CARTESIAN_POINT('Ctrl Pts',(9.22240501010057,3.37476171504071,2.02310040583366));
#87743=CARTESIAN_POINT('Ctrl Pts',(9.21655386972206,3.43145980742328,1.92186695430214));
#87744=CARTESIAN_POINT('Ctrl Pts',(9.21070220215456,3.48816300831595,1.82062438161526));
#87745=CARTESIAN_POINT('Ctrl Pts',(9.20485053458707,3.54037534419892,1.71688173437947));
#87746=CARTESIAN_POINT('Ctrl Pts',(9.19899886701957,3.58788452752248,1.61107840192983));
#87747=CARTESIAN_POINT('Ctrl Pts',(9.19314525533533,3.63540949496186,1.50523991812761));
#87748=CARTESIAN_POINT('Ctrl Pts',(9.1872916436511,3.67822803358777,1.39733976465732));
#87749=CARTESIAN_POINT('Ctrl Pts',(9.18143803196686,3.71617606955139,1.28783710930133));
#87750=CARTESIAN_POINT('Ctrl Pts',(9.17557776586697,3.75416724503605,1.17820997076762));
#87751=CARTESIAN_POINT('Ctrl Pts',(9.16971749976709,3.78727673113501,1.06697708503089));
#87752=CARTESIAN_POINT('Ctrl Pts',(9.1638572336672,3.81539036659949,0.954612670385135));
#87753=CARTESIAN_POINT('Ctrl Pts',(9.1579930204959,3.84352293747151,0.842172574812675));
#87754=CARTESIAN_POINT('Ctrl Pts',(9.15212880732459,3.86665287530667,0.72859983684903));
#87755=CARTESIAN_POINT('Ctrl Pts',(9.14626459415329,3.88471747623753,0.614377025786864));
#87756=CARTESIAN_POINT('Ctrl Pts',(9.140391745579,3.90280867836863,0.499986014835841));
#87757=CARTESIAN_POINT('Ctrl Pts',(9.13451889700471,3.9158196106186,0.384943429456174));
#87758=CARTESIAN_POINT('Ctrl Pts',(9.12864604843042,3.92373953450778,0.269735176313091));
#87759=CARTESIAN_POINT('Ctrl Pts',(9.12705130381763,3.92589015286551,0.238450913024903));
#87760=CARTESIAN_POINT('Ctrl Pts',(9.12545655920482,3.92766567290221,0.207154420949471));
#87761=CARTESIAN_POINT('Ctrl Pts',(9.12386181459203,3.92906654108815,0.175855382918928));
#87762=CARTESIAN_POINT('Ctrl Pts',(9.11798936845811,3.93422506170433,0.0606006183611476));
#87763=CARTESIAN_POINT('Ctrl Pts',(9.11211692232419,3.93431661533117,-0.0550742798645938));
#87764=CARTESIAN_POINT('Ctrl Pts',(9.10624447619028,3.92929448128277,-0.170686494371317));
#87765=CARTESIAN_POINT('Ctrl Pts',(9.10037963724543,3.92427885292593,-0.286148944375347));
#87766=CARTESIAN_POINT('Ctrl Pts',(9.09451479830059,3.91416272802553,-0.401548462979302));
#87767=CARTESIAN_POINT('Ctrl Pts',(9.08864995935575,3.8989512811163,-0.516398980906778));
#87768=CARTESIAN_POINT('Ctrl Pts',(9.08279114923572,3.88375547097896,-0.631131436998315));
#87769=CARTESIAN_POINT('Ctrl Pts',(9.0769323391157,3.86347481103469,-0.745315607620525));
#87770=CARTESIAN_POINT('Ctrl Pts',(9.07107352899568,3.83816645557921,-0.85846797218446));
#87771=CARTESIAN_POINT('Ctrl Pts',(9.06498774011471,3.81187761790205,-0.97600402268136));
#87772=CARTESIAN_POINT('Ctrl Pts',(9.05890195123374,3.78016366524417,-1.09242624895059));
#87773=CARTESIAN_POINT('Ctrl Pts',(9.05281616235277,3.74314767923944,-1.2072010815951));
#87774=CARTESIAN_POINT('Ctrl Pts',(9.0469641322745,3.70755349946864,-1.31756734404697));
#87775=CARTESIAN_POINT('Ctrl Pts',(9.04111210219623,3.66705722018621,-1.42641000338649));
#87776=CARTESIAN_POINT('Ctrl Pts',(9.03526007211797,3.62181958537068,-1.53326836888567));
#87777=CARTESIAN_POINT('Ctrl Pts',(9.02940893173945,3.57658882815353,-1.64011048842231));
#87778=CARTESIAN_POINT('Ctrl Pts',(9.02355779136093,3.52661830977212,-1.74496853340364));
#87779=CARTESIAN_POINT('Ctrl Pts',(9.01770665098242,3.47211706702969,-1.84740143792332));
#87780=CARTESIAN_POINT('Ctrl Pts',(9.01185498341492,3.41761091371376,-1.94984357166936));
#87781=CARTESIAN_POINT('Ctrl Pts',(9.00600331584742,3.35857341870767,-2.04985976564441));
#87782=CARTESIAN_POINT('Ctrl Pts',(9.00015164827992,3.29525941418505,-2.14703385935686));
#87783=CARTESIAN_POINT('Ctrl Pts',(8.99429803659569,3.23192437466436,-2.24424023750446));
#87784=CARTESIAN_POINT('Ctrl Pts',(8.98844442491144,3.16431022599136,-2.3386022916798));
#87785=CARTESIAN_POINT('Ctrl Pts',(8.9825908132272,3.09271450778762,-2.42973372477725));
#87786=CARTESIAN_POINT('Ctrl Pts',(8.97673054712731,3.02103739920585,-2.52096875655319));
#87787=CARTESIAN_POINT('Ctrl Pts',(8.97087028102742,2.9453699423276,-2.60896551165607));
#87788=CARTESIAN_POINT('Ctrl Pts',(8.96501001492753,2.86604932565287,-2.69337154193861));
#87789=CARTESIAN_POINT('Ctrl Pts',(8.95914580175622,2.78667528407667,-2.77783442230678));
#87790=CARTESIAN_POINT('Ctrl Pts',(8.95328158858492,2.70364347871848,-2.85870147450845));
#87791=CARTESIAN_POINT('Ctrl Pts',(8.94741737541361,2.61732594654579,-2.93565902133374));
#87792=CARTESIAN_POINT('Ctrl Pts',(8.94154452683932,2.53088130666863,-3.0127298927279));
#87793=CARTESIAN_POINT('Ctrl Pts',(8.93567167826502,2.44114160263122,-3.085879508777));
#87794=CARTESIAN_POINT('Ctrl Pts',(8.92979882969073,2.34850977704589,-3.15483610146706));
#87795=CARTESIAN_POINT('Ctrl Pts',(8.92820408507795,2.3233560372626,-3.17356094228616));
#87796=CARTESIAN_POINT('Ctrl Pts',(8.92660934046517,2.29798919101159,-3.19197685928441));
#87797=CARTESIAN_POINT('Ctrl Pts',(8.92501459585239,2.27241762498861,-3.21007899243011));
#87798=CARTESIAN_POINT('Ctrl Pts',(8.91914214971847,2.1782535545624,-3.27673781726956));
#87799=CARTESIAN_POINT('Ctrl Pts',(8.91326970358456,2.08099630301674,-3.33936143488604));
#87800=CARTESIAN_POINT('Ctrl Pts',(8.90739725745064,1.9810267582882,-3.39764947911731));
#87801=CARTESIAN_POINT('Ctrl Pts',(8.9015324185058,1.88118671448837,-3.45586201679425));
#87802=CARTESIAN_POINT('Ctrl Pts',(8.89566757956095,1.77864171843713,-3.50974994365985));
#87803=CARTESIAN_POINT('Ctrl Pts',(8.8898027406161,1.6738034538666,-3.55905478994413));
#87804=CARTESIAN_POINT('Ctrl Pts',(8.88394393049609,1.56907295892763,-3.60830895277672));
#87805=CARTESIAN_POINT('Ctrl Pts',(8.87808512037608,1.46205425625753,-3.65298923105742));
#87806=CARTESIAN_POINT('Ctrl Pts',(8.87222631025606,1.3531849915988,-3.69288225895597));
#87807=CARTESIAN_POINT('Ctrl Pts',(8.86614052137509,1.24009797447974,-3.73432080033894));
#87808=CARTESIAN_POINT('Ctrl Pts',(8.86005473249412,1.12501450101084,-3.77059343047534));
#87809=CARTESIAN_POINT('Ctrl Pts',(8.85396894361315,1.0084499660249,-3.80151518029645));
#87810=CARTESIAN_POINT('Ctrl Pts',(8.84811691353488,0.896362744772546,-3.83124920715228));
#87811=CARTESIAN_POINT('Ctrl Pts',(8.84226488345661,0.782906576640369,-3.85603571639762));
#87812=CARTESIAN_POINT('Ctrl Pts',(8.83641285337835,0.668555914690499,-3.87576082710638));
#87813=CARTESIAN_POINT('Ctrl Pts',(8.83056171299983,0.554222637776941,-3.89548293895392));
#87814=CARTESIAN_POINT('Ctrl Pts',(8.82471057262132,0.438995544672728,-3.91014511203182));
#87815=CARTESIAN_POINT('Ctrl Pts',(8.81885943224281,0.323358692289862,-3.91968470111061));
#87816=CARTESIAN_POINT('Ctrl Pts',(8.81300776467532,0.207711421002246,-3.92922514970839));
#87817=CARTESIAN_POINT('Ctrl Pts',(8.80715609710782,0.0916547290259299,
-3.93364206280956));
#87818=CARTESIAN_POINT('Ctrl Pts',(8.80130442954033,-0.0243235153582555,
-3.93292478527121));
#87819=CARTESIAN_POINT('Ctrl Pts',(8.7954508178561,-0.140340291535808,-3.93220726942963));
#87820=CARTESIAN_POINT('Ctrl Pts',(8.78959720617188,-0.25627815516653,-3.92635217372918));
#87821=CARTESIAN_POINT('Ctrl Pts',(8.78374359448765,-0.371651266961712,
-3.91540091635145));
#87822=CARTESIAN_POINT('Ctrl Pts',(8.77788332838776,-0.487155535499663,
-3.90443720952839));
#87823=CARTESIAN_POINT('Ctrl Pts',(8.77202306228787,-0.602093359015705,
-3.88836581679333));
#87824=CARTESIAN_POINT('Ctrl Pts',(8.76616279618798,-0.715985933712069,
-3.8672798117962));
#87825=CARTESIAN_POINT('Ctrl Pts',(8.76029858301667,-0.829955218598503,
-3.84617960471912));
#87826=CARTESIAN_POINT('Ctrl Pts',(8.75443436984537,-0.942877451107107,
-3.82005815303478));
#87827=CARTESIAN_POINT('Ctrl Pts',(8.74857015667407,-1.05428759897505,-3.78905880907745));
#87828=CARTESIAN_POINT('Ctrl Pts',(8.74269730809978,-1.1658618049178,-3.7580138167408));
#87829=CARTESIAN_POINT('Ctrl Pts',(8.73682445952549,-1.27591909083997,-3.7220767241443));
#87830=CARTESIAN_POINT('Ctrl Pts',(8.73095161095121,-1.38401296786932,-3.68143954245748));
#87831=CARTESIAN_POINT('Ctrl Pts',(8.72935686633839,-1.41336535553788,-3.67040470548605));
#87832=CARTESIAN_POINT('Ctrl Pts',(8.72776212172556,-1.44257310258369,-3.65902356318122));
#87833=CARTESIAN_POINT('Ctrl Pts',(8.72616737711274,-1.47162758593249,-3.64730054263732));
#87834=CARTESIAN_POINT('Ctrl Pts',(8.72029493097883,-1.57861706063779,-3.60413199632748));
#87835=CARTESIAN_POINT('Ctrl Pts',(8.71442248484491,-1.68388459775975,-3.55617956062416));
#87836=CARTESIAN_POINT('Ctrl Pts',(8.70855003871099,-1.78697157659788,-3.50360123079544));
#87837=CARTESIAN_POINT('Ctrl Pts',(8.70268519976615,-1.88992501617127,-3.45109101113529));
#87838=CARTESIAN_POINT('Ctrl Pts',(8.6968203608213,-1.99070314995889,-3.39396700018268));
#87839=CARTESIAN_POINT('Ctrl Pts',(8.69095552187646,-2.08886594927692,-3.33243575271173));
#87840=CARTESIAN_POINT('Ctrl Pts',(8.68509671175643,-2.18692784108041,-3.27096775695419));
#87841=CARTESIAN_POINT('Ctrl Pts',(8.67923790163641,-2.28237939777625,-3.20510175424569));
#87842=CARTESIAN_POINT('Ctrl Pts',(8.67337909151639,-2.37480449459196,-3.13509052699692));
#87843=CARTESIAN_POINT('Ctrl Pts',(8.66729330263542,-2.4708102730693,-3.06236696374684));
#87844=CARTESIAN_POINT('Ctrl Pts',(8.66120751375445,-2.56354994534687,-2.98517070251276));
#87845=CARTESIAN_POINT('Ctrl Pts',(8.65512172487348,-2.6525892345319,-2.90383528335294));
#87846=CARTESIAN_POINT('Ctrl Pts',(8.64926969479521,-2.73820847119117,-2.82562400644849));
#87847=CARTESIAN_POINT('Ctrl Pts',(8.64341766471695,-2.82040601552851,-2.74358598579513));
#87848=CARTESIAN_POINT('Ctrl Pts',(8.63756563463868,-2.89882952826502,-2.65805875895527));
#87849=CARTESIAN_POINT('Ctrl Pts',(8.63171449426016,-2.97724111806558,-2.57254453504796));
#87850=CARTESIAN_POINT('Ctrl Pts',(8.62586335388165,-3.05187953783439,-2.48354246429099));
#87851=CARTESIAN_POINT('Ctrl Pts',(8.62001221350314,-3.12243035531733,-2.39142586675667));
#87852=CARTESIAN_POINT('Ctrl Pts',(8.61416054593563,-3.19298752944389,-2.29930096949737));
#87853=CARTESIAN_POINT('Ctrl Pts',(8.60830887836813,-3.25945611779732,-2.20406131580116));
#87854=CARTESIAN_POINT('Ctrl Pts',(8.60245721080062,-3.3215633618016,-2.10611154346993));
#87855=CARTESIAN_POINT('Ctrl Pts',(8.59660359911638,-3.38369123987837,-2.00812922899749));
#87856=CARTESIAN_POINT('Ctrl Pts',(8.59074998743213,-3.44145467115868,-1.90743535442846));
#87857=CARTESIAN_POINT('Ctrl Pts',(8.58489637574788,-3.49462579870807,-1.80446100733819));
#87858=CARTESIAN_POINT('Ctrl Pts',(8.57903610964799,-3.54785737146671,-1.70136959848446));
#87859=CARTESIAN_POINT('Ctrl Pts',(8.5731758435481,-3.59648603068227,-1.59599291016126));
#87860=CARTESIAN_POINT('Ctrl Pts',(8.56731557744821,-3.64033117662272,-1.48878404226693));
#87861=CARTESIAN_POINT('Ctrl Pts',(8.56145136427691,-3.68420585363208,-1.38150296586699));
#87862=CARTESIAN_POINT('Ctrl Pts',(8.5555871511056,-3.7232904629761,-1.27238764088816));
#87863=CARTESIAN_POINT('Ctrl Pts',(8.5497229379343,-3.75745414621014,-1.16190676869024));
#87864=CARTESIAN_POINT('Ctrl Pts',(8.54385008936,-3.79166813750154,-1.051263206831));
#87865=CARTESIAN_POINT('Ctrl Pts',(8.5379772407857,-3.82094663625831,-0.939250482913397));
#87866=CARTESIAN_POINT('Ctrl Pts',(8.5321043922114,-3.84520974288296,-0.826348009762216));
#87867=CARTESIAN_POINT('Ctrl Pts',(8.53050964759863,-3.8517982762138,-0.795689870266806));
#87868=CARTESIAN_POINT('Ctrl Pts',(8.52891490298586,-3.85801728574547,-0.764966152912951));
#87869=CARTESIAN_POINT('Ctrl Pts',(8.52732015837309,-3.86386583300464,-0.734186505282812));
#87870=CARTESIAN_POINT('Ctrl Pts',(8.51861044952465,-3.89580771473652,-0.566083244629494));
#87871=CARTESIAN_POINT('Ctrl Pts',(8.50990074067621,-3.91678675781709,-0.395835647213497));
#87872=CARTESIAN_POINT('Ctrl Pts',(8.50119103182777,-3.92658132922545,-0.224606466910645));
#87873=CARTESIAN_POINT('Ctrl Pts',(8.4974485285635,-3.93078999062915,-0.151030440734303));
#87874=CARTESIAN_POINT('Ctrl Pts',(8.49370602529924,-3.9329341093572,-0.0772734915122383));
#87875=CARTESIAN_POINT('Ctrl Pts',(8.48996352203497,-3.93299850454534,-0.00342975860908187));
#87876=CARTESIAN_POINT('',(7.23996352203496,-3.92656899063656,-0.000561720325250592));
#87877=CARTESIAN_POINT('Ctrl Pts',(8.48996263443681,-3.93480154809321,-0.00341380960952649));
#87878=CARTESIAN_POINT('Ctrl Pts',(8.43613273616902,-3.9250547143977,1.05920602663723));
#87879=CARTESIAN_POINT('Ctrl Pts',(8.31602043165469,-2.93158872492316,3.44630354530614));
#87880=CARTESIAN_POINT('Ctrl Pts',(8.1296257208938,1.10778692872341,4.51783113251438));
#87881=CARTESIAN_POINT('Ctrl Pts',(7.93077850215417,4.39943155644481,1.51095731293844));
#87882=CARTESIAN_POINT('Ctrl Pts',(7.7319312834145,3.64984844976654,-2.8838509523037));
#87883=CARTESIAN_POINT('Ctrl Pts',(7.5330840646749,-0.452410699785362,-4.62961278943379));
#87884=CARTESIAN_POINT('Ctrl Pts',(7.36909481088169,-3.49281806885017,-2.56216828706881));
#87885=CARTESIAN_POINT('Ctrl Pts',(7.27138796333505,-3.92736124061847,-0.624189342625645));
#87886=CARTESIAN_POINT('Ctrl Pts',(7.23996352203496,-3.92656899063656,-0.000561720325250592));
#87887=CARTESIAN_POINT('',(5.98996351374692,-3.9329983211402,0.00363399344691532));
#87888=CARTESIAN_POINT('Ctrl Pts',(7.23996352203496,-3.92656899063656,-0.000561720325250592));
#87889=CARTESIAN_POINT('Ctrl Pts',(7.2051055570885,-3.92569017717304,0.691205225988917));
#87890=CARTESIAN_POINT('Ctrl Pts',(7.10396518589552,-3.42135043251264,2.69956464192561));
#87891=CARTESIAN_POINT('Ctrl Pts',(6.93654240845595,-0.212207213519058,
4.64682236801925));
#87892=CARTESIAN_POINT('Ctrl Pts',(6.7376951897163,3.79420578519414,2.69109503379691));
#87893=CARTESIAN_POINT('Ctrl Pts',(6.53884797097666,4.31533904892208,-1.73661708911133));
#87894=CARTESIAN_POINT('Ctrl Pts',(6.34000075223702,0.872490233572671,-4.56910831715266));
#87895=CARTESIAN_POINT('Ctrl Pts',(6.15703926925645,-3.03273667556589,-3.31352679892515));
#87896=CARTESIAN_POINT('Ctrl Pts',(6.04036019252243,-3.92357217526684,-0.992555741609356));
#87897=CARTESIAN_POINT('Ctrl Pts',(5.98996352203496,-3.93273349467542,0.00363358492567481));
#87898=CARTESIAN_POINT('',(4.73996306897106,-3.93526991228507,-0.00111206807604383));
#87899=CARTESIAN_POINT('Ctrl Pts',(5.98996351374692,-3.9329983211402,0.00363399344691532));
#87900=CARTESIAN_POINT('Ctrl Pts',(5.98202064724872,-3.93285324270482,0.160649478238822));
#87901=CARTESIAN_POINT('Ctrl Pts',(5.97407778075052,-3.9233014529818,0.317245508222898));
#87902=CARTESIAN_POINT('Ctrl Pts',(5.96613491425232,-3.90451705950222,0.472478075741249));
#87903=CARTESIAN_POINT('Ctrl Pts',(5.95819204775412,-3.88573266602263,0.627710643259604));
#87904=CARTESIAN_POINT('Ctrl Pts',(5.95024918125592,-3.85771583767056,0.781580297371852));
#87905=CARTESIAN_POINT('Ctrl Pts',(5.94230631475772,-3.82069139828797,0.933169994721377));
#87906=CARTESIAN_POINT('Ctrl Pts',(5.93643386862468,-3.79331790209118,1.04524569588167));
#87907=CARTESIAN_POINT('Ctrl Pts',(5.93056142249165,-3.76096297306108,1.15630355929294));
#87908=CARTESIAN_POINT('Ctrl Pts',(5.92468897635861,-3.72371717926471,1.26586704232668));
#87909=CARTESIAN_POINT('Ctrl Pts',(5.91882413741464,-3.68651963381137,1.37528859640749));
#87910=CARTESIAN_POINT('Ctrl Pts',(5.91295929847068,-3.64444395475189,1.4832192320268));
#87911=CARTESIAN_POINT('Ctrl Pts',(5.90709445952671,-3.59763143455672,1.58919383999855));
#87912=CARTESIAN_POINT('Ctrl Pts',(5.90123564940756,-3.55086703579952,1.6950595102224));
#87913=CARTESIAN_POINT('Ctrl Pts',(5.89537683928841,-3.49937564720674,1.79897277639081));
#87914=CARTESIAN_POINT('Ctrl Pts',(5.88951802916926,-3.44334773993833,1.9004855542365));
#87915=CARTESIAN_POINT('Ctrl Pts',(5.88343224028796,-3.38514923065708,2.00593108364589));
#87916=CARTESIAN_POINT('Ctrl Pts',(5.87734645140666,-3.32205573726382,2.10878593601703));
#87917=CARTESIAN_POINT('Ctrl Pts',(5.87126066252536,-3.25433504916551,2.20857247736472));
#87918=CARTESIAN_POINT('Ctrl Pts',(5.86540863244795,-3.18921555334596,2.30452615776302));
#87919=CARTESIAN_POINT('Ctrl Pts',(5.85955660237055,-3.11981802600965,2.39764251681994));
#87920=CARTESIAN_POINT('Ctrl Pts',(5.85370457229313,-3.04642596735118,2.48752443715604));
#87921=CARTESIAN_POINT('Ctrl Pts',(5.84785343191546,-2.97304506668316,2.57739269250401));
#87922=CARTESIAN_POINT('Ctrl Pts',(5.84200229153779,-2.89567110356855,2.66402716678029));
#87923=CARTESIAN_POINT('Ctrl Pts',(5.83615115116012,-2.81462842866851,2.74706312423487));
#87924=CARTESIAN_POINT('Ctrl Pts',(5.83029948359346,-2.73357845180618,2.83010656324692));
#87925=CARTESIAN_POINT('Ctrl Pts',(5.8244478160268,-2.64885939478492,2.90955054506941));
#87926=CARTESIAN_POINT('Ctrl Pts',(5.81859614846013,-2.56083258049191,2.98506708378407));
#87927=CARTESIAN_POINT('Ctrl Pts',(5.81274253677673,-2.47277652079121,3.06060871158074));
#87928=CARTESIAN_POINT('Ctrl Pts',(5.80688892509331,-2.38141083219527,3.13222003270251));
#87929=CARTESIAN_POINT('Ctrl Pts',(5.8010353134099,-2.28712945529186,3.19961370398621));
#87930=CARTESIAN_POINT('Ctrl Pts',(5.79517504731083,-2.19274089883748,3.26708398873976));
#87931=CARTESIAN_POINT('Ctrl Pts',(5.78931478121175,-2.0954303747829,3.33032681318384));
#87932=CARTESIAN_POINT('Ctrl Pts',(5.78345451511267,-1.99562038779009,3.38909844469536));
#87933=CARTESIAN_POINT('Ctrl Pts',(5.77759030194217,-1.89574317566776,3.44790966072803));
#87934=CARTESIAN_POINT('Ctrl Pts',(5.77172608877166,-1.7933635127187,3.50224349405051));
#87935=CARTESIAN_POINT('Ctrl Pts',(5.76586187560116,-1.68892647949197,3.55190320066171));
#87936=CARTESIAN_POINT('Ctrl Pts',(5.75998902702765,-1.58433565651648,3.60163603414722));
#87937=CARTESIAN_POINT('Ctrl Pts',(5.75411617845415,-1.47768179613982,3.64668084374541));
#87938=CARTESIAN_POINT('Ctrl Pts',(5.74824332988064,-1.36942789005103,3.68688978055357));
#87939=CARTESIAN_POINT('Ctrl Pts',(5.74664858525979,-1.34003204708651,3.69780832968393));
#87940=CARTESIAN_POINT('Ctrl Pts',(5.74505384063894,-1.31051829331303,3.70837058492205));
#87941=CARTESIAN_POINT('Ctrl Pts',(5.74345909601809,-1.28089604188996,3.71857423347587));
#87942=CARTESIAN_POINT('Ctrl Pts',(5.73758664988517,-1.17181583334536,3.75614788364412));
#87943=CARTESIAN_POINT('Ctrl Pts',(5.73171420375225,-1.06089832724938,3.78898075281574));
#87944=CARTESIAN_POINT('Ctrl Pts',(5.72584175761934,-0.948593366590205,
3.81689135617731));
#87945=CARTESIAN_POINT('Ctrl Pts',(5.7199769186755,-0.836433886204774,3.84476580403699));
#87946=CARTESIAN_POINT('Ctrl Pts',(5.71411207973167,-0.722890922930174,
3.86773056754548));
#87947=CARTESIAN_POINT('Ctrl Pts',(5.70824724078784,-0.608432129045196,
3.88565301388911));
#87948=CARTESIAN_POINT('Ctrl Pts',(5.70238843066883,-0.494090994319299,
3.90355703665956));
#87949=CARTESIAN_POINT('Ctrl Pts',(5.69652962054982,-0.378836307483879,
3.91642898857999));
#87950=CARTESIAN_POINT('Ctrl Pts',(5.69067081043082,-0.263147990725255,
3.92418681193662));
#87951=CARTESIAN_POINT('Ctrl Pts',(5.68458502154947,-0.142977741556796,
3.93224518457001));
#87952=CARTESIAN_POINT('Ctrl Pts',(5.67849923266812,-0.0223400249760971,
3.9347850473329));
#87953=CARTESIAN_POINT('Ctrl Pts',(5.67241344378677,0.098218572576491,3.93177340547507));
#87954=CARTESIAN_POINT('Ctrl Pts',(5.66656141370954,0.214146442027974,3.92887744258883));
#87955=CARTESIAN_POINT('Ctrl Pts',(5.6607093836323,0.330000706919892,3.92084859275499));
#87956=CARTESIAN_POINT('Ctrl Pts',(5.65485735355507,0.445294017114708,3.90771061343107));
#87957=CARTESIAN_POINT('Ctrl Pts',(5.6490062131776,0.560569798959709,3.89457463150924));
#87958=CARTESIAN_POINT('Ctrl Pts',(5.64315507280013,0.675284385091858,3.87633111132621));
#87959=CARTESIAN_POINT('Ctrl Pts',(5.63730393242266,0.788955576823385,3.85305568319474));
#87960=CARTESIAN_POINT('Ctrl Pts',(5.63145226485621,0.902637010353221,3.82977815794229));
#87961=CARTESIAN_POINT('Ctrl Pts',(5.62560059728976,1.01527445761994,3.80146790639584));
#87962=CARTESIAN_POINT('Ctrl Pts',(5.61974892972331,1.12639664296063,3.76825153124457));
#87963=CARTESIAN_POINT('Ctrl Pts',(5.61389531804012,1.23755574675206,3.73502412051919));
#87964=CARTESIAN_POINT('Ctrl Pts',(5.60804170635693,1.34719819176531,3.6968874634026));
#87965=CARTESIAN_POINT('Ctrl Pts',(5.60218809467374,1.45486925466066,3.65401757683829));
#87966=CARTESIAN_POINT('Ctrl Pts',(5.5963278285749,1.56266271857008,3.61109895556803));
#87967=CARTESIAN_POINT('Ctrl Pts',(5.59046756247606,1.6684799429835,3.56343651803073));
#87968=CARTESIAN_POINT('Ctrl Pts',(5.58460729637722,1.77188744524885,3.5112538901893));
#87969=CARTESIAN_POINT('Ctrl Pts',(5.57874308320696,1.87536459568188,3.45903611572568));
#87970=CARTESIAN_POINT('Ctrl Pts',(5.57287887003671,1.97642843265265,3.40229229064337));
#87971=CARTESIAN_POINT('Ctrl Pts',(5.56701465686646,2.07467279374348,3.34129043917176));
#87972=CARTESIAN_POINT('Ctrl Pts',(5.56114180829321,2.17306182550464,3.28019875884234));
#87973=CARTESIAN_POINT('Ctrl Pts',(5.55526895971995,2.26862275522921,3.21483677054345));
#87974=CARTESIAN_POINT('Ctrl Pts',(5.5493961111467,2.36098086675533,3.14551400359548));
#87975=CARTESIAN_POINT('Ctrl Pts',(5.54780136652395,2.38606028092498,3.12668972974507));
#87976=CARTESIAN_POINT('Ctrl Pts',(5.54620662190119,2.41090373307759,3.10757361651467));
#87977=CARTESIAN_POINT('Ctrl Pts',(5.54461187727843,2.43550418788018,3.08817233178754));
#87978=CARTESIAN_POINT('Ctrl Pts',(5.53873943113927,2.52609226309035,3.01672954529684));
#87979=CARTESIAN_POINT('Ctrl Pts',(5.5328669850001,2.61368579665593,2.94117781889425));
#87980=CARTESIAN_POINT('Ctrl Pts',(5.52699453886093,2.697888887224,2.86179743381555));
#87981=CARTESIAN_POINT('Ctrl Pts',(5.52112969991083,2.78198290078835,2.78251987838954));
#87982=CARTESIAN_POINT('Ctrl Pts',(5.51526486096071,2.86269490746571,2.69942380821862));
#87983=CARTESIAN_POINT('Ctrl Pts',(5.50940002201061,2.9396604709751,2.61283090064903));
#87984=CARTESIAN_POINT('Ctrl Pts',(5.50354121188531,3.01654691689862,2.52632700719807));
#87985=CARTESIAN_POINT('Ctrl Pts',(5.49768240176003,3.08969430693681,2.436333733331));
#87986=CARTESIAN_POINT('Ctrl Pts',(5.49182359163473,3.15877411456896,2.34321042442395));
#87987=CARTESIAN_POINT('Ctrl Pts',(5.48573780275574,3.23053017357422,2.24647938422938));
#87988=CARTESIAN_POINT('Ctrl Pts',(5.47965201387674,3.29789677730239,2.14637119149389));
#87989=CARTESIAN_POINT('Ctrl Pts',(5.47356622499774,3.36055062539171,2.04332779900322));
#87990=CARTESIAN_POINT('Ctrl Pts',(5.46771419491422,3.42079790165401,1.9442423649284));
#87991=CARTESIAN_POINT('Ctrl Pts',(5.46186216483071,3.47668754891229,1.84244344313218));
#87992=CARTESIAN_POINT('Ctrl Pts',(5.45601013474719,3.52797603694193,1.73835384279596));
#87993=CARTESIAN_POINT('Ctrl Pts',(5.45015899436344,3.57925672744571,1.63428006747979));
#87994=CARTESIAN_POINT('Ctrl Pts',(5.44430785397969,3.6259374669571,1.52791667676196));
#87995=CARTESIAN_POINT('Ctrl Pts',(5.43845671359594,3.66782114660131,1.41971019456234));
#87996=CARTESIAN_POINT('Ctrl Pts',(5.43260504602323,3.70970859997375,1.31149396293624));
#87997=CARTESIAN_POINT('Ctrl Pts',(5.42675337845052,3.74679798505335,1.20143469522053));
#87998=CARTESIAN_POINT('Ctrl Pts',(5.42090171087781,3.77894097757415,1.08999728807505));
#87999=CARTESIAN_POINT('Ctrl Pts',(5.41504809918838,3.81109464905581,0.978522857752298));
#88000=CARTESIAN_POINT('Ctrl Pts',(5.40919448749896,3.8382985457707,0.865669774521691));
#88001=CARTESIAN_POINT('Ctrl Pts',(5.40334087580953,3.86045486117469,0.751915729874504));
#88002=CARTESIAN_POINT('Ctrl Pts',(5.39748060970452,3.88263636399089,0.638032369049923));
#88003=CARTESIAN_POINT('Ctrl Pts',(5.39162034359951,3.89975875333545,0.523246408476939));
#88004=CARTESIAN_POINT('Ctrl Pts',(5.3857600774945,3.91177575685306,0.408043414475324));
#88005=CARTESIAN_POINT('Ctrl Pts',(5.3798958643181,3.92380085419607,0.292762827676268));
#88006=CARTESIAN_POINT('Ctrl Pts',(5.37403165114171,3.93071369410298,0.177065059762018));
#88007=CARTESIAN_POINT('Ctrl Pts',(5.36816743796531,3.93252012476649,0.0614367016249753));
#88008=CARTESIAN_POINT('Ctrl Pts',(5.36229458938602,3.93432921550666,-0.0543619261508433));
#88009=CARTESIAN_POINT('Ctrl Pts',(5.35642174080672,3.93101690137764,-0.170090528525728));
#88010=CARTESIAN_POINT('Ctrl Pts',(5.35054889222743,3.92264094833718,-0.285266525250295));
#88011=CARTESIAN_POINT('Ctrl Pts',(5.34895414766455,3.92036649746554,-0.31654202845293));
#88012=CARTESIAN_POINT('Ctrl Pts',(5.34735940310168,3.91771896165528,-0.34777683884738));
#88013=CARTESIAN_POINT('Ctrl Pts',(5.3457646585388,3.91470014591244,-0.378961432857152));
#88014=CARTESIAN_POINT('Ctrl Pts',(5.33989221241209,3.90358373690938,-0.493794775179618));
#88015=CARTESIAN_POINT('Ctrl Pts',(5.33401976628539,3.88739167171587,-0.608330828265449));
#88016=CARTESIAN_POINT('Ctrl Pts',(5.32814732015868,3.86614565748962,-0.722085005435037));
#88017=CARTESIAN_POINT('Ctrl Pts',(5.32228248122103,3.84492716543104,-0.835691825010722));
#88018=CARTESIAN_POINT('Ctrl Pts',(5.31641764228337,3.81866781899638,-0.948518380274054));
#88019=CARTESIAN_POINT('Ctrl Pts',(5.31055280334572,3.78744116160702,-1.06008416994352));
#88020=CARTESIAN_POINT('Ctrl Pts',(5.30469399323286,3.75624660399882,-1.17153527434944));
#88021=CARTESIAN_POINT('Ctrl Pts',(5.29883518312001,3.72009500269545,-1.28172779534265));
#88022=CARTESIAN_POINT('Ctrl Pts',(5.29297637300715,3.67911100457593,-1.39019107176254));
#88023=CARTESIAN_POINT('Ctrl Pts',(5.28689058412348,3.63653922713999,-1.50285637225994));
#88024=CARTESIAN_POINT('Ctrl Pts',(5.28080479523981,3.58875313545733,-1.61365528480874));
#88025=CARTESIAN_POINT('Ctrl Pts',(5.27471900635615,3.53594969233564,-1.72207687786333));
#88026=CARTESIAN_POINT('Ctrl Pts',(5.26886697628494,3.48517446123275,-1.82633393229826));
#88027=CARTESIAN_POINT('Ctrl Pts',(5.26301494621373,3.42976040546521,-1.92839252097583));
#88028=CARTESIAN_POINT('Ctrl Pts',(5.25716291614252,3.36993151659851,-2.02781916684798));
#88029=CARTESIAN_POINT('Ctrl Pts',(5.25131177577101,3.31011172367697,-2.12723069662262));
#88030=CARTESIAN_POINT('Ctrl Pts',(5.2454606353995,3.24587864528334,-2.22401072512109));
#88031=CARTESIAN_POINT('Ctrl Pts',(5.239609495028,3.17750132253168,-2.31775200254674));
#88032=CARTESIAN_POINT('Ctrl Pts',(5.23375782746744,3.1091178389681,-2.41150172608223));
#88033=CARTESIAN_POINT('Ctrl Pts',(5.22790615990689,3.0365896123767,-2.50221182029704));
#88034=CARTESIAN_POINT('Ctrl Pts',(5.22205449234634,2.96022751752167,-2.58950613911369));
#88035=CARTESIAN_POINT('Ctrl Pts',(5.21620088066899,2.88384005266226,-2.67682945997979));
#88036=CARTESIAN_POINT('Ctrl Pts',(5.21034726899164,2.80361645880228,-2.760734437947));
#88037=CARTESIAN_POINT('Ctrl Pts',(5.20449365731428,2.71990568928164,-2.84088050459948));
#88038=CARTESIAN_POINT('Ctrl Pts',(5.19863339122115,2.63609975692873,-2.92111768171171));
#88039=CARTESIAN_POINT('Ctrl Pts',(5.192773125128,2.54879903517819,-2.99758713241532));
#88040=CARTESIAN_POINT('Ctrl Pts',(5.18691285903486,2.45838696680936,-3.06998738131313));
#88041=CARTESIAN_POINT('Ctrl Pts',(5.18104864587024,2.36791400310042,-3.14243639403043));
#88042=CARTESIAN_POINT('Ctrl Pts',(5.17518443270562,2.27432585298839,-3.21081050433854));
#88043=CARTESIAN_POINT('Ctrl Pts',(5.16932021954099,2.17803500324615,-3.27485152711303));
#88044=CARTESIAN_POINT('Ctrl Pts',(5.16344737097323,2.08160235949294,-3.3389868541076));
#88045=CARTESIAN_POINT('Ctrl Pts',(5.15757452240548,1.98245942568906,-3.39877614624009));
#88046=CARTESIAN_POINT('Ctrl Pts',(5.15170167383772,1.88104338728578,-3.45400706066858));
#88047=CARTESIAN_POINT('Ctrl Pts',(5.1501069291582,1.85350433433802,-3.46900475827881));
#88048=CARTESIAN_POINT('Ctrl Pts',(5.14851218447868,1.8257977816723,-3.4836666104459));
#88049=CARTESIAN_POINT('Ctrl Pts',(5.14691743979915,1.79793271659332,-3.4979889860609));
#88050=CARTESIAN_POINT('Ctrl Pts',(5.14104499366954,1.69532312919306,-3.55072932771384));
#88051=CARTESIAN_POINT('Ctrl Pts',(5.13517254753993,1.59021916487394,-3.59903923479842));
#88052=CARTESIAN_POINT('Ctrl Pts',(5.12930010141032,1.48304019955298,-3.64267494658937));
#88053=CARTESIAN_POINT('Ctrl Pts',(5.12343526246986,1.37600007427319,-3.68625413251255));
#88054=CARTESIAN_POINT('Ctrl Pts',(5.1175704235294,1.266890672711,-3.72517100989488));
#88055=CARTESIAN_POINT('Ctrl Pts',(5.11170558458894,1.15615596250871,-3.75922763215472));
#88056=CARTESIAN_POINT('Ctrl Pts',(5.10584677447338,1.04553508325471,-3.79324924553974));
#88057=CARTESIAN_POINT('Ctrl Pts',(5.09998796435781,0.933292611302778,-3.82242042064039));
#88058=CARTESIAN_POINT('Ctrl Pts',(5.09412915424225,0.819891868860637,-3.84659152021321));
#88059=CARTESIAN_POINT('Ctrl Pts',(5.08804336535964,0.702097817846483,-3.87169904309917));
#88060=CARTESIAN_POINT('Ctrl Pts',(5.08195757647703,0.583054355908134,-3.89141106328964));
#88061=CARTESIAN_POINT('Ctrl Pts',(5.07587178759441,0.463297783022315,-3.90561700173565));
#88062=CARTESIAN_POINT('Ctrl Pts',(5.07001975752076,0.348141132082977,-3.91927728154721));
#88063=CARTESIAN_POINT('Ctrl Pts',(5.0641677274471,0.23232559014042,-3.92784660775168));
#88064=CARTESIAN_POINT('Ctrl Pts',(5.05831569737345,0.116336916484687,-3.9312790185718));
#88065=CARTESIAN_POINT('Ctrl Pts',(5.0524645569996,0.000365876897616496,
-3.93471090755331));
#88066=CARTESIAN_POINT('Ctrl Pts',(5.04661341662574,-0.115777829003163,
-3.93300742176772));
#88067=CARTESIAN_POINT('Ctrl Pts',(5.04076227625189,-0.231606145773011,
-3.92617467686299));
#88068=CARTESIAN_POINT('Ctrl Pts',(5.03491060868909,-0.347444898697882,
-3.91934131632654));
#88069=CARTESIAN_POINT('Ctrl Pts',(5.0290589411263,-0.462967793337763,-3.90737780230802));
#88070=CARTESIAN_POINT('Ctrl Pts',(5.0232072735635,-0.577690319090831,-3.89034225939425));
#88071=CARTESIAN_POINT('Ctrl Pts',(5.01735366188401,-0.692450959445473,
-3.87330105671203));
#88072=CARTESIAN_POINT('Ctrl Pts',(5.01150005020452,-0.806410293512435,
-3.85118453510873));
#88073=CARTESIAN_POINT('Ctrl Pts',(5.00564643852502,-0.919093149460135,
-3.82410208841441));
#88074=CARTESIAN_POINT('Ctrl Pts',(4.99978617242991,-1.03190410385344,-3.7969888542565));
#88075=CARTESIAN_POINT('Ctrl Pts',(4.99392590633479,-1.14343528161755,-3.7648985238529));
#88076=CARTESIAN_POINT('Ctrl Pts',(4.98806564023968,-1.25322574752353,-3.72799064185307));
#88077=CARTESIAN_POINT('Ctrl Pts',(4.98220142707317,-1.3630901607212,-3.69105790124742));
#88078=CARTESIAN_POINT('Ctrl Pts',(4.97633721390667,-1.47121114287337,-3.64930129660987));
#88079=CARTESIAN_POINT('Ctrl Pts',(4.97047300074017,-1.5771484705297,-3.60292821214992));
#88080=CARTESIAN_POINT('Ctrl Pts',(4.96460015217067,-1.68324179720764,-3.55648684056243));
#88081=CARTESIAN_POINT('Ctrl Pts',(4.95872730360118,-1.78714468219978,-3.50541560327032));
#88082=CARTESIAN_POINT('Ctrl Pts',(4.95285445503169,-1.88844211016409,-3.4499674486231));
#88083=CARTESIAN_POINT('Ctrl Pts',(4.9512597103743,-1.91594895460962,-3.43491076065655));
#88084=CARTESIAN_POINT('Ctrl Pts',(4.9496649657169,-1.94326385169254,-3.41953157537305));
#88085=CARTESIAN_POINT('Ctrl Pts',(4.94807022105951,-1.97037888736429,-3.40383548959539));
#88086=CARTESIAN_POINT('Ctrl Pts',(4.94219777489032,-2.07022658813591,-3.34603663234931));
#88087=CARTESIAN_POINT('Ctrl Pts',(4.93632532872113,-2.16769610294611,-3.28374390161609));
#88088=CARTESIAN_POINT('Ctrl Pts',(4.93045288255193,-2.26235561724438,-3.2171782762419));
#88089=CARTESIAN_POINT('Ctrl Pts',(4.92458804357171,-2.35689250924991,-3.15069888023051));
#88090=CARTESIAN_POINT('Ctrl Pts',(4.91872320459149,-2.44862630457141,-3.07995783255189));
#88091=CARTESIAN_POINT('Ctrl Pts',(4.91285836561127,-2.53715043092722,-3.00522157100701));
#88092=CARTESIAN_POINT('Ctrl Pts',(4.9069995554558,-2.62558355794854,-2.93056213541165));
#88093=CARTESIAN_POINT('Ctrl Pts',(4.90114074530033,-2.71081326476782,-2.85191591989841));
#88094=CARTESIAN_POINT('Ctrl Pts',(4.89528193514485,-2.79246315213798,-2.76959176485481));
#88095=CARTESIAN_POINT('Ctrl Pts',(4.88919614627715,-2.8772762733044,-2.68407825391778));
#88096=CARTESIAN_POINT('Ctrl Pts',(4.88311035740944,-2.9582262187963,-2.59459632385733));
#88097=CARTESIAN_POINT('Ctrl Pts',(4.87702456854174,-3.0349299856515,-2.5015373237658));
#88098=CARTESIAN_POINT('Ctrl Pts',(4.87117253842811,-3.10868751540201,-2.41205277497225));
#88099=CARTESIAN_POINT('Ctrl Pts',(4.86532050831447,-3.17851875865221,-2.31926123041867));
#88100=CARTESIAN_POINT('Ctrl Pts',(4.85946847820085,-3.24412239692127,-2.22354646315156));
#88101=CARTESIAN_POINT('Ctrl Pts',(4.85361733778706,-3.3097160612932,-2.12784624765729));
#88102=CARTESIAN_POINT('Ctrl Pts',(4.84776619737327,-3.37108316501876,-2.02922403397522));
#88103=CARTESIAN_POINT('Ctrl Pts',(4.84191505695948,-3.4279649560572,-1.9280936854945));
#88104=CARTESIAN_POINT('Ctrl Pts',(4.83606338935682,-3.4848518721558,-1.82695422515019));
#88105=CARTESIAN_POINT('Ctrl Pts',(4.83021172175417,-3.53725246954495,-1.72330654107269));
#88106=CARTESIAN_POINT('Ctrl Pts',(4.82436005415152,-3.5849536632997,-1.61758963646349));
#88107=CARTESIAN_POINT('Ctrl Pts',(4.81850644243229,-3.63267070496106,-1.51183760921898));
#88108=CARTESIAN_POINT('Ctrl Pts',(4.81265283071305,-3.67568506852689,-1.40401537104218));
#88109=CARTESIAN_POINT('Ctrl Pts',(4.80679921899382,-3.71383184678538,-1.29458179108261));
#88110=CARTESIAN_POINT('Ctrl Pts',(4.80093895285935,-3.75202199049317,-1.18502380647921));
#88111=CARTESIAN_POINT('Ctrl Pts',(4.7950786867249,-3.78533336808122,-1.07385121447151));
#88112=CARTESIAN_POINT('Ctrl Pts',(4.78921842059044,-3.81365095753085,-0.961538025313615));
#88113=CARTESIAN_POINT('Ctrl Pts',(4.78335420738475,-3.84198761975633,-0.849149189735145));
#88114=CARTESIAN_POINT('Ctrl Pts',(4.77748999417906,-3.86532371347404,-0.735618631212591));
#88115=CARTESIAN_POINT('Ctrl Pts',(4.77162578097338,-3.88359565880033,-0.62142880440744));
#88116=CARTESIAN_POINT('Ctrl Pts',(4.76575293236526,-3.90189451065192,-0.507070826296558));
#88117=CARTESIAN_POINT('Ctrl Pts',(4.75988008375715,-3.91511428388645,-0.392052051464341));
#88118=CARTESIAN_POINT('Ctrl Pts',(4.75400723514904,-3.9232433578633,-0.276858366284093));
#88119=CARTESIAN_POINT('Ctrl Pts',(4.75241249087265,-3.92545076947256,-0.245578065636703));
#88120=CARTESIAN_POINT('Ctrl Pts',(4.75081774659625,-3.92728310573871,-0.214284855227092));
#88121=CARTESIAN_POINT('Ctrl Pts',(4.74922300231986,-3.92874079555149,-0.182988418675829));
#88122=CARTESIAN_POINT('Ctrl Pts',(4.74613650889156,-3.93156203159178,-0.122416797774472));
#88123=CARTESIAN_POINT('Ctrl Pts',(4.74305001546326,-3.93298256131418,-0.0617794293185965));
#88124=CARTESIAN_POINT('Ctrl Pts',(4.73996352203496,-3.93299984043219,-0.00112033939962684));
#88125=CARTESIAN_POINT('',(3.48996393051077,-3.93195649834994,-0.00308191760686356));
#88126=CARTESIAN_POINT('Ctrl Pts',(4.73996229954107,-3.9391251331115,-0.00109802104096923));
#88127=CARTESIAN_POINT('Ctrl Pts',(4.67676679422078,-3.93442811003921,1.24282384787021));
#88128=CARTESIAN_POINT('Ctrl Pts',(4.54728888265397,-2.62580980838282,3.79991380728597));
#88129=CARTESIAN_POINT('Ctrl Pts',(4.35152856484057,1.7326990630354,4.31691369475902));
#88130=CARTESIAN_POINT('Ctrl Pts',(4.15268134610093,4.56831442476183,0.876637571345176));
#88131=CARTESIAN_POINT('Ctrl Pts',(3.95383412736129,3.20756968977473,-3.36889996732418));
#88132=CARTESIAN_POINT('Ctrl Pts',(3.75498690862166,-1.0995828420239,-4.51983480521305));
#88133=CARTESIAN_POINT('Ctrl Pts',(3.60036385291742,-3.66339751277891,-2.18634896287544));
#88134=CARTESIAN_POINT('Ctrl Pts',(3.51202320345975,-3.93249893558521,-0.440083035469798));
#88135=CARTESIAN_POINT('Ctrl Pts',(3.48996496024862,-3.9293289361394,-0.00310026290872592));
#88136=CARTESIAN_POINT('',(2.23996299489525,-3.93122786339409,0.00239984451894347));
#88137=CARTESIAN_POINT('Ctrl Pts',(3.48996352203496,-3.93299879819285,-0.00307464040323634));
#88138=CARTESIAN_POINT('Ctrl Pts',(3.48411632698161,-3.93308943701494,0.112868146911366));
#88139=CARTESIAN_POINT('Ctrl Pts',(3.47826913192826,-3.92804887411316,0.22887230601759));
#88140=CARTESIAN_POINT('Ctrl Pts',(3.47242193687491,-3.91788758060137,0.344450149904952));
#88141=CARTESIAN_POINT('Ctrl Pts',(3.46657571648118,-3.90772798085939,0.46000872830586));
#88142=CARTESIAN_POINT('Ctrl Pts',(3.46072949608744,-3.89244938353798,0.575140720950829));
#88143=CARTESIAN_POINT('Ctrl Pts',(3.45488327569371,-3.87211425780453,0.689362150474535));
#88144=CARTESIAN_POINT('Ctrl Pts',(3.44903661305097,-3.85177759377994,0.803592220506071));
#88145=CARTESIAN_POINT('Ctrl Pts',(3.44318995040824,-3.82638371318358,0.91691118327512));
#88146=CARTESIAN_POINT('Ctrl Pts',(3.4373432877655,-3.79604634517697,1.02884456808043));
#88147=CARTESIAN_POINT('Ctrl Pts',(3.43149476598082,-3.76569933038948,1.14081354584936));
#88148=CARTESIAN_POINT('Ctrl Pts',(3.42564624419614,-3.73040581037212,1.25139567053234));
#88149=CARTESIAN_POINT('Ctrl Pts',(3.41979772241146,-3.6903293742723,1.3601316514893));
#88150=CARTESIAN_POINT('Ctrl Pts',(3.41394225952107,-3.65020537490952,1.46899668179694));
#88151=CARTESIAN_POINT('Ctrl Pts',(3.40808679663068,-3.60528726960042,1.57601080554061));
#88152=CARTESIAN_POINT('Ctrl Pts',(3.40223133374028,-3.55578687625916,1.68073456875947));
#88153=CARTESIAN_POINT('Ctrl Pts',(3.39637201236529,-3.50625386440274,1.78552734019076));
#88154=CARTESIAN_POINT('Ctrl Pts',(3.3905126909903,-3.45213274449892,1.88802638072238));
#88155=CARTESIAN_POINT('Ctrl Pts',(3.38465336961531,-3.39368049041652,1.98781833399491));
#88156=CARTESIAN_POINT('Ctrl Pts',(3.37878453779344,-3.33513336066125,2.08777226269272));
#88157=CARTESIAN_POINT('Ctrl Pts',(3.37291570597156,-3.2722412835245,2.18500998390483));
#88158=CARTESIAN_POINT('Ctrl Pts',(3.36704687414968,-3.20530376084862,2.27914826211234));
#88159=CARTESIAN_POINT('Ctrl Pts',(3.36379540648058,-3.16821883535809,2.33130303112039));
#88160=CARTESIAN_POINT('Ctrl Pts',(3.36054393881147,-3.12989290496863,2.38250705129076));
#88161=CARTESIAN_POINT('Ctrl Pts',(3.35729247114236,-3.09038186934412,2.432699920177));
#88162=CARTESIAN_POINT('Ctrl Pts',(3.35142002361739,-3.01902133097346,2.52335282485225));
#88163=CARTESIAN_POINT('Ctrl Pts',(3.34554757609242,-2.94354913470549,2.61101491801737));
#88164=CARTESIAN_POINT('Ctrl Pts',(3.33967512856745,-2.86424520234117,2.6952900439221));
#88165=CARTESIAN_POINT('Ctrl Pts',(3.33381028825484,-2.78504400088289,2.77945599919956));
#88166=CARTESIAN_POINT('Ctrl Pts',(3.32794544794224,-2.70202121494443,2.8602434141433));
#88167=CARTESIAN_POINT('Ctrl Pts',(3.32208060762963,-2.61549819098514,2.9372875604805));
#88168=CARTESIAN_POINT('Ctrl Pts',(3.31622179616635,-2.52906410964768,3.01425250814827));
#88169=CARTESIAN_POINT('Ctrl Pts',(3.31036298470306,-2.43913725400455,3.08748156775208));
#88170=CARTESIAN_POINT('Ctrl Pts',(3.30450417323977,-2.3460766711313,3.15664588656591));
#88171=CARTESIAN_POINT('Ctrl Pts',(3.29841838487156,-2.2494108172567,3.22848970840077));
#88172=CARTESIAN_POINT('Ctrl Pts',(3.29233259650335,-2.14936382859677,3.29594714366392));
#88173=CARTESIAN_POINT('Ctrl Pts',(3.28624680813514,-2.04637736394949,3.35869449106571));
#88174=CARTESIAN_POINT('Ctrl Pts',(3.28039477678235,-1.94734664129446,3.41903169342689));
#88175=CARTESIAN_POINT('Ctrl Pts',(3.27454274542955,-1.84559847528112,3.47501373042732));
#88176=CARTESIAN_POINT('Ctrl Pts',(3.26869071407675,-1.74155545392517,3.52639668796684));
#88177=CARTESIAN_POINT('Ctrl Pts',(3.26283957245104,-1.63752825098992,3.57777183337991));
#88178=CARTESIAN_POINT('Ctrl Pts',(3.25698843082532,-1.53120725696807,3.62454910664573));
#88179=CARTESIAN_POINT('Ctrl Pts',(3.25113728919961,-1.42303881675763,3.66653099345976));
#88180=CARTESIAN_POINT('Ctrl Pts',(3.24528562041344,-1.31486063107721,3.70851666264523));
#88181=CARTESIAN_POINT('Ctrl Pts',(3.23943395162726,-1.20483505370261,3.74570593694982));
#88182=CARTESIAN_POINT('Ctrl Pts',(3.23358228284108,-1.09342684656628,3.77795006997288));
#88183=CARTESIAN_POINT('Ctrl Pts',(3.22772866996789,-0.98198162652704,3.81020491539313));
#88184=CARTESIAN_POINT('Ctrl Pts',(3.22187505709471,-0.869153260191447,
3.83751123784089));
#88185=CARTESIAN_POINT('Ctrl Pts',(3.21602144422152,-0.75541935019651,3.85977079699672));
#88186=CARTESIAN_POINT('Ctrl Pts',(3.21016117698241,-0.641556147904519,
3.88205566073879));
#88187=CARTESIAN_POINT('Ctrl Pts',(3.2043009097433,-0.52678575316777,3.89928223060361));
#88188=CARTESIAN_POINT('Ctrl Pts',(3.1984406425042,-0.411593690247987,3.91140379328804));
#88189=CARTESIAN_POINT('Ctrl Pts',(3.19257642822118,-0.296324042448196,
3.92353352016331));
#88190=CARTESIAN_POINT('Ctrl Pts',(3.18671221393815,-0.180632572544359,
3.9305513684321));
#88191=CARTESIAN_POINT('Ctrl Pts',(3.18084799965514,-0.0650058767105533,
3.93246274438717));
#88192=CARTESIAN_POINT('Ctrl Pts',(3.17497515001786,0.0507910853228681,
3.9343769349407));
#88193=CARTESIAN_POINT('Ctrl Pts',(3.1691023003806,0.166522671277312,3.93116965708302));
#88194=CARTESIAN_POINT('Ctrl Pts',(3.16322945074332,0.281706248466385,3.92289823849345));
#88195=CARTESIAN_POINT('Ctrl Pts',(3.16163471796312,0.312983573381783,3.92065219046255));
#88196=CARTESIAN_POINT('Ctrl Pts',(3.16003998518292,0.344220544794587,3.91803302618818));
#88197=CARTESIAN_POINT('Ctrl Pts',(3.15844525240272,0.375407637705265,3.91504254198502));
#88198=CARTESIAN_POINT('Ctrl Pts',(3.15257279710596,0.490251209761825,3.90403036175223));
#88199=CARTESIAN_POINT('Ctrl Pts',(3.14670034180919,0.604802094702504,3.88794224156575));
#88200=CARTESIAN_POINT('Ctrl Pts',(3.14082788651243,0.718575685062651,3.86679944978231));
#88201=CARTESIAN_POINT('Ctrl Pts',(3.13496303835688,0.832201893838007,3.84568404623677));
#88202=CARTESIAN_POINT('Ctrl Pts',(3.12909819020133,0.945052407752413,3.81952706714544));
#88203=CARTESIAN_POINT('Ctrl Pts',(3.12323334204578,1.05664665780864,3.78840162080815));
#88204=CARTESIAN_POINT('Ctrl Pts',(3.11737452267839,1.1681261942224,3.75730816996633));
#88205=CARTESIAN_POINT('Ctrl Pts',(3.11151570331101,1.27835163963612,3.72125652106592));
#88206=CARTESIAN_POINT('Ctrl Pts',(3.10565688394362,1.386852218885,3.68037089475691));
#88207=CARTESIAN_POINT('Ctrl Pts',(3.09957109851527,1.4995560253613,3.63790139139486));
#88208=CARTESIAN_POINT('Ctrl Pts',(3.09348531308692,1.61039817633966,3.59021589026558));
#88209=CARTESIAN_POINT('Ctrl Pts',(3.08739952765856,1.71886756388629,3.53751089013442));
#88210=CARTESIAN_POINT('Ctrl Pts',(3.08154748829966,1.82317080175622,3.48683021155815));
#88211=CARTESIAN_POINT('Ctrl Pts',(3.07569544894075,1.92527977674601,3.43150870229928));
#88212=CARTESIAN_POINT('Ctrl Pts',(3.06984340958185,2.0247608077048,3.37176996124923));
#88213=CARTESIAN_POINT('Ctrl Pts',(3.06399225992613,2.1242267142625,3.31204030246009));
#88214=CARTESIAN_POINT('Ctrl Pts',(3.05814111027041,2.22106511691968,3.2478949599131));
#88215=CARTESIAN_POINT('Ctrl Pts',(3.0522899606147,2.31486852090247,3.1796026058196));
#88216=CARTESIAN_POINT('Ctrl Pts',(3.04643828378327,2.4086803763656,3.11130409873524));
#88217=CARTESIAN_POINT('Ctrl Pts',(3.04058660695183,2.49945635537347,3.03885808065493));
#88218=CARTESIAN_POINT('Ctrl Pts',(3.0347349301204,2.58682002889609,2.96257508564797));
#88219=CARTESIAN_POINT('Ctrl Pts',(3.02888130919533,2.67421272711832,2.88626674725826));
#88220=CARTESIAN_POINT('Ctrl Pts',(3.02302768827026,2.75819055443164,2.80611916890222));
#88221=CARTESIAN_POINT('Ctrl Pts',(3.01717406734519,2.83841262488372,2.72248099550772));
#88222=CARTESIAN_POINT('Ctrl Pts',(3.01131379208539,2.91872589094215,2.63874774311696));
#88223=CARTESIAN_POINT('Ctrl Pts',(3.00545351682559,2.99527459205026,2.55151627404036));
#88224=CARTESIAN_POINT('Ctrl Pts',(2.99959324156578,3.06775690394131,2.46116975812731));
#88225=CARTESIAN_POINT('Ctrl Pts',(2.99372901927034,3.14028803440413,2.37076239167353));
#88226=CARTESIAN_POINT('Ctrl Pts',(2.9878647969749,3.20874707857506,2.27723613345821));
#88227=CARTESIAN_POINT('Ctrl Pts',(2.98200057467946,3.27287547605126,2.18100323664643));
#88228=CARTESIAN_POINT('Ctrl Pts',(2.97612771710436,3.33709830491464,2.08462863340981));
#88229=CARTESIAN_POINT('Ctrl Pts',(2.97025485952926,3.39697754681083,1.98553978951168));
#88230=CARTESIAN_POINT('Ctrl Pts',(2.96438200195416,3.45230046115742,1.88417369843979));
#88231=CARTESIAN_POINT('Ctrl Pts',(2.96278734585713,3.46732228342025,1.8566497796162));
#88232=CARTESIAN_POINT('Ctrl Pts',(2.9611926897601,3.48200844963443,1.82895807502124));
#88233=CARTESIAN_POINT('Ctrl Pts',(2.95959803366308,3.49635532112986,1.80110756713943));
#88234=CARTESIAN_POINT('Ctrl Pts',(2.95372561157408,3.54918858419822,1.69854630770556));
#88235=CARTESIAN_POINT('Ctrl Pts',(2.94785318948509,3.59759371831676,1.59348666178647));
#88236=CARTESIAN_POINT('Ctrl Pts',(2.9419807673961,3.64132658202465,1.48634777997637));
#88237=CARTESIAN_POINT('Ctrl Pts',(2.93611595250998,3.68500279367965,1.37934768710173));
#88238=CARTESIAN_POINT('Ctrl Pts',(2.93025113762386,3.7240186164411,1.27027409385835));
#88239=CARTESIAN_POINT('Ctrl Pts',(2.92438632273774,3.75817570053078,1.15957078435943));
#88240=CARTESIAN_POINT('Ctrl Pts',(2.91852753666256,3.79229767241213,1.04898127373329));
#88241=CARTESIAN_POINT('Ctrl Pts',(2.91266875058738,3.82157071901731,0.936765771704727));
#88242=CARTESIAN_POINT('Ctrl Pts',(2.9068099645122,3.84584478224221,0.823387460980775));
#88243=CARTESIAN_POINT('Ctrl Pts',(2.90072416661267,3.87105939856231,0.705616052978784));
#88244=CARTESIAN_POINT('Ctrl Pts',(2.89463836871314,3.89087962997266,0.586590322926661));
#88245=CARTESIAN_POINT('Ctrl Pts',(2.88855257081361,3.90519440852007,0.466846475475124));
#88246=CARTESIAN_POINT('Ctrl Pts',(2.88270056459753,3.91895927130785,0.35170270120082));
#88247=CARTESIAN_POINT('Ctrl Pts',(2.87684855838146,3.92763381818308,0.235895414327885));
#88248=CARTESIAN_POINT('Ctrl Pts',(2.87099655216538,3.93117164634012,0.119910329044353));
#88249=CARTESIAN_POINT('Ctrl Pts',(2.86514543554189,3.9347089366943,0.00394287523073171));
#88250=CARTESIAN_POINT('Ctrl Pts',(2.85929431891841,3.93311104833125,-0.112201910197163));
#88251=CARTESIAN_POINT('Ctrl Pts',(2.85344320229492,3.92638365376652,-0.228035969608107));
#88252=CARTESIAN_POINT('Ctrl Pts',(2.84759155835066,3.91965565290812,-0.343880468343655));
#88253=CARTESIAN_POINT('Ctrl Pts',(2.84173991440638,3.90779725083232,-0.45941377270361));
#88254=CARTESIAN_POINT('Ctrl Pts',(2.83588827046212,3.89086613218934,-0.574151322720711));
#88255=CARTESIAN_POINT('Ctrl Pts',(2.83003468224454,3.87392938799522,-0.688926995555842));
#88256=CARTESIAN_POINT('Ctrl Pts',(2.82418109402696,3.85191663609957,-0.802905979592701));
#88257=CARTESIAN_POINT('Ctrl Pts',(2.81832750580938,3.82493683883739,-0.915613007173139));
#88258=CARTESIAN_POINT('Ctrl Pts',(2.81246726282683,3.79792636907092,-1.02844816791758));
#88259=CARTESIAN_POINT('Ctrl Pts',(2.80660701984427,3.76593767924005,-1.14000808370118));
#88260=CARTESIAN_POINT('Ctrl Pts',(2.80074677686172,3.72912989537711,-1.24983167802897));
#88261=CARTESIAN_POINT('Ctrl Pts',(2.79488258663309,3.69229731913259,-1.35972924552687));
#88262=CARTESIAN_POINT('Ctrl Pts',(2.78901839640448,3.65063933369313,-1.46788777801986));
#88263=CARTESIAN_POINT('Ctrl Pts',(2.78315420617585,3.60436292335855,-1.57386686753301));
#88264=CARTESIAN_POINT('Ctrl Pts',(2.77728138011082,3.55801836456807,-1.68000202600781));
#88265=CARTESIAN_POINT('Ctrl Pts',(2.77140855404578,3.5070419882155,-1.78395096617584));
#88266=CARTESIAN_POINT('Ctrl Pts',(2.76553572798075,3.45168636551509,-1.88529844696197));
#88267=CARTESIAN_POINT('Ctrl Pts',(2.76394075696164,3.43665261294448,-1.91282289480423));
#88268=CARTESIAN_POINT('Ctrl Pts',(2.76234578594253,3.42129609739214,-1.94015563395403));
#88269=CARTESIAN_POINT('Ctrl Pts',(2.76075081492342,3.40562241094693,-1.96728874191259));
#88270=CARTESIAN_POINT('Ctrl Pts',(2.75487835257712,3.34791406867954,-2.0671890867564));
#88271=CARTESIAN_POINT('Ctrl Pts',(2.74900589023081,3.28570967715722,-2.16471531238949));
#88272=CARTESIAN_POINT('Ctrl Pts',(2.7431334278845,3.21922982444765,-2.25943540234873));
#88273=CARTESIAN_POINT('Ctrl Pts',(2.73726857287381,3.15283609141345,-2.35403278951807));
#88274=CARTESIAN_POINT('Ctrl Pts',(2.73140371786311,3.08217814665517,-2.44583093479365));
#88275=CARTESIAN_POINT('Ctrl Pts',(2.72553886285242,3.00752206006605,-2.53442302274424));
#88276=CARTESIAN_POINT('Ctrl Pts',(2.71968003682938,2.93294271887362,-2.62292403928668));
#88277=CARTESIAN_POINT('Ctrl Pts',(2.71382121080633,2.85437367569844,-2.70822523980445));
#88278=CARTESIAN_POINT('Ctrl Pts',(2.70796238478329,2.77212343038123,-2.78994994340963));
#88279=CARTESIAN_POINT('Ctrl Pts',(2.70187660192498,2.68668700829345,-2.87484046556288));
#88280=CARTESIAN_POINT('Ctrl Pts',(2.69579081906666,2.5972786756073,-2.9558714255448));
#88281=CARTESIAN_POINT('Ctrl Pts',(2.68970503620834,2.50428943062393,-3.03265946780466));
#88282=CARTESIAN_POINT('Ctrl Pts',(2.68385299072671,2.41487163448912,-3.10649830271091));
#88283=CARTESIAN_POINT('Ctrl Pts',(2.67800094524509,2.32214326583393,-3.17641383745267));
#88284=CARTESIAN_POINT('Ctrl Pts',(2.67214889976346,2.2264878251748,-3.24210440367801));
#88285=CARTESIAN_POINT('Ctrl Pts',(2.66629774419067,2.13084693064702,-3.30778498047047));
#88286=CARTESIAN_POINT('Ctrl Pts',(2.66044658861787,2.03228018979642,-3.36924163227354));
#88287=CARTESIAN_POINT('Ctrl Pts',(2.65459543304507,1.93120123218828,-3.42621522978263));
#88288=CARTESIAN_POINT('Ctrl Pts',(2.64874375050741,1.83011317123999,-3.4831939584293));
#88289=CARTESIAN_POINT('Ctrl Pts',(2.64289206796976,1.72651280387504,-3.5356886271821));
#88290=CARTESIAN_POINT('Ctrl Pts',(2.6370403854321,1.62083894102801,-3.58348575094798));
#88291=CARTESIAN_POINT('Ctrl Pts',(2.63118675901707,1.51512997425494,-3.63129875249718));
#88292=CARTESIAN_POINT('Ctrl Pts',(2.62533313260203,1.40734651879081,-3.67441093587548));
#88293=CARTESIAN_POINT('Ctrl Pts',(2.61947950618699,1.29794729539229,-3.71265697558822));
#88294=CARTESIAN_POINT('Ctrl Pts',(2.61361922578293,1.18842371468409,-3.75094649069737));
#88295=CARTESIAN_POINT('Ctrl Pts',(2.60775894537886,1.0772810904951,-3.78435868498092));
#88296=CARTESIAN_POINT('Ctrl Pts',(2.60189866497479,0.964993330107935,-3.81277810432855));
#88297=CARTESIAN_POINT('Ctrl Pts',(2.59603443772972,0.852629945022748,-3.84121666387453));
#88298=CARTESIAN_POINT('Ctrl Pts',(2.59017021048466,0.739120291873598,-3.8646556695139));
#88299=CARTESIAN_POINT('Ctrl Pts',(2.58430598323959,0.624946769273544,-3.88303110154613));
#88300=CARTESIAN_POINT('Ctrl Pts',(2.57843312103693,0.510605128439833,-3.90143359103534));
#88301=CARTESIAN_POINT('Ctrl Pts',(2.57256025883427,0.395598076254214,-3.91475757881186));
#88302=CARTESIAN_POINT('Ctrl Pts',(2.56668739663161,0.280411490422355,-3.9229910012692));
#88303=CARTESIAN_POINT('Ctrl Pts',(2.56509279648233,0.249136016790644,-3.9252265409816));
#88304=CARTESIAN_POINT('Ctrl Pts',(2.56349819633306,0.217847295216401,-3.92708708476973));
#88305=CARTESIAN_POINT('Ctrl Pts',(2.56190359618379,0.186555007060496,-3.9285730525651));
#88306=CARTESIAN_POINT('Ctrl Pts',(2.55603109559877,0.0713135902165479,
-3.93404548824221));
#88307=CARTESIAN_POINT('Ctrl Pts',(2.55015859501375,-0.0443617374728357,
-3.93445201940534));
#88308=CARTESIAN_POINT('Ctrl Pts',(2.54428609442874,-0.159988279027446,
-3.92974461645714));
#88309=CARTESIAN_POINT('Ctrl Pts',(2.5384212006791,-0.275465045872865,-3.92504331115656));
#88310=CARTESIAN_POINT('Ctrl Pts',(2.53255630692948,-0.390892743054991,
-3.91524126166845));
#88311=CARTESIAN_POINT('Ctrl Pts',(2.52669141317984,-0.505785281191382,
-3.90034232463385));
#88312=CARTESIAN_POINT('Ctrl Pts',(2.52083254796891,-0.620559721005375,
-3.88545870225325));
#88313=CARTESIAN_POINT('Ctrl Pts',(2.51497368275798,-0.734799688480384,
-3.86548866603212));
#88314=CARTESIAN_POINT('Ctrl Pts',(2.50911481754705,-0.848021502043583,
-3.84048805909766));
#88315=CARTESIAN_POINT('Ctrl Pts',(2.50302904920943,-0.965628189226883,
-3.81451922441289));
#88316=CARTESIAN_POINT('Ctrl Pts',(2.49694328087181,-1.08213581160459,-3.78312230989147));
#88317=CARTESIAN_POINT('Ctrl Pts',(2.49085751253419,-1.1970104796669,-3.74641894501504));
#88318=CARTESIAN_POINT('Ctrl Pts',(2.48500542699977,-1.30747416246644,-3.7111249248122));
#88319=CARTESIAN_POINT('Ctrl Pts',(2.47915334146535,-1.41642755348199,-3.67092459374291));
#88320=CARTESIAN_POINT('Ctrl Pts',(2.47330125593093,-1.52340951961511,-3.62597744553742));
#88321=CARTESIAN_POINT('Ctrl Pts',(2.46745006005592,-1.63037522188609,-3.58103713039219));
#88322=CARTESIAN_POINT('Ctrl Pts',(2.46159886418091,-1.73536971420839,-3.53135159301352));
#88323=CARTESIAN_POINT('Ctrl Pts',(2.4557476683059,-1.83795135695881,-3.47712867312288));
#88324=CARTESIAN_POINT('Ctrl Pts',(2.4498959452606,-1.94054224192142,-3.42290086795532));
#88325=CARTESIAN_POINT('Ctrl Pts',(2.4440442222153,-2.04071947970455,-3.36413506079299));
#88326=CARTESIAN_POINT('Ctrl Pts',(2.43819249917,-2.13806621141756,-3.30108495431344));
#88327=CARTESIAN_POINT('Ctrl Pts',(2.43233883208575,-2.23544528332108,-3.23801390154818));
#88328=CARTESIAN_POINT('Ctrl Pts',(2.4264851650015,-2.32999163259134,-3.17065594387585));
#88329=CARTESIAN_POINT('Ctrl Pts',(2.42063149791725,-2.42131814732685,-3.09930757257579));
#88330=CARTESIAN_POINT('Ctrl Pts',(2.41477117681327,-2.51274847535099,-3.02787809767637));
#88331=CARTESIAN_POINT('Ctrl Pts',(2.4089108557093,-2.60095133753657,-2.95244941004886));
#88332=CARTESIAN_POINT('Ctrl Pts',(2.40305053460533,-2.68557336280993,-2.87335774190506));
#88333=CARTESIAN_POINT('Ctrl Pts',(2.39718626659246,-2.77025238076647,-2.79421280575722));
#88334=CARTESIAN_POINT('Ctrl Pts',(2.3913219985796,-2.85134547116981,-2.71140027139316));
#88335=CARTESIAN_POINT('Ctrl Pts',(2.38545773056673,-2.92853793868478,-2.62529132510734));
#88336=CARTESIAN_POINT('Ctrl Pts',(2.3795848278157,-3.00584406688915,-2.53905558921999));
#88337=CARTESIAN_POINT('Ctrl Pts',(2.37371192506467,-3.07923784846847,-2.44951407278266));
#88338=CARTESIAN_POINT('Ctrl Pts',(2.36783902231364,-3.14844641281899,-2.35706898193651));
#88339=CARTESIAN_POINT('Ctrl Pts',(2.36624480735714,-3.16723326032574,-2.33197451796702));
#88340=CARTESIAN_POINT('Ctrl Pts',(2.36465059240064,-3.18571196968848,-2.30666624977724));
#88341=CARTESIAN_POINT('Ctrl Pts',(2.36305637744414,-3.20387766288088,-2.28115254231122));
#88342=CARTESIAN_POINT('Ctrl Pts',(2.35712726773537,-3.27143843154284,-2.18626347479458));
#88343=CARTESIAN_POINT('Ctrl Pts',(2.3511981580266,-3.33489067772598,-2.0882153493576));
#88344=CARTESIAN_POINT('Ctrl Pts',(2.34526904831783,-3.39392837568789,-1.98739507413613));
#88345=CARTESIAN_POINT('Ctrl Pts',(2.33934793526716,-3.45288644883106,-1.88671077637341));
#88346=CARTESIAN_POINT('Ctrl Pts',(2.33342682221649,-3.5074416140155,-1.78326210911534));
#88347=CARTESIAN_POINT('Ctrl Pts',(2.32750570916582,-3.55732956871809,-1.67746694141017));
#88348=CARTESIAN_POINT('Ctrl Pts',(2.32159124251937,-3.60716152457223,-1.57179052797339));
#88349=CARTESIAN_POINT('Ctrl Pts',(2.31567677587291,-3.65233652121262,-1.46377321579088));
#88350=CARTESIAN_POINT('Ctrl Pts',(2.30976230922646,-3.69263517094391,-1.35385911169075));
#88351=CARTESIAN_POINT('Ctrl Pts',(2.30385383432241,-3.73289299550144,-1.24405635778293));
#88352=CARTESIAN_POINT('Ctrl Pts',(2.29794535941836,-3.76828417076304,-1.1323610144258));
#88353=CARTESIAN_POINT('Ctrl Pts',(2.29203688451431,-3.79863692299823,-1.01923820926933));
#88354=CARTESIAN_POINT('Ctrl Pts',(2.28613199697543,-3.82897124638201,-0.906184087286985));
#88355=CARTESIAN_POINT('Ctrl Pts',(2.28022710943655,-3.85427312892714,-0.791704615900504));
#88356=CARTESIAN_POINT('Ctrl Pts',(2.27432222189767,-3.87442036676633,-0.676280874774886));
#88357=CARTESIAN_POINT('Ctrl Pts',(2.26841882637633,-3.89456251390191,-0.560886298344636));
#88358=CARTESIAN_POINT('Ctrl Pts',(2.26251543085498,-3.9095525322712,-0.444548322261923));
#88359=CARTESIAN_POINT('Ctrl Pts',(2.25661203533364,-3.9193192342614,-0.32775866113442));
#88360=CARTESIAN_POINT('Ctrl Pts',(2.25106253090075,-3.92850045137508,-0.217970194513854));
#88361=CARTESIAN_POINT('Ctrl Pts',(2.24551302646786,-3.93306623672388,-0.107782941556682));
#88362=CARTESIAN_POINT('Ctrl Pts',(2.23996352203497,-3.93299927353876,0.00239046931868954));
#88363=CARTESIAN_POINT('Ctrl Pts',(2.23996202763734,-3.92797747181863,0.00241704723849157));
#88364=CARTESIAN_POINT('Ctrl Pts',(2.21471107132639,-3.93073062284058,0.50308190472603));
#88365=CARTESIAN_POINT('Ctrl Pts',(2.12317770876889,-3.60912558829099,2.31455042910235));
#88366=CARTESIAN_POINT('Ctrl Pts',(1.96536193996485,-0.880790531217901,
4.56748308540991));
#88367=CARTESIAN_POINT('Ctrl Pts',(1.76651472122522,3.36599905195296,3.21069095555329));
#88368=CARTESIAN_POINT('Ctrl Pts',(1.56766750248557,4.52080778991678,-1.09560268340907));
#88369=CARTESIAN_POINT('Ctrl Pts',(1.36882028374592,1.52297741527043,-4.39506475690675));
#88370=CARTESIAN_POINT('Ctrl Pts',(1.1762528813402,-2.73512533544538,-3.68141236753163));
#88371=CARTESIAN_POINT('Ctrl Pts',(1.04996788518101,-3.93019899042183,-1.17946347387552));
#88372=CARTESIAN_POINT('Ctrl Pts',(0.989965295268386,-3.93800215978868,
0.00238238590750563));
#88373=CARTESIAN_POINT('Origin',(-1.72497344927317,0.,0.));
#88374=CARTESIAN_POINT('',(48.9000264684934,-3.22327929659544,-0.000763835567893241));
#88375=CARTESIAN_POINT('Ctrl Pts',(48.4702430335869,1.79020435040156,2.68143717906899));
#88376=CARTESIAN_POINT('Ctrl Pts',(48.4828219278093,1.62211098738932,2.7961192948877));
#88377=CARTESIAN_POINT('Ctrl Pts',(48.5616832282783,0.502078434973499,3.41252236229075));
#88378=CARTESIAN_POINT('Ctrl Pts',(48.7049441319495,-2.11679622861173,3.15040696403668));
#88379=CARTESIAN_POINT('Ctrl Pts',(48.8356261413985,-3.22539994567256,1.0376522699003));
#88380=CARTESIAN_POINT('Ctrl Pts',(48.9000257446008,-3.22793943922082,-0.00075326948836482));
#88381=CARTESIAN_POINT('',(49.2909945592456,1.2393601841108,-2.97491241829753));
#88382=CARTESIAN_POINT('Ctrl Pts',(48.9000265507268,-3.22274990919558,-0.000765035863639074));
#88383=CARTESIAN_POINT('Ctrl Pts',(48.9019090850623,-3.22274271499011,-0.0310709680741342));
#88384=CARTESIAN_POINT('Ctrl Pts',(48.9037916193978,-3.22230804770656,-0.0613722117935458));
#88385=CARTESIAN_POINT('Ctrl Pts',(48.9056741537333,-3.22144623788179,-0.091660781893286));
#88386=CARTESIAN_POINT('Ctrl Pts',(48.9118583995395,-3.21861513743701,-0.191160673651801));
#88387=CARTESIAN_POINT('Ctrl Pts',(48.9180426453456,-3.21116499472643,-0.290701504167739));
#88388=CARTESIAN_POINT('Ctrl Pts',(48.9242268911518,-3.19908700253732,-0.389820359520634));
#88389=CARTESIAN_POINT('Ctrl Pts',(48.9304027454209,-3.18702539923738,-0.488804718352069));
#88390=CARTESIAN_POINT('Ctrl Pts',(48.93657859969,-3.17034848093281,-0.587367814511488));
#88391=CARTESIAN_POINT('Ctrl Pts',(48.9427544539591,-3.14909943357514,-0.685047677141335));
#88392=CARTESIAN_POINT('Ctrl Pts',(48.9489237340616,-3.12787300572422,-0.782623560036202));
#88393=CARTESIAN_POINT('Ctrl Pts',(48.9550930141641,-3.10208421720153,-0.879317658376768));
#88394=CARTESIAN_POINT('Ctrl Pts',(48.9612622942666,-3.07182782715444,-0.974675003690801));
#88395=CARTESIAN_POINT('Ctrl Pts',(48.9674269579693,-3.0415940776085,-1.06996099422378));
#88396=CARTESIAN_POINT('Ctrl Pts',(48.973591621672,-3.00689950462653,-1.16391180970599));
#88397=CARTESIAN_POINT('Ctrl Pts',(48.9797562853747,-2.96788931441195,-1.25608541902984));
#88398=CARTESIAN_POINT('Ctrl Pts',(48.9859185412005,-2.92889436131994,-1.34822302595085));
#88399=CARTESIAN_POINT('Ctrl Pts',(48.9920807970262,-2.88558730919526,-1.43858440828709));
#88400=CARTESIAN_POINT('Ctrl Pts',(48.998243052852,-2.8381620212258,-1.52674618184277));
#88401=CARTESIAN_POINT('Ctrl Pts',(49.0044045333619,-2.79074270015833,-1.61489686315875));
#88402=CARTESIAN_POINT('Ctrl Pts',(49.0105660138719,-2.73920637843116,-1.70084810504075));
#88403=CARTESIAN_POINT('Ctrl Pts',(49.0167274943819,-2.68379307216665,-1.78420074775522));
#88404=CARTESIAN_POINT('Ctrl Pts',(49.0228898310577,-2.62837206596986,-1.86756497270053));
#88405=CARTESIAN_POINT('Ctrl Pts',(49.0290521677335,-2.5690732447375,-1.94832952103033));
#88406=CARTESIAN_POINT('Ctrl Pts',(49.0352145044093,-2.50617962029353,-2.02612469342964));
#88407=CARTESIAN_POINT('Ctrl Pts',(49.0413831875777,-2.44322122270653,-2.10399998583911));
#88408=CARTESIAN_POINT('Ctrl Pts',(49.047551870746,-2.3766609011367,-2.1788994583169));
#88409=CARTESIAN_POINT('Ctrl Pts',(49.0537205539143,-2.30682151610866,-2.25048707068451));
#88410=CARTESIAN_POINT('Ctrl Pts',(49.0598925621146,-2.23694448638683,-2.32211327007212));
#88411=CARTESIAN_POINT('Ctrl Pts',(49.0660645703149,-2.16378518883442,-2.39042375825355));
#88412=CARTESIAN_POINT('Ctrl Pts',(49.0722365785152,-2.08770134427464,-2.45512131260634));
#88413=CARTESIAN_POINT('Ctrl Pts',(49.0784185897541,-2.01149418982764,-2.51992372296603));
#88414=CARTESIAN_POINT('Ctrl Pts',(49.084600600993,-1.93235336273051,-2.58110123805993));
#88415=CARTESIAN_POINT('Ctrl Pts',(49.0907826122319,-1.85066756157063,-2.63839859366439));
#88416=CARTESIAN_POINT('Ctrl Pts',(49.095362198979,-1.79015534346653,-2.68084403742443));
#88417=CARTESIAN_POINT('Ctrl Pts',(49.099941785726,-1.72824714873466,-2.72116104277473));
#88418=CARTESIAN_POINT('Ctrl Pts',(49.104521372473,-1.66510947631706,-2.75926221921352));
#88419=CARTESIAN_POINT('Ctrl Pts',(49.1106420329124,-1.58072538771954,-2.81018479721126));
#88420=CARTESIAN_POINT('Ctrl Pts',(49.1167626933517,-1.49384475876965,-2.85732827472905));
#88421=CARTESIAN_POINT('Ctrl Pts',(49.1228833537911,-1.40484385906841,-2.90043639718884));
#88422=CARTESIAN_POINT('Ctrl Pts',(49.1289958344773,-1.3159619016606,-2.94348690923157));
#88423=CARTESIAN_POINT('Ctrl Pts',(49.1351083151635,-1.22496569788788,-2.98251259017556));
#88424=CARTESIAN_POINT('Ctrl Pts',(49.1412207958498,-1.13225917457918,-3.01730123190928));
#88425=CARTESIAN_POINT('Ctrl Pts',(49.1474613693246,-1.03760989877726,-3.05281890238933));
#88426=CARTESIAN_POINT('Ctrl Pts',(49.1537019427994,-0.941178201573555,
-3.08391968990434));
#88427=CARTESIAN_POINT('Ctrl Pts',(49.1599425162742,-0.843419239519438,
-3.11042787232054));
#88428=CARTESIAN_POINT('Ctrl Pts',(49.1660444940328,-0.747831387769098,
-3.13634733952568));
#88429=CARTESIAN_POINT('Ctrl Pts',(49.1721464717913,-0.650975063991087,
-3.15787595500614));
#88430=CARTESIAN_POINT('Ctrl Pts',(49.1782484495498,-0.553293273769149,
-3.17489907173469));
#88431=CARTESIAN_POINT('Ctrl Pts',(49.1843484520425,-0.455643104031581,
-3.19191667792546));
#88432=CARTESIAN_POINT('Ctrl Pts',(49.1904484545353,-0.357168434074009,
-3.2044316067882));
#88433=CARTESIAN_POINT('Ctrl Pts',(49.1965484570281,-0.258322749635708,
-3.21238025761594));
#88434=CARTESIAN_POINT('Ctrl Pts',(49.2026481837623,-0.159481533645042,
-3.22032854911459));
#88435=CARTESIAN_POINT('Ctrl Pts',(49.2087479104966,-0.0602697775203343,
-3.22371093833049));
#88436=CARTESIAN_POINT('Ctrl Pts',(49.2148476372308,0.0388547353954878,
-3.22251576753898));
#88437=CARTESIAN_POINT('Ctrl Pts',(49.2211932140654,0.141974471787196,-3.22127242526835));
#88438=CARTESIAN_POINT('Ctrl Pts',(49.2275387908999,0.244999266023637,-3.21507473082441));
#88439=CARTESIAN_POINT('Ctrl Pts',(49.2338843677345,0.347416415296945,-3.20396931896706));
#88440=CARTESIAN_POINT('Ctrl Pts',(49.2399921014271,0.445994793531956,-3.19328015706109));
#88441=CARTESIAN_POINT('Ctrl Pts',(49.2460998351197,0.54400982278241,-3.17804471411179));
#88442=CARTESIAN_POINT('Ctrl Pts',(49.2522075688123,0.641013560227601,-3.15835703778157));
#88443=CARTESIAN_POINT('Ctrl Pts',(49.2583193274449,0.738081222237557,-3.13865638745494));
#88444=CARTESIAN_POINT('Ctrl Pts',(49.2644310860774,0.834135838720248,-3.11449777424306));
#88445=CARTESIAN_POINT('Ctrl Pts',(49.27054284471,0.928744167988292,-3.08602524826479));
#88446=CARTESIAN_POINT('Ctrl Pts',(49.2766633536017,1.02348794884321,-3.05751195791772));
#88447=CARTESIAN_POINT('Ctrl Pts',(49.2827838624935,1.11678089806089,-3.02467258443918));
#88448=CARTESIAN_POINT('Ctrl Pts',(49.2889043713853,1.20820971163147,-2.9876992578269));
#88449=CARTESIAN_POINT('Ctrl Pts',(49.289601100672,1.21861752790873,-2.98349039220225));
#88450=CARTESIAN_POINT('Ctrl Pts',(49.2902978299588,1.22900121482326,-2.97922800554118));
#88451=CARTESIAN_POINT('Ctrl Pts',(49.2909945592456,1.2393601841108,-2.97491241829753));
#88452=CARTESIAN_POINT('',(49.291,-2.41015873594064,-2.13945143204257));
#88453=CARTESIAN_POINT('Origin',(49.291,0.,0.));
#88454=CARTESIAN_POINT('',(49.1465717854694,-3.2227472468638,0.00421252083431657));
#88455=CARTESIAN_POINT('Ctrl Pts',(49.1474903455921,-3.22274716839108,0.00427213380650271));
#88456=CARTESIAN_POINT('Ctrl Pts',(49.1650705708236,-3.22309010045641,-0.254423729326887));
#88457=CARTESIAN_POINT('Ctrl Pts',(49.1822124068069,-3.19228378391878,-0.512269410551018));
#88458=CARTESIAN_POINT('Ctrl Pts',(49.1994094148614,-3.12714433700966,-0.779323094869068));
#88459=CARTESIAN_POINT('Ctrl Pts',(49.2004120277926,-3.12321643923212,-0.794918409833965));
#88460=CARTESIAN_POINT('Ctrl Pts',(49.2020467655877,-3.11659923137243,-0.820384935923119));
#88461=CARTESIAN_POINT('Ctrl Pts',(49.2026809294181,-3.11397939742035,-0.830273766931297));
#88462=CARTESIAN_POINT('Ctrl Pts',(49.2039110190088,-3.10879509514848,-0.849472700089948));
#88463=CARTESIAN_POINT('Ctrl Pts',(49.2045070891921,-3.10623578217984,-0.858784070798633));
#88464=CARTESIAN_POINT('Ctrl Pts',(49.2055926166077,-3.10148899624475,-0.875755114408501));
#88465=CARTESIAN_POINT('Ctrl Pts',(49.2060824606648,-3.09931490863572,-0.883418424629367));
#88466=CARTESIAN_POINT('Ctrl Pts',(49.2071415003678,-3.09454510556339,-0.899996870650155));
#88467=CARTESIAN_POINT('Ctrl Pts',(49.2077103950552,-3.09193922404829,-0.908909024532861));
#88468=CARTESIAN_POINT('Ctrl Pts',(49.2092569826489,-3.08473624647955,-0.933153829996632));
#88469=CARTESIAN_POINT('Ctrl Pts',(49.2102324709514,-3.08006334185425,-0.948463812509861));
#88470=CARTESIAN_POINT('Ctrl Pts',(49.2150163898034,-3.05651090350066,-1.02361932162588));
#88471=CARTESIAN_POINT('Ctrl Pts',(49.2187774945533,-3.03599960184945,-1.08294160467731));
#88472=CARTESIAN_POINT('Ctrl Pts',(49.2329378837279,-2.95137927520276,-1.30632930034826));
#88473=CARTESIAN_POINT('Ctrl Pts',(49.2430150479392,-2.87559309043842,-1.46564180250813));
#88474=CARTESIAN_POINT('Ctrl Pts',(49.2635841370677,-2.69537914954554,-1.77608354902012));
#88475=CARTESIAN_POINT('Ctrl Pts',(49.2740464936761,-2.59031496761603,-1.92608320209543));
#88476=CARTESIAN_POINT('Ctrl Pts',(49.2862759598952,-2.4607104270521,-2.08120065731826));
#88477=CARTESIAN_POINT('Ctrl Pts',(49.2874531705541,-2.44817050077093,-2.09593729593858));
#88478=CARTESIAN_POINT('Ctrl Pts',(49.2890902648496,-2.43065694474039,-2.1161472168388));
#88479=CARTESIAN_POINT('Ctrl Pts',(49.2895439284707,-2.42579581533941,-2.12171790930695));
#88480=CARTESIAN_POINT('Ctrl Pts',(49.2901723486313,-2.4190520374575,-2.12939258317444));
#88481=CARTESIAN_POINT('Ctrl Pts',(49.2903461654365,-2.41718569210517,-2.13151093428477));
#88482=CARTESIAN_POINT('Ctrl Pts',(49.29067995891,-2.41359963194504,-2.13557044011824));
#88483=CARTESIAN_POINT('Ctrl Pts',(49.2908399100741,-2.41188035194401,-2.13751197794312));
#88484=CARTESIAN_POINT('Ctrl Pts',(49.291,-2.4101587359407,-2.1394514320425));
#88485=CARTESIAN_POINT('Ctrl Pts',(48.7170675950372,1.78943621037805,2.68030513402632));
#88486=CARTESIAN_POINT('Ctrl Pts',(48.7232382856736,1.70649272707747,2.73568019955477));
#88487=CARTESIAN_POINT('Ctrl Pts',(48.72940897631,1.62086774339839,2.78727412820618));
#88488=CARTESIAN_POINT('Ctrl Pts',(48.7355796669464,1.53294127050646,2.83482073924931));
#88489=CARTESIAN_POINT('Ctrl Pts',(48.7417443526567,1.44510036210128,2.88232108093538));
#88490=CARTESIAN_POINT('Ctrl Pts',(48.7479090383669,1.35496279683326,2.92578173148518));
#88491=CARTESIAN_POINT('Ctrl Pts',(48.7540737240772,1.26293658646254,2.96498039472007));
#88492=CARTESIAN_POINT('Ctrl Pts',(48.7602345908057,1.17096738571528,3.00415477464455));
#88493=CARTESIAN_POINT('Ctrl Pts',(48.7663954575343,1.0771122630716,3.0390722466243));
#88494=CARTESIAN_POINT('Ctrl Pts',(48.7725563242629,0.981802016714291,3.06955735611436));
#88495=CARTESIAN_POINT('Ctrl Pts',(48.7787153068185,0.886520919013163,3.10003314236783));
#88496=CARTESIAN_POINT('Ctrl Pts',(48.7848742893742,0.789785994042781,3.12607912820188));
#88497=CARTESIAN_POINT('Ctrl Pts',(48.7910332719298,0.692045250913403,3.1475690513773));
#88498=CARTESIAN_POINT('Ctrl Pts',(48.7971920049047,0.594308468537029,3.1690581037155));
#88499=CARTESIAN_POINT('Ctrl Pts',(48.8033507378796,0.495566372007346,3.18599136788259));
#88500=CARTESIAN_POINT('Ctrl Pts',(48.8095094708544,0.396278299924899,3.19829346238094));
#88501=CARTESIAN_POINT('Ctrl Pts',(48.8156695881842,0.296967909951592,3.21059832213393));
#88502=CARTESIAN_POINT('Ctrl Pts',(48.821829705514,0.197111730224007,3.21826989073169));
#88503=CARTESIAN_POINT('Ctrl Pts',(48.8279898228438,0.0971743868641642,
3.22128463520962));
#88504=CARTESIAN_POINT('Ctrl Pts',(48.8341567551182,-0.00287351728887686,
3.22430271490269));
#88505=CARTESIAN_POINT('Ctrl Pts',(48.8403236873926,-0.103002330928318,
3.22265367266331));
#88506=CARTESIAN_POINT('Ctrl Pts',(48.846490619667,-0.202747397780817,3.21636612579991));
#88507=CARTESIAN_POINT('Ctrl Pts',(48.8526613491965,-0.302553882116546,
3.21007470741367));
#88508=CARTESIAN_POINT('Ctrl Pts',(48.8588320787259,-0.40197571916703,3.19913914457342));
#88509=CARTESIAN_POINT('Ctrl Pts',(48.8650028082554,-0.500555384876538,
3.18363972037841));
#88510=CARTESIAN_POINT('Ctrl Pts',(48.8711834038326,-0.599292664314238,
3.16811551498725));
#88511=CARTESIAN_POINT('Ctrl Pts',(48.8773639994097,-0.697184660345036,
3.14801296595449));
#88512=CARTESIAN_POINT('Ctrl Pts',(48.8835445949869,-0.793786020148058,
3.12346303271185));
#88513=CARTESIAN_POINT('Ctrl Pts',(48.8867982508315,-0.844639950807991,
3.11053919183246));
#88514=CARTESIAN_POINT('Ctrl Pts',(48.8900519066761,-0.895136486724309,
3.09638367876077));
#88515=CARTESIAN_POINT('Ctrl Pts',(48.8933055625207,-0.945212836742466,
3.0810209761956));
#88516=CARTESIAN_POINT('Ctrl Pts',(48.8994111530019,-1.03918272802978,3.05219236769266));
#88517=CARTESIAN_POINT('Ctrl Pts',(48.9055167434831,-1.13201835900593,3.01900355677363));
#88518=CARTESIAN_POINT('Ctrl Pts',(48.9116223339642,-1.22327913816598,2.98156095235833));
#88519=CARTESIAN_POINT('Ctrl Pts',(48.9177195243747,-1.31441436075667,2.94416986147383));
#88520=CARTESIAN_POINT('Ctrl Pts',(48.9238167147852,-1.40397862858924,2.9025367696119));
#88521=CARTESIAN_POINT('Ctrl Pts',(48.9299139051958,-1.4915453703454,2.85681815499363));
#88522=CARTESIAN_POINT('Ctrl Pts',(48.9360046026441,-1.579018861358,2.81114822660854));
#88523=CARTESIAN_POINT('Ctrl Pts',(48.9420953000925,-1.66449866145113,2.7614016246746));
#88524=CARTESIAN_POINT('Ctrl Pts',(48.9481859975408,-1.74757812433479,2.70778290522828));
#88525=CARTESIAN_POINT('Ctrl Pts',(48.9542724982055,-1.83060034147023,2.65420113166013));
#88526=CARTESIAN_POINT('Ctrl Pts',(48.9603589988702,-1.91122513459973,2.59675278074639));
#88527=CARTESIAN_POINT('Ctrl Pts',(48.9664454995349,-1.9890713277967,2.5356878387209));
#88528=CARTESIAN_POINT('Ctrl Pts',(48.9725298594353,-2.06689014067044,2.4746443746609));
#88529=CARTESIAN_POINT('Ctrl Pts',(48.9786142193356,-2.14193194468348,2.40998711920826));
#88530=CARTESIAN_POINT('Ctrl Pts',(48.9846985792359,-2.21384626928613,2.34200816789095));
#88531=CARTESIAN_POINT('Ctrl Pts',(48.9907825096814,-2.28575551793002,2.2740340147603));
#88532=CARTESIAN_POINT('Ctrl Pts',(48.9968664401268,-2.35453740258873,2.20273893687918));
#88533=CARTESIAN_POINT('Ctrl Pts',(49.0029503705722,-2.41987700851893,2.12845315338193));
#88534=CARTESIAN_POINT('Ctrl Pts',(49.0090355821478,-2.48523037340599,2.05415172707698));
#88535=CARTESIAN_POINT('Ctrl Pts',(49.0151207937233,-2.54713972663897,1.97685867842956));
#88536=CARTESIAN_POINT('Ctrl Pts',(49.0212060052988,-2.60533002987135,1.89693779496075));
#88537=CARTESIAN_POINT('Ctrl Pts',(49.0272986882685,-2.66359177888423,1.81691878500727));
#88538=CARTESIAN_POINT('Ctrl Pts',(49.0333913712382,-2.71812509887946,1.73426585845953));
#88539=CARTESIAN_POINT('Ctrl Pts',(49.0394840542079,-2.76869805694995,1.64937219327281));
#88540=CARTESIAN_POINT('Ctrl Pts',(49.0455805507553,-2.81930267002543,1.56442539080686));
#88541=CARTESIAN_POINT('Ctrl Pts',(49.0516770473028,-2.86594177980861,1.47723545091154));
#88542=CARTESIAN_POINT('Ctrl Pts',(49.0577735438503,-2.90843033892423,1.38821847204433));
#88543=CARTESIAN_POINT('Ctrl Pts',(49.0638816534136,-2.95099983309956,1.29903192765996));
#88544=CARTESIAN_POINT('Ctrl Pts',(49.069989762977,-2.98940281426851,1.20801180324768));
#88545=CARTESIAN_POINT('Ctrl Pts',(49.0760978725403,-3.02350306175496,1.11559257709002));
#88546=CARTESIAN_POINT('Ctrl Pts',(49.0814495087804,-3.05338008317195,1.03461922930564));
#88547=CARTESIAN_POINT('Ctrl Pts',(49.0868011450204,-3.07995486263722,0.952572294301333));
#88548=CARTESIAN_POINT('Ctrl Pts',(49.0921527812604,-3.10316810876065,0.869750108520173));
#88549=CARTESIAN_POINT('Ctrl Pts',(49.100662198562,-3.14007853939013,0.738057947647774));
#88550=CARTESIAN_POINT('Ctrl Pts',(49.1091716158637,-3.1686037383271,0.604007833156265));
#88551=CARTESIAN_POINT('Ctrl Pts',(49.1176810331654,-3.18851392237117,0.468504567048382));
#88552=CARTESIAN_POINT('Ctrl Pts',(49.1259255518801,-3.2078043013882,0.337219524404909));
#88553=CARTESIAN_POINT('Ctrl Pts',(49.1341700705947,-3.21900782770081,0.204569851518107));
#88554=CARTESIAN_POINT('Ctrl Pts',(49.1424145893094,-3.22195894791002,0.0714009837645678));
#88555=CARTESIAN_POINT('Ctrl Pts',(49.1438003213627,-3.22245496981362,0.0490180679220658));
#88556=CARTESIAN_POINT('Ctrl Pts',(49.1451860534161,-3.22271795685899,0.0266205482591167));
#88557=CARTESIAN_POINT('Ctrl Pts',(49.1465717854694,-3.2227472468638,0.00421252083431657));
#88558=CARTESIAN_POINT('Origin',(0.,0.,0.));
#88559=CARTESIAN_POINT('',(0.,-1.2491397351303E-16,1.02));
#88560=CARTESIAN_POINT('Origin',(0.,0.,0.));
#88561=CARTESIAN_POINT('',(2.448,-1.2491397351303E-16,1.02));
#88562=CARTESIAN_POINT('',(0.,-1.2491397351303E-16,1.02));
#88563=CARTESIAN_POINT('Origin',(2.448,0.,0.));
#88564=CARTESIAN_POINT('Origin',(2.448,0.,0.));
#88565=CARTESIAN_POINT('Origin',(49.291,5.160062080289E-16,2.1385152528819E-16));
#88566=CARTESIAN_POINT('',(49.291,-0.996446678860641,3.80467909503385));
#88567=CARTESIAN_POINT('',(49.291,-3.933,4.81653586104654E-16));
#88568=CARTESIAN_POINT('Origin',(49.291,0.,0.));
#88569=CARTESIAN_POINT('Ctrl Pts',(49.2910000000001,-0.996446678860644,
3.80467909503386));
#88570=CARTESIAN_POINT('Ctrl Pts',(49.2910000000001,-1.04787446395986,3.78642472561806));
#88571=CARTESIAN_POINT('Ctrl Pts',(49.2910000000001,-1.09885704840169,3.76701980464874));
#88572=CARTESIAN_POINT('Ctrl Pts',(49.2910000000001,-1.14935789175992,3.74645332354063));
#88573=CARTESIAN_POINT('Ctrl Pts',(49.2910000000001,-1.26368142516242,3.69989503592438));
#88574=CARTESIAN_POINT('Ctrl Pts',(49.2910000000001,-1.37553846253051,3.64738695884623));
#88575=CARTESIAN_POINT('Ctrl Pts',(49.2910000000001,-1.48464424221647,3.58930502949026));
#88576=CARTESIAN_POINT('Ctrl Pts',(49.2910000000001,-1.59375002190243,3.53122310013429));
#88577=CARTESIAN_POINT('Ctrl Pts',(49.2910000000001,-1.70010512777846,3.46756648039375));
#88578=CARTESIAN_POINT('Ctrl Pts',(49.2910000000001,-1.80338619496161,3.3986729028763));
#88579=CARTESIAN_POINT('Ctrl Pts',(49.2910000000001,-1.82145558081485,3.38661972925091));
#88580=CARTESIAN_POINT('Ctrl Pts',(49.2910000000001,-1.83943154385614,3.3744055478693));
#88581=CARTESIAN_POINT('Ctrl Pts',(49.2910000000001,-1.85729837010941,3.36204194363082));
#88582=CARTESIAN_POINT('Ctrl Pts',(49.2910000000001,-1.95673406302392,3.29323377720289));
#88583=CARTESIAN_POINT('Ctrl Pts',(49.2910000000001,-2.05289507009515,3.21973309797708));
#88584=CARTESIAN_POINT('Ctrl Pts',(49.2910000000001,-2.14551174396067,3.14189100840979));
#88585=CARTESIAN_POINT('Ctrl Pts',(49.2910000000001,-2.23824482167426,3.06395108420442));
#88586=CARTESIAN_POINT('Ctrl Pts',(49.2910000000001,-2.32742518903523,2.98165804209933));
#88587=CARTESIAN_POINT('Ctrl Pts',(49.2910000000001,-2.41274059201778,2.89533360211057));
#88588=CARTESIAN_POINT('Ctrl Pts',(49.2910000000001,-2.43810143532588,2.8696728126203));
#88589=CARTESIAN_POINT('Ctrl Pts',(49.2910000000001,-2.46312044856481,2.84365563256905));
#88590=CARTESIAN_POINT('Ctrl Pts',(49.2910000000001,-2.4877886142742,2.81729014790106));
#88591=CARTESIAN_POINT('Ctrl Pts',(49.2910000000001,-2.50844926697038,2.79520791737331));
#88592=CARTESIAN_POINT('Ctrl Pts',(49.2910000000001,-2.52886359911005,2.77288158200795));
#88593=CARTESIAN_POINT('Ctrl Pts',(49.2910000000001,-2.54902671268354,2.75031513412511));
#88594=CARTESIAN_POINT('Ctrl Pts',(49.2910000000001,-2.56454011453025,2.73295261851046));
#88595=CARTESIAN_POINT('Ctrl Pts',(49.291,-2.57990529901037,2.71544717523286));
#88596=CARTESIAN_POINT('Ctrl Pts',(49.291,-2.59510362438686,2.69782010081254));
#88597=CARTESIAN_POINT('Ctrl Pts',(49.2910000000001,-2.67265098507086,2.60788038284924));
#88598=CARTESIAN_POINT('Ctrl Pts',(49.291,-2.74595669984527,2.51466762988873));
#88599=CARTESIAN_POINT('Ctrl Pts',(49.291,-2.81476512078422,2.41850780437463));
#88600=CARTESIAN_POINT('Ctrl Pts',(49.291,-2.88294028953555,2.3232329493196));
#88601=CARTESIAN_POINT('Ctrl Pts',(49.291,-2.94670096158189,2.2250642295418));
#88602=CARTESIAN_POINT('Ctrl Pts',(49.291,-3.0057531650948,2.12429641591241));
#88603=CARTESIAN_POINT('Ctrl Pts',(49.291,-3.06309302084408,2.02645058537676));
#88604=CARTESIAN_POINT('Ctrl Pts',(49.291,-3.11599369344923,1.92615350792922));
#88605=CARTESIAN_POINT('Ctrl Pts',(49.291,-3.16413915873218,1.82366487194788));
#88606=CARTESIAN_POINT('Ctrl Pts',(49.291,-3.21154220550962,1.72275664358147));
#88607=CARTESIAN_POINT('Ctrl Pts',(49.291,-3.25433581187686,1.61972334371028));
#88608=CARTESIAN_POINT('Ctrl Pts',(49.291,-3.29216896681703,1.51481212425853));
#88609=CARTESIAN_POINT('Ctrl Pts',(49.291,-3.2971950076517,1.50087492885909));
#88610=CARTESIAN_POINT('Ctrl Pts',(49.291,-3.30213229857781,1.48690762923938));
#88611=CARTESIAN_POINT('Ctrl Pts',(49.291,-3.30697750441129,1.47291855471233));
#88612=CARTESIAN_POINT('Ctrl Pts',(49.291,-3.3435823316148,1.36723312598158));
#88613=CARTESIAN_POINT('Ctrl Pts',(49.291,-3.37498240661714,1.26017600349772));
#88614=CARTESIAN_POINT('Ctrl Pts',(49.291,-3.4009150635724,1.15201104588828));
#88615=CARTESIAN_POINT('Ctrl Pts',(49.291,-3.41583937901282,1.08976181513079));
#88616=CARTESIAN_POINT('Ctrl Pts',(49.291,-3.42895196485492,1.02714544974631));
#88617=CARTESIAN_POINT('Ctrl Pts',(49.291,-3.44019492225294,0.964211348562105));
#88618=CARTESIAN_POINT('Ctrl Pts',(49.291,-3.46010351309487,0.852770094617592));
#88619=CARTESIAN_POINT('Ctrl Pts',(49.291,-3.47415249335439,0.740331870820918));
#88620=CARTESIAN_POINT('Ctrl Pts',(49.291,-3.48247133759665,0.627292733384211));
#88621=CARTESIAN_POINT('Ctrl Pts',(49.291,-3.48859838156326,0.544036484697046));
#88622=CARTESIAN_POINT('Ctrl Pts',(49.291,-3.4916158426533,0.460454247766092));
#88623=CARTESIAN_POINT('Ctrl Pts',(49.291,-3.49155833914504,0.376709317963282));
#88624=CARTESIAN_POINT('Ctrl Pts',(49.291,-3.49152958739091,0.334836853061878));
#88625=CARTESIAN_POINT('Ctrl Pts',(49.291,-3.49073187737215,0.292923804538428));
#88626=CARTESIAN_POINT('Ctrl Pts',(49.291,-3.48916828433049,0.250991241296264));
#88627=CARTESIAN_POINT('Ctrl Pts',(49.291,-3.48819573164138,0.224909245498223));
#88628=CARTESIAN_POINT('Ctrl Pts',(49.291,-3.48692685474254,0.198819676470504));
#88629=CARTESIAN_POINT('Ctrl Pts',(49.291,-3.48536224038303,0.17272774885287));
#88630=CARTESIAN_POINT('Ctrl Pts',(49.291,-3.48441139192721,0.156871145636885));
#88631=CARTESIAN_POINT('Ctrl Pts',(49.291,-3.48335133632153,0.141014949767345));
#88632=CARTESIAN_POINT('Ctrl Pts',(49.291,-3.48218335319603,0.125173095621732));
#88633=CARTESIAN_POINT('Ctrl Pts',(49.291,-3.47400097567051,0.014192013366608));
#88634=CARTESIAN_POINT('Ctrl Pts',(49.291,-3.4605166069301,-0.0962534958503473));
#88635=CARTESIAN_POINT('Ctrl Pts',(49.291,-3.44188652183421,-0.205793275630291));
#88636=CARTESIAN_POINT('Ctrl Pts',(49.291,-3.42320843589755,-0.315615287160677));
#88637=CARTESIAN_POINT('Ctrl Pts',(49.291,-3.39935769259813,-0.424527765102663));
#88638=CARTESIAN_POINT('Ctrl Pts',(49.291,-3.37044206707646,-0.532141159658396));
#88639=CARTESIAN_POINT('Ctrl Pts',(49.291,-3.34195964367767,-0.638142334172885));
#88640=CARTESIAN_POINT('Ctrl Pts',(49.291,-3.30856248028982,-0.742883787691385));
#88641=CARTESIAN_POINT('Ctrl Pts',(49.291,-3.2703120890578,-0.84596544270122));
#88642=CARTESIAN_POINT('Ctrl Pts',(49.291,-3.24749664417666,-0.907451188137614));
#88643=CARTESIAN_POINT('Ctrl Pts',(49.291,-3.22295374005823,-0.968345820777564));
#88644=CARTESIAN_POINT('Ctrl Pts',(49.291,-3.19669027020856,-1.02855802508857));
#88645=CARTESIAN_POINT('Ctrl Pts',(49.291,-3.18377971124691,-1.05815705440256));
#88646=CARTESIAN_POINT('Ctrl Pts',(49.291,-3.17045331195658,-1.0875910939131));
#88647=CARTESIAN_POINT('Ctrl Pts',(49.291,-3.15671152110727,-1.11684879068458));
#88648=CARTESIAN_POINT('Ctrl Pts',(49.291,-3.15009342463488,-1.13093940390357));
#88649=CARTESIAN_POINT('Ctrl Pts',(49.291,-3.14338306198869,-1.1449803992522));
#88650=CARTESIAN_POINT('Ctrl Pts',(49.291,-3.13658146830333,-1.15896934835303));
#88651=CARTESIAN_POINT('Ctrl Pts',(49.291,-3.08957842437905,-1.25564127841209));
#88652=CARTESIAN_POINT('Ctrl Pts',(49.291,-3.03821155674967,-1.34985216107223));
#88653=CARTESIAN_POINT('Ctrl Pts',(49.291,-2.98257948506975,-1.44125037056837));
#88654=CARTESIAN_POINT('Ctrl Pts',(49.291,-2.92773294523813,-1.53135802585232));
#88655=CARTESIAN_POINT('Ctrl Pts',(49.291,-2.86874034172397,-1.61873250557023));
#88656=CARTESIAN_POINT('Ctrl Pts',(49.291,-2.80565945595285,-1.70300335032673));
#88657=CARTESIAN_POINT('Ctrl Pts',(49.291,-2.74451889583004,-1.78468208053875));
#88658=CARTESIAN_POINT('Ctrl Pts',(49.291,-2.67953722771974,-1.86344557020302));
#88659=CARTESIAN_POINT('Ctrl Pts',(49.291,-2.61073916422542,-1.9389175189001));
#88660=CARTESIAN_POINT('Ctrl Pts',(49.291,-2.54714019487492,-2.00868602557333));
#88661=CARTESIAN_POINT('Ctrl Pts',(49.291,-2.48027938346939,-2.07564162707797));
#88662=CARTESIAN_POINT('Ctrl Pts',(49.291,-2.41015873594071,-2.1394514320425));
#88663=CARTESIAN_POINT('Ctrl Pts',(49.2909999999999,1.24155974343475,-2.97996389319987));
#88664=CARTESIAN_POINT('Ctrl Pts',(49.2909999999999,1.30609747649074,-2.96119741864278));
#88665=CARTESIAN_POINT('Ctrl Pts',(49.2909999999999,1.36990375724753,-2.94029757439427));
#88666=CARTESIAN_POINT('Ctrl Pts',(49.2909999999999,1.43287202055253,-2.91725941417401));
#88667=CARTESIAN_POINT('Ctrl Pts',(49.2909999999999,1.52953857307307,-2.8818920813619));
#88668=CARTESIAN_POINT('Ctrl Pts',(49.2909999999999,1.62423083505432,-2.84148829030612));
#88669=CARTESIAN_POINT('Ctrl Pts',(49.291,1.71676866792147,-2.7964134037744));
#88670=CARTESIAN_POINT('Ctrl Pts',(49.291,1.77471818041898,-2.76818637900559));
#88671=CARTESIAN_POINT('Ctrl Pts',(49.2909999999999,1.83182274814194,-2.7381264400551));
#88672=CARTESIAN_POINT('Ctrl Pts',(49.2909999999999,1.88803631231024,-2.70631314436809));
#88673=CARTESIAN_POINT('Ctrl Pts',(49.2909999999999,1.92428874636053,-2.68579657650977));
#88674=CARTESIAN_POINT('Ctrl Pts',(49.291,1.96017057617847,-2.66455062778348));
#88675=CARTESIAN_POINT('Ctrl Pts',(49.291,1.99566895445841,-2.64259506607457));
#88676=CARTESIAN_POINT('Ctrl Pts',(49.291,2.01164126184652,-2.63271627731052));
#88677=CARTESIAN_POINT('Ctrl Pts',(49.291,2.02753526337067,-2.62269413617559));
#88678=CARTESIAN_POINT('Ctrl Pts',(49.291,2.043338740134,-2.61253776460566));
#88679=CARTESIAN_POINT('Ctrl Pts',(49.291,2.13272190540694,-2.55509416202361));
#88680=CARTESIAN_POINT('Ctrl Pts',(49.291,2.21930400701889,-2.49330331451299));
#88681=CARTESIAN_POINT('Ctrl Pts',(49.291,2.30289476104567,-2.42754176486054));
#88682=CARTESIAN_POINT('Ctrl Pts',(49.291,2.3885789038207,-2.36013332866288));
#88683=CARTESIAN_POINT('Ctrl Pts',(49.291,2.4711206813037,-2.28855247169546));
#88684=CARTESIAN_POINT('Ctrl Pts',(49.291,2.55029884082011,-2.21315276753045));
#88685=CARTESIAN_POINT('Ctrl Pts',(49.291,2.57674354345376,-2.18797003068122));
#88686=CARTESIAN_POINT('Ctrl Pts',(49.291,2.60281285880127,-2.16236090782209));
#88687=CARTESIAN_POINT('Ctrl Pts',(49.291,2.62849794204176,-2.13633743752041));
#88688=CARTESIAN_POINT('Ctrl Pts',(49.291,2.64321859230724,-2.12142285066009));
#88689=CARTESIAN_POINT('Ctrl Pts',(49.291,2.65781302871306,-2.1063721544104));
#88690=CARTESIAN_POINT('Ctrl Pts',(49.291,2.67227953262755,-2.09118753901551));
#88691=CARTESIAN_POINT('Ctrl Pts',(49.291,2.68411484151633,-2.07876473011725));
#88692=CARTESIAN_POINT('Ctrl Pts',(49.291,2.6958637113429,-2.06625304941116));
#88693=CARTESIAN_POINT('Ctrl Pts',(49.291,2.70751679354967,-2.05366306839897));
#88694=CARTESIAN_POINT('Ctrl Pts',(49.291,2.78348489802944,-1.97158718701738));
#88695=CARTESIAN_POINT('Ctrl Pts',(49.291,2.85548187030216,-1.88608530691149));
#88696=CARTESIAN_POINT('Ctrl Pts',(49.291,2.92330271970775,-1.79755683447092));
#88697=CARTESIAN_POINT('Ctrl Pts',(49.291,2.99192600729937,-1.70798091677628));
#88698=CARTESIAN_POINT('Ctrl Pts',(49.291,3.05627448257204,-1.61530580669057));
#88699=CARTESIAN_POINT('Ctrl Pts',(49.291,3.11611202188338,-1.51989684308203));
#88700=CARTESIAN_POINT('Ctrl Pts',(49.291,3.17581269028068,-1.4247061155876));
#88701=CARTESIAN_POINT('Ctrl Pts',(49.291,3.23102371579603,-1.32679334572647));
#88702=CARTESIAN_POINT('Ctrl Pts',(49.291,3.28147664994958,-1.22648294339381));
#88703=CARTESIAN_POINT('Ctrl Pts',(49.291,3.31382283080201,-1.16217234442335));
#88704=CARTESIAN_POINT('Ctrl Pts',(49.291,3.34421258369244,-1.09687550021422));
#88705=CARTESIAN_POINT('Ctrl Pts',(49.291,3.37256580457531,-1.03067154124884));
#88706=CARTESIAN_POINT('Ctrl Pts',(49.291,3.38259777691676,-1.00724717306227));
#88707=CARTESIAN_POINT('Ctrl Pts',(49.291,3.39237472274341,-0.983709205287762));
#88708=CARTESIAN_POINT('Ctrl Pts',(49.291,3.40189284016588,-0.960061026530207));
#88709=CARTESIAN_POINT('Ctrl Pts',(49.291,3.40733925000965,-0.94652918321965));
#88710=CARTESIAN_POINT('Ctrl Pts',(49.291,3.41269973962293,-0.932964063311978));
#88711=CARTESIAN_POINT('Ctrl Pts',(49.291,3.41797075710576,-0.919374174560089));
#88712=CARTESIAN_POINT('Ctrl Pts',(49.291,3.45985945406193,-0.811375532276965));
#88713=CARTESIAN_POINT('Ctrl Pts',(49.291,3.49615814443692,-0.701673043089189));
#88714=CARTESIAN_POINT('Ctrl Pts',(49.291,3.526628671481,-0.590647306950014));
#88715=CARTESIAN_POINT('Ctrl Pts',(49.291,3.54303568422161,-0.530864925610285));
#88716=CARTESIAN_POINT('Ctrl Pts',(49.291,3.55775234160509,-0.470698196068018));
#88717=CARTESIAN_POINT('Ctrl Pts',(49.291,3.57073680375558,-0.410202350230981));
#88718=CARTESIAN_POINT('Ctrl Pts',(49.291,3.59424040049109,-0.300696854489483));
#88719=CARTESIAN_POINT('Ctrl Pts',(49.2910000000001,3.61207160669811,-0.190114079831296));
#88720=CARTESIAN_POINT('Ctrl Pts',(49.2910000000001,3.62443023878303,-0.0788005633581947));
#88721=CARTESIAN_POINT('Ctrl Pts',(49.2910000000001,3.63678887086796,0.0325129531149071));
#88722=CARTESIAN_POINT('Ctrl Pts',(49.291,3.6436748240379,0.144557927003784));
#88723=CARTESIAN_POINT('Ctrl Pts',(49.291,3.64523740891943,0.257002790496591));
#88724=CARTESIAN_POINT('Ctrl Pts',(49.291,3.64573156500446,0.292562659392238));
#88725=CARTESIAN_POINT('Ctrl Pts',(49.2910000000001,3.6456929614631,0.32816258953133));
#88726=CARTESIAN_POINT('Ctrl Pts',(49.2910000000001,3.64512529508925,0.363792226448562));
#88727=CARTESIAN_POINT('Ctrl Pts',(49.2910000000001,3.64486222011793,0.380304153421158));
#88728=CARTESIAN_POINT('Ctrl Pts',(49.2910000000001,3.64448543221427,0.396825027320545));
#88729=CARTESIAN_POINT('Ctrl Pts',(49.2910000000001,3.64399552440606,0.413345378021866));
#88730=CARTESIAN_POINT('Ctrl Pts',(49.2910000000001,3.64053542637784,0.530024540776952));
#88731=CARTESIAN_POINT('Ctrl Pts',(49.291,3.63144663106782,0.646416163441864));
#88732=CARTESIAN_POINT('Ctrl Pts',(49.2910000000001,3.61697648681964,0.762139257707719));
#88733=CARTESIAN_POINT('Ctrl Pts',(49.2910000000001,3.60244319778279,0.878367344197995));
#88734=CARTESIAN_POINT('Ctrl Pts',(49.2910000000001,3.58248137580691,0.993921830073509));
#88735=CARTESIAN_POINT('Ctrl Pts',(49.2910000000001,3.55728842902304,1.10843304586257));
#88736=CARTESIAN_POINT('Ctrl Pts',(49.2910000000001,3.53175390717093,1.22449684605884));
#88737=CARTESIAN_POINT('Ctrl Pts',(49.2910000000001,3.50084540844511,1.33948972685971));
#88738=CARTESIAN_POINT('Ctrl Pts',(49.2910000000001,3.46471501177006,1.45303135874471));
#88739=CARTESIAN_POINT('Ctrl Pts',(49.291,3.43001588946358,1.56207513723098));
#88740=CARTESIAN_POINT('Ctrl Pts',(49.291,3.39049995192555,1.66978108778202));
#88741=CARTESIAN_POINT('Ctrl Pts',(49.291,3.34625722541054,1.77580515381087));
#88742=CARTESIAN_POINT('Ctrl Pts',(49.291,3.33687123746234,1.7982979042436));
#88743=CARTESIAN_POINT('Ctrl Pts',(49.291,3.32726976310538,1.82072057743119));
#88744=CARTESIAN_POINT('Ctrl Pts',(49.291,3.31746764588934,1.84303814040658));
#88745=CARTESIAN_POINT('Ctrl Pts',(49.291,3.26814654678819,1.95533293457664));
#88746=CARTESIAN_POINT('Ctrl Pts',(49.291,3.21370135735444,2.06509026310669));
#88747=CARTESIAN_POINT('Ctrl Pts',(49.291,3.15434087104448,2.17191824325322));
#88748=CARTESIAN_POINT('Ctrl Pts',(49.291,3.09490644304957,2.27887929240478));
#88749=CARTESIAN_POINT('Ctrl Pts',(49.291,3.03054427425482,2.38290458632646));
#88750=CARTESIAN_POINT('Ctrl Pts',(49.291,2.96141160421367,2.48359656129828));
#88751=CARTESIAN_POINT('Ctrl Pts',(49.291,2.89240794490613,2.58410063168675));
#88752=CARTESIAN_POINT('Ctrl Pts',(49.291,2.81865136104634,2.68128471430845));
#88753=CARTESIAN_POINT('Ctrl Pts',(49.291,2.74024916152721,2.7747358172889));
#88754=CARTESIAN_POINT('Ctrl Pts',(49.291,2.66184696200807,2.86818692026936));
#88755=CARTESIAN_POINT('Ctrl Pts',(49.291,2.57879895493468,2.95790597872136));
#88756=CARTESIAN_POINT('Ctrl Pts',(49.291,2.49116634986212,3.04344857313454));
#88757=CARTESIAN_POINT('Origin',(49.291,0.,0.));
#88758=CARTESIAN_POINT('Ctrl Pts',(0.173056187199666,-1.43083790675438,
2.88251867495153));
#88759=CARTESIAN_POINT('Ctrl Pts',(0.239338593446214,-2.39121159098777,
2.40580395875854));
#88760=CARTESIAN_POINT('Ctrl Pts',(0.37190340593931,-3.78114133209139,0.425036707075511));
#88761=CARTESIAN_POINT('Ctrl Pts',(0.570750624678953,-2.39953276490048,
-2.95773654621702));
#88762=CARTESIAN_POINT('Ctrl Pts',(0.769597843418598,1.18945394678139,-3.61436653776285));
#88763=CARTESIAN_POINT('Ctrl Pts',(0.968445062158239,3.68418171216641,-0.955516875925982));
#88764=CARTESIAN_POINT('Ctrl Pts',(1.16729228089789,2.79555519642049,2.58343267463272));
#88765=CARTESIAN_POINT('Ctrl Pts',(1.36613949963753,-0.661460018592585,
3.74805170741327));
#88766=CARTESIAN_POINT('Ctrl Pts',(1.56498671837718,-3.51063697999909,1.47043618308769));
#88767=CARTESIAN_POINT('Ctrl Pts',(1.76383393711682,-3.1351373407493,-2.15823110503949));
#88768=CARTESIAN_POINT('Ctrl Pts',(1.96268115585646,0.120299360187439,-3.8042141985468));
#88769=CARTESIAN_POINT('Ctrl Pts',(2.16152837459611,3.26519802508846,-1.95581670897684));
#88770=CARTESIAN_POINT('Ctrl Pts',(2.36037559333575,3.41077016481472,1.68920239984469));
#88771=CARTESIAN_POINT('Ctrl Pts',(2.5592228120754,0.423269523206983,3.78252945499563));
#88772=CARTESIAN_POINT('Ctrl Pts',(2.75807003081503,-2.95303304907864,2.40131564870111));
#88773=CARTESIAN_POINT('Ctrl Pts',(2.95691724955468,-3.6167424373011,-1.18570445582992));
#88774=CARTESIAN_POINT('Ctrl Pts',(3.15576446829432,-0.958184980230354,
-3.68355711222238));
#88775=CARTESIAN_POINT('Ctrl Pts',(3.35461168703397,2.58054089412746,-2.79777152901459));
#88776=CARTESIAN_POINT('Ctrl Pts',(3.55345890577361,3.74883510575342,0.657990674924371));
#88777=CARTESIAN_POINT('Ctrl Pts',(3.75230612451326,1.47352597266888,3.50933560299747));
#88778=CARTESIAN_POINT('Ctrl Pts',(3.95115334325289,-2.15533384583538,3.13707698173024));
#88779=CARTESIAN_POINT('Ctrl Pts',(4.15000056199255,-3.80434818238047,-0.116836453731265));
#88780=CARTESIAN_POINT('Ctrl Pts',(4.34884778073217,-1.95876615891209,-3.26342624165674));
#88781=CARTESIAN_POINT('Ctrl Pts',(4.54769499947184,1.68609833178183,-3.41229955232396));
#88782=CARTESIAN_POINT('Ctrl Pts',(4.74654221821145,3.78214743079572,-0.426704352531632));
#88783=CARTESIAN_POINT('Ctrl Pts',(4.94538943695112,2.40399334842639,2.95085271673614));
#88784=CARTESIAN_POINT('Ctrl Pts',(5.14423665569075,-1.18241979186214,3.61781691467976));
#88785=CARTESIAN_POINT('Ctrl Pts',(5.3430838744304,-3.6826863264606,0.961528579047624));
#88786=CARTESIAN_POINT('Ctrl Pts',(5.54193109317004,-2.80011261657801,-2.57800021721949));
#88787=CARTESIAN_POINT('Ctrl Pts',(5.74077831190969,0.654587200762842,-3.74943080807304));
#88788=CARTESIAN_POINT('Ctrl Pts',(5.93962553064932,3.50799662053473,-1.47671104058992));
#88789=CARTESIAN_POINT('Ctrl Pts',(6.13847274938897,3.13903218278845,2.15248524787444));
#88790=CARTESIAN_POINT('Ctrl Pts',(6.33731996812863,-0.113382935647901,
3.80445266722274));
#88791=CARTESIAN_POINT('Ctrl Pts',(6.53616718686825,-3.26164681132122,1.96172777553185));
#88792=CARTESIAN_POINT('Ctrl Pts',(6.73501440560792,-3.41382871943484,-1.683000077672));
#88793=CARTESIAN_POINT('Ctrl Pts',(6.93386162434754,-0.430137475655535,
-3.78175852470304));
#88794=CARTESIAN_POINT('Ctrl Pts',(7.1327088430872,2.94866924473366,-2.40667103532393));
#88795=CARTESIAN_POINT('Ctrl Pts',(7.33155606182684,3.61888878095798,1.17913518231027));
#88796=CARTESIAN_POINT('Ctrl Pts',(7.53040328056648,0.96487119207266,3.68181196828677));
#88797=CARTESIAN_POINT('Ctrl Pts',(7.72925049930613,-2.57545731482602,2.80245167783803));
#88798=CARTESIAN_POINT('Ctrl Pts',(7.92809771804577,-3.75002347358853,-0.651183334125902));
#88799=CARTESIAN_POINT('Ctrl Pts',(8.12694493678541,-1.47989486401989,-3.50665467055948));
#88800=CARTESIAN_POINT('Ctrl Pts',(8.32579215552506,2.14963486174807,-3.14098483731869));
#88801=CARTESIAN_POINT('Ctrl Pts',(8.5246393742647,3.80455402461192,0.109929345116928));
#88802=CARTESIAN_POINT('Ctrl Pts',(8.72348659300433,1.96468777167325,3.25986468230605));
#88803=CARTESIAN_POINT('Ctrl Pts',(8.92233381174399,-1.67990043464857,3.41535507916472));
#88804=CARTESIAN_POINT('Ctrl Pts',(9.12118103048362,-3.78136650338711,0.433570241334211));
#88805=CARTESIAN_POINT('Ctrl Pts',(9.32002824922328,-2.40934673847672,-2.946483341358));
#88806=CARTESIAN_POINT('Ctrl Pts',(9.51887546796291,1.17584960081515,-3.61995766596401));
#88807=CARTESIAN_POINT('Ctrl Pts',(9.71772268670256,3.68093457632498,-0.968213009582048));
#88808=CARTESIAN_POINT('Ctrl Pts',(9.91656990544221,2.80478842969927,2.57291228994185));
#88809=CARTESIAN_POINT('Ctrl Pts',(10.1154171241818,-0.647778930849038,
3.75061304907035));
#88810=CARTESIAN_POINT('Ctrl Pts',(10.3142643429215,-3.50530983100003,1.48307746790353));
#88811=CARTESIAN_POINT('Ctrl Pts',(10.5131115616611,-3.14293490355597,-2.14678270421539));
#88812=CARTESIAN_POINT('Ctrl Pts',(10.7119587804008,0.106475663994328,-3.80465224693213));
#88813=CARTESIAN_POINT('Ctrl Pts',(10.9108059991404,3.25807986705142,-1.96764614883441));
#88814=CARTESIAN_POINT('Ctrl Pts',(11.1096532178801,3.4168786245208,1.67679940732383));
#88815=CARTESIAN_POINT('Ctrl Pts',(11.3085004366197,0.437002649736691,3.7809713660952));
#88816=CARTESIAN_POINT('Ctrl Pts',(11.5073476553593,-2.9442950099774,2.41202045624221));
#88817=CARTESIAN_POINT('Ctrl Pts',(11.706194874099,-3.62102356799794,-1.17256305037815));
#88818=CARTESIAN_POINT('Ctrl Pts',(11.9050420928386,-0.971554029250149,
-3.68005415114459));
#88819=CARTESIAN_POINT('Ctrl Pts',(12.1038893115783,2.57036514488798,-2.80712287031647));
#88820=CARTESIAN_POINT('Ctrl Pts',(12.3027365303179,3.75119953391568,0.644373993779587));
#88821=CARTESIAN_POINT('Ctrl Pts',(12.5015837490575,1.48625884967945,3.50396210294263));
#88822=CARTESIAN_POINT('Ctrl Pts',(12.7004309677972,-2.14392877765862,3.14488237990484));
#88823=CARTESIAN_POINT('Ctrl Pts',(12.8992781865368,-3.80474733408567,-0.103021895132036));
#88824=CARTESIAN_POINT('Ctrl Pts',(13.0981254052765,-1.97060290458628,-3.25629236702493));
#88825=CARTESIAN_POINT('Ctrl Pts',(13.2969726240161,1.67369699825765,-3.41839935424929));
#88826=CARTESIAN_POINT('Ctrl Pts',(13.4958198427558,3.78057311315052,-0.440434698033706));
#88827=CARTESIAN_POINT('Ctrl Pts',(13.6946670614954,2.41469218641841,2.94210425239463));
#88828=CARTESIAN_POINT('Ctrl Pts',(13.893514280235,-1.16927553370817,3.62208648618171));
#88829=CARTESIAN_POINT('Ctrl Pts',(14.0923614989747,-3.67917069347074,0.974894248323716));
#88830=CARTESIAN_POINT('Ctrl Pts',(14.2912087177143,-2.80945499776618,-2.56781588176319));
#88831=CARTESIAN_POINT('Ctrl Pts',(14.490055936454,0.640968525723349,-3.7517829276413));
#88832=CARTESIAN_POINT('Ctrl Pts',(14.6889031551936,3.5026114874978,-1.48943900672608));
#88833=CARTESIAN_POINT('Ctrl Pts',(14.8877503739333,3.14682726476055,2.14107308442948));
#88834=CARTESIAN_POINT('Ctrl Pts',(15.0865975926729,-0.0995680413761137,
3.80483928599425));
#88835=CARTESIAN_POINT('Ctrl Pts',(15.2854448114125,-3.25450218369954,1.97355803649236));
#88836=CARTESIAN_POINT('Ctrl Pts',(15.4842920301522,-3.41991726709704,-1.67059321000658));
#88837=CARTESIAN_POINT('Ctrl Pts',(15.6831392488918,-0.4438663833971,-3.78017174488127));
#88838=CARTESIAN_POINT('Ctrl Pts',(15.8819864676315,2.93991107041495,-2.41736192680373));
#88839=CARTESIAN_POINT('Ctrl Pts',(16.0808336863711,3.62314641963944,1.16598705351417));
#88840=CARTESIAN_POINT('Ctrl Pts',(16.2796809051108,0.978233664050299,3.67828420403148));
#88841=CARTESIAN_POINT('Ctrl Pts',(16.4785281238504,-2.56526450266828,2.81178481012661));
#88842=CARTESIAN_POINT('Ctrl Pts',(16.6773753425901,-3.75236322976644,-0.637562529486655));
#88843=CARTESIAN_POINT('Ctrl Pts',(16.8762225613297,-1.49261793642279,-3.50125798577849));
#88844=CARTESIAN_POINT('Ctrl Pts',(17.0750697800694,2.13821562688115,-3.14876955652043));
#88845=CARTESIAN_POINT('Ctrl Pts',(17.273916998809,3.80492810258206,0.0961141055726008));
#88846=CARTESIAN_POINT('Ctrl Pts',(17.4727642175486,1.97651154211755,3.25270931855043));
#88847=CARTESIAN_POINT('Ctrl Pts',(17.6716114362883,-1.66748804512824,3.42143236181325));
#88848=CARTESIAN_POINT('Ctrl Pts',(17.8704586550279,-3.77976726161816,0.447297702999042));
#88849=CARTESIAN_POINT('Ctrl Pts',(18.0693058737676,-2.42002967519819,-2.93771546584566));
#88850=CARTESIAN_POINT('Ctrl Pts',(18.2681530925072,1.16269761250606,-3.62420336749765));
#88851=CARTESIAN_POINT('Ctrl Pts',(18.4670003112469,3.67739468355725,-0.981572273678105));
#88852=CARTESIAN_POINT('Ctrl Pts',(18.6658475299865,2.81411230547795,2.5627110097056));
#88853=CARTESIAN_POINT('Ctrl Pts',(18.8646947487261,-0.634156007876128,
3.75294043981293));
#88854=CARTESIAN_POINT('Ctrl Pts',(19.0635419674658,-3.49990159890004,1.49579563615007));
#88855=CARTESIAN_POINT('Ctrl Pts',(19.2623891862054,-3.15070925358397,-2.13535640736833));
#88856=CARTESIAN_POINT('Ctrl Pts',(19.4612364049451,0.0926600905677234,
-3.80501378377591));
#88857=CARTESIAN_POINT('Ctrl Pts',(19.6600836236847,3.25091377305496,-1.97946341902805));
#88858=CARTESIAN_POINT('Ctrl Pts',(19.8589308424244,3.42294463714945,1.66438150618135));
#88859=CARTESIAN_POINT('Ctrl Pts',(20.057778061164,0.450728654012033,3.77935966369453));
#88860=CARTESIAN_POINT('Ctrl Pts',(20.2566252799037,-2.93551744049599,2.42269542940348));
#88861=CARTESIAN_POINT('Ctrl Pts',(20.4554724986433,-3.62525732888544,-1.15940721339442));
#88862=CARTESIAN_POINT('Ctrl Pts',(20.6543197173829,-0.984910074455989,
-3.67650213278107));
#88863=CARTESIAN_POINT('Ctrl Pts',(20.8531669361226,2.56015540497932,-2.81643748190223));
#88864=CARTESIAN_POINT('Ctrl Pts',(21.0520141548622,3.75351455730514,0.630748963698809));
#88865=CARTESIAN_POINT('Ctrl Pts',(21.2508613736019,1.49897210328941,3.49854232798016));
#88866=CARTESIAN_POINT('Ctrl Pts',(21.4497085923415,-2.13249542824708,3.15264635435279));
#88867=CARTESIAN_POINT('Ctrl Pts',(21.6485558110811,-3.80509632950521,-0.0892059992077045));
#88868=CARTESIAN_POINT('Ctrl Pts',(21.8474030298208,-1.98241366479137,-3.24911554869277));
#88869=CARTESIAN_POINT('Ctrl Pts',(22.0462502485605,1.66127359572584,-3.42445409185943));
#88870=CARTESIAN_POINT('Ctrl Pts',(22.2450974673001,3.77894895144623,-0.454159233608839));
#88871=CARTESIAN_POINT('Ctrl Pts',(22.4439446860397,2.42535918722295,2.93331699617719));
#88872=CARTESIAN_POINT('Ctrl Pts',(22.6427919047794,-1.15611585889066,3.62630830293429));
#88873=CARTESIAN_POINT('Ctrl Pts',(22.841639123519,-3.67560655243846,0.988247063633482));
#88874=CARTESIAN_POINT('Ctrl Pts',(23.0404863422586,-2.81876033748343,-2.55759769059541));
#88875=CARTESIAN_POINT('Ctrl Pts',(23.2393335609983,0.627341399762283,-3.75408558176995));
#88876=CARTESIAN_POINT('Ctrl Pts',(23.4381807797379,3.49718017413892,-1.50214733522328));
#88877=CARTESIAN_POINT('Ctrl Pts',(23.6370279984776,3.15458085723069,2.12963269187493));
#88878=CARTESIAN_POINT('Ctrl Pts',(23.8358752172172,-0.0857518343388183,
3.80517573970196));
#88879=CARTESIAN_POINT('Ctrl Pts',(24.0347224359569,-3.24731464694565,1.98536227697641));
#88880=CARTESIAN_POINT('Ctrl Pts',(24.2335696546965,-3.42596072469933,-1.65816431632281));
#88881=CARTESIAN_POINT('Ctrl Pts',(24.4324168734362,-0.457589438962482,
-3.7785351252117));
#88882=CARTESIAN_POINT('Ctrl Pts',(24.6312640921758,2.93111413470251,-2.42802094646151));
#88883=CARTESIAN_POINT('Ctrl Pts',(24.8301113109155,3.62735628877816,1.15282355170697));
#88884=CARTESIAN_POINT('Ctrl Pts',(25.0289585296551,0.991583238460796,3.67470794326736));
#88885=CARTESIAN_POINT('Ctrl Pts',(25.2278057483947,-2.55503786866146,2.82108087030743));
#88886=CARTESIAN_POINT('Ctrl Pts',(25.4266529671344,-3.75465351273682,-0.623933318874501));
#88887=CARTESIAN_POINT('Ctrl Pts',(25.6255001858741,-1.50532132933512,-3.49581513849881));
#88888=CARTESIAN_POINT('Ctrl Pts',(25.8243474046136,2.12676820061089,-3.1565127606235));
#88889=CARTESIAN_POINT('Ctrl Pts',(26.0231946233533,3.80525201430065,0.0822975988073659));
#88890=CARTESIAN_POINT('Ctrl Pts',(26.2220418420929,1.98830925315355,3.24551106929751));
#88891=CARTESIAN_POINT('Ctrl Pts',(26.4208890608326,-1.65505367053418,3.42746453442775));
#88892=CARTESIAN_POINT('Ctrl Pts',(26.6197362795722,-3.77811818533196,0.461019267246552));
#88893=CARTESIAN_POINT('Ctrl Pts',(26.8185834983119,-2.4306807049259,-2.92890885788714));
#88894=CARTESIAN_POINT('Ctrl Pts',(27.0174307170515,1.14953029455628,-3.62840128555349));
#88895=CARTESIAN_POINT('Ctrl Pts',(27.2162779357912,3.6738063060083,-0.994918596188816));
#88896=CARTESIAN_POINT('Ctrl Pts',(27.4151251545308,2.82339907846205,2.55247594128687));
#88897=CARTESIAN_POINT('Ctrl Pts',(27.6139723732705,-0.620524723843828,
3.75521834973777));
#88898=CARTESIAN_POINT('Ctrl Pts',(27.8128195920101,-3.49444722218464,1.50849408300949));
#88899=CARTESIAN_POINT('Ctrl Pts',(28.0116668107498,-3.15844206293931,-2.12390195681543));
#88900=CARTESIAN_POINT('Ctrl Pts',(28.2105140294894,0.0788432954598658,
-3.80532515323851));
#88901=CARTESIAN_POINT('Ctrl Pts',(28.409361248229,3.24370481723469,-1.99125459089417));
#88902=CARTESIAN_POINT('Ctrl Pts',(28.6082084669687,3.42896551980536,1.6519416609235));
#88903=CARTESIAN_POINT('Ctrl Pts',(28.8070556857083,0.464448715634499,3.7776981321506));
#88904=CARTESIAN_POINT('Ctrl Pts',(29.005902904448,-2.92670116754833,2.43333846042424));
#88905=CARTESIAN_POINT('Ctrl Pts',(29.2047501231876,-3.62944329239912,-1.14623609015233));
#88906=CARTESIAN_POINT('Ctrl Pts',(29.4035973419273,-0.998253134069163,
-3.67290164140422));
#88907=CARTESIAN_POINT('Ctrl Pts',(29.6024445606669,2.54991191058275,-2.82571496003703));
#88908=CARTESIAN_POINT('Ctrl Pts',(29.8012917794065,3.75578009230734,0.617115617479058));
#88909=CARTESIAN_POINT('Ctrl Pts',(30.0001389981462,1.51166559363194,3.49307642632366));
#88910=CARTESIAN_POINT('Ctrl Pts',(30.1989862168858,-2.1210339628504,3.16036876258829));
#88911=CARTESIAN_POINT('Ctrl Pts',(30.3978334356255,-3.80539515645523,-0.0753889271427265));
#88912=CARTESIAN_POINT('Ctrl Pts',(30.5966806543651,-1.99419828777131,-3.24189589224556));
#88913=CARTESIAN_POINT('Ctrl Pts',(30.7955278731047,1.64882829005506,-3.43046367959534));
#88914=CARTESIAN_POINT('Ctrl Pts',(30.9943750918444,3.77727496601373,-0.467877781300454));
#88915=CARTESIAN_POINT('Ctrl Pts',(31.1932223105841,2.43599421076651,2.92449106550537));
#88916=CARTESIAN_POINT('Ctrl Pts',(31.3920695293236,-1.1429409412098,3.63048230845643));
#88917=CARTESIAN_POINT('Ctrl Pts',(31.5909167480633,-3.67199395020061,1.00158684935393));
#88918=CARTESIAN_POINT('Ctrl Pts',(31.789763966803,-2.82802851312397,-2.54734577866189));
#88919=CARTESIAN_POINT('Ctrl Pts',(31.9886111855426,0.613706002589339,-3.75633873998267));
#88920=CARTESIAN_POINT('Ctrl Pts',(32.1874584042823,3.49170275204543,-1.51483585858905));
#88921=CARTESIAN_POINT('Ctrl Pts',(32.3863056230219,3.16229285798277,2.11816422107915));
#88922=CARTESIAN_POINT('Ctrl Pts',(32.5851528417615,-0.071934496702472,
3.80546202389314));
#88923=CARTESIAN_POINT('Ctrl Pts',(32.7840000605012,-3.24008429582074,1.99714034135926));
#88924=CARTESIAN_POINT('Ctrl Pts',(32.9828472792408,-3.43195901256317,-1.64571356049439));
#88925=CARTESIAN_POINT('Ctrl Pts',(33.1816944979805,-0.471306461418734,
-3.77684868727006));
#88926=CARTESIAN_POINT('Ctrl Pts',(33.3805417167201,2.92227855357939,-2.43864795376427));
#88927=CARTESIAN_POINT('Ctrl Pts',(33.5793889354597,3.63151833286923,1.13964485044393));
#88928=CARTESIAN_POINT('Ctrl Pts',(33.7782361541994,1.00491973929605,3.67108323314547));
#88929=CARTESIAN_POINT('Ctrl Pts',(33.977083372939,-2.544777547639,2.83033973581637));
#88930=CARTESIAN_POINT('Ctrl Pts',(34.1759305916787,-3.75689429230335,-0.610295881984437));
#88931=CARTESIAN_POINT('Ctrl Pts',(34.3747778104184,-1.5180048752684,-3.49032620048186));
#88932=CARTESIAN_POINT('Ctrl Pts',(34.573625029158,2.11529273386641,-3.16421434753728));
#88933=CARTESIAN_POINT('Ctrl Pts',(34.7724722478976,3.80552575549711,0.0684800069856816));
#88934=CARTESIAN_POINT('Ctrl Pts',(34.9713194666373,2.00008074923364,3.23827002945302));
#88935=CARTESIAN_POINT('Ctrl Pts',(35.1701666853769,-1.64259747480814,3.43345151747663));
#88936=CARTESIAN_POINT('Ctrl Pts',(35.3690139041165,-3.77641929627087,0.47473475316399));
#88937=CARTESIAN_POINT('Ctrl Pts',(35.5678611228562,-2.44129968723075,-2.92006363359358));
#88938=CARTESIAN_POINT('Ctrl Pts',(35.7667083415958,1.13634782057081,-3.63255136478379));
#88939=CARTESIAN_POINT('Ctrl Pts',(35.9655555603355,3.67016949098924,-1.00825180114912));
#88940=CARTESIAN_POINT('Ctrl Pts',(36.1644027790751,2.83264862620975,2.54220721963035));
#88941=CARTESIAN_POINT('Ctrl Pts',(36.3632499978148,-0.606885258474397,
3.75744674881163));
#88942=CARTESIAN_POINT('Ctrl Pts',(36.5620972165544,-3.48894677276732,1.52117264105857));
#88943=CARTESIAN_POINT('Ctrl Pts',(36.760944435294,-3.1661332296684,-2.11241950357836));
#88944=CARTESIAN_POINT('Ctrl Pts',(36.9597916540338,0.0650254608388847,
-3.80558635121468));
#88945=CARTESIAN_POINT('Ctrl Pts',(37.1586388727733,3.23645309463745,-2.00301950897151));
#88946=CARTESIAN_POINT('Ctrl Pts',(37.357486091513,3.43494119310586,1.63948003556406));
#88947=CARTESIAN_POINT('Ctrl Pts',(37.5563333102526,0.478162653711198,3.77598679336999));
#88948=CARTESIAN_POINT('Ctrl Pts',(37.7551805289923,-2.91784630737312,2.44394940898082));
#88949=CARTESIAN_POINT('Ctrl Pts',(37.9540277477319,-3.63358140334888,-1.13304985430729));
#88950=CARTESIAN_POINT('Ctrl Pts',(38.1528749664715,-1.01158303216742,-3.66925272448487));
#88951=CARTESIAN_POINT('Ctrl Pts',(38.3517221852113,2.53963479675394,-2.83495518240152));
#88952=CARTESIAN_POINT('Ctrl Pts',(38.5505694039508,3.75799610905227,0.603474134869659));
#88953=CARTESIAN_POINT('Ctrl Pts',(38.7494166226906,1.52433915334921,3.48756447003854));
#88954=CARTESIAN_POINT('Ctrl Pts',(38.9482638414301,-2.10954453258275,3.16804950279488));
#88955=CARTESIAN_POINT('Ctrl Pts',(39.1471110601698,-3.80564381099585,-0.0615708611088804));
#88956=CARTESIAN_POINT('Ctrl Pts',(39.3459582789094,-2.00595661815121,-3.23463349287117));
#88957=CARTESIAN_POINT('Ctrl Pts',(39.5448054976491,1.63636124533099,-3.43642803822336));
#88958=CARTESIAN_POINT('Ctrl Pts',(39.7436527163887,3.77555117892381,-0.481590160235665));
#88959=CARTESIAN_POINT('Ctrl Pts',(39.9424999351283,2.44659711683104,2.91562657674516));
#88960=CARTESIAN_POINT('Ctrl Pts',(40.141347153868,-1.12975095437104,3.63460844771571));
#88961=CARTESIAN_POINT('Ctrl Pts',(40.3401943726076,-3.66833293438782,1.01491342960588));
#88962=CARTESIAN_POINT('Ctrl Pts',(40.5390415913473,-2.83725940249097,-2.53706028112956));
#88963=CARTESIAN_POINT('Ctrl Pts',(40.7378888100869,0.600062513981104,-3.75854237257257));
#88964=CARTESIAN_POINT('Ctrl Pts',(40.9367360288266,3.48617929343457,-1.52750440953102));
#88965=CARTESIAN_POINT('Ctrl Pts',(41.1355832475663,3.16996316533766,2.10666782324859));
#88966=CARTESIAN_POINT('Ctrl Pts',(41.3344304663058,-0.0581162106423564,
3.80569813479336));
#88967=CARTESIAN_POINT('Ctrl Pts',(41.5332776850456,-3.23281122565374,2.00889207435229));
#88968=CARTESIAN_POINT('Ctrl Pts',(41.732124903785,-3.43791205160379,-1.63324110667881));
#88969=CARTESIAN_POINT('Ctrl Pts',(41.9309721225249,-0.48501726991304,-3.77511245329163));
#88970=CARTESIAN_POINT('Ctrl Pts',(42.1298193412644,2.91340444353883,-2.44924280859897));
#88971=CARTESIAN_POINT('Ctrl Pts',(42.3286665600041,3.63563249703791,1.12645112347912));
#88972=CARTESIAN_POINT('Ctrl Pts',(42.5275137787437,1.01824299072025,3.66741012145854));
#88973=CARTESIAN_POINT('Ctrl Pts',(42.7263609974834,-2.53448367487889,2.83956128457451));
#88974=CARTESIAN_POINT('Ctrl Pts',(42.925208216223,-3.75908553892202,-0.59665039861077));
#88975=CARTESIAN_POINT('Ctrl Pts',(43.1240554349627,-1.53066840699641,-3.48479124411454));
#88976=CARTESIAN_POINT('Ctrl Pts',(43.3229026537023,2.10378937794771,-3.17187421568591));
#88977=CARTESIAN_POINT('Ctrl Pts',(43.521749872442,3.80574932255986,0.0546615122211324));
#88978=CARTESIAN_POINT('Ctrl Pts',(43.7205970911815,2.01182587516079,3.23098629461087));
#88979=CARTESIAN_POINT('Ctrl Pts',(43.9194443099213,-1.63011962218803,3.43939323178678));
#88980=CARTESIAN_POINT('Ctrl Pts',(44.1182915286608,-3.77467061681703,0.488443980373654));
#88981=CARTESIAN_POINT('Ctrl Pts',(44.3171387474006,-2.45188648213872,-2.91117991045481));
#88982=CARTESIAN_POINT('Ctrl Pts',(44.5159859661402,1.12315036441649,-3.63665354880811));
#88983=CARTESIAN_POINT('Ctrl Pts',(44.7148331848798,3.66648428633161,-1.02157171594932));
#88984=CARTESIAN_POINT('Ctrl Pts',(44.9136804036194,2.84186082699613,2.53190498621347));
#88985=CARTESIAN_POINT('Ctrl Pts',(45.1125276223591,-0.59323779203106,3.75962559600542));
#88986=CARTESIAN_POINT('Ctrl Pts',(45.3113748410987,-3.48340032234089,1.53383116542125));
#88987=CARTESIAN_POINT('Ctrl Pts',(45.5102220598384,-3.17378265395104,-2.10090924168198));
#88988=CARTESIAN_POINT('Ctrl Pts',(45.7090692785781,0.0512067719178791,
-3.8057972926977));
#88989=CARTESIAN_POINT('Ctrl Pts',(45.9079164973176,3.22915869507492,-2.01475817418338));
#88990=CARTESIAN_POINT('Ctrl Pts',(46.1067637160574,3.44087158935841,1.62699709292146));
#88991=CARTESIAN_POINT('Ctrl Pts',(46.3056109347969,0.491870266206481,3.7742250988203));
#88992=CARTESIAN_POINT('Ctrl Pts',(46.5044581535366,-2.9089529361142,2.45452922773842));
#88993=CARTESIAN_POINT('Ctrl Pts',(46.7033053722762,-3.63767168485402,-1.11985076990585));
#88994=CARTESIAN_POINT('Ctrl Pts',(46.9021525910159,-1.02489944439545,-3.66555143137609));
#88995=CARTESIAN_POINT('Ctrl Pts',(47.1009998097555,2.52932391469176,-2.84416567720655));
#88996=CARTESIAN_POINT('Ctrl Pts',(47.2998470284952,3.76016312221924,0.589839331053052));
#88997=CARTESIAN_POINT('Ctrl Pts',(47.4986942472348,1.53699157481281,3.48197853288055));
#88998=CARTESIAN_POINT('Ctrl Pts',(47.6975414659745,-2.09802529825852,3.1757420386404));
#88999=CARTESIAN_POINT('Ctrl Pts',(47.896388684714,-3.80584609838521,-0.0478544593189315));
#89000=CARTESIAN_POINT('Ctrl Pts',(48.0952359034538,-2.01768121316929,-3.22713239264578));
#89001=CARTESIAN_POINT('Ctrl Pts',(48.2940831221933,1.62385866935796,-3.44272221687208));
#89002=CARTESIAN_POINT('Ctrl Pts',(48.4929303409331,3.77380444199112,-0.494578024227625));
#89003=CARTESIAN_POINT('Ctrl Pts',(48.6917775596727,2.45711528607269,2.90534518289334));
#89004=CARTESIAN_POINT('Ctrl Pts',(48.8906247784123,-1.11643535726112,3.64136445027353));
#89005=CARTESIAN_POINT('Ctrl Pts',(49.089471997152,-3.66492661322599,1.02274087396531));
#89006=CARTESIAN_POINT('Ctrl Pts',(49.2220368096451,-3.11846394970298,-1.33452918861123));
#89007=CARTESIAN_POINT('Ctrl Pts',(49.2883192158916,-2.4066862419943,-2.13636896613036));
#89008=CARTESIAN_POINT('Ctrl Pts',(0.311212348987778,-1.53723282329044,
3.09685835129577));
#89009=CARTESIAN_POINT('Ctrl Pts',(0.377494755234326,-2.56901842462149,
2.58469585852276));
#89010=CARTESIAN_POINT('Ctrl Pts',(0.510059567727422,-4.06230121368214,
0.456641786001921));
#89011=CARTESIAN_POINT('Ctrl Pts',(0.708906786467066,-2.57795834828882,
-3.17766930833127));
#89012=CARTESIAN_POINT('Ctrl Pts',(0.907754005206709,1.27789992154481,-3.88312530093257));
#89013=CARTESIAN_POINT('Ctrl Pts',(1.10660122394635,3.95813182483745,-1.02656764819223));
#89014=CARTESIAN_POINT('Ctrl Pts',(1.30544844268599,3.00342840161775,2.7755327738099));
#89015=CARTESIAN_POINT('Ctrl Pts',(1.50429566142564,-0.710645173066041,
4.02675109516382));
#89016=CARTESIAN_POINT('Ctrl Pts',(1.70314288016528,-3.77168257203434,1.5797755668379));
#89017=CARTESIAN_POINT('Ctrl Pts',(1.90199009890492,-3.36826135439415,-2.3187138663657));
#89018=CARTESIAN_POINT('Ctrl Pts',(2.10083731764456,0.12924463646661,-4.08708974316909));
#89019=CARTESIAN_POINT('Ctrl Pts',(2.29968453638421,3.50799315213455,-2.10124824565113));
#89020=CARTESIAN_POINT('Ctrl Pts',(2.49853175512385,3.66438981334077,1.81480890460361));
#89021=CARTESIAN_POINT('Ctrl Pts',(2.6973789738635,0.45474319704599,4.06379255528071));
#89022=CARTESIAN_POINT('Ctrl Pts',(2.89622619260314,-3.17261606634541,2.57987380459977));
#89023=CARTESIAN_POINT('Ctrl Pts',(3.09507341134279,-3.88567786872364,-1.27387162418561));
#89024=CARTESIAN_POINT('Ctrl Pts',(3.29392063008242,-1.02943414864856,-3.95746078059767));
#89025=CARTESIAN_POINT('Ctrl Pts',(3.49276784882208,2.77242596493276,-3.00580953731097));
#89026=CARTESIAN_POINT('Ctrl Pts',(3.69161506756171,4.02759274580539,0.706917854313252));
#89027=CARTESIAN_POINT('Ctrl Pts',(3.89046228630136,1.58309510844274,3.77028442663091));
#89028=CARTESIAN_POINT('Ctrl Pts',(4.089309505041,-2.31560117140205,3.37034522410938));
#89029=CARTESIAN_POINT('Ctrl Pts',(4.28815672378064,-4.08723368983554,-0.125524233587091));
#89030=CARTESIAN_POINT('Ctrl Pts',(4.48700394252029,-2.1044170121688,-3.50608962159895));
#89031=CARTESIAN_POINT('Ctrl Pts',(4.68585116125993,1.81147402279106,-3.66603292376414));
#89032=CARTESIAN_POINT('Ctrl Pts',(4.88469837999958,4.06338212434606,-0.458433435021463));
#89033=CARTESIAN_POINT('Ctrl Pts',(5.08354559873922,2.58275061397783,3.17027360782739));
#89034=CARTESIAN_POINT('Ctrl Pts',(5.28239281747886,-1.27034271763307,3.88683224259547));
#89035=CARTESIAN_POINT('Ctrl Pts',(5.48124003621851,-3.95652524453957,1.03302637235576));
#89036=CARTESIAN_POINT('Ctrl Pts',(5.68008725495814,-3.00832470456206,-2.76969636717897));
#89037=CARTESIAN_POINT('Ctrl Pts',(5.8789344736978,0.703261303022831,-4.02823274363765));
#89038=CARTESIAN_POINT('Ctrl Pts',(6.07778169243743,3.76884587948186,-1.58651701313895));
#89039=CARTESIAN_POINT('Ctrl Pts',(6.27662891117708,3.37244581092541,2.31254075605715));
#89040=CARTESIAN_POINT('Ctrl Pts',(6.47547612991672,-0.121813917185409,
4.08734594401073));
#89041=CARTESIAN_POINT('Ctrl Pts',(6.67432334865637,-3.5041778755475,2.107598850067));
#89042=CARTESIAN_POINT('Ctrl Pts',(6.87317056739601,-3.66767579740066,-1.80814538724816));
#89043=CARTESIAN_POINT('Ctrl Pts',(7.07201778613565,-0.462121839925715,
-4.06296429979165));
#89044=CARTESIAN_POINT('Ctrl Pts',(7.2708650048753,3.1679277761891,-2.58562740957428));
#89045=CARTESIAN_POINT('Ctrl Pts',(7.46971222361494,3.88798381120942,1.26681386954273));
#89046=CARTESIAN_POINT('Ctrl Pts',(7.66855944235458,1.03661753696874,3.95558587043034));
#89047=CARTESIAN_POINT('Ctrl Pts',(7.86740666109425,-2.766964378456,3.01083769483692));
#89048=CARTESIAN_POINT('Ctrl Pts',(8.06625387983386,-4.02886947885365,-0.699604330073128));
#89049=CARTESIAN_POINT('Ctrl Pts',(8.26510109857353,-1.58993758080563,-3.7674041441606));
#89050=CARTESIAN_POINT('Ctrl Pts',(8.46394831731315,2.30947841958156,-3.37454366185755));
#89051=CARTESIAN_POINT('Ctrl Pts',(8.6627955360528,4.08745483818023,0.118103522949025));
#89052=CARTESIAN_POINT('Ctrl Pts',(8.86164275479245,2.11077894699056,3.5022632301467));
#89053=CARTESIAN_POINT('Ctrl Pts',(9.06048997353207,-1.8048152595142,3.66931565490361));
#89054=CARTESIAN_POINT('Ctrl Pts',(9.25933719227176,-4.06254312837073,0.465809860805664));
#89055=CARTESIAN_POINT('Ctrl Pts',(9.45818441101136,-2.58850207391776,-3.16557933238444));
#89056=CARTESIAN_POINT('Ctrl Pts',(9.65703162975104,1.26328397723694,-3.88913217686831));
#89057=CARTESIAN_POINT('Ctrl Pts',(9.85587884849066,3.95464323694529,-1.04020784691275));
#89058=CARTESIAN_POINT('Ctrl Pts',(10.0547260672303,3.01334820398965,2.76423010941716));
#89059=CARTESIAN_POINT('Ctrl Pts',(10.25357328597,-0.695946780579781,4.02950289426584));
#89060=CARTESIAN_POINT('Ctrl Pts',(10.4524205047096,-3.76595930439009,1.59335683824238));
#89061=CARTESIAN_POINT('Ctrl Pts',(10.6512677234492,-3.37663873203523,-2.30641417998059));
#89062=CARTESIAN_POINT('Ctrl Pts',(10.8501149421889,0.114393031384766,-4.08756036416182));
#89063=CARTESIAN_POINT('Ctrl Pts',(11.0489621609285,3.50034569876179,-2.11395730454897));
#89064=CARTESIAN_POINT('Ctrl Pts',(11.2478093796682,3.67095248876026,1.80148364454438));
#89065=CARTESIAN_POINT('Ctrl Pts',(11.4466565984078,0.469497497842897,4.06211860927464));
#89066=CARTESIAN_POINT('Ctrl Pts',(11.6455038171475,-3.16322828003209,2.59137460524359));
#89067=CARTESIAN_POINT('Ctrl Pts',(11.8443510358871,-3.89027733774591,-1.25975304394023));
#89068=CARTESIAN_POINT('Ctrl Pts',(12.0431982546268,-1.0437972996892,-3.95369734469618));
#89069=CARTESIAN_POINT('Ctrl Pts',(12.2420454733664,2.76149356255603,-3.01585623003779));
#89070=CARTESIAN_POINT('Ctrl Pts',(12.4408926921061,4.03013298922653,0.692288657601849));
#89071=CARTESIAN_POINT('Ctrl Pts',(12.6397399108457,1.59677478269736,3.76451136133733));
#89072=CARTESIAN_POINT('Ctrl Pts',(12.8385871295853,-2.30334803981363,3.37873101974436));
#89073=CARTESIAN_POINT('Ctrl Pts',(13.037434348325,-4.08766252185056,-0.110682445556626));
#89074=CARTESIAN_POINT('Ctrl Pts',(13.2362815670646,-2.1171339201326,-3.49842528296947));
#89075=CARTESIAN_POINT('Ctrl Pts',(13.4351287858043,1.79815054508896,-3.67258629762356));
#89076=CARTESIAN_POINT('Ctrl Pts',(13.6339760045439,4.06169074285061,-0.473184747997776));
#89077=CARTESIAN_POINT('Ctrl Pts',(13.8328232232836,2.59424500118603,3.1608746210689));
#89078=CARTESIAN_POINT('Ctrl Pts',(14.0316704420232,-1.25622107256294,3.89141929289879));
#89079=CARTESIAN_POINT('Ctrl Pts',(14.2305176607629,-3.95274819446203,1.04738589234015));
#89080=CARTESIAN_POINT('Ctrl Pts',(14.4293648795025,-3.01836177091483,-2.7587547401275));
#89081=CARTESIAN_POINT('Ctrl Pts',(14.6282120982422,0.688629964153758,-4.03075976321656));
#89082=CARTESIAN_POINT('Ctrl Pts',(14.8270593169817,3.76306031619543,-1.60019141135405));
#89083=CARTESIAN_POINT('Ctrl Pts',(15.0259065357214,3.38082052326087,2.30028000160723));
#89084=CARTESIAN_POINT('Ctrl Pts',(15.2247537544611,-0.106971768522289,
4.08776131116228));
#89085=CARTESIAN_POINT('Ctrl Pts',(15.4236009732007,-3.49650198435228,2.12030879112374));
#89086=CARTESIAN_POINT('Ctrl Pts',(15.6224481919403,-3.67421708014717,-1.79481596389458));
#89087=CARTESIAN_POINT('Ctrl Pts',(15.82129541068,-0.476871608231848,-4.06125952945123));
#89088=CARTESIAN_POINT('Ctrl Pts',(16.0201426294196,3.15851835743435,-2.59711325937978));
#89089=CARTESIAN_POINT('Ctrl Pts',(16.2189898481593,3.89255804138596,1.25268806601546));
#89090=CARTESIAN_POINT('Ctrl Pts',(16.4178370668989,1.05097362190846,3.95179578702503));
#89091=CARTESIAN_POINT('Ctrl Pts',(16.6166842856386,-2.75601364438854,3.02086482455609));
#89092=CARTESIAN_POINT('Ctrl Pts',(16.8155315043782,-4.03138321571946,-0.684970703250532));
#89093=CARTESIAN_POINT('Ctrl Pts',(17.0143787231179,-1.60360672139697,-3.7616061701601));
#89094=CARTESIAN_POINT('Ctrl Pts',(17.2132259418575,2.29721006788957,-3.38290724086293));
#89095=CARTESIAN_POINT('Ctrl Pts',(17.4120731605971,4.08785673201563,0.103261003339431));
#89096=CARTESIAN_POINT('Ctrl Pts',(17.6109203793368,2.12348191490623,3.49457580449507));
#89097=CARTESIAN_POINT('Ctrl Pts',(17.8097675980764,-1.79147990370901,3.67584483498729));
#89098=CARTESIAN_POINT('Ctrl Pts',(18.0086148168161,-4.06082496943184,0.480558075507004));
#89099=CARTESIAN_POINT('Ctrl Pts',(18.2074620355557,-2.59997937746127,-3.15615949107014));
#89100=CARTESIAN_POINT('Ctrl Pts',(18.4063092542954,1.24915402720918,-3.89369358226904));
#89101=CARTESIAN_POINT('Ctrl Pts',(18.605156473035,3.95084012316994,-1.05456048543771));
#89102=CARTESIAN_POINT('Ctrl Pts',(18.8040036917746,3.02336538889901,2.75327027759783));
#89103=CARTESIAN_POINT('Ctrl Pts',(19.0028509105143,-0.681310877907465,
4.03200334622145));
#89104=CARTESIAN_POINT('Ctrl Pts',(19.2016981292539,-3.76014892442961,1.60702071001181));
#89105=CARTESIAN_POINT('Ctrl Pts',(19.4005453479936,-3.38499117083098,-2.29413824119044));
#89106=CARTESIAN_POINT('Ctrl Pts',(19.5993925667332,0.0995501530659145,
-4.08794878433189));
#89107=CARTESIAN_POINT('Ctrl Pts',(19.7982397854729,3.49264674498503,-2.1266532888653));
#89108=CARTESIAN_POINT('Ctrl Pts',(19.9970870042125,3.67746956080263,1.78814236728127));
#89109=CARTESIAN_POINT('Ctrl Pts',(20.1959342229522,0.484244146785501,4.06038706315052));
#89110=CARTESIAN_POINT('Ctrl Pts',(20.3947814416918,-3.15379802392003,2.60284335306874));
#89111=CARTESIAN_POINT('Ctrl Pts',(20.5936286604314,-3.89482591461231,-1.24561895905628));
#89112=CARTESIAN_POINT('Ctrl Pts',(20.7924758791711,-1.0581464799722,-3.94988120368429));
#89113=CARTESIAN_POINT('Ctrl Pts',(20.9913230979107,2.75052464201603,-3.02586346188301));
#89114=CARTESIAN_POINT('Ctrl Pts',(21.1901703166504,4.03262015421157,0.677650491140349));
#89115=CARTESIAN_POINT('Ctrl Pts',(21.38901753539,1.61043337438535,3.7586885802048));
#89116=CARTESIAN_POINT('Ctrl Pts',(21.5878647541296,-2.29106452404108,3.38707231144781));
#89117=CARTESIAN_POINT('Ctrl Pts',(21.7867119728693,-4.08803746803528,-0.0958392207596079));
#89118=CARTESIAN_POINT('Ctrl Pts',(21.9855591916089,-2.12982291038758,-3.49071480741183));
#89119=CARTESIAN_POINT('Ctrl Pts',(22.1844064103486,1.78480335736162,-3.67909125625429));
#89120=CARTESIAN_POINT('Ctrl Pts',(22.3832536290882,4.05994581096812,-0.487929819029873));
#89121=CARTESIAN_POINT('Ctrl Pts',(22.5821008478279,2.6057051838422,3.15143395792994));
#89122=CARTESIAN_POINT('Ctrl Pts',(22.7809480665675,-1.24208286446976,3.89595503748267));
#89123=CARTESIAN_POINT('Ctrl Pts',(22.9797952853071,-3.94891902935828,1.06173160255694));
#89124=CARTESIAN_POINT('Ctrl Pts',(23.1786425040468,-3.0283590414496,-2.74777673990566));
#89125=CARTESIAN_POINT('Ctrl Pts',(23.3774897227864,0.67398954596553,-4.0332336391815));
#89126=CARTESIAN_POINT('Ctrl Pts',(23.5763369415261,3.75722513868898,-1.61384471170543));
#89127=CARTESIAN_POINT('Ctrl Pts',(23.7751841602657,3.38915066099852,2.28798891897434));
#89128=CARTESIAN_POINT('Ctrl Pts',(23.9740313790054,-0.0921282094784277,
4.08812278305269));
#89129=CARTESIAN_POINT('Ctrl Pts',(24.172878597745,-3.48877999336747,2.13299077686121));
#89130=CARTESIAN_POINT('Ctrl Pts',(24.3717258164847,-3.68070992000593,-1.78146287670161));
#89131=CARTESIAN_POINT('Ctrl Pts',(24.5705730352243,-0.491615089202934,
-4.05950121324825));
#89132=CARTESIAN_POINT('Ctrl Pts',(24.769420253964,3.14906729504797,-2.60856486742333));
#89133=CARTESIAN_POINT('Ctrl Pts',(24.9682674727036,3.89708094994972,1.23854574636347));
#89134=CARTESIAN_POINT('Ctrl Pts',(25.1671146914432,1.06531585023767,3.94795360098474));
#89135=CARTESIAN_POINT('Ctrl Pts',(25.3659619101829,-2.74502657353107,3.03085212554231));
#89136=CARTESIAN_POINT('Ctrl Pts',(25.5648091289225,-4.03384380062572,-0.670328045399746));
#89137=CARTESIAN_POINT('Ctrl Pts',(25.7636563476621,-1.61725471916093,-3.75575860108816));
#89138=CARTESIAN_POINT('Ctrl Pts',(25.9625035664018,2.28491142852464,-3.39122621777043));
#89139=CARTESIAN_POINT('Ctrl Pts',(26.1613507851414,4.0882047293138,0.0884171222803186));
#89140=CARTESIAN_POINT('Ctrl Pts',(26.3601980038811,2.13615688567587,3.48684230444618));
#89141=CARTESIAN_POINT('Ctrl Pts',(26.5590452226207,-1.77812092805368,3.68232555072383));
#89142=CARTESIAN_POINT('Ctrl Pts',(26.7578924413604,-4.05905327035726,0.495299954268107));
#89143=CARTESIAN_POINT('Ctrl Pts',(26.9567396601,-2.61142240145579,-3.14669803722426));
#89144=CARTESIAN_POINT('Ctrl Pts',(27.1555868788397,1.23500760765211,-3.89820365108567));
#89145=CARTESIAN_POINT('Ctrl Pts',(27.3544340975793,3.94698491935925,-1.06889922006086));
#89146=CARTESIAN_POINT('Ctrl Pts',(27.5532813163189,3.03334271210678,2.74227414515849));
#89147=CARTESIAN_POINT('Ctrl Pts',(27.7521285350586,-0.666665992460189,
4.03445063804146));
#89148=CARTESIAN_POINT('Ctrl Pts',(27.9509757537983,-3.75428896861078,1.62066339394195));
#89149=CARTESIAN_POINT('Ctrl Pts',(28.1498229725379,-3.39329898005322,-2.28183205522795));
#89150=CARTESIAN_POINT('Ctrl Pts',(28.3486701912775,0.0847059622234647,
-4.08828330675111));
#89151=CARTESIAN_POINT('Ctrl Pts',(28.5475174100172,3.48490174224484,-2.13932123422241));
#89152=CARTESIAN_POINT('Ctrl Pts',(28.7463646287568,3.68393814707654,1.77477751417194));
#89153=CARTESIAN_POINT('Ctrl Pts',(28.9452118474964,0.498984411188661,4.05860198266432));
#89154=CARTESIAN_POINT('Ctrl Pts',(29.1440590662361,-3.14432618641123,2.61427778358472));
#89155=CARTESIAN_POINT('Ctrl Pts',(29.3429062849758,-3.89932313996533,-1.23146845125119));
#89156=CARTESIAN_POINT('Ctrl Pts',(29.5417535037154,-1.07248170907375,-3.94601298528001));
#89157=CARTESIAN_POINT('Ctrl Pts',(29.740600722455,2.73951945705602,-3.0358307990907));
#89158=CARTESIAN_POINT('Ctrl Pts',(29.9394479411946,4.03505415092864,0.663003390164515));
#89159=CARTESIAN_POINT('Ctrl Pts',(30.1382951599344,1.62407073323958,3.75281624246787));
#89160=CARTESIAN_POINT('Ctrl Pts',(30.3371423786739,-2.27875080162179,3.39536894613885));
#89161=CARTESIAN_POINT('Ctrl Pts',(30.5359895974136,-4.08835851529988,-0.0809947323659286));
#89162=CARTESIAN_POINT('Ctrl Pts',(30.7348368161532,-2.14248381989336,-3.48295830836248));
#89163=CARTESIAN_POINT('Ctrl Pts',(30.9336840348929,1.77143263781142,-3.68554770773524));
#89164=CARTESIAN_POINT('Ctrl Pts',(31.1325312536326,4.05814735054126,-0.502668456928601));
#89165=CARTESIAN_POINT('Ctrl Pts',(31.3313784723722,2.61713101145724,3.14195174456338));
#89166=CARTESIAN_POINT('Ctrl Pts',(31.5302256911118,-1.22792828007724,3.90043941566621));
#89167=CARTESIAN_POINT('Ctrl Pts',(31.7290729098515,-3.94503779954791,1.07606331432411));
#89168=CARTESIAN_POINT('Ctrl Pts',(31.9279201285911,-3.03831638444379,-2.73676251149355));
#89169=CARTESIAN_POINT('Ctrl Pts',(32.1267673473308,0.659340241530767,-4.03565433878998));
#89170=CARTESIAN_POINT('Ctrl Pts',(32.3256145660704,3.75134042387302,-1.62747673424613));
#89171=CARTESIAN_POINT('Ctrl Pts',(32.52446178481,3.39743611432164,2.27566767024519));
#89172=CARTESIAN_POINT('Ctrl Pts',(32.7233090035497,-0.0772834357659036,
4.0884303548981));
#89173=CARTESIAN_POINT('Ctrl Pts',(32.9221562222893,-3.48101200440053,2.14564464008266));
#89174=CARTESIAN_POINT('Ctrl Pts',(33.121003441029,-3.68715423137363,-1.7680863017284));
#89175=CARTESIAN_POINT('Ctrl Pts',(33.3198506597686,-0.506352088452131,
-4.05768937436273));
#89176=CARTESIAN_POINT('Ctrl Pts',(33.5186978785082,3.13957471363731,-2.61998208272218));
#89177=CARTESIAN_POINT('Ctrl Pts',(33.7175450972479,3.90155247726848,1.22438709704741));
#89178=CARTESIAN_POINT('Ctrl Pts',(33.9163923159875,1.0796440328606,3.94405936296661));
#89179=CARTESIAN_POINT('Ctrl Pts',(34.1152395347272,-2.73400331074305,3.04079946611777));
#89180=CARTESIAN_POINT('Ctrl Pts',(34.3140867534668,-4.03625120113083,-0.655676549577613));
#89181=CARTESIAN_POINT('Ctrl Pts',(34.5129339722065,-1.63088139415487,-3.7498615140423));
#89182=CARTESIAN_POINT('Ctrl Pts',(34.7117811909461,2.27258266363874,-3.39950048289815));
#89183=CARTESIAN_POINT('Ctrl Pts',(34.9106284096858,4.08849882548661,0.0735720754816196));
#89184=CARTESIAN_POINT('Ctrl Pts',(35.1094756284254,2.14880369218564,3.47906283196285));
#89185=CARTESIAN_POINT('Ctrl Pts',(35.3083228471651,-1.76473850868036,3.68875771666786));
#89186=CARTESIAN_POINT('Ctrl Pts',(35.5071700659047,-4.05722805450612,0.510035302723816));
#89187=CARTESIAN_POINT('Ctrl Pts',(35.7060172846443,-2.62283099503016,-3.13719509559179));
#89188=CARTESIAN_POINT('Ctrl Pts',(35.904864503384,1.22084490507974,-3.90266232385494));
#89189=CARTESIAN_POINT('Ctrl Pts',(36.1037117221236,3.94307767634231,-1.08322386173262));
#89190=CARTESIAN_POINT('Ctrl Pts',(36.3025589408633,3.04328004206655,2.73124185707811));
#89191=CARTESIAN_POINT('Ctrl Pts',(36.501406159603,-0.65201231732407,4.03684473745941));
#89192=CARTESIAN_POINT('Ctrl Pts',(36.7002533783425,-3.74837951419443,1.63428471016025));
#89193=CARTESIAN_POINT('Ctrl Pts',(36.8991005970822,-3.40156205016727,-2.26949578434459));
#89194=CARTESIAN_POINT('Ctrl Pts',(37.0979478158218,0.0698606545712825,
-4.08856392700898));
#89195=CARTESIAN_POINT('Ctrl Pts',(37.2967950345615,3.47711079265562,-2.15196097359922));
#89196=CARTESIAN_POINT('Ctrl Pts',(37.4956422533011,3.69035816229659,1.76138926142602));
#89197=CARTESIAN_POINT('Ctrl Pts',(37.6944894720408,0.513718096708562,4.05676339135156));
#89198=CARTESIAN_POINT('Ctrl Pts',(37.8933366907804,-3.13481289238768,2.62567774603361));
#89199=CARTESIAN_POINT('Ctrl Pts',(38.0921839095201,-3.90376895451103,-1.21730170709314));
#89200=CARTESIAN_POINT('Ctrl Pts',(38.2910311282597,-1.08680279799026,-3.94209274048399));
#89201=CARTESIAN_POINT('Ctrl Pts',(38.4898783469994,2.72847815277427,-3.04575811024604));
#89202=CARTESIAN_POINT('Ctrl Pts',(38.688725565739,4.03743494728661,0.648347547789554));
#89203=CARTESIAN_POINT('Ctrl Pts',(38.8875727844787,1.63768667945778,3.74689442555066));
#89204=CARTESIAN_POINT('Ctrl Pts',(39.0864200032183,-2.26640703490652,3.40362081443016));
#89205=CARTESIAN_POINT('Ctrl Pts',(39.2852672219579,-4.08862565941151,-0.0661491760933774));
#89206=CARTESIAN_POINT('Ctrl Pts',(39.4841144406975,-2.15511648172164,-3.47515588808729));
#89207=CARTESIAN_POINT('Ctrl Pts',(39.6829616594372,1.75803856272522,-3.69195556694108));
#89208=CARTESIAN_POINT('Ctrl Pts',(39.8818088781768,4.05629538528197,-0.517400467371642));
#89209=CARTESIAN_POINT('Ctrl Pts',(40.0806560969165,2.62852233338666,3.132428105988));
#89210=CARTESIAN_POINT('Ctrl Pts',(40.2795033156561,-1.21375750600731,3.90487236832485));
#89211=CARTESIAN_POINT('Ctrl Pts',(40.4783505343958,-3.94110455620326,1.09038083868435));
#89212=CARTESIAN_POINT('Ctrl Pts',(40.6771977531354,-3.04823366861422,-2.72571220010894));
#89213=CARTESIAN_POINT('Ctrl Pts',(40.8760449718751,0.64468224399396,-4.03802183012611));
#89214=CARTESIAN_POINT('Ctrl Pts',(41.0748921906147,3.74540624933471,-1.64108729924416));
#89215=CARTESIAN_POINT('Ctrl Pts',(41.2737394093544,3.40567677399036,2.26331641786971));
#89216=CARTESIAN_POINT('Ctrl Pts',(41.472586628094,-0.0624376431062618,
4.08868402264345));
#89217=CARTESIAN_POINT('Ctrl Pts',(41.6714338468336,-3.47319811986895,2.15827021395247));
#89218=CARTESIAN_POINT('Ctrl Pts',(41.8702810655733,-3.69354992928488,-1.75468641533891));
#89219=CARTESIAN_POINT('Ctrl Pts',(42.0691282843129,-0.521082411678686,
-4.05582403668333));
#89220=CARTESIAN_POINT('Ctrl Pts',(42.2679755030526,3.13004073835791,-2.63136475474465));
#89221=CARTESIAN_POINT('Ctrl Pts',(42.4668227217923,3.90597256438712,1.21021230474138));
#89222=CARTESIAN_POINT('Ctrl Pts',(42.6656699405318,1.09395798086656,3.94011312431713));
#89223=CARTESIAN_POINT('Ctrl Pts',(42.8645171592716,-2.72294400136152,3.05070671512597));
#89224=CARTESIAN_POINT('Ctrl Pts',(43.0633643780111,-4.03860538549387,-0.641016408947679));
#89225=CARTESIAN_POINT('Ctrl Pts',(43.2622115967508,-1.64448656671789,-3.74391498679197));
#89226=CARTESIAN_POINT('Ctrl Pts',(43.4610588154904,2.26022393578235,-3.40772992711721));
#89227=CARTESIAN_POINT('Ctrl Pts',(43.6599060342301,4.08873901665392,0.0587260585986082));
#89228=CARTESIAN_POINT('Ctrl Pts',(43.8587532529697,2.16142216769827,3.47123748974718));
#89229=CARTESIAN_POINT('Ctrl Pts',(44.0576004717093,-1.75133282203951,3.69514124775901));
#89230=CARTESIAN_POINT('Ctrl Pts',(44.2564476904491,-4.05534934592483,0.524763927083821));
#89231=CARTESIAN_POINT('Ctrl Pts',(44.4552949091886,-2.63420500780209,-3.1276507923989));
#89232=CARTESIAN_POINT('Ctrl Pts',(44.6541421279284,1.20666610628738,-3.90706954000401));
#89233=CARTESIAN_POINT('Ctrl Pts',(44.8529893466679,3.93911844550736,-1.09753422500833));
#89234=CARTESIAN_POINT('Ctrl Pts',(45.0518365654076,3.0531772480021,2.72017356535418));
#89235=CARTESIAN_POINT('Ctrl Pts',(45.2506837841472,-0.637350046166439,
4.03918560039532));
#89236=CARTESIAN_POINT('Ctrl Pts',(45.4495310028869,-3.74242063820434,1.6478845030179));
#89237=CARTESIAN_POINT('Ctrl Pts',(45.6483782216265,-3.40978027393047,-2.25712963699257));
#89238=CARTESIAN_POINT('Ctrl Pts',(45.8472254403661,0.0550144290946424,
-4.08879055377777));
#89239=CARTESIAN_POINT('Ctrl Pts',(46.0460726591059,3.46927399270728,-2.16457250798764));
#89240=CARTESIAN_POINT('Ctrl Pts',(46.2449198778454,3.69672953373671,1.74797810627639));
#89241=CARTESIAN_POINT('Ctrl Pts',(46.4437670965851,0.528444986286493,4.05487069989181));
#89242=CARTESIAN_POINT('Ctrl Pts',(46.6426143153247,-3.12525822365519,2.63704426391929));
#89243=CARTESIAN_POINT('Ctrl Pts',(46.8414615340643,-3.90816338308783,-1.20312115897968));
#89244=CARTESIAN_POINT('Ctrl Pts',(47.0403087528041,-1.10110939824789,-3.93811622488528));
#89245=CARTESIAN_POINT('Ctrl Pts',(47.2391559715436,2.71740056930501,-3.0556534833461));
#89246=CARTESIAN_POINT('Ctrl Pts',(47.4380031902834,4.03976309623561,0.63369888083219));
#89247=CARTESIAN_POINT('Ctrl Pts',(47.6368504090229,1.65127991561411,3.74089312665609));
#89248=CARTESIAN_POINT('Ctrl Pts',(47.8356976277626,-2.25403124795064,3.41188535546605));
#89249=CARTESIAN_POINT('Ctrl Pts',(48.0345448465023,-4.08884298858149,-0.051412843662276));
#89250=CARTESIAN_POINT('Ctrl Pts',(48.2333920652418,-2.16771289967819,-3.46709701753122));
#89251=CARTESIAN_POINT('Ctrl Pts',(48.4322392839815,1.74460631434076,-3.69871777107951));
#89252=CARTESIAN_POINT('Ctrl Pts',(48.6310865027212,4.05441876366472,-0.531354089049278));
#89253=CARTESIAN_POINT('Ctrl Pts',(48.8299337214608,2.63982261759276,3.12138220342728));
#89254=CARTESIAN_POINT('Ctrl Pts',(49.0287809402005,-1.19945178147874,3.91213073689135));
#89255=CARTESIAN_POINT('Ctrl Pts',(49.2276281589401,-3.93744494621396,1.09879031982473));
#89256=CARTESIAN_POINT('Ctrl Pts',(49.3601929714332,-3.35034815551191,-1.43376273628772));
#89257=CARTESIAN_POINT('Ctrl Pts',(49.4264753776797,-2.5856437469894,-2.29522609227205));
#89258=CARTESIAN_POINT('Ctrl Pts',(0.44936851077589,-1.6436277398265,3.31119802764001));
#89259=CARTESIAN_POINT('Ctrl Pts',(0.515650917022438,-2.74682525825521,
2.76358775828697));
#89260=CARTESIAN_POINT('Ctrl Pts',(0.648215729515534,-4.34346109527289,
0.488246864928335));
#89261=CARTESIAN_POINT('Ctrl Pts',(0.847062948255177,-2.75638393167717,
-3.39760207044552));
#89262=CARTESIAN_POINT('Ctrl Pts',(1.04591016699482,1.36634589630823,-4.15188406410229));
#89263=CARTESIAN_POINT('Ctrl Pts',(1.24475738573446,4.23208193750849,-1.09761842045847));
#89264=CARTESIAN_POINT('Ctrl Pts',(1.44360460447411,3.21130160681502,2.96763287298708));
#89265=CARTESIAN_POINT('Ctrl Pts',(1.64245182321375,-0.759830327539506,
4.30545048291438));
#89266=CARTESIAN_POINT('Ctrl Pts',(1.8412990419534,-4.03272816406958,1.68911495058811));
#89267=CARTESIAN_POINT('Ctrl Pts',(2.04014626069303,-3.60138536803899,-2.47919662769191));
#89268=CARTESIAN_POINT('Ctrl Pts',(2.23899347943268,0.138189912745784,-4.36996528779138));
#89269=CARTESIAN_POINT('Ctrl Pts',(2.43784069817232,3.75078827918065,-2.24667978232544));
#89270=CARTESIAN_POINT('Ctrl Pts',(2.63668791691197,3.91800946186683,1.94041540936253));
#89271=CARTESIAN_POINT('Ctrl Pts',(2.83553513565161,0.486216870884996,4.34505565556579));
#89272=CARTESIAN_POINT('Ctrl Pts',(3.03438235439126,-3.39219908361218,2.75843196049844));
#89273=CARTESIAN_POINT('Ctrl Pts',(3.2332295731309,-4.1546133001462,-1.36203879254129));
#89274=CARTESIAN_POINT('Ctrl Pts',(3.43207679187054,-1.10068331706675,-4.23136444897295));
#89275=CARTESIAN_POINT('Ctrl Pts',(3.63092401061018,2.96431103573806,-3.21384754560735));
#89276=CARTESIAN_POINT('Ctrl Pts',(3.82977122934983,4.30635038585737,0.75584503370213));
#89277=CARTESIAN_POINT('Ctrl Pts',(4.02861844808948,1.6926642442166,4.03123325026437));
#89278=CARTESIAN_POINT('Ctrl Pts',(4.22746566682911,-2.47586849696874,3.60361346648852));
#89279=CARTESIAN_POINT('Ctrl Pts',(4.42631288556876,-4.37011919729062,-0.134212013442915));
#89280=CARTESIAN_POINT('Ctrl Pts',(4.6251601043084,-2.25006786542551,-3.74875300154117));
#89281=CARTESIAN_POINT('Ctrl Pts',(4.82400732304805,1.93684971380027,-3.91976629520431));
#89282=CARTESIAN_POINT('Ctrl Pts',(5.02285454178769,4.34461681789642,-0.490162517511296));
#89283=CARTESIAN_POINT('Ctrl Pts',(5.22170176052733,2.76150787952927,3.38969449891865));
#89284=CARTESIAN_POINT('Ctrl Pts',(5.42054897926698,-1.35826564340401,4.15584757051117));
#89285=CARTESIAN_POINT('Ctrl Pts',(5.61939619800662,-4.23036416261854,1.10452416566391));
#89286=CARTESIAN_POINT('Ctrl Pts',(5.81824341674627,-3.21653679254611,-2.96139251713847));
#89287=CARTESIAN_POINT('Ctrl Pts',(6.01709063548591,0.751935405282821,-4.30703467920225));
#89288=CARTESIAN_POINT('Ctrl Pts',(6.21593785422555,4.02969513842899,-1.69632298568797));
#89289=CARTESIAN_POINT('Ctrl Pts',(6.41478507296519,3.60585943906238,2.47259626423985));
#89290=CARTESIAN_POINT('Ctrl Pts',(6.61363229170484,-0.13024489872292,4.37023922079874));
#89291=CARTESIAN_POINT('Ctrl Pts',(6.81247951044448,-3.74670893977377,2.25346992460214));
#89292=CARTESIAN_POINT('Ctrl Pts',(7.01132672918414,-3.92152287536647,-1.93329069682433));
#89293=CARTESIAN_POINT('Ctrl Pts',(7.21017394792375,-0.494106204195895,
-4.34417007488025));
#89294=CARTESIAN_POINT('Ctrl Pts',(7.40902116666343,3.38718630764454,-2.76458378382463));
#89295=CARTESIAN_POINT('Ctrl Pts',(7.60786838540304,4.15707884146084,1.35449255677521));
#89296=CARTESIAN_POINT('Ctrl Pts',(7.80671560414271,1.10836388186483,4.2293597725739));
#89297=CARTESIAN_POINT('Ctrl Pts',(8.00556282288234,-2.95847144208599,3.21922371183582));
#89298=CARTESIAN_POINT('Ctrl Pts',(8.20441004162199,-4.30771548411879,-0.748025326020356));
#89299=CARTESIAN_POINT('Ctrl Pts',(8.40325726036163,-1.69998029759137,-4.02815361776172));
#89300=CARTESIAN_POINT('Ctrl Pts',(8.60210447910126,2.46932197741505,-3.60810248639643));
#89301=CARTESIAN_POINT('Ctrl Pts',(8.80095169784093,4.37035565174856,0.12627770078113));
#89302=CARTESIAN_POINT('Ctrl Pts',(8.99979891658055,2.25687012230786,3.74466177798734));
#89303=CARTESIAN_POINT('Ctrl Pts',(9.19864613532021,-1.92973008437983,3.92327623064252));
#89304=CARTESIAN_POINT('Ctrl Pts',(9.39749335405985,-4.34371975335436,0.498049480277108));
#89305=CARTESIAN_POINT('Ctrl Pts',(9.59634057279949,-2.76765740935881,-3.38467532341086));
#89306=CARTESIAN_POINT('Ctrl Pts',(9.79518779153912,1.35071835365874,-4.15830668777264));
#89307=CARTESIAN_POINT('Ctrl Pts',(9.99403501027879,4.22835189756562,-1.11220268424345));
#89308=CARTESIAN_POINT('Ctrl Pts',(10.1928822290185,3.22190797828005,2.95554792889247));
#89309=CARTESIAN_POINT('Ctrl Pts',(10.3917294477581,-0.744114630310529,
4.30839273946131));
#89310=CARTESIAN_POINT('Ctrl Pts',(10.5905766664978,-4.02660877778014,1.70363620858125));
#89311=CARTESIAN_POINT('Ctrl Pts',(10.7894238852374,-3.61034256051451,-2.46604565574581));
#89312=CARTESIAN_POINT('Ctrl Pts',(10.988271103977,0.122310398775208,-4.37046848139152));
#89313=CARTESIAN_POINT('Ctrl Pts',(11.1871183227167,3.74261153047214,-2.26026846026354));
#89314=CARTESIAN_POINT('Ctrl Pts',(11.3859655414563,3.92502635299973,1.92616788176494));
#89315=CARTESIAN_POINT('Ctrl Pts',(11.584812760196,0.501992345949099,4.34326585245409));
#89316=CARTESIAN_POINT('Ctrl Pts',(11.7836599789356,-3.38216155008677,2.77072875424496));
#89317=CARTESIAN_POINT('Ctrl Pts',(11.9825071976753,-4.15953110749387,-1.34694303750231));
#89318=CARTESIAN_POINT('Ctrl Pts',(12.1813544164149,-1.11604057012827,-4.22734053824777));
#89319=CARTESIAN_POINT('Ctrl Pts',(12.3802016351546,2.95262198022411,-3.22458958975909));
#89320=CARTESIAN_POINT('Ctrl Pts',(12.5790488538942,4.30906644453736,0.74020332142411));
#89321=CARTESIAN_POINT('Ctrl Pts',(12.7778960726339,1.70729071571528,4.02506061973202));
#89322=CARTESIAN_POINT('Ctrl Pts',(12.9767432913735,-2.46276730196863,3.6125796595839));
#89323=CARTESIAN_POINT('Ctrl Pts',(13.1755905101131,-4.37057770961544,-0.118342995981215));
#89324=CARTESIAN_POINT('Ctrl Pts',(13.3744377288527,-2.26366493567891,-3.74055819891402));
#89325=CARTESIAN_POINT('Ctrl Pts',(13.5732849475924,1.92260409192027,-3.92677324099783));
#89326=CARTESIAN_POINT('Ctrl Pts',(13.772132166332,4.3428083725507,-0.505934797961845));
#89327=CARTESIAN_POINT('Ctrl Pts',(13.9709793850717,2.77379781595364,3.37964498974316));
#89328=CARTESIAN_POINT('Ctrl Pts',(14.1698266038113,-1.3431666114177,4.16075209961586));
#89329=CARTESIAN_POINT('Ctrl Pts',(14.368673822551,-4.22632569545333,1.11987753635658));
#89330=CARTESIAN_POINT('Ctrl Pts',(14.5675210412906,-3.22726854406347,-2.94969359849181));
#89331=CARTESIAN_POINT('Ctrl Pts',(14.7663682600303,0.736291402584172,-4.30973659879184));
#89332=CARTESIAN_POINT('Ctrl Pts',(14.9652154787699,4.02350914489306,-1.71094381598202));
#89333=CARTESIAN_POINT('Ctrl Pts',(15.1640626975095,3.61481378176121,2.45948691878498));
#89334=CARTESIAN_POINT('Ctrl Pts',(15.3629099162492,-0.114375495668469,
4.37068333633034));
#89335=CARTESIAN_POINT('Ctrl Pts',(15.5617571349889,-3.73850178500502,2.26705954575511));
#89336=CARTESIAN_POINT('Ctrl Pts',(15.7606043537285,-3.92851689319731,-1.91903871778258));
#89337=CARTESIAN_POINT('Ctrl Pts',(15.9594515724682,-0.50987683306659,-4.34234731402119));
#89338=CARTESIAN_POINT('Ctrl Pts',(16.1582987912078,3.37712564445375,-2.77686459195583));
#89339=CARTESIAN_POINT('Ctrl Pts',(16.3571460099474,4.16196966313251,1.33938907851674));
#89340=CARTESIAN_POINT('Ctrl Pts',(16.555993228687,1.12371357976661,4.22530737001858));
#89341=CARTESIAN_POINT('Ctrl Pts',(16.7548404474267,-2.94676278610879,3.22994483898557));
#89342=CARTESIAN_POINT('Ctrl Pts',(16.9536876661663,-4.31040320167247,-0.732378877014406));
#89343=CARTESIAN_POINT('Ctrl Pts',(17.152534884906,-1.71459550637115,-4.02195435454171));
#89344=CARTESIAN_POINT('Ctrl Pts',(17.3513821036456,2.45620450889799,-3.61704492520543));
#89345=CARTESIAN_POINT('Ctrl Pts',(17.5502293223853,4.37078536144919,0.110407901106263));
#89346=CARTESIAN_POINT('Ctrl Pts',(17.7490765411249,2.27045228769491,3.73644229043969));
#89347=CARTESIAN_POINT('Ctrl Pts',(17.9479237598646,-1.91547176228979,3.93025730816134));
#89348=CARTESIAN_POINT('Ctrl Pts',(18.1467709786042,-4.34188267724551,0.513818448014967));
#89349=CARTESIAN_POINT('Ctrl Pts',(18.3456181973439,-2.77992907972437,-3.37460351629462));
#89350=CARTESIAN_POINT('Ctrl Pts',(18.5444654160835,1.33561044191232,-4.16318379704042));
#89351=CARTESIAN_POINT('Ctrl Pts',(18.7433126348231,4.22428556278263,-1.12754869719732));
#89352=CARTESIAN_POINT('Ctrl Pts',(18.9421598535628,3.23261847232007,2.94382954549006));
#89353=CARTESIAN_POINT('Ctrl Pts',(19.1410070723024,-0.728465747938811,
4.31106625262998));
#89354=CARTESIAN_POINT('Ctrl Pts',(19.3398542910421,-4.02039624995918,1.71824578387354));
#89355=CARTESIAN_POINT('Ctrl Pts',(19.5387015097817,-3.619273088078,-2.45292007501254));
#89356=CARTESIAN_POINT('Ctrl Pts',(19.7375487285213,0.106440215564113,-4.37088378488787));
#89357=CARTESIAN_POINT('Ctrl Pts',(19.936395947261,3.73437971691508,-2.27384315870254));
#89358=CARTESIAN_POINT('Ctrl Pts',(20.1352431660006,3.93199448445579,1.91190322838119));
#89359=CARTESIAN_POINT('Ctrl Pts',(20.3340903847403,0.517759639558971,4.34141446260651));
#89360=CARTESIAN_POINT('Ctrl Pts',(20.5329376034799,-3.37207860734407,2.78299127673401));
#89361=CARTESIAN_POINT('Ctrl Pts',(20.7317848222196,-4.16439450033916,-1.33183070471814));
#89362=CARTESIAN_POINT('Ctrl Pts',(20.9306320409592,-1.13138288548842,-4.22326027458752));
#89363=CARTESIAN_POINT('Ctrl Pts',(21.1294792596989,2.94089387905273,-3.23528944186379));
#89364=CARTESIAN_POINT('Ctrl Pts',(21.3283264784385,4.31172575111801,0.724552018581892));
#89365=CARTESIAN_POINT('Ctrl Pts',(21.5271736971781,1.72189464548128,4.01883483242943));
#89366=CARTESIAN_POINT('Ctrl Pts',(21.7260209159178,-2.44963361983509,3.62149826854283));
#89367=CARTESIAN_POINT('Ctrl Pts',(21.9248681346574,-4.37097860656534,-0.102472442311512));
#89368=CARTESIAN_POINT('Ctrl Pts',(22.1237153533971,-2.27723215598379,-3.73231406613089));
#89369=CARTESIAN_POINT('Ctrl Pts',(22.3225625721367,1.90833311899741,-3.93372842064914));
#89370=CARTESIAN_POINT('Ctrl Pts',(22.5214097908764,4.34094267049002,-0.521700404450909));
#89371=CARTESIAN_POINT('Ctrl Pts',(22.720257009616,2.78605118046146,3.3695509196827));
#89372=CARTESIAN_POINT('Ctrl Pts',(22.9191042283557,-1.32804987004886,4.16560177203107));
#89373=CARTESIAN_POINT('Ctrl Pts',(23.1179514470953,-4.2222315062781,1.13521614148041));
#89374=CARTESIAN_POINT('Ctrl Pts',(23.3167986658349,-3.23795774541576,-2.93795578921591));
#89375=CARTESIAN_POINT('Ctrl Pts',(23.5156458845746,0.720637692168774,-4.31238169659305));
#89376=CARTESIAN_POINT('Ctrl Pts',(23.7144931033142,4.01727010323906,-1.72554208818758));
#89377=CARTESIAN_POINT('Ctrl Pts',(23.9133403220539,3.62372046476637,2.44634514607375));
#89378=CARTESIAN_POINT('Ctrl Pts',(24.1121875407935,-0.098504584618038,
4.37106982640343));
#89379=CARTESIAN_POINT('Ctrl Pts',(24.3110347595331,-3.73024533978929,2.280619276746));
#89380=CARTESIAN_POINT('Ctrl Pts',(24.5098819782728,-3.93545911531253,-1.90476143708042));
#89381=CARTESIAN_POINT('Ctrl Pts',(24.7087291970124,-0.525640739443385,
-4.3404673012848));
#89382=CARTESIAN_POINT('Ctrl Pts',(24.9075764157521,3.36702045539343,-2.78910878838517));
#89383=CARTESIAN_POINT('Ctrl Pts',(25.1064236344917,4.16680561112128,1.32426794101998));
#89384=CARTESIAN_POINT('Ctrl Pts',(25.3052708532314,1.13904846201456,4.22119925870213));
#89385=CARTESIAN_POINT('Ctrl Pts',(25.504118071971,-2.93501527840068,3.24062338077717));
#89386=CARTESIAN_POINT('Ctrl Pts',(25.7029652907107,-4.31303408851464,-0.716722771924983));
#89387=CARTESIAN_POINT('Ctrl Pts',(25.9018125094503,-1.72918810898676,-4.01570206367753));
#89388=CARTESIAN_POINT('Ctrl Pts',(26.1006597281899,2.44305465643839,-3.62593967491736));
#89389=CARTESIAN_POINT('Ctrl Pts',(26.2995069469296,4.37115744432694,0.0945366457532685));
#89390=CARTESIAN_POINT('Ctrl Pts',(26.4983541656693,2.28400451819822,3.72817353959486));
#89391=CARTESIAN_POINT('Ctrl Pts',(26.6972013844089,-1.90118818557316,3.93718656701993));
#89392=CARTESIAN_POINT('Ctrl Pts',(26.8960486031485,-4.33998835538258,0.529580641289662));
#89393=CARTESIAN_POINT('Ctrl Pts',(27.0948958218882,-2.79216409798571,-3.36448721656139));
#89394=CARTESIAN_POINT('Ctrl Pts',(27.2937430406278,1.32048492074795,-4.16800601661785));
#89395=CARTESIAN_POINT('Ctrl Pts',(27.4925902593675,4.2201635327102,-1.1428798439329));
#89396=CARTESIAN_POINT('Ctrl Pts',(27.6914374781071,3.24328634575149,2.93207234903013));
#89397=CARTESIAN_POINT('Ctrl Pts',(27.8902846968467,-0.71280726107655,4.31368292634515));
#89398=CARTESIAN_POINT('Ctrl Pts',(28.0891319155864,-4.01413071503691,1.7328327048744));
#89399=CARTESIAN_POINT('Ctrl Pts',(28.287979134326,-3.62815589716714,-2.43976215364049));
#89400=CARTESIAN_POINT('Ctrl Pts',(28.4868263530657,0.0905686289870616,
-4.37124146026373));
#89401=CARTESIAN_POINT('Ctrl Pts',(28.6856735718053,3.72609866725499,-2.28738787755066));
#89402=CARTESIAN_POINT('Ctrl Pts',(28.884520790545,3.93891077434772,1.89761336742039));
#89403=CARTESIAN_POINT('Ctrl Pts',(29.0833680092846,0.533520106742824,4.33950583317804));
#89404=CARTESIAN_POINT('Ctrl Pts',(29.2822152280243,-3.36195120527411,2.79521710674521));
#89405=CARTESIAN_POINT('Ctrl Pts',(29.4810624467639,-4.16920298753154,-1.31670081235005));
#89406=CARTESIAN_POINT('Ctrl Pts',(29.6799096655036,-1.14671028407833,-4.21912432915579));
#89407=CARTESIAN_POINT('Ctrl Pts',(29.8787568842432,2.92912700352929,-3.24594663814438));
#89408=CARTESIAN_POINT('Ctrl Pts',(30.0776041029828,4.31432820954993,0.708891162849975));
#89409=CARTESIAN_POINT('Ctrl Pts',(30.2764513217225,1.73647587284724,4.01255605861208));
#89410=CARTESIAN_POINT('Ctrl Pts',(30.4752985404621,-2.43646764039318,3.63036912968944));
#89411=CARTESIAN_POINT('Ctrl Pts',(30.6741457592018,-4.37132187414452,-0.086600537589134));
#89412=CARTESIAN_POINT('Ctrl Pts',(30.8729929779414,-2.29076935201543,-3.72402072447939));
#89413=CARTESIAN_POINT('Ctrl Pts',(31.071840196681,1.89403698556779,-3.94063173587515));
#89414=CARTESIAN_POINT('Ctrl Pts',(31.2706874154207,4.33901973506879,-0.537459132556749));
#89415=CARTESIAN_POINT('Ctrl Pts',(31.4695346341603,2.79826781214797,3.3594124236214));
#89416=CARTESIAN_POINT('Ctrl Pts',(31.6683818529,-1.31291561894468,4.170396522876));
#89417=CARTESIAN_POINT('Ctrl Pts',(31.8672290716396,-4.21808164889521,1.15053977929429));
#89418=CARTESIAN_POINT('Ctrl Pts',(32.0660762903793,-3.2486042557636,-2.92617924432523));
#89419=CARTESIAN_POINT('Ctrl Pts',(32.2649235091189,0.704974480472183,-4.31496993759728));
#89420=CARTESIAN_POINT('Ctrl Pts',(32.4637707278585,4.01097809570062,-1.7401176099032));
#89421=CARTESIAN_POINT('Ctrl Pts',(32.6626179465982,3.63257937066049,2.43317111941123));
#89422=CARTESIAN_POINT('Ctrl Pts',(32.8614651653378,-0.0826323748293277,
4.37139868590308));
#89423=CARTESIAN_POINT('Ctrl Pts',(33.0603123840775,-3.72193971298034,2.29414893880605));
#89424=CARTESIAN_POINT('Ctrl Pts',(33.2591596028171,-3.94234945018409,-1.8904590429624));
#89425=CARTESIAN_POINT('Ctrl Pts',(33.4580068215568,-0.541397715485528,
-4.3385300614554));
#89426=CARTESIAN_POINT('Ctrl Pts',(33.6568540402964,3.35687087369524,-2.80131621168008));
#89427=CARTESIAN_POINT('Ctrl Pts',(33.8557012590361,4.17158662166775,1.30912934365088));
#89428=CARTESIAN_POINT('Ctrl Pts',(34.0545484777757,1.15436832642516,4.21703549278773));
#89429=CARTESIAN_POINT('Ctrl Pts',(34.2533956965153,-2.9232290738471,3.25125919641916));
#89430=CARTESIAN_POINT('Ctrl Pts',(34.452242915255,-4.3156081099583,-0.701057217170789));
#89431=CARTESIAN_POINT('Ctrl Pts',(34.6510901339946,-1.74375791304135,-4.00939682760275));
#89432=CARTESIAN_POINT('Ctrl Pts',(34.8499373527343,2.42987259341109,-3.63478661825904));
#89433=CARTESIAN_POINT('Ctrl Pts',(35.0487845714739,4.3714718954761,0.0786641439775557));
#89434=CARTESIAN_POINT('Ctrl Pts',(35.2476317902135,2.29752663513765,3.71985563447269));
#89435=CARTESIAN_POINT('Ctrl Pts',(35.4464790089532,-1.88687954255259,3.94406391585908));
#89436=CARTESIAN_POINT('Ctrl Pts',(35.6453262276928,-4.33803681274136,0.545335852283642));
#89437=CARTESIAN_POINT('Ctrl Pts',(35.8441734464325,-2.80436230282958,-3.35432655758999));
#89438=CARTESIAN_POINT('Ctrl Pts',(36.0430206651721,1.30534198958868,-4.17277328292609));
#89439=CARTESIAN_POINT('Ctrl Pts',(36.2418678839118,4.21598586169539,-1.15819592231613));
#89440=CARTESIAN_POINT('Ctrl Pts',(36.4407151026514,3.25391145792333,2.92027649452588));
#89441=CARTESIAN_POINT('Ctrl Pts',(36.639562321391,-0.697139376173743,4.31624272610719));
#89442=CARTESIAN_POINT('Ctrl Pts',(36.8384095401307,-4.00781225562154,1.74739677926192));
#89443=CARTESIAN_POINT('Ctrl Pts',(37.0372567588703,-3.63699087066615,-2.42657206511082));
#89444=CARTESIAN_POINT('Ctrl Pts',(37.23610397761,0.0746958483036821,-4.37154150280327));
#89445=CARTESIAN_POINT('Ctrl Pts',(37.4349511963496,3.71776849067378,-2.30090243822691));
#89446=CARTESIAN_POINT('Ctrl Pts',(37.6337984150893,3.94577513148733,1.88329848728799));
#89447=CARTESIAN_POINT('Ctrl Pts',(37.8326456338289,0.549273539705922,4.33753998933313));
#89448=CARTESIAN_POINT('Ctrl Pts',(38.0314928525686,-3.35177947740222,2.80740608308638));
#89449=CARTESIAN_POINT('Ctrl Pts',(38.2303400713082,-4.17395650567318,-1.30155355987898));
#89450=CARTESIAN_POINT('Ctrl Pts',(38.4291872900478,-1.16202256381311,-4.21493275648311));
#89451=CARTESIAN_POINT('Ctrl Pts',(38.6280345087875,2.91732150879461,-3.25656103809055));
#89452=CARTESIAN_POINT('Ctrl Pts',(38.8268817275271,4.31687378552097,0.693220960709451));
#89453=CARTESIAN_POINT('Ctrl Pts',(39.0257289462668,1.75103420556635,4.00622438106276));
#89454=CARTESIAN_POINT('Ctrl Pts',(39.2245761650064,-2.4232695372303,3.63919212606545));
#89455=CARTESIAN_POINT('Ctrl Pts',(39.4234233837461,-4.37160750782718,-0.0707274910778739));
#89456=CARTESIAN_POINT('Ctrl Pts',(39.6222706024857,-2.30427634529205,-3.71567828330342));
#89457=CARTESIAN_POINT('Ctrl Pts',(39.8211178212254,1.87971588011944,-3.94748309565882));
#89458=CARTESIAN_POINT('Ctrl Pts',(40.0199650399649,4.33703959164013,-0.553210774507616));
#89459=CARTESIAN_POINT('Ctrl Pts',(40.2188122587047,2.81044754994229,3.34922963523084));
#89460=CARTESIAN_POINT('Ctrl Pts',(40.4176594774443,-1.29776405764359,4.175136288934));
#89461=CARTESIAN_POINT('Ctrl Pts',(40.6165066961839,-4.2138761780187,1.16584824776282));
#89462=CARTESIAN_POINT('Ctrl Pts',(40.8153539149236,-3.25920793473749,-2.9143641190883));
#89463=CARTESIAN_POINT('Ctrl Pts',(41.0142011336632,0.689301974006816,-4.31750128767965));
#89464=CARTESIAN_POINT('Ctrl Pts',(41.2130483524029,4.00463320523487,-1.75467018895728));
#89465=CARTESIAN_POINT('Ctrl Pts',(41.4118955711425,3.64139038264304,2.41996501249082));
#89466=CARTESIAN_POINT('Ctrl Pts',(41.6107427898821,-0.0667590755701654,
4.37166991049355));
#89467=CARTESIAN_POINT('Ctrl Pts',(41.8095900086218,-3.71358501408416,2.30764835355263));
#89468=CARTESIAN_POINT('Ctrl Pts',(42.0084372273614,-3.94918780696598,-1.87613172399901));
#89469=CARTESIAN_POINT('Ctrl Pts',(42.2072844461011,-0.55714755344433,-4.33653562007506));
#89470=CARTESIAN_POINT('Ctrl Pts',(42.4061316648407,3.34667703317699,-2.81348670089032));
#89471=CARTESIAN_POINT('Ctrl Pts',(42.6049788835804,4.17631263173634,1.29397348600364));
#89472=CARTESIAN_POINT('Ctrl Pts',(42.80382610232,1.16967297101287,4.21281612717571));
#89473=CARTESIAN_POINT('Ctrl Pts',(43.0026733210597,-2.91140432784414,3.26185214567742));
#89474=CARTESIAN_POINT('Ctrl Pts',(43.2015205397993,-4.31812523206573,-0.685382419284583));
#89475=CARTESIAN_POINT('Ctrl Pts',(43.4003677585389,-1.75830472643935,-4.0030387294694));
#89476=CARTESIAN_POINT('Ctrl Pts',(43.5992149772786,2.41665849361697,-3.64358563854853));
#89477=CARTESIAN_POINT('Ctrl Pts',(43.7980621960182,4.37172871074799,0.0627906049760806));
#89478=CARTESIAN_POINT('Ctrl Pts',(43.9969094147579,2.31101846023572,3.71148868488351));
#89479=CARTESIAN_POINT('Ctrl Pts',(44.1957566334975,-1.87254602189098,3.95088926373123));
#89480=CARTESIAN_POINT('Ctrl Pts',(44.3946038522372,-4.33602807503263,0.561083873793988));
#89481=CARTESIAN_POINT('Ctrl Pts',(44.5934510709768,-2.81652353346547,-3.34412167434298));
#89482=CARTESIAN_POINT('Ctrl Pts',(44.7922982897164,1.29018184815828,-4.17748553119992));
#89483=CARTESIAN_POINT('Ctrl Pts',(44.9911455084561,4.21175260468309,-1.17349673406733));
#89484=CARTESIAN_POINT('Ctrl Pts',(45.1899927271957,3.26449366900808,2.9084421444949));
#89485=CARTESIAN_POINT('Ctrl Pts',(45.3888399459354,-0.68146230030182,4.31874560478523));
#89486=CARTESIAN_POINT('Ctrl Pts',(45.587687164675,-4.00144095406779,1.76193784061454));
#89487=CARTESIAN_POINT('Ctrl Pts',(45.7865343834146,-3.64577789390988,-2.41335003230316));
#89488=CARTESIAN_POINT('Ctrl Pts',(45.9853816021543,0.0588220862714005,
-4.37178381485786));
#89489=CARTESIAN_POINT('Ctrl Pts',(46.184228820894,3.70938929033966,-2.31438684179189));
#89490=CARTESIAN_POINT('Ctrl Pts',(46.3830760396336,3.95258747811502,1.86895911963132));
#89491=CARTESIAN_POINT('Ctrl Pts',(46.5819232583732,0.565019706366512,4.33551630096333));
#89492=CARTESIAN_POINT('Ctrl Pts',(46.7807704771129,-3.34156351119619,2.81955930010015));
#89493=CARTESIAN_POINT('Ctrl Pts',(46.9796176958525,-4.17865508132162,-1.28639154805351));
#89494=CARTESIAN_POINT('Ctrl Pts',(47.1784649145922,-1.17731935210033,-4.21068101839448));
#89495=CARTESIAN_POINT('Ctrl Pts',(47.3773121333318,2.90547722391826,-3.26714128948564));
#89496=CARTESIAN_POINT('Ctrl Pts',(47.5761593520715,4.31936307025197,0.67755843061133));
#89497=CARTESIAN_POINT('Ctrl Pts',(47.7750065708111,1.76556825641542,3.99980772043163));
#89498=CARTESIAN_POINT('Ctrl Pts',(47.9738537895506,-2.41003719764277,3.6480286722917));
#89499=CARTESIAN_POINT('Ctrl Pts',(48.1727010082905,-4.37183987877779,-0.0549712280056266));
#89500=CARTESIAN_POINT('Ctrl Pts',(48.37154822703,-2.31774458618709,-3.70706164241665));
#89501=CARTESIAN_POINT('Ctrl Pts',(48.5703954457697,1.86535395932356,-3.95471332528694));
#89502=CARTESIAN_POINT('Ctrl Pts',(48.7692426645094,4.33503308533832,-0.56813015387093));
#89503=CARTESIAN_POINT('Ctrl Pts',(48.9680898832489,2.82252994911284,3.33741922396122));
#89504=CARTESIAN_POINT('Ctrl Pts',(49.1669371019887,-1.28246820569635,4.18289702350915));
#89505=CARTESIAN_POINT('Ctrl Pts',(49.3657843207282,-4.20996327920193,1.17483976568416));
#89506=CARTESIAN_POINT('Ctrl Pts',(49.4983491332213,-3.58223236132085,-1.53299628396422));
#89507=CARTESIAN_POINT('Ctrl Pts',(49.5646315394679,-2.76460125198451,-2.45408321841374));
#89508=CARTESIAN_POINT('Ctrl Pts',(0.587524672564003,-1.75002265636256,
3.52553770398425));
#89509=CARTESIAN_POINT('Ctrl Pts',(0.65380707881055,-2.92463209188894,2.94247965805119));
#89510=CARTESIAN_POINT('Ctrl Pts',(0.786371891303646,-4.62462097686364,
0.519851943854744));
#89511=CARTESIAN_POINT('Ctrl Pts',(0.985219110043291,-2.93480951506551,
-3.61753483255978));
#89512=CARTESIAN_POINT('Ctrl Pts',(1.18406632878293,1.45479187107165,-4.42064282727201));
#89513=CARTESIAN_POINT('Ctrl Pts',(1.38291354752258,4.50603205017953,-1.16866919272471));
#89514=CARTESIAN_POINT('Ctrl Pts',(1.58176076626222,3.41917481201227,3.15973297216424));
#89515=CARTESIAN_POINT('Ctrl Pts',(1.78060798500187,-0.80901548201296,4.58414987066494));
#89516=CARTESIAN_POINT('Ctrl Pts',(1.97945520374151,-4.29377375610484,1.79845433433831));
#89517=CARTESIAN_POINT('Ctrl Pts',(2.17830242248115,-3.83450938168383,-2.63967938901811));
#89518=CARTESIAN_POINT('Ctrl Pts',(2.3771496412208,0.147135189024952,-4.65284083241367));
#89519=CARTESIAN_POINT('Ctrl Pts',(2.57599685996044,3.99358340622675,-2.39211131899973));
#89520=CARTESIAN_POINT('Ctrl Pts',(2.77484407870008,4.17162911039287,2.06602191412145));
#89521=CARTESIAN_POINT('Ctrl Pts',(2.97369129743973,0.517690544724007,4.62631875585088));
#89522=CARTESIAN_POINT('Ctrl Pts',(3.17253851617937,-3.61178210087895,2.93699011639711));
#89523=CARTESIAN_POINT('Ctrl Pts',(3.37138573491902,-4.42354873156875,-1.45020596089697));
#89524=CARTESIAN_POINT('Ctrl Pts',(3.57023295365865,-1.17193248548496,-4.50526811734826));
#89525=CARTESIAN_POINT('Ctrl Pts',(3.7690801723983,3.15619610654337,-3.42188555390371));
#89526=CARTESIAN_POINT('Ctrl Pts',(3.96792739113794,4.58510802590933,0.804772213091007));
#89527=CARTESIAN_POINT('Ctrl Pts',(4.16677460987759,1.80223337999047,4.29218207389783));
#89528=CARTESIAN_POINT('Ctrl Pts',(4.36562182861723,-2.63613582253541,3.83688170886766));
#89529=CARTESIAN_POINT('Ctrl Pts',(4.56446904735687,-4.65300470474569,-0.142899793298736));
#89530=CARTESIAN_POINT('Ctrl Pts',(4.76331626609652,-2.39571871868222,-3.99141638148338));
#89531=CARTESIAN_POINT('Ctrl Pts',(4.96216348483616,2.06222540480949,-4.17349966664448));
#89532=CARTESIAN_POINT('Ctrl Pts',(5.1610107035758,4.62585151144676,-0.521891600001131));
#89533=CARTESIAN_POINT('Ctrl Pts',(5.35985792231545,2.9402651450807,3.60911539000991));
#89534=CARTESIAN_POINT('Ctrl Pts',(5.5587051410551,-1.44618856917494,4.42486289842688));
#89535=CARTESIAN_POINT('Ctrl Pts',(5.75755235979473,-4.50420308069752,1.17602195897205));
#89536=CARTESIAN_POINT('Ctrl Pts',(5.95639957853438,-3.42474888053015,-3.15308866709796));
#89537=CARTESIAN_POINT('Ctrl Pts',(6.15524679727402,0.800609507542814,-4.58583661476685));
#89538=CARTESIAN_POINT('Ctrl Pts',(6.35409401601367,4.29054439737612,-1.806128958237));
#89539=CARTESIAN_POINT('Ctrl Pts',(6.55294123475331,3.83927306719934,2.63265177242256));
#89540=CARTESIAN_POINT('Ctrl Pts',(6.75178845349296,-0.138675880260429,
4.65313249758675));
#89541=CARTESIAN_POINT('Ctrl Pts',(6.95063567223259,-3.98924000400005,2.3993409991373));
#89542=CARTESIAN_POINT('Ctrl Pts',(7.14948289097224,-4.17536995333229,-2.0584360064005));
#89543=CARTESIAN_POINT('Ctrl Pts',(7.34833010971188,-0.526090568466078,
-4.62537584996885));
#89544=CARTESIAN_POINT('Ctrl Pts',(7.54717732845153,3.60644483909998,-2.94354015807498));
#89545=CARTESIAN_POINT('Ctrl Pts',(7.74602454719117,4.42617387171228,1.44217124400768));
#89546=CARTESIAN_POINT('Ctrl Pts',(7.94487176593082,1.18011022676091,4.50313367471746));
#89547=CARTESIAN_POINT('Ctrl Pts',(8.14371898467045,-3.14997850571596,3.42760972883471));
#89548=CARTESIAN_POINT('Ctrl Pts',(8.3425662034101,-4.58656148938392,-0.796446321967582));
#89549=CARTESIAN_POINT('Ctrl Pts',(8.54141342214974,-1.81002301437711,-4.28890309136285));
#89550=CARTESIAN_POINT('Ctrl Pts',(8.74026064088939,2.62916553524853,-3.84166131093529));
#89551=CARTESIAN_POINT('Ctrl Pts',(8.93910785962903,4.65325646531687,0.134451878613232));
#89552=CARTESIAN_POINT('Ctrl Pts',(9.13795507836867,2.40296129762516,3.98706032582799));
#89553=CARTESIAN_POINT('Ctrl Pts',(9.33680229710831,-2.05464490924545,4.17723680638143));
#89554=CARTESIAN_POINT('Ctrl Pts',(9.53564951584797,-4.62489637833799,0.530289099748558));
#89555=CARTESIAN_POINT('Ctrl Pts',(9.73449673458759,-2.94681274479986,-3.6037713144373));
#89556=CARTESIAN_POINT('Ctrl Pts',(9.93334395332725,1.43815273008053,-4.42748119867695));
#89557=CARTESIAN_POINT('Ctrl Pts',(10.1321911720669,4.50206055818595,-1.18419752157415));
#89558=CARTESIAN_POINT('Ctrl Pts',(10.3310383908065,3.43046775257043,3.14686574836777));
#89559=CARTESIAN_POINT('Ctrl Pts',(10.5298856095462,-0.792282480041272,
4.58728258465681));
#89560=CARTESIAN_POINT('Ctrl Pts',(10.7287328282858,-4.28725825117018,1.81391557892011));
#89561=CARTESIAN_POINT('Ctrl Pts',(10.9275800470254,-3.84404638899377,-2.62567713151101));
#89562=CARTESIAN_POINT('Ctrl Pts',(11.1264272657651,0.13022776616565,-4.6533765986212));
#89563=CARTESIAN_POINT('Ctrl Pts',(11.3252744845047,3.9848773621825,-2.40657961597811));
#89564=CARTESIAN_POINT('Ctrl Pts',(11.5241217032444,4.17910021723919,2.0508521189855));
#89565=CARTESIAN_POINT('Ctrl Pts',(11.722968921984,0.534487194055304,4.62441309563352));
#89566=CARTESIAN_POINT('Ctrl Pts',(11.9218161407237,-3.60109482014146,2.95008290324633));
#89567=CARTESIAN_POINT('Ctrl Pts',(12.1206633594633,-4.42878487724183,-1.43413303106441));
#89568=CARTESIAN_POINT('Ctrl Pts',(12.3195105782029,-1.18828384056733,-4.50098373179936));
#89569=CARTESIAN_POINT('Ctrl Pts',(12.5183577969426,3.14375039789217,-3.43332294948041));
#89570=CARTESIAN_POINT('Ctrl Pts',(12.7172050156822,4.5879998998482,0.788117985246376));
#89571=CARTESIAN_POINT('Ctrl Pts',(12.9160522344219,1.81780664873319,4.28560987812672));
#89572=CARTESIAN_POINT('Ctrl Pts',(13.1148994531615,-2.62218656412363,3.84642829942343));
#89573=CARTESIAN_POINT('Ctrl Pts',(13.3137466719012,-4.65349289738031,-0.126003546405802));
#89574=CARTESIAN_POINT('Ctrl Pts',(13.5125938906408,-2.41019595122522,-3.98269111485857));
#89575=CARTESIAN_POINT('Ctrl Pts',(13.7114411093805,2.04705763875159,-4.18096018437209));
#89576=CARTESIAN_POINT('Ctrl Pts',(13.9102883281201,4.62392600225079,-0.538684847925919));
#89577=CARTESIAN_POINT('Ctrl Pts',(14.1091355468597,2.95335063072125,3.59841535841742));
#89578=CARTESIAN_POINT('Ctrl Pts',(14.3079827655994,-1.43011215027247,4.43008490633294));
#89579=CARTESIAN_POINT('Ctrl Pts',(14.506829984339,-4.49990319644462,1.19236918037302));
#89580=CARTESIAN_POINT('Ctrl Pts',(14.7056772030787,-3.43617531721211,-3.14063245685613));
#89581=CARTESIAN_POINT('Ctrl Pts',(14.9045244218183,0.783952841014584,-4.5887134343671));
#89582=CARTESIAN_POINT('Ctrl Pts',(15.1033716405579,4.28395797359069,-1.82169622061));
#89583=CARTESIAN_POINT('Ctrl Pts',(15.3022188592976,3.84880704026154,2.61869383596274));
#89584=CARTESIAN_POINT('Ctrl Pts',(15.5010660780373,-0.12177922281464,4.65360536149839));
#89585=CARTESIAN_POINT('Ctrl Pts',(15.6999132967769,-3.98050158565777,2.41381030038649));
#89586=CARTESIAN_POINT('Ctrl Pts',(15.8987605155165,-4.18281670624742,-2.04326147167056));
#89587=CARTESIAN_POINT('Ctrl Pts',(16.0976077342562,-0.542882057901342,
-4.62343509859117));
#89588=CARTESIAN_POINT('Ctrl Pts',(16.2964549529958,3.59573293147315,-2.95661592453187));
#89589=CARTESIAN_POINT('Ctrl Pts',(16.4953021717355,4.43138128487904,1.42609009101802));
#89590=CARTESIAN_POINT('Ctrl Pts',(16.6941493904751,1.19645353762478,4.49881895301213));
#89591=CARTESIAN_POINT('Ctrl Pts',(16.8929966092148,-3.13751192782905,3.43902485341504));
#89592=CARTESIAN_POINT('Ctrl Pts',(17.0918438279544,-4.58942318762548,-0.77978705077828));
#89593=CARTESIAN_POINT('Ctrl Pts',(17.290691046694,-1.82558429134533,-4.28230253892332));
#89594=CARTESIAN_POINT('Ctrl Pts',(17.4895382654337,2.61519894990641,-3.85118260954792));
#89595=CARTESIAN_POINT('Ctrl Pts',(17.6883854841733,4.65371399088276,0.117554798873092));
#89596=CARTESIAN_POINT('Ctrl Pts',(17.887232702913,2.41742266048359,3.97830877638432));
#89597=CARTESIAN_POINT('Ctrl Pts',(18.0860799216526,-2.03946362087056,4.18466978133538));
#89598=CARTESIAN_POINT('Ctrl Pts',(18.2849271403923,-4.62294038505918,0.547078820522931));
#89599=CARTESIAN_POINT('Ctrl Pts',(18.4837743591319,-2.95987878198744,-3.5930475415191));
#89600=CARTESIAN_POINT('Ctrl Pts',(18.6826215778715,1.42206685661543,-4.43267401181181));
#89601=CARTESIAN_POINT('Ctrl Pts',(18.8814687966112,4.49773100239534,-1.20053690895693));
#89602=CARTESIAN_POINT('Ctrl Pts',(19.0803160153508,3.44187155574113,3.1343888133823));
#89603=CARTESIAN_POINT('Ctrl Pts',(19.2791632340905,-0.775620617970148,
4.5901291590385));
#89604=CARTESIAN_POINT('Ctrl Pts',(19.4780104528301,-4.28064357548876,1.82947085773528));
#89605=CARTESIAN_POINT('Ctrl Pts',(19.6768576715698,-3.853555005325,-2.61170190883465));
#89606=CARTESIAN_POINT('Ctrl Pts',(19.8757048903094,0.1133302780623,-4.65381878544387));
#89607=CARTESIAN_POINT('Ctrl Pts',(20.0745521090491,3.97611268884515,-2.4210330285398));
#89608=CARTESIAN_POINT('Ctrl Pts',(20.2733993277887,4.18651940810897,2.0356640894811));
#89609=CARTESIAN_POINT('Ctrl Pts',(20.4722465465283,0.551275132332437,4.6224418620625));
#89610=CARTESIAN_POINT('Ctrl Pts',(20.671093765268,-3.5903591907681,2.96313920039928));
#89611=CARTESIAN_POINT('Ctrl Pts',(20.8699409840076,-4.43396308606603,-1.41804245038001));
#89612=CARTESIAN_POINT('Ctrl Pts',(21.0687882027473,-1.20461929100464,-4.49663934549075));
#89613=CARTESIAN_POINT('Ctrl Pts',(21.2676354214869,3.13126311608942,-3.44471542184459));
#89614=CARTESIAN_POINT('Ctrl Pts',(21.4664826402265,4.59083134802444,0.771453546023437));
#89615=CARTESIAN_POINT('Ctrl Pts',(21.6653298589662,1.83335591657723,4.27898108465407));
#89616=CARTESIAN_POINT('Ctrl Pts',(21.8641770777058,-2.6082027156291,3.85592422563786));
#89617=CARTESIAN_POINT('Ctrl Pts',(22.0630242964455,-4.65391974509539,-0.10910566386342));
#89618=CARTESIAN_POINT('Ctrl Pts',(22.2618715151851,-2.42464140158001,-3.97391332484995));
#89619=CARTESIAN_POINT('Ctrl Pts',(22.4607187339248,2.03186288063319,-4.18836558504399));
#89620=CARTESIAN_POINT('Ctrl Pts',(22.6595659526644,4.62193953001191,-0.555470989871944));
#89621=CARTESIAN_POINT('Ctrl Pts',(22.858413171404,2.96639717708072,3.58766788143545));
#89622=CARTESIAN_POINT('Ctrl Pts',(23.0572603901437,-1.41401687562795,4.43524850657946));
#89623=CARTESIAN_POINT('Ctrl Pts',(23.2561076088833,-4.49554398319792,1.20870068040387));
#89624=CARTESIAN_POINT('Ctrl Pts',(23.454954827623,-3.44755644938191,-3.12813483852616));
#89625=CARTESIAN_POINT('Ctrl Pts',(23.6538020463626,0.767285838372017,-4.59152975400461));
#89626=CARTESIAN_POINT('Ctrl Pts',(23.8526492651023,4.27731506778913,-1.83723946466974));
#89627=CARTESIAN_POINT('Ctrl Pts',(24.0514964838419,3.85829026853422,2.60470137317316));
#89628=CARTESIAN_POINT('Ctrl Pts',(24.2503437025816,-0.104880959757646,
4.65401686975417));
#89629=CARTESIAN_POINT('Ctrl Pts',(24.4491909213212,-3.97171068621112,2.4282477766308));
#89630=CARTESIAN_POINT('Ctrl Pts',(24.6480381400608,-4.19020831061913,-2.02805999745922));
#89631=CARTESIAN_POINT('Ctrl Pts',(24.8468853588005,-0.559666389683838,
-4.62143338932135));
#89632=CARTESIAN_POINT('Ctrl Pts',(25.0457325775401,3.58497361573888,-2.969652709347));
#89633=CARTESIAN_POINT('Ctrl Pts',(25.2445797962798,4.43653027229285,1.40999013567649));
#89634=CARTESIAN_POINT('Ctrl Pts',(25.4434270150194,1.21278107379143,4.49444491641952));
#89635=CARTESIAN_POINT('Ctrl Pts',(25.6422742337591,-3.1250039832703,3.45039463601204));
#89636=CARTESIAN_POINT('Ctrl Pts',(25.8411214524987,-4.59222437640355,-0.763117498450222));
#89637=CARTESIAN_POINT('Ctrl Pts',(26.0399686712383,-1.84112149881258,-4.27564552626689));
#89638=CARTESIAN_POINT('Ctrl Pts',(26.238815889978,2.60119788435214,-3.86065313206429));
#89639=CARTESIAN_POINT('Ctrl Pts',(26.4376631087176,4.65411015934009,0.10065616922622));
#89640=CARTESIAN_POINT('Ctrl Pts',(26.6365103274573,2.43185215072055,3.96950477474354));
#89641=CARTESIAN_POINT('Ctrl Pts',(26.8353575461969,-2.02425544309264,4.19204758331602));
#89642=CARTESIAN_POINT('Ctrl Pts',(27.0342047649366,-4.62092344040788,0.563861328311218));
#89643=CARTESIAN_POINT('Ctrl Pts',(27.2330519836762,-2.97290579451561,-3.58227639589851));
#89644=CARTESIAN_POINT('Ctrl Pts',(27.4318992024159,1.40596223384379,-4.43780838215003));
#89645=CARTESIAN_POINT('Ctrl Pts',(27.6307464211555,4.49334214606115,-1.21686046780494));
#89646=CARTESIAN_POINT('Ctrl Pts',(27.8295936398951,3.45322997939622,3.12187055290175));
#89647=CARTESIAN_POINT('Ctrl Pts',(28.0284408586348,-0.758948529692909,
4.59291521464886));
#89648=CARTESIAN_POINT('Ctrl Pts',(28.2272880773744,-4.27397246146306,1.84500201580684));
#89649=CARTESIAN_POINT('Ctrl Pts',(28.4261352961141,-3.86301281428105,-2.59769225205302));
#89650=CARTESIAN_POINT('Ctrl Pts',(28.6249825148537,0.0964312957506612,
-4.65419961377633));
#89651=CARTESIAN_POINT('Ctrl Pts',(28.8238297335934,3.96729559226513,-2.43545452087891));
#89652=CARTESIAN_POINT('Ctrl Pts',(29.022676952333,4.19388340161891,2.02044922066884));
#89653=CARTESIAN_POINT('Ctrl Pts',(29.2215241710727,0.568055802296986,4.62040968369177));
#89654=CARTESIAN_POINT('Ctrl Pts',(29.4203713898123,-3.57957622413699,2.9761564299057));
#89655=CARTESIAN_POINT('Ctrl Pts',(29.6192186085519,-4.43908283509774,-1.40193317344891));
#89656=CARTESIAN_POINT('Ctrl Pts',(29.8180658272916,-1.22093885908292,-4.49223567303157));
#89657=CARTESIAN_POINT('Ctrl Pts',(30.0169130460312,3.11873455000258,-3.45606247719805));
#89658=CARTESIAN_POINT('Ctrl Pts',(30.2157602647709,4.59360226817123,0.754778935535434));
#89659=CARTESIAN_POINT('Ctrl Pts',(30.4146074835105,1.84888101245487,4.27229587475631));
#89660=CARTESIAN_POINT('Ctrl Pts',(30.6134547022501,-2.59418447916456,3.86536931324001));
#89661=CARTESIAN_POINT('Ctrl Pts',(30.8123019209898,-4.65428523298917,-0.0922063428123347));
#89662=CARTESIAN_POINT('Ctrl Pts',(31.0111491397294,-2.43905488413748,-3.9650831405963));
#89663=CARTESIAN_POINT('Ctrl Pts',(31.2099963584691,2.01664133332414,-4.19571576401506));
#89664=CARTESIAN_POINT('Ctrl Pts',(31.4088435772087,4.61989211959633,-0.572249808184896));
#89665=CARTESIAN_POINT('Ctrl Pts',(31.6076907959484,2.97940461283869,3.57687310267941));
#89666=CARTESIAN_POINT('Ctrl Pts',(31.806538014688,-1.39790295781212,4.44035363008579));
#89667=CARTESIAN_POINT('Ctrl Pts',(32.0053852334276,-4.49112549824252,1.22501624426447));
#89668=CARTESIAN_POINT('Ctrl Pts',(32.2042324521673,-3.45889212708342,-3.11559597715689));
#89669=CARTESIAN_POINT('Ctrl Pts',(32.403079670907,0.750608719413602,-4.59428553640459));
#89670=CARTESIAN_POINT('Ctrl Pts',(32.6019268896466,4.2706157675282,-1.85275848556028));
#89671=CARTESIAN_POINT('Ctrl Pts',(32.8007741083862,3.86772262699936,2.59067456857727));
#89672=CARTESIAN_POINT('Ctrl Pts',(32.9996213271259,-0.0879813138927531,
4.65436701690806));
#89673=CARTESIAN_POINT('Ctrl Pts',(33.1984685458655,-3.96286742156015,2.44265323752946));
#89674=CARTESIAN_POINT('Ctrl Pts',(33.3973157646052,-4.19754466899455,-2.01283178419641));
#89675=CARTESIAN_POINT('Ctrl Pts',(33.5961629833448,-0.576443342518929,
-4.61937074854807));
#89676=CARTESIAN_POINT('Ctrl Pts',(33.7950102020845,3.57416703375318,-2.982650340638));
#89677=CARTESIAN_POINT('Ctrl Pts',(33.9938574208241,4.44162076606701,1.39387159025436));
#89678=CARTESIAN_POINT('Ctrl Pts',(34.1927046395637,1.22909261998972,4.49001162260886));
#89679=CARTESIAN_POINT('Ctrl Pts',(34.3915518583034,-3.11245483695114,3.46171892672056));
#89680=CARTESIAN_POINT('Ctrl Pts',(34.590399077043,-4.59496501878578,-0.746437884763965));
#89681=CARTESIAN_POINT('Ctrl Pts',(34.7892462957827,-1.85663443192783,-4.26893214116319));
#89682=CARTESIAN_POINT('Ctrl Pts',(34.9880935145223,2.58716252318344,-3.87007275361991));
#89683=CARTESIAN_POINT('Ctrl Pts',(35.1869407332619,4.65444496546559,0.0837562124734973));
#89684=CARTESIAN_POINT('Ctrl Pts',(35.3857879520017,2.44624957808966,3.96064843698251));
#89685=CARTESIAN_POINT('Ctrl Pts',(35.5846351707412,-2.00902057642482,4.1993701150503));
#89686=CARTESIAN_POINT('Ctrl Pts',(35.7834823894809,-4.6188455709766,0.580636401843466));
#89687=CARTESIAN_POINT('Ctrl Pts',(35.9823296082206,-2.98589361062901,-3.57145801958819));
#89688=CARTESIAN_POINT('Ctrl Pts',(36.1811768269602,1.38983907409762,-4.44288424199724));
#89689=CARTESIAN_POINT('Ctrl Pts',(36.3800240456998,4.48889404704846,-1.23316798289963));
#89690=CARTESIAN_POINT('Ctrl Pts',(36.5788712644394,3.46454287378012,3.10931113197366));
#89691=CARTESIAN_POINT('Ctrl Pts',(36.7777184831791,-0.742266435023419,
4.59564071475496));
#89692=CARTESIAN_POINT('Ctrl Pts',(36.9765657019187,-4.26724499704864,1.8605088483636));
#89693=CARTESIAN_POINT('Ctrl Pts',(37.1754129206584,-3.87241969116504,-2.58364834587705));
#89694=CARTESIAN_POINT('Ctrl Pts',(37.374260139398,0.0795310420360833,-4.65451907859756));
#89695=CARTESIAN_POINT('Ctrl Pts',(37.5731073581377,3.95842618869195,-2.44984390285462));
#89696=CARTESIAN_POINT('Ctrl Pts',(37.7719545768773,4.20119210067807,2.00520771314995));
#89697=CARTESIAN_POINT('Ctrl Pts',(37.970801795617,0.584828982703287,4.6183165873147));
#89698=CARTESIAN_POINT('Ctrl Pts',(38.1696490143566,-3.56874606241678,2.98913442013916));
#89699=CARTESIAN_POINT('Ctrl Pts',(38.3684962330963,-4.44414405683533,-1.38580541266483));
#89700=CARTESIAN_POINT('Ctrl Pts',(38.5673434518359,-1.23724232963595,-4.48777277248224));
#89701=CARTESIAN_POINT('Ctrl Pts',(38.7661906705756,3.10616486481495,-3.46736396593507));
#89702=CARTESIAN_POINT('Ctrl Pts',(38.9650378893152,4.59631262375533,0.738094373629349));
#89703=CARTESIAN_POINT('Ctrl Pts',(39.1638851080548,1.86438173167491,4.26555433657488));
#89704=CARTESIAN_POINT('Ctrl Pts',(39.3627323267945,-2.58013203955406,3.87476343770075));
#89705=CARTESIAN_POINT('Ctrl Pts',(39.5615795455341,-4.65458935624285,-0.075305806062374));
#89706=CARTESIAN_POINT('Ctrl Pts',(39.7604267642738,-2.45343620886246,-3.95620067851954));
#89707=CARTESIAN_POINT('Ctrl Pts',(39.9592739830134,2.00139319751365,-4.20301062437656));
#89708=CARTESIAN_POINT('Ctrl Pts',(40.158121201753,4.61778379799829,-0.589021081643585));
#89709=CARTESIAN_POINT('Ctrl Pts',(40.3569684204926,2.99237276649791,3.56603116447367));
#89710=CARTESIAN_POINT('Ctrl Pts',(40.5558156392324,-1.38177060927986,4.44540020954315));
#89711=CARTESIAN_POINT('Ctrl Pts',(40.7546628579719,-4.48664779983415,1.24131565684128));
#89712=CARTESIAN_POINT('Ctrl Pts',(40.9535100767116,-3.47018220086074,-3.10301603806767));
#89713=CARTESIAN_POINT('Ctrl Pts',(41.1523572954513,0.733921704019672,-4.59698074523321));
#89714=CARTESIAN_POINT('Ctrl Pts',(41.3512045141909,4.26386016113502,-1.86825307867041));
#89715=CARTESIAN_POINT('Ctrl Pts',(41.5500517329305,3.87710399129574,2.57661360711193));
#89716=CARTESIAN_POINT('Ctrl Pts',(41.7488989516702,-0.0710805080340738,
4.65465579834364));
#89717=CARTESIAN_POINT('Ctrl Pts',(41.9477461704099,-3.95397190829937,2.4570264931528));
#89718=CARTESIAN_POINT('Ctrl Pts',(42.1465933891494,-4.20482568464708,-1.9975770326591));
#89719=CARTESIAN_POINT('Ctrl Pts',(42.3454406078891,-0.593212695209971,
-4.61724720346677));
#89720=CARTESIAN_POINT('Ctrl Pts',(42.5442878266288,3.56331332799607,-2.995608647036));
#89721=CARTESIAN_POINT('Ctrl Pts',(42.7431350453684,4.44665269908555,1.37773466726589));
#89722=CARTESIAN_POINT('Ctrl Pts',(42.941982264108,1.24538796115919,4.48551913003431));
#89723=CARTESIAN_POINT('Ctrl Pts',(43.1408294828477,-3.09986465432677,3.47299757622888));
#89724=CARTESIAN_POINT('Ctrl Pts',(43.3396767015873,-4.59764507863759,-0.729748429621486));
#89725=CARTESIAN_POINT('Ctrl Pts',(43.538523920327,-1.87212288616081,-4.26216247214683));
#89726=CARTESIAN_POINT('Ctrl Pts',(43.7373711390666,2.5730930514516,-3.87944134997984));
#89727=CARTESIAN_POINT('Ctrl Pts',(43.9362183578062,4.65471840484205,0.0668551513535571));
#89728=CARTESIAN_POINT('Ctrl Pts',(44.1350655765459,2.46061475277319,3.95173988001982));
#89729=CARTESIAN_POINT('Ctrl Pts',(44.3339127952855,-1.99375922174246,4.20663727970347));
#89730=CARTESIAN_POINT('Ctrl Pts',(44.5327600140252,-4.61670680414042,0.59740382050415));
#89731=CARTESIAN_POINT('Ctrl Pts',(44.7316072327648,-2.99884205912885,-3.56059255628707));
#89732=CARTESIAN_POINT('Ctrl Pts',(44.9304544515045,1.37369759002917,-4.44790152239582));
#89733=CARTESIAN_POINT('Ctrl Pts',(45.1293016702441,4.48438676385885,-1.24945924312633));
#89734=CARTESIAN_POINT('Ctrl Pts',(45.3281488889838,3.47581009001405,3.09671072363562));
#89735=CARTESIAN_POINT('Ctrl Pts',(45.5269961077234,-0.725574554437197,
4.59830560917513));
#89736=CARTESIAN_POINT('Ctrl Pts',(45.7258433264631,-4.26046126993124,1.87599117821119));
#89737=CARTESIAN_POINT('Ctrl Pts',(45.9246905452027,-3.8817755138893,-2.56957042761375));
#89738=CARTESIAN_POINT('Ctrl Pts',(46.1235377639424,0.0626297434481601,
-4.65477707593793));
#89739=CARTESIAN_POINT('Ctrl Pts',(46.3223849826819,3.94950458797202,-2.46420117559616));
#89740=CARTESIAN_POINT('Ctrl Pts',(46.5212322014217,4.20844542249333,1.98994013298625));
#89741=CARTESIAN_POINT('Ctrl Pts',(46.7200794201614,0.601594426446524,4.61616190203485));
#89742=CARTESIAN_POINT('Ctrl Pts',(46.9189266389009,-3.55786879873718,3.00207433628102));
#89743=CARTESIAN_POINT('Ctrl Pts',(47.1177738576406,-4.44914677955542,-1.36966193712735));
#89744=CARTESIAN_POINT('Ctrl Pts',(47.3166210763802,-1.25352930595277,-4.48324581190367));
#89745=CARTESIAN_POINT('Ctrl Pts',(47.5154682951199,3.09355387853151,-3.47862909562517));
#89746=CARTESIAN_POINT('Ctrl Pts',(47.7143155138595,4.59896304426834,0.721417980390469));
#89747=CARTESIAN_POINT('Ctrl Pts',(47.9131627325991,1.87985659721673,4.25872231420717));
#89748=CARTESIAN_POINT('Ctrl Pts',(48.1120099513388,-2.5660431473349,3.88417198911736));
#89749=CARTESIAN_POINT('Ctrl Pts',(48.3108571700785,-4.65483676897409,-0.0585296123489751));
#89750=CARTESIAN_POINT('Ctrl Pts',(48.509704388818,-2.46777627269599,-3.94702626730209));
#89751=CARTESIAN_POINT('Ctrl Pts',(48.7085516075577,1.98610160430635,-4.21070887949438));
#89752=CARTESIAN_POINT('Ctrl Pts',(48.9073988262974,4.61564740701194,-0.604906218692581));
#89753=CARTESIAN_POINT('Ctrl Pts',(49.106246045037,3.00523728063291,3.55345624449517));
#89754=CARTESIAN_POINT('Ctrl Pts',(49.3050932637767,-1.36548462991396,4.45366331012696));
#89755=CARTESIAN_POINT('Ctrl Pts',(49.5039404825163,-4.4824816121899,1.25088921154358));
#89756=CARTESIAN_POINT('Ctrl Pts',(49.6365052950094,-3.81411656712978,-1.63222983164071));
#89757=CARTESIAN_POINT('Ctrl Pts',(49.7027877012559,-2.94355875697961,-2.61294034455543));
#89758=CARTESIAN_POINT('Ctrl Pts',(49.291,-0.918523134026602,3.82423904224853));
#89759=CARTESIAN_POINT('Ctrl Pts',(49.291,-0.944497648971282,3.81771905984364));
#89760=CARTESIAN_POINT('Ctrl Pts',(49.291,-0.970472163915961,3.81119907743874));
#89761=CARTESIAN_POINT('Ctrl Pts',(49.291,-0.99644667886064,3.80467909503385));
#89762=CARTESIAN_POINT('Ctrl Pts',(0.585800000000001,-1.87561177831641,
-2.627495997809));
#89763=CARTESIAN_POINT('Ctrl Pts',(0.585800000000003,-1.93432966665696,
-2.59479265455963));
#89764=CARTESIAN_POINT('Ctrl Pts',(0.585800000000004,-1.99185820734684,
-2.56017313445794));
#89765=CARTESIAN_POINT('Ctrl Pts',(0.585800000000003,-2.04809242124784,
-2.52365641141691));
#89766=CARTESIAN_POINT('Ctrl Pts',(0.585800000000001,-2.13571955057025,
-2.4667541202605));
#89767=CARTESIAN_POINT('Ctrl Pts',(0.585800000000001,-2.22020527745289,
-2.40524808224379));
#89768=CARTESIAN_POINT('Ctrl Pts',(0.585800000000002,-2.30145114296921,
-2.33955241913762));
#89769=CARTESIAN_POINT('Ctrl Pts',(0.585800000000003,-2.38269700848554,
-2.27385675603146));
#89770=CARTESIAN_POINT('Ctrl Pts',(0.585800000000001,-2.46070346620059,
-2.20397085949305));
#89771=CARTESIAN_POINT('Ctrl Pts',(0.585800000000001,-2.53534969830284,
-2.13025947000897));
#89772=CARTESIAN_POINT('Ctrl Pts',(0.585800000000001,-2.54871288358938,
-2.11706364045853));
#89773=CARTESIAN_POINT('Ctrl Pts',(0.5858,-2.56196773078561,-2.10374556313248));
#89774=CARTESIAN_POINT('Ctrl Pts',(0.5858,-2.57510436638075,-2.09031685798063));
#89775=CARTESIAN_POINT('Ctrl Pts',(0.585799999999998,-2.6494041349224,-2.01436516720182));
#89776=CARTESIAN_POINT('Ctrl Pts',(0.585799999999997,-2.72000285773494,
-1.93480144575629));
#89777=CARTESIAN_POINT('Ctrl Pts',(0.585799999999998,-2.78679913428153,
-1.85203521699974));
#89778=CARTESIAN_POINT('Ctrl Pts',(0.585799999999999,-2.85526820090954,
-1.76719626003589));
#89779=CARTESIAN_POINT('Ctrl Pts',(0.585799999999998,-2.91974257549655,
-1.67899189202741));
#89780=CARTESIAN_POINT('Ctrl Pts',(0.585799999999997,-2.98008554188355,
-1.58781616186147));
#89781=CARTESIAN_POINT('Ctrl Pts',(0.585799999999997,-3.00023946869769,
-1.5573644107625));
#89782=CARTESIAN_POINT('Ctrl Pts',(0.585799999999998,-3.01993227833314,
-1.52658086018387));
#89783=CARTESIAN_POINT('Ctrl Pts',(0.585799999999997,-3.03915803741692,
-1.49547921963615));
#89784=CARTESIAN_POINT('Ctrl Pts',(0.585799999999997,-3.05017677172482,
-1.47765413859557));
#89785=CARTESIAN_POINT('Ctrl Pts',(0.585799999999998,-3.0610420854361,-1.45972456616738));
#89786=CARTESIAN_POINT('Ctrl Pts',(0.585799999999997,-3.07175279236073,
-1.44169302107519));
#89787=CARTESIAN_POINT('Ctrl Pts',(0.585799999999996,-3.08051536309559,
-1.42694117598772));
#89788=CARTESIAN_POINT('Ctrl Pts',(0.585799999999998,-3.08917383312795,
-1.41212200437087));
#89789=CARTESIAN_POINT('Ctrl Pts',(0.585799999999998,-3.09772145058444,
-1.39724789804343));
#89790=CARTESIAN_POINT('Ctrl Pts',(0.585799999999998,-3.15344467524449,
-1.30028132546107));
#89791=CARTESIAN_POINT('Ctrl Pts',(0.585799999999995,-3.20453203572293,
-1.20086197202072));
#89792=CARTESIAN_POINT('Ctrl Pts',(0.585799999999994,-3.25087290134545,
-1.09942493104332));
#89793=CARTESIAN_POINT('Ctrl Pts',(0.585799999999993,-3.29776205531203,
-0.996787723722996));
#89794=CARTESIAN_POINT('Ctrl Pts',(0.585799999999992,-3.33979230665747,
-0.892084098641399));
#89795=CARTESIAN_POINT('Ctrl Pts',(0.585799999999992,-3.37681507082798,
-0.785722893322618));
#89796=CARTESIAN_POINT('Ctrl Pts',(0.585799999999992,-3.41375314830139,
-0.679604980998846));
#89797=CARTESIAN_POINT('Ctrl Pts',(0.585799999999991,-3.44570713185698,
-0.571836247002017));
#89798=CARTESIAN_POINT('Ctrl Pts',(0.585799999999993,-3.47248778918825,
-0.462792851071621));
#89799=CARTESIAN_POINT('Ctrl Pts',(0.585799999999993,-3.48965728959878,
-0.392883415764099));
#89800=CARTESIAN_POINT('Ctrl Pts',(0.585799999999996,-3.5046995408535,-0.32244948748404));
#89801=CARTESIAN_POINT('Ctrl Pts',(0.585799999999994,-3.51755413072086,
-0.251586084815355));
#89802=CARTESIAN_POINT('Ctrl Pts',(0.585799999999994,-3.52200137504234,
-0.227069793874057));
#89803=CARTESIAN_POINT('Ctrl Pts',(0.585799999999992,-3.52618669576443,
-0.202502078237746));
#89804=CARTESIAN_POINT('Ctrl Pts',(0.585799999999994,-3.53010733730041,
-0.177886819619966));
#89805=CARTESIAN_POINT('Ctrl Pts',(0.585799999999996,-3.53249109853745,
-0.16292067216823));
#89806=CARTESIAN_POINT('Ctrl Pts',(0.585799999999995,-3.53477657935189,
-0.147939396482612));
#89807=CARTESIAN_POINT('Ctrl Pts',(0.585799999999995,-3.53696191341059,
-0.132953840569866));
#89808=CARTESIAN_POINT('Ctrl Pts',(0.585799999999995,-3.55367763747858,
-0.0183286112394999));
#89809=CARTESIAN_POINT('Ctrl Pts',(0.585799999999994,-3.56456403896117,
0.096709245982323));
#89810=CARTESIAN_POINT('Ctrl Pts',(0.585799999999995,-3.56947395842516,
0.211735564449169));
#89811=CARTESIAN_POINT('Ctrl Pts',(0.585799999999994,-3.57211763385812,
0.273669829258397));
#89812=CARTESIAN_POINT('Ctrl Pts',(0.585799999999994,-3.57302793677542,
0.335601297332963));
#89813=CARTESIAN_POINT('Ctrl Pts',(0.585799999999994,-3.57217641958998,
0.39746679596036));
#89814=CARTESIAN_POINT('Ctrl Pts',(0.585799999999995,-3.57064955014543,
0.508398837193222));
#89815=CARTESIAN_POINT('Ctrl Pts',(0.585799999999993,-3.56346125874838,
0.619118451061581));
#89816=CARTESIAN_POINT('Ctrl Pts',(0.585799999999995,-3.55087631125224,
0.729340653175641));
#89817=CARTESIAN_POINT('Ctrl Pts',(0.585799999999996,-3.53805158338041,
0.841662913398155));
#89818=CARTESIAN_POINT('Ctrl Pts',(0.585799999999993,-3.51962249756278,
0.953469303091311));
#89819=CARTESIAN_POINT('Ctrl Pts',(0.585799999999995,-3.49581515276092,
1.06446168404778));
#89820=CARTESIAN_POINT('Ctrl Pts',(0.585799999999996,-3.48835663508087,
1.09923408905997));
#89821=CARTESIAN_POINT('Ctrl Pts',(0.585799999999993,-3.48036986358895,
1.13392658392764));
#89822=CARTESIAN_POINT('Ctrl Pts',(0.585799999999993,-3.47186075378713,
1.16852990102506));
#89823=CARTESIAN_POINT('Ctrl Pts',(0.585799999999995,-3.46514795967475,
1.19582828460338));
#89824=CARTESIAN_POINT('Ctrl Pts',(0.585799999999993,-3.45810778648413,
1.22307890759173));
#89825=CARTESIAN_POINT('Ctrl Pts',(0.585799999999994,-3.45075610902602,
1.25023064681264));
#89826=CARTESIAN_POINT('Ctrl Pts',(0.585799999999994,-3.42093932181936,
1.36035213068536));
#89827=CARTESIAN_POINT('Ctrl Pts',(0.585799999999994,-3.38597425835464,
1.46897437338361));
#89828=CARTESIAN_POINT('Ctrl Pts',(0.585799999999994,-3.34616091262472,
1.57580281021644));
#89829=CARTESIAN_POINT('Ctrl Pts',(0.585799999999993,-3.30508145284811,
1.6860285245697));
#89830=CARTESIAN_POINT('Ctrl Pts',(0.585799999999995,-3.25884040932796,
1.7943452321113));
#89831=CARTESIAN_POINT('Ctrl Pts',(0.585799999999997,-3.20771203882439,
1.90043247757802));
#89832=CARTESIAN_POINT('Ctrl Pts',(0.585799999999999,-3.15612402547689,
2.00747344487728));
#89833=CARTESIAN_POINT('Ctrl Pts',(0.585799999999998,-3.09956014992837,
2.11224548851188));
#89834=CARTESIAN_POINT('Ctrl Pts',(0.585799999999997,-3.03824934181154,
2.2144110110577));
#89835=CARTESIAN_POINT('Ctrl Pts',(0.585799999999997,-2.99849863814183,
2.2806497630285));
#89836=CARTESIAN_POINT('Ctrl Pts',(0.585799999999997,-2.95675147643439,
2.34579265403001));
#89837=CARTESIAN_POINT('Ctrl Pts',(0.585799999999995,-2.91305938898694,
2.40974333609371));
#89838=CARTESIAN_POINT('Ctrl Pts',(0.585799999999995,-2.89642626520271,
2.43408869638647));
#89839=CARTESIAN_POINT('Ctrl Pts',(0.585799999999994,-2.87951163347175,
2.4582606131126));
#89840=CARTESIAN_POINT('Ctrl Pts',(0.585799999999996,-2.86231665815064,
2.48225550433344));
#89841=CARTESIAN_POINT('Ctrl Pts',(0.585799999999997,-2.84712565273625,
2.50345393676189));
#89842=CARTESIAN_POINT('Ctrl Pts',(0.585799999999995,-2.83171488921404,
2.52451508711931));
#89843=CARTESIAN_POINT('Ctrl Pts',(0.585799999999996,-2.81610831463341,
2.54540619518073));
#89844=CARTESIAN_POINT('Ctrl Pts',(0.585799999999997,-2.74275312496236,
2.64360014455544));
#89845=CARTESIAN_POINT('Ctrl Pts',(0.585799999999995,-2.66498329274227,
2.73817129382513));
#89846=CARTESIAN_POINT('Ctrl Pts',(0.585799999999995,-2.58308793541154,
2.82878454959318));
#89847=CARTESIAN_POINT('Ctrl Pts',(0.585799999999995,-2.50105380468771,
2.91955135141527));
#89848=CARTESIAN_POINT('Ctrl Pts',(0.585799999999995,-2.4148797735425,3.00634766584885));
#89849=CARTESIAN_POINT('Ctrl Pts',(0.585799999999996,-2.32480654965838,
3.08882057079662));
#89850=CARTESIAN_POINT('Ctrl Pts',(0.585799999999997,-2.23610653303497,
3.17003613880226));
#89851=CARTESIAN_POINT('Ctrl Pts',(0.585799999999995,-2.14362482415573,
3.2470598493341));
#89852=CARTESIAN_POINT('Ctrl Pts',(0.585799999999996,-2.04754958290616,
3.31952755214537));
#89853=CARTESIAN_POINT('Ctrl Pts',(0.585799999999997,-1.9514743416566,3.39199525495664));
#89854=CARTESIAN_POINT('Ctrl Pts',(0.585799999999997,-1.85180519811705,
3.45990776211604));
#89855=CARTESIAN_POINT('Ctrl Pts',(0.585799999999996,-1.74869447533108,
3.5228619944509));
#89856=CARTESIAN_POINT('Origin',(0.585799999999996,-5.160062080289E-16,
2.1385152528819E-16));
#89857=CARTESIAN_POINT('',(0.585799999999997,-3.933,-4.81653586104654E-16));
#89858=CARTESIAN_POINT('Origin',(0.585799999999996,0.,0.));
#89859=CARTESIAN_POINT('',(0.585799999999996,1.82083948017239,3.48611999039699));
#89860=CARTESIAN_POINT('Origin',(0.585799999999996,0.,0.));
#89861=CARTESIAN_POINT('Ctrl Pts',(0.585799999999996,1.82083948017239,3.48611999039699));
#89862=CARTESIAN_POINT('Ctrl Pts',(0.585799999999996,1.86689239886374,3.45684336336271));
#89863=CARTESIAN_POINT('Ctrl Pts',(0.585799999999994,1.91225446113732,3.4265446583295));
#89864=CARTESIAN_POINT('Ctrl Pts',(0.585799999999993,1.95688759198411,3.39522130376487));
#89865=CARTESIAN_POINT('Ctrl Pts',(0.585799999999993,2.05792862938297,3.32431110365171));
#89866=CARTESIAN_POINT('Ctrl Pts',(0.585799999999995,2.15523691577152,3.24815207496259));
#89867=CARTESIAN_POINT('Ctrl Pts',(0.585799999999993,2.24861882171376,3.16717424928343));
#89868=CARTESIAN_POINT('Ctrl Pts',(0.585799999999991,2.342000727656,3.08619642360427));
#89869=CARTESIAN_POINT('Ctrl Pts',(0.585799999999997,2.43145663514149,3.00039885361381));
#89870=CARTESIAN_POINT('Ctrl Pts',(0.585799999999992,2.51674675544355,2.91018295065707));
#89871=CARTESIAN_POINT('Ctrl Pts',(0.585799999999992,2.53166856913533,2.89439935355123));
#89872=CARTESIAN_POINT('Ctrl Pts',(0.585799999999993,2.54646336716743,2.87847967405364));
#89873=CARTESIAN_POINT('Ctrl Pts',(0.585799999999993,2.56111841909083,2.86243871338739));
#89874=CARTESIAN_POINT('Ctrl Pts',(0.585799999999993,2.64273316869577,2.77310576560654));
#89875=CARTESIAN_POINT('Ctrl Pts',(0.585799999999991,2.72010252438485,2.67992491422671));
#89876=CARTESIAN_POINT('Ctrl Pts',(0.585799999999991,2.79304166360886,2.58329939719082));
#89877=CARTESIAN_POINT('Ctrl Pts',(0.585799999999991,2.86593404565316,2.48673582133924));
#89878=CARTESIAN_POINT('Ctrl Pts',(0.585799999999991,2.93440222148946,2.38673110322598));
#89879=CARTESIAN_POINT('Ctrl Pts',(0.585799999999989,2.99821451712912,2.28366714323217));
#89880=CARTESIAN_POINT('Ctrl Pts',(0.585799999999988,3.03261534584538,2.22810597592068));
#89881=CARTESIAN_POINT('Ctrl Pts',(0.585799999999991,3.0656622305983,2.1716554512815));
#89882=CARTESIAN_POINT('Ctrl Pts',(0.585799999999992,3.09731265936069,2.11437429574504));
#89883=CARTESIAN_POINT('Ctrl Pts',(0.585799999999992,3.10817794722411,2.09471022582911));
#89884=CARTESIAN_POINT('Ctrl Pts',(0.585799999999988,3.11888004010657,2.07494541123311));
#89885=CARTESIAN_POINT('Ctrl Pts',(0.585799999999988,3.12940560295807,2.05510444625068));
#89886=CARTESIAN_POINT('Ctrl Pts',(0.585799999999988,3.18506667019072,1.95018185907613));
#89887=CARTESIAN_POINT('Ctrl Pts',(0.585799999999991,3.23586400154897,1.84300973943562));
#89888=CARTESIAN_POINT('Ctrl Pts',(0.585799999999991,3.28162189719394,1.73396327121137));
#89889=CARTESIAN_POINT('Ctrl Pts',(0.585799999999992,3.3269647454697,1.625905909875));
#89890=CARTESIAN_POINT('Ctrl Pts',(0.585799999999992,3.36735937924477,1.51600719065838));
#89891=CARTESIAN_POINT('Ctrl Pts',(0.58579999999999,3.40258571934794,1.40462038544498));
#89892=CARTESIAN_POINT('Ctrl Pts',(0.585799999999989,3.43679103713209,1.29646208520354));
#89893=CARTESIAN_POINT('Ctrl Pts',(0.58579999999999,3.46612334072379,1.18689998727959));
#89894=CARTESIAN_POINT('Ctrl Pts',(0.585799999999992,3.49033317665986,1.07625791163838));
#89895=CARTESIAN_POINT('Ctrl Pts',(0.585799999999994,3.5145408993762,0.965625493684133));
#89896=CARTESIAN_POINT('Ctrl Pts',(0.585799999999996,3.5336272953427,0.853912602230459));
#89897=CARTESIAN_POINT('Ctrl Pts',(0.585799999999991,3.54729199691672,0.741453780800409));
#89898=CARTESIAN_POINT('Ctrl Pts',(0.58579999999999,3.54907908440556,0.726746269502171));
#89899=CARTESIAN_POINT('Ctrl Pts',(0.585799999999992,3.55077294157688,0.712029231162681));
#89900=CARTESIAN_POINT('Ctrl Pts',(0.585799999999992,3.55237217730448,0.697311529599281));
#89901=CARTESIAN_POINT('Ctrl Pts',(0.585799999999991,3.564454224488,0.58612093921081));
#89902=CARTESIAN_POINT('Ctrl Pts',(0.585799999999992,3.57115664198564,0.474755467253984));
#89903=CARTESIAN_POINT('Ctrl Pts',(0.585799999999994,3.57228231247333,0.363530962342787));
#89904=CARTESIAN_POINT('Ctrl Pts',(0.585799999999995,3.57293014058781,0.299520790548671));
#89905=CARTESIAN_POINT('Ctrl Pts',(0.585799999999992,3.57172999413913,0.235557298783211));
#89906=CARTESIAN_POINT('Ctrl Pts',(0.585799999999993,3.56863646597307,0.171701567603425));
#89907=CARTESIAN_POINT('Ctrl Pts',(0.585799999999994,3.56316184516739,0.0586959973568367));
#89908=CARTESIAN_POINT('Ctrl Pts',(0.585799999999995,3.55176000723791,-0.0539733642235792));
#89909=CARTESIAN_POINT('Ctrl Pts',(0.585799999999996,3.53464522492657,-0.165950017323518));
#89910=CARTESIAN_POINT('Ctrl Pts',(0.585799999999996,3.51745024634637,-0.278451369459369));
#89911=CARTESIAN_POINT('Ctrl Pts',(0.585799999999995,3.49448812402454,-0.390254307938234));
#89912=CARTESIAN_POINT('Ctrl Pts',(0.585799999999996,3.46593137547018,-0.500970793960552));
#89913=CARTESIAN_POINT('Ctrl Pts',(0.585799999999996,3.45734555588329,-0.534258609359854));
#89914=CARTESIAN_POINT('Ctrl Pts',(0.585799999999996,3.44825373273905,-0.567447988369024));
#89915=CARTESIAN_POINT('Ctrl Pts',(0.585799999999996,3.43865992038094,-0.600527751346839));
#89916=CARTESIAN_POINT('Ctrl Pts',(0.585799999999996,3.43333132637031,-0.61890090899228));
#89917=CARTESIAN_POINT('Ctrl Pts',(0.585799999999998,3.42784720581633,-0.637242086460123));
#89918=CARTESIAN_POINT('Ctrl Pts',(0.585799999999998,3.42221506109668,-0.655528003234818));
#89919=CARTESIAN_POINT('Ctrl Pts',(0.585799999999997,3.3894351801136,-0.761954632055157));
#89920=CARTESIAN_POINT('Ctrl Pts',(0.585799999999997,3.35159967116233,-0.866672925050383));
#89921=CARTESIAN_POINT('Ctrl Pts',(0.585799999999998,3.30894399549316,-0.969356272713158));
#89922=CARTESIAN_POINT('Ctrl Pts',(0.585799999999998,3.26622213144329,-1.07219895308841));
#89923=CARTESIAN_POINT('Ctrl Pts',(0.585799999999998,3.21866454774918,-1.17300112326194));
#89924=CARTESIAN_POINT('Ctrl Pts',(0.585799999999997,3.16646307567001,-1.27140745990975));
#89925=CARTESIAN_POINT('Ctrl Pts',(0.585799999999996,3.11519187949628,-1.36806010953914));
#89926=CARTESIAN_POINT('Ctrl Pts',(0.585799999999999,3.05944019547891,-1.46240213536194));
#89927=CARTESIAN_POINT('Ctrl Pts',(0.585799999999999,2.99935592247331,-1.55406095152871));
#89928=CARTESIAN_POINT('Ctrl Pts',(0.585799999999999,2.94555794445917,-1.6361299977246));
#89929=CARTESIAN_POINT('Ctrl Pts',(0.585799999999998,2.88828584813885,-1.7160477730359));
#89930=CARTESIAN_POINT('Ctrl Pts',(0.585799999999998,2.8276281243483,-1.79351600647639));
#89931=CARTESIAN_POINT('Ctrl Pts',(0.585799999999998,2.81803085597279,-1.80577303460807));
#89932=CARTESIAN_POINT('Ctrl Pts',(0.585800000000001,2.80835473108984,-1.81796109589995));
#89933=CARTESIAN_POINT('Ctrl Pts',(0.585800000000001,2.79860130069776,-1.83007805473447));
#89934=CARTESIAN_POINT('Ctrl Pts',(0.5858,2.73119899243548,-1.91381382376484));
#89935=CARTESIAN_POINT('Ctrl Pts',(0.585799999999997,2.660092568064,-1.99417628046629));
#89936=CARTESIAN_POINT('Ctrl Pts',(0.585799999999997,2.58545667302995,-2.070844698974));
#89937=CARTESIAN_POINT('Ctrl Pts',(0.585799999999998,2.51187463795161,-2.14643055826412));
#89938=CARTESIAN_POINT('Ctrl Pts',(0.585799999999998,2.43486151262633,-2.21842647190396));
#89939=CARTESIAN_POINT('Ctrl Pts',(0.585799999999998,2.35455634075026,-2.28648423693865));
#89940=CARTESIAN_POINT('Ctrl Pts',(0.585799999999999,2.27672129251548,-2.35244859889035));
#89941=CARTESIAN_POINT('Ctrl Pts',(0.585799999999995,2.19579306375139,-2.41471364081201));
#89942=CARTESIAN_POINT('Ctrl Pts',(0.585799999999996,2.11187976848003,-2.47291808201015));
#89943=CARTESIAN_POINT('Ctrl Pts',(0.585799999999996,2.03430797415558,-2.52672389343481));
#89944=CARTESIAN_POINT('Ctrl Pts',(0.585799999999997,1.9541847994988,-2.57705949460462));
#89945=CARTESIAN_POINT('Ctrl Pts',(0.585799999999993,1.87158653173903,-2.62360084935061));
#89946=CARTESIAN_POINT('Ctrl Pts',(0.173952222118149,2.28357519912527,-3.20566422525929));
#89947=CARTESIAN_POINT('Ctrl Pts',(0.240279004907857,3.35237972307857,-2.44437977786446));
#89948=CARTESIAN_POINT('Ctrl Pts',(0.372888193944113,4.64898952799387,0.217548081197305));
#89949=CARTESIAN_POINT('Ctrl Pts',(0.571779789226917,2.32539586803166,4.03618744464615));
#89950=CARTESIAN_POINT('Ctrl Pts',(0.77062700796656,-2.13583691697174,4.13464652641104));
#89951=CARTESIAN_POINT('Ctrl Pts',(0.969474226706204,-4.63403193779818,
0.440985093923363));
#89952=CARTESIAN_POINT('Ctrl Pts',(1.16832144544584,-2.87607675100017,-3.6608002142644));
#89953=CARTESIAN_POINT('Ctrl Pts',(1.36716866418549,1.524085161197,-4.39826153122039));
#89954=CARTESIAN_POINT('Ctrl Pts',(1.56601588292513,4.52409602411104,-1.09639957599426));
#89955=CARTESIAN_POINT('Ctrl Pts',(1.76486310166478,3.36844732971546,3.21302626912509));
#89956=CARTESIAN_POINT('Ctrl Pts',(1.96371032040441,-0.881431179013023,
4.57080526913485));
#89957=CARTESIAN_POINT('Ctrl Pts',(2.16255753914406,-4.3216225377087,1.73005466709287));
#89958=CARTESIAN_POINT('Ctrl Pts',(2.3614047578837,-3.79207170539569,-2.69995067838618));
#89959=CARTESIAN_POINT('Ctrl Pts',(2.56025197662336,0.220804693931135,-4.64980423380701));
#89960=CARTESIAN_POINT('Ctrl Pts',(2.759099195363,4.03085120606417,-2.32845977156154));
#89961=CARTESIAN_POINT('Ctrl Pts',(2.95794641410263,4.13824202747698,2.13176900450027));
#89962=CARTESIAN_POINT('Ctrl Pts',(3.15679363284228,0.444327587898382,4.63379380141549));
#89963=CARTESIAN_POINT('Ctrl Pts',(3.35564085158192,-3.65773661521517,2.87931292379523));
#89964=CARTESIAN_POINT('Ctrl Pts',(3.55448807032156,-4.39987910846512,-1.52004710629562));
#89965=CARTESIAN_POINT('Ctrl Pts',(3.75333528906121,-1.10038262959936,-4.52312233170167));
#89966=CARTESIAN_POINT('Ctrl Pts',(3.95218250780086,3.20990273307694,-3.37135035508323));
#89967=CARTESIAN_POINT('Ctrl Pts',(4.15102972654051,4.57163721316586,0.877275198462322));
#89968=CARTESIAN_POINT('Ctrl Pts',(4.34987694528013,1.73395935114604,4.32005362547157));
#89969=CARTESIAN_POINT('Ctrl Pts',(4.54872416401979,-2.69649805273161,3.79451930930212));
#89970=CARTESIAN_POINT('Ctrl Pts',(4.74757138275942,-4.65000757025798,-0.216582764486197));
#89971=CARTESIAN_POINT('Ctrl Pts',(4.94641860149908,-2.33211535592997,-4.02873633259774));
#89972=CARTESIAN_POINT('Ctrl Pts',(5.1452658202387,2.12801026500781,-4.14017521473941));
#89973=CARTESIAN_POINT('Ctrl Pts',(5.34411303897837,4.63338923547031,-0.44853392512834));
#89974=CARTESIAN_POINT('Ctrl Pts',(5.54296025771799,2.88263173829438,3.65512144091822));
#89975=CARTESIAN_POINT('Ctrl Pts',(5.74180747645765,-1.51605224178122,4.4012571034094));
#89976=CARTESIAN_POINT('Ctrl Pts',(5.94065469519728,-4.52212167899159,1.10448812091657));
#89977=CARTESIAN_POINT('Ctrl Pts',(6.13950191393694,-3.37426274767644,-3.20684103101759));
#89978=CARTESIAN_POINT('Ctrl Pts',(6.33834913267657,0.873124844100889,-4.57243168299889));
#89979=CARTESIAN_POINT('Ctrl Pts',(6.53719635141622,4.31847783430739,-1.7378802270194));
#89980=CARTESIAN_POINT('Ctrl Pts',(6.73604357015585,3.7969655214586,2.69305241644208));
#89981=CARTESIAN_POINT('Ctrl Pts',(6.93489078889551,-0.212361563592659,
4.65020225960404));
#89982=CARTESIAN_POINT('Ctrl Pts',(7.13373800763515,-4.02661766515626,2.33577153581771));
#89983=CARTESIAN_POINT('Ctrl Pts',(7.33258522637479,-4.14210523822186,-2.12425108788485));
#89984=CARTESIAN_POINT('Ctrl Pts',(7.53143244511446,-0.452739763174514,
-4.63298016353779));
#89985=CARTESIAN_POINT('Ctrl Pts',(7.73027966385406,3.65250318693606,-2.88594853701702));
#89986=CARTESIAN_POINT('Ctrl Pts',(7.92912688259373,4.40263150697405,1.5120563159779));
#89987=CARTESIAN_POINT('Ctrl Pts',(8.12797410133337,1.10859268358586,4.52111720162066));
#89988=CARTESIAN_POINT('Ctrl Pts',(8.32682132007301,-3.20377667673212,3.37717241113287));
#89989=CARTESIAN_POINT('Ctrl Pts',(8.52566853881265,-4.57322239004683,-0.86897379711017));
#89990=CARTESIAN_POINT('Ctrl Pts',(8.7245157575523,-1.74179966817418,-4.31689847052698));
#89991=CARTESIAN_POINT('Ctrl Pts',(8.92336297629194,2.68960455960068,-3.79940861212176));
#89992=CARTESIAN_POINT('Ctrl Pts',(9.12221019503159,4.65039311774333,0.208140191542384));
#89993=CARTESIAN_POINT('Ctrl Pts',(9.32105741377122,2.33942579057017,4.02449567763527));
#89994=CARTESIAN_POINT('Ctrl Pts',(9.51990463251087,-2.12049016010714,4.14403184951306));
#89995=CARTESIAN_POINT('Ctrl Pts',(9.71875185125051,-4.63256727397068,0.456945227599198));
#89996=CARTESIAN_POINT('Ctrl Pts',(9.91759906999016,-2.88926295756309,-3.64988192287692));
#89997=CARTESIAN_POINT('Ctrl Pts',(10.1164462887298,1.50805914415905,-4.404002282766));
#89998=CARTESIAN_POINT('Ctrl Pts',(10.3152935074695,4.52010899870567,-1.11269633265763));
#89999=CARTESIAN_POINT('Ctrl Pts',(10.5141407262091,3.38007929167327,3.2007096823816));
#90000=CARTESIAN_POINT('Ctrl Pts',(10.7129879449488,-0.86482203405061,4.57400932862083));
#90001=CARTESIAN_POINT('Ctrl Pts',(10.9118351636884,-4.31531554947323,1.74571767401385));
#90002=CARTESIAN_POINT('Ctrl Pts',(11.1106823824281,-3.80184857193813,-2.68615448642514));
#90003=CARTESIAN_POINT('Ctrl Pts',(11.3095296011677,0.203918647976768,-4.65058014379897));
#90004=CARTESIAN_POINT('Ctrl Pts',(11.5083768199074,4.02237037378927,-2.34307811755224));
#90005=CARTESIAN_POINT('Ctrl Pts',(11.707224038647,4.14595504597677,2.11672748497051));
#90006=CARTESIAN_POINT('Ctrl Pts',(11.9060712573866,0.46115031548507,4.6321505670064));
#90007=CARTESIAN_POINT('Ctrl Pts',(12.1049184761263,-3.64725765118733,2.89257499725508));
#90008=CARTESIAN_POINT('Ctrl Pts',(12.3037656948659,-4.40536942950588,-1.50406072964653));
#90009=CARTESIAN_POINT('Ctrl Pts',(12.5026129136056,-1.1167990648287,-4.51909707106271));
#90010=CARTESIAN_POINT('Ctrl Pts',(12.7014601323452,3.19764005053429,-3.38298338690999));
#90011=CARTESIAN_POINT('Ctrl Pts',(12.9003073510849,4.57479249805102,0.860669558347425));
#90012=CARTESIAN_POINT('Ctrl Pts',(13.0991545698245,1.74963424132104,4.31372907244841));
#90013=CARTESIAN_POINT('Ctrl Pts',(13.2980017885641,-2.68270219976425,3.80428539889818));
#90014=CARTESIAN_POINT('Ctrl Pts',(13.4968490073038,-4.65076333761376,-0.199696936375007));
#90015=CARTESIAN_POINT('Ctrl Pts',(13.6956962260434,-2.34672851375597,-4.02024175536926));
#90016=CARTESIAN_POINT('Ctrl Pts',(13.8945434447831,2.11296306557631,-4.1478748260284));
#90017=CARTESIAN_POINT('Ctrl Pts',(14.0933906635227,4.63173004298792,-0.465355023366944));
#90018=CARTESIAN_POINT('Ctrl Pts',(14.2922378822624,2.89588465336402,3.64463037402978));
#90019=CARTESIAN_POINT('Ctrl Pts',(14.491085101002,-1.50006107573536,4.40673294606713));
#90020=CARTESIAN_POINT('Ctrl Pts',(14.6899323197417,-4.51808141952556,1.12090087671823));
#90021=CARTESIAN_POINT('Ctrl Pts',(14.8887795384813,-3.38588469444997,-3.19456778371962));
#90022=CARTESIAN_POINT('Ctrl Pts',(15.0876267572209,0.856516373422385,-4.57557189769205));
#90023=CARTESIAN_POINT('Ctrl Pts',(15.2864739759606,4.31213904075985,-1.75354936686836));
#90024=CARTESIAN_POINT('Ctrl Pts',(15.4853211947002,3.80671909099388,2.67924770246286));
#90025=CARTESIAN_POINT('Ctrl Pts',(15.6841684134399,-0.195475060215983,
4.65094269903676));
#90026=CARTESIAN_POINT('Ctrl Pts',(15.8830156321795,-4.01810982412929,2.35037697617328));
#90027=CARTESIAN_POINT('Ctrl Pts',(16.0818628509192,-4.14979118808601,-2.10919690502656));
#90028=CARTESIAN_POINT('Ctrl Pts',(16.2807100696588,-0.469559347780013,
-4.63130570226176));
#90029=CARTESIAN_POINT('Ctrl Pts',(16.4795572883984,3.64200009356924,-2.89919192316264));
#90030=CARTESIAN_POINT('Ctrl Pts',(16.6784045071381,4.40809283132617,1.49606018572135));
#90031=CARTESIAN_POINT('Ctrl Pts',(16.8772517258777,1.12500176494622,4.51706204493116));
#90032=CARTESIAN_POINT('Ctrl Pts',(17.0760989446174,-3.19149288446924,3.38878321190246));
#90033=CARTESIAN_POINT('Ctrl Pts',(17.274946163357,-4.57634752690168,-0.852362482697826));
#90034=CARTESIAN_POINT('Ctrl Pts',(17.4737933820967,-1.75746304742967,-4.31054545571777));
#90035=CARTESIAN_POINT('Ctrl Pts',(17.6726406008363,2.67579099736758,-3.8091496462198));
#90036=CARTESIAN_POINT('Ctrl Pts',(17.8714878195759,4.65111822792017,0.191253022978689));
#90037=CARTESIAN_POINT('Ctrl Pts',(18.0703350383156,2.35402350179763,4.01597458182621));
#90038=CARTESIAN_POINT('Ctrl Pts',(18.2691822570552,-2.10542900642473,4.15170413057039));
#90039=CARTESIAN_POINT('Ctrl Pts',(18.4680294757949,-4.63087754517756,0.473763285259743));
#90040=CARTESIAN_POINT('Ctrl Pts',(18.6668766945345,-2.90249680392564,-3.63936681197312));
#90041=CARTESIAN_POINT('Ctrl Pts',(18.8657239132742,1.49205806290137,-4.40944908416242));
#90042=CARTESIAN_POINT('Ctrl Pts',(19.0645711320138,4.51603894811952,-1.12910172613336));
#90043=CARTESIAN_POINT('Ctrl Pts',(19.2634183507534,3.39167893687894,3.18841535531705));
#90044=CARTESIAN_POINT('Ctrl Pts',(19.4622655694931,-0.84820788959677,4.57711938504072));
#90045=CARTESIAN_POINT('Ctrl Pts',(19.6611127882327,-4.3089483186353,1.7613752797799));
#90046=CARTESIAN_POINT('Ctrl Pts',(19.8599600069724,-3.81157706257311,-2.67233208732681));
#90047=CARTESIAN_POINT('Ctrl Pts',(20.058807225712,0.187030828142195,-4.65128992411937));
#90048=CARTESIAN_POINT('Ctrl Pts',(20.2576544444516,4.01383603021948,-2.35766808762422));
#90049=CARTESIAN_POINT('Ctrl Pts',(20.4565016631913,4.15361365190522,2.10165937287571));
#90050=CARTESIAN_POINT('Ctrl Pts',(20.6553488819309,0.477966832341934,4.63044557208816));
#90051=CARTESIAN_POINT('Ctrl Pts',(20.8541961006706,-3.6367305314113,2.90579929292968));
#90052=CARTESIAN_POINT('Ctrl Pts',(21.0530433194102,-4.41080170345829,-1.48805471057328));
#90053=CARTESIAN_POINT('Ctrl Pts',(21.2518905381499,-1.13320075690117,-4.51501212993371));
#90054=CARTESIAN_POINT('Ctrl Pts',(21.4507377568895,3.18533519879899,-3.39457186699324));
#90055=CARTESIAN_POINT('Ctrl Pts',(21.6495849756292,4.57788747147318,0.844052597542735));
#90056=CARTESIAN_POINT('Ctrl Pts',(21.8484321943688,1.7652860606952,4.30734763082863));
#90057=CARTESIAN_POINT('Ctrl Pts',(22.0472794131084,-2.66887097519087,3.81400133805345));
#90058=CARTESIAN_POINT('Ctrl Pts',(22.2461266318481,-4.65145778749283,-0.182808479185734));
#90059=CARTESIAN_POINT('Ctrl Pts',(22.4449738505877,-2.3613107306498,-4.01169417107137));
#90060=CARTESIAN_POINT('Ctrl Pts',(22.6438210693274,2.09788800748582,-4.15551975051701));
#90061=CARTESIAN_POINT('Ctrl Pts',(22.8426682880671,4.63000978334952,-0.482169985562706));
#90062=CARTESIAN_POINT('Ctrl Pts',(23.0415155068066,2.90909938745336,3.63409125405627));
#90063=CARTESIAN_POINT('Ctrl Pts',(23.2403627255463,-1.48405013203601,4.41215068809913));
#90064=CARTESIAN_POINT('Ctrl Pts',(23.4392099442859,-4.51398159121979,1.13729885387195));
#90065=CARTESIAN_POINT('Ctrl Pts',(23.6380571630256,-3.39746199986158,-3.18225241745317));
#90066=CARTESIAN_POINT('Ctrl Pts',(23.8369043817652,0.839896609959785,-4.57865178556615));
#90067=CARTESIAN_POINT('Ctrl Pts',(24.0357516005049,4.30574339361672,-1.769195386953));
#90068=CARTESIAN_POINT('Ctrl Pts',(24.2345988192446,3.81642247066319,2.66540766381184));
#90069=CARTESIAN_POINT('Ctrl Pts',(24.4334460379841,-0.178585979588697,
4.65162181790224));
#90070=CARTESIAN_POINT('Ctrl Pts',(24.6322932567239,-4.00954900614679,2.36495142787269));
#90071=CARTESIAN_POINT('Ctrl Pts',(24.8311404754634,-4.15742242483508,-2.0941149133627));
#90072=CARTESIAN_POINT('Ctrl Pts',(25.0299876942031,-0.4863727414586,-4.62957017932074));
#90073=CARTESIAN_POINT('Ctrl Pts',(25.2288349129427,3.63144898208279,-2.91239708477736));
#90074=CARTESIAN_POINT('Ctrl Pts',(25.4276821316824,4.41349603697337,1.48004433058948));
#90075=CARTESIAN_POINT('Ctrl Pts',(25.626529350422,1.14139601366861,4.5129473328271));
#90076=CARTESIAN_POINT('Ctrl Pts',(25.8253765691617,-3.17916701381997,3.40034933310223));
#90077=CARTESIAN_POINT('Ctrl Pts',(26.0242237879013,-4.57941232668972,-0.835739930272565));
#90078=CARTESIAN_POINT('Ctrl Pts',(26.2230710066409,-1.77310325533199,-4.30413560832147));
#90079=CARTESIAN_POINT('Ctrl Pts',(26.4219182253806,2.66194215604348,-3.81884045840728));
#90080=CARTESIAN_POINT('Ctrl Pts',(26.6207654441202,4.65178201521246,0.174363332830453));
#90081=CARTESIAN_POINT('Ctrl Pts',(26.8196126628599,2.36859017629287,4.00740053721347));
#90082=CARTESIAN_POINT('Ctrl Pts',(27.0184598815995,-2.09034009361562,4.15932167329157));
#90083=CARTESIAN_POINT('Ctrl Pts',(27.2173071003392,-4.62912676036407,0.490575096566251));
#90084=CARTESIAN_POINT('Ctrl Pts',(27.4161543190788,-2.91569238218416,-3.62880371766826));
#90085=CARTESIAN_POINT('Ctrl Pts',(27.6150015378185,1.47603730953467,-4.41483774897238));
#90086=CARTESIAN_POINT('Ctrl Pts',(27.8138487565581,4.5119093556078,-1.14549223291496));
#90087=CARTESIAN_POINT('Ctrl Pts',(28.0126959752978,3.40323386433599,3.17607899044191));
#90088=CARTESIAN_POINT('Ctrl Pts',(28.2115431940374,-0.831582561906483,
4.58016909421725));
#90089=CARTESIAN_POINT('Ctrl Pts',(28.410390412777,-4.30252427626788,1.77700966261172));
#90090=CARTESIAN_POINT('Ctrl Pts',(28.6092376315167,-3.82125529929308,-2.65847445474172));
#90091=CARTESIAN_POINT('Ctrl Pts',(28.8080848502563,0.170140542390847,-4.65193837929144));
#90092=CARTESIAN_POINT('Ctrl Pts',(29.006932068996,4.00524876604184,-2.37222697291178));
#90093=CARTESIAN_POINT('Ctrl Pts',(29.2057792877356,4.16121749432138,2.08656355135507));
#90094=CARTESIAN_POINT('Ctrl Pts',(29.4046265064753,0.494777047422964,4.62867952684493));
#90095=CARTESIAN_POINT('Ctrl Pts',(29.6034737252149,-3.62615546299245,2.91898527695842));
#90096=CARTESIAN_POINT('Ctrl Pts',(29.8023209439545,-4.41617582299051,-1.47202907217344));
#90097=CARTESIAN_POINT('Ctrl Pts',(30.0011681626942,-1.14958750823563,-4.51086766041727));
#90098=CARTESIAN_POINT('Ctrl Pts',(30.2000153814338,3.17298834986358,-3.40611559118592));
#90099=CARTESIAN_POINT('Ctrl Pts',(30.3988626001735,4.58092208752509,0.827424508287263));
#90100=CARTESIAN_POINT('Ctrl Pts',(30.5977098189131,1.78091460557327,4.30090939878366));
#90101=CARTESIAN_POINT('Ctrl Pts',(30.7965570376528,-2.65500456276395,3.82366699133076));
#90102=CARTESIAN_POINT('Ctrl Pts',(30.9954042563924,-4.65209091001037,-0.165917611749485));
#90103=CARTESIAN_POINT('Ctrl Pts',(31.1942514751321,-2.37586181473258,-4.00309369440504));
#90104=CARTESIAN_POINT('Ctrl Pts',(31.3930986938717,2.08278528969322,-4.16310988636228));
#90105=CARTESIAN_POINT('Ctrl Pts',(31.5919459126113,4.62822847913179,-0.498978590566));
#90106=CARTESIAN_POINT('Ctrl Pts',(31.790793131351,2.92227576638665,3.62350422023752));
#90107=CARTESIAN_POINT('Ctrl Pts',(31.9896403500906,-1.46801962180864,4.41751025792524));
#90108=CARTESIAN_POINT('Ctrl Pts',(32.1884875688303,-4.50982224811389,1.15368183625598));
#90109=CARTESIAN_POINT('Ctrl Pts',(32.3873347875699,-3.40899451127737,-3.16989509463177));
#90110=CARTESIAN_POINT('Ctrl Pts',(32.5861820063095,0.823265772841283,-4.58167130599281));
#90111=CARTESIAN_POINT('Ctrl Pts',(32.7850292250492,4.29929097719954,-1.78481808099885));
#90112=CARTESIAN_POINT('Ctrl Pts',(32.9838764437888,3.82607553253298,2.65153248296947));
#90113=CARTESIAN_POINT('Ctrl Pts',(33.1827236625285,-0.161694544386196,
4.65223960724354));
#90114=CARTESIAN_POINT('Ctrl Pts',(33.3815708812681,-4.00093532407891,2.37949469876008));
#90115=CARTESIAN_POINT('Ctrl Pts',(33.5804181000078,-4.1649988478549,-2.07900531174335));
#90116=CARTESIAN_POINT('Ctrl Pts',(33.7792653187474,-0.503179722533174,
-4.6277736175964));
#90117=CARTESIAN_POINT('Ctrl Pts',(33.9781125374871,3.62084999158835,-2.92556384775728));
#90118=CARTESIAN_POINT('Ctrl Pts',(34.1769597562267,4.41884105267683,1.46400896174433));
#90119=CARTESIAN_POINT('Ctrl Pts',(34.3758069749664,1.15777521360213,4.50877311955908));
#90120=CARTESIAN_POINT('Ctrl Pts',(34.574654193706,-3.16679922729543,3.41187062223805));
#90121=CARTESIAN_POINT('Ctrl Pts',(34.7735014124457,-4.58241674900297,-0.81910635899549));
#90122=CARTESIAN_POINT('Ctrl Pts',(34.9723486311852,-1.78872008567185,-4.29766901284916));
#90123=CARTESIAN_POINT('Ctrl Pts',(35.1711958499249,2.64805821821942,-3.82848092091503));
#90124=CARTESIAN_POINT('Ctrl Pts',(35.3700430686646,4.65238447086841,0.157471343780943));
#90125=CARTESIAN_POINT('Ctrl Pts',(35.5688902874042,2.38312562200067,3.99877365684203));
#90126=CARTESIAN_POINT('Ctrl Pts',(35.7677375061439,-2.07522362062035,4.16688437724269));
#90127=CARTESIAN_POINT('Ctrl Pts',(35.9665847248835,-4.62731494261354,0.507380439862646));
#90128=CARTESIAN_POINT('Ctrl Pts',(36.1654319436232,-2.9288495183609,-3.61819277923204));
#90129=CARTESIAN_POINT('Ctrl Pts',(36.3642791623628,1.45999709528542,-4.42016820614871));
#90130=CARTESIAN_POINT('Ctrl Pts',(36.5631263811024,4.50772027561737,-1.16186763690095));
#90131=CARTESIAN_POINT('Ctrl Pts',(36.7619735998421,3.4147439216979,3.1637007504056));
#90132=CARTESIAN_POINT('Ctrl Pts',(36.9608208185817,-0.814946270177291,
4.58315841594136));
#90133=CARTESIAN_POINT('Ctrl Pts',(37.1596680373214,-4.29604350706908,1.79262061637693));
#90134=CARTESIAN_POINT('Ctrl Pts',(37.358515256061,-3.83088315449479,-2.64458177137669));
#90135=CARTESIAN_POINT('Ctrl Pts',(37.5573624748007,0.153248013413796,-4.65252550076564));
#90136=CARTESIAN_POINT('Ctrl Pts',(37.7562096935402,3.99660869447566,-2.38675458146231));
#90137=CARTESIAN_POINT('Ctrl Pts',(37.95505691228,4.16876647297188,2.07144021944043));
#90138=CARTESIAN_POINT('Ctrl Pts',(38.1539041310195,0.51158073909287,4.6268524545612));
#90139=CARTESIAN_POINT('Ctrl Pts',(38.3527513497593,-3.61553258535822,2.93213277548999));
#90140=CARTESIAN_POINT('Ctrl Pts',(38.5515985684988,-4.42149171724726,-1.4559840257378));
#90141=CARTESIAN_POINT('Ctrl Pts',(38.7504457872385,-1.16595910278014,-4.5066637171564));
#90142=CARTESIAN_POINT('Ctrl Pts',(38.9492930059781,3.1605996665157,-3.41761440728918));
#90143=CARTESIAN_POINT('Ctrl Pts',(39.1481402247178,4.58389630619673,0.81078550981488));
#90144=CARTESIAN_POINT('Ctrl Pts',(39.3469874434575,1.7965196698999,4.2944144611987));
#90145=CARTESIAN_POINT('Ctrl Pts',(39.545834662197,-2.64110314530594,3.8332822312928));
#90146=CARTESIAN_POINT('Ctrl Pts',(39.7446818809367,-4.65266269681899,-0.149024556764877));
#90147=CARTESIAN_POINT('Ctrl Pts',(39.9435290996763,-2.39038157415463,-3.99444043876384));
#90148=CARTESIAN_POINT('Ctrl Pts',(40.1423763184159,2.06765511132127,-4.17064513349156));
#90149=CARTESIAN_POINT('Ctrl Pts',(40.3412235371556,4.62638615382046,-0.515780616762658));
#90150=CARTESIAN_POINT('Ctrl Pts',(40.5400707558953,2.93541361643903,3.61286941215899));
#90151=CARTESIAN_POINT('Ctrl Pts',(40.7389179746349,-1.45196975640838,4.42281158488186));
#90152=CARTESIAN_POINT('Ctrl Pts',(40.9377651933746,-4.50560344504676,1.17004960786819));
#90153=CARTESIAN_POINT('Ctrl Pts',(41.1366124121142,-3.42048207664657,-3.15749597818099));
#90154=CARTESIAN_POINT('Ctrl Pts',(41.3354596308539,0.806624081336881,-4.58463041916116));
#90155=CARTESIAN_POINT('Ctrl Pts',(41.5343068495934,4.29278187658053,-1.80041724302757));
#90156=CARTESIAN_POINT('Ctrl Pts',(41.7331540683332,3.83567814933202,2.63762234287354));
#90157=CARTESIAN_POINT('Ctrl Pts',(41.9320012870728,-0.144800977314504,
4.65279605891583));
#90158=CARTESIAN_POINT('Ctrl Pts',(42.1308485058124,-3.99226889149313,2.3940065970881));
#90159=CARTESIAN_POINT('Ctrl Pts',(42.3296957245521,-4.17252035725389,-2.06386829938026));
#90160=CARTESIAN_POINT('Ctrl Pts',(42.5285429432917,-0.519980069410792,
-4.62591604077868));
#90161=CARTESIAN_POINT('Ctrl Pts',(42.7273901620314,3.61020326182819,-2.9386920384986));
#90162=CARTESIAN_POINT('Ctrl Pts',(42.926237380771,4.42412780796626,1.44795429059375));
#90163=CARTESIAN_POINT('Ctrl Pts',(43.1250845995107,1.17413914879181,4.50453946018377));
#90164=CARTESIAN_POINT('Ctrl Pts',(43.3239318182503,-3.15438968795409,3.42334692736563));
#90165=CARTESIAN_POINT('Ctrl Pts',(43.52277903699,-4.58536075423916,-0.802461988093299));
#90166=CARTESIAN_POINT('Ctrl Pts',(43.7216262557296,-1.80431333253019,-4.29114575471113));
#90167=CARTESIAN_POINT('Ctrl Pts',(43.9204734744692,2.63413936691317,-3.8380709063487));
#90168=CARTESIAN_POINT('Ctrl Pts',(44.1193206932088,4.65292558701255,0.140577277989422));
#90169=CARTESIAN_POINT('Ctrl Pts',(44.3181679119485,2.39762964714867,3.99009405551234));
#90170=CARTESIAN_POINT('Ctrl Pts',(44.5170151306882,-2.06007978649544,4.17439214068712));
#90171=CARTESIAN_POINT('Ctrl Pts',(44.7158623494278,-4.62544211628707,0.524179097453273));
#90172=CARTESIAN_POINT('Ctrl Pts',(44.9147095681674,-2.9419680380799,-3.60753414397816));
#90173=CARTESIAN_POINT('Ctrl Pts',(45.1135567869071,1.44393762990557,-4.42544037123081));
#90174=CARTESIAN_POINT('Ctrl Pts',(45.3124040056467,4.50347176669087,-1.17822774931598));
#90175=CARTESIAN_POINT('Ctrl Pts',(45.5112512243863,3.42620895087503,3.15128085030174));
#90176=CARTESIAN_POINT('Ctrl Pts',(45.710098443126,-0.798299221633414,4.58608721153467));
#90177=CARTESIAN_POINT('Ctrl Pts',(45.9089456618656,-4.28950611966511,1.80820812513962));
#90178=CARTESIAN_POINT('Ctrl Pts',(46.1077928806053,-3.84046045689732,-2.63065458364033));
#90179=CARTESIAN_POINT('Ctrl Pts',(46.306640099345,0.13635337910788,-4.65305058595005));
#90180=CARTESIAN_POINT('Ctrl Pts',(46.5054873180845,3.98791609169654,-2.40125205093354));
#90181=CARTESIAN_POINT('Ctrl Pts',(46.7043345368243,4.17626017793529,2.05629211917988));
#90182=CARTESIAN_POINT('Ctrl Pts',(46.9031817555638,0.528378279558735,4.62495951542089));
#90183=CARTESIAN_POINT('Ctrl Pts',(47.1020289743036,-3.60486317437669,2.945250919464));
#90184=CARTESIAN_POINT('Ctrl Pts',(47.3008761930431,-4.42674714342192,-1.43993758120542));
#90185=CARTESIAN_POINT('Ctrl Pts',(47.4997234117828,-1.18231948092862,-4.50236630858751));
#90186=CARTESIAN_POINT('Ctrl Pts',(47.6985706305225,3.14817726267048,-3.42913329311644));
#90187=CARTESIAN_POINT('Ctrl Pts',(47.8974178492621,4.58679487950342,0.794260410053871));
#90188=CARTESIAN_POINT('Ctrl Pts',(48.0962650680017,1.81213014044313,4.28762456725067));
#90189=CARTESIAN_POINT('Ctrl Pts',(48.2951122867414,-2.62722255147639,3.84330292215117));
#90190=CARTESIAN_POINT('Ctrl Pts',(48.493959505481,-4.65306675230442,-0.133002451839397));
#90191=CARTESIAN_POINT('Ctrl Pts',(48.6928067242207,-2.40507281684978,-3.98405898298613));
#90192=CARTESIAN_POINT('Ctrl Pts',(48.8916539429603,2.05288141093679,-4.1813817027399));
#90193=CARTESIAN_POINT('Ctrl Pts',(49.0905011617,4.62378860970624,-0.52589063841688));
#90194=CARTESIAN_POINT('Ctrl Pts',(49.2230659741931,3.50770681921098,2.21507238733057));
#90195=CARTESIAN_POINT('Ctrl Pts',(49.2893483804396,2.49297831328899,3.04566224204766));
#90196=CARTESIAN_POINT('Ctrl Pts',(0.312305742378132,2.14453946293883,-3.01048699365514));
#90197=CARTESIAN_POINT('Ctrl Pts',(0.37863252516784,3.14826970167303,-2.29555343657973));
#90198=CARTESIAN_POINT('Ctrl Pts',(0.511241714204097,4.36593527088205,0.204302641486374));
#90199=CARTESIAN_POINT('Ctrl Pts',(0.710133309486899,2.18381387565399,3.79044371220078));
#90200=CARTESIAN_POINT('Ctrl Pts',(0.908980528226543,-2.00579624292731,
3.88290810155421));
#90201=CARTESIAN_POINT('Ctrl Pts',(1.10782774696618,-4.35188837526965,0.414135666234644));
#90202=CARTESIAN_POINT('Ctrl Pts',(1.30667496570583,-2.70096649031909,-3.43791197611196));
#90203=CARTESIAN_POINT('Ctrl Pts',(1.50552218444547,1.43129106250514,-4.13047287675976));
#90204=CARTESIAN_POINT('Ctrl Pts',(1.70436940318511,4.2486459222133,-1.02964516288757));
#90205=CARTESIAN_POINT('Ctrl Pts',(1.90321662192475,3.16335903024921,3.01740079864124));
#90206=CARTESIAN_POINT('Ctrl Pts',(2.1020638406644,-0.827765141249585,4.29251126953189));
#90207=CARTESIAN_POINT('Ctrl Pts',(2.30091105940404,-4.05850005710013,1.62472009156678));
#90208=CARTESIAN_POINT('Ctrl Pts',(2.49975827814369,-3.56119098754892,-2.53556387370365));
#90209=CARTESIAN_POINT('Ctrl Pts',(2.69860549688333,0.207360974982843,-4.36670037323892));
#90210=CARTESIAN_POINT('Ctrl Pts',(2.89745271562298,3.78543237111287,-2.18669123306836));
#90211=CARTESIAN_POINT('Ctrl Pts',(3.09629993436261,3.88628469012808,2.00197600577016));
#90212=CARTESIAN_POINT('Ctrl Pts',(3.29514715310227,0.417274652083158,4.35166473784776));
#90213=CARTESIAN_POINT('Ctrl Pts',(3.49399437184191,-3.43503490463991,2.70400562836479));
#90214=CARTESIAN_POINT('Ctrl Pts',(3.69284159058154,-4.13199196762965,-1.4274988650365));
#90215=CARTESIAN_POINT('Ctrl Pts',(3.8916888093212,-1.0333857078201,-4.24773151317723));
#90216=CARTESIAN_POINT('Ctrl Pts',(4.09053602806083,3.01446743944127,-3.16608530458669));
#90217=CARTESIAN_POINT('Ctrl Pts',(4.28938324680048,4.29329256055578,0.823862198048239));
#90218=CARTESIAN_POINT('Ctrl Pts',(4.48823046554012,1.62838703848647,4.05702666826332));
#90219=CARTESIAN_POINT('Ctrl Pts',(4.68707768427977,-2.53232146155544,3.56348956881262));
#90220=CARTESIAN_POINT('Ctrl Pts',(4.88592490301941,-4.36689132952691,-0.203396098193201));
#90221=CARTESIAN_POINT('Ctrl Pts',(5.08477212175905,-2.190124246766,-3.78344626195841));
#90222=CARTESIAN_POINT('Ctrl Pts',(5.2836193404987,1.99844611755997,-3.88810017506377));
#90223=CARTESIAN_POINT('Ctrl Pts',(5.48246655923833,4.35128480394624,-0.421224885991602));
#90224=CARTESIAN_POINT('Ctrl Pts',(5.68131377797799,2.70712237646502,3.432578955528));
#90225=CARTESIAN_POINT('Ctrl Pts',(5.88016099671762,-1.42374722830323,4.13328606319474));
#90226=CARTESIAN_POINT('Ctrl Pts',(6.07900821545728,-4.24679178532139,1.03724123583069));
#90227=CARTESIAN_POINT('Ctrl Pts',(6.27785543419691,-3.16882037582503,-3.01159214946066));
#90228=CARTESIAN_POINT('Ctrl Pts',(6.47670265293655,0.81996453848499,-4.2940386590025));
#90229=CARTESIAN_POINT('Ctrl Pts',(6.6755498716762,4.05554681932371,-1.63206919138556));
#90230=CARTESIAN_POINT('Ctrl Pts',(6.87439709041584,3.56578684306324,2.52908561322399));
#90231=CARTESIAN_POINT('Ctrl Pts',(7.0732443091555,-0.199431905597023,4.36707416518995));
#90232=CARTESIAN_POINT('Ctrl Pts',(7.27209152789513,-3.78145658982552,2.1935578197247));
#90233=CARTESIAN_POINT('Ctrl Pts',(7.47093874663477,-3.88991268884659,-1.99491581836445));
#90234=CARTESIAN_POINT('Ctrl Pts',(7.66978596537443,-0.425174651109135,
-4.35090063840494));
#90235=CARTESIAN_POINT('Ctrl Pts',(7.86863318411405,3.43012011423786,-2.71023723151952));
#90236=CARTESIAN_POINT('Ctrl Pts',(8.06748040285371,4.13457678604175,1.41999459489774));
#90237=CARTESIAN_POINT('Ctrl Pts',(8.26632762159334,1.04109589173419,4.24584846566965));
#90238=CARTESIAN_POINT('Ctrl Pts',(8.46517484033299,-3.00871436873501,3.17155288409039));
#90239=CARTESIAN_POINT('Ctrl Pts',(8.66402205907265,-4.29478122376174,-0.816066228463263));
#90240=CARTESIAN_POINT('Ctrl Pts',(8.86286927781226,-1.63574999691905,-4.05406361528703));
#90241=CARTESIAN_POINT('Ctrl Pts',(9.06171649655193,2.52584767953922,-3.56808118587302));
#90242=CARTESIAN_POINT('Ctrl Pts',(9.26056371529156,4.36725340290968,0.195467552265011));
#90243=CARTESIAN_POINT('Ctrl Pts',(9.45941093403121,2.1969895847602,3.7794637997565));
#90244=CARTESIAN_POINT('Ctrl Pts',(9.65825815277085,-1.99138387510301,3.8917219981898));
#90245=CARTESIAN_POINT('Ctrl Pts',(9.85710537151049,-4.35051288766617,0.429124065353151));
#90246=CARTESIAN_POINT('Ctrl Pts',(10.0559525902501,-2.713349853193,-3.42765844613962));
#90247=CARTESIAN_POINT('Ctrl Pts',(10.2547998089898,1.4162407913405,-4.13586410199344));
#90248=CARTESIAN_POINT('Ctrl Pts',(10.4536470277294,4.24490164730402,-1.04494968966466));
#90249=CARTESIAN_POINT('Ctrl Pts',(10.6524942464691,3.17428277887788,3.00583410868497));
#90250=CARTESIAN_POINT('Ctrl Pts',(10.8513414652087,-0.812167245970631,
4.295520249491));
#90251=CARTESIAN_POINT('Ctrl Pts',(11.0501886839484,-4.05257707056199,1.63942945452676));
#90252=CARTESIAN_POINT('Ctrl Pts',(11.249035902688,-3.57037258845796,-2.52260766446206));
#90253=CARTESIAN_POINT('Ctrl Pts',(11.4478831214276,0.191503037860384,-4.36742904186261));
#90254=CARTESIAN_POINT('Ctrl Pts',(11.6467303401673,3.77746789527733,-2.20041953939783));
#90255=CARTESIAN_POINT('Ctrl Pts',(11.8455775589069,3.89352810061769,1.98785029087078));
#90256=CARTESIAN_POINT('Ctrl Pts',(12.0444247776466,0.433073125983973,4.3501215519529));
#90257=CARTESIAN_POINT('Ctrl Pts',(12.2432719963862,-3.42519395353086,2.71646023897098));
#90258=CARTESIAN_POINT('Ctrl Pts',(12.4421192151259,-4.13714800984828,-1.41248582075117));
#90259=CARTESIAN_POINT('Ctrl Pts',(12.6409664338655,-1.04880262652003,-4.2439513309909));
#90260=CARTESIAN_POINT('Ctrl Pts',(12.8398136526051,3.00295137172242,-3.17701005794523));
#90261=CARTESIAN_POINT('Ctrl Pts',(13.0386608713448,4.29625573556119,0.808267594223766));
#90262=CARTESIAN_POINT('Ctrl Pts',(13.2375080900844,1.64310756118719,4.05108718637159));
#90263=CARTESIAN_POINT('Ctrl Pts',(13.4363553088241,-2.51936557066787,3.57266104893089));
#90264=CARTESIAN_POINT('Ctrl Pts',(13.6352025275637,-4.36760108190112,-0.187538365650509));
#90265=CARTESIAN_POINT('Ctrl Pts',(13.8340497463034,-2.20384768081277,-3.77546887803236));
#90266=CARTESIAN_POINT('Ctrl Pts',(14.032896965043,1.98431506858032,-3.89533099464214));
#90267=CARTESIAN_POINT('Ctrl Pts',(14.2317441837827,4.34972663158719,-0.437021829747384));
#90268=CARTESIAN_POINT('Ctrl Pts',(14.4305914025223,2.71956838629063,3.42272663844241));
#90269=CARTESIAN_POINT('Ctrl Pts',(14.6294386212619,-1.40872968622409,4.13842850854834));
#90270=CARTESIAN_POINT('Ctrl Pts',(14.8282858400016,-4.24299751751331,1.05265469912532));
#90271=CARTESIAN_POINT('Ctrl Pts',(15.0271330587412,-3.17973471904507,-3.00006616022283));
#90272=CARTESIAN_POINT('Ctrl Pts',(15.2259802774809,0.804367276436096,-4.29698768136627));
#90273=CARTESIAN_POINT('Ctrl Pts',(15.4248274962205,4.04959396394355,-1.6467843138695));
#90274=CARTESIAN_POINT('Ctrl Pts',(15.6236747149602,3.57494656540606,2.51612140082828));
#90275=CARTESIAN_POINT('Ctrl Pts',(15.8225219336998,-0.183573538902467,
4.36776952288344));
#90276=CARTESIAN_POINT('Ctrl Pts',(16.0213691524394,-3.77346674966885,2.20727400618009));
#90277=CARTESIAN_POINT('Ctrl Pts',(16.2202163711791,-3.89713067877753,-1.98077821114473));
#90278=CARTESIAN_POINT('Ctrl Pts',(16.4190635899187,-0.440970173389522,
-4.34932812689449));
#90279=CARTESIAN_POINT('Ctrl Pts',(16.6179108086584,3.42025650290739,-2.72267429259073));
#90280=CARTESIAN_POINT('Ctrl Pts',(16.816758027398,4.13970559703845,1.40497239085444));
#90281=CARTESIAN_POINT('Ctrl Pts',(17.0156052461377,1.05650590430629,4.24204020765723));
#90282=CARTESIAN_POINT('Ctrl Pts',(17.2144524648773,-2.99717847656365,3.18245675993221));
#90283=CARTESIAN_POINT('Ctrl Pts',(17.4132996836169,-4.2977160863031,-0.800466295821592));
#90284=CARTESIAN_POINT('Ctrl Pts',(17.6121469023566,-1.65045970954389,-4.04809740450832));
#90285=CARTESIAN_POINT('Ctrl Pts',(17.8109941210962,2.51287515761657,-3.57722913600011));
#90286=CARTESIAN_POINT('Ctrl Pts',(18.0098413398359,4.3679343646708,0.179608560883422));
#90287=CARTESIAN_POINT('Ctrl Pts',(18.2086885585755,2.21069851267633,3.77146151183666));
#90288=CARTESIAN_POINT('Ctrl Pts',(18.4075357773152,-1.97723972147858,3.89892715154078));
#90289=CARTESIAN_POINT('Ctrl Pts',(18.6063829960548,-4.34892603820315,0.444918153656803));
#90290=CARTESIAN_POINT('Ctrl Pts',(18.8052302147944,-2.72577795531192,-3.41778354896127));
#90291=CARTESIAN_POINT('Ctrl Pts',(19.0040774335341,1.40121393773835,-4.14097927426623));
#90292=CARTESIAN_POINT('Ctrl Pts',(19.2029246522737,4.24107940221153,-1.0603562388894));
#90293=CARTESIAN_POINT('Ctrl Pts',(19.4017718710134,3.18517617836356,2.99428832312454));
#90294=CARTESIAN_POINT('Ctrl Pts',(19.600619089753,-0.796564655594856,4.2984409497714));
#90295=CARTESIAN_POINT('Ctrl Pts',(19.7994663084927,-4.04659750929911,1.65413374518173));
#90296=CARTESIAN_POINT('Ctrl Pts',(19.9983135272323,-3.57950875883217,-2.50962684370774));
#90297=CARTESIAN_POINT('Ctrl Pts',(20.197160745972,0.175643434860611,-4.36809560712733));
#90298=CARTESIAN_POINT('Ctrl Pts',(20.3960079647116,3.76945316618819,-2.2141211974796));
#90299=CARTESIAN_POINT('Ctrl Pts',(20.5948551834513,3.90072041145158,1.97369960249772));
#90300=CARTESIAN_POINT('Ctrl Pts',(20.7937024021909,0.448865767295954,4.34852036584451));
#90301=CARTESIAN_POINT('Ctrl Pts',(20.9925496209305,-3.41530777864185,2.72887937189667));
#90302=CARTESIAN_POINT('Ctrl Pts',(21.1913968396701,-4.14224953918214,-1.39745432997289));
#90303=CARTESIAN_POINT('Ctrl Pts',(21.3902440584098,-1.06420569970189,-4.24011510196797));
#90304=CARTESIAN_POINT('Ctrl Pts',(21.5890912771495,2.99139570228704,-3.18789297209824));
#90305=CARTESIAN_POINT('Ctrl Pts',(21.7879384958891,4.2991622711739,0.792662358970985));
#90306=CARTESIAN_POINT('Ctrl Pts',(21.9867857146287,1.65780641775542,4.04509427955192));
#90307=CARTESIAN_POINT('Ctrl Pts',(22.1856329333684,-2.50637646177856,3.58178543202368));
#90308=CARTESIAN_POINT('Ctrl Pts',(22.384480152108,-4.36825325012018,-0.171678164101458));
#90309=CARTESIAN_POINT('Ctrl Pts',(22.5833273708477,-2.21754205776954,-3.76744171437834));
#90310=CARTESIAN_POINT('Ctrl Pts',(22.7821745895873,1.97015785711929,-3.90251045703222));
#90311=CARTESIAN_POINT('Ctrl Pts',(22.981021808327,4.34811111015288,-0.452813011053976));
#90312=CARTESIAN_POINT('Ctrl Pts',(23.1798690270666,2.73197853978927,3.41282919398928));
#90313=CARTESIAN_POINT('Ctrl Pts',(23.3787162458063,-1.39369357065614,4.14351639073943));
#90314=CARTESIAN_POINT('Ctrl Pts',(23.5775634645459,-4.23914730772107,1.06805428357167));
#90315=CARTESIAN_POINT('Ctrl Pts',(23.7764106832856,-3.19060713889759,-2.9885006164347));
#90316=CARTESIAN_POINT('Ctrl Pts',(23.9752579020252,0.788759409165555,-4.29988004991624));
#90317=CARTESIAN_POINT('Ctrl Pts',(24.1741051207649,4.04358771650543,-1.66147772423859));
#90318=CARTESIAN_POINT('Ctrl Pts',(24.3729523395044,3.58405915369861,2.50312401450745));
#90319=CARTESIAN_POINT('Ctrl Pts',(24.5717995582441,-0.167712751873498,
4.36840729351942));
#90320=CARTESIAN_POINT('Ctrl Pts',(24.7706467769837,-3.7654271580646,2.2209610907272));
#90321=CARTESIAN_POINT('Ctrl Pts',(24.9694939957234,-3.90429728680765,-1.96661448826176));
#90322=CARTESIAN_POINT('Ctrl Pts',(25.1683412144631,-0.456759881678285,
-4.34769827146548));
#90323=CARTESIAN_POINT('Ctrl Pts',(25.3671884332027,3.41034779704597,-2.73507545643596));
#90324=CARTESIAN_POINT('Ctrl Pts',(25.5660356519423,4.14477982789419,1.3899316628871));
#90325=CARTESIAN_POINT('Ctrl Pts',(25.764882870682,1.07190198732727,4.23817602026845));
#90326=CARTESIAN_POINT('Ctrl Pts',(25.9637300894216,-2.98560306795325,3.19331867652491));
#90327=CARTESIAN_POINT('Ctrl Pts',(26.1625773081612,-4.30059428540685,-0.784855809394697));
#90328=CARTESIAN_POINT('Ctrl Pts',(26.3614245269009,-1.66514766160607,-4.04207782140107));
#90329=CARTESIAN_POINT('Ctrl Pts',(26.5602717456405,2.49986950457442,-3.5863299219834));
#90330=CARTESIAN_POINT('Ctrl Pts',(26.7591189643802,4.36855773719815,0.163747201444247));
#90331=CARTESIAN_POINT('Ctrl Pts',(26.9579661831198,2.22437829353522,3.7634094989071));
#90332=CARTESIAN_POINT('Ctrl Pts',(27.1568134018595,-1.96306949884509,3.90608089930546));
#90333=CARTESIAN_POINT('Ctrl Pts',(27.3556606205991,-4.34728185012251,0.460706375916406));
#90334=CARTESIAN_POINT('Ctrl Pts',(27.5545078393388,-2.73817011928469,-3.40786358985672));
#90335=CARTESIAN_POINT('Ctrl Pts',(27.7533550580784,1.38616860976576,-4.14603984960525));
#90336=CARTESIAN_POINT('Ctrl Pts',(27.952202276818,4.23720124041042,-1.0757488077981));
#90337=CARTESIAN_POINT('Ctrl Pts',(28.1510494955577,3.19602758274585,2.9827030592304));
#90338=CARTESIAN_POINT('Ctrl Pts',(28.3498967142973,-0.780951562875272,
4.30130497705724));
#90339=CARTESIAN_POINT('Ctrl Pts',(28.548743933037,-4.04056459548315,1.66881622683348));
#90340=CARTESIAN_POINT('Ctrl Pts',(28.7475911517766,-3.58859773500673,-2.49661293466152));
#90341=CARTESIAN_POINT('Ctrl Pts',(28.9464383705163,0.159781516081698,-4.36870458103238));
#90342=CARTESIAN_POINT('Ctrl Pts',(29.1452855892559,3.76138873856841,-2.22779366337761));
#90343=CARTESIAN_POINT('Ctrl Pts',(29.3441328079956,3.90786129305586,1.95952289179036));
#90344=CARTESIAN_POINT('Ctrl Pts',(29.5429800267352,0.464652490516438,4.34686184646714));
#90345=CARTESIAN_POINT('Ctrl Pts',(29.7418272454748,-3.40537657446858,2.74126252578542));
#90346=CARTESIAN_POINT('Ctrl Pts',(29.9406744642145,-4.14729645483434,-1.38240441439296));
#90347=CARTESIAN_POINT('Ctrl Pts',(30.1395216829541,-1.07959474181426,-4.23622296895025));
#90348=CARTESIAN_POINT('Ctrl Pts',(30.3383689016938,2.97980059265583,-3.19873385532817));
#90349=CARTESIAN_POINT('Ctrl Pts',(30.5372161204335,4.30201212428175,0.777046672824416));
#90350=CARTESIAN_POINT('Ctrl Pts',(30.736063339173,1.67248341689788,4.03904803999856));
#90351=CARTESIAN_POINT('Ctrl Pts',(30.9349105579127,-2.49335430745217,3.59086259089991));
#90352=CARTESIAN_POINT('Ctrl Pts',(31.1337577766523,-4.3688478249011,-0.155815699053587));
#90353=CARTESIAN_POINT('Ctrl Pts',(31.332604995392,-2.23120719744001,-3.75936487871377));
#90354=CARTESIAN_POINT('Ctrl Pts',(31.5314522141316,1.95597467002026,-3.90963846659173));
#90355=CARTESIAN_POINT('Ctrl Pts',(31.7302994328713,4.34643826084541,-0.468598222226493));
#90356=CARTESIAN_POINT('Ctrl Pts',(31.9291466516109,2.7443526733899,3.40288675293087));
#90357=CARTESIAN_POINT('Ctrl Pts',(32.1279938703505,-1.37863907987046,4.14854964254603));
#90358=CARTESIAN_POINT('Ctrl Pts',(32.3268410890903,-4.23524120669408,1.08343978620659));
#90359=CARTESIAN_POINT('Ctrl Pts',(32.5256883078298,-3.20143749204183,-2.97689567062125));
#90360=CARTESIAN_POINT('Ctrl Pts',(32.7245355265695,0.773141142459902,-4.30271572649768));
#90361=CARTESIAN_POINT('Ctrl Pts',(32.9233827453091,4.03752815619699,-1.67614922877742));
#90362=CARTESIAN_POINT('Ctrl Pts',(33.1222299640488,3.5931244877966,2.49009362563158));
#90363=CARTESIAN_POINT('Ctrl Pts',(33.3210771827884,-0.151849753627885,
4.36898746868628));
#90364=CARTESIAN_POINT('Ctrl Pts',(33.5199244015281,-3.75733792101087,2.23461889290957));
#90365=CARTESIAN_POINT('Ctrl Pts',(33.7187716202677,-3.91141241844866,-1.95242483645857));
#90366=CARTESIAN_POINT('Ctrl Pts',(33.9176188390074,-0.472543567795172,
-4.34601109360641));
#90367=CARTESIAN_POINT('Ctrl Pts',(34.116466057747,3.40039412729541,-2.74744055955165));
#90368=CARTESIAN_POINT('Ctrl Pts',(34.3153132764867,4.14979941170753,1.37487260930113));
#90369=CARTESIAN_POINT('Ctrl Pts',(34.5141604952263,1.08728393780662,4.23425595445086));
#90370=CARTESIAN_POINT('Ctrl Pts',(34.713007713966,-2.97398829552043,3.20413849065896));
#90371=CARTESIAN_POINT('Ctrl Pts',(34.9118549327056,-4.30341578312523,-0.769234975000029));
#90372=CARTESIAN_POINT('Ctrl Pts',(35.1107021514452,-1.67981365945132,-4.03600494533089));
#90373=CARTESIAN_POINT('Ctrl Pts',(35.3095493701849,2.48683089188669,-3.59538342383295));
#90374=CARTESIAN_POINT('Ctrl Pts',(35.5083965889245,4.36912351227285,0.147883683072671));
#90375=CARTESIAN_POINT('Ctrl Pts',(35.7072438076642,2.23802874697494,3.75530786712999));
#90376=CARTESIAN_POINT('Ctrl Pts',(35.9060910264038,-1.94887339403047,3.91318314716482));
#90377=CARTESIAN_POINT('Ctrl Pts',(36.1049382451435,-4.34558034510215,0.476488523971419));
#90378=CARTESIAN_POINT('Ctrl Pts',(36.3037854638831,-2.7505261817262,-3.39789869961619));
#90379=CARTESIAN_POINT('Ctrl Pts',(36.5026326826227,1.37110500578868,-4.15104576128906));
#90380=CARTESIAN_POINT('Ctrl Pts',(36.7014799013624,4.2332672130325,-1.09112719344661));
#90381=CARTESIAN_POINT('Ctrl Pts',(36.900327120102,3.20683684895383,2.97107846974908));
#90382=CARTESIAN_POINT('Ctrl Pts',(37.0991743388417,-0.765328173663516,
4.30411229358757));
#90383=CARTESIAN_POINT('Ctrl Pts',(37.2980215575813,-4.03447840865544,1.6834767059));
#90384=CARTESIAN_POINT('Ctrl Pts',(37.496868776321,-3.59763939714749,-2.48356610890607));
#90385=CARTESIAN_POINT('Ctrl Pts',(37.6957159950606,0.143917490656121,-4.36925595554871));
#90386=CARTESIAN_POINT('Ctrl Pts',(37.8945632138002,3.75327471874399,-2.24143675682628));
#90387=CARTESIAN_POINT('Ctrl Pts',(38.0934104325399,3.91495065128109,1.94532034566247));
#90388=CARTESIAN_POINT('Ctrl Pts',(38.2922576512795,0.480433087504437,4.34514601568757));
#90389=CARTESIAN_POINT('Ctrl Pts',(38.4911048700192,-3.39540047194947,2.75360953737089));
#90390=CARTESIAN_POINT('Ctrl Pts',(38.6899520887588,-4.15228869026357,-1.36733627243771));
#90391=CARTESIAN_POINT('Ctrl Pts',(38.8887993074985,-1.09496954995957,-4.2322749832538));
#90392=CARTESIAN_POINT('Ctrl Pts',(39.0876465262381,2.96816619570515,-3.20953256470283));
#90393=CARTESIAN_POINT('Ctrl Pts',(39.2864937449777,4.30480525731066,0.76142074166985));
#90394=CARTESIAN_POINT('Ctrl Pts',(39.4853409637174,1.68713836510498,4.03294854742849));
#90395=CARTESIAN_POINT('Ctrl Pts',(39.684188182457,-2.48029927938,3.59989240588131));
#90396=CARTESIAN_POINT('Ctrl Pts',(39.8830354011967,-4.36938479840474,-0.139951179646495));
#90397=CARTESIAN_POINT('Ctrl Pts',(40.0818826199362,-2.24484291965528,-3.75123847752822));
#90398=CARTESIAN_POINT('Ctrl Pts',(40.280729838676,1.9417656942824,-3.916714929341));
#90399=CARTESIAN_POINT('Ctrl Pts',(40.4795770574156,4.34470810572058,-0.484377255143766));
#90400=CARTESIAN_POINT('Ctrl Pts',(40.6784242761552,2.75669062394493,3.39289944635391));
#90401=CARTESIAN_POINT('Ctrl Pts',(40.8772714948949,-1.36356641235379,4.15352819760686));
#90402=CARTESIAN_POINT('Ctrl Pts',(41.0761187136345,-4.23127926593237,1.09881100417926));
#90403=CARTESIAN_POINT('Ctrl Pts',(41.2749659323742,-3.21222563568464,-2.96525147578833));
#90404=CARTESIAN_POINT('Ctrl Pts',(41.4738131511138,0.757512682238883,-4.30549467372362));
#90405=CARTESIAN_POINT('Ctrl Pts',(41.6726603698535,4.0314153629108,-1.69079863404868));
#90406=CARTESIAN_POINT('Ctrl Pts',(41.8715075885931,3.60214244817772,2.47703040600029));
#90407=CARTESIAN_POINT('Ctrl Pts',(42.0703548073327,-0.135984753312187,
4.36951004073511));
#90408=CARTESIAN_POINT('Ctrl Pts',(42.2692020260724,-3.74919914516051,2.24824723265442));
#90409=CARTESIAN_POINT('Ctrl Pts',(42.4680492448121,-3.91847597989089,-1.93820944281791));
#90410=CARTESIAN_POINT('Ctrl Pts',(42.6668964635516,-0.488321023638938,
-4.3442666155649));
#90411=CARTESIAN_POINT('Ctrl Pts',(42.8657436822913,3.39039562488978,-2.75976943890386));
#90412=CARTESIAN_POINT('Ctrl Pts',(43.064590901031,4.15476428229879,1.3597954286328));
#90413=CARTESIAN_POINT('Ctrl Pts',(43.2634381197705,1.10265155293779,4.230280061909));
#90414=CARTESIAN_POINT('Ctrl Pts',(43.4622853385103,-2.96233431239582,3.21491605964126));
#90415=CARTESIAN_POINT('Ctrl Pts',(43.6611325572498,-4.30618054226719,-0.75360399851666));
#90416=CARTESIAN_POINT('Ctrl Pts',(43.8599797759895,-1.69445750969802,-4.02987885650785));
#90417=CARTESIAN_POINT('Ctrl Pts',(44.0588269947292,2.47375949142812,-3.60438952191081));
#90418=CARTESIAN_POINT('Ctrl Pts',(44.2576742134688,4.3696316824989,0.132018214401751));
#90419=CARTESIAN_POINT('Ctrl Pts',(44.4565214322085,2.25164969289924,3.74715672431622));
#90420=CARTESIAN_POINT('Ctrl Pts',(44.6553686509481,-1.93465159397174,3.92023379957652));
#90421=CARTESIAN_POINT('Ctrl Pts',(44.8542158696878,-4.34382154601996,0.492264393380623));
#90422=CARTESIAN_POINT('Ctrl Pts',(45.0530630884273,-2.76284597887739,-3.38788901658417));
#90423=CARTESIAN_POINT('Ctrl Pts',(45.2519103071671,1.35602332278828,-4.15599692999943));
#90424=CARTESIAN_POINT('Ctrl Pts',(45.4507575259067,4.22927737505606,-1.10649121855319));
#90425=CARTESIAN_POINT('Ctrl Pts',(45.6496047446464,3.21760382852318,2.95941475667813));
#90426=CARTESIAN_POINT('Ctrl Pts',(45.8484519633859,-0.74969468256698,4.30686276912748));
#90427=CARTESIAN_POINT('Ctrl Pts',(46.0472991821257,-4.02833905082843,1.69811516741566));
#90428=CARTESIAN_POINT('Ctrl Pts',(46.2461464008652,-3.60663358440201,-2.4704868795819));
#90429=CARTESIAN_POINT('Ctrl Pts',(46.4449936196049,0.128051488084874,-4.36974907086184));
#90430=CARTESIAN_POINT('Ctrl Pts',(46.6438408383445,3.74511136607549,-2.25505154621694));
#90431=CARTESIAN_POINT('Ctrl Pts',(46.8426880570842,3.92198810116398,1.93109453921225));
#90432=CARTESIAN_POINT('Ctrl Pts',(47.0415352758238,0.496207907805146,4.3433683283625));
#90433=CARTESIAN_POINT('Ctrl Pts',(47.2403824945635,-3.38538066927122,2.76592898165438));
#90434=CARTESIAN_POINT('Ctrl Pts',(47.4392297133031,-4.15722413921679,-1.352266817509));
#90435=CARTESIAN_POINT('Ctrl Pts',(47.6380769320427,-1.1103338246204,-4.22823922289527));
#90436=CARTESIAN_POINT('Ctrl Pts',(47.8369241507824,2.95650013133344,-3.22035012185404));
#90437=CARTESIAN_POINT('Ctrl Pts',(48.035771369522,4.30752735065132,0.745901774490634));
#90438=CARTESIAN_POINT('Ctrl Pts',(48.2346185882617,1.70179839037054,4.02657205694712));
#90439=CARTESIAN_POINT('Ctrl Pts',(48.4334658070014,-2.4672638070873,3.60930298583502));
#90440=CARTESIAN_POINT('Ctrl Pts',(48.6323130257409,-4.36976425292589,-0.124904582404934));
#90441=CARTESIAN_POINT('Ctrl Pts',(48.8311602444807,-2.25863968436503,-3.7414890978684));
#90442=CARTESIAN_POINT('Ctrl Pts',(49.0300074632203,1.92789149232914,-3.92679780134734));
#90443=CARTESIAN_POINT('Ctrl Pts',(49.2288546819599,4.34226871337571,-0.493871726977649));
#90444=CARTESIAN_POINT('Ctrl Pts',(49.361419494453,3.29413968985974,2.08020745264537));
#90445=CARTESIAN_POINT('Ctrl Pts',(49.4277019006995,2.34119304463769,2.86022674942168));
#90446=CARTESIAN_POINT('Ctrl Pts',(0.450659262638117,2.00550372675239,-2.81530976205099));
#90447=CARTESIAN_POINT('Ctrl Pts',(0.516986045427824,2.94415968026748,-2.14672709529502));
#90448=CARTESIAN_POINT('Ctrl Pts',(0.649595234464078,4.08288101377022,0.191057201775436));
#90449=CARTESIAN_POINT('Ctrl Pts',(0.848486829746883,2.04223188327633,3.54469997975543));
#90450=CARTESIAN_POINT('Ctrl Pts',(1.04733404848652,-1.87575556888288,3.63116967669737));
#90451=CARTESIAN_POINT('Ctrl Pts',(1.24618126722617,-4.06974481274113,0.387286238545933));
#90452=CARTESIAN_POINT('Ctrl Pts',(1.44502848596581,-2.525856229638,-3.21502373795952));
#90453=CARTESIAN_POINT('Ctrl Pts',(1.64387570470545,1.33849696381325,-3.86268422229914));
#90454=CARTESIAN_POINT('Ctrl Pts',(1.8427229234451,3.97319582031557,-0.962890749780876));
#90455=CARTESIAN_POINT('Ctrl Pts',(2.04157014218474,2.95827073078296,2.82177532815739));
#90456=CARTESIAN_POINT('Ctrl Pts',(2.24041736092439,-0.77409910348615,4.01421726992893));
#90457=CARTESIAN_POINT('Ctrl Pts',(2.43926457966403,-3.79537757649156,1.51938551604069));
#90458=CARTESIAN_POINT('Ctrl Pts',(2.63811179840367,-3.33031026970215,-2.3711770690211));
#90459=CARTESIAN_POINT('Ctrl Pts',(2.83695901714332,0.193917256034556,-4.08359651267085));
#90460=CARTESIAN_POINT('Ctrl Pts',(3.03580623588295,3.54001353616159,-2.04492269457519));
#90461=CARTESIAN_POINT('Ctrl Pts',(3.2346534546226,3.63432735277917,1.87218300704005));
#90462=CARTESIAN_POINT('Ctrl Pts',(3.43350067336224,0.390221716267934,4.06953567428003));
#90463=CARTESIAN_POINT('Ctrl Pts',(3.63234789210189,-3.21233319406464,2.52869833293435));
#90464=CARTESIAN_POINT('Ctrl Pts',(3.83119511084153,-3.86410482679418,-1.33495062377738));
#90465=CARTESIAN_POINT('Ctrl Pts',(4.03004232958118,-0.966388786040835,
-3.97234069465277));
#90466=CARTESIAN_POINT('Ctrl Pts',(4.22888954832082,2.8190321458056,-2.96082025409016));
#90467=CARTESIAN_POINT('Ctrl Pts',(4.42773676706046,4.01494790794569,0.770449197634163));
#90468=CARTESIAN_POINT('Ctrl Pts',(4.62658398580011,1.52281472582692,3.79399971105506));
#90469=CARTESIAN_POINT('Ctrl Pts',(4.82543120453975,-2.36814487037926,3.33245982832313));
#90470=CARTESIAN_POINT('Ctrl Pts',(5.02427842327939,-4.08377508879584,-0.19020943190021));
#90471=CARTESIAN_POINT('Ctrl Pts',(5.22312564201904,-2.04813313760203,-3.53815619131909));
#90472=CARTESIAN_POINT('Ctrl Pts',(5.42197286075868,1.86888197011213,-3.63602513538813));
#90473=CARTESIAN_POINT('Ctrl Pts',(5.62082007949833,4.06918037242217,-0.393915846854869));
#90474=CARTESIAN_POINT('Ctrl Pts',(5.81966729823796,2.53161301463566,3.21003647013777));
#90475=CARTESIAN_POINT('Ctrl Pts',(6.01851451697762,-1.33144221482525,3.86531502298008));
#90476=CARTESIAN_POINT('Ctrl Pts',(6.21736173571725,-3.97146189165121,0.969994350744806));
#90477=CARTESIAN_POINT('Ctrl Pts',(6.4162089544569,-2.96337800397363,-2.81634326790372));
#90478=CARTESIAN_POINT('Ctrl Pts',(6.61505617319654,0.766804232869096,-4.01564563500611));
#90479=CARTESIAN_POINT('Ctrl Pts',(6.81390339193619,3.79261580434003,-1.52625815575171));
#90480=CARTESIAN_POINT('Ctrl Pts',(7.01275061067582,3.33460816466789,2.36511881000589));
#90481=CARTESIAN_POINT('Ctrl Pts',(7.21159782941548,-0.186502247601397,
4.08394607077586));
#90482=CARTESIAN_POINT('Ctrl Pts',(7.41044504815511,-3.53629551449476,2.0513441036317));
#90483=CARTESIAN_POINT('Ctrl Pts',(7.60929226689476,-3.63772013947132,-1.86558054884406));
#90484=CARTESIAN_POINT('Ctrl Pts',(7.80813948563441,-0.39760953904375,-4.0688211132721));
#90485=CARTESIAN_POINT('Ctrl Pts',(8.00698670437404,3.20773704153966,-2.53452592602202));
#90486=CARTESIAN_POINT('Ctrl Pts',(8.20583392311369,3.86652206510947,1.32793287381758));
#90487=CARTESIAN_POINT('Ctrl Pts',(8.40468114185334,0.973599099882512,3.97057972971866));
#90488=CARTESIAN_POINT('Ctrl Pts',(8.60352836059298,-2.8136520607379,2.96593335704791));
#90489=CARTESIAN_POINT('Ctrl Pts',(8.80237557933261,-4.01634005747664,-0.763158659816362));
#90490=CARTESIAN_POINT('Ctrl Pts',(9.00122279807226,-1.52970032566391,-3.79122876004706));
#90491=CARTESIAN_POINT('Ctrl Pts',(9.20007001681191,2.36209079947775,-3.33675375962428));
#90492=CARTESIAN_POINT('Ctrl Pts',(9.39891723555156,4.08411368807603,0.182794912987637));
#90493=CARTESIAN_POINT('Ctrl Pts',(9.59776445429119,2.05455337895022,3.53443192187775));
#90494=CARTESIAN_POINT('Ctrl Pts',(9.79661167303084,-1.86227759009887,3.63941214686655));
#90495=CARTESIAN_POINT('Ctrl Pts',(9.99545889177048,-4.06845850136166,0.401302903107108));
#90496=CARTESIAN_POINT('Ctrl Pts',(10.1943061105101,-2.53743674882291,-3.20543496940232));
#90497=CARTESIAN_POINT('Ctrl Pts',(10.3931533292497,1.32442243852197,-3.86772592122086));
#90498=CARTESIAN_POINT('Ctrl Pts',(10.5920005479894,3.96969429590236,-0.977203046671689));
#90499=CARTESIAN_POINT('Ctrl Pts',(10.790847766729,2.96848626608251,2.81095853498833));
#90500=CARTESIAN_POINT('Ctrl Pts',(10.9896949854687,-0.759512457890662,
4.01703117036116));
#90501=CARTESIAN_POINT('Ctrl Pts',(11.1885422042083,-3.78983859165073,1.53314123503966));
#90502=CARTESIAN_POINT('Ctrl Pts',(11.387389422948,-3.33889660497779,-2.35906084249899));
#90503=CARTESIAN_POINT('Ctrl Pts',(11.5862366416876,0.179087427744,-4.08427793992626));
#90504=CARTESIAN_POINT('Ctrl Pts',(11.7850838604272,3.53256541676539,-2.05776096124341));
#90505=CARTESIAN_POINT('Ctrl Pts',(11.9839310791669,3.64110115525862,1.85897309677104));
#90506=CARTESIAN_POINT('Ctrl Pts',(12.1827782979065,0.404995936482876,4.06809253689939));
#90507=CARTESIAN_POINT('Ctrl Pts',(12.3816255166462,-3.2031302558744,2.54034548068687));
#90508=CARTESIAN_POINT('Ctrl Pts',(12.5804727353858,-3.86892659019068,-1.3209109118558));
#90509=CARTESIAN_POINT('Ctrl Pts',(12.7793199541254,-0.980806188211366,
-3.96880559091908));
#90510=CARTESIAN_POINT('Ctrl Pts',(12.9781671728651,2.80826269291056,-2.97103672898048));
#90511=CARTESIAN_POINT('Ctrl Pts',(13.1770143916047,4.01771897307136,0.755865630100106));
#90512=CARTESIAN_POINT('Ctrl Pts',(13.3758616103444,1.53658088105336,3.78844530029476));
#90513=CARTESIAN_POINT('Ctrl Pts',(13.574708829084,-2.35602894157149,3.34103669896361));
#90514=CARTESIAN_POINT('Ctrl Pts',(13.7735560478237,-4.08443882618849,-0.175379794926021));
#90515=CARTESIAN_POINT('Ctrl Pts',(13.9724032665633,-2.06096684786957,-3.53069600069545));
#90516=CARTESIAN_POINT('Ctrl Pts',(14.171250485303,1.8556670715843,-3.6427871632559));
#90517=CARTESIAN_POINT('Ctrl Pts',(14.3700977040426,4.06772322018647,-0.408688636127811));
#90518=CARTESIAN_POINT('Ctrl Pts',(14.5689449227822,2.54325211921723,3.20082290285502));
#90519=CARTESIAN_POINT('Ctrl Pts',(14.7677921415219,-1.31739829671282,3.87012407102955));
#90520=CARTESIAN_POINT('Ctrl Pts',(14.9666393602615,-3.96791361550106,0.984408521532401));
#90521=CARTESIAN_POINT('Ctrl Pts',(15.1654865790012,-2.97358474364017,-2.80556453672602));
#90522=CARTESIAN_POINT('Ctrl Pts',(15.3643337977408,0.752218179449807,-4.0184034650405));
#90523=CARTESIAN_POINT('Ctrl Pts',(15.5631810164805,3.78704888712724,-1.54001926087062));
#90524=CARTESIAN_POINT('Ctrl Pts',(15.7620282352201,3.34317403981824,2.35299509919369));
#90525=CARTESIAN_POINT('Ctrl Pts',(15.9608754539597,-0.17167201758895,4.08459634673013));
#90526=CARTESIAN_POINT('Ctrl Pts',(16.1597226726994,-3.52882367520839,2.06417103618691));
#90527=CARTESIAN_POINT('Ctrl Pts',(16.358569891439,-3.64447016946904,-1.85235951726291));
#90528=CARTESIAN_POINT('Ctrl Pts',(16.5574171101787,-0.412380998999033,
-4.06735055152723));
#90529=CARTESIAN_POINT('Ctrl Pts',(16.7562643289183,3.19851291224554,-2.54615666201882));
#90530=CARTESIAN_POINT('Ctrl Pts',(16.955111547658,3.87131836275072,1.31388459598752));
#90531=CARTESIAN_POINT('Ctrl Pts',(17.1539587663976,0.988010043666368,3.96701837038329));
#90532=CARTESIAN_POINT('Ctrl Pts',(17.3528059851373,-2.80286406865807,2.97613030796197));
#90533=CARTESIAN_POINT('Ctrl Pts',(17.5516532038769,-4.01908464570452,-0.748570108945357));
#90534=CARTESIAN_POINT('Ctrl Pts',(17.7505004226165,-1.54345637165813,-3.78564935329887));
#90535=CARTESIAN_POINT('Ctrl Pts',(17.9493476413562,2.34995931786557,-3.34530862578044));
#90536=CARTESIAN_POINT('Ctrl Pts',(18.1481948600958,4.08475050142141,0.167964098788153));
#90537=CARTESIAN_POINT('Ctrl Pts',(18.3470420788355,2.06737352355503,3.52694844184712));
#90538=CARTESIAN_POINT('Ctrl Pts',(18.5458892975751,-1.84905043653246,3.64615017251118));
#90539=CARTESIAN_POINT('Ctrl Pts',(18.7447365163148,-4.06697453122874,0.41607302205387));
#90540=CARTESIAN_POINT('Ctrl Pts',(18.9435837350544,-2.54905910669821,-3.19620028594943));
#90541=CARTESIAN_POINT('Ctrl Pts',(19.1424309537941,1.31036981257533,-3.87250946437004));
#90542=CARTESIAN_POINT('Ctrl Pts',(19.3412781725337,3.96611985630356,-0.991610751645455));
#90543=CARTESIAN_POINT('Ctrl Pts',(19.5401253912733,2.97867341984819,2.80016129093203));
#90544=CARTESIAN_POINT('Ctrl Pts',(19.738972610013,-0.744921421592954,4.01976251450208));
#90545=CARTESIAN_POINT('Ctrl Pts',(19.9378198287526,-3.7842466999629,1.54689221058356));
#90546=CARTESIAN_POINT('Ctrl Pts',(20.1366670474923,-3.34744045509124,-2.34692160008868));
#90547=CARTESIAN_POINT('Ctrl Pts',(20.3355142662319,0.164256041579034,-4.0849012901353));
#90548=CARTESIAN_POINT('Ctrl Pts',(20.5343614849715,3.52507030215688,-2.07057430733499));
#90549=CARTESIAN_POINT('Ctrl Pts',(20.7332087037112,3.64782717099794,1.84573983211972));
#90550=CARTESIAN_POINT('Ctrl Pts',(20.9320559224508,0.41976470224997,4.06659515960087));
#90551=CARTESIAN_POINT('Ctrl Pts',(21.1309031411905,-3.19388502587238,2.55195945086366));
#90552=CARTESIAN_POINT('Ctrl Pts',(21.3297503599301,-3.87369737490602,-1.3068539493725));
#90553=CARTESIAN_POINT('Ctrl Pts',(21.5285975786698,-0.995210642502595,
-3.96521807400221));
#90554=CARTESIAN_POINT('Ctrl Pts',(21.7274447974094,2.79745620577507,-2.98121407720324));
#90555=CARTESIAN_POINT('Ctrl Pts',(21.926292016149,4.02043707087463,0.741272120399241));
#90556=CARTESIAN_POINT('Ctrl Pts',(22.1251392348887,1.55032677481563,3.78284092827519));
#90557=CARTESIAN_POINT('Ctrl Pts',(22.3239864536283,-2.34388194836624,3.34956952599391));
#90558=CARTESIAN_POINT('Ctrl Pts',(22.522833672368,-4.08504871274753,-0.160547849017186));
#90559=CARTESIAN_POINT('Ctrl Pts',(22.7216808911076,-2.07377338488927,-3.52318925768531));
#90560=CARTESIAN_POINT('Ctrl Pts',(22.9205281098473,1.84242770675276,-3.64950116354742));
#90561=CARTESIAN_POINT('Ctrl Pts',(23.1193753285869,4.06621243695624,-0.423456036545246));
#90562=CARTESIAN_POINT('Ctrl Pts',(23.3182225473265,2.55485769212517,3.1915671339223));
#90563=CARTESIAN_POINT('Ctrl Pts',(23.5170697660662,-1.30333700927628,3.87488209337974));
#90564=CARTESIAN_POINT('Ctrl Pts',(23.7159169848058,-3.96431302422234,0.998809713271379));
#90565=CARTESIAN_POINT('Ctrl Pts',(23.9147642035455,-2.9837522779336,-2.79474881541622));
#90566=CARTESIAN_POINT('Ctrl Pts',(24.1136114222851,0.737622208371319,-4.02110831426633));
#90567=CARTESIAN_POINT('Ctrl Pts',(24.3124586410248,3.78143203939415,-1.55376006152417));
#90568=CARTESIAN_POINT('Ctrl Pts',(24.5113058597644,3.35169583673403,2.34084036520304));
#90569=CARTESIAN_POINT('Ctrl Pts',(24.7101530785041,-0.156839524158292,
4.08519276913661));
#90570=CARTESIAN_POINT('Ctrl Pts',(24.9090002972437,-3.52130530998243,2.0769707535817));
#90571=CARTESIAN_POINT('Ctrl Pts',(25.1078475159834,-3.65117214878021,-1.83911406316082));
#90572=CARTESIAN_POINT('Ctrl Pts',(25.306694734723,-0.427147021897979,-4.06582636361022));
#90573=CARTESIAN_POINT('Ctrl Pts',(25.5055419534626,3.18924661200914,-2.55775382809456));
#90574=CARTESIAN_POINT('Ctrl Pts',(25.7043891722023,3.876063618815,1.29981899518472));
#90575=CARTESIAN_POINT('Ctrl Pts',(25.9032363909419,1.00240796098595,3.9634047077098));
#90576=CARTESIAN_POINT('Ctrl Pts',(26.1020836096816,-2.79203912208653,2.98628801994758));
#90577=CARTESIAN_POINT('Ctrl Pts',(26.3009308284212,-4.02177624412397,-0.733971688516825));
#90578=CARTESIAN_POINT('Ctrl Pts',(26.4997780471609,-1.55719206788015,-3.78002003448069));
#90579=CARTESIAN_POINT('Ctrl Pts',(26.6986252659005,2.33779685310535,-3.35381938555953));
#90580=CARTESIAN_POINT('Ctrl Pts',(26.8974724846401,4.08533345918385,0.153131070058041));
#90581=CARTESIAN_POINT('Ctrl Pts',(27.0963197033798,2.08016641077757,3.51941846060072));
#90582=CARTESIAN_POINT('Ctrl Pts',(27.2951669221194,-1.83579890407455,3.65284012531935));
#90583=CARTESIAN_POINT('Ctrl Pts',(27.4940141408591,-4.06543693988095,0.43083765526656));
#90584=CARTESIAN_POINT('Ctrl Pts',(27.6928613595987,-2.56064785638522,-3.18692346204518));
#90585=CARTESIAN_POINT('Ctrl Pts',(27.8917085783384,1.29629990999686,-3.87724195023812));
#90586=CARTESIAN_POINT('Ctrl Pts',(28.090555797078,3.96249312521304,-1.00600538268124));
#90587=CARTESIAN_POINT('Ctrl Pts',(28.2894030158177,2.98882130115569,2.7893271280189));
#90588=CARTESIAN_POINT('Ctrl Pts',(28.4882502345573,-0.730320563844051,
4.02244085989722));
#90589=CARTESIAN_POINT('Ctrl Pts',(28.687097453297,-3.77860491469843,1.56062279105523));
#90590=CARTESIAN_POINT('Ctrl Pts',(28.8859446720366,-3.35594017072038,-2.33475141458132));
#90591=CARTESIAN_POINT('Ctrl Pts',(29.0847918907762,0.149422489772549,-4.08547078277331));
#90592=CARTESIAN_POINT('Ctrl Pts',(29.2836391095159,3.51752871109499,-2.08336035384344));
#90593=CARTESIAN_POINT('Ctrl Pts',(29.4824863282555,3.65450509179034,1.83248223222565));
#90594=CARTESIAN_POINT('Ctrl Pts',(29.6813335469952,0.434527933609912,4.06504416608935));
#90595=CARTESIAN_POINT('Ctrl Pts',(29.8801807657348,-3.18459768594471,2.56353977461243));
#90596=CARTESIAN_POINT('Ctrl Pts',(30.0790279844744,-3.87841708667816,-1.29277975661249));
#90597=CARTESIAN_POINT('Ctrl Pts',(30.2778752032141,-1.00960197539289,-3.96157827748322));
#90598=CARTESIAN_POINT('Ctrl Pts',(30.4767224219538,2.78661283544809,-2.99135211947042));
#90599=CARTESIAN_POINT('Ctrl Pts',(30.6755696406933,4.02310216103839,0.726668837361569));
#90600=CARTESIAN_POINT('Ctrl Pts',(30.874416859433,1.56405222822251,3.77718668121347));
#90601=CARTESIAN_POINT('Ctrl Pts',(31.0732640781726,-2.33170405214038,3.35805819046906));
#90602=CARTESIAN_POINT('Ctrl Pts',(31.2721112969123,-4.08560473979183,-0.145713786357691));
#90603=CARTESIAN_POINT('Ctrl Pts',(31.4709585156519,-2.08655258014743,-3.5156360630225));
#90604=CARTESIAN_POINT('Ctrl Pts',(31.6698057343916,1.82916405034733,-3.65616704682118));
#90605=CARTESIAN_POINT('Ctrl Pts',(31.8686529531312,4.06464804255902,-0.438217853886986));
#90606=CARTESIAN_POINT('Ctrl Pts',(32.0675001718708,2.56642958039315,3.18226928562421));
#90607=CARTESIAN_POINT('Ctrl Pts',(32.2663473906105,-1.28925853793227,3.87958902716681));
#90608=CARTESIAN_POINT('Ctrl Pts',(32.4651946093501,-3.96066016527426,1.01319773615719));
#90609=CARTESIAN_POINT('Ctrl Pts',(32.6640418280898,-2.99388047280628,-2.78389624661074));
#90610=CARTESIAN_POINT('Ctrl Pts',(32.8628890468295,0.723016512078525,-4.02376014700256));
#90611=CARTESIAN_POINT('Ctrl Pts',(33.0617362655691,3.77576533519445,-1.56748037655599));
#90612=CARTESIAN_POINT('Ctrl Pts',(33.2605834843088,3.36017344306022,2.32865476829369));
#90613=CARTESIAN_POINT('Ctrl Pts',(33.4594307030483,-0.142004962869573,
4.08573533012904));
#90614=CARTESIAN_POINT('Ctrl Pts',(33.6582779217881,-3.51374051794282,2.08974308705905));
#90615=CARTESIAN_POINT('Ctrl Pts',(33.8571251405276,-3.65782598904241,-1.82584436117379));
#90616=CARTESIAN_POINT('Ctrl Pts',(34.0559723592673,-0.441907413057174,
-4.06424856961644));
#90617=CARTESIAN_POINT('Ctrl Pts',(34.2548195780069,3.17993826300249,-2.56931727134601));
#90618=CARTESIAN_POINT('Ctrl Pts',(34.4536667967466,3.88075777073823,1.28573625685793));
#90619=CARTESIAN_POINT('Ctrl Pts',(34.6525140154862,1.01679266201111,3.95973878934264));
#90620=CARTESIAN_POINT('Ctrl Pts',(34.8513612342259,-2.78117736374543,2.99640635907988));
#90621=CARTESIAN_POINT('Ctrl Pts',(35.0502084529655,-4.02441481724749,-0.719363591004572));
#90622=CARTESIAN_POINT('Ctrl Pts',(35.2490556717052,-1.57090723323079,-3.77434087781263));
#90623=CARTESIAN_POINT('Ctrl Pts',(35.4479028904449,2.32560356555396,-3.36228592675086));
#90624=CARTESIAN_POINT('Ctrl Pts',(35.6467501091844,4.08586255367729,0.138296022364396));
#90625=CARTESIAN_POINT('Ctrl Pts',(35.8455973279241,2.09293187194922,3.51184207741796));
#90626=CARTESIAN_POINT('Ctrl Pts',(36.0444445466637,-1.8225231674406,3.65948191708696));
#90627=CARTESIAN_POINT('Ctrl Pts',(36.2432917654034,-4.06384574759078,0.44559660808019));
#90628=CARTESIAN_POINT('Ctrl Pts',(36.442138984143,-2.57220284509149,-3.17760462000032));
#90629=CARTESIAN_POINT('Ctrl Pts',(36.6409862028826,1.28221291629195,-3.88192331642941));
#90630=CARTESIAN_POINT('Ctrl Pts',(36.8398334216223,3.95881415044763,-1.02038674999226));
#90631=CARTESIAN_POINT('Ctrl Pts',(37.038680640362,2.99892977620976,2.77845618909255));
#90632=CARTESIAN_POINT('Ctrl Pts',(37.2375278591016,-0.715710077149751,
4.02506617123379));
#90633=CARTESIAN_POINT('Ctrl Pts',(37.4363750778413,-3.77291331024181,1.57433279542307));
#90634=CARTESIAN_POINT('Ctrl Pts',(37.6352222965809,-3.36439563980019,-2.32255044643547));
#90635=CARTESIAN_POINT('Ctrl Pts',(37.8340695153205,0.134586967898456,-4.0859864103318));
#90636=CARTESIAN_POINT('Ctrl Pts',(38.0329167340602,3.5099407430123,-2.09611893219026));
#90637=CARTESIAN_POINT('Ctrl Pts',(38.2317639527998,3.66113482959032,1.81920047188451));
#90638=CARTESIAN_POINT('Ctrl Pts',(38.4306111715395,0.449285435915998,4.06343957681395));
#90639=CARTESIAN_POINT('Ctrl Pts',(38.6294583902791,-3.17526835854073,2.5750862992518));
#90640=CARTESIAN_POINT('Ctrl Pts',(38.8283056090187,-3.88308566327989,-1.27868851913763));
#90641=CARTESIAN_POINT('Ctrl Pts',(39.0271528277584,-1.02397999713899,-3.95788624935122));
#90642=CARTESIAN_POINT('Ctrl Pts',(39.226000046498,2.77573272489459,-3.00145072211647));
#90643=CARTESIAN_POINT('Ctrl Pts',(39.4248472652376,4.02571420842461,0.712055973524821));
#90644=CARTESIAN_POINT('Ctrl Pts',(39.6236944839773,1.57775706031004,3.77148263365828));
#90645=CARTESIAN_POINT('Ctrl Pts',(39.822541702717,-2.31949541345406,3.36650258046981));
#90646=CARTESIAN_POINT('Ctrl Pts',(40.0213889214566,-4.08610689999048,-0.13087780252811));
#90647=CARTESIAN_POINT('Ctrl Pts',(40.2202361401962,-2.09930426515592,-3.50803651629259));
#90648=CARTESIAN_POINT('Ctrl Pts',(40.4190833589359,1.81587627724355,-3.66278472519043));
#90649=CARTESIAN_POINT('Ctrl Pts',(40.6179305776756,4.06303005762069,-0.452973893524874));
#90650=CARTESIAN_POINT('Ctrl Pts',(40.8167777964151,2.57796763145084,3.17292948054884));
#90651=CARTESIAN_POINT('Ctrl Pts',(41.0156250151549,-1.2751630682992,3.88424481033186));
#90652=CARTESIAN_POINT('Ctrl Pts',(41.2144722338944,-3.95695508681798,1.02757240049034));
#90653=CARTESIAN_POINT('Ctrl Pts',(41.4133194526342,-3.00396919472272,-2.77300697339566));
#90654=CARTESIAN_POINT('Ctrl Pts',(41.6121666713737,0.708401283140883,-4.02635892828607));
#90655=CARTESIAN_POINT('Ctrl Pts',(41.8110138901134,3.77004884924109,-1.58118002506979));
#90656=CARTESIAN_POINT('Ctrl Pts',(42.009861108853,3.36860674702343,2.31643846912704));
#90657=CARTESIAN_POINT('Ctrl Pts',(42.2087083275927,-0.127168529309867,
4.08622402255439));
#90658=CARTESIAN_POINT('Ctrl Pts',(42.4075555463323,-3.50612939882789,2.10248786822073));
#90659=CARTESIAN_POINT('Ctrl Pts',(42.606402765072,-3.6644316025279,-1.81255058625554));
#90660=CARTESIAN_POINT('Ctrl Pts',(42.8052499838116,-0.456661977867081,
-4.06261719035113));
#90661=CARTESIAN_POINT('Ctrl Pts',(43.0040972025512,3.17058798795136,-2.58084683930912));
#90662=CARTESIAN_POINT('Ctrl Pts',(43.2029444212909,3.88540075663134,1.27163656667186));
#90663=CARTESIAN_POINT('Ctrl Pts',(43.4017916400305,1.03116395708377,3.95602066363422));
#90664=CARTESIAN_POINT('Ctrl Pts',(43.6006388587702,-2.77027893683754,3.00648519191689));
#90665=CARTESIAN_POINT('Ctrl Pts',(43.7994860775098,-4.0270003302952,-0.70474600894002));
#90666=CARTESIAN_POINT('Ctrl Pts',(43.9983332962495,-1.58460168686585,-3.76861195830456));
#90667=CARTESIAN_POINT('Ctrl Pts',(44.1971805149891,2.31337961594307,-3.37070813747293));
#90668=CARTESIAN_POINT('Ctrl Pts',(44.3960277337288,4.08633777798525,0.123459150814084));
#90669=CARTESIAN_POINT('Ctrl Pts',(44.5948749524684,2.10566973864982,3.50421939312008));
#90670=CARTESIAN_POINT('Ctrl Pts',(44.793722171208,-1.80922340144803,3.66607545846592));
#90671=CARTESIAN_POINT('Ctrl Pts',(44.9925693899477,-4.06220097575286,0.46034968930797));
#90672=CARTESIAN_POINT('Ctrl Pts',(45.1914166086873,-2.58372391967489,-3.16824388919018));
#90673=CARTESIAN_POINT('Ctrl Pts',(45.390263827427,1.26810901567099,-3.88655348876805));
#90674=CARTESIAN_POINT('Ctrl Pts',(45.5891110461666,3.95508298342125,-1.0347546877904));
#90675=CARTESIAN_POINT('Ctrl Pts',(45.7879582649063,3.00899870617135,2.76754866305454));
#90676=CARTESIAN_POINT('Ctrl Pts',(45.9868054836459,-0.701090143500552,
4.02763832672031));
#90677=CARTESIAN_POINT('Ctrl Pts',(46.1856527023856,-3.76717198199173,1.58802220969169));
#90678=CARTESIAN_POINT('Ctrl Pts',(46.3844999211252,-3.37280671190672,-2.31031917552347));
#90679=CARTESIAN_POINT('Ctrl Pts',(46.5833471398648,0.119749597061877,-4.08644755577365));
#90680=CARTESIAN_POINT('Ctrl Pts',(46.7821943586045,3.50230664045444,-2.10885104150034));
#90681=CARTESIAN_POINT('Ctrl Pts',(46.9810415773441,3.66771602439268,1.8058969592446));
#90682=CARTESIAN_POINT('Ctrl Pts',(47.1798887960838,0.464037536051553,4.06177714130411));
#90683=CARTESIAN_POINT('Ctrl Pts',(47.3787360148234,-3.16589816416573,2.58660704384476));
#90684=CARTESIAN_POINT('Ctrl Pts',(47.5775832335631,-3.88770113501167,-1.26459605381257));
#90685=CARTESIAN_POINT('Ctrl Pts',(47.7764304523026,-1.03834816831217,-3.95411213720304));
#90686=CARTESIAN_POINT('Ctrl Pts',(47.9752776710424,2.76482299999638,-3.01156695059165));
#90687=CARTESIAN_POINT('Ctrl Pts',(48.174124889782,4.02825982179923,0.697543138927408));
#90688=CARTESIAN_POINT('Ctrl Pts',(48.3729721085216,1.59146664029795,3.76551954664356));
#90689=CARTESIAN_POINT('Ctrl Pts',(48.5718193272613,-2.30730506269821,3.37530304951888));
#90690=CARTESIAN_POINT('Ctrl Pts',(48.7706665460009,-4.08646175354737,-0.116806712970479));
#90691=CARTESIAN_POINT('Ctrl Pts',(48.9695137647406,-2.11220655188028,-3.49891921275065));
#90692=CARTESIAN_POINT('Ctrl Pts',(49.1683609834802,1.80290157372149,-3.67221389995478));
#90693=CARTESIAN_POINT('Ctrl Pts',(49.3672082022199,4.06074881704516,-0.461852815538415));
#90694=CARTESIAN_POINT('Ctrl Pts',(49.4997730147129,3.08057256050849,1.94534251796016));
#90695=CARTESIAN_POINT('Ctrl Pts',(49.5660554209595,2.18940777598638,2.6747912567957));
#90696=CARTESIAN_POINT('Ctrl Pts',(0.589012782898099,1.86646799056595,-2.62013253044683));
#90697=CARTESIAN_POINT('Ctrl Pts',(0.655339565687807,2.74004965886194,-1.9979007540103));
#90698=CARTESIAN_POINT('Ctrl Pts',(0.787948754724062,3.79982675665839,0.1778117620645));
#90699=CARTESIAN_POINT('Ctrl Pts',(0.986840350006865,1.90064989089867,3.29895624731006));
#90700=CARTESIAN_POINT('Ctrl Pts',(1.18568756874651,-1.74571489483845,3.37943125184054));
#90701=CARTESIAN_POINT('Ctrl Pts',(1.38453478748615,-3.7876012502126,0.360436810857219));
#90702=CARTESIAN_POINT('Ctrl Pts',(1.58338200622579,-2.35074596895691,-2.99213549980709));
#90703=CARTESIAN_POINT('Ctrl Pts',(1.78222922496544,1.24570286512138,-3.59489556783852));
#90704=CARTESIAN_POINT('Ctrl Pts',(1.98107644370508,3.69774571841783,-0.896136336674187));
#90705=CARTESIAN_POINT('Ctrl Pts',(2.17992366244472,2.75318243131671,2.62614985767354));
#90706=CARTESIAN_POINT('Ctrl Pts',(2.37877088118437,-0.720433065722714,
3.73592327032595));
#90707=CARTESIAN_POINT('Ctrl Pts',(2.57761809992401,-3.53225509588298,1.41405094051461));
#90708=CARTESIAN_POINT('Ctrl Pts',(2.77646531866365,-3.09942955185539,-2.20679026433856));
#90709=CARTESIAN_POINT('Ctrl Pts',(2.9753125374033,0.180473537086268,-3.80049265210275));
#90710=CARTESIAN_POINT('Ctrl Pts',(3.17415975614294,3.29459470121029,-1.90315415608201));
#90711=CARTESIAN_POINT('Ctrl Pts',(3.37300697488258,3.38237001543028,1.74239000830994));
#90712=CARTESIAN_POINT('Ctrl Pts',(3.57185419362223,0.363168780452711,3.7874066107123));
#90713=CARTESIAN_POINT('Ctrl Pts',(3.77070141236187,-2.98963148348938,2.35339103750392));
#90714=CARTESIAN_POINT('Ctrl Pts',(3.96954863110152,-3.59621768595871,-1.24240238251827));
#90715=CARTESIAN_POINT('Ctrl Pts',(4.16839584984115,-0.899391864261573,
-3.69694987612832));
#90716=CARTESIAN_POINT('Ctrl Pts',(4.36724306858081,2.62359685216994,-2.75555520359363));
#90717=CARTESIAN_POINT('Ctrl Pts',(4.56609028732044,3.73660325533561,0.717036197220084));
#90718=CARTESIAN_POINT('Ctrl Pts',(4.76493750606009,1.41724241316736,3.5309727538468));
#90719=CARTESIAN_POINT('Ctrl Pts',(4.96378472479974,-2.20396827920308,3.10143008783366));
#90720=CARTESIAN_POINT('Ctrl Pts',(5.16263194353938,-3.80065884806476,-0.17702276560722));
#90721=CARTESIAN_POINT('Ctrl Pts',(5.36147916227902,-1.90614202843808,-3.29286612067976));
#90722=CARTESIAN_POINT('Ctrl Pts',(5.56032638101867,1.73931782266428,-3.38395009571249));
#90723=CARTESIAN_POINT('Ctrl Pts',(5.7591735997583,3.78707594089811,-0.366606807718136));
#90724=CARTESIAN_POINT('Ctrl Pts',(5.95802081849796,2.3561036528063,2.98749398474755));
#90725=CARTESIAN_POINT('Ctrl Pts',(6.15686803723759,-1.23913720134726,3.59734398276542));
#90726=CARTESIAN_POINT('Ctrl Pts',(6.35571525597724,-3.69613199798101,0.90274746565892));
#90727=CARTESIAN_POINT('Ctrl Pts',(6.55456247471689,-2.75793563212223,-2.62109438634679));
#90728=CARTESIAN_POINT('Ctrl Pts',(6.75340969345651,0.713643927253199,-3.73725261100972));
#90729=CARTESIAN_POINT('Ctrl Pts',(6.95225691219618,3.52968478935634,-1.42044712011787));
#90730=CARTESIAN_POINT('Ctrl Pts',(7.15110413093581,3.10342948627254,2.20115200678779));
#90731=CARTESIAN_POINT('Ctrl Pts',(7.34995134967546,-0.173572589605763,
3.80081797636178));
#90732=CARTESIAN_POINT('Ctrl Pts',(7.5487985684151,-3.29113443916401,1.90913038753869));
#90733=CARTESIAN_POINT('Ctrl Pts',(7.74764578715474,-3.38552759009604,-1.73624527932365));
#90734=CARTESIAN_POINT('Ctrl Pts',(7.94649300589439,-0.370044426978368,
-3.78674158813926));
#90735=CARTESIAN_POINT('Ctrl Pts',(8.14534022463402,2.98535396884146,-2.35881462052452));
#90736=CARTESIAN_POINT('Ctrl Pts',(8.34418744337368,3.59846734417717,1.23587115273742));
#90737=CARTESIAN_POINT('Ctrl Pts',(8.5430346621133,0.906102308030839,3.69531099376764));
#90738=CARTESIAN_POINT('Ctrl Pts',(8.74188188085297,-2.61858975274077,2.76031383000544));
#90739=CARTESIAN_POINT('Ctrl Pts',(8.9407290995926,-3.73789889119155,-0.710251091169461));
#90740=CARTESIAN_POINT('Ctrl Pts',(9.13957631833225,-1.42365065440879,-3.5283939048071));
#90741=CARTESIAN_POINT('Ctrl Pts',(9.33842353707189,2.19833391941629,-3.10542633337554));
#90742=CARTESIAN_POINT('Ctrl Pts',(9.53727075581154,3.80097397324239,0.170122273710265));
#90743=CARTESIAN_POINT('Ctrl Pts',(9.73611797455117,1.91211717314025,3.28940004399899));
#90744=CARTESIAN_POINT('Ctrl Pts',(9.93496519329084,-1.73317130509472,3.3871022955433));
#90745=CARTESIAN_POINT('Ctrl Pts',(10.1338124120305,-3.78640411505716,0.373481740861062));
#90746=CARTESIAN_POINT('Ctrl Pts',(10.3326596307701,-2.36152364445282,-2.98321149266503));
#90747=CARTESIAN_POINT('Ctrl Pts',(10.5315068495098,1.23260408570343,-3.5995877404483));
#90748=CARTESIAN_POINT('Ctrl Pts',(10.7303540682494,3.69448694450072,-0.909456403678715));
#90749=CARTESIAN_POINT('Ctrl Pts',(10.929201286989,2.76268975328713,2.6160829612917));
#90750=CARTESIAN_POINT('Ctrl Pts',(11.1280485057287,-0.706857669810684,
3.73854209123132));
#90751=CARTESIAN_POINT('Ctrl Pts',(11.3268957244683,-3.52710011273949,1.42685301555257));
#90752=CARTESIAN_POINT('Ctrl Pts',(11.525742943208,-3.10742062149762,-2.19551402053591));
#90753=CARTESIAN_POINT('Ctrl Pts',(11.7245901619476,0.166671817627617,-3.80112683798992));
#90754=CARTESIAN_POINT('Ctrl Pts',(11.9234373806873,3.28766293825345,-1.91510238308899));
#90755=CARTESIAN_POINT('Ctrl Pts',(12.1222845994269,3.38867420989955,1.73009590267132));
#90756=CARTESIAN_POINT('Ctrl Pts',(12.3211318181666,0.376918746981777,3.78606352184589));
#90757=CARTESIAN_POINT('Ctrl Pts',(12.5199790369062,-2.98106655821793,2.36423072240277));
#90758=CARTESIAN_POINT('Ctrl Pts',(12.7188262556458,-3.60070517053307,-1.22933600296043));
#90759=CARTESIAN_POINT('Ctrl Pts',(12.9176734743855,-0.912809749902704,
-3.69365985084727));
#90760=CARTESIAN_POINT('Ctrl Pts',(13.1165206931251,2.61357401409871,-2.76506340001571));
#90761=CARTESIAN_POINT('Ctrl Pts',(13.3153679118648,3.73918221058152,0.703463665976447));
#90762=CARTESIAN_POINT('Ctrl Pts',(13.5142151306044,1.43005420091953,3.52580341421793));
#90763=CARTESIAN_POINT('Ctrl Pts',(13.7130623493441,-2.19269231247512,3.10941234899633));
#90764=CARTESIAN_POINT('Ctrl Pts',(13.9119095680837,-3.80127657047585,-0.163221224201524));
#90765=CARTESIAN_POINT('Ctrl Pts',(14.1107567868233,-1.91808601492637,-3.28592312335854));
#90766=CARTESIAN_POINT('Ctrl Pts',(14.309604005563,1.72701907458831,-3.39024333186964));
#90767=CARTESIAN_POINT('Ctrl Pts',(14.5084512243026,3.78571980878574,-0.380355442508247));
#90768=CARTESIAN_POINT('Ctrl Pts',(14.7072984430423,2.36693585214384,2.97891916726764));
#90769=CARTESIAN_POINT('Ctrl Pts',(14.9061456617819,-1.22606690720154,3.60181963351076));
#90770=CARTESIAN_POINT('Ctrl Pts',(15.1049928805216,-3.6928297134888,0.91616234393948));
#90771=CARTESIAN_POINT('Ctrl Pts',(15.3038400992612,-2.76743476823527,-2.61106291322922));
#90772=CARTESIAN_POINT('Ctrl Pts',(15.5026873180008,0.700069082463514,-3.73981924871471));
#90773=CARTESIAN_POINT('Ctrl Pts',(15.7015345367405,3.52450381031094,-1.43325420787175));
#90774=CARTESIAN_POINT('Ctrl Pts',(15.9003817554801,3.11140151423042,2.18986879755912));
#90775=CARTESIAN_POINT('Ctrl Pts',(16.0992289742198,-0.159770496275433,
3.80142317057682));
#90776=CARTESIAN_POINT('Ctrl Pts',(16.2980761929594,-3.28418060074793,1.92106806619373));
#90777=CARTESIAN_POINT('Ctrl Pts',(16.4969234116991,-3.39180966016057,-1.7239408233811));
#90778=CARTESIAN_POINT('Ctrl Pts',(16.6957706304387,-0.383791824608539,
-3.78537297615996));
#90779=CARTESIAN_POINT('Ctrl Pts',(16.8946178491784,2.97676932158368,-2.36963903144691));
#90780=CARTESIAN_POINT('Ctrl Pts',(17.093465067918,3.60293112846299,1.22279680112061));
#90781=CARTESIAN_POINT('Ctrl Pts',(17.2923122866577,0.919514183026436,3.69199653310937));
#90782=CARTESIAN_POINT('Ctrl Pts',(17.4911595053973,-2.60854966075247,2.76980385599172));
#90783=CARTESIAN_POINT('Ctrl Pts',(17.6900067241369,-3.74045320510594,-0.696673922069122));
#90784=CARTESIAN_POINT('Ctrl Pts',(17.8888539428766,-1.43645303377236,-3.52320130208942));
#90785=CARTESIAN_POINT('Ctrl Pts',(18.0877011616162,2.18704347811457,-3.11338811556075));
#90786=CARTESIAN_POINT('Ctrl Pts',(18.2865483803559,3.80156663817204,0.15631963669288));
#90787=CARTESIAN_POINT('Ctrl Pts',(18.4853955990955,1.92404853443372,3.28243537185758));
#90788=CARTESIAN_POINT('Ctrl Pts',(18.6842428178352,-1.72086115158631,3.39337319348159));
#90789=CARTESIAN_POINT('Ctrl Pts',(18.8830900365748,-3.78502302425433,0.387227890450935));
#90790=CARTESIAN_POINT('Ctrl Pts',(19.0819372553145,-2.37234025808448,-2.97461702293759));
#90791=CARTESIAN_POINT('Ctrl Pts',(19.2807844740541,1.2195256874123,-3.60403965447385));
#90792=CARTESIAN_POINT('Ctrl Pts',(19.4796316927937,3.69116031039557,-0.922865264401502));
#90793=CARTESIAN_POINT('Ctrl Pts',(19.6784789115334,2.77217066133281,2.60603425873952));
#90794=CARTESIAN_POINT('Ctrl Pts',(19.877326130273,-0.693278187591044,3.74108407923277));
#90795=CARTESIAN_POINT('Ctrl Pts',(20.0761733490127,-3.52189589062669,1.4396506759854));
#90796=CARTESIAN_POINT('Ctrl Pts',(20.2750205677523,-3.11537215135031,-2.18421635646961));
#90797=CARTESIAN_POINT('Ctrl Pts',(20.473867786492,0.152868648297455,-3.80170697314327));
#90798=CARTESIAN_POINT('Ctrl Pts',(20.6727150052316,3.28068743812558,-1.92702741719039));
#90799=CARTESIAN_POINT('Ctrl Pts',(20.8715622239712,3.39493393054431,1.71778006174172));
#90800=CARTESIAN_POINT('Ctrl Pts',(21.0704094427109,0.390663637203989,3.78466995335721));
#90801=CARTESIAN_POINT('Ctrl Pts',(21.2692566614505,-2.97246227310292,2.37503952983065));
#90802=CARTESIAN_POINT('Ctrl Pts',(21.4681038801901,-3.60514521062988,-1.21625356877211));
#90803=CARTESIAN_POINT('Ctrl Pts',(21.6669510989298,-0.926215585303307,
-3.69032104603647));
#90804=CARTESIAN_POINT('Ctrl Pts',(21.8657983176694,2.60351670926311,-2.77453518230824));
#90805=CARTESIAN_POINT('Ctrl Pts',(22.0646455364091,3.74171187057536,0.68988188182749));
#90806=CARTESIAN_POINT('Ctrl Pts',(22.2634927551487,1.44284713187585,3.52058757699848));
#90807=CARTESIAN_POINT('Ctrl Pts',(22.4623399738884,-2.18138743495393,3.11735361996415));
#90808=CARTESIAN_POINT('Ctrl Pts',(22.661187192628,-3.80184417537488,-0.149417533932911));
#90809=CARTESIAN_POINT('Ctrl Pts',(22.8600344113677,-1.93000471200901,-3.27893680099228));
#90810=CARTESIAN_POINT('Ctrl Pts',(23.0588816301073,1.71469755638623,-3.39649187006262));
#90811=CARTESIAN_POINT('Ctrl Pts',(23.2577288488469,3.7843137637596,-0.394099062036515));
#90812=CARTESIAN_POINT('Ctrl Pts',(23.4565760675866,2.37773684446108,2.97030507385532));
#90813=CARTESIAN_POINT('Ctrl Pts',(23.6554232863262,-1.2129804478964,3.60624779602004));
#90814=CARTESIAN_POINT('Ctrl Pts',(23.8542705050659,-3.6894787407236,0.929565142971094));
#90815=CARTESIAN_POINT('Ctrl Pts',(24.0531177238055,-2.77689741696962,-2.60099701439775));
#90816=CARTESIAN_POINT('Ctrl Pts',(24.2519649425452,0.686485007577086,-3.74233657861642));
#90817=CARTESIAN_POINT('Ctrl Pts',(24.4508121612848,3.51927636228287,-1.44604239880977));
#90818=CARTESIAN_POINT('Ctrl Pts',(24.6496593800244,3.11933251976945,2.17855671589865));
#90819=CARTESIAN_POINT('Ctrl Pts',(24.8485065987641,-0.145966296443085,
3.80197824475378));
#90820=CARTESIAN_POINT('Ctrl Pts',(25.0473538175037,-3.27718346190025,1.93298041643621));
#90821=CARTESIAN_POINT('Ctrl Pts',(25.2462010362434,-3.39804701075277,-1.71161363805988));
#90822=CARTESIAN_POINT('Ctrl Pts',(25.445048254983,-0.397534162117675,-3.78395445575495));
#90823=CARTESIAN_POINT('Ctrl Pts',(25.6438954737227,2.96814542697233,-2.38043219975316));
#90824=CARTESIAN_POINT('Ctrl Pts',(25.8427426924623,3.6073474097358,1.20970632748235));
#90825=CARTESIAN_POINT('Ctrl Pts',(26.041589911202,0.932913934644615,3.68863339515115));
#90826=CARTESIAN_POINT('Ctrl Pts',(26.2404371299416,-2.59847517621982,2.77925736337026));
#90827=CARTESIAN_POINT('Ctrl Pts',(26.4392843486812,-3.74295820284109,-0.683087567638958));
#90828=CARTESIAN_POINT('Ctrl Pts',(26.6381315674209,-1.44923647415423,-3.51796224756029));
#90829=CARTESIAN_POINT('Ctrl Pts',(26.8369787861605,2.17572420163629,-3.12130884913566));
#90830=CARTESIAN_POINT('Ctrl Pts',(27.0358260049002,3.80210918116955,0.142514938671839));
#90831=CARTESIAN_POINT('Ctrl Pts',(27.2346732236398,1.93595452801991,3.27542742229433));
#90832=CARTESIAN_POINT('Ctrl Pts',(27.4335204423795,-1.70852830930399,3.39959935133324));
#90833=CARTESIAN_POINT('Ctrl Pts',(27.6323676611191,-3.78359202963939,0.400968934616709));
#90834=CARTESIAN_POINT('Ctrl Pts',(27.8312148798588,-2.38312559348573,-2.96598333423363));
#90835=CARTESIAN_POINT('Ctrl Pts',(28.0300620985984,1.20643121022795,-3.608444050871));
#90836=CARTESIAN_POINT('Ctrl Pts',(28.228909317338,3.68778501001565,-0.936261957564374));
#90837=CARTESIAN_POINT('Ctrl Pts',(28.4277565360777,2.78161501956553,2.59595119680741));
#90838=CARTESIAN_POINT('Ctrl Pts',(28.6266037548173,-0.679689564812835,
3.74357674273721));
#90839=CARTESIAN_POINT('Ctrl Pts',(28.825450973557,-3.51664523391372,1.45242935527699));
#90840=CARTESIAN_POINT('Ctrl Pts',(29.0242981922966,-3.12328260643402,-2.17288989450111));
#90841=CARTESIAN_POINT('Ctrl Pts',(29.2231454110363,0.139063463463399,-3.80223698451424));
#90842=CARTESIAN_POINT('Ctrl Pts',(29.4219926297759,3.27366868362155,-1.93892704430927));
#90843=CARTESIAN_POINT('Ctrl Pts',(29.6208398485156,3.40114889052482,1.70544157266093));
#90844=CARTESIAN_POINT('Ctrl Pts',(29.8196870672551,0.404403376703387,3.78322648571156));
#90845=CARTESIAN_POINT('Ctrl Pts',(30.0185342859949,-2.96381879742084,2.38581702343944));
#90846=CARTESIAN_POINT('Ctrl Pts',(30.2173815047344,-3.60953771852199,-1.20315509883203));
#90847=CARTESIAN_POINT('Ctrl Pts',(30.4162287234741,-0.939609208971511,
-3.6869335860162));
#90848=CARTESIAN_POINT('Ctrl Pts',(30.6150759422137,2.59342507824035,-2.78397038361267));
#90849=CARTESIAN_POINT('Ctrl Pts',(30.8139231609534,3.74419219779503,0.676291001898722));
#90850=CARTESIAN_POINT('Ctrl Pts',(31.012770379693,1.45562103954713,3.51532532242837));
#90851=CARTESIAN_POINT('Ctrl Pts',(31.2116175984327,-2.17005379682861,3.1252537900382));
#90852=CARTESIAN_POINT('Ctrl Pts',(31.4104648171723,-3.80236165468257,-0.135611873661794));
#90853=CARTESIAN_POINT('Ctrl Pts',(31.609312035912,-1.94189796285485,-3.27190724733122));
#90854=CARTESIAN_POINT('Ctrl Pts',(31.8081592546516,1.70235343067438,-3.40269562705064));
#90855=CARTESIAN_POINT('Ctrl Pts',(32.0070064733913,3.78285782427264,-0.40783748554748));
#90856=CARTESIAN_POINT('Ctrl Pts',(32.2058536921309,2.38850648739641,2.96165181831755));
#90857=CARTESIAN_POINT('Ctrl Pts',(32.4047009108705,-1.1998779959941,3.61062841178759));
#90858=CARTESIAN_POINT('Ctrl Pts',(32.6035481296102,-3.68607912385444,0.942955686107798));
#90859=CARTESIAN_POINT('Ctrl Pts',(32.8023953483499,-2.78632345357075,-2.59089682260023));
#90860=CARTESIAN_POINT('Ctrl Pts',(33.0012425670895,0.672891881697152,-3.74480456750742));
#90861=CARTESIAN_POINT('Ctrl Pts',(33.2000897858292,3.51400251419191,-1.45881152433458));
#90862=CARTESIAN_POINT('Ctrl Pts',(33.3989370045687,3.12722239832386,2.1672159109558));
#90863=CARTESIAN_POINT('Ctrl Pts',(33.5977842233084,-0.132160172111266,
3.80248319157178));
#90864=CARTESIAN_POINT('Ctrl Pts',(33.7966314420481,-3.27014311487478,1.94486728120854));
#90865=CARTESIAN_POINT('Ctrl Pts',(33.9954786607877,-3.40423955963616,-1.69926388588902));
#90866=CARTESIAN_POINT('Ctrl Pts',(34.1943258795274,-0.411271258319173,
-3.78248604562647));
#90867=CARTESIAN_POINT('Ctrl Pts',(34.393173098267,2.95948239870956,-2.39119398314037));
#90868=CARTESIAN_POINT('Ctrl Pts',(34.5920203170067,3.61171612976893,1.19659990441474));
#90869=CARTESIAN_POINT('Ctrl Pts',(34.7908675357462,0.946301386215602,3.68522162423442));
#90870=CARTESIAN_POINT('Ctrl Pts',(34.989714754486,-2.58836643197043,2.78867422750081));
#90871=CARTESIAN_POINT('Ctrl Pts',(35.1885619732255,-3.74541385136976,-0.669492207009116));
#90872=CARTESIAN_POINT('Ctrl Pts',(35.3874091919652,-1.46200080701025,-3.51267681029436));
#90873=CARTESIAN_POINT('Ctrl Pts',(35.5862564107049,2.16437623922122,-3.12918842966879));
#90874=CARTESIAN_POINT('Ctrl Pts',(35.7851036294445,3.80260159508174,0.128708361656123));
#90875=CARTESIAN_POINT('Ctrl Pts',(35.9839508481841,1.94783499692349,3.26837628770594));
#90876=CARTESIAN_POINT('Ctrl Pts',(36.1827980669238,-1.69617294085073,3.4057806870091));
#90877=CARTESIAN_POINT('Ctrl Pts',(36.3816452856634,-3.78211115007939,0.414704692188958));
#90878=CARTESIAN_POINT('Ctrl Pts',(36.580492504403,-2.39387950845679,-2.95731054038447));
#90879=CARTESIAN_POINT('Ctrl Pts',(36.7793397231427,1.1933208267952,-3.61280087156976));
#90880=CARTESIAN_POINT('Ctrl Pts',(36.9781869418823,3.68436108786276,-0.949646306537922));
#90881=CARTESIAN_POINT('Ctrl Pts',(37.177034160622,2.79102270346568,2.58583390843602));
#90882=CARTESIAN_POINT('Ctrl Pts',(37.3758813793616,-0.666091980635988,
3.74602004888));
#90883=CARTESIAN_POINT('Ctrl Pts',(37.5747285981013,-3.51134821182816,1.46518888494614));
#90884=CARTESIAN_POINT('Ctrl Pts',(37.7735758168409,-3.13115188245291,-2.16153478396487));
#90885=CARTESIAN_POINT('Ctrl Pts',(37.9724230355806,0.125256445140788,-3.80271686511487));
#90886=CARTESIAN_POINT('Ctrl Pts',(38.1712702543202,3.26660676728062,-1.95080110755424));
#90887=CARTESIAN_POINT('Ctrl Pts',(38.3701174730598,3.40731900789955,1.69308059810655));
#90888=CARTESIAN_POINT('Ctrl Pts',(38.5689646917995,0.418137784327558,3.78173313794033));
#90889=CARTESIAN_POINT('Ctrl Pts',(38.7678119105391,-2.95513624513198,2.39656306113269));
#90890=CARTESIAN_POINT('Ctrl Pts',(38.9666591292788,-3.61388263629621,-1.19004076583754));
#90891=CARTESIAN_POINT('Ctrl Pts',(39.1655063480184,-0.952990444318419,
-3.68349751544863));
#90892=CARTESIAN_POINT('Ctrl Pts',(39.3643535667581,2.58329925408403,-2.79336887953011));
#90893=CARTESIAN_POINT('Ctrl Pts',(39.5632007854977,3.74662315953856,0.662691205379788));
#90894=CARTESIAN_POINT('Ctrl Pts',(39.7620480042374,1.46837575551511,3.51001671988807));
#90895=CARTESIAN_POINT('Ctrl Pts',(39.960895222977,-2.15869154752812,3.13311275505833));
#90896=CARTESIAN_POINT('Ctrl Pts',(40.1597424417167,-3.80282900157622,-0.12180442540972));
#90897=CARTESIAN_POINT('Ctrl Pts',(40.3585896604562,-1.95376561065657,-3.26483455505699));
#90898=CARTESIAN_POINT('Ctrl Pts',(40.5574368791959,1.6899868602047,-3.40885452103984));
#90899=CARTESIAN_POINT('Ctrl Pts',(40.7562840979356,3.78135200952079,-0.421570531905988));
#90900=CARTESIAN_POINT('Ctrl Pts',(40.9551313166752,2.39924463895674,2.95295951474376));
#90901=CARTESIAN_POINT('Ctrl Pts',(41.1539785354149,-1.18675972424462,3.61496142305686));
#90902=CARTESIAN_POINT('Ctrl Pts',(41.3528257541545,-3.68263090770359,0.956333796801414));
#90903=CARTESIAN_POINT('Ctrl Pts',(41.5516729728942,-2.7957127537608,-2.580762471003));
#90904=CARTESIAN_POINT('Ctrl Pts',(41.7505201916338,0.659289884042882,-3.74722318284854));
#90905=CARTESIAN_POINT('Ctrl Pts',(41.9493674103735,3.50868233557138,-1.4715614160909));
#90906=CARTESIAN_POINT('Ctrl Pts',(42.148214629113,3.13507104586913,2.15584653225381));
#90907=CARTESIAN_POINT('Ctrl Pts',(42.3470618478528,-0.118352305307547,
3.80293800437367));
#90908=CARTESIAN_POINT('Ctrl Pts',(42.5459090665923,-3.26305965249527,1.95672850378705));
#90909=CARTESIAN_POINT('Ctrl Pts',(42.744756285332,-3.4103872251649,-1.68689172969318));
#90910=CARTESIAN_POINT('Ctrl Pts',(42.9436035040717,-0.425002932095231,
-3.78096776513734));
#90911=CARTESIAN_POINT('Ctrl Pts',(43.1424507228113,2.95078035101296,-2.4019242397144));
#90912=CARTESIAN_POINT('Ctrl Pts',(43.341297941551,3.61603723096387,1.18347770471091));
#90913=CARTESIAN_POINT('Ctrl Pts',(43.5401451602905,0.959676361229754,3.68176126535944));
#90914=CARTESIAN_POINT('Ctrl Pts',(43.7389923790303,-2.57822356127927,2.79805432419252));
#90915=CARTESIAN_POINT('Ctrl Pts',(43.9378395977698,-3.74782011832323,-0.655888019363382));
#90916=CARTESIAN_POINT('Ctrl Pts',(44.1366868165096,-1.47474586403367,-3.50734506010128));
#90917=CARTESIAN_POINT('Ctrl Pts',(44.3355340352491,2.15299974045801,-3.13702675303505));
#90918=CARTESIAN_POINT('Ctrl Pts',(44.5343812539888,3.80304387347161,0.114900087226417));
#90919=CARTESIAN_POINT('Ctrl Pts',(44.7332284727285,1.95968978440039,3.26128206192395));
#90920=CARTESIAN_POINT('Ctrl Pts',(44.9320756914681,-1.68379520892431,3.41191711735532));
#90921=CARTESIAN_POINT('Ctrl Pts',(45.1309229102078,-3.78058040548574,0.428434985235317));
#90922=CARTESIAN_POINT('Ctrl Pts',(45.3297701289473,-2.40460186047238,-2.94859876179618));
#90923=CARTESIAN_POINT('Ctrl Pts',(45.5286173476871,1.1801947085537,-3.61711004753668));
#90924=CARTESIAN_POINT('Ctrl Pts',(45.7274645664266,3.68088859178643,-0.963018157027625));
#90925=CARTESIAN_POINT('Ctrl Pts',(45.9263117851663,2.80039358381952,2.57568256943094));
#90926=CARTESIAN_POINT('Ctrl Pts',(46.1251590039059,-0.652485604434125,
3.74841388431312));
#90927=CARTESIAN_POINT('Ctrl Pts',(46.3240062226456,-3.50600491315505,1.47792925196772));
#90928=CARTESIAN_POINT('Ctrl Pts',(46.5228534413853,-3.13897983941142,-2.15015147146503));
#90929=CARTESIAN_POINT('Ctrl Pts',(46.7217006601249,0.111447706038876,-3.80314604068544));
#90930=CARTESIAN_POINT('Ctrl Pts',(46.9205478788645,3.2595019148334,-1.96265053678374));
#90931=CARTESIAN_POINT('Ctrl Pts',(47.1193950976042,3.41344394762139,1.68069937927697));
#90932=CARTESIAN_POINT('Ctrl Pts',(47.3182423163438,0.431867164297962,3.78018595424573));
#90933=CARTESIAN_POINT('Ctrl Pts',(47.5170895350834,-2.94641565906025,2.40728510603513));
#90934=CARTESIAN_POINT('Ctrl Pts',(47.7159367538232,-3.61817813080653,-1.17692529011616));
#90935=CARTESIAN_POINT('Ctrl Pts',(47.9147839725627,-0.966362512003955,
-3.6799850515108));
#90936=CARTESIAN_POINT('Ctrl Pts',(48.1136311913024,2.57314586865933,-2.80278377932925));
#90937=CARTESIAN_POINT('Ctrl Pts',(48.312478410042,3.74899229294714,0.649184503364175));
#90938=CARTESIAN_POINT('Ctrl Pts',(48.5113256287817,1.48113489022536,3.50446703634001));
#90939=CARTESIAN_POINT('Ctrl Pts',(48.7101728475214,-2.14734631830912,3.14130311320274));
#90940=CARTESIAN_POINT('Ctrl Pts',(48.9090200662609,-3.80315925416883,-0.108708843536021));
#90941=CARTESIAN_POINT('Ctrl Pts',(49.1078672850007,-1.96577341939554,-3.25634932763291));
#90942=CARTESIAN_POINT('Ctrl Pts',(49.3067145037402,1.67791165511384,-3.4176299985622));
#90943=CARTESIAN_POINT('Ctrl Pts',(49.5055617224799,3.77922892071463,-0.429833904099183));
#90944=CARTESIAN_POINT('Ctrl Pts',(49.638126534973,2.86700543115724,1.81047758327496));
#90945=CARTESIAN_POINT('Ctrl Pts',(49.7044089412195,2.03762250733507,2.48935576416972));
#90946=CARTESIAN_POINT('Ctrl Pts',(0.585799999999996,1.82083948017239,3.48611999039699));
#90947=CARTESIAN_POINT('Ctrl Pts',(0.585799999999996,1.79697629238951,3.49827540268515));
#90948=CARTESIAN_POINT('Ctrl Pts',(0.585799999999996,1.77311310460663,3.5104308149733));
#90949=CARTESIAN_POINT('Ctrl Pts',(0.585799999999996,1.74924991682375,3.52258622726146));
#90950=CARTESIAN_POINT('Origin',(0.,3.3472,0.));
#90951=CARTESIAN_POINT('',(-1.11022302462516E-15,-3.3472,-4.09913776610602E-16));
#90952=CARTESIAN_POINT('Origin',(0.,0.,0.));
#90953=CARTESIAN_POINT('Origin',(0.326399999999998,0.,0.));
#90954=CARTESIAN_POINT('',(0.326399999999998,-3.6736,-4.49886248134772E-16));
#90955=CARTESIAN_POINT('Origin',(49.724,0.,0.));
#90956=CARTESIAN_POINT('',(50.224,-3.,-3.67394039744206E-16));
#90957=CARTESIAN_POINT('',(49.724,-3.5,4.28626379701574E-16));
#90958=CARTESIAN_POINT('Origin',(50.224,0.,0.));
#90959=CARTESIAN_POINT('Origin',(51.224,0.,0.));
#90960=CARTESIAN_POINT('',(52.224,-3.,-3.67394039744206E-16));
#90961=CARTESIAN_POINT('Origin',(52.224,0.,0.));
#90962=CARTESIAN_POINT('',(51.224,-3.,-3.67394039744206E-16));
#90963=CARTESIAN_POINT('Origin',(52.224,3.95,0.));
#90964=CARTESIAN_POINT('',(52.224,-3.95,-4.83735485663205E-16));
#90965=CARTESIAN_POINT('Origin',(52.224,0.,0.));
#90966=CARTESIAN_POINT('Origin',(57.936,0.,0.));
#90967=CARTESIAN_POINT('',(63.648,-3.95,-4.83735485663205E-16));
#90968=CARTESIAN_POINT('Origin',(63.648,0.,0.));
#90969=CARTESIAN_POINT('',(57.936,-3.95,-4.83735485663205E-16));
#90970=CARTESIAN_POINT('Origin',(63.648,2.448,0.));
#90971=CARTESIAN_POINT('',(63.648,-2.448,-2.99793536431272E-16));
#90972=CARTESIAN_POINT('Origin',(63.648,0.,0.));
#90973=CARTESIAN_POINT('Origin',(66.3,0.,0.));
#90974=CARTESIAN_POINT('',(68.952,-2.448,-2.99793536431272E-16));
#90975=CARTESIAN_POINT('Origin',(68.952,0.,0.));
#90976=CARTESIAN_POINT('',(66.3,-2.448,-2.99793536431272E-16));
#90977=CARTESIAN_POINT('Origin',(69.156,0.,0.));
#90978=CARTESIAN_POINT('',(69.36,-2.04,-2.4982794702606E-16));
#90979=CARTESIAN_POINT('',(69.156,-2.244,2.74810741728666E-16));
#90980=CARTESIAN_POINT('Origin',(69.36,0.,0.));
#90981=CARTESIAN_POINT('Origin',(69.36,0.,0.));
#90982=CARTESIAN_POINT('',(0.,0.,0.));
#90983=CARTESIAN_POINT('Origin',(0.,14.688,9.576));
#90984=CARTESIAN_POINT('',(-7.65475852003184,22.032,9.576));
#90985=CARTESIAN_POINT('',(-6.79895050724742,22.032,8.976));
#90986=CARTESIAN_POINT('Ctrl Pts',(-7.65475852003184,22.032,9.576));
#90987=CARTESIAN_POINT('Ctrl Pts',(-7.65475852003184,22.032,9.50993230753524));
#90988=CARTESIAN_POINT('Ctrl Pts',(-7.6355023933674,22.032,9.43302512212287));
#90989=CARTESIAN_POINT('Ctrl Pts',(-7.57108059612176,22.032,9.30349794685379));
#90990=CARTESIAN_POINT('Ctrl Pts',(-7.50985737643954,22.032,9.23175552494297));
#90991=CARTESIAN_POINT('Ctrl Pts',(-7.37339958496305,22.032,9.12015369808754));
#90992=CARTESIAN_POINT('Ctrl Pts',(-7.26915110200772,22.032,9.06654458042145));
#90993=CARTESIAN_POINT('Ctrl Pts',(-7.06240578389491,22.032,8.99697822671308));
#90994=CARTESIAN_POINT('Ctrl Pts',(-6.91939858523134,22.032,8.976));
#90995=CARTESIAN_POINT('Ctrl Pts',(-6.79895050724742,22.032,8.976));
#90996=CARTESIAN_POINT('',(7.65475852003184,22.032,9.576));
#90997=CARTESIAN_POINT('Origin',(0.,14.688,9.576));
#90998=CARTESIAN_POINT('',(6.79895050724742,22.032,8.976));
#90999=CARTESIAN_POINT('Ctrl Pts',(6.79895050724742,22.032,8.976));
#91000=CARTESIAN_POINT('Ctrl Pts',(6.91939858523134,22.032,8.976));
#91001=CARTESIAN_POINT('Ctrl Pts',(7.06240578389491,22.032,8.99697822671308));
#91002=CARTESIAN_POINT('Ctrl Pts',(7.26915110200772,22.032,9.06654458042145));
#91003=CARTESIAN_POINT('Ctrl Pts',(7.37339958496305,22.032,9.12015369808754));
#91004=CARTESIAN_POINT('Ctrl Pts',(7.50985737643954,22.032,9.23175552494297));
#91005=CARTESIAN_POINT('Ctrl Pts',(7.57108059612176,22.032,9.30349794685379));
#91006=CARTESIAN_POINT('Ctrl Pts',(7.6355023933674,22.032,9.43302512212287));
#91007=CARTESIAN_POINT('Ctrl Pts',(7.65475852003183,22.032,9.50993230753524));
#91008=CARTESIAN_POINT('Ctrl Pts',(7.65475852003183,22.032,9.576));
#91009=CARTESIAN_POINT('Origin',(0.,14.688,8.976));
#91010=CARTESIAN_POINT('Origin',(0.,14.688,8.976));
#91011=CARTESIAN_POINT('',(-8.976,22.032,8.976));
#91012=CARTESIAN_POINT('Origin',(0.,14.688,9.576));
#91013=CARTESIAN_POINT('',(8.976,20.3414138359048,9.576));
#91014=CARTESIAN_POINT('',(8.976,19.1142272874311,8.976));
#91015=CARTESIAN_POINT('Ctrl Pts',(8.976,20.3414138359048,9.576));
#91016=CARTESIAN_POINT('Ctrl Pts',(8.976,20.3414138359048,9.54827127066274));
#91017=CARTESIAN_POINT('Ctrl Pts',(8.976,20.3367898671095,9.51531964531999));
#91018=CARTESIAN_POINT('Ctrl Pts',(8.976,20.3212334425194,9.45910065247902));
#91019=CARTESIAN_POINT('Ctrl Pts',(8.976,20.3065635015877,9.42543456124496));
#91020=CARTESIAN_POINT('Ctrl Pts',(8.976,20.249339321466,9.32728853684005));
#91021=CARTESIAN_POINT('Ctrl Pts',(8.976,20.1766041453243,9.25923361702201));
#91022=CARTESIAN_POINT('Ctrl Pts',(8.976,20.0032332384638,9.14149743330231));
#91023=CARTESIAN_POINT('Ctrl Pts',(8.976,19.8621493346214,9.08527290977984));
#91024=CARTESIAN_POINT('Ctrl Pts',(8.976,19.5489440827006,8.9996546128544));
#91025=CARTESIAN_POINT('Ctrl Pts',(8.976,19.3123620171841,8.976));
#91026=CARTESIAN_POINT('Ctrl Pts',(8.976,19.1142272874311,8.976));
#91027=CARTESIAN_POINT('',(10.502406415234,16.1810249459574,9.5759999995841));
#91028=CARTESIAN_POINT('Origin',(0.,14.688,9.576));
#91029=CARTESIAN_POINT('',(10.3410376317382,16.32,9.19200000000005));
#91030=CARTESIAN_POINT('Ctrl Pts',(10.3410376317382,16.32,9.19200000000005));
#91031=CARTESIAN_POINT('Ctrl Pts',(10.3617248081483,16.32,9.21653309283687));
#91032=CARTESIAN_POINT('Ctrl Pts',(10.3805706312753,16.318496659833,9.2425856919711));
#91033=CARTESIAN_POINT('Ctrl Pts',(10.427575989582,16.3085883313445,9.31828555819472));
#91034=CARTESIAN_POINT('Ctrl Pts',(10.4505455557009,16.2959510697933,9.36877738492597));
#91035=CARTESIAN_POINT('Ctrl Pts',(10.4861453619965,16.2525805866431,9.47477477792537));
#91036=CARTESIAN_POINT('Ctrl Pts',(10.4967081983238,16.2211079934846,9.5278768615026));
#91037=CARTESIAN_POINT('Ctrl Pts',(10.5024064153566,16.1810249450952,9.576));
#91038=CARTESIAN_POINT('',(9.87403868738623,16.32,8.976));
#91039=CARTESIAN_POINT('Ctrl Pts',(9.87403868738623,16.32,8.976));
#91040=CARTESIAN_POINT('Ctrl Pts',(9.94938560299478,16.32,8.976));
#91041=CARTESIAN_POINT('Ctrl Pts',(10.038098637739,16.32,8.99346724198458));
#91042=CARTESIAN_POINT('Ctrl Pts',(10.1769613378484,16.32,9.05056345745539));
#91043=CARTESIAN_POINT('Ctrl Pts',(10.2518064406884,16.32,9.1001029151404));
#91044=CARTESIAN_POINT('Ctrl Pts',(10.3170794694341,16.32,9.16489488688007));
#91045=CARTESIAN_POINT('Ctrl Pts',(10.3292581499021,16.32,9.17803061550182));
#91046=CARTESIAN_POINT('Ctrl Pts',(10.3410376317382,16.32,9.19200000000005));
#91047=CARTESIAN_POINT('Origin',(0.,14.688,8.976));
#91048=CARTESIAN_POINT('Origin',(0.,14.688,8.976));
#91049=CARTESIAN_POINT('',(8.976,16.32,8.976));
#91050=CARTESIAN_POINT('',(5.406,16.32,8.976));
#91051=CARTESIAN_POINT('',(8.976,8.16,8.976));
#91052=CARTESIAN_POINT('Origin',(0.,14.688,9.576));
#91053=CARTESIAN_POINT('',(5.47747094926116,6.312,8.976));
#91054=CARTESIAN_POINT('',(7.58586053127791,8.16,8.976));
#91055=CARTESIAN_POINT('Origin',(0.,14.688,8.976));
#91056=CARTESIAN_POINT('',(8.18447918304358,8.16,9.19200000701435));
#91057=CARTESIAN_POINT('Ctrl Pts',(8.18447918091711,8.16,9.19200000927994));
#91058=CARTESIAN_POINT('Ctrl Pts',(8.17765408238493,8.16,9.18559400894369));
#91059=CARTESIAN_POINT('Ctrl Pts',(8.17079622196017,8.16,9.17943259569684));
#91060=CARTESIAN_POINT('Ctrl Pts',(8.09540917035175,8.16,9.11433225757306));
#91061=CARTESIAN_POINT('Ctrl Pts',(8.00027281944003,8.16,9.06175915897253));
#91062=CARTESIAN_POINT('Ctrl Pts',(7.8158147055935,8.16,8.99600010426086));
#91063=CARTESIAN_POINT('Ctrl Pts',(7.69110952727826,8.16,8.976));
#91064=CARTESIAN_POINT('Ctrl Pts',(7.58586053127791,8.16,8.976));
#91065=CARTESIAN_POINT('',(8.46817714968195,8.2989750539222,9.57599999941013));
#91066=CARTESIAN_POINT('Ctrl Pts',(8.46817714985942,8.29897505415743,9.57599999910267));
#91067=CARTESIAN_POINT('Ctrl Pts',(8.46646237140931,8.29670224292752,9.57327129421563));
#91068=CARTESIAN_POINT('Ctrl Pts',(8.46474068975494,8.29445309065062,9.5705217301252));
#91069=CARTESIAN_POINT('Ctrl Pts',(8.42551239387429,8.24397830303708,9.50768581373269));
#91070=CARTESIAN_POINT('Ctrl Pts',(8.38629718940947,8.20954290244375,9.44114604862779));
#91071=CARTESIAN_POINT('Ctrl Pts',(8.29342701346891,8.16764410001386,9.30890416369621));
#91072=CARTESIAN_POINT('Ctrl Pts',(8.24325036594714,8.16000000085317,9.2471623230443));
#91073=CARTESIAN_POINT('Ctrl Pts',(8.18447918091711,8.16,9.19200000927994));
#91074=CARTESIAN_POINT('',(5.65341383590482,5.712,9.576));
#91075=CARTESIAN_POINT('Origin',(0.,14.688,9.576));
#91076=CARTESIAN_POINT('Ctrl Pts',(5.65341383590482,5.712,9.576));
#91077=CARTESIAN_POINT('Ctrl Pts',(5.65341383590482,5.712,9.52772474461145));
#91078=CARTESIAN_POINT('Ctrl Pts',(5.65173396439858,5.71782566101816,9.47980816220151));
#91079=CARTESIAN_POINT('Ctrl Pts',(5.64844008976608,5.72922449769278,9.43326698381046));
#91080=CARTESIAN_POINT('Ctrl Pts',(5.64659978410904,5.73559308968745,9.40726417452521));
#91081=CARTESIAN_POINT('Ctrl Pts',(5.64425566453178,5.74370160503296,9.38168922134117));
#91082=CARTESIAN_POINT('Ctrl Pts',(5.6414192185381,5.75350649531546,9.35671706581409));
#91083=CARTESIAN_POINT('Ctrl Pts',(5.63717068251911,5.76819263057785,9.31931282738847));
#91084=CARTESIAN_POINT('Ctrl Pts',(5.63186786836281,5.78651310378535,9.28369622394997));
#91085=CARTESIAN_POINT('Ctrl Pts',(5.62561273253842,5.80807427644408,9.25033319920716));
#91086=CARTESIAN_POINT('Ctrl Pts',(5.61998111348851,5.8274862147444,9.22029582656189));
#91087=CARTESIAN_POINT('Ctrl Pts',(5.61357756657825,5.84952614262748,9.192082716188));
#91088=CARTESIAN_POINT('Ctrl Pts',(5.6064764971916,5.87392073737792,9.16601639098558));
#91089=CARTESIAN_POINT('Ctrl Pts',(5.59861749266153,5.90091909779573,9.13716786737686));
#91090=CARTESIAN_POINT('Ctrl Pts',(5.58998168778861,5.9305354967636,9.1112326479035));
#91091=CARTESIAN_POINT('Ctrl Pts',(5.58070580865448,5.96225420525281,9.08847781685686));
#91092=CARTESIAN_POINT('Ctrl Pts',(5.57155614999854,5.99354130499686,9.06603261960497));
#91093=CARTESIAN_POINT('Ctrl Pts',(5.56178371804112,6.02687598894637,9.04667972811001));
#91094=CARTESIAN_POINT('Ctrl Pts',(5.55151973301419,6.06179064324785,9.03066040140691));
#91095=CARTESIAN_POINT('Ctrl Pts',(5.54013886714959,6.10050455370966,9.01289792338588));
#91096=CARTESIAN_POINT('Ctrl Pts',(5.52823111361269,6.1408904656362,8.99935811831371));
#91097=CARTESIAN_POINT('Ctrl Pts',(5.51599488507964,6.18224768010664,8.99019769931974));
#91098=CARTESIAN_POINT('Ctrl Pts',(5.50371027646634,6.22376841435361,8.98100106150189));
#91099=CARTESIAN_POINT('Ctrl Pts',(5.49114480790582,6.26609816507474,8.97625599324861));
#91100=CARTESIAN_POINT('Ctrl Pts',(5.4785070788898,6.30852211597862,8.97601007981572));
#91101=CARTESIAN_POINT('Ctrl Pts',(5.47816173573397,6.30968140821139,8.97600335989628));
#91102=CARTESIAN_POINT('Ctrl Pts',(5.47781635774676,6.31084070775401,8.976));
#91103=CARTESIAN_POINT('Ctrl Pts',(5.47747094926116,6.312,8.976));
#91104=CARTESIAN_POINT('Origin',(8.16,6.312,9.576));
#91105=CARTESIAN_POINT('',(-5.47747094926116,6.312,8.976));
#91106=CARTESIAN_POINT('',(8.16,6.312,8.976));
#91107=CARTESIAN_POINT('',(-5.65341383590482,5.712,9.576));
#91108=CARTESIAN_POINT('',(8.16,5.712,9.576));
#91109=CARTESIAN_POINT('Ctrl Pts',(-5.65341383590481,5.712,9.576));
#91110=CARTESIAN_POINT('Ctrl Pts',(-5.65341383590481,5.712,9.527724744611));
#91111=CARTESIAN_POINT('Ctrl Pts',(-5.65173396439855,5.71782566101826,9.47980816220062));
#91112=CARTESIAN_POINT('Ctrl Pts',(-5.64844008976599,5.7292244976931,9.43326698380916));
#91113=CARTESIAN_POINT('Ctrl Pts',(-5.64659978410896,5.73559308968772,9.40726417452436));
#91114=CARTESIAN_POINT('Ctrl Pts',(-5.64425566453173,5.74370160503312,9.38168922134076));
#91115=CARTESIAN_POINT('Ctrl Pts',(-5.6414192185381,5.75350649531546,9.35671706581409));
#91116=CARTESIAN_POINT('Ctrl Pts',(-5.63717068251911,5.76819263057784,9.31931282738848));
#91117=CARTESIAN_POINT('Ctrl Pts',(-5.63186786836281,5.78651310378534,9.28369622395));
#91118=CARTESIAN_POINT('Ctrl Pts',(-5.62561273253842,5.80807427644406,9.2503331992072));
#91119=CARTESIAN_POINT('Ctrl Pts',(-5.61998111348852,5.82748621474438,9.22029582656191));
#91120=CARTESIAN_POINT('Ctrl Pts',(-5.61357756657826,5.84952614262748,9.19208271618801));
#91121=CARTESIAN_POINT('Ctrl Pts',(-5.6064764971916,5.87392073737792,9.16601639098558));
#91122=CARTESIAN_POINT('Ctrl Pts',(-5.59861749266153,5.90091909779573,9.13716786737686));
#91123=CARTESIAN_POINT('Ctrl Pts',(-5.58998168778862,5.93053549676361,9.1112326479035));
#91124=CARTESIAN_POINT('Ctrl Pts',(-5.58070580865448,5.96225420525282,9.08847781685685));
#91125=CARTESIAN_POINT('Ctrl Pts',(-5.57155614999855,5.99354130499686,9.06603261960497));
#91126=CARTESIAN_POINT('Ctrl Pts',(-5.56178371804112,6.02687598894637,9.04667972811));
#91127=CARTESIAN_POINT('Ctrl Pts',(-5.55151973301419,6.06179064324785,9.03066040140691));
#91128=CARTESIAN_POINT('Ctrl Pts',(-5.54013886714958,6.10050455370967,9.01289792338587));
#91129=CARTESIAN_POINT('Ctrl Pts',(-5.52823111361269,6.1408904656362,8.99935811831371));
#91130=CARTESIAN_POINT('Ctrl Pts',(-5.51599488507965,6.18224768010664,8.99019769931973));
#91131=CARTESIAN_POINT('Ctrl Pts',(-5.50371027646635,6.22376841435361,8.98100106150188));
#91132=CARTESIAN_POINT('Ctrl Pts',(-5.49114480790581,6.2660981650747,8.97625599324862));
#91133=CARTESIAN_POINT('Ctrl Pts',(-5.47850707888982,6.30852211597862,8.97601007981572));
#91134=CARTESIAN_POINT('Ctrl Pts',(-5.47816173573398,6.30968140821139,8.97600335989628));
#91135=CARTESIAN_POINT('Ctrl Pts',(-5.47781635774676,6.310840707754,8.976));
#91136=CARTESIAN_POINT('Ctrl Pts',(-5.47747094926116,6.312,8.976));
#91137=CARTESIAN_POINT('Origin',(0.,14.688,9.576));
#91138=CARTESIAN_POINT('',(-8.46817714968195,8.2989750539222,9.57599999941013));
#91139=CARTESIAN_POINT('Origin',(0.,14.688,9.576));
#91140=CARTESIAN_POINT('',(-8.18447918304357,8.16,9.19200000701434));
#91141=CARTESIAN_POINT('Ctrl Pts',(-8.1844791809171,8.16,9.19200000927993));
#91142=CARTESIAN_POINT('Ctrl Pts',(-8.1949045656255,8.16000000015134,9.20178521851308));
#91143=CARTESIAN_POINT('Ctrl Pts',(-8.20514137021707,8.16023917963785,9.21185509928412));
#91144=CARTESIAN_POINT('Ctrl Pts',(-8.26618938143075,8.16340256599659,9.27462639810538));
#91145=CARTESIAN_POINT('Ctrl Pts',(-8.31021435687686,8.1731928977421,9.33158129444371));
#91146=CARTESIAN_POINT('Ctrl Pts',(-8.39504149753827,8.21647648944954,9.45541831434885));
#91147=CARTESIAN_POINT('Ctrl Pts',(-8.43230979342604,8.25143554213401,9.51892473628901));
#91148=CARTESIAN_POINT('Ctrl Pts',(-8.46817715042332,8.29897505490483,9.576));
#91149=CARTESIAN_POINT('',(-7.58586053127791,8.16,8.976));
#91150=CARTESIAN_POINT('Ctrl Pts',(-7.58586053127791,8.16,8.976));
#91151=CARTESIAN_POINT('Ctrl Pts',(-7.69110952727826,8.16,8.976));
#91152=CARTESIAN_POINT('Ctrl Pts',(-7.8158147055935,8.16,8.99600010426086));
#91153=CARTESIAN_POINT('Ctrl Pts',(-8.00027281944003,8.16,9.06175915897253));
#91154=CARTESIAN_POINT('Ctrl Pts',(-8.09540917035175,8.16,9.11433225757306));
#91155=CARTESIAN_POINT('Ctrl Pts',(-8.17079622196017,8.16,9.17943259569684));
#91156=CARTESIAN_POINT('Ctrl Pts',(-8.17765408238493,8.16,9.18559400894369));
#91157=CARTESIAN_POINT('Ctrl Pts',(-8.1844791809171,8.16,9.19200000927993));
#91158=CARTESIAN_POINT('Origin',(0.,14.688,8.976));
#91159=CARTESIAN_POINT('Origin',(0.,14.688,8.976));
#91160=CARTESIAN_POINT('',(-8.976,8.16,8.976));
#91161=CARTESIAN_POINT('Origin',(0.,14.688,9.576));
#91162=CARTESIAN_POINT('',(-10.50240641504,16.1810249473222,9.57599999836851));
#91163=CARTESIAN_POINT('',(-10.3410376317382,16.32,9.19200000000005));
#91164=CARTESIAN_POINT('Ctrl Pts',(-10.5024064150668,16.1810249471335,9.57599999755277));
#91165=CARTESIAN_POINT('Ctrl Pts',(-10.4982985638155,16.209920862045,9.54130797221599));
#91166=CARTESIAN_POINT('Ctrl Pts',(-10.4916339518921,16.2346056625403,9.50370530112817));
#91167=CARTESIAN_POINT('Ctrl Pts',(-10.4665021542091,16.2822987670594,9.40995456416038));
#91168=CARTESIAN_POINT('Ctrl Pts',(-10.4452499964683,16.3001798040925,9.35450358157013));
#91169=CARTESIAN_POINT('Ctrl Pts',(-10.3942868948604,16.3171607866726,9.26213931607076));
#91170=CARTESIAN_POINT('Ctrl Pts',(-10.3694620651598,16.32,9.22570876963314));
#91171=CARTESIAN_POINT('Ctrl Pts',(-10.3410376317382,16.32,9.19200000000005));
#91172=CARTESIAN_POINT('',(-8.976,20.3414138359048,9.576));
#91173=CARTESIAN_POINT('Origin',(0.,14.688,9.576));
#91174=CARTESIAN_POINT('',(-8.976,19.1142272874311,8.976));
#91175=CARTESIAN_POINT('Ctrl Pts',(-8.976,19.1142272874311,8.976));
#91176=CARTESIAN_POINT('Ctrl Pts',(-8.976,19.3123620171841,8.976));
#91177=CARTESIAN_POINT('Ctrl Pts',(-8.976,19.5489440827006,8.9996546128544));
#91178=CARTESIAN_POINT('Ctrl Pts',(-8.976,19.8621493346214,9.08527290977984));
#91179=CARTESIAN_POINT('Ctrl Pts',(-8.976,20.0032332384638,9.14149743330231));
#91180=CARTESIAN_POINT('Ctrl Pts',(-8.976,20.1766041453243,9.25923361702201));
#91181=CARTESIAN_POINT('Ctrl Pts',(-8.976,20.249339321466,9.32728853684005));
#91182=CARTESIAN_POINT('Ctrl Pts',(-8.976,20.3065635015877,9.42543456124496));
#91183=CARTESIAN_POINT('Ctrl Pts',(-8.976,20.3212334425194,9.45910065247902));
#91184=CARTESIAN_POINT('Ctrl Pts',(-8.976,20.3367898671095,9.51531964531999));
#91185=CARTESIAN_POINT('Ctrl Pts',(-8.976,20.3414138359048,9.54827127066274));
#91186=CARTESIAN_POINT('Ctrl Pts',(-8.976,20.3414138359048,9.576));
#91187=CARTESIAN_POINT('',(-9.87403868738623,16.32,8.976));
#91188=CARTESIAN_POINT('Origin',(0.,14.688,8.976));
#91189=CARTESIAN_POINT('Ctrl Pts',(-10.3410376317382,16.32,9.19200000000005));
#91190=CARTESIAN_POINT('Ctrl Pts',(-10.3292581499021,16.32,9.17803061550182));
#91191=CARTESIAN_POINT('Ctrl Pts',(-10.3170794694341,16.32,9.16489488688007));
#91192=CARTESIAN_POINT('Ctrl Pts',(-10.2518064406884,16.32,9.1001029151404));
#91193=CARTESIAN_POINT('Ctrl Pts',(-10.1769613378484,16.32,9.05056345745539));
#91194=CARTESIAN_POINT('Ctrl Pts',(-10.038098637739,16.32,8.99346724198458));
#91195=CARTESIAN_POINT('Ctrl Pts',(-9.94938560299478,16.32,8.976));
#91196=CARTESIAN_POINT('Ctrl Pts',(-9.87403868738623,16.32,8.976));
#91197=CARTESIAN_POINT('Origin',(0.,14.688,8.976));
#91198=CARTESIAN_POINT('',(-8.976,16.32,8.976));
#91199=CARTESIAN_POINT('',(-8.976,8.16,8.976));
#91200=CARTESIAN_POINT('',(-5.406,16.32,8.976));
#91201=CARTESIAN_POINT('Origin',(-9.486,15.72,7.128));
#91202=CARTESIAN_POINT('',(-8.976,16.32,7.128));
#91203=CARTESIAN_POINT('',(-8.976,15.72,6.528));
#91204=CARTESIAN_POINT('Origin',(-8.976,15.72,7.128));
#91205=CARTESIAN_POINT('',(-13.464,15.72,6.528));
#91206=CARTESIAN_POINT('',(-9.486,15.72,6.528));
#91207=CARTESIAN_POINT('',(-13.464,16.32,7.128));
#91208=CARTESIAN_POINT('Origin',(-13.464,15.72,7.128));
#91209=CARTESIAN_POINT('',(-9.486,16.32,7.128));
#91210=CARTESIAN_POINT('Origin',(-8.16,8.16,6.528));
#91211=CARTESIAN_POINT('',(-8.976,8.76,6.528));
#91212=CARTESIAN_POINT('',(-8.976,8.16,6.528));
#91213=CARTESIAN_POINT('',(-13.464,8.76,6.528));
#91214=CARTESIAN_POINT('',(-4.08,8.76,6.528));
#91215=CARTESIAN_POINT('',(-13.464,7.752,6.528));
#91216=CARTESIAN_POINT('Origin',(-4.08,8.76,7.128));
#91217=CARTESIAN_POINT('',(-8.376,8.16,7.128));
#91218=CARTESIAN_POINT('Origin',(-8.376,8.76,7.128));
#91219=CARTESIAN_POINT('',(-13.464,8.16,7.128));
#91220=CARTESIAN_POINT('',(-4.08,8.16,7.128));
#91221=CARTESIAN_POINT('Origin',(-13.464,8.76,7.128));
#91222=CARTESIAN_POINT('Origin',(0.,8.16,-8.16));
#91223=CARTESIAN_POINT('',(-8.376,8.16,-10.7469750549048));
#91224=CARTESIAN_POINT('',(-8.376,8.16,-12.24));
#91225=CARTESIAN_POINT('',(-8.16,8.16,-11.208));
#91226=CARTESIAN_POINT('Origin',(-8.76,8.16,-11.208));
#91227=CARTESIAN_POINT('',(-8.16,8.16,-13.272));
#91228=CARTESIAN_POINT('',(-8.16,8.16,-9.384));
#91229=CARTESIAN_POINT('',(-8.376,8.16,-13.7330249450952));
#91230=CARTESIAN_POINT('Origin',(-8.76,8.16,-13.272));
#91231=CARTESIAN_POINT('',(-8.376,8.16,-16.32));
#91232=CARTESIAN_POINT('',(-8.376,8.16,-12.24));
#91233=CARTESIAN_POINT('',(8.376,8.16,-16.32));
#91234=CARTESIAN_POINT('Origin',(0.,8.16,-16.32));
#91235=CARTESIAN_POINT('',(8.376,8.16,-13.7330249450952));
#91236=CARTESIAN_POINT('',(8.376,8.16,0.408000000000001));
#91237=CARTESIAN_POINT('',(8.16,8.16,-13.272));
#91238=CARTESIAN_POINT('Origin',(8.76,8.16,-13.272));
#91239=CARTESIAN_POINT('',(8.16,8.16,-11.208));
#91240=CARTESIAN_POINT('',(8.16,8.16,-11.016));
#91241=CARTESIAN_POINT('',(8.376,8.16,-10.7469750549048));
#91242=CARTESIAN_POINT('Origin',(8.76,8.16,-11.208));
#91243=CARTESIAN_POINT('',(8.376,8.16,7.128));
#91244=CARTESIAN_POINT('',(8.376,8.16,0.408000000000001));
#91245=CARTESIAN_POINT('',(13.464,8.16,7.128));
#91246=CARTESIAN_POINT('',(6.732,8.16,7.128));
#91247=CARTESIAN_POINT('',(13.464,8.16,9.192));
#91248=CARTESIAN_POINT('',(13.464,8.16,6.528));
#91249=CARTESIAN_POINT('',(4.08,8.16,9.192));
#91250=CARTESIAN_POINT('',(-13.464,8.16,9.192));
#91251=CARTESIAN_POINT('',(-7.752,8.16,9.192));
#91252=CARTESIAN_POINT('',(-13.464,8.16,8.976));
#91253=CARTESIAN_POINT('Origin',(8.376,8.76,0.408000000000001));
#91254=CARTESIAN_POINT('',(8.76,8.29897505490484,-10.608));
#91255=CARTESIAN_POINT('Ctrl Pts',(8.76,8.29897505490484,-10.608));
#91256=CARTESIAN_POINT('Ctrl Pts',(8.74559886385357,8.28697996366506,-10.608));
#91257=CARTESIAN_POINT('Ctrl Pts',(8.73070136992335,8.27571625725086,-10.6085196615488));
#91258=CARTESIAN_POINT('Ctrl Pts',(8.67676732474104,8.23871780749174,-10.6125388608906));
#91259=CARTESIAN_POINT('Ctrl Pts',(8.63186213304349,8.21512617965098,-10.6199246683574));
#91260=CARTESIAN_POINT('Ctrl Pts',(8.54101113694863,8.18110084923513,-10.6473790996848));
#91261=CARTESIAN_POINT('Ctrl Pts',(8.495153215849,8.1705557020042,-10.6676000307859));
#91262=CARTESIAN_POINT('Ctrl Pts',(8.42740104856703,8.16155857905989,-10.7075963115084));
#91263=CARTESIAN_POINT('Ctrl Pts',(8.40091268315884,8.16,-10.726224615184));
#91264=CARTESIAN_POINT('Ctrl Pts',(8.37600000000002,8.16,-10.7469750549048));
#91265=CARTESIAN_POINT('',(8.976,8.76,-10.608));
#91266=CARTESIAN_POINT('Origin',(8.376,8.76,-10.608));
#91267=CARTESIAN_POINT('',(8.976,8.76,6.528));
#91268=CARTESIAN_POINT('',(8.976,8.76,0.408000000000001));
#91269=CARTESIAN_POINT('Origin',(8.376,8.76,7.128));
#91270=CARTESIAN_POINT('Origin',(6.732,8.76,7.128));
#91271=CARTESIAN_POINT('',(13.464,8.76,6.528));
#91272=CARTESIAN_POINT('',(6.732,8.76,6.528));
#91273=CARTESIAN_POINT('Origin',(13.464,8.76,7.128));
#91274=CARTESIAN_POINT('Origin',(29.184,12.9636733990013,2.14076058017042));
#91275=CARTESIAN_POINT('',(29.7833084014095,14.3409676242539,0.0947520315295645));
#91276=CARTESIAN_POINT('',(29.7833084014095,8.04157168141595,9.22080000000005));
#91277=CARTESIAN_POINT('',(29.7833084014095,12.9399716334749,2.12440006945309));
#91278=CARTESIAN_POINT('',(29.7786415493758,7.944,9.27200892297725));
#91279=CARTESIAN_POINT('Origin',(29.184,8.0964461888534,9.192));
#91280=CARTESIAN_POINT('',(29.7684724489276,7.85881694748949,9.29752631904628));
#91281=CARTESIAN_POINT('Ctrl Pts',(29.7786415493758,7.944,9.27200892297725));
#91282=CARTESIAN_POINT('Ctrl Pts',(29.7773539804922,7.92576669289312,9.28157838007491));
#91283=CARTESIAN_POINT('Ctrl Pts',(29.7753882078911,7.90558549327391,9.28823908356366));
#91284=CARTESIAN_POINT('Ctrl Pts',(29.7712795144075,7.87601848599256,9.29474689974779));
#91285=CARTESIAN_POINT('Ctrl Pts',(29.7699574919428,7.86745703528122,9.29627565780888));
#91286=CARTESIAN_POINT('Ctrl Pts',(29.7684724489276,7.85881694748801,9.29752631903611));
#91287=CARTESIAN_POINT('',(29.184,8.3232,7.80729593694088));
#91288=CARTESIAN_POINT('Origin',(29.184,7.7232,9.73272845308249));
#91289=CARTESIAN_POINT('',(29.184,13.9939352485079,-0.408));
#91290=CARTESIAN_POINT('',(29.184,12.4698866172014,1.79991660689266));
#91291=CARTESIAN_POINT('',(29.184,14.6544658518362,-1.36492254071927));
#91292=CARTESIAN_POINT('Ctrl Pts',(29.184,14.6544658518362,-1.36492254071922));
#91293=CARTESIAN_POINT('Ctrl Pts',(29.1975798724823,14.6506113776277,-1.35933849475044));
#91294=CARTESIAN_POINT('Ctrl Pts',(29.210686992401,14.6467933040737,-1.35299257799626));
#91295=CARTESIAN_POINT('Ctrl Pts',(29.2845418076992,14.6246038654931,-1.31233545441248));
#91296=CARTESIAN_POINT('Ctrl Pts',(29.3450946879031,14.6026441192603,-1.25400741265493));
#91297=CARTESIAN_POINT('Ctrl Pts',(29.4303036451774,14.5605239942317,-1.1392095265953));
#91298=CARTESIAN_POINT('Ctrl Pts',(29.4669570195186,14.5351279130215,-1.06861054279322));
#91299=CARTESIAN_POINT('Ctrl Pts',(29.5168097217215,14.4724115251156,-0.925286302443268));
#91300=CARTESIAN_POINT('Ctrl Pts',(29.5300379575436,14.4344630406425,-0.852846813728985));
#91301=CARTESIAN_POINT('Ctrl Pts',(29.5300379575436,14.3909332450409,-0.789784417536817));
#91302=CARTESIAN_POINT('Ctrl Pts',(29.5300379575436,14.3517774897719,-0.733058772083134));
#91303=CARTESIAN_POINT('Ctrl Pts',(29.5188800554652,14.3030632457182,-0.677492662862742));
#91304=CARTESIAN_POINT('Ctrl Pts',(29.4694940045382,14.2020866968451,-0.583709983027462));
#91305=CARTESIAN_POINT('Ctrl Pts',(29.4311957085096,14.1505667362922,-0.544734083228222));
#91306=CARTESIAN_POINT('Ctrl Pts',(29.3431197137225,14.0686594841341,-0.481660747664236));
#91307=CARTESIAN_POINT('Ctrl Pts',(29.2811054870975,14.0289285262802,-0.449765893805952));
#91308=CARTESIAN_POINT('Ctrl Pts',(29.2105917253688,14.0021338893618,-0.419073891481067));
#91309=CARTESIAN_POINT('Ctrl Pts',(29.1974888758462,13.9977638944778,-0.413546628135857));
#91310=CARTESIAN_POINT('Ctrl Pts',(29.184,13.9939352485079,-0.407999999999951));
#91311=CARTESIAN_POINT('',(29.184,20.3587352485079,-9.6288));
#91312=CARTESIAN_POINT('',(29.184,12.4698866172014,1.79991660689266));
#91313=CARTESIAN_POINT('',(29.7835166971462,21.456077579674,-10.204722420326));
#91314=CARTESIAN_POINT('Origin',(29.184,21.5019541534552,-10.2288));
#91315=CARTESIAN_POINT('',(29.784,21.432,-10.1274561623021));
#91316=CARTESIAN_POINT('Origin',(29.184,21.432,-10.1274561623021));
#91317=CARTESIAN_POINT('',(29.784,21.0528,-9.57810231614827));
#91318=CARTESIAN_POINT('',(29.784,12.9636733990013,2.14076058017042));
#91319=CARTESIAN_POINT('',(29.7833084014095,21.0528,-9.62879999999999));
#91320=CARTESIAN_POINT('Origin',(29.184,21.0528,-9.57810231614827));
#91321=CARTESIAN_POINT('',(29.7833084014095,14.688,-0.408000000000001));
#91322=CARTESIAN_POINT('',(29.7833084014095,12.9399716334749,2.12440006945309));
#91323=CARTESIAN_POINT('',(29.784,14.688,-0.357302316148278));
#91324=CARTESIAN_POINT('Origin',(29.184,14.688,-0.357302316148276));
#91325=CARTESIAN_POINT('',(29.784,14.3584650549638,0.120100873455422));
#91326=CARTESIAN_POINT('',(29.784,12.9636733990013,2.14076058017042));
#91327=CARTESIAN_POINT('Origin',(29.184,14.3584650549638,0.120100873455422));
#91328=CARTESIAN_POINT('Origin',(29.784,8.3232,7.80729593694088));
#91329=CARTESIAN_POINT('',(28.968,8.3232,7.80729593694088));
#91330=CARTESIAN_POINT('',(29.784,8.3232,7.80729593694088));
#91331=CARTESIAN_POINT('',(28.968,13.9939352485079,-0.408));
#91332=CARTESIAN_POINT('',(28.968,13.9939352485079,-0.408));
#91333=CARTESIAN_POINT('',(29.784,13.9939352485079,-0.408));
#91334=CARTESIAN_POINT('Origin',(29.784,8.3232,7.80729593694088));
#91335=CARTESIAN_POINT('',(28.968,14.688,-1.41350406305912));
#91336=CARTESIAN_POINT('Origin',(28.9300379575436,14.324200550172,-0.886461270359634));
#91337=CARTESIAN_POINT('',(28.968,20.3587352485079,-9.6288));
#91338=CARTESIAN_POINT('',(28.968,20.3587352485079,-9.6288));
#91339=CARTESIAN_POINT('',(29.784,20.3587352485079,-9.6288));
#91340=CARTESIAN_POINT('Origin',(29.784,7.344,-10.608));
#91341=CARTESIAN_POINT('',(29.784,18.9366533000554,5.79779797752167));
#91342=CARTESIAN_POINT('',(29.784,11.2069968487015,-5.40029406097811));
#91343=CARTESIAN_POINT('',(29.784,18.7060084170374,6.41846497492097));
#91344=CARTESIAN_POINT('Origin',(29.784,19.9512,6.528));
#91345=CARTESIAN_POINT('',(29.784,13.7190338627358,-0.806254571695441));
#91346=CARTESIAN_POINT('Origin',(29.784,7.344,-10.608));
#91347=CARTESIAN_POINT('',(29.784,21.432,9.192));
#91348=CARTESIAN_POINT('',(29.784,21.432,-9.384));
#91349=CARTESIAN_POINT('',(29.784,21.3495435339861,9.192));
#91350=CARTESIAN_POINT('',(29.784,7.344,9.192));
#91351=CARTESIAN_POINT('',(29.784,20.3324059608682,7.71845454150864));
#91352=CARTESIAN_POINT('',(29.784,14.2128206445356,-1.1470985449732));
#91353=CARTESIAN_POINT('',(29.784,20.8019222240139,7.44384479993543));
#91354=CARTESIAN_POINT('Origin',(29.784,19.9512,6.528));
#91355=CARTESIAN_POINT('',(29.784,21.0528,7.80729593694088));
#91356=CARTESIAN_POINT('',(29.784,11.7007836305014,-5.74113803425587));
#91357=CARTESIAN_POINT('',(29.784,21.0528,7.11874312522449));
#91358=CARTESIAN_POINT('',(29.784,21.0528,-1.40035203152956));
#91359=CARTESIAN_POINT('',(29.784,21.0528,5.93725687477551));
#91360=CARTESIAN_POINT('Origin',(29.784,19.9512,6.528));
#91361=CARTESIAN_POINT('',(29.784,21.0528,-1.40035203152956));
#91362=CARTESIAN_POINT('Origin',(29.784,7.344,-10.608));
#91363=CARTESIAN_POINT('',(29.784,21.432,-10.2288));
#91364=CARTESIAN_POINT('',(29.784,7.94403556938437,-10.2288));
#91365=CARTESIAN_POINT('',(29.784,13.8513676242539,-10.2288));
#91366=CARTESIAN_POINT('',(29.784,7.944,-10.2288515300056));
#91367=CARTESIAN_POINT('',(29.784,11.0304206445356,-5.7574985449732));
#91368=CARTESIAN_POINT('',(29.784,7.944,-13.272));
#91369=CARTESIAN_POINT('',(29.784,7.944,-11.424));
#91370=CARTESIAN_POINT('',(29.784,21.432,-13.272));
#91371=CARTESIAN_POINT('',(29.784,7.344,-13.272));
#91372=CARTESIAN_POINT('',(29.784,21.432,-9.384));
#91373=CARTESIAN_POINT('Origin',(29.184,7.944,-11.424));
#91374=CARTESIAN_POINT('',(29.7737557460509,7.83359999999999,-10.1944488701125));
#91375=CARTESIAN_POINT('',(29.7737557460508,7.83359999999999,9.192));
#91376=CARTESIAN_POINT('',(29.7737557460508,7.83359999999999,-11.424));
#91377=CARTESIAN_POINT('',(29.184,7.344,9.192));
#91378=CARTESIAN_POINT('Origin',(29.184,7.944,9.192));
#91379=CARTESIAN_POINT('',(29.184,7.344,-13.272));
#91380=CARTESIAN_POINT('',(29.184,7.344,-11.424));
#91381=CARTESIAN_POINT('Origin',(29.184,7.944,-13.272));
#91382=CARTESIAN_POINT('Origin',(29.184,7.944,-10.2288515300056));
#91383=CARTESIAN_POINT('Origin',(29.184,7.944,9.192));
#91384=CARTESIAN_POINT('Ctrl Pts',(29.768472448926,7.85881694748961,9.29752631904605));
#91385=CARTESIAN_POINT('Ctrl Pts',(29.7694086634445,7.85478211554245,9.28908396170822));
#91386=CARTESIAN_POINT('Ctrl Pts',(29.7702047557464,7.85115959495503,9.28049359804113));
#91387=CARTESIAN_POINT('Ctrl Pts',(29.7728449807647,7.83875603249717,9.24614397494659));
#91388=CARTESIAN_POINT('Ctrl Pts',(29.7737557460509,7.8336,9.21936998988089));
#91389=CARTESIAN_POINT('Ctrl Pts',(29.7737557460509,7.8336,9.192));
#91390=CARTESIAN_POINT('',(29.184,7.944,9.792));
#91391=CARTESIAN_POINT('Origin',(29.184,7.944,9.192));
#91392=CARTESIAN_POINT('Origin',(29.184,7.944,9.192));
#91393=CARTESIAN_POINT('Origin',(29.184,7.344,9.192));
#91394=CARTESIAN_POINT('',(29.7737557460508,8.08439812505511,9.30240000000001));
#91395=CARTESIAN_POINT('Origin',(29.184,8.02645646601385,9.192));
#91396=CARTESIAN_POINT('',(29.7737557460509,21.2916018749449,9.30240000000001));
#91397=CARTESIAN_POINT('',(29.7737557460508,7.344,9.30240000000001));
#91398=CARTESIAN_POINT('Origin',(29.184,21.3495435339861,9.192));
#91399=CARTESIAN_POINT('',(29.184,21.432,9.792));
#91400=CARTESIAN_POINT('Origin',(29.184,21.432,9.192));
#91401=CARTESIAN_POINT('',(29.184,7.344,9.792));
#91402=CARTESIAN_POINT('Origin',(8.76,7.344,-11.208));
#91403=CARTESIAN_POINT('',(8.16,7.944,-11.208));
#91404=CARTESIAN_POINT('',(8.76,7.944,-10.608));
#91405=CARTESIAN_POINT('Origin',(8.76,7.944,-11.208));
#91406=CARTESIAN_POINT('',(8.76,7.344,-10.608));
#91407=CARTESIAN_POINT('',(8.16,7.344,-11.208));
#91408=CARTESIAN_POINT('Origin',(8.76,7.944,-13.056));
#91409=CARTESIAN_POINT('',(8.76,7.344,-11.208));
#91410=CARTESIAN_POINT('Origin',(8.76,7.944,-11.208));
#91411=CARTESIAN_POINT('',(8.16,7.944,-13.272));
#91412=CARTESIAN_POINT('',(8.16,7.944,-13.056));
#91413=CARTESIAN_POINT('',(8.76,7.344,-13.272));
#91414=CARTESIAN_POINT('Origin',(8.76,7.944,-13.272));
#91415=CARTESIAN_POINT('',(8.76,7.344,-13.056));
#91416=CARTESIAN_POINT('Origin',(8.76,7.344,-13.272));
#91417=CARTESIAN_POINT('',(8.76,8.29897505490484,-13.872));
#91418=CARTESIAN_POINT('Ctrl Pts',(8.76,8.29897505490484,-13.872));
#91419=CARTESIAN_POINT('Ctrl Pts',(8.73508731684117,8.27822461518402,-13.872));
#91420=CARTESIAN_POINT('Ctrl Pts',(8.70859895143297,8.25959631150844,-13.8704414209401));
#91421=CARTESIAN_POINT('Ctrl Pts',(8.640846784151,8.21960003078587,-13.8614442979958));
#91422=CARTESIAN_POINT('Ctrl Pts',(8.59498886305137,8.19937909968476,-13.8508991507649));
#91423=CARTESIAN_POINT('Ctrl Pts',(8.5041378669565,8.17192466835744,-13.816873820349));
#91424=CARTESIAN_POINT('Ctrl Pts',(8.45923267525896,8.16453886089061,-13.7932821925083));
#91425=CARTESIAN_POINT('Ctrl Pts',(8.40529863007666,8.16051966154879,-13.7562837427492));
#91426=CARTESIAN_POINT('Ctrl Pts',(8.39040113614645,8.16,-13.745020036335));
#91427=CARTESIAN_POINT('Ctrl Pts',(8.37600000000002,8.16,-13.7330249450952));
#91428=CARTESIAN_POINT('',(8.76,7.944,-13.872));
#91429=CARTESIAN_POINT('',(8.76,7.344,-13.872));
#91430=CARTESIAN_POINT('Origin',(8.76,7.944,-13.272));
#91431=CARTESIAN_POINT('',(8.16,7.344,-13.272));
#91432=CARTESIAN_POINT('Origin',(8.76,7.944,-13.272));
#91433=CARTESIAN_POINT('Origin',(8.76,7.944,-13.272));
#91434=CARTESIAN_POINT('Origin',(8.76,7.944,-11.208));
#91435=CARTESIAN_POINT('Origin',(8.76,7.944,-11.208));
#91436=CARTESIAN_POINT('Origin',(8.16,7.344,-10.608));
#91437=CARTESIAN_POINT('',(13.464,7.944,-10.608));
#91438=CARTESIAN_POINT('',(13.566,7.944,-10.608));
#91439=CARTESIAN_POINT('',(13.464,21.432,-10.608));
#91440=CARTESIAN_POINT('',(13.464,7.344,-10.608));
#91441=CARTESIAN_POINT('',(8.976,21.432,-10.608));
#91442=CARTESIAN_POINT('',(4.08,21.432,-10.608));
#91443=CARTESIAN_POINT('',(8.976,7.752,-10.608));
#91444=CARTESIAN_POINT('Origin',(13.566,7.944,-11.208));
#91445=CARTESIAN_POINT('',(14.064,7.344,-11.208));
#91446=CARTESIAN_POINT('',(13.566,7.344,-11.208));
#91447=CARTESIAN_POINT('Origin',(14.064,7.944,-11.208));
#91448=CARTESIAN_POINT('Origin',(18.972,7.344,-12.24));
#91449=CARTESIAN_POINT('',(24.378,7.344,-13.272));
#91450=CARTESIAN_POINT('',(27.528,7.344,9.192));
#91451=CARTESIAN_POINT('',(22.95,7.344,9.192));
#91452=CARTESIAN_POINT('',(27.528,7.344,-11.208));
#91453=CARTESIAN_POINT('',(27.528,7.344,-11.424));
#91454=CARTESIAN_POINT('',(14.904,7.344,-11.208));
#91455=CARTESIAN_POINT('',(13.566,7.344,-11.208));
#91456=CARTESIAN_POINT('',(14.904,7.344,9.192));
#91457=CARTESIAN_POINT('',(14.904,7.344,-1.224));
#91458=CARTESIAN_POINT('',(14.064,7.344,9.192));
#91459=CARTESIAN_POINT('',(13.566,7.344,9.192));
#91460=CARTESIAN_POINT('',(14.064,7.344,-11.424));
#91461=CARTESIAN_POINT('Origin',(24.378,7.944,-13.272));
#91462=CARTESIAN_POINT('',(29.184,7.944,-13.872));
#91463=CARTESIAN_POINT('',(24.378,7.944,-13.872));
#91464=CARTESIAN_POINT('Origin',(29.184,7.944,-13.272));
#91465=CARTESIAN_POINT('Origin',(29.784,7.344,-13.872));
#91466=CARTESIAN_POINT('',(8.976,8.76,-13.872));
#91467=CARTESIAN_POINT('Origin',(8.376,8.76,-13.872));
#91468=CARTESIAN_POINT('',(8.976,21.432,-13.872));
#91469=CARTESIAN_POINT('',(8.976,7.752,-13.872));
#91470=CARTESIAN_POINT('',(29.184,21.432,-13.872));
#91471=CARTESIAN_POINT('',(14.892,21.432,-13.872));
#91472=CARTESIAN_POINT('',(29.184,7.344,-13.872));
#91473=CARTESIAN_POINT('Origin',(0.,8.76,-16.32));
#91474=CARTESIAN_POINT('',(8.976,8.76,-16.32));
#91475=CARTESIAN_POINT('Origin',(8.376,8.76,-16.32));
#91476=CARTESIAN_POINT('',(-8.976,8.76,-16.32));
#91477=CARTESIAN_POINT('Origin',(-8.376,8.76,-16.32));
#91478=CARTESIAN_POINT('Origin',(0.,8.76,-16.32));
#91479=CARTESIAN_POINT('Origin',(-8.376,8.76,-12.24));
#91480=CARTESIAN_POINT('',(-8.76,8.29897505490484,-13.872));
#91481=CARTESIAN_POINT('',(-8.976,8.76,-13.872));
#91482=CARTESIAN_POINT('Origin',(-8.376,8.76,-13.872));
#91483=CARTESIAN_POINT('',(-8.976,8.76,-12.24));
#91484=CARTESIAN_POINT('Ctrl Pts',(-8.76,8.29897505490484,-13.872));
#91485=CARTESIAN_POINT('Ctrl Pts',(-8.74559886385357,8.28697996366506,-13.872));
#91486=CARTESIAN_POINT('Ctrl Pts',(-8.73070136992335,8.27571625725086,-13.8714803384512));
#91487=CARTESIAN_POINT('Ctrl Pts',(-8.67676732474104,8.23871780749174,-13.8674611391094));
#91488=CARTESIAN_POINT('Ctrl Pts',(-8.63186213304349,8.21512617965098,-13.8600753316426));
#91489=CARTESIAN_POINT('Ctrl Pts',(-8.54101113694863,8.18110084923513,-13.8326209003152));
#91490=CARTESIAN_POINT('Ctrl Pts',(-8.495153215849,8.1705557020042,-13.8123999692141));
#91491=CARTESIAN_POINT('Ctrl Pts',(-8.42740104856703,8.16155857905989,-13.7724036884916));
#91492=CARTESIAN_POINT('Ctrl Pts',(-8.40091268315884,8.16,-13.753775384816));
#91493=CARTESIAN_POINT('Ctrl Pts',(-8.37600000000002,8.16,-13.7330249450952));
#91494=CARTESIAN_POINT('Origin',(8.376,8.76,0.408000000000001));
#91495=CARTESIAN_POINT('',(8.976,8.76,0.408000000000001));
#91496=CARTESIAN_POINT('Origin',(-8.976,8.16,-16.32));
#91497=CARTESIAN_POINT('',(-8.976,21.432,-13.872));
#91498=CARTESIAN_POINT('',(-8.976,7.752,-13.872));
#91499=CARTESIAN_POINT('',(-8.976,22.032,-13.272));
#91500=CARTESIAN_POINT('Origin',(-8.976,21.432,-13.272));
#91501=CARTESIAN_POINT('',(-8.976,22.032,-16.32));
#91502=CARTESIAN_POINT('',(-8.976,22.032,-16.32));
#91503=CARTESIAN_POINT('',(-8.976,8.16,-16.32));
#91504=CARTESIAN_POINT('Origin',(0.,14.688,10.008));
#91505=CARTESIAN_POINT('',(-5.47747094926117,6.312,10.608));
#91506=CARTESIAN_POINT('',(5.47747094926117,6.312,10.608));
#91507=CARTESIAN_POINT('Origin',(0.,14.688,10.608));
#91508=CARTESIAN_POINT('',(5.65341383590482,5.712,10.008));
#91509=CARTESIAN_POINT('Ctrl Pts',(5.47747094926117,6.312,10.608));
#91510=CARTESIAN_POINT('Ctrl Pts',(5.47781635774676,6.31084070775401,10.608));
#91511=CARTESIAN_POINT('Ctrl Pts',(5.47816173573397,6.30968140821139,10.6079966401037));
#91512=CARTESIAN_POINT('Ctrl Pts',(5.4785070788898,6.30852211597863,10.6079899201843));
#91513=CARTESIAN_POINT('Ctrl Pts',(5.49114480790582,6.26609816507474,10.6077440067514));
#91514=CARTESIAN_POINT('Ctrl Pts',(5.50371027646633,6.22376841435361,10.6029989384981));
#91515=CARTESIAN_POINT('Ctrl Pts',(5.51599488507963,6.18224768010663,10.5938023006803));
#91516=CARTESIAN_POINT('Ctrl Pts',(5.52823111361268,6.14089046563618,10.5846418816863));
#91517=CARTESIAN_POINT('Ctrl Pts',(5.54013886714959,6.10050455370965,10.5711020766141));
#91518=CARTESIAN_POINT('Ctrl Pts',(5.55151973301418,6.06179064324784,10.5533395985931));
#91519=CARTESIAN_POINT('Ctrl Pts',(5.56320230330928,6.02205043492371,10.5351062409062));
#91520=CARTESIAN_POINT('Ctrl Pts',(5.57424805579781,5.98435659900368,10.5125540425903));
#91521=CARTESIAN_POINT('Ctrl Pts',(5.58446349626691,5.94940030608872,10.4860391845607));
#91522=CARTESIAN_POINT('Ctrl Pts',(5.592321877119,5.92250965328389,10.4656422321956));
#91523=CARTESIAN_POINT('Ctrl Pts',(5.59968890535143,5.89723842986285,10.4428992332132));
#91524=CARTESIAN_POINT('Ctrl Pts',(5.6064764971916,5.87392073737792,10.4179836090144));
#91525=CARTESIAN_POINT('Ctrl Pts',(5.61530694331658,5.84358514382786,10.385569155945));
#91526=CARTESIAN_POINT('Ctrl Pts',(5.62305875077558,5.81689014477726,10.3498344468399));
#91527=CARTESIAN_POINT('Ctrl Pts',(5.62958883887762,5.79436341720472,10.3114013318231));
#91528=CARTESIAN_POINT('Ctrl Pts',(5.63414258927943,5.77865442627962,10.2846000375349));
#91529=CARTESIAN_POINT('Ctrl Pts',(5.63810222290114,5.76497252652513,10.256485863173));
#91530=CARTESIAN_POINT('Ctrl Pts',(5.6414192185381,5.75350649531545,10.2272829341859));
#91531=CARTESIAN_POINT('Ctrl Pts',(5.6473255065113,5.73308992271604,10.1752837978781));
#91532=CARTESIAN_POINT('Ctrl Pts',(5.65109711175118,5.72002855160651,10.1206710696132));
#91533=CARTESIAN_POINT('Ctrl Pts',(5.65263031820826,5.71471580384279,10.0650227061865));
#91534=CARTESIAN_POINT('Ctrl Pts',(5.65315130687732,5.71291051442879,10.0461132066454));
#91535=CARTESIAN_POINT('Ctrl Pts',(5.65341383590482,5.712,10.0270842550942));
#91536=CARTESIAN_POINT('Ctrl Pts',(5.65341383590482,5.712,10.008));
#91537=CARTESIAN_POINT('',(-5.65341383590482,5.712,10.008));
#91538=CARTESIAN_POINT('Origin',(0.,14.688,10.008));
#91539=CARTESIAN_POINT('Ctrl Pts',(-5.47747094926117,6.312,10.608));
#91540=CARTESIAN_POINT('Ctrl Pts',(-5.47781635774676,6.31084070775401,10.608));
#91541=CARTESIAN_POINT('Ctrl Pts',(-5.47816173573397,6.30968140821138,10.6079966401037));
#91542=CARTESIAN_POINT('Ctrl Pts',(-5.4785070788898,6.30852211597862,10.6079899201843));
#91543=CARTESIAN_POINT('Ctrl Pts',(-5.49114480790583,6.26609816507479,10.6077440067514));
#91544=CARTESIAN_POINT('Ctrl Pts',(-5.50371027646632,6.22376841435361,10.6029989384981));
#91545=CARTESIAN_POINT('Ctrl Pts',(-5.51599488507963,6.18224768010662,10.5938023006803));
#91546=CARTESIAN_POINT('Ctrl Pts',(-5.52823111361268,6.14089046563617,10.5846418816863));
#91547=CARTESIAN_POINT('Ctrl Pts',(-5.54013886714959,6.10050455370965,10.5711020766141));
#91548=CARTESIAN_POINT('Ctrl Pts',(-5.55151973301419,6.06179064324784,10.5533395985931));
#91549=CARTESIAN_POINT('Ctrl Pts',(-5.56320230330927,6.02205043492372,10.5351062409062));
#91550=CARTESIAN_POINT('Ctrl Pts',(-5.5742480557978,5.98435659900372,10.5125540425904));
#91551=CARTESIAN_POINT('Ctrl Pts',(-5.5844634962669,5.94940030608877,10.4860391845607));
#91552=CARTESIAN_POINT('Ctrl Pts',(-5.592321877119,5.92250965328393,10.4656422321957));
#91553=CARTESIAN_POINT('Ctrl Pts',(-5.59968890535143,5.89723842986286,10.4428992332132));
#91554=CARTESIAN_POINT('Ctrl Pts',(-5.6064764971916,5.87392073737792,10.4179836090144));
#91555=CARTESIAN_POINT('Ctrl Pts',(-5.61530694331635,5.84358514382866,10.3855691559459));
#91556=CARTESIAN_POINT('Ctrl Pts',(-5.62305875077517,5.81689014477869,10.3498344468418));
#91557=CARTESIAN_POINT('Ctrl Pts',(-5.6295888388771,5.79436341720653,10.3114013318262));
#91558=CARTESIAN_POINT('Ctrl Pts',(-5.63414258927913,5.77865442628068,10.284600037537));
#91559=CARTESIAN_POINT('Ctrl Pts',(-5.63810222290101,5.76497252652559,10.2564858631742));
#91560=CARTESIAN_POINT('Ctrl Pts',(-5.6414192185381,5.75350649531547,10.2272829341859));
#91561=CARTESIAN_POINT('Ctrl Pts',(-5.64732550651149,5.73308992271537,10.1752837978765));
#91562=CARTESIAN_POINT('Ctrl Pts',(-5.65109711175142,5.72002855160565,10.1206710696096));
#91563=CARTESIAN_POINT('Ctrl Pts',(-5.6526303182084,5.71471580384227,10.065022706181));
#91564=CARTESIAN_POINT('Ctrl Pts',(-5.65315130687736,5.71291051442862,10.0461132066417));
#91565=CARTESIAN_POINT('Ctrl Pts',(-5.65341383590481,5.712,10.0270842550924));
#91566=CARTESIAN_POINT('Ctrl Pts',(-5.65341383590481,5.712,10.008));
#91567=CARTESIAN_POINT('Origin',(8.16,6.312,10.008));
#91568=CARTESIAN_POINT('',(8.16,5.712,10.008));
#91569=CARTESIAN_POINT('',(8.16,6.312,10.608));
#91570=CARTESIAN_POINT('Origin',(0.,14.688,8.976));
#91571=CARTESIAN_POINT('',(-7.65475852003184,22.032,8.976));
#91572=CARTESIAN_POINT('',(-7.65475852003184,22.032,8.976));
#91573=CARTESIAN_POINT('',(-8.976,20.3414138359048,8.976));
#91574=CARTESIAN_POINT('Origin',(0.,14.688,8.976));
#91575=CARTESIAN_POINT('',(-8.976,20.3414138359048,8.976));
#91576=CARTESIAN_POINT('',(-10.5576815636768,15.72,9.792));
#91577=CARTESIAN_POINT('Ctrl Pts',(-10.5024064151123,16.1810249468138,9.57599999793657));
#91578=CARTESIAN_POINT('Ctrl Pts',(-10.5040548222992,16.1694295329184,9.58992128726773));
#91579=CARTESIAN_POINT('Ctrl Pts',(-10.5057544224536,16.1573351630669,9.60315512266065));
#91580=CARTESIAN_POINT('Ctrl Pts',(-10.5148744531694,16.09155916125,9.66912629289288));
#91581=CARTESIAN_POINT('Ctrl Pts',(-10.5237938127571,16.0240325570758,9.71543522609453));
#91582=CARTESIAN_POINT('Ctrl Pts',(-10.5415281847411,15.8760247207448,9.77687307989452));
#91583=CARTESIAN_POINT('Ctrl Pts',(-10.5502978947739,15.7955372335741,9.792));
#91584=CARTESIAN_POINT('Ctrl Pts',(-10.5576815636768,15.72,9.792));
#91585=CARTESIAN_POINT('',(-8.79707224023993,8.76,9.792));
#91586=CARTESIAN_POINT('Origin',(0.,14.688,9.792));
#91587=CARTESIAN_POINT('Ctrl Pts',(-8.79707224023993,8.76,9.792));
#91588=CARTESIAN_POINT('Ctrl Pts',(-8.74475140209822,8.68235658016152,9.792));
#91589=CARTESIAN_POINT('Ctrl Pts',(-8.68731298961922,8.59955491146768,9.77616481923648));
#91590=CARTESIAN_POINT('Ctrl Pts',(-8.57761412027184,8.44595653818896,9.71004233715158));
#91591=CARTESIAN_POINT('Ctrl Pts',(-8.52538586265315,8.37511979542016,9.65979463855841));
#91592=CARTESIAN_POINT('Ctrl Pts',(-8.47797223677067,8.31197307918123,9.59120848887458));
#91593=CARTESIAN_POINT('Ctrl Pts',(-8.47304047669745,8.3054210319946,9.58373894855639));
#91594=CARTESIAN_POINT('Ctrl Pts',(-8.46817714985943,8.29897505415743,9.57599999910268));
#91595=CARTESIAN_POINT('',(-5.65341383590482,5.712,8.976));
#91596=CARTESIAN_POINT('',(5.65341383590482,5.712,8.976));
#91597=CARTESIAN_POINT('',(8.79707224023993,8.76,9.792));
#91598=CARTESIAN_POINT('Ctrl Pts',(8.46817714985943,8.29897505415743,9.57599999910267));
#91599=CARTESIAN_POINT('Ctrl Pts',(8.47304047669745,8.3054210319946,9.58373894855639));
#91600=CARTESIAN_POINT('Ctrl Pts',(8.47797223677067,8.31197307918123,9.59120848887458));
#91601=CARTESIAN_POINT('Ctrl Pts',(8.52538586265315,8.37511979542016,9.65979463855841));
#91602=CARTESIAN_POINT('Ctrl Pts',(8.57761412027184,8.44595653818896,9.71004233715158));
#91603=CARTESIAN_POINT('Ctrl Pts',(8.68731298961922,8.59955491146768,9.77616481923648));
#91604=CARTESIAN_POINT('Ctrl Pts',(8.74475140209822,8.68235658016152,9.792));
#91605=CARTESIAN_POINT('Ctrl Pts',(8.79707224023993,8.76,9.792));
#91606=CARTESIAN_POINT('',(10.5576815636768,15.72,9.792));
#91607=CARTESIAN_POINT('Origin',(0.,14.688,9.792));
#91608=CARTESIAN_POINT('Ctrl Pts',(10.5576815636768,15.72,9.792));
#91609=CARTESIAN_POINT('Ctrl Pts',(10.5502978947739,15.7955372335741,9.792));
#91610=CARTESIAN_POINT('Ctrl Pts',(10.5415281847411,15.8760247207448,9.77687307989452));
#91611=CARTESIAN_POINT('Ctrl Pts',(10.5237938127571,16.0240325570758,9.71543522609453));
#91612=CARTESIAN_POINT('Ctrl Pts',(10.5148744531694,16.09155916125,9.66912629289288));
#91613=CARTESIAN_POINT('Ctrl Pts',(10.505754422511,16.1573351626526,9.60315512307621));
#91614=CARTESIAN_POINT('Ctrl Pts',(10.5040548224124,16.169429532113,9.58992128814926));
#91615=CARTESIAN_POINT('Ctrl Pts',(10.502406415277,16.1810249456554,9.57599999932742));
#91616=CARTESIAN_POINT('',(8.976,20.3414138359048,8.976));
#91617=CARTESIAN_POINT('',(8.976,20.3414138359048,8.976));
#91618=CARTESIAN_POINT('',(7.65475852003184,22.032,8.976));
#91619=CARTESIAN_POINT('Origin',(0.,14.688,8.976));
#91620=CARTESIAN_POINT('',(7.65475852003184,22.032,8.976));
#91621=CARTESIAN_POINT('Origin',(0.,14.688,10.608));
#91622=CARTESIAN_POINT('',(4.65,14.688,10.608));
#91623=CARTESIAN_POINT('Origin',(0.,14.688,10.608));
#91624=CARTESIAN_POINT('Origin',(0.,14.688,10.008));
#91625=CARTESIAN_POINT('',(4.05,14.688,10.008));
#91626=CARTESIAN_POINT('Origin',(4.65,14.688,10.008));
#91627=CARTESIAN_POINT('',(-4.05,14.688,10.008));
#91628=CARTESIAN_POINT('Origin',(0.,14.688,10.008));
#91629=CARTESIAN_POINT('Origin',(0.,14.688,10.008));
#91630=CARTESIAN_POINT('Origin',(0.,14.688,-28.56));
#91631=CARTESIAN_POINT('',(4.05,14.688,-23.2866976394846));
#91632=CARTESIAN_POINT('',(-4.04973455112235,14.6878444994985,-23.2871855929692));
#91633=CARTESIAN_POINT('Ctrl Pts',(4.05,14.688,-23.2866976394846));
#91634=CARTESIAN_POINT('Ctrl Pts',(4.05,15.3075500635423,-23.2866976394846));
#91635=CARTESIAN_POINT('Ctrl Pts',(3.75477117913856,16.5345337141539,-23.5265143677541));
#91636=CARTESIAN_POINT('Ctrl Pts',(2.62544753954527,17.9400713904106,-24.2003505240322));
#91637=CARTESIAN_POINT('Ctrl Pts',(0.963114040854605,18.771782200002,-24.7161072950123));
#91638=CARTESIAN_POINT('Ctrl Pts',(-0.963758699703665,18.7714859564189,
-24.7169298905911));
#91639=CARTESIAN_POINT('Ctrl Pts',(-2.6247891146146,17.9416552607379,-24.198643675026));
#91640=CARTESIAN_POINT('Ctrl Pts',(-3.62840603788501,16.6894320905695,-23.603545323179));
#91641=CARTESIAN_POINT('Ctrl Pts',(-4.00295463234946,15.5145058470135,-23.3225641391335));
#91642=CARTESIAN_POINT('Ctrl Pts',(-4.04973093528918,14.8944907445965,-23.2872300244039));
#91643=CARTESIAN_POINT('Ctrl Pts',(-4.04973455112235,14.6878444994985,-23.2871855929692));
#91644=CARTESIAN_POINT('Ctrl Pts',(-4.04973455112235,14.6878444994985,-23.2871855929692));
#91645=CARTESIAN_POINT('Ctrl Pts',(-4.04973816739522,14.4811731258246,-23.2871411561315));
#91646=CARTESIAN_POINT('Ctrl Pts',(-4.00297597826243,13.8612353802335,-23.3222143734744));
#91647=CARTESIAN_POINT('Ctrl Pts',(-3.56692412346984,12.4914312155395,-23.6515378504812));
#91648=CARTESIAN_POINT('Ctrl Pts',(-2.45900653907373,11.2979783098687,-24.2862429721702));
#91649=CARTESIAN_POINT('Ctrl Pts',(-0.748537331746902,10.6045971182748,
-24.7151300001489));
#91650=CARTESIAN_POINT('Ctrl Pts',(0.962955411192786,10.6052665520818,-24.7155432146706));
#91651=CARTESIAN_POINT('Ctrl Pts',(2.62588127377557,11.4354962256271,-24.2004773236733));
#91652=CARTESIAN_POINT('Ctrl Pts',(3.75468223968067,12.8417317939884,-23.5263877718132));
#91653=CARTESIAN_POINT('Ctrl Pts',(4.05,14.0684499364577,-23.2866976394846));
#91654=CARTESIAN_POINT('Ctrl Pts',(4.05,14.688,-23.2866976394846));
#91655=CARTESIAN_POINT('',(-4.05,14.688,-28.56));
#91656=CARTESIAN_POINT('Ctrl Pts',(4.05,14.688,-23.2866976394846));
#91657=CARTESIAN_POINT('Ctrl Pts',(4.05,15.3075500635423,-23.2866976394846));
#91658=CARTESIAN_POINT('Ctrl Pts',(3.75477117913856,16.5345337141539,-23.5265143677541));
#91659=CARTESIAN_POINT('Ctrl Pts',(2.62544753954527,17.9400713904106,-24.2003505240322));
#91660=CARTESIAN_POINT('Ctrl Pts',(0.963114040854605,18.771782200002,-24.7161072950123));
#91661=CARTESIAN_POINT('Ctrl Pts',(-0.963758699703665,18.7714859564189,
-24.7169298905911));
#91662=CARTESIAN_POINT('Ctrl Pts',(-2.6247891146146,17.9416552607379,-24.198643675026));
#91663=CARTESIAN_POINT('Ctrl Pts',(-3.62840603788501,16.6894320905695,-23.603545323179));
#91664=CARTESIAN_POINT('Ctrl Pts',(-4.06538382593506,15.3186709166685,-23.275730620087));
#91665=CARTESIAN_POINT('Ctrl Pts',(-4.06526477212672,14.056908092805,-23.2751714313369));
#91666=CARTESIAN_POINT('Ctrl Pts',(-3.56692412346984,12.4914312155395,-23.6515378504812));
#91667=CARTESIAN_POINT('Ctrl Pts',(-2.45900653907373,11.2979783098687,-24.2862429721702));
#91668=CARTESIAN_POINT('Ctrl Pts',(-0.748537331746902,10.6045971182748,
-24.7151300001489));
#91669=CARTESIAN_POINT('Ctrl Pts',(0.962955411192786,10.6052665520818,-24.7155432146706));
#91670=CARTESIAN_POINT('Ctrl Pts',(2.62588127377557,11.4354962256271,-24.2004773236733));
#91671=CARTESIAN_POINT('Ctrl Pts',(3.75468223968067,12.8417317939884,-23.5263877718132));
#91672=CARTESIAN_POINT('Ctrl Pts',(4.05,14.0684499364577,-23.2866976394846));
#91673=CARTESIAN_POINT('Ctrl Pts',(4.05,14.688,-23.2866976394846));
#91674=CARTESIAN_POINT('Ctrl Pts',(4.05,14.688,-23.4100889968443));
#91675=CARTESIAN_POINT('Ctrl Pts',(4.05,15.2948979871226,-23.4100889968443));
#91676=CARTESIAN_POINT('Ctrl Pts',(3.76867099305398,16.5013175070435,-23.639268673431));
#91677=CARTESIAN_POINT('Ctrl Pts',(2.65216251760359,17.9217437403638,-24.2971624934918));
#91678=CARTESIAN_POINT('Ctrl Pts',(0.976083825977573,18.7724547871576,-24.8055724681825));
#91679=CARTESIAN_POINT('Ctrl Pts',(-0.976707458134028,18.7723064866295,
-24.8063670697087));
#91680=CARTESIAN_POINT('Ctrl Pts',(-2.65136659769237,17.9228893188326,-24.2955099393282));
#91681=CARTESIAN_POINT('Ctrl Pts',(-3.64400988855577,16.6582656006921,-23.7143336666613));
#91682=CARTESIAN_POINT('Ctrl Pts',(-4.06492675298839,15.3040417018377,-23.3994826671362));
#91683=CARTESIAN_POINT('Ctrl Pts',(-4.06464463936234,14.0716337705481,-23.3990003982703));
#91684=CARTESIAN_POINT('Ctrl Pts',(-3.58515476920467,12.5248416966978,-23.7603792715584));
#91685=CARTESIAN_POINT('Ctrl Pts',(-2.48508839011874,11.313229839728,-24.3818697514195));
#91686=CARTESIAN_POINT('Ctrl Pts',(-0.758425187594836,10.6039383832458,
-24.8046262524058));
#91687=CARTESIAN_POINT('Ctrl Pts',(0.975880653594945,10.6046020570128,-24.8050171266545));
#91688=CARTESIAN_POINT('Ctrl Pts',(2.6526462246547,11.4538234315344,-24.2972989549263));
#91689=CARTESIAN_POINT('Ctrl Pts',(3.76856749003345,12.8749501508879,-23.6391422854865));
#91690=CARTESIAN_POINT('Ctrl Pts',(4.05,14.0811020128774,-23.4100889968443));
#91691=CARTESIAN_POINT('Ctrl Pts',(4.05,14.688,-23.4100889968443));
#91692=CARTESIAN_POINT('Ctrl Pts',(4.12855382656681,14.688,-23.6556995045996));
#91693=CARTESIAN_POINT('Ctrl Pts',(4.12855382656681,15.2818241953714,-23.6556995045996));
#91694=CARTESIAN_POINT('Ctrl Pts',(3.86076516644458,16.4700009555522,-23.8638320218397));
#91695=CARTESIAN_POINT('Ctrl Pts',(2.73730116859749,17.9289229358609,-24.49025998471));
#91696=CARTESIAN_POINT('Ctrl Pts',(1.01067042684546,18.8148204133092,-24.9841553078376));
#91697=CARTESIAN_POINT('Ctrl Pts',(-1.01128961537565,18.81490920269,-24.9848957767023));
#91698=CARTESIAN_POINT('Ctrl Pts',(-2.7362314416444,17.9293448956734,-24.4886857048216));
#91699=CARTESIAN_POINT('Ctrl Pts',(-3.73581578291115,16.6318988939734,-23.9350596006894));
#91700=CARTESIAN_POINT('Ctrl Pts',(-4.14332588928732,15.2877734013966,-23.645879002476));
#91701=CARTESIAN_POINT('Ctrl Pts',(-4.14284376717838,14.0880200943702,-23.6455590375256));
#91702=CARTESIAN_POINT('Ctrl Pts',(-3.67922724871041,12.5523416357812,-23.9772276275149));
#91703=CARTESIAN_POINT('Ctrl Pts',(-2.56593899372256,11.3002974171402,-24.5726577012497));
#91704=CARTESIAN_POINT('Ctrl Pts',(-0.784992190544882,10.5616209397369,
-24.9832529516161));
#91705=CARTESIAN_POINT('Ctrl Pts',(1.01033058468266,10.5622313569691,-24.9836167715101));
#91706=CARTESIAN_POINT('Ctrl Pts',(2.73786236787182,11.4466555002175,-24.4904092543238));
#91707=CARTESIAN_POINT('Ctrl Pts',(3.86063072387617,12.9062661228527,-23.863707029497));
#91708=CARTESIAN_POINT('Ctrl Pts',(4.12855382656681,14.0941758046286,-23.6556995045996));
#91709=CARTESIAN_POINT('Ctrl Pts',(4.12855382656681,14.688,-23.6556995045996));
#91710=CARTESIAN_POINT('Ctrl Pts',(4.49055124896869,14.688,-23.9298855992356));
#91711=CARTESIAN_POINT('Ctrl Pts',(4.49055124896869,15.309268298706,-23.9298855992356));
#91712=CARTESIAN_POINT('Ctrl Pts',(4.19325789149789,16.5538991992546,-24.1296173306374));
#91713=CARTESIAN_POINT('Ctrl Pts',(2.96189964638343,18.0879203899391,-24.7457991886986));
#91714=CARTESIAN_POINT('Ctrl Pts',(1.09093099096877,19.0172471491435,-25.2365322104703));
#91715=CARTESIAN_POINT('Ctrl Pts',(-1.09160318155618,19.0173730121423,-25.2372474923589));
#91716=CARTESIAN_POINT('Ctrl Pts',(-2.96090595211656,18.0882153913716,-24.7443467710194));
#91717=CARTESIAN_POINT('Ctrl Pts',(-4.05617421288598,16.724281413124,-24.1994319815307));
#91718=CARTESIAN_POINT('Ctrl Pts',(-4.5067990157527,15.3149441912885,-23.9201607483296));
#91719=CARTESIAN_POINT('Ctrl Pts',(-4.50633590484044,14.0608366102828,-23.9198852215378));
#91720=CARTESIAN_POINT('Ctrl Pts',(-3.99334656067512,12.4505111204035,-24.2401598119502));
#91721=CARTESIAN_POINT('Ctrl Pts',(-2.77546567797919,11.1340757856475,-24.8276385061613));
#91722=CARTESIAN_POINT('Ctrl Pts',(-0.847516003767398,10.35925003365,-25.2356985806033));
#91723=CARTESIAN_POINT('Ctrl Pts',(1.09064974524935,10.3598283214159,-25.2360026321993));
#91724=CARTESIAN_POINT('Ctrl Pts',(2.96246104371384,11.2876559203943,-24.745975080844));
#91725=CARTESIAN_POINT('Ctrl Pts',(4.19313151491998,12.8223742307126,-24.1294895193316));
#91726=CARTESIAN_POINT('Ctrl Pts',(4.49055124896869,14.066731701294,-23.9298855992356));
#91727=CARTESIAN_POINT('Ctrl Pts',(4.49055124896869,14.688,-23.9298855992356));
#91728=CARTESIAN_POINT('Ctrl Pts',(4.82914930550667,14.688,-23.8884972217762));
#91729=CARTESIAN_POINT('Ctrl Pts',(4.82914930550667,15.3651411087864,-23.8884972217762));
#91730=CARTESIAN_POINT('Ctrl Pts',(4.48512211029089,16.7118615149729,-24.1201883032215));
#91731=CARTESIAN_POINT('Ctrl Pts',(3.1421225816263,18.2961229501612,-24.7935064927671));
#91732=CARTESIAN_POINT('Ctrl Pts',(1.15312867962539,19.2416794724688,-25.3160151570556));
#91733=CARTESIAN_POINT('Ctrl Pts',(-1.15390197288246,19.2415063677517,-25.3168334602295));
#91734=CARTESIAN_POINT('Ctrl Pts',(-3.14117672259674,18.2973849550254,-24.791625445862));
#91735=CARTESIAN_POINT('Ctrl Pts',(-4.33514015399536,16.8869796321539,-24.1971733451445));
#91736=CARTESIAN_POINT('Ctrl Pts',(-4.84744213589749,15.3752521866832,-23.8780908288589));
#91737=CARTESIAN_POINT('Ctrl Pts',(-4.84723895642577,14.0004341195354,-23.8776880000878));
#91738=CARTESIAN_POINT('Ctrl Pts',(-4.26310394920718,12.2736358697371,-24.243691927209));
#91739=CARTESIAN_POINT('Ctrl Pts',(-2.94305481018679,10.9230737806569,-24.8807692542566));
#91740=CARTESIAN_POINT('Ctrl Pts',(-0.896059274970361,10.1347927110523,
-25.3149364648599));
#91741=CARTESIAN_POINT('Ctrl Pts',(1.15283203136582,10.1354726840367,-25.3154441441371));
#91742=CARTESIAN_POINT('Ctrl Pts',(3.14266649875182,11.0794084952916,-24.7936105411821));
#91743=CARTESIAN_POINT('Ctrl Pts',(4.48499771640589,12.6644309839937,-24.1200645189159));
#91744=CARTESIAN_POINT('Ctrl Pts',(4.82914930550667,14.0108588912136,-23.8884972217762));
#91745=CARTESIAN_POINT('Ctrl Pts',(4.82914930550667,14.688,-23.8884972217762));
#91746=CARTESIAN_POINT('Ctrl Pts',(4.98309455587392,14.688,-23.7857447483302));
#91747=CARTESIAN_POINT('Ctrl Pts',(4.98309455587392,15.3993352581412,-23.7857447483302));
#91748=CARTESIAN_POINT('Ctrl Pts',(4.61984686946115,16.8080942643989,-24.0427403253296));
#91749=CARTESIAN_POINT('Ctrl Pts',(3.23033415828164,18.4218597445456,-24.7648455472437));
#91750=CARTESIAN_POINT('Ctrl Pts',(1.18500946510329,19.3767869703726,-25.3175476456579));
#91751=CARTESIAN_POINT('Ctrl Pts',(-1.1858026493011,19.3764468388513,-25.3184291664214));
#91752=CARTESIAN_POINT('Ctrl Pts',(-3.22952403638349,18.4236782623287,-24.7630164311167));
#91753=CARTESIAN_POINT('Ctrl Pts',(-4.46436799355182,16.9859405484317,-24.1252892575041));
#91754=CARTESIAN_POINT('Ctrl Pts',(-5.00202271865554,15.4121036450639,-23.7739921258239));
#91755=CARTESIAN_POINT('Ctrl Pts',(-5.00187623559771,13.9634129954428,-23.773392880573));
#91756=CARTESIAN_POINT('Ctrl Pts',(-4.38872103231554,12.1660136178416,-24.1767196449283));
#91757=CARTESIAN_POINT('Ctrl Pts',(-3.02554619696707,10.7957528742936,-24.8568907495462));
#91758=CARTESIAN_POINT('Ctrl Pts',(-0.920995630295405,9.99964854320438,
-25.3165003439991));
#91759=CARTESIAN_POINT('Ctrl Pts',(1.18481428816398,10.0004171523902,-25.3169431584149));
#91760=CARTESIAN_POINT('Ctrl Pts',(3.23086782215367,10.9536438146089,-24.7649814299536));
#91761=CARTESIAN_POINT('Ctrl Pts',(4.61973743891093,12.568210578283,-24.0426046609116));
#91762=CARTESIAN_POINT('Ctrl Pts',(4.98309455587392,13.9766647418588,-23.7857447483302));
#91763=CARTESIAN_POINT('Ctrl Pts',(4.98309455587392,14.688,-23.7857447483302));
#91764=CARTESIAN_POINT('',(4.98309455587393,14.688,-23.7857447483302));
#91765=CARTESIAN_POINT('Ctrl Pts',(4.98309455587392,14.688,-23.7857447483302));
#91766=CARTESIAN_POINT('Ctrl Pts',(4.82914930550667,14.688,-23.8884972217762));
#91767=CARTESIAN_POINT('Ctrl Pts',(4.49055124896869,14.688,-23.9298855992356));
#91768=CARTESIAN_POINT('Ctrl Pts',(4.12855382656681,14.688,-23.6556995045996));
#91769=CARTESIAN_POINT('Ctrl Pts',(4.05,14.688,-23.4100889968443));
#91770=CARTESIAN_POINT('Ctrl Pts',(4.05,14.688,-23.2866976394846));
#91771=CARTESIAN_POINT('Ctrl Pts',(4.98309455587392,14.688,-23.7857447483302));
#91772=CARTESIAN_POINT('Ctrl Pts',(4.98309455587392,13.9766647418588,-23.7857447483302));
#91773=CARTESIAN_POINT('Ctrl Pts',(4.61973743891093,12.568210578283,-24.0426046609116));
#91774=CARTESIAN_POINT('Ctrl Pts',(3.23086782215367,10.9536438146089,-24.7649814299536));
#91775=CARTESIAN_POINT('Ctrl Pts',(1.18481428816398,10.0004171523902,-25.3169431584149));
#91776=CARTESIAN_POINT('Ctrl Pts',(-0.920995630295405,9.99964854320438,
-25.3165003439991));
#91777=CARTESIAN_POINT('Ctrl Pts',(-3.02554619696707,10.7957528742936,-24.8568907495462));
#91778=CARTESIAN_POINT('Ctrl Pts',(-4.38872103231554,12.1660136178416,-24.1767196449283));
#91779=CARTESIAN_POINT('Ctrl Pts',(-5.00187623559771,13.9634129954428,-23.773392880573));
#91780=CARTESIAN_POINT('Ctrl Pts',(-5.00202271865554,15.4121036450639,-23.7739921258239));
#91781=CARTESIAN_POINT('Ctrl Pts',(-4.46436799355182,16.9859405484317,-24.1252892575041));
#91782=CARTESIAN_POINT('Ctrl Pts',(-3.22952403638349,18.4236782623287,-24.7630164311167));
#91783=CARTESIAN_POINT('Ctrl Pts',(-1.1858026493011,19.3764468388513,-25.3184291664214));
#91784=CARTESIAN_POINT('Ctrl Pts',(1.18500946510329,19.3767869703726,-25.3175476456579));
#91785=CARTESIAN_POINT('Ctrl Pts',(3.23033415828164,18.4218597445456,-24.7648455472437));
#91786=CARTESIAN_POINT('Ctrl Pts',(4.61984686946115,16.8080942643989,-24.0427403253296));
#91787=CARTESIAN_POINT('Ctrl Pts',(4.98309455587392,15.3993352581412,-23.7857447483302));
#91788=CARTESIAN_POINT('Ctrl Pts',(4.98309455587392,14.688,-23.7857447483302));
#91789=CARTESIAN_POINT('Origin',(0.,8.16,-16.32));
#91790=CARTESIAN_POINT('',(-7.46865811617337,22.032,-21.2987269400639));
#91791=CARTESIAN_POINT('Origin',(0.,22.032,-16.32));
#91792=CARTESIAN_POINT('',(-4.97872694006385,22.032,-23.7886581161734));
#91793=CARTESIAN_POINT('Ctrl Pts',(-4.97872694006383,22.032,-23.7886581161734));
#91794=CARTESIAN_POINT('Ctrl Pts',(-5.03175741160795,22.032,-23.7533071557714));
#91795=CARTESIAN_POINT('Ctrl Pts',(-5.08949447272707,22.0291665724821,-23.7140146374592));
#91796=CARTESIAN_POINT('Ctrl Pts',(-5.48848300667678,21.9864710060741,-23.4343486419447));
#91797=CARTESIAN_POINT('Ctrl Pts',(-5.78359160013614,21.8585898122974,-23.1919404268334));
#91798=CARTESIAN_POINT('Ctrl Pts',(-6.09332586727315,21.7641706681883,-22.9115678992333));
#91799=CARTESIAN_POINT('Ctrl Pts',(-6.16342892487598,21.7460214167023,-22.8461071850267));
#91800=CARTESIAN_POINT('Ctrl Pts',(-6.27276491697942,21.7305429498519,-22.7405954419643));
#91801=CARTESIAN_POINT('Ctrl Pts',(-6.31169904868965,21.7276769162343,-22.7023279477922));
#91802=CARTESIAN_POINT('Ctrl Pts',(-6.39092330907367,21.7280892293569,-22.6230057301446));
#91803=CARTESIAN_POINT('Ctrl Pts',(-6.42985838198943,21.7314874092212,-22.5832781971981));
#91804=CARTESIAN_POINT('Ctrl Pts',(-6.54332420993137,21.749515544574,-22.4653264460471));
#91805=CARTESIAN_POINT('Ctrl Pts',(-6.61627959897023,21.7715068490678,-22.3866393454028));
#91806=CARTESIAN_POINT('Ctrl Pts',(-6.86061183082832,21.8583157174666,-22.1139294317882));
#91807=CARTESIAN_POINT('Ctrl Pts',(-7.05075649756721,21.9512509923618,-21.8841548448483));
#91808=CARTESIAN_POINT('Ctrl Pts',(-7.30413662922104,22.0160133376152,-21.5381739817469));
#91809=CARTESIAN_POINT('Ctrl Pts',(-7.38436628991476,22.032,-21.4251742909413));
#91810=CARTESIAN_POINT('Ctrl Pts',(-7.46865811617335,22.032,-21.2987269400639));
#91811=CARTESIAN_POINT('',(8.976,22.032,-16.32));
#91812=CARTESIAN_POINT('Origin',(0.,22.032,-16.32));
#91813=CARTESIAN_POINT('',(8.976,8.16,-16.32));
#91814=CARTESIAN_POINT('Origin',(-4.896,21.432,-21.216));
#91815=CARTESIAN_POINT('',(-3.79798786503066,22.032,-21.216));
#91816=CARTESIAN_POINT('Origin',(-4.896,22.032,-21.216));
#91817=CARTESIAN_POINT('',(-3.264,21.7056,-21.216));
#91818=CARTESIAN_POINT('Origin',(-3.79798786503066,21.432,-21.216));
#91819=CARTESIAN_POINT('Origin',(-4.896,21.7056,-21.216));
#91820=CARTESIAN_POINT('Origin',(0.,22.032,-8.16));
#91821=CARTESIAN_POINT('Origin',(-8.376,8.76,-12.24));
#91822=CARTESIAN_POINT('',(-8.76,8.29897505490484,-10.608));
#91823=CARTESIAN_POINT('Ctrl Pts',(-8.37600000000002,8.16,-10.7469750549048));
#91824=CARTESIAN_POINT('Ctrl Pts',(-8.40091268315884,8.16,-10.726224615184));
#91825=CARTESIAN_POINT('Ctrl Pts',(-8.42740104856703,8.16155857905989,-10.7075963115084));
#91826=CARTESIAN_POINT('Ctrl Pts',(-8.495153215849,8.1705557020042,-10.6676000307859));
#91827=CARTESIAN_POINT('Ctrl Pts',(-8.54101113694863,8.18110084923513,-10.6473790996848));
#91828=CARTESIAN_POINT('Ctrl Pts',(-8.63186213304349,8.21512617965098,-10.6199246683574));
#91829=CARTESIAN_POINT('Ctrl Pts',(-8.67676732474104,8.23871780749174,-10.6125388608906));
#91830=CARTESIAN_POINT('Ctrl Pts',(-8.73070136992335,8.27571625725086,-10.6085196615488));
#91831=CARTESIAN_POINT('Ctrl Pts',(-8.74559886385357,8.28697996366506,-10.608));
#91832=CARTESIAN_POINT('Ctrl Pts',(-8.76,8.29897505490484,-10.608));
#91833=CARTESIAN_POINT('',(-8.976,8.76,-10.608));
#91834=CARTESIAN_POINT('',(-8.976,8.76,-12.24));
#91835=CARTESIAN_POINT('Origin',(-8.376,8.76,-10.608));
#91836=CARTESIAN_POINT('Origin',(27.528,7.344,9.192));
#91837=CARTESIAN_POINT('',(26.928,7.944,9.192));
#91838=CARTESIAN_POINT('',(27.528,7.944,9.792));
#91839=CARTESIAN_POINT('Origin',(27.528,7.944,9.192));
#91840=CARTESIAN_POINT('',(27.528,21.432,9.792));
#91841=CARTESIAN_POINT('',(27.528,7.344,9.792));
#91842=CARTESIAN_POINT('',(26.928,21.432,9.192));
#91843=CARTESIAN_POINT('Origin',(27.528,21.432,9.192));
#91844=CARTESIAN_POINT('',(26.928,7.344,9.192));
#91845=CARTESIAN_POINT('Origin',(13.464,21.432,9.192));
#91846=CARTESIAN_POINT('',(27.528,22.032,9.192));
#91847=CARTESIAN_POINT('Origin',(27.528,21.432,9.192));
#91848=CARTESIAN_POINT('',(13.464,21.432,9.792));
#91849=CARTESIAN_POINT('',(29.184,22.032,9.192));
#91850=CARTESIAN_POINT('Origin',(29.184,21.432,9.192));
#91851=CARTESIAN_POINT('',(13.464,22.032,9.192));
#91852=CARTESIAN_POINT('Origin',(27.528,21.432,9.192));
#91853=CARTESIAN_POINT('Origin',(27.528,21.432,9.192));
#91854=CARTESIAN_POINT('Origin',(29.184,21.432,9.192));
#91855=CARTESIAN_POINT('Origin',(29.184,21.432,9.192));
#91856=CARTESIAN_POINT('Origin',(22.95,7.944,9.192));
#91857=CARTESIAN_POINT('',(22.95,7.944,9.792));
#91858=CARTESIAN_POINT('Origin',(27.528,7.944,9.192));
#91859=CARTESIAN_POINT('Origin',(27.528,7.944,9.192));
#91860=CARTESIAN_POINT('Origin',(27.528,7.944,9.192));
#91861=CARTESIAN_POINT('Origin',(29.184,14.2128206445356,-1.1470985449732));
#91862=CARTESIAN_POINT('',(29.184,20.3587352485079,8.8128));
#91863=CARTESIAN_POINT('Origin',(29.184,21.5019541534552,9.4128));
#91864=CARTESIAN_POINT('',(29.184,19.6120909823364,7.73112305029005));
#91865=CARTESIAN_POINT('',(29.184,13.7190338627358,-0.806254571695441));
#91866=CARTESIAN_POINT('',(29.6730897616957,19.9512000004902,7.778));
#91867=CARTESIAN_POINT('Ctrl Pts',(29.184,19.6120909823364,7.73112305029004));
#91868=CARTESIAN_POINT('Ctrl Pts',(29.2236153010039,19.6120909823364,7.73112305029004));
#91869=CARTESIAN_POINT('Ctrl Pts',(29.2633091750366,19.6181170767952,7.73286634617824));
#91870=CARTESIAN_POINT('Ctrl Pts',(29.3404403169688,19.6411090544722,7.73898290297034));
#91871=CARTESIAN_POINT('Ctrl Pts',(29.3778828026048,19.6580635030102,7.74333332193731));
#91872=CARTESIAN_POINT('Ctrl Pts',(29.4840885147569,19.7211400971071,7.75740174366774));
#91873=CARTESIAN_POINT('Ctrl Pts',(29.5468609707651,19.779797513811,7.76771957622777));
#91874=CARTESIAN_POINT('Ctrl Pts',(29.6241709396688,19.8746468475679,7.77610895998165));
#91875=CARTESIAN_POINT('Ctrl Pts',(29.6500156297378,19.9117444532444,7.77800000003095));
#91876=CARTESIAN_POINT('Ctrl Pts',(29.6730897616957,19.9512000009804,7.778));
#91877=CARTESIAN_POINT('Ctrl Pts',(29.6730897616957,19.9512000009804,7.778));
#91878=CARTESIAN_POINT('Ctrl Pts',(29.6960587249166,19.9904757157272,7.77799999996919));
#91879=CARTESIAN_POINT('Ctrl Pts',(29.7162857661367,20.0320859161527,7.77611545312242));
#91880=CARTESIAN_POINT('Ctrl Pts',(29.7660314239133,20.160153365583,7.7633991486045));
#91881=CARTESIAN_POINT('Ctrl Pts',(29.784,20.2498877771072,7.7448784177953));
#91882=CARTESIAN_POINT('Ctrl Pts',(29.784,20.3324059608682,7.71845454150864));
#91883=CARTESIAN_POINT('Origin',(29.184,8.18063237574607,9.4128));
#91884=CARTESIAN_POINT('',(29.184,9.01726475149214,8.8128));
#91885=CARTESIAN_POINT('Origin',(29.184,7.87404584654483,9.4128));
#91886=CARTESIAN_POINT('',(29.184,8.18063237574607,8.8128));
#91887=CARTESIAN_POINT('Origin',(29.184,15.628584851675,-1.82133984076555));
#91888=CARTESIAN_POINT('',(29.184,14.688,0.59750406305912));
#91889=CARTESIAN_POINT('Origin',(29.184,14.323470193544,0.0694031896036992));
#91890=CARTESIAN_POINT('',(29.184,16.1223716334749,-1.48049586748779));
#91891=CARTESIAN_POINT('Origin',(26.928,7.344,9.792));
#91892=CARTESIAN_POINT('Origin',(29.184,21.432,-9.384));
#91893=CARTESIAN_POINT('Origin',(29.184,21.432,-10.2288));
#91894=CARTESIAN_POINT('',(29.184,22.032,-13.272));
#91895=CARTESIAN_POINT('Origin',(29.184,21.432,-13.272));
#91896=CARTESIAN_POINT('',(29.184,22.032,-9.384));
#91897=CARTESIAN_POINT('Origin',(13.464,19.9512,6.528));
#91898=CARTESIAN_POINT('',(27.528,19.9512,7.778));
#91899=CARTESIAN_POINT('Origin',(27.528,19.9512,6.528));
#91900=CARTESIAN_POINT('',(13.464,19.9512,7.778));
#91901=CARTESIAN_POINT('',(28.968,19.6120909823364,7.73112305029005));
#91902=CARTESIAN_POINT('',(13.464,19.6120909823364,7.73112305029005));
#91903=CARTESIAN_POINT('',(28.968,18.7060084170374,6.41846497492097));
#91904=CARTESIAN_POINT('Origin',(28.968,19.9512,6.528));
#91905=CARTESIAN_POINT('',(13.464,18.7060084170374,6.41846497492097));
#91906=CARTESIAN_POINT('',(29.184,19.3965172404536,5.40780937503389));
#91907=CARTESIAN_POINT('Ctrl Pts',(29.184,19.3965172404536,5.4078093750339));
#91908=CARTESIAN_POINT('Ctrl Pts',(29.2594100037102,19.3965172404536,5.4078093750339));
#91909=CARTESIAN_POINT('Ctrl Pts',(29.3397541554034,19.3827001386888,5.41433241819919));
#91910=CARTESIAN_POINT('Ctrl Pts',(29.4875100123773,19.3285720959285,5.44366515993349));
#91911=CARTESIAN_POINT('Ctrl Pts',(29.5549412887334,19.2884885638861,5.46679459941119));
#91912=CARTESIAN_POINT('Ctrl Pts',(29.6626423483001,19.1996511726765,5.52768435501259));
#91913=CARTESIAN_POINT('Ctrl Pts',(29.7092855081103,19.1449042633456,5.56984732632713));
#91914=CARTESIAN_POINT('Ctrl Pts',(29.7699321343959,19.0357206786645,5.67356042783162));
#91915=CARTESIAN_POINT('Ctrl Pts',(29.784,18.9815769113417,5.73538086530188));
#91916=CARTESIAN_POINT('Ctrl Pts',(29.784,18.9366533000553,5.79779797752169));
#91917=CARTESIAN_POINT('',(28.968,19.3965172404536,5.40780937503389));
#91918=CARTESIAN_POINT('',(13.464,19.3965172404536,5.40780937503389));
#91919=CARTESIAN_POINT('',(28.968,21.0528,5.93725687477551));
#91920=CARTESIAN_POINT('Origin',(28.968,19.9512,6.528));
#91921=CARTESIAN_POINT('',(13.464,21.0528,5.93725687477551));
#91922=CARTESIAN_POINT('',(28.968,21.0528,7.11874312522449));
#91923=CARTESIAN_POINT('',(13.464,21.0528,7.11874312522449));
#91924=CARTESIAN_POINT('',(28.968,20.8019222240139,7.44384479993544));
#91925=CARTESIAN_POINT('Origin',(28.968,19.9512,6.528));
#91926=CARTESIAN_POINT('',(13.464,20.8019222240139,7.44384479993543));
#91927=CARTESIAN_POINT('Origin',(28.9300379575436,10.9840064439642,-5.7254604242248));
#91928=CARTESIAN_POINT('',(28.968,9.01726475149214,-9.6288));
#91929=CARTESIAN_POINT('',(29.184,8.95019645516457,-9.6288));
#91930=CARTESIAN_POINT('Origin',(28.9300379575436,8.28966585183622,-9.6288));
#91931=CARTESIAN_POINT('',(28.968,14.688,-1.41350406305912));
#91932=CARTESIAN_POINT('',(29.184,12.1735582741579,-3.0452127961736));
#91933=CARTESIAN_POINT('',(29.184,10.5366338627358,-5.41665457169544));
#91934=CARTESIAN_POINT('',(29.184,11.0112188528984,-4.72911477825469));
#91935=CARTESIAN_POINT('Ctrl Pts',(29.184,12.1735582741579,-3.04521279617358));
#91936=CARTESIAN_POINT('Ctrl Pts',(29.2104713416293,12.1762030381632,-3.06315131981746));
#91937=CARTESIAN_POINT('Ctrl Pts',(29.234788995256,12.1788567912663,-3.08351224071388));
#91938=CARTESIAN_POINT('Ctrl Pts',(29.3226220296533,12.1881180495744,-3.17032211138502));
#91939=CARTESIAN_POINT('Ctrl Pts',(29.3688042730669,12.1918686315823,-3.24838022420768));
#91940=CARTESIAN_POINT('Ctrl Pts',(29.4381265282101,12.1842209848219,-3.41619439674659));
#91941=CARTESIAN_POINT('Ctrl Pts',(29.4608149636269,12.1728534227401,-3.50613803778445));
#91942=CARTESIAN_POINT('Ctrl Pts',(29.5078391962474,12.1108433156642,-3.77854749423463));
#91943=CARTESIAN_POINT('Ctrl Pts',(29.5133365788438,12.0301406684281,-3.96243903993894));
#91944=CARTESIAN_POINT('Ctrl Pts',(29.5133365788438,11.817993240571,-4.26978082644984));
#91945=CARTESIAN_POINT('Ctrl Pts',(29.5078391962474,11.6746662914965,-4.41044497796478));
#91946=CARTESIAN_POINT('Ctrl Pts',(29.4608149636269,11.4419449032558,-4.56501832883223));
#91947=CARTESIAN_POINT('Ctrl Pts',(29.4381265282101,11.3618762483097,-4.60753997656553));
#91948=CARTESIAN_POINT('Ctrl Pts',(29.3688042730669,11.2076777804307,-4.67419517523491));
#91949=CARTESIAN_POINT('Ctrl Pts',(29.3226220296533,11.1333617005729,-4.69836656570777));
#91950=CARTESIAN_POINT('Ctrl Pts',(29.234788995256,11.0489085147679,-4.72048859000003));
#91951=CARTESIAN_POINT('Ctrl Pts',(29.2104713416293,11.0289295908271,-4.72522695506081));
#91952=CARTESIAN_POINT('Ctrl Pts',(29.184,11.0112188528984,-4.7291147782547));
#91953=CARTESIAN_POINT('',(29.184,8.3232,-8.62329593694088));
#91954=CARTESIAN_POINT('',(29.184,10.5366338627358,-5.41665457169544));
#91955=CARTESIAN_POINT('',(29.5300378243943,8.21336101791777,-9.73863898202413));
#91956=CARTESIAN_POINT('Ctrl Pts',(29.5300378238068,8.21336101894687,-9.73863898202463));
#91957=CARTESIAN_POINT('Ctrl Pts',(29.5299652136275,8.21341227938468,-9.54712666911579));
#91958=CARTESIAN_POINT('Ctrl Pts',(29.5021917223446,8.23493660162334,-9.34335072376269));
#91959=CARTESIAN_POINT('Ctrl Pts',(29.4271072085953,8.27246070308698,-9.05540444339829));
#91960=CARTESIAN_POINT('Ctrl Pts',(29.3964683073732,8.28577461186978,-8.96300054972493));
#91961=CARTESIAN_POINT('Ctrl Pts',(29.3190911130439,8.30919077581502,-8.79060079716896));
#91962=CARTESIAN_POINT('Ctrl Pts',(29.2750026556793,8.32025772712183,-8.70955977314038));
#91963=CARTESIAN_POINT('Ctrl Pts',(29.1991477037336,8.32304864986649,-8.63633187201137));
#91964=CARTESIAN_POINT('Ctrl Pts',(29.1917743349867,8.3232,-8.62968955278653));
#91965=CARTESIAN_POINT('Ctrl Pts',(29.184,8.3232,-8.62329593694086));
#91966=CARTESIAN_POINT('Ctrl Pts',(29.184,8.95019645516454,-9.6288));
#91967=CARTESIAN_POINT('Ctrl Pts',(29.191656667606,8.9458499595919,-9.6288));
#91968=CARTESIAN_POINT('Ctrl Pts',(29.1990327024229,8.94132039915384,-9.62894711890317));
#91969=CARTESIAN_POINT('Ctrl Pts',(29.2633794371802,8.89917561711943,-9.63131462110273));
#91970=CARTESIAN_POINT('Ctrl Pts',(29.3088752624018,8.85082583416841,-9.6405225541825));
#91971=CARTESIAN_POINT('Ctrl Pts',(29.3873519467975,8.74278725437783,-9.6628387793616));
#91972=CARTESIAN_POINT('Ctrl Pts',(29.4198150443329,8.68279394360638,-9.67628824309362));
#91973=CARTESIAN_POINT('Ctrl Pts',(29.499741316798,8.4917590529397,-9.71516781540766));
#91974=CARTESIAN_POINT('Ctrl Pts',(29.5300379575436,8.3509498358972,-9.73863907546699));
#91975=CARTESIAN_POINT('Ctrl Pts',(29.5300379575436,8.21368550110616,-9.73863907546699));
#91976=CARTESIAN_POINT('Ctrl Pts',(29.5300379129813,8.21352326407097,-9.73863904400745));
#91977=CARTESIAN_POINT('Ctrl Pts',(29.5300378238059,8.21336101791847,-9.73863898105247));
#91978=CARTESIAN_POINT('Origin',(13.464,10.6896,-3.264));
#91979=CARTESIAN_POINT('',(27.528,10.6896,-1.764));
#91980=CARTESIAN_POINT('Origin',(27.528,10.6896,-3.264));
#91981=CARTESIAN_POINT('',(28.368,10.6896,-1.764));
#91982=CARTESIAN_POINT('',(13.464,10.6896,-1.764));
#91983=CARTESIAN_POINT('',(28.368,11.0112188528984,-4.72911477825469));
#91984=CARTESIAN_POINT('Origin',(28.368,10.6896,-3.264));
#91985=CARTESIAN_POINT('',(13.464,11.0112188528984,-4.72911477825469));
#91986=CARTESIAN_POINT('',(28.368,12.1735582741579,-3.0452127961736));
#91987=CARTESIAN_POINT('',(13.464,12.1735582741579,-3.0452127961736));
#91988=CARTESIAN_POINT('Origin',(28.368,10.6896,-3.264));
#91989=CARTESIAN_POINT('Origin',(13.566,7.944,9.192));
#91990=CARTESIAN_POINT('',(14.904,7.944,9.792));
#91991=CARTESIAN_POINT('Origin',(14.904,7.944,9.192));
#91992=CARTESIAN_POINT('',(14.064,7.944,9.792));
#91993=CARTESIAN_POINT('',(13.566,7.944,9.792));
#91994=CARTESIAN_POINT('Origin',(14.064,7.944,9.192));
#91995=CARTESIAN_POINT('Origin',(14.904,7.944,-1.224));
#91996=CARTESIAN_POINT('',(15.504,7.944,9.192));
#91997=CARTESIAN_POINT('Origin',(14.904,7.944,9.192));
#91998=CARTESIAN_POINT('',(15.504,7.944,-10.608));
#91999=CARTESIAN_POINT('Origin',(14.904,7.944,-11.208));
#92000=CARTESIAN_POINT('',(15.504,7.944,-1.224));
#92001=CARTESIAN_POINT('Origin',(14.904,7.944,9.192));
#92002=CARTESIAN_POINT('Origin',(14.904,7.944,9.192));
#92003=CARTESIAN_POINT('Origin',(14.064,7.752,9.192));
#92004=CARTESIAN_POINT('',(13.464,7.944,9.192));
#92005=CARTESIAN_POINT('Origin',(14.064,7.944,9.192));
#92006=CARTESIAN_POINT('',(14.064,8.76,9.792));
#92007=CARTESIAN_POINT('',(14.064,7.752,9.792));
#92008=CARTESIAN_POINT('Origin',(14.064,8.76,9.192));
#92009=CARTESIAN_POINT('',(13.464,7.752,9.192));
#92010=CARTESIAN_POINT('Origin',(14.064,7.944,9.192));
#92011=CARTESIAN_POINT('Origin',(14.064,7.944,9.192));
#92012=CARTESIAN_POINT('Origin',(14.064,7.944,-11.424));
#92013=CARTESIAN_POINT('',(13.464,7.944,-11.424));
#92014=CARTESIAN_POINT('Origin',(13.464,7.344,-10.608));
#92015=CARTESIAN_POINT('',(13.464,15.72,6.528));
#92016=CARTESIAN_POINT('',(13.464,8.16,6.528));
#92017=CARTESIAN_POINT('',(13.464,16.32,7.128));
#92018=CARTESIAN_POINT('Origin',(13.464,15.72,7.128));
#92019=CARTESIAN_POINT('',(13.464,16.32,9.192));
#92020=CARTESIAN_POINT('',(13.464,16.32,6.528));
#92021=CARTESIAN_POINT('',(13.464,21.432,9.192));
#92022=CARTESIAN_POINT('',(13.464,7.752,9.192));
#92023=CARTESIAN_POINT('',(13.464,21.432,7.63693253176196));
#92024=CARTESIAN_POINT('',(13.464,21.432,-9.384));
#92025=CARTESIAN_POINT('',(13.464,19.9512,8.378));
#92026=CARTESIAN_POINT('Origin',(13.464,19.9512,6.528));
#92027=CARTESIAN_POINT('',(13.464,21.432,5.41906746823804));
#92028=CARTESIAN_POINT('Origin',(13.464,19.9512,6.528));
#92029=CARTESIAN_POINT('',(13.464,21.432,-9.384));
#92030=CARTESIAN_POINT('',(13.464,10.6896,-1.164));
#92031=CARTESIAN_POINT('Origin',(13.464,10.6896,-3.264));
#92032=CARTESIAN_POINT('Origin',(14.904,19.9512,6.528));
#92033=CARTESIAN_POINT('',(15.504,21.432,7.63693253176196));
#92034=CARTESIAN_POINT('',(15.504,19.9512,4.678));
#92035=CARTESIAN_POINT('Origin',(15.504,19.9512,6.528));
#92036=CARTESIAN_POINT('',(14.904,19.9512,5.278));
#92037=CARTESIAN_POINT('Origin',(14.904,19.9512,4.678));
#92038=CARTESIAN_POINT('',(14.904,19.9512,7.778));
#92039=CARTESIAN_POINT('Origin',(14.904,19.9512,6.528));
#92040=CARTESIAN_POINT('Origin',(14.904,19.9512,6.528));
#92041=CARTESIAN_POINT('',(15.504,21.432,5.41906746823804));
#92042=CARTESIAN_POINT('Origin',(15.504,19.9512,6.528));
#92043=CARTESIAN_POINT('Ctrl Pts',(15.504,21.432,5.41906746823803));
#92044=CARTESIAN_POINT('Ctrl Pts',(15.504,21.4328877903851,5.42173404364279));
#92045=CARTESIAN_POINT('Ctrl Pts',(15.5039980295845,21.4337726990646,5.42440158176169));
#92046=CARTESIAN_POINT('Ctrl Pts',(15.5036999443769,21.5011431619309,5.62822703110169));
#92047=CARTESIAN_POINT('Ctrl Pts',(15.4928973998635,21.5511743231396,5.83454649786246));
#92048=CARTESIAN_POINT('Ctrl Pts',(15.479052798459,21.6048568406253,6.20610495800375));
#92049=CARTESIAN_POINT('Ctrl Pts',(15.4748965230232,21.6166,6.36623586415006));
#92050=CARTESIAN_POINT('Ctrl Pts',(15.4748965230232,21.6166,6.68976413584994));
#92051=CARTESIAN_POINT('Ctrl Pts',(15.479052798459,21.6048568406253,6.84989504199625));
#92052=CARTESIAN_POINT('Ctrl Pts',(15.4928973998635,21.5511743231396,7.22145350213754));
#92053=CARTESIAN_POINT('Ctrl Pts',(15.5036999443769,21.5011431619309,7.42777296889831));
#92054=CARTESIAN_POINT('Ctrl Pts',(15.5039980295845,21.4337726990639,7.63159841824056));
#92055=CARTESIAN_POINT('Ctrl Pts',(15.504,21.4328877903859,7.63426595635496));
#92056=CARTESIAN_POINT('Ctrl Pts',(15.504,21.432,7.63693253176197));
#92057=CARTESIAN_POINT('Origin',(14.904,21.432,0.816000000000001));
#92058=CARTESIAN_POINT('',(15.504,21.432,-10.608));
#92059=CARTESIAN_POINT('',(15.504,21.432,0.816000000000001));
#92060=CARTESIAN_POINT('',(14.904,22.032,-11.208));
#92061=CARTESIAN_POINT('Origin',(14.904,21.432,-11.208));
#92062=CARTESIAN_POINT('',(14.904,22.032,9.192));
#92063=CARTESIAN_POINT('',(14.904,22.032,0.816000000000001));
#92064=CARTESIAN_POINT('',(15.504,21.432,9.192));
#92065=CARTESIAN_POINT('Origin',(14.904,21.432,9.192));
#92066=CARTESIAN_POINT('',(15.504,21.432,0.816000000000001));
#92067=CARTESIAN_POINT('Origin',(13.464,19.9512,6.528));
#92068=CARTESIAN_POINT('',(14.064,19.9512,7.778));
#92069=CARTESIAN_POINT('Origin',(14.064,19.9512,6.528));
#92070=CARTESIAN_POINT('',(13.464,19.9512,7.778));
#92071=CARTESIAN_POINT('Origin',(14.904,10.6896,-3.264));
#92072=CARTESIAN_POINT('',(15.504,10.6896,-5.364));
#92073=CARTESIAN_POINT('Origin',(15.504,10.6896,-3.264));
#92074=CARTESIAN_POINT('',(14.904,10.6896,-4.764));
#92075=CARTESIAN_POINT('Origin',(14.904,10.6896,-5.364));
#92076=CARTESIAN_POINT('',(14.904,10.6896,-1.764));
#92077=CARTESIAN_POINT('Origin',(14.904,10.6896,-3.264));
#92078=CARTESIAN_POINT('Origin',(14.904,10.6896,-3.264));
#92079=CARTESIAN_POINT('Origin',(13.464,10.6896,-3.264));
#92080=CARTESIAN_POINT('',(14.064,10.6896,-1.764));
#92081=CARTESIAN_POINT('Origin',(14.064,10.6896,-3.264));
#92082=CARTESIAN_POINT('',(13.464,10.6896,-1.764));
#92083=CARTESIAN_POINT('Origin',(15.504,7.344,9.792));
#92084=CARTESIAN_POINT('',(15.504,7.344,-10.608));
#92085=CARTESIAN_POINT('',(15.504,7.752,9.192));
#92086=CARTESIAN_POINT('Origin',(14.064,10.6896,-3.264));
#92087=CARTESIAN_POINT('Origin',(14.064,10.6896,-1.164));
#92088=CARTESIAN_POINT('Origin',(14.064,19.9512,6.528));
#92089=CARTESIAN_POINT('Origin',(14.064,19.9512,8.378));
#92090=CARTESIAN_POINT('Ctrl Pts',(13.464,21.432,7.63693253176197));
#92091=CARTESIAN_POINT('Ctrl Pts',(13.464,21.4328877903851,7.63426595635721));
#92092=CARTESIAN_POINT('Ctrl Pts',(13.4640019704155,21.4337726990646,7.63159841823831));
#92093=CARTESIAN_POINT('Ctrl Pts',(13.4643000556231,21.5011431619309,7.42777296889831));
#92094=CARTESIAN_POINT('Ctrl Pts',(13.4751026001365,21.5511743231396,7.22145350213754));
#92095=CARTESIAN_POINT('Ctrl Pts',(13.488947201541,21.6048568406253,6.84989504199625));
#92096=CARTESIAN_POINT('Ctrl Pts',(13.4931034769768,21.6166,6.68976413584994));
#92097=CARTESIAN_POINT('Ctrl Pts',(13.4931034769768,21.6166,6.36623586415006));
#92098=CARTESIAN_POINT('Ctrl Pts',(13.488947201541,21.6048568406253,6.20610495800375));
#92099=CARTESIAN_POINT('Ctrl Pts',(13.4751026001365,21.5511743231396,5.83454649786246));
#92100=CARTESIAN_POINT('Ctrl Pts',(13.4643000556231,21.5011431619309,5.62822703110169));
#92101=CARTESIAN_POINT('Ctrl Pts',(13.4640019704155,21.4337726990639,5.42440158175944));
#92102=CARTESIAN_POINT('Ctrl Pts',(13.464,21.4328877903859,5.42173404364504));
#92103=CARTESIAN_POINT('Ctrl Pts',(13.464,21.432,5.41906746823803));
#92104=CARTESIAN_POINT('Origin',(14.064,21.432,-9.384));
#92105=CARTESIAN_POINT('',(14.064,22.032,9.192));
#92106=CARTESIAN_POINT('Origin',(14.064,21.432,9.192));
#92107=CARTESIAN_POINT('',(14.064,22.032,-11.208));
#92108=CARTESIAN_POINT('',(14.064,22.032,-9.384));
#92109=CARTESIAN_POINT('Origin',(14.064,21.432,-11.208));
#92110=CARTESIAN_POINT('Origin',(12.138,15.72,7.128));
#92111=CARTESIAN_POINT('',(8.976,15.72,6.528));
#92112=CARTESIAN_POINT('',(12.138,15.72,6.528));
#92113=CARTESIAN_POINT('',(8.976,16.32,7.128));
#92114=CARTESIAN_POINT('Origin',(8.976,15.72,7.128));
#92115=CARTESIAN_POINT('',(12.138,16.32,7.128));
#92116=CARTESIAN_POINT('Origin',(13.464,8.16,6.528));
#92117=CARTESIAN_POINT('',(8.976,8.16,6.528));
#92118=CARTESIAN_POINT('Origin',(4.08,8.76,9.192));
#92119=CARTESIAN_POINT('',(4.08,8.76,9.792));
#92120=CARTESIAN_POINT('Origin',(8.16,8.16,9.792));
#92121=CARTESIAN_POINT('',(14.904,21.432,9.792));
#92122=CARTESIAN_POINT('',(14.904,7.752,9.792));
#92123=CARTESIAN_POINT('',(14.064,21.432,9.792));
#92124=CARTESIAN_POINT('',(4.08,21.432,9.792));
#92125=CARTESIAN_POINT('',(14.064,15.72,9.792));
#92126=CARTESIAN_POINT('',(14.064,7.752,9.792));
#92127=CARTESIAN_POINT('',(9.486,15.72,9.792));
#92128=CARTESIAN_POINT('Origin',(9.486,15.72,9.192));
#92129=CARTESIAN_POINT('Origin',(14.064,15.72,9.192));
#92130=CARTESIAN_POINT('',(9.486,16.32,9.192));
#92131=CARTESIAN_POINT('Origin',(10.812,16.32,8.16));
#92132=CARTESIAN_POINT('',(8.976,16.32,8.568));
#92133=CARTESIAN_POINT('Origin',(14.064,7.752,9.192));
#92134=CARTESIAN_POINT('Origin',(14.064,21.432,9.192));
#92135=CARTESIAN_POINT('Origin',(4.08,21.432,9.192));
#92136=CARTESIAN_POINT('Origin',(14.064,21.432,9.192));
#92137=CARTESIAN_POINT('Origin',(14.904,21.432,9.192));
#92138=CARTESIAN_POINT('',(4.08,22.032,9.192));
#92139=CARTESIAN_POINT('Origin',(14.064,21.432,9.192));
#92140=CARTESIAN_POINT('Origin',(14.904,7.752,9.192));
#92141=CARTESIAN_POINT('Origin',(14.904,21.432,9.192));
#92142=CARTESIAN_POINT('Origin',(14.904,21.432,9.192));
#92143=CARTESIAN_POINT('Origin',(0.,22.032,-8.16));
#92144=CARTESIAN_POINT('',(8.976,22.032,-13.272));
#92145=CARTESIAN_POINT('',(14.892,22.032,-13.272));
#92146=CARTESIAN_POINT('',(8.976,22.032,8.976));
#92147=CARTESIAN_POINT('',(-3.07332505037306,22.032,-19.3985100942983));
#92148=CARTESIAN_POINT('Origin',(-4.896,22.032,-21.216));
#92149=CARTESIAN_POINT('Origin',(-4.896,22.032,-21.216));
#92150=CARTESIAN_POINT('',(-29.184,22.032,-13.272));
#92151=CARTESIAN_POINT('',(-4.08,22.032,-13.272));
#92152=CARTESIAN_POINT('',(-29.184,22.032,9.792));
#92153=CARTESIAN_POINT('',(-29.184,22.032,-11.016));
#92154=CARTESIAN_POINT('',(-27.528,22.032,9.792));
#92155=CARTESIAN_POINT('',(-26.928,22.032,9.792));
#92156=CARTESIAN_POINT('',(-26.928,22.032,9.192));
#92157=CARTESIAN_POINT('Origin',(-27.528,22.032,9.192));
#92158=CARTESIAN_POINT('',(-26.928,22.032,-11.208));
#92159=CARTESIAN_POINT('',(-26.928,22.032,-10.608));
#92160=CARTESIAN_POINT('',(-14.904,22.032,-11.208));
#92161=CARTESIAN_POINT('',(-14.892,22.032,-11.208));
#92162=CARTESIAN_POINT('',(-14.904,22.032,9.192));
#92163=CARTESIAN_POINT('',(-14.904,22.032,-9.384));
#92164=CARTESIAN_POINT('',(-14.064,22.032,9.192));
#92165=CARTESIAN_POINT('',(-7.752,22.032,9.192));
#92166=CARTESIAN_POINT('',(-14.064,22.032,-11.208));
#92167=CARTESIAN_POINT('',(-14.064,22.032,0.816000000000001));
#92168=CARTESIAN_POINT('',(-8.376,22.032,-11.208));
#92169=CARTESIAN_POINT('',(-14.892,22.032,-11.208));
#92170=CARTESIAN_POINT('',(-8.376,22.032,8.976));
#92171=CARTESIAN_POINT('',(-8.376,22.032,-12.24));
#92172=CARTESIAN_POINT('',(-8.976,22.032,8.976));
#92173=CARTESIAN_POINT('',(8.376,22.032,8.976));
#92174=CARTESIAN_POINT('',(-8.976,22.032,8.976));
#92175=CARTESIAN_POINT('',(8.376,22.032,-11.208));
#92176=CARTESIAN_POINT('',(8.376,22.032,0.408000000000001));
#92177=CARTESIAN_POINT('',(4.08,22.032,-11.208));
#92178=CARTESIAN_POINT('',(27.528,22.032,-11.208));
#92179=CARTESIAN_POINT('',(4.08,22.032,-11.208));
#92180=CARTESIAN_POINT('',(27.528,22.032,-9.384));
#92181=CARTESIAN_POINT('',(-6.72,22.032,-18.552));
#92182=CARTESIAN_POINT('',(-6.72,22.032,-5.112));
#92183=CARTESIAN_POINT('',(-6.72,22.032,-6.936));
#92184=CARTESIAN_POINT('',(6.72,22.032,-18.552));
#92185=CARTESIAN_POINT('',(-3.06,22.032,-18.552));
#92186=CARTESIAN_POINT('',(6.72,22.032,-5.112));
#92187=CARTESIAN_POINT('',(6.72,22.032,-13.056));
#92188=CARTESIAN_POINT('',(3.06,22.032,-5.112));
#92189=CARTESIAN_POINT('',(-6.72,22.032,-1.416));
#92190=CARTESIAN_POINT('',(-6.72,22.032,6.312));
#92191=CARTESIAN_POINT('',(-6.72,22.032,-1.224));
#92192=CARTESIAN_POINT('',(-0.830275135120883,22.032,-1.416));
#92193=CARTESIAN_POINT('',(-3.06,22.032,-1.416));
#92194=CARTESIAN_POINT('',(0.830275135120883,22.032,-1.416));
#92195=CARTESIAN_POINT('Origin',(0.,22.032,-2.1216));
#92196=CARTESIAN_POINT('',(6.72,22.032,-1.416));
#92197=CARTESIAN_POINT('',(-3.06,22.032,-1.416));
#92198=CARTESIAN_POINT('',(6.72,22.032,6.312));
#92199=CARTESIAN_POINT('',(6.72,22.032,-4.488));
#92200=CARTESIAN_POINT('',(3.06,22.032,6.312));
#92201=CARTESIAN_POINT('',(3.672,22.032,-2.0112));
#92202=CARTESIAN_POINT('Origin',(3.672,22.032,-3.264));
#92203=CARTESIAN_POINT('',(-3.672,22.032,-2.0112));
#92204=CARTESIAN_POINT('Origin',(-3.672,22.032,-3.264));
#92205=CARTESIAN_POINT('Origin',(13.566,7.944,-11.208));
#92206=CARTESIAN_POINT('',(26.928,7.944,-10.608));
#92207=CARTESIAN_POINT('Origin',(27.528,7.944,-11.208));
#92208=CARTESIAN_POINT('',(13.566,7.944,-10.608));
#92209=CARTESIAN_POINT('Origin',(27.528,7.944,-11.424));
#92210=CARTESIAN_POINT('',(26.928,7.944,-11.424));
#92211=CARTESIAN_POINT('Origin',(27.528,19.9512,6.528));
#92212=CARTESIAN_POINT('',(26.928,21.432,5.41906746823804));
#92213=CARTESIAN_POINT('',(26.928,19.9512,8.378));
#92214=CARTESIAN_POINT('Origin',(26.928,19.9512,6.528));
#92215=CARTESIAN_POINT('Origin',(27.528,19.9512,8.378));
#92216=CARTESIAN_POINT('',(26.928,21.432,7.63693253176196));
#92217=CARTESIAN_POINT('Origin',(26.928,19.9512,6.528));
#92218=CARTESIAN_POINT('Ctrl Pts',(26.928,21.432,7.63693253176197));
#92219=CARTESIAN_POINT('Ctrl Pts',(26.928,21.4328877904121,7.63426595627616));
#92220=CARTESIAN_POINT('Ctrl Pts',(26.9280019704154,21.4337726990382,7.63159841831919));
#92221=CARTESIAN_POINT('Ctrl Pts',(26.9283000556252,21.501143162412,7.42777296742251));
#92222=CARTESIAN_POINT('Ctrl Pts',(26.9391026001865,21.5511743233338,7.22145350079341));
#92223=CARTESIAN_POINT('Ctrl Pts',(26.952947201541,21.6048568406253,6.84989504199634));
#92224=CARTESIAN_POINT('Ctrl Pts',(26.9571034769768,21.6166,6.68976413584999));
#92225=CARTESIAN_POINT('Ctrl Pts',(26.9571034769768,21.6166,6.36623586415001));
#92226=CARTESIAN_POINT('Ctrl Pts',(26.952947201541,21.6048568406253,6.20610495800366));
#92227=CARTESIAN_POINT('Ctrl Pts',(26.9391026001865,21.5511743233338,5.83454649920659));
#92228=CARTESIAN_POINT('Ctrl Pts',(26.9283000556252,21.501143162412,5.6282270325775));
#92229=CARTESIAN_POINT('Ctrl Pts',(26.9280019704154,21.4337726990375,5.42440158167857));
#92230=CARTESIAN_POINT('Ctrl Pts',(26.928,21.4328877904128,5.42173404372609));
#92231=CARTESIAN_POINT('Ctrl Pts',(26.928,21.432,5.41906746823803));
#92232=CARTESIAN_POINT('Origin',(27.528,21.432,-9.384));
#92233=CARTESIAN_POINT('',(26.928,21.432,-10.608));
#92234=CARTESIAN_POINT('Origin',(27.528,21.432,-11.208));
#92235=CARTESIAN_POINT('',(26.928,21.432,-9.384));
#92236=CARTESIAN_POINT('',(26.928,21.432,-9.384));
#92237=CARTESIAN_POINT('Origin',(29.784,14.688,0.59750406305912));
#92238=CARTESIAN_POINT('',(28.968,14.688,0.59750406305912));
#92239=CARTESIAN_POINT('',(29.784,14.688,0.59750406305912));
#92240=CARTESIAN_POINT('',(28.968,9.01726475149214,8.8128));
#92241=CARTESIAN_POINT('',(28.968,9.01726475149214,8.8128));
#92242=CARTESIAN_POINT('',(29.784,9.01726475149214,8.8128));
#92243=CARTESIAN_POINT('Origin',(29.184,11.2069968487015,-5.40029406097811));
#92244=CARTESIAN_POINT('',(29.184,15.3820647514921,-0.408));
#92245=CARTESIAN_POINT('Origin',(29.184,14.6530051385802,-0.408000000000001));
#92246=CARTESIAN_POINT('',(29.184,11.7007836305014,-5.74113803425587));
#92247=CARTESIAN_POINT('Origin',(29.784,15.3820647514921,-0.407999999999999));
#92248=CARTESIAN_POINT('',(28.968,15.3820647514921,-0.408));
#92249=CARTESIAN_POINT('',(29.784,15.3820647514921,-0.408));
#92250=CARTESIAN_POINT('',(28.968,21.0528,7.80729593694088));
#92251=CARTESIAN_POINT('Origin',(29.184,18.810984851675,-6.43173984076555));
#92252=CARTESIAN_POINT('',(29.184,21.0528,-8.62329593694088));
#92253=CARTESIAN_POINT('Origin',(29.184,21.0528,-9.67949768385172));
#92254=CARTESIAN_POINT('',(29.184,19.3047716334749,-6.09089586748779));
#92255=CARTESIAN_POINT('Origin',(29.784,21.0528,-8.62329593694088));
#92256=CARTESIAN_POINT('',(28.968,21.0528,-8.62329593694088));
#92257=CARTESIAN_POINT('',(29.784,21.0528,-8.62329593694088));
#92258=CARTESIAN_POINT('',(28.968,15.3820647514921,-0.408));
#92259=CARTESIAN_POINT('Origin',(29.184,13.8513676242539,-10.2288));
#92260=CARTESIAN_POINT('',(29.184,13.8513676242539,-9.6288));
#92261=CARTESIAN_POINT('',(29.7662589059854,7.8680259866208,-10.0839740133792));
#92262=CARTESIAN_POINT('Origin',(29.184,7.7232,-10.2288));
#92263=CARTESIAN_POINT('Origin',(29.184,7.94403556938437,-10.2288));
#92264=CARTESIAN_POINT('Origin',(29.784,20.3587352485079,-9.6288));
#92265=CARTESIAN_POINT('',(28.968,9.01726475149214,-9.6288));
#92266=CARTESIAN_POINT('Origin',(29.184,7.944,-13.272));
#92267=CARTESIAN_POINT('Origin',(29.184,7.944,-13.272));
#92268=CARTESIAN_POINT('Origin',(29.184,7.7232,-9.61564796847044));
#92269=CARTESIAN_POINT('Origin',(29.184,7.7232,-10.5487284530825));
#92270=CARTESIAN_POINT('',(29.184,8.3232,-9.61564796847044));
#92271=CARTESIAN_POINT('Origin',(29.184,11.0304206445356,-5.7574985449732));
#92272=CARTESIAN_POINT('Origin',(29.184,7.344,-13.272));
#92273=CARTESIAN_POINT('Origin',(29.184,21.432,-13.272));
#92274=CARTESIAN_POINT('Origin',(14.892,21.432,-13.272));
#92275=CARTESIAN_POINT('Origin',(29.184,21.432,-13.272));
#92276=CARTESIAN_POINT('Origin',(8.976,21.432,-13.272));
#92277=CARTESIAN_POINT('Origin',(29.184,21.432,-13.272));
#92278=CARTESIAN_POINT('Origin',(-7.752,8.76,9.192));
#92279=CARTESIAN_POINT('',(-14.064,8.76,9.792));
#92280=CARTESIAN_POINT('',(-7.752,8.76,9.792));
#92281=CARTESIAN_POINT('Origin',(-14.064,8.76,9.192));
#92282=CARTESIAN_POINT('Origin',(-15.504,7.344,9.792));
#92283=CARTESIAN_POINT('',(-14.064,7.944,9.792));
#92284=CARTESIAN_POINT('',(-14.064,7.344,9.792));
#92285=CARTESIAN_POINT('',(-14.064,15.72,9.792));
#92286=CARTESIAN_POINT('',(-13.158,15.72,9.792));
#92287=CARTESIAN_POINT('',(-14.064,21.432,9.792));
#92288=CARTESIAN_POINT('',(-14.064,7.344,9.792));
#92289=CARTESIAN_POINT('',(-14.904,21.432,9.792));
#92290=CARTESIAN_POINT('',(-7.752,21.432,9.792));
#92291=CARTESIAN_POINT('',(-14.904,7.944,9.792));
#92292=CARTESIAN_POINT('',(-14.904,7.344,9.792));
#92293=CARTESIAN_POINT('',(-17.238,7.944,9.792));
#92294=CARTESIAN_POINT('Origin',(-13.158,15.72,9.192));
#92295=CARTESIAN_POINT('',(-13.464,16.32,9.192));
#92296=CARTESIAN_POINT('Origin',(-14.064,15.72,9.192));
#92297=CARTESIAN_POINT('',(-13.158,16.32,9.192));
#92298=CARTESIAN_POINT('Origin',(-14.904,10.6896,-3.264));
#92299=CARTESIAN_POINT('',(-15.504,10.6896,-1.164));
#92300=CARTESIAN_POINT('Origin',(-15.504,10.6896,-3.264));
#92301=CARTESIAN_POINT('',(-14.904,10.6896,-1.764));
#92302=CARTESIAN_POINT('Origin',(-14.904,10.6896,-1.164));
#92303=CARTESIAN_POINT('Origin',(-14.904,10.6896,-3.264));
#92304=CARTESIAN_POINT('Origin',(-13.464,10.6896,-3.264));
#92305=CARTESIAN_POINT('',(-14.064,10.6896,-4.764));
#92306=CARTESIAN_POINT('',(-14.064,10.6896,-1.764));
#92307=CARTESIAN_POINT('Origin',(-14.064,10.6896,-3.264));
#92308=CARTESIAN_POINT('Origin',(-14.064,10.6896,-3.264));
#92309=CARTESIAN_POINT('',(-13.464,10.6896,-1.764));
#92310=CARTESIAN_POINT('Origin',(-15.504,7.344,-10.608));
#92311=CARTESIAN_POINT('',(-15.504,21.432,5.41906746823804));
#92312=CARTESIAN_POINT('',(-15.504,19.9512,8.378));
#92313=CARTESIAN_POINT('Origin',(-15.504,19.9512,6.528));
#92314=CARTESIAN_POINT('',(-15.504,21.432,-10.608));
#92315=CARTESIAN_POINT('',(-15.504,21.432,-9.384));
#92316=CARTESIAN_POINT('',(-15.504,7.944,-10.608));
#92317=CARTESIAN_POINT('',(-15.504,7.344,-10.608));
#92318=CARTESIAN_POINT('',(-15.504,7.944,9.192));
#92319=CARTESIAN_POINT('',(-15.504,7.944,-11.424));
#92320=CARTESIAN_POINT('',(-15.504,21.432,9.192));
#92321=CARTESIAN_POINT('',(-15.504,7.344,9.192));
#92322=CARTESIAN_POINT('',(-15.504,21.432,7.63693253176196));
#92323=CARTESIAN_POINT('',(-15.504,21.432,-9.384));
#92324=CARTESIAN_POINT('Origin',(-15.504,19.9512,6.528));
#92325=CARTESIAN_POINT('Origin',(-14.904,19.9512,6.528));
#92326=CARTESIAN_POINT('',(-14.904,19.9512,7.778));
#92327=CARTESIAN_POINT('Origin',(-14.904,19.9512,8.378));
#92328=CARTESIAN_POINT('Origin',(-14.904,19.9512,6.528));
#92329=CARTESIAN_POINT('Ctrl Pts',(-15.504,21.432,7.63693253176197));
#92330=CARTESIAN_POINT('Ctrl Pts',(-15.504,21.4328877903851,7.63426595635721));
#92331=CARTESIAN_POINT('Ctrl Pts',(-15.5039980295845,21.4337726990646,7.63159841823831));
#92332=CARTESIAN_POINT('Ctrl Pts',(-15.5036999443769,21.5011431619309,7.42777296889831));
#92333=CARTESIAN_POINT('Ctrl Pts',(-15.4928973998635,21.5511743231396,7.22145350213754));
#92334=CARTESIAN_POINT('Ctrl Pts',(-15.479052798459,21.6048568406253,6.84989504199625));
#92335=CARTESIAN_POINT('Ctrl Pts',(-15.4748965230232,21.6166,6.68976413584994));
#92336=CARTESIAN_POINT('Ctrl Pts',(-15.4748965230232,21.6166,6.36623586415006));
#92337=CARTESIAN_POINT('Ctrl Pts',(-15.479052798459,21.6048568406253,6.20610495800375));
#92338=CARTESIAN_POINT('Ctrl Pts',(-15.4928973998635,21.5511743231396,5.83454649786246));
#92339=CARTESIAN_POINT('Ctrl Pts',(-15.5036999443769,21.5011431619309,5.62822703110169));
#92340=CARTESIAN_POINT('Ctrl Pts',(-15.5039980295845,21.4337726990639,5.42440158175944));
#92341=CARTESIAN_POINT('Ctrl Pts',(-15.504,21.4328877903859,5.42173404364504));
#92342=CARTESIAN_POINT('Ctrl Pts',(-15.504,21.432,5.41906746823803));
#92343=CARTESIAN_POINT('Origin',(-14.904,21.432,-9.384));
#92344=CARTESIAN_POINT('Origin',(-14.904,21.432,9.192));
#92345=CARTESIAN_POINT('Origin',(-14.904,21.432,-11.208));
#92346=CARTESIAN_POINT('Origin',(-13.464,19.9512,6.528));
#92347=CARTESIAN_POINT('',(-14.064,19.9512,5.278));
#92348=CARTESIAN_POINT('',(-14.064,19.9512,7.778));
#92349=CARTESIAN_POINT('Origin',(-14.064,19.9512,6.528));
#92350=CARTESIAN_POINT('Origin',(-14.064,19.9512,6.528));
#92351=CARTESIAN_POINT('',(-13.464,19.9512,7.778));
#92352=CARTESIAN_POINT('Origin',(26.928,7.344,-10.608));
#92353=CARTESIAN_POINT('',(26.928,7.344,-10.608));
#92354=CARTESIAN_POINT('',(26.928,10.6896,-1.164));
#92355=CARTESIAN_POINT('Origin',(26.928,10.6896,-3.264));
#92356=CARTESIAN_POINT('Origin',(4.08,21.432,-11.208));
#92357=CARTESIAN_POINT('',(4.08,21.432,-10.608));
#92358=CARTESIAN_POINT('Origin',(8.16,7.344,-10.608));
#92359=CARTESIAN_POINT('Origin',(4.08,21.432,-11.208));
#92360=CARTESIAN_POINT('Origin',(8.376,21.432,-11.208));
#92361=CARTESIAN_POINT('Origin',(8.376,21.432,0.408000000000001));
#92362=CARTESIAN_POINT('',(8.976,21.432,8.976));
#92363=CARTESIAN_POINT('Origin',(8.376,21.432,8.976));
#92364=CARTESIAN_POINT('',(8.976,21.432,0.408000000000001));
#92365=CARTESIAN_POINT('Origin',(-8.976,8.16,8.976));
#92366=CARTESIAN_POINT('',(8.976,8.16,8.976));
#92367=CARTESIAN_POINT('Origin',(-8.376,21.432,-12.24));
#92368=CARTESIAN_POINT('',(-8.976,21.432,8.976));
#92369=CARTESIAN_POINT('Origin',(-8.376,21.432,8.976));
#92370=CARTESIAN_POINT('',(-8.976,21.432,-10.608));
#92371=CARTESIAN_POINT('Origin',(-8.376,21.432,-11.208));
#92372=CARTESIAN_POINT('',(-8.976,21.432,-12.24));
#92373=CARTESIAN_POINT('Origin',(-8.976,8.16,-16.32));
#92374=CARTESIAN_POINT('',(-8.976,16.32,-4.08));
#92375=CARTESIAN_POINT('',(-8.976,8.16,8.976));
#92376=CARTESIAN_POINT('',(-8.976,7.752,-10.608));
#92377=CARTESIAN_POINT('Origin',(-14.892,21.432,-11.208));
#92378=CARTESIAN_POINT('',(-13.464,21.432,-10.608));
#92379=CARTESIAN_POINT('Origin',(-14.064,21.432,-11.208));
#92380=CARTESIAN_POINT('',(-14.892,21.432,-10.608));
#92381=CARTESIAN_POINT('Origin',(-29.784,7.344,-10.608));
#92382=CARTESIAN_POINT('',(-13.464,7.944,-10.608));
#92383=CARTESIAN_POINT('',(-13.464,7.344,-10.608));
#92384=CARTESIAN_POINT('',(-8.76,7.944,-10.608));
#92385=CARTESIAN_POINT('',(-24.378,7.944,-10.608));
#92386=CARTESIAN_POINT('',(-8.76,7.344,-10.608));
#92387=CARTESIAN_POINT('Origin',(-14.892,21.432,-11.208));
#92388=CARTESIAN_POINT('',(-26.928,21.432,-10.608));
#92389=CARTESIAN_POINT('Origin',(-26.928,21.432,-11.208));
#92390=CARTESIAN_POINT('',(-14.892,21.432,-10.608));
#92391=CARTESIAN_POINT('Origin',(-29.784,7.344,-10.608));
#92392=CARTESIAN_POINT('',(-26.928,7.944,-10.608));
#92393=CARTESIAN_POINT('',(-26.928,7.344,-10.608));
#92394=CARTESIAN_POINT('',(-24.378,7.944,-10.608));
#92395=CARTESIAN_POINT('Origin',(3.06,21.432,-5.112));
#92396=CARTESIAN_POINT('',(6.12,21.432,-5.712));
#92397=CARTESIAN_POINT('Origin',(6.72,21.432,-5.112));
#92398=CARTESIAN_POINT('',(-6.12,21.432,-5.712));
#92399=CARTESIAN_POINT('',(3.06,21.432,-5.712));
#92400=CARTESIAN_POINT('Origin',(-6.72,21.432,-5.112));
#92401=CARTESIAN_POINT('Origin',(6.12,22.032,-5.712));
#92402=CARTESIAN_POINT('',(6.12,16.32,-5.712));
#92403=CARTESIAN_POINT('',(6.12,22.032,-5.712));
#92404=CARTESIAN_POINT('',(5.47389440891949,16.32,-5.712));
#92405=CARTESIAN_POINT('',(6.12,16.32,-5.712));
#92406=CARTESIAN_POINT('',(-5.47389440891949,16.32,-5.712));
#92407=CARTESIAN_POINT('Origin',(0.,14.688,-5.712));
#92408=CARTESIAN_POINT('',(-6.12,16.32,-5.712));
#92409=CARTESIAN_POINT('',(6.12,16.32,-5.712));
#92410=CARTESIAN_POINT('',(-6.12,22.032,-5.712));
#92411=CARTESIAN_POINT('Origin',(-3.06,21.432,-18.552));
#92412=CARTESIAN_POINT('',(-6.12,21.432,-17.952));
#92413=CARTESIAN_POINT('Origin',(-6.72,21.432,-18.552));
#92414=CARTESIAN_POINT('',(6.12,21.432,-17.952));
#92415=CARTESIAN_POINT('',(-3.06,21.432,-17.952));
#92416=CARTESIAN_POINT('Origin',(6.72,21.432,-18.552));
#92417=CARTESIAN_POINT('Origin',(-6.12,22.032,-17.952));
#92418=CARTESIAN_POINT('',(-6.12,16.32,-17.952));
#92419=CARTESIAN_POINT('',(-6.12,22.032,-17.952));
#92420=CARTESIAN_POINT('',(-5.47389440891949,16.32,-17.952));
#92421=CARTESIAN_POINT('',(-6.12,16.32,-17.952));
#92422=CARTESIAN_POINT('',(5.47389440891949,16.32,-17.952));
#92423=CARTESIAN_POINT('Origin',(0.,14.688,-17.952));
#92424=CARTESIAN_POINT('',(6.12,16.32,-17.952));
#92425=CARTESIAN_POINT('',(-6.12,16.32,-17.952));
#92426=CARTESIAN_POINT('',(6.12,22.032,-17.952));
#92427=CARTESIAN_POINT('Origin',(3.06,21.432,6.312));
#92428=CARTESIAN_POINT('',(6.12,21.432,5.712));
#92429=CARTESIAN_POINT('Origin',(6.72,21.432,6.312));
#92430=CARTESIAN_POINT('',(-6.12,21.432,5.712));
#92431=CARTESIAN_POINT('',(3.06,21.432,5.712));
#92432=CARTESIAN_POINT('Origin',(-6.72,21.432,6.312));
#92433=CARTESIAN_POINT('Origin',(6.12,22.032,5.712));
#92434=CARTESIAN_POINT('',(6.12,16.32,5.712));
#92435=CARTESIAN_POINT('',(6.12,22.032,5.712));
#92436=CARTESIAN_POINT('',(5.47389440891949,16.32,5.712));
#92437=CARTESIAN_POINT('',(6.12,16.32,5.712));
#92438=CARTESIAN_POINT('',(-5.47389440891949,16.32,5.712));
#92439=CARTESIAN_POINT('Origin',(0.,14.688,5.712));
#92440=CARTESIAN_POINT('',(-6.12,16.32,5.712));
#92441=CARTESIAN_POINT('',(6.12,16.32,5.712));
#92442=CARTESIAN_POINT('',(-6.12,22.032,5.712));
#92443=CARTESIAN_POINT('Origin',(-3.06,21.432,-1.416));
#92444=CARTESIAN_POINT('',(-1.07003852625037E-16,22.0004505255517,-1.224));
#92445=CARTESIAN_POINT('Ctrl Pts',(0.830275135120883,22.032,-1.416));
#92446=CARTESIAN_POINT('Ctrl Pts',(0.828552577377265,22.032,-1.4152033217116));
#92447=CARTESIAN_POINT('Ctrl Pts',(0.826829075614662,22.0319984132633,-1.41440868610083));
#92448=CARTESIAN_POINT('Ctrl Pts',(0.70474528426719,22.0317754702238,-1.35829688696515));
#92449=CARTESIAN_POINT('Ctrl Pts',(0.580104214213408,22.024045489527,-1.31311205364223));
#92450=CARTESIAN_POINT('Ctrl Pts',(0.30409125108285,22.0079879748714,-1.24371396306971));
#92451=CARTESIAN_POINT('Ctrl Pts',(0.153641828682257,22.0004505255517,-1.224));
#92452=CARTESIAN_POINT('Ctrl Pts',(6.93889390390723E-17,22.0004505255517,
-1.224));
#92453=CARTESIAN_POINT('Ctrl Pts',(-1.04083408558608E-16,22.0004505255517,
-1.224));
#92454=CARTESIAN_POINT('Ctrl Pts',(-0.153641828682253,22.0004505255517,
-1.224));
#92455=CARTESIAN_POINT('Ctrl Pts',(-0.304091251082843,22.0079879748714,
-1.24371396306971));
#92456=CARTESIAN_POINT('Ctrl Pts',(-0.580104214214111,22.024045489527,-1.31311205364241));
#92457=CARTESIAN_POINT('Ctrl Pts',(-0.704745284267943,22.0317754702238,
-1.35829688696549));
#92458=CARTESIAN_POINT('Ctrl Pts',(-0.826829075614615,22.0319984132633,
-1.41440868610081));
#92459=CARTESIAN_POINT('Ctrl Pts',(-0.828552577377312,22.032,-1.41520332171162));
#92460=CARTESIAN_POINT('Ctrl Pts',(-0.830275135120883,22.032,-1.416));
#92461=CARTESIAN_POINT('',(-6.12,21.432,-0.816));
#92462=CARTESIAN_POINT('Origin',(-6.72,21.432,-1.416));
#92463=CARTESIAN_POINT('',(6.12,21.432,-0.816));
#92464=CARTESIAN_POINT('',(-3.06,21.432,-0.816));
#92465=CARTESIAN_POINT('Origin',(6.72,21.432,-1.416));
#92466=CARTESIAN_POINT('Origin',(-6.12,22.032,-0.816));
#92467=CARTESIAN_POINT('',(-6.12,16.32,-0.816));
#92468=CARTESIAN_POINT('',(-6.12,22.032,-0.816));
#92469=CARTESIAN_POINT('',(-5.47389440891949,16.32,-0.815999999999999));
#92470=CARTESIAN_POINT('',(-6.12,16.32,-0.816));
#92471=CARTESIAN_POINT('',(5.47389440891949,16.32,-0.815999999999999));
#92472=CARTESIAN_POINT('Origin',(0.,14.688,-0.815999999999999));
#92473=CARTESIAN_POINT('',(6.12,16.32,-0.816));
#92474=CARTESIAN_POINT('',(-6.12,16.32,-0.816));
#92475=CARTESIAN_POINT('',(6.12,22.032,-0.816));
#92476=CARTESIAN_POINT('Origin',(0.,21.432,-2.1216));
#92477=CARTESIAN_POINT('',(-5.99587072862544E-17,21.432,-1.632));
#92478=CARTESIAN_POINT('Origin',(-1.33437515235096E-16,21.432,-1.032));
#92479=CARTESIAN_POINT('',(-0.4896,21.432,-2.1216));
#92480=CARTESIAN_POINT('Origin',(0.,21.432,-2.1216));
#92481=CARTESIAN_POINT('Origin',(0.,21.432,-2.1216));
#92482=CARTESIAN_POINT('Origin',(-6.72,21.432,-1.224));
#92483=CARTESIAN_POINT('',(-6.12,21.432,-1.224));
#92484=CARTESIAN_POINT('Origin',(-6.12,22.032,5.712));
#92485=CARTESIAN_POINT('',(-6.12,16.32,5.712));
#92486=CARTESIAN_POINT('Origin',(6.72,21.432,-4.488));
#92487=CARTESIAN_POINT('',(6.12,21.432,-4.488));
#92488=CARTESIAN_POINT('Origin',(6.12,22.032,-0.816));
#92489=CARTESIAN_POINT('',(6.12,16.32,-0.816));
#92490=CARTESIAN_POINT('Origin',(-6.72,21.432,-6.936));
#92491=CARTESIAN_POINT('',(-6.12,21.432,-6.936));
#92492=CARTESIAN_POINT('Origin',(-6.12,22.032,-5.712));
#92493=CARTESIAN_POINT('',(-6.12,16.32,-5.712));
#92494=CARTESIAN_POINT('Origin',(6.72,21.432,-13.056));
#92495=CARTESIAN_POINT('',(6.12,21.432,-13.056));
#92496=CARTESIAN_POINT('Origin',(6.12,22.032,-17.952));
#92497=CARTESIAN_POINT('',(6.12,16.32,-17.952));
#92498=CARTESIAN_POINT('Origin',(-3.672,21.432,-3.264));
#92499=CARTESIAN_POINT('',(-3.672,21.432,-2.6112));
#92500=CARTESIAN_POINT('Origin',(-3.672,21.432,-2.0112));
#92501=CARTESIAN_POINT('',(-4.3248,21.432,-3.264));
#92502=CARTESIAN_POINT('Origin',(-3.672,21.432,-3.264));
#92503=CARTESIAN_POINT('Origin',(-3.672,21.432,-3.264));
#92504=CARTESIAN_POINT('Origin',(-3.672,22.032,-3.264));
#92505=CARTESIAN_POINT('',(-4.3248,20.808,-3.264));
#92506=CARTESIAN_POINT('',(-4.3248,22.032,-3.264));
#92507=CARTESIAN_POINT('Origin',(-3.672,20.808,-3.264));
#92508=CARTESIAN_POINT('Origin',(3.672,21.432,-3.264));
#92509=CARTESIAN_POINT('',(3.672,21.432,-2.6112));
#92510=CARTESIAN_POINT('Origin',(3.672,21.432,-2.0112));
#92511=CARTESIAN_POINT('',(3.0192,21.432,-3.264));
#92512=CARTESIAN_POINT('Origin',(3.672,21.432,-3.264));
#92513=CARTESIAN_POINT('Origin',(3.672,21.432,-3.264));
#92514=CARTESIAN_POINT('Origin',(3.672,22.032,-3.264));
#92515=CARTESIAN_POINT('',(3.0192,20.808,-3.264));
#92516=CARTESIAN_POINT('',(3.0192,22.032,-3.264));
#92517=CARTESIAN_POINT('Origin',(3.672,20.808,-3.264));
#92518=CARTESIAN_POINT('Origin',(0.,22.032,-2.1216));
#92519=CARTESIAN_POINT('',(-0.4896,20.808,-2.1216));
#92520=CARTESIAN_POINT('',(-0.4896,22.032,-2.1216));
#92521=CARTESIAN_POINT('Origin',(0.,20.808,-2.1216));
#92522=CARTESIAN_POINT('Origin',(-4.896,21.432,-21.216));
#92523=CARTESIAN_POINT('',(-3.45144894062868,21.7056,-19.775558318824));
#92524=CARTESIAN_POINT('Origin',(-4.896,21.7056,-21.216));
#92525=CARTESIAN_POINT('Origin',(-3.07332505037306,21.432,-19.3985100942983));
#92526=CARTESIAN_POINT('Origin',(-14.064,19.9512,6.528));
#92527=CARTESIAN_POINT('',(-13.464,21.432,7.63693253176196));
#92528=CARTESIAN_POINT('',(-13.464,19.9512,4.678));
#92529=CARTESIAN_POINT('Origin',(-13.464,19.9512,6.528));
#92530=CARTESIAN_POINT('Origin',(-14.064,19.9512,4.678));
#92531=CARTESIAN_POINT('',(-13.464,21.432,5.41906746823804));
#92532=CARTESIAN_POINT('Origin',(-13.464,19.9512,6.528));
#92533=CARTESIAN_POINT('Ctrl Pts',(-13.464,21.432,5.41906746823803));
#92534=CARTESIAN_POINT('Ctrl Pts',(-13.464,21.4328877903851,5.42173404364279));
#92535=CARTESIAN_POINT('Ctrl Pts',(-13.4640019704155,21.4337726990646,5.42440158176169));
#92536=CARTESIAN_POINT('Ctrl Pts',(-13.4643000556231,21.5011431619309,5.62822703110169));
#92537=CARTESIAN_POINT('Ctrl Pts',(-13.4751026001365,21.5511743231396,5.83454649786246));
#92538=CARTESIAN_POINT('Ctrl Pts',(-13.488947201541,21.6048568406253,6.20610495800375));
#92539=CARTESIAN_POINT('Ctrl Pts',(-13.4931034769768,21.6166,6.36623586415006));
#92540=CARTESIAN_POINT('Ctrl Pts',(-13.4931034769768,21.6166,6.68976413584994));
#92541=CARTESIAN_POINT('Ctrl Pts',(-13.488947201541,21.6048568406253,6.84989504199625));
#92542=CARTESIAN_POINT('Ctrl Pts',(-13.4751026001365,21.5511743231396,7.22145350213754));
#92543=CARTESIAN_POINT('Ctrl Pts',(-13.4643000556231,21.5011431619309,7.42777296889831));
#92544=CARTESIAN_POINT('Ctrl Pts',(-13.4640019704155,21.4337726990639,7.63159841824056));
#92545=CARTESIAN_POINT('Ctrl Pts',(-13.464,21.4328877903859,7.63426595635496));
#92546=CARTESIAN_POINT('Ctrl Pts',(-13.464,21.432,7.63693253176197));
#92547=CARTESIAN_POINT('Origin',(-14.064,21.432,0.816000000000001));
#92548=CARTESIAN_POINT('',(-13.464,21.432,0.816000000000001));
#92549=CARTESIAN_POINT('',(-13.464,21.432,9.192));
#92550=CARTESIAN_POINT('Origin',(-14.064,21.432,9.192));
#92551=CARTESIAN_POINT('',(-13.464,21.432,0.816000000000001));
#92552=CARTESIAN_POINT('Origin',(-14.064,10.6896,-3.264));
#92553=CARTESIAN_POINT('',(-13.464,10.6896,-5.364));
#92554=CARTESIAN_POINT('Origin',(-13.464,10.6896,-3.264));
#92555=CARTESIAN_POINT('Origin',(-14.064,10.6896,-5.364));
#92556=CARTESIAN_POINT('Origin',(-13.464,7.344,9.792));
#92557=CARTESIAN_POINT('',(-13.464,7.344,9.192));
#92558=CARTESIAN_POINT('',(-13.464,16.32,8.976));
#92559=CARTESIAN_POINT('',(-13.464,7.944,9.192));
#92560=CARTESIAN_POINT('',(-13.464,7.344,9.192));
#92561=CARTESIAN_POINT('',(-13.464,7.944,-1.224));
#92562=CARTESIAN_POINT('Origin',(-7.752,21.432,9.192));
#92563=CARTESIAN_POINT('Origin',(-14.904,21.432,9.192));
#92564=CARTESIAN_POINT('Origin',(-14.064,21.432,9.192));
#92565=CARTESIAN_POINT('Origin',(-14.064,7.344,9.192));
#92566=CARTESIAN_POINT('Origin',(-14.064,21.432,9.192));
#92567=CARTESIAN_POINT('Origin',(-14.064,21.432,9.192));
#92568=CARTESIAN_POINT('Origin',(-14.904,21.432,9.192));
#92569=CARTESIAN_POINT('Origin',(-14.904,21.432,9.192));
#92570=CARTESIAN_POINT('Origin',(-14.904,7.344,9.192));
#92571=CARTESIAN_POINT('Origin',(-14.904,7.944,9.192));
#92572=CARTESIAN_POINT('Origin',(-14.064,7.944,-1.224));
#92573=CARTESIAN_POINT('',(-14.064,7.344,9.192));
#92574=CARTESIAN_POINT('Origin',(-14.064,7.944,9.192));
#92575=CARTESIAN_POINT('',(-14.064,7.344,-11.208));
#92576=CARTESIAN_POINT('',(-14.064,7.344,-1.224));
#92577=CARTESIAN_POINT('Origin',(-14.064,7.944,-11.208));
#92578=CARTESIAN_POINT('Origin',(-14.064,7.344,9.192));
#92579=CARTESIAN_POINT('Origin',(-14.064,7.944,9.192));
#92580=CARTESIAN_POINT('Origin',(-14.064,7.944,9.192));
#92581=CARTESIAN_POINT('Origin',(-14.064,7.944,9.192));
#92582=CARTESIAN_POINT('Origin',(-18.972,7.344,-12.24));
#92583=CARTESIAN_POINT('',(-8.76,7.344,-11.208));
#92584=CARTESIAN_POINT('',(-24.378,7.344,-11.208));
#92585=CARTESIAN_POINT('',(-14.904,7.344,9.192));
#92586=CARTESIAN_POINT('',(-17.238,7.344,9.192));
#92587=CARTESIAN_POINT('',(-14.904,7.344,-11.208));
#92588=CARTESIAN_POINT('',(-14.904,7.344,-11.424));
#92589=CARTESIAN_POINT('',(-26.928,7.344,-11.208));
#92590=CARTESIAN_POINT('',(-24.378,7.344,-11.208));
#92591=CARTESIAN_POINT('',(-26.928,7.344,9.192));
#92592=CARTESIAN_POINT('',(-26.928,7.344,-10.608));
#92593=CARTESIAN_POINT('',(-27.528,7.344,9.792));
#92594=CARTESIAN_POINT('Origin',(-27.528,7.344,9.192));
#92595=CARTESIAN_POINT('',(-29.184,7.344,9.792));
#92596=CARTESIAN_POINT('',(-26.928,7.344,9.792));
#92597=CARTESIAN_POINT('',(-29.184,7.344,-13.272));
#92598=CARTESIAN_POINT('',(-29.184,7.344,-13.056));
#92599=CARTESIAN_POINT('',(-8.76,7.344,-13.272));
#92600=CARTESIAN_POINT('',(-13.566,7.344,-13.272));
#92601=CARTESIAN_POINT('',(-8.76,7.344,-11.424));
#92602=CARTESIAN_POINT('Origin',(-17.238,7.944,9.192));
#92603=CARTESIAN_POINT('Origin',(-14.904,7.944,9.192));
#92604=CARTESIAN_POINT('Origin',(-8.76,7.344,-13.272));
#92605=CARTESIAN_POINT('',(-8.16,7.944,-13.272));
#92606=CARTESIAN_POINT('',(-8.76,7.944,-13.872));
#92607=CARTESIAN_POINT('Origin',(-8.76,7.944,-13.272));
#92608=CARTESIAN_POINT('',(-8.76,7.344,-13.872));
#92609=CARTESIAN_POINT('',(-8.16,7.344,-13.272));
#92610=CARTESIAN_POINT('Origin',(-8.76,7.944,-11.424));
#92611=CARTESIAN_POINT('Origin',(-8.76,7.944,-13.272));
#92612=CARTESIAN_POINT('',(-8.16,7.944,-11.208));
#92613=CARTESIAN_POINT('',(-8.16,7.944,-11.424));
#92614=CARTESIAN_POINT('Origin',(-8.76,7.944,-11.208));
#92615=CARTESIAN_POINT('Origin',(-8.76,7.344,-11.208));
#92616=CARTESIAN_POINT('Origin',(-8.76,7.944,-11.208));
#92617=CARTESIAN_POINT('',(-8.16,7.344,-11.208));
#92618=CARTESIAN_POINT('Origin',(-8.76,7.944,-11.208));
#92619=CARTESIAN_POINT('Origin',(-8.76,7.944,-11.208));
#92620=CARTESIAN_POINT('Origin',(-8.76,7.944,-13.272));
#92621=CARTESIAN_POINT('Origin',(-8.76,7.944,-13.272));
#92622=CARTESIAN_POINT('Origin',(-8.16,7.344,-13.872));
#92623=CARTESIAN_POINT('',(-29.184,7.944,-13.872));
#92624=CARTESIAN_POINT('',(-13.566,7.944,-13.872));
#92625=CARTESIAN_POINT('',(-29.184,21.432,-13.872));
#92626=CARTESIAN_POINT('',(-29.184,7.344,-13.872));
#92627=CARTESIAN_POINT('',(-4.08,21.432,-13.872));
#92628=CARTESIAN_POINT('Origin',(-13.566,7.944,-13.272));
#92629=CARTESIAN_POINT('Origin',(-29.184,7.944,-13.272));
#92630=CARTESIAN_POINT('Origin',(-24.378,7.944,-11.208));
#92631=CARTESIAN_POINT('Origin',(-14.904,7.944,-11.424));
#92632=CARTESIAN_POINT('Origin',(-14.904,7.944,9.192));
#92633=CARTESIAN_POINT('Origin',(-14.904,7.944,-11.208));
#92634=CARTESIAN_POINT('Origin',(-14.904,7.944,9.192));
#92635=CARTESIAN_POINT('Origin',(-27.528,19.9512,6.528));
#92636=CARTESIAN_POINT('',(-26.928,19.9512,4.678));
#92637=CARTESIAN_POINT('Origin',(-26.928,19.9512,6.528));
#92638=CARTESIAN_POINT('',(-27.528,19.9512,5.278));
#92639=CARTESIAN_POINT('Origin',(-27.528,19.9512,4.678));
#92640=CARTESIAN_POINT('',(-27.528,19.9512,7.778));
#92641=CARTESIAN_POINT('Origin',(-27.528,19.9512,6.528));
#92642=CARTESIAN_POINT('Origin',(-27.528,19.9512,6.528));
#92643=CARTESIAN_POINT('Origin',(-13.464,19.9512,6.528));
#92644=CARTESIAN_POINT('',(-29.6730897616957,19.9512000004902,7.778));
#92645=CARTESIAN_POINT('',(-13.464,19.9512,7.778));
#92646=CARTESIAN_POINT('',(-29.784,20.3324059608682,7.71845454150864));
#92647=CARTESIAN_POINT('Ctrl Pts',(-29.784,20.3324059608683,7.71845454150862));
#92648=CARTESIAN_POINT('Ctrl Pts',(-29.784,20.2498877771073,7.74487841779528));
#92649=CARTESIAN_POINT('Ctrl Pts',(-29.7660314239133,20.1601533655831,7.76339914860449));
#92650=CARTESIAN_POINT('Ctrl Pts',(-29.7162857661367,20.0320859161528,7.77611545312242));
#92651=CARTESIAN_POINT('Ctrl Pts',(-29.6960587249165,19.9904757157273,7.77799999996919));
#92652=CARTESIAN_POINT('Ctrl Pts',(-29.6730897616957,19.9512000009805,7.778));
#92653=CARTESIAN_POINT('',(-29.784,20.8019222240139,7.44384479993544));
#92654=CARTESIAN_POINT('Origin',(-29.784,19.9512,6.528));
#92655=CARTESIAN_POINT('',(-28.968,20.8019222240139,7.44384479993544));
#92656=CARTESIAN_POINT('',(-13.464,20.8019222240139,7.44384479993544));
#92657=CARTESIAN_POINT('',(-28.968,21.0528,7.11874312522449));
#92658=CARTESIAN_POINT('Origin',(-28.968,19.9512,6.528));
#92659=CARTESIAN_POINT('',(-29.784,21.0528,7.11874312522449));
#92660=CARTESIAN_POINT('',(-13.464,21.0528,7.11874312522449));
#92661=CARTESIAN_POINT('',(-29.784,21.2011648366643,6.5186241212227));
#92662=CARTESIAN_POINT('Origin',(-29.784,19.9512,6.528));
#92663=CARTESIAN_POINT('',(-29.184,21.0528,5.93725687477551));
#92664=CARTESIAN_POINT('Ctrl Pts',(-29.184,21.0528,5.93725687477551));
#92665=CARTESIAN_POINT('Ctrl Pts',(-29.1843643716593,21.0528,5.93725687477551));
#92666=CARTESIAN_POINT('Ctrl Pts',(-29.1847287348529,21.0528001568623,5.93725716728446));
#92667=CARTESIAN_POINT('Ctrl Pts',(-29.1850930927556,21.0528004705669,5.93725775227563));
#92668=CARTESIAN_POINT('Ctrl Pts',(-29.1854574506584,21.0528007842715,5.93725833726681));
#92669=CARTESIAN_POINT('Ctrl Pts',(-29.1858218032704,21.0528012548157,5.93725921473157));
#92670=CARTESIAN_POINT('Ctrl Pts',(-29.1861861682784,21.0528018822333,5.9372603847344));
#92671=CARTESIAN_POINT('Ctrl Pts',(-29.1869148982942,21.0528031370684,5.93726272474006));
#92672=CARTESIAN_POINT('Ctrl Pts',(-29.1876437020802,21.0528050195554,5.93726623516292));
#92673=CARTESIAN_POINT('Ctrl Pts',(-29.1883724308858,21.0528075292884,5.93727091538062));
#92674=CARTESIAN_POINT('Ctrl Pts',(-29.2140257893958,21.0528958791364,5.93743567255998));
#92675=CARTESIAN_POINT('Ctrl Pts',(-29.2395868437148,21.0537649140596,5.93904973301454));
#92676=CARTESIAN_POINT('Ctrl Pts',(-29.2648654234066,21.0553765973136,5.9420869196893));
#92677=CARTESIAN_POINT('Ctrl Pts',(-29.2911930452573,21.0570551642177,5.94525014734044));
#92678=CARTESIAN_POINT('Ctrl Pts',(-29.317214696756,21.059538683867,5.94995587684859));
#92679=CARTESIAN_POINT('Ctrl Pts',(-29.3427576953088,21.06274486309,5.95618814364165));
#92680=CARTESIAN_POINT('Ctrl Pts',(-29.3701245988851,21.0661799804457,5.96286542720468));
#92681=CARTESIAN_POINT('Ctrl Pts',(-29.3969434897638,21.0704443645938,5.97129396545307));
#92682=CARTESIAN_POINT('Ctrl Pts',(-29.4230353027292,21.0754000536626,5.9814884852252));
#92683=CARTESIAN_POINT('Ctrl Pts',(-29.436375271561,21.0779337502595,5.98670064032517));
#92684=CARTESIAN_POINT('Ctrl Pts',(-29.4495255641454,21.0806476187178,5.99237507558155));
#92685=CARTESIAN_POINT('Ctrl Pts',(-29.4624629247498,21.0835199890972,5.99851776017422));
#92686=CARTESIAN_POINT('Ctrl Pts',(-29.491900288897,21.0900557126817,6.01249467932527));
#92687=CARTESIAN_POINT('Ctrl Pts',(-29.5199069050774,21.0973412988018,6.02874058300624));
#92688=CARTESIAN_POINT('Ctrl Pts',(-29.546232223272,21.1050194431494,6.04716462401558));
#92689=CARTESIAN_POINT('Ctrl Pts',(-29.5761900183259,21.113757049778,6.06813089080651));
#92690=CARTESIAN_POINT('Ctrl Pts',(-29.6039758940397,21.123003229535,6.09192107855449));
#92691=CARTESIAN_POINT('Ctrl Pts',(-29.6292361556442,21.1321942394425,6.11842373510109));
#92692=CARTESIAN_POINT('Ctrl Pts',(-29.6318717651081,21.1331532125946,6.12118897377937));
#92693=CARTESIAN_POINT('Ctrl Pts',(-29.634479847044,21.1341115517782,6.12398372285587));
#92694=CARTESIAN_POINT('Ctrl Pts',(-29.637059970908,21.1350685929626,6.12680783333075));
#92695=CARTESIAN_POINT('Ctrl Pts',(-29.6606845986466,21.1438316380342,6.15266649833204));
#92696=CARTESIAN_POINT('Ctrl Pts',(-29.6816748166557,21.1523727019991,6.18066728533513));
#92697=CARTESIAN_POINT('Ctrl Pts',(-29.6998946563564,21.1602188363698,6.21055018568484));
#92698=CARTESIAN_POINT('Ctrl Pts',(-29.7145933027143,21.1665486151322,6.23465787222898));
#92699=CARTESIAN_POINT('Ctrl Pts',(-29.727488936724,21.1724272487578,6.25999254756523));
#92700=CARTESIAN_POINT('Ctrl Pts',(-29.7384895609047,21.1776282813931,6.28639364956891));
#92701=CARTESIAN_POINT('Ctrl Pts',(-29.7411248596723,21.1788742356833,6.29271827173847));
#92702=CARTESIAN_POINT('Ctrl Pts',(-29.7436513097999,21.1800813857086,6.2991039028086));
#92703=CARTESIAN_POINT('Ctrl Pts',(-29.74606747585,21.1812467758105,6.30554791680398));
#92704=CARTESIAN_POINT('Ctrl Pts',(-29.7558166581436,21.1859491018555,6.33154938600753));
#92705=CARTESIAN_POINT('Ctrl Pts',(-29.7636632911079,21.1899142199256,6.35820864735865));
#92706=CARTESIAN_POINT('Ctrl Pts',(-29.7696422788167,21.1930311323737,6.38535410754034));
#92707=CARTESIAN_POINT('Ctrl Pts',(-29.7754622120256,21.1960651279512,6.41177743752124));
#92708=CARTESIAN_POINT('Ctrl Pts',(-29.7795115673198,21.1982958942782,6.43866313565451));
#92709=CARTESIAN_POINT('Ctrl Pts',(-29.7817936299994,21.1996502871013,6.46582876709134));
#92710=CARTESIAN_POINT('Ctrl Pts',(-29.7832639221287,21.2005228981499,6.48333109708591));
#92711=CARTESIAN_POINT('Ctrl Pts',(-29.784,21.2010322571302,6.50094900407838));
#92712=CARTESIAN_POINT('Ctrl Pts',(-29.784,21.2011648366643,6.51862412122269));
#92713=CARTESIAN_POINT('',(-28.968,21.0528,5.93725687477551));
#92714=CARTESIAN_POINT('',(-13.464,21.0528,5.93725687477551));
#92715=CARTESIAN_POINT('',(-28.968,19.3965172404536,5.40780937503389));
#92716=CARTESIAN_POINT('Origin',(-28.968,19.9512,6.528));
#92717=CARTESIAN_POINT('',(-29.184,19.3965172404536,5.40780937503389));
#92718=CARTESIAN_POINT('',(-13.464,19.3965172404536,5.40780937503389));
#92719=CARTESIAN_POINT('',(-29.7833084014095,18.9547400881553,5.77330294456311));
#92720=CARTESIAN_POINT('Ctrl Pts',(-29.7833084013013,18.9547400885983,5.77330294490483));
#92721=CARTESIAN_POINT('Ctrl Pts',(-29.780236728844,18.9953746586557,5.71965132428977));
#92722=CARTESIAN_POINT('Ctrl Pts',(-29.7661621997996,19.0422228222755,5.66748165925228));
#92723=CARTESIAN_POINT('Ctrl Pts',(-29.7101860638315,19.1436049154608,5.57097131021595));
#92724=CARTESIAN_POINT('Ctrl Pts',(-29.664083283762,19.1980745167137,5.52887551744315));
#92725=CARTESIAN_POINT('Ctrl Pts',(-29.5569063007166,19.2872387664837,5.46754555210684));
#92726=CARTESIAN_POINT('Ctrl Pts',(-29.4892209293256,19.327765216772,5.4441184609697));
#92727=CARTESIAN_POINT('Ctrl Pts',(-29.3407268100904,19.3825207083351,5.41441389821227));
#92728=CARTESIAN_POINT('Ctrl Pts',(-29.259898021901,19.3965172404535,5.4078093750339));
#92729=CARTESIAN_POINT('Ctrl Pts',(-29.184,19.3965172404535,5.4078093750339));
#92730=CARTESIAN_POINT('',(-29.184,18.7060084170374,6.41846497492097));
#92731=CARTESIAN_POINT('Ctrl Pts',(-29.184,18.7060084170374,6.41846497492091));
#92732=CARTESIAN_POINT('Ctrl Pts',(-29.2236153010039,18.7060084170374,6.41846497492091));
#92733=CARTESIAN_POINT('Ctrl Pts',(-29.2633091750366,18.7065151598125,6.41221228695973));
#92734=CARTESIAN_POINT('Ctrl Pts',(-29.3404403169687,18.7089486562131,6.38854540292828));
#92735=CARTESIAN_POINT('Ctrl Pts',(-29.3778828026048,18.7108927130172,6.37114999797291));
#92736=CARTESIAN_POINT('Ctrl Pts',(-29.4840885147569,18.7201044508453,6.30718343562169));
#92737=CARTESIAN_POINT('Ctrl Pts',(-29.5468609707651,18.7312561019511,6.2486788128922));
#92738=CARTESIAN_POINT('Ctrl Pts',(-29.6514157141007,18.7661319382575,6.1247154358701));
#92739=CARTESIAN_POINT('Ctrl Pts',(-29.6996533413331,18.7937050469554,6.04833557739996));
#92740=CARTESIAN_POINT('Ctrl Pts',(-29.7621956886305,18.8657461678681,5.9034546521282));
#92741=CARTESIAN_POINT('Ctrl Pts',(-29.7797742106915,18.9079869437835,5.83503319047208));
#92742=CARTESIAN_POINT('Ctrl Pts',(-29.7833084015176,18.9547400885983,5.77330294490483));
#92743=CARTESIAN_POINT('',(-28.968,18.7060084170374,6.41846497492097));
#92744=CARTESIAN_POINT('',(-13.464,18.7060084170374,6.41846497492097));
#92745=CARTESIAN_POINT('',(-28.968,19.6120909823364,7.73112305029005));
#92746=CARTESIAN_POINT('Origin',(-28.968,19.9512,6.528));
#92747=CARTESIAN_POINT('',(-29.184,19.6120909823364,7.73112305029005));
#92748=CARTESIAN_POINT('',(-13.464,19.6120909823364,7.73112305029005));
#92749=CARTESIAN_POINT('Ctrl Pts',(-29.6730897616957,19.9512000009805,7.778));
#92750=CARTESIAN_POINT('Ctrl Pts',(-29.6500156297378,19.9117444532444,7.77800000003095));
#92751=CARTESIAN_POINT('Ctrl Pts',(-29.6241709396688,19.8746468475679,7.77610895998165));
#92752=CARTESIAN_POINT('Ctrl Pts',(-29.5468609707651,19.779797513811,7.76771957622778));
#92753=CARTESIAN_POINT('Ctrl Pts',(-29.4840885147569,19.7211400971072,7.75740174366776));
#92754=CARTESIAN_POINT('Ctrl Pts',(-29.3778828026048,19.6580635030103,7.74333332193733));
#92755=CARTESIAN_POINT('Ctrl Pts',(-29.3404403169687,19.6411090544722,7.73898290297035));
#92756=CARTESIAN_POINT('Ctrl Pts',(-29.2633091750366,19.6181170767952,7.73286634617826));
#92757=CARTESIAN_POINT('Ctrl Pts',(-29.2236153010039,19.6120909823365,7.73112305029007));
#92758=CARTESIAN_POINT('Ctrl Pts',(-29.184,19.6120909823365,7.73112305029007));
#92759=CARTESIAN_POINT('Origin',(-26.928,7.344,9.792));
#92760=CARTESIAN_POINT('',(-26.928,7.344,9.192));
#92761=CARTESIAN_POINT('Origin',(-26.928,7.944,-11.208));
#92762=CARTESIAN_POINT('',(-26.928,10.6896,-5.364));
#92763=CARTESIAN_POINT('Origin',(-26.928,10.6896,-3.264));
#92764=CARTESIAN_POINT('Origin',(-24.378,7.944,-11.208));
#92765=CARTESIAN_POINT('Origin',(-8.16,7.344,-10.608));
#92766=CARTESIAN_POINT('Origin',(-29.184,10.6144737596866,-6.36008826276735));
#92767=CARTESIAN_POINT('',(-29.7835166971462,21.456077579674,9.38872242032599));
#92768=CARTESIAN_POINT('',(-29.784,21.432,9.31145616230212));
#92769=CARTESIAN_POINT('Origin',(-29.184,21.432,9.31145616230212));
#92770=CARTESIAN_POINT('',(-29.784,10.6144737596866,-6.36008826276735));
#92771=CARTESIAN_POINT('',(-29.184,20.3587352485079,8.8128));
#92772=CARTESIAN_POINT('',(-29.184,10.1206869778867,-6.01924428948959));
#92773=CARTESIAN_POINT('Origin',(-29.184,21.5019541534552,9.4128));
#92774=CARTESIAN_POINT('Origin',(-29.784,14.688,0.59750406305912));
#92775=CARTESIAN_POINT('',(-28.968,20.3587352485079,8.8128));
#92776=CARTESIAN_POINT('',(-28.968,14.688,0.59750406305912));
#92777=CARTESIAN_POINT('',(-29.784,20.3587352485079,8.8128));
#92778=CARTESIAN_POINT('Origin',(-29.784,7.344,-13.872));
#92779=CARTESIAN_POINT('',(-29.784,21.432,6.4022379066467));
#92780=CARTESIAN_POINT('',(-29.784,21.432,-11.016));
#92781=CARTESIAN_POINT('Origin',(-29.784,21.0528,5.93725687477551));
#92782=CARTESIAN_POINT('',(-29.784,21.0528,7.80729593694088));
#92783=CARTESIAN_POINT('',(-29.784,21.0528,-11.2476479684704));
#92784=CARTESIAN_POINT('',(-29.784,13.7731719941602,-2.73883181510914));
#92785=CARTESIAN_POINT('Origin',(-29.784,7.344,-13.872));
#92786=CARTESIAN_POINT('',(-29.784,21.432,9.4128));
#92787=CARTESIAN_POINT('',(-29.784,7.944,9.4128));
#92788=CARTESIAN_POINT('',(-29.784,13.8513676242539,9.4128));
#92789=CARTESIAN_POINT('',(-29.784,7.944,9.792));
#92790=CARTESIAN_POINT('',(-29.784,7.944,-13.056));
#92791=CARTESIAN_POINT('',(-29.784,21.432,9.792));
#92792=CARTESIAN_POINT('',(-29.784,7.344,9.792));
#92793=CARTESIAN_POINT('',(-29.784,21.432,-11.016));
#92794=CARTESIAN_POINT('Origin',(-29.184,8.18063237574607,-10.2288));
#92795=CARTESIAN_POINT('',(-29.7835166971462,21.456077579674,-10.204722420326));
#92796=CARTESIAN_POINT('',(-29.784,21.432,-10.2288));
#92797=CARTESIAN_POINT('Origin',(-29.184,21.432,-10.2288));
#92798=CARTESIAN_POINT('',(-29.784,7.944,-10.2288));
#92799=CARTESIAN_POINT('',(-29.784,8.18063237574607,-10.2288));
#92800=CARTESIAN_POINT('',(-29.7835166971462,7.91992242032599,-10.204722420326));
#92801=CARTESIAN_POINT('Origin',(-29.184,7.944,-10.2288));
#92802=CARTESIAN_POINT('',(-29.184,9.01726475149214,-9.6288));
#92803=CARTESIAN_POINT('Origin',(-29.184,7.87404584654483,-10.2288));
#92804=CARTESIAN_POINT('',(-29.184,20.3587352485079,-9.6288));
#92805=CARTESIAN_POINT('',(-29.184,8.18063237574607,-9.6288));
#92806=CARTESIAN_POINT('Origin',(-29.184,21.5019541534552,-10.2288));
#92807=CARTESIAN_POINT('Origin',(-29.184,7.944,-13.056));
#92808=CARTESIAN_POINT('',(-29.784,7.944,-10.1274561623021));
#92809=CARTESIAN_POINT('Origin',(-29.184,7.944,-10.1274561623021));
#92810=CARTESIAN_POINT('',(-29.784,7.944,-13.272));
#92811=CARTESIAN_POINT('',(-29.784,7.944,-13.056));
#92812=CARTESIAN_POINT('Origin',(-29.184,7.944,-13.272));
#92813=CARTESIAN_POINT('Origin',(-29.184,7.944,9.792));
#92814=CARTESIAN_POINT('',(-29.7835166971462,7.91992242032593,9.38872242032602));
#92815=CARTESIAN_POINT('Origin',(-29.184,7.944,9.4128));
#92816=CARTESIAN_POINT('',(-29.784,7.944,9.31145616230212));
#92817=CARTESIAN_POINT('Origin',(-29.184,7.944,9.31145616230212));
#92818=CARTESIAN_POINT('',(-29.784,7.944,8.35664978309472));
#92819=CARTESIAN_POINT('',(-29.784,7.944,-13.056));
#92820=CARTESIAN_POINT('',(-29.7737557460509,7.83359999999999,8.5165882446332));
#92821=CARTESIAN_POINT('Origin',(-29.184,7.944,8.35664978309472));
#92822=CARTESIAN_POINT('',(-29.7737557460509,7.83359999999999,-9.3325882446332));
#92823=CARTESIAN_POINT('',(-29.7737557460508,7.83359999999999,-13.056));
#92824=CARTESIAN_POINT('',(-29.784,7.944,-9.17264978309472));
#92825=CARTESIAN_POINT('Origin',(-29.184,7.944,-9.17264978309472));
#92826=CARTESIAN_POINT('',(-29.784,7.944,-13.056));
#92827=CARTESIAN_POINT('Origin',(-29.784,7.344,-13.872));
#92828=CARTESIAN_POINT('',(-29.784,21.432,-13.272));
#92829=CARTESIAN_POINT('',(-29.784,21.432,-11.016));
#92830=CARTESIAN_POINT('',(-29.784,7.344,-13.272));
#92831=CARTESIAN_POINT('Origin',(-29.784,7.344,-13.872));
#92832=CARTESIAN_POINT('',(-29.784,21.432,-10.1274561623021));
#92833=CARTESIAN_POINT('',(-29.784,14.7229948614198,-0.408000000000001));
#92834=CARTESIAN_POINT('',(-29.784,19.7444202838503,-7.68262913762374));
#92835=CARTESIAN_POINT('',(-29.784,15.052529806456,0.0694031896036967));
#92836=CARTESIAN_POINT('',(-29.784,10.6144737596866,-6.36008826276735));
#92837=CARTESIAN_POINT('',(-29.784,21.432,-9.17264978309473));
#92838=CARTESIAN_POINT('',(-29.784,17.2323832698161,-3.08858964834107));
#92839=CARTESIAN_POINT('',(-29.784,21.432,-11.016));
#92840=CARTESIAN_POINT('Origin',(-29.784,7.344,-13.872));
#92841=CARTESIAN_POINT('',(-29.784,12.4742196642688,-3.56444562304089));
#92842=CARTESIAN_POINT('',(-29.784,10.0969852123603,-7.00838784183138));
#92843=CARTESIAN_POINT('',(-29.784,11.0112188528984,-4.72911477825469));
#92844=CARTESIAN_POINT('',(-29.784,6.93828697788673,-10.6296442894896));
#92845=CARTESIAN_POINT('',(-29.784,12.1405883340853,-3.64430626388261));
#92846=CARTESIAN_POINT('Origin',(-29.784,10.6896,-3.264));
#92847=CARTESIAN_POINT('Origin',(-29.784,12.1735582741579,-3.0452127961736));
#92848=CARTESIAN_POINT('Origin',(-29.184,10.0969852123603,-7.00838784183138));
#92849=CARTESIAN_POINT('',(-29.784,14.6530051385802,-0.408000000000001));
#92850=CARTESIAN_POINT('',(-29.7833084014095,14.688,-0.407999999999989));
#92851=CARTESIAN_POINT('Origin',(-29.184,14.6530051385802,-0.408000000000002));
#92852=CARTESIAN_POINT('',(-29.184,14.688,-1.41350406305912));
#92853=CARTESIAN_POINT('Origin',(-29.184,14.688,-0.357302316148279));
#92854=CARTESIAN_POINT('',(-29.184,10.5907719941602,-7.34923181510914));
#92855=CARTESIAN_POINT('',(-29.7833084014095,12.6436432904313,-3.369696258734));
#92856=CARTESIAN_POINT('Ctrl Pts',(-29.784,12.4742196642688,-3.56444562304089));
#92857=CARTESIAN_POINT('Ctrl Pts',(-29.784,12.4770960656062,-3.56178870707269));
#92858=CARTESIAN_POINT('Ctrl Pts',(-29.7839981607211,12.4799597304405,-3.55911809821074));
#92859=CARTESIAN_POINT('Ctrl Pts',(-29.7839947131496,12.4828105409336,-3.55643374451523));
#92860=CARTESIAN_POINT('Ctrl Pts',(-29.7839651892816,12.5072239441763,-3.53344582252835));
#92861=CARTESIAN_POINT('Ctrl Pts',(-29.7838218910197,12.5306539102921,-3.50948777896365));
#92862=CARTESIAN_POINT('Ctrl Pts',(-29.783683917326,12.5530399267613,-3.48453639277156));
#92863=CARTESIAN_POINT('Ctrl Pts',(-29.7836552812666,12.5576860827128,-3.47935780141234));
#92864=CARTESIAN_POINT('Ctrl Pts',(-29.7836266970853,12.562287284019,-3.47413643089436));
#92865=CARTESIAN_POINT('Ctrl Pts',(-29.7835989418307,12.5668430063734,-3.46887208513704));
#92866=CARTESIAN_POINT('Ctrl Pts',(-29.7834716813667,12.5877314237255,-3.44473456254201));
#92867=CARTESIAN_POINT('Ctrl Pts',(-29.7833664628523,12.60758001705,-3.41979037882897));
#92868=CARTESIAN_POINT('Ctrl Pts',(-29.7833269962461,12.6263747771475,-3.39402765987634));
#92869=CARTESIAN_POINT('Ctrl Pts',(-29.7833146936516,12.6322335102483,-3.38599686333995));
#92870=CARTESIAN_POINT('Ctrl Pts',(-29.7833084014095,12.6379898333541,-3.37788652347427));
#92871=CARTESIAN_POINT('Ctrl Pts',(-29.7833084014095,12.6436432904314,-3.36969625873406));
#92872=CARTESIAN_POINT('',(-29.7833084014095,14.3409676242539,-0.910752031529554));
#92873=CARTESIAN_POINT('',(-29.7833084014095,10.1206869778867,-7.02474835254872));
#92874=CARTESIAN_POINT('',(-29.784,14.323470193544,-0.885403189603699));
#92875=CARTESIAN_POINT('Origin',(-29.184,14.323470193544,-0.885403189603698));
#92876=CARTESIAN_POINT('',(-29.784,10.0969852123603,-7.00838784183138));
#92877=CARTESIAN_POINT('Origin',(-29.184,10.6144737596866,-6.36008826276735));
#92878=CARTESIAN_POINT('Origin',(-29.184,14.7229948614198,-0.408000000000003));
#92879=CARTESIAN_POINT('',(-29.184,14.688,0.59750406305912));
#92880=CARTESIAN_POINT('Origin',(-29.184,14.688,-0.458697683851722));
#92881=CARTESIAN_POINT('',(-29.184,10.1206869778867,-6.01924428948959));
#92882=CARTESIAN_POINT('',(-29.7833084014095,15.0350323757461,0.0947520315295554));
#92883=CARTESIAN_POINT('',(-29.7833084014095,10.5907719941602,-6.34372775205002));
#92884=CARTESIAN_POINT('Origin',(-29.184,15.052529806456,0.0694031896036995));
#92885=CARTESIAN_POINT('Origin',(-29.184,13.5561964880162,1.18096637838117));
#92886=CARTESIAN_POINT('',(-29.784,13.5561964880162,1.18096637838117));
#92887=CARTESIAN_POINT('',(-29.184,9.01726475149214,8.8128));
#92888=CARTESIAN_POINT('Origin',(-29.184,7.87404584654483,9.4128));
#92889=CARTESIAN_POINT('',(-29.184,14.0499832698161,1.52181035165893));
#92890=CARTESIAN_POINT('Origin',(-29.784,7.344,-13.872));
#92891=CARTESIAN_POINT('',(-29.784,16.0682335020505,-3.41307311090149));
#92892=CARTESIAN_POINT('Origin',(-29.784,13.9939352485079,-0.408));
#92893=CARTESIAN_POINT('',(-29.184,13.9939352485079,-0.408));
#92894=CARTESIAN_POINT('Origin',(-29.184,14.3584650549638,-0.936100873455419));
#92895=CARTESIAN_POINT('',(-28.968,13.9939352485079,-0.408));
#92896=CARTESIAN_POINT('',(-29.784,13.9939352485079,-0.408));
#92897=CARTESIAN_POINT('',(-28.968,8.3232,7.80729593694088));
#92898=CARTESIAN_POINT('',(-28.968,13.9939352485079,-0.408));
#92899=CARTESIAN_POINT('',(-29.184,8.3232,7.80729593694088));
#92900=CARTESIAN_POINT('',(-29.784,8.3232,7.80729593694088));
#92901=CARTESIAN_POINT('Origin',(-29.184,7.7232,8.67652670617165));
#92902=CARTESIAN_POINT('Origin',(-29.184,7.43207375968655,-10.9704882627674));
#92903=CARTESIAN_POINT('',(-29.1857320434525,12.1735590034295,-3.04521774270319));
#92904=CARTESIAN_POINT('Origin',(-29.184,12.6673450559578,-3.38605676945136));
#92905=CARTESIAN_POINT('',(-29.184,6.93828697788673,-10.6296442894896));
#92906=CARTESIAN_POINT('Origin',(-29.784,15.3820647514921,-0.408));
#92907=CARTESIAN_POINT('',(-29.184,15.3820647514921,-0.408));
#92908=CARTESIAN_POINT('Origin',(-29.184,15.0175349450362,0.120100873455421));
#92909=CARTESIAN_POINT('',(-28.968,15.3820647514921,-0.408));
#92910=CARTESIAN_POINT('',(-29.784,15.3820647514921,-0.408));
#92911=CARTESIAN_POINT('',(-28.968,21.0528,-8.62329593694088));
#92912=CARTESIAN_POINT('',(-28.968,15.3820647514921,-0.408));
#92913=CARTESIAN_POINT('',(-29.184,21.0528,-8.62329593694088));
#92914=CARTESIAN_POINT('',(-29.784,21.0528,-8.62329593694088));
#92915=CARTESIAN_POINT('',(-29.7737557460508,21.5424,-9.3325882446332));
#92916=CARTESIAN_POINT('Origin',(-29.184,21.6528,-9.49252670617165));
#92917=CARTESIAN_POINT('Origin',(-29.184,21.432,-9.17264978309473));
#92918=CARTESIAN_POINT('Origin',(-29.184,13.2793852123603,-2.39798784183138));
#92919=CARTESIAN_POINT('',(-29.184,13.7731719941602,-2.73883181510914));
#92920=CARTESIAN_POINT('Origin',(-4.08,21.432,-13.272));
#92921=CARTESIAN_POINT('Origin',(-29.184,21.432,-13.272));
#92922=CARTESIAN_POINT('Origin',(-29.184,7.344,-13.272));
#92923=CARTESIAN_POINT('Origin',(-29.184,7.944,-13.272));
#92924=CARTESIAN_POINT('Origin',(-29.184,21.432,-13.272));
#92925=CARTESIAN_POINT('Origin',(-29.184,21.432,-13.272));
#92926=CARTESIAN_POINT('Origin',(-29.184,21.432,-13.272));
#92927=CARTESIAN_POINT('Origin',(-29.184,7.944,-13.272));
#92928=CARTESIAN_POINT('Origin',(-29.184,21.432,-11.016));
#92929=CARTESIAN_POINT('Origin',(-29.184,21.432,9.4128));
#92930=CARTESIAN_POINT('Origin',(-29.184,21.432,9.792));
#92931=CARTESIAN_POINT('Origin',(-29.184,21.432,-10.1274561623021));
#92932=CARTESIAN_POINT('',(-29.7737557460508,21.5424,5.93725687477551));
#92933=CARTESIAN_POINT('',(-29.7737557460508,21.5424,-11.016));
#92934=CARTESIAN_POINT('Ctrl Pts',(-29.7737557460509,21.5424,5.93725687477551));
#92935=CARTESIAN_POINT('Ctrl Pts',(-29.7737557460509,21.5424,5.96670869882893));
#92936=CARTESIAN_POINT('Ctrl Pts',(-29.7740088989078,21.5410717904559,5.9960597320568));
#92937=CARTESIAN_POINT('Ctrl Pts',(-29.7744834610748,21.5384391008847,6.02533043536184));
#92938=CARTESIAN_POINT('Ctrl Pts',(-29.7746717989984,21.5373942740489,6.03694700293919));
#92939=CARTESIAN_POINT('Ctrl Pts',(-29.7748944336911,21.5361438842468,6.04855091829811));
#92940=CARTESIAN_POINT('Ctrl Pts',(-29.7751471540983,21.534689055899,6.06014346040397));
#92941=CARTESIAN_POINT('Ctrl Pts',(-29.775853643425,21.5306220289779,6.09255084434131));
#92942=CARTESIAN_POINT('Ctrl Pts',(-29.7767945331539,21.5249853227474,6.12464572125983));
#92943=CARTESIAN_POINT('Ctrl Pts',(-29.7778229194578,21.5178739793336,6.15641892625882));
#92944=CARTESIAN_POINT('Ctrl Pts',(-29.7785157033164,21.5130833438392,6.17782329879137));
#92945=CARTESIAN_POINT('Ctrl Pts',(-29.7792468574529,21.5076233361447,6.19908169040163));
#92946=CARTESIAN_POINT('Ctrl Pts',(-29.7799584187364,21.5015238314338,6.22019129919245));
#92947=CARTESIAN_POINT('Ctrl Pts',(-29.7811964208663,21.4909116747602,6.25691862156105));
#92948=CARTESIAN_POINT('Ctrl Pts',(-29.7823703798565,21.4784143085855,6.29303346610638));
#92949=CARTESIAN_POINT('Ctrl Pts',(-29.7831330157742,21.4642432847158,6.32849767780225));
#92950=CARTESIAN_POINT('Ctrl Pts',(-29.7836200003229,21.4551943145547,6.35114350751594));
#92951=CARTESIAN_POINT('Ctrl Pts',(-29.7839381728052,21.4454635235311,6.37352404053474));
#92952=CARTESIAN_POINT('Ctrl Pts',(-29.7839919096164,21.4351158297269,6.39562934236959));
#92953=CARTESIAN_POINT('Ctrl Pts',(-29.7839972715979,21.4340833132552,6.397835059768));
#92954=CARTESIAN_POINT('Ctrl Pts',(-29.784,21.433044682114,6.40003791857));
#92955=CARTESIAN_POINT('Ctrl Pts',(-29.784,21.432,6.4022379066467));
#92956=CARTESIAN_POINT('Origin',(-27.528,7.344,9.192));
#92957=CARTESIAN_POINT('',(-27.528,7.344,9.792));
#92958=CARTESIAN_POINT('Origin',(-29.784,7.344,9.792));
#92959=CARTESIAN_POINT('Origin',(27.528,10.6896,-3.264));
#92960=CARTESIAN_POINT('Origin',(27.528,10.6896,-1.164));
#92961=CARTESIAN_POINT('Origin',(28.368,10.6896,-3.264));
#92962=CARTESIAN_POINT('',(28.968,12.609642670068,-2.4134495046629));
#92963=CARTESIAN_POINT('Ctrl Pts',(28.968,12.609642670068,-2.41344950466293));
#92964=CARTESIAN_POINT('Ctrl Pts',(28.968,12.5563563145717,-2.49064640429212));
#92965=CARTESIAN_POINT('Ctrl Pts',(28.9480231288294,12.4934277609683,-2.58181212938432));
#92966=CARTESIAN_POINT('Ctrl Pts',(28.8849632069594,12.3934003848311,-2.72672358455736));
#92967=CARTESIAN_POINT('Ctrl Pts',(28.8306825733401,12.3378273727896,-2.80723320456632));
#92968=CARTESIAN_POINT('Ctrl Pts',(28.719257430577,12.2610925274537,-2.91840035229654));
#92969=CARTESIAN_POINT('Ctrl Pts',(28.6451394651737,12.2244553812516,-2.97147724358932));
#92970=CARTESIAN_POINT('Ctrl Pts',(28.5128362786337,12.1855396693978,-3.02785513383895));
#92971=CARTESIAN_POINT('Ctrl Pts',(28.4351123331488,12.173558274158,-3.04521279617364));
#92972=CARTESIAN_POINT('Ctrl Pts',(28.368,12.173558274158,-3.04521279617364));
#92973=CARTESIAN_POINT('',(28.968,10.5751344569884,-5.3608780697654));
#92974=CARTESIAN_POINT('Origin',(28.968,10.6896,-3.264));
#92975=CARTESIAN_POINT('Ctrl Pts',(28.368,11.0112188528985,-4.72911477825469));
#92976=CARTESIAN_POINT('Ctrl Pts',(28.4351123331488,11.0112188528985,-4.72911477825469));
#92977=CARTESIAN_POINT('Ctrl Pts',(28.5128362786337,10.9992374576586,-4.74647244058937));
#92978=CARTESIAN_POINT('Ctrl Pts',(28.6451394651737,10.9603217458049,-4.802850330839));
#92979=CARTESIAN_POINT('Ctrl Pts',(28.719257430577,10.9236845996028,-4.85592722213179));
#92980=CARTESIAN_POINT('Ctrl Pts',(28.8306825733401,10.8469497542669,-4.967094369862));
#92981=CARTESIAN_POINT('Ctrl Pts',(28.8849632069594,10.7913767422253,-5.04760398987096));
#92982=CARTESIAN_POINT('Ctrl Pts',(28.9480231288294,10.6913493660881,-5.19251544504401));
#92983=CARTESIAN_POINT('Ctrl Pts',(28.968,10.6284208124847,-5.28368117013621));
#92984=CARTESIAN_POINT('Ctrl Pts',(28.968,10.5751344569884,-5.3608780697654));
#92985=CARTESIAN_POINT('Origin',(28.968,11.1585676242539,-0.408000000000002));
#92986=CARTESIAN_POINT('',(28.968,8.3232,-8.62329593694088));
#92987=CARTESIAN_POINT('',(28.968,8.3232,-8.62329593694088));
#92988=CARTESIAN_POINT('',(28.968,8.3232,7.80729593694088));
#92989=CARTESIAN_POINT('',(28.968,8.3232,-8.62329593694088));
#92990=CARTESIAN_POINT('Origin',(29.784,8.3232,-8.62329593694088));
#92991=CARTESIAN_POINT('',(29.784,8.3232,-8.62329593694088));
#92992=CARTESIAN_POINT('Origin',(29.784,13.9939352485079,-0.407999999999999));
#92993=CARTESIAN_POINT('Origin',(29.784,13.9939352485079,-0.407999999999999));
#92994=CARTESIAN_POINT('Ctrl Pts',(-29.784,21.2011648366643,6.51862412122269));
#92995=CARTESIAN_POINT('Ctrl Pts',(-29.784,21.6528,6.40336689328349));
#92996=CARTESIAN_POINT('Ctrl Pts',(-29.784,21.6528,5.93725687477551));
#92997=CARTESIAN_POINT('Ctrl Pts',(-29.784,21.0528,5.93725687477551));
#92998=CARTESIAN_POINT('Ctrl Pts',(-29.784,21.0528,5.93725687477551));
#92999=CARTESIAN_POINT('Ctrl Pts',(-29.784,21.0528,5.93725687477551));
#93000=CARTESIAN_POINT('Ctrl Pts',(-29.184,21.0528,5.93725687477551));
#93001=CARTESIAN_POINT('Ctrl Pts',(-29.184,21.0528,5.93725687477551));
#93002=CARTESIAN_POINT('Ctrl Pts',(-29.184,21.0528,5.93725687477551));
#93003=CARTESIAN_POINT('Origin',(-29.184,21.6528,5.93725687477551));
#93004=CARTESIAN_POINT('Origin',(-29.184,21.6528,-11.2476479684704));
#93005=CARTESIAN_POINT('',(-29.184,21.0528,-11.2476479684704));
#93006=CARTESIAN_POINT('Origin',(-29.784,8.3232,-8.62329593694088));
#93007=CARTESIAN_POINT('',(-29.184,8.3232,-8.62329593694088));
#93008=CARTESIAN_POINT('Origin',(-29.184,7.7232,-9.49252670617165));
#93009=CARTESIAN_POINT('',(-28.968,8.3232,-8.62329593694088));
#93010=CARTESIAN_POINT('',(-29.784,8.3232,-8.62329593694088));
#93011=CARTESIAN_POINT('',(-28.968,10.5751344569884,-5.3608780697654));
#93012=CARTESIAN_POINT('',(-28.968,8.3232,-8.62329593694088));
#93013=CARTESIAN_POINT('',(-28.368,11.0112188528984,-4.72911477825469));
#93014=CARTESIAN_POINT('Ctrl Pts',(-28.968,10.5751344569884,-5.3608780697654));
#93015=CARTESIAN_POINT('Ctrl Pts',(-28.968,10.6284208124846,-5.28368117013621));
#93016=CARTESIAN_POINT('Ctrl Pts',(-28.9480231288294,10.6913493660881,-5.192515445044));
#93017=CARTESIAN_POINT('Ctrl Pts',(-28.8849632069594,10.7913767422253,-5.04760398987097));
#93018=CARTESIAN_POINT('Ctrl Pts',(-28.8306825733401,10.8469497542668,-4.96709436986201));
#93019=CARTESIAN_POINT('Ctrl Pts',(-28.719257430577,10.9236845996027,-4.85592722213179));
#93020=CARTESIAN_POINT('Ctrl Pts',(-28.6451394651737,10.9603217458048,-4.80285033083901));
#93021=CARTESIAN_POINT('Ctrl Pts',(-28.5128362786337,10.9992374576586,-4.74647244058938));
#93022=CARTESIAN_POINT('Ctrl Pts',(-28.4351123331488,11.0112188528984,-4.72911477825469));
#93023=CARTESIAN_POINT('Ctrl Pts',(-28.368,11.0112188528984,-4.72911477825469));
#93024=CARTESIAN_POINT('',(-13.464,11.0112188528984,-4.72911477825469));
#93025=CARTESIAN_POINT('Origin',(-29.184,7.7232,-3.03235203152956));
#93026=CARTESIAN_POINT('',(-29.184,8.3232,-3.03235203152956));
#93027=CARTESIAN_POINT('Origin',(-29.784,9.01726475149214,8.8128));
#93028=CARTESIAN_POINT('',(-28.968,9.01726475149214,8.8128));
#93029=CARTESIAN_POINT('',(-29.784,9.01726475149214,8.8128));
#93030=CARTESIAN_POINT('',(-28.968,14.688,0.59750406305912));
#93031=CARTESIAN_POINT('',(-28.968,9.01726475149214,8.8128));
#93032=CARTESIAN_POINT('',(-29.784,14.688,0.59750406305912));
#93033=CARTESIAN_POINT('Origin',(-29.184,13.8513676242539,9.4128));
#93034=CARTESIAN_POINT('',(-29.184,13.8513676242539,8.8128));
#93035=CARTESIAN_POINT('Origin',(-29.784,20.3587352485079,8.8128));
#93036=CARTESIAN_POINT('',(-28.968,20.3587352485079,8.8128));
#93037=CARTESIAN_POINT('Origin',(-29.184,19.7444202838503,-7.68262913762374));
#93038=CARTESIAN_POINT('',(-29.184,19.2506335020505,-8.02347311090149));
#93039=CARTESIAN_POINT('Origin',(-29.784,20.3587352485079,-9.6288));
#93040=CARTESIAN_POINT('',(-28.968,20.3587352485079,-9.6288));
#93041=CARTESIAN_POINT('',(-29.784,20.3587352485079,-9.6288));
#93042=CARTESIAN_POINT('',(-28.968,14.688,-1.41350406305912));
#93043=CARTESIAN_POINT('',(-28.968,20.3587352485079,-9.6288));
#93044=CARTESIAN_POINT('',(-29.784,14.688,-1.41350406305912));
#93045=CARTESIAN_POINT('Origin',(-29.784,21.0528,-8.62329593694088));
#93046=CARTESIAN_POINT('',(-28.968,21.0528,-8.62329593694088));
#93047=CARTESIAN_POINT('Origin',(-27.528,10.6896,-3.264));
#93048=CARTESIAN_POINT('',(-27.528,10.6896,-4.764));
#93049=CARTESIAN_POINT('Origin',(-27.528,10.6896,-5.364));
#93050=CARTESIAN_POINT('',(-27.528,10.6896,-1.764));
#93051=CARTESIAN_POINT('Origin',(-27.528,10.6896,-3.264));
#93052=CARTESIAN_POINT('Origin',(-27.528,10.6896,-3.264));
#93053=CARTESIAN_POINT('Origin',(-13.464,10.6896,-3.264));
#93054=CARTESIAN_POINT('',(-28.368,10.6896,-1.764));
#93055=CARTESIAN_POINT('',(-13.464,10.6896,-1.764));
#93056=CARTESIAN_POINT('',(-28.368,12.1735582741579,-3.0452127961736));
#93057=CARTESIAN_POINT('Origin',(-28.368,10.6896,-3.264));
#93058=CARTESIAN_POINT('',(-13.464,12.1735582741579,-3.0452127961736));
#93059=CARTESIAN_POINT('Ctrl Pts',(-29.784,12.1405883340853,-3.64430626388261));
#93060=CARTESIAN_POINT('Ctrl Pts',(-29.784,12.147511185521,-3.6178934023925));
#93061=CARTESIAN_POINT('Ctrl Pts',(-29.7822104609222,12.1536772931533,-3.59140178696739));
#93062=CARTESIAN_POINT('Ctrl Pts',(-29.7786474905659,12.1590759523918,-3.56504634540795));
#93063=CARTESIAN_POINT('Ctrl Pts',(-29.7748844514047,12.1647777584978,-3.53721098648425));
#93064=CARTESIAN_POINT('Ctrl Pts',(-29.7691451014835,12.1696236218268,-3.50952645920431));
#93065=CARTESIAN_POINT('Ctrl Pts',(-29.7614332365283,12.1736419782786,-3.48220709085635));
#93066=CARTESIAN_POINT('Ctrl Pts',(-29.7564653648374,12.1762305452953,-3.46460834951199));
#93067=CARTESIAN_POINT('Ctrl Pts',(-29.7506784545669,12.1784765265179,-3.44716030561529));
#93068=CARTESIAN_POINT('Ctrl Pts',(-29.7440660203898,12.1803955912691,-3.42991716322555));
#93069=CARTESIAN_POINT('Ctrl Pts',(-29.7333900045645,12.1834939912084,-3.40207748178614));
#93070=CARTESIAN_POINT('Ctrl Pts',(-29.7206781216082,12.185706516543,-3.37507844369262));
#93071=CARTESIAN_POINT('Ctrl Pts',(-29.7060488214569,12.1871803802583,-3.34916282903413));
#93072=CARTESIAN_POINT('Ctrl Pts',(-29.6880947954994,12.1889892013999,-3.31735750591742));
#93073=CARTESIAN_POINT('Ctrl Pts',(-29.6672533785123,12.1896851014655,-3.28718063548158));
#93074=CARTESIAN_POINT('Ctrl Pts',(-29.6437054196481,12.1895918142645,-3.2590338036487));
#93075=CARTESIAN_POINT('Ctrl Pts',(-29.6391149556756,12.189573628759,-3.25354683052235));
#93076=CARTESIAN_POINT('Ctrl Pts',(-29.634421550843,12.1895255901819,-3.24813699762495));
#93077=CARTESIAN_POINT('Ctrl Pts',(-29.629626466634,12.1894502829085,-3.24280733949571));
#93078=CARTESIAN_POINT('Ctrl Pts',(-29.6034219992866,12.189038739148,-3.21368150012913));
#93079=CARTESIAN_POINT('Ctrl Pts',(-29.5745073160778,12.1878210298843,-3.18731184548696));
#93080=CARTESIAN_POINT('Ctrl Pts',(-29.5432973065778,12.1862640863858,-3.16400903809615));
#93081=CARTESIAN_POINT('Ctrl Pts',(-29.5172821877694,12.1849662953649,-3.14458497150485));
#93082=CARTESIAN_POINT('Ctrl Pts',(-29.4896684020062,12.1834330785157,-3.12728965954881));
#93083=CARTESIAN_POINT('Ctrl Pts',(-29.4607047388456,12.1819102823203,-3.1123093189926));
#93084=CARTESIAN_POINT('Ctrl Pts',(-29.4570107007678,12.1817160642375,-3.11039871990417));
#93085=CARTESIAN_POINT('Ctrl Pts',(-29.4532947581774,12.181521974349,-3.10852580118053));
#93086=CARTESIAN_POINT('Ctrl Pts',(-29.449557483041,12.1813284837015,-3.1066909700191));
#93087=CARTESIAN_POINT('Ctrl Pts',(-29.4234055951258,12.1799745170972,-3.09385158915324));
#93088=CARTESIAN_POINT('Ctrl Pts',(-29.3964447704895,12.1786654665046,-3.08299045789682));
#93089=CARTESIAN_POINT('Ctrl Pts',(-29.3688630741448,12.1775347113506,-3.07412927688624));
#93090=CARTESIAN_POINT('Ctrl Pts',(-29.342732972425,12.1764634666083,-3.06573445017687));
#93091=CARTESIAN_POINT('Ctrl Pts',(-29.3160437828719,12.1755521928172,-3.0591353667864));
#93092=CARTESIAN_POINT('Ctrl Pts',(-29.2889754148028,12.1748799314263,-3.05437250687602));
#93093=CARTESIAN_POINT('Ctrl Pts',(-29.2636838866422,12.174251799067,-3.04992229379924));
#93094=CARTESIAN_POINT('Ctrl Pts',(-29.2380607642433,12.1738323335988,-3.04707636428828));
#93095=CARTESIAN_POINT('Ctrl Pts',(-29.2122867480549,12.173655437531,-3.04587283722916));
#93096=CARTESIAN_POINT('Ctrl Pts',(-29.2043276450809,12.1736008114297,-3.04550118402132));
#93097=CARTESIAN_POINT('Ctrl Pts',(-29.1963544354037,12.1735690833018,-3.04528611569323));
#93098=CARTESIAN_POINT('Ctrl Pts',(-29.1883732215644,12.1735605987272,-3.04522856350714));
#93099=CARTESIAN_POINT('Ctrl Pts',(-29.1880701860807,12.1735602765798,-3.04522637833144));
#93100=CARTESIAN_POINT('Ctrl Pts',(-29.1877671376288,12.1735599878973,-3.04522442020813));
#93101=CARTESIAN_POINT('Ctrl Pts',(-29.187464086905,12.1735597327011,-3.04522268923278));
#93102=CARTESIAN_POINT('Origin',(-28.368,10.6896,-3.264));
#93103=CARTESIAN_POINT('Origin',(-29.784,8.3232,7.80729593694088));
#93104=CARTESIAN_POINT('',(-28.968,8.3232,7.80729593694088));
#93105=CARTESIAN_POINT('Ctrl Pts',(-29.784,12.6673450559584,-3.38605676945045));
#93106=CARTESIAN_POINT('Ctrl Pts',(-29.784,12.4763303711457,-3.66278317180831));
#93107=CARTESIAN_POINT('Ctrl Pts',(-29.784,12.1405883340853,-3.64430626388262));
#93108=CARTESIAN_POINT('Ctrl Pts',(-29.784,12.1735582741579,-3.04521279617361));
#93109=CARTESIAN_POINT('Ctrl Pts',(-29.784,12.1735582741579,-3.04521279617361));
#93110=CARTESIAN_POINT('Ctrl Pts',(-29.784,12.1735582741579,-3.04521279617361));
#93111=CARTESIAN_POINT('Ctrl Pts',(-29.184,12.1735582741579,-3.0452127961736));
#93112=CARTESIAN_POINT('Ctrl Pts',(-29.184,12.1735582741579,-3.04521279617361));
#93113=CARTESIAN_POINT('Ctrl Pts',(-29.184,12.1735582741579,-3.04521279617361));
#93114=CARTESIAN_POINT('Origin',(-28.368,10.6896,-3.264));
#93115=CARTESIAN_POINT('',(-28.968,12.609642670068,-2.4134495046629));
#93116=CARTESIAN_POINT('Origin',(-28.968,10.6896,-3.264));
#93117=CARTESIAN_POINT('Ctrl Pts',(-28.368,12.1735582741579,-3.0452127961736));
#93118=CARTESIAN_POINT('Ctrl Pts',(-28.4351123331488,12.1735582741579,-3.0452127961736));
#93119=CARTESIAN_POINT('Ctrl Pts',(-28.5128362786337,12.1855396693978,-3.02785513383891));
#93120=CARTESIAN_POINT('Ctrl Pts',(-28.6451394651737,12.2244553812515,-2.97147724358928));
#93121=CARTESIAN_POINT('Ctrl Pts',(-28.719257430577,12.2610925274536,-2.9184003522965));
#93122=CARTESIAN_POINT('Ctrl Pts',(-28.8306825733401,12.3378273727895,-2.80723320456628));
#93123=CARTESIAN_POINT('Ctrl Pts',(-28.8849632069594,12.3934003848311,-2.72672358455733));
#93124=CARTESIAN_POINT('Ctrl Pts',(-28.9480231288294,12.4934277609683,-2.58181212938429));
#93125=CARTESIAN_POINT('Ctrl Pts',(-28.968,12.5563563145717,-2.49064640429208));
#93126=CARTESIAN_POINT('Ctrl Pts',(-28.968,12.609642670068,-2.4134495046629));
#93127=CARTESIAN_POINT('Origin',(-28.968,11.1585676242539,-0.408000000000002));
#93128=CARTESIAN_POINT('',(-28.968,8.3232,-8.62329593694088));
#93129=CARTESIAN_POINT('Origin',(-29.784,8.3232,-8.62329593694088));
#93130=CARTESIAN_POINT('Origin',(-28.968,18.2174323757461,-0.407999999999999));
#93131=CARTESIAN_POINT('',(-28.968,21.0528,7.80729593694088));
#93132=CARTESIAN_POINT('Origin',(-29.784,21.0528,7.80729593694088));
#93133=CARTESIAN_POINT('Origin',(-29.784,21.0528,-8.62329593694088));
#93134=CARTESIAN_POINT('',(-28.968,21.0528,7.80729593694088));
#93135=CARTESIAN_POINT('',(-28.968,21.0528,-8.62329593694088));
#93136=CARTESIAN_POINT('',(-29.784,21.0528,7.80729593694088));
#93137=CARTESIAN_POINT('Origin',(-29.784,21.0528,7.80729593694088));
#93138=CARTESIAN_POINT('',(-28.968,21.0528,7.80729593694088));
#93139=CARTESIAN_POINT('Origin',(-28.968,18.2174323757461,-0.407999999999999));
#93140=CARTESIAN_POINT('Origin',(-29.784,14.688,0.59750406305912));
#93141=CARTESIAN_POINT('',(-28.968,14.688,0.59750406305912));
#93142=CARTESIAN_POINT('Origin',(-28.968,14.688,4.70515203152956));
#93143=CARTESIAN_POINT('Origin',(-29.784,9.01726475149214,-9.6288));
#93144=CARTESIAN_POINT('',(-28.968,9.01726475149214,-9.6288));
#93145=CARTESIAN_POINT('',(-29.784,9.01726475149214,-9.6288));
#93146=CARTESIAN_POINT('',(-28.968,9.01726475149214,-9.6288));
#93147=CARTESIAN_POINT('Origin',(-29.784,14.688,-1.41350406305912));
#93148=CARTESIAN_POINT('',(-28.968,14.688,-1.41350406305912));
#93149=CARTESIAN_POINT('Origin',(-28.968,14.688,-5.52115203152956));
#93150=CARTESIAN_POINT('Origin',(28.968,18.2174323757461,-0.407999999999999));
#93151=CARTESIAN_POINT('',(28.968,21.0528,-8.62329593694088));
#93152=CARTESIAN_POINT('Origin',(29.784,21.0528,7.80729593694088));
#93153=CARTESIAN_POINT('Origin',(29.784,15.3820647514921,-0.407999999999999));
#93154=CARTESIAN_POINT('',(28.968,21.0528,7.80729593694088));
#93155=CARTESIAN_POINT('',(28.968,21.0528,7.80729593694088));
#93156=CARTESIAN_POINT('',(29.784,21.0528,7.80729593694088));
#93157=CARTESIAN_POINT('Origin',(29.784,21.0528,7.80729593694088));
#93158=CARTESIAN_POINT('',(28.968,21.0528,-8.62329593694088));
#93159=CARTESIAN_POINT('Origin',(28.968,18.2174323757461,-0.407999999999999));
#93160=CARTESIAN_POINT('Origin',(29.784,20.3587352485079,8.8128));
#93161=CARTESIAN_POINT('',(28.968,20.3587352485079,8.8128));
#93162=CARTESIAN_POINT('',(29.784,20.3587352485079,8.8128));
#93163=CARTESIAN_POINT('',(28.968,14.688,0.59750406305912));
#93164=CARTESIAN_POINT('Origin',(29.784,9.01726475149214,8.8128));
#93165=CARTESIAN_POINT('',(28.968,20.3587352485079,8.8128));
#93166=CARTESIAN_POINT('Origin',(29.784,20.3587352485079,8.8128));
#93167=CARTESIAN_POINT('',(28.968,14.688,0.59750406305912));
#93168=CARTESIAN_POINT('Origin',(28.968,14.688,4.70515203152956));
#93169=CARTESIAN_POINT('Origin',(28.968,14.688,-5.52115203152956));
#93170=CARTESIAN_POINT('Origin',(-4.896,21.7056,-21.216));
#93171=CARTESIAN_POINT('Origin',(0.,20.808,-2.1216));
#93172=CARTESIAN_POINT('Origin',(3.672,20.808,-3.264));
#93173=CARTESIAN_POINT('Origin',(-3.672,20.808,-3.264));
#93174=CARTESIAN_POINT('Origin',(0.,14.688,-22.032));
#93175=CARTESIAN_POINT('',(-5.47389440891949,16.32,-22.032));
#93176=CARTESIAN_POINT('',(5.47389440891949,16.32,-22.032));
#93177=CARTESIAN_POINT('Origin',(0.,14.688,-22.032));
#93178=CARTESIAN_POINT('',(-5.47389440891949,16.32,-22.032));
#93179=CARTESIAN_POINT('',(5.47389440891949,16.32,-22.032));
#93180=CARTESIAN_POINT('Origin',(0.,16.32,-11.832));
#93181=CARTESIAN_POINT('Origin',(0.,16.32,2.448));
#93182=CARTESIAN_POINT('Origin',(0.,16.32,-11.832));
#93183=CARTESIAN_POINT('Origin',(0.,16.32,2.448));
#93184=CARTESIAN_POINT('Origin',(-10.812,16.32,8.16));
#93185=CARTESIAN_POINT('Origin',(8.16,7.344,-13.872));
#93186=CARTESIAN_POINT('Origin',(8.976,8.16,8.976));
#93187=CARTESIAN_POINT('Origin',(16.32,5.712,8.568));
#93188=CARTESIAN_POINT('Origin',(-8.976,8.16,8.976));
#93189=CARTESIAN_POINT('Origin',(8.976,8.16,8.976));
#93190=CARTESIAN_POINT('',(0.,0.,0.));
#93191=CARTESIAN_POINT('Origin',(22.032,0.,0.));
#93192=CARTESIAN_POINT('',(22.0319999995994,-11.5000119847845,0.0228638357956435));
#93193=CARTESIAN_POINT('',(22.032,-10.2055351096819,0.0182135250455447));
#93194=CARTESIAN_POINT('Ctrl Pts',(22.032,-11.5000119837245,0.0228638357581901));
#93195=CARTESIAN_POINT('Ctrl Pts',(22.032,-11.4660039066419,0.98463424605543));
#93196=CARTESIAN_POINT('Ctrl Pts',(22.0320000000025,-11.3136952518557,1.93685858767515));
#93197=CARTESIAN_POINT('Ctrl Pts',(22.0320000000025,-10.8106581948625,3.60550041619086));
#93198=CARTESIAN_POINT('Ctrl Pts',(22.0320000001919,-10.5043379386651,4.32629225339571));
#93199=CARTESIAN_POINT('Ctrl Pts',(22.0320000001919,-9.46446343489987,6.15504317488174));
#93200=CARTESIAN_POINT('Ctrl Pts',(22.0319999999366,-8.72063759985904,6.938122886154));
#93201=CARTESIAN_POINT('Ctrl Pts',(22.0319999999366,-8.03193816956031,7.51949158019168));
#93202=CARTESIAN_POINT('Ctrl Pts',(22.0319999999997,-7.85932443550526,7.63633005181417));
#93203=CARTESIAN_POINT('Ctrl Pts',(22.0319999999997,-7.73686440492364,7.68512650246837));
#93204=CARTESIAN_POINT('Ctrl Pts',(22.0320000000002,-7.71458757555367,7.69219740534354));
#93205=CARTESIAN_POINT('Ctrl Pts',(22.0320000000002,-7.68888585032816,7.69366409920399));
#93206=CARTESIAN_POINT('Ctrl Pts',(22.032,-7.68166282362026,7.69332086239068));
#93207=CARTESIAN_POINT('Ctrl Pts',(22.032,-7.6709934259232,7.69016254445955));
#93208=CARTESIAN_POINT('Ctrl Pts',(22.032,-7.66713809909079,7.68831385381647));
#93209=CARTESIAN_POINT('Ctrl Pts',(22.032,-7.66088557595881,7.68327738229244));
#93210=CARTESIAN_POINT('Ctrl Pts',(22.032,-7.65855096777891,7.68044695877115));
#93211=CARTESIAN_POINT('Ctrl Pts',(22.032,-7.65460320422513,7.67333693309721));
#93212=CARTESIAN_POINT('Ctrl Pts',(22.032,-7.65329985444339,7.66908195382268));
#93213=CARTESIAN_POINT('Ctrl Pts',(22.032,-7.65126894293338,7.65725956689985));
#93214=CARTESIAN_POINT('Ctrl Pts',(22.032,-7.65158753554677,7.64913230233977));
#93215=CARTESIAN_POINT('Ctrl Pts',(22.032,-7.65481301559317,7.62353907721947));
#93216=CARTESIAN_POINT('Ctrl Pts',(22.032,-7.66148618499009,7.6028062413979));
#93217=CARTESIAN_POINT('Ctrl Pts',(22.032,-7.69333704035368,7.52201090468904));
#93218=CARTESIAN_POINT('Ctrl Pts',(22.032,-7.74069889072153,7.43827269921366));
#93219=CARTESIAN_POINT('Ctrl Pts',(22.032,-8.0762146857713,6.89691692694695));
#93220=CARTESIAN_POINT('Ctrl Pts',(22.0320000000002,-8.64551455485788,6.11724445629462));
#93221=CARTESIAN_POINT('Ctrl Pts',(22.0320000000002,-9.48552373995225,4.32369687901933));
#93222=CARTESIAN_POINT('Ctrl Pts',(22.0319999999999,-9.73628062912841,3.61588039473753));
#93223=CARTESIAN_POINT('Ctrl Pts',(22.0319999999999,-10.1372396947166,1.93922249627196));
#93224=CARTESIAN_POINT('Ctrl Pts',(22.032,-10.2326443525765,0.983079921512957));
#93225=CARTESIAN_POINT('Ctrl Pts',(22.032,-10.2055351096819,0.0182135250456028));
#93226=CARTESIAN_POINT('',(22.032,-5.42639624653361,0.00104482810403733));
#93227=CARTESIAN_POINT('Origin',(21.2976,-10.8528,-1.59247615094671E-14));
#93228=CARTESIAN_POINT('',(20.6563591733144,-11.5926712737699,-0.0152754849923013));
#93229=CARTESIAN_POINT('Ctrl Pts',(22.0319999992972,-11.5000119845197,0.0228638358451183));
#93230=CARTESIAN_POINT('Ctrl Pts',(21.9350321970426,-11.610239680658,0.0205479470244637));
#93231=CARTESIAN_POINT('Ctrl Pts',(21.8275399155968,-11.6829048894223,0.0178027823963555));
#93232=CARTESIAN_POINT('Ctrl Pts',(21.626607745303,-11.7823418227845,0.0125405838911135));
#93233=CARTESIAN_POINT('Ctrl Pts',(21.503231827314,-11.8204901071103,0.00922720623917468));
#93234=CARTESIAN_POINT('Ctrl Pts',(21.2741540024461,-11.8356971493868,0.00287527591883714));
#93235=CARTESIAN_POINT('Ctrl Pts',(21.1398060819373,-11.833007170968,-0.000891661286779711));
#93236=CARTESIAN_POINT('Ctrl Pts',(20.8648819597256,-11.7401403524706,-0.00891401040353155));
#93237=CARTESIAN_POINT('Ctrl Pts',(20.7523786699402,-11.6759522630052,-0.012290951791703));
#93238=CARTESIAN_POINT('Ctrl Pts',(20.6563591733144,-11.5926712737699,-0.015275484992302));
#93239=CARTESIAN_POINT('',(20.3193037808912,-10.8848592494362,-0.0272277890842044));
#93240=CARTESIAN_POINT('Ctrl Pts',(20.6563591733144,-11.5926712737699,-0.0152754849923009));
#93241=CARTESIAN_POINT('Ctrl Pts',(20.6055977297694,-11.5486441398856,-0.0168532813658944));
#93242=CARTESIAN_POINT('Ctrl Pts',(20.5595669862461,-11.4992460137549,-0.0183180703571777));
#93243=CARTESIAN_POINT('Ctrl Pts',(20.4783995888503,-11.3921384623027,-0.020972833860049));
#93244=CARTESIAN_POINT('Ctrl Pts',(20.4432698252404,-11.3344418887259,-0.0221625695045156));
#93245=CARTESIAN_POINT('Ctrl Pts',(20.3852853252821,-11.2131046998991,-0.0242201017929761));
#93246=CARTESIAN_POINT('Ctrl Pts',(20.3624460868063,-11.1494529184308,-0.0250875051257663));
#93247=CARTESIAN_POINT('Ctrl Pts',(20.3305045689841,-11.0185761815986,-0.0264509701549973));
#93248=CARTESIAN_POINT('Ctrl Pts',(20.3215498650961,-10.9516061699761,-0.0269419887804196));
#93249=CARTESIAN_POINT('Ctrl Pts',(20.3193957862769,-10.8845984096372,-0.0272429516870437));
#93250=CARTESIAN_POINT('',(20.3193161062581,-10.8205589424572,-0.0274550152749159));
#93251=CARTESIAN_POINT('Ctrl Pts',(20.3182662561622,-10.8845986717901,-0.0272745400228147));
#93252=CARTESIAN_POINT('Ctrl Pts',(20.3186047499116,-10.8739814510219,-0.0273032150225033));
#93253=CARTESIAN_POINT('Ctrl Pts',(20.318769563458,-10.8633587412999,-0.0273367670103365));
#93254=CARTESIAN_POINT('Ctrl Pts',(20.3187534786035,-10.8421008046921,-0.0274135843898352));
#93255=CARTESIAN_POINT('Ctrl Pts',(20.3185721644116,-10.8314655952278,-0.0274568613472546));
#93256=CARTESIAN_POINT('Ctrl Pts',(20.3182184169768,-10.8208361620798,-0.0275049399497529));
#93257=CARTESIAN_POINT('',(20.8715427754356,-9.97121102350762,-0.0150824746661654));
#93258=CARTESIAN_POINT('Ctrl Pts',(20.3193928792644,-10.8208352952865,-0.02747209717959));
#93259=CARTESIAN_POINT('Ctrl Pts',(20.3222338376522,-10.7320725931465,-0.0277115181605737));
#93260=CARTESIAN_POINT('Ctrl Pts',(20.3369462701113,-10.6435913145696,-0.0276179216934669));
#93261=CARTESIAN_POINT('Ctrl Pts',(20.3900860096127,-10.4733016174146,-0.0267435292273411));
#93262=CARTESIAN_POINT('Ctrl Pts',(20.428288215811,-10.3933182142733,-0.0259624723348962));
#93263=CARTESIAN_POINT('Ctrl Pts',(20.5260865493615,-10.244975468023,-0.0237602817105972));
#93264=CARTESIAN_POINT('Ctrl Pts',(20.5849926040816,-10.177509639553,-0.0223552371780158));
#93265=CARTESIAN_POINT('Ctrl Pts',(20.717898292447,-10.060226299178,-0.0190596296319128));
#93266=CARTESIAN_POINT('Ctrl Pts',(20.7920498117973,-10.0102371102918,-0.0171654356066794));
#93267=CARTESIAN_POINT('Ctrl Pts',(20.8715427754356,-9.97121102350762,-0.0150824746661655));
#93268=CARTESIAN_POINT('',(21.8012598463038,-10.0131352633455,0.0110692926695165));
#93269=CARTESIAN_POINT('Ctrl Pts',(20.8715427754356,-9.97121102350762,-0.0150824746661655));
#93270=CARTESIAN_POINT('Ctrl Pts',(20.9442163306386,-9.93553284090563,-0.0131782032694574));
#93271=CARTESIAN_POINT('Ctrl Pts',(21.0203053921159,-9.90953391310775,-0.0111436392942924));
#93272=CARTESIAN_POINT('Ctrl Pts',(21.1794653443307,-9.87759783181623,-0.0068071819094258));
#93273=CARTESIAN_POINT('Ctrl Pts',(21.2608328138172,-9.87179676321389,-0.00455243876800186));
#93274=CARTESIAN_POINT('Ctrl Pts',(21.4223470658279,-9.87962131412445,-7.30220672824389E-6));
#93275=CARTESIAN_POINT('Ctrl Pts',(21.5026568601935,-9.89321709277015,0.00228754292219898));
#93276=CARTESIAN_POINT('Ctrl Pts',(21.6574749417698,-9.93919782733929,0.00678248263126461));
#93277=CARTESIAN_POINT('Ctrl Pts',(21.7320415886282,-9.97158827955724,0.00898422908565387));
#93278=CARTESIAN_POINT('Ctrl Pts',(21.8012598463038,-10.0131352633455,0.0110692926695161));
#93279=CARTESIAN_POINT('Ctrl Pts',(21.8012598463038,-10.0131352633455,0.0110692926695162));
#93280=CARTESIAN_POINT('Ctrl Pts',(21.8443447378487,-10.0389961756343,0.0123671401073386));
#93281=CARTESIAN_POINT('Ctrl Pts',(21.885392900488,-10.0682342167638,0.013620158954269));
#93282=CARTESIAN_POINT('Ctrl Pts',(21.9625903176812,-10.1326420227271,0.0160104994198505));
#93283=CARTESIAN_POINT('Ctrl Pts',(21.9987394741801,-10.1678180480274,0.0171478407864812));
#93284=CARTESIAN_POINT('Ctrl Pts',(22.032,-10.2055351096819,0.0182135250455451));
#93285=CARTESIAN_POINT('Origin',(0.,0.,0.));
#93286=CARTESIAN_POINT('',(-4.16932807723036E-10,11.5001144173584,0.0228642038285899));
#93287=CARTESIAN_POINT('',(5.58994029708336E-16,10.205522161444,0.0182134784999908));
#93288=CARTESIAN_POINT('Ctrl Pts',(3.15981143696682E-18,11.5001144184625,
0.0228642038676663));
#93289=CARTESIAN_POINT('Ctrl Pts',(3.15981143696682E-18,11.4666648155453,
0.967921600731115));
#93290=CARTESIAN_POINT('Ctrl Pts',(-1.8863341238837E-12,11.3189678591532,
1.90385824366225));
#93291=CARTESIAN_POINT('Ctrl Pts',(-1.88634172183575E-12,10.8311683388227,
3.54908849500464));
#93292=CARTESIAN_POINT('Ctrl Pts',(-4.24723149583475E-18,10.5332036884033,
4.26226166170117));
#93293=CARTESIAN_POINT('Ctrl Pts',(7.68212098176784E-18,9.47876554604743,
6.15082285610065));
#93294=CARTESIAN_POINT('Ctrl Pts',(-3.46944695195361E-16,8.6951852496647,
6.96624905203417));
#93295=CARTESIAN_POINT('Ctrl Pts',(-3.46944695195361E-16,8.01684087521194,
7.5287776435044));
#93296=CARTESIAN_POINT('Ctrl Pts',(7.62904918881266E-13,7.85893173523043,
7.63486304190703));
#93297=CARTESIAN_POINT('Ctrl Pts',(7.62905461193962E-13,7.73987625544612,
7.68416881913137));
#93298=CARTESIAN_POINT('Ctrl Pts',(-3.02327607393238E-13,7.71568897779549,
7.69225569369772));
#93299=CARTESIAN_POINT('Ctrl Pts',(-3.02327607393238E-13,7.68852262290096,
7.6939848370806));
#93300=CARTESIAN_POINT('Ctrl Pts',(-7.80625564189563E-16,7.68119863204128,
7.69369346751344));
#93301=CARTESIAN_POINT('Ctrl Pts',(-7.80625564189563E-16,7.67039722237102,
7.69059423969854));
#93302=CARTESIAN_POINT('Ctrl Pts',(-5.20417042793042E-17,7.66649558212329,
7.6887691875303));
#93303=CARTESIAN_POINT('Ctrl Pts',(-5.20417042793042E-17,7.66017498071618,
7.68376907703856));
#93304=CARTESIAN_POINT('Ctrl Pts',(3.46992765880931E-17,7.65781392986216,
7.68095885930986));
#93305=CARTESIAN_POINT('Ctrl Pts',(3.46888586034366E-17,7.65382955269162,
7.67390838917976));
#93306=CARTESIAN_POINT('Ctrl Pts',(5.20417042793042E-17,7.65250629254514,
7.6697025383618));
#93307=CARTESIAN_POINT('Ctrl Pts',(5.20417042793042E-17,7.65042516861425,
7.65804982966815));
#93308=CARTESIAN_POINT('Ctrl Pts',(-1.73472347597681E-17,7.65068602749646,
7.65006360430989));
#93309=CARTESIAN_POINT('Ctrl Pts',(-1.73472347597681E-17,7.65369059736511,
7.62507165521352));
#93310=CARTESIAN_POINT('Ctrl Pts',(2.60208521396521E-17,7.66004240645279,
7.60490404284757));
#93311=CARTESIAN_POINT('Ctrl Pts',(2.60208521396521E-17,7.69041651575825,
7.52681063325573));
#93312=CARTESIAN_POINT('Ctrl Pts',(-8.78203759713259E-17,7.73535299370069,
7.44659886752905));
#93313=CARTESIAN_POINT('Ctrl Pts',(-8.78203759713259E-17,8.06204860091466,
6.91667103262996));
#93314=CARTESIAN_POINT('Ctrl Pts',(-3.59719505845404E-13,8.6362158993291,
6.13221168027708));
#93315=CARTESIAN_POINT('Ctrl Pts',(-3.59707701754705E-13,9.47953422855764,
4.3392821160567));
#93316=CARTESIAN_POINT('Ctrl Pts',(7.94902241816546E-14,9.73203279797478,
3.62981596955891));
#93317=CARTESIAN_POINT('Ctrl Pts',(7.94981390428919E-14,10.1364001920077,
1.94730306292097));
#93318=CARTESIAN_POINT('Ctrl Pts',(9.43168451234247E-18,10.2327414932924,
0.987187282335549));
#93319=CARTESIAN_POINT('Ctrl Pts',(9.43168451234247E-18,10.205522161444,
0.018213478499991));
#93320=CARTESIAN_POINT('',(0.,5.42639624653295,0.00104482830329189));
#93321=CARTESIAN_POINT('Origin',(0.7344,10.8528,5.18225781656585E-18));
#93322=CARTESIAN_POINT('',(1.37078399030106,11.5968559808931,-0.0151246218382906));
#93323=CARTESIAN_POINT('Ctrl Pts',(1.37078399030106,11.5968559808931,-0.0151246218382906));
#93324=CARTESIAN_POINT('Ctrl Pts',(1.27515758559223,11.6787046729424,-0.0121562275697988));
#93325=CARTESIAN_POINT('Ctrl Pts',(1.1634760436845,11.7417288632361,-0.00880644902523928));
#93326=CARTESIAN_POINT('Ctrl Pts',(0.88822355641489,11.8338390991337,-0.000777634600949455));
#93327=CARTESIAN_POINT('Ctrl Pts',(0.753591200162323,11.8356484498897,0.00299409374586479));
#93328=CARTESIAN_POINT('Ctrl Pts',(0.536934457303539,11.8205287432007,0.00899896059682586));
#93329=CARTESIAN_POINT('Ctrl Pts',(0.412342432885092,11.7863075085859,0.0123604564058159));
#93330=CARTESIAN_POINT('Ctrl Pts',(0.21382646341409,11.6872334852206,0.0175563853606194));
#93331=CARTESIAN_POINT('Ctrl Pts',(0.103404433621971,11.6177861304089,0.0203950453979665));
#93332=CARTESIAN_POINT('Ctrl Pts',(-7.31578044671499E-10,11.5001144176338,
0.0228642037764085));
#93333=CARTESIAN_POINT('',(1.71367396487917,10.884828376917,-0.0272688936357386));
#93334=CARTESIAN_POINT('Ctrl Pts',(1.71323760973584,10.884757371723,-0.0272600945708667));
#93335=CARTESIAN_POINT('Ctrl Pts',(1.71095380282436,10.9522588475904,-0.0269537299596494));
#93336=CARTESIAN_POINT('Ctrl Pts',(1.70125599859845,11.0194421721267,-0.0264411629320617));
#93337=CARTESIAN_POINT('Ctrl Pts',(1.66832024614853,11.150863447781,-0.0250479361935688));
#93338=CARTESIAN_POINT('Ctrl Pts',(1.64499600892519,11.2151054272743,-0.0241648487888341));
#93339=CARTESIAN_POINT('Ctrl Pts',(1.58618668503831,11.3373729668203,-0.0220809066579494));
#93340=CARTESIAN_POINT('Ctrl Pts',(1.5506912354297,11.3955174606547,-0.0208793348533259));
#93341=CARTESIAN_POINT('Ctrl Pts',(1.46868851153284,11.5032546695393,-0.0181989480045432));
#93342=CARTESIAN_POINT('Ctrl Pts',(1.42218772068958,11.552858424867,-0.0167202746198522));
#93343=CARTESIAN_POINT('Ctrl Pts',(1.37078399030106,11.5968559808931,-0.0151246218382906));
#93344=CARTESIAN_POINT('',(1.71371885186958,10.8205931966853,-0.0274987012850932));
#93345=CARTESIAN_POINT('Ctrl Pts',(1.71367158232227,10.8847577695798,-0.0272722299410126));
#93346=CARTESIAN_POINT('Ctrl Pts',(1.71332804833583,10.8740884873295,-0.027300951008168));
#93347=CARTESIAN_POINT('Ctrl Pts',(1.71316046545629,10.8634136017891,-0.0273346129839613));
#93348=CARTESIAN_POINT('Ctrl Pts',(1.71317536219933,10.8420544454392,-0.0274117607591387));
#93349=CARTESIAN_POINT('Ctrl Pts',(1.71335815656387,10.831370214279,-0.0274552552183969));
#93350=CARTESIAN_POINT('Ctrl Pts',(1.71371536404704,10.8206918479203,-0.0275036063755117));
#93351=CARTESIAN_POINT('',(1.70529432647543,10.72808525788,-0.0276007795948528));
#93352=CARTESIAN_POINT('Ctrl Pts',(1.70529432647543,10.72808525788,-0.0276007795948528));
#93353=CARTESIAN_POINT('Ctrl Pts',(1.70735454658141,10.7434173025721,-0.0276033180225536));
#93354=CARTESIAN_POINT('Ctrl Pts',(1.70904613121517,10.7587984274458,-0.0275953706002022));
#93355=CARTESIAN_POINT('Ctrl Pts',(1.71168063254266,10.7896797461349,-0.0275581102060633));
#93356=CARTESIAN_POINT('Ctrl Pts',(1.71262079348754,10.8051786491146,-0.0275287248021881));
#93357=CARTESIAN_POINT('Ctrl Pts',(1.71317372525099,10.8206923858305,-0.0274884565705673));
#93358=CARTESIAN_POINT('',(0.236247419988345,10.0098541173715,0.0109034851016902));
#93359=CARTESIAN_POINT('Ctrl Pts',(0.236247419988345,10.0098541173715,0.0109034851016902));
#93360=CARTESIAN_POINT('Ctrl Pts',(0.30606056814941,9.96856972869477,0.00880272772994621));
#93361=CARTESIAN_POINT('Ctrl Pts',(0.381103068719988,9.93630945446466,0.00658814085987126));
#93362=CARTESIAN_POINT('Ctrl Pts',(0.536789596238908,9.89086391615539,0.00207083621442976));
#93363=CARTESIAN_POINT('Ctrl Pts',(0.617427443273441,9.87767541233786,-0.000231720367397251));
#93364=CARTESIAN_POINT('Ctrl Pts',(0.72992935704866,9.87330259655987,-0.00339374139128517));
#93365=CARTESIAN_POINT('Ctrl Pts',(0.761467622684855,9.87359480108384,-0.00427471421096523));
#93366=CARTESIAN_POINT('Ctrl Pts',(0.942427970193946,9.88416684405416,-0.00929760631769659));
#93367=CARTESIAN_POINT('Ctrl Pts',(1.0684186552677,9.92647143273604,-0.0126691792673942));
#93368=CARTESIAN_POINT('Ctrl Pts',(1.26139994575964,10.0202638957781,-0.0177292948903863));
#93369=CARTESIAN_POINT('Ctrl Pts',(1.36839556444661,10.0913712265771,-0.0204661660330931));
#93370=CARTESIAN_POINT('Ctrl Pts',(1.52969665304764,10.2744047761715,-0.0243196977313969));
#93371=CARTESIAN_POINT('Ctrl Pts',(1.58325884460451,10.3578038615545,-0.0255180527928208));
#93372=CARTESIAN_POINT('Ctrl Pts',(1.66446908023142,10.5360177894713,-0.0271490183867767));
#93373=CARTESIAN_POINT('Ctrl Pts',(1.69226021046953,10.6310860835949,-0.0275847200675102));
#93374=CARTESIAN_POINT('Ctrl Pts',(1.70529432647543,10.72808525788,-0.0276007795948528));
#93375=CARTESIAN_POINT('Ctrl Pts',(1.2490009027033E-15,10.205522161444,
0.0182134784999908));
#93376=CARTESIAN_POINT('Ctrl Pts',(0.033968553860442,10.1670088719863,0.0171251326194028));
#93377=CARTESIAN_POINT('Ctrl Pts',(0.0709495090590134,10.1311471009747,
0.0159620650678615));
#93378=CARTESIAN_POINT('Ctrl Pts',(0.150002720154503,10.0656333354706,0.0135158510258428));
#93379=CARTESIAN_POINT('Ctrl Pts',(0.192074236372062,10.035976172164,0.0122327066532125));
#93380=CARTESIAN_POINT('Ctrl Pts',(0.236247419988344,10.0098541173715,0.0109034851016902));
#93381=CARTESIAN_POINT('Ctrl Pts',(1.30897478982197,11.3504630390858,-2.50498148137219));
#93382=CARTESIAN_POINT('Ctrl Pts',(1.38386448873185,11.8926837577678,0.261422345341801));
#93383=CARTESIAN_POINT('Ctrl Pts',(1.51312640105233,11.2420912813384,4.85222885469421));
#93384=CARTESIAN_POINT('Ctrl Pts',(1.69450156347185,6.96747103308611,9.80841498077292));
#93385=CARTESIAN_POINT('Ctrl Pts',(1.85302105907588,1.69666347680562,11.8855184550591));
#93386=CARTESIAN_POINT('Ctrl Pts',(2.01132807879988,-3.94947939190903,11.3373251838206));
#93387=CARTESIAN_POINT('Ctrl Pts',(2.16948245088834,-8.70317504738577,8.24890086458565));
#93388=CARTESIAN_POINT('Ctrl Pts',(2.32764998417709,-11.5100452091871,3.33273214547989));
#93389=CARTESIAN_POINT('Ctrl Pts',(2.48532551435814,-11.7452138138953,-2.32118714406843));
#93390=CARTESIAN_POINT('Ctrl Pts',(2.64369910587744,-9.36167700277716,-7.44664390195442));
#93391=CARTESIAN_POINT('Ctrl Pts',(2.80006441572129,-4.89466326032176,-10.9038432854129));
#93392=CARTESIAN_POINT('Ctrl Pts',(2.96038504525873,0.655585150116943,-11.9232041725978));
#93393=CARTESIAN_POINT('Ctrl Pts',(3.11196817314966,6.05030776943863,-10.2836091806122));
#93394=CARTESIAN_POINT('Ctrl Pts',(3.28097474479473,10.0860135530921,-6.35229193778149));
#93395=CARTESIAN_POINT('Ctrl Pts',(3.41362143929016,11.8666268602166,-1.01359022713016));
#93396=CARTESIAN_POINT('Ctrl Pts',(3.62798652276341,10.9978448176373,4.53108407232712));
#93397=CARTESIAN_POINT('Ctrl Pts',(3.83136289374924,7.68047060934463,9.06465386067078));
#93398=CARTESIAN_POINT('Ctrl Pts',(4.05934605751117,2.10302841524976,11.8468921137569));
#93399=CARTESIAN_POINT('Ctrl Pts',(4.30893325794595,-4.85958883366253,11.1951873452828));
#93400=CARTESIAN_POINT('Ctrl Pts',(4.58111469907456,-10.5439802324246,6.10854505812171));
#93401=CARTESIAN_POINT('Ctrl Pts',(4.85266833009858,-12.0838233435126,-1.33981903278729));
#93402=CARTESIAN_POINT('Ctrl Pts',(5.12382899664887,-8.91442850896208,-8.23976580227665));
#93403=CARTESIAN_POINT('Ctrl Pts',(5.39447422289012,-2.27332112649084,-11.9037038363946));
#93404=CARTESIAN_POINT('Ctrl Pts',(5.63462866738158,4.38930278932178,-11.0139596956066));
#93405=CARTESIAN_POINT('Ctrl Pts',(5.84443876548001,8.89587552847269,-7.49634408243274));
#93406=CARTESIAN_POINT('Ctrl Pts',(6.02405598838773,11.1785196113352,-3.17466519093072));
#93407=CARTESIAN_POINT('Ctrl Pts',(6.23334858135947,11.5367789170952,2.51834492771313));
#93408=CARTESIAN_POINT('Ctrl Pts',(6.47216536153378,8.52591928036444,8.48613021692799));
#93409=CARTESIAN_POINT('Ctrl Pts',(6.74032351979013,1.81378966884307,11.8672295275066));
#93410=CARTESIAN_POINT('Ctrl Pts',(7.0079645542307,-5.57435948674926,10.605462370046));
#93411=CARTESIAN_POINT('Ctrl Pts',(7.27508531570782,-10.7625364349888,5.21331503061486));
#93412=CARTESIAN_POINT('Ctrl Pts',(7.5416794938748,-11.7311710285706,-2.19176367291935));
#93413=CARTESIAN_POINT('Ctrl Pts',(7.8077437693088,-8.1229758038346,-8.7108511612512));
#93414=CARTESIAN_POINT('Ctrl Pts',(8.07327440627059,-1.35788077218519,-11.810228596338));
#93415=CARTESIAN_POINT('Ctrl Pts',(8.3088229880755,5.09482672424843,-10.4525999052638));
#93416=CARTESIAN_POINT('Ctrl Pts',(8.51457805138463,9.24392923696522,-6.68374543262319));
#93417=CARTESIAN_POINT('Ctrl Pts',(8.69069787800009,11.1618634053179,-2.28846725754921));
#93418=CARTESIAN_POINT('Ctrl Pts',(8.86657573197387,11.0975692878018,2.49903950200297));
#93419=CARTESIAN_POINT('Ctrl Pts',(9.06172558105388,8.85449784911366,7.32026089744886));
#93420=CARTESIAN_POINT('Ctrl Pts',(9.23707598578613,4.95803577700564,10.2175308052139));
#93421=CARTESIAN_POINT('Ctrl Pts',(9.41218197984377,0.353935032346256,11.2200746322382));
#93422=CARTESIAN_POINT('Ctrl Pts',(9.56765013607029,-3.83951280272671,10.6454205565639));
#93423=CARTESIAN_POINT('Ctrl Pts',(9.74230644009734,-7.8631980922651,8.10968127001615));
#93424=CARTESIAN_POINT('Ctrl Pts',(9.94578506400173,-10.9327846091029,3.49606033646916));
#93425=CARTESIAN_POINT('Ctrl Pts',(10.1779215386847,-11.3026255166413,-2.99474193137141));
#93426=CARTESIAN_POINT('Ctrl Pts',(10.3950862741132,-7.96186222719694,-8.07924641994259));
#93427=CARTESIAN_POINT('Ctrl Pts',(10.5685399649705,-3.88496594820853,-10.3692560271556));
#93428=CARTESIAN_POINT('Ctrl Pts',(10.7418080726905,0.698226275935602,-11.2916890703984));
#93429=CARTESIAN_POINT('Ctrl Pts',(10.9292134877369,5.73545411152713,-9.83539908865925));
#93430=CARTESIAN_POINT('Ctrl Pts',(11.1306736564829,9.51259625505713,-5.8530435057731));
#93431=CARTESIAN_POINT('Ctrl Pts',(11.303106225153,11.0641086404226,-1.42127934142605));
#93432=CARTESIAN_POINT('Ctrl Pts',(11.4561595909811,10.6960254211943,2.72874079862435));
#93433=CARTESIAN_POINT('Ctrl Pts',(11.6281385166885,8.7278532497703,6.91733533563937));
#93434=CARTESIAN_POINT('Ctrl Pts',(11.7998702409163,5.11081927142178,10.0033545553924));
#93435=CARTESIAN_POINT('Ctrl Pts',(11.990363183906,0.0338904688058861,11.0876495659952));
#93436=CARTESIAN_POINT('Ctrl Pts',(12.1615603432201,-4.52246394700098,10.1101748948404));
#93437=CARTESIAN_POINT('Ctrl Pts',(12.3325112871038,-8.26592723037474,7.34305430882504));
#93438=CARTESIAN_POINT('Ctrl Pts',(12.5316675984782,-10.9260818914473,2.61447385314119));
#93439=CARTESIAN_POINT('Ctrl Pts',(12.7588657234676,-10.8119033324059,-3.74505536412208));
#93440=CARTESIAN_POINT('Ctrl Pts',(13.0139143775298,-6.45822803221135,-9.41359275769931));
#93441=CARTESIAN_POINT('Ctrl Pts',(13.2684156739832,0.391051711522962,-11.3845366962931));
#93442=CARTESIAN_POINT('Ctrl Pts',(13.5223720121342,7.06058079564972,-8.90911861064873));
#93443=CARTESIAN_POINT('Ctrl Pts',(13.7757872242173,10.9472554116764,-2.96870788326275));
#93444=CARTESIAN_POINT('Ctrl Pts',(14.0286634776398,10.5494242808733,4.10178934251099));
#93445=CARTESIAN_POINT('Ctrl Pts',(14.2810050361338,6.0378241672127,9.54734246153401));
#93446=CARTESIAN_POINT('Ctrl Pts',(14.5048367771901,-0.0457796910363487,
11.0484597831507));
#93447=CARTESIAN_POINT('Ctrl Pts',(14.7003478024558,-5.15247455494966,9.53528368421946));
#93448=CARTESIAN_POINT('Ctrl Pts',(14.8676959182846,-8.60689881955561,6.56596087686259));
#93449=CARTESIAN_POINT('Ctrl Pts',(15.0348124912905,-10.5304401021696,2.44009830321553));
#93450=CARTESIAN_POINT('Ctrl Pts',(15.2016992363267,-10.5889896031044,-2.10339644174452));
#93451=CARTESIAN_POINT('Ctrl Pts',(15.3683571298684,-8.77365701916214,-6.26387195102793));
#93452=CARTESIAN_POINT('Ctrl Pts',(15.5347882691619,-5.41443881745476,-9.30488661898314));
#93453=CARTESIAN_POINT('Ctrl Pts',(15.7009938729794,-1.10506303701437,-10.6939689442717));
#93454=CARTESIAN_POINT('Ctrl Pts',(15.8669756154884,3.38421159098208,-10.1885736990089));
#93455=CARTESIAN_POINT('Ctrl Pts',(16.0603620719526,7.91915265148676,-7.50326322098924));
#93456=CARTESIAN_POINT('Ctrl Pts',(16.239636841349,10.346417595362,-3.11521415876683));
#93457=CARTESIAN_POINT('Ctrl Pts',(16.4048767410778,10.4634131688112,1.34239684552686));
#93458=CARTESIAN_POINT('Ctrl Pts',(16.5493197829215,9.35599017071544,5.07525108848545));
#93459=CARTESIAN_POINT('Ctrl Pts',(16.7141963176832,6.49237344325913,8.56862170466309));
#93460=CARTESIAN_POINT('Ctrl Pts',(16.8994136289952,1.83069526121731,10.5775323405323));
#93461=CARTESIAN_POINT('Ctrl Pts',(17.0843650545091,-3.22035309403346,10.2223670343401));
#93462=CARTESIAN_POINT('Ctrl Pts',(17.2895747157592,-8.03234514251166,7.30506860791021));
#93463=CARTESIAN_POINT('Ctrl Pts',(17.5149342113487,-10.8733400024111,1.67419416675553));
#93464=CARTESIAN_POINT('Ctrl Pts',(17.7603281370208,-9.73044464288831,-5.10667512772299));
#93465=CARTESIAN_POINT('Ctrl Pts',(17.9848608346678,-5.19699805192515,-9.46388837584811));
#93466=CARTESIAN_POINT('Ctrl Pts',(18.1886661451407,0.265632069066906,-10.6262404306785));
#93467=CARTESIAN_POINT('Ctrl Pts',(18.3718394205153,5.10633304707169,-9.30876868720459));
#93468=CARTESIAN_POINT('Ctrl Pts',(18.5547939179018,8.79802794991572,-5.91765010486416));
#93469=CARTESIAN_POINT('Ctrl Pts',(18.7374627363208,10.5191177631719,-1.2179863155584));
#93470=CARTESIAN_POINT('Ctrl Pts',(18.9200143211695,9.89212967677138,3.74154082705846));
#93471=CARTESIAN_POINT('Ctrl Pts',(19.1020930075487,7.06236441759157,7.85504180831257));
#93472=CARTESIAN_POINT('Ctrl Pts',(19.2844116650314,2.66565483537424,10.2072618947442));
#93473=CARTESIAN_POINT('Ctrl Pts',(19.4657299037891,-2.31400728008752,10.2809442197002));
#93474=CARTESIAN_POINT('Ctrl Pts',(19.648066469154,-6.76693935292665,8.0595630932652));
#93475=CARTESIAN_POINT('Ctrl Pts',(19.8276165222382,-9.70035629775437,4.05485210714321));
#93476=CARTESIAN_POINT('Ctrl Pts',(20.0175251180967,-10.4657896755927,-0.857742150482306));
#93477=CARTESIAN_POINT('Ctrl Pts',(20.1343530166592,-8.89702629841736,-5.56249800699203));
#93478=CARTESIAN_POINT('Ctrl Pts',(20.2829990256603,-5.34622937894769,-9.01726442891408));
#93479=CARTESIAN_POINT('Ctrl Pts',(20.416084338308,-0.60971988323014,-10.4571484597653));
#93480=CARTESIAN_POINT('Ctrl Pts',(20.5566179423485,4.25527008514754,-9.56204556806775));
#93481=CARTESIAN_POINT('Ctrl Pts',(20.6934363685739,8.16330759088052,-6.53628165676501));
#93482=CARTESIAN_POINT('Ctrl Pts',(20.8317979438454,10.2448413935788,-2.05829576335044));
#93483=CARTESIAN_POINT('Ctrl Pts',(20.9693138595582,10.0386345642595,2.87335852336565));
#93484=CARTESIAN_POINT('Ctrl Pts',(21.1070527977384,7.59382441058238,7.15294197070558));
#93485=CARTESIAN_POINT('Ctrl Pts',(21.2445261479924,3.46011245261836,9.83939395559342));
#93486=CARTESIAN_POINT('Ctrl Pts',(21.3820140102286,-1.44110991972201,10.3106942348191));
#93487=CARTESIAN_POINT('Ctrl Pts',(21.5192385743442,-6.00937269882226,8.51719726799948));
#93488=CARTESIAN_POINT('Ctrl Pts',(21.6765786177924,-9.70830673657193,4.21254883161156));
#93489=CARTESIAN_POINT('Ctrl Pts',(21.7873558901873,-10.268703591987,0.279124218596134));
#93490=CARTESIAN_POINT('Ctrl Pts',(21.8541003835446,-9.80111969116135,-2.18436427930479));
#93491=CARTESIAN_POINT('Ctrl Pts',(1.18974746786317,11.4517922664652,-2.52090132956655));
#93492=CARTESIAN_POINT('Ctrl Pts',(1.26518414667326,11.9988181450597,0.265780471340153));
#93493=CARTESIAN_POINT('Ctrl Pts',(1.39565853232302,11.3425692650812,4.89981968805774));
#93494=CARTESIAN_POINT('Ctrl Pts',(1.57866787392373,7.02897372769986,9.90043289144675));
#93495=CARTESIAN_POINT('Ctrl Pts',(1.73867035820078,1.70925650077172,11.9974400786412));
#93496=CARTESIAN_POINT('Ctrl Pts',(1.89846534925839,-3.99014183964466,11.4439163937075));
#93497=CARTESIAN_POINT('Ctrl Pts',(2.05813461856846,-8.78937060554582,8.32616088827542));
#93498=CARTESIAN_POINT('Ctrl Pts',(2.2178372191676,-11.6235870025466,3.36222965129985));
#93499=CARTESIAN_POINT('Ctrl Pts',(2.37706510609572,-11.8611623899059,-2.3473285393946));
#93500=CARTESIAN_POINT('Ctrl Pts',(2.53702005955193,-9.4538997106099,-7.52403366560333));
#93501=CARTESIAN_POINT('Ctrl Pts',(2.69496675943479,-4.94174608981969,-11.0162600707292));
#93502=CARTESIAN_POINT('Ctrl Pts',(2.85693169535897,0.665427965998577,-12.046217394457));
#93503=CARTESIAN_POINT('Ctrl Pts',(3.01008843650435,6.11617669158266,-10.3895731296628));
#93504=CARTESIAN_POINT('Ctrl Pts',(3.18087145496237,10.1944375660391,-6.41713549186393));
#93505=CARTESIAN_POINT('Ctrl Pts',(3.31492761737946,11.9939986422514,-1.02153441070433));
#93506=CARTESIAN_POINT('Ctrl Pts',(3.53165396391817,11.1159703877652,4.58442295205435));
#93507=CARTESIAN_POINT('Ctrl Pts',(3.73722553710061,7.76246260128082,9.16681927618251));
#93508=CARTESIAN_POINT('Ctrl Pts',(3.96775616233569,2.12305632832777,11.980505907057));
#93509=CARTESIAN_POINT('Ctrl Pts',(4.22015087915041,-4.918109620414,11.3214168981758));
#93510=CARTESIAN_POINT('Ctrl Pts',(4.49546369841027,-10.6680280311112,6.1766295866806));
#93511=CARTESIAN_POINT('Ctrl Pts',(4.77019090889438,-12.2260930284393,-1.35884290056484));
#93512=CARTESIAN_POINT('Ctrl Pts',(5.04457454319731,-9.01924683266811,-8.34087088097074));
#93513=CARTESIAN_POINT('Ctrl Pts',(5.31848644889902,-2.29805924217776,-12.049253587911));
#93514=CARTESIAN_POINT('Ctrl Pts',(5.56158289892602,4.4462322167097,-11.1487877087618));
#93515=CARTESIAN_POINT('Ctrl Pts',(5.77399527205737,9.00875437884592,-7.58759241958776));
#93516=CARTESIAN_POINT('Ctrl Pts',(5.95586064806108,11.3200193718728,-3.21184415601971));
#93517=CARTESIAN_POINT('Ctrl Pts',(6.167795918538,11.6828725325942,2.55304786169007));
#93518=CARTESIAN_POINT('Ctrl Pts',(6.40966019967681,8.63373216818036,8.5970722721158));
#93519=CARTESIAN_POINT('Ctrl Pts',(6.68128293317983,1.83495642429353,12.0220246559432));
#93520=CARTESIAN_POINT('Ctrl Pts',(6.95242181181914,-5.64979323947622,10.7439345769541));
#93521=CARTESIAN_POINT('Ctrl Pts',(7.22307251307632,-10.9066557638468,5.28064151031707));
#93522=CARTESIAN_POINT('Ctrl Pts',(7.49322591235527,-11.8883788942064,-2.22329037953124));
#93523=CARTESIAN_POINT('Ctrl Pts',(7.762877003322,-8.23166841266443,-8.83034127715893));
#93524=CARTESIAN_POINT('Ctrl Pts',(8.03202026329645,-1.37458546094406,-11.9720187625362));
#93525=CARTESIAN_POINT('Ctrl Pts',(8.27080031567461,5.1666841103954,-10.5958720135022));
#93526=CARTESIAN_POINT('Ctrl Pts',(8.47939743040809,9.37312928197355,-6.77498911346165));
#93527=CARTESIAN_POINT('Ctrl Pts',(8.65796190964001,11.3177170749869,-2.3187107460461));
#93528=CARTESIAN_POINT('Ctrl Pts',(8.83629282307935,11.2525571600563,2.53557131712909));
#93529=CARTESIAN_POINT('Ctrl Pts',(9.03417691141257,8.97809165929157,7.42435568944228));
#93530=CARTESIAN_POINT('Ctrl Pts',(9.21199612018571,5.02679642075796,10.3624580547133));
#93531=CARTESIAN_POINT('Ctrl Pts',(9.38957733795619,0.35761650699035,11.3791857664677));
#93532=CARTESIAN_POINT('Ctrl Pts',(9.54724976039764,-3.8952913802988,10.7964042010188));
#93533=CARTESIAN_POINT('Ctrl Pts',(9.72439118282002,-7.97624041142031,8.22460440416845));
#93534=CARTESIAN_POINT('Ctrl Pts',(9.93077429626411,-11.0896632215142,3.54514357646063));
#93535=CARTESIAN_POINT('Ctrl Pts',(10.1662370872959,-11.4648622236249,-3.03865513251931));
#93536=CARTESIAN_POINT('Ctrl Pts',(10.3865254314365,-8.07608583722479,-8.19631869413491));
#93537=CARTESIAN_POINT('Ctrl Pts',(10.5624802891134,-3.94040545902368,-10.5193556970742));
#93538=CARTESIAN_POINT('Ctrl Pts',(10.7382506126395,0.708969224933737,-11.4551172204512));
#93539=CARTESIAN_POINT('Ctrl Pts',(10.9283685210332,5.81910754761555,-9.97777463152521));
#93540=CARTESIAN_POINT('Ctrl Pts',(11.1327495067884,9.65101628657111,-5.93769000513916));
#93541=CARTESIAN_POINT('Ctrl Pts',(11.3076849817366,11.2250562811182,-1.44160136579286));
#93542=CARTESIAN_POINT('Ctrl Pts',(11.4629625774418,10.8516272644798,2.76872199953724));
#93543=CARTESIAN_POINT('Ctrl Pts',(11.6374418821889,8.85484247875078,7.01821193605031));
#93544=CARTESIAN_POINT('Ctrl Pts',(11.8116716998053,5.18519912941044,10.1491227347192));
#93545=CARTESIAN_POINT('Ctrl Pts',(12.0049367578346,0.0343959505934401,
11.2491953572123));
#93546=CARTESIAN_POINT('Ctrl Pts',(12.1786245890754,-4.58824344319239,10.2574978750432));
#93547=CARTESIAN_POINT('Ctrl Pts',(12.352062477449,-8.38615633729713,7.45012563881324));
#93548=CARTESIAN_POINT('Ctrl Pts',(12.554113756606,-11.0849733631632,2.65280836007122));
#93549=CARTESIAN_POINT('Ctrl Pts',(12.7846122961941,-10.9691146512919,-3.7990828045243));
#93550=CARTESIAN_POINT('Ctrl Pts',(13.0433583516889,-6.55230109938501,-9.54976360017405));
#93551=CARTESIAN_POINT('Ctrl Pts',(13.3015404849569,0.396035834484766,-11.5491659899366));
#93552=CARTESIAN_POINT('Ctrl Pts',(13.5591589282335,7.16170582651916,-9.03800376659064));
#93553=CARTESIAN_POINT('Ctrl Pts',(13.8162148628397,11.1041565484206,-3.0122242034893));
#93554=CARTESIAN_POINT('Ctrl Pts',(14.0727093835286,10.7005567366767,4.15941404407192));
#93555=CARTESIAN_POINT('Ctrl Pts',(14.3286435930605,6.12466583879098,9.68243478675451));
#93556=CARTESIAN_POINT('Ctrl Pts',(14.5556458025187,-0.0451007091892611,
11.20471923806));
#93557=CARTESIAN_POINT('Ctrl Pts',(14.7539104053305,-5.22370059967178,9.670201548657));
#93558=CARTESIAN_POINT('Ctrl Pts',(14.9236060827809,-8.72655048304717,6.65920792858466));
#93559=CARTESIAN_POINT('Ctrl Pts',(15.0930560971764,-10.6769135579603,2.47573475735213));
#93560=CARTESIAN_POINT('Ctrl Pts',(15.2622606653902,-10.7362380843536,-2.13085705163885));
#93561=CARTESIAN_POINT('Ctrl Pts',(15.4312223228812,-8.89578686497418,-6.34881194318317));
#93562=CARTESIAN_POINT('Ctrl Pts',(15.5999407121251,-5.49038444331317,-9.43157994135716));
#93563=CARTESIAN_POINT('Ctrl Pts',(15.7684173535114,-1.12212996432778,-10.8396028454176));
#93564=CARTESIAN_POINT('Ctrl Pts',(15.9366523292351,3.42807230949616,-10.3273045410418));
#93565=CARTESIAN_POINT('Ctrl Pts',(16.1326467590311,8.02413915422211,-7.60574003322458));
#93566=CARTESIAN_POINT('Ctrl Pts',(16.314321409095,10.4837845689353,-3.1589303196056));
#93567=CARTESIAN_POINT('Ctrl Pts',(16.4817523929375,10.6022981932295,1.35777601683656));
#93568=CARTESIAN_POINT('Ctrl Pts',(16.628100233848,9.48025342044983,5.13984100178697));
#93569=CARTESIAN_POINT('Ctrl Pts',(16.7951358098011,6.5790973516086,8.67890252146067));
#93570=CARTESIAN_POINT('Ctrl Pts',(16.9827558713765,1.85693486775176,10.7137909459705));
#93571=CARTESIAN_POINT('Ctrl Pts',(17.1700831822853,-3.25897596162862,10.3539932205293));
#93572=CARTESIAN_POINT('Ctrl Pts',(17.3779027649741,-8.13209734273167,7.39951611744703));
#93573=CARTESIAN_POINT('Ctrl Pts',(17.6060922224903,-11.0086032355239,1.69787761110265));
#93574=CARTESIAN_POINT('Ctrl Pts',(17.8545207088345,-9.85135526552179,-5.16679810337559));
#93575=CARTESIAN_POINT('Ctrl Pts',(18.0817887133709,-5.26259033002558,-9.57691066568822));
#93576=CARTESIAN_POINT('Ctrl Pts',(18.2880380245083,0.265548580560466,-10.7530867295508));
#93577=CARTESIAN_POINT('Ctrl Pts',(18.4733796814325,5.16350438434969,-9.41993410006301));
#93578=CARTESIAN_POINT('Ctrl Pts',(18.6584701908049,8.89821185951937,-5.98916918444961));
#93579=CARTESIAN_POINT('Ctrl Pts',(18.8432409950164,10.6390066358219,-1.23539709009161));
#93580=CARTESIAN_POINT('Ctrl Pts',(19.0278628981949,10.0048039354509,3.78029736455163));
#93581=CARTESIAN_POINT('Ctrl Pts',(19.2119723825552,7.14338976532434,7.93968275473146));
#93582=CARTESIAN_POINT('Ctrl Pts',(19.3962971146005,2.69833785744414,10.3175199556526));
#93583=CARTESIAN_POINT('Ctrl Pts',(19.579564992325,-2.33502128752636,10.3921141672789));
#93584=CARTESIAN_POINT('Ctrl Pts',(19.7638538077289,-6.83522052429279,8.14659582436836));
#93585=CARTESIAN_POINT('Ctrl Pts',(19.9452412106374,-9.79898956792458,4.10104273626897));
#93586=CARTESIAN_POINT('Ctrl Pts',(20.1371455329409,-10.5721168787306,-0.863355728409352));
#93587=CARTESIAN_POINT('Ctrl Pts',(20.2551462392215,-8.98758519098429,-5.61547760810045));
#93588=CARTESIAN_POINT('Ctrl Pts',(20.4052645664765,-5.40151747470937,-9.1042056824633));
#93589=CARTESIAN_POINT('Ctrl Pts',(20.5396467848151,-0.618870314778679,
-10.5581353506426));
#93590=CARTESIAN_POINT('Ctrl Pts',(20.681528826317,4.29274934883192,-9.65430165578985));
#93591=CARTESIAN_POINT('Ctrl Pts',(20.8196362604007,8.2375272330093,-6.59999125855159));
#93592=CARTESIAN_POINT('Ctrl Pts',(20.9592798997399,10.3382476746094,-2.0804841092725));
#93593=CARTESIAN_POINT('Ctrl Pts',(21.0980466529407,10.1300663649379,2.8959570685733));
#93594=CARTESIAN_POINT('Ctrl Pts',(21.2370151017179,7.66334706916283,7.21373849358107));
#93595=CARTESIAN_POINT('Ctrl Pts',(21.3756941059591,3.49341097342452,9.92347886797355));
#93596=CARTESIAN_POINT('Ctrl Pts',(21.5143584573025,-1.44987922468851,10.3989557782019));
#93597=CARTESIAN_POINT('Ctrl Pts',(21.6527478812955,-6.05651644093992,8.58980440466931));
#93598=CARTESIAN_POINT('Ctrl Pts',(21.8113618981694,-9.78578944726137,4.2505359954563));
#93599=CARTESIAN_POINT('Ctrl Pts',(21.9230775074673,-10.3505739977289,0.283696021016612));
#93600=CARTESIAN_POINT('Ctrl Pts',(21.9902419502383,-9.87925711877443,-2.19539365961811));
#93601=CARTESIAN_POINT('Ctrl Pts',(0.903441628217493,11.5956865362208,-2.54034914141355));
#93602=CARTESIAN_POINT('Ctrl Pts',(0.979658017345533,12.1495390241206,0.275253015337542));
#93603=CARTESIAN_POINT('Ctrl Pts',(1.11185919217728,11.4853157251709,4.97085529600647));
#93604=CARTESIAN_POINT('Ctrl Pts',(1.29722630370222,7.11559218861858,10.03559800166));
#93605=CARTESIAN_POINT('Ctrl Pts',(1.4593901240281,1.72464681668832,12.1616878256515));
#93606=CARTESIAN_POINT('Ctrl Pts',(1.62137479817313,-4.05308567022919,11.6004162607819));
#93607=CARTESIAN_POINT('Ctrl Pts',(1.78329400206896,-8.9199643442394,8.43919520839999));
#93608=CARTESIAN_POINT('Ctrl Pts',(1.94529726649785,-11.7952180436883,3.40376438492117));
#93609=CARTESIAN_POINT('Ctrl Pts',(2.10687154681895,-12.0365246368009,-2.38985096138074));
#93610=CARTESIAN_POINT('Ctrl Pts',(2.26923745269956,-9.59318307000292,-7.64468833195954));
#93611=CARTESIAN_POINT('Ctrl Pts',(2.42961363996627,-5.01176400552785,-11.1907591909536));
#93612=CARTESIAN_POINT('Ctrl Pts',(2.59412589846795,0.683543359587545,-12.2372546878033));
#93613=CARTESIAN_POINT('Ctrl Pts',(2.74973808312862,6.22167787228081,-10.5540021858096));
#93614=CARTESIAN_POINT('Ctrl Pts',(2.92331316951063,10.3669128347436,-6.5171622001184));
#93615=CARTESIAN_POINT('Ctrl Pts',(3.05959909542248,12.1964574224635,-1.03146587853192));
#93616=CARTESIAN_POINT('Ctrl Pts',(3.28013866994355,11.3038043278321,4.67361588913699));
#93617=CARTESIAN_POINT('Ctrl Pts',(3.48921509325285,7.89233189478907,9.33384404675561));
#93618=CARTESIAN_POINT('Ctrl Pts',(3.7238939372982,2.15239269705436,12.1990469837114));
#93619=CARTESIAN_POINT('Ctrl Pts',(3.98088049228753,-5.01739795831119,11.5278737873867));
#93620=CARTESIAN_POINT('Ctrl Pts',(4.26138198908379,-10.8759517203058,6.28713144448326));
#93621=CARTESIAN_POINT('Ctrl Pts',(4.54141217777241,-12.4647033890014,-1.39391008316943));
#93622=CARTESIAN_POINT('Ctrl Pts',(4.82123757322336,-9.19485740050448,-8.51453853976309));
#93623=CARTESIAN_POINT('Ctrl Pts',(5.1007140760936,-2.33739080685041,-12.298841317748));
#93624=CARTESIAN_POINT('Ctrl Pts',(5.34886880731605,4.54729884524234,-11.3801342835202));
#93625=CARTESIAN_POINT('Ctrl Pts',(5.56578483547677,9.20670066674851,-7.74358589277483));
#93626=CARTESIAN_POINT('Ctrl Pts',(5.75156316224047,11.5678259674798,-3.27376473974182));
#93627=CARTESIAN_POINT('Ctrl Pts',(5.96812411478037,11.938803177318,2.61691849448023));
#93628=CARTESIAN_POINT('Ctrl Pts',(6.21535908381347,8.82238390057781,8.79536260171968));
#93629=CARTESIAN_POINT('Ctrl Pts',(6.49313495565504,1.86984596831206,12.298388326641));
#93630=CARTESIAN_POINT('Ctrl Pts',(6.77053350207384,-5.78779554802438,10.9913053328563));
#93631=CARTESIAN_POINT('Ctrl Pts',(7.04754819093855,-11.1686313246679,5.39990857726151));
#93632=CARTESIAN_POINT('Ctrl Pts',(7.324164919137,-12.1743331960759,-2.28349397809555));
#93633=CARTESIAN_POINT('Ctrl Pts',(7.60037559731866,-8.42908729095345,-9.05150436343379));
#93634=CARTESIAN_POINT('Ctrl Pts',(7.87617142963179,-1.40270668032046,-12.2712679337148));
#93635=CARTESIAN_POINT('Ctrl Pts',(8.12094266444456,5.30279634249133,-10.860966895162));
#93636=CARTESIAN_POINT('Ctrl Pts',(8.33483813586797,9.61619727452542,-6.94314027168755));
#93637=CARTESIAN_POINT('Ctrl Pts',(8.51798011869584,11.6107486373453,-2.37266665322963));
#93638=CARTESIAN_POINT('Ctrl Pts',(8.70092420271314,11.5440204005338,2.60719448233829));
#93639=CARTESIAN_POINT('Ctrl Pts',(8.90397235759044,9.21032715117327,7.62361020233496));
#93640=CARTESIAN_POINT('Ctrl Pts',(9.08647734189219,5.15501713728993,10.6392974998355));
#93641=CARTESIAN_POINT('Ctrl Pts',(9.26877643799424,0.361793133769277,11.6830912584508));
#93642=CARTESIAN_POINT('Ctrl Pts',(9.430664325476,-4.00483936387056,11.0848200731915));
#93643=CARTESIAN_POINT('Ctrl Pts',(9.61257868421856,-8.19580469716808,8.4438069689631));
#93644=CARTESIAN_POINT('Ctrl Pts',(9.82456303798387,-11.3938252065926,3.63741421882482));
#93645=CARTESIAN_POINT('Ctrl Pts',(10.0664719630594,-11.7795844654107,-3.12660926401823));
#93646=CARTESIAN_POINT('Ctrl Pts',(10.2928503059377,-8.2973304430841,-8.42702524023792));
#93647=CARTESIAN_POINT('Ctrl Pts',(10.4737043934838,-4.04650394557917,-10.8147950872555));
#93648=CARTESIAN_POINT('Ctrl Pts',(10.6543909804151,0.732894864854846,-11.7767781854194));
#93649=CARTESIAN_POINT('Ctrl Pts',(10.8498591133757,5.98692392555446,-10.2580419437641));
#93650=CARTESIAN_POINT('Ctrl Pts',(11.0600325724026,9.92751353416783,-6.1035108728662));
#93651=CARTESIAN_POINT('Ctrl Pts',(11.2399512369267,11.546460582177,-1.47936245392121));
#93652=CARTESIAN_POINT('Ctrl Pts',(11.3996731072529,11.1624047905268,2.85148184763383));
#93653=CARTESIAN_POINT('Ctrl Pts',(11.5791658207047,9.10827354395886,7.22309597989244));
#93654=CARTESIAN_POINT('Ctrl Pts',(11.7584243417152,5.33277954211481,10.4444566098854));
#93655=CARTESIAN_POINT('Ctrl Pts',(11.9572932478171,0.0326178630782873,
11.5764970906776));
#93656=CARTESIAN_POINT('Ctrl Pts',(12.1360376686652,-4.72461621902352,10.5559808042784));
#93657=CARTESIAN_POINT('Ctrl Pts',(12.3145418868021,-8.63351244335065,7.66662870298955));
#93658=CARTESIAN_POINT('Ctrl Pts',(12.5225155707071,-11.4114946324002,2.72871466178511));
#93659=CARTESIAN_POINT('Ctrl Pts',(12.7597959443576,-11.2923500573187,-3.91302535507406));
#93660=CARTESIAN_POINT('Ctrl Pts',(13.0261856238862,-6.74514927963575,-9.83368730756411));
#93661=CARTESIAN_POINT('Ctrl Pts',(13.292021165761,0.409157784142408,-11.8924724744053));
#93662=CARTESIAN_POINT('Ctrl Pts',(13.557298875633,7.37603514967898,-9.30672631479365));
#93663=CARTESIAN_POINT('Ctrl Pts',(13.8220144202162,11.43603621917,-3.10140811095855));
#93664=CARTESIAN_POINT('Ctrl Pts',(14.086165589555,11.0204456508738,4.28435228537355));
#93665=CARTESIAN_POINT('Ctrl Pts',(14.3497490950746,6.30779512977284,9.97248011234989));
#93666=CARTESIAN_POINT('Ctrl Pts',(14.5835381803786,-0.0464713597019573,
11.5403085937317));
#93667=CARTESIAN_POINT('Ctrl Pts',(14.7877335980687,-5.37998875590803,9.95988209741448));
#93668=CARTESIAN_POINT('Ctrl Pts',(14.9625028495183,-8.98758107606861,6.85885374524538));
#93669=CARTESIAN_POINT('Ctrl Pts',(15.1370166293793,-10.9962276335929,2.55034433801783));
#93670=CARTESIAN_POINT('Ctrl Pts',(15.3112747861453,-11.057316471522,-2.19384403747148));
#93671=CARTESIAN_POINT('Ctrl Pts',(15.4852762580546,-9.16194215872132,-6.53762558663525));
#93672=CARTESIAN_POINT('Ctrl Pts',(15.6590212752161,-5.65505712284883,-9.71224134793712));
#93673=CARTESIAN_POINT('Ctrl Pts',(15.8325093831332,-1.15683632859144,-11.1621233815762));
#93674=CARTESIAN_POINT('Ctrl Pts',(16.0057407273942,3.52850982383791,-10.634588642758));
#93675=CARTESIAN_POINT('Ctrl Pts',(16.2075439831294,8.26078713351443,-7.83231510161214));
#93676=CARTESIAN_POINT('Ctrl Pts',(16.3945835370073,10.79301239595,-3.25410627544597));
#93677=CARTESIAN_POINT('Ctrl Pts',(16.5669469472843,10.9149944222274,1.39566838694312));
#93678=CARTESIAN_POINT('Ctrl Pts',(16.7175961104587,9.75994551453762,5.28890387414351));
#93679=CARTESIAN_POINT('Ctrl Pts',(16.8895254520512,6.77373145232914,8.93163549966943));
#93680=CARTESIAN_POINT('Ctrl Pts',(17.0826211217225,1.91369898979447,11.025856134666));
#93681=CARTESIAN_POINT('Ctrl Pts',(17.2753922254922,-3.3508976031883,10.6555208202389));
#93682=CARTESIAN_POINT('Ctrl Pts',(17.4892223589,-8.36495116825048,7.61549170937787));
#93683=CARTESIAN_POINT('Ctrl Pts',(17.7239740129484,-11.323999962384,1.74977000123159));
#93684=CARTESIAN_POINT('Ctrl Pts',(17.9794946102052,-10.1334781781364,-5.31086964421616));
#93685=CARTESIAN_POINT('Ctrl Pts',(18.2131956523234,-5.41461046876539,-9.84567084479958));
#93686=CARTESIAN_POINT('Ctrl Pts',(18.4252409173706,0.2689155062104,-11.0547790277262));
#93687=CARTESIAN_POINT('Ctrl Pts',(18.6157538537825,5.30353569117718,-9.68430051555971));
#93688=CARTESIAN_POINT('Ctrl Pts',(18.8059711829349,9.14161879340698,-6.15840703222966));
#93689=CARTESIAN_POINT('Ctrl Pts',(18.9958193954241,10.9301430713354,-1.27390300512045));
#93690=CARTESIAN_POINT('Ctrl Pts',(19.1854745393041,10.2785058526305,3.87847986224289));
#93691=CARTESIAN_POINT('Ctrl Pts',(19.3745566088602,7.33965248047654,8.15027554492915));
#93692=CARTESIAN_POINT('Ctrl Pts',(19.5638226072173,2.77544111869361,10.5915075520203));
#93693=CARTESIAN_POINT('Ctrl Pts',(19.7519388114443,-2.39136880705402,10.6682602417168));
#93694=CARTESIAN_POINT('Ctrl Pts',(19.9410928244703,-7.0098241819731,8.36292115754712));
#93695=CARTESIAN_POINT('Ctrl Pts',(20.1271442720693,-10.0503377871766,4.21349399010993));
#93696=CARTESIAN_POINT('Ctrl Pts',(20.3240622194817,-10.8431563294057,-0.880894283363258));
#93697=CARTESIAN_POINT('Ctrl Pts',(20.4450629396927,-9.21826875757226,-5.75417784878344));
#93698=CARTESIAN_POINT('Ctrl Pts',(20.5989705638437,-5.54148991110627,-9.330623077557));
#93699=CARTESIAN_POINT('Ctrl Pts',(20.7367118993859,-0.639233991474592,
-10.8209454851943));
#93700=CARTESIAN_POINT('Ctrl Pts',(20.8821091417125,4.39406593230452,-9.8944887684073));
#93701=CARTESIAN_POINT('Ctrl Pts',(21.0236016284966,8.43547518933461,-6.76521535821915));
#93702=CARTESIAN_POINT('Ctrl Pts',(21.1666348355068,10.5870605911627,-2.13587908149872));
#93703=CARTESIAN_POINT('Ctrl Pts',(21.3087336481745,10.3737327496134,2.95997788375124));
#93704=CARTESIAN_POINT('Ctrl Pts',(21.4510017239846,7.84825374656463,7.380423184045));
#93705=CARTESIAN_POINT('Ctrl Pts',(21.59294179475,3.58032156429269,10.1533105718855));
#93706=CARTESIAN_POINT('Ctrl Pts',(21.7348140241776,-1.47776662004928,10.6402982054532));
#93707=CARTESIAN_POINT('Ctrl Pts',(21.8764055683373,-6.19000771396059,8.788190550891));
#93708=CARTESIAN_POINT('Ctrl Pts',(22.0385534863357,-10.0035800617522,4.35288066991984));
#93709=CARTESIAN_POINT('Ctrl Pts',(22.1528974355741,-10.5806803818037,0.292347047550849));
#93710=CARTESIAN_POINT('Ctrl Pts',(22.2212444823395,-10.0989252768157,-2.23060044547888));
#93711=CARTESIAN_POINT('Ctrl Pts',(0.423670339017024,11.5945440159359,-2.5274869736091));
#93712=CARTESIAN_POINT('Ctrl Pts',(0.499910026360594,12.1482059396284,0.288878858844674));
#93713=CARTESIAN_POINT('Ctrl Pts',(0.632109379329947,11.4845538919804,4.9846161952424));
#93714=CARTESIAN_POINT('Ctrl Pts',(0.817612579386571,7.11199402872522,10.0533146758472));
#93715=CARTESIAN_POINT('Ctrl Pts',(0.979985218407911,1.71424573113258,12.1825515349628));
#93716=CARTESIAN_POINT('Ctrl Pts',(1.14226800128799,-4.07414027681685,11.6205930393753));
#93717=CARTESIAN_POINT('Ctrl Pts',(1.30457476479594,-8.95288746042918,8.45215882401799));
#93718=CARTESIAN_POINT('Ctrl Pts',(1.46705658537464,-11.8369449681502,3.40204576066399));
#93719=CARTESIAN_POINT('Ctrl Pts',(1.62919612679919,-12.0795032442586,-2.41181865880537));
#93720=CARTESIAN_POINT('Ctrl Pts',(1.7922231908137,-9.62655368386558,-7.68820709553356));
#93721=CARTESIAN_POINT('Ctrl Pts',(1.95333642472349,-5.02430928732878,-11.2508211808369));
#93722=CARTESIAN_POINT('Ctrl Pts',(2.11870241151089,0.700466955544165,-12.3033343538523));
#93723=CARTESIAN_POINT('Ctrl Pts',(2.27520347918107,6.27024822871081,-10.6103749171108));
#93724=CARTESIAN_POINT('Ctrl Pts',(2.44986594459918,10.4419736262804,-6.54920361312032));
#93725=CARTESIAN_POINT('Ctrl Pts',(2.58707156317327,12.2839753927472,-1.02582701461511));
#93726=CARTESIAN_POINT('Ctrl Pts',(2.80947697362479,11.3852443672071,4.7283936720716));
#93727=CARTESIAN_POINT('Ctrl Pts',(3.02012261112198,7.94675209063415,9.42308149047911));
#93728=CARTESIAN_POINT('Ctrl Pts',(3.25695544175519,2.1558172122942,12.3161751177547));
#93729=CARTESIAN_POINT('Ctrl Pts',(3.51639564443165,-5.08337488329011,11.6384542804377));
#93730=CARTESIAN_POINT('Ctrl Pts',(3.79990696773698,-11.0053104607542,6.34331092371967));
#93731=CARTESIAN_POINT('Ctrl Pts',(4.08317996499983,-12.6136176870944,-1.42687314372758));
#93732=CARTESIAN_POINT('Ctrl Pts',(4.36652199501975,-9.30382142526618,-8.63724843788744));
#93733=CARTESIAN_POINT('Ctrl Pts',(4.64976733453564,-2.35439972201832,-12.4737105684233));
#93734=CARTESIAN_POINT('Ctrl Pts',(4.90150350992193,4.62977560927775,-11.5427208503617));
#93735=CARTESIAN_POINT('Ctrl Pts',(5.12171659361905,9.36028395486059,-7.8512031028979));
#93736=CARTESIAN_POINT('Ctrl Pts',(5.31043357641154,11.7590219812312,-3.31083020027306));
#93737=CARTESIAN_POINT('Ctrl Pts',(5.53055349196105,12.1365080578965,2.67659366125153));
#93738=CARTESIAN_POINT('Ctrl Pts',(5.78204065257121,8.96738060148916,8.96171723805314));
#93739=CARTESIAN_POINT('Ctrl Pts',(6.06484712251421,1.88946402405893,12.5292031204931));
#93740=CARTESIAN_POINT('Ctrl Pts',(6.34751963344422,-5.91395276198827,11.1983677940525));
#93741=CARTESIAN_POINT('Ctrl Pts',(6.63004974724334,-11.4027073465007,5.49642901003884));
#93742=CARTESIAN_POINT('Ctrl Pts',(6.91241907517974,-12.4304112089619,-2.34661336699943));
#93743=CARTESIAN_POINT('Ctrl Pts',(7.19461683901169,-8.60493455977115,-9.26183221523559));
#93744=CARTESIAN_POINT('Ctrl Pts',(7.47663110699745,-1.42059143694494,-12.5551778481077));
#93745=CARTESIAN_POINT('Ctrl Pts',(7.7271314516778,5.44207090065182,-11.1127539908751));
#93746=CARTESIAN_POINT('Ctrl Pts',(7.94618529937553,9.85975525065126,-7.10070001078025));
#93747=CARTESIAN_POINT('Ctrl Pts',(8.13384686792588,11.9037917265843,-2.41755821962657));
#93748=CARTESIAN_POINT('Ctrl Pts',(8.32140797882049,11.8356666147205,2.68798146599893));
#93749=CARTESIAN_POINT('Ctrl Pts',(8.52969267973505,9.44210865594734,7.83388635082118));
#93750=CARTESIAN_POINT('Ctrl Pts',(8.7170210774575,5.27991968869386,10.9296745279879));
#93751=CARTESIAN_POINT('Ctrl Pts',(8.90423692873056,0.357432150175136,12.0017609531342));
#93752=CARTESIAN_POINT('Ctrl Pts',(9.07056383278122,-4.12894815337104,11.3873305431638));
#93753=CARTESIAN_POINT('Ctrl Pts',(9.2575629576071,-8.43721289934054,8.67272832383416));
#93754=CARTESIAN_POINT('Ctrl Pts',(9.47558408444354,-11.7265578415237,3.7296686533837));
#93755=CARTESIAN_POINT('Ctrl Pts',(9.7245411344107,-12.1243895083082,-3.23133011071166));
#93756=CARTESIAN_POINT('Ctrl Pts',(9.95768828784286,-8.53865012954471,-8.69066976617957));
#93757=CARTESIAN_POINT('Ctrl Pts',(10.1440524905267,-4.15835460390148,-11.1513280757522));
#93758=CARTESIAN_POINT('Ctrl Pts',(10.3303115703698,0.768371413765467,-12.1431266911025));
#93759=CARTESIAN_POINT('Ctrl Pts',(10.5319176514054,6.1875553550476,-10.5772889499276));
#93760=CARTESIAN_POINT('Ctrl Pts',(10.7488175153498,10.2544916217239,-6.28999306444741));
#93761=CARTESIAN_POINT('Ctrl Pts',(10.9345802297141,11.9262575937623,-1.51572827249708));
#93762=CARTESIAN_POINT('Ctrl Pts',(11.0995661281895,11.5297510391498,2.95786818177737));
#93763=CARTESIAN_POINT('Ctrl Pts',(11.2850434916283,9.4072473885783,7.47527420050668));
#93764=CARTESIAN_POINT('Ctrl Pts',(11.4703614167965,5.50440093654708,10.8058306130731));
#93765=CARTESIAN_POINT('Ctrl Pts',(11.6760576098715,0.0223254280214599,
11.977008200122));
#93766=CARTESIAN_POINT('Ctrl Pts',(11.8610173200076,-4.90036432229749,10.9212226493378));
#93767=CARTESIAN_POINT('Ctrl Pts',(12.0458069090812,-8.94702876856218,7.93031395909145));
#93768=CARTESIAN_POINT('Ctrl Pts',(12.2611920470817,-11.8242343241244,2.81657705125164));
#93769=CARTESIAN_POINT('Ctrl Pts',(12.507054950679,-11.7014296258157,-4.06536850085611));
#93770=CARTESIAN_POINT('Ctrl Pts',(12.7832424374564,-6.98756758515652,-10.204238068239));
#93771=CARTESIAN_POINT('Ctrl Pts',(13.0590144035629,0.433956965789265,-12.3406476876779));
#93772=CARTESIAN_POINT('Ctrl Pts',(13.3343616190032,7.6655120483341,-9.65738889411834));
#93773=CARTESIAN_POINT('Ctrl Pts',(13.609272528718,11.8824312629553,-3.21343169127533));
#93774=CARTESIAN_POINT('Ctrl Pts',(13.8837411210347,11.4512344395676,4.46083420421942));
#93775=CARTESIAN_POINT('Ctrl Pts',(14.157756841466,6.55253517995481,10.37448148582));
#93776=CARTESIAN_POINT('Ctrl Pts',(14.4009162181298,-0.0562993866030424,
12.0056367310909));
#93777=CARTESIAN_POINT('Ctrl Pts',(14.613377610303,-5.60579188925755,10.3614149373415));
#93778=CARTESIAN_POINT('Ctrl Pts',(14.7952761706161,-9.36063725916999,7.13400533499643));
#93779=CARTESIAN_POINT('Ctrl Pts',(14.9769616528988,-11.4519683094566,2.64850567104104));
#93780=CARTESIAN_POINT('Ctrl Pts',(15.1584316174266,-11.5157281433124,-2.29202178385935));
#93781=CARTESIAN_POINT('Ctrl Pts',(15.3396841079563,-9.5415030993255,-6.81686991985697));
#93782=CARTESIAN_POINT('Ctrl Pts',(15.520716584191,-5.88761675003304,-10.1247386305629));
#93783=CARTESIAN_POINT('Ctrl Pts',(15.7015273430644,-1.19957735055218,-11.635944756842));
#93784=CARTESIAN_POINT('Ctrl Pts',(15.8821144770507,3.6847281306788,-11.0861297401642));
#93785=CARTESIAN_POINT('Ctrl Pts',(16.092535838484,8.61916674222325,-8.164317052411));
#93786=CARTESIAN_POINT('Ctrl Pts',(16.2876180879184,11.2605086022686,-3.38938545620713));
#93787=CARTESIAN_POINT('Ctrl Pts',(16.4674350022227,11.3878313110805,1.46147344387607));
#93788=CARTESIAN_POINT('Ctrl Pts',(16.6246226123464,10.1826987634612,5.523689705124));
#93789=CARTESIAN_POINT('Ctrl Pts',(16.8040468044215,7.06640964607396,9.32529450302247));
#93790=CARTESIAN_POINT('Ctrl Pts',(17.0056015586567,1.99352102361405,11.5113829717538));
#93791=CARTESIAN_POINT('Ctrl Pts',(17.2068563683828,-3.50277342848018,11.1248679174581));
#93792=CARTESIAN_POINT('Ctrl Pts',(17.4301372643576,-8.73849927430506,7.95059990444826));
#93793=CARTESIAN_POINT('Ctrl Pts',(17.6753124404026,-11.8291357002828,1.82452958899942));
#93794=CARTESIAN_POINT('Ctrl Pts',(17.9422312867441,-10.5857337571376,-5.55110411124777));
#93795=CARTESIAN_POINT('Ctrl Pts',(18.1864008297577,-5.65560812392042,-10.2891705783639));
#93796=CARTESIAN_POINT('Ctrl Pts',(18.4079732642625,0.283267861568415,-11.5526785802843));
#93797=CARTESIAN_POINT('Ctrl Pts',(18.6070659207362,5.54463515770339,-10.1205401749562));
#93798=CARTESIAN_POINT('Ctrl Pts',(18.8058667587473,9.55594572003318,-6.43558073229036));
#93799=CARTESIAN_POINT('Ctrl Pts',(19.004296009319,11.4253516620804,-1.33031017300727));
#93800=CARTESIAN_POINT('Ctrl Pts',(19.2025352896204,10.7442529016399,4.05527348946615));
#93801=CARTESIAN_POINT('Ctrl Pts',(19.4001836338508,7.6722717924416,8.52063310338956));
#93802=CARTESIAN_POINT('Ctrl Pts',(19.5980315539952,2.90113062562472,11.072540055233));
#93803=CARTESIAN_POINT('Ctrl Pts',(19.7946776467893,-2.5000090595846,11.1528230858435));
#93804=CARTESIAN_POINT('Ctrl Pts',(19.9924152586705,-7.32795514376305,8.74282571258241));
#93805=CARTESIAN_POINT('Ctrl Pts',(20.1868948262722,-10.506301854141,4.40543523386043));
#93806=CARTESIAN_POINT('Ctrl Pts',(20.3927492397039,-11.3350287821838,-0.920131778514912));
#93807=CARTESIAN_POINT('Ctrl Pts',(20.5192302799543,-9.63653174764009,-6.01425458044086));
#93808=CARTESIAN_POINT('Ctrl Pts',(20.6801053219349,-5.79329331148848,-9.75250286771838));
#93809=CARTESIAN_POINT('Ctrl Pts',(20.824073482086,-0.669397782210286,-11.3102133361092));
#93810=CARTESIAN_POINT('Ctrl Pts',(20.9760363808395,4.59117028503297,-10.341855027379));
#93811=CARTESIAN_POINT('Ctrl Pts',(21.1239075502339,8.81475307055138,-7.07151228909026));
#93812=CARTESIAN_POINT('Ctrl Pts',(21.2733782519326,11.0631196578749,-2.23372990206915));
#93813=CARTESIAN_POINT('Ctrl Pts',(21.4218610235557,10.8401809746124,3.09085572555693));
#93814=CARTESIAN_POINT('Ctrl Pts',(21.5705041401616,8.20139051869354,7.7097335231965));
#93815=CARTESIAN_POINT('Ctrl Pts',(21.7188009929258,3.74263352723652,10.6058633049019));
#93816=CARTESIAN_POINT('Ctrl Pts',(21.8669806048059,-1.54112766069498,11.1157326171366));
#93817=CARTESIAN_POINT('Ctrl Pts',(22.0149272318989,-6.46295628686545,9.17861775642755));
#93818=CARTESIAN_POINT('Ctrl Pts',(22.184149004847,-10.4455333151633,4.55128270428701));
#93819=CARTESIAN_POINT('Ctrl Pts',(22.303825740982,-11.0480802116222,0.300873741754191));
#93820=CARTESIAN_POINT('Ctrl Pts',(22.374548238521,-10.5449815461394,-2.31029863300481));
#93821=CARTESIAN_POINT('Ctrl Pts',(0.000900289619140335,11.3804638834915,
-2.47613834775811));
#93822=CARTESIAN_POINT('Ctrl Pts',(0.0760295925109289,11.9237491928521,
0.298886540614988));
#93823=CARTESIAN_POINT('Ctrl Pts',(0.205681996899962,11.2728196273968,4.90414136366958));
#93824=CARTESIAN_POINT('Ctrl Pts',(0.38794973553318,6.97799472302775,9.88526793682913));
#93825=CARTESIAN_POINT('Ctrl Pts',(0.547505005240074,1.67325159616518,11.9771828269468));
#93826=CARTESIAN_POINT('Ctrl Pts',(0.707085602513105,-4.01842843579301,
11.4254349394003));
#93827=CARTESIAN_POINT('Ctrl Pts',(0.866758979071408,-8.81835900038039,
8.30837071392562));
#93828=CARTESIAN_POINT('Ctrl Pts',(1.02669281100368,-11.6574299498413,3.33779701847597));
#93829=CARTESIAN_POINT('Ctrl Pts',(1.1863696529269,-11.8966938796723,-2.38782040177236));
#93830=CARTESIAN_POINT('Ctrl Pts',(1.34700769853469,-9.48000818153135,-7.58698885918058));
#93831=CARTESIAN_POINT('Ctrl Pts',(1.50583823722894,-4.94319286098826,-11.0993660324489));
#93832=CARTESIAN_POINT('Ctrl Pts',(1.66895327102401,0.703563529205378,-12.1380990070998));
#93833=CARTESIAN_POINT('Ctrl Pts',(1.82340078503438,6.20026236479091,-10.4672689721285));
#93834=CARTESIAN_POINT('Ctrl Pts',(1.99586293482947,10.3199138911453,-6.45818496655306));
#93835=CARTESIAN_POINT('Ctrl Pts',(2.13140208596345,12.1396560511668,-1.0012609065115));
#93836=CARTESIAN_POINT('Ctrl Pts',(2.35147265048197,11.2517822360554,4.69337676657042));
#93837=CARTESIAN_POINT('Ctrl Pts',(2.55971574243581,7.85115399103111,9.33401839064537));
#93838=CARTESIAN_POINT('Ctrl Pts',(2.79422737759169,2.11861543132166,12.2002863161899));
#93839=CARTESIAN_POINT('Ctrl Pts',(3.0512206555009,-5.0531972452128,11.5288550107248));
#93840=CARTESIAN_POINT('Ctrl Pts',(3.33238525234115,-10.9266143368972,6.27934698525193));
#93841=CARTESIAN_POINT('Ctrl Pts',(3.6135516195531,-12.5241293849237,-1.43321866908381));
#93842=CARTESIAN_POINT('Ctrl Pts',(3.895065976677,-9.23684114979357,-8.59733339719354));
#93843=CARTESIAN_POINT('Ctrl Pts',(4.17674612036772,-2.3263774897798,-12.4137395464659));
#93844=CARTESIAN_POINT('Ctrl Pts',(4.42733432200923,4.62604823359843,-11.4880055956006));
#93845=CARTESIAN_POINT('Ctrl Pts',(4.64671446045608,9.33895743109829,-7.81077468702255));
#93846=CARTESIAN_POINT('Ctrl Pts',(4.83483829661682,11.7304278021032,-3.28483832386075));
#93847=CARTESIAN_POINT('Ctrl Pts',(5.05440724020435,12.1074033960408,2.68751675904296));
#93848=CARTESIAN_POINT('Ctrl Pts',(5.30546640657026,8.94463140752224,8.96236282495723));
#93849=CARTESIAN_POINT('Ctrl Pts',(5.58806199031735,1.87258526440905,12.528277867321));
#93850=CARTESIAN_POINT('Ctrl Pts',(5.87079511955371,-5.93268261644051,11.1983565302455));
#93851=CARTESIAN_POINT('Ctrl Pts',(6.15365719351318,-11.428734123529,5.49059286230551));
#93852=CARTESIAN_POINT('Ctrl Pts',(6.43662965392189,-12.4598385816407,-2.36901622871161));
#93853=CARTESIAN_POINT('Ctrl Pts',(6.71970157861287,-8.62358728920016,-9.3061984871583));
#93854=CARTESIAN_POINT('Ctrl Pts',(7.00286024125015,-1.41063629995952,-12.6140167198692));
#93855=CARTESIAN_POINT('Ctrl Pts',(7.25461839642261,5.48668947887283,-11.1653717969649));
#93856=CARTESIAN_POINT('Ctrl Pts',(7.47494586003375,9.93035099743477,-7.13029121147144));
#93857=CARTESIAN_POINT('Ctrl Pts',(7.66381885286863,11.9878796392882,-2.41707720971809));
#93858=CARTESIAN_POINT('Ctrl Pts',(7.85271039473043,11.9196078305902,2.72466571552369));
#93859=CARTESIAN_POINT('Ctrl Pts',(8.06260425041251,9.50793750751671,7.91045632829471));
#93860=CARTESIAN_POINT('Ctrl Pts',(8.25151943811564,5.31086519215702,11.0329345940469));
#93861=CARTESIAN_POINT('Ctrl Pts',(8.4404389964955,0.343601266253404,12.1149463652386));
#93862=CARTESIAN_POINT('Ctrl Pts',(8.60836913040726,-4.18601440528256,11.4948946391602));
#93863=CARTESIAN_POINT('Ctrl Pts',(8.79728667337804,-8.53866643130548,8.75273207656539));
#93864=CARTESIAN_POINT('Ctrl Pts',(9.01768164738511,-11.8641266373615,3.75611609832303));
#93865=CARTESIAN_POINT('Ctrl Pts',(9.26954822543693,-12.2676543833531,-3.28608472892146));
#93866=CARTESIAN_POINT('Ctrl Pts',(9.50563786526714,-8.63747604798216,-8.81485613790273));
#93867=CARTESIAN_POINT('Ctrl Pts',(9.69448333045407,-4.19892530952498,-11.3084481812179));
#93868=CARTESIAN_POINT('Ctrl Pts',(9.88330841704327,0.795573210174991,-12.31409890475));
#93869=CARTESIAN_POINT('Ctrl Pts',(10.0878363483475,6.29348062935308,-10.7263386495003));
#93870=CARTESIAN_POINT('Ctrl Pts',(10.3080425852288,10.4227066096295,-6.373952123734));
#93871=CARTESIAN_POINT('Ctrl Pts',(10.4967508502962,12.1212890942399,-1.5241070887372));
#93872=CARTESIAN_POINT('Ctrl Pts',(10.6644551092141,11.7185241015762,3.02321116376383));
#93873=CARTESIAN_POINT('Ctrl Pts',(10.8530809920984,9.56015331219004,7.61733162462507));
#93874=CARTESIAN_POINT('Ctrl Pts',(11.0416565818448,5.58907527410401,11.0068489757527));
#93875=CARTESIAN_POINT('Ctrl Pts',(11.2511145551901,0.00682605008962356,
12.1998226540138));
#93876=CARTESIAN_POINT('Ctrl Pts',(11.4395654059283,-5.008825606421,11.1244108695771));
#93877=CARTESIAN_POINT('Ctrl Pts',(11.6279548005678,-9.13449427634377,8.07551137181917));
#93878=CARTESIAN_POINT('Ctrl Pts',(11.8476610895102,-12.0697351676139,2.85940599125345));
#93879=CARTESIAN_POINT('Ctrl Pts',(12.0986399649365,-11.9453291153835,-4.1656754855368));
#93880=CARTESIAN_POINT('Ctrl Pts',(12.380813347536,-7.1301861622191,-10.4382358096941));
#93881=CARTESIAN_POINT('Ctrl Pts',(12.6628007775777,0.458280864595954,-12.6238052602907));
#93882=CARTESIAN_POINT('Ctrl Pts',(12.9445891529439,7.85932826240679,-9.87877525418112));
#93883=CARTESIAN_POINT('Ctrl Pts',(13.2261623670661,12.1792965341059,-3.27924005831069));
#93884=CARTESIAN_POINT('Ctrl Pts',(13.5075123240597,11.7382981773641,4.58743988341015));
#93885=CARTESIAN_POINT('Ctrl Pts',(13.78862270095,6.7135683306726,10.6548364892803));
#93886=CARTESIAN_POINT('Ctrl Pts',(14.0382770210205,-0.0715674345651694,
12.3303771601699));
#93887=CARTESIAN_POINT('Ctrl Pts',(14.2565522948072,-5.77303535786754,10.6414830835723));
#93888=CARTESIAN_POINT('Ctrl Pts',(14.4435258860147,-9.63278931728537,7.3242445945618));
#93889=CARTESIAN_POINT('Ctrl Pts',(14.6303754923499,-11.7838090680834,2.71138944009352));
#93890=CARTESIAN_POINT('Ctrl Pts',(14.8170958795502,-11.8496754051594,-2.37206455387923));
#93891=CARTESIAN_POINT('Ctrl Pts',(15.0036871297529,-9.81756163638772,-7.03027663503322));
#93892=CARTESIAN_POINT('Ctrl Pts',(15.1901423954911,-6.05440883736194,-10.4374095339218));
#93893=CARTESIAN_POINT('Ctrl Pts',(15.3764600570967,-1.22369089789884,-11.9948963860826));
#93894=CARTESIAN_POINT('Ctrl Pts',(15.562635366768,3.81176920962088,-11.4283094282349));
#93895=CARTESIAN_POINT('Ctrl Pts',(15.7796703137958,8.90143044882656,-8.41495584271175));
#93896=CARTESIAN_POINT('Ctrl Pts',(15.981004715721,11.6279173541602,-3.4873266676171));
#93897=CARTESIAN_POINT('Ctrl Pts',(16.1666763388528,11.7595350467105,1.52149245812212));
#93898=CARTESIAN_POINT('Ctrl Pts',(16.3290372382266,10.5148554672375,5.71740896283513));
#93899=CARTESIAN_POINT('Ctrl Pts',(16.5144448880648,7.29489788686152,9.64596057464015));
#93900=CARTESIAN_POINT('Ctrl Pts',(16.7228234986026,2.05041108784682,11.9063669249619));
#93901=CARTESIAN_POINT('Ctrl Pts',(16.930992551001,-3.63471752235437,11.5068909821674));
#93902=CARTESIAN_POINT('Ctrl Pts',(17.1620546044951,-9.05305178321521,8.22235330647674));
#93903=CARTESIAN_POINT('Ctrl Pts',(17.4159113519357,-12.2537284610614,1.87968497770613));
#93904=CARTESIAN_POINT('Ctrl Pts',(17.6924475759089,-10.9662624459213,-5.76178740457814));
#93905=CARTESIAN_POINT('Ctrl Pts',(17.945566339639,-5.85591523772921,-10.6739734171909));
#93906=CARTESIAN_POINT('Ctrl Pts',(18.1753717303344,0.303573719096216,-11.9847397656707));
#93907=CARTESIAN_POINT('Ctrl Pts',(18.3819490799225,5.76277859895906,-10.4990413623162));
#93908=CARTESIAN_POINT('Ctrl Pts',(18.5883070393005,9.92675289335987,-6.67420313817307));
#93909=CARTESIAN_POINT('Ctrl Pts',(18.7943617430537,11.8682318114508,-1.37288219672597));
#93910=CARTESIAN_POINT('Ctrl Pts',(19.0002970711139,11.1609539414397,4.22186752150935));
#93911=CARTESIAN_POINT('Ctrl Pts',(19.2056993787138,7.96869361929753,8.86238310851352));
#93912=CARTESIAN_POINT('Ctrl Pts',(19.4113749853726,3.00880991732028,11.5157353993555));
#93913=CARTESIAN_POINT('Ctrl Pts',(19.6158941321298,-2.60825633138589,11.5990543182677));
#93914=CARTESIAN_POINT('Ctrl Pts',(19.8215745264496,-7.63078703075867,9.09294033135363));
#93915=CARTESIAN_POINT('Ctrl Pts',(20.0240196534198,-10.9387245165996,4.57767395040845));
#93916=CARTESIAN_POINT('Ctrl Pts',(20.2382196602506,-11.8016588555741,-0.963371624759982));
#93917=CARTESIAN_POINT('Ctrl Pts',(20.3699279122194,-10.0330275954534,-6.2677802445981));
#93918=CARTESIAN_POINT('Ctrl Pts',(20.5374857980306,-6.03037781526117,-10.1616546059296));
#93919=CARTESIAN_POINT('Ctrl Pts',(20.6874666540089,-0.692498617449417,
-11.7843870861828));
#93920=CARTESIAN_POINT('Ctrl Pts',(20.8458089263913,4.78891142674402,-10.7755909958413));
#93921=CARTESIAN_POINT('Ctrl Pts',(20.9999220312606,9.19085121893355,-7.36733395392426));
#93922=CARTESIAN_POINT('Ctrl Pts',(21.1557315978258,11.5346665649489,-2.32438533941469));
#93923=CARTESIAN_POINT('Ctrl Pts',(21.3105437060683,11.302391404217,3.22695219679456));
#93924=CARTESIAN_POINT('Ctrl Pts',(21.4655482862605,8.55068275589101,8.04392519302322));
#93925=CARTESIAN_POINT('Ctrl Pts',(21.6202312153138,3.9003498130575,11.063996769607));
#93926=CARTESIAN_POINT('Ctrl Pts',(21.7747884398775,-1.61158669978775,11.5971907852724));
#93927=CARTESIAN_POINT('Ctrl Pts',(21.9292048348329,-6.74680889827636,9.57370973440197));
#93928=CARTESIAN_POINT('Ctrl Pts',(22.1056736106782,-10.9027234868844,4.74979039067917));
#93929=CARTESIAN_POINT('Ctrl Pts',(22.2308646891255,-11.5318780889901,0.303165289390478));
#93930=CARTESIAN_POINT('Ctrl Pts',(22.304029593088,-11.0066085895293,-2.39878637653492));
#93931=CARTESIAN_POINT('Ctrl Pts',(-0.274269641050573,11.0004695673906,
-2.39761094709083));
#93932=CARTESIAN_POINT('Ctrl Pts',(-0.201135280450074,11.5254245847803,
0.303191618745211));
#93933=CARTESIAN_POINT('Ctrl Pts',(-0.076018233199116,10.8966599438403,
4.74719998282454));
#93934=CARTESIAN_POINT('Ctrl Pts',(0.100354336277068,6.74303500522591,9.56853913405492));
#93935=CARTESIAN_POINT('Ctrl Pts',(0.254685225272068,1.61062313657491,11.5908849925943));
#93936=CARTESIAN_POINT('Ctrl Pts',(0.409158220632143,-3.89832589267103,
11.0580000084071));
#93937=CARTESIAN_POINT('Ctrl Pts',(0.563757230594105,-8.54615907764945,
8.0395458607866));
#93938=CARTESIAN_POINT('Ctrl Pts',(0.718678293364365,-11.2964009987587,
3.22515286261878));
#93939=CARTESIAN_POINT('Ctrl Pts',(0.87340785468557,-11.5285575146058,-2.3232498873316));
#93940=CARTESIAN_POINT('Ctrl Pts',(1.02913439746881,-9.18597776810957,-7.363536753465));
#93941=CARTESIAN_POINT('Ctrl Pts',(1.18316711498639,-4.78633731515139,-10.7700426512527));
#93942=CARTESIAN_POINT('Ctrl Pts',(1.3414248089356,0.692236946541352,-11.7782646755505));
#93943=CARTESIAN_POINT('Ctrl Pts',(1.49133112294563,6.02737678504246,-10.1564808574998));
#93944=CARTESIAN_POINT('Ctrl Pts',(1.65879364084819,10.0279923142955,-6.26431175924732));
#93945=CARTESIAN_POINT('Ctrl Pts',(1.79044918943787,11.7957247916513,-0.963149160289205));
#93946=CARTESIAN_POINT('Ctrl Pts',(2.00450680071523,10.9332197456105,4.5765641208312));
#93947=CARTESIAN_POINT('Ctrl Pts',(2.20691084524558,7.62686256520766,9.0867291314954));
#93948=CARTESIAN_POINT('Ctrl Pts',(2.4351468519884,2.04896770526915,11.8775245776043));
#93949=CARTESIAN_POINT('Ctrl Pts',(2.68534078308583,-4.93385442790983,11.2237829300574));
#93950=CARTESIAN_POINT('Ctrl Pts',(2.95932835724008,-10.6578654904289,6.1096651465346));
#93951=CARTESIAN_POINT('Ctrl Pts',(3.23352058266583,-12.2167042661632,-1.41175057439282));
#93952=CARTESIAN_POINT('Ctrl Pts',(3.50827847232005,-9.00925924299354,-8.40424538776617));
#93953=CARTESIAN_POINT('Ctrl Pts',(3.78342130461475,-2.25959033454623,-12.1330610356035));
#93954=CARTESIAN_POINT('Ctrl Pts',(4.02839617829052,4.53728952345717,-11.228935417426));
#93955=CARTESIAN_POINT('Ctrl Pts',(4.24301582882195,9.14819504519508,-7.63175549721547));
#93956=CARTESIAN_POINT('Ctrl Pts',(4.42716125447877,11.489350822963,-3.20165828960071));
#93957=CARTESIAN_POINT('Ctrl Pts',(4.64220730361779,11.8589357929702,2.64765770593709));
#93958=CARTESIAN_POINT('Ctrl Pts',(4.88827003082658,8.75992235184213,8.79806219469721));
#93959=CARTESIAN_POINT('Ctrl Pts',(5.16548273281936,1.82302921333241,12.2970640865527));
#93960=CARTESIAN_POINT('Ctrl Pts',(5.44307400835471,-5.84053666929798,10.9923890055324));
#93961=CARTESIAN_POINT('Ctrl Pts',(5.72103722792618,-11.2422406693477,5.38420624340654));
#93962=CARTESIAN_POINT('Ctrl Pts',(5.99935768984567,-12.25751466873,-2.3461082746222));
#93963=CARTESIAN_POINT('Ctrl Pts',(6.27802614604401,-8.48189613373607,-9.17597296653521));
#93964=CARTESIAN_POINT('Ctrl Pts',(6.5570329715071,-1.37513713028755,-12.4363664797683));
#93965=CARTESIAN_POINT('Ctrl Pts',(6.80532498827725,5.42752948217785,-11.0086321842624));
#93966=CARTESIAN_POINT('Ctrl Pts',(7.0227875379952,9.8137364793638,-7.02627359380098));
#93967=CARTESIAN_POINT('Ctrl Pts',(7.20931847710744,11.8460716008633,-2.37160812629482));
#93968=CARTESIAN_POINT('Ctrl Pts',(7.39598279382656,11.7789295620232,2.70955515259177));
#93969=CARTESIAN_POINT('Ctrl Pts',(7.6035319327092,9.39456410752855,7.83758421962789));
#93970=CARTESIAN_POINT('Ctrl Pts',(7.79047118958947,5.24170674678976,10.9278934529097));
#93971=CARTESIAN_POINT('Ctrl Pts',(7.97753301867008,0.323277611298938,11.9994386003805));
#93972=CARTESIAN_POINT('Ctrl Pts',(8.14389525793364,-4.16411557432759,11.3854632941077));
#93973=CARTESIAN_POINT('Ctrl Pts',(8.33117028318344,-8.47913095199905,8.66739933230884));
#93974=CARTESIAN_POINT('Ctrl Pts',(8.5497868133909,-11.7780926744232,3.71133890204296));
#93975=CARTESIAN_POINT('Ctrl Pts',(8.79981268641912,-12.1797020209906,-3.27938720685819));
#93976=CARTESIAN_POINT('Ctrl Pts',(9.03440097162593,-8.57341027780405,-8.77362867592834));
#93977=CARTESIAN_POINT('Ctrl Pts',(9.22218188156679,-4.15989549397587,-11.2533688331925));
#93978=CARTESIAN_POINT('Ctrl Pts',(9.41003302249585,0.808765494160608,-12.2540291038378));
#93979=CARTESIAN_POINT('Ctrl Pts',(9.61364471581217,6.2823757029123,-10.6741610615063));
#93980=CARTESIAN_POINT('Ctrl Pts',(9.83304623986146,10.3968674534573,-6.33793941805998));
#93981=CARTESIAN_POINT('Ctrl Pts',(10.0211848030554,12.0906486399765,-1.50282609668041));
#93982=CARTESIAN_POINT('Ctrl Pts',(10.1884870588186,11.6891499040377,3.03367054210446));
#93983=CARTESIAN_POINT('Ctrl Pts',(10.3767631363507,9.53493716486031,7.61934830129794));
#93984=CARTESIAN_POINT('Ctrl Pts',(10.5651100391956,5.56904507615985,11.0052203614278));
#93985=CARTESIAN_POINT('Ctrl Pts',(10.7744673930001,-0.0105150758165145,
12.1980348159159));
#93986=CARTESIAN_POINT('Ctrl Pts',(10.9629516928778,-5.02713480755923,11.1227644880695));
#93987=CARTESIAN_POINT('Ctrl Pts',(11.1514917238607,-9.15634821021125,8.07165786784285));
#93988=CARTESIAN_POINT('Ctrl Pts',(11.3715173352852,-12.0962213591835,2.84818528749816));
#93989=CARTESIAN_POINT('Ctrl Pts',(11.62305833115,-11.9725739258084,-4.19269902494711));
#93990=CARTESIAN_POINT('Ctrl Pts',(11.9061372568435,-7.14292658277634,-10.4861879255579));
#93991=CARTESIAN_POINT('Ctrl Pts',(12.1892998809645,0.476910464515135,-12.6820398490254));
#93992=CARTESIAN_POINT('Ctrl Pts',(12.4725334331891,7.91638967099688,-9.92404980923661));
#93993=CARTESIAN_POINT('Ctrl Pts',(12.7558205103974,12.2636994513997,-3.28495237398259));
#93994=CARTESIAN_POINT('Ctrl Pts',(13.0391515836362,11.8207969469138,4.63725930776699));
#93995=CARTESIAN_POINT('Ctrl Pts',(13.3225108438936,6.75677175138148,10.7540029972883));
#93996=CARTESIAN_POINT('Ctrl Pts',(13.5743965363279,-0.0888694770886342,
12.4455753705037));
#93997=CARTESIAN_POINT('Ctrl Pts',(13.7948007691669,-5.84611408574753,10.7405846022518));
#93998=CARTESIAN_POINT('Ctrl Pts',(13.9837133047971,-9.74613607726721,7.38918223972257));
#93999=CARTESIAN_POINT('Ctrl Pts',(14.1726181730569,-11.9211450660727,2.72569989767666));
#94000=CARTESIAN_POINT('Ctrl Pts',(14.3615117518733,-11.988121384906,-2.41692924665857));
#94001=CARTESIAN_POINT('Ctrl Pts',(14.5503884862477,-9.93140392485721,-7.13237619420355));
#94002=CARTESIAN_POINT('Ctrl Pts',(14.7392452066992,-6.11998765128524,-10.5836631714223));
#94003=CARTESIAN_POINT('Ctrl Pts',(14.9280778158491,-1.22412417528949,-12.1624991437306));
#94004=CARTESIAN_POINT('Ctrl Pts',(15.1168834927693,3.88253460149443,-11.5882300272317));
#94005=CARTESIAN_POINT('Ctrl Pts',(15.3371190205423,9.04745529657373,-8.53078661826523));
#94006=CARTESIAN_POINT('Ctrl Pts',(15.5415710603206,11.8168749142472,-3.52716602342221));
#94007=CARTESIAN_POINT('Ctrl Pts',(15.7302511825858,11.950835437091,1.56286779537959));
#94008=CARTESIAN_POINT('Ctrl Pts',(15.8953162505218,10.6855628547944,5.82871724506087));
#94009=CARTESIAN_POINT('Ctrl Pts',(16.0839158470169,7.41047732554085,9.8251853488451));
#94010=CARTESIAN_POINT('Ctrl Pts',(16.2960238194692,2.07226966928086,12.1265039457095));
#94011=CARTESIAN_POINT('Ctrl Pts',(16.5080591542134,-3.71851480918685,11.7200354231081));
#94012=CARTESIAN_POINT('Ctrl Pts',(16.7435666491117,-9.24138915696723,8.37276765492118));
#94013=CARTESIAN_POINT('Ctrl Pts',(17.0025061938178,-12.5070246239786,1.90348792745417));
#94014=CARTESIAN_POINT('Ctrl Pts',(17.2848235291397,-11.1937440869041,-5.89791089480221));
#94015=CARTESIAN_POINT('Ctrl Pts',(17.5434502580148,-5.9727692152997,-10.917765370183));
#94016=CARTESIAN_POINT('Ctrl Pts',(17.7784330357828,0.325439291644578,-12.2585604897127));
#94017=CARTESIAN_POINT('Ctrl Pts',(17.9897960153653,5.91125375060957,-10.7388470513632));
#94018=CARTESIAN_POINT('Ctrl Pts',(18.2010656267775,10.1746651964443,-6.82324727932377));
#94019=CARTESIAN_POINT('Ctrl Pts',(18.4121556179949,12.1639803531377,-1.39254738980368));
#94020=CARTESIAN_POINT('Ctrl Pts',(18.623249012421,11.439407044246,4.34255520019844));
#94021=CARTESIAN_POINT('Ctrl Pts',(18.833930169963,8.16546807026437,9.10231198480979));
#94022=CARTESIAN_POINT('Ctrl Pts',(19.0450003933591,3.07545188059067,11.8261473540039));
#94023=CARTESIAN_POINT('Ctrl Pts',(19.2550466668237,-2.69287874609835,11.911356465016));
#94024=CARTESIAN_POINT('Ctrl Pts',(19.4663250727336,-7.85339118005448,9.33825389834762));
#94025=CARTESIAN_POINT('Ctrl Pts',(19.674563394974,-11.2548968968117,4.6933339960141));
#94026=CARTESIAN_POINT('Ctrl Pts',(19.8947281535767,-12.1430001285698,-1.00131534254292));
#94027=CARTESIAN_POINT('Ctrl Pts',(20.0302869032443,-10.3227462744336,-6.46036505053996));
#94028=CARTESIAN_POINT('Ctrl Pts',(20.2028081276818,-6.20191802184683,-10.470307721667));
#94029=CARTESIAN_POINT('Ctrl Pts',(20.3572959081572,-0.703609801586646,
-12.1417469327381));
#94030=CARTESIAN_POINT('Ctrl Pts',(20.5204610212607,4.94483734805194,-11.1026481640325));
#94031=CARTESIAN_POINT('Ctrl Pts',(20.6793382723823,9.48304514425589,-7.58922197930745));
#94032=CARTESIAN_POINT('Ctrl Pts',(20.8400261065306,11.9004900835925,-2.38841591491118));
#94033=CARTESIAN_POINT('Ctrl Pts',(20.9997527597285,11.6611545549498,3.33902598665685));
#94034=CARTESIAN_POINT('Ctrl Pts',(21.1597380220168,8.82116047529457,8.31122758162113));
#94035=CARTESIAN_POINT('Ctrl Pts',(21.3194635002342,4.01963780285365,11.4293273846779));
#94036=CARTESIAN_POINT('Ctrl Pts',(21.4790975980088,-1.67397197125274,11.9812737524744));
#94037=CARTESIAN_POINT('Ctrl Pts',(21.6387068761042,-6.98053832771844,9.88862498096864));
#94038=CARTESIAN_POINT('Ctrl Pts',(21.8210381178984,-11.2768707271801,4.90577138996948));
#94039=CARTESIAN_POINT('Ctrl Pts',(21.950736446027,-11.9279866435774,0.298808494733318));
#94040=CARTESIAN_POINT('Ctrl Pts',(22.0258906953141,-11.3845340025562,-2.4770968460111));
#94041=CARTESIAN_POINT('Ctrl Pts',(-0.342078111258781,10.5385239376104,
-2.30907696986698));
#94042=CARTESIAN_POINT('Ctrl Pts',(-0.271391112954986,11.0413243101621,
0.300787646455928));
#94043=CARTESIAN_POINT('Ctrl Pts',(-0.151790900733858,10.4391275085012,
4.54845706796136));
#94044=CARTESIAN_POINT('Ctrl Pts',(0.0173289685761135,6.45898872181764,
9.17301359026322));
#94045=CARTESIAN_POINT('Ctrl Pts',(0.165184575802352,1.54017202925644,11.1089082992411));
#94046=CARTESIAN_POINT('Ctrl Pts',(0.313274054906384,-3.74035295571867,
10.5993670185937));
#94047=CARTESIAN_POINT('Ctrl Pts',(0.461480450893154,-8.19638378875494,
7.70499910147591));
#94048=CARTESIAN_POINT('Ctrl Pts',(0.610033066368199,-10.8335607401376,
3.08895036516842));
#94049=CARTESIAN_POINT('Ctrl Pts',(0.758425688373396,-11.0563640988628,
-2.23239233265665));
#94050=CARTESIAN_POINT('Ctrl Pts',(0.907805392951706,-8.80936728323739,
-7.06721474411051));
#94051=CARTESIAN_POINT('Ctrl Pts',(1.05558749393355,-4.5883542812499,-10.3355905940881));
#94052=CARTESIAN_POINT('Ctrl Pts',(1.20745702701853,0.669020108857811,-11.3033060660648));
#94053=CARTESIAN_POINT('Ctrl Pts',(1.35134080974254,5.789809206371,-9.74664754437023));
#94054=CARTESIAN_POINT('Ctrl Pts',(1.51211172233338,9.63072280992876,-6.01039119164893));
#94055=CARTESIAN_POINT('Ctrl Pts',(1.63852912473268,11.3281842217455,-0.919880530777273));
#94056=CARTESIAN_POINT('Ctrl Pts',(1.84422696532119,10.4999572635067,4.40380525519473));
#94057=CARTESIAN_POINT('Ctrl Pts',(2.03864904197804,7.32344207081827,8.73590098616535));
#94058=CARTESIAN_POINT('Ctrl Pts',(2.25804528095925,1.96228541100584,11.4192375806519));
#94059=CARTESIAN_POINT('Ctrl Pts',(2.49859694289973,-4.75177863315334,10.7907046256551));
#94060=CARTESIAN_POINT('Ctrl Pts',(2.76217572136555,-10.2585538162154,5.87169453114436));
#94061=CARTESIAN_POINT('Ctrl Pts',(3.02606783573862,-11.7594204097944,-1.36721213881776));
#94062=CARTESIAN_POINT('Ctrl Pts',(3.2906456441965,-8.67140560944054,-8.10074009311899));
#94063=CARTESIAN_POINT('Ctrl Pts',(3.55573137608955,-2.16878112255051,-11.6938502007532));
#94064=CARTESIAN_POINT('Ctrl Pts',(3.79188453176902,4.38335528919225,-10.8228371958529));
#94065=CARTESIAN_POINT('Ctrl Pts',(3.9988685297872,8.83037624726696,-7.35382587376631));
#94066=CARTESIAN_POINT('Ctrl Pts',(4.17653174548993,11.0892681298178,-3.07977873822734));
#94067=CARTESIAN_POINT('Ctrl Pts',(4.38408991959369,11.4462359752871,2.56580322371247));
#94068=CARTESIAN_POINT('Ctrl Pts',(4.62170526191261,8.45420647422841,8.50527953784366));
#94069=CARTESIAN_POINT('Ctrl Pts',(4.88956462289703,1.75175609268675,11.8868850409351));
#94070=CARTESIAN_POINT('Ctrl Pts',(5.1579605953482,-5.65803149243908,10.6261941333783));
#94071=CARTESIAN_POINT('Ctrl Pts',(5.426889583736,-10.8847053678964,5.20087057403979));
#94072=CARTESIAN_POINT('Ctrl Pts',(5.6963440916033,-11.8684406358239,-2.28303986368077));
#94073=CARTESIAN_POINT('Ctrl Pts',(5.96631928763454,-8.21135175237803,-8.90018015900593));
#94074=CARTESIAN_POINT('Ctrl Pts',(6.23680942051052,-1.3219346212245,-12.0618160834734));
#94075=CARTESIAN_POINT('Ctrl Pts',(6.47769576851895,5.27793256781067,-10.677406515464));
#94076=CARTESIAN_POINT('Ctrl Pts',(6.68879639076236,9.53602370145207,-6.81177563294094));
#94077=CARTESIAN_POINT('Ctrl Pts',(6.86996019641698,11.5100899515073,-2.29118021789925));
#94078=CARTESIAN_POINT('Ctrl Pts',(7.05134297697175,11.4451001779805,2.64619255534257));
#94079=CARTESIAN_POINT('Ctrl Pts',(7.25311916862402,9.12734611943007,7.6316750467065));
#94080=CARTESIAN_POINT('Ctrl Pts',(7.43496751499411,5.08789384860659,10.6381766966852));
#94081=CARTESIAN_POINT('Ctrl Pts',(7.61702685389441,0.301013202030219,11.6811996322699));
#94082=CARTESIAN_POINT('Ctrl Pts',(7.77901346572604,-4.06831574126187,11.0836178899377));
#94083=CARTESIAN_POINT('Ctrl Pts',(7.96145422098787,-8.27209638982045,8.43595842149749));
#94084=CARTESIAN_POINT('Ctrl Pts',(8.1745399784263,-11.4878311447154,3.60551009010721));
#94085=CARTESIAN_POINT('Ctrl Pts',(8.41840722616007,-11.8804344880585,-3.21286435233645));
#94086=CARTESIAN_POINT('Ctrl Pts',(8.64740235484385,-8.36083904060513,-8.57653734389561));
#94087=CARTESIAN_POINT('Ctrl Pts',(8.8308165934691,-4.05002414261445,-10.9987567640481));
#94088=CARTESIAN_POINT('Ctrl Pts',(9.01437446933271,0.804983153667267,-11.9767120191619));
#94089=CARTESIAN_POINT('Ctrl Pts',(9.21346374406834,6.15713977460773,-10.432629123365));
#94090=CARTESIAN_POINT('Ctrl Pts',(9.42813593686045,10.1831972076906,-6.19012228467193));
#94091=CARTESIAN_POINT('Ctrl Pts',(9.61232353302086,11.8416906339914,-1.45667444959611));
#94092=CARTESIAN_POINT('Ctrl Pts',(9.7762080275955,11.4486469482307,2.98714889568544));
#94093=CARTESIAN_POINT('Ctrl Pts',(9.96072433801779,9.33761180924535,7.48126572599483));
#94094=CARTESIAN_POINT('Ctrl Pts',(10.1454158537006,5.44905605214366,10.8018176189898));
#94095=CARTESIAN_POINT('Ctrl Pts',(10.3508522783911,-0.0259045708147128,
11.9726580271132));
#94096=CARTESIAN_POINT('Ctrl Pts',(10.535911563002,-4.95140312035918,10.9172233439656));
#94097=CARTESIAN_POINT('Ctrl Pts',(10.7211379748348,-9.00820528356076,7.92003054877835));
#94098=CARTESIAN_POINT('Ctrl Pts',(10.9374220425718,-11.8983876651759,2.78562722922065));
#94099=CARTESIAN_POINT('Ctrl Pts',(11.1848729346765,-11.7777413136033,-4.14068320944885));
#94100=CARTESIAN_POINT('Ctrl Pts',(11.4635980779861,-7.02331972060775,-10.338030997822));
#94101=CARTESIAN_POINT('Ctrl Pts',(11.74265928929,0.485771185227506,-12.5031515715995));
#94102=CARTESIAN_POINT('Ctrl Pts',(12.0220452423349,7.82452146813134,-9.78373091459582));
#94103=CARTESIAN_POINT('Ctrl Pts',(12.3017414264954,12.1176670139685,-3.22947077724254));
#94104=CARTESIAN_POINT('Ctrl Pts',(12.5817404915373,11.6811207583279,4.59955148712552));
#94105=CARTESIAN_POINT('Ctrl Pts',(12.8620270450134,6.67296756288785,10.6506950365554));
#94106=CARTESIAN_POINT('Ctrl Pts',(13.1114181050387,-0.10457717046341,12.3264734729167));
#94107=CARTESIAN_POINT('Ctrl Pts',(13.3298047978312,-5.80925739830131,10.6374828466507));
#94108=CARTESIAN_POINT('Ctrl Pts',(13.5171085156676,-9.67623713023754,7.31489439723108));
#94109=CARTESIAN_POINT('Ctrl Pts',(13.7045226807009,-11.8343851470158,2.68839440087991));
#94110=CARTESIAN_POINT('Ctrl Pts',(13.8920417432291,-11.9012035933258,-2.41678325350551));
#94111=CARTESIAN_POINT('Ctrl Pts',(14.079665958182,-9.85846808915857,-7.10106027918717));
#94112=CARTESIAN_POINT('Ctrl Pts',(14.2673878802831,-6.07020448910423,-10.5318302742615));
#94113=CARTESIAN_POINT('Ctrl Pts',(14.4552057276401,-1.20080043304805,-12.1025206353879));
#94114=CARTESIAN_POINT('Ctrl Pts',(14.6431142432908,3.8816049546317,-11.5313035488319));
#94115=CARTESIAN_POINT('Ctrl Pts',(14.8624426279901,9.0254261845754,-8.48686288050747));
#94116=CARTESIAN_POINT('Ctrl Pts',(15.0662215925831,11.7864106250798,-3.50019926818456));
#94117=CARTESIAN_POINT('Ctrl Pts',(15.254409406039,11.9202349594292,1.5765729310934));
#94118=CARTESIAN_POINT('Ctrl Pts',(15.4191235409337,10.6578227800216,5.83335525776536));
#94119=CARTESIAN_POINT('Ctrl Pts',(15.6074366748314,7.38808957059488,9.82399360787681));
#94120=CARTESIAN_POINT('Ctrl Pts',(15.8193743748441,2.05440533968246,12.1239164257433));
#94121=CARTESIAN_POINT('Ctrl Pts',(16.0313917910744,-3.73589016362928,11.717970713382));
#94122=CARTESIAN_POINT('Ctrl Pts',(16.267050002056,-9.26251206309682,8.36911230129259));
#94123=CARTESIAN_POINT('Ctrl Pts',(16.5263714569448,-12.533929235738,1.89081660411466));
#94124=CARTESIAN_POINT('Ctrl Pts',(16.8093751255442,-11.2186654351146,-5.92967881388903));
#94125=CARTESIAN_POINT('Ctrl Pts',(17.0688842231128,-5.98069892529497,-10.9674338194529));
#94126=CARTESIAN_POINT('Ctrl Pts',(17.3048617982993,0.344066224609658,-12.3144477215541));
#94127=CARTESIAN_POINT('Ctrl Pts',(17.5172733718789,5.95765915627426,-10.7876969598574));
#94128=CARTESIAN_POINT('Ctrl Pts',(17.7297418565277,10.2455913891075,-6.85024088753073));
#94129=CARTESIAN_POINT('Ctrl Pts',(17.9421831783442,12.248073460281,-1.38505961147241));
#94130=CARTESIAN_POINT('Ctrl Pts',(18.1547754227988,11.5188638260364,4.39096010934591));
#94131=CARTESIAN_POINT('Ctrl Pts',(18.3671125344183,8.21967595083557,9.1880203878024));
#94132=CARTESIAN_POINT('Ctrl Pts',(18.5799708194115,3.08654720046552,11.9359926983551));
#94133=CARTESIAN_POINT('Ctrl Pts',(18.7919954923611,-2.73535569069524,12.0215380695732));
#94134=CARTESIAN_POINT('Ctrl Pts',(19.0053084385149,-7.94711295728738,9.42520690240711));
#94135=CARTESIAN_POINT('Ctrl Pts',(19.2159056093561,-11.3857266012703,4.72718457448586));
#94136=CARTESIAN_POINT('Ctrl Pts',(19.4383538857774,-12.2844643908536,-1.02563854021835));
#94137=CARTESIAN_POINT('Ctrl Pts',(19.5755497693638,-10.4423848684627,-6.54989237074188));
#94138=CARTESIAN_POINT('Ctrl Pts',(19.7502330266567,-6.27044368623733,-10.6109788360224));
#94139=CARTESIAN_POINT('Ctrl Pts',(19.9067401471095,-0.700332527302415,
-12.304166099507));
#94140=CARTESIAN_POINT('Ctrl Pts',(20.0721200843413,5.02482750250949,-11.2515282704222));
#94141=CARTESIAN_POINT('Ctrl Pts',(20.2332449466593,9.62741902390977,-7.68867788673749));
#94142=CARTESIAN_POINT('Ctrl Pts',(20.3962864578522,12.0805747843324,-2.41184681685216));
#94143=CARTESIAN_POINT('Ctrl Pts',(20.5584408125953,11.8380006987581,3.40253336230924));
#94144=CARTESIAN_POINT('Ctrl Pts',(20.7209391746282,8.95366751262233,8.45314344278682));
#94145=CARTESIAN_POINT('Ctrl Pts',(20.8832633852329,4.07441140443369,11.6219108468804));
#94146=CARTESIAN_POINT('Ctrl Pts',(21.0455652300593,-1.7146252320768,12.1839430152868));
#94147=CARTESIAN_POINT('Ctrl Pts',(21.2079576291958,-7.11302875026615,10.0544459268831));
#94148=CARTESIAN_POINT('Ctrl Pts',(21.3934853478725,-11.4861546019893,4.98512765023302));
#94149=CARTESIAN_POINT('Ctrl Pts',(21.5257040221825,-12.1499364246399,0.288695447581215));
#94150=CARTESIAN_POINT('Ctrl Pts',(21.6019507193,-11.5961781364247,-2.52793074198454));
#94151=CARTESIAN_POINT('Ctrl Pts',(-0.185619006479058,10.0933261135196,
-2.22965916229763));
#94152=CARTESIAN_POINT('Ctrl Pts',(-0.117300790501088,10.5748062538398,
0.292199444285957));
#94153=CARTESIAN_POINT('Ctrl Pts',(-0.00302478330723105,9.99803717212611,
4.35034456802874));
#94154=CARTESIAN_POINT('Ctrl Pts',(0.159034371049183,6.18659475687002,8.78323627108909));
#94155=CARTESIAN_POINT('Ctrl Pts',(0.300544972038591,1.47700746620311,10.6342663436784));
#94156=CARTESIAN_POINT('Ctrl Pts',(0.442337090194551,-3.57821420110069,
10.1475684647875));
#94157=CARTESIAN_POINT('Ctrl Pts',(0.584195829308131,-7.84371227150242,
7.37625010341519));
#94158=CARTESIAN_POINT('Ctrl Pts',(0.72638210808798,-10.367739942029,2.95834583624723));
#94159=CARTESIAN_POINT('Ctrl Pts',(0.868398654429114,-10.5809430214755,
-2.13457721884431));
#94160=CARTESIAN_POINT('Ctrl Pts',(1.01134841234015,-8.43060470673339,-6.76121401375651));
#94161=CARTESIAN_POINT('Ctrl Pts',(1.15275825406684,-4.39155286462621,-9.88868216121412));
#94162=CARTESIAN_POINT('Ctrl Pts',(1.29806892103168,0.638793885868586,-10.8145395134698));
#94163=CARTESIAN_POINT('Ctrl Pts',(1.43573014356304,5.53815777824442,-9.32520081283725));
#94164=CARTESIAN_POINT('Ctrl Pts',(1.58954140736491,9.21275358259364,-5.75061203927714));
#94165=CARTESIAN_POINT('Ctrl Pts',(1.71047817919196,10.8366639978476,-0.88074887746556));
#94166=CARTESIAN_POINT('Ctrl Pts',(1.90724751534395,10.04431618838,4.21181408041434));
#94167=CARTESIAN_POINT('Ctrl Pts',(2.09324214724154,7.00555778279355,8.35618508415984));
#94168=CARTESIAN_POINT('Ctrl Pts',(2.30311330738613,1.87705741752283,10.9229722067622));
#94169=CARTESIAN_POINT('Ctrl Pts',(2.5332257405624,-4.54561841310713,10.3217734068532));
#94170=CARTESIAN_POINT('Ctrl Pts',(2.78536647948873,-9.81351567061726,5.61618222831888));
#94171=CARTESIAN_POINT('Ctrl Pts',(3.03782338103716,-11.2494025829444,-1.3090245995979));
#94172=CARTESIAN_POINT('Ctrl Pts',(3.29095008907448,-8.29511055112181,-7.75122091179339));
#94173=CARTESIAN_POINT('Ctrl Pts',(3.54458903946069,-2.07331878640508,-11.1892909019698));
#94174=CARTESIAN_POINT('Ctrl Pts',(3.77056982278458,4.19665237318481,-10.3559315238114));
#94175=CARTESIAN_POINT('Ctrl Pts',(3.96866456430814,8.45273696730399,-7.03593621691386));
#94176=CARTESIAN_POINT('Ctrl Pts',(4.13871597273587,10.6149061400342,-2.94502419387331));
#94177=CARTESIAN_POINT('Ctrl Pts',(4.33740334598655,10.9566874777779,2.45929408029225));
#94178=CARTESIAN_POINT('Ctrl Pts',(4.56489938943493,8.09225092751257,8.14593648910699));
#94179=CARTESIAN_POINT('Ctrl Pts',(4.82140674035802,1.67392883349891,11.3844888654692));
#94180=CARTESIAN_POINT('Ctrl Pts',(5.0784905353754,-5.42364562133815,10.1772068941644));
#94181=CARTESIAN_POINT('Ctrl Pts',(5.336151281316,-10.4315834824905,4.9793900503427));
#94182=CARTESIAN_POINT('Ctrl Pts',(5.59439033959415,-11.3747242087523,-2.19301745790991));
#94183=CARTESIAN_POINT('Ctrl Pts',(5.85320774256082,-7.86907925564315,-8.53689977516254));
#94184=CARTESIAN_POINT('Ctrl Pts',(6.11260412203838,-1.26235022387817,-11.5692530353362));
#94185=CARTESIAN_POINT('Ctrl Pts',(6.34369227098713,5.06919294204147,-10.2415176535993));
#94186=CARTESIAN_POINT('Ctrl Pts',(6.54627005947845,9.15551290375705,-6.53203957187647));
#94187=CARTESIAN_POINT('Ctrl Pts',(6.72016445010838,11.0505027548576,-2.19287267091472));
#94188=CARTESIAN_POINT('Ctrl Pts',(6.89431529161194,10.9882369915932,2.54767804033175));
#94189=CARTESIAN_POINT('Ctrl Pts',(7.08810135472563,8.76241579151075,7.33582397855815));
#94190=CARTESIAN_POINT('Ctrl Pts',(7.2628065037542,4.88176934217404,10.224447229933));
#94191=CARTESIAN_POINT('Ctrl Pts',(7.43776736394009,0.281512668682108,11.2268839659177));
#94192=CARTESIAN_POINT('Ctrl Pts',(7.59347538540535,-3.91850390490377,10.6525957197084));
#94193=CARTESIAN_POINT('Ctrl Pts',(7.76890244595317,-7.96078056106154,8.1068360055412));
#94194=CARTESIAN_POINT('Ctrl Pts',(7.97386284239987,-11.0540605057285,3.46069251756181));
#94195=CARTESIAN_POINT('Ctrl Pts',(8.20852292562262,-11.4323534240288,-3.10028647612775));
#94196=CARTESIAN_POINT('Ctrl Pts',(8.42898801261747,-8.04427720537063,-8.26450393249604));
#94197=CARTESIAN_POINT('Ctrl Pts',(8.60564238755027,-3.89233801355417,-10.5975657495071));
#94198=CARTESIAN_POINT('Ctrl Pts',(8.78248401029939,0.784991099698641,-11.5398447216046));
#94199=CARTESIAN_POINT('Ctrl Pts',(8.97436271810468,5.94350829980616,-10.0521140215687));
#94200=CARTESIAN_POINT('Ctrl Pts',(9.18136388578912,9.82591071360329,-5.96135288429516));
#94201=CARTESIAN_POINT('Ctrl Pts',(9.35903887805549,11.4259511373913,-1.39532146785222));
#94202=CARTESIAN_POINT('Ctrl Pts',(9.51718886382132,11.046839530257,2.89306782909364));
#94203=CARTESIAN_POINT('Ctrl Pts',(9.69531065618581,9.00905509810931,7.23148778947319));
#94204=CARTESIAN_POINT('Ctrl Pts',(9.87367490207668,5.2539372050763,10.4385707953799));
#94205=CARTESIAN_POINT('Ctrl Pts',(10.0721679770359,-0.0359846706333819,
11.5700988759545));
#94206=CARTESIAN_POINT('Ctrl Pts',(10.2510516766973,-4.79716825546636,10.5500969177149));
#94207=CARTESIAN_POINT('Ctrl Pts',(10.4301715895454,-8.72039401479544,7.65185637941947));
#94208=CARTESIAN_POINT('Ctrl Pts',(10.6394202628606,-11.5168011966333,2.68460959360604));
#94209=CARTESIAN_POINT('Ctrl Pts',(10.8789516349422,-11.4007138619713,-4.02009897255846));
#94210=CARTESIAN_POINT('Ctrl Pts',(11.1489446719379,-6.79589583934775,-10.0238491212784));
#94211=CARTESIAN_POINT('Ctrl Pts',(11.4194521684921,0.482857387799818,-12.1234364564696));
#94212=CARTESIAN_POINT('Ctrl Pts',(11.6904683222343,7.60210633467787,-9.48629381739815));
#94213=CARTESIAN_POINT('Ctrl Pts',(11.9619844318012,11.7704714210056,-3.12417202096832));
#94214=CARTESIAN_POINT('Ctrl Pts',(12.2339955399624,11.3472899568952,4.48161077014586));
#94215=CARTESIAN_POINT('Ctrl Pts',(12.5064934469842,6.47900806171408,10.3652310553541));
#94216=CARTESIAN_POINT('Ctrl Pts',(12.7491382824443,-0.115092593871167,
11.9965207438775));
#94217=CARTESIAN_POINT('Ctrl Pts',(12.9617604208479,-5.66932712881705,10.3524164038613));
#94218=CARTESIAN_POINT('Ctrl Pts',(13.1442139405268,-9.43637405277016,7.11605841772142));
#94219=CARTESIAN_POINT('Ctrl Pts',(13.3268721736923,-11.5400301082066,2.60705350414733));
#94220=CARTESIAN_POINT('Ctrl Pts',(13.5097329412205,-11.6054789249675,-2.3713096424544));
#94221=CARTESIAN_POINT('Ctrl Pts',(13.6927926573215,-9.61268254417223,-6.94178412299867));
#94222=CARTESIAN_POINT('Ctrl Pts',(13.8760493751974,-5.91470652543587,-10.2911833251264));
#94223=CARTESIAN_POINT('Ctrl Pts',(14.0595003754106,-1.15857060513477,-11.8256418676525));
#94224=CARTESIAN_POINT('Ctrl Pts',(14.2431438187993,3.80852772916814,-11.2676768952274));
#94225=CARTESIAN_POINT('Ctrl Pts',(14.4576147034959,8.83860998669587,-8.29097831594669));
#94226=CARTESIAN_POINT('Ctrl Pts',(14.6570160689187,11.5409394968827,-3.41172603447321));
#94227=CARTESIAN_POINT('Ctrl Pts',(14.8412851520698,11.6721745564983,1.55937792284147));
#94228=CARTESIAN_POINT('Ctrl Pts',(15.0026382754732,10.4356527910619,5.72934455817101));
#94229=CARTESIAN_POINT('Ctrl Pts',(15.1872075685466,7.23121856863992,9.64091306653126));
#94230=CARTESIAN_POINT('Ctrl Pts',(15.3950684928386,2.00027267799374,11.8970379868734));
#94231=CARTESIAN_POINT('Ctrl Pts',(15.6031452748645,-3.68246582260826,11.4990590640796));
#94232=CARTESIAN_POINT('Ctrl Pts',(15.8345765195311,-9.11024577131713,8.2107324415602));
#94233=CARTESIAN_POINT('Ctrl Pts',(16.0894467450161,-12.326401693567,1.84403017349057));
#94234=CARTESIAN_POINT('Ctrl Pts',(16.3678445378864,-11.0336854894674,-5.84936519393046));
#94235=CARTESIAN_POINT('Ctrl Pts',(16.6233577253131,-5.87699554144271,-10.8103679738959));
#94236=CARTESIAN_POINT('Ctrl Pts',(16.8558911710288,0.355399540435648,-12.1382610506978));
#94237=CARTESIAN_POINT('Ctrl Pts',(17.0653460588931,5.89099933966217,-10.6332079424033));
#94238=CARTESIAN_POINT('Ctrl Pts',(17.2750019757892,10.1225327187077,-6.74818253139266));
#94239=CARTESIAN_POINT('Ctrl Pts',(17.4847784853901,12.1003364385946,-1.35176206524406));
#94240=CARTESIAN_POINT('Ctrl Pts',(17.6948470084932,11.3802690665637,4.35595591482899));
#94241=CARTESIAN_POINT('Ctrl Pts',(17.9048201429876,8.11824693147351,9.09954721971294));
#94242=CARTESIAN_POINT('Ctrl Pts',(18.1154347704745,3.03915862004288,11.8196545783736));
#94243=CARTESIAN_POINT('Ctrl Pts',(18.325423469146,-2.72613110987367,11.9038913215774));
#94244=CARTESIAN_POINT('Ctrl Pts',(18.5367299625652,-7.89050873461128,9.33351651045655));
#94245=CARTESIAN_POINT('Ctrl Pts',(18.7457054460238,-11.3012202672818,4.67113223677404));
#94246=CARTESIAN_POINT('Ctrl Pts',(18.9662251567336,-12.193620628485,-1.03097537473009));
#94247=CARTESIAN_POINT('Ctrl Pts',(19.1024647483826,-10.3645021296875,-6.51607209457868));
#94248=CARTESIAN_POINT('Ctrl Pts',(19.2760119384225,-6.22017837815075,-10.5517199199323));
#94249=CARTESIAN_POINT('Ctrl Pts',(19.4315873565836,-0.683226350082178,
-12.2347432990342));
#94250=CARTESIAN_POINT('Ctrl Pts',(19.5960678744438,5.0109095220934,-11.1884067790233));
#94251=CARTESIAN_POINT('Ctrl Pts',(19.7564113157442,9.59142240873504,-7.64306850438877));
#94252=CARTESIAN_POINT('Ctrl Pts',(19.9187466440103,12.0343012504836,-2.3892255621501));
#94253=CARTESIAN_POINT('Ctrl Pts',(20.0802909525939,11.793043994749,3.4033212507376));
#94254=CARTESIAN_POINT('Ctrl Pts',(20.2422658654157,8.91830151793921,8.43786839370665));
#94255=CARTESIAN_POINT('Ctrl Pts',(20.4041575536249,4.05224680745339,11.5985615600057));
#94256=CARTESIAN_POINT('Ctrl Pts',(20.5661165762954,-1.72455343266205,12.1597439014428));
#94257=CARTESIAN_POINT('Ctrl Pts',(20.7282547450467,-7.11467144874381,10.0339938166866));
#94258=CARTESIAN_POINT('Ctrl Pts',(20.9135960702887,-11.4837610123811,4.96998028147232));
#94259=CARTESIAN_POINT('Ctrl Pts',(21.0457773344246,-12.1478998213886,0.275052131649602));
#94260=CARTESIAN_POINT('Ctrl Pts',(21.121985606656,-11.5941213892729,-2.54022968745642));
#94261=CARTESIAN_POINT('Ctrl Pts',(0.0468883190715043,9.87513244460898,
-2.19475014191929));
#94262=CARTESIAN_POINT('Ctrl Pts',(0.114030713978885,10.3462550411863,0.283509053294733));
#94263=CARTESIAN_POINT('Ctrl Pts',(0.225696291009577,9.78169823289018,4.24859024618672));
#94264=CARTESIAN_POINT('Ctrl Pts',(0.38424441193138,6.05401391249468,8.58604538141497));
#94265=CARTESIAN_POINT('Ctrl Pts',(0.522572982615551,1.4493723242407,10.39438467727));
#94266=CARTESIAN_POINT('Ctrl Pts',(0.661176886801409,-3.49174235122776,
9.91912528151));
#94267=CARTESIAN_POINT('Ctrl Pts',(0.799793926350337,-7.65981690416216,
7.21058321160161));
#94268=CARTESIAN_POINT('Ctrl Pts',(0.938699675819258,-10.1254171052646,
2.89475805670008));
#94269=CARTESIAN_POINT('Ctrl Pts',(1.0774028348938,-10.3334998105185,-2.07940899395324));
#94270=CARTESIAN_POINT('Ctrl Pts',(1.21698159467311,-8.23375157199671,-6.59680525048484));
#94271=CARTESIAN_POINT('Ctrl Pts',(1.35502420317193,-4.29082503876726,-9.6497000433534));
#94272=CARTESIAN_POINT('Ctrl Pts',(1.49683806736127,0.61845798375215,-10.5530464314786));
#94273=CARTESIAN_POINT('Ctrl Pts',(1.63115645888639,5.39880279485396,-9.09992044033476));
#94274=CARTESIAN_POINT('Ctrl Pts',(1.78119823087382,8.98311851124421,-5.61262810702319));
#94275=CARTESIAN_POINT('Ctrl Pts',(1.89914716909541,10.5668634406556,-0.863359736108471));
#94276=CARTESIAN_POINT('Ctrl Pts',(2.09092707093951,9.79411297578629,4.09974224607044));
#94277=CARTESIAN_POINT('Ctrl Pts',(2.27227504460956,6.83178142521456,8.1407345402975));
#94278=CARTESIAN_POINT('Ctrl Pts',(2.47677050336701,1.8341135810532,10.6412176269922));
#94279=CARTESIAN_POINT('Ctrl Pts',(2.70096262760981,-4.42295544725151,10.0555858579246));
#94280=CARTESIAN_POINT('Ctrl Pts',(2.94651424708369,-9.55296973843427,5.47242477730225));
#94281=CARTESIAN_POINT('Ctrl Pts',(3.19230186483792,-10.9506117802351,-1.26972603849257));
#94282=CARTESIAN_POINT('Ctrl Pts',(3.43866776969254,-8.07492744395638,-7.53972790059379));
#94283=CARTESIAN_POINT('Ctrl Pts',(3.68546398000364,-2.02091240779182,-10.8847378569879));
#94284=CARTESIAN_POINT('Ctrl Pts',(3.90529255407266,4.07825689510438,-10.0738326461541));
#94285=CARTESIAN_POINT('Ctrl Pts',(4.09795042603787,8.21745567231149,-6.84490401927142));
#94286=CARTESIAN_POINT('Ctrl Pts',(4.26330957581834,10.319891481976,-2.86685448795266));
#94287=CARTESIAN_POINT('Ctrl Pts',(4.45648701258071,10.6521098287859,2.3875741469057));
#94288=CARTESIAN_POINT('Ctrl Pts',(4.67763710085154,7.86743005469358,7.91545385483815));
#94289=CARTESIAN_POINT('Ctrl Pts',(4.926939430199,1.62934305813083,11.0628341733645));
#94290=CARTESIAN_POINT('Ctrl Pts',(5.17675887001051,-5.26758965195953,9.8894979002806));
#94291=CARTESIAN_POINT('Ctrl Pts',(5.4270982839676,-10.133076375223,4.8392917781549));
#94292=CARTESIAN_POINT('Ctrl Pts',(5.67796487531094,-11.0491418208461,-2.12831927355943));
#94293=CARTESIAN_POINT('Ctrl Pts',(5.92936241374252,-7.64390736818979,-8.29022018966899));
#94294=CARTESIAN_POINT('Ctrl Pts',(6.18129477974471,-1.22728028249969,-11.23520053354));
#94295=CARTESIAN_POINT('Ctrl Pts',(6.40571582591634,4.92150724239765,-9.9457051776774));
#94296=CARTESIAN_POINT('Ctrl Pts',(6.60243453809443,8.88960333168464,-6.34350746355418));
#94297=CARTESIAN_POINT('Ctrl Pts',(6.77129389446513,10.7296919156058,-2.1300022505958));
#94298=CARTESIAN_POINT('Ctrl Pts',(6.94039652441011,10.6692178625933,2.47310728894808));
#94299=CARTESIAN_POINT('Ctrl Pts',(7.12855930053127,8.50797601358858,7.12228923056046));
#94300=CARTESIAN_POINT('Ctrl Pts',(7.29819263731241,4.7400095745379,9.92702859165824));
#94301=CARTESIAN_POINT('Ctrl Pts',(7.46807153457936,0.273380586784091,10.9003466502549));
#94302=CARTESIAN_POINT('Ctrl Pts',(7.61925924909045,-3.80466580324696,10.3427388138934));
#94303=CARTESIAN_POINT('Ctrl Pts',(7.78959139326839,-7.72954127611913,7.87093104257765));
#94304=CARTESIAN_POINT('Ctrl Pts',(7.98860172481287,-10.7330126993619,3.35968762659343));
#94305=CARTESIAN_POINT('Ctrl Pts',(8.2164580403836,-11.1003918261383,-3.01100747504486));
#94306=CARTESIAN_POINT('Ctrl Pts',(8.43054075733716,-7.81046194370647,-8.02571834499739));
#94307=CARTESIAN_POINT('Ctrl Pts',(8.60208730154287,-3.77859473411447,-10.2913249526089));
#94308=CARTESIAN_POINT('Ctrl Pts',(8.77382123972295,0.763621927493125,-11.2064020023924));
#94309=CARTESIAN_POINT('Ctrl Pts',(8.96017336877873,5.77352570649464,-9.76160039398119));
#94310=CARTESIAN_POINT('Ctrl Pts',(9.16122393237721,9.54433910015271,-5.78846853353381));
#94311=CARTESIAN_POINT('Ctrl Pts',(9.33380383741733,11.0985302356744,-1.35340417939127));
#94312=CARTESIAN_POINT('Ctrl Pts',(9.48743167162671,10.7302913508911,2.81235066996444));
#94313=CARTESIAN_POINT('Ctrl Pts',(9.66047154404099,8.75067522278089,7.02698063644771));
#94314=CARTESIAN_POINT('Ctrl Pts',(9.83376200706454,5.10244018493771,10.1428909049288));
#94315=CARTESIAN_POINT('Ctrl Pts',(10.0266323623159,-0.0375966260133391,
11.2424270292935));
#94316=CARTESIAN_POINT('Ctrl Pts',(10.200465347967,-4.66435103389636,10.2512760419087));
#94317=CARTESIAN_POINT('Ctrl Pts',(10.3745490662983,-8.47729079196604,7.43459200187802));
#94318=CARTESIAN_POINT('Ctrl Pts',(10.5779374592024,-11.1954312635547,2.60651789413556));
#94319=CARTESIAN_POINT('Ctrl Pts',(10.8107978298792,-11.0827892717403,-3.91143012134676));
#94320=CARTESIAN_POINT('Ctrl Pts',(11.0733244705727,-6.60553148650756,-9.74928532905834));
#94321=CARTESIAN_POINT('Ctrl Pts',(11.3364087177861,0.473374528820086,-11.7915043150319));
#94322=CARTESIAN_POINT('Ctrl Pts',(11.6000483863509,7.39892601293791,-9.22641799008054));
#94323=CARTESIAN_POINT('Ctrl Pts',(11.8642402274303,11.4550878200309,-3.03610638012168));
#94324=CARTESIAN_POINT('Ctrl Pts',(12.1289822792327,11.0435290122831,4.36640970745214));
#94325=CARTESIAN_POINT('Ctrl Pts',(12.3942707801871,6.30432840493419,10.0945732748139));
#94326=CARTESIAN_POINT('Ctrl Pts',(12.6305653527167,-0.117105282786375,
11.6834591349301));
#94327=CARTESIAN_POINT('Ctrl Pts',(12.8376729609091,-5.52732785933807,10.0821181565203));
#94328=CARTESIAN_POINT('Ctrl Pts',(13.0154321048852,-9.19750920314661,6.92911563257701));
#94329=CARTESIAN_POINT('Ctrl Pts',(13.1934285394712,-11.2475761619162,2.53524663869076));
#94330=CARTESIAN_POINT('Ctrl Pts',(13.3716607445812,-11.3114796153966,-2.31709443318142));
#94331=CARTESIAN_POINT('Ctrl Pts',(13.5501275727524,-9.36879757076698,-6.77293750521516));
#94332=CARTESIAN_POINT('Ctrl Pts',(13.7288272740876,-5.76286586238848,-10.0391279784165));
#94333=CARTESIAN_POINT('Ctrl Pts',(13.9077586256967,-1.12395467957662,-11.5359049681128));
#94334=CARTESIAN_POINT('Ctrl Pts',(14.086920220302,3.72193056449534,-10.991676187186));
#94335=CARTESIAN_POINT('Ctrl Pts',(14.2962084781089,8.63052987121803,-8.08705962566316));
#94336=CARTESIAN_POINT('Ctrl Pts',(14.4908538017284,11.2686759469096,-3.32435546363631));
#94337=CARTESIAN_POINT('Ctrl Pts',(14.6707791287713,11.3969035793279,1.52957519084057));
#94338=CARTESIAN_POINT('Ctrl Pts',(14.8283599138058,10.1893571480635,5.60205724013665));
#94339=CARTESIAN_POINT('Ctrl Pts',(15.0086594519658,7.05920045221355,9.4232425043886));
#94340=CARTESIAN_POINT('Ctrl Pts',(15.211773956704,1.94778936772532,11.6280440864309));
#94341=CARTESIAN_POINT('Ctrl Pts',(15.4151630308288,-3.60693517107769,11.2392351797925));
#94342=CARTESIAN_POINT('Ctrl Pts',(15.6414526624567,-8.91423786935106,8.02419552881062));
#94343=CARTESIAN_POINT('Ctrl Pts',(15.8907548211699,-12.0605597097748,1.79679831518536));
#94344=CARTESIAN_POINT('Ctrl Pts',(16.163191580604,-10.7960738679334,-5.73193800227007));
#94345=CARTESIAN_POINT('Ctrl Pts',(16.41334739475,-5.74785323359727,-10.5893059881456));
#94346=CARTESIAN_POINT('Ctrl Pts',(16.6410977293422,0.356304475045441,-11.8901509760637));
#94347=CARTESIAN_POINT('Ctrl Pts',(16.8463169597766,5.78001582433962,-10.4157688994121));
#94348=CARTESIAN_POINT('Ctrl Pts',(17.0518065043981,9.92763508001442,-6.60811463582451));
#94349=CARTESIAN_POINT('Ctrl Pts',(17.2574901073631,11.8670731514498,-1.31710918465926));
#94350=CARTESIAN_POINT('Ctrl Pts',(17.4635339299854,11.161059099898,4.28138607926673));
#94351=CARTESIAN_POINT('Ctrl Pts',(17.6695666131704,7.96049490837238,8.93590314995754));
#94352=CARTESIAN_POINT('Ctrl Pts',(17.8762947475351,2.97510156392891,11.6064115606909));
#94353=CARTESIAN_POINT('Ctrl Pts',(18.0825158331318,-2.68633915899874,11.6888620853711));
#94354=CARTESIAN_POINT('Ctrl Pts',(18.2900516890882,-7.75946435507434,9.16520199964202));
#94355=CARTESIAN_POINT('Ctrl Pts',(18.4954960228899,-11.1117450252379,4.58131790262806));
#94356=CARTESIAN_POINT('Ctrl Pts',(18.7121686537848,-11.9893823770525,-1.02085731366645));
#94357=CARTESIAN_POINT('Ctrl Pts',(18.8461604978706,-10.1905191614686,-6.4150574092785));
#94358=CARTESIAN_POINT('Ctrl Pts',(19.0168888857437,-6.11378020764086,-10.3857054152766));
#94359=CARTESIAN_POINT('Ctrl Pts',(19.1699862042231,-0.665040585986461,
-12.0418702738763));
#94360=CARTESIAN_POINT('Ctrl Pts',(19.3318944658821,4.94010577090635,-11.0122286489555));
#94361=CARTESIAN_POINT('Ctrl Pts',(19.4897842633542,9.45065765391111,-7.52127249356902));
#94362=CARTESIAN_POINT('Ctrl Pts',(19.6496837846903,11.8570837283046,-2.34636545288141));
#94363=CARTESIAN_POINT('Ctrl Pts',(19.8088568555673,11.6195942596276,3.36123155851592));
#94364=CARTESIAN_POINT('Ctrl Pts',(19.9685059338027,8.78633570480602,8.32349554013287));
#94365=CARTESIAN_POINT('Ctrl Pts',(20.1281223497918,3.98869219334678,11.4402304690933));
#94366=CARTESIAN_POINT('Ctrl Pts',(20.2878661710919,-1.70886274984082,11.9935718342937));
#94367=CARTESIAN_POINT('Ctrl Pts',(20.4478171504923,-7.02689664581043,9.89725056153651));
#94368=CARTESIAN_POINT('Ctrl Pts',(20.6307713581253,-11.3391595667794,4.89815896715976));
#94369=CARTESIAN_POINT('Ctrl Pts',(20.7612036626925,-11.9952158857887,0.265588695805443));
#94370=CARTESIAN_POINT('Ctrl Pts',(20.8366222476259,-11.448353871513,-2.52040522030094));
#94371=CARTESIAN_POINT('Ctrl Pts',(0.183614459124478,9.79786316135237,-2.18390363605074));
#94372=CARTESIAN_POINT('Ctrl Pts',(0.250341770018844,10.2652923627661,0.278931271446855));
#94373=CARTESIAN_POINT('Ctrl Pts',(0.361079149189646,9.70507677462218,4.21096420845386));
#94374=CARTESIAN_POINT('Ctrl Pts',(0.518366888107835,6.00740767582931,8.51416777379075));
#94375=CARTESIAN_POINT('Ctrl Pts',(0.655542474297922,1.44074519809565,10.3070121042654));
#94376=CARTESIAN_POINT('Ctrl Pts',(0.792981618713115,-3.4587220983823,9.83588618154369));
#94377=CARTESIAN_POINT('Ctrl Pts',(0.930404605240617,-7.59092267674199,
7.15040523375962));
#94378=CARTESIAN_POINT('Ctrl Pts',(1.06809234888974,-10.0348185367602,2.87241801630468));
#94379=CARTESIAN_POINT('Ctrl Pts',(1.20555599039251,-10.2409431246026,-2.05737109410186));
#94380=CARTESIAN_POINT('Ctrl Pts',(1.34386398892466,-8.16021043925077,-6.53361307400495));
#94381=CARTESIAN_POINT('Ctrl Pts',(1.48062853400263,-4.25370717449432,-9.55820608939274));
#94382=CARTESIAN_POINT('Ctrl Pts',(1.62110525372889,0.609335041197672,-10.4528924440852));
#94383=CARTESIAN_POINT('Ctrl Pts',(1.75413692600142,5.34391651279451,-9.01369845472587));
#94384=CARTESIAN_POINT('Ctrl Pts',(1.90271849574803,8.89323649719505,-5.5600974036933));
#94385=CARTESIAN_POINT('Ctrl Pts',(2.01950257907449,10.461335073174,-0.857833757076778));
#94386=CARTESIAN_POINT('Ctrl Pts',(2.20930202147911,9.69621420838626,4.05382364169921));
#94387=CARTESIAN_POINT('Ctrl Pts',(2.38882434817707,6.76402558143954,8.05427559657762));
#94388=CARTESIAN_POINT('Ctrl Pts',(2.5911696751643,1.81848501841292,10.528109479656));
#94389=CARTESIAN_POINT('Ctrl Pts',(2.81298349260819,-4.37201424850356,9.94872151500545));
#94390=CARTESIAN_POINT('Ctrl Pts',(3.05585519071514,-9.4459783465168,5.41513931684729));
#94391=CARTESIAN_POINT('Ctrl Pts',(3.29891245926674,-10.8278396352703,-1.25208481677035));
#94392=CARTESIAN_POINT('Ctrl Pts',(3.54248087609222,-7.98456011415915,-7.45088636332916));
#94393=CARTESIAN_POINT('Ctrl Pts',(3.78642356161324,-2.00041219665082,-10.756998482402));
#94394=CARTESIAN_POINT('Ctrl Pts',(4.00366193024937,4.02691199090365,-9.95545715254609));
#94395=CARTESIAN_POINT('Ctrl Pts',(4.1940202968856,8.11665682827487,-6.76499932942405));
#94396=CARTESIAN_POINT('Ctrl Pts',(4.3573838136257,10.1936786032613,-2.83492279490684));
#94397=CARTESIAN_POINT('Ctrl Pts',(4.54820422110693,10.5217640364167,2.35542955113606));
#94398=CARTESIAN_POINT('Ctrl Pts',(4.76662107188633,7.7713273867228,7.81493817752817));
#94399=CARTESIAN_POINT('Ctrl Pts',(5.01279825332115,1.6113145881985,10.9227010562467));
#94400=CARTESIAN_POINT('Ctrl Pts',(5.25944392263343,-5.19799627007342,9.76407920684044));
#94401=CARTESIAN_POINT('Ctrl Pts',(5.50656218450572,-10.0007734626784,4.77870524483264));
#94402=CARTESIAN_POINT('Ctrl Pts',(5.75416271454751,-10.9047480542855,-2.09824403734041));
#94403=CARTESIAN_POINT('Ctrl Pts',(6.00225064241072,-7.54418842815771,-8.17897689802922));
#94404=CARTESIAN_POINT('Ctrl Pts',(6.25083187444897,-1.21282426517761,-11.0846551043006));
#94405=CARTESIAN_POINT('Ctrl Pts',(6.47223861252284,4.85337527232899,-9.81235965589673));
#94406=CARTESIAN_POINT('Ctrl Pts',(6.66629611401229,8.76777044247514,-6.25884918518984));
#94407=CARTESIAN_POINT('Ctrl Pts',(6.8328580147061,10.5827983584686,-2.10264444945471));
#94408=CARTESIAN_POINT('Ctrl Pts',(6.99964746572987,10.5231160301507,2.43751391214038));
#94409=CARTESIAN_POINT('Ctrl Pts',(7.18522401361308,8.39154110993935,7.02279159226047));
#94410=CARTESIAN_POINT('Ctrl Pts',(7.35251256900072,4.67561428720135,9.7887253479214));
#94411=CARTESIAN_POINT('Ctrl Pts',(7.52003349787157,0.270973981687257,10.7485202607095));
#94412=CARTESIAN_POINT('Ctrl Pts',(7.66911434284302,-3.75025726686191,10.19865478183));
#94413=CARTESIAN_POINT('Ctrl Pts',(7.83706491325344,-7.62024552686739,7.76137857280017));
#94414=CARTESIAN_POINT('Ctrl Pts',(8.03328290043577,-10.5815581157576,3.31340924681337));
#94415=CARTESIAN_POINT('Ctrl Pts',(8.25792683192658,-10.9436830883588,-2.9675090618203));
#94416=CARTESIAN_POINT('Ctrl Pts',(8.46897913755438,-7.70027205447012,-7.91121797030631));
#94417=CARTESIAN_POINT('Ctrl Pts',(8.63809112468196,-3.7256112018197,-10.1446667494925));
#94418=CARTESIAN_POINT('Ctrl Pts',(8.80738397054104,0.752049767529649,-11.0467272685672));
#94419=CARTESIAN_POINT('Ctrl Pts',(8.99107917523528,5.69053692893971,-9.62248736715413));
#94420=CARTESIAN_POINT('Ctrl Pts',(9.1892589915876,9.40750408742455,-5.70607502743658));
#94421=CARTESIAN_POINT('Ctrl Pts',(9.35937116238761,10.9394620207273,-1.33441905354762));
#94422=CARTESIAN_POINT('Ctrl Pts',(9.51079897972392,10.5764897772339,2.77169008628882));
#94423=CARTESIAN_POINT('Ctrl Pts',(9.68135954194658,8.62523117889842,6.92593653995051));
#94424=CARTESIAN_POINT('Ctrl Pts',(9.85216535947771,5.02929449040856,9.99716749705792));
#94425=CARTESIAN_POINT('Ctrl Pts',(10.0422684509943,-0.0370046278410104,
11.0809239533146));
#94426=CARTESIAN_POINT('Ctrl Pts',(10.2136076308811,-4.59738656225664,10.1039913431277));
#94427=CARTESIAN_POINT('Ctrl Pts',(10.3851935207641,-8.35562322052339,7.32771401866009));
#94428=CARTESIAN_POINT('Ctrl Pts',(10.5856653585996,-11.0347880660269,2.56887395258143));
#94429=CARTESIAN_POINT('Ctrl Pts',(10.8151879901628,-10.9237726058889,-3.8556653985514));
#94430=CARTESIAN_POINT('Ctrl Pts',(11.0739580396521,-6.5106008392871,-9.61000610749268));
#94431=CARTESIAN_POINT('Ctrl Pts',(11.3332851299844,0.467209227920453,-11.6230950570897));
#94432=CARTESIAN_POINT('Ctrl Pts',(11.5931693281801,7.2941286449926,-9.09458958873076));
#94433=CARTESIAN_POINT('Ctrl Pts',(11.853609980442,11.2927459882514,-2.99220026576765));
#94434=CARTESIAN_POINT('Ctrl Pts',(12.1146065789635,10.8870722493502,4.30559358746303));
#94435=CARTESIAN_POINT('Ctrl Pts',(12.3761579386682,6.21469160094993,9.95311235977421));
#94436=CARTESIAN_POINT('Ctrl Pts',(12.6091398388233,-0.116703708482184,
11.5197928369494));
#94437=CARTESIAN_POINT('Ctrl Pts',(12.8133567685166,-5.45142549612194,9.94083145824057));
#94438=CARTESIAN_POINT('Ctrl Pts',(12.9886444160827,-9.07059415929487,6.83168724086131));
#94439=CARTESIAN_POINT('Ctrl Pts',(13.1641760934311,-11.092299460829,2.4986734042833));
#94440=CARTESIAN_POINT('Ctrl Pts',(13.3399509622567,-11.1553520037565,-2.28676417024083));
#94441=CARTESIAN_POINT('Ctrl Pts',(13.5159684793945,-9.23936112946262,-6.68146663577346));
#94442=CARTESIAN_POINT('Ctrl Pts',(13.6922275712029,-5.68270256836087,-9.90307032808977));
#94443=CARTESIAN_POINT('Ctrl Pts',(13.8687275286725,-1.10683977756436,-11.3795432290739));
#94444=CARTESIAN_POINT('Ctrl Pts',(14.0454674390564,3.67354689666366,-10.8427052739739));
#94445=CARTESIAN_POINT('Ctrl Pts',(14.2519425858938,8.51618802247031,-7.977176725935));
#94446=CARTESIAN_POINT('Ctrl Pts',(14.4439915267229,11.1192240057796,-3.27805817500437));
#94447=CARTESIAN_POINT('Ctrl Pts',(14.6215329808132,11.2457792395615,1.51156293289995));
#94448=CARTESIAN_POINT('Ctrl Pts',(14.7770361230669,10.0541750259763,5.53035051060673));
#94449=CARTESIAN_POINT('Ctrl Pts',(14.9549735676819,6.965075696007,9.30150472580482));
#94450=CARTESIAN_POINT('Ctrl Pts',(15.1554478199515,1.92014154542388,11.4777065223719));
#94451=CARTESIAN_POINT('Ctrl Pts',(15.3562146123695,-3.56296549636649,11.0939794920203));
#94452=CARTESIAN_POINT('Ctrl Pts',(15.5796118099573,-8.80245651644644,7.92011556461129));
#94453=CARTESIAN_POINT('Ctrl Pts',(15.8257599378043,-11.9091213200236,1.77158588855571));
#94454=CARTESIAN_POINT('Ctrl Pts',(16.0947928420177,-10.6606265159978,-5.66310190677918));
#94455=CARTESIAN_POINT('Ctrl Pts',(16.3418651896297,-5.67477284967232,-10.460720415196));
#94456=CARTESIAN_POINT('Ctrl Pts',(16.5668411838028,0.35500497682303,-11.7458113053674));
#94457=CARTESIAN_POINT('Ctrl Pts',(16.7695877632996,5.7133734584233,-10.2892834180772));
#94458=CARTESIAN_POINT('Ctrl Pts',(16.9726287036363,9.81162565530563,-6.52706848478553));
#94459=CARTESIAN_POINT('Ctrl Pts',(17.175890110972,11.7283013091856,-1.29843299398321));
#94460=CARTESIAN_POINT('Ctrl Pts',(17.3795355657123,11.0306030975541,4.23493323563435));
#94461=CARTESIAN_POINT('Ctrl Pts',(17.5832017988026,7.86690031490684,8.83595145758763));
#94462=CARTESIAN_POINT('Ctrl Pts',(17.7875808547236,2.93815531618296,11.476341011785));
#94463=CARTESIAN_POINT('Ctrl Pts',(17.9915008910348,-2.65993296615087,11.5577566949746));
#94464=CARTESIAN_POINT('Ctrl Pts',(18.1967285688977,-7.6769832497116,9.0625069894267));
#94465=CARTESIAN_POINT('Ctrl Pts',(18.3999671286159,-10.9929383413539,4.52773913144796));
#94466=CARTESIAN_POINT('Ctrl Pts',(18.6142643904826,-11.8612734120244,-1.01283062439117));
#94467=CARTESIAN_POINT('Ctrl Pts',(18.746839574998,-10.0814706687781,-6.34979580437877));
#94468=CARTESIAN_POINT('Ctrl Pts',(18.9157801590528,-6.04754161886867,-10.2790745664293));
#94469=CARTESIAN_POINT('Ctrl Pts',(19.0672944337368,-0.655174918774475,
-11.9180843893191));
#94470=CARTESIAN_POINT('Ctrl Pts',(19.2275478343006,4.89268465504261,-10.8991049408004));
#94471=CARTESIAN_POINT('Ctrl Pts',(19.3838460285229,9.3578015813762,-7.44340319910321));
#94472=CARTESIAN_POINT('Ctrl Pts',(19.5421535987863,11.7403421743398,-2.32008648120949));
#94473=CARTESIAN_POINT('Ctrl Pts',(19.6997636988169,11.5052746138427,3.33148982193097));
#94474=CARTESIAN_POINT('Ctrl Pts',(19.8578668941574,8.69955374686446,8.24565437927413));
#94475=CARTESIAN_POINT('Ctrl Pts',(20.0159574924546,3.94777155655652,11.3328450679878));
#94476=CARTESIAN_POINT('Ctrl Pts',(20.1742022741564,-1.69613308293156,11.8808152256684));
#94477=CARTESIAN_POINT('Ctrl Pts',(20.3326590484748,-6.96488480194656,9.80454780154648));
#94478=CARTESIAN_POINT('Ctrl Pts',(20.5139662157656,-11.237866859747,4.85022961102954));
#94479=CARTESIAN_POINT('Ctrl Pts',(20.6431763802473,-11.8882199022414,0.261240555255304));
#94480=CARTESIAN_POINT('Ctrl Pts',(20.7180435334305,-11.3462020984903,-2.50431251217421));
#94481=CARTESIAN_POINT('Ctrl Pts',(21.8012598463038,-10.0131352633455,0.0110692926695161));
#94482=CARTESIAN_POINT('Ctrl Pts',(21.7552321039728,-10.0072228406033,1.65687208126129));
#94483=CARTESIAN_POINT('Ctrl Pts',(21.7096578718089,-9.62567683521378,3.2083740442833));
#94484=CARTESIAN_POINT('Ctrl Pts',(21.6639548339268,-8.89621852178167,4.61102195828347));
#94485=CARTESIAN_POINT('Ctrl Pts',(21.6639546335718,-8.8962153239491,4.61102810727525));
#94486=CARTESIAN_POINT('Ctrl Pts',(21.6639544332167,-8.89621212610985,4.61103425626419));
#94487=CARTESIAN_POINT('Ctrl Pts',(21.6639542328617,-8.89620892826391,4.61104040525026));
#94488=CARTESIAN_POINT('Ctrl Pts',(21.6182513942267,-8.16675076227458,6.01368086513788));
#94489=CARTESIAN_POINT('Ctrl Pts',(21.5724221870221,-7.08938010597456,7.26746591912194));
#94490=CARTESIAN_POINT('Ctrl Pts',(21.526625916955,-5.78896373027067,8.1934202438268));
#94491=CARTESIAN_POINT('Ctrl Pts',(21.5266257407303,-5.78895872624974,8.19342380691236));
#94492=CARTESIAN_POINT('Ctrl Pts',(21.5266255645056,-5.78895372222556,8.19342736999304));
#94493=CARTESIAN_POINT('Ctrl Pts',(21.5266253882809,-5.78894871819804,8.19343093306889));
#94494=CARTESIAN_POINT('Ctrl Pts',(21.4808290939245,-4.48852992910524,9.11938323095388));
#94495=CARTESIAN_POINT('Ctrl Pts',(21.4350653781105,-2.96506634557888,9.71750451332759));
#94496=CARTESIAN_POINT('Ctrl Pts',(21.3892587628962,-1.38607543009952,9.93797605507653));
#94497=CARTESIAN_POINT('Ctrl Pts',(21.3892586998405,-1.38607325652168,9.93797635856913));
#94498=CARTESIAN_POINT('Ctrl Pts',(21.3892586367849,-1.38607108294374,9.93797666206101));
#94499=CARTESIAN_POINT('Ctrl Pts',(21.3892585737293,-1.38606890936569,9.93797696555218));
#94500=CARTESIAN_POINT('Ctrl Pts',(21.3434518723909,0.192925123692123,10.1584478815394));
#94501=CARTESIAN_POINT('Ctrl Pts',(21.2976024042792,1.82744571608953,10.0012674688134));
#94502=CARTESIAN_POINT('Ctrl Pts',(21.2517547214262,3.33399312150951,9.47471961389721));
#94503=CARTESIAN_POINT('Ctrl Pts',(21.2517546941993,3.3339940161786,9.4747193012047));
#94504=CARTESIAN_POINT('Ctrl Pts',(21.2517546669725,3.33399491084763,9.47471898851206));
#94505=CARTESIAN_POINT('Ctrl Pts',(21.2517546397457,3.33399580551663,9.47471867581929));
#94506=CARTESIAN_POINT('Ctrl Pts',(21.205906928113,4.84054400470364,8.94817005165259));
#94507=CARTESIAN_POINT('Ctrl Pts',(21.1600609297291,6.21911907103573,8.05225365383932));
#94508=CARTESIAN_POINT('Ctrl Pts',(21.114170584641,7.31607797187692,6.89067769931178));
#94509=CARTESIAN_POINT('Ctrl Pts',(21.1141705230266,7.31607944470209,6.89067613972892));
#94510=CARTESIAN_POINT('Ctrl Pts',(21.1141704614123,7.31608091752672,6.89067458014561));
#94511=CARTESIAN_POINT('Ctrl Pts',(21.1141703997979,7.31608239035088,6.89067302056179));
#94512=CARTESIAN_POINT('Ctrl Pts',(21.0682800523852,8.41304058769296,5.72909629683467));
#94513=CARTESIAN_POINT('Ctrl Pts',(21.0223453621309,9.22838215118901,4.3018603581543));
#94514=CARTESIAN_POINT('Ctrl Pts',(20.9764473487262,9.67043942004942,2.76588563764872));
#94515=CARTESIAN_POINT('Ctrl Pts',(20.9764472893075,9.67043999232902,2.76588364920274));
#94516=CARTESIAN_POINT('Ctrl Pts',(20.9764472298887,9.67044056460801,2.7658816607565));
#94517=CARTESIAN_POINT('Ctrl Pts',(20.9764471704699,9.67044113688636,2.76587967231016));
#94518=CARTESIAN_POINT('Ctrl Pts',(20.9305491360636,10.11249764244,1.22990396426352));
#94519=CARTESIAN_POINT('Ctrl Pts',(20.8846874736051,10.1812698512961,-0.414810572222863));
#94520=CARTESIAN_POINT('Ctrl Pts',(20.8386848325414,9.86855581097698,-1.9838833732313));
#94521=CARTESIAN_POINT('Ctrl Pts',(20.838684794132,9.86855554987952,-1.98388468331296));
#94522=CARTESIAN_POINT('Ctrl Pts',(20.8386847557225,9.86855528878179,-1.98388599339458));
#94523=CARTESIAN_POINT('Ctrl Pts',(20.8386847173131,9.86855502768379,-1.98388730347614));
#94524=CARTESIAN_POINT('Ctrl Pts',(20.7926820752953,9.55584034544212,-3.55296000268544));
#94525=CARTESIAN_POINT('Ctrl Pts',(20.7465380004342,8.86163811437252,-5.04638936815762));
#94526=CARTESIAN_POINT('Ctrl Pts',(20.7006508715133,7.86285962965014,-6.29766374980489));
#94527=CARTESIAN_POINT('Ctrl Pts',(20.7006508339172,7.86285881133398,-6.29766477499523));
#94528=CARTESIAN_POINT('Ctrl Pts',(20.7006507963211,7.8628579930176,-6.29766580018542));
#94529=CARTESIAN_POINT('Ctrl Pts',(20.700650758725,7.86285717470103,-6.29766682537543));
#94530=CARTESIAN_POINT('Ctrl Pts',(20.654763592629,6.864077372574,-7.54894183541054));
#94531=CARTESIAN_POINT('Ctrl Pts',(20.6091309971028,5.56071904099251,-8.55806363998203));
#94532=CARTESIAN_POINT('Ctrl Pts',(20.5628824954473,4.09777307274928,-9.21188334086465));
#94533=CARTESIAN_POINT('Ctrl Pts',(20.5166339937918,2.63482710450628,-9.86570304174717));
#94534=CARTESIAN_POINT('Ctrl Pts',(20.4697652785271,1.01230003976588,-10.1642142991518));
#94535=CARTESIAN_POINT('Ctrl Pts',(20.4241375419168,-0.588808414128353,
-10.0733777577267));
#94536=CARTESIAN_POINT('Ctrl Pts',(20.4241375049837,-0.588809710136394,
-10.0733776841996));
#94537=CARTESIAN_POINT('Ctrl Pts',(20.4241374680506,-0.588811006144456,
-10.0733776106722));
#94538=CARTESIAN_POINT('Ctrl Pts',(20.4241374311175,-0.588812302152469,
-10.0733775371446));
#94539=CARTESIAN_POINT('Ctrl Pts',(20.3869849920578,-1.89251680263734,-9.99941325827055));
#94540=CARTESIAN_POINT('Ctrl Pts',(20.3506467756454,-3.18203022746201,-9.66729770391613));
#94541=CARTESIAN_POINT('Ctrl Pts',(20.3130702272109,-4.36215581350889,-9.10582210716729));
#94542=CARTESIAN_POINT('Ctrl Pts',(20.3044982202458,-4.63136746717885,-8.97773762558053));
#94543=CARTESIAN_POINT('Ctrl Pts',(20.2958617694733,-4.89488680516154,-8.83771756778075));
#94544=CARTESIAN_POINT('Ctrl Pts',(20.2871365063085,-5.15158403690282,-8.68610395029341));
#94545=CARTESIAN_POINT('Ctrl Pts',(20.2577530055678,-6.01604659310811,-8.17552464081054));
#94546=CARTESIAN_POINT('Ctrl Pts',(20.2273530245799,-6.80312796209644,-7.53346619228489));
#94547=CARTESIAN_POINT('Ctrl Pts',(20.1978687745464,-7.48035522254219,-6.79116690820229));
#94548=CARTESIAN_POINT('Ctrl Pts',(20.1802182937909,-7.88577122308478,-6.34679612673033));
#94549=CARTESIAN_POINT('Ctrl Pts',(20.1628959739862,-8.25181824281081,-5.86650099312686));
#94550=CARTESIAN_POINT('Ctrl Pts',(20.1463164348685,-8.57152250286074,-5.35697778778339));
#94551=CARTESIAN_POINT('Ctrl Pts',(20.1463158899337,-8.57153301087137,-5.35696104082088));
#94552=CARTESIAN_POINT('Ctrl Pts',(20.1463153449997,-8.57154351883193,-5.35694429382681));
#94553=CARTESIAN_POINT('Ctrl Pts',(20.1463148000665,-8.57155402674243,-5.35692754680115));
#94554=CARTESIAN_POINT('Ctrl Pts',(20.124177885672,-8.9984186839762,-4.67661024045451));
#94555=CARTESIAN_POINT('Ctrl Pts',(20.1033676350582,-9.34266561105165,-3.94417968405986));
#94556=CARTESIAN_POINT('Ctrl Pts',(20.0816978875363,-9.59692940229535,-3.18135205301605));
#94557=CARTESIAN_POINT('Ctrl Pts',(20.0600281400144,-9.85119319353904,-2.41852442197224));
#94558=CARTESIAN_POINT('Ctrl Pts',(20.0374986949878,-10.0154731210975,-1.6253016744882));
#94559=CARTESIAN_POINT('Ctrl Pts',(20.0119245448109,-10.0824548219061,-0.823411832214975));
#94560=CARTESIAN_POINT('Ctrl Pts',(20.0119241634875,-10.0824558206367,-0.823399875636732));
#94561=CARTESIAN_POINT('Ctrl Pts',(20.0119237821635,-10.0824568193457,-0.823387919056553));
#94562=CARTESIAN_POINT('Ctrl Pts',(20.0119234008388,-10.0824578180331,-0.823375962474456));
#94563=CARTESIAN_POINT('Ctrl Pts',(19.9903962735522,-10.1388372485164,-0.148384658059219));
#94564=CARTESIAN_POINT('Ctrl Pts',(19.9666927510919,-10.1262680360043,0.532755007697934));
#94565=CARTESIAN_POINT('Ctrl Pts',(19.941867359469,-10.0468329681363,1.20616332848875));
#94566=CARTESIAN_POINT('Ctrl Pts',(19.9174215132727,-9.96861235106805,1.86927618034265));
#94567=CARTESIAN_POINT('Ctrl Pts',(19.8918877223371,-9.82555490974834,2.52489398467586));
#94568=CARTESIAN_POINT('Ctrl Pts',(19.8662718761862,-9.61960087318472,3.15976851342234));
#94569=CARTESIAN_POINT('Ctrl Pts',(19.8560918131859,-9.53775212007169,3.41207572442991));
#94570=CARTESIAN_POINT('Ctrl Pts',(19.8458987889727,-9.44596912518285,3.66110671853785));
#94571=CARTESIAN_POINT('Ctrl Pts',(19.835755958896,-9.34437144790041,3.90602921000172));
#94572=CARTESIAN_POINT('Ctrl Pts',(19.8357530127888,-9.34434193763071,3.90610035069086));
#94573=CARTESIAN_POINT('Ctrl Pts',(19.8357500666855,-9.34431242653295,3.90617149103258));
#94574=CARTESIAN_POINT('Ctrl Pts',(19.8357471205861,-9.34428291460712,3.90624263102687));
#94575=CARTESIAN_POINT('Ctrl Pts',(19.8117357691311,-9.10375429369162,4.48604907321725));
#94576=CARTESIAN_POINT('Ctrl Pts',(19.7879846941381,-8.80821627629863,5.04277518921063));
#94577=CARTESIAN_POINT('Ctrl Pts',(19.7643605893076,-8.4641163047614,5.56782142106315));
#94578=CARTESIAN_POINT('Ctrl Pts',(19.7410989170983,-8.12529539270751,6.08481258020796));
#94579=CARTESIAN_POINT('Ctrl Pts',(19.7179603319782,-7.73939199826957,6.57108722534719));
#94580=CARTESIAN_POINT('Ctrl Pts',(19.6948177172066,-7.31260286916265,7.01846154723225));
#94581=CARTESIAN_POINT('Ctrl Pts',(19.6811884207982,-7.06125549109592,7.28193208842314));
#94582=CARTESIAN_POINT('Ctrl Pts',(19.6675577307813,-6.7957282621181,7.5319112443041));
#94583=CARTESIAN_POINT('Ctrl Pts',(19.6538997436435,-6.51729200697241,7.76673429501901));
#94584=CARTESIAN_POINT('Ctrl Pts',(19.6538977922536,-6.51725222529157,7.76676784544746));
#94585=CARTESIAN_POINT('Ctrl Pts',(19.6538958408632,-6.51721244334721,7.76680139556654));
#94586=CARTESIAN_POINT('Ctrl Pts',(19.6538938894722,-6.51717266113936,7.76683494537624));
#94587=CARTESIAN_POINT('Ctrl Pts',(19.634469850311,-6.1211827374716,8.10078791825245));
#94588=CARTESIAN_POINT('Ctrl Pts',(19.6148942435515,-5.69895233032108,8.40408527570492));
#94589=CARTESIAN_POINT('Ctrl Pts',(19.595280716088,-5.25602148926852,8.67378800972723));
#94590=CARTESIAN_POINT('Ctrl Pts',(19.5757664198158,-4.81533157887535,8.94212623021926));
#94591=CARTESIAN_POINT('Ctrl Pts',(19.5562145820723,-4.35415070186316,9.17721014280609));
#94592=CARTESIAN_POINT('Ctrl Pts',(19.5367352573205,-3.87788785491096,9.37616483050553));
#94593=CARTESIAN_POINT('Ctrl Pts',(19.5175565925449,-3.40897604184072,9.57204868734002));
#94594=CARTESIAN_POINT('Ctrl Pts',(19.4984482568019,-2.92544428516652,9.73291139569341));
#94595=CARTESIAN_POINT('Ctrl Pts',(19.479513211645,-2.43240488101956,9.8560087263723));
#94596=CARTESIAN_POINT('Ctrl Pts',(19.4768973989063,-2.36429314728155,9.87301420816653));
#94597=CARTESIAN_POINT('Ctrl Pts',(19.4742848894049,-2.29599988597296,9.88929893672284));
#94598=CARTESIAN_POINT('Ctrl Pts',(19.47167595057,-2.22753849970242,9.90485565245439));
#94599=CARTESIAN_POINT('Ctrl Pts',(19.4716749594633,-2.22751249198904,9.90486156227635));
#94600=CARTESIAN_POINT('Ctrl Pts',(19.4716739683572,-2.22748648425137,9.90486747199325));
#94601=CARTESIAN_POINT('Ctrl Pts',(19.4716729772516,-2.22746047648946,9.90487338160508));
#94602=CARTESIAN_POINT('Ctrl Pts',(19.4526695341822,-1.72878805869038,10.0181841859249));
#94603=CARTESIAN_POINT('Ctrl Pts',(19.4335943739675,-1.22127886684315,10.0925805320568));
#94604=CARTESIAN_POINT('Ctrl Pts',(19.4144573514764,-0.710925040065703,
10.1285809678906));
#94605=CARTESIAN_POINT('Ctrl Pts',(19.4034059597798,-0.416202073304849,
10.1493707703706));
#94606=CARTESIAN_POINT('Ctrl Pts',(19.3923339298187,-0.120530316333381,
10.1573568038));
#94607=CARTESIAN_POINT('Ctrl Pts',(19.3812431031346,0.174938904745155,10.1526464163313));
#94608=CARTESIAN_POINT('Ctrl Pts',(19.367234298816,0.54814557527839,10.1466967339322));
#94609=CARTESIAN_POINT('Ctrl Pts',(19.3532302365177,0.921032258087055,10.1205304950431));
#94610=CARTESIAN_POINT('Ctrl Pts',(19.339224780055,1.29144034910869,10.0743364254749));
#94611=CARTESIAN_POINT('Ctrl Pts',(19.3253210843792,1.6591571305744,10.0284779925837));
#94612=CARTESIAN_POINT('Ctrl Pts',(19.3114160154,2.02443215356254,9.96288156953981));
#94613=CARTESIAN_POINT('Ctrl Pts',(19.297503567475,2.38514521264296,9.8776815478027));
#94614=CARTESIAN_POINT('Ctrl Pts',(19.2951223254824,2.44688453329987,9.86309878920945));
#94615=CARTESIAN_POINT('Ctrl Pts',(19.292740867301,2.50849016982679,9.84794161757506));
#94616=CARTESIAN_POINT('Ctrl Pts',(19.2903591627888,2.56995143539188,9.83221056223149));
#94617=CARTESIAN_POINT('Ctrl Pts',(19.2813733359762,2.80183590519031,9.7728595645881));
#94618=CARTESIAN_POINT('Ctrl Pts',(19.2721417232226,3.03161724004271,9.70509961279013));
#94619=CARTESIAN_POINT('Ctrl Pts',(19.2628557069655,3.25871007913323,9.62915773747277));
#94620=CARTESIAN_POINT('Ctrl Pts',(19.2564784511862,3.41466814343352,9.57700396670104));
#94621=CARTESIAN_POINT('Ctrl Pts',(19.2500754855842,3.56935930716621,9.52099122486019));
#94622=CARTESIAN_POINT('Ctrl Pts',(19.2437084341844,3.7226077917393,9.46118958148128));
#94623=CARTESIAN_POINT('Ctrl Pts',(19.2384963879363,3.84805647102597,9.41223616310356));
#94624=CARTESIAN_POINT('Ctrl Pts',(19.2333426313397,3.9725439656621,9.36077843730233));
#94625=CARTESIAN_POINT('Ctrl Pts',(19.2282358010473,4.09595243702679,9.30681574951009));
#94626=CARTESIAN_POINT('Ctrl Pts',(19.2172042602722,4.36253376162538,9.19024802420344));
#94627=CARTESIAN_POINT('Ctrl Pts',(19.206391616527,4.62408128943517,9.06198823680086));
#94628=CARTESIAN_POINT('Ctrl Pts',(19.1956845759001,4.87965142449191,8.92270348980286));
#94629=CARTESIAN_POINT('Ctrl Pts',(19.1890405303381,5.03824049506218,8.83627305235708));
#94630=CARTESIAN_POINT('Ctrl Pts',(19.1824371599625,5.19452748575743,8.7455983281303));
#94631=CARTESIAN_POINT('Ctrl Pts',(19.1758476884273,5.34828392190368,8.65084831487406));
#94632=CARTESIAN_POINT('Ctrl Pts',(19.1642510595093,5.61887562629458,8.48410038405133));
#94633=CARTESIAN_POINT('Ctrl Pts',(19.1524794813995,5.88150243049401,8.30454934728981));
#94634=CARTESIAN_POINT('Ctrl Pts',(19.1406254170227,6.13522621453266,8.11322353794057));
#94635=CARTESIAN_POINT('Ctrl Pts',(19.1298638760916,6.36556568294915,7.93953116855219));
#94636=CARTESIAN_POINT('Ctrl Pts',(19.1190342942608,6.58856830199439,7.75613396617955));
#94637=CARTESIAN_POINT('Ctrl Pts',(19.108204579914,6.80354429825768,7.56376615684175));
#94638=CARTESIAN_POINT('Ctrl Pts',(19.0919038331487,7.12712340325566,7.2742166040642));
#94639=CARTESIAN_POINT('Ctrl Pts',(19.0754871645745,7.43259455463111,6.96412257454898));
#94640=CARTESIAN_POINT('Ctrl Pts',(19.0589508125994,7.71724725468761,6.63579139086323));
#94641=CARTESIAN_POINT('Ctrl Pts',(19.0447034020989,7.96249867857266,6.35290740525968));
#94642=CARTESIAN_POINT('Ctrl Pts',(19.0303671439565,8.19229576213723,6.05648491838939));
#94643=CARTESIAN_POINT('Ctrl Pts',(19.0159394491088,8.40487491321349,5.74799131248794));
#94644=CARTESIAN_POINT('Ctrl Pts',(19.0055524005619,8.55791876294694,5.52589498353811));
#94645=CARTESIAN_POINT('Ctrl Pts',(18.9953172726759,8.70218781720836,5.29768840615742));
#94646=CARTESIAN_POINT('Ctrl Pts',(18.9852673388218,8.83701581138607,5.06402271675237));
#94647=CARTESIAN_POINT('Ctrl Pts',(18.9802364943451,8.90450866055792,4.94705321625779));
#94648=CARTESIAN_POINT('Ctrl Pts',(18.9752520388962,8.96963621777626,4.82871589318936));
#94649=CARTESIAN_POINT('Ctrl Pts',(18.9703179714697,9.03237656637081,4.70912775998958));
#94650=CARTESIAN_POINT('Ctrl Pts',(18.9617751113042,9.14100540713056,4.50207248265815));
#94651=CARTESIAN_POINT('Ctrl Pts',(18.9533225967343,9.242415344085,4.29124763660322));
#94652=CARTESIAN_POINT('Ctrl Pts',(18.944777313324,9.33632158440304,4.07713252975304));
#94653=CARTESIAN_POINT('Ctrl Pts',(18.9385277279412,9.40499982930891,3.92053963777375));
#94654=CARTESIAN_POINT('Ctrl Pts',(18.9322286104738,9.46966391058422,3.76218776214099));
#94655=CARTESIAN_POINT('Ctrl Pts',(18.9258092124385,9.53019546327616,3.602280621641));
#94656=CARTESIAN_POINT('Ctrl Pts',(18.9121976210768,9.65854562246522,3.26321601771301));
#94657=CARTESIAN_POINT('Ctrl Pts',(18.8985893188567,9.76890358393514,2.91729476422134));
#94658=CARTESIAN_POINT('Ctrl Pts',(18.8849695342091,9.86087135309376,2.56646304735015));
#94659=CARTESIAN_POINT('Ctrl Pts',(18.8713326158262,9.95295481801741,2.21518998299113));
#94660=CARTESIAN_POINT('Ctrl Pts',(18.8576841867703,10.0266019242977,1.85899313727757));
#94661=CARTESIAN_POINT('Ctrl Pts',(18.8440095841095,10.0813622058563,1.49981740195999));
#94662=CARTESIAN_POINT('Ctrl Pts',(18.8408455278202,10.0940327468269,1.41671061834878));
#94663=CARTESIAN_POINT('Ctrl Pts',(18.8376800709236,10.1056919125858,1.33344435017619));
#94664=CARTESIAN_POINT('Ctrl Pts',(18.8345130329549,10.1163337231934,1.25004270792199));
#94665=CARTESIAN_POINT('Ctrl Pts',(18.8214905737337,10.1600915012969,0.907105712539461));
#94666=CARTESIAN_POINT('Ctrl Pts',(18.8083373000925,10.1865317447387,0.561871096406014));
#94667=CARTESIAN_POINT('Ctrl Pts',(18.7951789993763,10.1953684639573,0.216188414535579));
#94668=CARTESIAN_POINT('Ctrl Pts',(18.7820567714032,10.2041809578062,-0.128546597662148));
#94669=CARTESIAN_POINT('Ctrl Pts',(18.7689295439125,10.1954871963454,-0.473726922080629));
#94670=CARTESIAN_POINT('Ctrl Pts',(18.7559203408355,10.1690199689852,-0.817567059789181));
#94671=CARTESIAN_POINT('Ctrl Pts',(18.7513969361009,10.1598171007662,-0.937123046242575));
#94672=CARTESIAN_POINT('Ctrl Pts',(18.7468877842316,10.148465489433,-1.05651745587199));
#94673=CARTESIAN_POINT('Ctrl Pts',(18.7423979944009,10.1349540741866,-1.17567670015723));
#94674=CARTESIAN_POINT('Ctrl Pts',(18.7423966095271,10.1349499065963,-1.17571345477601));
#94675=CARTESIAN_POINT('Ctrl Pts',(18.7423952246546,10.1349457387999,-1.17575020937153));
#94676=CARTESIAN_POINT('Ctrl Pts',(18.7423938397834,10.1349415707974,-1.17578696394395));
#94677=CARTESIAN_POINT('Ctrl Pts',(18.7293207128352,10.0955957997368,-1.5227486117345));
#94678=CARTESIAN_POINT('Ctrl Pts',(18.7163628972734,10.0378869685745,-1.86764796597857));
#94679=CARTESIAN_POINT('Ctrl Pts',(18.703411088082,9.96250064782994,-2.20873737228892));
#94680=CARTESIAN_POINT('Ctrl Pts',(18.6904833212053,9.88725426596347,-2.54919361772379));
#94681=CARTESIAN_POINT('Ctrl Pts',(18.6775615325368,9.79439528578715,-2.88585351530137));
#94682=CARTESIAN_POINT('Ctrl Pts',(18.6645392706148,9.68463728913615,-3.21693841612392));
#94683=CARTESIAN_POINT('Ctrl Pts',(18.6603209734357,9.649083416051,-3.32418664316367));
#94684=CARTESIAN_POINT('Ctrl Pts',(18.6560921506786,9.61175661398904,-3.43084959950089));
#94685=CARTESIAN_POINT('Ctrl Pts',(18.6518492277839,9.57268203809672,-3.53686607171212));
#94686=CARTESIAN_POINT('Ctrl Pts',(18.6381474504394,9.44649752991839,-3.87922772501948));
#94687=CARTESIAN_POINT('Ctrl Pts',(18.6244496581371,9.30225079458742,-4.21491485204093));
#94688=CARTESIAN_POINT('Ctrl Pts',(18.6107369118527,9.14080367032811,-4.54213068876285));
#94689=CARTESIAN_POINT('Ctrl Pts',(18.5970130610206,8.97922580659091,-4.86961150405186));
#94690=CARTESIAN_POINT('Ctrl Pts',(18.583274233299,8.80041916864338,-5.188608118226));
#94691=CARTESIAN_POINT('Ctrl Pts',(18.569501693905,8.60520333982285,-5.4972929078017));
#94692=CARTESIAN_POINT('Ctrl Pts',(18.5664378308966,8.56177528785086,-5.56596346164793));
#94693=CARTESIAN_POINT('Ctrl Pts',(18.5633723004489,8.5175350014068,-5.63412356014589));
#94694=CARTESIAN_POINT('Ctrl Pts',(18.560304897842,8.47249124519888,-5.70175284157591));
#94695=CARTESIAN_POINT('Ctrl Pts',(18.5451573471326,8.25005465348676,-6.03572203348332));
#94696=CARTESIAN_POINT('Ctrl Pts',(18.5300479666999,8.00805772463506,-6.35687179147185));
#94697=CARTESIAN_POINT('Ctrl Pts',(18.5149615377423,7.74768798431707,-6.66252915693987));
#94698=CARTESIAN_POINT('Ctrl Pts',(18.5097041125412,7.65695250024724,-6.76904679213579));
#94699=CARTESIAN_POINT('Ctrl Pts',(18.5044494775643,7.56398621837468,-6.87368306948572));
#94700=CARTESIAN_POINT('Ctrl Pts',(18.4991969987272,7.46884082764176,-6.97632527323337));
#94701=CARTESIAN_POINT('Ctrl Pts',(18.4842276610716,7.1976805765599,-7.2688511173695));
#94702=CARTESIAN_POINT('Ctrl Pts',(18.4692758071308,6.90881780322808,-7.54517844328599));
#94703=CARTESIAN_POINT('Ctrl Pts',(18.4543266982082,6.60466043780798,-7.80369363392125));
#94704=CARTESIAN_POINT('Ctrl Pts',(18.439392442126,6.30080527105759,-8.06195197413765));
#94705=CARTESIAN_POINT('Ctrl Pts',(18.4244609248482,5.98168662098567,-8.30243285908742));
#94706=CARTESIAN_POINT('Ctrl Pts',(18.4095178565894,5.64974343316438,-8.52356187903403));
#94707=CARTESIAN_POINT('Ctrl Pts',(18.3988128677656,5.41194433767359,-8.68197537525669));
#94708=CARTESIAN_POINT('Ctrl Pts',(18.3881019597623,5.1675644243093,-8.8304580363769));
#94709=CARTESIAN_POINT('Ctrl Pts',(18.3773800048889,4.91750920954781,-8.96844496388976));
#94710=CARTESIAN_POINT('Ctrl Pts',(18.3638173439019,4.60120363412619,-9.14299055194817));
#94711=CARTESIAN_POINT('Ctrl Pts',(18.3502497557113,4.27559261611256,-9.30089922915152));
#94712=CARTESIAN_POINT('Ctrl Pts',(18.3366746234865,3.94241652222267,-9.44101520914165));
#94713=CARTESIAN_POINT('Ctrl Pts',(18.3153574710193,3.41922709951646,-9.66104059519825));
#94714=CARTESIAN_POINT('Ctrl Pts',(18.2940216981756,2.87738122411373,-9.83718946395088));
#94715=CARTESIAN_POINT('Ctrl Pts',(18.2726580888735,2.32458303169984,-9.96772456439307));
#94716=CARTESIAN_POINT('Ctrl Pts',(18.250729396379,1.75716292016651,-10.1017124143325));
#94717=CARTESIAN_POINT('Ctrl Pts',(18.2287713755917,1.17820441143369,-10.1876408285472));
#94718=CARTESIAN_POINT('Ctrl Pts',(18.2067744407027,0.59607679853009,-10.2236697840988));
#94719=CARTESIAN_POINT('Ctrl Pts',(18.2024571223697,0.481823143279075,-10.2307411543196));
#94720=CARTESIAN_POINT('Ctrl Pts',(18.1981383061371,0.367447494538484,-10.2358904563959));
#94721=CARTESIAN_POINT('Ctrl Pts',(18.1938179211529,0.253013238920589,-10.2391039859528));
#94722=CARTESIAN_POINT('Ctrl Pts',(18.1869926579869,0.072232148197292,-10.2441806596746));
#94723=CARTESIAN_POINT('Ctrl Pts',(18.1801772901769,-0.108689414234473,
-10.2444430843383));
#94724=CARTESIAN_POINT('Ctrl Pts',(18.1733699101441,-0.28950481593069,-10.2398365230604));
#94725=CARTESIAN_POINT('Ctrl Pts',(18.1505110747668,-0.896673723967822,
-10.2243679249506));
#94726=CARTESIAN_POINT('Ctrl Pts',(18.1277421344973,-1.5026493854274,-10.1539963544201));
#94727=CARTESIAN_POINT('Ctrl Pts',(18.1049918601463,-2.09793712912939,-10.0310006372786));
#94728=CARTESIAN_POINT('Ctrl Pts',(18.0826179976676,-2.68337561252395,-9.91003993068066));
#94729=CARTESIAN_POINT('Ctrl Pts',(18.0602621798692,-3.25847588047912,-9.73818053721335));
#94730=CARTESIAN_POINT('Ctrl Pts',(18.0378589922131,-3.81416626982286,-9.51761782230471));
#94731=CARTESIAN_POINT('Ctrl Pts',(18.0287633782693,-4.03977457750649,-9.42807015007052));
#94732=CARTESIAN_POINT('Ctrl Pts',(18.0196599837846,-4.26218311516417,-9.33049500578815));
#94733=CARTESIAN_POINT('Ctrl Pts',(18.0105445400155,-4.48078356598075,-9.22504148541237));
#94734=CARTESIAN_POINT('Ctrl Pts',(18.0105443969714,-4.48078699636842,-9.22503983058296));
#94735=CARTESIAN_POINT('Ctrl Pts',(18.0105442539273,-4.48079042675514,-9.22503817575162));
#94736=CARTESIAN_POINT('Ctrl Pts',(18.0105441108832,-4.48079385714093,-9.22503652091832));
#94737=CARTESIAN_POINT('Ctrl Pts',(17.9947726209851,-4.85901491375055,-9.04258100869975));
#94738=CARTESIAN_POINT('Ctrl Pts',(17.9788511214764,-5.22592814798086,-8.83634109782422));
#94739=CARTESIAN_POINT('Ctrl Pts',(17.9628770807745,-5.57902035708451,-8.60833729963736));
#94740=CARTESIAN_POINT('Ctrl Pts',(17.9468726103616,-5.93278518835648,-8.3798991661546));
#94741=CARTESIAN_POINT('Ctrl Pts',(17.9308153584739,-6.27267695388216,-8.12961526102735));
#94742=CARTESIAN_POINT('Ctrl Pts',(17.914801353746,-6.5962127162598,-7.85949148218387));
#94743=CARTESIAN_POINT('Ctrl Pts',(17.9131347589807,-6.62988343243225,-7.83137940881668));
#94744=CARTESIAN_POINT('Ctrl Pts',(17.9114686310051,-6.66337703423234,-7.8030524221574));
#94745=CARTESIAN_POINT('Ctrl Pts',(17.9098030769116,-6.69669074562728,-7.77451275984648));
#94746=CARTESIAN_POINT('Ctrl Pts',(17.8965015877788,-6.96274152825989,-7.54658860561832));
#94747=CARTESIAN_POINT('Ctrl Pts',(17.8833189848059,-7.21737240451834,-7.30519034945689));
#94748=CARTESIAN_POINT('Ctrl Pts',(17.8702570945366,-7.45904810393093,-7.05150363832918));
#94749=CARTESIAN_POINT('Ctrl Pts',(17.862275778808,-7.60672122176878,-6.89649133184858));
#94750=CARTESIAN_POINT('Ctrl Pts',(17.8543395215989,-7.74955791441653,-6.73689169375406));
#94751=CARTESIAN_POINT('Ctrl Pts',(17.8464486327562,-7.88721516077749,-6.57298155457178));
#94752=CARTESIAN_POINT('Ctrl Pts',(17.8434686957871,-7.9392004219654,-6.5110820787215));
#94753=CARTESIAN_POINT('Ctrl Pts',(17.8404952281761,-7.99044708500258,-6.44856790943521));
#94754=CARTESIAN_POINT('Ctrl Pts',(17.8375282434978,-8.04094407617035,-6.38546053050246));
#94755=CARTESIAN_POINT('Ctrl Pts',(17.8256875700402,-8.24246799619445,-6.13361094321279));
#94756=CARTESIAN_POINT('Ctrl Pts',(17.8137158795033,-8.43175580671531,-5.87217915639835));
#94757=CARTESIAN_POINT('Ctrl Pts',(17.801679482491,-8.6082791557546,-5.60247192802518));
#94758=CARTESIAN_POINT('Ctrl Pts',(17.7896430854786,-8.78480250479389,-5.33276469965201));
#94759=CARTESIAN_POINT('Ctrl Pts',(17.7775419369184,-8.94856212650403,-5.05478186072294));
#94760=CARTESIAN_POINT('Ctrl Pts',(17.7654406557367,-9.09902413406252,-4.76977631388784));
#94761=CARTESIAN_POINT('Ctrl Pts',(17.7411908055945,-9.40053610462235,-4.1986515134074));
#94762=CARTESIAN_POINT('Ctrl Pts',(17.7166586862939,-9.64865843917535,-3.59854123922697));
#94763=CARTESIAN_POINT('Ctrl Pts',(17.6919981760056,-9.83778134329656,-2.97969614991501));
#94764=CARTESIAN_POINT('Ctrl Pts',(17.6889624280202,-9.8610626731826,-2.90351533649331));
#94765=CARTESIAN_POINT('Ctrl Pts',(17.6859247268684,-9.88344988947285,-2.82705055961025));
#94766=CARTESIAN_POINT('Ctrl Pts',(17.6828853537619,-9.90493248426554,-2.75032089323));
#94767=CARTESIAN_POINT('Ctrl Pts',(17.6769842082569,-9.94664237418528,-2.60134513079617));
#94768=CARTESIAN_POINT('Ctrl Pts',(17.6710767608705,-9.98494213149595,-2.4513708248295));
#94769=CARTESIAN_POINT('Ctrl Pts',(17.6651650595282,-10.0198195814703,-2.30055459795124));
#94770=CARTESIAN_POINT('Ctrl Pts',(17.6522973219507,-10.0957357767686,-1.97227961964137));
#94771=CARTESIAN_POINT('Ctrl Pts',(17.6396119481788,-10.1556767585313,-1.6401897808721));
#94772=CARTESIAN_POINT('Ctrl Pts',(17.6270298268239,-10.1994143540277,-1.30593710606664));
#94773=CARTESIAN_POINT('Ctrl Pts',(17.6153714576621,-10.239940829664,-0.996224541209333));
#94774=CARTESIAN_POINT('Ctrl Pts',(17.6038016807299,-10.2665555446432,-0.684655874297618));
#94775=CARTESIAN_POINT('Ctrl Pts',(17.592258525595,-10.2790961038348,-0.372580399566067));
#94776=CARTESIAN_POINT('Ctrl Pts',(17.5770275132283,-10.2956431752291,0.0391983004023063));
#94777=CARTESIAN_POINT('Ctrl Pts',(17.5617901530121,-10.2876170727355,0.45185830932181));
#94778=CARTESIAN_POINT('Ctrl Pts',(17.5464539621659,-10.2547463325197,0.862452069769172));
#94779=CARTESIAN_POINT('Ctrl Pts',(17.5376242304394,-10.2358211756363,1.09884928141659));
#94780=CARTESIAN_POINT('Ctrl Pts',(17.5287617958741,-10.2086600559606,1.33456068044002));
#94781=CARTESIAN_POINT('Ctrl Pts',(17.5198493665046,-10.1732095241468,1.56901604699944));
#94782=CARTESIAN_POINT('Ctrl Pts',(17.5198486089956,-10.1732065110404,1.56903597445689));
#94783=CARTESIAN_POINT('Ctrl Pts',(17.5198478514862,-10.1732034978741,1.56905590190525));
#94784=CARTESIAN_POINT('Ctrl Pts',(17.5198470939764,-10.173200484648,1.56907582934455));
#94785=CARTESIAN_POINT('Ctrl Pts',(17.5073558585623,-10.1235127845277,1.89767666268265));
#94786=CARTESIAN_POINT('Ctrl Pts',(17.4947058589523,-10.0574516897075,2.22385097079879));
#94787=CARTESIAN_POINT('Ctrl Pts',(17.4819881459334,-9.97568559399591,2.54614782892651));
#94788=CARTESIAN_POINT('Ctrl Pts',(17.4692759110215,-9.89395471872187,2.86830585889723));
#94789=CARTESIAN_POINT('Ctrl Pts',(17.4564959558442,-9.79653311063687,3.18659026499953));
#94790=CARTESIAN_POINT('Ctrl Pts',(17.4437376902098,-9.68405996070656,3.49959551421119));
#94791=CARTESIAN_POINT('Ctrl Pts',(17.435309506378,-9.60975954943429,3.70636858637299));
#94792=CARTESIAN_POINT('Ctrl Pts',(17.4268907678939,-9.52889003367656,3.91083872808492));
#94793=CARTESIAN_POINT('Ctrl Pts',(17.4185069695538,-9.44162666556968,4.11260939061742));
#94794=CARTESIAN_POINT('Ctrl Pts',(17.4056815386412,-9.30813224532637,4.42127565231723));
#94795=CARTESIAN_POINT('Ctrl Pts',(17.3929528110469,-9.1596979908372,4.72361317346604));
#94796=CARTESIAN_POINT('Ctrl Pts',(17.3803993074446,-8.99699031080038,5.01807797662169));
#94797=CARTESIAN_POINT('Ctrl Pts',(17.3716642666606,-8.88377425048699,5.22297392810165));
#94798=CARTESIAN_POINT('Ctrl Pts',(17.3630140391623,-8.76364774845,5.42405912621152));
#94799=CARTESIAN_POINT('Ctrl Pts',(17.3544741344264,-8.63683711837772,5.62082821221169));
#94800=CARTESIAN_POINT('Ctrl Pts',(17.3515975246203,-8.59412180558889,5.68710856308511));
#94801=CARTESIAN_POINT('Ctrl Pts',(17.3487334237889,-8.55064809122632,5.75289929874202));
#94802=CARTESIAN_POINT('Ctrl Pts',(17.3458827774153,-8.50643221126271,5.81818680387046));
#94803=CARTESIAN_POINT('Ctrl Pts',(17.333387457021,-8.31261947048099,6.10436340644308));
#94804=CARTESIAN_POINT('Ctrl Pts',(17.3206960069218,-8.1040504070193,6.38039507946295));
#94805=CARTESIAN_POINT('Ctrl Pts',(17.3078818058807,-7.88208910730421,6.64515211263132));
#94806=CARTESIAN_POINT('Ctrl Pts',(17.2966211407256,-7.68703739354777,6.87781119831359));
#94807=CARTESIAN_POINT('Ctrl Pts',(17.2852655739288,-7.48164344051485,7.10176455976691));
#94808=CARTESIAN_POINT('Ctrl Pts',(17.2738630253563,-7.26680488894806,7.31626338617272));
#94809=CARTESIAN_POINT('Ctrl Pts',(17.2601931479087,-7.0092469708878,7.573414026747));
#94810=CARTESIAN_POINT('Ctrl Pts',(17.246519862059,-6.73811367023367,7.81712741973527));
#94811=CARTESIAN_POINT('Ctrl Pts',(17.232838571973,-6.45474920951727,8.04604258360217));
#94812=CARTESIAN_POINT('Ctrl Pts',(17.2311296270908,-6.4193538453433,8.07463662665728));
#94813=CARTESIAN_POINT('Ctrl Pts',(17.2294205573127,-6.38376760392316,8.10299972063845));
#94814=CARTESIAN_POINT('Ctrl Pts',(17.2277113536755,-6.34799307482937,8.1311291639497));
#94815=CARTESIAN_POINT('Ctrl Pts',(17.2157248791348,-6.09710987235723,8.32839814275821));
#94816=CARTESIAN_POINT('Ctrl Pts',(17.2037337009365,-5.83700500887216,8.51414434313586));
#94817=CARTESIAN_POINT('Ctrl Pts',(17.1917362801185,-5.56867428550647,8.68737258916926));
#94818=CARTESIAN_POINT('Ctrl Pts',(17.1746250574966,-5.18596980147988,8.93443794823621));
#94819=CARTESIAN_POINT('Ctrl Pts',(17.157501125857,-4.78653121196277,9.1560375088926));
#94820=CARTESIAN_POINT('Ctrl Pts',(17.1403602309021,-4.37418424228961,9.35048218560049));
#94821=CARTESIAN_POINT('Ctrl Pts',(17.1232193359472,-3.96183727261646,9.54492686230837));
#94822=CARTESIAN_POINT('Ctrl Pts',(17.1060614790304,-3.53658299214965,9.71221603175966));
#94823=CARTESIAN_POINT('Ctrl Pts',(17.088882648315,-3.1022762544726,9.85070806374306));
#94824=CARTESIAN_POINT('Ctrl Pts',(17.0798919309307,-2.87497736543456,9.92318929021174));
#94825=CARTESIAN_POINT('Ctrl Pts',(17.0707785452362,-2.6451035355068,9.98762468745663));
#94826=CARTESIAN_POINT('Ctrl Pts',(17.0616638621188,-2.41324806760956,10.0439612834198));
#94827=CARTESIAN_POINT('Ctrl Pts',(17.0550977813797,-2.24622287294053,10.0845453205058));
#94828=CARTESIAN_POINT('Ctrl Pts',(17.0485309919751,-2.07816827881241,10.1209268635885));
#94829=CARTESIAN_POINT('Ctrl Pts',(17.0420084069395,-1.90928964157372,10.1530893845166));
#94830=CARTESIAN_POINT('Ctrl Pts',(17.0368192409607,-1.77493504533108,10.178676886785));
#94831=CARTESIAN_POINT('Ctrl Pts',(17.0316753337053,-1.64006844984146,10.2016195926033));
#94832=CARTESIAN_POINT('Ctrl Pts',(17.0265606532138,-1.50478892215686,10.2218482631423));
#94833=CARTESIAN_POINT('Ctrl Pts',(17.0169201874437,-1.24980571094689,10.2599765110806));
#94834=CARTESIAN_POINT('Ctrl Pts',(17.0073834009016,-0.993352406314393,
10.2884619906838));
#94835=CARTESIAN_POINT('Ctrl Pts',(16.9978442181521,-0.736177067748153,
10.3072445951958));
#94836=CARTESIAN_POINT('Ctrl Pts',(16.9896563520273,-0.515433079705401,
10.3233664638358));
#94837=CARTESIAN_POINT('Ctrl Pts',(16.9814667573228,-0.294158037725752,
10.332339608172));
#94838=CARTESIAN_POINT('Ctrl Pts',(16.973209772397,-0.0728546445390353,
10.3341336755772));
#94839=CARTESIAN_POINT('Ctrl Pts',(16.9607343221617,0.261511894023068,10.336844325873));
#94840=CARTESIAN_POINT('Ctrl Pts',(16.9482197472632,0.595934418746781,10.3233565855621));
#94841=CARTESIAN_POINT('Ctrl Pts',(16.9356858030079,0.92896255063804,10.2939768071048));
#94842=CARTESIAN_POINT('Ctrl Pts',(16.9251316367267,1.20938778699667,10.2692376618822));
#94843=CARTESIAN_POINT('Ctrl Pts',(16.9145637222918,1.48882505774369,10.2332295968734));
#94844=CARTESIAN_POINT('Ctrl Pts',(16.9039935118895,1.76641698560807,10.1861081975525));
#94845=CARTESIAN_POINT('Ctrl Pts',(16.8906069793433,2.11797038289025,10.1264317936188));
#94846=CARTESIAN_POINT('Ctrl Pts',(16.8771989382669,2.46670015958735,10.0488841547053));
#94847=CARTESIAN_POINT('Ctrl Pts',(16.8637111621511,2.8106670883483,9.95360013039481));
#94848=CARTESIAN_POINT('Ctrl Pts',(16.8502653922987,3.15356276820557,9.85861285817887));
#94849=CARTESIAN_POINT('Ctrl Pts',(16.836740438657,3.49172508490791,9.74599881830258));
#94850=CARTESIAN_POINT('Ctrl Pts',(16.8230795479737,3.82318234957965,9.61590290219076));
#94851=CARTESIAN_POINT('Ctrl Pts',(16.8188828865038,3.92500689117315,9.5759370953336));
#94852=CARTESIAN_POINT('Ctrl Pts',(16.814673399183,4.02619830248631,9.53432158410991));
#94853=CARTESIAN_POINT('Ctrl Pts',(16.8104494423104,4.12669850269955,9.49106093869667));
#94854=CARTESIAN_POINT('Ctrl Pts',(16.7998612020997,4.37862348516496,9.38261899217268));
#94855=CARTESIAN_POINT('Ctrl Pts',(16.7894225580707,4.62632461651229,9.26421710021958));
#94856=CARTESIAN_POINT('Ctrl Pts',(16.779164157344,4.86888897051797,9.13605335050842));
#94857=CARTESIAN_POINT('Ctrl Pts',(16.7740341448704,4.99019035022373,9.07196132951896));
#94858=CARTESIAN_POINT('Ctrl Pts',(16.7689491755291,5.11020755854454,9.00542848872651));
#94859=CARTESIAN_POINT('Ctrl Pts',(16.763912847087,5.22886012688302,8.93654589424496));
#94860=CARTESIAN_POINT('Ctrl Pts',(16.7561547036587,5.41163685677494,8.83043664147353));
#94861=CARTESIAN_POINT('Ctrl Pts',(16.7484773850953,5.59114098951574,8.71870478050094));
#94862=CARTESIAN_POINT('Ctrl Pts',(16.7407503797405,5.7669795739698,8.60146812722601));
#94863=CARTESIAN_POINT('Ctrl Pts',(16.7334306293306,5.93355051465727,8.49041047921498));
#94864=CARTESIAN_POINT('Ctrl Pts',(16.7260663875089,6.096831513901,8.37441282019649));
#94865=CARTESIAN_POINT('Ctrl Pts',(16.7185490576543,6.25645321374314,8.25360003215423));
#94866=CARTESIAN_POINT('Ctrl Pts',(16.7050907291846,6.54222506477346,8.03730804866381));
#94867=CARTESIAN_POINT('Ctrl Pts',(16.6916366227093,6.81683913927164,7.80621957500194));
#94868=CARTESIAN_POINT('Ctrl Pts',(16.678178118772,7.07903371690306,7.56169564596312));
#94869=CARTESIAN_POINT('Ctrl Pts',(16.6646383037058,7.34281237380756,7.3156943969459));
#94870=CARTESIAN_POINT('Ctrl Pts',(16.6510940379693,7.5940216671676,7.05609418330936));
#94871=CARTESIAN_POINT('Ctrl Pts',(16.6375366443296,7.83134159126811,6.78424238248881));
#94872=CARTESIAN_POINT('Ctrl Pts',(16.6336236717245,7.89983752686763,6.70577976072541));
#94873=CARTESIAN_POINT('Ctrl Pts',(16.6297096061469,7.9671761768322,6.62629633588331));
#94874=CARTESIAN_POINT('Ctrl Pts',(16.6257942404647,8.03332514219299,6.54582403594911));
#94875=CARTESIAN_POINT('Ctrl Pts',(16.6137509363714,8.23679326495746,6.29829865572819));
#94876=CARTESIAN_POINT('Ctrl Pts',(16.6016014173788,8.42887435709483,6.04131725621301));
#94877=CARTESIAN_POINT('Ctrl Pts',(16.5894318446657,8.60865950196754,5.77600887199669));
#94878=CARTESIAN_POINT('Ctrl Pts',(16.5772785966527,8.78820347661546,5.51105638193783));
#94879=CARTESIAN_POINT('Ctrl Pts',(16.565105327834,8.95548506186407,5.23779982601913));
#94880=CARTESIAN_POINT('Ctrl Pts',(16.5529962083458,9.10963578220361,4.9573272331238));
#94881=CARTESIAN_POINT('Ctrl Pts',(16.546054400568,9.19800592921988,4.79654041218904));
#94882=CARTESIAN_POINT('Ctrl Pts',(16.5391336504345,9.28206138381152,4.633381391311));
#94883=CARTESIAN_POINT('Ctrl Pts',(16.5322495270048,9.3616427939792,4.4680487041676));
#94884=CARTESIAN_POINT('Ctrl Pts',(16.5322421302684,9.3617283012663,4.46787106029931));
#94885=CARTESIAN_POINT('Ctrl Pts',(16.5322347335515,9.36181380333707,4.46769341393065));
#94886=CARTESIAN_POINT('Ctrl Pts',(16.5322273368541,9.36189930019134,4.46751576506169));
#94887=CARTESIAN_POINT('Ctrl Pts',(16.5170311457259,9.53754884622812,4.10254393712876));
#94888=CARTESIAN_POINT('Ctrl Pts',(16.5019172397916,9.69118368878955,3.72701619034863));
#94889=CARTESIAN_POINT('Ctrl Pts',(16.4868192787626,9.82235262384252,3.34363337215857));
#94890=CARTESIAN_POINT('Ctrl Pts',(16.4717015541957,9.95369326169836,2.95974869806468));
#94891=CARTESIAN_POINT('Ctrl Pts',(16.4565997965269,10.0625082017002,2.56798774771891));
#94892=CARTESIAN_POINT('Ctrl Pts',(16.4414497127382,10.148314464651,2.17110439390891));
#94893=CARTESIAN_POINT('Ctrl Pts',(16.4306934647361,10.2092351471575,1.88932537267978));
#94894=CARTESIAN_POINT('Ctrl Pts',(16.4199129149323,10.2585571610524,1.60496520114311));
#94895=CARTESIAN_POINT('Ctrl Pts',(16.4090857225671,10.2961025663235,1.31902458207523));
#94896=CARTESIAN_POINT('Ctrl Pts',(16.3935638465982,10.3499277043803,0.909099767406544));
#94897=CARTESIAN_POINT('Ctrl Pts',(16.3780342325787,10.3797334643755,0.495806927140564));
#94898=CARTESIAN_POINT('Ctrl Pts',(16.3624725822917,10.3850267082106,0.0821820927440673));
#94899=CARTESIAN_POINT('Ctrl Pts',(16.347062775554,10.390268302965,-0.327406777482861));
#94900=CARTESIAN_POINT('Ctrl Pts',(16.3316215680962,10.3714728916886,-0.737320326153107));
#94901=CARTESIAN_POINT('Ctrl Pts',(16.3161261538691,10.3282038630816,-1.14458308412128));
#94902=CARTESIAN_POINT('Ctrl Pts',(16.3056238364201,10.2988774399556,-1.42061331517058));
#94903=CARTESIAN_POINT('Ctrl Pts',(16.2950966355493,10.2583094116598,-1.69542527755611));
#94904=CARTESIAN_POINT('Ctrl Pts',(16.2845375939976,10.2063769096049,-1.96808849315878));
#94905=CARTESIAN_POINT('Ctrl Pts',(16.2845327402885,10.2063530376221,-1.96821382914944));
#94906=CARTESIAN_POINT('Ctrl Pts',(16.2845278865727,10.2063291632382,-1.968339164686));
#94907=CARTESIAN_POINT('Ctrl Pts',(16.2845230328501,10.2063052864533,-1.96846449976846));
#94908=CARTESIAN_POINT('Ctrl Pts',(16.2675935855644,10.123024718359,-2.40562456484032));
#94909=CARTESIAN_POINT('Ctrl Pts',(16.2506612866968,10.0106855389608,-2.83726190886183));
#94910=CARTESIAN_POINT('Ctrl Pts',(16.233745990735,9.87114738724374,-3.26013776798451));
#94911=CARTESIAN_POINT('Ctrl Pts',(16.216491482196,9.72881099326279,-3.69149381038911));
#94912=CARTESIAN_POINT('Ctrl Pts',(16.1992546745454,9.55817403403809,-4.1137343165391));
#94913=CARTESIAN_POINT('Ctrl Pts',(16.1820559763094,9.36115909406157,-4.52343959234944));
#94914=CARTESIAN_POINT('Ctrl Pts',(16.164890733688,9.16452739564169,-4.93234789262239));
#94915=CARTESIAN_POINT('Ctrl Pts',(16.1477634692771,8.94162021511415,-5.3287707485719));
#94916=CARTESIAN_POINT('Ctrl Pts',(16.130693624495,8.69429725958992,-5.70931127112533));
#94917=CARTESIAN_POINT('Ctrl Pts',(16.1141347970773,8.45437837402047,-6.0784596095459));
#94918=CARTESIAN_POINT('Ctrl Pts',(16.0976300219097,8.19148340162108,-6.43266330773966));
#94919=CARTESIAN_POINT('Ctrl Pts',(16.0811959875537,7.9072640299243,-6.76880915533248));
#94920=CARTESIAN_POINT('Ctrl Pts',(16.0658638493284,7.64210146552994,-7.08241654397072));
#94921=CARTESIAN_POINT('Ctrl Pts',(16.0505932952338,7.35837773213623,-7.38030705297337));
#94922=CARTESIAN_POINT('Ctrl Pts',(16.0353967360999,7.05739941319241,-7.65993078023443));
#94923=CARTESIAN_POINT('Ctrl Pts',(16.0353826375841,7.05712018237657,-7.66019019945693));
#94924=CARTESIAN_POINT('Ctrl Pts',(16.0353685391679,7.05684093680483,-7.66044960295446));
#94925=CARTESIAN_POINT('Ctrl Pts',(16.0353544408512,7.05656167647816,-7.66070899072457));
#94926=CARTESIAN_POINT('Ctrl Pts',(16.0247062135628,6.84564093307695,-7.85662031816399));
#94927=CARTESIAN_POINT('Ctrl Pts',(16.0141145376293,6.62629924338843,-8.04356174782181));
#94928=CARTESIAN_POINT('Ctrl Pts',(16.0035064641038,6.39938093475859,-8.22098427349818));
#94929=CARTESIAN_POINT('Ctrl Pts',(15.9929182041099,6.17288645926429,-8.39807541319768));
#94930=CARTESIAN_POINT('Ctrl Pts',(15.9823136262558,5.9388434237568,-8.56568254415566));
#94931=CARTESIAN_POINT('Ctrl Pts',(15.9716228343142,5.69814046512725,-8.7232431399173));
#94932=CARTESIAN_POINT('Ctrl Pts',(15.9656811223411,5.56436294340201,-8.81081192653526));
#94933=CARTESIAN_POINT('Ctrl Pts',(15.9597128284198,5.42852913428555,-8.8952771974175));
#94934=CARTESIAN_POINT('Ctrl Pts',(15.9537062016035,5.29079848157823,-8.97654131976764));
#94935=CARTESIAN_POINT('Ctrl Pts',(15.9372437511037,4.91331805507004,-9.19926309565096));
#94936=CARTESIAN_POINT('Ctrl Pts',(15.9207847232432,4.52189152109994,-9.39845519891271));
#94937=CARTESIAN_POINT('Ctrl Pts',(15.9043256130699,4.11966267623208,-9.57279360603444));
#94938=CARTESIAN_POINT('Ctrl Pts',(15.8931339644216,3.84616041149253,-9.69133793667424));
#94939=CARTESIAN_POINT('Ctrl Pts',(15.8819422773134,3.56766274531486,-9.79839028808058));
#94940=CARTESIAN_POINT('Ctrl Pts',(15.8707494446982,3.28515006290952,-9.89352326144506));
#94941=CARTESIAN_POINT('Ctrl Pts',(15.8542197930833,2.86793340494329,-10.0340162859408));
#94942=CARTESIAN_POINT('Ctrl Pts',(15.8376603167854,2.44177297052336,-10.148525138475));
#94943=CARTESIAN_POINT('Ctrl Pts',(15.8210904408439,2.01002203189374,-10.235577364366));
#94944=CARTESIAN_POINT('Ctrl Pts',(15.8099406797445,1.71949965036582,-10.2941542375593));
#94945=CARTESIAN_POINT('Ctrl Pts',(15.7987861972866,1.42644628402294,-10.3403001921712));
#94946=CARTESIAN_POINT('Ctrl Pts',(15.7876327631621,1.13188391954781,-10.3735799091102));
#94947=CARTESIAN_POINT('Ctrl Pts',(15.771130668305,0.696063343958851,-10.422819007994));
#94948=CARTESIAN_POINT('Ctrl Pts',(15.7546308957414,0.256940656409019,-10.4438908172818));
#94949=CARTESIAN_POINT('Ctrl Pts',(15.7381516557369,-0.181833886135203,
-10.437269986716));
#94950=CARTESIAN_POINT('Ctrl Pts',(15.726937850918,-0.48041149518777,-10.43276463928));
#94951=CARTESIAN_POINT('Ctrl Pts',(15.7157335424594,-0.778828137337496,
-10.4154371764929));
#94952=CARTESIAN_POINT('Ctrl Pts',(15.7045443026975,-1.07594033927089,-10.3854492430376));
#94953=CARTESIAN_POINT('Ctrl Pts',(15.6907228568828,-1.44294652443974,-10.3484068160121));
#94954=CARTESIAN_POINT('Ctrl Pts',(15.6768856301063,-1.80819298526913,-10.2919584362545));
#94955=CARTESIAN_POINT('Ctrl Pts',(15.6630372227924,-2.16952225816341,-10.2163385634445));
#94956=CARTESIAN_POINT('Ctrl Pts',(15.6446444371282,-2.64942234486199,-10.1159039011018));
#94957=CARTESIAN_POINT('Ctrl Pts',(15.6262319401275,-3.12241154657823,-9.98164920097705));
#94958=CARTESIAN_POINT('Ctrl Pts',(15.6078102070798,-3.58380281291204,-9.81505615852526));
#94959=CARTESIAN_POINT('Ctrl Pts',(15.5893310518789,-4.04663227617918,-9.64794383098888));
#94960=CARTESIAN_POINT('Ctrl Pts',(15.5708426027203,-4.49779029758976,-9.44829177668541));
#94961=CARTESIAN_POINT('Ctrl Pts',(15.5523551122187,-4.93256648390252,-9.21764286844699));
#94962=CARTESIAN_POINT('Ctrl Pts',(15.5476710210738,-5.04272374316576,-9.1592044065821));
#94963=CARTESIAN_POINT('Ctrl Pts',(15.5429869898688,-5.15182953511281,-9.09877634468125));
#94964=CARTESIAN_POINT('Ctrl Pts',(15.5383031820876,-5.25980758410986,-9.03638419374356));
#94965=CARTESIAN_POINT('Ctrl Pts',(15.5382992206031,-5.2598989100963,-9.03633142352976));
#94966=CARTESIAN_POINT('Ctrl Pts',(15.5382952591187,-5.25999023527604,-9.03627865191097));
#94967=CARTESIAN_POINT('Ctrl Pts',(15.5382912976346,-5.26008155964901,-9.0362258788872));
#94968=CARTESIAN_POINT('Ctrl Pts',(15.5171750148634,-5.74687671076682,-8.75492471862091));
#94969=CARTESIAN_POINT('Ctrl Pts',(15.4960560699421,-6.21070130947555,-8.43371373452666));
#94970=CARTESIAN_POINT('Ctrl Pts',(15.474932053349,-6.64612860392156,-8.07752024759905));
#94971=CARTESIAN_POINT('Ctrl Pts',(15.4534657601675,-7.08861121231323,-7.71555528766612));
#94972=CARTESIAN_POINT('Ctrl Pts',(15.4319942296936,-7.50176993470843,-7.31746417752711));
#94973=CARTESIAN_POINT('Ctrl Pts',(15.4105149040284,-7.87988533001615,-6.88837076383642));
#94974=CARTESIAN_POINT('Ctrl Pts',(15.3975983738548,-8.10726392600793,-6.63033668438587));
#94975=CARTESIAN_POINT('Ctrl Pts',(15.3846790242293,-8.3219696627552,-6.36109075811446));
#94976=CARTESIAN_POINT('Ctrl Pts',(15.3717562937892,-8.52275198993461,-6.08174115861502));
#94977=CARTESIAN_POINT('Ctrl Pts',(15.3717550334894,-8.52277157139504,-6.0817139148172));
#94978=CARTESIAN_POINT('Ctrl Pts',(15.3717537731895,-8.52279115272298,-6.08168667092321));
#94979=CARTESIAN_POINT('Ctrl Pts',(15.3717525128895,-8.5228107339184,-6.08165942693309));
#94980=CARTESIAN_POINT('Ctrl Pts',(15.3467310365703,-8.91156771833097,-5.54076847442808));
#94981=CARTESIAN_POINT('Ctrl Pts',(15.3216830068258,-9.24809282431701,-4.96197684085428));
#94982=CARTESIAN_POINT('Ctrl Pts',(15.2966257752012,-9.52733228393928,-4.35651691105738));
#94983=CARTESIAN_POINT('Ctrl Pts',(15.2712591734181,-9.81001938523021,-3.74358164491119));
#94984=CARTESIAN_POINT('Ctrl Pts',(15.2458831434973,-10.033997612566,-3.10331726827767));
#94985=CARTESIAN_POINT('Ctrl Pts',(15.220514661223,-10.1940753908267,-2.44737864135056));
#94986=CARTESIAN_POINT('Ctrl Pts',(15.2153027494342,-10.2269630997016,-2.31261715954723));
#94987=CARTESIAN_POINT('Ctrl Pts',(15.2100911527011,-10.2571538033918,-2.17719403680014));
#94988=CARTESIAN_POINT('Ctrl Pts',(15.2048800126993,-10.284602740453,-2.04121024681705));
#94989=CARTESIAN_POINT('Ctrl Pts',(15.2048778801433,-10.2846139733877,-2.04115459813993));
#94990=CARTESIAN_POINT('Ctrl Pts',(15.2048757475874,-10.2846252058633,-2.04109894936894));
#94991=CARTESIAN_POINT('Ctrl Pts',(15.2048736150315,-10.2846364378797,-2.04104330050404));
#94992=CARTESIAN_POINT('Ctrl Pts',(15.1746996600235,-10.4435604621839,-1.25365649080174));
#94993=CARTESIAN_POINT('Ctrl Pts',(15.1445280227636,-10.5105303001057,-0.447479827685317));
#94994=CARTESIAN_POINT('Ctrl Pts',(15.1143457843457,-10.4858083682396,0.356187421247338));
#94995=CARTESIAN_POINT('Ctrl Pts',(15.0888798080307,-10.4649494735928,1.0342740112203));
#94996=CARTESIAN_POINT('Ctrl Pts',(15.0634062998675,-10.3788140387298,1.71057487855672));
#94997=CARTESIAN_POINT('Ctrl Pts',(15.0379180035962,-10.2275328575131,2.37228587195548));
#94998=CARTESIAN_POINT('Ctrl Pts',(15.0379163092748,-10.2275228011743,2.37232985885346));
#94999=CARTESIAN_POINT('Ctrl Pts',(15.0379146149534,-10.2275127445477,2.37237384568694));
#95000=CARTESIAN_POINT('Ctrl Pts',(15.0379129206319,-10.2275026876333,2.37241783245596));
#95001=CARTESIAN_POINT('Ctrl Pts',(15.0014002445382,-10.0107758993464,3.32033393562414));
#95002=CARTESIAN_POINT('Ctrl Pts',(14.9648672981753,-9.66037793399265,4.23831865808117));
#95003=CARTESIAN_POINT('Ctrl Pts',(14.9283181376167,-9.19199335040588,5.09164640273109));
#95004=CARTESIAN_POINT('Ctrl Pts',(14.9091157361511,-8.9459108501002,5.53997248420801));
#95005=CARTESIAN_POINT('Ctrl Pts',(14.8899088549882,-8.66726141839536,5.97045145954754));
#95006=CARTESIAN_POINT('Ctrl Pts',(14.8706980550175,-8.35832468417983,6.37805012061861));
#95007=CARTESIAN_POINT('Ctrl Pts',(14.8706952732979,-8.35827995021,6.37810914081331));
#95008=CARTESIAN_POINT('Ctrl Pts',(14.8706924915783,-8.35823521560515,6.37816816052829));
#95009=CARTESIAN_POINT('Ctrl Pts',(14.8706897098586,-8.35819048036528,6.37822717976354));
#95010=CARTESIAN_POINT('Ctrl Pts',(14.8215160136613,-7.56738574854429,7.42153645083545));
#95011=CARTESIAN_POINT('Ctrl Pts',(14.7723101054862,-6.57812722396956,8.31492006499422));
#95012=CARTESIAN_POINT('Ctrl Pts',(14.7230696429686,-5.45991725204736,8.99943735221583));
#95013=CARTESIAN_POINT('Ctrl Pts',(14.7164572422931,-5.30975512936079,9.09135977416325));
#95014=CARTESIAN_POINT('Ctrl Pts',(14.7098442193276,-5.15726760390441,9.17951573392545));
#95015=CARTESIAN_POINT('Ctrl Pts',(14.703230569178,-5.00262299218413,9.26376257707146));
#95016=CARTESIAN_POINT('Ctrl Pts',(14.7032289667057,-5.00258552214691,9.26378298988968));
#95017=CARTESIAN_POINT('Ctrl Pts',(14.7032273642332,-5.0025480519831,9.26380340247838));
#95018=CARTESIAN_POINT('Ctrl Pts',(14.7032257617608,-5.0025105816926,9.26382381483761));
#95019=CARTESIAN_POINT('Ctrl Pts',(14.669244157884,-4.20792557978978,9.696682868843));
#95020=CARTESIAN_POINT('Ctrl Pts',(14.635240371231,-3.35638823792469,10.0263304665229));
#95021=CARTESIAN_POINT('Ctrl Pts',(14.6012204808335,-2.47697562262436,10.2427935754682));
#95022=CARTESIAN_POINT('Ctrl Pts',(14.5793124068725,-1.91065290985073,10.3821911380463));
#95023=CARTESIAN_POINT('Ctrl Pts',(14.5573976373706,-1.33276908367124,10.4746496677617));
#95024=CARTESIAN_POINT('Ctrl Pts',(14.5354776096679,-0.751083147259138,
10.5174961589306));
#95025=CARTESIAN_POINT('Ctrl Pts',(14.5354752857554,-0.751021478212826,
10.5175007014201));
#95026=CARTESIAN_POINT('Ctrl Pts',(14.5354729618429,-0.750959809123862,
10.517505243352));
#95027=CARTESIAN_POINT('Ctrl Pts',(14.5354706379304,-0.750898139992239,
10.5175097847264));
#95028=CARTESIAN_POINT('Ctrl Pts',(14.4977727039571,0.249483258113779,10.5911788369562));
#95029=CARTESIAN_POINT('Ctrl Pts',(14.4600691123741,1.26109171283965,10.5181313904752));
#95030=CARTESIAN_POINT('Ctrl Pts',(14.4223521457816,2.243651747854,10.307475847821));
#95031=CARTESIAN_POINT('Ctrl Pts',(14.3839984443421,3.24279928366774,10.0932640349567));
#95032=CARTESIAN_POINT('Ctrl Pts',(14.3456309067135,4.21190728518531,9.73675766133124));
#95033=CARTESIAN_POINT('Ctrl Pts',(14.3072425487459,5.10859782900886,9.24757723114086));
#95034=CARTESIAN_POINT('Ctrl Pts',(14.2993282970171,5.29346207073116,9.14672641932464));
#95035=CARTESIAN_POINT('Ctrl Pts',(14.2914131642866,5.47524831837985,9.04023672261371));
#95036=CARTESIAN_POINT('Ctrl Pts',(14.2834970954803,5.65358523092099,8.92819272516899));
#95037=CARTESIAN_POINT('Ctrl Pts',(14.2834970378564,5.65358652909998,8.92819190956014));
#95038=CARTESIAN_POINT('Ctrl Pts',(14.2834969802325,5.65358782727877,8.92819109395101));
#95039=CARTESIAN_POINT('Ctrl Pts',(14.2834969226085,5.65358912545739,8.92819027834158));
#95040=CARTESIAN_POINT('Ctrl Pts',(14.2310050134086,6.8361511516281,8.18521952881629));
#95041=CARTESIAN_POINT('Ctrl Pts',(14.1784678415063,7.86707443414694,7.19799366623765));
#95042=CARTESIAN_POINT('Ctrl Pts',(14.125894307937,8.67403110736602,6.05305298708846));
#95043=CARTESIAN_POINT('Ctrl Pts',(14.0942621071495,9.15955707035689,5.36417036890058));
#95044=CARTESIAN_POINT('Ctrl Pts',(14.062616708956,9.56400502859731,4.6181920265712));
#95045=CARTESIAN_POINT('Ctrl Pts',(14.030959744161,9.87162305591945,3.83395878718145));
#95046=CARTESIAN_POINT('Ctrl Pts',(14.0309595161733,9.87162527132882,3.83395313927558));
#95047=CARTESIAN_POINT('Ctrl Pts',(14.0309592881856,9.87162748673317,3.83394749136769));
#95048=CARTESIAN_POINT('Ctrl Pts',(14.0309590601978,9.8716297021325,3.83394184345784));
#95049=CARTESIAN_POINT('Ctrl Pts',(13.9708935521266,10.4552974463881,2.34594698595516));
#95050=CARTESIAN_POINT('Ctrl Pts',(13.9107899888404,10.6903708731197,0.720259109315623));
#95051=CARTESIAN_POINT('Ctrl Pts',(13.8506391863266,10.5665434814408,-0.876732594070744));
#95052=CARTESIAN_POINT('Ctrl Pts',(13.8263984315185,10.5166410808947,-1.52031975657813));
#95053=CARTESIAN_POINT('Ctrl Pts',(13.8021500272319,10.4084495920086,-2.15924596122222));
#95054=CARTESIAN_POINT('Ctrl Pts',(13.777893464215,10.2412934788638,-2.78261871014446));
#95055=CARTESIAN_POINT('Ctrl Pts',(13.7778934103748,10.2412931078421,-2.78262009378993));
#95056=CARTESIAN_POINT('Ctrl Pts',(13.7778933565347,10.2412927368201,-2.78262147743535));
#95057=CARTESIAN_POINT('Ctrl Pts',(13.7778933026945,10.2412923657979,-2.78262286108066));
#95058=CARTESIAN_POINT('Ctrl Pts',(13.7049944159232,9.73893291691786,-4.65606116753667));
#95059=CARTESIAN_POINT('Ctrl Pts',(13.6320253888064,8.70401339334478,-6.38903511110609));
#95060=CARTESIAN_POINT('Ctrl Pts',(13.5589900344303,7.29765576143082,-7.73099682974251));
#95061=CARTESIAN_POINT('Ctrl Pts',(13.5474207740948,7.07487985095129,-7.94357202179451));
#95062=CARTESIAN_POINT('Ctrl Pts',(13.5358498473615,6.84278367381023,-8.14633580197754));
#95063=CARTESIAN_POINT('Ctrl Pts',(13.5242772670359,6.60200771009854,-8.33829239537025));
#95064=CARTESIAN_POINT('Ctrl Pts',(13.524277150712,6.60200528989507,-8.33829432485693));
#95065=CARTESIAN_POINT('Ctrl Pts',(13.5242770343881,6.60200286969076,-8.33829625434248));
#95066=CARTESIAN_POINT('Ctrl Pts',(13.5242769180642,6.60200044948554,-8.33829818382697));
#95067=CARTESIAN_POINT('Ctrl Pts',(13.4396479365417,4.84123157000304,-9.74205362168631));
#95068=CARTESIAN_POINT('Ctrl Pts',(13.3549284631214,2.61628154009548,-10.5678525763947));
#95069=CARTESIAN_POINT('Ctrl Pts',(13.2701176421097,0.361346148799453,-10.6519993370047));
#95070=CARTESIAN_POINT('Ctrl Pts',(13.2701176136022,0.361345390846792,-10.651999365289));
#95071=CARTESIAN_POINT('Ctrl Pts',(13.2701175850947,0.361344632894097,-10.6519993935732));
#95072=CARTESIAN_POINT('Ctrl Pts',(13.2701175565871,0.361343874941429,-10.6519994218574));
#95073=CARTESIAN_POINT('Ctrl Pts',(13.1853067394119,-1.89359143287809,-10.7361456800139));
#95074=CARTESIAN_POINT('Ctrl Pts',(13.100405505491,-4.17851204919358,-10.0786394971838));
#95075=CARTESIAN_POINT('Ctrl Pts',(13.0154126752357,-6.04716707214536,-8.80437263473603));
#95076=CARTESIAN_POINT('Ctrl Pts',(13.0154126427607,-6.04716778613988,-8.80437214785132));
#95077=CARTESIAN_POINT('Ctrl Pts',(13.0154126102858,-6.04716850013435,-8.80437166096652));
#95078=CARTESIAN_POINT('Ctrl Pts',(13.0154125778109,-6.04716921412875,-8.80437117408163));
#95079=CARTESIAN_POINT('Ctrl Pts',(12.9304197333074,-7.91582423070209,-7.53010362774895));
#95080=CARTESIAN_POINT('Ctrl Pts',(12.8453353201699,-9.36821421426481,-5.63907631050066));
#95081=CARTESIAN_POINT('Ctrl Pts',(12.7601592286344,-10.115835605735,-3.50019255496931));
#95082=CARTESIAN_POINT('Ctrl Pts',(12.7601592102983,-10.1158357666775,-3.50019209452601));
#95083=CARTESIAN_POINT('Ctrl Pts',(12.7601591919622,-10.11583592762,-3.50019163408269));
#95084=CARTESIAN_POINT('Ctrl Pts',(12.7601591736261,-10.1158360885624,-3.50019117363937));
#95085=CARTESIAN_POINT('Ctrl Pts',(12.674983063715,-10.8634573375402,-1.36130685095101));
#95086=CARTESIAN_POINT('Ctrl Pts',(12.5897152272118,-10.9063092390295,1.02543387185629));
#95087=CARTESIAN_POINT('Ctrl Pts',(12.5043551624473,-10.2388599315667,3.19702913316979));
#95088=CARTESIAN_POINT('Ctrl Pts',(12.4474484526043,-9.79389372659145,4.64475930737875));
#95089=CARTESIAN_POINT('Ctrl Pts',(12.3905007264825,-9.03323813748135,5.99686930213596));
#95090=CARTESIAN_POINT('Ctrl Pts',(12.3335121832258,-8.02849753094572,7.13448234478132));
#95091=CARTESIAN_POINT('Ctrl Pts',(12.2765236756013,-7.02375755262432,8.27209467613394));
#95092=CARTESIAN_POINT('Ctrl Pts',(12.2194943956609,-5.77493250040647,9.19520997384836));
#95093=CARTESIAN_POINT('Ctrl Pts',(12.1624238991661,-4.39051675511366,9.81981072751928));
#95094=CARTESIAN_POINT('Ctrl Pts',(12.1624238634828,-4.39051588950701,9.81981111805122));
#95095=CARTESIAN_POINT('Ctrl Pts',(12.1624238277994,-4.39051502390029,9.81981150858305));
#95096=CARTESIAN_POINT('Ctrl Pts',(12.1624237921161,-4.39051415829352,9.81981189911476));
#95097=CARTESIAN_POINT('Ctrl Pts',(12.1053532598864,-3.00609737783877,10.4444126700251));
#95098=CARTESIAN_POINT('Ctrl Pts',(12.0482416553095,-1.48609015210989,10.7705020422654));
#95099=CARTESIAN_POINT('Ctrl Pts',(11.9910889029797,0.0360657324407392,
10.7707675453198));
#95100=CARTESIAN_POINT('Ctrl Pts',(11.991088873251,0.0360665242078553,10.7707675454579));
#95101=CARTESIAN_POINT('Ctrl Pts',(11.9910888435224,0.0360673159750026,
10.7707675455959));
#95102=CARTESIAN_POINT('Ctrl Pts',(11.9910888137937,0.0360681077421199,
10.7707675457339));
#95103=CARTESIAN_POINT('Ctrl Pts',(11.9339360911498,1.55822320275625,10.7710327096852));
#95104=CARTESIAN_POINT('Ctrl Pts',(11.876742229104,3.08252202922973,10.4454709204958));
#95105=CARTESIAN_POINT('Ctrl Pts',(11.8195073882191,4.47068816216161,9.81823304479766));
#95106=CARTESIAN_POINT('Ctrl Pts',(11.8195072882203,4.47069058751851,9.81823194890887));
#95107=CARTESIAN_POINT('Ctrl Pts',(11.8195071882216,4.47069301287499,9.81823085301915));
#95108=CARTESIAN_POINT('Ctrl Pts',(11.8195070882228,4.47069543823106,9.81822975712852));
#95109=CARTESIAN_POINT('Ctrl Pts',(11.7647262028572,5.79934320531001,9.21788382628587));
#95110=CARTESIAN_POINT('Ctrl Pts',(11.7099064063734,7.00328222838745,8.34115772527208));
#95111=CARTESIAN_POINT('Ctrl Pts',(11.6550500153073,7.99116085304476,7.26550933943654));
#95112=CARTESIAN_POINT('Ctrl Pts',(11.6334881613261,8.37945644161783,6.84271496708076));
#95113=CARTESIAN_POINT('Ctrl Pts',(11.6119206340189,8.73437210179503,6.38918775421612));
#95114=CARTESIAN_POINT('Ctrl Pts',(11.5903474976357,9.05036237110234,5.90963037900502));
#95115=CARTESIAN_POINT('Ctrl Pts',(11.5903472031011,9.05036668526645,5.90962383168564));
#95116=CARTESIAN_POINT('Ctrl Pts',(11.5903469085666,9.05037099942332,5.90961728436137));
#95117=CARTESIAN_POINT('Ctrl Pts',(11.590346614032,9.05037531357291,5.90961073703228));
#95118=CARTESIAN_POINT('Ctrl Pts',(11.5521177424565,9.6103268421719,5.05980549672893));
#95119=CARTESIAN_POINT('Ctrl Pts',(11.5138705621619,10.04802451717,4.12825797978597));
#95120=CARTESIAN_POINT('Ctrl Pts',(11.4756033482928,10.3475045060857,3.15400626050042));
#95121=CARTESIAN_POINT('Ctrl Pts',(11.4756027701249,10.3475090308397,3.15399154082099));
#95122=CARTESIAN_POINT('Ctrl Pts',(11.4756021919569,10.3475135555622,3.15397682113182));
#95123=CARTESIAN_POINT('Ctrl Pts',(11.4756016137889,10.3475180802532,3.15396210143288));
#95124=CARTESIAN_POINT('Ctrl Pts',(11.4445194665227,10.5907641957754,2.36263521950445));
#95125=CARTESIAN_POINT('Ctrl Pts',(11.413423181403,10.7428069207936,1.54311887101492));
#95126=CARTESIAN_POINT('Ctrl Pts',(11.3823157836203,10.8009630036407,0.716963741758189));
#95127=CARTESIAN_POINT('Ctrl Pts',(11.3559768003265,10.8502044125571,0.0174489093190168));
#95128=CARTESIAN_POINT('Ctrl Pts',(11.3296298305488,10.8321379003915,-0.686825019406177));
#95129=CARTESIAN_POINT('Ctrl Pts',(11.3032760407308,10.7451581043584,-1.3827939101456));
#95130=CARTESIAN_POINT('Ctrl Pts',(11.3032751042502,10.7451550135354,-1.38281864136757));
#95131=CARTESIAN_POINT('Ctrl Pts',(11.3032741677695,10.7451519226254,-1.38284337257904));
#95132=CARTESIAN_POINT('Ctrl Pts',(11.3032732312888,10.7451488316284,-1.38286810378004));
#95133=CARTESIAN_POINT('Ctrl Pts',(11.276427626827,10.6565408306116,-2.09182455745042));
#95134=CARTESIAN_POINT('Ctrl Pts',(11.2495747669126,10.4964033124759,-2.7921500741643));
#95135=CARTESIAN_POINT('Ctrl Pts',(11.2227120936351,10.2695128164393,-3.47058196733028));
#95136=CARTESIAN_POINT('Ctrl Pts',(11.1961226945325,10.0449304791044,-4.14211216780692));
#95137=CARTESIAN_POINT('Ctrl Pts',(11.1695236812975,9.75494559229498,-4.79219337877807));
#95138=CARTESIAN_POINT('Ctrl Pts',(11.1429127933632,9.40414738125851,-5.40793884114943));
#95139=CARTESIAN_POINT('Ctrl Pts',(11.1388448428612,9.35052159612138,-5.50206655567435));
#95140=CARTESIAN_POINT('Ctrl Pts',(11.1347766152765,9.29547462001186,-5.59539182062596));
#95141=CARTESIAN_POINT('Ctrl Pts',(11.1307081029784,9.23902277573395,-5.68786851634614));
#95142=CARTESIAN_POINT('Ctrl Pts',(11.1307077878792,9.23901840363643,-5.68787567850598));
#95143=CARTESIAN_POINT('Ctrl Pts',(11.1307074727799,9.23901403153045,-5.6878828406608));
#95144=CARTESIAN_POINT('Ctrl Pts',(11.1307071576807,9.23900965941608,-5.68789000281049));
#95145=CARTESIAN_POINT('Ctrl Pts',(11.1087126902279,8.93382856876452,-6.18782034961866));
#95146=CARTESIAN_POINT('Ctrl Pts',(11.0867101411768,8.58762339757433,-6.66296969610626));
#95147=CARTESIAN_POINT('Ctrl Pts',(11.0647020280532,8.20552966826705,-7.10739697135233));
#95148=CARTESIAN_POINT('Ctrl Pts',(11.0430057911313,7.82885057584139,-7.54552628321619));
#95149=CARTESIAN_POINT('Ctrl Pts',(11.021304148256,7.41729343552421,-7.95379682567712));
#95150=CARTESIAN_POINT('Ctrl Pts',(10.9996002320039,6.97582456482181,-8.32653423594124));
#95151=CARTESIAN_POINT('Ctrl Pts',(10.9856977369036,6.69304063124135,-8.56529206930643));
#95152=CARTESIAN_POINT('Ctrl Pts',(10.9717943237775,6.39798460599023,-8.7894707983027));
#95153=CARTESIAN_POINT('Ctrl Pts',(10.9578909660409,6.09197018180152,-8.99758667411823));
#95154=CARTESIAN_POINT('Ctrl Pts',(10.9578863159333,6.09186783242472,-8.99765628041293));
#95155=CARTESIAN_POINT('Ctrl Pts',(10.9578816658257,6.09176548182219,-8.99772588491082));
#95156=CARTESIAN_POINT('Ctrl Pts',(10.9578770157181,6.09166312999389,-8.99779548761196));
#95157=CARTESIAN_POINT('Ctrl Pts',(10.9383945955149,5.66284265850238,-9.28940789567403));
#95158=CARTESIAN_POINT('Ctrl Pts',(10.918910893143,5.2124075741954,-9.54944778025722));
#95159=CARTESIAN_POINT('Ctrl Pts',(10.8994243975854,4.74555262774488,-9.77638020724774));
#95160=CARTESIAN_POINT('Ctrl Pts',(10.8798301960368,4.27611727505877,-10.0045669378589));
#95161=CARTESIAN_POINT('Ctrl Pts',(10.8602331571735,3.79008010926782,-10.1992803732407));
#95162=CARTESIAN_POINT('Ctrl Pts',(10.8406301278026,3.29267026192362,-10.3589639008086));
#95163=CARTESIAN_POINT('Ctrl Pts',(10.8211593846148,2.798617061599,-10.5175698436849));
#95164=CARTESIAN_POINT('Ctrl Pts',(10.8016827442102,2.29334380119201,-10.6416182908074));
#95165=CARTESIAN_POINT('Ctrl Pts',(10.7821955326892,1.78192541675302,-10.7295699425325));
#95166=CARTESIAN_POINT('Ctrl Pts',(10.7633071045453,1.28622138051714,-10.8148191046282));
#95167=CARTESIAN_POINT('Ctrl Pts',(10.7444087737147,0.784743322812868,-10.8661567175532));
#95168=CARTESIAN_POINT('Ctrl Pts',(10.7254944885072,0.282074720709333,-10.8821514898605));
#95169=CARTESIAN_POINT('Ctrl Pts',(10.7164126013939,0.0407132603268094,
-10.8898315430534));
#95170=CARTESIAN_POINT('Ctrl Pts',(10.7073270064101,-0.20092318772183,-10.889362630306));
#95171=CARTESIAN_POINT('Ctrl Pts',(10.6982368407905,-0.442329630350118,
-10.8805826918547));
#95172=CARTESIAN_POINT('Ctrl Pts',(10.6982355033686,-0.442365148102834,
-10.8805814000761));
#95173=CARTESIAN_POINT('Ctrl Pts',(10.6982341659467,-0.442400665849766,
-10.8805801081155));
#95174=CARTESIAN_POINT('Ctrl Pts',(10.6982328285249,-0.442436183590935,
-10.880578815973));
#95175=CARTESIAN_POINT('Ctrl Pts',(10.6817905060337,-0.8790928361865,-10.8646931591655));
#95176=CARTESIAN_POINT('Ctrl Pts',(10.6653483153528,-1.31487411611491,-10.8213005155887));
#95177=CARTESIAN_POINT('Ctrl Pts',(10.6489086997776,-1.74664947052937,-10.7516253321206));
#95178=CARTESIAN_POINT('Ctrl Pts',(10.6324561907571,-2.17876346253965,-10.6818955030217));
#95179=CARTESIAN_POINT('Ctrl Pts',(10.6160062390361,-2.60686458099451,-10.5858427064414));
#95180=CARTESIAN_POINT('Ctrl Pts',(10.5995600031669,-3.02785330284519,-10.4647288798457));
#95181=CARTESIAN_POINT('Ctrl Pts',(10.5890775919128,-3.2961807761276,-10.3875340159854));
#95182=CARTESIAN_POINT('Ctrl Pts',(10.5785966663672,-3.56161967797226,-10.3001588571056));
#95183=CARTESIAN_POINT('Ctrl Pts',(10.5681172994041,-3.82337729854416,-10.202935230923));
#95184=CARTESIAN_POINT('Ctrl Pts',(10.5517035494577,-4.23336619823257,-10.050654630896));
#95185=CARTESIAN_POINT('Ctrl Pts',(10.5352900090993,-4.6344161363684,-9.87418397575912));
#95186=CARTESIAN_POINT('Ctrl Pts',(10.5188765390162,-5.02358347131284,-9.6745851249155));
#95187=CARTESIAN_POINT('Ctrl Pts',(10.5026744444006,-5.40773904293458,-9.47755674212017));
#95188=CARTESIAN_POINT('Ctrl Pts',(10.4864724376194,-5.78031654354983,-9.2579911487857));
#95189=CARTESIAN_POINT('Ctrl Pts',(10.4702713454141,-6.13843979100847,-9.01688710342178));
#95190=CARTESIAN_POINT('Ctrl Pts',(10.4595375757754,-6.37570851287987,-8.85714754703308));
#95191=CARTESIAN_POINT('Ctrl Pts',(10.4488042284911,-6.60663158645119,-8.68795323280413));
#95192=CARTESIAN_POINT('Ctrl Pts',(10.4380716961009,-6.83036021601855,-8.50959177631948));
#95193=CARTESIAN_POINT('Ctrl Pts',(10.4380538739088,-6.83073173454504,-8.50929559345891));
#95194=CARTESIAN_POINT('Ctrl Pts',(10.4380360517174,-6.83110323324723,-8.50899938533706));
#95195=CARTESIAN_POINT('Ctrl Pts',(10.4380182295268,-6.83147471212122,-8.50870315195564));
#95196=CARTESIAN_POINT('Ctrl Pts',(10.4240239199098,-7.12316670974611,-8.27609528959938));
#95197=CARTESIAN_POINT('Ctrl Pts',(10.4100301843033,-7.40262900123163,-8.027914184564));
#95198=CARTESIAN_POINT('Ctrl Pts',(10.3960314849731,-7.66869202103855,-7.76587198354066));
#95199=CARTESIAN_POINT('Ctrl Pts',(10.3813641610424,-7.94746309865262,-7.49131377243469));
#95200=CARTESIAN_POINT('Ctrl Pts',(10.3666914133372,-8.21152444193502,-7.20153998553732));
#95201=CARTESIAN_POINT('Ctrl Pts',(10.3520053807219,-8.4595868661027,-6.89849586245379));
#95202=CARTESIAN_POINT('Ctrl Pts',(10.3373193481065,-8.70764929027039,-6.59545173937024));
#95203=CARTESIAN_POINT('Ctrl Pts',(10.3226201383575,-8.93971350484724,-6.27913822071352));
#95204=CARTESIAN_POINT('Ctrl Pts',(10.307897451588,-9.15453835988915,-5.95146045198642));
#95205=CARTESIAN_POINT('Ctrl Pts',(10.3078926968971,-9.15460773756404,-5.9513546284694));
#95206=CARTESIAN_POINT('Ctrl Pts',(10.3078879422038,-9.15467711344128,-5.95124880376669));
#95207=CARTESIAN_POINT('Ctrl Pts',(10.307883187508,-9.15474648752083,-5.95114297787839));
#95208=CARTESIAN_POINT('Ctrl Pts',(10.2950118141782,-9.34254812824675,-5.66466313436061));
#95209=CARTESIAN_POINT('Ctrl Pts',(10.2821249864793,-9.51713738035586,-5.36954274635421));
#95210=CARTESIAN_POINT('Ctrl Pts',(10.2692307460949,-9.67765166003237,-5.06699870239409));
#95211=CARTESIAN_POINT('Ctrl Pts',(10.2563266189396,-9.83828901542888,-4.76422268015691));
#95212=CARTESIAN_POINT('Ctrl Pts',(10.2434150115707,-9.98482905816014,-4.4540111652875));
#95213=CARTESIAN_POINT('Ctrl Pts',(10.230506763713,-10.1163788997621,-4.1376276009189));
#95214=CARTESIAN_POINT('Ctrl Pts',(10.2176290652104,-10.247617408418,-3.82199280694777));
#95215=CARTESIAN_POINT('Ctrl Pts',(10.2047547508469,-10.363935759884,-3.5002148636008));
#95216=CARTESIAN_POINT('Ctrl Pts',(10.1918974615459,-10.4644310230913,-3.17359719965375));
#95217=CARTESIAN_POINT('Ctrl Pts',(10.1869804590058,-10.5028633436909,-3.04868907589055));
#95218=CARTESIAN_POINT('Ctrl Pts',(10.1820659724405,-10.5389813997489,-2.92307366388694));
#95219=CARTESIAN_POINT('Ctrl Pts',(10.1771548409931,-10.5727344554174,-2.79682587267854));
#95220=CARTESIAN_POINT('Ctrl Pts',(10.1771531125453,-10.5727463346347,-2.79678144040639));
#95221=CARTESIAN_POINT('Ctrl Pts',(10.1771513840978,-10.5727582135592,-2.79673700805592));
#95222=CARTESIAN_POINT('Ctrl Pts',(10.1771496556507,-10.5727700921907,-2.79669257562713));
#95223=CARTESIAN_POINT('Ctrl Pts',(10.1600923132765,-10.6899954840456,-2.35820697423387));
#95224=CARTESIAN_POINT('Ctrl Pts',(10.1430357320927,-10.7791375076164,-1.912114575594));
#95225=CARTESIAN_POINT('Ctrl Pts',(10.125984049529,-10.8402521913098,-1.46190596578374));
#95226=CARTESIAN_POINT('Ctrl Pts',(10.1089323669653,-10.9013668750032,-1.01169735597347));
#95227=CARTESIAN_POINT('Ctrl Pts',(10.0918856236707,-10.9344533695982,-0.557371477539993));
#95228=CARTESIAN_POINT('Ctrl Pts',(10.0748490921613,-10.93952229677,-0.10245759066365));
#95229=CARTESIAN_POINT('Ctrl Pts',(10.0592286476227,-10.9441698915995,0.314643574314747));
#95230=CARTESIAN_POINT('Ctrl Pts',(10.0436100742942,-10.9253234912044,0.732257491259243));
#95231=CARTESIAN_POINT('Ctrl Pts',(10.0279840463942,-10.8831643611597,1.14755960306089));
#95232=CARTESIAN_POINT('Ctrl Pts',(10.0123763869989,-10.8410547894665,1.56237352433246));
#95233=CARTESIAN_POINT('Ctrl Pts',(9.99676130151046,-10.775688316319,1.97488078916013));
#95234=CARTESIAN_POINT('Ctrl Pts',(9.98112802898836,-10.687259935448,2.38231663280635));
#95235=CARTESIAN_POINT('Ctrl Pts',(9.96557287319891,-10.5992734157533,2.78771659069503));
#95236=CARTESIAN_POINT('Ctrl Pts',(9.94999978403184,-10.4884559072605,3.18809569448487));
#95237=CARTESIAN_POINT('Ctrl Pts',(9.93439608171986,-10.3549982254007,3.58078175974953));
#95238=CARTESIAN_POINT('Ctrl Pts',(9.92831144655146,-10.3029566465303,3.73390897245062));
#95239=CARTESIAN_POINT('Ctrl Pts',(9.92222212763273,-10.2474723168187,3.88586693574198));
#95240=CARTESIAN_POINT('Ctrl Pts',(9.91612723880565,-10.1885559866788,4.0364992796125));
#95241=CARTESIAN_POINT('Ctrl Pts',(9.91612511809011,-10.1885354867516,4.03655169211108));
#95242=CARTESIAN_POINT('Ctrl Pts',(9.91612299737397,-10.1885149864093,4.03660410444787));
#95243=CARTESIAN_POINT('Ctrl Pts',(9.91612087665721,-10.1884944856518,4.0366565166229));
#95244=CARTESIAN_POINT('Ctrl Pts',(9.90424230788015,-10.0736655449819,4.33022784125202));
#95245=CARTESIAN_POINT('Ctrl Pts',(9.89234445392564,-9.94580834537035,4.6187281425354));
#95246=CARTESIAN_POINT('Ctrl Pts',(9.8804433786764,-9.80555473114634,4.90117931235152));
#95247=CARTESIAN_POINT('Ctrl Pts',(9.86853193699502,-9.66517894900519,5.18387651127215));
#95248=CARTESIAN_POINT('Ctrl Pts',(9.85661725743133,-9.51238449680269,5.46051361479744));
#95249=CARTESIAN_POINT('Ctrl Pts',(9.84471830064194,-9.34783275583516,5.73006603077023));
#95250=CARTESIAN_POINT('Ctrl Pts',(9.83932807489827,-9.27329084043639,5.85217323710445));
#95251=CARTESIAN_POINT('Ctrl Pts',(9.83394111531266,-9.19633666345336,5.97282604479221));
#95252=CARTESIAN_POINT('Ctrl Pts',(9.8285593516629,-9.11703410606218,6.09192663296797));
#95253=CARTESIAN_POINT('Ctrl Pts',(9.81375791075102,-8.89892863102168,6.41948845715402));
#95254=CARTESIAN_POINT('Ctrl Pts',(9.79897061721313,-8.66324738954729,6.73542959730272));
#95255=CARTESIAN_POINT('Ctrl Pts',(9.78418769195425,-8.41148443703231,7.03808188949212));
#95256=CARTESIAN_POINT('Ctrl Pts',(9.76987296525404,-8.16769521430548,7.33114870624292));
#95257=CARTESIAN_POINT('Ctrl Pts',(9.75556231771307,-7.9088263515839,7.61175589603912));
#95258=CARTESIAN_POINT('Ctrl Pts',(9.74124597042629,-7.63618864220333,7.87838006913979));
#95259=CARTESIAN_POINT('Ctrl Pts',(9.73131841879647,-7.44713029639129,8.06326837837052));
#95260=CARTESIAN_POINT('Ctrl Pts',(9.7213931377954,-7.25139733094209,8.24141573136087));
#95261=CARTESIAN_POINT('Ctrl Pts',(9.71149210718083,-7.04932308698385,8.41213375761355));
#95262=CARTESIAN_POINT('Ctrl Pts',(9.70688153567211,-6.95522401910804,8.49163130675839));
#95263=CARTESIAN_POINT('Ctrl Pts',(9.70227624358616,-6.85975041147126,8.56951733569182));
#95264=CARTESIAN_POINT('Ctrl Pts',(9.69767849528538,-6.76293888476845,8.64571985600731));
#95265=CARTESIAN_POINT('Ctrl Pts',(9.68554012472698,-6.50734982060734,8.846899731147));
#95266=CARTESIAN_POINT('Ctrl Pts',(9.67336295672748,-6.24287541021037,9.03690912957521));
#95267=CARTESIAN_POINT('Ctrl Pts',(9.66113765782758,-5.97046298774467,9.21476964386224));
#95268=CARTESIAN_POINT('Ctrl Pts',(9.65879580270697,-5.91828017964376,9.24884026737405));
#95269=CARTESIAN_POINT('Ctrl Pts',(9.6564521725576,-5.86580607557735,9.28246524616543));
#95270=CARTESIAN_POINT('Ctrl Pts',(9.65410668749291,-5.81304730592889,9.31563792018204));
#95271=CARTESIAN_POINT('Ctrl Pts',(9.64680021884648,-5.64869738016574,9.41897479760209));
#95272=CARTESIAN_POINT('Ctrl Pts',(9.63947579902925,-5.48158521451971,9.51792205096366));
#95273=CARTESIAN_POINT('Ctrl Pts',(9.63213061486297,-5.31200090258064,9.61242722059944));
#95274=CARTESIAN_POINT('Ctrl Pts',(9.62097856935138,-5.05452444971298,9.75591252049098));
#95275=CARTESIAN_POINT('Ctrl Pts',(9.60986719987094,-4.79106445159546,9.88856816815131));
#95276=CARTESIAN_POINT('Ctrl Pts',(9.59877852810167,-4.52266849084066,10.0102947770022));
#95277=CARTESIAN_POINT('Ctrl Pts',(9.58798006298252,-4.26129684231154,10.1288356236519));
#95278=CARTESIAN_POINT('Ctrl Pts',(9.57720302703863,-3.99524420678122,10.2370126121934));
#95279=CARTESIAN_POINT('Ctrl Pts',(9.5664284793928,-3.72543397488881,10.3347516488405));
#95280=CARTESIAN_POINT('Ctrl Pts',(9.55408976253708,-3.4164546872633,10.4466797165962));
#95281=CARTESIAN_POINT('Ctrl Pts',(9.54175218849227,-3.10249573876305,10.5449422787711));
#95282=CARTESIAN_POINT('Ctrl Pts',(9.5294102067266,-2.78471433156453,10.6292485760067));
#95283=CARTESIAN_POINT('Ctrl Pts',(9.52718922994239,-2.72752861040209,10.6444197480663));
#95284=CARTESIAN_POINT('Ctrl Pts',(9.52496811040537,-2.67021906674301,10.659138842928));
#95285=CARTESIAN_POINT('Ctrl Pts',(9.52274681574758,-2.61279239892922,10.6734039929166));
#95286=CARTESIAN_POINT('Ctrl Pts',(9.50957782861494,-2.27233731934088,10.757975202767));
#95287=CARTESIAN_POINT('Ctrl Pts',(9.49640208211643,-1.92774945005703,10.8265966109633));
#95288=CARTESIAN_POINT('Ctrl Pts',(9.4832339184354,-1.58054382301562,10.8787209774921));
#95289=CARTESIAN_POINT('Ctrl Pts',(9.47455588396265,-1.35172965624335,10.9130717845267));
#95290=CARTESIAN_POINT('Ctrl Pts',(9.46588117844456,-1.12177946918322,10.9402572872661));
#95291=CARTESIAN_POINT('Ctrl Pts',(9.45721419258468,-0.891138086337386,
10.9601155441168));
#95292=CARTESIAN_POINT('Ctrl Pts',(9.44738282224253,-0.629510700803001,
10.9826417003384));
#95293=CARTESIAN_POINT('Ctrl Pts',(9.43756127496004,-0.366999143975139,
10.9957394251776));
#95294=CARTESIAN_POINT('Ctrl Pts',(9.42772347258561,-0.104322862781696,
10.9994016033688));
#95295=CARTESIAN_POINT('Ctrl Pts',(9.41789152627671,0.158197057320262,11.0030616016061));
#95296=CARTESIAN_POINT('Ctrl Pts',(9.40804341476379,0.420881371031134,10.9972978968109));
#95297=CARTESIAN_POINT('Ctrl Pts',(9.39815138092922,0.683062679165209,10.9821145355309));
#95298=CARTESIAN_POINT('Ctrl Pts',(9.39597581796097,0.74072442542335,10.978775246656));
#95299=CARTESIAN_POINT('Ctrl Pts',(9.39379812055835,0.798362040111534,10.9749803553368));
#95300=CARTESIAN_POINT('Ctrl Pts',(9.39161797327781,0.855968760489002,10.9707299301633));
#95301=CARTESIAN_POINT('Ctrl Pts',(9.39161740661138,0.855983733695031,10.9707288253879));
#95302=CARTESIAN_POINT('Ctrl Pts',(9.39161683994479,0.85599870689897,10.9707277205816));
#95303=CARTESIAN_POINT('Ctrl Pts',(9.39161627327803,0.856013680100825,10.9707266157446));
#95304=CARTESIAN_POINT('Ctrl Pts',(9.37394596126279,1.32292151416537,10.9362745949034));
#95305=CARTESIAN_POINT('Ctrl Pts',(9.35629746476006,1.78747736955613,10.870794368147));
#95306=CARTESIAN_POINT('Ctrl Pts',(9.33867148090217,2.24598873793039,10.7758863557475));
#95307=CARTESIAN_POINT('Ctrl Pts',(9.3214200148757,2.69475763265044,10.6829949537839));
#95308=CARTESIAN_POINT('Ctrl Pts',(9.30419010193193,3.1377356506204,10.5619136932599));
#95309=CARTESIAN_POINT('Ctrl Pts',(9.28698169162748,3.57150226341286,10.4141705750997));
#95310=CARTESIAN_POINT('Ctrl Pts',(9.28283455480297,3.67603774701233,10.3785652568251));
#95311=CARTESIAN_POINT('Ctrl Pts',(9.27868866402646,3.78003845909759,10.3414115615419));
#95312=CARTESIAN_POINT('Ctrl Pts',(9.27454401349585,3.88345694555816,10.3027310589707));
#95313=CARTESIAN_POINT('Ctrl Pts',(9.26173983131444,4.20295050280404,10.1832343250163));
#95314=CARTESIAN_POINT('Ctrl Pts',(9.24893344583012,4.51708431878307,10.0491376720003));
#95315=CARTESIAN_POINT('Ctrl Pts',(9.23614139349798,4.82448797231439,9.90086735627349));
#95316=CARTESIAN_POINT('Ctrl Pts',(9.22345462903181,5.12936147088459,9.75381741275308));
#95317=CARTESIAN_POINT('Ctrl Pts',(9.21078201863816,5.4276151908266,9.59282545578268));
#95318=CARTESIAN_POINT('Ctrl Pts',(9.19814075939927,5.71786135179877,9.41830487169184));
#95319=CARTESIAN_POINT('Ctrl Pts',(9.1892140139505,5.92282143904346,9.29506550128486));
#95320=CARTESIAN_POINT('Ctrl Pts',(9.18030293369877,6.12378739923758,9.16507986810741));
#95321=CARTESIAN_POINT('Ctrl Pts',(9.1714135761887,6.32025498189214,9.02849560697713));
#95322=CARTESIAN_POINT('Ctrl Pts',(9.15963076376754,6.58067207847463,8.84745364452293));
#95323=CARTESIAN_POINT('Ctrl Pts',(9.14778454022514,6.83347258097126,8.65533909466343));
#95324=CARTESIAN_POINT('Ctrl Pts',(9.1358582875849,7.07756053330412,8.45272405369443));
#95325=CARTESIAN_POINT('Ctrl Pts',(9.13356736965186,7.12444747123071,8.41380366144192));
#95326=CARTESIAN_POINT('Ctrl Pts',(9.13127348637172,7.17101308047551,8.37449583067599));
#95327=CARTESIAN_POINT('Ctrl Pts',(9.12897649995789,7.21724981291642,8.33480463150905));
#95328=CARTESIAN_POINT('Ctrl Pts',(9.12142168216154,7.36932301935194,8.20425976802198));
#95329=CARTESIAN_POINT('Ctrl Pts',(9.11383338299965,7.51783794744756,8.0695678436588));
#95330=CARTESIAN_POINT('Ctrl Pts',(9.10620600819097,7.66265230395864,7.93101579732647));
#95331=CARTESIAN_POINT('Ctrl Pts',(9.08745532896714,8.0186552032591,7.59040778451148));
#95332=CARTESIAN_POINT('Ctrl Pts',(9.06880435751816,8.35096412388481,7.22520305099041));
#95333=CARTESIAN_POINT('Ctrl Pts',(9.05026519954328,8.65724948375359,6.83929469703732));
#95334=CARTESIAN_POINT('Ctrl Pts',(9.04703363894821,8.7106380843115,6.77202701251596));
#95335=CARTESIAN_POINT('Ctrl Pts',(9.04380546309821,8.7632359176161,6.70413016195419));
#95336=CARTESIAN_POINT('Ctrl Pts',(9.04058071946552,8.81503055537896,6.63562463964333));
#95337=CARTESIAN_POINT('Ctrl Pts',(9.02766259082993,9.02251675256724,6.36119564612947));
#95338=CARTESIAN_POINT('Ctrl Pts',(9.01474413415878,9.21737630810118,6.07712410118515));
#95339=CARTESIAN_POINT('Ctrl Pts',(9.00182002655774,9.39887812276248,5.78458511222852));
#95340=CARTESIAN_POINT('Ctrl Pts',(9.00011373135565,9.42284075794672,5.74596288091574));
#95341=CARTESIAN_POINT('Ctrl Pts',(8.99840733764636,9.44657049929936,5.70719301937561));
#95342=CARTESIAN_POINT('Ctrl Pts',(8.99670083317216,9.47006560548064,5.66827819795195));
#95343=CARTESIAN_POINT('Ctrl Pts',(8.98502581887399,9.6308068779185,5.40204326953455));
#95344=CARTESIAN_POINT('Ctrl Pts',(8.97340281255853,9.78033206732416,5.12881471684042));
#95345=CARTESIAN_POINT('Ctrl Pts',(8.96180410195002,9.91811115413175,4.84969521228766));
#95346=CARTESIAN_POINT('Ctrl Pts',(8.95020453516649,10.055900411295,4.57055510413893));
#95347=CARTESIAN_POINT('Ctrl Pts',(8.93862916408886,10.1819423440877,4.28552370912528));
#95348=CARTESIAN_POINT('Ctrl Pts',(8.92704867470572,10.2957451194813,3.99566856776635));
#95349=CARTESIAN_POINT('Ctrl Pts',(8.9154766341582,10.4094648672143,3.70602489747416));
#95350=CARTESIAN_POINT('Ctrl Pts',(8.90389948983685,10.5109639151262,3.41156494279894));
#95351=CARTESIAN_POINT('Ctrl Pts',(8.89228712084619,10.5997813700364,3.11331137960146));
#95352=CARTESIAN_POINT('Ctrl Pts',(8.8834668673401,10.6672432693874,2.88677086589459));
#95353=CARTESIAN_POINT('Ctrl Pts',(8.87462630058372,10.727389516561,2.65804087414844));
#95354=CARTESIAN_POINT('Ctrl Pts',(8.8657515832713,10.7800262063301,2.42755112095466));
#95355=CARTESIAN_POINT('Ctrl Pts',(8.86573523696568,10.7801231576343,2.42712658281845));
#95356=CARTESIAN_POINT('Ctrl Pts',(8.86571889054395,10.7802200834631,2.42670203870736));
#95357=CARTESIAN_POINT('Ctrl Pts',(8.86570254400602,10.7803169838174,2.42627748862456));
#95358=CARTESIAN_POINT('Ctrl Pts',(8.85391139131615,10.8502135501323,2.12003925806498));
#95359=CARTESIAN_POINT('Ctrl Pts',(8.8420497849596,10.9069009882179,1.81079706389893));
#95360=CARTESIAN_POINT('Ctrl Pts',(8.83014882942962,10.9503521553503,1.49965539489733));
#95361=CARTESIAN_POINT('Ctrl Pts',(8.81819935166284,10.9939804803434,1.18724514794795));
#95362=CARTESIAN_POINT('Ctrl Pts',(8.80621005785882,11.0242635506925,0.872919835380537));
#95363=CARTESIAN_POINT('Ctrl Pts',(8.79421476148775,11.0411678356221,0.557849550303085));
#95364=CARTESIAN_POINT('Ctrl Pts',(8.78846357505489,11.0492726536389,0.406788009772473));
#95365=CARTESIAN_POINT('Ctrl Pts',(8.7827110572473,11.0543020041665,0.255555991386337));
#95366=CARTESIAN_POINT('Ctrl Pts',(8.77696122488992,11.0562525456141,0.104286681754343));
#95367=CARTESIAN_POINT('Ctrl Pts',(8.76744115389902,11.059482082042,-0.146171849369996));
#95368=CARTESIAN_POINT('Ctrl Pts',(8.75799061301917,11.0539796414036,-0.396747075555581));
#95369=CARTESIAN_POINT('Ctrl Pts',(8.74857110277678,11.0399950780339,-0.646838836509623));
#95370=CARTESIAN_POINT('Ctrl Pts',(8.7433043604888,11.0321758720048,-0.786672948835796));
#95371=CARTESIAN_POINT('Ctrl Pts',(8.73804724784972,11.0217048656153,-0.926356853973552));
#95372=CARTESIAN_POINT('Ctrl Pts',(8.73279264605785,11.0086247373998,-1.06579266178105));
#95373=CARTESIAN_POINT('Ctrl Pts',(8.72130194515204,10.9800212680816,-1.37070923330026));
#95374=CARTESIAN_POINT('Ctrl Pts',(8.709811581266,10.938995324277,-1.67444970805189));
#95375=CARTESIAN_POINT('Ctrl Pts',(8.69834247180759,10.8855161855157,-1.97602583502142));
#95376=CARTESIAN_POINT('Ctrl Pts',(8.69518671476814,10.870801253269,-2.05900533653078));
#95377=CARTESIAN_POINT('Ctrl Pts',(8.692032574245,10.8551433260322,-2.14182072967303));
#95378=CARTESIAN_POINT('Ctrl Pts',(8.6888805008341,10.8385413880217,-2.22445084384318));
#95379=CARTESIAN_POINT('Ctrl Pts',(8.67427062587417,10.7615913279162,-2.60744180838551));
#95380=CARTESIAN_POINT('Ctrl Pts',(8.65963925766812,10.6645750156873,-2.98669631489204));
#95381=CARTESIAN_POINT('Ctrl Pts',(8.64498787790579,10.5476602194324,-3.35982430183711));
#95382=CARTESIAN_POINT('Ctrl Pts',(8.63033649814347,10.4307454231775,-3.73295228878218));
#95383=CARTESIAN_POINT('Ctrl Pts',(8.6156651102302,10.2939323547083,-4.09995268161777));
#95384=CARTESIAN_POINT('Ctrl Pts',(8.60097492287562,10.1374461559647,-4.45844717160862));
#95385=CARTESIAN_POINT('Ctrl Pts',(8.58628891771984,9.98100450780262,-4.81683960059872));
#95386=CARTESIAN_POINT('Ctrl Pts',(8.57158412839069,9.80490129183946,-5.16672999235309));
#95387=CARTESIAN_POINT('Ctrl Pts',(8.55686143044795,9.61070036994355,-5.50636554871548));
#95388=CARTESIAN_POINT('Ctrl Pts',(8.54213873250521,9.41649944804763,-5.84600110507788));
#95389=CARTESIAN_POINT('Ctrl Pts',(8.52739813169481,9.20420164947267,-6.17538109796706));
#95390=CARTESIAN_POINT('Ctrl Pts',(8.51264009359485,8.9754144165332,-6.49279241538405));
#95391=CARTESIAN_POINT('Ctrl Pts',(8.497227712024,8.73648319080253,-6.82427714972365));
#95392=CARTESIAN_POINT('Ctrl Pts',(8.48185121176318,8.47927918088958,-7.1426891506523));
#95393=CARTESIAN_POINT('Ctrl Pts',(8.46648978902769,8.20552414307779,-7.44626598819801));
#95394=CARTESIAN_POINT('Ctrl Pts',(8.45242853743153,7.95493938093226,-7.72414847115558));
#95395=CARTESIAN_POINT('Ctrl Pts',(8.43837988325975,7.69048611062595,-7.98960150491039));
#95396=CARTESIAN_POINT('Ctrl Pts',(8.42432677244307,7.41344658696125,-8.2412742508201));
#95397=CARTESIAN_POINT('Ctrl Pts',(8.40962405987569,7.12360097630753,-8.50458051036805));
#95398=CARTESIAN_POINT('Ctrl Pts',(8.39491626642312,6.81997188474144,-8.75280416621937));
#95399=CARTESIAN_POINT('Ctrl Pts',(8.38023523264272,6.50398366978781,-8.98416903734638));
#95400=CARTESIAN_POINT('Ctrl Pts',(8.36555419886231,6.18799545483416,-9.2155339084734));
#95401=CARTESIAN_POINT('Ctrl Pts',(8.35089999149063,5.85964777077985,-9.43003908131022));
#95402=CARTESIAN_POINT('Ctrl Pts',(8.33630581874266,5.52041797009034,-9.62588983413724));
#95403=CARTESIAN_POINT('Ctrl Pts',(8.33630560542693,5.52041301173797,-9.62589269678976));
#95404=CARTESIAN_POINT('Ctrl Pts',(8.33630539211122,5.5204080533833,-9.62589555943828));
#95405=CARTESIAN_POINT('Ctrl Pts',(8.33630517879552,5.52040309502629,-9.62589842208283));
#95406=CARTESIAN_POINT('Ctrl Pts',(8.32139797797909,5.17389684229249,-9.82594941329877));
#95407=CARTESIAN_POINT('Ctrl Pts',(8.30650499563908,4.81613020648062,-10.0067024134377));
#95408=CARTESIAN_POINT('Ctrl Pts',(8.29159566636577,4.44948056334772,-10.1676188745158));
#95409=CARTESIAN_POINT('Ctrl Pts',(8.27672502322162,4.08378228799208,-10.3281177960196));
#95410=CARTESIAN_POINT('Ctrl Pts',(8.26183814788653,3.7092474760114,-10.4688838498593));
#95411=CARTESIAN_POINT('Ctrl Pts',(8.24690344554343,3.32818901516837,-10.5894060653215));
#95412=CARTESIAN_POINT('Ctrl Pts',(8.23284526090791,2.96949487608279,-10.7028548317398));
#95413=CARTESIAN_POINT('Ctrl Pts',(8.21874475651843,2.60502013603582,-10.7983670812942));
#95414=CARTESIAN_POINT('Ctrl Pts',(8.20457381338371,2.23665246595822,-10.87552500873));
#95415=CARTESIAN_POINT('Ctrl Pts',(8.20456244779311,2.23635702224024,-10.8755868920787));
#95416=CARTESIAN_POINT('Ctrl Pts',(8.20455108215707,2.23606157601586,-10.8756487636208));
#95417=CARTESIAN_POINT('Ctrl Pts',(8.20453971647558,2.23576612728608,-10.8757106233563));
#95418=CARTESIAN_POINT('Ctrl Pts',(8.19131068089454,1.89187986228734,-10.9477119936699));
#95419=CARTESIAN_POINT('Ctrl Pts',(8.17802314470091,1.54465766477505,-11.0037037525121));
#95420=CARTESIAN_POINT('Ctrl Pts',(8.16471225861559,1.19560697869185,-11.0433202676434));
#95421=CARTESIAN_POINT('Ctrl Pts',(8.1513852003287,0.846132209792844,-11.0829849152779));
#95422=CARTESIAN_POINT('Ctrl Pts',(8.13803468467661,0.494824289630856,-11.1062336694404));
#95423=CARTESIAN_POINT('Ctrl Pts',(8.12469866360721,0.14324613009726,-11.1126845249433));
#95424=CARTESIAN_POINT('Ctrl Pts',(8.11137603138464,-0.207979058628419,
-11.1191289040381));
#95425=CARTESIAN_POINT('Ctrl Pts',(8.09806790537919,-0.559473985274116,
-11.108808265246));
#95426=CARTESIAN_POINT('Ctrl Pts',(8.08481486157169,-0.909628717147954,
-11.0813392565442));
#95427=CARTESIAN_POINT('Ctrl Pts',(8.08018383993,-1.03198356368732,-11.0717407389793));
#95428=CARTESIAN_POINT('Ctrl Pts',(8.07555956469545,-1.15417430605097,-11.0600484092193));
#95429=CARTESIAN_POINT('Ctrl Pts',(8.07094382065994,-1.2761307670632,-11.0462461270049));
#95430=CARTESIAN_POINT('Ctrl Pts',(8.07094256944499,-1.27616382646709,-11.0462423855449));
#95431=CARTESIAN_POINT('Ctrl Pts',(8.07094131823068,-1.27619688585376,-11.0462386439298));
#95432=CARTESIAN_POINT('Ctrl Pts',(8.07094006701699,-1.27622994522321,-11.0462349021597));
#95433=CARTESIAN_POINT('Ctrl Pts',(8.04671457520307,-1.91631204428851,-10.9737882675603));
#95434=CARTESIAN_POINT('Ctrl Pts',(8.02248078127624,-2.55028638804477,-10.8440120921138));
#95435=CARTESIAN_POINT('Ctrl Pts',(7.99824053625373,-3.16902712658607,-10.6607906274779));
#95436=CARTESIAN_POINT('Ctrl Pts',(7.973109117478,-3.81051538709868,-10.4708331682116));
#95437=CARTESIAN_POINT('Ctrl Pts',(7.94797076485528,-4.43562813347157,-10.2234287113763));
#95438=CARTESIAN_POINT('Ctrl Pts',(7.92282746351364,-5.03418592806953,-9.92296298718306));
#95439=CARTESIAN_POINT('Ctrl Pts',(7.89720134970723,-5.64423748636169,-9.61672759118328));
#95440=CARTESIAN_POINT('Ctrl Pts',(7.87157009539991,-6.22670301212677,-9.25537407620778));
#95441=CARTESIAN_POINT('Ctrl Pts',(7.84593572027054,-6.77081614111878,-8.8435975657615));
#95442=CARTESIAN_POINT('Ctrl Pts',(7.83235257565593,-7.0591308466853,-8.62540539754739));
#95443=CARTESIAN_POINT('Ctrl Pts',(7.81876855342073,-7.33667755373648,-8.39305663640217));
#95444=CARTESIAN_POINT('Ctrl Pts',(7.80518394485515,-7.60185783775227,-8.14725473688907));
#95445=CARTESIAN_POINT('Ctrl Pts',(7.80517720761467,-7.60198935301348,-8.14713283227184));
#95446=CARTESIAN_POINT('Ctrl Pts',(7.80517047037404,-7.60212086523309,-8.14701092434567));
#95447=CARTESIAN_POINT('Ctrl Pts',(7.80516373313327,-7.60225237441096,-8.14688901311081));
#95448=CARTESIAN_POINT('Ctrl Pts',(7.78072942945136,-8.07920359217663,-7.70474715751269));
#95449=CARTESIAN_POINT('Ctrl Pts',(7.75628358169676,-8.51608048184164,-7.21921732485523));
#95450=CARTESIAN_POINT('Ctrl Pts',(7.73182870837808,-8.90798904969996,-6.6991970798396));
#95451=CARTESIAN_POINT('Ctrl Pts',(7.7065854677389,-9.31253182357114,-6.16241261111158));
#95452=CARTESIAN_POINT('Ctrl Pts',(7.68133260625059,-9.66916085721407,-5.58887669198447));
#95453=CARTESIAN_POINT('Ctrl Pts',(7.65607339934336,-9.97245221159837,-4.98833609696704));
#95454=CARTESIAN_POINT('Ctrl Pts',(7.63088020110482,-10.2749509892956,-4.38936486575889));
#95455=CARTESIAN_POINT('Ctrl Pts',(7.60568069097792,-10.5243908685266,-3.76352836231937));
#95456=CARTESIAN_POINT('Ctrl Pts',(7.58047863651457,-10.7153424597389,-3.12048150287961));
#95457=CARTESIAN_POINT('Ctrl Pts',(7.56662102963664,-10.8203391411636,-2.76689562379342));
#95458=CARTESIAN_POINT('Ctrl Pts',(7.55276266260403,-10.9076512315918,-2.40810612198082));
#95459=CARTESIAN_POINT('Ctrl Pts',(7.53890422701102,-10.9763693314388,-2.045718580393));
#95460=CARTESIAN_POINT('Ctrl Pts',(7.53889927044658,-10.976393908938,-2.04558897000591));
#95461=CARTESIAN_POINT('Ctrl Pts',(7.53889431388162,-10.9764184840602,-2.0454593591586));
#95462=CARTESIAN_POINT('Ctrl Pts',(7.53888935731614,-10.9764430568053,-2.04532974785116));
#95463=CARTESIAN_POINT('Ctrl Pts',(7.50995500813713,-11.1198884303692,-1.28871332803983));
#95464=CARTESIAN_POINT('Ctrl Pts',(7.481002919287,-11.1823251731434,-0.516413750306353));
#95465=CARTESIAN_POINT('Ctrl Pts',(7.4520371360579,-11.1657699667983,0.254856495553427));
#95466=CARTESIAN_POINT('Ctrl Pts',(7.42206844780455,-11.1486415565634,1.05283103587334));
#95467=CARTESIAN_POINT('Ctrl Pts',(7.39208509902904,-11.0469562263886,1.84970208167534));
#95468=CARTESIAN_POINT('Ctrl Pts',(7.36209180085476,-10.8629991228641,2.62693895094568));
#95469=CARTESIAN_POINT('Ctrl Pts',(7.33209850268048,-10.6790420193395,3.40417582021604));
#95470=CARTESIAN_POINT('Ctrl Pts',(7.3020952552254,-10.4128131726403,4.16177655833391));
#95471=CARTESIAN_POINT('Ctrl Pts',(7.27208700464185,-10.0666499299777,4.8812170112621));
#95472=CARTESIAN_POINT('Ctrl Pts',(7.27208662092667,-10.066645503592,4.88122621073938));
#95473=CARTESIAN_POINT('Ctrl Pts',(7.2720862372115,-10.0666410771933,4.88123541021042));
#95474=CARTESIAN_POINT('Ctrl Pts',(7.27208585349632,-10.0666366507816,4.88124460967523));
#95475=CARTESIAN_POINT('Ctrl Pts',(7.23228903670486,-9.6075536928767,5.83536224009391));
#95476=CARTESIAN_POINT('Ctrl Pts',(7.19248043715747,-9.00787535320312,6.7224152676858));
#95477=CARTESIAN_POINT('Ctrl Pts',(7.15265826104708,-8.29767799140454,7.51084519278056));
#95478=CARTESIAN_POINT('Ctrl Pts',(7.11184999850807,-7.5698945494739,8.31879841180325));
#95479=CARTESIAN_POINT('Ctrl Pts',(7.0710274788903,-6.72604943649446,9.0231857719293));
#95480=CARTESIAN_POINT('Ctrl Pts',(7.03018869589303,-5.79846489065266,9.59002045639908));
#95481=CARTESIAN_POINT('Ctrl Pts',(7.02173023308444,-5.60634507691215,9.70742234120858));
#95482=CARTESIAN_POINT('Ctrl Pts',(7.01327107234976,-5.41063290456088,9.81892334267702));
#95483=CARTESIAN_POINT('Ctrl Pts',(7.00481119545851,-5.21161542129423,9.92422123240472));
#95484=CARTESIAN_POINT('Ctrl Pts',(7.00481117113412,-5.21161484906612,9.92422153516411));
#95485=CARTESIAN_POINT('Ctrl Pts',(7.00481114680973,-5.21161427683798,9.92422183792345));
#95486=CARTESIAN_POINT('Ctrl Pts',(7.00481112248533,-5.21161370460982,9.92422214068274));
#95487=CARTESIAN_POINT('Ctrl Pts',(6.95949580048587,-4.14557665577187,10.4882499890114));
#95488=CARTESIAN_POINT('Ctrl Pts',(6.91413937966825,-2.98477603349806,10.8743265992955));
#95489=CARTESIAN_POINT('Ctrl Pts',(6.86875514637579,-1.79216017556988,11.0712521117833));
#95490=CARTESIAN_POINT('Ctrl Pts',(6.82484072307876,-0.638168275380296,
11.2618000110427));
#95491=CARTESIAN_POINT('Ctrl Pts',(6.78090026783952,0.54561229331462,11.275247854403));
#95492=CARTESIAN_POINT('Ctrl Pts',(6.73694742131768,1.70211153428016,11.1014270624495));
#95493=CARTESIAN_POINT('Ctrl Pts',(6.73694635133782,1.70213968788115,11.1014228309887));
#95494=CARTESIAN_POINT('Ctrl Pts',(6.73694528135794,1.70216784146597,11.1014185994169));
#95495=CARTESIAN_POINT('Ctrl Pts',(6.73694421137806,1.70219599503462,11.1014143677342));
#95496=CARTESIAN_POINT('Ctrl Pts',(6.69068820405194,2.91929521429124,10.9184756481802));
#95497=CARTESIAN_POINT('Ctrl Pts',(6.64441099772795,4.10619837218388,10.5281362965954));
#95498=CARTESIAN_POINT('Ctrl Pts',(6.59811266643679,5.20164540543921,9.96066846821707));
#95499=CARTESIAN_POINT('Ctrl Pts',(6.55495578108234,6.22276389303163,9.4317046086418));
#95500=CARTESIAN_POINT('Ctrl Pts',(6.51178053818585,7.1644145500614,8.74883553718005));
#95501=CARTESIAN_POINT('Ctrl Pts',(6.46858684323349,7.97700317709334,7.93661371656795));
#95502=CARTESIAN_POINT('Ctrl Pts',(6.46858241565496,7.97708647165656,7.93653045960431));
#95503=CARTESIAN_POINT('Ctrl Pts',(6.46857798807624,7.97716976486372,7.93644720128152));
#95504=CARTESIAN_POINT('Ctrl Pts',(6.46857356049733,7.97725305671478,7.93636394159967));
#95505=CARTESIAN_POINT('Ctrl Pts',(6.41597493735464,8.96674116546658,6.94725799566618));
#95506=CARTESIAN_POINT('Ctrl Pts',(6.36334786988935,9.76486922000591,5.76632989175888));
#95507=CARTESIAN_POINT('Ctrl Pts',(6.3106911995868,10.3278483444582,4.48170981970171));
#95508=CARTESIAN_POINT('Ctrl Pts',(6.27371870834979,10.7231399689729,3.57972334611484));
#95509=CARTESIAN_POINT('Ctrl Pts',(6.23673162266534,11.0025015723476,2.62661508981526));
#95510=CARTESIAN_POINT('Ctrl Pts',(6.19972953977931,11.1507603510177,1.65288782707181));
#95511=CARTESIAN_POINT('Ctrl Pts',(6.18620303910717,11.204957907288,1.29693158226929));
#95512=CARTESIAN_POINT('Ctrl Pts',(6.17267489270487,11.2416340018188,0.938229413935324));
#95513=CARTESIAN_POINT('Ctrl Pts',(6.15914510492325,11.2609492036324,0.578477224997408));
#95514=CARTESIAN_POINT('Ctrl Pts',(6.11285293765214,11.3270361643196,-0.652414846280726));
#95515=CARTESIAN_POINT('Ctrl Pts',(6.0665415518186,11.1898853054317,-1.89559503509316));
#95516=CARTESIAN_POINT('Ctrl Pts',(6.02021108604259,10.8559260765016,-3.08317147400487));
#95517=CARTESIAN_POINT('Ctrl Pts',(6.02020856522246,10.8559079059278,-3.08323608951306));
#95518=CARTESIAN_POINT('Ctrl Pts',(6.02020604440228,10.8558897347714,-3.08330070485664));
#95519=CARTESIAN_POINT('Ctrl Pts',(6.02020352358204,10.8558715630324,-3.08336532003562));
#95520=CARTESIAN_POINT('Ctrl Pts',(5.98978091762796,10.636565304282,-3.86317583451194));
#95521=CARTESIAN_POINT('Ctrl Pts',(5.95939936030158,10.332268746888,-4.61907445363975));
#95522=CARTESIAN_POINT('Ctrl Pts',(5.92902341902273,9.95150322999734,-5.33455706247603));
#95523=CARTESIAN_POINT('Ctrl Pts',(5.8996254815835,9.58299709081924,-6.02700352134749));
#95524=CARTESIAN_POINT('Ctrl Pts',(5.87023278073892,9.14286870013787,-6.68159552966999));
#95525=CARTESIAN_POINT('Ctrl Pts',(5.84081112680754,8.63883207786456,-7.28341797140726));
#95526=CARTESIAN_POINT('Ctrl Pts',(5.84080847416191,8.63878663410579,-7.28347223149999));
#95527=CARTESIAN_POINT('Ctrl Pts',(5.84080582151604,8.6387411898275,-7.2835264911638));
#95528=CARTESIAN_POINT('Ctrl Pts',(5.84080316886994,8.63869574502971,-7.28358075039867));
#95529=CARTESIAN_POINT('Ctrl Pts',(5.81466418682828,8.19088600845037,-7.81824730980955));
#95530=CARTESIAN_POINT('Ctrl Pts',(5.78845545804168,7.69275291643841,-8.31127372036197));
#95531=CARTESIAN_POINT('Ctrl Pts',(5.76221253802134,7.15365412876904,-8.75474726498968));
#95532=CARTESIAN_POINT('Ctrl Pts',(5.7356328223173,6.60763666952502,-9.20391224851042));
#95533=CARTESIAN_POINT('Ctrl Pts',(5.70901800908207,6.01959384493397,-9.60224326500889));
#95534=CARTESIAN_POINT('Ctrl Pts',(5.68240714568773,5.39927719035735,-9.94147517498252));
#95535=CARTESIAN_POINT('Ctrl Pts',(5.67516337950511,5.23042025631692,-10.0338177871375));
#95536=CARTESIAN_POINT('Ctrl Pts',(5.66791991878384,5.05917210024071,-10.1217810351109));
#95537=CARTESIAN_POINT('Ctrl Pts',(5.66067757974053,4.8857299708475,-10.2051978341173));
#95538=CARTESIAN_POINT('Ctrl Pts',(5.66067284953871,4.88561669028005,-10.2052523162801));
#95539=CARTESIAN_POINT('Ctrl Pts',(5.66066811933736,4.88550340877672,-10.2053067965034));
#95540=CARTESIAN_POINT('Ctrl Pts',(5.6606633891365,4.88539012633754,-10.2053612747873));
#95541=CARTESIAN_POINT('Ctrl Pts',(5.62118471048364,3.93992477681437,-10.6600418952297));
#95542=CARTESIAN_POINT('Ctrl Pts',(5.58172432895299,2.92921033768375,-10.9796773858916));
#95543=CARTESIAN_POINT('Ctrl Pts',(5.54226356021694,1.89377849318269,-11.1580953544777));
#95544=CARTESIAN_POINT('Ctrl Pts',(5.50157002294364,0.825999387306831,-11.3420871642534));
#95545=CARTESIAN_POINT('Ctrl Pts',(5.46087607647536,-0.26806365938397,-11.3759020335183));
#95546=CARTESIAN_POINT('Ctrl Pts',(5.42015933791027,-1.34399290354479,-11.2528125098426));
#95547=CARTESIAN_POINT('Ctrl Pts',(5.41017075462064,-1.6079386233591,-11.2226163300245));
#95548=CARTESIAN_POINT('Ctrl Pts',(5.40018079084945,-1.87079324599402,-11.1829775503671));
#95549=CARTESIAN_POINT('Ctrl Pts',(5.39018909898668,-2.13190145643179,-11.1337970135774));
#95550=CARTESIAN_POINT('Ctrl Pts',(5.39018544367648,-2.13199697894367,-11.1337790216176));
#95551=CARTESIAN_POINT('Ctrl Pts',(5.39018178836605,-2.13209250122182,-11.1337610283809));
#95552=CARTESIAN_POINT('Ctrl Pts',(5.39017813305539,-2.1321880232662,-11.1337430338671));
#95553=CARTESIAN_POINT('Ctrl Pts',(5.34005511352045,-3.44202287456579,-10.8869953703623));
#95554=CARTESIAN_POINT('Ctrl Pts',(5.28991456891932,-4.70786373365093,-10.4001007459573));
#95555=CARTESIAN_POINT('Ctrl Pts',(5.23975236461588,-5.85487486493485,-9.71395761238606));
#95556=CARTESIAN_POINT('Ctrl Pts',(5.19962465794871,-6.77243673964246,-9.16507123911028));
#95557=CARTESIAN_POINT('Ctrl Pts',(5.15948308710158,-7.61395644577873,-8.48867732473233));
#95558=CARTESIAN_POINT('Ctrl Pts',(5.11932545839374,-8.3411162598051,-7.70569001257604));
#95559=CARTESIAN_POINT('Ctrl Pts',(5.11932451336444,-8.34113337205387,-7.70567158653899));
#95560=CARTESIAN_POINT('Ctrl Pts',(5.11932356833513,-8.34115048423931,-7.70565316044291));
#95561=CARTESIAN_POINT('Ctrl Pts',(5.1193226233058,-8.34116759636142,-7.7056347342878));
#95562=CARTESIAN_POINT('Ctrl Pts',(5.06030728534759,-9.40978805765443,-6.55495533566297));
#95563=CARTESIAN_POINT('Ctrl Pts',(5.00125411221408,-10.2314223980218,-5.17406477254987));
#95564=CARTESIAN_POINT('Ctrl Pts',(4.94216997403342,-10.7485626406966,-3.68783542484532));
#95565=CARTESIAN_POINT('Ctrl Pts',(4.91079087924851,-11.0232115260263,-2.89851136918884));
#95566=CARTESIAN_POINT('Ctrl Pts',(4.87940305062228,-11.2119758229205,-2.0794765216812));
#95567=CARTESIAN_POINT('Ctrl Pts',(4.84800751790959,-11.3062457605422,-1.24943989390665));
#95568=CARTESIAN_POINT('Ctrl Pts',(4.84800722672529,-11.306246634868,-1.24943219556201));
#95569=CARTESIAN_POINT('Ctrl Pts',(4.84800693554099,-11.3062475091857,-1.24942449721643));
#95570=CARTESIAN_POINT('Ctrl Pts',(4.8480066443567,-11.3062483834953,-1.2494167988699));
#95571=CARTESIAN_POINT('Ctrl Pts',(4.75749576470224,-11.5780162292644,1.14351483703349));
#95572=CARTESIAN_POINT('Ctrl Pts',(4.66692016212201,-11.0644284693562,3.62790218399632));
#95573=CARTESIAN_POINT('Ctrl Pts',(4.57624214332606,-9.85962740447419,5.71840762354233));
#95574=CARTESIAN_POINT('Ctrl Pts',(4.57624210922295,-9.85962695136046,5.71840840976068));
#95575=CARTESIAN_POINT('Ctrl Pts',(4.57624207511985,-9.85962649824664,5.71840919597897));
#95576=CARTESIAN_POINT('Ctrl Pts',(4.57624204101675,-9.85962604513272,5.71840998219722));
#95577=CARTESIAN_POINT('Ctrl Pts',(4.48556405918101,-8.65482495242934,7.80891427160857));
#95578=CARTESIAN_POINT('Ctrl Pts',(4.39477592636952,-6.75882245833947,9.50552941330722));
#95579=CARTESIAN_POINT('Ctrl Pts',(4.30397532251536,-4.54410559013394,10.4724028831779));
#95580=CARTESIAN_POINT('Ctrl Pts',(4.30397525127883,-4.54410385260408,10.472403641727));
#95581=CARTESIAN_POINT('Ctrl Pts',(4.30397518004229,-4.54410211507402,10.4724044002757));
#95582=CARTESIAN_POINT('Ctrl Pts',(4.30397510880575,-4.54410037754377,10.4724051588239));
#95583=CARTESIAN_POINT('Ctrl Pts',(4.21317449695879,-2.32938281477614,11.4392775685767));
#95584=CARTESIAN_POINT('Ctrl Pts',(4.12236011008899,0.204050645536416,11.6764109304539));
#95585=CARTESIAN_POINT('Ctrl Pts',(4.03129677776446,2.56543232038823,11.1417036427205));
#95586=CARTESIAN_POINT('Ctrl Pts',(4.03129671431827,2.56543396562396,11.1417032701761));
#95587=CARTESIAN_POINT('Ctrl Pts',(4.03129665087209,2.56543561085961,11.1417028976313));
#95588=CARTESIAN_POINT('Ctrl Pts',(4.03129658742591,2.56543725609518,11.1417025250862));
#95589=CARTESIAN_POINT('Ctrl Pts',(3.96299908741186,4.33647334566173,10.7406712496474));
#95590=CARTESIAN_POINT('Ctrl Pts',(3.89456170172107,6.01072971361824,9.90548016627018));
#95591=CARTESIAN_POINT('Ctrl Pts',(3.82642688347337,7.40108554833901,8.73184202297608));
#95592=CARTESIAN_POINT('Ctrl Pts',(3.82642683651131,7.4010865066444,8.73184121404377));
#95593=CARTESIAN_POINT('Ctrl Pts',(3.82642678954926,7.40108746494964,8.73184040511131));
#95594=CARTESIAN_POINT('Ctrl Pts',(3.82642674258721,7.40108842325476,8.73183959617868));
#95595=CARTESIAN_POINT('Ctrl Pts',(3.75829190713916,8.79144422611794,7.55820068286923));
#95596=CARTESIAN_POINT('Ctrl Pts',(3.6904595686611,9.89789927334666,6.04611449400784));
#95597=CARTESIAN_POINT('Ctrl Pts',(3.6207940229697,10.5960088267933,4.36539634576722));
#95598=CARTESIAN_POINT('Ctrl Pts',(3.62079399296584,10.5960091274581,4.36539562190821));
#95599=CARTESIAN_POINT('Ctrl Pts',(3.62079396296198,10.5960094281229,4.36539489804917));
#95600=CARTESIAN_POINT('Ctrl Pts',(3.62079393295812,10.5960097287876,4.36539417419011));
#95601=CARTESIAN_POINT('Ctrl Pts',(3.55112837455883,11.2941190420186,2.68467561220641));
#95602=CARTESIAN_POINT('Ctrl Pts',(3.47962957405442,11.5838826054181,0.835325224206452));
#95603=CARTESIAN_POINT('Ctrl Pts',(3.42175958283319,11.4318218501684,-0.979655960985377));
#95604=CARTESIAN_POINT('Ctrl Pts',(3.42175956715402,11.4318218089694,-0.979656452732337));
#95605=CARTESIAN_POINT('Ctrl Pts',(3.42175955147486,11.4318217677704,-0.979656944479301));
#95606=CARTESIAN_POINT('Ctrl Pts',(3.42175953579569,11.4318217265713,-0.979657436226255));
#95607=CARTESIAN_POINT('Ctrl Pts',(3.3638895362804,11.2797606907088,-2.79463909454147));
#95608=CARTESIAN_POINT('Ctrl Pts',(3.31964848099095,10.6858751883979,-4.57525165075327));
#95609=CARTESIAN_POINT('Ctrl Pts',(3.26934389910569,9.71592393542433,-6.12115521092141));
#95610=CARTESIAN_POINT('Ctrl Pts',(3.21903931722043,8.74597268245079,-7.66705877108943));
#95611=CARTESIAN_POINT('Ctrl Pts',(3.16267108324328,7.39995562580389,-8.97825315031857));
#95612=CARTESIAN_POINT('Ctrl Pts',(3.1092085985088,5.8273121468005,-9.90727266988443));
#95613=CARTESIAN_POINT('Ctrl Pts',(3.05574611377432,4.25466866779709,-10.8362921894503));
#95614=CARTESIAN_POINT('Ctrl Pts',(3.00518947058605,2.45539879241857,-11.3831369591947));
#95615=CARTESIAN_POINT('Ctrl Pts',(2.95317599819347,0.630199733268789,-11.4865686023698));
#95616=CARTESIAN_POINT('Ctrl Pts',(2.90116252580088,-1.19499932588101,-11.5900002455448));
#95617=CARTESIAN_POINT('Ctrl Pts',(2.84769218566752,-3.04612758015582,-11.2500187197434));
#95618=CARTESIAN_POINT('Ctrl Pts',(2.79488159658331,-4.71660844897229,-10.5035064391955));
#95619=CARTESIAN_POINT('Ctrl Pts',(2.7420710074991,-6.38708931778873,-9.75699415864752));
#95620=CARTESIAN_POINT('Ctrl Pts',(2.68992015353981,-7.87692275998864,-8.60395112887428));
#95621=CARTESIAN_POINT('Ctrl Pts',(2.63743468235449,-9.01931348046436,-7.17271637140658));
#95622=CARTESIAN_POINT('Ctrl Pts',(2.63743467004437,-9.0193137484046,-7.17271603571986));
#95623=CARTESIAN_POINT('Ctrl Pts',(2.63743465773425,-9.01931401634483,-7.17271570003313));
#95624=CARTESIAN_POINT('Ctrl Pts',(2.63743464542413,-9.01931428428504,-7.17271536434638));
#95625=CARTESIAN_POINT('Ctrl Pts',(2.58494918639199,-10.1617045738397,-5.74148081206935));
#95626=CARTESIAN_POINT('Ctrl Pts',(2.53212914832179,-10.9566523403097,-4.03205471200254));
#95627=CARTESIAN_POINT('Ctrl Pts',(2.47942578441284,-11.3149095833295,-2.2345112037788));
#95628=CARTESIAN_POINT('Ctrl Pts',(2.47942576112028,-11.3149097416634,-2.23451040934395));
#95629=CARTESIAN_POINT('Ctrl Pts',(2.47942573782772,-11.3149098999972,-2.23450961490907));
#95630=CARTESIAN_POINT('Ctrl Pts',(2.47942571453516,-11.3149100583309,-2.23450882047418));
#95631=CARTESIAN_POINT('Ctrl Pts',(2.42672236166057,-11.673166841048,-0.436965607195262));
#95632=CARTESIAN_POINT('Ctrl Pts',(2.37413557642947,-11.594733173071,1.44869484258399));
#95633=CARTESIAN_POINT('Ctrl Pts',(2.32146716899691,-11.0874541804838,3.21132484352732));
#95634=CARTESIAN_POINT('Ctrl Pts',(2.32146714047697,-11.0874539057922,3.21132579799139));
#95635=CARTESIAN_POINT('Ctrl Pts',(2.32146711195703,-11.0874536311005,3.21132675245542));
#95636=CARTESIAN_POINT('Ctrl Pts',(2.32146708343709,-11.0874533564087,3.21132770691942));
#95637=CARTESIAN_POINT('Ctrl Pts',(2.26879868115906,-10.5801739498787,4.97395739916155));
#95638=CARTESIAN_POINT('Ctrl Pts',(2.21604875089909,-9.64404943021566,6.61355667467342));
#95639=CARTESIAN_POINT('Ctrl Pts',(2.16330110871024,-8.38328705927666,7.94836318859917));
#95640=CARTESIAN_POINT('Ctrl Pts',(2.1633010790123,-8.38328634944304,7.94836394012108));
#95641=CARTESIAN_POINT('Ctrl Pts',(2.16330104931436,-8.38328563960932,7.94836469164289));
#95642=CARTESIAN_POINT('Ctrl Pts',(2.16330101961641,-8.38328492977549,7.9483654431646));
#95643=CARTESIAN_POINT('Ctrl Pts',(2.1105533785651,-7.12252222041275,9.28317158515742));
#95644=CARTESIAN_POINT('Ctrl Pts',(2.05780789908406,-5.53712179696833,10.3131846727588));
#95645=CARTESIAN_POINT('Ctrl Pts',(2.00503741874543,-3.8029092346673,10.9196062470078));
#95646=CARTESIAN_POINT('Ctrl Pts',(1.9522669689543,-2.06869767625853,11.5260274702144));
#95647=CARTESIAN_POINT('Ctrl Pts',(1.89947155499029,-0.185674043531211,
11.7088577069818));
#95648=CARTESIAN_POINT('Ctrl Pts',(1.84664003082162,1.63475428012898,11.4539068979886));
#95649=CARTESIAN_POINT('Ctrl Pts',(1.84663997049356,1.634756358867,11.4539066068616));
#95650=CARTESIAN_POINT('Ctrl Pts',(1.84663991016551,1.63475843760494,11.4539063157339));
#95651=CARTESIAN_POINT('Ctrl Pts',(1.84663984983746,1.6347605163428,11.4539060246057));
#95652=CARTESIAN_POINT('Ctrl Pts',(1.79380839845376,3.45518618623734,11.1989545674529));
#95653=CARTESIAN_POINT('Ctrl Pts',(1.74094090272129,5.21301617918042,10.5062232930386));
#95654=CARTESIAN_POINT('Ctrl Pts',(1.68809114646529,6.71448492712146,9.43804832595781));
#95655=CARTESIAN_POINT('Ctrl Pts',(1.68809101322363,6.71448871253515,9.43804563293862));
#95656=CARTESIAN_POINT('Ctrl Pts',(1.68809087998197,6.71449249794722,9.43804293991704));
#95657=CARTESIAN_POINT('Ctrl Pts',(1.68809074674031,6.71449628335766,9.43804024689308));
#95658=CARTESIAN_POINT('Ctrl Pts',(1.63524099091071,8.21596372907952,8.36986339353148));
#95659=CARTESIAN_POINT('Ctrl Pts',(1.58240874757455,9.46106908054857,6.92624306034315));
#95660=CARTESIAN_POINT('Ctrl Pts',(1.52945999603721,10.3045992775066,5.30076081748356));
#95661=CARTESIAN_POINT('Ctrl Pts',(1.52945986220838,10.3046014095429,5.30075670905086));
#95662=CARTESIAN_POINT('Ctrl Pts',(1.52945972837956,10.3046035415765,5.30075260061701));
#95663=CARTESIAN_POINT('Ctrl Pts',(1.52945959455073,10.3046056736076,5.30074849218199));
#95664=CARTESIAN_POINT('Ctrl Pts',(1.47651070859563,11.1481359726256,3.67526122157152));
#95665=CARTESIAN_POINT('Ctrl Pts',(1.42344639163322,11.5900913133187,1.86791206070984));
#95666=CARTESIAN_POINT('Ctrl Pts',(1.37078399030106,11.5968559808931,-0.0151246218382906));
#95667=CARTESIAN_POINT('Ctrl Pts',(20.6563591733144,-11.5926712737699,-0.0152754849923014));
#95668=CARTESIAN_POINT('Ctrl Pts',(20.6037145486049,-11.585908889594,1.86712555758729));
#95669=CARTESIAN_POINT('Ctrl Pts',(20.5506704336544,-11.1441131812359,3.67379159074529));
#95670=CARTESIAN_POINT('Ctrl Pts',(20.4977411586544,-10.3008921028426,5.29867567785781));
#95671=CARTESIAN_POINT('Ctrl Pts',(20.4977410246894,-10.3008899686352,5.29867979046809));
#95672=CARTESIAN_POINT('Ctrl Pts',(20.4977408907245,-10.3008878344252,5.29868390307719));
#95673=CARTESIAN_POINT('Ctrl Pts',(20.4977407567596,-10.3008857002126,5.29868801568514));
#95674=CARTESIAN_POINT('Ctrl Pts',(20.4448116163112,-9.4576647239953,6.92356707000062));
#95675=CARTESIAN_POINT('Ctrl Pts',(20.3919983869448,-8.21301820129604,8.36666416537622));
#95676=CARTESIAN_POINT('Ctrl Pts',(20.3391682146961,-6.71210990886197,9.43444527360875));
#95677=CARTESIAN_POINT('Ctrl Pts',(20.33916808131,-6.71210611935304,9.43444796955364));
#95678=CARTESIAN_POINT('Ctrl Pts',(20.3391679479238,-6.7121023298424,9.4344506654962));
#95679=CARTESIAN_POINT('Ctrl Pts',(20.3391678145376,-6.7120985403302,9.4344533614363));
#95680=CARTESIAN_POINT('Ctrl Pts',(20.286337641874,-5.21118894454904,10.5022325811003));
#95681=CARTESIAN_POINT('Ctrl Pts',(20.2334903071855,-3.45401843924274,11.1946955874164));
#95682=CARTESIAN_POINT('Ctrl Pts',(20.1806788768804,-1.63428162441622,11.4495487431153));
#95683=CARTESIAN_POINT('Ctrl Pts',(20.1806788168593,-1.63427955625594,11.44954903276));
#95684=CARTESIAN_POINT('Ctrl Pts',(20.1806787568383,-1.63427748809554,11.4495493224042));
#95685=CARTESIAN_POINT('Ctrl Pts',(20.1806786968172,-1.6342754199351,11.4495496120478));
#95686=CARTESIAN_POINT('Ctrl Pts',(20.127867193276,0.185464063436388,11.7044021268553));
#95687=CARTESIAN_POINT('Ctrl Pts',(20.0750916629277,2.06776954364581,11.5216435485773));
#95688=CARTESIAN_POINT('Ctrl Pts',(20.0223414858343,3.80131493537512,10.9154560212435));
#95689=CARTESIAN_POINT('Ctrl Pts',(19.9695912794199,5.53486129069071,10.309268156962));
#95690=CARTESIAN_POINT('Ctrl Pts',(19.9168664069274,7.1196474471959,9.27965093289917));
#95691=CARTESIAN_POINT('Ctrl Pts',(19.8641392593043,8.37991863116215,7.94536453312017));
#95692=CARTESIAN_POINT('Ctrl Pts',(19.8641392286874,8.37991936295992,7.94536375834421));
#95693=CARTESIAN_POINT('Ctrl Pts',(19.8641391980705,8.37992009475757,7.94536298356816));
#95694=CARTESIAN_POINT('Ctrl Pts',(19.8641391674536,8.37992082655512,7.945362208792));
#95695=CARTESIAN_POINT('Ctrl Pts',(19.8114120255027,9.64019149801263,6.61107559879492));
#95696=CARTESIAN_POINT('Ctrl Pts',(19.7586826779208,10.5759470416542,4.9721199710173));
#95697=CARTESIAN_POINT('Ctrl Pts',(19.7060352623099,11.0830256424956,3.21018842377476));
#95698=CARTESIAN_POINT('Ctrl Pts',(19.7060352260731,11.0830259915146,3.2101872110484));
#95699=CARTESIAN_POINT('Ctrl Pts',(19.7060351898362,11.0830263405333,3.210185998322));
#95700=CARTESIAN_POINT('Ctrl Pts',(19.7060351535993,11.0830266895519,3.21018478559552));
#95701=CARTESIAN_POINT('Ctrl Pts',(19.6533877226761,11.5901048488513,1.44825255283667));
#95702=CARTESIAN_POINT('Ctrl Pts',(19.6008218004355,11.6685061651627,-0.436655556151005));
#95703=CARTESIAN_POINT('Ctrl Pts',(19.5481397518776,11.3103928857645,-2.2334789716602));
#95704=CARTESIAN_POINT('Ctrl Pts',(19.5481397310522,11.3103927442013,-2.23347968194976));
#95705=CARTESIAN_POINT('Ctrl Pts',(19.5481397102268,11.310392602638,-2.23348039223931));
#95706=CARTESIAN_POINT('Ctrl Pts',(19.5481396894015,11.3103924610746,-2.23348110252884));
#95707=CARTESIAN_POINT('Ctrl Pts',(19.4954576505601,10.9522789032391,-4.03030411386188));
#95708=CARTESIAN_POINT('Ctrl Pts',(19.4426589642928,10.1576489530311,-5.73904072781481));
#95709=CARTESIAN_POINT('Ctrl Pts',(19.3901948846326,9.01572496391351,-7.16969094962721));
#95710=CARTESIAN_POINT('Ctrl Pts',(19.3901948541255,9.01572429990197,-7.16969178152869));
#95711=CARTESIAN_POINT('Ctrl Pts',(19.3901948236184,9.01572363589031,-7.16969261343008));
#95712=CARTESIAN_POINT('Ctrl Pts',(19.3901947931114,9.01572297187853,-7.16969344533137));
#95713=CARTESIAN_POINT('Ctrl Pts',(19.3377306833332,7.87379791485763,-8.60034417564005));
#95714=CARTESIAN_POINT('Ctrl Pts',(19.2855977093484,6.3845758633306,-9.75290960514574));
#95715=CARTESIAN_POINT('Ctrl Pts',(19.2328105722069,4.71478199691756,-10.4991167385146));
#95716=CARTESIAN_POINT('Ctrl Pts',(19.2328105576676,4.71478153700262,-10.4991169440441));
#95717=CARTESIAN_POINT('Ctrl Pts',(19.2328105431283,4.71478107708768,-10.4991171495735));
#95718=CARTESIAN_POINT('Ctrl Pts',(19.232810528589,4.71478061717272,-10.4991173551029));
#95719=CARTESIAN_POINT('Ctrl Pts',(19.1800234056227,3.0449871112073,-11.2453240590873));
#95720=CARTESIAN_POINT('Ctrl Pts',(19.126575436485,1.19462796304064,-11.5851614135244));
#95721=CARTESIAN_POINT('Ctrl Pts',(19.0745838253278,-0.629806639099064,
-11.4817745800324));
#95722=CARTESIAN_POINT('Ctrl Pts',(19.0745837795721,-0.629808244709866,
-11.4817744890458));
#95723=CARTESIAN_POINT('Ctrl Pts',(19.0745837338164,-0.62980985032067,-11.4817743980589));
#95724=CARTESIAN_POINT('Ctrl Pts',(19.0745836880607,-0.629811455931433,
-11.4817743070717));
#95725=CARTESIAN_POINT('Ctrl Pts',(19.0353427236988,-2.00681388582104,-11.4037419135721));
#95726=CARTESIAN_POINT('Ctrl Pts',(18.9969205011456,-3.36905776993691,-11.0732077906153));
#95727=CARTESIAN_POINT('Ctrl Pts',(18.9574625391331,-4.63027157441452,-10.5165193993473));
#95728=CARTESIAN_POINT('Ctrl Pts',(18.9446414170003,-5.04007926335718,-10.3356339838239));
#95729=CARTESIAN_POINT('Ctrl Pts',(18.9317109342901,-5.43922050625814,-10.1308713769124));
#95730=CARTESIAN_POINT('Ctrl Pts',(18.9186074542421,-5.82473675705504,-9.9031359251377));
#95731=CARTESIAN_POINT('Ctrl Pts',(18.8866679432054,-6.76442609927844,-9.34803461245184));
#95732=CARTESIAN_POINT('Ctrl Pts',(18.8536879756499,-7.62314728010116,-8.65644218333828));
#95733=CARTESIAN_POINT('Ctrl Pts',(18.8215823250737,-8.36902821121461,-7.85982151710422));
#95734=CARTESIAN_POINT('Ctrl Pts',(18.7999795800723,-8.87090483626633,-7.32380393743614));
#95735=CARTESIAN_POINT('Ctrl Pts',(18.7787726604597,-9.32169308761486,-6.7402340793714));
#95736=CARTESIAN_POINT('Ctrl Pts',(18.7585450056109,-9.71167301288714,-6.11868848475595));
#95737=CARTESIAN_POINT('Ctrl Pts',(18.7585444020376,-9.71168464950343,-6.11866993844851));
#95738=CARTESIAN_POINT('Ctrl Pts',(18.7585437984652,-9.71169628606556,-6.11865139210728));
#95739=CARTESIAN_POINT('Ctrl Pts',(18.7585431948937,-9.71170792257357,-6.1186328457322));
#95740=CARTESIAN_POINT('Ctrl Pts',(18.7348347109139,-10.1687937088616,-5.39012525343856));
#95741=CARTESIAN_POINT('Ctrl Pts',(18.7124730873212,-10.5423427757897,-4.60943846859312));
#95742=CARTESIAN_POINT('Ctrl Pts',(18.689397148694,-10.8254413080832,-3.79760667526428));
#95743=CARTESIAN_POINT('Ctrl Pts',(18.6666931274324,-11.1039771111179,-2.99885926159179));
#95744=CARTESIAN_POINT('Ctrl Pts',(18.6432974588946,-11.2949540425782,-2.16996449215795));
#95745=CARTESIAN_POINT('Ctrl Pts',(18.6172478588867,-11.3918346917951,-1.33096655160278));
#95746=CARTESIAN_POINT('Ctrl Pts',(18.6136145412749,-11.4053473049997,-1.21394571470871));
#95747=CARTESIAN_POINT('Ctrl Pts',(18.6099295983133,-11.4170294700437,-1.0967283249332));
#95748=CARTESIAN_POINT('Ctrl Pts',(18.6061877098378,-11.4268635310544,-0.979368755714328));
#95749=CARTESIAN_POINT('Ctrl Pts',(18.6061870500506,-11.4268652650419,-0.979348062328425));
#95750=CARTESIAN_POINT('Ctrl Pts',(18.6061863902616,-11.4268669989719,-0.979327368938115));
#95751=CARTESIAN_POINT('Ctrl Pts',(18.6061857304709,-11.4268687328444,-0.979306675543372));
#95752=CARTESIAN_POINT('Ctrl Pts',(18.5834005247388,-11.4867462659404,-0.264681229497011));
#95753=CARTESIAN_POINT('Ctrl Pts',(18.5584830336108,-11.478078130921,0.455221826164347));
#95754=CARTESIAN_POINT('Ctrl Pts',(18.5323945625552,-11.4029360819467,1.16806210182922));
#95755=CARTESIAN_POINT('Ctrl Pts',(18.5066208390778,-11.3287005934944,1.87230222802751));
#95756=CARTESIAN_POINT('Ctrl Pts',(18.4797041152464,-11.1895856521491,2.56965049513616));
#95757=CARTESIAN_POINT('Ctrl Pts',(18.452570095882,-10.9875404649071,3.24821661673467));
#95758=CARTESIAN_POINT('Ctrl Pts',(18.4374500639232,-10.8749537652667,3.62633757651284));
#95759=CARTESIAN_POINT('Ctrl Pts',(18.4222625456683,-10.7428256417688,3.99862650688148));
#95760=CARTESIAN_POINT('Ctrl Pts',(18.4071677397897,-10.591486415767,4.36302445712109));
#95761=CARTESIAN_POINT('Ctrl Pts',(18.4071644116394,-10.5914530480183,4.3631048007276));
#95762=CARTESIAN_POINT('Ctrl Pts',(18.4071610834933,-10.5914196793356,4.36318514394952));
#95763=CARTESIAN_POINT('Ctrl Pts',(18.4071577553514,-10.5913863097188,4.36326548678688));
#95764=CARTESIAN_POINT('Ctrl Pts',(18.3820082452178,-10.3392247339024,4.97038592893616));
#95765=CARTESIAN_POINT('Ctrl Pts',(18.3570973782381,-10.0337233596071,5.55554420614552));
#95766=CARTESIAN_POINT('Ctrl Pts',(18.3323202199419,-9.68078489052606,6.11065375339466));
#95767=CARTESIAN_POINT('Ctrl Pts',(18.3079231460669,-9.3332605376296,6.65724785716777));
#95768=CARTESIAN_POINT('Ctrl Pts',(18.2836556957903,-8.93974412258217,7.17470688012032));
#95769=CARTESIAN_POINT('Ctrl Pts',(18.2594178245586,-8.50591348580286,7.65533477953397));
#95770=CARTESIAN_POINT('Ctrl Pts',(18.2401528907354,-8.16109283599554,8.03735119456104));
#95771=CARTESIAN_POINT('Ctrl Pts',(18.2209066430271,-7.79080458210409,8.39609973384926));
#95772=CARTESIAN_POINT('Ctrl Pts',(18.2016290017132,-7.39791434534383,8.72773455289831));
#95773=CARTESIAN_POINT('Ctrl Pts',(18.2016255775624,-7.39784455903638,8.72779345884017));
#95774=CARTESIAN_POINT('Ctrl Pts',(18.2016221534106,-7.39777477201591,8.72785236392661));
#95775=CARTESIAN_POINT('Ctrl Pts',(18.2016187292579,-7.39770498428236,8.72791126815769));
#95776=CARTESIAN_POINT('Ctrl Pts',(18.1823945443621,-7.00589644234068,9.05861667612544));
#95777=CARTESIAN_POINT('Ctrl Pts',(18.163049995771,-6.59146899869525,9.36233212467602));
#95778=CARTESIAN_POINT('Ctrl Pts',(18.1436704590147,-6.15866743141592,9.63698434701735));
#95779=CARTESIAN_POINT('Ctrl Pts',(18.1243556225998,-5.72731081142756,9.91071961800122));
#95780=CARTESIAN_POINT('Ctrl Pts',(18.105006048155,-5.27770302579153,10.1555864360692));
#95781=CARTESIAN_POINT('Ctrl Pts',(18.0857040287375,-4.8139995903071,10.3695537217475));
#95782=CARTESIAN_POINT('Ctrl Pts',(18.0666496124358,-4.35624446587525,10.5807762704389));
#95783=CARTESIAN_POINT('Ctrl Pts',(18.0476414992938,-3.88475311646732,10.7618881686774));
#95784=CARTESIAN_POINT('Ctrl Pts',(18.028756860855,-3.40347319721907,10.9109396938641));
#95785=CARTESIAN_POINT('Ctrl Pts',(18.017902919585,-3.12685768271607,10.9966070210848));
#95786=CARTESIAN_POINT('Ctrl Pts',(18.0070897307925,-2.84700769423683,11.0716836019147));
#95787=CARTESIAN_POINT('Ctrl Pts',(17.9963317599933,-2.56466511419696,11.135797362719));
#95788=CARTESIAN_POINT('Ctrl Pts',(17.9963311846464,-2.56465001423521,11.1358007915867));
#95789=CARTESIAN_POINT('Ctrl Pts',(17.9963306092995,-2.56463491426632,11.135804220423));
#95790=CARTESIAN_POINT('Ctrl Pts',(17.9963300339529,-2.56461981429031,11.1358076492279));
#95791=CARTESIAN_POINT('Ctrl Pts',(17.9768958491772,-2.05456952995011,11.2516265701319));
#95792=CARTESIAN_POINT('Ctrl Pts',(17.9574004091647,-1.53644606554202,11.331299040876));
#95793=CARTESIAN_POINT('Ctrl Pts',(17.9378512061723,-1.0153381659182,11.3752735917127));
#95794=CARTESIAN_POINT('Ctrl Pts',(17.9234700491171,-0.631990847352272,
11.4076229883742));
#95795=CARTESIAN_POINT('Ctrl Pts',(17.9090597997092,-0.247028601760643,
11.4206550469504));
#95796=CARTESIAN_POINT('Ctrl Pts',(17.8946234605342,0.137526945126385,11.414565855171));
#95797=CARTESIAN_POINT('Ctrl Pts',(17.8794344836361,0.542131273611075,11.408159203724));
#95798=CARTESIAN_POINT('Ctrl Pts',(17.8642540867261,0.946288682112462,11.3806441565564));
#95799=CARTESIAN_POINT('Ctrl Pts',(17.8490764860305,1.34782593038233,11.3322244716497));
#95800=CARTESIAN_POINT('Ctrl Pts',(17.8339924594865,1.74688758925703,11.2841033076374));
#95801=CARTESIAN_POINT('Ctrl Pts',(17.8189111952324,2.14336221523588,11.2153343458876));
#95802=CARTESIAN_POINT('Ctrl Pts',(17.8038270235645,2.53510906264001,11.1260671287608));
#95803=CARTESIAN_POINT('Ctrl Pts',(17.8000535704286,2.63310836962008,11.103736060949));
#95804=CARTESIAN_POINT('Ctrl Pts',(17.7962799353667,2.73081173799778,11.0801219712589));
#95805=CARTESIAN_POINT('Ctrl Pts',(17.7925060296454,2.82818547696053,11.055226717161));
#95806=CARTESIAN_POINT('Ctrl Pts',(17.7828056836779,3.07847232190678,10.9912366242605));
#95807=CARTESIAN_POINT('Ctrl Pts',(17.7728937466464,3.32652271866186,10.9184862906763));
#95808=CARTESIAN_POINT('Ctrl Pts',(17.7629110876035,3.57174719113817,10.8372136533684));
#95809=CARTESIAN_POINT('Ctrl Pts',(17.7553786878304,3.75678093344116,10.775889511956));
#95810=CARTESIAN_POINT('Ctrl Pts',(17.7478060134944,3.94020683028634,10.7097132161103));
#95811=CARTESIAN_POINT('Ctrl Pts',(17.7402525390214,4.12179077946943,10.6387825823858));
#95812=CARTESIAN_POINT('Ctrl Pts',(17.7343980689171,4.26253101837736,10.5838063888335));
#95813=CARTESIAN_POINT('Ctrl Pts',(17.7285938577166,4.40218261181708,10.5260274920075));
#95814=CARTESIAN_POINT('Ctrl Pts',(17.7228420832576,4.54061669736803,10.465461273219));
#95815=CARTESIAN_POINT('Ctrl Pts',(17.7156518837169,4.71367089228399,10.389748429884));
#95816=CARTESIAN_POINT('Ctrl Pts',(17.7085436164182,4.88482235323807,10.3096796974154));
#95817=CARTESIAN_POINT('Ctrl Pts',(17.7015219415102,5.05388155833274,10.2254292304244));
#95818=CARTESIAN_POINT('Ctrl Pts',(17.6871005257297,5.40110257327522,10.0523920234788));
#95819=CARTESIAN_POINT('Ctrl Pts',(17.6727915987991,5.73922499208294,9.86143185706003));
#95820=CARTESIAN_POINT('Ctrl Pts',(17.6584917271518,6.06671669227161,9.65383289905655));
#95821=CARTESIAN_POINT('Ctrl Pts',(17.6441416360901,6.39535850357742,9.44550487870013));
#95822=CARTESIAN_POINT('Ctrl Pts',(17.6298006652466,6.71329440145111,9.22041996616636));
#95823=CARTESIAN_POINT('Ctrl Pts',(17.6153658278202,7.0189267110527,8.97989280350298));
#95824=CARTESIAN_POINT('Ctrl Pts',(17.6063665968301,7.20946960882593,8.82993895004162));
#95825=CARTESIAN_POINT('Ctrl Pts',(17.597330904034,7.39522944235641,8.67398348006849));
#95826=CARTESIAN_POINT('Ctrl Pts',(17.5882342232595,7.57581058956664,8.5123507333688));
#95827=CARTESIAN_POINT('Ctrl Pts',(17.570801635833,7.92187051124135,8.20260291900894));
#95828=CARTESIAN_POINT('Ctrl Pts',(17.5532521221025,8.24925679949015,7.87193935681038));
#95829=CARTESIAN_POINT('Ctrl Pts',(17.5356012364988,8.55538584983627,7.52267230287006));
#95830=CARTESIAN_POINT('Ctrl Pts',(17.5188462385182,8.84597702670678,7.19113263313973));
#95831=CARTESIAN_POINT('Ctrl Pts',(17.5019999135686,9.11741460146095,6.8428292824108));
#95832=CARTESIAN_POINT('Ctrl Pts',(17.4850755148002,9.36745291600106,6.47971529953186));
#95833=CARTESIAN_POINT('Ctrl Pts',(17.4734938848635,9.53855803285768,6.23123073992728));
#95834=CARTESIAN_POINT('Ctrl Pts',(17.4620681140206,9.69985748204413,5.97600618604054));
#95835=CARTESIAN_POINT('Ctrl Pts',(17.4508315775933,9.85063309773795,5.71477009049237));
#95836=CARTESIAN_POINT('Ctrl Pts',(17.445209014683,9.92607853326528,5.58405219613394));
#95837=CARTESIAN_POINT('Ctrl Pts',(17.4396338452531,9.99888949830509,5.45182917745403));
#95838=CARTESIAN_POINT('Ctrl Pts',(17.4341103385296,10.0690450450509,5.31822958070305));
#95839=CARTESIAN_POINT('Ctrl Pts',(17.4253224355891,10.1806625674672,5.10567253173293));
#95840=CARTESIAN_POINT('Ctrl Pts',(17.4166052134124,10.2854698674235,4.88959849063566));
#95841=CARTESIAN_POINT('Ctrl Pts',(17.407821599972,10.3831861088303,4.67040458670955));
#95842=CARTESIAN_POINT('Ctrl Pts',(17.4000512154975,10.4696303461929,4.47649567672039));
#95843=CARTESIAN_POINT('Ctrl Pts',(17.3922288216349,10.5505245652096,4.28014573517023));
#95844=CARTESIAN_POINT('Ctrl Pts',(17.3842603515511,10.6256619800217,4.08166139633652));
#95845=CARTESIAN_POINT('Ctrl Pts',(17.3694478756162,10.7653338539217,3.7127016761487));
#95846=CARTESIAN_POINT('Ctrl Pts',(17.3546425838804,10.8858945263555,3.33657659901067));
#95847=CARTESIAN_POINT('Ctrl Pts',(17.3398311092709,10.9869532301011,2.95529661764224));
#95848=CARTESIAN_POINT('Ctrl Pts',(17.3250017259557,11.0881341249612,2.57355562674091));
#95849=CARTESIAN_POINT('Ctrl Pts',(17.3101661438342,11.1697659678492,2.18664632400007));
#95850=CARTESIAN_POINT('Ctrl Pts',(17.2953111696126,11.2314054174755,1.7965788629401));
#95851=CARTESIAN_POINT('Ctrl Pts',(17.2909948894645,11.2493154541267,1.6832403667923));
#95852=CARTESIAN_POINT('Ctrl Pts',(17.2866769736132,11.2655372811745,1.56963524128526));
#95853=CARTESIAN_POINT('Ctrl Pts',(17.2823571021727,11.2800591949974,1.45581285081457));
#95854=CARTESIAN_POINT('Ctrl Pts',(17.269239278253,11.3241567824215,1.1101770843575));
#95855=CARTESIAN_POINT('Ctrl Pts',(17.2560129092754,11.3524343047511,0.762525396881152));
#95856=CARTESIAN_POINT('Ctrl Pts',(17.2427740669595,11.3647067757544,0.414395378551398));
#95857=CARTESIAN_POINT('Ctrl Pts',(17.2295616876319,11.3769547154392,0.0669612338036552));
#95858=CARTESIAN_POINT('Ctrl Pts',(17.2163368990233,11.3732623098732,-0.280949084064888));
#95859=CARTESIAN_POINT('Ctrl Pts',(17.2031927160801,11.3534609095458,-0.627856637969633));
#95860=CARTESIAN_POINT('Ctrl Pts',(17.195334121398,11.3416221227621,-0.835264422088129));
#95861=CARTESIAN_POINT('Ctrl Pts',(17.1875042852075,11.3240253214374,-1.04231473548696));
#95862=CARTESIAN_POINT('Ctrl Pts',(17.179722732406,11.3006352045343,-1.2487003895174));
#95863=CARTESIAN_POINT('Ctrl Pts',(17.1797220690039,11.3006332104526,-1.24871798454966));
#95864=CARTESIAN_POINT('Ctrl Pts',(17.1797214056021,11.3006312163286,-1.24873557957695));
#95865=CARTESIAN_POINT('Ctrl Pts',(17.1797207422005,11.3006292221623,-1.24875317459922));
#95866=CARTESIAN_POINT('Ctrl Pts',(17.1664171336884,11.2606389538955,-1.60159720896684));
#95867=CARTESIAN_POINT('Ctrl Pts',(17.1532153799316,11.2036540450757,-1.95243587269292));
#95868=CARTESIAN_POINT('Ctrl Pts',(17.1400310196288,11.1302347366909,-2.29979918441093));
#95869=CARTESIAN_POINT('Ctrl Pts',(17.1268509988193,11.0568395934985,-2.64704816515195));
#95870=CARTESIAN_POINT('Ctrl Pts',(17.1136883759637,10.9670201751712,-2.99082366113072));
#95871=CARTESIAN_POINT('Ctrl Pts',(17.1004602987123,10.8613632646006,-3.32961276547741));
#95872=CARTESIAN_POINT('Ctrl Pts',(17.093264264523,10.8038862234286,-3.51391301800193));
#95873=CARTESIAN_POINT('Ctrl Pts',(17.0860488828582,10.7417228848526,-3.69673689788994));
#95874=CARTESIAN_POINT('Ctrl Pts',(17.0788010422857,10.6749721170883,-3.87783609052177));
#95875=CARTESIAN_POINT('Ctrl Pts',(17.0618512862622,10.5188691762622,-4.30135356452081));
#95876=CARTESIAN_POINT('Ctrl Pts',(17.0449116121264,10.3379612816245,-4.71558713436491));
#95877=CARTESIAN_POINT('Ctrl Pts',(17.0279776992362,10.1336467949107,-5.11775193322988));
#95878=CARTESIAN_POINT('Ctrl Pts',(17.0147660258491,9.97424262859502,-5.43151698002458));
#95879=CARTESIAN_POINT('Ctrl Pts',(17.0015577606713,9.80059010964242,-5.73793916776007));
#95880=CARTESIAN_POINT('Ctrl Pts',(16.9883050898332,9.61323203514672,-6.03569643286859));
#95881=CARTESIAN_POINT('Ctrl Pts',(16.9845712997621,9.56044601738282,-6.11958617355713));
#95882=CARTESIAN_POINT('Ctrl Pts',(16.9808339915489,9.50657195391244,-6.20278783938413));
#95883=CARTESIAN_POINT('Ctrl Pts',(16.9770921125338,9.45162167652532,-6.28527117954114));
#95884=CARTESIAN_POINT('Ctrl Pts',(16.9608377334333,9.21292271359193,-6.6435712408139));
#95885=CARTESIAN_POINT('Ctrl Pts',(16.9446245873696,8.95405231378699,-6.98850040250276));
#95886=CARTESIAN_POINT('Ctrl Pts',(16.9284389646338,8.67621779025595,-7.31739009469023));
#95887=CARTESIAN_POINT('Ctrl Pts',(16.9220180229297,8.56599902956192,-7.44786277251745));
#95888=CARTESIAN_POINT('Ctrl Pts',(16.9156014195238,8.45279634404502,-7.57581128912845));
#95889=CARTESIAN_POINT('Ctrl Pts',(16.9091883236421,8.33668733010234,-7.70106952046181));
#95890=CARTESIAN_POINT('Ctrl Pts',(16.8931331960915,8.0460094635932,-8.01465236997828));
#95891=CARTESIAN_POINT('Ctrl Pts',(16.8771000186673,7.73711305391114,-8.31137203881411));
#95892=CARTESIAN_POINT('Ctrl Pts',(16.8610758846774,7.4124119890984,-8.58963890716383));
#95893=CARTESIAN_POINT('Ctrl Pts',(16.845044908476,7.08757227883031,-8.86802459383862));
#95894=CARTESIAN_POINT('Ctrl Pts',(16.8290229844305,6.74691507681148,-9.12794100812106));
#95895=CARTESIAN_POINT('Ctrl Pts',(16.8129976534456,6.39289795770402,-9.36782843649133));
#95896=CARTESIAN_POINT('Ctrl Pts',(16.8000012737082,6.10579369022996,-9.56237469055983));
#95897=CARTESIAN_POINT('Ctrl Pts',(16.7870026607976,5.8099034735611,-9.74374822440784));
#95898=CARTESIAN_POINT('Ctrl Pts',(16.7739953989264,5.50655304996275,-9.91113745714248));
#95899=CARTESIAN_POINT('Ctrl Pts',(16.7589630605645,5.15597456120005,-10.1045872092515));
#95900=CARTESIAN_POINT('Ctrl Pts',(16.7439297861409,4.79518685920721,-10.2795409072731));
#95901=CARTESIAN_POINT('Ctrl Pts',(16.7288930927054,4.42613322613574,-10.4347396739405));
#95902=CARTESIAN_POINT('Ctrl Pts',(16.7059890749003,3.86398763081691,-10.6711397395757));
#95903=CARTESIAN_POINT('Ctrl Pts',(16.6830771012879,3.28266179623832,-10.8617032120053));
#95904=CARTESIAN_POINT('Ctrl Pts',(16.660149213089,2.68995422151479,-11.0047568660834));
#95905=CARTESIAN_POINT('Ctrl Pts',(16.6366666976463,2.08290900846487,-11.1512709982133));
#95906=CARTESIAN_POINT('Ctrl Pts',(16.613167482723,1.46392562965263,-11.2479482536141));
#95907=CARTESIAN_POINT('Ctrl Pts',(16.5896435621228,0.841421641600292,-11.29302792262));
#95908=CARTESIAN_POINT('Ctrl Pts',(16.583381022206,0.675698582941044,-11.3050290355034));
#95909=CARTESIAN_POINT('Ctrl Pts',(16.5771167345246,0.509726175893628,-11.3133734986216));
#95910=CARTESIAN_POINT('Ctrl Pts',(16.5708505551953,0.343663562097396,-11.3180286219251));
#95911=CARTESIAN_POINT('Ctrl Pts',(16.563309919019,0.143826039527265,-11.3236305348842));
#95912=CARTESIAN_POINT('Ctrl Pts',(16.555780015154,-0.0561365062592693,
-11.3239139818911));
#95913=CARTESIAN_POINT('Ctrl Pts',(16.5482589551089,-0.255950842440518,
-11.3188205116742));
#95914=CARTESIAN_POINT('Ctrl Pts',(16.5254989223572,-0.860623695532547,
-11.3034067869783));
#95915=CARTESIAN_POINT('Ctrl Pts',(16.5028197022815,-1.46394306304044,-11.2387517590465));
#95916=CARTESIAN_POINT('Ctrl Pts',(16.4801704660534,-2.05826210501978,-11.1267611656254));
#95917=CARTESIAN_POINT('Ctrl Pts',(16.4577078735389,-2.64768359054951,-11.0156934439522));
#95918=CARTESIAN_POINT('Ctrl Pts',(16.4352747935128,-3.22825166601579,-10.8580657122636));
#95919=CARTESIAN_POINT('Ctrl Pts',(16.4128237642916,-3.79246292298964,-10.6557613845628));
#95920=CARTESIAN_POINT('Ctrl Pts',(16.3980607989102,-4.16346735100046,-10.522733550653));
#95921=CARTESIAN_POINT('Ctrl Pts',(16.3832901110842,-4.52739834561009,-10.3703885974072));
#95922=CARTESIAN_POINT('Ctrl Pts',(16.3684987026711,-4.88211519408174,-10.1992720087013));
#95923=CARTESIAN_POINT('Ctrl Pts',(16.3684981996459,-4.88212725726756,-10.1992661893803));
#95924=CARTESIAN_POINT('Ctrl Pts',(16.3684976966207,-4.8821393204427,-10.1992603700376));
#95925=CARTESIAN_POINT('Ctrl Pts',(16.3684971935955,-4.88215138360721,-10.1992545506731));
#95926=CARTESIAN_POINT('Ctrl Pts',(16.3510590516397,-5.30033950116647,-9.99751734883505));
#95927=CARTESIAN_POINT('Ctrl Pts',(16.3334957030325,-5.70581057641984,-9.76945707877262));
#95928=CARTESIAN_POINT('Ctrl Pts',(16.3158833545317,-6.09580305607242,-9.51735400966098));
#95929=CARTESIAN_POINT('Ctrl Pts',(16.298271006031,-6.485795535725,-9.26525094054935));
#95930=CARTESIAN_POINT('Ctrl Pts',(16.2806097240013,-6.86031024912703,-8.98910619483964));
#95931=CARTESIAN_POINT('Ctrl Pts',(16.2629726827512,-7.21663392926645,-8.69116642701088));
#95932=CARTESIAN_POINT('Ctrl Pts',(16.2483995158922,-7.51105771457272,-8.44498420807137));
#95933=CARTESIAN_POINT('Ctrl Pts',(16.2339252337094,-7.79315311500984,-8.18404924571618));
#95934=CARTESIAN_POINT('Ctrl Pts',(16.2195735026631,-8.06130761505714,-7.90967958982998));
#95935=CARTESIAN_POINT('Ctrl Pts',(16.2089571825821,-8.25966793789824,-7.70672176697118));
#95936=CARTESIAN_POINT('Ctrl Pts',(16.1984079167211,-8.45040074228537,-7.49641327831099));
#95937=CARTESIAN_POINT('Ctrl Pts',(16.1879354848093,-8.63287033435264,-7.27929465333164));
#95938=CARTESIAN_POINT('Ctrl Pts',(16.1855091838064,-8.67514572539506,-7.22899161560571));
#95939=CARTESIAN_POINT('Ctrl Pts',(16.1830870082473,-8.71697763175051,-7.17832304343388));
#95940=CARTESIAN_POINT('Ctrl Pts',(16.1806690820714,-8.75836150028961,-7.12729848826442));
#95941=CARTESIAN_POINT('Ctrl Pts',(16.1682911799108,-8.97021473258396,-6.86609243574614));
#95942=CARTESIAN_POINT('Ctrl Pts',(16.1558057071422,-9.1699270812072,-6.59534961160817));
#95943=CARTESIAN_POINT('Ctrl Pts',(16.1432642674463,-9.35701879829506,-6.31633651487297));
#95944=CARTESIAN_POINT('Ctrl Pts',(16.1306238735717,-9.54558670214291,-6.03512195542379));
#95945=CARTESIAN_POINT('Ctrl Pts',(16.1179266926506,-9.72133466453958,-5.74550612004991));
#95946=CARTESIAN_POINT('Ctrl Pts',(16.1052247240192,-9.88377661046624,-5.44873326416131));
#95947=CARTESIAN_POINT('Ctrl Pts',(16.1030773577283,-9.91123868103423,-5.39856151163407));
#95948=CARTESIAN_POINT('Ctrl Pts',(16.1009298515565,-9.93832045718344,-5.34818508711592));
#95949=CARTESIAN_POINT('Ctrl Pts',(16.0987824528555,-9.96501958366583,-5.29760985599476));
#95950=CARTESIAN_POINT('Ctrl Pts',(16.0810524102623,-10.1854614836817,-4.88003439526046));
#95951=CARTESIAN_POINT('Ctrl Pts',(16.0632530007794,-10.3798600347158,-4.44855263773922));
#95952=CARTESIAN_POINT('Ctrl Pts',(16.0453685199868,-10.5463722689621,-4.00643121409874));
#95953=CARTESIAN_POINT('Ctrl Pts',(16.033077414964,-10.6608077609632,-3.70258337452398));
#95954=CARTESIAN_POINT('Ctrl Pts',(16.0207461488524,-10.7620713071895,-3.39371069163026));
#95955=CARTESIAN_POINT('Ctrl Pts',(16.0083699646992,-10.8495527626949,-3.08088155401435));
#95956=CARTESIAN_POINT('Ctrl Pts',(16.0035940901124,-10.8833111857265,-2.9601631880107));
#95957=CARTESIAN_POINT('Ctrl Pts',(15.9988115299569,-10.9150171691888,-2.83885573418935));
#95958=CARTESIAN_POINT('Ctrl Pts',(15.9940220242916,-10.9446640919374,-2.71702798364124));
#95959=CARTESIAN_POINT('Ctrl Pts',(15.9807342044901,-11.0269153710227,-2.37903377103331));
#95960=CARTESIAN_POINT('Ctrl Pts',(15.9676012984832,-11.0937025818476,-2.037245337332));
#95961=CARTESIAN_POINT('Ctrl Pts',(15.9545647436297,-11.1448107093041,-1.69315726102379));
#95962=CARTESIAN_POINT('Ctrl Pts',(15.9415160036568,-11.1959666069453,-1.34874756950933));
#95963=CARTESIAN_POINT('Ctrl Pts',(15.9285639096431,-11.2314133261888,-1.00203424509647));
#95964=CARTESIAN_POINT('Ctrl Pts',(15.9156522578572,-11.2509545749342,-0.654564312121401));
#95965=CARTESIAN_POINT('Ctrl Pts',(15.9142425832482,-11.2530880589098,-0.616628070499019));
#95966=CARTESIAN_POINT('Ctrl Pts',(15.9128333923135,-11.2550319762816,-0.57868285440704));
#95967=CARTESIAN_POINT('Ctrl Pts',(15.9114246129926,-11.2567860916136,-0.540730709036398));
#95968=CARTESIAN_POINT('Ctrl Pts',(15.896297122496,-11.2756218046469,-0.133200083115572));
#95969=CARTESIAN_POINT('Ctrl Pts',(15.8811812274722,-11.2724972532996,0.275133806617833));
#95970=CARTESIAN_POINT('Ctrl Pts',(15.866009903517,-11.2471854056454,0.681880736138495));
#95971=CARTESIAN_POINT('Ctrl Pts',(15.8538996454936,-11.2269806425646,1.00655973457034));
#95972=CARTESIAN_POINT('Ctrl Pts',(15.8417540721048,-11.1926381024088,1.33022661539188));
#95973=CARTESIAN_POINT('Ctrl Pts',(15.8295400541171,-11.1440408971964,1.65164183924907));
#95974=CARTESIAN_POINT('Ctrl Pts',(15.8295391702672,-11.1440373805293,1.6516650980013));
#95975=CARTESIAN_POINT('Ctrl Pts',(15.8295382864169,-11.1440338637875,1.65168835674174));
#95976=CARTESIAN_POINT('Ctrl Pts',(15.8295374025663,-11.1440303469711,1.65171161547037));
#95977=CARTESIAN_POINT('Ctrl Pts',(15.816784962099,-11.093288750435,1.98729496184131));
#95978=CARTESIAN_POINT('Ctrl Pts',(15.8039130298149,-11.0269101699919,2.32045746517097));
#95979=CARTESIAN_POINT('Ctrl Pts',(15.7909874558207,-10.9455312672853,2.64991634597987));
#95980=CARTESIAN_POINT('Ctrl Pts',(15.7780454877898,-10.8640491483724,2.97979309302464));
#95981=CARTESIAN_POINT('Ctrl Pts',(15.7650498239764,-10.7675292664881,3.30595720866079));
#95982=CARTESIAN_POINT('Ctrl Pts',(15.75206424864,-10.6565846729906,3.62716614328774));
#95983=CARTESIAN_POINT('Ctrl Pts',(15.7426825785663,-10.5764306909228,3.85922950369542));
#95984=CARTESIAN_POINT('Ctrl Pts',(15.7333061132432,-10.488747063491,4.08870743526162));
#95985=CARTESIAN_POINT('Ctrl Pts',(15.7239579733421,-10.3937536873271,4.31514398655314));
#95986=CARTESIAN_POINT('Ctrl Pts',(15.7107915749463,-10.2599601574097,4.63406880766187));
#95987=CARTESIAN_POINT('Ctrl Pts',(15.6976909195897,-10.1116875116354,4.9469541132507));
#95988=CARTESIAN_POINT('Ctrl Pts',(15.6847177269443,-9.94958308666377,5.2524241885062));
#95989=CARTESIAN_POINT('Ctrl Pts',(15.6727187110484,-9.79965132929213,5.53495605162788));
#95990=CARTESIAN_POINT('Ctrl Pts',(15.6608285954209,-9.63788771127589,5.811145088744));
#95991=CARTESIAN_POINT('Ctrl Pts',(15.6490961272982,-9.46479960650109,6.07994229205141));
#95992=CARTESIAN_POINT('Ctrl Pts',(15.6467196831804,-9.42974012846632,6.13438791474411));
#95993=CARTESIAN_POINT('Ctrl Pts',(15.6443497106583,-9.39421600074739,6.18853039061903));
#95994=CARTESIAN_POINT('Ctrl Pts',(15.6419866226875,-9.35823486758082,6.24236374822694));
#95995=CARTESIAN_POINT('Ctrl Pts',(15.6269862132743,-9.12983383667652,6.58408712635861));
#95996=CARTESIAN_POINT('Ctrl Pts',(15.611834850162,-8.8822881668317,6.91267923813996));
#95997=CARTESIAN_POINT('Ctrl Pts',(15.5965715424223,-8.61750993968684,7.22650596940827));
#95998=CARTESIAN_POINT('Ctrl Pts',(15.584724568317,-8.41199611174719,7.47008994362021));
#95999=CARTESIAN_POINT('Ctrl Pts',(15.5728102156546,-8.19609987425416,7.7047794729152));
#96000=CARTESIAN_POINT('Ctrl Pts',(15.5608469949931,-7.97069767366566,7.92982292259678));
#96001=CARTESIAN_POINT('Ctrl Pts',(15.546547793163,-7.70128263482498,8.1988091595479));
#96002=CARTESIAN_POINT('Ctrl Pts',(15.5322500538376,-7.41833237647199,8.45421872950808));
#96003=CARTESIAN_POINT('Ctrl Pts',(15.5179489803913,-7.12315253349482,8.69476756943813));
#96004=CARTESIAN_POINT('Ctrl Pts',(15.5154829894361,-7.07225349953903,8.73624636232635));
#96005=CARTESIAN_POINT('Ctrl Pts',(15.5130168993599,-7.02099076553669,8.77728319147544));
#96006=CARTESIAN_POINT('Ctrl Pts',(15.5105506855879,-6.96937094029732,8.81787134061039));
#96007=CARTESIAN_POINT('Ctrl Pts',(15.4974931629857,-6.69606655670022,9.03276782716831));
#96008=CARTESIAN_POINT('Ctrl Pts',(15.4844339968103,-6.41278921190233,9.23505585109763));
#96009=CARTESIAN_POINT('Ctrl Pts',(15.4713723156188,-6.12063727973133,9.42366104347754));
#96010=CARTESIAN_POINT('Ctrl Pts',(15.4537235811276,-5.72588626671685,9.67850135960518));
#96011=CARTESIAN_POINT('Ctrl Pts',(15.436070244661,-5.31493186286818,9.90835908134703));
#96012=CARTESIAN_POINT('Ctrl Pts',(15.4184103849752,-4.89133265966661,10.1117089124309));
#96013=CARTESIAN_POINT('Ctrl Pts',(15.4007051415832,-4.46664485768154,10.3155813280171));
#96014=CARTESIAN_POINT('Ctrl Pts',(15.3829933396985,-4.02924810549658,10.4928088688309));
#96015=CARTESIAN_POINT('Ctrl Pts',(15.3652733218964,-3.58275659444785,10.6418978456182));
#96016=CARTESIAN_POINT('Ctrl Pts',(15.3633532580213,-3.53437672088036,10.6580524771595));
#96017=CARTESIAN_POINT('Ctrl Pts',(15.3614330979687,-3.48589008528935,10.6738767821366));
#96018=CARTESIAN_POINT('Ctrl Pts',(15.3595128398411,-3.43730129811629,10.6893688951891));
#96019=CARTESIAN_POINT('Ctrl Pts',(15.3503867735382,-3.20638208630126,10.7629954815599));
#96020=CARTESIAN_POINT('Ctrl Pts',(15.3411706767005,-2.97305390698645,10.8289328157232));
#96021=CARTESIAN_POINT('Ctrl Pts',(15.3319491449979,-2.73785862511626,10.8871720241923));
#96022=CARTESIAN_POINT('Ctrl Pts',(15.3241947349801,-2.54008230023958,10.9361455262249));
#96023=CARTESIAN_POINT('Ctrl Pts',(15.3164364503988,-2.34098490422853,10.9796760416066));
#96024=CARTESIAN_POINT('Ctrl Pts',(15.3087231597288,-2.14086073602318,11.0177641579777));
#96025=CARTESIAN_POINT('Ctrl Pts',(15.3030975434798,-1.99490204982233,11.045543368631));
#96026=CARTESIAN_POINT('Ctrl Pts',(15.2975031964061,-1.84840170014174,11.0704447887901));
#96027=CARTESIAN_POINT('Ctrl Pts',(15.2919401866255,-1.70147371298188,11.0924211245245));
#96028=CARTESIAN_POINT('Ctrl Pts',(15.2849796942184,-1.51763597417496,11.1199181313697));
#96029=CARTESIAN_POINT('Ctrl Pts',(15.2780682522276,-1.33312876471508,11.1428357490647));
#96030=CARTESIAN_POINT('Ctrl Pts',(15.2712062606979,-1.14818779157993,11.1612111263306));
#96031=CARTESIAN_POINT('Ctrl Pts',(15.2565513847108,-0.753216883420893,
11.2004546715735));
#96032=CARTESIAN_POINT('Ctrl Pts',(15.2417880158008,-0.356230914403019,
11.2181470297901));
#96033=CARTESIAN_POINT('Ctrl Pts',(15.2269407912071,0.0403976675311114,
11.2147424095226));
#96034=CARTESIAN_POINT('Ctrl Pts',(15.223025529029,0.144989934983414,11.2138445999098));
#96035=CARTESIAN_POINT('Ctrl Pts',(15.2191044397254,0.249557517966656,11.2114799435831));
#96036=CARTESIAN_POINT('Ctrl Pts',(15.2151779818984,0.354057296599062,11.2076572361261));
#96037=CARTESIAN_POINT('Ctrl Pts',(15.2022992179719,0.696816098215689,11.1951187729444));
#96038=CARTESIAN_POINT('Ctrl Pts',(15.1894285714027,1.03885434801065,11.167063534534));
#96039=CARTESIAN_POINT('Ctrl Pts',(15.176560634575,1.37888273726765,11.1237375046297));
#96040=CARTESIAN_POINT('Ctrl Pts',(15.1706282521209,1.53564278958491,11.1037633173881));
#96041=CARTESIAN_POINT('Ctrl Pts',(15.1646964456791,1.69197568407878,11.0805427435218));
#96042=CARTESIAN_POINT('Ctrl Pts',(15.1587646858145,1.84775483686978,11.0540961733022));
#96043=CARTESIAN_POINT('Ctrl Pts',(15.1453128659511,2.20102488651213,10.9941216452156));
#96044=CARTESIAN_POINT('Ctrl Pts',(15.1318527589919,2.55155730831782,10.9175263915371));
#96045=CARTESIAN_POINT('Ctrl Pts',(15.1183411040416,2.89768337032284,10.824420911768));
#96046=CARTESIAN_POINT('Ctrl Pts',(15.1048923411799,3.24219833501767,10.7317488058603));
#96047=CARTESIAN_POINT('Ctrl Pts',(15.0913924504108,3.58234777223796,10.6227191870421));
#96048=CARTESIAN_POINT('Ctrl Pts',(15.0778008782604,3.91643536896289,10.4974497033195));
#96049=CARTESIAN_POINT('Ctrl Pts',(15.0711231977693,4.08057607338532,10.4359035055486));
#96050=CARTESIAN_POINT('Ctrl Pts',(15.0644234239915,4.2432527662515,10.3704374251837));
#96051=CARTESIAN_POINT('Ctrl Pts',(15.0576970245877,4.40425989922078,10.3010668804539));
#96052=CARTESIAN_POINT('Ctrl Pts',(15.0463063079057,4.67691492984938,10.183592408055));
#96053=CARTESIAN_POINT('Ctrl Pts',(15.0350395082811,4.94494615285118,10.0554153771109));
#96054=CARTESIAN_POINT('Ctrl Pts',(15.0239216225122,5.20738442942893,9.91676673804391));
#96055=CARTESIAN_POINT('Ctrl Pts',(15.0183628066874,5.33860056846611,9.84744400304363));
#96056=CARTESIAN_POINT('Ctrl Pts',(15.0128412401794,5.46841903543546,9.7755038407282));
#96057=CARTESIAN_POINT('Ctrl Pts',(15.0073602513422,5.59675654054199,9.70104559446499));
#96058=CARTESIAN_POINT('Ctrl Pts',(14.9991386428056,5.78926573165558,9.58935652315283));
#96059=CARTESIAN_POINT('Ctrl Pts',(14.990982342604,5.97840148681949,9.47194440885129));
#96060=CARTESIAN_POINT('Ctrl Pts',(14.982793878564,6.16375328342834,9.34889430887797));
#96061=CARTESIAN_POINT('Ctrl Pts',(14.9746054145239,6.34910508003718,9.22584420890465));
#96062=CARTESIAN_POINT('Ctrl Pts',(14.9663846757789,6.53067257440623,9.09715565980792));
#96063=CARTESIAN_POINT('Ctrl Pts',(14.958035400268,6.70799664566802,8.96294977261773));
#96064=CARTESIAN_POINT('Ctrl Pts',(14.9438663009938,7.00892363821142,8.73519629433143));
#96065=CARTESIAN_POINT('Ctrl Pts',(14.9297048407444,7.29829892641942,8.49233128970611));
#96066=CARTESIAN_POINT('Ctrl Pts',(14.9155444032486,7.5748854850347,8.23573319682833));
#96067=CARTESIAN_POINT('Ctrl Pts',(14.9012834997017,7.85343438127926,7.97731458130559));
#96068=CARTESIAN_POINT('Ctrl Pts',(14.8870236331363,8.11901308083736,7.7049666699828));
#96069=CARTESIAN_POINT('Ctrl Pts',(14.8727581311784,8.37032354391681,7.42005806068027));
#96070=CARTESIAN_POINT('Ctrl Pts',(14.8678011884713,8.45764830618842,7.32105869443179));
#96071=CARTESIAN_POINT('Ctrl Pts',(14.8628435661219,8.54324996292118,7.22054243972945));
#96072=CARTESIAN_POINT('Ctrl Pts',(14.857884986722,8.6270728691673,7.11856583587876));
#96073=CARTESIAN_POINT('Ctrl Pts',(14.8456785387162,8.83341824840889,6.86753181740228));
#96074=CARTESIAN_POINT('Ctrl Pts',(14.8333979230135,9.02883460105979,6.60753129588973));
#96075=CARTESIAN_POINT('Ctrl Pts',(14.8211015218869,9.21253500466722,6.33960528723982));
#96076=CARTESIAN_POINT('Ctrl Pts',(14.8088177332149,9.39604698623265,6.07195409108165));
#96077=CARTESIAN_POINT('Ctrl Pts',(14.7965182230185,9.56786759034857,5.79639418886013));
#96078=CARTESIAN_POINT('Ctrl Pts',(14.784258731834,9.72724843380699,5.513926181261));
#96079=CARTESIAN_POINT('Ctrl Pts',(14.7752122552789,9.84485813244661,5.30548847615037));
#96080=CARTESIAN_POINT('Ctrl Pts',(14.7661874995261,9.95569494145445,5.09328842147978));
#96081=CARTESIAN_POINT('Ctrl Pts',(14.757206081749,10.0594678533509,4.8777126536179));
#96082=CARTESIAN_POINT('Ctrl Pts',(14.7571975315397,10.0595666440024,4.87750742789788));
#96083=CARTESIAN_POINT('Ctrl Pts',(14.7571889813498,10.0596654281814,4.87730219912515));
#96084=CARTESIAN_POINT('Ctrl Pts',(14.7571804311792,10.0597642058877,4.8770969673));
#96085=CARTESIAN_POINT('Ctrl Pts',(14.7417401730578,10.2381411483223,4.50648069317787));
#96086=CARTESIAN_POINT('Ctrl Pts',(14.7263628645334,10.3954128046633,4.1259070187093));
#96087=CARTESIAN_POINT('Ctrl Pts',(14.7110044208977,10.5311860218655,3.73780135474113));
#96088=CARTESIAN_POINT('Ctrl Pts',(14.6956232644371,10.6671600272069,3.34912174094907));
#96089=CARTESIAN_POINT('Ctrl Pts',(14.6802610526129,10.7815710421429,2.95288732267195));
#96090=CARTESIAN_POINT('Ctrl Pts',(14.6648752094907,10.8739972606444,2.55157887666387));
#96091=CARTESIAN_POINT('Ctrl Pts',(14.6514061812039,10.9549087415138,2.20026664969692));
#96092=CARTESIAN_POINT('Ctrl Pts',(14.6379190447941,11.018971273041,1.84506648378009));
#96093=CARTESIAN_POINT('Ctrl Pts',(14.624386376264,11.0658933994358,1.4876744121179));
#96094=CARTESIAN_POINT('Ctrl Pts',(14.6080772663412,11.122442343606,1.05695769358589));
#96095=CARTESIAN_POINT('Ctrl Pts',(14.591766379385,11.1543157325057,0.622938756550116));
#96096=CARTESIAN_POINT('Ctrl Pts',(14.5754370498476,11.161049334572,0.188663963741718));
#96097=CARTESIAN_POINT('Ctrl Pts',(14.5592396394342,11.1677285381474,-0.242102470069903));
#96098=CARTESIAN_POINT('Ctrl Pts',(14.5430240690424,11.1496719435507,-0.67311983496954));
#96099=CARTESIAN_POINT('Ctrl Pts',(14.5267752198866,11.1064667572452,-1.1013843654405));
#96100=CARTESIAN_POINT('Ctrl Pts',(14.5147782440051,11.0745671701981,-1.41758394324903));
#96101=CARTESIAN_POINT('Ctrl Pts',(14.5027631463582,11.0289591688627,-1.73228216587942));
#96102=CARTESIAN_POINT('Ctrl Pts',(14.4907243493819,10.9694936230759,-2.04426332029249));
#96103=CARTESIAN_POINT('Ctrl Pts',(14.4907194949762,10.969469644776,-2.04438912049456));
#96104=CARTESIAN_POINT('Ctrl Pts',(14.4907146405667,10.9694456642232,-2.04451492025482));
#96105=CARTESIAN_POINT('Ctrl Pts',(14.4907097861533,10.9694216814175,-2.04464071957316));
#96106=CARTESIAN_POINT('Ctrl Pts',(14.4730988720036,10.8824164968376,-2.50101738523806));
#96107=CARTESIAN_POINT('Ctrl Pts',(14.4554966900047,10.7659459820233,-2.95158140987517));
#96108=CARTESIAN_POINT('Ctrl Pts',(14.4379151671712,10.6218907828759,-3.39316742440224));
#96109=CARTESIAN_POINT('Ctrl Pts',(14.419954168372,10.4747263259973,-3.84428454046353));
#96110=CARTESIAN_POINT('Ctrl Pts',(14.4020147262933,10.298773834897,-4.28603272975413));
#96111=CARTESIAN_POINT('Ctrl Pts',(14.384108374905,10.0959871954966,-4.71505652523921));
#96112=CARTESIAN_POINT('Ctrl Pts',(14.3662964980548,9.89427046552061,-5.14181677612684));
#96113=CARTESIAN_POINT('Ctrl Pts',(14.3485173441753,9.66600198051707,-5.55598757991483));
#96114=CARTESIAN_POINT('Ctrl Pts',(14.3307812918777,9.41305321993345,-5.95427108959876));
#96115=CARTESIAN_POINT('Ctrl Pts',(14.3129041310352,9.15809199169641,-6.35572335440244));
#96116=CARTESIAN_POINT('Ctrl Pts',(14.29507073134,8.87805625267711,-6.7410357153329));
#96117=CARTESIAN_POINT('Ctrl Pts',(14.2772910900074,8.5748095345901,-7.10681912034434));
#96118=CARTESIAN_POINT('Ctrl Pts',(14.2605178060459,8.28872708682073,-7.45189857419375));
#96119=CARTESIAN_POINT('Ctrl Pts',(14.2437923326192,7.98198635718675,-7.77959808581969));
#96120=CARTESIAN_POINT('Ctrl Pts',(14.227122973847,7.65610933899355,-8.08704727484651));
#96121=CARTESIAN_POINT('Ctrl Pts',(14.2261228517416,7.63655748855957,-8.10549349910998));
#96122=CARTESIAN_POINT('Ctrl Pts',(14.2251229316967,7.61693674075024,-8.12386681794129));
#96123=CARTESIAN_POINT('Ctrl Pts',(14.2241232155377,7.59724741963854,-8.14216660735697));
#96124=CARTESIAN_POINT('Ctrl Pts',(14.2241072450444,7.5969328821891,-8.14245894699912));
#96125=CARTESIAN_POINT('Ctrl Pts',(14.224091274633,7.59661832736125,-8.1427512678872));
#96126=CARTESIAN_POINT('Ctrl Pts',(14.2240753043035,7.59630375515616,-8.14304357001812));
#96127=CARTESIAN_POINT('Ctrl Pts',(14.2131549621309,7.38120261376546,-8.3429166706131));
#96128=CARTESIAN_POINT('Ctrl Pts',(14.2022727831546,7.15797252043843,-8.53402145897874));
#96129=CARTESIAN_POINT('Ctrl Pts',(14.1913844675769,6.9273861129154,-8.71584559113722));
#96130=CARTESIAN_POINT('Ctrl Pts',(14.1804968209202,6.69681387141111,-8.89765855297526));
#96131=CARTESIAN_POINT('Ctrl Pts',(14.1696030234366,6.45888600183346,-9.07019140447614));
#96132=CARTESIAN_POINT('Ctrl Pts',(14.1586596895839,6.21442397422352,-9.23291415592088));
#96133=CARTESIAN_POINT('Ctrl Pts',(14.1512643133734,6.04921941337559,-9.34288027603868));
#96134=CARTESIAN_POINT('Ctrl Pts',(14.1438463206219,5.88103179822744,-9.44836586224379));
#96135=CARTESIAN_POINT('Ctrl Pts',(14.1363927682876,5.71012790879231,-9.54920486720541));
#96136=CARTESIAN_POINT('Ctrl Pts',(14.1216281677088,5.37158763273423,-9.74895494129653));
#96137=CARTESIAN_POINT('Ctrl Pts',(14.1068694552858,5.02262805541314,-9.93091603163188));
#96138=CARTESIAN_POINT('Ctrl Pts',(14.0921174001175,4.66529778493237,-10.0942603848338));
#96139=CARTESIAN_POINT('Ctrl Pts',(14.0773653449492,4.30796751445161,-10.2576047380358));
#96140=CARTESIAN_POINT('Ctrl Pts',(14.0626199458783,3.94226743200403,-10.402335429853));
#96141=CARTESIAN_POINT('Ctrl Pts',(14.0478772200694,3.57014454984236,-10.5276384934889));
#96142=CARTESIAN_POINT('Ctrl Pts',(14.0305614199039,3.13307439415546,-10.6748109253835));
#96143=CARTESIAN_POINT('Ctrl Pts',(14.0132282417536,2.68696134846804,-10.7951794302555));
#96144=CARTESIAN_POINT('Ctrl Pts',(13.9958926142567,2.23521888289641,-10.8873008395147));
#96145=CARTESIAN_POINT('Ctrl Pts',(13.9837106207932,1.91777298924478,-10.9520358717853));
#96146=CARTESIAN_POINT('Ctrl Pts',(13.971527403441,1.59754753804668,-11.0028233533345));
#96147=CARTESIAN_POINT('Ctrl Pts',(13.9593479247777,1.27572652031624,-11.0391779100375));
#96148=CARTESIAN_POINT('Ctrl Pts',(13.9420765290348,0.819360668440139,-11.0907313429248));
#96149=CARTESIAN_POINT('Ctrl Pts',(13.9248126805284,0.359787528436995,-11.113259270819));
#96150=CARTESIAN_POINT('Ctrl Pts',(13.9075699047137,-0.0993101696415865,
-11.1072933181119));
#96151=CARTESIAN_POINT('Ctrl Pts',(13.8953468761735,-0.424754536992514,
-11.1030641840679));
#96152=CARTESIAN_POINT('Ctrl Pts',(13.8831344205217,-0.749960265695552,
-11.084517719827));
#96153=CARTESIAN_POINT('Ctrl Pts',(13.8709371529732,-1.07362401428721,-11.0518567173184));
#96154=CARTESIAN_POINT('Ctrl Pts',(13.8562299511789,-1.46389077240429,-11.0124747858498));
#96155=CARTESIAN_POINT('Ctrl Pts',(13.8415141838714,-1.8521538137257,-10.9524664405571));
#96156=CARTESIAN_POINT('Ctrl Pts',(13.8267936423669,-2.23612309892015,-10.8721120054768));
#96157=CARTESIAN_POINT('Ctrl Pts',(13.8074272722069,-2.7412737623547,-10.7663975700887));
#96158=CARTESIAN_POINT('Ctrl Pts',(13.7880526528729,-3.23899168788081,-10.6254662692622));
#96159=CARTESIAN_POINT('Ctrl Pts',(13.7686781120946,-3.72446110312998,-10.4509094002611));
#96160=CARTESIAN_POINT('Ctrl Pts',(13.7492251037983,-4.21189668524437,-10.2756455702834));
#96161=CARTESIAN_POINT('Ctrl Pts',(13.7297721758329,-4.68698327940954,-10.0664838182762));
#96162=CARTESIAN_POINT('Ctrl Pts',(13.7103273747444,-5.14486845773911,-9.82508158909665));
#96163=CARTESIAN_POINT('Ctrl Pts',(13.7050057894525,-5.27018087514552,-9.75901546960325));
#96164=CARTESIAN_POINT('Ctrl Pts',(13.6996848106097,-5.39420510479515,-9.69053481749199));
#96165=CARTESIAN_POINT('Ctrl Pts',(13.6943645980911,-5.51684212818613,-9.61967412727097));
#96166=CARTESIAN_POINT('Ctrl Pts',(13.6943603323047,-5.51694045947439,-9.61961731063629));
#96167=CARTESIAN_POINT('Ctrl Pts',(13.6943560665187,-5.51703878987083,-9.61956049247151));
#96168=CARTESIAN_POINT('Ctrl Pts',(13.6943518007333,-5.51713711937541,-9.61950367277666));
#96169=CARTESIAN_POINT('Ctrl Pts',(13.672318355336,-6.02502430590092,-9.32602111045481));
#96170=CARTESIAN_POINT('Ctrl Pts',(13.650294336554,-6.50906190953783,-8.99172904315948));
#96171=CARTESIAN_POINT('Ctrl Pts',(13.6282771905346,-6.96384305218222,-8.62166957247464));
#96172=CARTESIAN_POINT('Ctrl Pts',(13.6058802342115,-7.42646946976525,-8.24522633162227));
#96173=CARTESIAN_POINT('Ctrl Pts',(13.5834903898995,-7.85882243931573,-7.83177022822399));
#96174=CARTESIAN_POINT('Ctrl Pts',(13.5611049469218,-8.25518594461479,-7.38656161626531));
#96175=CARTESIAN_POINT('Ctrl Pts',(13.5467276107356,-8.50975545986931,-7.10062070844145));
#96176=CARTESIAN_POINT('Ctrl Pts',(13.5323520896496,-8.74947872840078,-6.80158092168345));
#96177=CARTESIAN_POINT('Ctrl Pts',(13.5179776605464,-8.97283292601846,-6.49082829953906));
#96178=CARTESIAN_POINT('Ctrl Pts',(13.5179763595475,-8.97285314133025,-6.49080017398237));
#96179=CARTESIAN_POINT('Ctrl Pts',(13.5179750585485,-8.9728733565079,-6.49077204832963));
#96180=CARTESIAN_POINT('Ctrl Pts',(13.5179737575496,-8.97289357155134,-6.49074392258092));
#96181=CARTESIAN_POINT('Ctrl Pts',(13.4921480292973,-9.37417615952936,-5.93242836588278));
#96182=CARTESIAN_POINT('Ctrl Pts',(13.4663166539886,-9.7225828106941,-5.33627768736209));
#96183=CARTESIAN_POINT('Ctrl Pts',(13.440491435221,-10.0132972689579,-4.71338935698886));
#96184=CARTESIAN_POINT('Ctrl Pts',(13.4143413439915,-10.3076688161562,-4.08266530343198));
#96185=CARTESIAN_POINT('Ctrl Pts',(13.3881975686009,-10.5428877259154,-3.42452840408841));
#96186=CARTESIAN_POINT('Ctrl Pts',(13.3620711711185,-10.7140055390992,-2.75049821329857));
#96187=CARTESIAN_POINT('Ctrl Pts',(13.3553005411707,-10.7583505503597,-2.57582395908512));
#96188=CARTESIAN_POINT('Ctrl Pts',(13.3485310720448,-10.7983909050603,-2.40008225456296));
#96189=CARTESIAN_POINT('Ctrl Pts',(13.34176294332,-10.8340410075211,-2.22347335356751));
#96190=CARTESIAN_POINT('Ctrl Pts',(13.3417607609311,-10.8340525029272,-2.22341640587578));
#96191=CARTESIAN_POINT('Ctrl Pts',(13.3417585785423,-10.8340639978769,-2.22335945809389));
#96192=CARTESIAN_POINT('Ctrl Pts',(13.3417563961537,-10.8340754923701,-2.22330251022183));
#96193=CARTESIAN_POINT('Ctrl Pts',(13.3105788808085,-10.9982853547507,-1.40974752574804));
#96194=CARTESIAN_POINT('Ctrl Pts',(13.2794222220121,-11.069299590073,-0.577797912359255));
#96195=CARTESIAN_POINT('Ctrl Pts',(13.2482776981295,-11.0476511917255,0.251461408095067));
#96196=CARTESIAN_POINT('Ctrl Pts',(13.2208054288712,-11.0285553586777,0.982942660542084));
#96197=CARTESIAN_POINT('Ctrl Pts',(13.1933426162945,-10.937358983901,1.71233147641963));
#96198=CARTESIAN_POINT('Ctrl Pts',(13.1658839303791,-10.7743974792278,2.42514198951792));
#96199=CARTESIAN_POINT('Ctrl Pts',(13.1658821827909,-10.7743871076607,2.42518735582724));
#96200=CARTESIAN_POINT('Ctrl Pts',(13.1658804352027,-10.774376735803,2.42523272206939));
#96201=CARTESIAN_POINT('Ctrl Pts',(13.1658786876146,-10.7743663636545,2.42527808824439));
#96202=CARTESIAN_POINT('Ctrl Pts',(13.1280368516429,-10.5497704613986,3.40762586902646));
#96203=CARTESIAN_POINT('Ctrl Pts',(13.0902086077735,-10.1888936274173,4.35849696440613));
#96204=CARTESIAN_POINT('Ctrl Pts',(13.0523973489158,-9.70795439135571,5.24321458223078));
#96205=CARTESIAN_POINT('Ctrl Pts',(13.0316692936244,-9.4443044791854,5.72821498299888));
#96206=CARTESIAN_POINT('Ctrl Pts',(13.0109463370872,-9.14457426237966,6.19333505790884));
#96207=CARTESIAN_POINT('Ctrl Pts',(12.9902289974229,-8.81144133675073,6.63286537247014));
#96208=CARTESIAN_POINT('Ctrl Pts',(12.9902260976388,-8.81139470848843,6.63292689306214));
#96209=CARTESIAN_POINT('Ctrl Pts',(12.9902231978549,-8.81134807957172,6.63298841315281));
#96210=CARTESIAN_POINT('Ctrl Pts',(12.990220298071,-8.81130145000063,6.63304993274213));
#96211=CARTESIAN_POINT('Ctrl Pts',(12.9380037558956,-7.9716405999951,7.74083603199739));
#96212=CARTESIAN_POINT('Ctrl Pts',(12.8858195375993,-6.91977593055457,8.68604892505739));
#96213=CARTESIAN_POINT('Ctrl Pts',(12.8336661371426,-5.73205062687898,9.40563273683172));
#96214=CARTESIAN_POINT('Ctrl Pts',(12.8273800139828,-5.58889241526566,9.49236519195473));
#96215=CARTESIAN_POINT('Ctrl Pts',(12.8210943397431,-5.44376046343101,9.57581980868288));
#96216=CARTESIAN_POINT('Ctrl Pts',(12.8148091127809,-5.29678846581114,9.65588622909681));
#96217=CARTESIAN_POINT('Ctrl Pts',(12.8148074440706,-5.2967494451542,9.65590748650893));
#96218=CARTESIAN_POINT('Ctrl Pts',(12.8148057753604,-5.29671042436758,9.65592874368221));
#96219=CARTESIAN_POINT('Ctrl Pts',(12.8148041066501,-5.29667140345124,9.65595000061667));
#96220=CARTESIAN_POINT('Ctrl Pts',(12.7795911172689,-4.47325515726357,10.104512126223));
#96221=CARTESIAN_POINT('Ctrl Pts',(12.7443897733396,-3.59207956867088,10.4467162251273));
#96222=CARTESIAN_POINT('Ctrl Pts',(12.7092021403706,-2.68282119992599,10.6728297518592));
#96223=CARTESIAN_POINT('Ctrl Pts',(12.6859989915403,-2.08324528432376,10.8219317337387));
#96224=CARTESIAN_POINT('Ctrl Pts',(12.6628017875576,-1.47145724776612,10.9205542219341));
#96225=CARTESIAN_POINT('Ctrl Pts',(12.6396109205276,-0.855959330699359,
10.9658962051474));
#96226=CARTESIAN_POINT('Ctrl Pts',(12.639608461027,-0.855894054248407,10.9659010138781));
#96227=CARTESIAN_POINT('Ctrl Pts',(12.6396060015265,-0.855828777755838,
10.9659058220097));
#96228=CARTESIAN_POINT('Ctrl Pts',(12.6396035420261,-0.855763501221594,
10.9659106295421));
#96229=CARTESIAN_POINT('Ctrl Pts',(12.600852474588,0.172711781201659,11.0416565048728));
#96230=CARTESIAN_POINT('Ctrl Pts',(12.5621242554643,1.21152764921655,10.9686607859318));
#96231=CARTESIAN_POINT('Ctrl Pts',(12.523415689347,2.22066350476061,10.7565359105041));
#96232=CARTESIAN_POINT('Ctrl Pts',(12.4839776371738,3.24881712843266,10.5404134150604));
#96233=CARTESIAN_POINT('Ctrl Pts',(12.4445599840427,4.24615952376666,10.1798673325154));
#96234=CARTESIAN_POINT('Ctrl Pts',(12.4051604950114,5.17033547788135,9.68510657471025));
#96235=CARTESIAN_POINT('Ctrl Pts',(12.3958748650144,5.38814429147203,9.56850188142757));
#96236=CARTESIAN_POINT('Ctrl Pts',(12.3865902489369,5.60188906417856,9.44444251544705));
#96237=CARTESIAN_POINT('Ctrl Pts',(12.3773066267887,5.81101532521251,9.3130625511924));
#96238=CARTESIAN_POINT('Ctrl Pts',(12.3773065522333,5.81101700467344,9.31306149610005));
#96239=CARTESIAN_POINT('Ctrl Pts',(12.377306477678,5.81101868413409,9.31306044100723));
#96240=CARTESIAN_POINT('Ctrl Pts',(12.3773064031226,5.81102036359442,9.31305938591394));
#96241=CARTESIAN_POINT('Ctrl Pts',(12.3241086670831,7.00937155969095,8.56021498805325));
#96242=CARTESIAN_POINT('Ctrl Pts',(12.2709407504699,8.05609808609067,7.56696251764249));
#96243=CARTESIAN_POINT('Ctrl Pts',(12.2178065051586,8.8827252865088,6.41753671029591));
#96244=CARTESIAN_POINT('Ctrl Pts',(12.1837058825503,9.4132400615682,5.67985547584888));
#96245=CARTESIAN_POINT('Ctrl Pts',(12.1496190936948,9.85310033145007,4.87784795278562));
#96246=CARTESIAN_POINT('Ctrl Pts',(12.1155467762475,10.1842082928,4.03376973742849));
#96247=CARTESIAN_POINT('Ctrl Pts',(12.1155465571978,10.1842104214813,4.03376431087971));
#96248=CARTESIAN_POINT('Ctrl Pts',(12.1155463381481,10.1842125501581,4.03375888432918));
#96249=CARTESIAN_POINT('Ctrl Pts',(12.1155461190984,10.1842146788304,4.03375345777692));
#96250=CARTESIAN_POINT('Ctrl Pts',(12.0549794961925,10.7727865153168,2.53332719255639));
#96251=CARTESIAN_POINT('Ctrl Pts',(11.9944605437619,11.0177216674262,0.899991790145014));
#96252=CARTESIAN_POINT('Ctrl Pts',(11.9339855927979,10.9113240835915,-0.707007078692226));
#96253=CARTESIAN_POINT('Ctrl Pts',(11.9074297722812,10.8646026709291,-1.41267401766815));
#96254=CARTESIAN_POINT('Ctrl Pts',(11.8808824625675,10.7501342130751,-2.11326202676983));
#96255=CARTESIAN_POINT('Ctrl Pts',(11.8543434757932,10.5672658927243,-2.79528406953566));
#96256=CARTESIAN_POINT('Ctrl Pts',(11.8543434226523,10.5672655265544,-2.79528543519573));
#96257=CARTESIAN_POINT('Ctrl Pts',(11.8543433695114,10.5672651603842,-2.79528680085578));
#96258=CARTESIAN_POINT('Ctrl Pts',(11.8543433163706,10.5672647942137,-2.7952881665157));
#96259=CARTESIAN_POINT('Ctrl Pts',(11.7800575547027,10.0553939777664,-4.70434829349969));
#96260=CARTESIAN_POINT('Ctrl Pts',(11.7058378548569,9.00761473780677,-6.46795760223549));
#96261=CARTESIAN_POINT('Ctrl Pts',(11.6316861718067,7.58770537091745,-7.83892251958424));
#96262=CARTESIAN_POINT('Ctrl Pts',(11.6190193009064,7.34515108353452,-8.07311593101516));
#96263=CARTESIAN_POINT('Ctrl Pts',(11.606354412188,7.09173782638425,-8.29585177971521));
#96264=CARTESIAN_POINT('Ctrl Pts',(11.5936915121807,6.82828205311893,-8.5058980015901));
#96265=CARTESIAN_POINT('Ctrl Pts',(11.5936913931372,6.82827957638059,-8.50589997622716));
#96266=CARTESIAN_POINT('Ctrl Pts',(11.5936912740938,6.82827709964131,-8.50590195086313));
#96267=CARTESIAN_POINT('Ctrl Pts',(11.5936911550503,6.82827462290119,-8.50590392549794));
#96268=CARTESIAN_POINT('Ctrl Pts',(11.5068997264266,5.0225492848719,-9.94555763904382));
#96269=CARTESIAN_POINT('Ctrl Pts',(11.4202013141422,2.74505378677467,-10.7890813085325));
#96270=CARTESIAN_POINT('Ctrl Pts',(11.3335954869663,0.442386430243757,-10.8750546437055));
#96271=CARTESIAN_POINT('Ctrl Pts',(11.3335954593555,0.442385696129285,-10.8750546711147));
#96272=CARTESIAN_POINT('Ctrl Pts',(11.3335954317446,0.442384962014812,-10.8750546985239));
#96273=CARTESIAN_POINT('Ctrl Pts',(11.3335954041338,0.442384227900335,-10.8750547259329));
#96274=CARTESIAN_POINT('Ctrl Pts',(11.2469895821273,-1.86028300880753,-10.9610275730008));
#96275=CARTESIAN_POINT('Ctrl Pts',(11.1604765226659,-4.18812205175047,-10.2894500642299));
#96276=CARTESIAN_POINT('Ctrl Pts',(11.0740563207977,-6.0881731640799,-8.99381874970801));
#96277=CARTESIAN_POINT('Ctrl Pts',(11.0740562881466,-6.08817388195301,-8.99381826019546));
#96278=CARTESIAN_POINT('Ctrl Pts',(11.0740562554955,-6.08817459982607,-8.9938177706828));
#96279=CARTESIAN_POINT('Ctrl Pts',(11.0740562228444,-6.08817531769906,-8.99381728117006));
#96280=CARTESIAN_POINT('Ctrl Pts',(10.9876360070261,-7.98822641502771,-7.69818528489756));
#96281=CARTESIAN_POINT('Ctrl Pts',(10.9013086316892,-9.46049010855842,-5.77850039221671));
#96282=CARTESIAN_POINT('Ctrl Pts',(10.8150741171685,-10.2174550760751,-3.6130677051965));
#96283=CARTESIAN_POINT('Ctrl Pts',(10.8150740985777,-10.217455239265,-3.61306723836286));
#96284=CARTESIAN_POINT('Ctrl Pts',(10.8150740799868,-10.2174554024549,-3.61306677152912));
#96285=CARTESIAN_POINT('Ctrl Pts',(10.815074061396,-10.2174555656447,-3.61306630469546));
#96286=CARTESIAN_POINT('Ctrl Pts',(10.7288395283245,-10.9744203879367,-1.44763304488258));
#96287=CARTESIAN_POINT('Ctrl Pts',(10.64269786965,-11.0160857164996,0.963547943719072));
#96288=CARTESIAN_POINT('Ctrl Pts',(10.5566490107872,-10.3432575454559,3.15272781414372));
#96289=CARTESIAN_POINT('Ctrl Pts',(10.4992831048788,-9.89470543142672,4.61218106109354));
#96290=CARTESIAN_POINT('Ctrl Pts',(10.4419584574757,-9.12860066636951,5.97296717125667));
#96291=CARTESIAN_POINT('Ctrl Pts',(10.3846748536244,-8.11866041143882,7.11645359126049));
#96292=CARTESIAN_POINT('Ctrl Pts',(10.3273912859189,-7.10872079377668,8.25993928972863));
#96293=CARTESIAN_POINT('Ctrl Pts',(10.270148710313,-5.85494574612279,9.18612541739735));
#96294=CARTESIAN_POINT('Ctrl Pts',(10.212947625229,-4.46736999604014,9.81217383299535));
#96295=CARTESIAN_POINT('Ctrl Pts',(10.2129475891353,-4.4673691204844,9.81217422802984));
#96296=CARTESIAN_POINT('Ctrl Pts',(10.2129475530416,-4.46736824492864,9.8121746230642));
#96297=CARTESIAN_POINT('Ctrl Pts',(10.2129475169479,-4.46736736937278,9.81217501809846));
#96298=CARTESIAN_POINT('Ctrl Pts',(10.1557463958226,-3.07979057487988,10.4382234499593));
#96299=CARTESIAN_POINT('Ctrl Pts',(10.0985865820643,-1.55841352331276,10.764137510334));
#96300=CARTESIAN_POINT('Ctrl Pts',(10.0414676010471,-0.0371553896940832,
10.7643933921731));
#96301=CARTESIAN_POINT('Ctrl Pts',(10.0414675736428,-0.0371546598294985,
10.7643933922959));
#96302=CARTESIAN_POINT('Ctrl Pts',(10.0414675462384,-0.0371539299649098,
10.7643933924186));
#96303=CARTESIAN_POINT('Ctrl Pts',(10.041467518834,-0.0371532001003252,
10.7643933925412));
#96304=CARTESIAN_POINT('Ctrl Pts',(9.9843485652607,1.48410420353549,10.7646489617688));
#96305=CARTESIAN_POINT('Ctrl Pts',(9.92727075752572,3.00523791058294,10.4392434588977));
#96306=CARTESIAN_POINT('Ctrl Pts',(9.87023419783678,4.38858771822708,9.81420125308147));
#96307=CARTESIAN_POINT('Ctrl Pts',(9.87023410346677,4.38859000705254,9.81420021891607));
#96308=CARTESIAN_POINT('Ctrl Pts',(9.87023400909677,4.3885922958776,9.81419918474985));
#96309=CARTESIAN_POINT('Ctrl Pts',(9.87023391472676,4.3885945847023,9.81419815058281));
#96310=CARTESIAN_POINT('Ctrl Pts',(9.81492195756586,5.73011589466252,9.20805425213235));
#96311=CARTESIAN_POINT('Ctrl Pts',(9.75965008730089,6.94206068657357,8.32010181699716));
#96312=CARTESIAN_POINT('Ctrl Pts',(9.70441539209234,7.9310140168344,7.23174142669155));
#96313=CARTESIAN_POINT('Ctrl Pts',(9.68370762696688,8.30177759588128,6.82370964070612));
#96314=CARTESIAN_POINT('Ctrl Pts',(9.66300506861179,8.64119941133731,6.38750964268081));
#96315=CARTESIAN_POINT('Ctrl Pts',(9.6423074979077,8.94435870693281,5.92742985065327));
#96316=CARTESIAN_POINT('Ctrl Pts',(9.64230720657879,8.94436297405523,5.92742337479446));
#96317=CARTESIAN_POINT('Ctrl Pts',(9.64230691524988,8.94436724117044,5.92741689893095));
#96318=CARTESIAN_POINT('Ctrl Pts',(9.64230662392097,8.94437150827848,5.92741042306268));
#96319=CARTESIAN_POINT('Ctrl Pts',(9.60435433150811,9.50026049356103,5.08377960741856));
#96320=CARTESIAN_POINT('Ctrl Pts',(9.56642190939225,9.9342040024153,4.159855444481));
#96321=CARTESIAN_POINT('Ctrl Pts',(9.5285088642955,10.2309211646493,3.19456526247108));
#96322=CARTESIAN_POINT('Ctrl Pts',(9.52850829697134,10.2309256046729,3.19455081803803));
#96323=CARTESIAN_POINT('Ctrl Pts',(9.52850772964719,10.2309300446658,3.1945363735957));
#96324=CARTESIAN_POINT('Ctrl Pts',(9.52850716232304,10.2309344846279,3.19452192914411));
#96325=CARTESIAN_POINT('Ctrl Pts',(9.49751616091674,10.4734746138266,2.4054703449874));
#96326=CARTESIAN_POINT('Ctrl Pts',(9.46653980188838,10.6243054333359,1.58876224559805));
#96327=CARTESIAN_POINT('Ctrl Pts',(9.43557487104774,10.6810137934708,0.766165713708518));
#96328=CARTESIAN_POINT('Ctrl Pts',(9.40971907541639,10.7283654177255,0.0792955273978293));
#96329=CARTESIAN_POINT('Ctrl Pts',(9.38387122529526,10.7100934152529,-0.611679955836055));
#96330=CARTESIAN_POINT('Ctrl Pts',(9.3580287865665,10.6248148432736,-1.29410491435847));
#96331=CARTESIAN_POINT('Ctrl Pts',(9.35802791788757,10.6248119766827,-1.29412785368672));
#96332=CARTESIAN_POINT('Ctrl Pts',(9.35802704920864,10.6248091100161,-1.29415079300532));
#96333=CARTESIAN_POINT('Ctrl Pts',(9.35802618052972,10.6248062432738,-1.29417373231425));
#96334=CARTESIAN_POINT('Ctrl Pts',(9.33136117227495,10.5368085895391,-1.99831981820764));
#96335=CARTESIAN_POINT('Ctrl Pts',(9.30470642071757,10.3774519767225,-2.69334920017192));
#96336=CARTESIAN_POINT('Ctrl Pts',(9.27806101664121,10.1517039759143,-3.3660344562145));
#96337=CARTESIAN_POINT('Ctrl Pts',(9.25166522032462,9.92807072827676,-4.0324181579887));
#96338=CARTESIAN_POINT('Ctrl Pts',(9.22527859740385,9.63928326821499,-4.67687583326026));
#96339=CARTESIAN_POINT('Ctrl Pts',(9.1989005456505,9.29012867331838,-5.28652206468518));
#96340=CARTESIAN_POINT('Ctrl Pts',(9.19519318643189,9.24105600039261,-5.37220608704211));
#96341=CARTESIAN_POINT('Ctrl Pts',(9.19148599698024,9.19079080927959,-5.45720239902285));
#96342=CARTESIAN_POINT('Ctrl Pts',(9.18777897607309,9.13934633775977,-5.54147516031589));
#96343=CARTESIAN_POINT('Ctrl Pts',(9.18777862752297,9.13934150072836,-5.54148308400489));
#96344=CARTESIAN_POINT('Ctrl Pts',(9.18777827897285,9.13933666368652,-5.54149100768753));
#96345=CARTESIAN_POINT('Ctrl Pts',(9.18777793042273,9.13933182663427,-5.54149893136375));
#96346=CARTESIAN_POINT('Ctrl Pts',(9.16595156155315,8.83643338769895,-6.03768318532182));
#96347=CARTESIAN_POINT('Ctrl Pts',(9.14412404033658,8.49268493443823,-6.5088028215877));
#96348=CARTESIAN_POINT('Ctrl Pts',(9.12230283605917,8.11333699133592,-6.94895344648578));
#96349=CARTESIAN_POINT('Ctrl Pts',(9.1007799800376,7.73917564544167,-7.38308615552656));
#96350=CARTESIAN_POINT('Ctrl Pts',(9.07926327119728,7.33038224266112,-7.78708966817594));
#96351=CARTESIAN_POINT('Ctrl Pts',(9.05776052154422,6.8920401299936,-8.15531820550438));
#96352=CARTESIAN_POINT('Ctrl Pts',(9.04442758288083,6.62024286703547,-8.38364102846997));
#96353=CARTESIAN_POINT('Ctrl Pts',(9.03110002353198,6.33708584074756,-8.59820985818628));
#96354=CARTESIAN_POINT('Ctrl Pts',(9.01777983194417,6.04378813771145,-8.79768591775239));
#96355=CARTESIAN_POINT('Ctrl Pts',(9.01777534574994,6.04368935606449,-8.79775310059593));
#96356=CARTESIAN_POINT('Ctrl Pts',(9.01777085955654,6.04359057326732,-8.79782028172752));
#96357=CARTESIAN_POINT('Ctrl Pts',(9.01776637336399,6.04349178931997,-8.79788746114716));
#96358=CARTESIAN_POINT('Ctrl Pts',(8.99835752642122,5.61611768741423,-9.08852925980856));
#96359=CARTESIAN_POINT('Ctrl Pts',(8.97897750190263,5.16711889953788,-9.34709581950139));
#96360=CARTESIAN_POINT('Ctrl Pts',(8.95961099581836,4.70183043817049,-9.57208606414997));
#96361=CARTESIAN_POINT('Ctrl Pts',(8.94010759386849,4.23325299600327,-9.79866669552901));
#96362=CARTESIAN_POINT('Ctrl Pts',(8.92061791695976,3.74815476838732,-9.99119583465263));
#96363=CARTESIAN_POINT('Ctrl Pts',(8.90112442847188,3.25193223126937,-10.1481415373154));
#96364=CARTESIAN_POINT('Ctrl Pts',(8.88176502595483,2.75912296113442,-10.3040076888798));
#96365=CARTESIAN_POINT('Ctrl Pts',(8.86240184781724,2.25534145763491,-10.4247794736471));
#96366=CARTESIAN_POINT('Ctrl Pts',(8.84301586321307,1.74582552457155,-10.5089394452822));
#96367=CARTESIAN_POINT('Ctrl Pts',(8.82424818602389,1.25256037710942,-10.5904151718006));
#96368=CARTESIAN_POINT('Ctrl Pts',(8.80545909132578,0.75391995921181,-10.6375782823634));
#96369=CARTESIAN_POINT('Ctrl Pts',(8.78663001960709,0.254620932449703,-10.6490198881749));
#96370=CARTESIAN_POINT('Ctrl Pts',(8.77889317541281,0.0494595291618394,
-10.6537212310143));
#96371=CARTESIAN_POINT('Ctrl Pts',(8.77114956980311,-0.155813432184366,
-10.6523909638077));
#96372=CARTESIAN_POINT('Ctrl Pts',(8.76339787861685,-0.360872045124682,
-10.6449290957503));
#96373=CARTESIAN_POINT('Ctrl Pts',(8.76339639289417,-0.360911347546018,
-10.6449276655764));
#96374=CARTESIAN_POINT('Ctrl Pts',(8.76339490717174,-0.360950649958548,
-10.6449262351748));
#96375=CARTESIAN_POINT('Ctrl Pts',(8.76339342144957,-0.360989952362255,
-10.6449248045455));
#96376=CARTESIAN_POINT('Ctrl Pts',(8.7472112451467,-0.789063545175176,-10.6293426885334));
#96377=CARTESIAN_POINT('Ctrl Pts',(8.73105993269548,-1.21608690026484,-10.5867478851266));
#96378=CARTESIAN_POINT('Ctrl Pts',(8.71493237946594,-1.6389963910984,-10.5183805109206));
#96379=CARTESIAN_POINT('Ctrl Pts',(8.69877732719559,-2.06262698358809,-10.4498965637177));
#96380=CARTESIAN_POINT('Ctrl Pts',(8.68264613405947,-2.48212897303565,-10.3555528793687));
#96381=CARTESIAN_POINT('Ctrl Pts',(8.66653095761318,-2.89445997262348,-10.2366322226155));
#96382=CARTESIAN_POINT('Ctrl Pts',(8.65637934997417,-3.1542041050669,-10.1617192453015));
#96383=CARTESIAN_POINT('Ctrl Pts',(8.64623408231994,-3.41110338803429,-10.0770541792883));
#96384=CARTESIAN_POINT('Ctrl Pts',(8.63609301378944,-3.66440656040103,-9.98296294023557));
#96385=CARTESIAN_POINT('Ctrl Pts',(8.61999121628629,-4.06659656395806,-9.83356664402763));
#96386=CARTESIAN_POINT('Ctrl Pts',(8.60389650957975,-4.45980978303877,-9.66037870828455));
#96387=CARTESIAN_POINT('Ctrl Pts',(8.58781889640342,-4.8411520976406,-9.46449648788158));
#96388=CARTESIAN_POINT('Ctrl Pts',(8.57193722196419,-5.21784697293012,-9.27100149464125));
#96389=CARTESIAN_POINT('Ctrl Pts',(8.55607221493741,-5.58295902660875,-9.05536112634003));
#96390=CARTESIAN_POINT('Ctrl Pts',(8.54023467305762,-5.93365513709574,-8.81860803880677));
#96391=CARTESIAN_POINT('Ctrl Pts',(8.52997407019511,-6.16085917812977,-8.66522379356907));
#96392=CARTESIAN_POINT('Ctrl Pts',(8.51972501786341,-6.38201150082015,-8.50297743261047));
#96393=CARTESIAN_POINT('Ctrl Pts',(8.50949077051101,-6.596330404719,-8.33214655552495));
#96394=CARTESIAN_POINT('Ctrl Pts',(8.50947347554573,-6.59669258455251,-8.33185786657827));
#96395=CARTESIAN_POINT('Ctrl Pts',(8.50945618061979,-6.59705474487907,-8.33156915312288));
#96396=CARTESIAN_POINT('Ctrl Pts',(8.50943888573315,-6.59741688569491,-8.3312804151605));
#96397=CARTESIAN_POINT('Ctrl Pts',(8.49562499333087,-6.88666852213946,-8.10065761742697));
#96398=CARTESIAN_POINT('Ctrl Pts',(8.4818363825045,-7.16346871481822,-7.854401200835));
#96399=CARTESIAN_POINT('Ctrl Pts',(8.46804513914204,-7.42663655013192,-7.59427885300374));
#96400=CARTESIAN_POINT('Ctrl Pts',(8.45397426302108,-7.69514040525225,-7.32888223600308));
#96401=CARTESIAN_POINT('Ctrl Pts',(8.43990064456776,-7.94945379603481,-7.04905274715913));
#96402=CARTESIAN_POINT('Ctrl Pts',(8.42579182381223,-8.18837355310747,-6.75664594045687));
#96403=CARTESIAN_POINT('Ctrl Pts',(8.41168300305669,-8.42729331018012,-6.46423913375461));
#96404=CARTESIAN_POINT('Ctrl Pts',(8.39753889189418,-8.65082004612712,-6.15925583448179));
#96405=CARTESIAN_POINT('Ctrl Pts',(8.3833249342102,-8.85779381202089,-5.84351584079338));
#96406=CARTESIAN_POINT('Ctrl Pts',(8.38332138896566,-8.85784543540609,-5.84343708894168));
#96407=CARTESIAN_POINT('Ctrl Pts',(8.38331784371677,-8.85789705776173,-5.84335833642056));
#96408=CARTESIAN_POINT('Ctrl Pts',(8.38331429846353,-8.85794867908778,-5.84327958323009));
#96409=CARTESIAN_POINT('Ctrl Pts',(8.37051523834771,-9.04431179920568,-5.55896510664368));
#96410=CARTESIAN_POINT('Ctrl Pts',(8.35766296116299,-9.21721824714137,-5.26597631159482));
#96411=CARTESIAN_POINT('Ctrl Pts',(8.34479347421291,-9.37579863677535,-4.96559013941187));
#96412=CARTESIAN_POINT('Ctrl Pts',(8.33191202528665,-9.53452642426984,-4.66492476322892));
#96413=CARTESIAN_POINT('Ctrl Pts',(8.31901338599653,-9.67890075224488,-4.35684781344631));
#96414=CARTESIAN_POINT('Ctrl Pts',(8.30613513665175,-9.80802233333987,-4.04268415445901));
#96415=CARTESIAN_POINT('Ctrl Pts',(8.29328204869782,-9.93689163802027,-3.72913430519128));
#96416=CARTESIAN_POINT('Ctrl Pts',(8.28044923194413,-10.0505668707882,-3.40952124130343));
#96417=CARTESIAN_POINT('Ctrl Pts',(8.26767542199453,-10.1481388416316,-3.08521150397574));
#96418=CARTESIAN_POINT('Ctrl Pts',(8.26369649813215,-10.1785316096953,-2.98419201505693));
#96419=CARTESIAN_POINT('Ctrl Pts',(8.25972331273786,-10.2073618763737,-2.88271720020414));
#96420=CARTESIAN_POINT('Ctrl Pts',(8.25575708057026,-10.2346020753326,-2.78082939218218));
#96421=CARTESIAN_POINT('Ctrl Pts',(8.25575524159449,-10.2346147054722,-2.78078215107212));
#96422=CARTESIAN_POINT('Ctrl Pts',(8.25575340262021,-10.23462733527,-2.78073490987328));
#96423=CARTESIAN_POINT('Ctrl Pts',(8.25575156364743,-10.2346399647259,-2.78068766858567));
#96424=CARTESIAN_POINT('Ctrl Pts',(8.23893975591997,-10.3500978914959,-2.3488099092274));
#96425=CARTESIAN_POINT('Ctrl Pts',(8.22213948265902,-10.4374195792317,-1.90951906036571));
#96426=CARTESIAN_POINT('Ctrl Pts',(8.20536583923801,-10.4967246634927,-1.4663631741822));
#96427=CARTESIAN_POINT('Ctrl Pts',(8.18866213713668,-10.5557824624291,-1.02505512193209));
#96428=CARTESIAN_POINT('Ctrl Pts',(8.17198481832912,-10.587056050329,-0.579913295276316));
#96429=CARTESIAN_POINT('Ctrl Pts',(8.15535026019998,-10.5906237611432,-0.134473438999874));
#96430=CARTESIAN_POINT('Ctrl Pts',(8.14675394429533,-10.5924674632107,0.0957185319170201));
#96431=CARTESIAN_POINT('Ctrl Pts',(8.13816907393653,-10.5869115670197,0.325989486190348));
#96432=CARTESIAN_POINT('Ctrl Pts',(8.12959810751433,-10.5739637046953,0.555846992221927));
#96433=CARTESIAN_POINT('Ctrl Pts',(8.11399970135177,-10.5503997323819,0.974167466480529));
#96434=CARTESIAN_POINT('Ctrl Pts',(8.09840440902365,-10.502506383742,1.39112198332939));
#96435=CARTESIAN_POINT('Ctrl Pts',(8.08278120579911,-10.4305106422116,1.80368115067515));
#96436=CARTESIAN_POINT('Ctrl Pts',(8.06723453277086,-10.3588675715229,2.21421939864826));
#96437=CARTESIAN_POINT('Ctrl Pts',(8.0516601675866,-10.2633587199306,2.62040500791612));
#96438=CARTESIAN_POINT('Ctrl Pts',(8.03602523301925,-10.1442192815926,3.01930278573934));
#96439=CARTESIAN_POINT('Ctrl Pts',(8.02525642685694,-10.0621601266776,3.29404988042343));
#96440=CARTESIAN_POINT('Ctrl Pts',(8.01445883116972,-9.96889090332492,3.56534070631904));
#96441=CARTESIAN_POINT('Ctrl Pts',(8.00362135560029,-9.86448776295425,3.83223060469584));
#96442=CARTESIAN_POINT('Ctrl Pts',(8.00361847717217,-9.86446003353207,3.83230149052017));
#96443=CARTESIAN_POINT('Ctrl Pts',(8.00361559874135,-9.86443230332504,3.83237237603219));
#96444=CARTESIAN_POINT('Ctrl Pts',(8.00361272030785,-9.86440457233314,3.8324432612319));
#96445=CARTESIAN_POINT('Ctrl Pts',(7.99175489825204,-9.75016564112609,4.12445767902653));
#96446=CARTESIAN_POINT('Ctrl Pts',(7.97985127327469,-9.6226052671416,4.41117579171117));
#96447=CARTESIAN_POINT('Ctrl Pts',(7.96794656006958,-9.48241448953288,4.69158072901337));
#96448=CARTESIAN_POINT('Ctrl Pts',(7.9560368093057,-9.34216438926174,4.97210432153467));
#96449=CARTESIAN_POINT('Ctrl Pts',(7.94412597831665,-9.18927254031056,5.24630895141322));
#96450=CARTESIAN_POINT('Ctrl Pts',(7.93226013853909,-9.02445980303907,5.51313322716271));
#96451=CARTESIAN_POINT('Ctrl Pts',(7.92772634728073,-8.96148688569672,5.61508349714716));
#96452=CARTESIAN_POINT('Ctrl Pts',(7.9231991379743,-8.89677397751238,5.71595588881535));
#96453=CARTESIAN_POINT('Ctrl Pts',(7.91868114386462,-8.83036269920675,5.81568976264978));
#96454=CARTESIAN_POINT('Ctrl Pts',(7.90363802990147,-8.6092396955607,6.14776368608839));
#96455=CARTESIAN_POINT('Ctrl Pts',(7.88863551605419,-8.36946664710543,6.467329519687));
#96456=CARTESIAN_POINT('Ctrl Pts',(7.87366135061745,-8.1127219252988,6.77251705231258));
#96457=CARTESIAN_POINT('Ctrl Pts',(7.86059975399369,-7.8887698121954,7.03872463914581));
#96458=CARTESIAN_POINT('Ctrl Pts',(7.84755972805931,-7.65190353345911,7.29399255982887));
#96459=CARTESIAN_POINT('Ctrl Pts',(7.83453293268559,-7.40320723697946,7.53706684196062));
#96460=CARTESIAN_POINT('Ctrl Pts',(7.82055549866077,-7.13636217059618,7.79787962393472));
#96461=CARTESIAN_POINT('Ctrl Pts',(7.80655344619261,-6.85586588937608,8.0448321766411));
#96462=CARTESIAN_POINT('Ctrl Pts',(7.79253868315848,-6.56314195267823,8.27617014315061));
#96463=CARTESIAN_POINT('Ctrl Pts',(7.77852392012436,-6.27041801598037,8.50750810966013));
#96464=CARTESIAN_POINT('Ctrl Pts',(7.76449645060328,-5.96546692684914,8.72323061436176));
#96465=CARTESIAN_POINT('Ctrl Pts',(7.75046860256975,-5.64975683954333,8.92161329300628));
#96466=CARTESIAN_POINT('Ctrl Pts',(7.73643453651719,-5.33390680979414,9.12008390725339));
#96467=CARTESIAN_POINT('Ctrl Pts',(7.72240009304984,-5.00728898979586,9.30119876896146));
#96468=CARTESIAN_POINT('Ctrl Pts',(7.7083779972811,-4.67208326333854,9.46439566421491));
#96469=CARTESIAN_POINT('Ctrl Pts',(7.69435590151235,-4.33687753688123,9.62759255946835));
#96470=CARTESIAN_POINT('Ctrl Pts',(7.6803461522571,-3.99308478902251,9.77287109063093));
#96471=CARTESIAN_POINT('Ctrl Pts',(7.66636185182228,-3.64290807812789,9.89971719420171));
#96472=CARTESIAN_POINT('Ctrl Pts',(7.65445708985596,-3.34480447196023,10.0077006200731));
#96473=CARTESIAN_POINT('Ctrl Pts',(7.64255734761132,-3.04196792755086,10.1024013789332));
#96474=CARTESIAN_POINT('Ctrl Pts',(7.63065709966863,-2.7355264387069,10.1835564166123));
#96475=CARTESIAN_POINT('Ctrl Pts',(7.62858144652543,-2.68207660786407,10.1977115594174));
#96476=CARTESIAN_POINT('Ctrl Pts',(7.62650577801372,-2.6285170677211,10.2114544823994));
#96477=CARTESIAN_POINT('Ctrl Pts',(7.62443006483418,-2.57485376276606,10.2247836327651));
#96478=CARTESIAN_POINT('Ctrl Pts',(7.61136764785412,-2.23715177544045,10.3086636802508));
#96479=CARTESIAN_POINT('Ctrl Pts',(7.59830284456884,-1.89532432840384,10.3761631879042));
#96480=CARTESIAN_POINT('Ctrl Pts',(7.58526635791234,-1.55097828880704,10.4267423524011));
#96481=CARTESIAN_POINT('Ctrl Pts',(7.57738000331749,-1.34266794851768,10.457339954105));
#96482=CARTESIAN_POINT('Ctrl Pts',(7.56950403796996,-1.13343670299237,10.4817448062152));
#96483=CARTESIAN_POINT('Ctrl Pts',(7.56164556698497,-0.923648317160969,
10.4998327504193));
#96484=CARTESIAN_POINT('Ctrl Pts',(7.55198659798043,-0.665794146785195,
10.5220649241789));
#96485=CARTESIAN_POINT('Ctrl Pts',(7.54235885760643,-0.407101643435756,
10.5347386581196));
#96486=CARTESIAN_POINT('Ctrl Pts',(7.53270344148809,-0.148322417901669,
10.5378431069723));
#96487=CARTESIAN_POINT('Ctrl Pts',(7.52305485201656,0.110273843547451,10.5409453608936));
#96488=CARTESIAN_POINT('Ctrl Pts',(7.51337856162289,0.368956567182821,10.5344924572168));
#96489=CARTESIAN_POINT('Ctrl Pts',(7.50361357471649,0.627026431465063,10.5184847695713));
#96490=CARTESIAN_POINT('Ctrl Pts',(7.50205789272213,0.668140121119621,10.5159345489023));
#96491=CARTESIAN_POINT('Ctrl Pts',(7.50049995672176,0.709238362916833,10.5131418363632));
#96492=CARTESIAN_POINT('Ctrl Pts',(7.49893951778007,0.750318451084926,10.5101066441853));
#96493=CARTESIAN_POINT('Ctrl Pts',(7.49893946511535,0.750319837535474,10.5101065417478));
#96494=CARTESIAN_POINT('Ctrl Pts',(7.49893941245062,0.750321223986051,10.5101064393099));
#96495=CARTESIAN_POINT('Ctrl Pts',(7.49893935978589,0.750322610436558,10.5101063368718));
#96496=CARTESIAN_POINT('Ctrl Pts',(7.48198998805347,1.19653141131127,10.4771381309561));
#96497=CARTESIAN_POINT('Ctrl Pts',(7.46508225238495,1.64030606335611,10.4146175450127));
#96498=CARTESIAN_POINT('Ctrl Pts',(7.44821688158249,2.07814433184817,10.3240954784714));
#96499=CARTESIAN_POINT('Ctrl Pts',(7.43170948506089,2.50668930693269,10.2354947792129));
#96500=CARTESIAN_POINT('Ctrl Pts',(7.41524267753539,2.92954651537385,10.1200692709601));
#96501=CARTESIAN_POINT('Ctrl Pts',(7.39881712372831,3.34346707870409,9.97930837620721));
#96502=CARTESIAN_POINT('Ctrl Pts',(7.39478374456776,3.4451074004778,9.94474381502492));
#96503=CARTESIAN_POINT('Ctrl Pts',(7.39075285267287,3.54620906299803,9.90865174356461));
#96504=CARTESIAN_POINT('Ctrl Pts',(7.38672445736098,3.64672436865318,9.87105448655237));
#96505=CARTESIAN_POINT('Ctrl Pts',(7.37411964003414,3.96123597147262,9.75341296432386));
#96506=CARTESIAN_POINT('Ctrl Pts',(7.3615169623578,4.27020880049875,9.62100692760719));
#96507=CARTESIAN_POINT('Ctrl Pts',(7.34895020829766,4.5722323797965,9.47431349544438));
#96508=CARTESIAN_POINT('Ctrl Pts',(7.33647642255021,4.87202160148474,9.32870529506109));
#96509=CARTESIAN_POINT('Ctrl Pts',(7.32403798719921,5.16496412382945,9.16901956140302));
#96510=CARTESIAN_POINT('Ctrl Pts',(7.31166977747338,5.44962988328277,8.99571647636085));
#96511=CARTESIAN_POINT('Ctrl Pts',(7.30318261108378,5.64496984916783,8.87679448593627));
#96512=CARTESIAN_POINT('Ctrl Pts',(7.29472854479695,5.83641137531478,8.75146020726419));
#96513=CARTESIAN_POINT('Ctrl Pts',(7.28631958659107,6.02347818357612,8.61986325984403));
#96514=CARTESIAN_POINT('Ctrl Pts',(7.27463137819316,6.28349562994193,8.4369473137403));
#96515=CARTESIAN_POINT('Ctrl Pts',(7.26280946049035,6.53535117459058,8.24246766819848));
#96516=CARTESIAN_POINT('Ctrl Pts',(7.25082513989488,6.77780730593302,8.03703899672175));
#96517=CARTESIAN_POINT('Ctrl Pts',(7.24996567306476,6.79519527557118,8.02230648621493));
#96518=CARTESIAN_POINT('Ctrl Pts',(7.24910537184593,6.81253492333505,8.00751767055478));
#96519=CARTESIAN_POINT('Ctrl Pts',(7.24824422611732,6.8298258026593,7.99267277976961));
#96520=CARTESIAN_POINT('Ctrl Pts',(7.24064310929476,6.98244804688657,7.86164066136463));
#96521=CARTESIAN_POINT('Ctrl Pts',(7.23297614520133,7.13126997787669,7.72623952432876));
#96522=CARTESIAN_POINT('Ctrl Pts',(7.22523669377821,7.27612659363062,7.58678420492436));
#96523=CARTESIAN_POINT('Ctrl Pts',(7.20794988167096,7.59967783287577,7.27529728264758));
#96524=CARTESIAN_POINT('Ctrl Pts',(7.19085345038819,7.90238058333808,6.94257127578086));
#96525=CARTESIAN_POINT('Ctrl Pts',(7.17393416520806,8.18237619965603,6.59192414856784));
#96526=CARTESIAN_POINT('Ctrl Pts',(7.17045404182884,8.23996842533526,6.51979963194222));
#96527=CARTESIAN_POINT('Ctrl Pts',(7.16698142602644,8.29659997351081,6.44691672877537));
#96528=CARTESIAN_POINT('Ctrl Pts',(7.16351622164847,8.35225469332804,6.37330404858248));
#96529=CARTESIAN_POINT('Ctrl Pts',(7.1511588668378,8.55072642678239,6.11079196892269));
#96530=CARTESIAN_POINT('Ctrl Pts',(7.13880542955081,8.73699807123786,5.8391004948121));
#96531=CARTESIAN_POINT('Ctrl Pts',(7.12645060901618,8.91038567592227,5.55937107268271));
#96532=CARTESIAN_POINT('Ctrl Pts',(7.1248820524924,8.93239880494414,5.5238568854272));
#96533=CARTESIAN_POINT('Ctrl Pts',(7.12331347368119,8.95420420288556,5.48821310102129));
#96534=CARTESIAN_POINT('Ctrl Pts',(7.1217448617425,8.97580041811654,5.45244202516763));
#96535=CARTESIAN_POINT('Ctrl Pts',(7.11016696045319,9.13520176015734,5.18841624859845));
#96536=CARTESIAN_POINT('Ctrl Pts',(7.09869336515209,9.28299403518174,4.91725496648527));
#96537=CARTESIAN_POINT('Ctrl Pts',(7.08726976744149,9.41861036362551,4.64013730851957));
#96538=CARTESIAN_POINT('Ctrl Pts',(7.07582835505919,9.55443818064142,4.36258749597136));
#96539=CARTESIAN_POINT('Ctrl Pts',(7.06443718727363,9.67805264090616,4.07906329225098));
#96540=CARTESIAN_POINT('Ctrl Pts',(7.0530392780045,9.78892239703109,3.79071360024181));
#96541=CARTESIAN_POINT('Ctrl Pts',(7.04163873223882,9.89981779888827,3.50229720889771));
#96542=CARTESIAN_POINT('Ctrl Pts',(7.03023142720831,9.9979632434126,3.20905351964547));
#96543=CARTESIAN_POINT('Ctrl Pts',(7.01875734339556,10.0828558637816,2.91208901810758));
#96544=CARTESIAN_POINT('Ctrl Pts',(7.01184760207909,10.1339785552311,2.73325575182819));
#96545=CARTESIAN_POINT('Ctrl Pts',(7.00491358093342,10.1802956248337,2.5530722654501));
#96546=CARTESIAN_POINT('Ctrl Pts',(6.99794178234568,10.2217007833587,2.3717717922649));
#96547=CARTESIAN_POINT('Ctrl Pts',(6.99792744780864,10.2217859154478,2.37139902499172));
#96548=CARTESIAN_POINT('Ctrl Pts',(6.99791311311183,10.2218710267728,2.37102625299427));
#96549=CARTESIAN_POINT('Ctrl Pts',(6.99789877825514,10.2219561173342,2.37065347627479));
#96550=CARTESIAN_POINT('Ctrl Pts',(6.98620503756456,10.2913692256778,2.06655875193916));
#96551=CARTESIAN_POINT('Ctrl Pts',(6.97438164383785,10.3470087783027,1.75942986008445));
#96552=CARTESIAN_POINT('Ctrl Pts',(6.96249146361515,10.3888788479672,1.45047588388174));
#96553=CARTESIAN_POINT('Ctrl Pts',(6.95054014680674,10.4309642039481,1.13993333703588));
#96554=CARTESIAN_POINT('Ctrl Pts',(6.93852148280035,10.4591373233995,0.827546860502543));
#96555=CARTESIAN_POINT('Ctrl Pts',(6.92650127112355,10.4733989646626,0.514596639856709));
#96556=CARTESIAN_POINT('Ctrl Pts',(6.92205360172844,10.4786759986347,0.398800083524568));
#96557=CARTESIAN_POINT('Ctrl Pts',(6.91760573093899,10.4820484148576,0.282926858573439));
#96558=CARTESIAN_POINT('Ctrl Pts',(6.91316102314921,10.4835164749871,0.167043612462112));
#96559=CARTESIAN_POINT('Ctrl Pts',(6.90321253510248,10.4868024004835,-0.0923352136112138));
#96560=CARTESIAN_POINT('Ctrl Pts',(6.8933906550617,10.480273521832,-0.351782186675668));
#96561=CARTESIAN_POINT('Ctrl Pts',(6.883627223104,10.4641867797313,-0.610563600947552));
#96562=CARTESIAN_POINT('Ctrl Pts',(6.87945102918872,10.4573058638025,-0.721254326540172));
#96563=CARTESIAN_POINT('Ctrl Pts',(6.87528552576304,10.4486761771571,-0.831823931034166));
#96564=CARTESIAN_POINT('Ctrl Pts',(6.87112532674824,10.4383173506522,-0.942217865737286));
#96565=CARTESIAN_POINT('Ctrl Pts',(6.85983053833117,10.4101935149399,-1.24193336746276));
#96566=CARTESIAN_POINT('Ctrl Pts',(6.84853943064584,10.3694127824273,-1.54036539315888));
#96567=CARTESIAN_POINT('Ctrl Pts',(6.83728918438053,10.3159772580025,-1.83647285089519));
#96568=CARTESIAN_POINT('Ctrl Pts',(6.83470795559292,10.3037171429194,-1.90441101652365));
#96569=CARTESIAN_POINT('Ctrl Pts',(6.83212888371649,10.2907907219817,-1.97222664598265));
#96570=CARTESIAN_POINT('Ctrl Pts',(6.82955242909833,10.2771977868899,-2.03990685551943));
#96571=CARTESIAN_POINT('Ctrl Pts',(6.81574446378667,10.2043493171716,-2.40262466897609));
#96572=CARTESIAN_POINT('Ctrl Pts',(6.80192036382046,10.1125117745603,-2.76168806542135));
#96573=CARTESIAN_POINT('Ctrl Pts',(6.78807745902409,10.0018741101773,-3.11483240124537));
#96574=CARTESIAN_POINT('Ctrl Pts',(6.77423455422773,9.89123644579426,-3.46797673706938));
#96575=CARTESIAN_POINT('Ctrl Pts',(6.76037284161516,9.76179888759734,-3.81520099936977));
#96576=CARTESIAN_POINT('Ctrl Pts',(6.74648934354437,9.61380470446798,-4.15425276629866));
#96577=CARTESIAN_POINT('Ctrl Pts',(6.73261001329415,9.46585494913316,-4.49320275002283));
#96578=CARTESIAN_POINT('Ctrl Pts',(6.71870890610072,9.29936006367006,-4.82398422208848));
#96579=CARTESIAN_POINT('Ctrl Pts',(6.70478279576421,9.11581742043377,-5.14496074671712));
#96580=CARTESIAN_POINT('Ctrl Pts',(6.69085668542771,8.93227477719748,-5.46593727134576));
#96581=CARTESIAN_POINT('Ctrl Pts',(6.67690556584498,8.73168518099751,-5.77710817676585));
#96582=CARTESIAN_POINT('Ctrl Pts',(6.6629260401176,8.51558669495431,-6.07687546169718));
#96583=CARTESIAN_POINT('Ctrl Pts',(6.64807074331246,8.28595035307013,-6.39542217615415));
#96584=CARTESIAN_POINT('Ctrl Pts',(6.63327942254754,8.03853954349429,-6.70106938587962));
#96585=CARTESIAN_POINT('Ctrl Pts',(6.61851871389973,7.77508392304408,-6.99208883334353));
#96586=CARTESIAN_POINT('Ctrl Pts',(6.6054942236311,7.54261709190193,-7.24887731497497));
#96587=CARTESIAN_POINT('Ctrl Pts',(6.59249356624743,7.29765716313496,-7.49427743212588));
#96588=CARTESIAN_POINT('Ctrl Pts',(6.57949316050575,7.04135873008535,-7.72710075685483));
#96589=CARTESIAN_POINT('Ctrl Pts',(6.56562633850373,6.76797920477563,-7.97544066763027));
#96590=CARTESIAN_POINT('Ctrl Pts',(6.55175959586778,6.48169310717675,-8.20947273883599));
#96591=CARTESIAN_POINT('Ctrl Pts',(6.53794775738398,6.18385922718087,-8.42753754943576));
#96592=CARTESIAN_POINT('Ctrl Pts',(6.52413591890019,5.886025347185,-8.64560236003553));
#96593=CARTESIAN_POINT('Ctrl Pts',(6.51037891881835,5.57664330890136,-8.84769897987254));
#96594=CARTESIAN_POINT('Ctrl Pts',(6.49673405207432,5.25712342423703,-9.03214895234355));
#96595=CARTESIAN_POINT('Ctrl Pts',(6.49673387958854,5.2571193851622,-9.03215128398949));
#96596=CARTESIAN_POINT('Ctrl Pts',(6.49673370710277,5.25711534608575,-9.0321536156326));
#96597=CARTESIAN_POINT('Ctrl Pts',(6.49673353461703,5.25711130700768,-9.0321559472729));
#96598=CARTESIAN_POINT('Ctrl Pts',(6.47784823489588,4.81487650934325,-9.28744501520444));
#96599=CARTESIAN_POINT('Ctrl Pts',(6.45884300813255,4.35359187063555,-9.50957315768382));
#96600=CARTESIAN_POINT('Ctrl Pts',(6.43975306559737,3.87857966579415,-9.69706314280026));
#96601=CARTESIAN_POINT('Ctrl Pts',(6.42033130758202,3.39531094564121,-9.88781202088218));
#96602=CARTESIAN_POINT('Ctrl Pts',(6.40082193578461,2.89783297111858,-10.0427069401333));
#96603=CARTESIAN_POINT('Ctrl Pts',(6.38126510777301,2.3918007507519,-10.1601748393213));
#96604=CARTESIAN_POINT('Ctrl Pts',(6.3783858841865,2.31730094415984,-10.1774688680769));
#96605=CARTESIAN_POINT('Ctrl Pts',(6.37550563631349,2.24261581791397,-10.1939516648252));
#96606=CARTESIAN_POINT('Ctrl Pts',(6.37262449652578,2.16776351169906,-10.2096182042152));
#96607=CARTESIAN_POINT('Ctrl Pts',(6.35286828018625,1.65449499158147,-10.3170449742732));
#96608=CARTESIAN_POINT('Ctrl Pts',(6.33306997362655,1.13336162687368,-10.3860905466361));
#96609=CARTESIAN_POINT('Ctrl Pts',(6.3132733717463,0.610349461919558,-10.4158264066385));
#96610=CARTESIAN_POINT('Ctrl Pts',(6.29373395326672,0.0941318997962036,
-10.4451759594532));
#96611=CARTESIAN_POINT('Ctrl Pts',(6.27419620422037,-0.423915227717483,
-10.4362291878969));
#96612=CARTESIAN_POINT('Ctrl Pts',(6.25470391212629,-0.937992906419497,
-10.3881184713038));
#96613=CARTESIAN_POINT('Ctrl Pts',(6.25226070791324,-1.00242846609496,-10.3820881745636));
#96614=CARTESIAN_POINT('Ctrl Pts',(6.24981822003481,-1.06680161607427,-10.3754426356291));
#96615=CARTESIAN_POINT('Ctrl Pts',(6.24737653663699,-1.13110089858024,-10.3681801908432));
#96616=CARTESIAN_POINT('Ctrl Pts',(6.24737506176842,-1.13113973776426,-10.3681758040536));
#96617=CARTESIAN_POINT('Ctrl Pts',(6.24737358690014,-1.1311785769213,-10.3681714170388));
#96618=CARTESIAN_POINT('Ctrl Pts',(6.24737211203216,-1.13121741605142,-10.3681670297989));
#96619=CARTESIAN_POINT('Ctrl Pts',(6.22417898983719,-1.74198441449639,-10.2991752343847));
#96620=CARTESIAN_POINT('Ctrl Pts',(6.20101181766919,-2.34646124507136,-10.1745430361542));
#96621=CARTESIAN_POINT('Ctrl Pts',(6.17786738316811,-2.93569442720166,-9.99822295766118));
#96622=CARTESIAN_POINT('Ctrl Pts',(6.15379904898534,-3.54844913237382,-9.81486438080322));
#96623=CARTESIAN_POINT('Ctrl Pts',(6.12975530887175,-4.14471762789403,-9.57560943680304));
#96624=CARTESIAN_POINT('Ctrl Pts',(6.10573222227401,-4.71443073759851,-9.28496134416452));
#96625=CARTESIAN_POINT('Ctrl Pts',(6.08121404253301,-5.29588509683334,-8.98832326863274));
#96626=CARTESIAN_POINT('Ctrl Pts',(6.05671737982178,-5.8496768475326,-8.63815268934198));
#96627=CARTESIAN_POINT('Ctrl Pts',(6.03223764683064,-6.36512167495428,-8.23928595966293));
#96628=CARTESIAN_POINT('Ctrl Pts',(6.0209303082614,-6.60320879704551,-8.0550469747802));
#96629=CARTESIAN_POINT('Ctrl Pts',(6.00962657594759,-6.83311473533747,-7.86041891267326));
#96630=CARTESIAN_POINT('Ctrl Pts',(5.998325967254,-7.0537891945181,-7.65588108533446));
#96631=CARTESIAN_POINT('Ctrl Pts',(5.99831956952164,-7.05391412726871,-7.65576528818481));
#96632=CARTESIAN_POINT('Ctrl Pts',(5.99831317179029,-7.05403905706055,-7.65564948785897));
#96633=CARTESIAN_POINT('Ctrl Pts',(5.99830677405993,-7.05416398389352,-7.65553368435712));
#96634=CARTESIAN_POINT('Ctrl Pts',(5.97508168029947,-7.50767440834225,-7.2351428521476));
#96635=CARTESIAN_POINT('Ctrl Pts',(5.95185196548336,-7.92212415910938,-6.7730276653975));
#96636=CARTESIAN_POINT('Ctrl Pts',(5.92862314188893,-8.2928164442724,-6.27799373205562));
#96637=CARTESIAN_POINT('Ctrl Pts',(5.90462840496468,-8.6757313958704,-5.76663727223179));
#96638=CARTESIAN_POINT('Ctrl Pts',(5.8806346180938,-9.0119563867889,-5.22015401889032));
#96639=CARTESIAN_POINT('Ctrl Pts',(5.85664836077958,-9.29627330714031,-4.64821044104104));
#96640=CARTESIAN_POINT('Ctrl Pts',(5.83271966389727,-9.57990794494461,-4.07763937074639));
#96641=CARTESIAN_POINT('Ctrl Pts',(5.80879846099807,-9.81188372396935,-3.48172845089952));
#96642=CARTESIAN_POINT('Ctrl Pts',(5.7848917759895,-9.98697203229548,-2.87005949959171));
#96643=CARTESIAN_POINT('Ctrl Pts',(5.77325976611036,-10.0721628034728,-2.57244653979286));
#96644=CARTESIAN_POINT('Ctrl Pts',(5.76163120054524,-10.1438853013618,-2.27110294951748));
#96645=CARTESIAN_POINT('Ctrl Pts',(5.75000693068917,-10.2015327465523,-1.96713277598939));
#96646=CARTESIAN_POINT('Ctrl Pts',(5.75000229790167,-10.201555721618,-1.96701163038288));
#96647=CARTESIAN_POINT('Ctrl Pts',(5.74999766511417,-10.2015786944493,-1.96689048435908));
#96648=CARTESIAN_POINT('Ctrl Pts',(5.74999303232669,-10.2016016650461,-1.96676933791808));
#96649=CARTESIAN_POINT('Ctrl Pts',(5.72266451037347,-10.3371037708125,-1.2521341023623));
#96650=CARTESIAN_POINT('Ctrl Pts',(5.69533641472616,-10.394848005795,-0.522978506931299));
#96651=CARTESIAN_POINT('Ctrl Pts',(5.66801289675197,-10.3769973889688,0.204494087600538));
#96652=CARTESIAN_POINT('Ctrl Pts',(5.63977329699423,-10.3585482904641,0.956356820785527));
#96653=CARTESIAN_POINT('Ctrl Pts',(5.61153858643246,-10.2593502213994,1.70642010905303));
#96654=CARTESIAN_POINT('Ctrl Pts',(5.58331348970829,-10.0818433849781,2.43677691238762));
#96655=CARTESIAN_POINT('Ctrl Pts',(5.5562635484521,-9.91172706811686,3.13672521794417));
#96656=CARTESIAN_POINT('Ctrl Pts',(5.5292224381274,-9.66968745763753,3.81857221540741));
#96657=CARTESIAN_POINT('Ctrl Pts',(5.50219443957856,-9.35791672220047,4.46656365982966));
#96658=CARTESIAN_POINT('Ctrl Pts',(5.50219405281362,-9.3579122608272,4.46657293245014));
#96659=CARTESIAN_POINT('Ctrl Pts',(5.50219366604868,-9.35790779943968,4.46658220506364));
#96660=CARTESIAN_POINT('Ctrl Pts',(5.50219327928375,-9.35790333803786,4.46659147767025));
#96661=CARTESIAN_POINT('Ctrl Pts',(5.46506916479616,-8.92967012276696,5.35663418252138));
#96662=CARTESIAN_POINT('Ctrl Pts',(5.42796768099261,-8.36987247228588,6.18285085526827));
#96663=CARTESIAN_POINT('Ctrl Pts',(5.39088688229172,-7.70723164974139,6.91584755034263));
#96664=CARTESIAN_POINT('Ctrl Pts',(5.3528736784168,-7.02792857198343,7.66727561515523));
#96665=CARTESIAN_POINT('Ctrl Pts',(5.31488221310929,-6.24054371848018,8.32073862513858));
#96666=CARTESIAN_POINT('Ctrl Pts',(5.27691036332006,-5.37597656080281,8.84454225364133));
#96667=CARTESIAN_POINT('Ctrl Pts',(5.26958608558794,-5.20921276035468,8.94557718540107));
#96668=CARTESIAN_POINT('Ctrl Pts',(5.26226253757739,-5.03957727573607,9.04178795673227));
#96669=CARTESIAN_POINT('Ctrl Pts',(5.25493970393503,-4.86729175390944,9.13294690721646));
#96670=CARTESIAN_POINT('Ctrl Pts',(5.25493968611562,-4.86729133466932,9.13294712904293));
#96671=CARTESIAN_POINT('Ctrl Pts',(5.25493966829622,-4.86729091542919,9.13294735086937));
#96672=CARTESIAN_POINT('Ctrl Pts',(5.25493965047681,-4.86729049618903,9.13294757269579));
#96673=CARTESIAN_POINT('Ctrl Pts',(5.21070364291279,-3.82654253050402,9.68362332642355));
#96674=CARTESIAN_POINT('Ctrl Pts',(5.16646436531577,-2.68916245918068,10.0499722137216));
#96675=CARTESIAN_POINT('Ctrl Pts',(5.12224167595592,-1.52387103549523,10.2206421596411));
#96676=CARTESIAN_POINT('Ctrl Pts',(5.08416977506241,-0.520656164649018,
10.3675741839165));
#96677=CARTESIAN_POINT('Ctrl Pts',(5.04611019969174,0.503245735025882,10.369472651501));
#96678=CARTESIAN_POINT('Ctrl Pts',(5.00807667263332,1.50395692832491,10.2190800401682));
#96679=CARTESIAN_POINT('Ctrl Pts',(5.00807571336979,1.50398216778658,10.2190762470373));
#96680=CARTESIAN_POINT('Ctrl Pts',(5.00807475410628,1.50400740723351,10.2190724538095));
#96681=CARTESIAN_POINT('Ctrl Pts',(5.00807379484279,1.50403264666567,10.2190686604848));
#96682=CARTESIAN_POINT('Ctrl Pts',(4.96444129015806,2.65205886646503,10.0465276883694));
#96683=CARTESIAN_POINT('Ctrl Pts',(4.92083357238826,3.76958415940242,9.67356309954827));
#96684=CARTESIAN_POINT('Ctrl Pts',(4.87724979701675,4.79633951199453,9.1308780752111));
#96685=CARTESIAN_POINT('Ctrl Pts',(4.83871681435949,5.7041072732183,8.6510831870242));
#96686=CARTESIAN_POINT('Ctrl Pts',(4.80020254377808,6.54092293690988,8.03862698318508));
#96687=CARTESIAN_POINT('Ctrl Pts',(4.76170628627147,7.26515529284603,7.31475570640799));
#96688=CARTESIAN_POINT('Ctrl Pts',(4.76170224698123,7.2652312842508,7.31467975289011));
#96689=CARTESIAN_POINT('Ctrl Pts',(4.76169820769119,7.26530727441612,7.31460379814559));
#96690=CARTESIAN_POINT('Ctrl Pts',(4.76169416840135,7.26538326334192,7.31452784217451));
#96691=CARTESIAN_POINT('Ctrl Pts',(4.71294834591452,8.18241146189463,6.39789733855326));
#96692=CARTESIAN_POINT('Ctrl Pts',(4.66423043686984,8.91894727366709,5.3026200862389));
#96693=CARTESIAN_POINT('Ctrl Pts',(4.61553898512807,9.43455879998508,4.11255713400774));
#96694=CARTESIAN_POINT('Ctrl Pts',(4.58228459333126,9.78670167307214,3.29978983583315));
#96695=CARTESIAN_POINT('Ctrl Pts',(4.54904254230922,10.0357967364297,2.44280989826008));
#96696=CARTESIAN_POINT('Ctrl Pts',(4.51581236975189,10.1689504712162,1.56832823132173));
#96697=CARTESIAN_POINT('Ctrl Pts',(4.50221482292277,10.2234360186839,1.21049664327063));
#96698=CARTESIAN_POINT('Ctrl Pts',(4.48861965687846,10.2585067326653,0.849744968950366));
#96699=CARTESIAN_POINT('Ctrl Pts',(4.4750268723026,10.2743826178923,0.488134898172381));
#96700=CARTESIAN_POINT('Ctrl Pts',(4.43404183365644,10.3222516741507,-0.602193771641681));
#96701=CARTESIAN_POINT('Ctrl Pts',(4.39307844339743,10.1956112695613,-1.70032308395014));
#96702=CARTESIAN_POINT('Ctrl Pts',(4.35213669516808,9.9004959265895,-2.74976740252401));
#96703=CARTESIAN_POINT('Ctrl Pts',(4.35213425480337,9.90047833601024,-2.74982995546783));
#96704=CARTESIAN_POINT('Ctrl Pts',(4.35213181443874,9.9004607448324,-2.74989250823873));
#96705=CARTESIAN_POINT('Ctrl Pts',(4.35212937407419,9.90044315305601,-2.74995506083663));
#96706=CARTESIAN_POINT('Ctrl Pts',(4.32158644227856,9.68026931644747,-3.53284617798636));
#96707=CARTESIAN_POINT('Ctrl Pts',(4.29112143584156,9.36621225935035,-4.28872013106504));
#96708=CARTESIAN_POINT('Ctrl Pts',(4.26068196180613,8.96886291644311,-4.99759054013052));
#96709=CARTESIAN_POINT('Ctrl Pts',(4.23679094882394,8.65699555964141,-5.55396126210704));
#96710=CARTESIAN_POINT('Ctrl Pts',(4.21291561406977,8.29381931908319,-6.0813783156756));
#96711=CARTESIAN_POINT('Ctrl Pts',(4.18902945460217,7.88444870906465,-6.57020010178684));
#96712=CARTESIAN_POINT('Ctrl Pts',(4.18902715704074,7.88440933253259,-6.57024712056703));
#96713=CARTESIAN_POINT('Ctrl Pts',(4.18902485947921,7.88436995557313,-6.57029413899016));
#96714=CARTESIAN_POINT('Ctrl Pts',(4.18902256191758,7.88433057818626,-6.5703411570562));
#96715=CARTESIAN_POINT('Ctrl Pts',(4.1632552257245,7.44271005679019,-7.09765250229566));
#96716=CARTESIAN_POINT('Ctrl Pts',(4.13741478222157,6.94744670774601,-7.58004695698877));
#96717=CARTESIAN_POINT('Ctrl Pts',(4.11155104549517,6.40953211685417,-8.00846912279131));
#96718=CARTESIAN_POINT('Ctrl Pts',(4.08529628275577,5.86348495795648,-8.44336847374108));
#96719=CARTESIAN_POINT('Ctrl Pts',(4.05901752914186,5.27348561834659,-8.82265002777255));
#96720=CARTESIAN_POINT('Ctrl Pts',(4.03276906429671,4.65106218177041,-9.13679878128589));
#96721=CARTESIAN_POINT('Ctrl Pts',(4.03036741752322,4.59411251835131,-9.16554234189878));
#96722=CARTESIAN_POINT('Ctrl Pts',(4.02796602575629,4.53689144154322,-9.19374061335957));
#96723=CARTESIAN_POINT('Ctrl Pts',(4.02556493144338,4.47940780021195,-9.22138629613659));
#96724=CARTESIAN_POINT('Ctrl Pts',(4.02556067586587,4.47930591912809,-9.22143529393945));
#96725=CARTESIAN_POINT('Ctrl Pts',(4.0255564202893,4.47920403721944,-9.22148429000651));
#96726=CARTESIAN_POINT('Ctrl Pts',(4.02555216471366,4.47910215448609,-9.22153328433775));
#96727=CARTESIAN_POINT('Ctrl Pts',(3.9873185556959,3.5637513479104,-9.66171582700827));
#96728=CARTESIAN_POINT('Ctrl Pts',(3.94914314148061,2.58176394555035,-9.9618342338202));
#96729=CARTESIAN_POINT('Ctrl Pts',(3.91100064892575,1.57790761846552,-10.1155811452561));
#96730=CARTESIAN_POINT('Ctrl Pts',(3.87146176774654,0.537300322533742,-10.2749566987596));
#96731=CARTESIAN_POINT('Ctrl Pts',(3.83195827482488,-0.52680434757945,-10.2770491449444));
#96732=CARTESIAN_POINT('Ctrl Pts',(3.7924602653118,-1.5645710703495,-10.1148748761191));
#96733=CARTESIAN_POINT('Ctrl Pts',(3.788594769662,-1.66613271362796,-10.0990035970754));
#96734=CARTESIAN_POINT('Ctrl Pts',(3.78472932511899,-1.76744213763999,-10.0815590438861));
#96735=CARTESIAN_POINT('Ctrl Pts',(3.78086390273701,-1.86845265557679,-10.0625346803859));
#96736=CARTESIAN_POINT('Ctrl Pts',(3.780860589853,-1.86853922726204,-10.0625183754382));
#96737=CARTESIAN_POINT('Ctrl Pts',(3.78085727696901,-1.86862579872775,-10.0625020693301));
#96738=CARTESIAN_POINT('Ctrl Pts',(3.78085396408503,-1.86871236997385,-10.0624857620616));
#96739=CARTESIAN_POINT('Ctrl Pts',(3.73455994817976,-3.07845308838546,-9.83460909809688));
#96740=CARTESIAN_POINT('Ctrl Pts',(3.68829656615448,-4.24527786346278,-9.38011420520289));
#96741=CARTESIAN_POINT('Ctrl Pts',(3.6420593453693,-5.29746547139911,-8.73927930300581));
#96742=CARTESIAN_POINT('Ctrl Pts',(3.60692904188819,-6.09690084744844,-8.25238315714807));
#96743=CARTESIAN_POINT('Ctrl Pts',(3.5718138394396,-6.83016017244939,-7.65791659589164));
#96744=CARTESIAN_POINT('Ctrl Pts',(3.53671175474974,-7.46577881040882,-6.97352719727064));
#96745=CARTESIAN_POINT('Ctrl Pts',(3.5367108904692,-7.46579446055678,-6.97351034629316));
#96746=CARTESIAN_POINT('Ctrl Pts',(3.53671002618867,-7.46581011064555,-6.97349349526117));
#96747=CARTESIAN_POINT('Ctrl Pts',(3.53670916190815,-7.46582576067513,-6.97347664417466));
#96748=CARTESIAN_POINT('Ctrl Pts',(3.4823015581945,-8.45101585130913,-5.9126784287268));
#96749=CARTESIAN_POINT('Ctrl Pts',(3.4279208344336,-9.20162723145157,-4.63584441625589));
#96750=CARTESIAN_POINT('Ctrl Pts',(3.37357498862076,-9.6634632420053,-3.2641321751324));
#96751=CARTESIAN_POINT('Ctrl Pts',(3.34671036430489,-9.89176129742237,-2.58605764199928));
#96752=CARTESIAN_POINT('Ctrl Pts',(3.31985426267946,-10.0494949150043,-1.8847995037906));
#96753=CARTESIAN_POINT('Ctrl Pts',(3.29300764938461,-10.1301213490435,-1.17499530757419));
#96754=CARTESIAN_POINT('Ctrl Pts',(3.29300737878892,-10.1301221617033,-1.17498815322841));
#96755=CARTESIAN_POINT('Ctrl Pts',(3.29300710819324,-10.1301229743554,-1.17498099888179));
#96756=CARTESIAN_POINT('Ctrl Pts',(3.29300683759755,-10.1301237869996,-1.17497384453428));
#96757=CARTESIAN_POINT('Ctrl Pts',(3.21185057929997,-10.3738496355576,0.970736917854522));
#96758=CARTESIAN_POINT('Ctrl Pts',(3.13078041734505,-9.91295623704456,3.19455927349203));
#96759=CARTESIAN_POINT('Ctrl Pts',(3.0497432811088,-8.83631410419166,5.0625402813841));
#96760=CARTESIAN_POINT('Ctrl Pts',(3.04974324576439,-8.83631363461336,5.06254109610547));
#96761=CARTESIAN_POINT('Ctrl Pts',(3.04974321041998,-8.83631316503494,5.06254191082676));
#96762=CARTESIAN_POINT('Ctrl Pts',(3.04974317507557,-8.83631269545641,5.06254272554799));
#96763=CARTESIAN_POINT('Ctrl Pts',(2.96870606622953,-7.75967038899954,6.93052279233136));
#96764=CARTESIAN_POINT('Ctrl Pts',(2.88769487591149,-6.06728729027483,8.44265309220118));
#96765=CARTESIAN_POINT('Ctrl Pts',(2.8068361779323,-4.09486592668815,9.30412583679137));
#96766=CARTESIAN_POINT('Ctrl Pts',(2.80683611536455,-4.09486440044578,9.30412650339143));
#96767=CARTESIAN_POINT('Ctrl Pts',(2.8068360527968,-4.09486287420324,9.3041271699911));
#96768=CARTESIAN_POINT('Ctrl Pts',(2.80683599022905,-4.09486134796053,9.30412783659038));
#96769=CARTESIAN_POINT('Ctrl Pts',(2.72597728129989,-2.12243927812803,10.1655996934111));
#96770=CARTESIAN_POINT('Ctrl Pts',(2.64526902547895,0.130022929717388,10.3764171800569));
#96771=CARTESIAN_POINT('Ctrl Pts',(2.56440160022704,2.22644944606699,9.9009745582931));
#96772=CARTESIAN_POINT('Ctrl Pts',(2.56440154883982,2.22645077824169,9.90097425617298));
#96773=CARTESIAN_POINT('Ctrl Pts',(2.56440149745259,2.22645211041634,9.90097395405258));
#96774=CARTESIAN_POINT('Ctrl Pts',(2.56440144606537,2.22645344259091,9.9009736519319));
#96775=CARTESIAN_POINT('Ctrl Pts',(2.50375088007378,3.79877310078287,9.54439104970355));
#96776=CARTESIAN_POINT('Ctrl Pts',(2.44301069353154,5.28332210046277,8.80178787523277));
#96777=CARTESIAN_POINT('Ctrl Pts',(2.38270289273039,6.51457988529196,7.76336126950861));
#96778=CARTESIAN_POINT('Ctrl Pts',(2.38270285132624,6.51458073060865,7.76336055657964));
#96779=CARTESIAN_POINT('Ctrl Pts',(2.38270280992208,6.51458157592522,7.76335984365053));
#96780=CARTESIAN_POINT('Ctrl Pts',(2.38270276851792,6.51458242124167,7.76335913072129));
#96781=CARTESIAN_POINT('Ctrl Pts',(2.32239495750723,7.7458400788396,6.72493193278451));
#96782=CARTESIAN_POINT('Ctrl Pts',(2.26251945886829,8.72380625407125,5.39068122422641));
#96783=CARTESIAN_POINT('Ctrl Pts',(2.20092967279735,9.34038183650534,3.904460088484));
#96784=CARTESIAN_POINT('Ctrl Pts',(2.20092964154596,9.34038214936309,3.90445933435779));
#96785=CARTESIAN_POINT('Ctrl Pts',(2.20092961029457,9.34038246222075,3.90445858023155));
#96786=CARTESIAN_POINT('Ctrl Pts',(2.20092957904319,9.34038277507832,3.90445782610527));
#96787=CARTESIAN_POINT('Ctrl Pts',(2.13933978131243,9.95695809007495,2.41823629675763));
#96788=CARTESIAN_POINT('Ctrl Pts',(2.07603570970493,10.2121426779904,0.780044366453755));
#96789=CARTESIAN_POINT('Ctrl Pts',(2.02490864864471,10.0782374348533,-0.8232068657955));
#96790=CARTESIAN_POINT('Ctrl Pts',(2.02490863093715,10.078237388476,-0.823207421072074));
#96791=CARTESIAN_POINT('Ctrl Pts',(2.0249086132296,10.0782373420987,-0.823207976348632));
#96792=CARTESIAN_POINT('Ctrl Pts',(2.02490859552205,10.0782372957213,-0.823208531625197));
#96793=CARTESIAN_POINT('Ctrl Pts',(1.97378152518914,9.94433173668894,-2.42646029494826));
#96794=CARTESIAN_POINT('Ctrl Pts',(1.93483149973001,9.42133607968513,-3.99477132083159));
#96795=CARTESIAN_POINT('Ctrl Pts',(1.89057925223621,8.56795357878977,-5.35484594214714));
#96796=CARTESIAN_POINT('Ctrl Pts',(1.84632700474241,7.71457107789448,-6.71492056346257));
#96797=CARTESIAN_POINT('Ctrl Pts',(1.79677221505219,6.53080200225584,-7.86675896507663));
#96798=CARTESIAN_POINT('Ctrl Pts',(1.74981056084319,5.14938720565873,-8.68267575370497));
#96799=CARTESIAN_POINT('Ctrl Pts',(1.70284890663419,3.7679724090616,-9.49859254233332));
#96800=CARTESIAN_POINT('Ctrl Pts',(1.65848047414983,2.18891191363664,-9.97858753801619));
#96801=CARTESIAN_POINT('Ctrl Pts',(1.61287087089241,0.588436780637463,-10.0693886900755));
#96802=CARTESIAN_POINT('Ctrl Pts',(1.56726126763499,-1.01203835236172,-10.1601898421347));
#96803=CARTESIAN_POINT('Ctrl Pts',(1.52041065882194,-2.63392819356923,-9.86179707393502));
#96804=CARTESIAN_POINT('Ctrl Pts',(1.47417904873224,-4.0963019978624,-9.20823383025107));
#96805=CARTESIAN_POINT('Ctrl Pts',(1.42794743864254,-5.55867580215555,-8.55467058656714));
#96806=CARTESIAN_POINT('Ctrl Pts',(1.38233482776403,-6.86153352960957,-7.54593681589203));
#96807=CARTESIAN_POINT('Ctrl Pts',(1.33646527388512,-7.85993138550466,-6.29513977391115));
#96808=CARTESIAN_POINT('Ctrl Pts',(1.33646525437671,-7.85993181012511,-6.29513924194485));
#96809=CARTESIAN_POINT('Ctrl Pts',(1.33646523486831,-7.85993223474552,-6.29513870997851));
#96810=CARTESIAN_POINT('Ctrl Pts',(1.3364652153599,-7.85993265936586,-6.29513817801212));
#96811=CARTESIAN_POINT('Ctrl Pts',(1.29059568077079,-8.85832983166594,-5.04434146209779));
#96812=CARTESIAN_POINT('Ctrl Pts',(1.2444691451342,-9.55226747109698,-3.55148181412588));
#96813=CARTESIAN_POINT('Ctrl Pts',(1.19848374839593,-9.86486406742352,-1.98300024121239));
#96814=CARTESIAN_POINT('Ctrl Pts',(1.19848371043099,-9.86486432549917,-1.98299894629458));
#96815=CARTESIAN_POINT('Ctrl Pts',(1.19848367246605,-9.86486458357456,-1.98299765137672));
#96816=CARTESIAN_POINT('Ctrl Pts',(1.19848363450111,-9.86486484164969,-1.98299635645881));
#96817=CARTESIAN_POINT('Ctrl Pts',(1.15249825640295,-10.1774606831884,-0.414515286520078));
#96818=CARTESIAN_POINT('Ctrl Pts',(1.10665389177668,-10.108715622417,1.22958744142003));
#96819=CARTESIAN_POINT('Ctrl Pts',(1.06077272615717,-9.6668224629688,2.76499530979388));
#96820=CARTESIAN_POINT('Ctrl Pts',(1.06077267392965,-9.66682195995227,2.76499705758183));
#96821=CARTESIAN_POINT('Ctrl Pts',(1.06077262170212,-9.66682145693525,2.76499880536965));
#96822=CARTESIAN_POINT('Ctrl Pts',(1.0607725694746,-9.66682095391775,2.76500055315732));
#96823=CARTESIAN_POINT('Ctrl Pts',(1.01489141812013,-9.22492708313986,4.30040769389711));
#96824=CARTESIAN_POINT('Ctrl Pts',(0.968973556976535,-8.40988552547852,
5.7271200694946));
#96825=CARTESIAN_POINT('Ctrl Pts',(0.923099914547117,-7.31332528013523,
6.88827573562447));
#96826=CARTESIAN_POINT('Ctrl Pts',(0.923099853871573,-7.31332382975139,
6.88827727144652));
#96827=CARTESIAN_POINT('Ctrl Pts',(0.923099793196029,-7.31332237936706,
6.88827880726812));
#96828=CARTESIAN_POINT('Ctrl Pts',(0.923099732520485,-7.31332092898224,
6.88828034308924));
#96829=CARTESIAN_POINT('Ctrl Pts',(0.877226098664229,-6.21676014107444,
8.04943509267856));
#96830=CARTESIAN_POINT('Ctrl Pts',(0.831396537222939,-4.83868108936204,
8.94503264313261));
#96831=CARTESIAN_POINT('Ctrl Pts',(0.785565047764798,-3.33266910390279,
9.47139320809289));
#96832=CARTESIAN_POINT('Ctrl Pts',(0.785565021561048,-3.33266824285372,
9.4713935090349));
#96833=CARTESIAN_POINT('Ctrl Pts',(0.785564995357298,-3.33266738180461,
9.47139380997679));
#96834=CARTESIAN_POINT('Ctrl Pts',(0.785564969153548,-3.33266652075545,
9.47139411091856));
#96835=CARTESIAN_POINT('Ctrl Pts',(0.739733508623329,-1.82665533964524,
9.99775392140918));
#96836=CARTESIAN_POINT('Ctrl Pts',(0.69390009258822,-0.192711114356479,
10.1548771844308));
#96837=CARTESIAN_POINT('Ctrl Pts',(0.648109453171715,1.38573190269856,9.93448485345363));
#96838=CARTESIAN_POINT('Ctrl Pts',(0.648109389881921,1.38573408435262,9.9344845488371));
#96839=CARTESIAN_POINT('Ctrl Pts',(0.648109326592126,1.38573626600657,9.93448424421986));
#96840=CARTESIAN_POINT('Ctrl Pts',(0.648109263302332,1.38573844766041,9.9344839396019));
#96841=CARTESIAN_POINT('Ctrl Pts',(0.602318710855294,2.96417831745571,9.71409098307494));
#96842=CARTESIAN_POINT('Ctrl Pts',(0.55657106409896,4.48711614855536,9.11618402724221));
#96843=CARTESIAN_POINT('Ctrl Pts',(0.510790325696514,5.78709048373477,8.19054629258984));
#96844=CARTESIAN_POINT('Ctrl Pts',(0.510790149412866,5.7870954894255,8.19054272832237));
#96845=CARTESIAN_POINT('Ctrl Pts',(0.510789973129217,5.78710049511293,8.19053916405004));
#96846=CARTESIAN_POINT('Ctrl Pts',(0.510789796845568,5.78710550079706,8.19053559977285));
#96847=CARTESIAN_POINT('Ctrl Pts',(0.465009082869899,7.08707741803496,7.26489584023529));
#96848=CARTESIAN_POINT('Ctrl Pts',(0.419194914517885,8.16408492797094,6.01152556991958));
#96849=CARTESIAN_POINT('Ctrl Pts',(0.373507579661479,8.89329891757632,4.60936110569497));
#96850=CARTESIAN_POINT('Ctrl Pts',(0.373507379106137,8.89330211863328,4.60935495056302));
#96851=CARTESIAN_POINT('Ctrl Pts',(0.373507178550797,8.89330531968354,4.60934879542821));
#96852=CARTESIAN_POINT('Ctrl Pts',(0.373506977995459,8.8933085207271,4.60934264029053));
#96853=CARTESIAN_POINT('Ctrl Pts',(0.327819443697221,9.6225226579455,3.20717071459683));
#96854=CARTESIAN_POINT('Ctrl Pts',(0.282261170678959,10.0039434919652,1.6562059829034));
#96855=CARTESIAN_POINT('Ctrl Pts',(0.236247419988345,10.0098541173715,0.0109034851016902));
#96856=CARTESIAN_POINT('Ctrl Pts',(20.3193161062581,-10.8205589424572,-0.0274550152749159));
#96857=CARTESIAN_POINT('Ctrl Pts',(20.3174123187361,-10.8253380330767,0.034723062884607));
#96858=CARTESIAN_POINT('Ctrl Pts',(20.3156419101068,-10.8304776395509,0.092329568131463));
#96859=CARTESIAN_POINT('Ctrl Pts',(20.3139884606019,-10.838945329927,0.146171788417064));
#96860=CARTESIAN_POINT('Ctrl Pts',(20.313582681329,-10.8417916635006,0.159397329278271));
#96861=CARTESIAN_POINT('Ctrl Pts',(20.3132737488013,-10.8459274194006,0.16951983910409));
#96862=CARTESIAN_POINT('Ctrl Pts',(20.3132119638891,-10.8470106149663,0.171551138051299));
#96863=CARTESIAN_POINT('Ctrl Pts',(20.3131578861053,-10.8486133792296,0.17334615859031));
#96864=CARTESIAN_POINT('Ctrl Pts',(20.3131442649206,-10.8491158658176,0.173800871954156));
#96865=CARTESIAN_POINT('Ctrl Pts',(20.313129658019,-10.8500405501164,0.174298436740182));
#96866=CARTESIAN_POINT('Ctrl Pts',(20.313125892081,-10.850423694506,0.174430447775073));
#96867=CARTESIAN_POINT('Ctrl Pts',(20.313124076547,-10.851186062719,0.174508900562405));
#96868=CARTESIAN_POINT('Ctrl Pts',(20.3131254455118,-10.8515368492789,0.174473476044135));
#96869=CARTESIAN_POINT('Ctrl Pts',(20.3131327610704,-10.8522949105386,0.174255487039109));
#96870=CARTESIAN_POINT('Ctrl Pts',(20.3131393815545,-10.8526798380712,0.174050470864689));
#96871=CARTESIAN_POINT('Ctrl Pts',(20.3131611608867,-10.8536464139303,0.173368233548088));
#96872=CARTESIAN_POINT('Ctrl Pts',(20.3131798412209,-10.8541953909257,0.172775776396129));
#96873=CARTESIAN_POINT('Ctrl Pts',(20.3132437615228,-10.8557810771898,0.17074055793655));
#96874=CARTESIAN_POINT('Ctrl Pts',(20.3133043635337,-10.8567788351687,0.168797239405895));
#96875=CARTESIAN_POINT('Ctrl Pts',(20.3144462591772,-10.872740236646,0.132090055974202));
#96876=CARTESIAN_POINT('Ctrl Pts',(20.3187259620078,-10.8834290614676,-0.00816301187489857));
#96877=CARTESIAN_POINT('Ctrl Pts',(20.3193037808912,-10.8848592494362,-0.0272277890842044));
#96878=CARTESIAN_POINT('Ctrl Pts',(1.71371885186958,10.8205931966853,-0.0274987012850931));
#96879=CARTESIAN_POINT('Ctrl Pts',(1.71468534383149,10.822944877955,0.0031147715923076));
#96880=CARTESIAN_POINT('Ctrl Pts',(1.71561699929121,10.8253939137338,0.0326182964624533));
#96881=CARTESIAN_POINT('Ctrl Pts',(1.71645436246431,10.8279623679907,0.0591357896026434));
#96882=CARTESIAN_POINT('Ctrl Pts',(1.71731777406016,10.8306107208919,0.0864781803428588));
#96883=CARTESIAN_POINT('Ctrl Pts',(1.71808091120447,10.83338814387,0.110645999870019));
#96884=CARTESIAN_POINT('Ctrl Pts',(1.71867722902095,10.8363614917576,0.129574074291803));
#96885=CARTESIAN_POINT('Ctrl Pts',(1.7191988450607,10.8389623631505,0.146130995697381));
#96886=CARTESIAN_POINT('Ctrl Pts',(1.71961433221267,10.8418050748521,0.159355934500197));
#96887=CARTESIAN_POINT('Ctrl Pts',(1.71985385804639,10.8449464085218,0.167054167370949));
#96888=CARTESIAN_POINT('Ctrl Pts',(1.71992928349054,10.8459355982203,0.169478301020406));
#96889=CARTESIAN_POINT('Ctrl Pts',(1.71999209380181,10.8470174704317,0.171509656335478));
#96890=CARTESIAN_POINT('Ctrl Pts',(1.72003208873138,10.848191838748,0.172826512697616));
#96891=CARTESIAN_POINT('Ctrl Pts',(1.72004661177751,10.8486182779345,0.17330469245437));
#96892=CARTESIAN_POINT('Ctrl Pts',(1.72006027466401,10.849120139148,0.173759399065278));
#96893=CARTESIAN_POINT('Ctrl Pts',(1.72006907171516,10.8496850261903,0.174063734720378));
#96894=CARTESIAN_POINT('Ctrl Pts',(1.72007465702634,10.8500436770448,0.17425695962123));
#96895=CARTESIAN_POINT('Ctrl Pts',(1.72007826406952,10.8504263471907,0.174388971008971));
#96896=CARTESIAN_POINT('Ctrl Pts',(1.72007897475741,10.850831577322,0.174430726563144));
#96897=CARTESIAN_POINT('Ctrl Pts',(1.72007959945218,10.8511877746751,0.174467429702221));
#96898=CARTESIAN_POINT('Ctrl Pts',(1.72007794588743,10.851538129416,0.17443201029948));
#96899=CARTESIAN_POINT('Ctrl Pts',(1.72007428397974,10.8518822489634,0.174332940383375));
#96900=CARTESIAN_POINT('Ctrl Pts',(1.72006988897607,10.8522952595587,0.174214037155319));
#96901=CARTESIAN_POINT('Ctrl Pts',(1.72006280779778,10.8526797158702,0.174009032859097));
#96902=CARTESIAN_POINT('Ctrl Pts',(1.72005441611114,10.8530306271272,0.173761060114384));
#96903=CARTESIAN_POINT('Ctrl Pts',(1.72003972135017,10.8536451111113,0.173326832721801));
#96904=CARTESIAN_POINT('Ctrl Pts',(1.72002011456704,10.854193422193,0.172734406146005));
#96905=CARTESIAN_POINT('Ctrl Pts',(1.72000063610676,10.85465461806,0.172141778503934));
#96906=CARTESIAN_POINT('Ctrl Pts',(1.71995322459096,10.8557771911396,0.170699294117637));
#96907=CARTESIAN_POINT('Ctrl Pts',(1.71989015281157,10.8567737612288,0.168756077607141));
#96908=CARTESIAN_POINT('Ctrl Pts',(1.71982793196062,10.8576097087584,0.166831443441117));
#96909=CARTESIAN_POINT('Ctrl Pts',(1.71954665823757,10.8613886682289,0.158130999632178));
#96910=CARTESIAN_POINT('Ctrl Pts',(1.71905811143705,10.8649667346043,0.142845235796171));
#96911=CARTESIAN_POINT('Ctrl Pts',(1.71847477844653,10.8681807676781,0.124502662428512));
#96912=CARTESIAN_POINT('Ctrl Pts',(1.71794817753767,10.8710822197908,0.107943997029649));
#96913=CARTESIAN_POINT('Ctrl Pts',(1.71734433393044,10.8736847458312,0.0888946809006036));
#96914=CARTESIAN_POINT('Ctrl Pts',(1.71674529327921,10.875903541945,0.0699625924862081));
#96915=CARTESIAN_POINT('Ctrl Pts',(1.71612325783427,10.8782075088378,0.0503037763168473));
#96916=CARTESIAN_POINT('Ctrl Pts',(1.71550633896194,10.8800975192133,0.0307717296376784));
#96917=CARTESIAN_POINT('Ctrl Pts',(1.71498600196939,10.8815377327113,0.0142938555230019));
#96918=CARTESIAN_POINT('Ctrl Pts',(1.71434319878671,10.8833169139602,-0.0060622407692471));
#96919=CARTESIAN_POINT('Ctrl Pts',(1.71384733713533,10.8844151671384,-0.0217562947441692));
#96920=CARTESIAN_POINT('Ctrl Pts',(1.71367396487917,10.884828376917,-0.0272688936357385));
#96921=CARTESIAN_POINT('Ctrl Pts',(0.236247419988345,10.0098541173715,0.0109034851016902));
#96922=CARTESIAN_POINT('Ctrl Pts',(0.282261170678959,10.0039434919652,1.6562059829034));
#96923=CARTESIAN_POINT('Ctrl Pts',(0.373376072507811,9.24109505723063,4.75816615273069));
#96924=CARTESIAN_POINT('Ctrl Pts',(0.510813799656914,6.01005809224591,8.51828336844459));
#96925=CARTESIAN_POINT('Ctrl Pts',(0.648055013464543,1.44123444891801,10.3120076322213));
#96926=CARTESIAN_POINT('Ctrl Pts',(0.785560276845269,-3.46060058477824,
9.84063572967199));
#96927=CARTESIAN_POINT('Ctrl Pts',(0.923051233060837,-7.5948417795504,7.15384051951451));
#96928=CARTESIAN_POINT('Ctrl Pts',(1.06080804358272,-10.0399709608217,2.87369562638161));
#96929=CARTESIAN_POINT('Ctrl Pts',(1.19834240096617,-10.2462067287989,-2.05861808649073));
#96930=CARTESIAN_POINT('Ctrl Pts',(1.33672216659611,-8.16439259011698,-6.53720175974399));
#96931=CARTESIAN_POINT('Ctrl Pts',(1.47356002226354,-4.25581898226483,-9.56340404211238));
#96932=CARTESIAN_POINT('Ctrl Pts',(1.61411187128628,0.609851298358065,-10.4585827142956));
#96933=CARTESIAN_POINT('Ctrl Pts',(1.74721742089645,5.34703287910853,-9.01859753161106));
#96934=CARTESIAN_POINT('Ctrl Pts',(1.8958818256709,8.89834087463024,-5.56308141247177));
#96935=CARTESIAN_POINT('Ctrl Pts',(2.01273080137881,10.4673283008352,-0.858147598243681));
#96936=CARTESIAN_POINT('Ctrl Pts',(2.20264435693172,9.70177269289523,4.05643050727519));
#96937=CARTESIAN_POINT('Ctrl Pts',(2.3822686105234,6.76787291889619,8.05918655449917));
#96938=CARTESIAN_POINT('Ctrl Pts',(2.58473753279966,1.81936906742815,10.5345311540723));
#96939=CARTESIAN_POINT('Ctrl Pts',(2.80668585042627,-4.37490532884103,9.95478178818736));
#96940=CARTESIAN_POINT('Ctrl Pts',(3.04970976329908,-9.4520606964986,5.41839539962617));
#96941=CARTESIAN_POINT('Ctrl Pts',(3.29292182462279,-10.8347486360525,-1.25311526530803));
#96942=CARTESIAN_POINT('Ctrl Pts',(3.53664883451739,-7.9896728535523,-7.45590618383817));
#96943=CARTESIAN_POINT('Ctrl Pts',(3.78075336580612,-2.00123281219044,-10.7644231829639));
#96944=CARTESIAN_POINT('Ctrl Pts',(3.99813845688202,4.02995046692096,-9.96214692229989));
#96945=CARTESIAN_POINT('Ctrl Pts',(4.18862746148973,8.12371844357838,-6.77022205761317));
#96946=CARTESIAN_POINT('Ctrl Pts',(4.35210354637076,10.199344026804,-2.83597488023603));
#96947=CARTESIAN_POINT('Ctrl Pts',(4.54305768697987,10.5289705057324,2.35743250402144));
#96948=CARTESIAN_POINT('Ctrl Pts',(4.76162944769493,7.77638110638611,7.82086590797216));
#96949=CARTESIAN_POINT('Ctrl Pts',(5.00798370995861,1.61236315088105,10.9305672780317));
#96950=CARTESIAN_POINT('Ctrl Pts',(5.25480916755377,-5.20207512827217,9.7714803690324));
#96951=CARTESIAN_POINT('Ctrl Pts',(5.50210984394784,-10.0080544559059,4.78164235860356));
#96952=CARTESIAN_POINT('Ctrl Pts',(5.74989536055484,-10.9132436390617,-2.09865134769182));
#96953=CARTESIAN_POINT('Ctrl Pts',(5.99817059546363,-7.54875564608264,-8.18768977461551));
#96954=CARTESIAN_POINT('Ctrl Pts',(6.20547988627588,-2.27065875717826,-10.6033776168208));
#96955=CARTESIAN_POINT('Ctrl Pts',(6.37157872831103,2.2034281101606,-10.38310575704));
#96956=CARTESIAN_POINT('Ctrl Pts',(6.5378458851255,6.39609170629518,-8.79205815441647));
#96957=CARTESIAN_POINT('Ctrl Pts',(6.74599686093403,10.2823120730407,-4.45053869669907));
#96958=CARTESIAN_POINT('Ctrl Pts',(6.99629129235853,10.940060962212,2.53477782652384));
#96959=CARTESIAN_POINT('Ctrl Pts',(7.24710420019219,7.31061279457704,8.54766467124672));
#96960=CARTESIAN_POINT('Ctrl Pts',(7.49843906124326,0.807422651314364,11.2437313176264));
#96961=CARTESIAN_POINT('Ctrl Pts',(7.75030187340421,-6.03794504664792,9.54528916818388));
#96962=CARTESIAN_POINT('Ctrl Pts',(8.00269551261862,-10.5549932902737,4.10604724051843));
#96963=CARTESIAN_POINT('Ctrl Pts',(8.21346992637613,-10.8796133252787,-1.78960216096524));
#96964=CARTESIAN_POINT('Ctrl Pts',(8.38235875812152,-9.00997128676483,-5.94254396635746));
#96965=CARTESIAN_POINT('Ctrl Pts',(8.55142780992127,-5.94780734069486,-9.31990615096143));
#96966=CARTESIAN_POINT('Ctrl Pts',(8.76310273990339,-0.391070994991625,
-11.3900354500284));
#96967=CARTESIAN_POINT('Ctrl Pts',(8.98937409723999,5.69639989756584,-9.62925783989565));
#96968=CARTESIAN_POINT('Ctrl Pts',(9.18771619472723,9.41506511084373,-5.71114232305533));
#96969=CARTESIAN_POINT('Ctrl Pts',(9.35796785690745,10.9487245660541,-1.3352779507663));
#96970=CARTESIAN_POINT('Ctrl Pts',(9.50952001769988,10.5851488734647,2.77388645518095));
#96971=CARTESIAN_POINT('Ctrl Pts',(9.6802207005967,8.6323656393866,6.93167007488376));
#96972=CARTESIAN_POINT('Ctrl Pts',(9.8511669282714,5.03341926711359,10.005370594796));
#96973=CARTESIAN_POINT('Ctrl Pts',(10.0414263863103,-0.0370302011065132,
11.0900539763085));
#96974=CARTESIAN_POINT('Ctrl Pts',(10.2129064709966,-4.60117272512858,10.1123079833804));
#96975=CARTESIAN_POINT('Ctrl Pts',(10.3846334810773,-8.36249887462001,7.333757088142));
#96976=CARTESIAN_POINT('Ctrl Pts',(10.5852700849522,-11.0438636264105,2.5710018780358));
#96977=CARTESIAN_POINT('Ctrl Pts',(10.8149812572377,-10.9327543857081,-3.85881574900101));
#96978=CARTESIAN_POINT('Ctrl Pts',(11.0739634856436,-6.51596063212015,-9.61787231659027));
#96979=CARTESIAN_POINT('Ctrl Pts',(11.3335027624831,0.467553896182886,-11.6326133959484));
#96980=CARTESIAN_POINT('Ctrl Pts',(11.5935990303907,7.30006443089141,-9.10202411414065));
#96981=CARTESIAN_POINT('Ctrl Pts',(11.8542514832384,11.3018959077801,-2.99469731082429));
#96982=CARTESIAN_POINT('Ctrl Pts',(12.1154595427833,10.8959931621228,4.30909650104135));
#96983=CARTESIAN_POINT('Ctrl Pts',(12.3772218554197,6.21966653448416,9.9610404039248));
#96984=CARTESIAN_POINT('Ctrl Pts',(12.6103907594023,-0.116341202195039,
11.5293645744839));
#96985=CARTESIAN_POINT('Ctrl Pts',(12.8147708022338,-5.45592049951901,9.9487140666827));
#96986=CARTESIAN_POINT('Ctrl Pts',(12.9901979397853,-9.07795159496635,6.83698031594479));
#96987=CARTESIAN_POINT('Ctrl Pts',(13.1658687037173,-11.1011708103344,2.50074889324405));
#96988=CARTESIAN_POINT('Ctrl Pts',(13.3417822439288,-11.1644930733986,-2.28894820766289));
#96989=CARTESIAN_POINT('Ctrl Pts',(13.5179379354906,-9.24673925825825,-6.68611271245235));
#96990=CARTESIAN_POINT('Ctrl Pts',(13.6796349152431,-5.98273132472607,-9.64237799750398));
#96991=CARTESIAN_POINT('Ctrl Pts',(13.8268076250129,-2.27546195949532,-11.054929025411));
#96992=CARTESIAN_POINT('Ctrl Pts',(14.0035943286413,2.48773327673549,-11.2885440550832));
#96993=CARTESIAN_POINT('Ctrl Pts',(14.2249137140213,8.12400984323024,-8.72005906989793));
#96994=CARTESIAN_POINT('Ctrl Pts',(14.491030376488,11.7338624047256,-2.18962997847152));
#96995=CARTESIAN_POINT('Ctrl Pts',(14.7576764173397,10.7646370052319,5.21155646912779));
#96996=CARTESIAN_POINT('Ctrl Pts',(15.0248485147023,5.57521599023327,10.6101885382146));
#96997=CARTESIAN_POINT('Ctrl Pts',(15.2627969903976,-0.992496529899604,
11.7232808389446));
#96998=CARTESIAN_POINT('Ctrl Pts',(15.4713367560048,-6.30461690989114,9.70932698413165));
#96999=CARTESIAN_POINT('Ctrl Pts',(15.6503127453385,-9.75400287905629,6.26911361970484));
#97000=CARTESIAN_POINT('Ctrl Pts',(15.8295149691491,-11.4822959817887,1.70334083365234));
#97001=CARTESIAN_POINT('Ctrl Pts',(16.0089418448568,-11.181216258242,-3.17259926566968));
#97002=CARTESIAN_POINT('Ctrl Pts',(16.188591039425,-8.89748663297175,-7.50014918261716));
#97003=CARTESIAN_POINT('Ctrl Pts',(16.3684625089748,-5.03250485728561,-10.5077706500309));
#97004=CARTESIAN_POINT('Ctrl Pts',(16.5485511407028,-0.265185102376701,
-11.6644002694677));
#97005=CARTESIAN_POINT('Ctrl Pts',(16.7288620799578,4.55737364209454,-10.7511864391277));
#97006=CARTESIAN_POINT('Ctrl Pts',(16.9394631424965,9.2650231182667,-7.47067789966794));
#97007=CARTESIAN_POINT('Ctrl Pts',(17.1805382346314,12.0898447529122,-1.34171254597968));
#97008=CARTESIAN_POINT('Ctrl Pts',(17.4521367413488,10.5409864853984,6.10996614926754));
#97009=CARTESIAN_POINT('Ctrl Pts',(17.724365137213,4.86145703151405,11.1967036665295));
#97010=CARTESIAN_POINT('Ctrl Pts',(17.9739918587982,-2.10415293108078,11.8489255250914));
#97011=CARTESIAN_POINT('Ctrl Pts',(18.202015234118,-7.68156807420211,9.06610251823513));
#97012=CARTESIAN_POINT('Ctrl Pts',(18.4054199419476,-10.9997362923052,4.53187719411499));
#97013=CARTESIAN_POINT('Ctrl Pts',(18.6198245873421,-11.8684771618245,-1.01371487948541));
#97014=CARTESIAN_POINT('Ctrl Pts',(18.7524864795234,-10.0876335066935,-6.35323592041183));
#97015=CARTESIAN_POINT('Ctrl Pts',(18.9215214647306,-6.05127039623785,-10.2851587824557));
#97016=CARTESIAN_POINT('Ctrl Pts',(19.0731272889727,-0.65573725462633,-11.9250004543447));
#97017=CARTESIAN_POINT('Ctrl Pts',(19.2334715077428,4.89535067915303,-10.9054852425954));
#97018=CARTESIAN_POINT('Ctrl Pts',(19.3898602964296,9.36302270195755,-7.44777342140719));
#97019=CARTESIAN_POINT('Ctrl Pts',(19.5482566143342,11.746908296497,-2.3215667695402));
#97020=CARTESIAN_POINT('Ctrl Pts',(19.7059549578916,11.5117047090732,3.33316592178669));
#97021=CARTESIAN_POINT('Ctrl Pts',(19.8641448857339,8.70443639357988,8.25003611575385));
#97022=CARTESIAN_POINT('Ctrl Pts',(20.0223213623772,3.95007659628246,11.3388902742205));
#97023=CARTESIAN_POINT('Ctrl Pts',(20.1806504341427,-1.69684253053496,11.8871678578889));
#97024=CARTESIAN_POINT('Ctrl Pts',(20.3391911994786,-6.96836333841185,9.80977543797914));
#97025=CARTESIAN_POINT('Ctrl Pts',(20.4976257595637,-10.7023126456679,5.48047659314321));
#97026=CARTESIAN_POINT('Ctrl Pts',(20.6037145486049,-11.585908889594,1.86712555758727));
#97027=CARTESIAN_POINT('Ctrl Pts',(20.6563591733144,-11.5926712737699,-0.0152754849923013));
#97028=CARTESIAN_POINT('Ctrl Pts',(0.414857473372219,9.90423208112614,0.00552890457929189));
#97029=CARTESIAN_POINT('Ctrl Pts',(0.460418169951906,9.89837965208721,1.63463165667105));
#97030=CARTESIAN_POINT('Ctrl Pts',(0.550524238756086,9.14347953248729,4.70199787951103));
#97031=CARTESIAN_POINT('Ctrl Pts',(0.686487743555868,5.94756858734584,8.42194829459827));
#97032=CARTESIAN_POINT('Ctrl Pts',(0.822188845948616,1.4295973741879,10.1949329202965));
#97033=CARTESIAN_POINT('Ctrl Pts',(0.958137305849702,-3.41644857527999,
9.72909274177817));
#97034=CARTESIAN_POINT('Ctrl Pts',(1.09403361926965,-7.50266239378958,7.07318924692806));
#97035=CARTESIAN_POINT('Ctrl Pts',(1.23016410051787,-9.91874295184523,2.84369449537073));
#97036=CARTESIAN_POINT('Ctrl Pts',(1.36604419717911,-10.1223645889116,-2.02923787138832));
#97037=CARTESIAN_POINT('Ctrl Pts',(1.50272853890757,-8.06598625809779,-6.45277962201427));
#97038=CARTESIAN_POINT('Ctrl Pts',(1.63786199458176,-4.2061118422785,-9.44114405015345));
#97039=CARTESIAN_POINT('Ctrl Pts',(1.77663105190054,0.597760567220721,-10.3247533804463));
#97040=CARTESIAN_POINT('Ctrl Pts',(1.90802235015697,5.27380437963824,-8.90337943938992));
#97041=CARTESIAN_POINT('Ctrl Pts',(2.05474079138054,8.77838187416392,-5.49286562090779));
#97042=CARTESIAN_POINT('Ctrl Pts',(2.17004101494486,10.3264823775258,-0.850681306693522));
#97043=CARTESIAN_POINT('Ctrl Pts',(2.35731632897177,9.57112254251312,3.99528315347118));
#97044=CARTESIAN_POINT('Ctrl Pts',(2.53450866734066,6.67744212272248,7.94394089643617));
#97045=CARTESIAN_POINT('Ctrl Pts',(2.73411483620783,1.79849490485795,10.3837363556879));
#97046=CARTESIAN_POINT('Ctrl Pts',(2.95290126451474,-4.30712195173813,9.81235656214055));
#97047=CARTESIAN_POINT('Ctrl Pts',(3.19236937666179,-9.30963369487423,5.34191601965425));
#97048=CARTESIAN_POINT('Ctrl Pts',(3.43194408501429,-10.6713573734611,-1.22966566693323));
#97049=CARTESIAN_POINT('Ctrl Pts',(3.67195964496792,-7.86933007701237,-7.33773481169104));
#97050=CARTESIAN_POINT('Ctrl Pts',(3.91227453885146,-1.97387050712104,-10.5945289197493));
#97051=CARTESIAN_POINT('Ctrl Pts',(4.12623048182538,3.96194440519949,-9.80466577550004));
#97052=CARTESIAN_POINT('Ctrl Pts',(4.31366124218865,7.98986025797959,-6.66394873887548));
#97053=CARTESIAN_POINT('Ctrl Pts',(4.47448428722267,10.0317165049964,-2.79356697241387));
#97054=CARTESIAN_POINT('Ctrl Pts',(4.66230978502311,10.3558279725464,2.31468255910313));
#97055=CARTESIAN_POINT('Ctrl Pts',(4.87726295846424,7.64870922201446,7.68740832032523));
#97056=CARTESIAN_POINT('Ctrl Pts',(5.11947477571608,1.58835118409914,10.7445226945064));
#97057=CARTESIAN_POINT('Ctrl Pts',(5.36209607434172,-5.1097851329423,9.60498844990581));
#97058=CARTESIAN_POINT('Ctrl Pts',(5.60512955006172,-9.8325723537292,4.70119518673858));
#97059=CARTESIAN_POINT('Ctrl Pts',(5.84859118648436,-10.721707014825,-2.05887588402894));
#97060=CARTESIAN_POINT('Ctrl Pts',(6.09248402304501,-7.41650091760526,-8.04022127100391));
#97061=CARTESIAN_POINT('Ctrl Pts',(6.29610216773837,-2.23247694919502,-10.412668314822));
#97062=CARTESIAN_POINT('Ctrl Pts',(6.45921389034127,2.1610887235209,-10.1963335049597));
#97063=CARTESIAN_POINT('Ctrl Pts',(6.62247800296255,6.27795117697407,-8.63400813873752));
#97064=CARTESIAN_POINT('Ctrl Pts',(6.82685309104326,10.0935096431048,-4.37126941277162));
#97065=CARTESIAN_POINT('Ctrl Pts',(7.07257095820066,10.7389892523422,2.48613635755055));
#97066=CARTESIAN_POINT('Ctrl Pts',(7.31875400381713,7.17651830463057,8.38788425967839));
#97067=CARTESIAN_POINT('Ctrl Pts',(7.56542542195868,0.7940738232045,11.0337241535568));
#97068=CARTESIAN_POINT('Ctrl Pts',(7.81258883522782,-5.92334267223987,9.36691902027508));
#97069=CARTESIAN_POINT('Ctrl Pts',(8.06023568790507,-10.355305921526,4.02992322014796));
#97070=CARTESIAN_POINT('Ctrl Pts',(8.26704359020869,-10.6737649965103,-1.7545294942458));
#97071=CARTESIAN_POINT('Ctrl Pts',(8.43273095233146,-8.83955444072362,-5.82870686778807));
#97072=CARTESIAN_POINT('Ctrl Pts',(8.59859108870107,-5.83554619435488,-9.1418987825165));
#97073=CARTESIAN_POINT('Ctrl Pts',(8.80624576829024,-0.38447258030216,-11.1726177352634));
#97074=CARTESIAN_POINT('Ctrl Pts',(9.02820909153645,5.58689185174015,-9.44533260690079));
#97075=CARTESIAN_POINT('Ctrl Pts',(9.22275895514135,9.23437826127017,-5.60217944378132));
#97076=CARTESIAN_POINT('Ctrl Pts',(9.38974987490141,10.738646239023,-1.31016596208437));
#97077=CARTESIAN_POINT('Ctrl Pts',(9.53840307001713,10.382012686018,2.72029969805813));
#97078=CARTESIAN_POINT('Ctrl Pts',(9.70583136768617,8.46668714972023,6.79831087477145));
#97079=CARTESIAN_POINT('Ctrl Pts',(9.87349729187605,4.93684808690671,9.81299815163281));
#97080=CARTESIAN_POINT('Ctrl Pts',(10.0601111882738,-0.0363289028640763,
10.8768934600605));
#97081=CARTESIAN_POINT('Ctrl Pts',(10.2282978646472,-4.51277420606732,9.91792503778587));
#97082=CARTESIAN_POINT('Ctrl Pts',(10.3967352451322,-8.20197618078149,7.19270305477791));
#97083=CARTESIAN_POINT('Ctrl Pts',(10.5935240094408,-10.831887292633,2.52135107060561));
#97084=CARTESIAN_POINT('Ctrl Pts',(10.8188415967134,-10.722977073751,-3.78530740392195));
#97085=CARTESIAN_POINT('Ctrl Pts',(11.072873928545,-6.39071183862135,-9.43422014294441));
#97086=CARTESIAN_POINT('Ctrl Pts',(11.3274651584233,0.459488233287932,-11.4105773080049));
#97087=CARTESIAN_POINT('Ctrl Pts',(11.5826156827513,7.16198049444802,-8.92822222363093));
#97088=CARTESIAN_POINT('Ctrl Pts',(11.8383292692865,11.0879837567681,-2.93677974621958));
#97089=CARTESIAN_POINT('Ctrl Pts',(12.0946076320618,10.6898359444383,4.22903042659061));
#97090=CARTESIAN_POINT('Ctrl Pts',(12.3514514772082,6.10154484510121,9.77475286626462));
#97091=CARTESIAN_POINT('Ctrl Pts',(12.5802650565851,-0.115947755772311,
11.3138309860641));
#97092=CARTESIAN_POINT('Ctrl Pts',(12.7808402128593,-5.35607564736957,9.76266262815981));
#97093=CARTESIAN_POINT('Ctrl Pts',(12.9530170339153,-8.91094778509916,6.7086566819509));
#97094=CARTESIAN_POINT('Ctrl Pts',(13.12544599583,-10.8968596648658,2.45251970711059));
#97095=CARTESIAN_POINT('Ctrl Pts',(13.2981269698541,-10.9590328324087,-2.24910381637141));
#97096=CARTESIAN_POINT('Ctrl Pts',(13.4710607907509,-9.07644430667711,-6.56582822441653));
#97097=CARTESIAN_POINT('Ctrl Pts',(13.629817907228,-5.8718461928328,-9.46833191108338));
#97098=CARTESIAN_POINT('Ctrl Pts',(13.7743254679023,-2.23176961892461,-10.8553170599986));
#97099=CARTESIAN_POINT('Ctrl Pts',(13.947922654666,2.44544351510108,-11.0847627749313));
#97100=CARTESIAN_POINT('Ctrl Pts',(14.1652771291645,7.9807212902622,-8.56247132454596));
#97101=CARTESIAN_POINT('Ctrl Pts',(14.426673351802,11.5266952104283,-2.14812344542611));
#97102=CARTESIAN_POINT('Ctrl Pts',(14.6886334109526,10.5747101394929,5.12290089122906));
#97103=CARTESIAN_POINT('Ctrl Pts',(14.9511576251903,5.47582248770765,10.4277192621086));
#97104=CARTESIAN_POINT('Ctrl Pts',(15.1850168097518,-0.978866148033905,
11.5218445338106));
#97105=CARTESIAN_POINT('Ctrl Pts',(15.3899998038495,-6.20039383677261,9.54233873489365));
#97106=CARTESIAN_POINT('Ctrl Pts',(15.5659485697773,-9.5914515069554,6.16037833139429));
#97107=CARTESIAN_POINT('Ctrl Pts',(15.7421485688689,-11.290841170853,1.67118798331995));
#97108=CARTESIAN_POINT('Ctrl Pts',(15.91859349859,-10.9948392663885,-3.12368117664651));
#97109=CARTESIAN_POINT('Ctrl Pts',(16.0952847407158,-8.7488133900966,-7.37996072217231));
#97110=CARTESIAN_POINT('Ctrl Pts',(16.2722211526758,-4.94699126663771,-10.3385555770745));
#97111=CARTESIAN_POINT('Ctrl Pts',(16.4493977178716,-0.256815859048274,
-11.4765472264812));
#97112=CARTESIAN_POINT('Ctrl Pts',(16.6268217932286,4.48852118140762,-10.5780577674155));
#97113=CARTESIAN_POINT('Ctrl Pts',(16.8340855571211,9.12157653404527,-7.34965948087608));
#97114=CARTESIAN_POINT('Ctrl Pts',(17.0713925325136,11.9024947483016,-1.31664378789847));
#97115=CARTESIAN_POINT('Ctrl Pts',(17.3388171639219,10.3777655633468,6.02036145965717));
#97116=CARTESIAN_POINT('Ctrl Pts',(17.6069246364637,4.78440903108591,11.0305903935865));
#97117=CARTESIAN_POINT('Ctrl Pts',(17.8528590762609,-2.07781594109665,11.6730984248505));
#97118=CARTESIAN_POINT('Ctrl Pts',(18.0775302086984,-7.57370613884857,8.9316707861517));
#97119=CARTESIAN_POINT('Ctrl Pts',(18.2780483340467,-10.8443366541153,4.46167669141483));
#97120=CARTESIAN_POINT('Ctrl Pts',(18.4893454671788,-11.7009227432788,-1.00327493205492));
#97121=CARTESIAN_POINT('Ctrl Pts',(18.620155096919,-9.94500696839018,-6.26795196146921));
#97122=CARTESIAN_POINT('Ctrl Pts',(18.7868531643319,-5.96462321927576,-10.1457961598287));
#97123=CARTESIAN_POINT('Ctrl Pts',(18.9363899977649,-0.642776950505896,
-11.7632196848552));
#97124=CARTESIAN_POINT('Ctrl Pts',(19.0945718779567,4.83344916781054,-10.7576469690656));
#97125=CARTESIAN_POINT('Ctrl Pts',(19.2488814384357,9.24176762102788,-7.34599960699894));
#97126=CARTESIAN_POINT('Ctrl Pts',(19.4051985522719,11.5944628332931,-2.28718014002714));
#97127=CARTESIAN_POINT('Ctrl Pts',(19.560856029607,11.3624302638596,3.29440256703827));
#97128=CARTESIAN_POINT('Ctrl Pts',(19.7170279013492,8.59111746859576,8.14848688572577));
#97129=CARTESIAN_POINT('Ctrl Pts',(19.8732130134576,3.8966145319634,11.1987915952599));
#97130=CARTESIAN_POINT('Ctrl Pts',(20.0295862073395,-1.68030661482981,11.7400692616394));
#97131=CARTESIAN_POINT('Ctrl Pts',(20.1861778729395,-6.8875480967494,9.68884223286411));
#97132=CARTESIAN_POINT('Ctrl Pts',(20.3427366995498,-10.5767665435211,5.41053330586961));
#97133=CARTESIAN_POINT('Ctrl Pts',(20.447527115044,-11.450015111617,1.84158505298324));
#97134=CARTESIAN_POINT('Ctrl Pts',(20.4995937278547,-11.4567032481648,-0.0201481587004812));
#97135=CARTESIAN_POINT('Ctrl Pts',(0.840394518298377,9.8112024191675,-0.00670618228483209));
#97136=CARTESIAN_POINT('Ctrl Pts',(0.885552519579505,9.80540171773232,1.60799749190895));
#97137=CARTESIAN_POINT('Ctrl Pts',(0.974750578127202,9.0576922562742,4.64438287980197));
#97138=CARTESIAN_POINT('Ctrl Pts',(1.10934238128961,5.89424784709291,8.3269760036482));
#97139=CARTESIAN_POINT('Ctrl Pts',(1.24355928276938,1.42507842855297,10.0798499360501));
#97140=CARTESIAN_POINT('Ctrl Pts',(1.37796108194799,-3.36571918358726,9.61929687754925));
#97141=CARTESIAN_POINT('Ctrl Pts',(1.51222657698763,-7.40286551116007,6.99470771718013));
#97142=CARTESIAN_POINT('Ctrl Pts',(1.64664791909928,-9.78837229914064,2.81815601860371));
#97143=CARTESIAN_POINT('Ctrl Pts',(1.78074561536888,-9.98898798636914,-1.99102191145044));
#97144=CARTESIAN_POINT('Ctrl Pts',(1.91555781226548,-7.96044407001117,-6.35391906224498));
#97145=CARTESIAN_POINT('Ctrl Pts',(2.04876863167595,-4.15521006841318,-9.29963433652184));
#97146=CARTESIAN_POINT('Ctrl Pts',(2.18548090920051,0.577631937284577,-10.169672800332));
#97147=CARTESIAN_POINT('Ctrl Pts',(2.31485557822428,5.18201744899307,-8.77015906126499));
#97148=CARTESIAN_POINT('Ctrl Pts',(2.45924280692048,8.63054056692016,-5.41297393495632));
#97149=CARTESIAN_POINT('Ctrl Pts',(2.57265305016202,10.15324509706,-0.847239260661916));
#97150=CARTESIAN_POINT('Ctrl Pts',(2.75655298519099,9.4102732574346,3.91072658414708));
#97151=CARTESIAN_POINT('Ctrl Pts',(2.93071565980367,6.56718797325696,7.7923694311073));
#97152=CARTESIAN_POINT('Ctrl Pts',(3.12658638027203,1.77805349278155,10.1852620677513));
#97153=CARTESIAN_POINT('Ctrl Pts',(3.34119969408586,-4.21044791581097,9.62486450025235));
#97154=CARTESIAN_POINT('Ctrl Pts',(3.5758276553806,-9.11166252069733,5.24318208444361));
#97155=CARTESIAN_POINT('Ctrl Pts',(3.81038380928619,-10.4439097069757,-1.19065991693002));
#97156=CARTESIAN_POINT('Ctrl Pts',(4.0451423272918,-7.70232284178181,-7.16496362076518));
#97157=CARTESIAN_POINT('Ctrl Pts',(4.27999813823747,-1.94023943533083,-10.3469623541626));
#97158=CARTESIAN_POINT('Ctrl Pts',(4.48890492429656,3.8556110503865,-9.57499253837833));
#97159=CARTESIAN_POINT('Ctrl Pts',(4.67179748834899,7.78584865357542,-6.51004394062785));
#97160=CARTESIAN_POINT('Ctrl Pts',(4.82863972732285,9.77698041904427,-2.73530434634081));
#97161=CARTESIAN_POINT('Ctrl Pts',(5.0117133577872,10.09260835835,2.24386005062187));
#97162=CARTESIAN_POINT('Ctrl Pts',(5.22107968543367,7.45508083801071,7.4768077396953));
#97163=CARTESIAN_POINT('Ctrl Pts',(5.45681647748818,1.55619885325388,10.4515425114258));
#97164=CARTESIAN_POINT('Ctrl Pts',(5.69276964571786,-4.95793332420886,9.34248767908207));
#97165=CARTESIAN_POINT('Ctrl Pts',(5.92894764174431,-9.54706610725953,4.57634563628634));
#97166=CARTESIAN_POINT('Ctrl Pts',(6.16536813622835,-10.4097935511739,-1.98854928432125));
#97167=CARTESIAN_POINT('Ctrl Pts',(6.4020422586417,-7.20166324917165,-7.79263732418621));
#97168=CARTESIAN_POINT('Ctrl Pts',(6.59949026276999,-2.17429698465326,-10.092758157656));
#97169=CARTESIAN_POINT('Ctrl Pts',(6.75759161856712,2.08433598343559,-9.88295467395817));
#97170=CARTESIAN_POINT('Ctrl Pts',(6.9157878368503,6.07347841979099,-8.36898824279205));
#97171=CARTESIAN_POINT('Ctrl Pts',(7.1137119010795,9.76828400366959,-4.24027621390453));
#97172=CARTESIAN_POINT('Ctrl Pts',(7.35152456967961,10.3924428604999,2.39684477307773));
#97173=CARTESIAN_POINT('Ctrl Pts',(7.58965789216565,6.94580978226224,8.10535272771152));
#97174=CARTESIAN_POINT('Ctrl Pts',(7.82811381443578,0.775522719167843,10.662626855712));
#97175=CARTESIAN_POINT('Ctrl Pts',(8.06691045556968,-5.71462403419679,9.05160752136358));
#97176=CARTESIAN_POINT('Ctrl Pts',(8.30606116330518,-9.99419182866903,3.89729828508907));
#97177=CARTESIAN_POINT('Ctrl Pts',(8.50564975817593,-10.301053359501,-1.68557337935384));
#97178=CARTESIAN_POINT('Ctrl Pts',(8.66551277345512,-8.53125361604988,-5.6165326975031));
#97179=CARTESIAN_POINT('Ctrl Pts',(8.82550163905307,-5.63343798709349,-8.81248942392093));
#97180=CARTESIAN_POINT('Ctrl Pts',(9.02572387901138,-0.377112405932923,
-10.7702099814649));
#97181=CARTESIAN_POINT('Ctrl Pts',(9.23964628508325,5.37806574910098,-9.10510040701057));
#97182=CARTESIAN_POINT('Ctrl Pts',(9.42709466339725,8.89239633905225,-5.40205281095219));
#97183=CARTESIAN_POINT('Ctrl Pts',(9.58794944648292,10.3412852051172,-1.26764760710221));
#97184=CARTESIAN_POINT('Ctrl Pts',(9.73109312372931,9.99778113623362,2.61357300057332));
#97185=CARTESIAN_POINT('Ctrl Pts',(9.89229087385157,8.15364281688216,6.53990392141035));
#97186=CARTESIAN_POINT('Ctrl Pts',(10.0536805462786,4.75573838903045,9.44164371222992));
#97187=CARTESIAN_POINT('Ctrl Pts',(10.2332520784286,-0.0299529409807728,
10.4652778834182));
#97188=CARTESIAN_POINT('Ctrl Pts',(10.3950687359733,-4.33689811382311,9.54254148160714));
#97189=CARTESIAN_POINT('Ctrl Pts',(10.5570818172104,-7.88545311500811,6.92103924802403));
#97190=CARTESIAN_POINT('Ctrl Pts',(10.7463390558374,-10.414668932124,2.42833144703078));
#97191=CARTESIAN_POINT('Ctrl Pts',(10.9629699253934,-10.3096478902391,-3.63548669311155));
#97192=CARTESIAN_POINT('Ctrl Pts',(11.207157532618,-6.14495684043231,-9.06547916791598));
#97193=CARTESIAN_POINT('Ctrl Pts',(11.4518252038093,0.438548929035689,-10.9646249539477));
#97194=CARTESIAN_POINT('Ctrl Pts',(11.6969823136692,6.87865568211547,-8.57922988332477));
#97195=CARTESIAN_POINT('Ctrl Pts',(11.9426382962662,10.6502059987716,-2.82316358352909));
#97196=CARTESIAN_POINT('Ctrl Pts',(12.1887977605246,10.2676274637117,4.05994586492189));
#97197=CARTESIAN_POINT('Ctrl Pts',(12.4354709555491,5.86080066266984,9.38613385806551));
#97198=CARTESIAN_POINT('Ctrl Pts',(12.6551953046859,-0.109975039867466,
10.8640910801617));
#97199=CARTESIAN_POINT('Ctrl Pts',(12.8477989586744,-5.14194189665667,9.37452435506929));
#97200=CARTESIAN_POINT('Ctrl Pts',(13.0131218263297,-8.55543065539852,6.44200174199404));
#97201=CARTESIAN_POINT('Ctrl Pts',(13.1786832680645,-10.4622549707042,2.35527172510316));
#97202=CARTESIAN_POINT('Ctrl Pts',(13.3444852793881,-10.5220007104345,-2.15915681205131));
#97203=CARTESIAN_POINT('Ctrl Pts',(13.5105288776343,-8.71433212967542,-6.30395785253688));
#97204=CARTESIAN_POINT('Ctrl Pts',(13.662956387324,-5.63744684102453,-9.09082112151706));
#97205=CARTESIAN_POINT('Ctrl Pts',(13.8017063001416,-2.14229738687632,-10.4225698278804));
#97206=CARTESIAN_POINT('Ctrl Pts',(13.9683923393898,2.34877791247678,-10.6428567220425));
#97207=CARTESIAN_POINT('Ctrl Pts',(14.1770945402735,7.66388977684096,-8.22094702734011));
#97208=CARTESIAN_POINT('Ctrl Pts',(14.4280953126858,11.068982097841,-2.06146913677415));
#97209=CARTESIAN_POINT('Ctrl Pts',(14.679663690643,10.1548744665846,4.92137235826369));
#97210=CARTESIAN_POINT('Ctrl Pts',(14.9318023145324,5.25763196840611,10.0165288092755));
#97211=CARTESIAN_POINT('Ctrl Pts',(15.1564310783341,-0.942520850929141,
11.0677083375238));
#97212=CARTESIAN_POINT('Ctrl Pts',(15.3533633298778,-5.95905978015328,9.16595882332264));
#97213=CARTESIAN_POINT('Ctrl Pts',(15.5224192741083,-9.21737896803036,5.91650325731429));
#97214=CARTESIAN_POINT('Ctrl Pts',(15.6917292680821,-10.850427368977,1.6027367108997));
#97215=CARTESIAN_POINT('Ctrl Pts',(15.8613012109163,-10.5660287731456,-3.00545159510626));
#97216=CARTESIAN_POINT('Ctrl Pts',(16.0311313871158,-8.40721701333872,-7.09661446390494));
#97217=CARTESIAN_POINT('Ctrl Pts',(16.2012245630604,-4.75238379045116,-9.94086992193184));
#97218=CARTESIAN_POINT('Ctrl Pts',(16.3715791736397,-0.242748863921299,
-11.0351697210793));
#97219=CARTESIAN_POINT('Ctrl Pts',(16.5421999866943,4.32073643703397,-10.1711459420049));
#97220=CARTESIAN_POINT('Ctrl Pts',(16.7415533331513,8.77708241140647,-7.06604653174035));
#97221=CARTESIAN_POINT('Ctrl Pts',(16.9698445054398,11.4526883383421,-1.2620410011127));
#97222=CARTESIAN_POINT('Ctrl Pts',(17.2272005571437,9.98569686135026,5.79875321887713));
#97223=CARTESIAN_POINT('Ctrl Pts',(17.4852834652622,4.60144346399131,10.6224289494326));
#97224=CARTESIAN_POINT('Ctrl Pts',(17.7221264018559,-2.00689161588762,11.2411048053495));
#97225=CARTESIAN_POINT('Ctrl Pts',(17.9385221855771,-7.30110778520626,8.60120368104034));
#97226=CARTESIAN_POINT('Ctrl Pts',(18.1317864645908,-10.4529103768998,4.29265039185786));
#97227=CARTESIAN_POINT('Ctrl Pts',(18.3353557032759,-11.2787530887185,-0.972196076855361));
#97228=CARTESIAN_POINT('Ctrl Pts',(18.461467953364,-9.58587761179443,-6.04767973256785));
#97229=CARTESIAN_POINT('Ctrl Pts',(18.6222145537073,-5.74771983808596,-9.7875564324453));
#97230=CARTESIAN_POINT('Ctrl Pts',(18.7664485808866,-0.614496977722204,
-11.3476121811775));
#97231=CARTESIAN_POINT('Ctrl Pts',(18.919057129735,4.6689269100397,-10.37770030444));
#97232=CARTESIAN_POINT('Ctrl Pts',(19.0679708368727,8.92327404926781,-7.0853647814176));
#97233=CARTESIAN_POINT('Ctrl Pts',(19.2188596216407,11.1944683039804,-2.20224801907994));
#97234=CARTESIAN_POINT('Ctrl Pts',(19.3691524522802,10.9705879762662,3.18723371060556));
#97235=CARTESIAN_POINT('Ctrl Pts',(19.5199850143116,8.29418732152164,7.87525299435256));
#97236=CARTESIAN_POINT('Ctrl Pts',(19.6708643849559,3.75892317031939,10.8228124930193));
#97237=CARTESIAN_POINT('Ctrl Pts',(19.8219912701959,-1.63037658945895,11.3451400693921));
#97238=CARTESIAN_POINT('Ctrl Pts',(19.9733148456315,-6.66397468925673,9.36442000366302));
#97239=CARTESIAN_POINT('Ctrl Pts',(20.1247714457631,-10.2313788447333,5.22459154891526));
#97240=CARTESIAN_POINT('Ctrl Pts',(20.2259938430529,-11.0759875132312,1.77747672674462));
#97241=CARTESIAN_POINT('Ctrl Pts',(20.2764796593326,-11.0824725909955,-0.0277323278312897));
#97242=CARTESIAN_POINT('Ctrl Pts',(1.5069621239122,10.1062642497049,-0.0242879192054315));
#97243=CARTESIAN_POINT('Ctrl Pts',(1.55334346900726,10.1003064055261,1.63415856235628));
#97244=CARTESIAN_POINT('Ctrl Pts',(1.64530857322812,9.3301337990831,4.76502605162024));
#97245=CARTESIAN_POINT('Ctrl Pts',(1.78368715348376,6.07563011846298,8.5500818783867));
#97246=CARTESIAN_POINT('Ctrl Pts',(1.92166086015211,1.48240340871853,10.3526479088268));
#97247=CARTESIAN_POINT('Ctrl Pts',(2.05964680268286,-3.43668383608774,9.87845827712341));
#97248=CARTESIAN_POINT('Ctrl Pts',(2.19738578920598,-7.57775083240144,7.18602209416567));
#97249=CARTESIAN_POINT('Ctrl Pts',(2.33514751881056,-10.0221669614262,2.90512444626086));
#97250=CARTESIAN_POINT('Ctrl Pts',(2.47245339717927,-10.2269687721166,-2.01903352888235));
#97251=CARTESIAN_POINT('Ctrl Pts',(2.61035542825578,-8.15142492455985,-6.48177840056761));
#97252=CARTESIAN_POINT('Ctrl Pts',(2.74649771620373,-4.26209165119445,-9.49194667508545));
#97253=CARTESIAN_POINT('Ctrl Pts',(2.8860755063246,0.570107557856309,-10.379365507633));
#97254=CARTESIAN_POINT('Ctrl Pts',(3.01804263479664,5.26675673347687,-8.95193129729442));
#97255=CARTESIAN_POINT('Ctrl Pts',(3.16518084822296,8.78023376225081,-5.52933408693512));
#97256=CARTESIAN_POINT('Ctrl Pts',(3.28065563177323,10.3304739499724,-0.8814684930199));
#97257=CARTESIAN_POINT('Ctrl Pts',(3.46733327630008,9.57406157984235,3.94707456960536));
#97258=CARTESIAN_POINT('Ctrl Pts',(3.64442432694637,6.68527681753859,7.89475514720481));
#97259=CARTESIAN_POINT('Ctrl Pts',(3.84299745953732,1.8275257206148,10.318269563343));
#97260=CARTESIAN_POINT('Ctrl Pts',(4.06042336981818,-4.23805330991327,9.75068525772592));
#97261=CARTESIAN_POINT('Ctrl Pts',(4.29761943218592,-9.19209258466678,5.31824870856728));
#97262=CARTESIAN_POINT('Ctrl Pts',(4.53437161274713,-10.5350051791128,-1.17556335380542));
#97263=CARTESIAN_POINT('Ctrl Pts',(4.7708980371129,-7.77097759235335,-7.19441649509308));
#97264=CARTESIAN_POINT('Ctrl Pts',(5.00711660622112,-1.97462556771702,-10.3930919627927));
#97265=CARTESIAN_POINT('Ctrl Pts',(5.21686324657125,3.84430502097436,-9.61644715696625));
#97266=CARTESIAN_POINT('Ctrl Pts',(5.40022325876364,7.78412965343201,-6.54316740517288));
#97267=CARTESIAN_POINT('Ctrl Pts',(5.55728136173065,9.77755506434019,-2.7630113948148));
#97268=CARTESIAN_POINT('Ctrl Pts',(5.74039202752718,10.0925810161338,2.21725805512244));
#97269=CARTESIAN_POINT('Ctrl Pts',(5.94949375129097,7.45693493819098,7.44288523114148));
#97270=CARTESIAN_POINT('Ctrl Pts',(6.18451777235544,1.57504642791826,10.4069276145566));
#97271=CARTESIAN_POINT('Ctrl Pts',(6.41934409059153,-4.9076259651148,9.30134643286956));
#97272=CARTESIAN_POINT('Ctrl Pts',(6.65398123255926,-9.46546493887723,4.56502892019478));
#97273=CARTESIAN_POINT('Ctrl Pts',(6.88844862201365,-10.3192263205529,-1.94583617559358));
#97274=CARTESIAN_POINT('Ctrl Pts',(7.12275735358216,-7.14154658054596,-7.69098867775806));
#97275=CARTESIAN_POINT('Ctrl Pts',(7.31789383154067,-2.17248871763666,-9.96277635107079));
#97276=CARTESIAN_POINT('Ctrl Pts',(7.47393908444266,2.03065753434173,-9.75540780747296));
#97277=CARTESIAN_POINT('Ctrl Pts',(7.6299434805996,5.9644634282179,-8.26211446422332));
#97278=CARTESIAN_POINT('Ctrl Pts',(7.82487598081776,9.60233065552826,-4.1948354558297));
#97279=CARTESIAN_POINT('Ctrl Pts',(8.05869462024724,10.2141341233479,2.33092319144744));
#97280=CARTESIAN_POINT('Ctrl Pts',(8.29242713293129,6.82975323685128,7.93295582313208));
#97281=CARTESIAN_POINT('Ctrl Pts',(8.52608518374186,0.782992881230091,10.4371166486048));
#97282=CARTESIAN_POINT('Ctrl Pts',(8.75968779881235,-5.56546712895628,8.85948026402679));
#97283=CARTESIAN_POINT('Ctrl Pts',(8.99324390420264,-9.74358840205274,3.82461799473537));
#97284=CARTESIAN_POINT('Ctrl Pts',(9.18785311736504,-10.0413667217101,-1.61886906842269));
#97285=CARTESIAN_POINT('Ctrl Pts',(9.34353133992201,-8.31767691397426,-5.4467288803861));
#97286=CARTESIAN_POINT('Ctrl Pts',(9.49920792635024,-5.49774110980979,-8.55637463672939));
#97287=CARTESIAN_POINT('Ctrl Pts',(9.69380443073233,-0.388675826148052,
-10.4577620504452));
#97288=CARTESIAN_POINT('Ctrl Pts',(9.90138990968947,5.19543696900351,-8.84060317707353));
#97289=CARTESIAN_POINT('Ctrl Pts',(10.0830435383244,8.60064437435068,-5.25171837777729));
#97290=CARTESIAN_POINT('Ctrl Pts',(10.2387643960254,10.0028444638209,-1.24914248103297));
#97291=CARTESIAN_POINT('Ctrl Pts',(10.37720298638,9.67023254520016,2.50437837408168));
#97292=CARTESIAN_POINT('Ctrl Pts',(10.5329676769268,7.88804604937092,6.29825863224296));
#97293=CARTESIAN_POINT('Ctrl Pts',(10.6887607398496,4.60750562412172,9.0987655073134));
#97294=CARTESIAN_POINT('Ctrl Pts',(10.8619109109484,-0.00703355469036902,
10.0852618131503));
#97295=CARTESIAN_POINT('Ctrl Pts',(11.0177828805925,-4.15564321735493,9.19600425219595));
#97296=CARTESIAN_POINT('Ctrl Pts',(11.1737001608909,-7.57035238191842,6.67287428521118));
#97297=CARTESIAN_POINT('Ctrl Pts',(11.3556582804353,-10.0015525960454,2.35319965804952));
#97298=CARTESIAN_POINT('Ctrl Pts',(11.5636962223343,-9.89945473807122,-3.46995082097515));
#97299=CARTESIAN_POINT('Ctrl Pts',(11.7978709095172,-5.90444684023231,-8.6762915307363));
#97300=CARTESIAN_POINT('Ctrl Pts',(12.0321903548044,0.400833060828008,-10.4937295217811));
#97301=CARTESIAN_POINT('Ctrl Pts',(12.2666675462662,6.55977924120225,-8.21100202194529));
#97302=CARTESIAN_POINT('Ctrl Pts',(12.5013204486353,10.1611836230131,-2.71214958148474));
#97303=CARTESIAN_POINT('Ctrl Pts',(12.7361586173256,9.79488883170482,3.85415353952862));
#97304=CARTESIAN_POINT('Ctrl Pts',(12.9711981732529,5.59499649365486,8.92819941309873));
#97305=CARTESIAN_POINT('Ctrl Pts',(13.1803153631814,-0.0875873623257469,
10.3336777025827));
#97306=CARTESIAN_POINT('Ctrl Pts',(13.3634371883564,-4.8715902948797,8.91705557662938));
#97307=CARTESIAN_POINT('Ctrl Pts',(13.520505724078,-8.11433355257515,6.13074937900602));
#97308=CARTESIAN_POINT('Ctrl Pts',(13.677682974814,-9.92426658237873,2.2509045507049));
#97309=CARTESIAN_POINT('Ctrl Pts',(13.8349734047848,-9.98057122548719,-2.0316952253054));
#97310=CARTESIAN_POINT('Ctrl Pts',(13.9923803080536,-8.2666973670815,-5.96072336484286));
#97311=CARTESIAN_POINT('Ctrl Pts',(14.1367835222368,-5.35165095933992,-8.6005816687047));
#97312=CARTESIAN_POINT('Ctrl Pts',(14.2681481522955,-2.04257932770994,-9.86129725114235));
#97313=CARTESIAN_POINT('Ctrl Pts',(14.4258813335358,2.20726207074819,-10.0695922061582));
#97314=CARTESIAN_POINT('Ctrl Pts',(14.6232328885067,7.23285997487796,-7.77868641881626));
#97315=CARTESIAN_POINT('Ctrl Pts',(14.8603648356027,10.4488462542502,-1.9592940246166));
#97316=CARTESIAN_POINT('Ctrl Pts',(15.0978152410641,9.58510242747451,4.63131300952894));
#97317=CARTESIAN_POINT('Ctrl Pts',(15.3355945418123,4.96624008693659,9.43556607275977));
#97318=CARTESIAN_POINT('Ctrl Pts',(15.5472659450391,-0.876115585652837,
10.4252628531268));
#97319=CARTESIAN_POINT('Ctrl Pts',(15.7327007535624,-5.59959226313437,8.63432403909379));
#97320=CARTESIAN_POINT('Ctrl Pts',(15.8918077602256,-8.6659356307169,5.57596084701422));
#97321=CARTESIAN_POINT('Ctrl Pts',(16.0510831684788,-10.2019230830579,1.51791718343275));
#97322=CARTESIAN_POINT('Ctrl Pts',(16.2105256124773,-9.9342900388101,-2.81488948283342));
#97323=CARTESIAN_POINT('Ctrl Pts',(16.3701404794229,-7.90520615830692,-6.65973809987124));
#97324=CARTESIAN_POINT('Ctrl Pts',(16.5299308091608,-4.47173190491229,-9.3315218483862));
#97325=CARTESIAN_POINT('Ctrl Pts',(16.689895927779,-0.237156293344815,-10.3588395266908));
#97326=CARTESIAN_POINT('Ctrl Pts',(16.8500471787606,4.04617623445192,-9.547731017281));
#97327=CARTESIAN_POINT('Ctrl Pts',(17.0370951498213,8.22725055971312,-6.63413010802371));
#97328=CARTESIAN_POINT('Ctrl Pts',(17.2512080029201,10.7361609685627,-1.19069424451522));
#97329=CARTESIAN_POINT('Ctrl Pts',(17.4924479420939,9.36052958618687,5.42776286527152));
#97330=CARTESIAN_POINT('Ctrl Pts',(17.7342626534981,4.31561709585493,9.94660037034397));
#97331=CARTESIAN_POINT('Ctrl Pts',(17.9560677398241,-1.87318360886642,10.5258988523837));
#97332=CARTESIAN_POINT('Ctrl Pts',(18.1586777030311,-6.82953792919343,8.0537380447665));
#97333=CARTESIAN_POINT('Ctrl Pts',(18.3395298833531,-9.77919804704876,4.02216254357936));
#97334=CARTESIAN_POINT('Ctrl Pts',(18.5300740388948,-10.5517653438536,-0.90606004736438));
#97335=CARTESIAN_POINT('Ctrl Pts',(18.64805587877,-8.96809223471218,-5.6541368174137));
#97336=CARTESIAN_POINT('Ctrl Pts',(18.7984112754343,-5.37797595348926,-9.15197600853212));
#97337=CARTESIAN_POINT('Ctrl Pts',(18.9333053939666,-0.577353141871393,
-10.6109679620998));
#97338=CARTESIAN_POINT('Ctrl Pts',(19.0760117727805,4.36310404586792,-9.7039080890023));
#97339=CARTESIAN_POINT('Ctrl Pts',(19.2152458180293,8.34073515999311,-6.62558477275444));
#97340=CARTESIAN_POINT('Ctrl Pts',(19.3563124474702,10.4639838983962,-2.06055455074961));
#97341=CARTESIAN_POINT('Ctrl Pts',(19.4968066664293,10.2545994787298,2.97769872115227));
#97342=CARTESIAN_POINT('Ctrl Pts',(19.6377988698527,7.75298183285304,7.35915813897839));
#97343=CARTESIAN_POINT('Ctrl Pts',(19.7788087536973,3.51396003949119,10.1150854546748));
#97344=CARTESIAN_POINT('Ctrl Pts',(19.9200865166857,-1.5228146944367,10.6014255500044));
#97345=CARTESIAN_POINT('Ctrl Pts',(20.0614293133846,-6.22707474371873,8.75402786138048));
#97346=CARTESIAN_POINT('Ctrl Pts',(20.2031253543693,-9.56103685363943,4.87911794644152));
#97347=CARTESIAN_POINT('Ctrl Pts',(20.2974622713297,-10.3504309907549,1.6673870870399));
#97348=CARTESIAN_POINT('Ctrl Pts',(20.3448886687027,-10.3565230755762,-0.028427069738528));
#97349=CARTESIAN_POINT('Ctrl Pts',(1.83818426640986,10.8689493708656,-0.0308112345521901));
#97350=CARTESIAN_POINT('Ctrl Pts',(1.88776189648677,10.8625809528271,1.74192403210919));
#97351=CARTESIAN_POINT('Ctrl Pts',(1.98696005135264,10.0340075995239,5.11962447490025));
#97352=CARTESIAN_POINT('Ctrl Pts',(2.13551416471739,6.53596609625885,9.18048144916341));
#97353=CARTESIAN_POINT('Ctrl Pts',(2.28385549019855,1.60092055185801,11.1212281400739));
#97354=CARTESIAN_POINT('Ctrl Pts',(2.43201757162897,-3.6820951696278,10.6096556943922));
#97355=CARTESIAN_POINT('Ctrl Pts',(2.57990783088367,-8.12742516058339,7.72019468550292));
#97356=CARTESIAN_POINT('Ctrl Pts',(2.72773989858082,-10.7503724424901,3.12577566618505));
#97357=CARTESIAN_POINT('Ctrl Pts',(2.87502614211072,-10.969712571133,-2.15572865673128));
#97358=CARTESIAN_POINT('Ctrl Pts',(3.02288074463859,-8.74423490665549,-6.94037080074683));
#97359=CARTESIAN_POINT('Ctrl Pts',(3.16878612908498,-4.57600120570609,-10.1660120144097));
#97360=CARTESIAN_POINT('Ctrl Pts',(3.31829567125103,0.599901256008977,-11.11609137723));
#97361=CARTESIAN_POINT('Ctrl Pts',(3.45958938695334,5.62820968933488,-9.58793407736161));
#97362=CARTESIAN_POINT('Ctrl Pts',(3.61704293708648,9.38747189660534,-5.92469929399861));
#97363=CARTESIAN_POINT('Ctrl Pts',(3.74056654439857,11.0455000317742,-0.9538859493391));
#97364=CARTESIAN_POINT('Ctrl Pts',(3.9398976454627,10.2365319010948,4.20107343062296));
#97365=CARTESIAN_POINT('Ctrl Pts',(4.12916837477669,7.15042126932385,8.42057304437813));
#97366=CARTESIAN_POINT('Ctrl Pts',(4.34103991393533,1.96602379561902,11.0048501470889));
#97367=CARTESIAN_POINT('Ctrl Pts',(4.5729306213578,-4.50201320676947,10.3996247365394));
#97368=CARTESIAN_POINT('Ctrl Pts',(4.8255857070546,-9.77799551649871,5.67675453717147));
#97369=CARTESIAN_POINT('Ctrl Pts',(5.07749033585182,-11.2056768141972,-1.23238566466435));
#97370=CARTESIAN_POINT('Ctrl Pts',(5.32887240299551,-8.26686359636807,-7.6286025326305));
#97371=CARTESIAN_POINT('Ctrl Pts',(5.57962526190281,-2.11347710892471,-11.0227160727275));
#97372=CARTESIAN_POINT('Ctrl Pts',(5.80201065073146,4.05562182529484,-10.1981135862017));
#97373=CARTESIAN_POINT('Ctrl Pts',(5.99619748242115,8.22765205976638,-6.94304765662431));
#97374=CARTESIAN_POINT('Ctrl Pts',(6.16238502036293,10.3365757371908,-2.94306233307449));
#97375=CARTESIAN_POINT('Ctrl Pts',(6.35597213040649,10.6690844793293,2.32209917177999));
#97376=CARTESIAN_POINT('Ctrl Pts',(6.57679779675907,7.88462429552231,7.8399572546674));
#97377=CARTESIAN_POINT('Ctrl Pts',(6.82464760372649,1.68122123786173,10.9642470927747));
#97378=CARTESIAN_POINT('Ctrl Pts',(7.0719359806289,-5.1449584383304,9.79849951504099));
#97379=CARTESIAN_POINT('Ctrl Pts',(7.31866327856874,-9.93634104403059,4.81715538296204));
#97380=CARTESIAN_POINT('Ctrl Pts',(7.56484307141959,-10.8310545876768,-2.01893420180603));
#97381=CARTESIAN_POINT('Ctrl Pts',(7.81047672182262,-7.49838634017914,-8.04079854736679));
#97382=CARTESIAN_POINT('Ctrl Pts',(8.0147315059415,-2.29677092419376,-10.4173489247643));
#97383=CARTESIAN_POINT('Ctrl Pts',(8.17786172927881,2.0970715104821,-10.2002860770181));
#97384=CARTESIAN_POINT('Ctrl Pts',(8.34081833458581,6.20607454866971,-8.64017166703644));
#97385=CARTESIAN_POINT('Ctrl Pts',(8.54419898417021,10.000471803415,-4.39575725264335));
#97386=CARTESIAN_POINT('Ctrl Pts',(8.78774561141104,10.6357859285607,2.40148995762388));
#97387=CARTESIAN_POINT('Ctrl Pts',(9.03078021376301,7.11527379626338,8.22542500490687));
#97388=CARTESIAN_POINT('Ctrl Pts',(9.27332878581485,0.837846907564282,10.8230720357878));
#97389=CARTESIAN_POINT('Ctrl Pts',(9.51539756520767,-5.74004007217375,9.18649736408127));
#97390=CARTESIAN_POINT('Ctrl Pts',(9.75697918017891,-10.0602275893844,3.97738562041968));
#97391=CARTESIAN_POINT('Ctrl Pts',(9.95792867482619,-10.3661161112419,-1.64326633591469));
#97392=CARTESIAN_POINT('Ctrl Pts',(10.1184478344858,-8.58857431044701,-5.58991834917576));
#97393=CARTESIAN_POINT('Ctrl Pts',(10.2788200862377,-5.683335003516,-8.79316631224028));
#97394=CARTESIAN_POINT('Ctrl Pts',(10.4790161508981,-0.426755680715147,
-10.7476973019787));
#97395=CARTESIAN_POINT('Ctrl Pts',(10.6921776353054,5.30667425331728,-9.08543831520305));
#97396=CARTESIAN_POINT('Ctrl Pts',(10.8784122755464,8.79717325481755,-5.40566075731209));
#97397=CARTESIAN_POINT('Ctrl Pts',(11.0378573747148,10.2323564000071,-1.30718768757403));
#97398=CARTESIAN_POINT('Ctrl Pts',(11.1794315307463,9.89171945814866,2.53120787155922));
#97399=CARTESIAN_POINT('Ctrl Pts',(11.3385508759767,8.07088824484368,6.40668023386538));
#97400=CARTESIAN_POINT('Ctrl Pts',(11.4974943772879,4.72338085120294,9.26303381412744));
#97401=CARTESIAN_POINT('Ctrl Pts',(11.6738835255329,0.0224914630507778,
10.2672914814035));
#97402=CARTESIAN_POINT('Ctrl Pts',(11.8324606855234,-4.19799457821475,9.36203711938622));
#97403=CARTESIAN_POINT('Ctrl Pts',(11.9908814020297,-7.6671319801918,6.797988448667));
#97404=CARTESIAN_POINT('Ctrl Pts',(12.1755152746382,-10.1334735184091,2.41440828085528));
#97405=CARTESIAN_POINT('Ctrl Pts',(12.3862701364914,-10.0282559850612,-3.48472158440349));
#97406=CARTESIAN_POINT('Ctrl Pts',(12.6230299247251,-5.98748195420321,-8.7472018168645));
#97407=CARTESIAN_POINT('Ctrl Pts',(12.859465524537,0.37524583457908,-10.579038475418));
#97408=CARTESIAN_POINT('Ctrl Pts',(13.0955874024424,6.57663912099642,-8.2783325277854));
#97409=CARTESIAN_POINT('Ctrl Pts',(13.3314131098248,10.1942562826981,-2.75087923652243));
#97410=CARTESIAN_POINT('Ctrl Pts',(13.5669515207943,9.82478241877411,3.83487919978063));
#97411=CARTESIAN_POINT('Ctrl Pts',(13.8022183194738,5.61919167439339,8.91245356687083));
#97412=CARTESIAN_POINT('Ctrl Pts',(14.0111170136416,-0.0578387583680794,
10.3146871657184));
#97413=CARTESIAN_POINT('Ctrl Pts',(14.1937410470241,-4.82856420086894,8.9012331076977));
#97414=CARTESIAN_POINT('Ctrl Pts',(14.350172686012,-8.05780235173047,6.12577966918914));
#97415=CARTESIAN_POINT('Ctrl Pts',(14.506503362215,-9.85743405856432,2.26657374520578));
#97416=CARTESIAN_POINT('Ctrl Pts',(14.662737409681,-9.91277321911816,-1.98729168662078));
#97417=CARTESIAN_POINT('Ctrl Pts',(14.8188789169398,-8.21212706834228,-5.88449319471934));
#97418=CARTESIAN_POINT('Ctrl Pts',(14.9619297947965,-5.32400842064335,-8.49923201713043));
#97419=CARTESIAN_POINT('Ctrl Pts',(15.0919132392097,-2.04965056788055,-9.74644660641511));
#97420=CARTESIAN_POINT('Ctrl Pts',(15.2478333215524,2.15143905872322,-9.95199811185607));
#97421=CARTESIAN_POINT('Ctrl Pts',(15.4426246944657,7.11126846897201,-7.68925041226127));
#97422=CARTESIAN_POINT('Ctrl Pts',(15.6762169225839,10.2774005373863,-1.95566702569206));
#97423=CARTESIAN_POINT('Ctrl Pts',(15.909663704702,9.42624261870193,4.52362470256974));
#97424=CARTESIAN_POINT('Ctrl Pts',(16.1429778981499,4.89257476540304,9.23627484965717));
#97425=CARTESIAN_POINT('Ctrl Pts',(16.3502681848699,-0.829186051812911,
10.2038045922452));
#97426=CARTESIAN_POINT('Ctrl Pts',(16.5315794164556,-5.44734383968922,8.45205581404979));
#97427=CARTESIAN_POINT('Ctrl Pts',(16.6869491325359,-8.44132728453901,5.46511601110685));
#97428=CARTESIAN_POINT('Ctrl Pts',(16.8422824860369,-9.93878585482269,1.50724672168229));
#97429=CARTESIAN_POINT('Ctrl Pts',(16.9975846873159,-9.67755952490929,-2.71305977140622));
#97430=CARTESIAN_POINT('Ctrl Pts',(17.1528587616045,-7.70313312175431,-6.45315215757489));
#97431=CARTESIAN_POINT('Ctrl Pts',(17.3081114703888,-4.36678293396964,-9.04865359635369));
#97432=CARTESIAN_POINT('Ctrl Pts',(17.4633433266442,-0.257307507931174,
-10.0450555316724));
#97433=CARTESIAN_POINT('Ctrl Pts',(17.6185664673369,3.89412154725938,-9.25838762996026));
#97434=CARTESIAN_POINT('Ctrl Pts',(17.7996358527774,7.94134476011658,-6.43722851335476));
#97435=CARTESIAN_POINT('Ctrl Pts',(18.006594507299,10.364912084505,-1.17513016360907));
#97436=CARTESIAN_POINT('Ctrl Pts',(18.2393437052062,9.03587592715122,5.21087315758684));
#97437=CARTESIAN_POINT('Ctrl Pts',(18.4722791560659,4.17530017099195,9.56114196894378));
#97438=CARTESIAN_POINT('Ctrl Pts',(18.685483449533,-1.77503968503135,10.1181556762285));
#97439=CARTESIAN_POINT('Ctrl Pts',(18.880106854292,-6.53372445406436,7.74112266949097));
#97440=CARTESIAN_POINT('Ctrl Pts',(19.0533284606598,-9.36098152271742,3.88031745665509));
#97441=CARTESIAN_POINT('Ctrl Pts',(19.2361266589478,-10.1000769718,-0.848911211642665));
#97442=CARTESIAN_POINT('Ctrl Pts',(19.3489763573003,-8.58507867110896,-5.39153275737696));
#97443=CARTESIAN_POINT('Ctrl Pts',(19.4926766226755,-5.15305056101582,-8.73333966878052));
#97444=CARTESIAN_POINT('Ctrl Pts',(19.6214820850813,-0.568968113951337,
-10.1266503521605));
#97445=CARTESIAN_POINT('Ctrl Pts',(19.7576303738871,4.144475299569,-9.26047530960638));
#97446=CARTESIAN_POINT('Ctrl Pts',(19.8903381036552,7.93547183918914,-6.32599142257229));
#97447=CARTESIAN_POINT('Ctrl Pts',(20.024680461408,9.95714380136737,-1.97832471792147));
#97448=CARTESIAN_POINT('Ctrl Pts',(20.1583550467776,9.75736223240569,2.81574382815119));
#97449=CARTESIAN_POINT('Ctrl Pts',(20.2923937974737,7.37877459907573,6.98054580469578));
#97450=CARTESIAN_POINT('Ctrl Pts',(20.4263199844727,3.35188564930949,9.59874115052656));
#97451=CARTESIAN_POINT('Ctrl Pts',(20.560425364838,-1.42837773210827,10.0584164488272));
#97452=CARTESIAN_POINT('Ctrl Pts',(20.6943868066463,-5.88919751845155,8.30912295420081));
#97453=CARTESIAN_POINT('Ctrl Pts',(20.8287698213737,-9.04785423569596,4.63223803957308));
#97454=CARTESIAN_POINT('Ctrl Pts',(20.9178530496044,-9.79467800620001,1.59976306232615));
#97455=CARTESIAN_POINT('Ctrl Pts',(20.9629606708448,-9.80047223620488,-0.0131391802037495));
#97456=CARTESIAN_POINT('Ctrl Pts',(1.5809870441838,11.4169386758616,-0.0216496558209534));
#97457=CARTESIAN_POINT('Ctrl Pts',(1.63289675206296,11.4102706943643,1.83447314990275));
#97458=CARTESIAN_POINT('Ctrl Pts',(1.73729284798262,10.5405348425062,5.39040289704493));
#97459=CARTESIAN_POINT('Ctrl Pts',(1.8933082281801,6.86421115644908,9.65429347040028));
#97460=CARTESIAN_POINT('Ctrl Pts',(2.04932475230953,1.67555195478847,11.6979359622337));
#97461=CARTESIAN_POINT('Ctrl Pts',(2.20512511369068,-3.8812787875302,11.1586878225894));
#97462=CARTESIAN_POINT('Ctrl Pts',(2.36072469806447,-8.55856555251663,8.11941596439485));
#97463=CARTESIAN_POINT('Ctrl Pts',(2.51630371286344,-11.3195400105841,3.28336209072214));
#97464=CARTESIAN_POINT('Ctrl Pts',(2.67136081404846,-11.5506449296019,-2.27719803269604));
#97465=CARTESIAN_POINT('Ctrl Pts',(2.82706597810207,-9.20692048539113,-7.31662279645037));
#97466=CARTESIAN_POINT('Ctrl Pts',(2.98076287682068,-4.81569331332354,-10.7149974591792));
#97467=CARTESIAN_POINT('Ctrl Pts',(3.13830732477856,0.638935692629033,-11.7165434272761));
#97468=CARTESIAN_POINT('Ctrl Pts',(3.28723251892036,5.93951699244716,-10.1055865581304));
#97469=CARTESIAN_POINT('Ctrl Pts',(3.45324044352558,9.90367736049909,-6.2433617525658));
#97470=CARTESIAN_POINT('Ctrl Pts',(3.58349680980263,11.6524189813092,-1.00031976365907));
#97471=CARTESIAN_POINT('Ctrl Pts',(3.79388045160135,10.7991398987405,4.44122959128948));
#97472=CARTESIAN_POINT('Ctrl Pts',(3.99355019295073,7.54252592952349,8.89267332393697));
#97473=CARTESIAN_POINT('Ctrl Pts',(4.21723559604996,2.06922068053357,11.6220329583823));
#97474=CARTESIAN_POINT('Ctrl Pts',(4.46207111387019,-4.76093494914438,10.9825998628467));
#97475=CARTESIAN_POINT('Ctrl Pts',(4.72893719312375,-10.334874453495,5.99419965381685));
#97476=CARTESIAN_POINT('Ctrl Pts',(4.99514679887966,-11.8437987505411,-1.30785848843795));
#97477=CARTESIAN_POINT('Ctrl Pts',(5.26084090744296,-8.73780244151131,-8.06924018541072));
#97478=CARTESIAN_POINT('Ctrl Pts',(5.52595750953483,-2.23133107764473,-11.6583422596195));
#97479=CARTESIAN_POINT('Ctrl Pts',(5.7611068176764,4.29279932288354,-10.7865607271241));
#97480=CARTESIAN_POINT('Ctrl Pts',(5.96652714516798,8.7064943800609,-7.34305887020326));
#97481=CARTESIAN_POINT('Ctrl Pts',(6.14235049354763,10.9378177637936,-3.11093327658175));
#97482=CARTESIAN_POINT('Ctrl Pts',(6.34717311281565,11.2897503542811,2.46018182270645));
#97483=CARTESIAN_POINT('Ctrl Pts',(6.58081017622451,8.34335570885647,8.29891791849555));
#97484=CARTESIAN_POINT('Ctrl Pts',(6.84309571117951,1.77811161543802,11.6055559975002));
#97485=CARTESIAN_POINT('Ctrl Pts',(7.10480193995066,-5.44689514012842,10.3716741505217));
#97486=CARTESIAN_POINT('Ctrl Pts',(7.3659363394261,-10.5184885864916,5.09901317667749));
#97487=CARTESIAN_POINT('Ctrl Pts',(7.62648869550098,-11.4655827108715,-2.13697521097448));
#97488=CARTESIAN_POINT('Ctrl Pts',(7.88646893283754,-7.93788982756581,-8.51098443842803));
#97489=CARTESIAN_POINT('Ctrl Pts',(8.1026212089916,-2.4326177345364,-11.0262083103435));
#97490=CARTESIAN_POINT('Ctrl Pts',(8.27527724919823,2.21799111278608,-10.7964225498402));
#97491=CARTESIAN_POINT('Ctrl Pts',(8.44773846159635,6.56691865522038,-9.14522106162279));
#97492=CARTESIAN_POINT('Ctrl Pts',(8.6629306742405,10.5818216065013,-4.65374125637833));
#97493=CARTESIAN_POINT('Ctrl Pts',(8.92058295804147,11.2539961301362,2.53794920615522));
#97494=CARTESIAN_POINT('Ctrl Pts',(9.17768234425578,7.52916588638302,8.69903847266077));
#97495=CARTESIAN_POINT('Ctrl Pts',(9.43418691040704,0.889964532955913,11.4461559338261));
#97496=CARTESIAN_POINT('Ctrl Pts',(9.69011268842353,-6.06506695109494,9.71534908612722));
#97497=CARTESIAN_POINT('Ctrl Pts',(9.94549168521195,-10.6318873005423,4.20842658922282));
#97498=CARTESIAN_POINT('Ctrl Pts',(10.1577958510016,-10.9546044353997,-1.73065225296835));
#97499=CARTESIAN_POINT('Ctrl Pts',(10.327383585701,-9.0765773666272,-5.90032179774202));
#97500=CARTESIAN_POINT('Ctrl Pts',(10.49677789506,-6.00767290500012,-9.28392549693938));
#97501=CARTESIAN_POINT('Ctrl Pts',(10.7081504461604,-0.457028090683516,
-11.3473051979206));
#97502=CARTESIAN_POINT('Ctrl Pts',(10.9331123366397,5.59420942624187,-9.59252532148522));
#97503=CARTESIAN_POINT('Ctrl Pts',(11.1296073081414,9.27704839612523,-5.70971854781571));
#97504=CARTESIAN_POINT('Ctrl Pts',(11.297786940236,10.7907142084956,-1.38653999583745));
#97505=CARTESIAN_POINT('Ctrl Pts',(11.4470487914226,10.4314326507295,2.66052368848947));
#97506=CARTESIAN_POINT('Ctrl Pts',(11.6147735026284,8.5119640671563,6.74573039814433));
#97507=CARTESIAN_POINT('Ctrl Pts',(11.7822558891056,4.98427451759871,9.75536146854628));
#97508=CARTESIAN_POINT('Ctrl Pts',(11.9680227641689,0.0331256487114618,
10.8127717293753));
#97509=CARTESIAN_POINT('Ctrl Pts',(12.1349843154738,-4.41056739519488,9.85946584683898));
#97510=CARTESIAN_POINT('Ctrl Pts',(12.3016942670706,-8.06126526847656,7.16083504228128));
#97511=CARTESIAN_POINT('Ctrl Pts',(12.4959220969932,-10.655623004286,2.54919301777192));
#97512=CARTESIAN_POINT('Ctrl Pts',(12.717489767947,-10.5442072791782,-3.65300085548494));
#97513=CARTESIAN_POINT('Ctrl Pts',(12.9662363807326,-6.29803981578373,-9.18160665973904));
#97514=CARTESIAN_POINT('Ctrl Pts',(13.214460617168,0.382489528166651,-11.1040129548448));
#97515=CARTESIAN_POINT('Ctrl Pts',(13.4621717586644,6.88816657569474,-8.68945672393844));
#97516=CARTESIAN_POINT('Ctrl Pts',(13.7093763702802,10.6796831715465,-2.89458716516783));
#97517=CARTESIAN_POINT('Ctrl Pts',(13.9560791595477,10.291740536784,4.00350012428347));
#97518=CARTESIAN_POINT('Ctrl Pts',(14.2022892176303,5.88962980452267,9.31674394387247));
#97519=CARTESIAN_POINT('Ctrl Pts',(14.4207087523392,-0.0465033974837142,
10.7820677674357));
#97520=CARTESIAN_POINT('Ctrl Pts',(14.6115180151071,-5.03098776215844,9.30489515804488));
#97521=CARTESIAN_POINT('Ctrl Pts',(14.7748574763112,-8.40269313292153,6.40659876167101));
#97522=CARTESIAN_POINT('Ctrl Pts',(14.9379888665339,-10.2803266780696,2.37931588593463));
#97523=CARTESIAN_POINT('Ctrl Pts',(15.1009157458048,-10.3377315800466,-2.05682724723024));
#97524=CARTESIAN_POINT('Ctrl Pts',(15.263638577978,-8.56506525302953,-6.11818660926039));
#97525=CARTESIAN_POINT('Ctrl Pts',(15.4126178905096,-5.55702315674806,-8.84107798464344));
#97526=CARTESIAN_POINT('Ctrl Pts',(15.5479084789727,-2.14891101096889,-10.1390596050238));
#97527=CARTESIAN_POINT('Ctrl Pts',(15.7101105471896,2.2215090845951,-10.3526814778452));
#97528=CARTESIAN_POINT('Ctrl Pts',(15.9125903919246,7.37675549081694,-7.99971492454468));
#97529=CARTESIAN_POINT('Ctrl Pts',(16.1551398067183,10.66316984791,-2.04563823051419));
#97530=CARTESIAN_POINT('Ctrl Pts',(16.3972724776516,9.77911126777587,4.67451911452633));
#97531=CARTESIAN_POINT('Ctrl Pts',(16.6389940080972,5.08114453646148,9.55608842508968));
#97532=CARTESIAN_POINT('Ctrl Pts',(16.8535101459097,-0.840131908612288,
10.5561550864893));
#97533=CARTESIAN_POINT('Ctrl Pts',(17.0409517630139,-5.61421615837297,8.7447801338398));
#97534=CARTESIAN_POINT('Ctrl Pts',(17.2014479827319,-8.70669146981356,5.65902412117622));
#97535=CARTESIAN_POINT('Ctrl Pts',(17.3617817749257,-10.2519259768557,1.57368476722833));
#97536=CARTESIAN_POINT('Ctrl Pts',(17.5219505321004,-9.98210887180923,-2.77878183638506));
#97537=CARTESIAN_POINT('Ctrl Pts',(17.6819601751567,-7.9471388192863,-6.63264401487525));
#97538=CARTESIAN_POINT('Ctrl Pts',(17.841813076855,-4.51175814935185,-9.30470904997924));
#97539=CARTESIAN_POINT('Ctrl Pts',(18.0015074983284,-0.284100670960046,
-10.3292985319853));
#97540=CARTESIAN_POINT('Ctrl Pts',(18.1610574640256,3.98286343161655,-9.5203859703373));
#97541=CARTESIAN_POINT('Ctrl Pts',(18.3470121213786,8.13897972179755,-6.62263664608639));
#97542=CARTESIAN_POINT('Ctrl Pts',(18.5593421327914,10.6241500885949,-1.22395338402533));
#97543=CARTESIAN_POINT('Ctrl Pts',(18.797792357215,9.26114234990766,5.31857227275897));
#97544=CARTESIAN_POINT('Ctrl Pts',(19.0361531638009,4.28697136791716,9.76769129949924));
#97545=CARTESIAN_POINT('Ctrl Pts',(19.253957480802,-1.7926669194774,10.3368279771911));
#97546=CARTESIAN_POINT('Ctrl Pts',(19.4526697367228,-6.64906312358094,7.90795031395204));
#97547=CARTESIAN_POINT('Ctrl Pts',(19.6291042447626,-9.53038483805921,3.97628906838568));
#97548=CARTESIAN_POINT('Ctrl Pts',(19.8155522410141,-10.2823637494848,-0.848298560168487));
#97549=CARTESIAN_POINT('Ctrl Pts',(19.9303748982537,-8.74083838503278,-5.4707959614783));
#97550=CARTESIAN_POINT('Ctrl Pts',(20.0764801747596,-5.25087077138079,-8.86716469444201));
#97551=CARTESIAN_POINT('Ctrl Pts',(20.207336615988,-0.594041765760311,-10.2826716766978));
#97552=CARTESIAN_POINT('Ctrl Pts',(20.3455459356972,4.19039095150704,-9.40267864491185));
#97553=CARTESIAN_POINT('Ctrl Pts',(20.4801452049017,8.03490413176417,-6.42622072618347));
#97554=CARTESIAN_POINT('Ctrl Pts',(20.6162967802764,10.0832377386608,-2.02003780110226));
#97555=CARTESIAN_POINT('Ctrl Pts',(20.7516569644152,9.88041700244468,2.83412583686586));
#97556=CARTESIAN_POINT('Ctrl Pts',(20.8872752484866,7.47350957465415,7.04757904292594));
#97557=CARTESIAN_POINT('Ctrl Pts',(21.0226693111701,3.40249785529857,9.69366523532026));
#97558=CARTESIAN_POINT('Ctrl Pts',(21.1581257461099,-1.42584389188091,10.1577350821885));
#97559=CARTESIAN_POINT('Ctrl Pts',(21.2933416880766,-5.92768137593638,8.3913040602114));
#97560=CARTESIAN_POINT('Ctrl Pts',(21.4288360559202,-9.11241563482646,4.6841853921408));
#97561=CARTESIAN_POINT('Ctrl Pts',(21.5186264843219,-9.86491503987726,1.6277742877437));
#97562=CARTESIAN_POINT('Ctrl Pts',(21.5640403001055,-9.87074860163053,0.0039235213980661));
#97563=CARTESIAN_POINT('Ctrl Pts',(1.37078399030106,11.5968559808931,-0.0151246218382906));
#97564=CARTESIAN_POINT('Ctrl Pts',(1.42344639163322,11.5900913133187,1.86791206070984));
#97565=CARTESIAN_POINT('Ctrl Pts',(1.52957558472544,10.7061758009457,5.48262935286527));
#97566=CARTESIAN_POINT('Ctrl Pts',(1.68806725517556,6.97084997875402,9.81349774501377));
#97567=CARTESIAN_POINT('Ctrl Pts',(1.8466683983699,1.6973507383663,11.8916950100086));
#97568=CARTESIAN_POINT('Ctrl Pts',(2.0050573808635,-3.9517229938656,11.3432022055592));
#97569=CARTESIAN_POINT('Ctrl Pts',(2.16329525988592,-8.70792520129272,8.25316135195273));
#97570=CARTESIAN_POINT('Ctrl Pts',(2.32154720540008,-11.5163007375259,3.33435837475925));
#97571=CARTESIAN_POINT('Ctrl Pts',(2.47930854099689,-11.7516016019017,-2.32262613844776));
#97572=CARTESIAN_POINT('Ctrl Pts',(2.63776873621243,-9.36675741608683,-7.45090770551429));
#97573=CARTESIAN_POINT('Ctrl Pts',(2.794221957083,-4.89725641148081,-10.9100368889974));
#97574=CARTESIAN_POINT('Ctrl Pts',(2.95463219424662,0.65612867535488,-11.9299825759692));
#97575=CARTESIAN_POINT('Ctrl Pts',(3.10630295800782,6.05393905269005,-10.2894470217606));
#97576=CARTESIAN_POINT('Ctrl Pts',(3.27540722237603,10.0919898594489,-6.355864787022));
#97577=CARTESIAN_POINT('Ctrl Pts',(3.40813022326932,11.8736472086377,-1.01402480604459));
#97578=CARTESIAN_POINT('Ctrl Pts',(3.62262736521885,11.0043548607243,4.5340281022513));
#97579=CARTESIAN_POINT('Ctrl Pts',(3.82612278073918,7.68498823728818,9.0702913426232));
#97580=CARTESIAN_POINT('Ctrl Pts',(4.05424821818397,2.10412498813912,11.8542631681714));
#97581=CARTESIAN_POINT('Ctrl Pts',(4.303989670121,-4.8628204540389,11.2021430709084));
#97582=CARTESIAN_POINT('Ctrl Pts',(4.57634402750476,-10.5508382917611,6.11230439642354));
#97583=CARTESIAN_POINT('Ctrl Pts',(4.84807252719374,-12.0916100956696,-1.34090444160256));
#97584=CARTESIAN_POINT('Ctrl Pts',(5.11941097117775,-8.92019588881371,-8.24532599345198));
#97585=CARTESIAN_POINT('Ctrl Pts',(5.39023633845774,-2.27430390790531,-11.9119316600466));
#97586=CARTESIAN_POINT('Ctrl Pts',(5.63055313505298,4.39258743413944,-11.0213734801145));
#97587=CARTESIAN_POINT('Ctrl Pts',(5.84050673057507,8.90360029523043,-7.50212221815739));
#97588=CARTESIAN_POINT('Ctrl Pts',(6.02024823233398,11.1846843243296,-3.17590078333041));
#97589=CARTESIAN_POINT('Ctrl Pts',(6.22968662701296,11.544641290149,2.52046272257992));
#97590=CARTESIAN_POINT('Ctrl Pts',(6.46867162670811,8.53143552522916,8.49250563983966));
#97591=CARTESIAN_POINT('Ctrl Pts',(6.73702105051741,1.81498495087946,11.8757023821266));
#97592=CARTESIAN_POINT('Ctrl Pts',(7.00485521835245,-5.57868259143474,10.6134222524762));
#97593=CARTESIAN_POINT('Ctrl Pts',(7.2721709266545,-10.7702618995273,5.21651065947963));
#97594=CARTESIAN_POINT('Ctrl Pts',(7.53896165766792,-11.7402232781411,-2.19213779211188));
#97595=CARTESIAN_POINT('Ctrl Pts',(7.80522410360587,-8.12778048205399,-8.71999414935387));
#97596=CARTESIAN_POINT('Ctrl Pts',(8.02666584019603,-2.4883280973737,-11.2967625293358));
#97597=CARTESIAN_POINT('Ctrl Pts',(8.20355086005244,2.27606964817821,-11.0614057110565));
#97598=CARTESIAN_POINT('Ctrl Pts',(8.38025653867744,6.73185738052523,-9.36966081926595));
#97599=CARTESIAN_POINT('Ctrl Pts',(8.60080147814508,10.8466067486195,-4.76692154743445));
#97600=CARTESIAN_POINT('Ctrl Pts',(8.8649123953267,11.53567362654,2.60451498005851));
#97601=CARTESIAN_POINT('Ctrl Pts',(9.12847741076998,7.71759982857128,8.92050555669179));
#97602=CARTESIAN_POINT('Ctrl Pts',(9.39149464051184,0.910228632703197,11.7373707917927));
#97603=CARTESIAN_POINT('Ctrl Pts',(9.65396108917076,-6.22213213447626,9.96266504826013));
#97604=CARTESIAN_POINT('Ctrl Pts',(9.91587545576831,-10.9058248797927,4.31498350177216));
#97605=CARTESIAN_POINT('Ctrl Pts',(10.1336756686123,-11.2371057762643,-1.77728859852975));
#97606=CARTESIAN_POINT('Ctrl Pts',(10.3076382792719,-9.31065173826634,-6.05446460465524));
#97607=CARTESIAN_POINT('Ctrl Pts',(10.4814156460693,-6.16247232954605,-9.52550747694019));
#97608=CARTESIAN_POINT('Ctrl Pts',(10.6982897832722,-0.46769691448907,-11.6426103959247));
#97609=CARTESIAN_POINT('Ctrl Pts',(10.9291272306577,5.74125850040209,-9.84212207388334));
#97610=CARTESIAN_POINT('Ctrl Pts',(11.1307489689019,9.52008597182504,-5.85814707876185));
#97611=CARTESIAN_POINT('Ctrl Pts',(11.3033199977502,11.0732864155087,-1.42217404507495));
#97612=CARTESIAN_POINT('Ctrl Pts',(11.4564964171182,10.7046015292691,2.73085096518305));
#97613=CARTESIAN_POINT('Ctrl Pts',(11.6286136828385,8.73492349297909,6.92294423096825));
#97614=CARTESIAN_POINT('Ctrl Pts',(11.8004836313932,5.11492430571815,10.0113894279398));
#97615=CARTESIAN_POINT('Ctrl Pts',(11.9911299728693,0.0339235184241942,
11.0965941162476));
#97616=CARTESIAN_POINT('Ctrl Pts',(12.162464967972,-4.52610964494761,10.1183218009339));
#97617=CARTESIAN_POINT('Ctrl Pts',(12.3335535502395,-8.27258546931572,7.34898304513248));
#97618=CARTESIAN_POINT('Ctrl Pts',(12.532870094617,-10.9348781729764,2.61659421510092));
#97619=CARTESIAN_POINT('Ctrl Pts',(12.760250907581,-10.8206047745579,-3.74804922686595));
#97620=CARTESIAN_POINT('Ctrl Pts',(13.0155042484857,-6.46343218839986,-9.42113306769874));
#97621=CARTESIAN_POINT('Ctrl Pts',(13.2702093387032,0.391327358387318,-11.3936597114125));
#97622=CARTESIAN_POINT('Ctrl Pts',(13.524368452853,7.06620025081125,-8.9162445302784));
#97623=CARTESIAN_POINT('Ctrl Pts',(13.777985289017,10.9559308253974,-2.97113304537923));
#97624=CARTESIAN_POINT('Ctrl Pts',(14.031061929482,10.5578777907155,4.10505318065189));
#97625=CARTESIAN_POINT('Ctrl Pts',(14.2836025108293,6.04255217281376,9.55477027287382));
#97626=CARTESIAN_POINT('Ctrl Pts',(14.5076098421657,-0.0453816316895607,
11.0574491674935));
#97627=CARTESIAN_POINT('Ctrl Pts',(14.7032734937542,-5.15662434425682,9.54266445836023));
#97628=CARTESIAN_POINT('Ctrl Pts',(14.8707516580605,-8.61371327624903,6.57092670033119));
#97629=CARTESIAN_POINT('Ctrl Pts',(15.0379975327689,-10.5386613119923,2.44207817038835));
#97630=CARTESIAN_POINT('Ctrl Pts',(15.2050127003932,-10.5974563283306,-2.1053734957677));
#97631=CARTESIAN_POINT('Ctrl Pts',(15.3717983084661,-8.7805015035724,-6.26810077555588));
#97632=CARTESIAN_POINT('Ctrl Pts',(15.524476514162,-5.69774406154741,-9.05856483432574));
#97633=CARTESIAN_POINT('Ctrl Pts',(15.6631094354508,-2.20543986778316,-10.388596236232));
#97634=CARTESIAN_POINT('Ctrl Pts',(15.8293004622731,2.27246813187408,-10.6074440625974));
#97635=CARTESIAN_POINT('Ctrl Pts',(16.0367241073791,7.55354012610783,-8.1968485777852));
#97636=CARTESIAN_POINT('Ctrl Pts',(16.2851349651193,10.9191675552082,-2.09873860741072));
#97637=CARTESIAN_POINT('Ctrl Pts',(16.5330544248483,10.0137352869958,4.7820760466034));
#97638=CARTESIAN_POINT('Ctrl Pts',(16.7804874957598,5.20451469300203,9.77881847117864));
#97639=CARTESIAN_POINT('Ctrl Pts',(17.0000035731033,-0.854928450922944,
10.8020033214215));
#97640=CARTESIAN_POINT('Ctrl Pts',(17.191773677799,-5.73923533968931,8.94868572317326));
#97641=CARTESIAN_POINT('Ctrl Pts',(17.3559407800684,-8.90243151287278,5.79227145828906));
#97642=CARTESIAN_POINT('Ctrl Pts',(17.5199021456526,-10.4825864347342,1.61438667171539));
#97643=CARTESIAN_POINT('Ctrl Pts',(17.6836608334526,-10.2066412558964,-2.83569312779677));
#97644=CARTESIAN_POINT('Ctrl Pts',(17.8472177794713,-8.12643600848449,-6.77504806505468));
#97645=CARTESIAN_POINT('Ctrl Pts',(18.010577720969,-4.61555788199374,-9.50568575518433));
#97646=CARTESIAN_POINT('Ctrl Pts',(18.1737385767459,-0.296033859425129,
-10.5524578266823));
#97647=CARTESIAN_POINT('Ctrl Pts',(18.3367119961153,4.06252364851462,-9.72604612296011));
#97648=CARTESIAN_POINT('Ctrl Pts',(18.5266075658491,8.30676695663606,-6.7667072174541));
#97649=CARTESIAN_POINT('Ctrl Pts',(18.7433599818689,10.8434180575509,-1.2552796992343));
#97650=CARTESIAN_POINT('Ctrl Pts',(18.9866784786254,9.45215064511234,5.42117041791776));
#97651=CARTESIAN_POINT('Ctrl Pts',(19.2298169638985,4.37791280923335,9.9588947253312));
#97652=CARTESIAN_POINT('Ctrl Pts',(19.451862738617,-1.82076892763169,10.5392741564668));
#97653=CARTESIAN_POINT('Ctrl Pts',(19.6544197627791,-6.77058311285345,8.06270985402027));
#97654=CARTESIAN_POINT('Ctrl Pts',(19.8341212662609,-9.7059697419469,4.05833494626081));
#97655=CARTESIAN_POINT('Ctrl Pts',(20.0241128660578,-10.4716758765513,-0.858388280088311));
#97656=CARTESIAN_POINT('Ctrl Pts',(20.1410146593591,-8.90209080241453,-5.56525451310402));
#97657=CARTESIAN_POINT('Ctrl Pts',(20.2897362311998,-5.3492990423135,-9.02216707869922));
#97658=CARTESIAN_POINT('Ctrl Pts',(20.4228963780776,-0.610233353923302,
-10.4627269070358));
#97659=CARTESIAN_POINT('Ctrl Pts',(20.5635028431947,4.2573586450909,-9.56719051602513));
#97660=CARTESIAN_POINT('Ctrl Pts',(20.7003940395719,8.16743907076133,-6.53981610359476));
#97661=CARTESIAN_POINT('Ctrl Pts',(20.8388262275972,10.2500428497637,-2.05952756842641));
#97662=CARTESIAN_POINT('Ctrl Pts',(20.9764120894268,10.043725870545,2.87462578415665));
#97663=CARTESIAN_POINT('Ctrl Pts',(21.1142192325514,7.59769699822165,7.15633992564172));
#97664=CARTESIAN_POINT('Ctrl Pts',(21.2517597955772,3.46196734104235,9.84409234348526));
#97665=CARTESIAN_POINT('Ctrl Pts',(21.3893130359357,-1.44159676850522,10.3156356270535));
#97666=CARTESIAN_POINT('Ctrl Pts',(21.5266025241148,-6.01199771485613,8.52126837621254));
#97667=CARTESIAN_POINT('Ctrl Pts',(21.6640852851583,-9.24412410769275,4.75990666379241));
#97668=CARTESIAN_POINT('Ctrl Pts',(21.7552321039728,-10.0072228406033,1.65687208126127));
#97669=CARTESIAN_POINT('Ctrl Pts',(21.8012598463038,-10.0131352633455,0.0110692926695165));
#97670=CARTESIAN_POINT('',(0.,0.,0.));
#97671=CARTESIAN_POINT('Origin',(0.3,0.,0.));
#97672=CARTESIAN_POINT('',(0.,-5.66374651669668E-16,4.6248));
#97673=CARTESIAN_POINT('Origin',(0.,0.,0.));
#97674=CARTESIAN_POINT('',(0.3,-5.29635247695247E-16,4.3248));
#97675=CARTESIAN_POINT('Origin',(0.3,-5.66374651669668E-16,4.6248));
#97676=CARTESIAN_POINT('',(0.3,-4.3248,-5.29635247695247E-16));
#97677=CARTESIAN_POINT('Origin',(0.3,0.,0.));
#97678=CARTESIAN_POINT('Origin',(0.3,0.,0.));
#97679=CARTESIAN_POINT('Origin',(0.612,0.,0.));
#97680=CARTESIAN_POINT('',(0.924,-4.3248,-5.29635247695247E-16));
#97681=CARTESIAN_POINT('',(0.612,-4.3248,-5.29635247695247E-16));
#97682=CARTESIAN_POINT('',(0.924,-5.29635247695247E-16,4.3248));
#97683=CARTESIAN_POINT('Origin',(0.924,0.,0.));
#97684=CARTESIAN_POINT('Origin',(0.924,0.,0.));
#97685=CARTESIAN_POINT('Origin',(0.,11.832,0.));
#97686=CARTESIAN_POINT('',(0.,-1.41226268877673E-15,11.532));
#97687=CARTESIAN_POINT('Origin',(0.,0.,0.));
#97688=CARTESIAN_POINT('Origin',(0.924,0.,0.));
#97689=CARTESIAN_POINT('',(1.224,-5.66374651669668E-16,4.6248));
#97690=CARTESIAN_POINT('Origin',(0.924,-5.66374651669668E-16,4.6248));
#97691=CARTESIAN_POINT('Origin',(1.224,0.,0.));
#97692=CARTESIAN_POINT('Origin',(1.224,4.3248,0.));
#97693=CARTESIAN_POINT('',(1.224,-10.404,-1.27412252983291E-15));
#97694=CARTESIAN_POINT('Origin',(1.224,0.,0.));
#97695=CARTESIAN_POINT('Origin',(6.228,0.,0.));
#97696=CARTESIAN_POINT('',(6.228,-10.404,-1.27412252983291E-15));
#97697=CARTESIAN_POINT('',(6.228,-1.27412252983291E-15,10.404));
#97698=CARTESIAN_POINT('Origin',(6.228,0.,0.));
#97699=CARTESIAN_POINT('',(6.528,-1.31086193380733E-15,10.704));
#97700=CARTESIAN_POINT('Origin',(6.228,-1.31086193380733E-15,10.704));
#97701=CARTESIAN_POINT('Origin',(6.528,0.,0.));
#97702=CARTESIAN_POINT('Origin',(6.228,0.,0.));
#97703=CARTESIAN_POINT('Origin',(6.528,10.404,0.));
#97704=CARTESIAN_POINT('',(6.528,-1.33731430466891E-15,10.92));
#97705=CARTESIAN_POINT('Origin',(6.528,0.,0.));
#97706=CARTESIAN_POINT('Origin',(3.876,0.,0.));
#97707=CARTESIAN_POINT('',(3.876,-10.404,-1.27412252983291E-15));
#97708=CARTESIAN_POINT('Origin',(6.228,0.,0.));
#97709=CARTESIAN_POINT('',(6.228,-1.37405370864333E-15,11.22));
#97710=CARTESIAN_POINT('Origin',(6.228,-1.33731430466891E-15,10.92));
#97711=CARTESIAN_POINT('',(6.228,-11.22,-1.37405370864333E-15));
#97712=CARTESIAN_POINT('Origin',(6.228,0.,0.));
#97713=CARTESIAN_POINT('Origin',(6.228,0.,0.));
#97714=CARTESIAN_POINT('Origin',(3.876,0.,0.));
#97715=CARTESIAN_POINT('',(1.224,-11.22,-1.37405370864333E-15));
#97716=CARTESIAN_POINT('',(3.876,-11.22,-1.37405370864333E-15));
#97717=CARTESIAN_POINT('Origin',(1.224,0.,0.));
#97718=CARTESIAN_POINT('',(6.2016,2.04,11.0329869029198));
#97719=CARTESIAN_POINT('',(6.2016,-2.04,11.0329869029198));
#97720=CARTESIAN_POINT('Origin',(6.2016,0.,0.));
#97721=CARTESIAN_POINT('',(1.7952,-2.04,11.0329869029198));
#97722=CARTESIAN_POINT('',(3.876,-2.04,11.0329869029198));
#97723=CARTESIAN_POINT('',(1.7952,2.04,11.0329869029198));
#97724=CARTESIAN_POINT('Origin',(1.7952,0.,0.));
#97725=CARTESIAN_POINT('',(3.876,2.04,11.0329869029198));
#97726=CARTESIAN_POINT('Origin',(0.924,0.,0.));
#97727=CARTESIAN_POINT('',(1.224,-1.41226268877673E-15,11.532));
#97728=CARTESIAN_POINT('Origin',(1.224,0.,0.));
#97729=CARTESIAN_POINT('',(0.924,-1.44900209275115E-15,11.832));
#97730=CARTESIAN_POINT('Origin',(0.924,-1.41226268877673E-15,11.532));
#97731=CARTESIAN_POINT('',(0.924,-11.832,-1.44900209275115E-15));
#97732=CARTESIAN_POINT('Origin',(0.924,0.,0.));
#97733=CARTESIAN_POINT('Origin',(0.924,0.,0.));
#97734=CARTESIAN_POINT('Origin',(0.612,0.,0.));
#97735=CARTESIAN_POINT('',(0.3,-11.832,-1.44900209275115E-15));
#97736=CARTESIAN_POINT('',(0.612,-11.832,-1.44900209275115E-15));
#97737=CARTESIAN_POINT('',(0.3,-1.44900209275115E-15,11.832));
#97738=CARTESIAN_POINT('Origin',(0.3,0.,0.));
#97739=CARTESIAN_POINT('Origin',(0.3,0.,0.));
#97740=CARTESIAN_POINT('Origin',(1.224,11.22,0.));
#97741=CARTESIAN_POINT('Origin',(0.3,0.,0.));
#97742=CARTESIAN_POINT('Origin',(0.3,-1.41226268877673E-15,11.532));
#97743=CARTESIAN_POINT('Origin',(2.8968,-1.74,12.0216));
#97744=CARTESIAN_POINT('',(1.7952,-2.04,12.0216));
#97745=CARTESIAN_POINT('',(6.2016,-2.04,12.0216));
#97746=CARTESIAN_POINT('',(2.8968,-2.04,12.0216));
#97747=CARTESIAN_POINT('',(5.9016,-1.74,12.3216));
#97748=CARTESIAN_POINT('Origin',(5.9016,-1.74,12.0216));
#97749=CARTESIAN_POINT('',(2.0952,-1.74,12.3216));
#97750=CARTESIAN_POINT('',(2.8968,-1.74,12.3216));
#97751=CARTESIAN_POINT('Origin',(2.0952,-1.74,12.0216));
#97752=CARTESIAN_POINT('Origin',(5.9016,-2.04,12.0216));
#97753=CARTESIAN_POINT('',(5.9016,1.74,12.3216));
#97754=CARTESIAN_POINT('',(5.9016,-2.04,12.3216));
#97755=CARTESIAN_POINT('',(6.2016,2.04,12.0216));
#97756=CARTESIAN_POINT('',(6.2016,-2.04,12.0216));
#97757=CARTESIAN_POINT('Origin',(5.9016,1.74,12.0216));
#97758=CARTESIAN_POINT('Origin',(2.0952,-2.04,12.0216));
#97759=CARTESIAN_POINT('',(1.7952,2.04,12.0216));
#97760=CARTESIAN_POINT('',(1.7952,-2.04,12.0216));
#97761=CARTESIAN_POINT('',(2.0952,1.74,12.3216));
#97762=CARTESIAN_POINT('',(2.0952,-2.04,12.3216));
#97763=CARTESIAN_POINT('Origin',(2.0952,1.74,12.0216));
#97764=CARTESIAN_POINT('Origin',(2.8968,1.74,12.0216));
#97765=CARTESIAN_POINT('',(2.8968,2.04,12.0216));
#97766=CARTESIAN_POINT('',(2.8968,1.74,12.3216));
#97767=CARTESIAN_POINT('Origin',(6.2016,-2.04,12.3216));
#97768=CARTESIAN_POINT('',(6.2016,-2.04,10.8528));
#97769=CARTESIAN_POINT('',(6.2016,2.04,10.8528));
#97770=CARTESIAN_POINT('Origin',(3.9984,-2.04,11.5872));
#97771=CARTESIAN_POINT('',(1.7952,-2.04,12.3216));
#97772=CARTESIAN_POINT('Origin',(1.7952,-2.04,12.3216));
#97773=CARTESIAN_POINT('',(4.7328,-0.9792,12.3216));
#97774=CARTESIAN_POINT('',(3.264,-0.9792,12.3216));
#97775=CARTESIAN_POINT('',(3.264,-0.9792,12.3216));
#97776=CARTESIAN_POINT('',(3.264,0.9792,12.3216));
#97777=CARTESIAN_POINT('',(3.264,-1.5096,12.3216));
#97778=CARTESIAN_POINT('',(4.7328,0.9792,12.3216));
#97779=CARTESIAN_POINT('',(2.5296,0.9792,12.3216));
#97780=CARTESIAN_POINT('',(4.7328,-0.5304,12.3216));
#97781=CARTESIAN_POINT('Origin',(4.7328,-0.9792,12.3216));
#97782=CARTESIAN_POINT('',(4.7328,-0.9792,11.2608));
#97783=CARTESIAN_POINT('',(4.7328,-0.9792,12.3216));
#97784=CARTESIAN_POINT('',(3.264,-0.9792,11.2608));
#97785=CARTESIAN_POINT('',(3.264,-0.9792,11.2608));
#97786=CARTESIAN_POINT('',(3.264,-0.9792,12.3216));
#97787=CARTESIAN_POINT('Origin',(4.7328,0.9792,12.3216));
#97788=CARTESIAN_POINT('',(4.7328,0.9792,11.2608));
#97789=CARTESIAN_POINT('',(4.7328,0.9792,12.3216));
#97790=CARTESIAN_POINT('',(4.7328,-0.9792,11.2608));
#97791=CARTESIAN_POINT('Origin',(3.264,0.9792,12.3216));
#97792=CARTESIAN_POINT('',(3.264,0.9792,11.2608));
#97793=CARTESIAN_POINT('',(3.264,0.9792,12.3216));
#97794=CARTESIAN_POINT('',(4.7328,0.9792,11.2608));
#97795=CARTESIAN_POINT('Origin',(3.264,-0.9792,12.3216));
#97796=CARTESIAN_POINT('',(3.264,0.9792,11.2608));
#97797=CARTESIAN_POINT('Origin',(3.9984,0.,11.2608));
#97798=CARTESIAN_POINT('Origin',(1.7952,-2.04,10.8528));
#97799=CARTESIAN_POINT('',(1.7952,2.04,12.3216));
#97800=CARTESIAN_POINT('Origin',(3.9984,2.04,11.5872));
#97801=CARTESIAN_POINT('',(0.,0.,0.));
#97802=CARTESIAN_POINT('Origin',(12.348,-1.428,45.396));
#97803=CARTESIAN_POINT('',(12.648,0.924,45.396));
#97804=CARTESIAN_POINT('',(12.348,0.924,45.696));
#97805=CARTESIAN_POINT('Origin',(12.348,0.924,45.396));
#97806=CARTESIAN_POINT('',(12.348,0.708,45.696));
#97807=CARTESIAN_POINT('',(12.348,-1.428,45.696));
#97808=CARTESIAN_POINT('',(12.648,0.708,45.396));
#97809=CARTESIAN_POINT('Origin',(12.348,0.708,45.396));
#97810=CARTESIAN_POINT('',(12.648,-1.428,45.396));
#97811=CARTESIAN_POINT('Origin',(0.,0.708,45.396));
#97812=CARTESIAN_POINT('',(-12.348,0.708,45.696));
#97813=CARTESIAN_POINT('',(-12.348,0.408,45.396));
#97814=CARTESIAN_POINT('Origin',(-12.348,0.708,45.396));
#97815=CARTESIAN_POINT('',(12.348,0.408,45.396));
#97816=CARTESIAN_POINT('',(0.,0.408,45.396));
#97817=CARTESIAN_POINT('Origin',(12.348,0.708,45.396));
#97818=CARTESIAN_POINT('',(0.,0.708,45.696));
#97819=CARTESIAN_POINT('Origin',(-12.348,-1.428,45.396));
#97820=CARTESIAN_POINT('',(-12.648,0.708,45.396));
#97821=CARTESIAN_POINT('Origin',(-12.348,0.708,45.396));
#97822=CARTESIAN_POINT('',(-12.348,0.924,45.696));
#97823=CARTESIAN_POINT('',(-12.348,-1.428,45.696));
#97824=CARTESIAN_POINT('',(-12.648,0.924,45.396));
#97825=CARTESIAN_POINT('Origin',(-12.348,0.924,45.396));
#97826=CARTESIAN_POINT('',(-12.648,-1.428,45.396));
#97827=CARTESIAN_POINT('Origin',(0.,0.924,45.396));
#97828=CARTESIAN_POINT('',(12.348,1.224,45.396));
#97829=CARTESIAN_POINT('Origin',(12.348,0.924,45.396));
#97830=CARTESIAN_POINT('',(-12.348,1.224,45.396));
#97831=CARTESIAN_POINT('',(0.,1.224,45.396));
#97832=CARTESIAN_POINT('Origin',(-12.348,0.924,45.396));
#97833=CARTESIAN_POINT('',(0.,0.924,45.696));
#97834=CARTESIAN_POINT('Origin',(-12.348,0.924,45.396));
#97835=CARTESIAN_POINT('Origin',(-12.348,0.924,45.396));
#97836=CARTESIAN_POINT('Origin',(-12.348,0.708,45.396));
#97837=CARTESIAN_POINT('Origin',(-12.348,0.708,45.396));
#97838=CARTESIAN_POINT('Origin',(12.348,0.708,45.396));
#97839=CARTESIAN_POINT('Origin',(12.348,0.708,45.396));
#97840=CARTESIAN_POINT('Origin',(12.348,0.924,45.396));
#97841=CARTESIAN_POINT('Origin',(12.348,0.924,45.396));
#97842=CARTESIAN_POINT('Origin',(-12.348,0.708,43.86));
#97843=CARTESIAN_POINT('',(-12.648,0.708,42.0374493210098));
#97844=CARTESIAN_POINT('',(-12.648,0.708,43.86));
#97845=CARTESIAN_POINT('',(-12.348,0.408,42.0374493210099));
#97846=CARTESIAN_POINT('Origin',(-12.348,0.708,42.0374493210099));
#97847=CARTESIAN_POINT('',(-12.348,0.408,43.86));
#97848=CARTESIAN_POINT('Origin',(-12.648,-4.08,42.024));
#97849=CARTESIAN_POINT('',(-12.648,0.924000000000001,42.0374493210099));
#97850=CARTESIAN_POINT('',(-12.648,0.924,26.4792));
#97851=CARTESIAN_POINT('',(-12.648,0.708,42.03744932101));
#97852=CARTESIAN_POINT('Origin',(-12.348,0.924,26.4792));
#97853=CARTESIAN_POINT('',(-12.348,1.224,42.0374493210099));
#97854=CARTESIAN_POINT('',(-12.348,1.224,26.4792));
#97855=CARTESIAN_POINT('Origin',(-12.348,0.924,42.0374493210099));
#97856=CARTESIAN_POINT('Origin',(0.,1.224,10.9344));
#97857=CARTESIAN_POINT('',(12.348,1.224,42.0374493210129));
#97858=CARTESIAN_POINT('',(12.348,1.224,28.3152));
#97859=CARTESIAN_POINT('',(7.98599766308269,1.224,11.2854385811275));
#97860=CARTESIAN_POINT('Ctrl Pts',(7.98599766308269,1.224,11.2854385811275));
#97861=CARTESIAN_POINT('Ctrl Pts',(8.26166260011058,1.224,12.0417095524849));
#97862=CARTESIAN_POINT('Ctrl Pts',(8.80736065451927,1.224,13.5673576300013));
#97863=CARTESIAN_POINT('Ctrl Pts',(9.7934853134899,1.224,16.6303022412252));
#97864=CARTESIAN_POINT('Ctrl Pts',(10.8098927869894,1.224,19.6660154770441));
#97865=CARTESIAN_POINT('Ctrl Pts',(11.7490851570277,1.224,22.7510694457356));
#97866=CARTESIAN_POINT('Ctrl Pts',(12.3879445445635,1.224,25.0858368018936));
#97867=CARTESIAN_POINT('Ctrl Pts',(12.9162393467085,1.224,27.0283271988516));
#97868=CARTESIAN_POINT('Ctrl Pts',(13.318072367284,1.224,28.3480811193172));
#97869=CARTESIAN_POINT('Ctrl Pts',(13.5413604393248,1.224,29.0034673861264));
#97870=CARTESIAN_POINT('Ctrl Pts',(13.6793149470157,1.224,29.3805129744774));
#97871=CARTESIAN_POINT('Ctrl Pts',(13.8956419055917,1.224,29.9480318039803));
#97872=CARTESIAN_POINT('Ctrl Pts',(14.1903040593961,1.224,30.6134675776983));
#97873=CARTESIAN_POINT('Ctrl Pts',(14.5193620015612,1.224,31.3678458791788));
#97874=CARTESIAN_POINT('Ctrl Pts',(14.711967368694,1.224,31.9396546207724));
#97875=CARTESIAN_POINT('Ctrl Pts',(14.7690013588176,1.224,32.5519725397467));
#97876=CARTESIAN_POINT('Ctrl Pts',(14.5616693526593,1.224,33.1335095406623));
#97877=CARTESIAN_POINT('Ctrl Pts',(14.1770509140562,1.224,33.6045046700376));
#97878=CARTESIAN_POINT('Ctrl Pts',(13.5570600775614,1.224,34.1220294622509));
#97879=CARTESIAN_POINT('Ctrl Pts',(12.6963985226976,1.224,34.6417186073242));
#97880=CARTESIAN_POINT('Ctrl Pts',(11.6986604523811,1.224,35.333270779735));
#97881=CARTESIAN_POINT('Ctrl Pts',(10.9714653585921,1.224,36.3268151158983));
#97882=CARTESIAN_POINT('Ctrl Pts',(10.704924469272,1.224,37.5319055503386));
#97883=CARTESIAN_POINT('Ctrl Pts',(10.8999667707481,1.224,38.7410381732305));
#97884=CARTESIAN_POINT('Ctrl Pts',(11.4452668024532,1.224,39.8274946497674));
#97885=CARTESIAN_POINT('Ctrl Pts',(12.0610698910061,1.224,40.8549578815901));
#97886=CARTESIAN_POINT('Ctrl Pts',(12.3110725606623,1.224,41.6363966051383));
#97887=CARTESIAN_POINT('Ctrl Pts',(12.348,1.224,42.0374493210131));
#97888=CARTESIAN_POINT('',(-7.98599766308436,1.224,11.2854385811275));
#97889=CARTESIAN_POINT('',(0.,1.224,11.2854385811275));
#97890=CARTESIAN_POINT('Ctrl Pts',(-12.348,1.224,42.03744932101));
#97891=CARTESIAN_POINT('Ctrl Pts',(-12.3110725606702,1.224,41.6363966051328));
#97892=CARTESIAN_POINT('Ctrl Pts',(-12.0609852952635,1.224,40.8549204601091));
#97893=CARTESIAN_POINT('Ctrl Pts',(-11.4450821737987,1.224,39.8274092249604));
#97894=CARTESIAN_POINT('Ctrl Pts',(-10.8997688026688,1.224,38.7409075676707));
#97895=CARTESIAN_POINT('Ctrl Pts',(-10.7043533514793,1.224,37.5315890187733));
#97896=CARTESIAN_POINT('Ctrl Pts',(-10.9709851394883,1.224,36.3263525491271));
#97897=CARTESIAN_POINT('Ctrl Pts',(-11.6986135266186,1.224,35.3339416136743));
#97898=CARTESIAN_POINT('Ctrl Pts',(-12.5309171577631,1.224,34.7574741120408));
#97899=CARTESIAN_POINT('Ctrl Pts',(-13.2114636130569,1.224,34.3298336160849));
#97900=CARTESIAN_POINT('Ctrl Pts',(-13.7131082734894,1.224,33.9932968374398));
#97901=CARTESIAN_POINT('Ctrl Pts',(-14.1769757204202,1.224,33.6048339401135));
#97902=CARTESIAN_POINT('Ctrl Pts',(-14.5620228329377,1.224,33.1340383684088));
#97903=CARTESIAN_POINT('Ctrl Pts',(-14.7683961662382,1.224,32.5514380647304));
#97904=CARTESIAN_POINT('Ctrl Pts',(-14.711659402932,1.224,31.939868704061));
#97905=CARTESIAN_POINT('Ctrl Pts',(-14.5189773065471,1.224,31.3678083420515));
#97906=CARTESIAN_POINT('Ctrl Pts',(-14.1888423807734,1.224,30.613847819264));
#97907=CARTESIAN_POINT('Ctrl Pts',(-13.6063457415431,1.224,29.2804450588471));
#97908=CARTESIAN_POINT('Ctrl Pts',(-13.0245909094872,1.224,27.4180026826501));
#97909=CARTESIAN_POINT('Ctrl Pts',(-12.3871316955906,1.224,25.0852094102837));
#97910=CARTESIAN_POINT('Ctrl Pts',(-11.7493811375928,1.224,22.7517028806517));
#97911=CARTESIAN_POINT('Ctrl Pts',(-10.8084555662763,1.224,19.6656582368069));
#97912=CARTESIAN_POINT('Ctrl Pts',(-9.79376320963301,1.224,16.6304717567395));
#97913=CARTESIAN_POINT('Ctrl Pts',(-8.80744652629141,1.224,13.5670274338247));
#97914=CARTESIAN_POINT('Ctrl Pts',(-8.26166260011136,1.224,12.0417095524852));
#97915=CARTESIAN_POINT('Ctrl Pts',(-7.98599766308436,1.224,11.2854385811275));
#97916=CARTESIAN_POINT('',(6.528,1.224,44.032));
#97917=CARTESIAN_POINT('Origin',(6.528,1.224,42.432));
#97918=CARTESIAN_POINT('',(-6.528,1.224,44.032));
#97919=CARTESIAN_POINT('Origin',(-6.528,1.224,42.432));
#97920=CARTESIAN_POINT('Origin',(0.,1.224,45.696));
#97921=CARTESIAN_POINT('Origin',(12.348,0.924,28.3152));
#97922=CARTESIAN_POINT('',(12.648,0.924,42.0374493210128));
#97923=CARTESIAN_POINT('',(12.648,0.924,28.3152));
#97924=CARTESIAN_POINT('Origin',(12.348,0.924,42.0374493210129));
#97925=CARTESIAN_POINT('Origin',(12.3479078516757,0.708,42.0374535543961));
#97926=CARTESIAN_POINT('',(12.646736323466,0.924,42.009942793751));
#97927=CARTESIAN_POINT('Origin',(12.348,0.924,42.037449321013));
#97928=CARTESIAN_POINT('',(12.648,0.708,42.0374493210129));
#97929=CARTESIAN_POINT('',(12.648,0.924,42.037449321013));
#97930=CARTESIAN_POINT('',(12.646736323466,0.708000000000001,42.009942793751));
#97931=CARTESIAN_POINT('Origin',(12.348,0.708,42.037449321013));
#97932=CARTESIAN_POINT('',(12.646736323466,0.708,42.0099427937509));
#97933=CARTESIAN_POINT('Origin',(12.348,0.924,42.037449321013));
#97934=CARTESIAN_POINT('Origin',(12.348,0.924,42.037449321013));
#97935=CARTESIAN_POINT('Origin',(12.348,0.708,45.696));
#97936=CARTESIAN_POINT('',(12.348,0.408,42.0374493210129));
#97937=CARTESIAN_POINT('',(12.348,0.408,45.696));
#97938=CARTESIAN_POINT('Origin',(12.348,0.708,42.0374493210129));
#97939=CARTESIAN_POINT('',(12.648,0.708,45.696));
#97940=CARTESIAN_POINT('Origin',(12.348,0.708,42.037449321013));
#97941=CARTESIAN_POINT('Origin',(12.348,0.708,42.037449321013));
#97942=CARTESIAN_POINT('Ctrl Pts',(7.98599766308269,1.224,11.2854385811275));
#97943=CARTESIAN_POINT('Ctrl Pts',(8.26166260011058,1.224,12.0417095524849));
#97944=CARTESIAN_POINT('Ctrl Pts',(8.80736065451927,1.224,13.5673576300013));
#97945=CARTESIAN_POINT('Ctrl Pts',(9.7934853134899,1.224,16.6303022412252));
#97946=CARTESIAN_POINT('Ctrl Pts',(10.8098927869894,1.224,19.6660154770441));
#97947=CARTESIAN_POINT('Ctrl Pts',(11.7490851570277,1.224,22.7510694457356));
#97948=CARTESIAN_POINT('Ctrl Pts',(12.3879445445635,1.224,25.0858368018936));
#97949=CARTESIAN_POINT('Ctrl Pts',(12.9162393467085,1.224,27.0283271988516));
#97950=CARTESIAN_POINT('Ctrl Pts',(13.318072367284,1.224,28.3480811193172));
#97951=CARTESIAN_POINT('Ctrl Pts',(13.5413604393248,1.224,29.0034673861264));
#97952=CARTESIAN_POINT('Ctrl Pts',(13.6793149470157,1.224,29.3805129744774));
#97953=CARTESIAN_POINT('Ctrl Pts',(13.8956419055917,1.224,29.9480318039803));
#97954=CARTESIAN_POINT('Ctrl Pts',(14.1903040593961,1.224,30.6134675776983));
#97955=CARTESIAN_POINT('Ctrl Pts',(14.5193620015612,1.224,31.3678458791788));
#97956=CARTESIAN_POINT('Ctrl Pts',(14.711967368694,1.224,31.9396546207724));
#97957=CARTESIAN_POINT('Ctrl Pts',(14.7690013588176,1.224,32.5519725397467));
#97958=CARTESIAN_POINT('Ctrl Pts',(14.5616693526593,1.224,33.1335095406623));
#97959=CARTESIAN_POINT('Ctrl Pts',(14.1770509140562,1.224,33.6045046700376));
#97960=CARTESIAN_POINT('Ctrl Pts',(13.5570600775614,1.224,34.1220294622509));
#97961=CARTESIAN_POINT('Ctrl Pts',(12.6963985226976,1.224,34.6417186073242));
#97962=CARTESIAN_POINT('Ctrl Pts',(11.6986604523811,1.224,35.333270779735));
#97963=CARTESIAN_POINT('Ctrl Pts',(10.9714653585921,1.224,36.3268151158983));
#97964=CARTESIAN_POINT('Ctrl Pts',(10.704924469272,1.224,37.5319055503386));
#97965=CARTESIAN_POINT('Ctrl Pts',(10.8999667707481,1.224,38.7410381732305));
#97966=CARTESIAN_POINT('Ctrl Pts',(11.4452668024532,1.224,39.8274946497674));
#97967=CARTESIAN_POINT('Ctrl Pts',(12.0610698910061,1.224,40.8549578815901));
#97968=CARTESIAN_POINT('Ctrl Pts',(12.3110725606623,1.224,41.6363966051383));
#97969=CARTESIAN_POINT('Ctrl Pts',(12.348,1.224,42.0374493210131));
#97970=CARTESIAN_POINT('Ctrl Pts',(8.05978824615337,1.224,11.2585415069228));
#97971=CARTESIAN_POINT('Ctrl Pts',(8.33546863203364,1.224,12.0148310799991));
#97972=CARTESIAN_POINT('Ctrl Pts',(8.88191390907659,1.224,13.5426216579679));
#97973=CARTESIAN_POINT('Ctrl Pts',(9.86823614904903,1.224,16.6062333317922));
#97974=CARTESIAN_POINT('Ctrl Pts',(10.8843947824238,1.224,19.6411006535636));
#97975=CARTESIAN_POINT('Ctrl Pts',(11.8246493128098,1.224,22.7295876128389));
#97976=CARTESIAN_POINT('Ctrl Pts',(12.4637767343052,1.224,25.0654345278681));
#97977=CARTESIAN_POINT('Ctrl Pts',(12.9919022546425,1.224,27.0072148023256));
#97978=CARTESIAN_POINT('Ctrl Pts',(13.39292056091,1.224,28.3242302479708));
#97979=CARTESIAN_POINT('Ctrl Pts',(13.6154785859392,1.224,28.9774817878985));
#97980=CARTESIAN_POINT('Ctrl Pts',(13.7528646368703,1.224,29.3529231195986));
#97981=CARTESIAN_POINT('Ctrl Pts',(13.9683464603798,1.224,29.918401670249));
#97982=CARTESIAN_POINT('Ctrl Pts',(14.2615438634277,1.224,30.5801122589648));
#97983=CARTESIAN_POINT('Ctrl Pts',(14.5921672247916,1.224,31.3385970564082));
#97984=CARTESIAN_POINT('Ctrl Pts',(14.7888026951731,1.224,31.9199846429038));
#97985=CARTESIAN_POINT('Ctrl Pts',(14.8496195982487,1.224,32.5610656869859));
#97986=CARTESIAN_POINT('Ctrl Pts',(14.6302688785353,1.224,33.1755044896258));
#97987=CARTESIAN_POINT('Ctrl Pts',(14.2320817324303,1.224,33.6607769671911));
#97988=CARTESIAN_POINT('Ctrl Pts',(13.6008246044553,1.224,34.1879453054762));
#97989=CARTESIAN_POINT('Ctrl Pts',(12.7358933411632,1.224,34.7091332477064));
#97990=CARTESIAN_POINT('Ctrl Pts',(11.7523239260966,1.224,35.3928958840521));
#97991=CARTESIAN_POINT('Ctrl Pts',(11.0455333850698,1.224,36.3596210864882));
#97992=CARTESIAN_POINT('Ctrl Pts',(10.7852936168046,1.224,37.5340147061541));
#97993=CARTESIAN_POINT('Ctrl Pts',(10.9753230697622,1.224,38.7144559876328));
#97994=CARTESIAN_POINT('Ctrl Pts',(11.5120188762668,1.224,39.7864283699758));
#97995=CARTESIAN_POINT('Ctrl Pts',(12.1314071774355,1.224,40.8188642924511));
#97996=CARTESIAN_POINT('Ctrl Pts',(12.3884534787586,1.224,41.6182742012834));
#97997=CARTESIAN_POINT('Ctrl Pts',(12.4262089865968,1.224,42.0302481290154));
#97998=CARTESIAN_POINT('Ctrl Pts',(8.20673516090132,1.15894437659295,11.2049785466419));
#97999=CARTESIAN_POINT('Ctrl Pts',(8.48246583853968,1.15894437659295,11.9614138362237));
#98000=CARTESIAN_POINT('Ctrl Pts',(9.03031785403706,1.15894437659295,13.493174874988));
#98001=CARTESIAN_POINT('Ctrl Pts',(10.0171159532212,1.15894437659295,16.5583667565347));
#98002=CARTESIAN_POINT('Ctrl Pts',(11.032807640009,1.15894437659295,19.5916239397643));
#98003=CARTESIAN_POINT('Ctrl Pts',(11.9750949600252,1.15894437659295,22.6867145384626));
#98004=CARTESIAN_POINT('Ctrl Pts',(12.6148189226952,1.15894437659295,25.0249062630847));
#98005=CARTESIAN_POINT('Ctrl Pts',(13.1425604647687,1.15894437659295,26.9651479861995));
#98006=CARTESIAN_POINT('Ctrl Pts',(13.5419982523509,1.15894437659294,28.276870675056));
#98007=CARTESIAN_POINT('Ctrl Pts',(13.7630823643497,1.15894437659294,28.9257801857052));
#98008=CARTESIAN_POINT('Ctrl Pts',(13.8993694172056,1.15894437659294,29.2982183234201));
#98009=CARTESIAN_POINT('Ctrl Pts',(14.1130820755258,1.15894437659295,29.8590949099225));
#98010=CARTESIAN_POINT('Ctrl Pts',(14.4033529215945,1.15894437659295,30.5138988935207));
#98011=CARTESIAN_POINT('Ctrl Pts',(14.7371296392622,1.15894437659295,31.27998110634));
#98012=CARTESIAN_POINT('Ctrl Pts',(14.941677315901,1.15894437659295,31.8806320069506));
#98013=CARTESIAN_POINT('Ctrl Pts',(15.0102531276634,1.15894437659295,32.5790650964589));
#98014=CARTESIAN_POINT('Ctrl Pts',(14.7668033293489,1.15894437659295,33.2588822083198));
#98015=CARTESIAN_POINT('Ctrl Pts',(14.3419892667217,1.15894437659295,33.772786749341));
#98016=CARTESIAN_POINT('Ctrl Pts',(13.687845201664,1.15894437659295,34.3192421394686));
#98017=CARTESIAN_POINT('Ctrl Pts',(12.814864656712,1.15894437659295,34.8436494734496));
#98018=CARTESIAN_POINT('Ctrl Pts',(11.8591318733617,1.15894437659295,35.5117504800206));
#98019=CARTESIAN_POINT('Ctrl Pts',(11.192774610864,1.15894437659295,36.4248976115355));
#98020=CARTESIAN_POINT('Ctrl Pts',(10.945224692698,1.15894437659295,37.5383568976139));
#98021=CARTESIAN_POINT('Ctrl Pts',(11.1252475782242,1.15894437659295,38.6613956307185));
#98022=CARTESIAN_POINT('Ctrl Pts',(11.6448524105777,1.15894437659295,39.7049780164935));
#98023=CARTESIAN_POINT('Ctrl Pts',(12.2714401993632,1.15894437659295,40.7466056673881));
#98024=CARTESIAN_POINT('Ctrl Pts',(12.5422016913503,1.15894437659295,41.582867190141));
#98025=CARTESIAN_POINT('Ctrl Pts',(12.5819547309413,1.15894437659295,42.0159076413469));
#98026=CARTESIAN_POINT('Ctrl Pts',(8.26785692826664,1.00253981633974,11.1826993255823));
#98027=CARTESIAN_POINT('Ctrl Pts',(8.543613066273,1.00253981633974,11.9392205016025));
#98028=CARTESIAN_POINT('Ctrl Pts',(9.09203130090063,1.00253981633974,13.4725641556529));
#98029=CARTESIAN_POINT('Ctrl Pts',(10.0790464956501,1.00253981633974,16.5384718863773));
#98030=CARTESIAN_POINT('Ctrl Pts',(11.0945506094751,1.00253981633974,19.5710766504504));
#98031=CARTESIAN_POINT('Ctrl Pts',(12.0376642913239,1.00253981633974,22.6688598415768));
#98032=CARTESIAN_POINT('Ctrl Pts',(12.677650983484,1.00253981633974,25.00807222563));
#98033=CARTESIAN_POINT('Ctrl Pts',(13.2052219103856,1.00253981633974,26.9476450599348));
#98034=CARTESIAN_POINT('Ctrl Pts',(13.6040120371276,1.00253981633974,28.2572036225122));
#98035=CARTESIAN_POINT('Ctrl Pts',(13.8244784093479,1.00253981633974,28.9042859415608));
#98036=CARTESIAN_POINT('Ctrl Pts',(13.9603160223219,1.00253981633974,29.2755194655201));
#98037=CARTESIAN_POINT('Ctrl Pts',(14.1732727660916,1.00253981633974,29.8343565362973));
#98038=CARTESIAN_POINT('Ctrl Pts',(14.4623240833064,1.00253981633974,30.4864067831395));
#98039=CARTESIAN_POINT('Ctrl Pts',(14.7974207893837,1.00253981633974,31.2555141309736));
#98040=CARTESIAN_POINT('Ctrl Pts',(15.0052331383414,1.00253981633974,31.8642212193198));
#98041=CARTESIAN_POINT('Ctrl Pts',(15.0770886981136,1.00253981633974,32.586526563643));
#98042=CARTESIAN_POINT('Ctrl Pts',(14.8235766521624,1.00253981633974,33.2935042835916));
#98043=CARTESIAN_POINT('Ctrl Pts',(14.3877788802376,1.00253981633974,33.8193647133348));
#98044=CARTESIAN_POINT('Ctrl Pts',(13.7240101751605,1.00253981633974,34.3738617173899));
#98045=CARTESIAN_POINT('Ctrl Pts',(12.8477870409378,1.00253981633974,34.8996627244856));
#98046=CARTESIAN_POINT('Ctrl Pts',(11.9035446247143,1.00253981633974,35.5612145865672));
#98047=CARTESIAN_POINT('Ctrl Pts',(11.2539587421444,1.00253981633974,36.4520365963864));
#98048=CARTESIAN_POINT('Ctrl Pts',(11.0117200719654,1.00253981633974,37.5401960385209));
#98049=CARTESIAN_POINT('Ctrl Pts',(11.1875752081005,1.00253981633975,38.6392965146994));
#98050=CARTESIAN_POINT('Ctrl Pts',(11.7000812655187,1.00253981633974,39.6711757625401));
#98051=CARTESIAN_POINT('Ctrl Pts',(12.3296775691092,1.00253981633975,40.7164613105102));
#98052=CARTESIAN_POINT('Ctrl Pts',(12.6060713603057,1.00253981633974,41.5682984715638));
#98053=CARTESIAN_POINT('Ctrl Pts',(12.646736323466,1.00253981633974,42.0099427937509));
#98054=CARTESIAN_POINT('Ctrl Pts',(8.26785692826664,0.923999999999997,11.1826993255823));
#98055=CARTESIAN_POINT('Ctrl Pts',(8.543613066273,0.923999999999997,11.9392205016025));
#98056=CARTESIAN_POINT('Ctrl Pts',(9.09203130090063,0.924,13.4725641556529));
#98057=CARTESIAN_POINT('Ctrl Pts',(10.0790464956501,0.923999999999999,16.5384718863773));
#98058=CARTESIAN_POINT('Ctrl Pts',(11.0945506094751,0.924,19.5710766504504));
#98059=CARTESIAN_POINT('Ctrl Pts',(12.0376642913239,0.924,22.6688598415768));
#98060=CARTESIAN_POINT('Ctrl Pts',(12.677650983484,0.924,25.00807222563));
#98061=CARTESIAN_POINT('Ctrl Pts',(13.2052219103856,0.923999999999999,26.9476450599348));
#98062=CARTESIAN_POINT('Ctrl Pts',(13.6040120371276,0.923999999999998,28.2572036225122));
#98063=CARTESIAN_POINT('Ctrl Pts',(13.8244784093479,0.923999999999997,28.9042859415608));
#98064=CARTESIAN_POINT('Ctrl Pts',(13.9603160223219,0.923999999999998,29.2755194655201));
#98065=CARTESIAN_POINT('Ctrl Pts',(14.1732727660916,0.923999999999998,29.8343565362973));
#98066=CARTESIAN_POINT('Ctrl Pts',(14.4623240833064,0.923999999999999,30.4864067831395));
#98067=CARTESIAN_POINT('Ctrl Pts',(14.7974207893837,0.923999999999999,31.2555141309736));
#98068=CARTESIAN_POINT('Ctrl Pts',(15.0052331383414,0.923999999999999,31.8642212193198));
#98069=CARTESIAN_POINT('Ctrl Pts',(15.0770886981136,0.923999999999999,32.586526563643));
#98070=CARTESIAN_POINT('Ctrl Pts',(14.8235766521624,0.924,33.2935042835916));
#98071=CARTESIAN_POINT('Ctrl Pts',(14.3877788802376,0.924,33.8193647133348));
#98072=CARTESIAN_POINT('Ctrl Pts',(13.7240101751605,0.924,34.3738617173899));
#98073=CARTESIAN_POINT('Ctrl Pts',(12.8477870409378,0.924,34.8996627244856));
#98074=CARTESIAN_POINT('Ctrl Pts',(11.9035446247143,0.924,35.5612145865672));
#98075=CARTESIAN_POINT('Ctrl Pts',(11.2539587421444,0.924,36.4520365963864));
#98076=CARTESIAN_POINT('Ctrl Pts',(11.0117200719654,0.924,37.5401960385209));
#98077=CARTESIAN_POINT('Ctrl Pts',(11.1875752081005,0.924,38.6392965146994));
#98078=CARTESIAN_POINT('Ctrl Pts',(11.7000812655187,0.924,39.6711757625401));
#98079=CARTESIAN_POINT('Ctrl Pts',(12.3296775691092,0.924,40.7164613105102));
#98080=CARTESIAN_POINT('Ctrl Pts',(12.6060713603057,0.924,41.5682984715638));
#98081=CARTESIAN_POINT('Ctrl Pts',(12.646736323466,0.924,42.0099427937509));
#98082=CARTESIAN_POINT('',(8.26785692826664,0.924,11.1826993255823));
#98083=CARTESIAN_POINT('Ctrl Pts',(12.646736323466,0.924,42.0099427937509));
#98084=CARTESIAN_POINT('Ctrl Pts',(12.6060713603057,0.924,41.5682984715638));
#98085=CARTESIAN_POINT('Ctrl Pts',(12.3296775691092,0.924,40.7164613105102));
#98086=CARTESIAN_POINT('Ctrl Pts',(11.7000812655187,0.924,39.6711757625401));
#98087=CARTESIAN_POINT('Ctrl Pts',(11.1875752081005,0.924,38.6392965146994));
#98088=CARTESIAN_POINT('Ctrl Pts',(11.0117200719654,0.924,37.5401960385209));
#98089=CARTESIAN_POINT('Ctrl Pts',(11.2539587421444,0.924,36.4520365963864));
#98090=CARTESIAN_POINT('Ctrl Pts',(11.9035446247143,0.924,35.5612145865672));
#98091=CARTESIAN_POINT('Ctrl Pts',(12.8477870409378,0.924,34.8996627244856));
#98092=CARTESIAN_POINT('Ctrl Pts',(13.7240101751605,0.924,34.3738617173899));
#98093=CARTESIAN_POINT('Ctrl Pts',(14.3877788802376,0.924,33.8193647133348));
#98094=CARTESIAN_POINT('Ctrl Pts',(14.8235766521624,0.924,33.2935042835916));
#98095=CARTESIAN_POINT('Ctrl Pts',(15.0770886981136,0.923999999999999,32.586526563643));
#98096=CARTESIAN_POINT('Ctrl Pts',(15.0052331383414,0.923999999999999,31.8642212193198));
#98097=CARTESIAN_POINT('Ctrl Pts',(14.7974207893837,0.923999999999999,31.2555141309736));
#98098=CARTESIAN_POINT('Ctrl Pts',(14.4623240833064,0.923999999999999,30.4864067831395));
#98099=CARTESIAN_POINT('Ctrl Pts',(14.1732727660916,0.923999999999998,29.8343565362973));
#98100=CARTESIAN_POINT('Ctrl Pts',(13.9603160223219,0.923999999999998,29.2755194655201));
#98101=CARTESIAN_POINT('Ctrl Pts',(13.8244784093479,0.923999999999997,28.9042859415608));
#98102=CARTESIAN_POINT('Ctrl Pts',(13.6040120371276,0.923999999999998,28.2572036225122));
#98103=CARTESIAN_POINT('Ctrl Pts',(13.2052219103856,0.923999999999999,26.9476450599348));
#98104=CARTESIAN_POINT('Ctrl Pts',(12.677650983484,0.924,25.00807222563));
#98105=CARTESIAN_POINT('Ctrl Pts',(12.0376642913239,0.924,22.6688598415768));
#98106=CARTESIAN_POINT('Ctrl Pts',(11.0945506094751,0.924,19.5710766504504));
#98107=CARTESIAN_POINT('Ctrl Pts',(10.0790464956501,0.923999999999999,16.5384718863773));
#98108=CARTESIAN_POINT('Ctrl Pts',(9.09203130090063,0.924,13.4725641556529));
#98109=CARTESIAN_POINT('Ctrl Pts',(8.543613066273,0.923999999999997,11.9392205016025));
#98110=CARTESIAN_POINT('Ctrl Pts',(8.26785692826664,0.923999999999997,11.1826993255823));
#98111=CARTESIAN_POINT('Origin',(7.98599766308269,0.924,11.2854385811275));
#98112=CARTESIAN_POINT('Ctrl Pts',(12.648,-4.08,42.024));
#98113=CARTESIAN_POINT('Ctrl Pts',(12.648,10.608,42.024));
#98114=CARTESIAN_POINT('Ctrl Pts',(12.641053196814,-4.08,41.9448017311235));
#98115=CARTESIAN_POINT('Ctrl Pts',(12.641053196814,10.608,41.9448017311235));
#98116=CARTESIAN_POINT('Ctrl Pts',(12.6222832973035,-4.08,41.7862967053182));
#98117=CARTESIAN_POINT('Ctrl Pts',(12.6222832973035,10.608,41.7862967053182));
#98118=CARTESIAN_POINT('Ctrl Pts',(12.5795001090523,-4.08,41.5482135599818));
#98119=CARTESIAN_POINT('Ctrl Pts',(12.5795001090523,10.608,41.5482135599818));
#98120=CARTESIAN_POINT('Ctrl Pts',(12.4931832123772,-4.08,41.2301191386837));
#98121=CARTESIAN_POINT('Ctrl Pts',(12.4931832123772,10.608,41.2301191386837));
#98122=CARTESIAN_POINT('Ctrl Pts',(12.3384198670333,-4.08,40.8311101407486));
#98123=CARTESIAN_POINT('Ctrl Pts',(12.3384198670333,10.608,40.8311101407486));
#98124=CARTESIAN_POINT('Ctrl Pts',(12.1425787135413,-4.08,40.4298136303283));
#98125=CARTESIAN_POINT('Ctrl Pts',(12.1425787135413,10.608,40.4298136303283));
#98126=CARTESIAN_POINT('Ctrl Pts',(11.9174888407591,-4.08,40.024395675874));
#98127=CARTESIAN_POINT('Ctrl Pts',(11.9174888407591,10.608,40.024395675874));
#98128=CARTESIAN_POINT('Ctrl Pts',(11.6825137471499,-4.08,39.6119151152301));
#98129=CARTESIAN_POINT('Ctrl Pts',(11.6825137471499,10.608,39.6119151152301));
#98130=CARTESIAN_POINT('Ctrl Pts',(11.4604343652151,-4.08,39.1895865074125));
#98131=CARTESIAN_POINT('Ctrl Pts',(11.4604343652151,10.608,39.1895865074125));
#98132=CARTESIAN_POINT('Ctrl Pts',(11.2737132025486,-4.08,38.7559673641863));
#98133=CARTESIAN_POINT('Ctrl Pts',(11.2737132025486,10.608,38.7559673641863));
#98134=CARTESIAN_POINT('Ctrl Pts',(11.1408514716204,-4.08,38.3120740300016));
#98135=CARTESIAN_POINT('Ctrl Pts',(11.1408514716204,10.608,38.3120740300016));
#98136=CARTESIAN_POINT('Ctrl Pts',(11.0720880317828,-4.08,37.8627943234146));
#98137=CARTESIAN_POINT('Ctrl Pts',(11.0720880317828,10.608,37.8627943234146));
#98138=CARTESIAN_POINT('Ctrl Pts',(11.0709679278862,-4.08,37.4158119459997));
#98139=CARTESIAN_POINT('Ctrl Pts',(11.0709679278862,10.608,37.4158119459997));
#98140=CARTESIAN_POINT('Ctrl Pts',(11.1371764695442,-4.08,36.9800311993457));
#98141=CARTESIAN_POINT('Ctrl Pts',(11.1371764695442,10.608,36.9800311993457));
#98142=CARTESIAN_POINT('Ctrl Pts',(11.2687034908357,-4.08,36.5642101034699));
#98143=CARTESIAN_POINT('Ctrl Pts',(11.2687034908357,10.608,36.5642101034699));
#98144=CARTESIAN_POINT('Ctrl Pts',(11.464839430664,-4.08,36.1754277041587));
#98145=CARTESIAN_POINT('Ctrl Pts',(11.464839430664,10.608,36.1754277041587));
#98146=CARTESIAN_POINT('Ctrl Pts',(11.7250208885943,-4.08,35.8180786547663));
#98147=CARTESIAN_POINT('Ctrl Pts',(11.7250208885943,10.608,35.8180786547663));
#98148=CARTESIAN_POINT('Ctrl Pts',(12.0463519007611,-4.08,35.4928858294797));
#98149=CARTESIAN_POINT('Ctrl Pts',(12.0463519007611,10.608,35.4928858294797));
#98150=CARTESIAN_POINT('Ctrl Pts',(12.4217894296778,-4.08,35.1961083216786));
#98151=CARTESIAN_POINT('Ctrl Pts',(12.4217894296778,10.608,35.1961083216786));
#98152=CARTESIAN_POINT('Ctrl Pts',(12.8374851087503,-4.08,34.9181535900632));
#98153=CARTESIAN_POINT('Ctrl Pts',(12.8374851087503,10.608,34.9181535900632));
#98154=CARTESIAN_POINT('Ctrl Pts',(13.2738213034495,-4.08,34.6454993802755));
#98155=CARTESIAN_POINT('Ctrl Pts',(13.2738213034495,10.608,34.6454993802755));
#98156=CARTESIAN_POINT('Ctrl Pts',(13.7077402642196,-4.08,34.3639065568125));
#98157=CARTESIAN_POINT('Ctrl Pts',(13.7077402642196,10.608,34.3639065568125));
#98158=CARTESIAN_POINT('Ctrl Pts',(14.1146548169614,-4.08,34.0610864824012));
#98159=CARTESIAN_POINT('Ctrl Pts',(14.1146548169614,10.608,34.0610864824012));
#98160=CARTESIAN_POINT('Ctrl Pts',(14.4705118919346,-4.08,33.7298729261479));
#98161=CARTESIAN_POINT('Ctrl Pts',(14.4705118919346,10.608,33.7298729261479));
#98162=CARTESIAN_POINT('Ctrl Pts',(14.7538514224949,-4.08,33.3703634670861));
#98163=CARTESIAN_POINT('Ctrl Pts',(14.7538514224949,10.608,33.3703634670861));
#98164=CARTESIAN_POINT('Ctrl Pts',(14.9484729279409,-4.08,32.9871564326143));
#98165=CARTESIAN_POINT('Ctrl Pts',(14.9484729279409,10.608,32.9871564326143));
#98166=CARTESIAN_POINT('Ctrl Pts',(15.0458732472955,-4.08,32.5872458409767));
#98167=CARTESIAN_POINT('Ctrl Pts',(15.0458732472955,10.608,32.5872458409767));
#98168=CARTESIAN_POINT('Ctrl Pts',(15.0480973104188,-4.08,32.1776017680613));
#98169=CARTESIAN_POINT('Ctrl Pts',(15.0480973104188,10.608,32.1776017680613));
#98170=CARTESIAN_POINT('Ctrl Pts',(14.9695221769895,-4.08,31.7630680429362));
#98171=CARTESIAN_POINT('Ctrl Pts',(14.9695221769895,10.608,31.7630680429362));
#98172=CARTESIAN_POINT('Ctrl Pts',(14.8310295566835,-4.08,31.345457108689));
#98173=CARTESIAN_POINT('Ctrl Pts',(14.8310295566835,10.608,31.345457108689));
#98174=CARTESIAN_POINT('Ctrl Pts',(14.6552019413825,-4.08,30.9226538837489));
#98175=CARTESIAN_POINT('Ctrl Pts',(14.6552019413825,10.608,30.9226538837489));
#98176=CARTESIAN_POINT('Ctrl Pts',(14.4606799971796,-4.08,30.4874491673258));
#98177=CARTESIAN_POINT('Ctrl Pts',(14.4606799971796,10.608,30.4874491673258));
#98178=CARTESIAN_POINT('Ctrl Pts',(14.2582197141431,-4.08,30.0272537125157));
#98179=CARTESIAN_POINT('Ctrl Pts',(14.2582197141431,10.608,30.0272537125157));
#98180=CARTESIAN_POINT('Ctrl Pts',(14.0530623083977,-4.08,29.527374209947));
#98181=CARTESIAN_POINT('Ctrl Pts',(14.0530623083977,10.608,29.527374209947));
#98182=CARTESIAN_POINT('Ctrl Pts',(13.846419362806,-4.08,28.9738645264781));
#98183=CARTESIAN_POINT('Ctrl Pts',(13.846419362806,10.608,28.9738645264781));
#98184=CARTESIAN_POINT('Ctrl Pts',(13.6372170146976,-4.08,28.3563238803391));
#98185=CARTESIAN_POINT('Ctrl Pts',(13.6372170146976,10.608,28.3563238803391));
#98186=CARTESIAN_POINT('Ctrl Pts',(13.4239120315548,-4.08,27.6712450999957));
#98187=CARTESIAN_POINT('Ctrl Pts',(13.4239120315548,10.608,27.6712450999957));
#98188=CARTESIAN_POINT('Ctrl Pts',(13.2056470980329,-4.08,26.9233802340016));
#98189=CARTESIAN_POINT('Ctrl Pts',(13.2056470980329,10.608,26.9233802340016));
#98190=CARTESIAN_POINT('Ctrl Pts',(12.9819542120748,-4.08,26.1231223827782));
#98191=CARTESIAN_POINT('Ctrl Pts',(12.9819542120748,10.608,26.1231223827782));
#98192=CARTESIAN_POINT('Ctrl Pts',(12.7527764582699,-4.08,25.2847489984795));
#98193=CARTESIAN_POINT('Ctrl Pts',(12.7527764582699,10.608,25.2847489984795));
#98194=CARTESIAN_POINT('Ctrl Pts',(12.5183627807979,-4.08,24.4243412707547));
#98195=CARTESIAN_POINT('Ctrl Pts',(12.5183627807979,10.608,24.4243412707547));
#98196=CARTESIAN_POINT('Ctrl Pts',(12.2792174635073,-4.08,23.5578155700232));
#98197=CARTESIAN_POINT('Ctrl Pts',(12.2792174635073,10.608,23.5578155700232));
#98198=CARTESIAN_POINT('Ctrl Pts',(12.0360270133741,-4.08,22.6989792594677));
#98199=CARTESIAN_POINT('Ctrl Pts',(12.0360270133741,10.608,22.6989792594677));
#98200=CARTESIAN_POINT('Ctrl Pts',(11.7895961018279,-4.08,21.8574023995585));
#98201=CARTESIAN_POINT('Ctrl Pts',(11.7895961018279,10.608,21.8574023995585));
#98202=CARTESIAN_POINT('Ctrl Pts',(11.5407830377121,-4.08,21.0368752434048));
#98203=CARTESIAN_POINT('Ctrl Pts',(11.5407830377121,10.608,21.0368752434048));
#98204=CARTESIAN_POINT('Ctrl Pts',(11.2904565074992,-4.08,20.2370106667995));
#98205=CARTESIAN_POINT('Ctrl Pts',(11.2904565074992,10.608,20.2370106667995));
#98206=CARTESIAN_POINT('Ctrl Pts',(11.0394491705041,-4.08,19.4544416356463));
#98207=CARTESIAN_POINT('Ctrl Pts',(11.0394491705041,10.608,19.4544416356463));
#98208=CARTESIAN_POINT('Ctrl Pts',(10.7885123454296,-4.08,18.6841717409459));
#98209=CARTESIAN_POINT('Ctrl Pts',(10.7885123454296,10.608,18.6841717409459));
#98210=CARTESIAN_POINT('Ctrl Pts',(10.53827045241,-4.08,17.9208535267659));
#98211=CARTESIAN_POINT('Ctrl Pts',(10.53827045241,10.608,17.9208535267659));
#98212=CARTESIAN_POINT('Ctrl Pts',(10.2891746222216,-4.08,17.1601046394454));
#98213=CARTESIAN_POINT('Ctrl Pts',(10.2891746222216,10.608,17.1601046394454));
#98214=CARTESIAN_POINT('Ctrl Pts',(10.0414581777664,-4.08,16.3997893456003));
#98215=CARTESIAN_POINT('Ctrl Pts',(10.0414581777664,10.608,16.3997893456003));
#98216=CARTESIAN_POINT('Ctrl Pts',(9.79508602811751,-4.08,15.6413708166744));
#98217=CARTESIAN_POINT('Ctrl Pts',(9.79508602811751,10.608,15.6413708166744));
#98218=CARTESIAN_POINT('Ctrl Pts',(9.5499270515922,-4.08,14.8889496617949));
#98219=CARTESIAN_POINT('Ctrl Pts',(9.5499270515922,10.608,14.8889496617949));
#98220=CARTESIAN_POINT('Ctrl Pts',(9.30593478897464,-4.08,14.1482310979355));
#98221=CARTESIAN_POINT('Ctrl Pts',(9.30593478897464,10.608,14.1482310979355));
#98222=CARTESIAN_POINT('Ctrl Pts',(9.06332174046596,-4.08,13.4255332425459));
#98223=CARTESIAN_POINT('Ctrl Pts',(9.06332174046596,10.608,13.4255332425459));
#98224=CARTESIAN_POINT('Ctrl Pts',(8.8227443525195,-4.08,12.7267521352114));
#98225=CARTESIAN_POINT('Ctrl Pts',(8.8227443525195,10.608,12.7267521352114));
#98226=CARTESIAN_POINT('Ctrl Pts',(8.58546625544561,-4.08,12.0564083534334));
#98227=CARTESIAN_POINT('Ctrl Pts',(8.58546625544561,10.608,12.0564083534334));
#98228=CARTESIAN_POINT('Ctrl Pts',(8.35357461247668,-4.08,11.4165038934492));
#98229=CARTESIAN_POINT('Ctrl Pts',(8.35357461247668,10.608,11.4165038934492));
#98230=CARTESIAN_POINT('Ctrl Pts',(8.13003837378074,-4.08,10.8059423150097));
#98231=CARTESIAN_POINT('Ctrl Pts',(8.13003837378074,10.608,10.8059423150097));
#98232=CARTESIAN_POINT('Ctrl Pts',(7.91830414509172,-4.08,10.2215845279223));
#98233=CARTESIAN_POINT('Ctrl Pts',(7.91830414509172,10.608,10.2215845279223));
#98234=CARTESIAN_POINT('Ctrl Pts',(7.72198141303743,-4.08,9.65899621297674));
#98235=CARTESIAN_POINT('Ctrl Pts',(7.72198141303743,10.608,9.65899621297674));
#98236=CARTESIAN_POINT('Ctrl Pts',(7.54448066029805,-4.08,9.1133393417742));
#98237=CARTESIAN_POINT('Ctrl Pts',(7.54448066029805,10.608,9.1133393417742));
#98238=CARTESIAN_POINT('Ctrl Pts',(7.38869925602481,-4.08,8.58014320427039));
#98239=CARTESIAN_POINT('Ctrl Pts',(7.38869925602481,10.608,8.58014320427039));
#98240=CARTESIAN_POINT('Ctrl Pts',(7.25661399291181,-4.08,8.05627564240542));
#98241=CARTESIAN_POINT('Ctrl Pts',(7.25661399291181,10.608,8.05627564240542));
#98242=CARTESIAN_POINT('Ctrl Pts',(7.14936655485922,-4.08,7.53989292370001));
#98243=CARTESIAN_POINT('Ctrl Pts',(7.14936655485922,10.608,7.53989292370001));
#98244=CARTESIAN_POINT('Ctrl Pts',(7.08388326066375,-4.08,7.13202122230479));
#98245=CARTESIAN_POINT('Ctrl Pts',(7.08388326066375,10.608,7.13202122230479));
#98246=CARTESIAN_POINT('Ctrl Pts',(7.04627094532923,-4.08,6.82892101237943));
#98247=CARTESIAN_POINT('Ctrl Pts',(7.04627094532923,10.608,6.82892101237943));
#98248=CARTESIAN_POINT('Ctrl Pts',(7.02630542760751,-4.08,6.62809945147867));
#98249=CARTESIAN_POINT('Ctrl Pts',(7.02630542760751,10.608,6.62809945147867));
#98250=CARTESIAN_POINT('Ctrl Pts',(7.0176,-4.08,6.528));
#98251=CARTESIAN_POINT('Ctrl Pts',(7.0176,10.608,6.528));
#98252=CARTESIAN_POINT('',(8.14898645568258,0.708,10.8564616996591));
#98253=CARTESIAN_POINT('Ctrl Pts',(8.14898645568258,0.708,10.8564616996591));
#98254=CARTESIAN_POINT('Ctrl Pts',(8.42682850339849,0.708,11.6200722130095));
#98255=CARTESIAN_POINT('Ctrl Pts',(9.00124539599189,0.708,13.1989442398348));
#98256=CARTESIAN_POINT('Ctrl Pts',(10.0164790416783,0.708,16.3416950229929));
#98257=CARTESIAN_POINT('Ctrl Pts',(11.0099910748761,0.708,19.3240277115474));
#98258=CARTESIAN_POINT('Ctrl Pts',(11.9597260958242,0.708,22.3963108112752));
#98259=CARTESIAN_POINT('Ctrl Pts',(12.5087951337059,0.708,24.3892412418576));
#98260=CARTESIAN_POINT('Ctrl Pts',(12.9454833732632,0.708,25.9917673847204));
#98261=CARTESIAN_POINT('Ctrl Pts',(13.3905704701645,0.708,27.5812925495815));
#98262=CARTESIAN_POINT('Ctrl Pts',(13.8494654471821,0.708,29.0499451471956));
#98263=CARTESIAN_POINT('Ctrl Pts',(14.4628824756264,0.708,30.5144902537932));
#98264=CARTESIAN_POINT('Ctrl Pts',(14.8791134736059,0.708,31.4019992941433));
#98265=CARTESIAN_POINT('Ctrl Pts',(15.0241066822088,0.708,32.072069761124));
#98266=CARTESIAN_POINT('Ctrl Pts',(15.0561190850721,0.708,32.5519007446637));
#98267=CARTESIAN_POINT('Ctrl Pts',(14.8974552701336,0.708,33.1680022242259));
#98268=CARTESIAN_POINT('Ctrl Pts',(14.4744331847702,0.708,33.7318712545294));
#98269=CARTESIAN_POINT('Ctrl Pts',(13.8144693967793,0.708,34.3132874952525));
#98270=CARTESIAN_POINT('Ctrl Pts',(12.9271273497437,0.708,34.8526242972181));
#98271=CARTESIAN_POINT('Ctrl Pts',(11.9610261122155,0.708,35.5093720750203));
#98272=CARTESIAN_POINT('Ctrl Pts',(11.2776408422597,0.708,36.3939284497855));
#98273=CARTESIAN_POINT('Ctrl Pts',(11.0124943973279,0.708,37.4880654661885));
#98274=CARTESIAN_POINT('Ctrl Pts',(11.1732013451346,0.708000000000001,38.6029112675029));
#98275=CARTESIAN_POINT('Ctrl Pts',(11.6860758153009,0.708000000000001,39.6451967054032));
#98276=CARTESIAN_POINT('Ctrl Pts',(12.2174359085071,0.708000000000002,40.5301422030716));
#98277=CARTESIAN_POINT('Ctrl Pts',(12.5379284974733,0.708000000000002,41.3444114032542));
#98278=CARTESIAN_POINT('Ctrl Pts',(12.626182924755,0.708000000000003,41.7867213486322));
#98279=CARTESIAN_POINT('Ctrl Pts',(12.646736323466,0.708000000000003,42.0099427937509));
#98280=CARTESIAN_POINT('',(7.97249537063514,0.848449567099299,10.3682028984962));
#98281=CARTESIAN_POINT('Ctrl Pts',(7.97249537063515,0.8484495670993,10.3682028984962));
#98282=CARTESIAN_POINT('Ctrl Pts',(7.99114484243814,0.815737457406984,10.4202957778083));
#98283=CARTESIAN_POINT('Ctrl Pts',(8.01093169220768,0.788564609464305,10.4753461577291));
#98284=CARTESIAN_POINT('Ctrl Pts',(8.03148980819837,0.767115793117118,10.5323403272196));
#98285=CARTESIAN_POINT('Ctrl Pts',(8.05105340780021,0.746704581547924,10.586577355168));
#98286=CARTESIAN_POINT('Ctrl Pts',(8.07131517713305,0.731476987267821,10.642575146733));
#98287=CARTESIAN_POINT('Ctrl Pts',(8.09193208585319,0.721592241216325,10.6994226011466));
#98288=CARTESIAN_POINT('Ctrl Pts',(8.11074776377252,0.712571092578381,10.7513034823833));
#98289=CARTESIAN_POINT('Ctrl Pts',(8.12985877118522,0.708,10.8038918993056));
#98290=CARTESIAN_POINT('Ctrl Pts',(8.14898645568256,0.708,10.8564616996591));
#98291=CARTESIAN_POINT('',(7.19430053092001,2.51634941530375,7.74120895321939));
#98292=CARTESIAN_POINT('Ctrl Pts',(7.19430053092001,2.51634941530375,7.74120895321939));
#98293=CARTESIAN_POINT('Ctrl Pts',(7.37274783895485,1.95099709579208,8.62351966308874));
#98294=CARTESIAN_POINT('Ctrl Pts',(7.65957903289365,1.3973205309983,9.49414527429423));
#98295=CARTESIAN_POINT('Ctrl Pts',(7.97249537063514,0.848449567099299,10.3682028984962));
#98296=CARTESIAN_POINT('',(7.06369006012584,2.748,6.95461383265853));
#98297=CARTESIAN_POINT('Ctrl Pts',(7.06369006012584,2.748,6.95461383265853));
#98298=CARTESIAN_POINT('Ctrl Pts',(7.07278956030561,2.748,7.0252168756328));
#98299=CARTESIAN_POINT('Ctrl Pts',(7.08259944156938,2.74270356870423,7.09569043605442));
#98300=CARTESIAN_POINT('Ctrl Pts',(7.09299220344838,2.73232722308212,7.16540040552519));
#98301=CARTESIAN_POINT('Ctrl Pts',(7.1035593690914,2.72177674918165,7.23628019695548));
#98302=CARTESIAN_POINT('Ctrl Pts',(7.11472903256084,2.70597443554641,7.30637055164591));
#98303=CARTESIAN_POINT('Ctrl Pts',(7.12631318750442,2.68514788338026,7.37499313226435));
#98304=CARTESIAN_POINT('Ctrl Pts',(7.13851349793525,2.66321357717764,7.44726571409596));
#98305=CARTESIAN_POINT('Ctrl Pts',(7.15117348734242,2.63570634471393,7.51791031719418));
#98306=CARTESIAN_POINT('Ctrl Pts',(7.16401500155562,2.60289207116545,7.58612079978413));
#98307=CARTESIAN_POINT('Ctrl Pts',(7.17405198241766,2.57724429862555,7.63943439637247));
#98308=CARTESIAN_POINT('Ctrl Pts',(7.18419849695384,2.54835442786152,7.69126069197653));
#98309=CARTESIAN_POINT('Ctrl Pts',(7.19430053092,2.51634941530376,7.74120895321938));
#98310=CARTESIAN_POINT('',(7.0176,2.748,6.528));
#98311=CARTESIAN_POINT('Origin',(17.3375887917909,2.748,5.6288564499836));
#98312=CARTESIAN_POINT('',(7.01759999912457,2.964,6.52800003889039));
#98313=CARTESIAN_POINT('',(7.0176,-4.08,6.528));
#98314=CARTESIAN_POINT('',(7.10945460790829,2.964,7.27219995625688));
#98315=CARTESIAN_POINT('Ctrl Pts',(7.10945460790824,2.964,7.27219995625657));
#98316=CARTESIAN_POINT('Ctrl Pts',(7.07010676471875,2.964,7.02501555776906));
#98317=CARTESIAN_POINT('Ctrl Pts',(7.0393340867141,2.964,6.77791646744438));
#98318=CARTESIAN_POINT('Ctrl Pts',(7.01759999655105,2.964,6.5280000391142));
#98319=CARTESIAN_POINT('',(7.1959607894463,2.8235504329007,7.74940308223601));
#98320=CARTESIAN_POINT('Ctrl Pts',(7.1959607894463,2.8235504329007,7.74940308223601));
#98321=CARTESIAN_POINT('Ctrl Pts',(7.16707443778447,2.91473432807616,7.60709256187426));
#98322=CARTESIAN_POINT('Ctrl Pts',(7.13617229126044,2.964,7.44004129019165));
#98323=CARTESIAN_POINT('Ctrl Pts',(7.10945460790829,2.964,7.27219995625688));
#98324=CARTESIAN_POINT('',(7.97548942358869,1.15565058469624,10.3765642386028));
#98325=CARTESIAN_POINT('Ctrl Pts',(7.97548942358869,1.15565058469624,10.3765642386028));
#98326=CARTESIAN_POINT('Ctrl Pts',(7.92841680860499,1.23817684922741,10.2451356716828));
#98327=CARTESIAN_POINT('Ctrl Pts',(7.88185377697889,1.32081047655035,10.1137894131233));
#98328=CARTESIAN_POINT('Ctrl Pts',(7.83611965044893,1.4035750711076,9.98250367791854));
#98329=CARTESIAN_POINT('Ctrl Pts',(7.78358181411942,1.49865227171574,9.83168701229214));
#98330=CARTESIAN_POINT('Ctrl Pts',(7.73213915445198,1.59390230515535,9.68094939752157));
#98331=CARTESIAN_POINT('Ctrl Pts',(7.68228607385709,1.68936095544672,9.53018191941683));
#98332=CARTESIAN_POINT('Ctrl Pts',(7.63343757783075,1.78289602777913,9.38245254207013));
#98333=CARTESIAN_POINT('Ctrl Pts',(7.58611766324347,1.87663139403831,9.23468984690772));
#98334=CARTESIAN_POINT('Ctrl Pts',(7.54077186667867,1.97060071830208,9.08676770712007));
#98335=CARTESIAN_POINT('Ctrl Pts',(7.50151579609986,2.05195040680673,8.95871081101122));
#98336=CARTESIAN_POINT('Ctrl Pts',(7.46373946462395,2.13347543389321,8.83053302698475));
#98337=CARTESIAN_POINT('Ctrl Pts',(7.42769958251337,2.2151976407413,8.70217698826003));
#98338=CARTESIAN_POINT('Ctrl Pts',(7.39230419049043,2.29545843458885,8.5761163009572));
#98339=CARTESIAN_POINT('Ctrl Pts',(7.35858386467001,2.37590941904463,8.44988328475345));
#98340=CARTESIAN_POINT('Ctrl Pts',(7.32674606854267,2.45657128438007,8.3234586653794));
#98341=CARTESIAN_POINT('Ctrl Pts',(7.29405805691174,2.53938719229378,8.1936579275392));
#98342=CARTESIAN_POINT('Ctrl Pts',(7.26335447294836,2.62242539445146,8.06365535232646));
#98343=CARTESIAN_POINT('Ctrl Pts',(7.23482034813647,2.70570828335953,7.93346923864727));
#98344=CARTESIAN_POINT('Ctrl Pts',(7.22138097542936,2.74493394006146,7.87215249196028));
#98345=CARTESIAN_POINT('Ctrl Pts',(7.20842230574121,2.78421387670058,7.81079556575853));
#98346=CARTESIAN_POINT('Ctrl Pts',(7.1959607894463,2.8235504329007,7.74940308223601));
#98347=CARTESIAN_POINT('Ctrl Pts',(8.26785692826664,0.924,11.1826993255823));
#98348=CARTESIAN_POINT('Ctrl Pts',(8.16503869361036,0.924000000000001,10.900623385729));
#98349=CARTESIAN_POINT('Ctrl Pts',(8.06230591927477,1.00344656775053,10.6189592620572));
#98350=CARTESIAN_POINT('Ctrl Pts',(7.97548942358868,1.15565058469624,10.3765642386028));
#98351=CARTESIAN_POINT('Ctrl Pts',(12.348,0.408,42.037449321013));
#98352=CARTESIAN_POINT('Ctrl Pts',(12.3293356677322,0.408,41.8347441976619));
#98353=CARTESIAN_POINT('Ctrl Pts',(12.2491547332484,0.408,41.431777240383));
#98354=CARTESIAN_POINT('Ctrl Pts',(11.9515727626208,0.408,40.6719616755841));
#98355=CARTESIAN_POINT('Ctrl Pts',(11.4307610148928,0.408,39.8019086889107));
#98356=CARTESIAN_POINT('Ctrl Pts',(10.8841273859392,0.408,38.7014536362885));
#98357=CARTESIAN_POINT('Ctrl Pts',(10.7053425599407,0.408,37.474766830819));
#98358=CARTESIAN_POINT('Ctrl Pts',(10.9975978291513,0.408,36.2617575584325));
#98359=CARTESIAN_POINT('Ctrl Pts',(11.762395791144,0.408,35.2772961441942));
#98360=CARTESIAN_POINT('Ctrl Pts',(12.7774343330734,0.408,34.5940530264168));
#98361=CARTESIAN_POINT('Ctrl Pts',(13.6438993253844,0.408,34.0639119954373));
#98362=CARTESIAN_POINT('Ctrl Pts',(14.2563720009146,0.408,33.5240486245267));
#98363=CARTESIAN_POINT('Ctrl Pts',(14.6230727172179,0.408,33.0266397369592));
#98364=CARTESIAN_POINT('Ctrl Pts',(14.7520512685869,0.408,32.5233081857418));
#98365=CARTESIAN_POINT('Ctrl Pts',(14.72627612058,0.408,32.1151402003716));
#98366=CARTESIAN_POINT('Ctrl Pts',(14.5982512199706,0.408,31.5160291164143));
#98367=CARTESIAN_POINT('Ctrl Pts',(14.1926078528925,0.408,30.6420288149888));
#98368=CARTESIAN_POINT('Ctrl Pts',(13.5644842062294,0.408,29.1492480693531));
#98369=CARTESIAN_POINT('Ctrl Pts',(13.1029533106643,0.408,27.6651812531195));
#98370=CARTESIAN_POINT('Ctrl Pts',(12.6560033050097,0.408,26.0711413023541));
#98371=CARTESIAN_POINT('Ctrl Pts',(12.2193900748355,0.408,24.4678689044597));
#98372=CARTESIAN_POINT('Ctrl Pts',(11.6714124934966,0.408,22.4795644823352));
#98373=CARTESIAN_POINT('Ctrl Pts',(10.7256257418815,0.408,19.4196973710059));
#98374=CARTESIAN_POINT('Ctrl Pts',(9.73067490339078,0.408,16.4328440977713));
#98375=CARTESIAN_POINT('Ctrl Pts',(8.71690211803928,0.408,13.294725251134));
#98376=CARTESIAN_POINT('Ctrl Pts',(8.14529762208715,0.408,11.7237141318561));
#98377=CARTESIAN_POINT('Ctrl Pts',(7.86706805722616,0.408,10.9590385811275));
#98378=CARTESIAN_POINT('Ctrl Pts',(12.4262089865968,0.408,42.0302481290153));
#98379=CARTESIAN_POINT('Ctrl Pts',(12.407041514443,0.408,41.8222299675208));
#98380=CARTESIAN_POINT('Ctrl Pts',(12.3247745295799,0.408,41.4088555280366));
#98381=CARTESIAN_POINT('Ctrl Pts',(12.0211738664984,0.408,40.6349151774764));
#98382=CARTESIAN_POINT('Ctrl Pts',(11.4975746041849,0.408,39.7608196137453));
#98383=CARTESIAN_POINT('Ctrl Pts',(10.9598179347726,0.408,38.675714715495));
#98384=CARTESIAN_POINT('Ctrl Pts',(10.7857556730067,0.408,37.4782170679473));
#98385=CARTESIAN_POINT('Ctrl Pts',(11.0708840374197,0.408,36.2963924897708));
#98386=CARTESIAN_POINT('Ctrl Pts',(11.8144929812671,0.408,35.3380422741074));
#98387=CARTESIAN_POINT('Ctrl Pts',(12.8166027375096,0.408,34.6616909757881));
#98388=CARTESIAN_POINT('Ctrl Pts',(13.6886183136859,0.408,34.1291779206297));
#98389=CARTESIAN_POINT('Ctrl Pts',(14.3134155906142,0.408,33.5785454640157));
#98390=CARTESIAN_POINT('Ctrl Pts',(14.6948792272124,0.408,33.0635168942324));
#98391=CARTESIAN_POINT('Ctrl Pts',(14.8316844100114,0.408,32.5308695841929));
#98392=CARTESIAN_POINT('Ctrl Pts',(14.804346338616,0.408,32.1037914102775));
#98393=CARTESIAN_POINT('Ctrl Pts',(14.6715776101179,0.408,31.4862764667729));
#98394=CARTESIAN_POINT('Ctrl Pts',(14.2634371814432,0.408,30.6086052959154));
#98395=CARTESIAN_POINT('Ctrl Pts',(13.6389720109982,0.408,29.1233338664017));
#98396=CARTESIAN_POINT('Ctrl Pts',(13.178243006681,0.408,27.6432224346962));
#98397=CARTESIAN_POINT('Ctrl Pts',(12.7317968740594,0.408,26.0503759497634));
#98398=CARTESIAN_POINT('Ctrl Pts',(12.2951426945594,0.408,24.4472662518418));
#98399=CARTESIAN_POINT('Ctrl Pts',(11.7469042071722,0.408,22.4577846978806));
#98400=CARTESIAN_POINT('Ctrl Pts',(10.8000742806557,0.408,19.3946624048871));
#98401=CARTESIAN_POINT('Ctrl Pts',(9.80548641546268,0.407999999999999,16.4089323484146));
#98402=CARTESIAN_POINT('Ctrl Pts',(8.79135149928353,0.408000000000001,13.2696900665871));
#98403=CARTESIAN_POINT('Ctrl Pts',(8.21899977033033,0.407999999999999,11.6965458507707));
#98404=CARTESIAN_POINT('Ctrl Pts',(7.94087412135137,0.408,10.9321840163567));
#98405=CARTESIAN_POINT('Ctrl Pts',(12.581955104232,0.473055248537292,42.0159076069757));
#98406=CARTESIAN_POINT('Ctrl Pts',(12.5618055796328,0.473055248537293,41.7971742246958));
#98407=CARTESIAN_POINT('Ctrl Pts',(12.4753204441731,0.473055248537293,41.3633235477922));
#98408=CARTESIAN_POINT('Ctrl Pts',(12.1597821186542,0.473055248537292,40.5609508438889));
#98409=CARTESIAN_POINT('Ctrl Pts',(11.6306919845739,0.473055248537292,39.6791381576489));
#98410=CARTESIAN_POINT('Ctrl Pts',(11.1105229237936,0.473055248537292,38.6243202097953));
#98411=CARTESIAN_POINT('Ctrl Pts',(10.9458889057599,0.473055248537292,37.4851605747719));
#98412=CARTESIAN_POINT('Ctrl Pts',(11.2168938631936,0.473055248537292,36.3652890517585));
#98413=CARTESIAN_POINT('Ctrl Pts',(11.9180174414507,0.473055248537292,35.4590386817689));
#98414=CARTESIAN_POINT('Ctrl Pts',(12.8946520834261,0.473055248537292,34.796515348691));
#98415=CARTESIAN_POINT('Ctrl Pts',(13.7775240669142,0.473055248537292,34.2591964757362));
#98416=CARTESIAN_POINT('Ctrl Pts',(14.4271163836494,0.473055248537292,33.6868645901221));
#98417=CARTESIAN_POINT('Ctrl Pts',(14.8379372503615,0.473055248537292,33.1372592611523));
#98418=CARTESIAN_POINT('Ctrl Pts',(14.9902008053167,0.473055248537292,32.5457514490063));
#98419=CARTESIAN_POINT('Ctrl Pts',(14.9595880150098,0.473055248537292,32.0813605528424));
#98420=CARTESIAN_POINT('Ctrl Pts',(14.8180716457112,0.473055248537292,31.4267941892507));
#98421=CARTESIAN_POINT('Ctrl Pts',(14.404321342134,0.473055248537292,30.5421242336123));
#98422=CARTESIAN_POINT('Ctrl Pts',(13.7875862672428,0.473055248537292,29.0715350395797));
#98423=CARTESIAN_POINT('Ctrl Pts',(13.3281948697516,0.473055248537292,27.5994860312853));
#98424=CARTESIAN_POINT('Ctrl Pts',(12.8827146686647,0.473055248537292,26.0089895623799));
#98425=CARTESIAN_POINT('Ctrl Pts',(12.4460283648194,0.473055248537292,24.4062796267624));
#98426=CARTESIAN_POINT('Ctrl Pts',(11.897212710331,0.473055248537292,22.4143751808534));
#98427=CARTESIAN_POINT('Ctrl Pts',(10.9483274733356,0.473055248537292,19.3447813493081));
#98428=CARTESIAN_POINT('Ctrl Pts',(9.95449421874235,0.473055248537291,16.3614278429735));
#98429=CARTESIAN_POINT('Ctrl Pts',(8.93959102601856,0.473055248537292,13.2197414791673));
#98430=CARTESIAN_POINT('Ctrl Pts',(8.36577664166789,0.473055248537291,11.6425235888116));
#98431=CARTESIAN_POINT('Ctrl Pts',(8.08785221741985,0.473055248537292,10.8787055813861));
#98432=CARTESIAN_POINT('Ctrl Pts',(12.646736323466,0.629460183660257,42.0099427937509));
#98433=CARTESIAN_POINT('Ctrl Pts',(12.626182924755,0.629460183660258,41.7867213486322));
#98434=CARTESIAN_POINT('Ctrl Pts',(12.5379284974733,0.629460183660258,41.3444114032542));
#98435=CARTESIAN_POINT('Ctrl Pts',(12.2174359085071,0.629460183660257,40.5301422030716));
#98436=CARTESIAN_POINT('Ctrl Pts',(11.6860758153009,0.629460183660256,39.6451967054032));
#98437=CARTESIAN_POINT('Ctrl Pts',(11.1732013451346,0.629460183660256,38.6029112675029));
#98438=CARTESIAN_POINT('Ctrl Pts',(11.0124943973279,0.629460183660256,37.4880654661885));
#98439=CARTESIAN_POINT('Ctrl Pts',(11.2776408422597,0.629460183660255,36.3939284497855));
#98440=CARTESIAN_POINT('Ctrl Pts',(11.9610261122155,0.629460183660255,35.5093720750203));
#98441=CARTESIAN_POINT('Ctrl Pts',(12.9271273497437,0.629460183660255,34.8526242972181));
#98442=CARTESIAN_POINT('Ctrl Pts',(13.8144693967793,0.629460183660255,34.3132874952525));
#98443=CARTESIAN_POINT('Ctrl Pts',(14.4744331847702,0.629460183660255,33.7318712545294));
#98444=CARTESIAN_POINT('Ctrl Pts',(14.8974552701336,0.629460183660255,33.1680022242259));
#98445=CARTESIAN_POINT('Ctrl Pts',(15.0561190850721,0.629460183660255,32.5519007446637));
#98446=CARTESIAN_POINT('Ctrl Pts',(15.0241066822088,0.629460183660255,32.072069761124));
#98447=CARTESIAN_POINT('Ctrl Pts',(14.8791134736059,0.629460183660255,31.4019992941433));
#98448=CARTESIAN_POINT('Ctrl Pts',(14.4628824756264,0.629460183660255,30.5144902537932));
#98449=CARTESIAN_POINT('Ctrl Pts',(13.8494654471821,0.629460183660255,29.0499451471956));
#98450=CARTESIAN_POINT('Ctrl Pts',(13.3905704701645,0.629460183660255,27.5812925495815));
#98451=CARTESIAN_POINT('Ctrl Pts',(12.9454833732632,0.629460183660255,25.9917673847204));
#98452=CARTESIAN_POINT('Ctrl Pts',(12.5087951337059,0.629460183660255,24.3892412418576));
#98453=CARTESIAN_POINT('Ctrl Pts',(11.9597260958242,0.629460183660255,22.3963108112752));
#98454=CARTESIAN_POINT('Ctrl Pts',(11.0099910748761,0.629460183660255,19.3240277115474));
#98455=CARTESIAN_POINT('Ctrl Pts',(10.0164790416783,0.629460183660255,16.3416950229929));
#98456=CARTESIAN_POINT('Ctrl Pts',(9.00124539599189,0.629460183660255,13.1989442398348));
#98457=CARTESIAN_POINT('Ctrl Pts',(8.42682850339849,0.629460183660254,11.6200722130095));
#98458=CARTESIAN_POINT('Ctrl Pts',(8.14898645568258,0.629460183660255,10.8564616996591));
#98459=CARTESIAN_POINT('Ctrl Pts',(12.646736323466,0.708000000000003,42.0099427937509));
#98460=CARTESIAN_POINT('Ctrl Pts',(12.626182924755,0.708000000000003,41.7867213486322));
#98461=CARTESIAN_POINT('Ctrl Pts',(12.5379284974733,0.708000000000002,41.3444114032542));
#98462=CARTESIAN_POINT('Ctrl Pts',(12.2174359085071,0.708000000000002,40.5301422030716));
#98463=CARTESIAN_POINT('Ctrl Pts',(11.6860758153009,0.708000000000001,39.6451967054032));
#98464=CARTESIAN_POINT('Ctrl Pts',(11.1732013451346,0.708000000000001,38.6029112675029));
#98465=CARTESIAN_POINT('Ctrl Pts',(11.0124943973279,0.708,37.4880654661885));
#98466=CARTESIAN_POINT('Ctrl Pts',(11.2776408422597,0.708,36.3939284497855));
#98467=CARTESIAN_POINT('Ctrl Pts',(11.9610261122155,0.708,35.5093720750203));
#98468=CARTESIAN_POINT('Ctrl Pts',(12.9271273497437,0.708,34.8526242972181));
#98469=CARTESIAN_POINT('Ctrl Pts',(13.8144693967793,0.708,34.3132874952525));
#98470=CARTESIAN_POINT('Ctrl Pts',(14.4744331847702,0.708,33.7318712545294));
#98471=CARTESIAN_POINT('Ctrl Pts',(14.8974552701336,0.708,33.1680022242259));
#98472=CARTESIAN_POINT('Ctrl Pts',(15.0561190850721,0.708,32.5519007446637));
#98473=CARTESIAN_POINT('Ctrl Pts',(15.0241066822088,0.708,32.072069761124));
#98474=CARTESIAN_POINT('Ctrl Pts',(14.8791134736059,0.708,31.4019992941433));
#98475=CARTESIAN_POINT('Ctrl Pts',(14.4628824756264,0.708,30.5144902537932));
#98476=CARTESIAN_POINT('Ctrl Pts',(13.8494654471821,0.708,29.0499451471956));
#98477=CARTESIAN_POINT('Ctrl Pts',(13.3905704701645,0.708,27.5812925495815));
#98478=CARTESIAN_POINT('Ctrl Pts',(12.9454833732632,0.708,25.9917673847204));
#98479=CARTESIAN_POINT('Ctrl Pts',(12.5087951337059,0.708,24.3892412418576));
#98480=CARTESIAN_POINT('Ctrl Pts',(11.9597260958242,0.708,22.3963108112752));
#98481=CARTESIAN_POINT('Ctrl Pts',(11.0099910748761,0.708,19.3240277115474));
#98482=CARTESIAN_POINT('Ctrl Pts',(10.0164790416783,0.708,16.3416950229929));
#98483=CARTESIAN_POINT('Ctrl Pts',(9.00124539599189,0.708,13.1989442398348));
#98484=CARTESIAN_POINT('Ctrl Pts',(8.42682850339849,0.708,11.6200722130095));
#98485=CARTESIAN_POINT('Ctrl Pts',(8.14898645568258,0.708,10.8564616996591));
#98486=CARTESIAN_POINT('',(7.86706805722616,0.408,10.9590385811275));
#98487=CARTESIAN_POINT('Ctrl Pts',(12.348,0.408,42.037449321013));
#98488=CARTESIAN_POINT('Ctrl Pts',(12.3293356677322,0.408,41.8347441976619));
#98489=CARTESIAN_POINT('Ctrl Pts',(12.2491547332484,0.408,41.431777240383));
#98490=CARTESIAN_POINT('Ctrl Pts',(11.9515727626208,0.408,40.6719616755841));
#98491=CARTESIAN_POINT('Ctrl Pts',(11.4307610148928,0.408,39.8019086889107));
#98492=CARTESIAN_POINT('Ctrl Pts',(10.8841273859392,0.408,38.7014536362885));
#98493=CARTESIAN_POINT('Ctrl Pts',(10.7053425599407,0.408,37.474766830819));
#98494=CARTESIAN_POINT('Ctrl Pts',(10.9975978291513,0.408,36.2617575584325));
#98495=CARTESIAN_POINT('Ctrl Pts',(11.762395791144,0.408,35.2772961441942));
#98496=CARTESIAN_POINT('Ctrl Pts',(12.7774343330734,0.408,34.5940530264168));
#98497=CARTESIAN_POINT('Ctrl Pts',(13.6438993253844,0.408,34.0639119954373));
#98498=CARTESIAN_POINT('Ctrl Pts',(14.2563720009146,0.408,33.5240486245267));
#98499=CARTESIAN_POINT('Ctrl Pts',(14.6230727172179,0.408,33.0266397369592));
#98500=CARTESIAN_POINT('Ctrl Pts',(14.7520512685869,0.408,32.5233081857418));
#98501=CARTESIAN_POINT('Ctrl Pts',(14.72627612058,0.408,32.1151402003716));
#98502=CARTESIAN_POINT('Ctrl Pts',(14.5982512199706,0.408,31.5160291164143));
#98503=CARTESIAN_POINT('Ctrl Pts',(14.1926078528925,0.408,30.6420288149888));
#98504=CARTESIAN_POINT('Ctrl Pts',(13.5644842062294,0.408,29.1492480693531));
#98505=CARTESIAN_POINT('Ctrl Pts',(13.1029533106643,0.408,27.6651812531195));
#98506=CARTESIAN_POINT('Ctrl Pts',(12.6560033050097,0.408,26.0711413023541));
#98507=CARTESIAN_POINT('Ctrl Pts',(12.2193900748355,0.408,24.4678689044597));
#98508=CARTESIAN_POINT('Ctrl Pts',(11.6714124934966,0.408,22.4795644823352));
#98509=CARTESIAN_POINT('Ctrl Pts',(10.7256257418815,0.408,19.4196973710059));
#98510=CARTESIAN_POINT('Ctrl Pts',(9.73067490339078,0.408,16.4328440977713));
#98511=CARTESIAN_POINT('Ctrl Pts',(8.71690211803928,0.408,13.294725251134));
#98512=CARTESIAN_POINT('Ctrl Pts',(8.14529762208715,0.408,11.7237141318561));
#98513=CARTESIAN_POINT('Ctrl Pts',(7.86706805722616,0.408,10.9590385811275));
#98514=CARTESIAN_POINT('Origin',(7.86706805722616,0.708,10.9590385811275));
#98515=CARTESIAN_POINT('Origin',(0.,0.408,45.696));
#98516=CARTESIAN_POINT('',(-7.86706805722818,0.408,10.9590385811275));
#98517=CARTESIAN_POINT('Ctrl Pts',(-7.86706805722818,0.408,10.9590385811275));
#98518=CARTESIAN_POINT('Ctrl Pts',(-8.14529762208872,0.408,11.7237141318567));
#98519=CARTESIAN_POINT('Ctrl Pts',(-8.71704186979063,0.408,13.2944622451918));
#98520=CARTESIAN_POINT('Ctrl Pts',(-9.73047444441272,0.408,16.4333423355267));
#98521=CARTESIAN_POINT('Ctrl Pts',(-10.7261073804545,0.408,19.4185393496298));
#98522=CARTESIAN_POINT('Ctrl Pts',(-11.6714712785442,0.408,22.4801977909835));
#98523=CARTESIAN_POINT('Ctrl Pts',(-12.3283245256811,0.408,24.863229880916));
#98524=CARTESIAN_POINT('Ctrl Pts',(-12.8745412424139,0.408,26.8802191948613));
#98525=CARTESIAN_POINT('Ctrl Pts',(-13.2776635653459,0.408,28.2207382228647));
#98526=CARTESIAN_POINT('Ctrl Pts',(-13.5275915188378,0.408,28.9655691222892));
#98527=CARTESIAN_POINT('Ctrl Pts',(-13.7965168172222,0.408,29.7066451167418));
#98528=CARTESIAN_POINT('Ctrl Pts',(-14.1174916376575,0.408,30.4559864726176));
#98529=CARTESIAN_POINT('Ctrl Pts',(-14.4607164581972,0.408,31.2259562265925));
#98530=CARTESIAN_POINT('Ctrl Pts',(-14.6785938108899,0.408,31.8124084143345));
#98531=CARTESIAN_POINT('Ctrl Pts',(-14.758965754309,0.408,32.318839178772));
#98532=CARTESIAN_POINT('Ctrl Pts',(-14.7021471218213,0.408,32.7251838170679));
#98533=CARTESIAN_POINT('Ctrl Pts',(-14.5601534893954,0.408,33.1087788993748));
#98534=CARTESIAN_POINT('Ctrl Pts',(-14.2578487820426,0.408,33.5241316135338));
#98535=CARTESIAN_POINT('Ctrl Pts',(-13.6438437735972,0.408,34.0632940521152));
#98536=CARTESIAN_POINT('Ctrl Pts',(-12.7773832461027,0.408,34.5944195816753));
#98537=CARTESIAN_POINT('Ctrl Pts',(-11.7611413721559,0.408,35.2761453566851));
#98538=CARTESIAN_POINT('Ctrl Pts',(-10.9988226749202,0.408,36.2620634912197));
#98539=CARTESIAN_POINT('Ctrl Pts',(-10.7057193819818,0.408,37.4749048193445));
#98540=CARTESIAN_POINT('Ctrl Pts',(-10.8844352537976,0.408,38.7015205845166));
#98541=CARTESIAN_POINT('Ctrl Pts',(-11.4308693301032,0.408,39.8019474928579));
#98542=CARTESIAN_POINT('Ctrl Pts',(-11.9516179428138,0.408,40.6719746799563));
#98543=CARTESIAN_POINT('Ctrl Pts',(-12.2491730342286,0.408,41.4317865452711));
#98544=CARTESIAN_POINT('Ctrl Pts',(-12.3293356677362,0.408,41.8347441976576));
#98545=CARTESIAN_POINT('Ctrl Pts',(-12.348,0.408,42.03744932101));
#98546=CARTESIAN_POINT('',(0.,0.408,10.9590385811275));
#98547=CARTESIAN_POINT('',(6.528,0.408,40.832));
#98548=CARTESIAN_POINT('Origin',(6.528,0.408,42.432));
#98549=CARTESIAN_POINT('',(-6.528,0.408,40.832));
#98550=CARTESIAN_POINT('Origin',(-6.528,0.408,42.432));
#98551=CARTESIAN_POINT('Origin',(-12.3479078516845,0.708,42.0374535543929));
#98552=CARTESIAN_POINT('',(-12.6467363234665,0.924,42.0099427937539));
#98553=CARTESIAN_POINT('Origin',(-12.348,0.924000000000001,42.03744932101));
#98554=CARTESIAN_POINT('',(-12.6467363234665,0.708000000000001,42.0099427937538));
#98555=CARTESIAN_POINT('',(-12.6467363234665,0.924000000000001,42.0099427937538));
#98556=CARTESIAN_POINT('Origin',(-12.348,0.708,42.03744932101));
#98557=CARTESIAN_POINT('Origin',(-12.348,0.924,42.03744932101));
#98558=CARTESIAN_POINT('Origin',(-12.348,0.924,42.03744932101));
#98559=CARTESIAN_POINT('Origin',(-12.348,0.708,42.0374493210099));
#98560=CARTESIAN_POINT('Origin',(-12.348,0.708,42.0374493210099));
#98561=CARTESIAN_POINT('Ctrl Pts',(-7.86706805722818,0.408,10.9590385811275));
#98562=CARTESIAN_POINT('Ctrl Pts',(-8.14529762208872,0.408,11.7237141318567));
#98563=CARTESIAN_POINT('Ctrl Pts',(-8.71704186979063,0.408,13.2944622451918));
#98564=CARTESIAN_POINT('Ctrl Pts',(-9.73047444441272,0.408,16.4333423355267));
#98565=CARTESIAN_POINT('Ctrl Pts',(-10.7261073804545,0.408,19.4185393496298));
#98566=CARTESIAN_POINT('Ctrl Pts',(-11.6714712785442,0.408,22.4801977909835));
#98567=CARTESIAN_POINT('Ctrl Pts',(-12.3283245256811,0.408,24.863229880916));
#98568=CARTESIAN_POINT('Ctrl Pts',(-12.8745412424139,0.408,26.8802191948613));
#98569=CARTESIAN_POINT('Ctrl Pts',(-13.2776635653459,0.408,28.2207382228647));
#98570=CARTESIAN_POINT('Ctrl Pts',(-13.5275915188378,0.408,28.9655691222892));
#98571=CARTESIAN_POINT('Ctrl Pts',(-13.7965168172222,0.408,29.7066451167418));
#98572=CARTESIAN_POINT('Ctrl Pts',(-14.1174916376575,0.408,30.4559864726176));
#98573=CARTESIAN_POINT('Ctrl Pts',(-14.4607164581972,0.408,31.2259562265925));
#98574=CARTESIAN_POINT('Ctrl Pts',(-14.6785938108899,0.408,31.8124084143345));
#98575=CARTESIAN_POINT('Ctrl Pts',(-14.758965754309,0.408,32.318839178772));
#98576=CARTESIAN_POINT('Ctrl Pts',(-14.7021471218213,0.408,32.7251838170679));
#98577=CARTESIAN_POINT('Ctrl Pts',(-14.5601534893954,0.408,33.1087788993748));
#98578=CARTESIAN_POINT('Ctrl Pts',(-14.2578487820426,0.408,33.5241316135338));
#98579=CARTESIAN_POINT('Ctrl Pts',(-13.6438437735972,0.408,34.0632940521152));
#98580=CARTESIAN_POINT('Ctrl Pts',(-12.7773832461027,0.408,34.5944195816753));
#98581=CARTESIAN_POINT('Ctrl Pts',(-11.7611413721559,0.408,35.2761453566851));
#98582=CARTESIAN_POINT('Ctrl Pts',(-10.9988226749202,0.408,36.2620634912197));
#98583=CARTESIAN_POINT('Ctrl Pts',(-10.7057193819818,0.408,37.4749048193445));
#98584=CARTESIAN_POINT('Ctrl Pts',(-10.8844352537976,0.408,38.7015205845166));
#98585=CARTESIAN_POINT('Ctrl Pts',(-11.4308693301032,0.408,39.8019474928579));
#98586=CARTESIAN_POINT('Ctrl Pts',(-11.9516179428138,0.408,40.6719746799563));
#98587=CARTESIAN_POINT('Ctrl Pts',(-12.2491730342286,0.408,41.4317865452711));
#98588=CARTESIAN_POINT('Ctrl Pts',(-12.3293356677362,0.408,41.8347441976576));
#98589=CARTESIAN_POINT('Ctrl Pts',(-12.348,0.408,42.03744932101));
#98590=CARTESIAN_POINT('Ctrl Pts',(-7.9408741213534,0.408,10.9321840163568));
#98591=CARTESIAN_POINT('Ctrl Pts',(-8.21899448195459,0.408,11.6965386637911));
#98592=CARTESIAN_POINT('Ctrl Pts',(-8.79150002820804,0.408,13.2694389389543));
#98593=CARTESIAN_POINT('Ctrl Pts',(-9.80527206182065,0.408,16.4094120358171));
#98594=CARTESIAN_POINT('Ctrl Pts',(-10.8005761179624,0.408,19.3935296469743));
#98595=CARTESIAN_POINT('Ctrl Pts',(-11.7469489940788,0.408,22.4584202360245));
#98596=CARTESIAN_POINT('Ctrl Pts',(-12.4041693706504,0.408,24.8428586149106));
#98597=CARTESIAN_POINT('Ctrl Pts',(-12.9502306891845,0.408,26.8592184864153));
#98598=CARTESIAN_POINT('Ctrl Pts',(-13.3526242310787,0.408,28.1972479280124));
#98599=CARTESIAN_POINT('Ctrl Pts',(-13.6017477475719,0.408,28.9396772692248));
#98600=CARTESIAN_POINT('Ctrl Pts',(-13.8696691564005,0.408,29.6779559679235));
#98601=CARTESIAN_POINT('Ctrl Pts',(-14.188972446946,0.408,30.4233668377294));
#98602=CARTESIAN_POINT('Ctrl Pts',(-14.5329455827326,0.408,31.1951619690078));
#98603=CARTESIAN_POINT('Ctrl Pts',(-14.7542894776902,0.408,31.7898177864783));
#98604=CARTESIAN_POINT('Ctrl Pts',(-14.8386547730419,0.408,32.3155727527421));
#98605=CARTESIAN_POINT('Ctrl Pts',(-14.7789340688096,0.408,32.7447317667957));
#98606=CARTESIAN_POINT('Ctrl Pts',(-14.629183409932,0.408,33.1483645673388));
#98607=CARTESIAN_POINT('Ctrl Pts',(-14.3150723184658,0.408,33.5787328885495));
#98608=CARTESIAN_POINT('Ctrl Pts',(-13.6884615573532,0.408,34.1284959992061));
#98609=CARTESIAN_POINT('Ctrl Pts',(-12.816577976426,0.408,34.6620649760208));
#98610=CARTESIAN_POINT('Ctrl Pts',(-11.8132710691042,0.408,35.3369167701079));
#98611=CARTESIAN_POINT('Ctrl Pts',(-11.0721272704617,0.408,36.2967378483312));
#98612=CARTESIAN_POINT('Ctrl Pts',(-10.7861220821357,0.408,37.4783331896387));
#98613=CARTESIAN_POINT('Ctrl Pts',(-10.960131624409,0.408,38.6757938575208));
#98614=CARTESIAN_POINT('Ctrl Pts',(-11.4976792812224,0.408,39.7608508017226));
#98615=CARTESIAN_POINT('Ctrl Pts',(-12.0212210638666,0.408,40.6349324038072));
#98616=CARTESIAN_POINT('Ctrl Pts',(-12.3247915762225,0.408,41.4088622076599));
#98617=CARTESIAN_POINT('Ctrl Pts',(-12.407042265963,0.408,41.8222315403878));
#98618=CARTESIAN_POINT('Ctrl Pts',(-12.4262089865969,0.408,42.0302481290139));
#98619=CARTESIAN_POINT('Ctrl Pts',(-8.08785221742193,0.473055248537291,
10.8787055813863));
#98620=CARTESIAN_POINT('Ctrl Pts',(-8.36577308576392,0.473055248537292,
11.6425187562859));
#98621=CARTESIAN_POINT('Ctrl Pts',(-8.93974692360289,0.473055248537292,
13.2194998310699));
#98622=CARTESIAN_POINT('Ctrl Pts',(-9.95426584407475,0.473055248537292,
16.3618905475388));
#98623=CARTESIAN_POINT('Ctrl Pts',(-10.9488714128454,0.473055248537292,
19.343709455506));
#98624=CARTESIAN_POINT('Ctrl Pts',(-11.8972430237721,0.473055248537292,
22.4150157545571));
#98625=CARTESIAN_POINT('Ctrl Pts',(-12.5552259541882,0.473055248537292,
24.802337614812));
#98626=CARTESIAN_POINT('Ctrl Pts',(-13.1009715712584,0.473055248537292,
26.817426547811));
#98627=CARTESIAN_POINT('Ctrl Pts',(-13.5019423383403,0.473055248537292,
28.1505676628167));
#98628=CARTESIAN_POINT('Ctrl Pts',(-13.7494718765433,0.473055248537292,
28.8882437809313));
#98629=CARTESIAN_POINT('Ctrl Pts',(-14.0153723178963,0.473055248537292,
29.6208791675758));
#98630=CARTESIAN_POINT('Ctrl Pts',(-14.3312811591807,0.473055248537292,
30.3584027105315));
#98631=CARTESIAN_POINT('Ctrl Pts',(-14.6768487098997,0.473055248537292,
31.1339357497066));
#98632=CARTESIAN_POINT('Ctrl Pts',(-14.9049633344377,0.473055248537292,
31.7447250380521));
#98633=CARTESIAN_POINT('Ctrl Pts',(-14.9973884818485,0.473055248537292,
32.3092032034564));
#98634=CARTESIAN_POINT('Ctrl Pts',(-14.9317626077194,0.473055248537292,
32.7835254048073));
#98635=CARTESIAN_POINT('Ctrl Pts',(-14.7666231464089,0.473055248537292,
33.2271698211528));
#98636=CARTESIAN_POINT('Ctrl Pts',(-14.4292891563142,0.473055248537292,
33.6872556604146));
#98637=CARTESIAN_POINT('Ctrl Pts',(-13.7771527815462,0.473055248537292,
34.2582504768461));
#98638=CARTESIAN_POINT('Ctrl Pts',(-12.894911422127,0.473055248537292,34.7968855412878));
#98639=CARTESIAN_POINT('Ctrl Pts',(-11.9170146182718,0.473055248537292,
35.4579926075445));
#98640=CARTESIAN_POINT('Ctrl Pts',(-11.2178736627465,0.473055248537292,
36.365562487716));
#98641=CARTESIAN_POINT('Ctrl Pts',(-10.9461492507296,0.473055248537292,
37.4852260297065));
#98642=CARTESIAN_POINT('Ctrl Pts',(-11.1107671811473,0.473055248537292,
38.6243802726169));
#98643=CARTESIAN_POINT('Ctrl Pts',(-11.6307663593404,0.473055248537292,
39.6791570877032));
#98644=CARTESIAN_POINT('Ctrl Pts',(-12.1598187182913,0.473055248537292,
40.5609653170687));
#98645=CARTESIAN_POINT('Ctrl Pts',(-12.4753335077982,0.473055248537292,
41.3633294566678));
#98646=CARTESIAN_POINT('Ctrl Pts',(-12.5618060849566,0.473055248537292,
41.797175282291));
#98647=CARTESIAN_POINT('Ctrl Pts',(-12.5819551042324,0.473055248537292,
42.0159076069773));
#98648=CARTESIAN_POINT('Ctrl Pts',(-8.14898645568467,0.629460183660255,
10.8564616996593));
#98649=CARTESIAN_POINT('Ctrl Pts',(-8.42682850340027,0.629460183660255,
11.6200722130106));
#98650=CARTESIAN_POINT('Ctrl Pts',(-9.00140202108135,0.629460183660255,
13.1987032575008));
#98651=CARTESIAN_POINT('Ctrl Pts',(-10.0162479906236,0.629460183660255,
16.3421552779583));
#98652=CARTESIAN_POINT('Ctrl Pts',(-11.0105529606629,0.629460183660255,
19.3229835736891));
#98653=CARTESIAN_POINT('Ctrl Pts',(-11.9597534877299,0.629460183660255,
22.3969536172018));
#98654=CARTESIAN_POINT('Ctrl Pts',(-12.6180608664011,0.629460183660255,
24.7854940213506));
#98655=CARTESIAN_POINT('Ctrl Pts',(-13.1636737275955,0.629460183660255,
26.8000502819042));
#98656=CARTESIAN_POINT('Ctrl Pts',(-13.5640592992395,0.629460183660255,
28.1311741992264));
#98657=CARTESIAN_POINT('Ctrl Pts',(-13.8109276823942,0.629460183660255,
28.866880021582));
#98658=CARTESIAN_POINT('Ctrl Pts',(-14.0759824773703,0.629460183660255,
29.5971513030824));
#98659=CARTESIAN_POINT('Ctrl Pts',(-14.3904642268911,0.629460183660255,
30.3313802830276));
#98660=CARTESIAN_POINT('Ctrl Pts',(-14.7367190536345,0.629460183660255,
31.1084918464257));
#98661=CARTESIAN_POINT('Ctrl Pts',(-14.9676192527248,0.629460183660255,
31.7259447042262));
#98662=CARTESIAN_POINT('Ctrl Pts',(-15.0634216666442,0.629460183660255,
32.3065851128709));
#98663=CARTESIAN_POINT('Ctrl Pts',(-14.995310469097,0.629460183660255,32.799630218064));
#98664=CARTESIAN_POINT('Ctrl Pts',(-14.8237837226447,0.629460183660255,
33.2599421532119));
#98665=CARTESIAN_POINT('Ctrl Pts',(-14.4768570601396,0.629460183660255,
33.7323460288388));
#98666=CARTESIAN_POINT('Ctrl Pts',(-13.8140058769173,0.629460183660255,
34.312200058379));
#98667=CARTESIAN_POINT('Ctrl Pts',(-12.9275584185962,0.629460183660254,
34.852988598105));
#98668=CARTESIAN_POINT('Ctrl Pts',(-11.9601501028038,0.629460183660255,
35.5083657619793));
#98669=CARTESIAN_POINT('Ctrl Pts',(-11.2784416996154,0.629460183660255,
36.394137190602));
#98670=CARTESIAN_POINT('Ctrl Pts',(-11.0126908986932,0.629460183660255,
37.488108200426));
#98671=CARTESIAN_POINT('Ctrl Pts',(-11.1733979901704,0.629460183660255,
38.6029533695122));
#98672=CARTESIAN_POINT('Ctrl Pts',(-11.6861322554559,0.629460183660255,
39.6452112093278));
#98673=CARTESIAN_POINT('Ctrl Pts',(-12.2174647212886,0.629460183660255,
40.5301529508079));
#98674=CARTESIAN_POINT('Ctrl Pts',(-12.5379395610492,0.629460183660255,
41.3444180220226));
#98675=CARTESIAN_POINT('Ctrl Pts',(-12.6261829247595,0.629460183660255,
41.7867213486289));
#98676=CARTESIAN_POINT('Ctrl Pts',(-12.6467363234665,0.629460183660255,
42.0099427937538));
#98677=CARTESIAN_POINT('Ctrl Pts',(-8.14898645568467,0.708,10.8564616996593));
#98678=CARTESIAN_POINT('Ctrl Pts',(-8.42682850340027,0.708,11.6200722130106));
#98679=CARTESIAN_POINT('Ctrl Pts',(-9.00140202108135,0.708,13.1987032575008));
#98680=CARTESIAN_POINT('Ctrl Pts',(-10.0162479906236,0.708,16.3421552779583));
#98681=CARTESIAN_POINT('Ctrl Pts',(-11.0105529606629,0.708,19.3229835736891));
#98682=CARTESIAN_POINT('Ctrl Pts',(-11.9597534877299,0.708,22.3969536172018));
#98683=CARTESIAN_POINT('Ctrl Pts',(-12.6180608664011,0.708,24.7854940213506));
#98684=CARTESIAN_POINT('Ctrl Pts',(-13.1636737275955,0.708,26.8000502819042));
#98685=CARTESIAN_POINT('Ctrl Pts',(-13.5640592992395,0.708,28.1311741992264));
#98686=CARTESIAN_POINT('Ctrl Pts',(-13.8109276823942,0.708,28.866880021582));
#98687=CARTESIAN_POINT('Ctrl Pts',(-14.0759824773703,0.708,29.5971513030824));
#98688=CARTESIAN_POINT('Ctrl Pts',(-14.3904642268911,0.708,30.3313802830276));
#98689=CARTESIAN_POINT('Ctrl Pts',(-14.7367190536345,0.708,31.1084918464257));
#98690=CARTESIAN_POINT('Ctrl Pts',(-14.9676192527248,0.708,31.7259447042262));
#98691=CARTESIAN_POINT('Ctrl Pts',(-15.0634216666442,0.708,32.3065851128709));
#98692=CARTESIAN_POINT('Ctrl Pts',(-14.995310469097,0.708,32.799630218064));
#98693=CARTESIAN_POINT('Ctrl Pts',(-14.8237837226447,0.708,33.2599421532119));
#98694=CARTESIAN_POINT('Ctrl Pts',(-14.4768570601396,0.708,33.7323460288388));
#98695=CARTESIAN_POINT('Ctrl Pts',(-13.8140058769173,0.708,34.312200058379));
#98696=CARTESIAN_POINT('Ctrl Pts',(-12.9275584185962,0.708,34.852988598105));
#98697=CARTESIAN_POINT('Ctrl Pts',(-11.9601501028038,0.708,35.5083657619793));
#98698=CARTESIAN_POINT('Ctrl Pts',(-11.2784416996154,0.708,36.394137190602));
#98699=CARTESIAN_POINT('Ctrl Pts',(-11.0126908986932,0.708,37.488108200426));
#98700=CARTESIAN_POINT('Ctrl Pts',(-11.1733979901704,0.708,38.6029533695122));
#98701=CARTESIAN_POINT('Ctrl Pts',(-11.6861322554559,0.708,39.6452112093278));
#98702=CARTESIAN_POINT('Ctrl Pts',(-12.2174647212886,0.708,40.5301529508079));
#98703=CARTESIAN_POINT('Ctrl Pts',(-12.5379395610492,0.708,41.3444180220226));
#98704=CARTESIAN_POINT('Ctrl Pts',(-12.6261829247595,0.708,41.7867213486289));
#98705=CARTESIAN_POINT('Ctrl Pts',(-12.6467363234665,0.708,42.0099427937538));
#98706=CARTESIAN_POINT('',(-8.14898645568467,0.708,10.8564616996593));
#98707=CARTESIAN_POINT('Ctrl Pts',(-12.6467363234665,0.708,42.0099427937538));
#98708=CARTESIAN_POINT('Ctrl Pts',(-12.6261829247595,0.708,41.7867213486289));
#98709=CARTESIAN_POINT('Ctrl Pts',(-12.5379395610492,0.708,41.3444180220226));
#98710=CARTESIAN_POINT('Ctrl Pts',(-12.2174647212886,0.708,40.5301529508079));
#98711=CARTESIAN_POINT('Ctrl Pts',(-11.6861322554559,0.708,39.6452112093278));
#98712=CARTESIAN_POINT('Ctrl Pts',(-11.1733979901704,0.708,38.6029533695122));
#98713=CARTESIAN_POINT('Ctrl Pts',(-11.0126908986932,0.708,37.488108200426));
#98714=CARTESIAN_POINT('Ctrl Pts',(-11.2784416996154,0.708,36.394137190602));
#98715=CARTESIAN_POINT('Ctrl Pts',(-11.9601501028038,0.708,35.5083657619793));
#98716=CARTESIAN_POINT('Ctrl Pts',(-12.9275584185962,0.708,34.852988598105));
#98717=CARTESIAN_POINT('Ctrl Pts',(-13.8140058769173,0.708,34.312200058379));
#98718=CARTESIAN_POINT('Ctrl Pts',(-14.4768570601396,0.708,33.7323460288388));
#98719=CARTESIAN_POINT('Ctrl Pts',(-14.8237837226447,0.708,33.2599421532119));
#98720=CARTESIAN_POINT('Ctrl Pts',(-14.995310469097,0.708,32.799630218064));
#98721=CARTESIAN_POINT('Ctrl Pts',(-15.0634216666442,0.708,32.3065851128709));
#98722=CARTESIAN_POINT('Ctrl Pts',(-14.9676192527248,0.708,31.7259447042262));
#98723=CARTESIAN_POINT('Ctrl Pts',(-14.7367190536345,0.708,31.1084918464257));
#98724=CARTESIAN_POINT('Ctrl Pts',(-14.3904642268911,0.708,30.3313802830276));
#98725=CARTESIAN_POINT('Ctrl Pts',(-14.0759824773703,0.708,29.5971513030824));
#98726=CARTESIAN_POINT('Ctrl Pts',(-13.8109276823942,0.708,28.866880021582));
#98727=CARTESIAN_POINT('Ctrl Pts',(-13.5640592992395,0.708,28.1311741992264));
#98728=CARTESIAN_POINT('Ctrl Pts',(-13.1636737275955,0.708,26.8000502819042));
#98729=CARTESIAN_POINT('Ctrl Pts',(-12.6180608664011,0.708,24.7854940213506));
#98730=CARTESIAN_POINT('Ctrl Pts',(-11.9597534877299,0.708,22.3969536172018));
#98731=CARTESIAN_POINT('Ctrl Pts',(-11.0105529606629,0.708,19.3229835736891));
#98732=CARTESIAN_POINT('Ctrl Pts',(-10.0162479906236,0.708,16.3421552779583));
#98733=CARTESIAN_POINT('Ctrl Pts',(-9.00140202108135,0.708,13.1987032575008));
#98734=CARTESIAN_POINT('Ctrl Pts',(-8.42682850340027,0.708,11.6200722130106));
#98735=CARTESIAN_POINT('Ctrl Pts',(-8.14898645568467,0.708,10.8564616996593));
#98736=CARTESIAN_POINT('Origin',(-7.86706805722818,0.708,10.9590385811275));
#98737=CARTESIAN_POINT('Ctrl Pts',(-7.0176,-4.08,6.528));
#98738=CARTESIAN_POINT('Ctrl Pts',(-7.0176,10.608,6.528));
#98739=CARTESIAN_POINT('Ctrl Pts',(-7.02630542760862,-4.08,6.62809945148413));
#98740=CARTESIAN_POINT('Ctrl Pts',(-7.02630542760862,10.608,6.62809945148413));
#98741=CARTESIAN_POINT('Ctrl Pts',(-7.04627094533223,-4.08,6.82892101239418));
#98742=CARTESIAN_POINT('Ctrl Pts',(-7.04627094533223,10.608,6.82892101239418));
#98743=CARTESIAN_POINT('Ctrl Pts',(-7.0838832606686,-4.08,7.13202122232862));
#98744=CARTESIAN_POINT('Ctrl Pts',(-7.0838832606686,10.608,7.13202122232862));
#98745=CARTESIAN_POINT('Ctrl Pts',(-7.14936655486467,-4.08,7.5398929237269));
#98746=CARTESIAN_POINT('Ctrl Pts',(-7.14936655486467,10.608,7.5398929237269));
#98747=CARTESIAN_POINT('Ctrl Pts',(-7.25661399291583,-4.08,8.05627564242548));
#98748=CARTESIAN_POINT('Ctrl Pts',(-7.25661399291583,10.608,8.05627564242548));
#98749=CARTESIAN_POINT('Ctrl Pts',(-7.38869925602642,-4.08,8.58014320427852));
#98750=CARTESIAN_POINT('Ctrl Pts',(-7.38869925602642,10.608,8.58014320427852));
#98751=CARTESIAN_POINT('Ctrl Pts',(-7.54448066029731,-4.08,9.11333934177059));
#98752=CARTESIAN_POINT('Ctrl Pts',(-7.54448066029731,10.608,9.11333934177059));
#98753=CARTESIAN_POINT('Ctrl Pts',(-7.72198141303516,-4.08,9.65899621296523));
#98754=CARTESIAN_POINT('Ctrl Pts',(-7.72198141303516,10.608,9.65899621296523));
#98755=CARTESIAN_POINT('Ctrl Pts',(-7.91830414508894,-4.08,10.2215845279079));
#98756=CARTESIAN_POINT('Ctrl Pts',(-7.91830414508894,10.608,10.2215845279079));
#98757=CARTESIAN_POINT('Ctrl Pts',(-8.13003837377838,-4.08,10.8059423149972));
#98758=CARTESIAN_POINT('Ctrl Pts',(-8.13003837377838,10.608,10.8059423149972));
#98759=CARTESIAN_POINT('Ctrl Pts',(-8.35357461247532,-4.08,11.4165038934416));
#98760=CARTESIAN_POINT('Ctrl Pts',(-8.35357461247532,10.608,11.4165038934416));
#98761=CARTESIAN_POINT('Ctrl Pts',(-8.58546625544539,-4.08,12.056408353432));
#98762=CARTESIAN_POINT('Ctrl Pts',(-8.58546625544539,10.608,12.056408353432));
#98763=CARTESIAN_POINT('Ctrl Pts',(-8.82274435252017,-4.08,12.7267521352155));
#98764=CARTESIAN_POINT('Ctrl Pts',(-8.82274435252017,10.608,12.7267521352155));
#98765=CARTESIAN_POINT('Ctrl Pts',(-9.06332174046713,-4.08,13.4255332425537));
#98766=CARTESIAN_POINT('Ctrl Pts',(-9.06332174046713,10.608,13.4255332425537));
#98767=CARTESIAN_POINT('Ctrl Pts',(-9.3059347889759,-4.08,14.1482310979449));
#98768=CARTESIAN_POINT('Ctrl Pts',(-9.3059347889759,10.608,14.1482310979449));
#98769=CARTESIAN_POINT('Ctrl Pts',(-9.54992705159325,-4.08,14.8889496618037));
#98770=CARTESIAN_POINT('Ctrl Pts',(-9.54992705159325,10.608,14.8889496618037));
#98771=CARTESIAN_POINT('Ctrl Pts',(-9.79508602811817,-4.08,15.6413708166808));
#98772=CARTESIAN_POINT('Ctrl Pts',(-9.79508602811817,10.608,15.6413708166808));
#98773=CARTESIAN_POINT('Ctrl Pts',(-10.0414581777666,-4.08,16.3997893456033));
#98774=CARTESIAN_POINT('Ctrl Pts',(-10.0414581777666,10.608,16.3997893456033));
#98775=CARTESIAN_POINT('Ctrl Pts',(-10.2891746222215,-4.08,17.1601046394451));
#98776=CARTESIAN_POINT('Ctrl Pts',(-10.2891746222215,10.608,17.1601046394451));
#98777=CARTESIAN_POINT('Ctrl Pts',(-10.5382704524098,-4.08,17.920853526763));
#98778=CARTESIAN_POINT('Ctrl Pts',(-10.5382704524098,10.608,17.920853526763));
#98779=CARTESIAN_POINT('Ctrl Pts',(-10.7885123454294,-4.08,18.6841717409417));
#98780=CARTESIAN_POINT('Ctrl Pts',(-10.7885123454294,10.608,18.6841717409417));
#98781=CARTESIAN_POINT('Ctrl Pts',(-11.0394491705041,-4.08,19.454441635642));
#98782=CARTESIAN_POINT('Ctrl Pts',(-11.0394491705041,10.608,19.454441635642));
#98783=CARTESIAN_POINT('Ctrl Pts',(-11.2904565074993,-4.08,20.2370106667962));
#98784=CARTESIAN_POINT('Ctrl Pts',(-11.2904565074993,10.608,20.2370106667962));
#98785=CARTESIAN_POINT('Ctrl Pts',(-11.5407830377124,-4.08,21.0368752434028));
#98786=CARTESIAN_POINT('Ctrl Pts',(-11.5407830377124,10.608,21.0368752434028));
#98787=CARTESIAN_POINT('Ctrl Pts',(-11.7895961018281,-4.08,21.8574023995577));
#98788=CARTESIAN_POINT('Ctrl Pts',(-11.7895961018281,10.608,21.8574023995577));
#98789=CARTESIAN_POINT('Ctrl Pts',(-12.0360270133741,-4.08,22.6989792594677));
#98790=CARTESIAN_POINT('Ctrl Pts',(-12.0360270133741,10.608,22.6989792594677));
#98791=CARTESIAN_POINT('Ctrl Pts',(-12.2792174635072,-4.08,23.5578155700236));
#98792=CARTESIAN_POINT('Ctrl Pts',(-12.2792174635072,10.608,23.5578155700236));
#98793=CARTESIAN_POINT('Ctrl Pts',(-12.5183627807975,-4.08,24.4243412707551));
#98794=CARTESIAN_POINT('Ctrl Pts',(-12.5183627807975,10.608,24.4243412707551));
#98795=CARTESIAN_POINT('Ctrl Pts',(-12.7527764582694,-4.08,25.2847489984795));
#98796=CARTESIAN_POINT('Ctrl Pts',(-12.7527764582694,10.608,25.2847489984795));
#98797=CARTESIAN_POINT('Ctrl Pts',(-12.9819542120743,-4.08,26.1231223827779));
#98798=CARTESIAN_POINT('Ctrl Pts',(-12.9819542120743,10.608,26.1231223827779));
#98799=CARTESIAN_POINT('Ctrl Pts',(-13.2056470980325,-4.08,26.9233802340012));
#98800=CARTESIAN_POINT('Ctrl Pts',(-13.2056470980325,10.608,26.9233802340012));
#98801=CARTESIAN_POINT('Ctrl Pts',(-13.4239120315545,-4.08,27.6712450999953));
#98802=CARTESIAN_POINT('Ctrl Pts',(-13.4239120315545,10.608,27.6712450999953));
#98803=CARTESIAN_POINT('Ctrl Pts',(-13.6372170146976,-4.08,28.356323880339));
#98804=CARTESIAN_POINT('Ctrl Pts',(-13.6372170146976,10.608,28.356323880339));
#98805=CARTESIAN_POINT('Ctrl Pts',(-13.8464193628061,-4.08,28.9738645264783));
#98806=CARTESIAN_POINT('Ctrl Pts',(-13.8464193628061,10.608,28.9738645264783));
#98807=CARTESIAN_POINT('Ctrl Pts',(-14.0530623083977,-4.08,29.5273742099472));
#98808=CARTESIAN_POINT('Ctrl Pts',(-14.0530623083977,10.608,29.5273742099472));
#98809=CARTESIAN_POINT('Ctrl Pts',(-14.2582197141431,-4.08,30.027253712516));
#98810=CARTESIAN_POINT('Ctrl Pts',(-14.2582197141431,10.608,30.027253712516));
#98811=CARTESIAN_POINT('Ctrl Pts',(-14.4606799971795,-4.08,30.487449167326));
#98812=CARTESIAN_POINT('Ctrl Pts',(-14.4606799971795,10.608,30.487449167326));
#98813=CARTESIAN_POINT('Ctrl Pts',(-14.6552019413825,-4.08,30.9226538837488));
#98814=CARTESIAN_POINT('Ctrl Pts',(-14.6552019413825,10.608,30.9226538837488));
#98815=CARTESIAN_POINT('Ctrl Pts',(-14.8310295566836,-4.08,31.3454571086889));
#98816=CARTESIAN_POINT('Ctrl Pts',(-14.8310295566836,10.608,31.3454571086889));
#98817=CARTESIAN_POINT('Ctrl Pts',(-14.9695221769896,-4.08,31.7630680429362));
#98818=CARTESIAN_POINT('Ctrl Pts',(-14.9695221769896,10.608,31.7630680429362));
#98819=CARTESIAN_POINT('Ctrl Pts',(-15.048097310419,-4.08,32.1776017680614));
#98820=CARTESIAN_POINT('Ctrl Pts',(-15.048097310419,10.608,32.1776017680614));
#98821=CARTESIAN_POINT('Ctrl Pts',(-15.0458732472955,-4.08,32.5872458409768));
#98822=CARTESIAN_POINT('Ctrl Pts',(-15.0458732472955,10.608,32.5872458409768));
#98823=CARTESIAN_POINT('Ctrl Pts',(-14.9484729279408,-4.08,32.9871564326141));
#98824=CARTESIAN_POINT('Ctrl Pts',(-14.9484729279408,10.608,32.9871564326141));
#98825=CARTESIAN_POINT('Ctrl Pts',(-14.7538514224946,-4.08,33.3703634670857));
#98826=CARTESIAN_POINT('Ctrl Pts',(-14.7538514224946,10.608,33.3703634670857));
#98827=CARTESIAN_POINT('Ctrl Pts',(-14.4705118919343,-4.08,33.7298729261475));
#98828=CARTESIAN_POINT('Ctrl Pts',(-14.4705118919343,10.608,33.7298729261475));
#98829=CARTESIAN_POINT('Ctrl Pts',(-14.1146548169613,-4.08,34.0610864824011));
#98830=CARTESIAN_POINT('Ctrl Pts',(-14.1146548169613,10.608,34.0610864824011));
#98831=CARTESIAN_POINT('Ctrl Pts',(-13.7077402642199,-4.08,34.3639065568129));
#98832=CARTESIAN_POINT('Ctrl Pts',(-13.7077402642199,10.608,34.3639065568129));
#98833=CARTESIAN_POINT('Ctrl Pts',(-13.2738213034502,-4.08,34.6454993802762));
#98834=CARTESIAN_POINT('Ctrl Pts',(-13.2738213034502,10.608,34.6454993802762));
#98835=CARTESIAN_POINT('Ctrl Pts',(-12.837485108751,-4.08,34.9181535900641));
#98836=CARTESIAN_POINT('Ctrl Pts',(-12.837485108751,10.608,34.9181535900641));
#98837=CARTESIAN_POINT('Ctrl Pts',(-12.4217894296783,-4.08,35.1961083216792));
#98838=CARTESIAN_POINT('Ctrl Pts',(-12.4217894296783,10.608,35.1961083216792));
#98839=CARTESIAN_POINT('Ctrl Pts',(-12.046351900761,-4.08,35.4928858294795));
#98840=CARTESIAN_POINT('Ctrl Pts',(-12.046351900761,10.608,35.4928858294795));
#98841=CARTESIAN_POINT('Ctrl Pts',(-11.7250208885935,-4.08,35.8180786547651));
#98842=CARTESIAN_POINT('Ctrl Pts',(-11.7250208885935,10.608,35.8180786547651));
#98843=CARTESIAN_POINT('Ctrl Pts',(-11.464839430663,-4.08,36.175427704157));
#98844=CARTESIAN_POINT('Ctrl Pts',(-11.464839430663,10.608,36.175427704157));
#98845=CARTESIAN_POINT('Ctrl Pts',(-11.268703490835,-4.08,36.5642101034686));
#98846=CARTESIAN_POINT('Ctrl Pts',(-11.268703490835,10.608,36.5642101034686));
#98847=CARTESIAN_POINT('Ctrl Pts',(-11.1371764695444,-4.08,36.980031199346));
#98848=CARTESIAN_POINT('Ctrl Pts',(-11.1371764695444,10.608,36.980031199346));
#98849=CARTESIAN_POINT('Ctrl Pts',(-11.0709679278875,-4.08,37.4158119460019));
#98850=CARTESIAN_POINT('Ctrl Pts',(-11.0709679278875,10.608,37.4158119460019));
#98851=CARTESIAN_POINT('Ctrl Pts',(-11.0720880317847,-4.08,37.8627943234178));
#98852=CARTESIAN_POINT('Ctrl Pts',(-11.0720880317847,10.608,37.8627943234178));
#98853=CARTESIAN_POINT('Ctrl Pts',(-11.1408514716218,-4.08,38.3120740300041));
#98854=CARTESIAN_POINT('Ctrl Pts',(-11.1408514716218,10.608,38.3120740300041));
#98855=CARTESIAN_POINT('Ctrl Pts',(-11.2737132025484,-4.08,38.755967364186));
#98856=CARTESIAN_POINT('Ctrl Pts',(-11.2737132025484,10.608,38.755967364186));
#98857=CARTESIAN_POINT('Ctrl Pts',(-11.4604343652129,-4.08,39.1895865074084));
#98858=CARTESIAN_POINT('Ctrl Pts',(-11.4604343652129,10.608,39.1895865074084));
#98859=CARTESIAN_POINT('Ctrl Pts',(-11.6825137471463,-4.08,39.6119151152234));
#98860=CARTESIAN_POINT('Ctrl Pts',(-11.6825137471463,10.608,39.6119151152234));
#98861=CARTESIAN_POINT('Ctrl Pts',(-11.9174888407557,-4.08,40.0243956758678));
#98862=CARTESIAN_POINT('Ctrl Pts',(-11.9174888407557,10.608,40.0243956758678));
#98863=CARTESIAN_POINT('Ctrl Pts',(-12.1425787135405,-4.08,40.4298136303268));
#98864=CARTESIAN_POINT('Ctrl Pts',(-12.1425787135405,10.608,40.4298136303268));
#98865=CARTESIAN_POINT('Ctrl Pts',(-12.3384198670367,-4.08,40.831110140755));
#98866=CARTESIAN_POINT('Ctrl Pts',(-12.3384198670367,10.608,40.831110140755));
#98867=CARTESIAN_POINT('Ctrl Pts',(-12.4931832123844,-4.08,41.2301191386975));
#98868=CARTESIAN_POINT('Ctrl Pts',(-12.4931832123844,10.608,41.2301191386975));
#98869=CARTESIAN_POINT('Ctrl Pts',(-12.5795001090599,-4.08,41.5482135599962));
#98870=CARTESIAN_POINT('Ctrl Pts',(-12.5795001090599,10.608,41.5482135599962));
#98871=CARTESIAN_POINT('Ctrl Pts',(-12.6222832973086,-4.08,41.7862967053278));
#98872=CARTESIAN_POINT('Ctrl Pts',(-12.6222832973086,10.608,41.7862967053278));
#98873=CARTESIAN_POINT('Ctrl Pts',(-12.6410531968159,-4.08,41.9448017311272));
#98874=CARTESIAN_POINT('Ctrl Pts',(-12.6410531968159,10.608,41.9448017311272));
#98875=CARTESIAN_POINT('Ctrl Pts',(-12.648,-4.08,42.024));
#98876=CARTESIAN_POINT('Ctrl Pts',(-12.648,10.608,42.024));
#98877=CARTESIAN_POINT('',(-8.26785692826842,0.924,11.1826993255826));
#98878=CARTESIAN_POINT('Ctrl Pts',(-8.26785692826842,0.924,11.1826993255826));
#98879=CARTESIAN_POINT('Ctrl Pts',(-8.54361306627396,0.924,11.9392205016032));
#98880=CARTESIAN_POINT('Ctrl Pts',(-9.09212599991816,0.924,13.4722442013831));
#98881=CARTESIAN_POINT('Ctrl Pts',(-10.0793574851517,0.924,16.5387499289064));
#98882=CARTESIAN_POINT('Ctrl Pts',(-11.0930194846002,0.924000000000001,
19.5704317186628));
#98883=CARTESIAN_POINT('Ctrl Pts',(-12.0379540421531,0.924,22.6694941250056));
#98884=CARTESIAN_POINT('Ctrl Pts',(-12.676785825845,0.924,25.0072588185284));
#98885=CARTESIAN_POINT('Ctrl Pts',(-13.3134204366261,0.924,27.3367371289618));
#98886=CARTESIAN_POINT('Ctrl Pts',(-13.8892654107988,0.924,29.1794300100813));
#98887=CARTESIAN_POINT('Ctrl Pts',(-14.4608280370914,0.924,30.4864933436934));
#98888=CARTESIAN_POINT('Ctrl Pts',(-14.7969073569086,0.924,31.255443467967));
#98889=CARTESIAN_POINT('Ctrl Pts',(-15.0048415747375,0.924,31.8645500407944));
#98890=CARTESIAN_POINT('Ctrl Pts',(-15.0761879359655,0.924,32.5848794176223));
#98891=CARTESIAN_POINT('Ctrl Pts',(-14.8238908844334,0.923999999999999,
33.2948194019013));
#98892=CARTESIAN_POINT('Ctrl Pts',(-14.3877781203166,0.924,33.8201146754649));
#98893=CARTESIAN_POINT('Ctrl Pts',(-13.8907462265714,0.924,34.2368869147185));
#98894=CARTESIAN_POINT('Ctrl Pts',(-13.3725424358171,0.924,34.5834843095939));
#98895=CARTESIAN_POINT('Ctrl Pts',(-12.6910734237184,0.924,35.0111461040952));
#98896=CARTESIAN_POINT('Ctrl Pts',(-11.9032876540853,0.924,35.5613424749907));
#98897=CARTESIAN_POINT('Ctrl Pts',(-11.2537874910971,0.924,36.4518523554272));
#98898=CARTESIAN_POINT('Ctrl Pts',(-11.0113749925991,0.924,37.5398403917748));
#98899=CARTESIAN_POINT('Ctrl Pts',(-11.1874609600943,0.924,38.6392410506538));
#98900=CARTESIAN_POINT('Ctrl Pts',(-11.6999497096383,0.924,39.6710971369163));
#98901=CARTESIAN_POINT('Ctrl Pts',(-12.3296022375865,0.924,40.7164504695946));
#98902=CARTESIAN_POINT('Ctrl Pts',(-12.6060713603138,0.924,41.5682984715533));
#98903=CARTESIAN_POINT('Ctrl Pts',(-12.6467363234665,0.924,42.0099427937538));
#98904=CARTESIAN_POINT('',(-7.97548942359086,1.15565058469624,10.3765642386027));
#98905=CARTESIAN_POINT('Ctrl Pts',(-7.97548942359086,1.15565058469624,10.3765642386027));
#98906=CARTESIAN_POINT('Ctrl Pts',(-8.06230799714572,1.0034429248949,10.6189650635473));
#98907=CARTESIAN_POINT('Ctrl Pts',(-8.16503623275751,0.92400000000006,10.9006166345145));
#98908=CARTESIAN_POINT('Ctrl Pts',(-8.2678569282683,0.924,11.1826993255823));
#98909=CARTESIAN_POINT('',(-7.19596078944639,2.8235504329007,7.74940308223659));
#98910=CARTESIAN_POINT('Ctrl Pts',(-7.19596078944639,2.8235504329007,7.74940308223659));
#98911=CARTESIAN_POINT('Ctrl Pts',(-7.22233262615032,2.74030396336476,7.8793256784926));
#98912=CARTESIAN_POINT('Ctrl Pts',(-7.25093335954429,2.65731106826831,8.00908682877084));
#98913=CARTESIAN_POINT('Ctrl Pts',(-7.28159746422587,2.5745495730776,8.13865166883888));
#98914=CARTESIAN_POINT('Ctrl Pts',(-7.31161939938325,2.49352127409596,8.26550315423493));
#98915=CARTESIAN_POINT('Ctrl Pts',(-7.34361926028415,2.41271478452361,8.39216624339057));
#98916=CARTESIAN_POINT('Ctrl Pts',(-7.3774062658177,2.33210929399645,8.5186423305201));
#98917=CARTESIAN_POINT('Ctrl Pts',(-7.41168327760693,2.25033479798993,8.6469526753149));
#98918=CARTESIAN_POINT('Ctrl Pts',(-7.4477997057716,2.16876717340375,8.77507050652281));
#98919=CARTESIAN_POINT('Ctrl Pts',(-7.48551767859797,2.08738469125336,8.90303614781032));
#98920=CARTESIAN_POINT('Ctrl Pts',(-7.52666669782826,1.9985991847143,9.04264228885072));
#98921=CARTESIAN_POINT('Ctrl Pts',(-7.5697219334645,1.91003403589183,9.18206778255516));
#98922=CARTESIAN_POINT('Ctrl Pts',(-7.61432732220447,1.82166103025293,9.32140797710534));
#98923=CARTESIAN_POINT('Ctrl Pts',(-7.6664953999531,1.71830468790771,9.48437281853242));
#98924=CARTESIAN_POINT('Ctrl Pts',(-7.72078165008511,1.61521116652034,9.64722711387514));
#98925=CARTESIAN_POINT('Ctrl Pts',(-7.77656785595829,1.5123353298502,9.81013231365598));
#98926=CARTESIAN_POINT('Ctrl Pts',(-7.82095433614413,1.43048182835304,9.93974837750305));
#98927=CARTESIAN_POINT('Ctrl Pts',(-7.8662889047216,1.34876613526015,10.0693975485112));
#98928=CARTESIAN_POINT('Ctrl Pts',(-7.9122593737334,1.26716551546311,10.1991238167179));
#98929=CARTESIAN_POINT('Ctrl Pts',(-7.93321343005476,1.22997068104352,10.2582550718213));
#98930=CARTESIAN_POINT('Ctrl Pts',(-7.9542997016531,1.19279975515514,10.3174017130308));
#98931=CARTESIAN_POINT('Ctrl Pts',(-7.97548942359086,1.15565058469625,10.3765642386027));
#98932=CARTESIAN_POINT('',(-7.10945460790939,2.964,7.27219995625739));
#98933=CARTESIAN_POINT('Ctrl Pts',(-7.10945460790939,2.964,7.27219995625739));
#98934=CARTESIAN_POINT('Ctrl Pts',(-7.13617164034088,2.964,7.44003720108978));
#98935=CARTESIAN_POINT('Ctrl Pts',(-7.16707514154032,2.91473210657155,7.60709602897267));
#98936=CARTESIAN_POINT('Ctrl Pts',(-7.19596078944639,2.8235504329007,7.74940308223659));
#98937=CARTESIAN_POINT('',(-7.01760000081282,2.964,6.52800003819785));
#98938=CARTESIAN_POINT('Ctrl Pts',(-7.01760000330315,2.964,6.52800003798128));
#98939=CARTESIAN_POINT('Ctrl Pts',(-7.02446531775896,2.964,6.60694092546319));
#98940=CARTESIAN_POINT('Ctrl Pts',(-7.03215675137159,2.964,6.68470062724588));
#98941=CARTESIAN_POINT('Ctrl Pts',(-7.04064330589647,2.964,6.76177920847414));
#98942=CARTESIAN_POINT('Ctrl Pts',(-7.04922558187721,2.964,6.83972717361903));
#98943=CARTESIAN_POINT('Ctrl Pts',(-7.05862115895179,2.964,6.91697853001615));
#98944=CARTESIAN_POINT('Ctrl Pts',(-7.06884967735363,2.964,6.99406426404567));
#98945=CARTESIAN_POINT('Ctrl Pts',(-7.07915808333351,2.964,7.07175205913145));
#98946=CARTESIAN_POINT('Ctrl Pts',(-7.09031256144649,2.964,7.1492715590365));
#98947=CARTESIAN_POINT('Ctrl Pts',(-7.10238379369393,2.964,7.22718103044211));
#98948=CARTESIAN_POINT('Ctrl Pts',(-7.10470640653238,2.964,7.24217150820068));
#98949=CARTESIAN_POINT('Ctrl Pts',(-7.10706310656637,2.964,7.25717646899493));
#98950=CARTESIAN_POINT('Ctrl Pts',(-7.10945460790939,2.964,7.27219995625739));
#98951=CARTESIAN_POINT('',(-7.0176,2.748,6.528));
#98952=CARTESIAN_POINT('',(-7.0176,-4.08,6.528));
#98953=CARTESIAN_POINT('',(-7.06369006012712,2.748,6.95461383265843));
#98954=CARTESIAN_POINT('Origin',(-17.3375887932806,2.748,5.62885644979173));
#98955=CARTESIAN_POINT('',(-7.19430053092012,2.51634941530375,7.74120895321998));
#98956=CARTESIAN_POINT('Ctrl Pts',(-7.19430053092012,2.51634941530376,7.74120895321997));
#98957=CARTESIAN_POINT('Ctrl Pts',(-7.18139423288357,2.5572388274877,7.67739535408007));
#98958=CARTESIAN_POINT('Ctrl Pts',(-7.16841680020877,2.59304356056116,7.61051677367225));
#98959=CARTESIAN_POINT('Ctrl Pts',(-7.15568446739969,2.62349886615165,7.54138656787107));
#98960=CARTESIAN_POINT('Ctrl Pts',(-7.14341508067495,2.65284682050636,7.47476992800986));
#98961=CARTESIAN_POINT('Ctrl Pts',(-7.1313737350991,2.67722728429196,7.40606237419146));
#98962=CARTESIAN_POINT('Ctrl Pts',(-7.11979834628682,2.69640335049437,7.33597973689174));
#98963=CARTESIAN_POINT('Ctrl Pts',(-7.10857994715557,2.71498801904542,7.26805847652209));
#98964=CARTESIAN_POINT('Ctrl Pts',(-7.0977993730232,2.72868435141184,7.1988456068992));
#98965=CARTESIAN_POINT('Ctrl Pts',(-7.08762578934646,2.73727669046519,7.12898188155835));
#98966=CARTESIAN_POINT('Ctrl Pts',(-7.07920950084515,2.74438486460243,7.07118580036135));
#98967=CARTESIAN_POINT('Ctrl Pts',(-7.0712078148154,2.748,7.01294410869989));
#98968=CARTESIAN_POINT('Ctrl Pts',(-7.06369006012712,2.748,6.95461383265843));
#98969=CARTESIAN_POINT('',(-7.97249537063732,0.848449567099298,10.3682028984961));
#98970=CARTESIAN_POINT('Ctrl Pts',(-7.97249537063731,0.848449567099298,
10.3682028984961));
#98971=CARTESIAN_POINT('Ctrl Pts',(-7.65957903289542,1.39732053099838,9.49414527429354));
#98972=CARTESIAN_POINT('Ctrl Pts',(-7.37274783895309,1.9509970957918,8.62351966308919));
#98973=CARTESIAN_POINT('Ctrl Pts',(-7.19430053092012,2.51634941530375,7.74120895321998));
#98974=CARTESIAN_POINT('Ctrl Pts',(-8.14898645568466,0.707999999999999,
10.8564616996593));
#98975=CARTESIAN_POINT('Ctrl Pts',(-8.12815013435031,0.707999999999999,
10.7991959468286));
#98976=CARTESIAN_POINT('Ctrl Pts',(-8.10733389973439,0.713424220187055,
10.7419087307375));
#98977=CARTESIAN_POINT('Ctrl Pts',(-8.08689701837362,0.724116204510082,
10.6855367371928));
#98978=CARTESIAN_POINT('Ctrl Pts',(-8.06554794403206,0.735285421776732,
10.6266485996279));
#98979=CARTESIAN_POINT('Ctrl Pts',(-8.04461331168835,0.752203147474417,
10.5687589560619));
#98980=CARTESIAN_POINT('Ctrl Pts',(-8.02447437612234,0.774691026458215,
10.5128836557502));
#98981=CARTESIAN_POINT('Ctrl Pts',(-8.00642490774828,0.794845729232223,
10.4628055638589));
#98982=CARTESIAN_POINT('Ctrl Pts',(-7.98901420075669,0.819474709872172,
10.414344335255));
#98983=CARTESIAN_POINT('Ctrl Pts',(-7.97249537063731,0.848449567099298,
10.3682028984961));
#98984=CARTESIAN_POINT('Ctrl Pts',(-12.348,1.224,42.03744932101));
#98985=CARTESIAN_POINT('Ctrl Pts',(-12.3110725606702,1.224,41.6363966051328));
#98986=CARTESIAN_POINT('Ctrl Pts',(-12.0609852952635,1.224,40.8549204601091));
#98987=CARTESIAN_POINT('Ctrl Pts',(-11.4450821737987,1.224,39.8274092249604));
#98988=CARTESIAN_POINT('Ctrl Pts',(-10.8997688026688,1.224,38.7409075676707));
#98989=CARTESIAN_POINT('Ctrl Pts',(-10.7043533514793,1.224,37.5315890187733));
#98990=CARTESIAN_POINT('Ctrl Pts',(-10.9709851394883,1.224,36.3263525491271));
#98991=CARTESIAN_POINT('Ctrl Pts',(-11.6986135266186,1.224,35.3339416136743));
#98992=CARTESIAN_POINT('Ctrl Pts',(-12.5309171577631,1.224,34.7574741120408));
#98993=CARTESIAN_POINT('Ctrl Pts',(-13.2114636130569,1.224,34.3298336160849));
#98994=CARTESIAN_POINT('Ctrl Pts',(-13.7131082734894,1.224,33.9932968374398));
#98995=CARTESIAN_POINT('Ctrl Pts',(-14.1769757204202,1.224,33.6048339401135));
#98996=CARTESIAN_POINT('Ctrl Pts',(-14.5620228329377,1.224,33.1340383684088));
#98997=CARTESIAN_POINT('Ctrl Pts',(-14.7683961662382,1.224,32.5514380647304));
#98998=CARTESIAN_POINT('Ctrl Pts',(-14.711659402932,1.224,31.939868704061));
#98999=CARTESIAN_POINT('Ctrl Pts',(-14.5189773065471,1.224,31.3678083420515));
#99000=CARTESIAN_POINT('Ctrl Pts',(-14.1888423807734,1.224,30.613847819264));
#99001=CARTESIAN_POINT('Ctrl Pts',(-13.6063457415431,1.224,29.2804450588471));
#99002=CARTESIAN_POINT('Ctrl Pts',(-13.0245909094872,1.224,27.4180026826501));
#99003=CARTESIAN_POINT('Ctrl Pts',(-12.3871316955906,1.224,25.0852094102837));
#99004=CARTESIAN_POINT('Ctrl Pts',(-11.7493811375928,1.224,22.7517028806517));
#99005=CARTESIAN_POINT('Ctrl Pts',(-10.8084555662763,1.224,19.6656582368069));
#99006=CARTESIAN_POINT('Ctrl Pts',(-9.79376320963301,1.224,16.6304717567395));
#99007=CARTESIAN_POINT('Ctrl Pts',(-8.80744652629141,1.224,13.5670274338247));
#99008=CARTESIAN_POINT('Ctrl Pts',(-8.26166260011136,1.224,12.0417095524852));
#99009=CARTESIAN_POINT('Ctrl Pts',(-7.98599766308436,1.224,11.2854385811275));
#99010=CARTESIAN_POINT('Ctrl Pts',(-12.4262089865969,1.224,42.0302481290138));
#99011=CARTESIAN_POINT('Ctrl Pts',(-12.3884597397384,1.224,41.6182718077793));
#99012=CARTESIAN_POINT('Ctrl Pts',(-12.1313110647987,1.224,40.8188312736214));
#99013=CARTESIAN_POINT('Ctrl Pts',(-11.5118493291914,1.224,39.7863371802633));
#99014=CARTESIAN_POINT('Ctrl Pts',(-10.9750998698324,1.224,38.7143350236826));
#99015=CARTESIAN_POINT('Ctrl Pts',(-10.7847684351755,1.224,37.5336806373346));
#99016=CARTESIAN_POINT('Ctrl Pts',(-11.0449682137518,1.224,36.3591917863843));
#99017=CARTESIAN_POINT('Ctrl Pts',(-11.7523600195699,1.224,35.3934310919955));
#99018=CARTESIAN_POINT('Ctrl Pts',(-12.5726728148048,1.224,34.8237749281237));
#99019=CARTESIAN_POINT('Ctrl Pts',(-13.2536375709064,1.224,34.3961247440975));
#99020=CARTESIAN_POINT('Ctrl Pts',(-13.7595078804483,1.224,34.0569555347383));
#99021=CARTESIAN_POINT('Ctrl Pts',(-14.2321163943034,1.224,33.6610389297134));
#99022=CARTESIAN_POINT('Ctrl Pts',(-14.6305352247796,1.224,33.1760304630879));
#99023=CARTESIAN_POINT('Ctrl Pts',(-14.8490560326206,1.224,32.5605118065707));
#99024=CARTESIAN_POINT('Ctrl Pts',(-14.7884740076186,1.224,31.9202106499033));
#99025=CARTESIAN_POINT('Ctrl Pts',(-14.5917916222844,1.224,31.3385534447848));
#99026=CARTESIAN_POINT('Ctrl Pts',(-14.2600864674804,1.224,30.5805368096967));
#99027=CARTESIAN_POINT('Ctrl Pts',(-13.6804549117615,1.224,29.2541245480614));
#99028=CARTESIAN_POINT('Ctrl Pts',(-13.1002241344054,1.224,27.3967600289198));
#99029=CARTESIAN_POINT('Ctrl Pts',(-12.4629663663438,1.224,25.0648149363375));
#99030=CARTESIAN_POINT('Ctrl Pts',(-11.8249399914061,1.224,22.7302062906546));
#99031=CARTESIAN_POINT('Ctrl Pts',(-10.8829597173486,1.224,19.6407501735903));
#99032=CARTESIAN_POINT('Ctrl Pts',(-9.86851299468442,1.224,16.6063977618495));
#99033=CARTESIAN_POINT('Ctrl Pts',(-8.88199052732757,1.224,13.5422656081676));
#99034=CARTESIAN_POINT('Ctrl Pts',(-8.33547603090265,1.224,12.014852000593));
#99035=CARTESIAN_POINT('Ctrl Pts',(-8.05978824615506,1.224,11.2585415069229));
#99036=CARTESIAN_POINT('Ctrl Pts',(-12.5819547309417,1.15894437659295,42.0159076413485));
#99037=CARTESIAN_POINT('Ctrl Pts',(-12.5422059135609,1.15894437659295,41.5828655760323));
#99038=CARTESIAN_POINT('Ctrl Pts',(-12.2713534566526,1.15894437659295,40.7465873386517));
#99039=CARTESIAN_POINT('Ctrl Pts',(-11.6447101463389,1.15894437659295,39.7048928283908));
#99040=CARTESIAN_POINT('Ctrl Pts',(-11.1250833790616,1.15894437659295,38.661317107898));
#99041=CARTESIAN_POINT('Ctrl Pts',(-10.9448216674133,1.15894437659295,37.5380048122601));
#99042=CARTESIAN_POINT('Ctrl Pts',(-11.1924245222642,1.15894437659295,36.4246263108199));
#99043=CARTESIAN_POINT('Ctrl Pts',(-11.8590135202287,1.15894437659295,35.5120005020376));
#99044=CARTESIAN_POINT('Ctrl Pts',(-12.6562264341236,1.15894437659295,34.9560623847726));
#99045=CARTESIAN_POINT('Ctrl Pts',(-13.3376146000376,1.15894437659295,34.528402435818));
#99046=CARTESIAN_POINT('Ctrl Pts',(-13.8521536514053,1.15894437659294,34.1839876724815));
#99047=CARTESIAN_POINT('Ctrl Pts',(-14.3420333075769,1.15894437659295,33.7733258205512));
#99048=CARTESIAN_POINT('Ctrl Pts',(-14.7670742413869,1.15894437659295,33.2598860740197));
#99049=CARTESIAN_POINT('Ctrl Pts',(-15.0094967148898,1.15894437659295,32.5778425903243));
#99050=CARTESIAN_POINT('Ctrl Pts',(-14.9413046656758,1.15894437659295,31.8809237312434));
#99051=CARTESIAN_POINT('Ctrl Pts',(-14.736672983979,1.15894437659295,31.27991937865));
#99052=CARTESIAN_POINT('Ctrl Pts',(-14.4018732837384,1.15894437659295,30.5141308692897));
#99053=CARTESIAN_POINT('Ctrl Pts',(-13.8279413241913,1.15894437659295,29.2014197421003));
#99054=CARTESIAN_POINT('Ctrl Pts',(-13.2507991784978,1.15894437659295,27.3543817300241));
#99055=CARTESIAN_POINT('Ctrl Pts',(-12.6139760164723,1.15894437659295,25.0241712948571));
#99056=CARTESIAN_POINT('Ctrl Pts',(-11.9753835861599,1.15894437659295,22.6873385363609));
#99057=CARTESIAN_POINT('Ctrl Pts',(-11.0313149108527,1.15894437659295,19.5910967451308));
#99058=CARTESIAN_POINT('Ctrl Pts',(-10.0174132153215,1.15894437659295,16.5585986749172));
#99059=CARTESIAN_POINT('Ctrl Pts',(-9.03040284012067,1.15894437659295,13.4928334566676));
#99060=CARTESIAN_POINT('Ctrl Pts',(-8.48247082810459,1.15894437659295,11.9614279444147));
#99061=CARTESIAN_POINT('Ctrl Pts',(-8.20673516090307,1.15894437659295,11.2049785466421));
#99062=CARTESIAN_POINT('Ctrl Pts',(-12.6467363234665,1.00253981633974,42.0099427937538));
#99063=CARTESIAN_POINT('Ctrl Pts',(-12.6060713603138,1.00253981633975,41.5682984715533));
#99064=CARTESIAN_POINT('Ctrl Pts',(-12.3296022375865,1.00253981633974,40.7164504695946));
#99065=CARTESIAN_POINT('Ctrl Pts',(-11.6999497096383,1.00253981633974,39.6710971369163));
#99066=CARTESIAN_POINT('Ctrl Pts',(-11.1874609600943,1.00253981633974,38.6392410506538));
#99067=CARTESIAN_POINT('Ctrl Pts',(-11.0113749925991,1.00253981633974,37.5398403917748));
#99068=CARTESIAN_POINT('Ctrl Pts',(-11.2537874910971,1.00253981633974,36.4518523554272));
#99069=CARTESIAN_POINT('Ctrl Pts',(-11.9032876540853,1.00253981633974,35.5613424749907));
#99070=CARTESIAN_POINT('Ctrl Pts',(-12.6910734237184,1.00253981633974,35.0111461040952));
#99071=CARTESIAN_POINT('Ctrl Pts',(-13.3725424358171,1.00253981633974,34.5834843095939));
#99072=CARTESIAN_POINT('Ctrl Pts',(-13.8907462265714,1.00253981633974,34.2368869147185));
#99073=CARTESIAN_POINT('Ctrl Pts',(-14.3877781203166,1.00253981633974,33.8201146754649));
#99074=CARTESIAN_POINT('Ctrl Pts',(-14.8238908844334,1.00253981633974,33.2948194019013));
#99075=CARTESIAN_POINT('Ctrl Pts',(-15.0761879359655,1.00253981633974,32.5848794176223));
#99076=CARTESIAN_POINT('Ctrl Pts',(-15.0048415747375,1.00253981633974,31.8645500407944));
#99077=CARTESIAN_POINT('Ctrl Pts',(-14.7969073569086,1.00253981633974,31.255443467967));
#99078=CARTESIAN_POINT('Ctrl Pts',(-14.4608280370914,1.00253981633974,30.4864933436934));
#99079=CARTESIAN_POINT('Ctrl Pts',(-13.8892654107988,1.00253981633974,29.1794300100813));
#99080=CARTESIAN_POINT('Ctrl Pts',(-13.3134204366261,1.00253981633974,27.3367371289618));
#99081=CARTESIAN_POINT('Ctrl Pts',(-12.676785825845,1.00253981633974,25.0072588185284));
#99082=CARTESIAN_POINT('Ctrl Pts',(-12.0379540421531,1.00253981633974,22.6694941250056));
#99083=CARTESIAN_POINT('Ctrl Pts',(-11.0930194846002,1.00253981633975,19.5704317186628));
#99084=CARTESIAN_POINT('Ctrl Pts',(-10.0793574851517,1.00253981633975,16.5387499289064));
#99085=CARTESIAN_POINT('Ctrl Pts',(-9.09212599991816,1.00253981633974,13.4722442013831));
#99086=CARTESIAN_POINT('Ctrl Pts',(-8.54361306627396,1.00253981633975,11.9392205016032));
#99087=CARTESIAN_POINT('Ctrl Pts',(-8.26785692826842,1.00253981633974,11.1826993255826));
#99088=CARTESIAN_POINT('Ctrl Pts',(-12.6467363234665,0.924,42.0099427937538));
#99089=CARTESIAN_POINT('Ctrl Pts',(-12.6060713603138,0.924,41.5682984715533));
#99090=CARTESIAN_POINT('Ctrl Pts',(-12.3296022375865,0.924,40.7164504695946));
#99091=CARTESIAN_POINT('Ctrl Pts',(-11.6999497096383,0.924,39.6710971369163));
#99092=CARTESIAN_POINT('Ctrl Pts',(-11.1874609600943,0.924,38.6392410506538));
#99093=CARTESIAN_POINT('Ctrl Pts',(-11.0113749925991,0.924,37.5398403917748));
#99094=CARTESIAN_POINT('Ctrl Pts',(-11.2537874910971,0.924,36.4518523554272));
#99095=CARTESIAN_POINT('Ctrl Pts',(-11.9032876540853,0.924,35.5613424749907));
#99096=CARTESIAN_POINT('Ctrl Pts',(-12.6910734237184,0.924,35.0111461040952));
#99097=CARTESIAN_POINT('Ctrl Pts',(-13.3725424358171,0.924,34.5834843095939));
#99098=CARTESIAN_POINT('Ctrl Pts',(-13.8907462265714,0.924,34.2368869147185));
#99099=CARTESIAN_POINT('Ctrl Pts',(-14.3877781203166,0.924,33.8201146754649));
#99100=CARTESIAN_POINT('Ctrl Pts',(-14.8238908844334,0.923999999999999,
33.2948194019013));
#99101=CARTESIAN_POINT('Ctrl Pts',(-15.0761879359655,0.924,32.5848794176223));
#99102=CARTESIAN_POINT('Ctrl Pts',(-15.0048415747375,0.924,31.8645500407944));
#99103=CARTESIAN_POINT('Ctrl Pts',(-14.7969073569086,0.924,31.255443467967));
#99104=CARTESIAN_POINT('Ctrl Pts',(-14.4608280370914,0.924,30.4864933436934));
#99105=CARTESIAN_POINT('Ctrl Pts',(-13.8892654107988,0.924,29.1794300100813));
#99106=CARTESIAN_POINT('Ctrl Pts',(-13.3134204366261,0.924,27.3367371289618));
#99107=CARTESIAN_POINT('Ctrl Pts',(-12.676785825845,0.924,25.0072588185284));
#99108=CARTESIAN_POINT('Ctrl Pts',(-12.0379540421531,0.924,22.6694941250056));
#99109=CARTESIAN_POINT('Ctrl Pts',(-11.0930194846002,0.924000000000001,
19.5704317186628));
#99110=CARTESIAN_POINT('Ctrl Pts',(-10.0793574851517,0.924,16.5387499289064));
#99111=CARTESIAN_POINT('Ctrl Pts',(-9.09212599991816,0.924,13.4722442013831));
#99112=CARTESIAN_POINT('Ctrl Pts',(-8.54361306627396,0.924,11.9392205016032));
#99113=CARTESIAN_POINT('Ctrl Pts',(-8.26785692826842,0.924,11.1826993255826));
#99114=CARTESIAN_POINT('Origin',(-7.98599766308436,0.924,11.2854385811275));
#99115=CARTESIAN_POINT('Ctrl Pts',(-7.97548942359086,1.15565058469624,10.3765642386027));
#99116=CARTESIAN_POINT('Ctrl Pts',(-8.06230799714572,1.0034429248949,10.6189650635473));
#99117=CARTESIAN_POINT('Ctrl Pts',(-8.16503623275751,0.92400000000006,10.9006166345145));
#99118=CARTESIAN_POINT('Ctrl Pts',(-8.2678569282683,0.924,11.1826993255823));
#99119=CARTESIAN_POINT('Ctrl Pts',(-7.99045555921432,1.23108469744854,10.4183502697803));
#99120=CARTESIAN_POINT('Ctrl Pts',(-8.07217904790317,1.08475451411851,10.6463513703776));
#99121=CARTESIAN_POINT('Ctrl Pts',(-8.16981771984119,1.00573927772529,10.9134327420293));
#99122=CARTESIAN_POINT('Ctrl Pts',(-8.2678569282683,1.00253981633975,11.1826993255823));
#99123=CARTESIAN_POINT('Ctrl Pts',(-7.94326110749956,1.38102048348872,10.5289633581403));
#99124=CARTESIAN_POINT('Ctrl Pts',(-8.02040943412811,1.24654612868385,10.7271275165187));
#99125=CARTESIAN_POINT('Ctrl Pts',(-8.11273806656634,1.16832799177458,10.9631249146767));
#99126=CARTESIAN_POINT('Ctrl Pts',(-8.20680380061954,1.15901743402805,11.2049535270869));
#99127=CARTESIAN_POINT('Ctrl Pts',(-7.77680414049113,1.42353079316072,10.6151507309428));
#99128=CARTESIAN_POINT('Ctrl Pts',(-7.86054014004693,1.29840666751811,10.8060533124044));
#99129=CARTESIAN_POINT('Ctrl Pts',(-7.95999863022133,1.2290893043484,11.0310584243187));
#99130=CARTESIAN_POINT('Ctrl Pts',(-8.05978824615495,1.22400000000001,11.2585415069226));
#99131=CARTESIAN_POINT('Ctrl Pts',(-7.69305806525894,1.41005007589777,10.6367198785636));
#99132=CARTESIAN_POINT('Ctrl Pts',(-7.78028187341949,1.28780455385259,10.8323127138358));
#99133=CARTESIAN_POINT('Ctrl Pts',(-7.88321097351839,1.22400000000005,11.0589589073799));
#99134=CARTESIAN_POINT('Ctrl Pts',(-7.98599766308424,1.224,11.2854385811272));
#99135=CARTESIAN_POINT('',(-7.69305806525894,1.41005007589777,10.6367198785636));
#99136=CARTESIAN_POINT('Ctrl Pts',(-7.98599766308424,1.224,11.2854385811272));
#99137=CARTESIAN_POINT('Ctrl Pts',(-7.88321097351839,1.22400000000005,11.0589589073799));
#99138=CARTESIAN_POINT('Ctrl Pts',(-7.78028187341949,1.28780455385259,10.8323127138358));
#99139=CARTESIAN_POINT('Ctrl Pts',(-7.69305806525894,1.41005007589777,10.6367198785636));
#99140=CARTESIAN_POINT('Origin',(-7.69305806525894,1.15565058469624,10.4777201965626));
#99141=CARTESIAN_POINT('Ctrl Pts',(-7.69402636887568,1.40836049654452,10.6394232055288));
#99142=CARTESIAN_POINT('Ctrl Pts',(-7.37878397297215,1.9583789756659,9.75939363893455));
#99143=CARTESIAN_POINT('Ctrl Pts',(-7.08515088258527,2.51315943171085,8.87174490926262));
#99144=CARTESIAN_POINT('Ctrl Pts',(-6.90139152215332,3.07969017441782,7.96529572093148));
#99145=CARTESIAN_POINT('Ctrl Pts',(-7.77777254631837,1.42184316271539,10.6178510368671));
#99146=CARTESIAN_POINT('Ctrl Pts',(-7.4624969034848,1.97122882668992,9.7388021111409));
#99147=CARTESIAN_POINT('Ctrl Pts',(-7.16880498204814,2.52378465263871,8.85489320618927));
#99148=CARTESIAN_POINT('Ctrl Pts',(-6.98399462243714,3.08721662507797,7.95325294287824));
#99149=CARTESIAN_POINT('Ctrl Pts',(-7.94428975230827,1.37932471088278,10.5316287085264));
#99150=CARTESIAN_POINT('Ctrl Pts',(-7.6289893652189,1.92813146670491,9.65491827136533));
#99151=CARTESIAN_POINT('Ctrl Pts',(-7.33511759437778,2.4782573725025,8.7798016390015));
#99152=CARTESIAN_POINT('Ctrl Pts',(-7.14841699910981,3.03896615778005,7.88976143408875));
#99153=CARTESIAN_POINT('Ctrl Pts',(-7.99145271748562,1.22929648674672,10.4209666875345));
#99154=CARTESIAN_POINT('Ctrl Pts',(-7.67704649076099,1.77889550193203,9.5452221915896));
#99155=CARTESIAN_POINT('Ctrl Pts',(-7.38682021808006,2.3321450604213,8.67350113810941));
#99156=CARTESIAN_POINT('Ctrl Pts',(-7.2041455986097,2.89666826892147,7.78952721320216));
#99157=CARTESIAN_POINT('Ctrl Pts',(-7.97642326903403,1.15381020723204,10.3791715289931));
#99158=CARTESIAN_POINT('Ctrl Pts',(-7.6626379783708,1.70382952596046,9.50320731474293));
#99159=CARTESIAN_POINT('Ctrl Pts',(-7.3746278026873,2.258613046434,8.63077157801953));
#99160=CARTESIAN_POINT('Ctrl Pts',(-7.19539240778044,2.82514780747502,7.74660133539471));
#99161=CARTESIAN_POINT('',(-6.90195634553822,3.07794992410223,7.96808012143643));
#99162=CARTESIAN_POINT('Origin',(-6.90195634553822,2.8235504329007,7.80908043943548));
#99163=CARTESIAN_POINT('Ctrl Pts',(-7.69305806525894,1.41005007589777,10.6367198785636));
#99164=CARTESIAN_POINT('Ctrl Pts',(-7.37850550563988,1.95895191811054,9.75847693102314));
#99165=CARTESIAN_POINT('Ctrl Pts',(-7.08556384332816,2.512603379587,8.87263459266079));
#99166=CARTESIAN_POINT('Ctrl Pts',(-6.90195634553822,3.07794992410223,7.96808012143643));
#99167=CARTESIAN_POINT('Ctrl Pts',(-7.10945460790939,2.964,7.27219995625739));
#99168=CARTESIAN_POINT('Ctrl Pts',(-7.13617164034088,2.964,7.44003720108978));
#99169=CARTESIAN_POINT('Ctrl Pts',(-7.16707514154032,2.91473210657155,7.60709602897267));
#99170=CARTESIAN_POINT('Ctrl Pts',(-7.19596078944639,2.8235504329007,7.74940308223659));
#99171=CARTESIAN_POINT('Ctrl Pts',(-7.10945460790939,3.04253981633974,7.27219995625739));
#99172=CARTESIAN_POINT('Ctrl Pts',(-7.13849656639519,3.04402078814626,7.45433830770972));
#99173=CARTESIAN_POINT('Ctrl Pts',(-7.17237393335723,2.99262131539692,7.63626955159092));
#99174=CARTESIAN_POINT('Ctrl Pts',(-7.20466995675359,2.89502896886372,7.79230937050473));
#99175=CARTESIAN_POINT('Ctrl Pts',(-7.04529077570142,3.19902831055547,7.28241382259999));
#99176=CARTESIAN_POINT('Ctrl Pts',(-7.07642208754616,3.20333799642574,7.49435291163428));
#99177=CARTESIAN_POINT('Ctrl Pts',(-7.11349156987445,3.14769091692951,7.70773779464215));
#99178=CARTESIAN_POINT('Ctrl Pts',(-7.14894649883125,3.03726886686138,7.89252011776886));
#99179=CARTESIAN_POINT('Ctrl Pts',(-6.89074805761638,3.264,7.30701457683218));
#99180=CARTESIAN_POINT('Ctrl Pts',(-6.91946353963399,3.26635574534166,7.53407746642906));
#99181=CARTESIAN_POINT('Ctrl Pts',(-6.95292678377081,3.20426081663271,7.76083290171336));
#99182=CARTESIAN_POINT('Ctrl Pts',(-6.98456267119525,3.08548589091379,7.95602257453795));
#99183=CARTESIAN_POINT('Ctrl Pts',(-6.8131848044464,3.264,7.31936141887254));
#99184=CARTESIAN_POINT('Ctrl Pts',(-6.8406282557194,3.264,7.5477362807522));
#99185=CARTESIAN_POINT('Ctrl Pts',(-6.87234328942337,3.19873603727695,7.77482234035689));
#99186=CARTESIAN_POINT('Ctrl Pts',(-6.90195634553822,3.07794992410224,7.96808012143643));
#99187=CARTESIAN_POINT('',(-6.8131848044464,3.264,7.31936141887254));
#99188=CARTESIAN_POINT('Ctrl Pts',(-6.90195634553822,3.07794992410224,7.96808012143643));
#99189=CARTESIAN_POINT('Ctrl Pts',(-6.87234328942337,3.19873603727695,7.77482234035689));
#99190=CARTESIAN_POINT('Ctrl Pts',(-6.8406282557194,3.264,7.5477362807522));
#99191=CARTESIAN_POINT('Ctrl Pts',(-6.8131848044464,3.264,7.31936141887254));
#99192=CARTESIAN_POINT('Origin',(-6.8131848044464,2.964,7.31936141887254));
#99193=CARTESIAN_POINT('Ctrl Pts',(-6.8131848044464,3.264,7.31936141887255));
#99194=CARTESIAN_POINT('Ctrl Pts',(-6.77276542502368,3.264,7.06544559579084));
#99195=CARTESIAN_POINT('Ctrl Pts',(-6.74100318491171,3.26399999999999,6.81013961060119));
#99196=CARTESIAN_POINT('Ctrl Pts',(-6.71835209239445,3.264,6.5496683313293));
#99197=CARTESIAN_POINT('Ctrl Pts',(-6.71797603803041,3.264,6.54534447147308));
#99198=CARTESIAN_POINT('Ctrl Pts',(-6.71760000000007,3.264,6.54102059420173));
#99199=CARTESIAN_POINT('Ctrl Pts',(-6.89074805761638,3.264,7.30701457683219));
#99200=CARTESIAN_POINT('Ctrl Pts',(-6.85060859506975,3.264,7.05485515618756));
#99201=CARTESIAN_POINT('Ctrl Pts',(-6.81908071837931,3.26399999999999,6.80141438915615));
#99202=CARTESIAN_POINT('Ctrl Pts',(-6.79659880028861,3.264,6.54288927009049));
#99203=CARTESIAN_POINT('Ctrl Pts',(-6.79621901877148,3.264,6.53852248974404));
#99204=CARTESIAN_POINT('Ctrl Pts',(-6.7958444767614,3.264,6.53421584534326));
#99205=CARTESIAN_POINT('Ctrl Pts',(-7.04528673824326,3.1989628628934,7.28241446529942));
#99206=CARTESIAN_POINT('Ctrl Pts',(-7.00570552018148,3.1989628628934,7.03376395992905));
#99207=CARTESIAN_POINT('Ctrl Pts',(-6.97504274772807,3.19896286289339,6.78861582425716));
#99208=CARTESIAN_POINT('Ctrl Pts',(-6.95249369350636,3.19896286289341,6.52931900008258));
#99209=CARTESIAN_POINT('Ctrl Pts',(-6.95211645163852,3.1989628628934,6.52498147096217));
#99210=CARTESIAN_POINT('Ctrl Pts',(-6.95174044180733,3.1989628628934,6.52065791852088));
#99211=CARTESIAN_POINT('Ctrl Pts',(-7.10945460790939,3.04253981633974,7.27219995625739));
#99212=CARTESIAN_POINT('Ctrl Pts',(-7.07010511574258,3.04253981633974,7.0250051988394));
#99213=CARTESIAN_POINT('Ctrl Pts',(-7.0397495283659,3.04253981633974,6.78270237401318));
#99214=CARTESIAN_POINT('Ctrl Pts',(-7.01722541347195,3.04253981633974,6.52369262500357));
#99215=CARTESIAN_POINT('Ctrl Pts',(-7.01684792393932,3.04253981633974,6.5193522454573));
#99216=CARTESIAN_POINT('Ctrl Pts',(-7.01647188590898,3.04253981633974,6.51502836818595));
#99217=CARTESIAN_POINT('Ctrl Pts',(-7.10945460790939,2.964,7.27219995625739));
#99218=CARTESIAN_POINT('Ctrl Pts',(-7.07010511574258,2.964,7.0250051988394));
#99219=CARTESIAN_POINT('Ctrl Pts',(-7.0397495283659,2.96399999999999,6.78270237401318));
#99220=CARTESIAN_POINT('Ctrl Pts',(-7.01722541347195,2.964,6.52369262500357));
#99221=CARTESIAN_POINT('Ctrl Pts',(-7.01684792393932,2.964,6.5193522454573));
#99222=CARTESIAN_POINT('Ctrl Pts',(-7.01647188590898,2.964,6.51502836818595));
#99223=CARTESIAN_POINT('',(-6.7176,3.264,6.54102059420174));
#99224=CARTESIAN_POINT('Ctrl Pts',(-6.8131848044464,3.264,7.31936141887255));
#99225=CARTESIAN_POINT('Ctrl Pts',(-6.77276542502368,3.264,7.06544559579084));
#99226=CARTESIAN_POINT('Ctrl Pts',(-6.74100318491171,3.26399999999999,6.81013961060119));
#99227=CARTESIAN_POINT('Ctrl Pts',(-6.71835209239445,3.264,6.5496683313293));
#99228=CARTESIAN_POINT('Ctrl Pts',(-6.71797603803041,3.264,6.54534447147308));
#99229=CARTESIAN_POINT('Ctrl Pts',(-6.71760000000007,3.264,6.54102059420173));
#99230=CARTESIAN_POINT('Ctrl Pts',(-6.7176000000002,3.264,6.54102059420098));
#99231=CARTESIAN_POINT('Ctrl Pts',(-6.71833165319913,3.264,6.54120934340536));
#99232=CARTESIAN_POINT('Ctrl Pts',(-6.71906410849758,3.26399732346502,6.54139488274335));
#99233=CARTESIAN_POINT('Ctrl Pts',(-6.74443279705516,3.26381150391108,6.54770283617451));
#99234=CARTESIAN_POINT('Ctrl Pts',(-6.76899387896665,3.26065160540924,6.54990773601873));
#99235=CARTESIAN_POINT('Ctrl Pts',(-6.81740983957415,3.24798417582051,6.54861388368172));
#99236=CARTESIAN_POINT('Ctrl Pts',(-6.84022091954467,3.23887327016054,6.54532375830639));
#99237=CARTESIAN_POINT('Ctrl Pts',(-6.88647361235057,3.21357659218827,6.53744289499075));
#99238=CARTESIAN_POINT('Ctrl Pts',(-6.90943210370148,3.19642495146849,6.53274268516599));
#99239=CARTESIAN_POINT('Ctrl Pts',(-6.94706293362363,3.15880713459934,6.53103362429698));
#99240=CARTESIAN_POINT('Ctrl Pts',(-6.96534422261705,3.13628933865456,6.53291537653795));
#99241=CARTESIAN_POINT('Ctrl Pts',(-6.99299814551648,3.08561018365874,6.53348362099248));
#99242=CARTESIAN_POINT('Ctrl Pts',(-7.00213172179733,3.06230910196935,6.53267399033088));
#99243=CARTESIAN_POINT('Ctrl Pts',(-7.0147942159154,3.01264906168983,6.52984196355258));
#99244=CARTESIAN_POINT('Ctrl Pts',(-7.0176,2.98769953894126,6.52800007780761));
#99245=CARTESIAN_POINT('Ctrl Pts',(-7.0176,2.964,6.52800007780761));
#99246=CARTESIAN_POINT('Origin',(-6.7176,2.964,-19.584));
#99247=CARTESIAN_POINT('',(-6.7176,3.264,-14.688));
#99248=CARTESIAN_POINT('',(-6.7176,3.264,-19.584));
#99249=CARTESIAN_POINT('',(-7.0176,2.964,-14.688));
#99250=CARTESIAN_POINT('Origin',(-6.7176,2.964,-14.688));
#99251=CARTESIAN_POINT('',(-7.0176,2.964,-19.584));
#99252=CARTESIAN_POINT('Origin',(0.,2.964,-14.688));
#99253=CARTESIAN_POINT('',(6.7176,3.264,-14.688));
#99254=CARTESIAN_POINT('',(7.0176,2.964,-14.688));
#99255=CARTESIAN_POINT('Origin',(6.7176,2.964,-14.688));
#99256=CARTESIAN_POINT('Origin',(0.,2.964,-14.688));
#99257=CARTESIAN_POINT('Origin',(0.,3.264,-14.688));
#99258=CARTESIAN_POINT('Origin',(6.7176,2.964,-8.976));
#99259=CARTESIAN_POINT('',(7.0176,2.964,-8.976));
#99260=CARTESIAN_POINT('',(6.71760000000007,3.264,6.54102059420079));
#99261=CARTESIAN_POINT('',(6.7176,3.264,-8.976));
#99262=CARTESIAN_POINT('Ctrl Pts',(6.71760000000026,3.264,6.54102059420005));
#99263=CARTESIAN_POINT('Ctrl Pts',(6.71833161535042,3.264,6.54121031917896));
#99264=CARTESIAN_POINT('Ctrl Pts',(6.71906402903224,3.26399732374162,6.54139686702817));
#99265=CARTESIAN_POINT('Ctrl Pts',(6.744304090703,3.26381245686305,6.54770905827349));
#99266=CARTESIAN_POINT('Ctrl Pts',(6.76874616727742,3.26068433500669,6.54999627440179));
#99267=CARTESIAN_POINT('Ctrl Pts',(6.81694811446642,3.24813572935757,6.54892168893177));
#99268=CARTESIAN_POINT('Ctrl Pts',(6.83966741557286,3.23911015473846,6.54576286024958));
#99269=CARTESIAN_POINT('Ctrl Pts',(6.88609886105684,3.21385739564275,6.53802232312692));
#99270=CARTESIAN_POINT('Ctrl Pts',(6.90926565630398,3.1965906610116,6.53330291862062));
#99271=CARTESIAN_POINT('Ctrl Pts',(6.94715428211924,3.15871639917427,6.53154772477979));
#99272=CARTESIAN_POINT('Ctrl Pts',(6.96558458258161,3.13600641445292,6.53338605654475));
#99273=CARTESIAN_POINT('Ctrl Pts',(6.99322546109818,3.08507067475937,6.53373480681712));
#99274=CARTESIAN_POINT('Ctrl Pts',(7.00227690287596,3.06185555957858,6.53282707247597));
#99275=CARTESIAN_POINT('Ctrl Pts',(7.01481452566474,3.01244578554285,6.52986850096268));
#99276=CARTESIAN_POINT('Ctrl Pts',(7.0176,2.98761215526521,6.528000078773));
#99277=CARTESIAN_POINT('Ctrl Pts',(7.0176,2.964,6.528000078773));
#99278=CARTESIAN_POINT('Ctrl Pts',(7.1959607894463,2.8235504329007,7.74940308223601));
#99279=CARTESIAN_POINT('Ctrl Pts',(7.16707443778447,2.91473432807616,7.60709256187426));
#99280=CARTESIAN_POINT('Ctrl Pts',(7.13617229126044,2.964,7.44004129019165));
#99281=CARTESIAN_POINT('Ctrl Pts',(7.10945460790829,2.964,7.27219995625688));
#99282=CARTESIAN_POINT('Ctrl Pts',(7.20466995675359,2.89502896886377,7.79230937050415));
#99283=CARTESIAN_POINT('Ctrl Pts',(7.1723731465128,2.99262369308791,7.63626574991444));
#99284=CARTESIAN_POINT('Ctrl Pts',(7.13849727395811,3.04402082422793,7.45434274523658));
#99285=CARTESIAN_POINT('Ctrl Pts',(7.10945460790829,3.04253981633974,7.27219995625688));
#99286=CARTESIAN_POINT('Ctrl Pts',(7.14894649883135,3.03726886686152,7.89252011776843));
#99287=CARTESIAN_POINT('Ctrl Pts',(7.11349070606817,3.14769360719685,7.70773329269815));
#99288=CARTESIAN_POINT('Ctrl Pts',(7.07642284601308,3.20333810142481,7.49435807521152));
#99289=CARTESIAN_POINT('Ctrl Pts',(7.04529077570034,3.19902831055547,7.2824138225996));
#99290=CARTESIAN_POINT('Ctrl Pts',(6.9845626711953,3.08548589091386,7.95602257453783));
#99291=CARTESIAN_POINT('Ctrl Pts',(6.95292601300975,3.2042637104052,7.76082814621037));
#99292=CARTESIAN_POINT('Ctrl Pts',(6.91946423924288,3.26635580273589,7.53408299847537));
#99293=CARTESIAN_POINT('Ctrl Pts',(6.89074805761534,3.264,7.30701457683205));
#99294=CARTESIAN_POINT('Ctrl Pts',(6.90195634553824,3.07794992410223,7.96808012143643));
#99295=CARTESIAN_POINT('Ctrl Pts',(6.87234256794554,3.19873898004894,7.77481763192169));
#99296=CARTESIAN_POINT('Ctrl Pts',(6.84062892433718,3.264,7.54774184476293));
#99297=CARTESIAN_POINT('Ctrl Pts',(6.81318480444538,3.264,7.31936141887254));
#99298=CARTESIAN_POINT('',(6.81318480444538,3.264,7.31936141887254));
#99299=CARTESIAN_POINT('Origin',(6.81318480444538,2.964,7.31936141887254));
#99300=CARTESIAN_POINT('',(6.90195634553824,3.07794992410223,7.96808012143643));
#99301=CARTESIAN_POINT('Ctrl Pts',(6.81318480444538,3.264,7.31936141887254));
#99302=CARTESIAN_POINT('Ctrl Pts',(6.84062892433718,3.264,7.54774184476293));
#99303=CARTESIAN_POINT('Ctrl Pts',(6.87234256794554,3.19873898004894,7.77481763192169));
#99304=CARTESIAN_POINT('Ctrl Pts',(6.90195634553824,3.07794992410223,7.96808012143643));
#99305=CARTESIAN_POINT('Origin',(6.90195634553824,2.8235504329007,7.80908043943548));
#99306=CARTESIAN_POINT('Ctrl Pts',(6.71760000000007,3.264,6.54102059420079));
#99307=CARTESIAN_POINT('Ctrl Pts',(6.71797603803036,3.264,6.54534447147182));
#99308=CARTESIAN_POINT('Ctrl Pts',(6.71835209239434,3.264,6.54966833132773));
#99309=CARTESIAN_POINT('Ctrl Pts',(6.74100318491002,3.264,6.81013961059996));
#99310=CARTESIAN_POINT('Ctrl Pts',(6.77276542502211,3.264,7.0654455957901));
#99311=CARTESIAN_POINT('Ctrl Pts',(6.81318480444533,3.264,7.31936141887222));
#99312=CARTESIAN_POINT('Ctrl Pts',(6.79584447676144,3.264,6.53421584534281));
#99313=CARTESIAN_POINT('Ctrl Pts',(6.79621901877147,3.264,6.53852248974327));
#99314=CARTESIAN_POINT('Ctrl Pts',(6.79659880028854,3.264,6.54288927008942));
#99315=CARTESIAN_POINT('Ctrl Pts',(6.81908071837765,3.264,6.80141438915507));
#99316=CARTESIAN_POINT('Ctrl Pts',(6.85060859506817,3.264,7.05485515618676));
#99317=CARTESIAN_POINT('Ctrl Pts',(6.89074805761529,3.264,7.30701457683173));
#99318=CARTESIAN_POINT('Ctrl Pts',(6.95166378082186,3.19894727191536,6.52066458555755));
#99319=CARTESIAN_POINT('Ctrl Pts',(6.95203954305117,3.19894727191536,6.52498528583783));
#99320=CARTESIAN_POINT('Ctrl Pts',(6.9524209881539,3.19894727191536,6.52937115569764));
#99321=CARTESIAN_POINT('Ctrl Pts',(6.97463672769311,3.19894727191537,6.78483527185625));
#99322=CARTESIAN_POINT('Ctrl Pts',(7.00562922258625,3.19894727191536,7.03377380853805));
#99323=CARTESIAN_POINT('Ctrl Pts',(7.0452107446937,3.19894727191536,7.2824265622686));
#99324=CARTESIAN_POINT('Ctrl Pts',(7.01647188590914,3.04253981633974,6.51502836818689));
#99325=CARTESIAN_POINT('Ctrl Pts',(7.01684792393943,3.04253981633974,6.51935224545793));
#99326=CARTESIAN_POINT('Ctrl Pts',(7.0172303787086,3.04253981633974,6.52374971782953));
#99327=CARTESIAN_POINT('Ctrl Pts',(7.03933150750459,3.04253981633974,6.77789575673342));
#99328=CARTESIAN_POINT('Ctrl Pts',(7.07010511574098,3.04253981633974,7.02500519883843));
#99329=CARTESIAN_POINT('Ctrl Pts',(7.10945460790824,3.04253981633974,7.27219995625657));
#99330=CARTESIAN_POINT('Ctrl Pts',(7.01647188590914,2.964,6.51502836818689));
#99331=CARTESIAN_POINT('Ctrl Pts',(7.01684792393943,2.964,6.51935224545793));
#99332=CARTESIAN_POINT('Ctrl Pts',(7.0172303787086,2.964,6.52374971782953));
#99333=CARTESIAN_POINT('Ctrl Pts',(7.03933150750459,2.964,6.77789575673342));
#99334=CARTESIAN_POINT('Ctrl Pts',(7.07010511574098,2.964,7.02500519883843));
#99335=CARTESIAN_POINT('Ctrl Pts',(7.10945460790824,2.964,7.27219995625657));
#99336=CARTESIAN_POINT('Ctrl Pts',(6.71760000000007,3.264,6.54102059420079));
#99337=CARTESIAN_POINT('Ctrl Pts',(6.71797603803036,3.264,6.54534447147182));
#99338=CARTESIAN_POINT('Ctrl Pts',(6.71835209239434,3.264,6.54966833132773));
#99339=CARTESIAN_POINT('Ctrl Pts',(6.74100318491002,3.264,6.81013961059996));
#99340=CARTESIAN_POINT('Ctrl Pts',(6.77276542502211,3.264,7.0654455957901));
#99341=CARTESIAN_POINT('Ctrl Pts',(6.81318480444533,3.264,7.31936141887222));
#99342=CARTESIAN_POINT('Ctrl Pts',(6.90139152214811,3.07969017443392,7.96529572090572));
#99343=CARTESIAN_POINT('Ctrl Pts',(7.08515088258326,2.51315943171628,8.87174490925396));
#99344=CARTESIAN_POINT('Ctrl Pts',(7.37878397297277,1.95837897566052,9.75939363894316));
#99345=CARTESIAN_POINT('Ctrl Pts',(7.69402636888245,1.40836049652889,10.6394232055538));
#99346=CARTESIAN_POINT('Ctrl Pts',(6.98399462243194,3.08721662509406,7.9532529428525));
#99347=CARTESIAN_POINT('Ctrl Pts',(7.16880498204613,2.52378465264413,8.85489320618061));
#99348=CARTESIAN_POINT('Ctrl Pts',(7.46249690348542,1.97122882668447,9.7388021111496));
#99349=CARTESIAN_POINT('Ctrl Pts',(7.77777254632515,1.42184316269977,10.6178510368922));
#99350=CARTESIAN_POINT('Ctrl Pts',(7.14841699910512,3.03896615779599,7.88976143406284));
#99351=CARTESIAN_POINT('Ctrl Pts',(7.33511759437628,2.47825737250777,8.77980163899264));
#99352=CARTESIAN_POINT('Ctrl Pts',(7.62898936522003,1.92813146669928,9.654918271374));
#99353=CARTESIAN_POINT('Ctrl Pts',(7.94428975231557,1.37932471086703,10.531628708551));
#99354=CARTESIAN_POINT('Ctrl Pts',(7.20414559860485,2.89666826893669,7.78952721317584));
#99355=CARTESIAN_POINT('Ctrl Pts',(7.38682021807838,2.33214506042582,8.67350113810013));
#99356=CARTESIAN_POINT('Ctrl Pts',(7.67704649076199,1.7788955019257,9.54522219159796));
#99357=CARTESIAN_POINT('Ctrl Pts',(7.99145271749268,1.22929648673017,10.4209666875588));
#99358=CARTESIAN_POINT('Ctrl Pts',(7.19539240777509,2.8251478074898,7.74660133536821));
#99359=CARTESIAN_POINT('Ctrl Pts',(7.37462780268508,2.25861304643806,8.6307715780101));
#99360=CARTESIAN_POINT('Ctrl Pts',(7.6626379783713,1.70382952595369,9.50320731475117));
#99361=CARTESIAN_POINT('Ctrl Pts',(7.9764232690405,1.153810207215,10.3791715290174));
#99362=CARTESIAN_POINT('',(7.69305806525675,1.41005007589777,10.6367198785636));
#99363=CARTESIAN_POINT('Origin',(7.69305806525675,1.15565058469624,10.4777201965626));
#99364=CARTESIAN_POINT('Ctrl Pts',(6.90195634553824,3.07794992410223,7.96808012143643));
#99365=CARTESIAN_POINT('Ctrl Pts',(7.08556384332996,2.51260337958728,8.87263459266035));
#99366=CARTESIAN_POINT('Ctrl Pts',(7.37850550563793,1.95895191811046,9.75847693102326));
#99367=CARTESIAN_POINT('Ctrl Pts',(7.69305806525675,1.41005007589777,10.6367198785636));
#99368=CARTESIAN_POINT('Ctrl Pts',(8.26785692826664,0.924,11.1826993255823));
#99369=CARTESIAN_POINT('Ctrl Pts',(8.16503869361036,0.924000000000001,10.900623385729));
#99370=CARTESIAN_POINT('Ctrl Pts',(8.06230591927477,1.00344656775053,10.6189592620572));
#99371=CARTESIAN_POINT('Ctrl Pts',(7.97548942358868,1.15565058469624,10.3765642386028));
#99372=CARTESIAN_POINT('Ctrl Pts',(8.26785692826664,1.00253981633975,11.1826993255823));
#99373=CARTESIAN_POINT('Ctrl Pts',(8.16982006625653,1.00573920115106,10.9134391865099));
#99374=CARTESIAN_POINT('Ctrl Pts',(8.07217709197523,1.08475801630582,10.6463459135227));
#99375=CARTESIAN_POINT('Ctrl Pts',(7.99045555921214,1.23108469744854,10.4183502697804));
#99376=CARTESIAN_POINT('Ctrl Pts',(8.20680380061789,1.15901743402804,11.2049535270869));
#99377=CARTESIAN_POINT('Ctrl Pts',(8.11274031788272,1.1683277689407,10.9631307024719));
#99378=CARTESIAN_POINT('Ctrl Pts',(8.02040758769964,1.2465493471202,10.7271227737651));
#99379=CARTESIAN_POINT('Ctrl Pts',(7.94326110749736,1.38102048348871,10.5289633581403));
#99380=CARTESIAN_POINT('Ctrl Pts',(8.05978824615337,1.224,11.2585415069228));
#99381=CARTESIAN_POINT('Ctrl Pts',(7.96000101853004,1.22908918254371,11.0310638687758));
#99382=CARTESIAN_POINT('Ctrl Pts',(7.86053813595267,1.29840966217113,10.8060487434454));
#99383=CARTESIAN_POINT('Ctrl Pts',(7.77680414048894,1.42353079316071,10.6151507309429));
#99384=CARTESIAN_POINT('Ctrl Pts',(7.98599766308269,1.224,11.2854385811275));
#99385=CARTESIAN_POINT('Ctrl Pts',(7.88321343355745,1.224,11.0589643278221));
#99386=CARTESIAN_POINT('Ctrl Pts',(7.7802797858499,1.28780747961066,10.8323080326229));
#99387=CARTESIAN_POINT('Ctrl Pts',(7.69305806525675,1.41005007589777,10.6367198785636));
#99388=CARTESIAN_POINT('Ctrl Pts',(7.69305806525675,1.41005007589777,10.6367198785636));
#99389=CARTESIAN_POINT('Ctrl Pts',(7.7802797858499,1.28780747961066,10.8323080326229));
#99390=CARTESIAN_POINT('Ctrl Pts',(7.88321343355745,1.224,11.0589643278221));
#99391=CARTESIAN_POINT('Ctrl Pts',(7.98599766308269,1.224,11.2854385811275));
#99392=CARTESIAN_POINT('Origin',(-7.0176,-4.08,-14.688));
#99393=CARTESIAN_POINT('',(-7.0176,2.448,-14.688));
#99394=CARTESIAN_POINT('',(-7.0176,-4.08,-14.688));
#99395=CARTESIAN_POINT('',(-7.0176,2.448,6.99296141887254));
#99396=CARTESIAN_POINT('',(-7.0176,2.448,-3.672));
#99397=CARTESIAN_POINT('',(-7.0176,2.26194992410223,7.64168012143644));
#99398=CARTESIAN_POINT('Origin',(-7.0176,1.224,6.99296141887254));
#99399=CARTESIAN_POINT('',(-7.01760431834114,1.93536901811185,8.16420957102104));
#99400=CARTESIAN_POINT('',(-7.0176,5.46215730337078,2.52134831460674));
#99401=CARTESIAN_POINT('',(-7.01770541278284,2.29368306071046,7.63779914846271));
#99402=CARTESIAN_POINT('Origin',(-7.0176,3.0385827613015,7.37874354812469));
#99403=CARTESIAN_POINT('',(-7.01761410688719,2.58763798856244,6.96055221898186));
#99404=CARTESIAN_POINT('Ctrl Pts',(-7.0176,2.29351434713884,7.63766291347531));
#99405=CARTESIAN_POINT('Ctrl Pts',(-7.0176,2.3740423712826,7.52757570477833));
#99406=CARTESIAN_POINT('Ctrl Pts',(-7.01759999999634,2.44050724085831,7.40695060784198));
#99407=CARTESIAN_POINT('Ctrl Pts',(-7.01759999999634,2.53393775667856,7.17694898676314));
#99408=CARTESIAN_POINT('Ctrl Pts',(-7.0176,2.56551852364822,7.07078797586639));
#99409=CARTESIAN_POINT('Ctrl Pts',(-7.0176,2.58767722915247,6.96056009343683));
#99410=CARTESIAN_POINT('Ctrl Pts',(-7.0176,2.58761674131499,6.96054790557659));
#99411=CARTESIAN_POINT('Ctrl Pts',(-7.0176,2.59970615397228,6.90071766460443));
#99412=CARTESIAN_POINT('Ctrl Pts',(-7.0176,2.61360398776887,6.83777005305424));
#99413=CARTESIAN_POINT('Ctrl Pts',(-7.0176,2.63916505855607,6.73818458534492));
#99414=CARTESIAN_POINT('Ctrl Pts',(-7.01759999998582,2.65165291111849,6.69372255866987));
#99415=CARTESIAN_POINT('Ctrl Pts',(-7.01759999998582,2.68155149694533,6.60703862938188));
#99416=CARTESIAN_POINT('Ctrl Pts',(-7.0176,2.69834666935346,6.56963566225437));
#99417=CARTESIAN_POINT('Ctrl Pts',(-7.0176,2.72097423429567,6.54173976032029));
#99418=CARTESIAN_POINT('Ctrl Pts',(-7.01759999999971,2.7266719134448,6.5361535692381));
#99419=CARTESIAN_POINT('Ctrl Pts',(-7.01759999999971,2.73523606353071,6.53109114103823));
#99420=CARTESIAN_POINT('Ctrl Pts',(-7.0176,2.73773933071856,6.52993454070379));
#99421=CARTESIAN_POINT('Ctrl Pts',(-7.0176,2.74285825285848,6.52839954478026));
#99422=CARTESIAN_POINT('Ctrl Pts',(-7.0176,2.74540196897649,6.52799999999999));
#99423=CARTESIAN_POINT('Ctrl Pts',(-7.0176,2.748,6.52799999999999));
#99424=CARTESIAN_POINT('Origin',(0.,-4.08,-14.688));
#99425=CARTESIAN_POINT('',(7.0176,2.448,-14.688));
#99426=CARTESIAN_POINT('',(7.0176,-4.08,-14.688));
#99427=CARTESIAN_POINT('Origin',(0.,2.448,-14.688));
#99428=CARTESIAN_POINT('Origin',(7.0176,-4.08,6.528));
#99429=CARTESIAN_POINT('',(7.01761391330466,2.5876376799666,6.96055224393119));
#99430=CARTESIAN_POINT('Ctrl Pts',(7.0176,2.748,6.52799999999999));
#99431=CARTESIAN_POINT('Ctrl Pts',(7.0176,2.74511036893714,6.52799999999999));
#99432=CARTESIAN_POINT('Ctrl Pts',(7.0176,2.74229339126459,6.52849427846896));
#99433=CARTESIAN_POINT('Ctrl Pts',(7.0176,2.73662501896236,6.53037541474026));
#99434=CARTESIAN_POINT('Ctrl Pts',(7.0176,2.73386178483929,6.53179413745192));
#99435=CARTESIAN_POINT('Ctrl Pts',(7.0176,2.72454608146371,6.5378716410484));
#99436=CARTESIAN_POINT('Ctrl Pts',(7.0176,2.71812411704449,6.54466757895269));
#99437=CARTESIAN_POINT('Ctrl Pts',(7.0176,2.69356885127018,6.57837479338247));
#99438=CARTESIAN_POINT('Ctrl Pts',(7.01760000001758,2.67322594731515,6.62433548265231));
#99439=CARTESIAN_POINT('Ctrl Pts',(7.01760000001758,2.62579638706691,6.78269963358924));
#99440=CARTESIAN_POINT('Ctrl Pts',(7.0176,2.60429557786619,6.87800461107322));
#99441=CARTESIAN_POINT('Ctrl Pts',(7.0176,2.58761652893502,6.9605489566511));
#99442=CARTESIAN_POINT('',(7.01770541278263,2.2936830607088,7.63779914846461));
#99443=CARTESIAN_POINT('Ctrl Pts',(7.0176,2.58767682077497,6.960562124904));
#99444=CARTESIAN_POINT('Ctrl Pts',(7.0176,2.56298409413704,7.08339472961271));
#99445=CARTESIAN_POINT('Ctrl Pts',(7.01759999990208,2.52660430658189,7.20111310457098));
#99446=CARTESIAN_POINT('Ctrl Pts',(7.01759999990208,2.42819109620806,7.42898400669956));
#99447=CARTESIAN_POINT('Ctrl Pts',(7.0176,2.36665124679277,7.53767986755727));
#99448=CARTESIAN_POINT('Ctrl Pts',(7.0176,2.29351434713977,7.63766291347403));
#99449=CARTESIAN_POINT('',(7.01760411951713,1.93536442690257,8.16421691695589));
#99450=CARTESIAN_POINT('Origin',(7.0176,3.00424770096522,7.39945472980219));
#99451=CARTESIAN_POINT('',(7.0176,2.26194992410223,7.64168012143644));
#99452=CARTESIAN_POINT('',(7.0176,0.694516853932584,10.1495730337079));
#99453=CARTESIAN_POINT('',(7.0176,2.448,6.99296141887254));
#99454=CARTESIAN_POINT('Origin',(7.0176,1.224,6.99296141887254));
#99455=CARTESIAN_POINT('',(7.0176,2.448,6.936));
#99456=CARTESIAN_POINT('Origin',(12.648,-4.08,45.696));
#99457=CARTESIAN_POINT('Ctrl Pts',(7.69004994112325,0.594050075897773,10.3103198785636));
#99458=CARTESIAN_POINT('Ctrl Pts',(7.37565292717766,1.14292103979677,9.43212633632517));
#99459=CARTESIAN_POINT('Ctrl Pts',(7.08320222221595,1.69659760459055,8.54624383265512));
#99460=CARTESIAN_POINT('Ctrl Pts',(6.90025424549142,2.26194992410223,7.64168012143644));
#99461=CARTESIAN_POINT('Ctrl Pts',(7.7566099417083,0.604759632121113,10.2931845886062));
#99462=CARTESIAN_POINT('Ctrl Pts',(7.44282948876134,1.15322808712422,9.41561937075493));
#99463=CARTESIAN_POINT('Ctrl Pts',(7.15265898639664,1.70551531081992,8.53207367891967));
#99464=CARTESIAN_POINT('Ctrl Pts',(6.97247659379773,2.26851485319919,7.6311762348813));
#99465=CARTESIAN_POINT('Ctrl Pts',(7.88938556140221,0.668907343792859,10.2857426732368));
#99466=CARTESIAN_POINT('Ctrl Pts',(7.57681706437755,1.21707193313268,9.40974380083994));
#99467=CARTESIAN_POINT('Ctrl Pts',(7.29124285060054,1.76814635786057,8.53186871114456));
#99468=CARTESIAN_POINT('Ctrl Pts',(7.11645477354901,2.3292995967516,7.64004711813782));
#99469=CARTESIAN_POINT('Ctrl Pts',(7.96060515342953,0.788498764169074,10.3349903948698));
#99470=CARTESIAN_POINT('Ctrl Pts',(7.64807518901572,1.3371289727315,9.46045329326645));
#99471=CARTESIAN_POINT('Ctrl Pts',(7.36254955939489,1.88994777765749,8.58798846944997));
#99472=CARTESIAN_POINT('Ctrl Pts',(7.18671249288602,2.4538649372709,7.70369083485712));
#99473=CARTESIAN_POINT('Ctrl Pts',(7.97249537063514,0.848449567099299,10.3682028984962));
#99474=CARTESIAN_POINT('Ctrl Pts',(7.65957903289365,1.3973205309983,9.49414527429423));
#99475=CARTESIAN_POINT('Ctrl Pts',(7.37274783895485,1.95099709579208,8.62351966308874));
#99476=CARTESIAN_POINT('Ctrl Pts',(7.19430053092001,2.51634941530375,7.74120895321939));
#99477=CARTESIAN_POINT('Origin',(6.90025424549142,2.51634941530375,7.80067980343739));
#99478=CARTESIAN_POINT('',(7.69004994112325,0.594050075897772,10.3103198785636));
#99479=CARTESIAN_POINT('Origin',(7.69004994112325,0.848449567099299,10.4693195605645));
#99480=CARTESIAN_POINT('Ctrl Pts',(7.69004994112325,0.594050075897773,10.3103198785636));
#99481=CARTESIAN_POINT('Ctrl Pts',(7.43642528501577,1.03682530368781,9.6018795140995));
#99482=CARTESIAN_POINT('Ctrl Pts',(7.19708258213954,1.4827278622412,8.88843542041408));
#99483=CARTESIAN_POINT('Ctrl Pts',(7.0179868222806,1.93536441515841,8.16421693574654));
#99484=CARTESIAN_POINT('Ctrl Pts',(7.06362916696882,2.7480230090648,6.95414127896201));
#99485=CARTESIAN_POINT('Ctrl Pts',(7.0993690878108,2.74811551919964,7.23155382342856));
#99486=CARTESIAN_POINT('Ctrl Pts',(7.14696080934769,2.66643382276424,7.5071905074376));
#99487=CARTESIAN_POINT('Ctrl Pts',(7.19438354265699,2.51611178510552,7.74161935745458));
#99488=CARTESIAN_POINT('Ctrl Pts',(7.06363490740171,2.69944028986368,6.95415602179895));
#99489=CARTESIAN_POINT('Ctrl Pts',(7.09821965127004,2.70026704502072,7.22262797399989));
#99490=CARTESIAN_POINT('Ctrl Pts',(7.14400277235035,2.62236748381514,7.49012436326919));
#99491=CARTESIAN_POINT('Ctrl Pts',(7.18969017835144,2.47747072284844,7.7184010716774));
#99492=CARTESIAN_POINT('Ctrl Pts',(7.03586871828684,2.5860173677501,6.95776948019296));
#99493=CARTESIAN_POINT('Ctrl Pts',(7.06872790702351,2.58856514291509,7.20598605294365));
#99494=CARTESIAN_POINT('Ctrl Pts',(7.11175827397579,2.51949133545424,7.45491010747032));
#99495=CARTESIAN_POINT('Ctrl Pts',(7.15489990897123,2.38727021999165,7.66902358769554));
#99496=CARTESIAN_POINT('Ctrl Pts',(6.95031555185498,2.50367339927269,6.96881823558572));
#99497=CARTESIAN_POINT('Ctrl Pts',(6.98392692928157,2.50655355403587,7.20376129641692));
#99498=CARTESIAN_POINT('Ctrl Pts',(7.02813588214951,2.44235324221148,7.4396687902832));
#99499=CARTESIAN_POINT('Ctrl Pts',(7.07234001721698,2.31860209564757,7.64277634582262));
#99500=CARTESIAN_POINT('Ctrl Pts',(6.89212767908006,2.47624041956814,6.97632364997776));
#99501=CARTESIAN_POINT('Ctrl Pts',(6.9266553668271,2.47850902575585,7.20761906768847));
#99502=CARTESIAN_POINT('Ctrl Pts',(6.9721868803631,2.41488748239933,7.43917519062995));
#99503=CARTESIAN_POINT('Ctrl Pts',(7.01767749054815,2.29330136612035,7.63800974414734));
#99504=CARTESIAN_POINT('Origin',(6.76615104985734,2.748,6.99296141887254));
#99505=CARTESIAN_POINT('Ctrl Pts',(7.0176,2.58761550237112,6.96055403711337));
#99506=CARTESIAN_POINT('Ctrl Pts',(6.99922349531616,2.58761550237112,6.81797069470138));
#99507=CARTESIAN_POINT('Ctrl Pts',(6.98374576415963,2.58761550237112,6.67509413737213));
#99508=CARTESIAN_POINT('Ctrl Pts',(6.97130347175975,2.58761550237112,6.53202630652935));
#99509=CARTESIAN_POINT('Ctrl Pts',(7.04750769996015,2.63528330527516,6.95669945649334));
#99510=CARTESIAN_POINT('Ctrl Pts',(7.0291833743663,2.63528330527516,6.81452097176143));
#99511=CARTESIAN_POINT('Ctrl Pts',(7.01375047339114,2.63528330527516,6.6720564108619));
#99512=CARTESIAN_POINT('Ctrl Pts',(7.00134514825194,2.63528330527516,6.52941364845733));
#99513=CARTESIAN_POINT('Ctrl Pts',(7.06369006012584,2.69159478975873,6.95461383265853));
#99514=CARTESIAN_POINT('Ctrl Pts',(7.04539389161563,2.69159478975873,6.81265381880386));
#99515=CARTESIAN_POINT('Ctrl Pts',(7.02998537672209,2.69159478975873,6.67041338531935));
#99516=CARTESIAN_POINT('Ctrl Pts',(7.0176,2.69159478975873,6.52799999999999));
#99517=CARTESIAN_POINT('Ctrl Pts',(7.06369006012584,2.748,6.95461383265853));
#99518=CARTESIAN_POINT('Ctrl Pts',(7.04539374054096,2.748,6.81265264661519));
#99519=CARTESIAN_POINT('Ctrl Pts',(7.02998548375378,2.748,6.67041461602444));
#99520=CARTESIAN_POINT('Ctrl Pts',(7.0176,2.748,6.52799999999999));
#99521=CARTESIAN_POINT('Ctrl Pts',(7.97238210650129,0.848667810146576,10.3678865203214));
#99522=CARTESIAN_POINT('Ctrl Pts',(8.02503872423604,0.756217482327583,10.5149731412681));
#99523=CARTESIAN_POINT('Ctrl Pts',(8.0869221616882,0.707947174569549,10.6858877147699));
#99524=CARTESIAN_POINT('Ctrl Pts',(8.14912361676156,0.708019010352448,10.8568386685929));
#99525=CARTESIAN_POINT('Ctrl Pts',(7.96048761218596,0.788731610271414,10.3346498829601));
#99526=CARTESIAN_POINT('Ctrl Pts',(8.01637706856055,0.687463302222747,10.4908448248288));
#99527=CARTESIAN_POINT('Ctrl Pts',(8.08215444077848,0.632587778955639,10.673073122701));
#99528=CARTESIAN_POINT('Ctrl Pts',(8.14913906922441,0.629465787637592,10.8568651972294));
#99529=CARTESIAN_POINT('Ctrl Pts',(7.88930781714838,0.669130461784413,10.2853123218851));
#99530=CARTESIAN_POINT('Ctrl Pts',(7.94769055067623,0.550421641857097,10.4612353255528));
#99531=CARTESIAN_POINT('Ctrl Pts',(8.01711568751401,0.482182663833425,10.6678349016059));
#99532=CARTESIAN_POINT('Ctrl Pts',(8.08808615036449,0.472961311892119,10.8791433605056));
#99533=CARTESIAN_POINT('Ctrl Pts',(7.75648913737719,0.605033293429871,10.2927630564965));
#99534=CARTESIAN_POINT('Ctrl Pts',(7.81126536355006,0.480889739048768,10.4838995104295));
#99535=CARTESIAN_POINT('Ctrl Pts',(7.87574497017474,0.412984275736593,10.7069427306825));
#99536=CARTESIAN_POINT('Ctrl Pts',(7.94101805558994,0.407988882551097,10.9326817955771));
#99537=CARTESIAN_POINT('Ctrl Pts',(7.68993326017409,0.594320041958723,10.3098881354259));
#99538=CARTESIAN_POINT('Ctrl Pts',(7.74283997308695,0.471850558728837,10.5056555873966));
#99539=CARTESIAN_POINT('Ctrl Pts',(7.80491620373074,0.407905964356365,10.7327647510929));
#99540=CARTESIAN_POINT('Ctrl Pts',(7.86720541257493,0.408000103793674,10.9595386471955));
#99541=CARTESIAN_POINT('Ctrl Pts',(7.86706805722616,0.408,10.9590385811275));
#99542=CARTESIAN_POINT('Ctrl Pts',(7.80487073631488,0.408,10.7325975869917));
#99543=CARTESIAN_POINT('Ctrl Pts',(7.74289233196934,0.471846546370078,10.5058455258079));
#99544=CARTESIAN_POINT('Ctrl Pts',(7.69004994112325,0.594050075897772,10.3103198785636));
#99545=CARTESIAN_POINT('Origin',(0.,1.632,10.9590385811275));
#99546=CARTESIAN_POINT('',(-7.69004994112544,0.594050075897772,10.3103198785636));
#99547=CARTESIAN_POINT('Ctrl Pts',(-7.69004994112544,0.594050075897771,
10.3103198785636));
#99548=CARTESIAN_POINT('Ctrl Pts',(-7.74289233197148,0.471846546370226,
10.5058455258076));
#99549=CARTESIAN_POINT('Ctrl Pts',(-7.80487073631704,0.407999999999999,
10.7325975869917));
#99550=CARTESIAN_POINT('Ctrl Pts',(-7.86706805722818,0.408,10.9590385811275));
#99551=CARTESIAN_POINT('',(0.,0.594050075897772,10.3103198785636));
#99552=CARTESIAN_POINT('Ctrl Pts',(-6.90025424549141,2.26194992410223,7.64168012143643));
#99553=CARTESIAN_POINT('Ctrl Pts',(-7.08320222221414,1.69659760459028,8.54624383265556));
#99554=CARTESIAN_POINT('Ctrl Pts',(-7.37565292717963,1.14292103979685,9.43212633632503));
#99555=CARTESIAN_POINT('Ctrl Pts',(-7.69004994112544,0.594050075897773,
10.3103198785636));
#99556=CARTESIAN_POINT('Ctrl Pts',(-6.97247659379779,2.26851485319913,7.63117623488139));
#99557=CARTESIAN_POINT('Ctrl Pts',(-7.15265898639484,1.70551531081965,8.5320736789201));
#99558=CARTESIAN_POINT('Ctrl Pts',(-7.44282948876322,1.15322808712435,9.41561937075472));
#99559=CARTESIAN_POINT('Ctrl Pts',(-7.75660994171048,0.604759632121117,
10.2931845886062));
#99560=CARTESIAN_POINT('Ctrl Pts',(-7.11645477354922,2.32929959675149,7.64004711813815));
#99561=CARTESIAN_POINT('Ctrl Pts',(-7.29124285059876,1.7681463578603,8.53186871114499));
#99562=CARTESIAN_POINT('Ctrl Pts',(-7.57681706437927,1.21707193313286,9.40974380083951));
#99563=CARTESIAN_POINT('Ctrl Pts',(-7.88938556140438,0.668907343792867,
10.2857426732367));
#99564=CARTESIAN_POINT('Ctrl Pts',(-7.1867124928862,2.45386493727086,7.70369083485765));
#99565=CARTESIAN_POINT('Ctrl Pts',(-7.36254955939313,1.88994777765721,8.58798846945041));
#99566=CARTESIAN_POINT('Ctrl Pts',(-7.64807518901743,1.33712897273161,9.46045329326583));
#99567=CARTESIAN_POINT('Ctrl Pts',(-7.9606051534317,0.788498764169076,10.3349903948698));
#99568=CARTESIAN_POINT('Ctrl Pts',(-7.19430053092012,2.51634941530375,7.74120895321998));
#99569=CARTESIAN_POINT('Ctrl Pts',(-7.37274783895309,1.9509970957918,8.62351966308919));
#99570=CARTESIAN_POINT('Ctrl Pts',(-7.65957903289542,1.39732053099838,9.49414527429354));
#99571=CARTESIAN_POINT('Ctrl Pts',(-7.97249537063731,0.848449567099298,
10.3682028984961));
#99572=CARTESIAN_POINT('Ctrl Pts',(-7.01798682228076,1.93536441515669,8.1642169357493));
#99573=CARTESIAN_POINT('Ctrl Pts',(-7.19708258213963,1.48272786223998,8.88843542041603));
#99574=CARTESIAN_POINT('Ctrl Pts',(-7.43642528501808,1.03682530368735,9.60187951410025));
#99575=CARTESIAN_POINT('Ctrl Pts',(-7.69004994112544,0.594050075897773,
10.3103198785636));
#99576=CARTESIAN_POINT('Origin',(-7.69004994112544,0.848449567099298,10.4693195605645));
#99577=CARTESIAN_POINT('Origin',(-6.90025424549141,2.51634941530375,7.80067980343738));
#99578=CARTESIAN_POINT('Ctrl Pts',(-8.14912361676368,0.708019010352452,
10.8568386685932));
#99579=CARTESIAN_POINT('Ctrl Pts',(-8.08692216169042,0.707947174569534,
10.6858877147701));
#99580=CARTESIAN_POINT('Ctrl Pts',(-8.02503872423826,0.756217482327601,
10.5149731412681));
#99581=CARTESIAN_POINT('Ctrl Pts',(-7.97238210650343,0.848667810146629,
10.3678865203213));
#99582=CARTESIAN_POINT('Ctrl Pts',(-8.14913906922654,0.629465787637593,
10.8568651972297));
#99583=CARTESIAN_POINT('Ctrl Pts',(-8.08215444078069,0.632587778955616,
10.6730731227012));
#99584=CARTESIAN_POINT('Ctrl Pts',(-8.01637706856275,0.687463302222793,
10.4908448248287));
#99585=CARTESIAN_POINT('Ctrl Pts',(-7.96048761218811,0.788731610271473,
10.33464988296));
#99586=CARTESIAN_POINT('Ctrl Pts',(-8.08808615036661,0.472961311892115,
10.8791433605059));
#99587=CARTESIAN_POINT('Ctrl Pts',(-8.01711568751622,0.482182663833384,
10.6678349016059));
#99588=CARTESIAN_POINT('Ctrl Pts',(-7.9476905506784,0.5504216418572,10.4612353255527));
#99589=CARTESIAN_POINT('Ctrl Pts',(-7.88930781715051,0.669130461784486,
10.285312321885));
#99590=CARTESIAN_POINT('Ctrl Pts',(-7.941018055592,0.407988882551094,10.9326817955773));
#99591=CARTESIAN_POINT('Ctrl Pts',(-7.87574497017693,0.412984275736558,
10.7069427306826));
#99592=CARTESIAN_POINT('Ctrl Pts',(-7.8112653635522,0.480889739048908,10.4838995104293));
#99593=CARTESIAN_POINT('Ctrl Pts',(-7.75648913737935,0.605033293429943,
10.2927630564964));
#99594=CARTESIAN_POINT('Ctrl Pts',(-7.86720541257699,0.408000103793674,
10.9595386471957));
#99595=CARTESIAN_POINT('Ctrl Pts',(-7.80491620373291,0.407905964356341,
10.7327647510929));
#99596=CARTESIAN_POINT('Ctrl Pts',(-7.74283997308907,0.471850558728987,
10.5056555873962));
#99597=CARTESIAN_POINT('Ctrl Pts',(-7.68993326017625,0.59432004195879,10.3098881354258));
#99598=CARTESIAN_POINT('Ctrl Pts',(-7.19438354265706,2.51611178510568,7.7416193574549));
#99599=CARTESIAN_POINT('Ctrl Pts',(-7.1469608093483,2.66643382276422,7.50719050743819));
#99600=CARTESIAN_POINT('Ctrl Pts',(-7.09936908781228,2.74811551919956,7.23155382342925));
#99601=CARTESIAN_POINT('Ctrl Pts',(-7.06362916697013,2.74802300906478,6.95414127896222));
#99602=CARTESIAN_POINT('Ctrl Pts',(-7.18969017835153,2.47747072284855,7.71840107167769));
#99603=CARTESIAN_POINT('Ctrl Pts',(-7.14400277235099,2.62236748381509,7.49012436326975));
#99604=CARTESIAN_POINT('Ctrl Pts',(-7.09821965127153,2.70026704502063,7.22262797400058));
#99605=CARTESIAN_POINT('Ctrl Pts',(-7.06363490740302,2.69944028986365,6.95415602179916));
#99606=CARTESIAN_POINT('Ctrl Pts',(-7.15489990897137,2.38727021999166,7.66902358769571));
#99607=CARTESIAN_POINT('Ctrl Pts',(-7.11175827397647,2.5194913354541,7.45491010747078));
#99608=CARTESIAN_POINT('Ctrl Pts',(-7.06872790702496,2.58856514291498,7.20598605294427));
#99609=CARTESIAN_POINT('Ctrl Pts',(-7.03586871828815,2.58601736775003,6.95776948019315));
#99610=CARTESIAN_POINT('Ctrl Pts',(-7.07234001721701,2.31860209564756,7.64277634582264));
#99611=CARTESIAN_POINT('Ctrl Pts',(-7.02813588215008,2.44235324221132,7.43966879028346));
#99612=CARTESIAN_POINT('Ctrl Pts',(-6.98392692928295,2.50655355403575,7.20376129641736));
#99613=CARTESIAN_POINT('Ctrl Pts',(-6.95031555185623,2.50367339927263,6.96881823558593));
#99614=CARTESIAN_POINT('Ctrl Pts',(-7.0176774905481,2.29330136612037,7.63800974414729));
#99615=CARTESIAN_POINT('Ctrl Pts',(-6.97218688036359,2.4148874823992,7.4391751906301));
#99616=CARTESIAN_POINT('Ctrl Pts',(-6.92665536682843,2.47850902575575,7.20761906768879));
#99617=CARTESIAN_POINT('Ctrl Pts',(-6.89212767908127,2.47624041956808,6.97632364997799));
#99618=CARTESIAN_POINT('Origin',(-6.76615104985863,2.748,6.99296141887254));
#99619=CARTESIAN_POINT('Ctrl Pts',(-6.97130347175849,2.58761550236908,6.53202630652976));
#99620=CARTESIAN_POINT('Ctrl Pts',(-6.98374576415926,2.58761550236908,6.6750941373724));
#99621=CARTESIAN_POINT('Ctrl Pts',(-6.99922349531613,2.58761550236907,6.81797069470162));
#99622=CARTESIAN_POINT('Ctrl Pts',(-7.0176,2.58761550236908,6.96055403711345));
#99623=CARTESIAN_POINT('Ctrl Pts',(-7.00134514825147,2.63528330527356,6.52941364845747));
#99624=CARTESIAN_POINT('Ctrl Pts',(-7.01375047339156,2.63528330527356,6.67205641086196));
#99625=CARTESIAN_POINT('Ctrl Pts',(-7.02918337436707,2.63528330527356,6.81452097176152));
#99626=CARTESIAN_POINT('Ctrl Pts',(-7.04750769996096,2.63528330527356,6.9566994564933));
#99627=CARTESIAN_POINT('Ctrl Pts',(-7.0176,2.69159478975793,6.52799999999999));
#99628=CARTESIAN_POINT('Ctrl Pts',(-7.02998537672299,2.69159478975793,6.6704133853193));
#99629=CARTESIAN_POINT('Ctrl Pts',(-7.04539389161687,2.69159478975793,6.81265381880387));
#99630=CARTESIAN_POINT('Ctrl Pts',(-7.06369006012712,2.69159478975793,6.95461383265843));
#99631=CARTESIAN_POINT('Ctrl Pts',(-7.0176,2.748,6.52799999999999));
#99632=CARTESIAN_POINT('Ctrl Pts',(-7.02998548375468,2.748,6.67041461602438));
#99633=CARTESIAN_POINT('Ctrl Pts',(-7.04539374054221,2.748,6.8126526466152));
#99634=CARTESIAN_POINT('Ctrl Pts',(-7.06369006012712,2.748,6.95461383265843));
#99635=CARTESIAN_POINT('Origin',(0.,1.224,6.99296141887254));
#99636=CARTESIAN_POINT('',(0.,2.26194992410223,7.64168012143644));
#99637=CARTESIAN_POINT('',(0.,2.448,6.99296141887254));
#99638=CARTESIAN_POINT('Origin',(0.,2.448,7.344));
#99639=CARTESIAN_POINT('',(-2.87791997799628E-16,2.448,-9.694));
#99640=CARTESIAN_POINT('Origin',(0.,2.448,-7.344));
#99641=CARTESIAN_POINT('',(-2.87791997799628E-16,2.448,-17.854));
#99642=CARTESIAN_POINT('Origin',(0.,2.448,-15.504));
#99643=CARTESIAN_POINT('Origin',(6.528,0.708,42.432));
#99644=CARTESIAN_POINT('',(6.528,0.708,41.132));
#99645=CARTESIAN_POINT('Origin',(6.528,0.708,40.832));
#99646=CARTESIAN_POINT('',(5.228,0.708,42.432));
#99647=CARTESIAN_POINT('Origin',(6.528,0.708,42.432));
#99648=CARTESIAN_POINT('Origin',(6.528,0.708,42.432));
#99649=CARTESIAN_POINT('Origin',(6.528,-4.08,42.432));
#99650=CARTESIAN_POINT('',(5.228,0.924,42.432));
#99651=CARTESIAN_POINT('',(5.228,-4.08,42.432));
#99652=CARTESIAN_POINT('',(6.528,0.924,43.732));
#99653=CARTESIAN_POINT('Origin',(6.528,0.924,42.432));
#99654=CARTESIAN_POINT('Origin',(6.528,0.924,42.432));
#99655=CARTESIAN_POINT('Origin',(6.528,0.924,42.432));
#99656=CARTESIAN_POINT('Origin',(6.528,0.924,44.032));
#99657=CARTESIAN_POINT('Origin',(0.,2.748,-7.344));
#99658=CARTESIAN_POINT('',(-2.51052593825207E-16,2.748,-9.394));
#99659=CARTESIAN_POINT('Origin',(-2.87791997799628E-16,2.748,-9.694));
#99660=CARTESIAN_POINT('',(-2.05,2.748,-7.344));
#99661=CARTESIAN_POINT('Origin',(0.,2.748,-7.344));
#99662=CARTESIAN_POINT('Origin',(0.,2.748,-7.344));
#99663=CARTESIAN_POINT('Origin',(0.,-4.08,-7.344));
#99664=CARTESIAN_POINT('',(-2.05,2.964,-7.344));
#99665=CARTESIAN_POINT('',(-2.05,-4.08,-7.344));
#99666=CARTESIAN_POINT('',(-2.51052593825207E-16,2.964,-5.294));
#99667=CARTESIAN_POINT('Origin',(0.,2.964,-7.344));
#99668=CARTESIAN_POINT('Origin',(0.,2.964,-7.344));
#99669=CARTESIAN_POINT('Origin',(0.,2.964,-7.344));
#99670=CARTESIAN_POINT('',(-2.87791997799628E-16,3.264,-4.994));
#99671=CARTESIAN_POINT('Origin',(0.,3.264,-7.344));
#99672=CARTESIAN_POINT('Origin',(-2.87791997799628E-16,2.964,-4.994));
#99673=CARTESIAN_POINT('Origin',(0.,3.264,-24.48));
#99674=CARTESIAN_POINT('',(0.,3.264,7.31936141887254));
#99675=CARTESIAN_POINT('',(-2.87791997799628E-16,3.264,-13.154));
#99676=CARTESIAN_POINT('Origin',(0.,3.264,-15.504));
#99677=CARTESIAN_POINT('Origin',(-6.528,0.708,42.432));
#99678=CARTESIAN_POINT('',(-6.528,0.708,41.132));
#99679=CARTESIAN_POINT('Origin',(-6.528,0.708,40.832));
#99680=CARTESIAN_POINT('',(-7.828,0.708,42.432));
#99681=CARTESIAN_POINT('Origin',(-6.528,0.708,42.432));
#99682=CARTESIAN_POINT('Origin',(-6.528,0.708,42.432));
#99683=CARTESIAN_POINT('Origin',(-6.528,-4.08,42.432));
#99684=CARTESIAN_POINT('',(-7.828,0.924,42.432));
#99685=CARTESIAN_POINT('',(-7.828,-4.08,42.432));
#99686=CARTESIAN_POINT('',(-6.528,0.924,43.732));
#99687=CARTESIAN_POINT('Origin',(-6.528,0.924,42.432));
#99688=CARTESIAN_POINT('Origin',(-6.528,0.924,42.432));
#99689=CARTESIAN_POINT('Origin',(-6.528,0.924,42.432));
#99690=CARTESIAN_POINT('Origin',(-6.528,0.924,44.032));
#99691=CARTESIAN_POINT('Origin',(0.,2.748,-15.504));
#99692=CARTESIAN_POINT('',(-2.51052593825207E-16,2.748,-17.554));
#99693=CARTESIAN_POINT('Origin',(-2.87791997799628E-16,2.748,-17.854));
#99694=CARTESIAN_POINT('',(-2.05,2.748,-15.504));
#99695=CARTESIAN_POINT('Origin',(0.,2.748,-15.504));
#99696=CARTESIAN_POINT('Origin',(0.,2.748,-15.504));
#99697=CARTESIAN_POINT('Origin',(0.,-4.08,-15.504));
#99698=CARTESIAN_POINT('',(-2.05,2.964,-15.504));
#99699=CARTESIAN_POINT('',(-2.05,-4.08,-15.504));
#99700=CARTESIAN_POINT('',(-2.51052593825207E-16,2.964,-13.454));
#99701=CARTESIAN_POINT('Origin',(0.,2.964,-15.504));
#99702=CARTESIAN_POINT('Origin',(0.,2.964,-15.504));
#99703=CARTESIAN_POINT('Origin',(0.,2.964,-15.504));
#99704=CARTESIAN_POINT('Origin',(-2.87791997799628E-16,2.964,-13.154));
#99705=CARTESIAN_POINT('Origin',(0.,0.408,10.608));
#99706=CARTESIAN_POINT('Origin',(0.,2.04,7.31936141887254));
#99707=CARTESIAN_POINT('',(0.,3.07794992410223,7.96808012143643));
#99708=CARTESIAN_POINT('Origin',(0.,2.448,11.2854385811275));
#99709=CARTESIAN_POINT('',(0.,1.41005007589777,10.6367198785636));
#99710=CARTESIAN_POINT('Origin',(0.,3.264,7.6704));
#99711=CARTESIAN_POINT('',(0.,0.,0.));
#99712=CARTESIAN_POINT('Origin',(-5.4672,2.8556,0.));
#99713=CARTESIAN_POINT('',(-5.4672,-2.8556,-3.49710139964518E-16));
#99714=CARTESIAN_POINT('Origin',(-5.4672,0.,0.));
#99715=CARTESIAN_POINT('',(-5.4672,-1.55,-1.8982025386784E-16));
#99716=CARTESIAN_POINT('Origin',(-5.4672,0.,0.));
#99717=CARTESIAN_POINT('Origin',(-5.3856,0.,0.));
#99718=CARTESIAN_POINT('',(-5.304,-2.8556,-3.49710139964518E-16));
#99719=CARTESIAN_POINT('Origin',(-5.304,0.,0.));
#99720=CARTESIAN_POINT('',(-5.3856,-2.8556,-3.49710139964518E-16));
#99721=CARTESIAN_POINT('Origin',(-5.1,0.,0.));
#99722=CARTESIAN_POINT('',(-5.304,-5.3856,-6.59545780148798E-16));
#99723=CARTESIAN_POINT('Origin',(-5.304,0.,0.));
#99724=CARTESIAN_POINT('',(-4.896,-5.3856,-6.59545780148798E-16));
#99725=CARTESIAN_POINT('',(-5.1,-5.3856,-6.59545780148799E-16));
#99726=CARTESIAN_POINT('Origin',(-4.896,0.,0.));
#99727=CARTESIAN_POINT('Origin',(-4.896,3.2636,0.));
#99728=CARTESIAN_POINT('',(-4.896,-3.2636,-3.9967572936973E-16));
#99729=CARTESIAN_POINT('Origin',(-4.896,0.,0.));
#99730=CARTESIAN_POINT('Origin',(-5.1,0.,0.));
#99731=CARTESIAN_POINT('',(-5.304,-3.2636,-3.9967572936973E-16));
#99732=CARTESIAN_POINT('',(-5.1,-3.2636,-3.9967572936973E-16));
#99733=CARTESIAN_POINT('Origin',(-5.304,0.,0.));
#99734=CARTESIAN_POINT('Origin',(-5.304,6.0384,0.));
#99735=CARTESIAN_POINT('Origin',(5.3856,0.,0.));
#99736=CARTESIAN_POINT('',(5.4672,-2.8556,-3.49710139964518E-16));
#99737=CARTESIAN_POINT('Origin',(5.4672,0.,0.));
#99738=CARTESIAN_POINT('',(5.304,-2.8556,-3.49710139964518E-16));
#99739=CARTESIAN_POINT('',(5.3856,-2.8556,-3.49710139964518E-16));
#99740=CARTESIAN_POINT('Origin',(5.304,0.,0.));
#99741=CARTESIAN_POINT('Origin',(5.4672,1.55,0.));
#99742=CARTESIAN_POINT('',(5.4672,-1.55,-1.8982025386784E-16));
#99743=CARTESIAN_POINT('Origin',(5.4672,0.,0.));
#99744=CARTESIAN_POINT('Origin',(5.1,0.,0.));
#99745=CARTESIAN_POINT('',(5.304,-3.2636,-3.9967572936973E-16));
#99746=CARTESIAN_POINT('Origin',(5.304,0.,0.));
#99747=CARTESIAN_POINT('',(4.896,-3.2636,-3.9967572936973E-16));
#99748=CARTESIAN_POINT('',(5.1,-3.2636,-3.9967572936973E-16));
#99749=CARTESIAN_POINT('Origin',(4.896,0.,0.));
#99750=CARTESIAN_POINT('Origin',(4.896,5.3856,0.));
#99751=CARTESIAN_POINT('',(4.896,-5.3856,-6.59545780148798E-16));
#99752=CARTESIAN_POINT('Origin',(4.896,0.,0.));
#99753=CARTESIAN_POINT('Origin',(5.1,0.,0.));
#99754=CARTESIAN_POINT('',(5.304,-5.3856,-6.59545780148798E-16));
#99755=CARTESIAN_POINT('',(5.1,-5.3856,-6.59545780148799E-16));
#99756=CARTESIAN_POINT('Origin',(5.304,0.,0.));
#99757=CARTESIAN_POINT('Origin',(5.304,1.55,0.));
#99758=CARTESIAN_POINT('',(5.304,-6.0384,-7.39490723197138E-16));
#99759=CARTESIAN_POINT('Origin',(5.304,0.,0.));
#99760=CARTESIAN_POINT('Origin',(3.9984,6.2424,0.));
#99761=CARTESIAN_POINT('',(3.9984,-6.528,-7.99449430483392E-16));
#99762=CARTESIAN_POINT('Origin',(3.9984,0.,0.));
#99763=CARTESIAN_POINT('',(3.9984,-6.2424,-7.64473517899744E-16));
#99764=CARTESIAN_POINT('Origin',(3.9984,0.,0.));
#99765=CARTESIAN_POINT('Origin',(3.672,0.,0.));
#99766=CARTESIAN_POINT('',(3.3456,-6.2424,-7.64473517899744E-16));
#99767=CARTESIAN_POINT('',(3.672,-6.2424,-7.64473517899744E-16));
#99768=CARTESIAN_POINT('Origin',(3.3456,0.,0.));
#99769=CARTESIAN_POINT('Origin',(3.3456,6.936,0.));
#99770=CARTESIAN_POINT('',(3.3456,-6.528,7.99449430483392E-16));
#99771=CARTESIAN_POINT('Origin',(3.3456,0.,0.));
#99772=CARTESIAN_POINT('Origin',(0.,0.,0.));
#99773=CARTESIAN_POINT('',(-3.3456,-6.528,-7.99449430483392E-16));
#99774=CARTESIAN_POINT('',(0.,-6.528,-7.99449430483392E-16));
#99775=CARTESIAN_POINT('Origin',(-3.3456,0.,0.));
#99776=CARTESIAN_POINT('Origin',(-3.3456,6.2424,0.));
#99777=CARTESIAN_POINT('',(-3.3456,-6.2424,-7.64473517899744E-16));
#99778=CARTESIAN_POINT('Origin',(-3.3456,0.,0.));
#99779=CARTESIAN_POINT('Origin',(-3.672,0.,0.));
#99780=CARTESIAN_POINT('',(-3.9984,-6.2424,-7.64473517899744E-16));
#99781=CARTESIAN_POINT('',(-3.672,-6.2424,-7.64473517899744E-16));
#99782=CARTESIAN_POINT('Origin',(-3.9984,0.,0.));
#99783=CARTESIAN_POINT('Origin',(-3.9984,6.936,0.));
#99784=CARTESIAN_POINT('',(-3.9984,-6.528,7.99449430483392E-16));
#99785=CARTESIAN_POINT('Origin',(-3.9984,0.,0.));
#99786=CARTESIAN_POINT('Origin',(0.,0.,0.));
#99787=CARTESIAN_POINT('',(-4.8144,-6.528,-7.99449430483392E-16));
#99788=CARTESIAN_POINT('',(0.,-6.528,-7.99449430483392E-16));
#99789=CARTESIAN_POINT('Origin',(-4.8144,0.,0.));
#99790=CARTESIAN_POINT('Origin',(-5.0592,0.,0.));
#99791=CARTESIAN_POINT('',(-5.304,-6.0384,-7.39490723197138E-16));
#99792=CARTESIAN_POINT('',(-5.0592,-6.2832,-7.69470076840265E-16));
#99793=CARTESIAN_POINT('Origin',(-5.304,0.,0.));
#99794=CARTESIAN_POINT('Origin',(0.,0.,0.));
#99795=CARTESIAN_POINT('',(4.8144,-6.528,-7.99449430483392E-16));
#99796=CARTESIAN_POINT('Origin',(4.8144,0.,0.));
#99797=CARTESIAN_POINT('',(0.,-6.528,-7.99449430483392E-16));
#99798=CARTESIAN_POINT('Origin',(5.0592,0.,0.));
#99799=CARTESIAN_POINT('',(5.0592,-6.2832,7.69470076840265E-16));
#99800=CARTESIAN_POINT('Origin',(5.304,1.55,0.));
#99801=CARTESIAN_POINT('Origin',(0.,0.,0.));
#99802=CARTESIAN_POINT('',(0.,-1.55,-1.8982025386784E-16));
#99803=CARTESIAN_POINT('Origin',(-5.304,6.0384,0.));
#99804=CARTESIAN_POINT('',(0.,0.,0.));
#99805=CARTESIAN_POINT('Origin',(-5.1816,0.,0.));
#99806=CARTESIAN_POINT('',(-5.0592,-2.448,-2.99793536431272E-16));
#99807=CARTESIAN_POINT('Origin',(-5.0592,0.,0.));
#99808=CARTESIAN_POINT('',(-5.304,-2.2032,-2.69814182788145E-16));
#99809=CARTESIAN_POINT('',(-5.1816,-2.3256,-2.84803859609709E-16));
#99810=CARTESIAN_POINT('Origin',(-5.304,0.,0.));
#99811=CARTESIAN_POINT('Origin',(0.,0.,0.));
#99812=CARTESIAN_POINT('',(5.0592,-2.448,-2.99793536431272E-16));
#99813=CARTESIAN_POINT('Origin',(5.0592,0.,0.));
#99814=CARTESIAN_POINT('',(0.,-2.448,-2.99793536431272E-16));
#99815=CARTESIAN_POINT('Origin',(5.1816,0.,0.));
#99816=CARTESIAN_POINT('',(5.304,-2.2032,-2.69814182788145E-16));
#99817=CARTESIAN_POINT('',(5.1816,-2.3256,2.84803859609709E-16));
#99818=CARTESIAN_POINT('Origin',(5.304,0.,0.));
#99819=CARTESIAN_POINT('Origin',(5.304,1.3,0.));
#99820=CARTESIAN_POINT('',(5.304,-1.3,-1.59204083889156E-16));
#99821=CARTESIAN_POINT('Origin',(5.304,0.,0.));
#99822=CARTESIAN_POINT('Origin',(0.,0.,0.));
#99823=CARTESIAN_POINT('',(-5.304,-1.3,-1.59204083889156E-16));
#99824=CARTESIAN_POINT('Origin',(-5.304,0.,0.));
#99825=CARTESIAN_POINT('',(0.,-1.3,-1.59204083889156E-16));
#99826=CARTESIAN_POINT('Origin',(-5.304,2.2032,0.));
#99827=CARTESIAN_POINT('',(0.,0.,0.));
#99828=CARTESIAN_POINT('Origin',(-7.8368,0.,0.));
#99829=CARTESIAN_POINT('',(-7.6736,-1.5,-1.83697019872103E-16));
#99830=CARTESIAN_POINT('Origin',(-7.6736,0.,0.));
#99831=CARTESIAN_POINT('',(-8.,-1.1736,-1.43724548347933E-16));
#99832=CARTESIAN_POINT('',(-7.8368,-1.3368,-1.63710784110018E-16));
#99833=CARTESIAN_POINT('Origin',(-8.,0.,0.));
#99834=CARTESIAN_POINT('Origin',(0.,0.,0.));
#99835=CARTESIAN_POINT('',(7.6736,-1.5,-1.83697019872103E-16));
#99836=CARTESIAN_POINT('Origin',(7.6736,0.,0.));
#99837=CARTESIAN_POINT('',(0.,-1.5,-1.83697019872103E-16));
#99838=CARTESIAN_POINT('Origin',(7.8368,0.,0.));
#99839=CARTESIAN_POINT('',(8.,-1.1736,-1.43724548347933E-16));
#99840=CARTESIAN_POINT('',(7.8368,-1.3368,1.63710784110018E-16));
#99841=CARTESIAN_POINT('Origin',(8.,0.,0.));
#99842=CARTESIAN_POINT('Origin',(8.,0.,0.));
#99843=CARTESIAN_POINT('Origin',(-8.,1.1736,0.));
#99844=CARTESIAN_POINT('',(0.,0.,0.));
#99845=CARTESIAN_POINT('Origin',(-7.8368,0.,0.));
#99846=CARTESIAN_POINT('',(-7.6736,-1.25,-1.53080849893419E-16));
#99847=CARTESIAN_POINT('Origin',(-7.6736,0.,0.));
#99848=CARTESIAN_POINT('',(-8.,-0.9236,-1.1310837836925E-16));
#99849=CARTESIAN_POINT('',(-7.8368,-1.0868,-1.33094614131334E-16));
#99850=CARTESIAN_POINT('Origin',(-8.,0.,0.));
#99851=CARTESIAN_POINT('Origin',(0.,0.,0.));
#99852=CARTESIAN_POINT('',(7.6736,-1.25,-1.53080849893419E-16));
#99853=CARTESIAN_POINT('Origin',(7.6736,0.,0.));
#99854=CARTESIAN_POINT('',(0.,-1.25,-1.53080849893419E-16));
#99855=CARTESIAN_POINT('Origin',(7.8368,0.,0.));
#99856=CARTESIAN_POINT('',(8.,-0.9236,-1.1310837836925E-16));
#99857=CARTESIAN_POINT('',(7.8368,-1.0868,1.33094614131334E-16));
#99858=CARTESIAN_POINT('Origin',(8.,0.,0.));
#99859=CARTESIAN_POINT('Origin',(8.,0.,0.));
#99860=CARTESIAN_POINT('Origin',(-8.,0.9236,0.));
#99861=CARTESIAN_POINT('',(0.,0.,0.));
#99862=CARTESIAN_POINT('Origin',(0.,2.1216,0.));
#99863=CARTESIAN_POINT('',(5.20417042793042E-16,-2.1216,-2.59821064907102E-16));
#99864=CARTESIAN_POINT('Origin',(0.,0.,0.));
#99865=CARTESIAN_POINT('Origin',(0.163200000000001,0.,0.));
#99866=CARTESIAN_POINT('',(0.326400000000001,-2.448,-2.99793536431272E-16));
#99867=CARTESIAN_POINT('Origin',(0.3264,0.,0.));
#99868=CARTESIAN_POINT('',(0.163200000000001,-2.2848,-2.79807300669187E-16));
#99869=CARTESIAN_POINT('Origin',(0.7752,0.,0.));
#99870=CARTESIAN_POINT('',(1.224,-2.448,-2.99793536431272E-16));
#99871=CARTESIAN_POINT('Origin',(1.224,0.,0.));
#99872=CARTESIAN_POINT('',(0.7752,-2.448,-2.99793536431272E-16));
#99873=CARTESIAN_POINT('Origin',(1.224,4.488,0.));
#99874=CARTESIAN_POINT('',(1.224,-4.488,-5.49621483457332E-16));
#99875=CARTESIAN_POINT('Origin',(1.224,0.,0.));
#99876=CARTESIAN_POINT('Origin',(4.284,0.,0.));
#99877=CARTESIAN_POINT('',(7.344,-4.488,-5.49621483457332E-16));
#99878=CARTESIAN_POINT('Origin',(7.344,0.,0.));
#99879=CARTESIAN_POINT('',(4.284,-4.488,-5.49621483457332E-16));
#99880=CARTESIAN_POINT('Origin',(7.548,0.,0.));
#99881=CARTESIAN_POINT('',(7.752,-4.08,-4.9965589405212E-16));
#99882=CARTESIAN_POINT('',(7.548,-4.284,5.24638688754726E-16));
#99883=CARTESIAN_POINT('Origin',(7.752,0.,0.));
#99884=CARTESIAN_POINT('Origin',(7.752,3.264,0.));
#99885=CARTESIAN_POINT('',(7.752,-3.264,-3.99724715241696E-16));
#99886=CARTESIAN_POINT('Origin',(7.752,0.,0.));
#99887=CARTESIAN_POINT('Origin',(10.2,0.,0.));
#99888=CARTESIAN_POINT('',(12.648,-3.264,-3.99724715241696E-16));
#99889=CARTESIAN_POINT('Origin',(12.648,0.,0.));
#99890=CARTESIAN_POINT('',(10.2,-3.264,-3.99724715241696E-16));
#99891=CARTESIAN_POINT('Origin',(12.648,2.9376,0.));
#99892=CARTESIAN_POINT('',(12.648,-2.9376,-3.59752243717526E-16));
#99893=CARTESIAN_POINT('Origin',(12.648,0.,0.));
#99894=CARTESIAN_POINT('Origin',(12.9744,0.,0.));
#99895=CARTESIAN_POINT('',(13.3008,-2.9376,-3.59752243717526E-16));
#99896=CARTESIAN_POINT('Origin',(13.3008,0.,0.));
#99897=CARTESIAN_POINT('',(12.9744,-2.9376,-3.59752243717527E-16));
#99898=CARTESIAN_POINT('Origin',(13.3008,3.264,0.));
#99899=CARTESIAN_POINT('',(13.3008,-3.264,-3.99724715241696E-16));
#99900=CARTESIAN_POINT('Origin',(13.3008,0.,0.));
#99901=CARTESIAN_POINT('Origin',(14.28,0.,0.));
#99902=CARTESIAN_POINT('',(15.2592,-3.264,-3.99724715241696E-16));
#99903=CARTESIAN_POINT('Origin',(15.2592,0.,0.));
#99904=CARTESIAN_POINT('',(14.28,-3.264,-3.99724715241696E-16));
#99905=CARTESIAN_POINT('Origin',(15.5856,0.,0.));
#99906=CARTESIAN_POINT('',(15.912,-2.6112,-3.19779772193357E-16));
#99907=CARTESIAN_POINT('',(15.5856,-2.9376,3.59752243717527E-16));
#99908=CARTESIAN_POINT('Origin',(15.912,0.,0.));
#99909=CARTESIAN_POINT('Origin',(15.912,0.,0.));
#99910=CARTESIAN_POINT('',(0.,0.,0.));
#99911=CARTESIAN_POINT('Origin',(0.2448,0.,0.));
#99912=CARTESIAN_POINT('',(0.4896,-2.5,-3.06161699786838E-16));
#99913=CARTESIAN_POINT('Origin',(0.4896,0.,0.));
#99914=CARTESIAN_POINT('',(0.,-2.0104,-2.46202992500584E-16));
#99915=CARTESIAN_POINT('',(0.2448,-2.2552,-2.76182346143711E-16));
#99916=CARTESIAN_POINT('Origin',(0.,0.,0.));
#99917=CARTESIAN_POINT('Origin',(4.,0.,0.));
#99918=CARTESIAN_POINT('',(7.5104,-2.5,-3.06161699786838E-16));
#99919=CARTESIAN_POINT('Origin',(7.5104,0.,0.));
#99920=CARTESIAN_POINT('',(4.,-2.5,-3.06161699786838E-16));
#99921=CARTESIAN_POINT('Origin',(7.7552,0.,0.));
#99922=CARTESIAN_POINT('',(8.,-2.0104,-2.46202992500584E-16));
#99923=CARTESIAN_POINT('',(7.7552,-2.2552,2.76182346143711E-16));
#99924=CARTESIAN_POINT('Origin',(8.,0.,0.));
#99925=CARTESIAN_POINT('Origin',(8.,0.,0.));
#99926=CARTESIAN_POINT('Origin',(0.,2.0104,0.));
#99927=CARTESIAN_POINT('',(0.,0.,0.));
#99928=CARTESIAN_POINT('Origin',(1.35208333333333,-4.16333634234434E-16,
0.));
#99929=CARTESIAN_POINT('',(0.,3.5,0.));
#99930=CARTESIAN_POINT('Origin',(0.,0.,0.));
#99931=CARTESIAN_POINT('Origin',(0.,2.,0.));
#99932=CARTESIAN_POINT('',(0.,-2.,-2.44929359829471E-16));
#99933=CARTESIAN_POINT('Origin',(0.,0.,0.));
#99934=CARTESIAN_POINT('Origin',(2.7336,0.,0.));
#99935=CARTESIAN_POINT('',(5.4672,-2.,-2.44929359829471E-16));
#99936=CARTESIAN_POINT('Origin',(5.4672,0.,0.));
#99937=CARTESIAN_POINT('',(2.7336,-2.,-2.44929359829471E-16));
#99938=CARTESIAN_POINT('Origin',(5.4672,3.2,0.));
#99939=CARTESIAN_POINT('',(5.4672,-3.2,-3.91886975727153E-16));
#99940=CARTESIAN_POINT('Origin',(5.4672,0.,0.));
#99941=CARTESIAN_POINT('Origin',(5.916,0.,0.));
#99942=CARTESIAN_POINT('',(6.3648,-3.2,-3.91886975727153E-16));
#99943=CARTESIAN_POINT('Origin',(6.3648,0.,0.));
#99944=CARTESIAN_POINT('',(5.916,-3.2,-3.91886975727153E-16));
#99945=CARTESIAN_POINT('Origin',(6.528,0.,0.));
#99946=CARTESIAN_POINT('',(6.6912,-2.8736,-3.51914504202983E-16));
#99947=CARTESIAN_POINT('',(6.528,-3.0368,3.71900739965068E-16));
#99948=CARTESIAN_POINT('Origin',(6.6912,0.,0.));
#99949=CARTESIAN_POINT('Origin',(6.6912,0.,0.));
#99950=CARTESIAN_POINT('',(0.,0.,0.));
#99951=CARTESIAN_POINT('Origin',(0.863333333333333,5.55111512312578E-16,
0.));
#99952=CARTESIAN_POINT('',(0.,2.2,0.));
#99953=CARTESIAN_POINT('Origin',(0.,0.,0.));
#99954=CARTESIAN_POINT('Origin',(0.,1.25,0.));
#99955=CARTESIAN_POINT('',(0.,-1.25,-1.53080849893419E-16));
#99956=CARTESIAN_POINT('Origin',(0.,0.,0.));
#99957=CARTESIAN_POINT('Origin',(2.5296,0.,0.));
#99958=CARTESIAN_POINT('',(5.0592,-1.25,-1.53080849893419E-16));
#99959=CARTESIAN_POINT('Origin',(5.0592,0.,0.));
#99960=CARTESIAN_POINT('',(2.5296,-1.25,-1.53080849893419E-16));
#99961=CARTESIAN_POINT('Origin',(5.1816,0.,0.));
#99962=CARTESIAN_POINT('',(5.304,-1.0052,-1.23101496250292E-16));
#99963=CARTESIAN_POINT('',(5.1816,-1.1276,1.38091173071856E-16));
#99964=CARTESIAN_POINT('Origin',(5.304,0.,0.));
#99965=CARTESIAN_POINT('Origin',(5.304,0.,0.));
#99966=CARTESIAN_POINT('',(0.,0.,14.688));
#99967=CARTESIAN_POINT('',(0.,0.,0.));
#99968=CARTESIAN_POINT('',(0.,0.,0.));
#99969=CARTESIAN_POINT('',(0.,0.,0.));
#99970=CARTESIAN_POINT('',(0.,14.688,40.8));
#99971=CARTESIAN_POINT('',(0.,14.688,-22.848));
#99972=CARTESIAN_POINT('',(0.,0.,0.));
#99973=CARTESIAN_POINT('',(0.,14.688,10.608));
#99974=CARTESIAN_POINT('',(0.,14.688,32.64));
#99975=CARTESIAN_POINT('',(21.216,10.6896,-3.264));
#99976=CARTESIAN_POINT('',(21.216,19.9512,6.528));
#99977=CARTESIAN_POINT('',(21.624,10.6896,-3.264));
#99978=CARTESIAN_POINT('',(21.624,19.9512,6.528));
#99979=CARTESIAN_POINT('',(44.064,22.44,37.944));
#99980=CARTESIAN_POINT('',(28.152,25.704,28.56));
#99981=CARTESIAN_POINT('',(0.,-2.12745657088303,-7.344));
#99982=CARTESIAN_POINT('',(6.528,0.408,42.432));
#99983=CARTESIAN_POINT('',(0.,0.,0.));
#99984=CARTESIAN_POINT('',(-21.216,10.6896,-3.264));
#99985=CARTESIAN_POINT('',(-21.216,19.9512,6.528));
#99986=CARTESIAN_POINT('',(-21.624,10.6896,-3.264));
#99987=CARTESIAN_POINT('',(-21.624,19.9512,6.528));
#99988=CARTESIAN_POINT('',(-44.064,22.44,37.944));
#99989=CARTESIAN_POINT('',(-28.152,25.704,28.56));
#99990=CARTESIAN_POINT('',(0.,-2.1884740360911,-15.504));
#99991=CARTESIAN_POINT('',(-6.528,0.408,42.432));
#99992=UNCERTAINTY_MEASURE_WITH_UNIT(LENGTH_MEASURE(0.01),#100032,
'DISTANCE_ACCURACY_VALUE',
'Maximum model space distance between geometric entities at asserted c
onnectivities');
#99993=UNCERTAINTY_MEASURE_WITH_UNIT(LENGTH_MEASURE(0.01),#100032,
'DISTANCE_ACCURACY_VALUE',
'Maximum model space distance between geometric entities at asserted c
onnectivities');
#99994=UNCERTAINTY_MEASURE_WITH_UNIT(LENGTH_MEASURE(0.01),#100032,
'DISTANCE_ACCURACY_VALUE',
'Maximum model space distance between geometric entities at asserted c
onnectivities');
#99995=UNCERTAINTY_MEASURE_WITH_UNIT(LENGTH_MEASURE(0.01),#100032,
'DISTANCE_ACCURACY_VALUE',
'Maximum model space distance between geometric entities at asserted c
onnectivities');
#99996=UNCERTAINTY_MEASURE_WITH_UNIT(LENGTH_MEASURE(0.01),#100032,
'DISTANCE_ACCURACY_VALUE',
'Maximum model space distance between geometric entities at asserted c
onnectivities');
#99997=UNCERTAINTY_MEASURE_WITH_UNIT(LENGTH_MEASURE(0.01),#100032,
'DISTANCE_ACCURACY_VALUE',
'Maximum model space distance between geometric entities at asserted c
onnectivities');
#99998=UNCERTAINTY_MEASURE_WITH_UNIT(LENGTH_MEASURE(0.01),#100032,
'DISTANCE_ACCURACY_VALUE',
'Maximum model space distance between geometric entities at asserted c
onnectivities');
#99999=UNCERTAINTY_MEASURE_WITH_UNIT(LENGTH_MEASURE(0.01),#100032,
'DISTANCE_ACCURACY_VALUE',
'Maximum model space distance between geometric entities at asserted c
onnectivities');
#100000=UNCERTAINTY_MEASURE_WITH_UNIT(LENGTH_MEASURE(0.01),#100032,
'DISTANCE_ACCURACY_VALUE',
'Maximum model space distance between geometric entities at asserted c
onnectivities');
#100001=UNCERTAINTY_MEASURE_WITH_UNIT(LENGTH_MEASURE(0.01),#100032,
'DISTANCE_ACCURACY_VALUE',
'Maximum model space distance between geometric entities at asserted c
onnectivities');
#100002=UNCERTAINTY_MEASURE_WITH_UNIT(LENGTH_MEASURE(0.01),#100032,
'DISTANCE_ACCURACY_VALUE',
'Maximum model space distance between geometric entities at asserted c
onnectivities');
#100003=UNCERTAINTY_MEASURE_WITH_UNIT(LENGTH_MEASURE(0.01),#100032,
'DISTANCE_ACCURACY_VALUE',
'Maximum model space distance between geometric entities at asserted c
onnectivities');
#100004=UNCERTAINTY_MEASURE_WITH_UNIT(LENGTH_MEASURE(0.01),#100032,
'DISTANCE_ACCURACY_VALUE',
'Maximum model space distance between geometric entities at asserted c
onnectivities');
#100005=UNCERTAINTY_MEASURE_WITH_UNIT(LENGTH_MEASURE(0.01),#100032,
'DISTANCE_ACCURACY_VALUE',
'Maximum model space distance between geometric entities at asserted c
onnectivities');
#100006=UNCERTAINTY_MEASURE_WITH_UNIT(LENGTH_MEASURE(0.01),#100032,
'DISTANCE_ACCURACY_VALUE',
'Maximum model space distance between geometric entities at asserted c
onnectivities');
#100007=UNCERTAINTY_MEASURE_WITH_UNIT(LENGTH_MEASURE(0.01),#100032,
'DISTANCE_ACCURACY_VALUE',
'Maximum model space distance between geometric entities at asserted c
onnectivities');
#100008=UNCERTAINTY_MEASURE_WITH_UNIT(LENGTH_MEASURE(0.01),#100032,
'DISTANCE_ACCURACY_VALUE',
'Maximum model space distance between geometric entities at asserted c
onnectivities');
#100009=UNCERTAINTY_MEASURE_WITH_UNIT(LENGTH_MEASURE(0.01),#100032,
'DISTANCE_ACCURACY_VALUE',
'Maximum model space distance between geometric entities at asserted c
onnectivities');
#100010=UNCERTAINTY_MEASURE_WITH_UNIT(LENGTH_MEASURE(0.01),#100032,
'DISTANCE_ACCURACY_VALUE',
'Maximum model space distance between geometric entities at asserted c
onnectivities');
#100011=UNCERTAINTY_MEASURE_WITH_UNIT(LENGTH_MEASURE(0.01),#100032,
'DISTANCE_ACCURACY_VALUE',
'Maximum model space distance between geometric entities at asserted c
onnectivities');
#100012=(
GEOMETRIC_REPRESENTATION_CONTEXT(3)
GLOBAL_UNCERTAINTY_ASSIGNED_CONTEXT((#99992))
GLOBAL_UNIT_ASSIGNED_CONTEXT((#100032,#100034,#100035))
REPRESENTATION_CONTEXT('','3D')
);
#100013=(
GEOMETRIC_REPRESENTATION_CONTEXT(3)
GLOBAL_UNCERTAINTY_ASSIGNED_CONTEXT((#99993))
GLOBAL_UNIT_ASSIGNED_CONTEXT((#100032,#100034,#100035))
REPRESENTATION_CONTEXT('','3D')
);
#100014=(
GEOMETRIC_REPRESENTATION_CONTEXT(3)
GLOBAL_UNCERTAINTY_ASSIGNED_CONTEXT((#99994))
GLOBAL_UNIT_ASSIGNED_CONTEXT((#100032,#100034,#100035))
REPRESENTATION_CONTEXT('','3D')
);
#100015=(
GEOMETRIC_REPRESENTATION_CONTEXT(3)
GLOBAL_UNCERTAINTY_ASSIGNED_CONTEXT((#99995))
GLOBAL_UNIT_ASSIGNED_CONTEXT((#100032,#100034,#100035))
REPRESENTATION_CONTEXT('','3D')
);
#100016=(
GEOMETRIC_REPRESENTATION_CONTEXT(3)
GLOBAL_UNCERTAINTY_ASSIGNED_CONTEXT((#99996))
GLOBAL_UNIT_ASSIGNED_CONTEXT((#100032,#100034,#100035))
REPRESENTATION_CONTEXT('','3D')
);
#100017=(
GEOMETRIC_REPRESENTATION_CONTEXT(3)
GLOBAL_UNCERTAINTY_ASSIGNED_CONTEXT((#99997))
GLOBAL_UNIT_ASSIGNED_CONTEXT((#100032,#100034,#100035))
REPRESENTATION_CONTEXT('','3D')
);
#100018=(
GEOMETRIC_REPRESENTATION_CONTEXT(3)
GLOBAL_UNCERTAINTY_ASSIGNED_CONTEXT((#99998))
GLOBAL_UNIT_ASSIGNED_CONTEXT((#100032,#100034,#100035))
REPRESENTATION_CONTEXT('','3D')
);
#100019=(
GEOMETRIC_REPRESENTATION_CONTEXT(3)
GLOBAL_UNCERTAINTY_ASSIGNED_CONTEXT((#99999))
GLOBAL_UNIT_ASSIGNED_CONTEXT((#100032,#100034,#100035))
REPRESENTATION_CONTEXT('','3D')
);
#100020=(
GEOMETRIC_REPRESENTATION_CONTEXT(3)
GLOBAL_UNCERTAINTY_ASSIGNED_CONTEXT((#100000))
GLOBAL_UNIT_ASSIGNED_CONTEXT((#100032,#100034,#100035))
REPRESENTATION_CONTEXT('','3D')
);
#100021=(
GEOMETRIC_REPRESENTATION_CONTEXT(3)
GLOBAL_UNCERTAINTY_ASSIGNED_CONTEXT((#100001))
GLOBAL_UNIT_ASSIGNED_CONTEXT((#100032,#100034,#100035))
REPRESENTATION_CONTEXT('','3D')
);
#100022=(
GEOMETRIC_REPRESENTATION_CONTEXT(3)
GLOBAL_UNCERTAINTY_ASSIGNED_CONTEXT((#100002))
GLOBAL_UNIT_ASSIGNED_CONTEXT((#100032,#100034,#100035))
REPRESENTATION_CONTEXT('','3D')
);
#100023=(
GEOMETRIC_REPRESENTATION_CONTEXT(3)
GLOBAL_UNCERTAINTY_ASSIGNED_CONTEXT((#100003))
GLOBAL_UNIT_ASSIGNED_CONTEXT((#100032,#100034,#100035))
REPRESENTATION_CONTEXT('','3D')
);
#100024=(
GEOMETRIC_REPRESENTATION_CONTEXT(3)
GLOBAL_UNCERTAINTY_ASSIGNED_CONTEXT((#100004))
GLOBAL_UNIT_ASSIGNED_CONTEXT((#100032,#100034,#100035))
REPRESENTATION_CONTEXT('','3D')
);
#100025=(
GEOMETRIC_REPRESENTATION_CONTEXT(3)
GLOBAL_UNCERTAINTY_ASSIGNED_CONTEXT((#100005))
GLOBAL_UNIT_ASSIGNED_CONTEXT((#100032,#100034,#100035))
REPRESENTATION_CONTEXT('','3D')
);
#100026=(
GEOMETRIC_REPRESENTATION_CONTEXT(3)
GLOBAL_UNCERTAINTY_ASSIGNED_CONTEXT((#100006))
GLOBAL_UNIT_ASSIGNED_CONTEXT((#100032,#100034,#100035))
REPRESENTATION_CONTEXT('','3D')
);
#100027=(
GEOMETRIC_REPRESENTATION_CONTEXT(3)
GLOBAL_UNCERTAINTY_ASSIGNED_CONTEXT((#100007))
GLOBAL_UNIT_ASSIGNED_CONTEXT((#100032,#100034,#100035))
REPRESENTATION_CONTEXT('','3D')
);
#100028=(
GEOMETRIC_REPRESENTATION_CONTEXT(3)
GLOBAL_UNCERTAINTY_ASSIGNED_CONTEXT((#100008))
GLOBAL_UNIT_ASSIGNED_CONTEXT((#100032,#100034,#100035))
REPRESENTATION_CONTEXT('','3D')
);
#100029=(
GEOMETRIC_REPRESENTATION_CONTEXT(3)
GLOBAL_UNCERTAINTY_ASSIGNED_CONTEXT((#100009))
GLOBAL_UNIT_ASSIGNED_CONTEXT((#100032,#100034,#100035))
REPRESENTATION_CONTEXT('','3D')
);
#100030=(
GEOMETRIC_REPRESENTATION_CONTEXT(3)
GLOBAL_UNCERTAINTY_ASSIGNED_CONTEXT((#100010))
GLOBAL_UNIT_ASSIGNED_CONTEXT((#100032,#100034,#100035))
REPRESENTATION_CONTEXT('','3D')
);
#100031=(
GEOMETRIC_REPRESENTATION_CONTEXT(3)
GLOBAL_UNCERTAINTY_ASSIGNED_CONTEXT((#100011))
GLOBAL_UNIT_ASSIGNED_CONTEXT((#100032,#100034,#100035))
REPRESENTATION_CONTEXT('','3D')
);
#100032=(
LENGTH_UNIT()
NAMED_UNIT(*)
SI_UNIT(.MILLI.,.METRE.)
);
#100033=(
LENGTH_UNIT()
NAMED_UNIT(*)
SI_UNIT($,.METRE.)
);
#100034=(
NAMED_UNIT(*)
PLANE_ANGLE_UNIT()
SI_UNIT($,.RADIAN.)
);
#100035=(
NAMED_UNIT(*)
SI_UNIT($,.STERADIAN.)
SOLID_ANGLE_UNIT()
);
#100036=SHAPE_DEFINITION_REPRESENTATION(#100055,#100100);
#100037=SHAPE_DEFINITION_REPRESENTATION(#100056,#100101);
#100038=SHAPE_DEFINITION_REPRESENTATION(#100057,#100102);
#100039=SHAPE_DEFINITION_REPRESENTATION(#100058,#100103);
#100040=SHAPE_DEFINITION_REPRESENTATION(#100059,#100104);
#100041=SHAPE_DEFINITION_REPRESENTATION(#100060,#100105);
#100042=SHAPE_DEFINITION_REPRESENTATION(#100061,#100106);
#100043=SHAPE_DEFINITION_REPRESENTATION(#100062,#100107);
#100044=SHAPE_DEFINITION_REPRESENTATION(#100063,#100108);
#100045=SHAPE_DEFINITION_REPRESENTATION(#100064,#100109);
#100046=SHAPE_DEFINITION_REPRESENTATION(#100065,#100110);
#100047=SHAPE_DEFINITION_REPRESENTATION(#100066,#100111);
#100048=SHAPE_DEFINITION_REPRESENTATION(#100067,#100112);
#100049=SHAPE_DEFINITION_REPRESENTATION(#100068,#100113);
#100050=SHAPE_DEFINITION_REPRESENTATION(#100069,#100114);
#100051=SHAPE_DEFINITION_REPRESENTATION(#100070,#100115);
#100052=SHAPE_DEFINITION_REPRESENTATION(#100071,#100116);
#100053=SHAPE_DEFINITION_REPRESENTATION(#100072,#100117);
#100054=SHAPE_DEFINITION_REPRESENTATION(#100073,#100118);
#100055=PRODUCT_DEFINITION_SHAPE('',$,#100120);
#100056=PRODUCT_DEFINITION_SHAPE('',$,#100121);
#100057=PRODUCT_DEFINITION_SHAPE('',$,#100122);
#100058=PRODUCT_DEFINITION_SHAPE('',$,#100123);
#100059=PRODUCT_DEFINITION_SHAPE('',$,#100124);
#100060=PRODUCT_DEFINITION_SHAPE('',$,#100125);
#100061=PRODUCT_DEFINITION_SHAPE('',$,#100126);
#100062=PRODUCT_DEFINITION_SHAPE('',$,#100127);
#100063=PRODUCT_DEFINITION_SHAPE('',$,#100128);
#100064=PRODUCT_DEFINITION_SHAPE('',$,#100129);
#100065=PRODUCT_DEFINITION_SHAPE('',$,#100130);
#100066=PRODUCT_DEFINITION_SHAPE('',$,#100131);
#100067=PRODUCT_DEFINITION_SHAPE('',$,#100132);
#100068=PRODUCT_DEFINITION_SHAPE('',$,#100133);
#100069=PRODUCT_DEFINITION_SHAPE('',$,#100134);
#100070=PRODUCT_DEFINITION_SHAPE('',$,#100135);
#100071=PRODUCT_DEFINITION_SHAPE('',$,#100136);
#100072=PRODUCT_DEFINITION_SHAPE('',$,#100137);
#100073=PRODUCT_DEFINITION_SHAPE('',$,#100138);
#100074=PRODUCT_DEFINITION_SHAPE($,$,#89);
#100075=PRODUCT_DEFINITION_SHAPE($,$,#90);
#100076=PRODUCT_DEFINITION_SHAPE($,$,#91);
#100077=PRODUCT_DEFINITION_SHAPE($,$,#92);
#100078=PRODUCT_DEFINITION_SHAPE($,$,#93);
#100079=PRODUCT_DEFINITION_SHAPE($,$,#94);
#100080=PRODUCT_DEFINITION_SHAPE($,$,#95);
#100081=PRODUCT_DEFINITION_SHAPE($,$,#96);
#100082=PRODUCT_DEFINITION_SHAPE($,$,#97);
#100083=PRODUCT_DEFINITION_SHAPE($,$,#98);
#100084=PRODUCT_DEFINITION_SHAPE($,$,#99);
#100085=PRODUCT_DEFINITION_SHAPE($,$,#100);
#100086=PRODUCT_DEFINITION_SHAPE($,$,#101);
#100087=PRODUCT_DEFINITION_SHAPE($,$,#102);
#100088=PRODUCT_DEFINITION_SHAPE($,$,#103);
#100089=PRODUCT_DEFINITION_SHAPE($,$,#104);
#100090=PRODUCT_DEFINITION_SHAPE($,$,#105);
#100091=PRODUCT_DEFINITION_SHAPE($,$,#106);
#100092=PRODUCT_DEFINITION_SHAPE($,$,#107);
#100093=PRODUCT_DEFINITION_SHAPE($,$,#108);
#100094=PRODUCT_DEFINITION_SHAPE($,$,#109);
#100095=PRODUCT_DEFINITION_SHAPE($,$,#110);
#100096=PRODUCT_DEFINITION_SHAPE($,$,#111);
#100097=PRODUCT_DEFINITION_SHAPE($,$,#112);
#100098=PRODUCT_DEFINITION_SHAPE($,$,#113);
#100099=PRODUCT_DEFINITION_SHAPE($,$,#114);
#100100=SHAPE_REPRESENTATION('',(#20334,#22499,#22500,#22501,#22502,#22503,
#22504,#22505,#22506,#22507,#22508,#22509,#22510,#22511,#22512,#22513,#22514,
#22515,#22516,#22517,#22518,#22519,#22520,#22521,#22522,#22523,#22524),
#100012);
#100101=SHAPE_REPRESENTATION('',(#20335),#100013);
#100102=SHAPE_REPRESENTATION('',(#20343),#100014);
#100103=SHAPE_REPRESENTATION('',(#20892),#100015);
#100104=SHAPE_REPRESENTATION('',(#21261),#100016);
#100105=SHAPE_REPRESENTATION('',(#21437),#100017);
#100106=SHAPE_REPRESENTATION('',(#21537),#100018);
#100107=SHAPE_REPRESENTATION('',(#21611),#100019);
#100108=SHAPE_REPRESENTATION('',(#22152),#100020);
#100109=SHAPE_REPRESENTATION('',(#22157),#100021);
#100110=SHAPE_REPRESENTATION('',(#22218),#100022);
#100111=SHAPE_REPRESENTATION('',(#22351),#100023);
#100112=SHAPE_REPRESENTATION('',(#22404),#100024);
#100113=SHAPE_REPRESENTATION('',(#22417),#100025);
#100114=SHAPE_REPRESENTATION('',(#22427),#100026);
#100115=SHAPE_REPRESENTATION('',(#22437),#100027);
#100116=SHAPE_REPRESENTATION('',(#22465),#100028);
#100117=SHAPE_REPRESENTATION('',(#22475),#100029);
#100118=SHAPE_REPRESENTATION('',(#22489),#100030);
#100119=PRODUCT_DEFINITION_CONTEXT('part definition',#100178,'design');
#100120=PRODUCT_DEFINITION('2026-10-12-11-54-00-144',
'MAS-360',#100139,#100119);
#100121=PRODUCT_DEFINITION('2026-10-12-11-54-00-493',
'01_Release_Fork_Lever_Fork-A',#100140,#100119);
#100122=PRODUCT_DEFINITION('2026-10-12-11-54-52-874',
'02_Actuator_Frame_Plate',#100141,#100119);
#100123=PRODUCT_DEFINITION('2026-10-12-11-54-54-063',
'03_Coupling_Bracket_U-Channel',#100142,#100119);
#100124=PRODUCT_DEFINITION('2026-10-12-11-54-56-863',
'04_Motor_Coupling_Housing',#100143,#100119);
#100125=PRODUCT_DEFINITION('2026-10-12-11-54-59-762',
'05_Input_Spline_Bush_14T',#100144,#100119);
#100126=PRODUCT_DEFINITION('2026-10-12-11-55-01-005',
'06_Actuator_Spindle_M8x1.25',#100145,#100119);
#100127=PRODUCT_DEFINITION('2026-10-12-11-55-02-014',
'07_Spindle_Nut_Roller_Carriage',#100146,#100119);
#100128=PRODUCT_DEFINITION('2026-10-12-11-55-10-897',
'08_Compression_Spring_OD24',#100147,#100119);
#100129=PRODUCT_DEFINITION('2026-10-12-11-55-14-987',
'09_Spring_Seat_Clip_Band',#100148,#100119);
#100130=PRODUCT_DEFINITION('2026-10-12-11-55-30-112',
'18_Coupling_Cover_Leaf_Plate',#100149,#100119);
#100131=PRODUCT_DEFINITION('2026-10-12-11-55-17-173',
'10_Lever_Roller_D13x10.6',#100150,#100119);
#100132=PRODUCT_DEFINITION('2026-10-12-11-55-20-566',
'11_Support_Roller_D4.9x10.6',#100151,#100119);
#100133=PRODUCT_DEFINITION('2026-10-12-11-55-21-464',
'12_ISO_2338_Pin_3m6x16',#100152,#100119);
#100134=PRODUCT_DEFINITION('2026-10-12-11-55-22-396',
'13_ISO_2338_Pin_2.5m6x16',#100153,#100119);
#100135=PRODUCT_DEFINITION('2026-10-12-11-55-23-498',
'14_Stop_Post_Stepped_D9',#100154,#100119);
#100136=PRODUCT_DEFINITION('2026-10-12-11-55-24-841',
'15_ISO_8734_Dowel_5x8',#100155,#100119);
#100137=PRODUCT_DEFINITION('2026-10-12-11-55-27-737',
'16_ISO_1051_Rivet_4x7',#100156,#100119);
#100138=PRODUCT_DEFINITION('2026-10-12-11-55-28-971',
'17_ISO_1051_Rivet_2.5x5',#100157,#100119);
#100139=PRODUCT_DEFINITION_FORMATION('',$,#100180);
#100140=PRODUCT_DEFINITION_FORMATION('',$,#100181);
#100141=PRODUCT_DEFINITION_FORMATION('',$,#100182);
#100142=PRODUCT_DEFINITION_FORMATION('',$,#100183);
#100143=PRODUCT_DEFINITION_FORMATION('',$,#100184);
#100144=PRODUCT_DEFINITION_FORMATION('',$,#100185);
#100145=PRODUCT_DEFINITION_FORMATION('',$,#100186);
#100146=PRODUCT_DEFINITION_FORMATION('',$,#100187);
#100147=PRODUCT_DEFINITION_FORMATION('',$,#100188);
#100148=PRODUCT_DEFINITION_FORMATION('',$,#100189);
#100149=PRODUCT_DEFINITION_FORMATION('',$,#100190);
#100150=PRODUCT_DEFINITION_FORMATION('',$,#100191);
#100151=PRODUCT_DEFINITION_FORMATION('',$,#100192);
#100152=PRODUCT_DEFINITION_FORMATION('',$,#100193);
#100153=PRODUCT_DEFINITION_FORMATION('',$,#100194);
#100154=PRODUCT_DEFINITION_FORMATION('',$,#100195);
#100155=PRODUCT_DEFINITION_FORMATION('',$,#100196);
#100156=PRODUCT_DEFINITION_FORMATION('',$,#100197);
#100157=PRODUCT_DEFINITION_FORMATION('',$,#100198);
#100158=PRODUCT_RELATED_PRODUCT_CATEGORY(
'MAS-360','MAS-360',(#100180));
#100159=PRODUCT_RELATED_PRODUCT_CATEGORY('01_Release_Fork_Lever_Fork-A',
'01_Release_Fork_Lever_Fork-A',(#100181));
#100160=PRODUCT_RELATED_PRODUCT_CATEGORY('02_Actuator_Frame_Plate',
'02_Actuator_Frame_Plate',(#100182));
#100161=PRODUCT_RELATED_PRODUCT_CATEGORY(
'03_Coupling_Bracket_U-Channel','03_Coupling_Bracket_U-Channel',(#100183));
#100162=PRODUCT_RELATED_PRODUCT_CATEGORY('04_Motor_Coupling_Housing',
'04_Motor_Coupling_Housing',(#100184));
#100163=PRODUCT_RELATED_PRODUCT_CATEGORY('05_Input_Spline_Bush_14T',
'05_Input_Spline_Bush_14T',(#100185));
#100164=PRODUCT_RELATED_PRODUCT_CATEGORY('06_Actuator_Spindle_M8x1.25',
'06_Actuator_Spindle_M8x1.25',(#100186));
#100165=PRODUCT_RELATED_PRODUCT_CATEGORY(
'07_Spindle_Nut_Roller_Carriage','07_Spindle_Nut_Roller_Carriage',(#100187));
#100166=PRODUCT_RELATED_PRODUCT_CATEGORY('08_Compression_Spring_OD24',
'08_Compression_Spring_OD24',(#100188));
#100167=PRODUCT_RELATED_PRODUCT_CATEGORY('09_Spring_Seat_Clip_Band',
'09_Spring_Seat_Clip_Band',(#100189));
#100168=PRODUCT_RELATED_PRODUCT_CATEGORY('18_Coupling_Cover_Leaf_Plate',
'18_Coupling_Cover_Leaf_Plate',(#100190));
#100169=PRODUCT_RELATED_PRODUCT_CATEGORY('10_Lever_Roller_D13x10.6',
'10_Lever_Roller_D13x10.6',(#100191));
#100170=PRODUCT_RELATED_PRODUCT_CATEGORY('11_Support_Roller_D4.9x10.6',
'11_Support_Roller_D4.9x10.6',(#100192));
#100171=PRODUCT_RELATED_PRODUCT_CATEGORY('12_ISO_2338_Pin_3m6x16',
'12_ISO_2338_Pin_3m6x16',(#100193));
#100172=PRODUCT_RELATED_PRODUCT_CATEGORY('13_ISO_2338_Pin_2.5m6x16',
'13_ISO_2338_Pin_2.5m6x16',(#100194));
#100173=PRODUCT_RELATED_PRODUCT_CATEGORY('14_Stop_Post_Stepped_D9',
'14_Stop_Post_Stepped_D9',(#100195));
#100174=PRODUCT_RELATED_PRODUCT_CATEGORY('15_ISO_8734_Dowel_5x8',
'15_ISO_8734_Dowel_5x8',(#100196));
#100175=PRODUCT_RELATED_PRODUCT_CATEGORY('16_ISO_1051_Rivet_4x7',
'16_ISO_1051_Rivet_4x7',(#100197));
#100176=PRODUCT_RELATED_PRODUCT_CATEGORY('17_ISO_1051_Rivet_2.5x5',
'17_ISO_1051_Rivet_2.5x5',(#100198));
#100177=APPLICATION_PROTOCOL_DEFINITION('international standard',
'automotive_design',2009,#100178);
#100178=APPLICATION_CONTEXT(
'Core Data for Automotive Mechanical Design Process');
#100179=PRODUCT_CONTEXT('part definition',#100178,'mechanical');
#100180=PRODUCT('2026-10-12-11-54-00-144',
'MAS-360',$,(#100179));
#100181=PRODUCT('2026-10-12-11-54-00-493',
'01_Release_Fork_Lever_Fork-A',$,(#100179));
#100182=PRODUCT('2026-10-12-11-54-52-874','02_Actuator_Frame_Plate',$,(#100179));
#100183=PRODUCT('2026-10-12-11-54-54-063',
'03_Coupling_Bracket_U-Channel',$,(#100179));
#100184=PRODUCT('2026-10-12-11-54-56-863','04_Motor_Coupling_Housing',$,
(#100179));
#100185=PRODUCT('2026-10-12-11-54-59-762','05_Input_Spline_Bush_14T',$,
(#100179));
#100186=PRODUCT('2026-10-12-11-55-01-005','06_Actuator_Spindle_M8x1.25',
$,(#100179));
#100187=PRODUCT('2026-10-12-11-55-02-014',
'07_Spindle_Nut_Roller_Carriage',$,(#100179));
#100188=PRODUCT('2026-10-12-11-55-10-897','08_Compression_Spring_OD24',
$,(#100179));
#100189=PRODUCT('2026-10-12-11-55-14-987','09_Spring_Seat_Clip_Band',$,
(#100179));
#100190=PRODUCT('2026-10-12-11-55-30-112',
'18_Coupling_Cover_Leaf_Plate',$,(#100179));
#100191=PRODUCT('2026-10-12-11-55-17-173','10_Lever_Roller_D13x10.6',$,
(#100179));
#100192=PRODUCT('2026-10-12-11-55-20-566','11_Support_Roller_D4.9x10.6',
$,(#100179));
#100193=PRODUCT('2026-10-12-11-55-21-464','12_ISO_2338_Pin_3m6x16',$,(#100179));
#100194=PRODUCT('2026-10-12-11-55-22-396','13_ISO_2338_Pin_2.5m6x16',$,
(#100179));
#100195=PRODUCT('2026-10-12-11-55-23-498','14_Stop_Post_Stepped_D9',$,(#100179));
#100196=PRODUCT('2026-10-12-11-55-24-841','15_ISO_8734_Dowel_5x8',$,(#100179));
#100197=PRODUCT('2026-10-12-11-55-27-737','16_ISO_1051_Rivet_4x7',$,(#100179));
#100198=PRODUCT('2026-10-12-11-55-28-971','17_ISO_1051_Rivet_2.5x5',$,(#100179));
#100199=PRESENTATION_STYLE_ASSIGNMENT((#100205));
#100200=PRESENTATION_STYLE_ASSIGNMENT((#100206));
#100201=PRESENTATION_STYLE_ASSIGNMENT((#100207));
#100202=PRESENTATION_STYLE_ASSIGNMENT((#100208));
#100203=PRESENTATION_STYLE_ASSIGNMENT((#100209));
#100204=PRESENTATION_STYLE_ASSIGNMENT((#100210));
#100205=SURFACE_STYLE_USAGE(.BOTH.,#100211);
#100206=SURFACE_STYLE_USAGE(.BOTH.,#100212);
#100207=SURFACE_STYLE_USAGE(.BOTH.,#100213);
#100208=SURFACE_STYLE_USAGE(.BOTH.,#100214);
#100209=SURFACE_STYLE_USAGE(.BOTH.,#100215);
#100210=SURFACE_STYLE_USAGE(.BOTH.,#100216);
#100211=SURFACE_SIDE_STYLE('',(#100217));
#100212=SURFACE_SIDE_STYLE('',(#100218));
#100213=SURFACE_SIDE_STYLE('',(#100219));
#100214=SURFACE_SIDE_STYLE('',(#100220));
#100215=SURFACE_SIDE_STYLE('',(#100221));
#100216=SURFACE_SIDE_STYLE('',(#100222));
#100217=SURFACE_STYLE_FILL_AREA(#100223);
#100218=SURFACE_STYLE_FILL_AREA(#100224);
#100219=SURFACE_STYLE_FILL_AREA(#100225);
#100220=SURFACE_STYLE_FILL_AREA(#100226);
#100221=SURFACE_STYLE_FILL_AREA(#100227);
#100222=SURFACE_STYLE_FILL_AREA(#100228);
#100223=FILL_AREA_STYLE('Steel - Satin',(#100229));
#100224=FILL_AREA_STYLE('Opaque(227,224,212)',(#100230));
#100225=FILL_AREA_STYLE('Opaque(20,51,87)',(#100231));
#100226=FILL_AREA_STYLE('Opaque(31,36,43)',(#100232));
#100227=FILL_AREA_STYLE('Opaque(122,133,145)',(#100233));
#100228=FILL_AREA_STYLE('Opaque(97,158,199)',(#100234));
#100229=FILL_AREA_STYLE_COLOUR('Steel - Satin',#100235);
#100230=FILL_AREA_STYLE_COLOUR('Opaque(227,224,212)',#100236);
#100231=FILL_AREA_STYLE_COLOUR('Opaque(20,51,87)',#100237);
#100232=FILL_AREA_STYLE_COLOUR('Opaque(31,36,43)',#100238);
#100233=FILL_AREA_STYLE_COLOUR('Opaque(122,133,145)',#100239);
#100234=FILL_AREA_STYLE_COLOUR('Opaque(97,158,199)',#100240);
#100235=COLOUR_RGB('Steel - Satin',0.627450980392157,0.627450980392157,
0.627450980392157);
#100236=COLOUR_RGB('Opaque(227,224,212)',0.890196078431372,0.87843137254902,
0.831372549019608);
#100237=COLOUR_RGB('Opaque(20,51,87)',0.0784313725490196,0.2,0.341176470588235);
#100238=COLOUR_RGB('Opaque(31,36,43)',0.12156862745098,0.141176470588235,
0.168627450980392);
#100239=COLOUR_RGB('Opaque(122,133,145)',0.47843137254902,0.52156862745098,
0.568627450980392);
#100240=COLOUR_RGB('Opaque(97,158,199)',0.380392156862745,0.619607843137255,
0.780392156862745);
ENDSEC;
END-ISO-10303-21;
